#157446=CARTESIAN_POINT('Ctrl Pts',(-17.2910127431203,67.8540944890057,
12.));
#157447=CARTESIAN_POINT('Ctrl Pts',(-17.2911366591419,67.8424198971214,
0.));
#157448=CARTESIAN_POINT('Ctrl Pts',(-17.2911366591419,67.8424198971214,
12.));
#157449=CARTESIAN_POINT('Ctrl Pts',(-17.2912149114145,67.8346476309106,
0.));
#157450=CARTESIAN_POINT('Ctrl Pts',(-17.2912149114145,67.8346476309106,
12.));
#157451=CARTESIAN_POINT('Ctrl Pts',(-17.2912529479484,67.8307641965655,
0.));
#157452=CARTESIAN_POINT('Ctrl Pts',(-17.2912529479484,67.8307641965655,
12.));
#157453=CARTESIAN_POINT('',(-17.2912529479484,67.8307641965655,12.));
#157454=CARTESIAN_POINT('Ctrl Pts',(-17.2912529479484,67.8307641965655,
12.));
#157455=CARTESIAN_POINT('Ctrl Pts',(-17.2912149114145,67.8346476309106,
12.));
#157456=CARTESIAN_POINT('Ctrl Pts',(-17.2911366591419,67.8424198971214,
12.));
#157457=CARTESIAN_POINT('Ctrl Pts',(-17.2910127431203,67.8540944890057,
12.));
#157458=CARTESIAN_POINT('Ctrl Pts',(-17.2908344459816,67.8696929979178,
12.));
#157459=CARTESIAN_POINT('Ctrl Pts',(-17.2905897724029,67.8892451049871,
12.));
#157460=CARTESIAN_POINT('Ctrl Pts',(-17.2903232740717,67.908851149676,12.));
#157461=CARTESIAN_POINT('Ctrl Pts',(-17.2900349103956,67.9285110571662,
12.));
#157462=CARTESIAN_POINT('Ctrl Pts',(-17.2897246158895,67.9482246901517,
12.));
#157463=CARTESIAN_POINT('Ctrl Pts',(-17.2893923013852,67.9679918502441,
12.));
#157464=CARTESIAN_POINT('Ctrl Pts',(-17.2890378644843,67.9878123049133,
12.));
#157465=CARTESIAN_POINT('Ctrl Pts',(-17.28866119774,68.007685808115,12.));
#157466=CARTESIAN_POINT('Ctrl Pts',(-17.2882621974737,68.027612122741,12.));
#157467=CARTESIAN_POINT('Ctrl Pts',(-17.2878407730981,68.0475910442494,
12.));
#157468=CARTESIAN_POINT('Ctrl Pts',(-17.2873968440855,68.0676223930469,
12.));
#157469=CARTESIAN_POINT('Ctrl Pts',(-17.2869303355438,68.0877060033229,
12.));
#157470=CARTESIAN_POINT('Ctrl Pts',(-17.2864411745455,68.1078417137865,
12.));
#157471=CARTESIAN_POINT('Ctrl Pts',(-17.2859292855694,68.1280293561473,
12.));
#157472=CARTESIAN_POINT('Ctrl Pts',(-17.2853945882059,68.1482687493176,
12.));
#157473=CARTESIAN_POINT('Ctrl Pts',(-17.2848369995283,68.1685597054193,
12.));
#157474=CARTESIAN_POINT('Ctrl Pts',(-17.2842564355796,68.1889020335418,
12.));
#157475=CARTESIAN_POINT('Ctrl Pts',(-17.2836528130825,68.2092955440591,
12.));
#157476=CARTESIAN_POINT('Ctrl Pts',(-17.2830260513879,68.2297400535339,
12.));
#157477=CARTESIAN_POINT('Ctrl Pts',(-17.2823760723886,68.250235384512,12.));
#157478=CARTESIAN_POINT('Ctrl Pts',(-17.2817027995838,68.2707813631761,
12.));
#157479=CARTESIAN_POINT('Ctrl Pts',(-17.2810061574352,68.2913778177258,
12.));
#157480=CARTESIAN_POINT('Ctrl Pts',(-17.2802860705807,68.3120245763884,
12.));
#157481=CARTESIAN_POINT('Ctrl Pts',(-17.2795424631789,68.3327214657533,
12.));
#157482=CARTESIAN_POINT('Ctrl Pts',(-17.2787752592475,68.353468311648,12.));
#157483=CARTESIAN_POINT('Ctrl Pts',(-17.2779843829605,68.374264939895,12.));
#157484=CARTESIAN_POINT('Ctrl Pts',(-17.2771697589387,68.3951111770498,
12.));
#157485=CARTESIAN_POINT('Ctrl Pts',(-17.2763313126026,68.4160068512781,
12.));
#157486=CARTESIAN_POINT('Ctrl Pts',(-17.2754689703001,68.4369517926803,
12.));
#157487=CARTESIAN_POINT('Ctrl Pts',(-17.2745826591125,68.4579458328208,
12.));
#157488=CARTESIAN_POINT('Ctrl Pts',(-17.2736723067367,68.4789888044357,
12.));
#157489=CARTESIAN_POINT('Ctrl Pts',(-17.2727378413485,68.5000805410897,
12.));
#157490=CARTESIAN_POINT('Ctrl Pts',(-17.2717791914538,68.5212208767835,
12.));
#157491=CARTESIAN_POINT('Ctrl Pts',(-17.2707962858912,68.5424096459746,
12.));
#157492=CARTESIAN_POINT('Ctrl Pts',(-17.2697890538956,68.5636466837502,
12.));
#157493=CARTESIAN_POINT('Ctrl Pts',(-17.2687574251429,68.5849318259449,
12.));
#157494=CARTESIAN_POINT('Ctrl Pts',(-17.2677013298061,68.6062649092781,
12.));
#157495=CARTESIAN_POINT('Ctrl Pts',(-17.2666206986091,68.6276457714757,
12.));
#157496=CARTESIAN_POINT('Ctrl Pts',(-17.2655154627935,68.6490742512085,
12.));
#157497=CARTESIAN_POINT('Ctrl Pts',(-17.2643855540896,68.6705501880263,
12.));
#157498=CARTESIAN_POINT('Ctrl Pts',(-17.263230904689,68.6920734222932,12.));
#157499=CARTESIAN_POINT('Ctrl Pts',(-17.2620514472176,68.7136437951075,
12.));
#157500=CARTESIAN_POINT('Ctrl Pts',(-17.2608471147178,68.7352611482519,
12.));
#157501=CARTESIAN_POINT('Ctrl Pts',(-17.2596178406545,68.7569253242312,
12.));
#157502=CARTESIAN_POINT('Ctrl Pts',(-17.2583635589197,68.7786361662876,
12.));
#157503=CARTESIAN_POINT('Ctrl Pts',(-17.2570842038385,68.8003935184193,
12.));
#157504=CARTESIAN_POINT('Ctrl Pts',(-17.2557797101816,68.8221972253954,
12.));
#157505=CARTESIAN_POINT('Ctrl Pts',(-17.2544500131627,68.8440471327563,
12.));
#157506=CARTESIAN_POINT('Ctrl Pts',(-17.2530950484259,68.8659430867977,
12.));
#157507=CARTESIAN_POINT('Ctrl Pts',(-17.2517147520376,68.8878849345557,
12.));
#157508=CARTESIAN_POINT('Ctrl Pts',(-17.2503090604792,68.9098725237868,
12.));
#157509=CARTESIAN_POINT('Ctrl Pts',(-17.248877910643,68.9319057029407,12.));
#157510=CARTESIAN_POINT('Ctrl Pts',(-17.2474212398275,68.9539843211618,
12.));
#157511=CARTESIAN_POINT('Ctrl Pts',(-17.2459389857327,68.9761082282922,
12.));
#157512=CARTESIAN_POINT('Ctrl Pts',(-17.2444310864585,68.9982772748694,
12.));
#157513=CARTESIAN_POINT('Ctrl Pts',(-17.2428974805043,69.0204913121226,
12.));
#157514=CARTESIAN_POINT('Ctrl Pts',(-17.2413381067722,69.0427501919636,
12.));
#157515=CARTESIAN_POINT('Ctrl Pts',(-17.2397529045587,69.0650537669859,
12.));
#157516=CARTESIAN_POINT('Ctrl Pts',(-17.238141813549,69.0874018904598,12.));
#157517=CARTESIAN_POINT('Ctrl Pts',(-17.2365047738125,69.1097944163243,
12.));
#157518=CARTESIAN_POINT('Ctrl Pts',(-17.2348417258017,69.1322311991759,
12.));
#157519=CARTESIAN_POINT('Ctrl Pts',(-17.2331526103511,69.1547120942542,
12.));
#157520=CARTESIAN_POINT('Ctrl Pts',(-17.2314373686705,69.1772369574462,
12.));
#157521=CARTESIAN_POINT('Ctrl Pts',(-17.229695942341,69.1998056452837,12.));
#157522=CARTESIAN_POINT('Ctrl Pts',(-17.2279282733119,69.2224180149377,
12.));
#157523=CARTESIAN_POINT('Ctrl Pts',(-17.2261343039015,69.2450739242092,
12.));
#157524=CARTESIAN_POINT('Ctrl Pts',(-17.2243139767963,69.26777323152,12.));
#157525=CARTESIAN_POINT('Ctrl Pts',(-17.2224672350432,69.2905157959142,
12.));
#157526=CARTESIAN_POINT('Ctrl Pts',(-17.2205940220455,69.3133014770541,
12.));
#157527=CARTESIAN_POINT('Ctrl Pts',(-17.2186942815604,69.3361301352149,
12.));
#157528=CARTESIAN_POINT('Ctrl Pts',(-17.2167679576991,69.359001631272,12.));
#157529=CARTESIAN_POINT('Ctrl Pts',(-17.2148149949261,69.3819158266955,
12.));
#157530=CARTESIAN_POINT('Ctrl Pts',(-17.2128353380511,69.4048725835516,
12.));
#157531=CARTESIAN_POINT('Ctrl Pts',(-17.2108289322258,69.4278717644989,
12.));
#157532=CARTESIAN_POINT('Ctrl Pts',(-17.208795722942,69.4509132327836,12.));
#157533=CARTESIAN_POINT('Ctrl Pts',(-17.2067356560326,69.4739968522271,
12.));
#157534=CARTESIAN_POINT('Ctrl Pts',(-17.2046486776697,69.497122487222,12.));
#157535=CARTESIAN_POINT('Ctrl Pts',(-17.2025347343568,69.5202900027329,
12.));
#157536=CARTESIAN_POINT('Ctrl Pts',(-17.2003937729266,69.5434992642932,
12.));
#157537=CARTESIAN_POINT('Ctrl Pts',(-17.198225740538,69.5667501379984,12.));
#157538=CARTESIAN_POINT('Ctrl Pts',(-17.1960305846787,69.5900424904954,
12.));
#157539=CARTESIAN_POINT('Ctrl Pts',(-17.193808253162,69.6133761889787,12.));
#157540=CARTESIAN_POINT('Ctrl Pts',(-17.1915586941198,69.6367511011927,
12.));
#157541=CARTESIAN_POINT('Ctrl Pts',(-17.1892818560004,69.6601670954277,
12.));
#157542=CARTESIAN_POINT('Ctrl Pts',(-17.1869776875663,69.6836240405152,
12.));
#157543=CARTESIAN_POINT('Ctrl Pts',(-17.1846461378966,69.7071218058149,
12.));
#157544=CARTESIAN_POINT('Ctrl Pts',(-17.1822871563835,69.7306602612125,
12.));
#157545=CARTESIAN_POINT('Ctrl Pts',(-17.1799006927256,69.7542392771216,
12.));
#157546=CARTESIAN_POINT('Ctrl Pts',(-17.1774866969256,69.7778587244788,
12.));
#157547=CARTESIAN_POINT('Ctrl Pts',(-17.1750451192887,69.8015184747404,
12.));
#157548=CARTESIAN_POINT('Ctrl Pts',(-17.1725759104254,69.8252183998713,
12.));
#157549=CARTESIAN_POINT('Ctrl Pts',(-17.1700790212476,69.8489583723417,
12.));
#157550=CARTESIAN_POINT('Ctrl Pts',(-17.1675544029622,69.8727382651292,
12.));
#157551=CARTESIAN_POINT('Ctrl Pts',(-17.1650020070686,69.8965579517147,
12.));
#157552=CARTESIAN_POINT('Ctrl Pts',(-17.1624217853577,69.9204173060779,
12.));
#157553=CARTESIAN_POINT('Ctrl Pts',(-17.1598136899144,69.9443162026865,
12.));
#157554=CARTESIAN_POINT('Ctrl Pts',(-17.157177673114,69.9682545164942,12.));
#157555=CARTESIAN_POINT('Ctrl Pts',(-17.1545136876162,69.9922321229428,
12.));
#157556=CARTESIAN_POINT('Ctrl Pts',(-17.1518216863624,70.0162488979587,
12.));
#157557=CARTESIAN_POINT('Ctrl Pts',(-17.1491016225748,70.0403047179481,
12.));
#157558=CARTESIAN_POINT('Ctrl Pts',(-17.1463534497592,70.0643994597865,
12.));
#157559=CARTESIAN_POINT('Ctrl Pts',(-17.1435771217015,70.0885330008169,
12.));
#157560=CARTESIAN_POINT('Ctrl Pts',(-17.1407725924615,70.1127052188515,
12.));
#157561=CARTESIAN_POINT('Ctrl Pts',(-17.1379398163708,70.1369159921686,
12.));
#157562=CARTESIAN_POINT('Ctrl Pts',(-17.1350787480313,70.1611651995085,
12.));
#157563=CARTESIAN_POINT('Ctrl Pts',(-17.1321893423183,70.1854527200636,
12.));
#157564=CARTESIAN_POINT('Ctrl Pts',(-17.1292715543779,70.2097784334749,
12.));
#157565=CARTESIAN_POINT('Ctrl Pts',(-17.1263253396202,70.2341422198363,
12.));
#157566=CARTESIAN_POINT('Ctrl Pts',(-17.1233506537176,70.2585439596899,
12.));
#157567=CARTESIAN_POINT('Ctrl Pts',(-17.1203474526031,70.2829835340239,
12.));
#157568=CARTESIAN_POINT('Ctrl Pts',(-17.1173156924734,70.3074608242613,
12.));
#157569=CARTESIAN_POINT('Ctrl Pts',(-17.1142553297869,70.3319757122577,
12.));
#157570=CARTESIAN_POINT('Ctrl Pts',(-17.111166321257,70.356528080303,12.));
#157571=CARTESIAN_POINT('Ctrl Pts',(-17.10804862385,70.3811178111206,12.));
#157572=CARTESIAN_POINT('Ctrl Pts',(-17.1049021947833,70.4057447878621,
12.));
#157573=CARTESIAN_POINT('Ctrl Pts',(-17.1017269915289,70.4304088940998,
12.));
#157574=CARTESIAN_POINT('Ctrl Pts',(-17.098522971812,70.4551100138221,12.));
#157575=CARTESIAN_POINT('Ctrl Pts',(-17.0952900936044,70.4798480314364,
12.));
#157576=CARTESIAN_POINT('Ctrl Pts',(-17.0920283151217,70.5046228317669,
12.));
#157577=CARTESIAN_POINT('Ctrl Pts',(-17.0887375948221,70.5294343000516,
12.));
#157578=CARTESIAN_POINT('Ctrl Pts',(-17.085417891409,70.5542823219346,12.));
#157579=CARTESIAN_POINT('Ctrl Pts',(-17.0820691638314,70.5791667834599,
12.));
#157580=CARTESIAN_POINT('Ctrl Pts',(-17.0786913712767,70.6040875710762,
12.));
#157581=CARTESIAN_POINT('Ctrl Pts',(-17.0752844731679,70.6290445716341,
12.));
#157582=CARTESIAN_POINT('Ctrl Pts',(-17.0718484291623,70.6540376723839,
12.));
#157583=CARTESIAN_POINT('Ctrl Pts',(-17.0683831991532,70.6790667609678,
12.));
#157584=CARTESIAN_POINT('Ctrl Pts',(-17.0648887432714,70.7041317254128,
12.));
#157585=CARTESIAN_POINT('Ctrl Pts',(-17.0613650218789,70.7292324541348,
12.));
#157586=CARTESIAN_POINT('Ctrl Pts',(-17.0578119955651,70.754368835938,12.));
#157587=CARTESIAN_POINT('Ctrl Pts',(-17.0542296251462,70.7795407600127,
12.));
#157588=CARTESIAN_POINT('Ctrl Pts',(-17.0506178716662,70.8047481159298,
12.));
#157589=CARTESIAN_POINT('Ctrl Pts',(-17.0469766964001,70.8299907936334,
12.));
#157590=CARTESIAN_POINT('Ctrl Pts',(-17.0433060608475,70.8552686834423,
12.));
#157591=CARTESIAN_POINT('Ctrl Pts',(-17.0396059267277,70.8805816760501,
12.));
#157592=CARTESIAN_POINT('Ctrl Pts',(-17.0358762559786,70.9059296625214,
12.));
#157593=CARTESIAN_POINT('Ctrl Pts',(-17.0321170107564,70.9313125342876,
12.));
#157594=CARTESIAN_POINT('Ctrl Pts',(-17.0283281534392,70.956730183136,12.));
#157595=CARTESIAN_POINT('Ctrl Pts',(-17.0245096466229,70.9821825012136,
12.));
#157596=CARTESIAN_POINT('Ctrl Pts',(-17.0206614531166,71.0076693810301,
12.));
#157597=CARTESIAN_POINT('Ctrl Pts',(-17.0167835359419,71.0331907154574,
12.));
#157598=CARTESIAN_POINT('Ctrl Pts',(-17.0128758583335,71.0587463977268,
12.));
#157599=CARTESIAN_POINT('Ctrl Pts',(-17.0089383837437,71.0843363214221,
12.));
#157600=CARTESIAN_POINT('Ctrl Pts',(-17.0049710758394,71.1099603804786,
12.));
#157601=CARTESIAN_POINT('Ctrl Pts',(-17.0009738984936,71.1356184691806,
12.));
#157602=CARTESIAN_POINT('Ctrl Pts',(-16.9969468157824,71.1613104821568,
12.));
#157603=CARTESIAN_POINT('Ctrl Pts',(-16.9928897919828,71.187036314374,12.));
#157604=CARTESIAN_POINT('Ctrl Pts',(-16.9888027915742,71.212795861124,12.));
#157605=CARTESIAN_POINT('Ctrl Pts',(-16.9846857792384,71.2385890180221,
12.));
#157606=CARTESIAN_POINT('Ctrl Pts',(-16.9805387198571,71.2644156810198,
12.));
#157607=CARTESIAN_POINT('Ctrl Pts',(-16.9763615785137,71.290275746412,12.));
#157608=CARTESIAN_POINT('Ctrl Pts',(-16.9721543204951,71.3161691108427,
12.));
#157609=CARTESIAN_POINT('Ctrl Pts',(-16.9679169112994,71.3420956713082,
12.));
#157610=CARTESIAN_POINT('Ctrl Pts',(-16.9636493166397,71.3680553251562,
12.));
#157611=CARTESIAN_POINT('Ctrl Pts',(-16.9593515024276,71.3940479700677,
12.));
#157612=CARTESIAN_POINT('Ctrl Pts',(-16.9550234347621,71.4200735040384,
12.));
#157613=CARTESIAN_POINT('Ctrl Pts',(-16.9506650799189,71.4461318253563,
12.));
#157614=CARTESIAN_POINT('Ctrl Pts',(-16.9462764043443,71.4722228325794,
12.));
#157615=CARTESIAN_POINT('Ctrl Pts',(-16.9418573746489,71.4983464245055,
12.));
#157616=CARTESIAN_POINT('Ctrl Pts',(-16.9374079576201,71.5245025002139,
12.));
#157617=CARTESIAN_POINT('Ctrl Pts',(-16.9329281202377,71.5506909591129,
12.));
#157618=CARTESIAN_POINT('Ctrl Pts',(-16.9284178296933,71.5769117009842,
12.));
#157619=CARTESIAN_POINT('Ctrl Pts',(-16.9238770534071,71.6031646260174,
12.));
#157620=CARTESIAN_POINT('Ctrl Pts',(-16.9193057590607,71.6294496348653,
12.));
#157621=CARTESIAN_POINT('Ctrl Pts',(-16.9147039145717,71.6557666285917,
12.));
#157622=CARTESIAN_POINT('Ctrl Pts',(-16.9100714880368,71.6821155085612,
12.));
#157623=CARTESIAN_POINT('Ctrl Pts',(-16.9054084476847,71.7084961763357,
12.));
#157624=CARTESIAN_POINT('Ctrl Pts',(-16.9007147618344,71.7349085335796,
12.));
#157625=CARTESIAN_POINT('Ctrl Pts',(-16.895990398841,71.7613524819235,12.));
#157626=CARTESIAN_POINT('Ctrl Pts',(-16.8912353270942,71.7878279229546,
12.));
#157627=CARTESIAN_POINT('Ctrl Pts',(-16.8864495151344,71.8143347584962,
12.));
#157628=CARTESIAN_POINT('Ctrl Pts',(-16.881632931747,71.8408728908258,12.));
#157629=CARTESIAN_POINT('Ctrl Pts',(-16.87678554607,71.867442222915,12.));
#157630=CARTESIAN_POINT('Ctrl Pts',(-16.871907327697,71.8940426586534,12.));
#157631=CARTESIAN_POINT('Ctrl Pts',(-16.866998246792,71.9206741030887,12.));
#157632=CARTESIAN_POINT('Ctrl Pts',(-16.8620582738437,71.9473364618922,
12.));
#157633=CARTESIAN_POINT('Ctrl Pts',(-16.8570873794269,71.9740296408347,
12.));
#157634=CARTESIAN_POINT('Ctrl Pts',(-16.8520855339446,72.0007535452081,
12.));
#157635=CARTESIAN_POINT('Ctrl Pts',(-16.8470527074275,72.0275080793727,
12.));
#157636=CARTESIAN_POINT('Ctrl Pts',(-16.8419888691976,72.0542931459825,
12.));
#157637=CARTESIAN_POINT('Ctrl Pts',(-16.8368939881446,72.0811086466121,
12.));
#157638=CARTESIAN_POINT('Ctrl Pts',(-16.8317680333404,72.1079544831513,
12.));
#157639=CARTESIAN_POINT('Ctrl Pts',(-16.8266109745795,72.13483055902,12.));
#157640=CARTESIAN_POINT('Ctrl Pts',(-16.8214227828943,72.1617367803235,
12.));
#157641=CARTESIAN_POINT('Ctrl Pts',(-16.8162034312269,72.1886730573452,
12.));
#157642=CARTESIAN_POINT('Ctrl Pts',(-16.8109528945896,72.2156393048975,
12.));
#157643=CARTESIAN_POINT('Ctrl Pts',(-16.8064254147776,72.2387802230856,
12.));
#157644=CARTESIAN_POINT('Ctrl Pts',(-16.8029374213794,72.256538003526,12.));
#157645=CARTESIAN_POINT('Ctrl Pts',(-16.8005027425863,72.2688994295264,
12.));
#157646=CARTESIAN_POINT('Ctrl Pts',(-16.7991305317749,72.2758557891329,
12.));
#157647=CARTESIAN_POINT('Ctrl Pts',(-16.7988252568748,72.2774028393914,
12.));
#157648=CARTESIAN_POINT('',(-17.2912529479484,67.8307641965655,0.));
#157649=CARTESIAN_POINT('',(-17.2912529479484,67.8307641965655,0.));
#157650=CARTESIAN_POINT('Ctrl Pts',(-16.7988252568748,72.2774028393914,
0.));
#157651=CARTESIAN_POINT('Ctrl Pts',(-16.7991305317749,72.2758557891329,
0.));
#157652=CARTESIAN_POINT('Ctrl Pts',(-16.8005027425863,72.2688994295264,
0.));
#157653=CARTESIAN_POINT('Ctrl Pts',(-16.8029374213794,72.256538003526,0.));
#157654=CARTESIAN_POINT('Ctrl Pts',(-16.8064254147776,72.2387802230856,
0.));
#157655=CARTESIAN_POINT('Ctrl Pts',(-16.8109528945896,72.2156393048975,
0.));
#157656=CARTESIAN_POINT('Ctrl Pts',(-16.8162034312269,72.1886730573452,
0.));
#157657=CARTESIAN_POINT('Ctrl Pts',(-16.8214227828943,72.1617367803235,
0.));
#157658=CARTESIAN_POINT('Ctrl Pts',(-16.8266109745795,72.13483055902,0.));
#157659=CARTESIAN_POINT('Ctrl Pts',(-16.8317680333404,72.1079544831513,
0.));
#157660=CARTESIAN_POINT('Ctrl Pts',(-16.8368939881446,72.0811086466121,
0.));
#157661=CARTESIAN_POINT('Ctrl Pts',(-16.8419888691976,72.0542931459825,
0.));
#157662=CARTESIAN_POINT('Ctrl Pts',(-16.8470527074275,72.0275080793727,
0.));
#157663=CARTESIAN_POINT('Ctrl Pts',(-16.8520855339446,72.0007535452081,
0.));
#157664=CARTESIAN_POINT('Ctrl Pts',(-16.8570873794269,71.9740296408347,
0.));
#157665=CARTESIAN_POINT('Ctrl Pts',(-16.8620582738437,71.9473364618922,
0.));
#157666=CARTESIAN_POINT('Ctrl Pts',(-16.866998246792,71.9206741030887,0.));
#157667=CARTESIAN_POINT('Ctrl Pts',(-16.871907327697,71.8940426586534,0.));
#157668=CARTESIAN_POINT('Ctrl Pts',(-16.87678554607,71.867442222915,0.));
#157669=CARTESIAN_POINT('Ctrl Pts',(-16.881632931747,71.8408728908258,0.));
#157670=CARTESIAN_POINT('Ctrl Pts',(-16.8864495151344,71.8143347584962,
0.));
#157671=CARTESIAN_POINT('Ctrl Pts',(-16.8912353270942,71.7878279229546,
0.));
#157672=CARTESIAN_POINT('Ctrl Pts',(-16.895990398841,71.7613524819235,0.));
#157673=CARTESIAN_POINT('Ctrl Pts',(-16.9007147618344,71.7349085335796,
0.));
#157674=CARTESIAN_POINT('Ctrl Pts',(-16.9054084476847,71.7084961763357,
0.));
#157675=CARTESIAN_POINT('Ctrl Pts',(-16.9100714880368,71.6821155085612,
0.));
#157676=CARTESIAN_POINT('Ctrl Pts',(-16.9147039145717,71.6557666285917,
0.));
#157677=CARTESIAN_POINT('Ctrl Pts',(-16.9193057590607,71.6294496348653,
0.));
#157678=CARTESIAN_POINT('Ctrl Pts',(-16.9238770534071,71.6031646260174,
0.));
#157679=CARTESIAN_POINT('Ctrl Pts',(-16.9284178296933,71.5769117009842,
0.));
#157680=CARTESIAN_POINT('Ctrl Pts',(-16.9329281202377,71.5506909591129,
0.));
#157681=CARTESIAN_POINT('Ctrl Pts',(-16.9374079576201,71.5245025002139,
0.));
#157682=CARTESIAN_POINT('Ctrl Pts',(-16.9418573746489,71.4983464245055,
0.));
#157683=CARTESIAN_POINT('Ctrl Pts',(-16.9462764043443,71.4722228325794,
0.));
#157684=CARTESIAN_POINT('Ctrl Pts',(-16.9506650799189,71.4461318253563,
0.));
#157685=CARTESIAN_POINT('Ctrl Pts',(-16.9550234347621,71.4200735040384,
0.));
#157686=CARTESIAN_POINT('Ctrl Pts',(-16.9593515024276,71.3940479700677,
0.));
#157687=CARTESIAN_POINT('Ctrl Pts',(-16.9636493166397,71.3680553251562,
0.));
#157688=CARTESIAN_POINT('Ctrl Pts',(-16.9679169112994,71.3420956713082,
0.));
#157689=CARTESIAN_POINT('Ctrl Pts',(-16.9721543204951,71.3161691108427,
0.));
#157690=CARTESIAN_POINT('Ctrl Pts',(-16.9763615785137,71.290275746412,0.));
#157691=CARTESIAN_POINT('Ctrl Pts',(-16.9805387198571,71.2644156810198,
0.));
#157692=CARTESIAN_POINT('Ctrl Pts',(-16.9846857792384,71.2385890180221,
0.));
#157693=CARTESIAN_POINT('Ctrl Pts',(-16.9888027915742,71.212795861124,0.));
#157694=CARTESIAN_POINT('Ctrl Pts',(-16.9928897919828,71.187036314374,0.));
#157695=CARTESIAN_POINT('Ctrl Pts',(-16.9969468157824,71.1613104821568,
0.));
#157696=CARTESIAN_POINT('Ctrl Pts',(-17.0009738984936,71.1356184691806,
0.));
#157697=CARTESIAN_POINT('Ctrl Pts',(-17.0049710758394,71.1099603804786,
0.));
#157698=CARTESIAN_POINT('Ctrl Pts',(-17.0089383837437,71.0843363214221,
0.));
#157699=CARTESIAN_POINT('Ctrl Pts',(-17.0128758583335,71.0587463977268,
0.));
#157700=CARTESIAN_POINT('Ctrl Pts',(-17.0167835359419,71.0331907154574,
0.));
#157701=CARTESIAN_POINT('Ctrl Pts',(-17.0206614531166,71.0076693810301,
0.));
#157702=CARTESIAN_POINT('Ctrl Pts',(-17.0245096466229,70.9821825012136,
0.));
#157703=CARTESIAN_POINT('Ctrl Pts',(-17.0283281534392,70.956730183136,0.));
#157704=CARTESIAN_POINT('Ctrl Pts',(-17.0321170107564,70.9313125342876,
0.));
#157705=CARTESIAN_POINT('Ctrl Pts',(-17.0358762559786,70.9059296625214,
0.));
#157706=CARTESIAN_POINT('Ctrl Pts',(-17.0396059267277,70.8805816760501,
0.));
#157707=CARTESIAN_POINT('Ctrl Pts',(-17.0433060608475,70.8552686834423,
0.));
#157708=CARTESIAN_POINT('Ctrl Pts',(-17.0469766964001,70.8299907936334,
0.));
#157709=CARTESIAN_POINT('Ctrl Pts',(-17.0506178716662,70.8047481159298,
0.));
#157710=CARTESIAN_POINT('Ctrl Pts',(-17.0542296251462,70.7795407600127,
0.));
#157711=CARTESIAN_POINT('Ctrl Pts',(-17.0578119955651,70.754368835938,0.));
#157712=CARTESIAN_POINT('Ctrl Pts',(-17.0613650218789,70.7292324541348,
0.));
#157713=CARTESIAN_POINT('Ctrl Pts',(-17.0648887432714,70.7041317254128,
0.));
#157714=CARTESIAN_POINT('Ctrl Pts',(-17.0683831991532,70.6790667609678,
0.));
#157715=CARTESIAN_POINT('Ctrl Pts',(-17.0718484291623,70.6540376723839,
0.));
#157716=CARTESIAN_POINT('Ctrl Pts',(-17.0752844731679,70.6290445716341,
0.));
#157717=CARTESIAN_POINT('Ctrl Pts',(-17.0786913712767,70.6040875710762,
0.));
#157718=CARTESIAN_POINT('Ctrl Pts',(-17.0820691638314,70.5791667834599,
0.));
#157719=CARTESIAN_POINT('Ctrl Pts',(-17.085417891409,70.5542823219346,0.));
#157720=CARTESIAN_POINT('Ctrl Pts',(-17.0887375948221,70.5294343000516,
0.));
#157721=CARTESIAN_POINT('Ctrl Pts',(-17.0920283151217,70.5046228317669,
0.));
#157722=CARTESIAN_POINT('Ctrl Pts',(-17.0952900936044,70.4798480314364,
0.));
#157723=CARTESIAN_POINT('Ctrl Pts',(-17.098522971812,70.4551100138221,0.));
#157724=CARTESIAN_POINT('Ctrl Pts',(-17.1017269915289,70.4304088940998,
0.));
#157725=CARTESIAN_POINT('Ctrl Pts',(-17.1049021947833,70.4057447878621,
0.));
#157726=CARTESIAN_POINT('Ctrl Pts',(-17.10804862385,70.3811178111206,0.));
#157727=CARTESIAN_POINT('Ctrl Pts',(-17.111166321257,70.356528080303,0.));
#157728=CARTESIAN_POINT('Ctrl Pts',(-17.1142553297869,70.3319757122577,
0.));
#157729=CARTESIAN_POINT('Ctrl Pts',(-17.1173156924734,70.3074608242613,
0.));
#157730=CARTESIAN_POINT('Ctrl Pts',(-17.1203474526031,70.2829835340239,
0.));
#157731=CARTESIAN_POINT('Ctrl Pts',(-17.1233506537176,70.2585439596899,
0.));
#157732=CARTESIAN_POINT('Ctrl Pts',(-17.1263253396202,70.2341422198363,
0.));
#157733=CARTESIAN_POINT('Ctrl Pts',(-17.1292715543779,70.2097784334749,
0.));
#157734=CARTESIAN_POINT('Ctrl Pts',(-17.1321893423183,70.1854527200636,
0.));
#157735=CARTESIAN_POINT('Ctrl Pts',(-17.1350787480313,70.1611651995085,
0.));
#157736=CARTESIAN_POINT('Ctrl Pts',(-17.1379398163708,70.1369159921686,
0.));
#157737=CARTESIAN_POINT('Ctrl Pts',(-17.1407725924615,70.1127052188515,
0.));
#157738=CARTESIAN_POINT('Ctrl Pts',(-17.1435771217015,70.0885330008169,
0.));
#157739=CARTESIAN_POINT('Ctrl Pts',(-17.1463534497592,70.0643994597865,
0.));
#157740=CARTESIAN_POINT('Ctrl Pts',(-17.1491016225748,70.0403047179481,
0.));
#157741=CARTESIAN_POINT('Ctrl Pts',(-17.1518216863624,70.0162488979587,
0.));
#157742=CARTESIAN_POINT('Ctrl Pts',(-17.1545136876162,69.9922321229428,
0.));
#157743=CARTESIAN_POINT('Ctrl Pts',(-17.157177673114,69.9682545164942,0.));
#157744=CARTESIAN_POINT('Ctrl Pts',(-17.1598136899144,69.9443162026865,
0.));
#157745=CARTESIAN_POINT('Ctrl Pts',(-17.1624217853577,69.9204173060779,
0.));
#157746=CARTESIAN_POINT('Ctrl Pts',(-17.1650020070686,69.8965579517147,
0.));
#157747=CARTESIAN_POINT('Ctrl Pts',(-17.1675544029622,69.8727382651292,
0.));
#157748=CARTESIAN_POINT('Ctrl Pts',(-17.1700790212476,69.8489583723417,
0.));
#157749=CARTESIAN_POINT('Ctrl Pts',(-17.1725759104254,69.8252183998713,
0.));
#157750=CARTESIAN_POINT('Ctrl Pts',(-17.1750451192887,69.8015184747404,
0.));
#157751=CARTESIAN_POINT('Ctrl Pts',(-17.1774866969256,69.7778587244788,
0.));
#157752=CARTESIAN_POINT('Ctrl Pts',(-17.1799006927256,69.7542392771216,
0.));
#157753=CARTESIAN_POINT('Ctrl Pts',(-17.1822871563835,69.7306602612125,
0.));
#157754=CARTESIAN_POINT('Ctrl Pts',(-17.1846461378966,69.7071218058149,
0.));
#157755=CARTESIAN_POINT('Ctrl Pts',(-17.1869776875663,69.6836240405152,
0.));
#157756=CARTESIAN_POINT('Ctrl Pts',(-17.1892818560004,69.6601670954277,
0.));
#157757=CARTESIAN_POINT('Ctrl Pts',(-17.1915586941198,69.6367511011927,
0.));
#157758=CARTESIAN_POINT('Ctrl Pts',(-17.193808253162,69.6133761889787,0.));
#157759=CARTESIAN_POINT('Ctrl Pts',(-17.1960305846787,69.5900424904954,
0.));
#157760=CARTESIAN_POINT('Ctrl Pts',(-17.198225740538,69.5667501379984,0.));
#157761=CARTESIAN_POINT('Ctrl Pts',(-17.2003937729266,69.5434992642932,
0.));
#157762=CARTESIAN_POINT('Ctrl Pts',(-17.2025347343568,69.5202900027329,
0.));
#157763=CARTESIAN_POINT('Ctrl Pts',(-17.2046486776697,69.497122487222,0.));
#157764=CARTESIAN_POINT('Ctrl Pts',(-17.2067356560326,69.4739968522271,
0.));
#157765=CARTESIAN_POINT('Ctrl Pts',(-17.208795722942,69.4509132327836,0.));
#157766=CARTESIAN_POINT('Ctrl Pts',(-17.2108289322258,69.4278717644989,
0.));
#157767=CARTESIAN_POINT('Ctrl Pts',(-17.2128353380511,69.4048725835516,
0.));
#157768=CARTESIAN_POINT('Ctrl Pts',(-17.2148149949261,69.3819158266955,
0.));
#157769=CARTESIAN_POINT('Ctrl Pts',(-17.2167679576991,69.359001631272,0.));
#157770=CARTESIAN_POINT('Ctrl Pts',(-17.2186942815604,69.3361301352149,
0.));
#157771=CARTESIAN_POINT('Ctrl Pts',(-17.2205940220455,69.3133014770541,
0.));
#157772=CARTESIAN_POINT('Ctrl Pts',(-17.2224672350432,69.2905157959142,
0.));
#157773=CARTESIAN_POINT('Ctrl Pts',(-17.2243139767963,69.26777323152,0.));
#157774=CARTESIAN_POINT('Ctrl Pts',(-17.2261343039015,69.2450739242092,
0.));
#157775=CARTESIAN_POINT('Ctrl Pts',(-17.2279282733119,69.2224180149377,
0.));
#157776=CARTESIAN_POINT('Ctrl Pts',(-17.229695942341,69.1998056452837,0.));
#157777=CARTESIAN_POINT('Ctrl Pts',(-17.2314373686705,69.1772369574462,
0.));
#157778=CARTESIAN_POINT('Ctrl Pts',(-17.2331526103511,69.1547120942542,
0.));
#157779=CARTESIAN_POINT('Ctrl Pts',(-17.2348417258017,69.1322311991759,
0.));
#157780=CARTESIAN_POINT('Ctrl Pts',(-17.2365047738125,69.1097944163243,
0.));
#157781=CARTESIAN_POINT('Ctrl Pts',(-17.238141813549,69.0874018904598,0.));
#157782=CARTESIAN_POINT('Ctrl Pts',(-17.2397529045587,69.0650537669859,
0.));
#157783=CARTESIAN_POINT('Ctrl Pts',(-17.2413381067722,69.0427501919636,
0.));
#157784=CARTESIAN_POINT('Ctrl Pts',(-17.2428974805043,69.0204913121226,
0.));
#157785=CARTESIAN_POINT('Ctrl Pts',(-17.2444310864585,68.9982772748694,
0.));
#157786=CARTESIAN_POINT('Ctrl Pts',(-17.2459389857327,68.9761082282922,
0.));
#157787=CARTESIAN_POINT('Ctrl Pts',(-17.2474212398275,68.9539843211618,
0.));
#157788=CARTESIAN_POINT('Ctrl Pts',(-17.248877910643,68.9319057029407,0.));
#157789=CARTESIAN_POINT('Ctrl Pts',(-17.2503090604792,68.9098725237868,
0.));
#157790=CARTESIAN_POINT('Ctrl Pts',(-17.2517147520376,68.8878849345557,
0.));
#157791=CARTESIAN_POINT('Ctrl Pts',(-17.2530950484259,68.8659430867977,
0.));
#157792=CARTESIAN_POINT('Ctrl Pts',(-17.2544500131627,68.8440471327563,
0.));
#157793=CARTESIAN_POINT('Ctrl Pts',(-17.2557797101816,68.8221972253954,
0.));
#157794=CARTESIAN_POINT('Ctrl Pts',(-17.2570842038385,68.8003935184193,
0.));
#157795=CARTESIAN_POINT('Ctrl Pts',(-17.2583635589197,68.7786361662876,
0.));
#157796=CARTESIAN_POINT('Ctrl Pts',(-17.2596178406545,68.7569253242312,
0.));
#157797=CARTESIAN_POINT('Ctrl Pts',(-17.2608471147178,68.7352611482519,
0.));
#157798=CARTESIAN_POINT('Ctrl Pts',(-17.2620514472176,68.7136437951075,
0.));
#157799=CARTESIAN_POINT('Ctrl Pts',(-17.263230904689,68.6920734222932,0.));
#157800=CARTESIAN_POINT('Ctrl Pts',(-17.2643855540896,68.6705501880263,
0.));
#157801=CARTESIAN_POINT('Ctrl Pts',(-17.2655154627935,68.6490742512085,
0.));
#157802=CARTESIAN_POINT('Ctrl Pts',(-17.2666206986091,68.6276457714757,
0.));
#157803=CARTESIAN_POINT('Ctrl Pts',(-17.2677013298061,68.6062649092781,
0.));
#157804=CARTESIAN_POINT('Ctrl Pts',(-17.2687574251429,68.5849318259449,
0.));
#157805=CARTESIAN_POINT('Ctrl Pts',(-17.2697890538956,68.5636466837502,
0.));
#157806=CARTESIAN_POINT('Ctrl Pts',(-17.2707962858912,68.5424096459746,
0.));
#157807=CARTESIAN_POINT('Ctrl Pts',(-17.2717791914538,68.5212208767835,
0.));
#157808=CARTESIAN_POINT('Ctrl Pts',(-17.2727378413485,68.5000805410897,
0.));
#157809=CARTESIAN_POINT('Ctrl Pts',(-17.2736723067367,68.4789888044357,
0.));
#157810=CARTESIAN_POINT('Ctrl Pts',(-17.2745826591125,68.4579458328208,
0.));
#157811=CARTESIAN_POINT('Ctrl Pts',(-17.2754689703001,68.4369517926803,
0.));
#157812=CARTESIAN_POINT('Ctrl Pts',(-17.2763313126026,68.4160068512781,
0.));
#157813=CARTESIAN_POINT('Ctrl Pts',(-17.2771697589387,68.3951111770498,
0.));
#157814=CARTESIAN_POINT('Ctrl Pts',(-17.2779843829605,68.374264939895,0.));
#157815=CARTESIAN_POINT('Ctrl Pts',(-17.2787752592475,68.353468311648,0.));
#157816=CARTESIAN_POINT('Ctrl Pts',(-17.2795424631789,68.3327214657533,
0.));
#157817=CARTESIAN_POINT('Ctrl Pts',(-17.2802860705807,68.3120245763884,
0.));
#157818=CARTESIAN_POINT('Ctrl Pts',(-17.2810061574352,68.2913778177258,
0.));
#157819=CARTESIAN_POINT('Ctrl Pts',(-17.2817027995838,68.2707813631761,
0.));
#157820=CARTESIAN_POINT('Ctrl Pts',(-17.2823760723886,68.250235384512,0.));
#157821=CARTESIAN_POINT('Ctrl Pts',(-17.2830260513879,68.2297400535339,
0.));
#157822=CARTESIAN_POINT('Ctrl Pts',(-17.2836528130825,68.2092955440591,
0.));
#157823=CARTESIAN_POINT('Ctrl Pts',(-17.2842564355796,68.1889020335418,
0.));
#157824=CARTESIAN_POINT('Ctrl Pts',(-17.2848369995283,68.1685597054193,
0.));
#157825=CARTESIAN_POINT('Ctrl Pts',(-17.2853945882059,68.1482687493176,
0.));
#157826=CARTESIAN_POINT('Ctrl Pts',(-17.2859292855694,68.1280293561473,
0.));
#157827=CARTESIAN_POINT('Ctrl Pts',(-17.2864411745455,68.1078417137865,
0.));
#157828=CARTESIAN_POINT('Ctrl Pts',(-17.2869303355438,68.0877060033229,
0.));
#157829=CARTESIAN_POINT('Ctrl Pts',(-17.2873968440855,68.0676223930469,
0.));
#157830=CARTESIAN_POINT('Ctrl Pts',(-17.2878407730981,68.0475910442494,
0.));
#157831=CARTESIAN_POINT('Ctrl Pts',(-17.2882621974737,68.027612122741,0.));
#157832=CARTESIAN_POINT('Ctrl Pts',(-17.28866119774,68.007685808115,0.));
#157833=CARTESIAN_POINT('Ctrl Pts',(-17.2890378644843,67.9878123049133,
0.));
#157834=CARTESIAN_POINT('Ctrl Pts',(-17.2893923013852,67.9679918502441,
0.));
#157835=CARTESIAN_POINT('Ctrl Pts',(-17.2897246158895,67.9482246901517,
0.));
#157836=CARTESIAN_POINT('Ctrl Pts',(-17.2900349103956,67.9285110571662,
0.));
#157837=CARTESIAN_POINT('Ctrl Pts',(-17.2903232740717,67.908851149676,0.));
#157838=CARTESIAN_POINT('Ctrl Pts',(-17.2905897724029,67.8892451049871,
0.));
#157839=CARTESIAN_POINT('Ctrl Pts',(-17.2908344459816,67.8696929979178,
0.));
#157840=CARTESIAN_POINT('Ctrl Pts',(-17.2910127431203,67.8540944890057,
0.));
#157841=CARTESIAN_POINT('Ctrl Pts',(-17.2911366591419,67.8424198971214,
0.));
#157842=CARTESIAN_POINT('Ctrl Pts',(-17.2912149114145,67.8346476309106,
0.));
#157843=CARTESIAN_POINT('Ctrl Pts',(-17.2912529479484,67.8307641965655,
0.));
#157844=CARTESIAN_POINT('Ctrl Pts',(-10.343287191141,73.778495580227,0.));
#157845=CARTESIAN_POINT('Ctrl Pts',(-10.343287191141,73.778495580227,12.));
#157846=CARTESIAN_POINT('Ctrl Pts',(-10.3449014384453,73.7731377048058,
0.));
#157847=CARTESIAN_POINT('Ctrl Pts',(-10.3449014384453,73.7731377048058,
12.));
#157848=CARTESIAN_POINT('Ctrl Pts',(-10.3481265449342,73.7624245587789,
0.));
#157849=CARTESIAN_POINT('Ctrl Pts',(-10.3481265449342,73.7624245587789,
12.));
#157850=CARTESIAN_POINT('Ctrl Pts',(-10.3529540403092,73.7463626541854,
0.));
#157851=CARTESIAN_POINT('Ctrl Pts',(-10.3529540403092,73.7463626541854,
12.));
#157852=CARTESIAN_POINT('Ctrl Pts',(-10.359370371262,73.7249624109173,0.));
#157853=CARTESIAN_POINT('Ctrl Pts',(-10.359370371262,73.7249624109173,12.));
#157854=CARTESIAN_POINT('Ctrl Pts',(-10.3673568984582,73.6982381645206,
0.));
#157855=CARTESIAN_POINT('Ctrl Pts',(-10.3673568984582,73.6982381645206,
12.));
#157856=CARTESIAN_POINT('Ctrl Pts',(-10.3753095356342,73.6715399947839,
0.));
#157857=CARTESIAN_POINT('Ctrl Pts',(-10.3753095356342,73.6715399947839,
12.));
#157858=CARTESIAN_POINT('Ctrl Pts',(-10.3832282820371,73.6448679350696,
0.));
#157859=CARTESIAN_POINT('Ctrl Pts',(-10.3832282820371,73.6448679350696,
12.));
#157860=CARTESIAN_POINT('Ctrl Pts',(-10.3911131417463,73.6182220363156,
0.));
#157861=CARTESIAN_POINT('Ctrl Pts',(-10.3911131417463,73.6182220363156,
12.));
#157862=CARTESIAN_POINT('Ctrl Pts',(-10.3989641265285,73.5916023719713,
0.));
#157863=CARTESIAN_POINT('Ctrl Pts',(-10.3989641265285,73.5916023719713,
12.));
#157864=CARTESIAN_POINT('Ctrl Pts',(-10.406781255551,73.5650090359839,0.));
#157865=CARTESIAN_POINT('Ctrl Pts',(-10.406781255551,73.5650090359839,12.));
#157866=CARTESIAN_POINT('Ctrl Pts',(-10.414564552681,73.5384421354543,0.));
#157867=CARTESIAN_POINT('Ctrl Pts',(-10.414564552681,73.5384421354543,12.));
#157868=CARTESIAN_POINT('Ctrl Pts',(-10.4223140444605,73.5119017847575,
0.));
#157869=CARTESIAN_POINT('Ctrl Pts',(-10.4223140444605,73.5119017847575,
12.));
#157870=CARTESIAN_POINT('Ctrl Pts',(-10.430029757865,73.485388099225,0.));
#157871=CARTESIAN_POINT('Ctrl Pts',(-10.430029757865,73.485388099225,12.));
#157872=CARTESIAN_POINT('Ctrl Pts',(-10.4377117180222,73.4589011886197,
0.));
#157873=CARTESIAN_POINT('Ctrl Pts',(-10.4377117180222,73.4589011886197,
12.));
#157874=CARTESIAN_POINT('Ctrl Pts',(-10.4453599463547,73.4324411518554,
0.));
#157875=CARTESIAN_POINT('Ctrl Pts',(-10.4453599463547,73.4324411518554,
12.));
#157876=CARTESIAN_POINT('Ctrl Pts',(-10.452974461845,73.4060080806686,0.));
#157877=CARTESIAN_POINT('Ctrl Pts',(-10.452974461845,73.4060080806686,12.));
#157878=CARTESIAN_POINT('Ctrl Pts',(-10.4605552819397,73.37960206225,0.));
#157879=CARTESIAN_POINT('Ctrl Pts',(-10.4605552819397,73.37960206225,12.));
#157880=CARTESIAN_POINT('Ctrl Pts',(-10.4681024236289,73.3532231823659,
0.));
#157881=CARTESIAN_POINT('Ctrl Pts',(-10.4681024236289,73.3532231823659,
12.));
#157882=CARTESIAN_POINT('Ctrl Pts',(-10.4756159043806,73.3268715280575,
0.));
#157883=CARTESIAN_POINT('Ctrl Pts',(-10.4756159043806,73.3268715280575,
12.));
#157884=CARTESIAN_POINT('Ctrl Pts',(-10.4830957433305,73.3005471910583,
0.));
#157885=CARTESIAN_POINT('Ctrl Pts',(-10.4830957433305,73.3005471910583,
12.));
#157886=CARTESIAN_POINT('Ctrl Pts',(-10.4905419611523,73.2742502674304,
0.));
#157887=CARTESIAN_POINT('Ctrl Pts',(-10.4905419611523,73.2742502674304,
12.));
#157888=CARTESIAN_POINT('Ctrl Pts',(-10.4979545795192,73.2479808560189,
0.));
#157889=CARTESIAN_POINT('Ctrl Pts',(-10.4979545795192,73.2479808560189,
12.));
#157890=CARTESIAN_POINT('Ctrl Pts',(-10.5053336206908,73.2217390572562,
0.));
#157891=CARTESIAN_POINT('Ctrl Pts',(-10.5053336206908,73.2217390572562,
12.));
#157892=CARTESIAN_POINT('Ctrl Pts',(-10.5126791070805,73.1955249719048,
0.));
#157893=CARTESIAN_POINT('Ctrl Pts',(-10.5126791070805,73.1955249719048,
12.));
#157894=CARTESIAN_POINT('Ctrl Pts',(-10.5199910607654,73.1693386996138,
0.));
#157895=CARTESIAN_POINT('Ctrl Pts',(-10.5199910607654,73.1693386996138,
12.));
#157896=CARTESIAN_POINT('Ctrl Pts',(-10.5272695032653,73.1431803382711,
0.));
#157897=CARTESIAN_POINT('Ctrl Pts',(-10.5272695032653,73.1431803382711,
12.));
#157898=CARTESIAN_POINT('Ctrl Pts',(-10.53451445581,73.1170499848039,0.));
#157899=CARTESIAN_POINT('Ctrl Pts',(-10.53451445581,73.1170499848039,12.));
#157900=CARTESIAN_POINT('Ctrl Pts',(-10.5417259395003,73.0909477356474,
0.));
#157901=CARTESIAN_POINT('Ctrl Pts',(-10.5417259395003,73.0909477356474,
12.));
#157902=CARTESIAN_POINT('Ctrl Pts',(-10.5489039755138,73.0648736873434,
0.));
#157903=CARTESIAN_POINT('Ctrl Pts',(-10.5489039755138,73.0648736873434,
12.));
#157904=CARTESIAN_POINT('Ctrl Pts',(-10.5560485852974,73.0388279370834,
0.));
#157905=CARTESIAN_POINT('Ctrl Pts',(-10.5560485852974,73.0388279370834,
12.));
#157906=CARTESIAN_POINT('Ctrl Pts',(-10.5631597907651,73.0128105832621,
0.));
#157907=CARTESIAN_POINT('Ctrl Pts',(-10.5631597907651,73.0128105832621,
12.));
#157908=CARTESIAN_POINT('Ctrl Pts',(-10.570237614205,72.9868217252283,0.));
#157909=CARTESIAN_POINT('Ctrl Pts',(-10.570237614205,72.9868217252283,12.));
#157910=CARTESIAN_POINT('Ctrl Pts',(-10.5772820781958,72.9608614630534,
0.));
#157911=CARTESIAN_POINT('Ctrl Pts',(-10.5772820781958,72.9608614630534,
12.));
#157912=CARTESIAN_POINT('Ctrl Pts',(-10.5842932055209,72.9349298972822,
0.));
#157913=CARTESIAN_POINT('Ctrl Pts',(-10.5842932055209,72.9349298972822,
12.));
#157914=CARTESIAN_POINT('Ctrl Pts',(-10.5912710190928,72.9090271287083,
0.));
#157915=CARTESIAN_POINT('Ctrl Pts',(-10.5912710190928,72.9090271287083,
12.));
#157916=CARTESIAN_POINT('Ctrl Pts',(-10.5982155418626,72.8831532580845,
0.));
#157917=CARTESIAN_POINT('Ctrl Pts',(-10.5982155418626,72.8831532580845,
12.));
#157918=CARTESIAN_POINT('Ctrl Pts',(-10.6051267968203,72.8573083861337,
0.));
#157919=CARTESIAN_POINT('Ctrl Pts',(-10.6051267968203,72.8573083861337,
12.));
#157920=CARTESIAN_POINT('Ctrl Pts',(-10.6120048070367,72.8314926136881,
0.));
#157921=CARTESIAN_POINT('Ctrl Pts',(-10.6120048070367,72.8314926136881,
12.));
#157922=CARTESIAN_POINT('Ctrl Pts',(-10.6188495956973,72.8057060417887,
0.));
#157923=CARTESIAN_POINT('Ctrl Pts',(-10.6188495956973,72.8057060417887,
12.));
#157924=CARTESIAN_POINT('Ctrl Pts',(-10.6256611861394,72.7799487717911,
0.));
#157925=CARTESIAN_POINT('Ctrl Pts',(-10.6256611861394,72.7799487717911,
12.));
#157926=CARTESIAN_POINT('Ctrl Pts',(-10.6324396018998,72.7542209054812,
0.));
#157927=CARTESIAN_POINT('Ctrl Pts',(-10.6324396018998,72.7542209054812,
12.));
#157928=CARTESIAN_POINT('Ctrl Pts',(-10.6391848667352,72.7285225451293,
0.));
#157929=CARTESIAN_POINT('Ctrl Pts',(-10.6391848667352,72.7285225451293,
12.));
#157930=CARTESIAN_POINT('Ctrl Pts',(-10.6458970045946,72.7028537934317,
0.));
#157931=CARTESIAN_POINT('Ctrl Pts',(-10.6458970045946,72.7028537934317,
12.));
#157932=CARTESIAN_POINT('Ctrl Pts',(-10.6525760396054,72.6772147534752,
0.));
#157933=CARTESIAN_POINT('Ctrl Pts',(-10.6525760396054,72.6772147534752,
12.));
#157934=CARTESIAN_POINT('Ctrl Pts',(-10.659221996058,72.651605528691,0.));
#157935=CARTESIAN_POINT('Ctrl Pts',(-10.659221996058,72.651605528691,12.));
#157936=CARTESIAN_POINT('Ctrl Pts',(-10.6658348983944,72.6260262228065,
0.));
#157937=CARTESIAN_POINT('Ctrl Pts',(-10.6658348983944,72.6260262228065,
12.));
#157938=CARTESIAN_POINT('Ctrl Pts',(-10.6724147711995,72.6004769398019,
0.));
#157939=CARTESIAN_POINT('Ctrl Pts',(-10.6724147711995,72.6004769398019,
12.));
#157940=CARTESIAN_POINT('Ctrl Pts',(-10.6789616392042,72.5749577839415,
0.));
#157941=CARTESIAN_POINT('Ctrl Pts',(-10.6789616392042,72.5749577839415,
12.));
#157942=CARTESIAN_POINT('Ctrl Pts',(-10.6854755272904,72.5494688597961,
0.));
#157943=CARTESIAN_POINT('Ctrl Pts',(-10.6854755272904,72.5494688597961,
12.));
#157944=CARTESIAN_POINT('Ctrl Pts',(-10.691956460499,72.5240102722664,0.));
#157945=CARTESIAN_POINT('Ctrl Pts',(-10.691956460499,72.5240102722664,12.));
#157946=CARTESIAN_POINT('Ctrl Pts',(-10.6984044640398,72.4985821266023,
0.));
#157947=CARTESIAN_POINT('Ctrl Pts',(-10.6984044640398,72.4985821266023,
12.));
#157948=CARTESIAN_POINT('Ctrl Pts',(-10.7048195633061,72.4731845284227,
0.));
#157949=CARTESIAN_POINT('Ctrl Pts',(-10.7048195633061,72.4731845284227,
12.));
#157950=CARTESIAN_POINT('Ctrl Pts',(-10.7112017838706,72.4478175837156,
0.));
#157951=CARTESIAN_POINT('Ctrl Pts',(-10.7112017838706,72.4478175837156,
12.));
#157952=CARTESIAN_POINT('Ctrl Pts',(-10.7175511514788,72.4224813988347,
0.));
#157953=CARTESIAN_POINT('Ctrl Pts',(-10.7175511514788,72.4224813988347,
12.));
#157954=CARTESIAN_POINT('Ctrl Pts',(-10.7238676920469,72.3971760804933,
0.));
#157955=CARTESIAN_POINT('Ctrl Pts',(-10.7238676920469,72.3971760804933,
12.));
#157956=CARTESIAN_POINT('Ctrl Pts',(-10.7301514316607,72.3719017357571,
0.));
#157957=CARTESIAN_POINT('Ctrl Pts',(-10.7301514316607,72.3719017357571,
12.));
#157958=CARTESIAN_POINT('Ctrl Pts',(-10.73640239658,72.3466584720318,0.));
#157959=CARTESIAN_POINT('Ctrl Pts',(-10.73640239658,72.3466584720318,12.));
#157960=CARTESIAN_POINT('Ctrl Pts',(-10.7426206132375,72.3214463970641,
0.));
#157961=CARTESIAN_POINT('Ctrl Pts',(-10.7426206132375,72.3214463970641,
12.));
#157962=CARTESIAN_POINT('Ctrl Pts',(-10.7488061082368,72.2962656189556,
0.));
#157963=CARTESIAN_POINT('Ctrl Pts',(-10.7488061082368,72.2962656189556,
12.));
#157964=CARTESIAN_POINT('Ctrl Pts',(-10.7549589083535,72.2711162461681,
0.));
#157965=CARTESIAN_POINT('Ctrl Pts',(-10.7549589083535,72.2711162461681,
12.));
#157966=CARTESIAN_POINT('Ctrl Pts',(-10.7610790405385,72.2459983875296,
0.));
#157967=CARTESIAN_POINT('Ctrl Pts',(-10.7610790405385,72.2459983875296,
12.));
#157968=CARTESIAN_POINT('Ctrl Pts',(-10.7671665319255,72.2209121522366,
0.));
#157969=CARTESIAN_POINT('Ctrl Pts',(-10.7671665319255,72.2209121522366,
12.));
#157970=CARTESIAN_POINT('Ctrl Pts',(-10.7732214098344,72.1958576498558,
0.));
#157971=CARTESIAN_POINT('Ctrl Pts',(-10.7732214098344,72.1958576498558,
12.));
#157972=CARTESIAN_POINT('Ctrl Pts',(-10.7792437017662,72.1708349903305,
0.));
#157973=CARTESIAN_POINT('Ctrl Pts',(-10.7792437017662,72.1708349903305,
12.));
#157974=CARTESIAN_POINT('Ctrl Pts',(-10.7852334354016,72.1458442839834,
0.));
#157975=CARTESIAN_POINT('Ctrl Pts',(-10.7852334354016,72.1458442839834,
12.));
#157976=CARTESIAN_POINT('Ctrl Pts',(-10.7911906386027,72.1208856415171,
0.));
#157977=CARTESIAN_POINT('Ctrl Pts',(-10.7911906386027,72.1208856415171,
12.));
#157978=CARTESIAN_POINT('Ctrl Pts',(-10.7971153394166,72.0959591740114,
0.));
#157979=CARTESIAN_POINT('Ctrl Pts',(-10.7971153394166,72.0959591740114,
12.));
#157980=CARTESIAN_POINT('Ctrl Pts',(-10.8030075660808,72.0710649929202,
0.));
#157981=CARTESIAN_POINT('Ctrl Pts',(-10.8030075660808,72.0710649929202,
12.));
#157982=CARTESIAN_POINT('Ctrl Pts',(-10.8088673470184,72.0462032100815,
0.));
#157983=CARTESIAN_POINT('Ctrl Pts',(-10.8088673470184,72.0462032100815,
12.));
#157984=CARTESIAN_POINT('Ctrl Pts',(-10.8146947108375,72.0213739377223,
0.));
#157985=CARTESIAN_POINT('Ctrl Pts',(-10.8146947108375,72.0213739377223,
12.));
#157986=CARTESIAN_POINT('Ctrl Pts',(-10.8204896863328,71.9965772884619,
0.));
#157987=CARTESIAN_POINT('Ctrl Pts',(-10.8204896863328,71.9965772884619,
12.));
#157988=CARTESIAN_POINT('Ctrl Pts',(-10.8262523024898,71.9718133753127,
0.));
#157989=CARTESIAN_POINT('Ctrl Pts',(-10.8262523024898,71.9718133753127,
12.));
#157990=CARTESIAN_POINT('Ctrl Pts',(-10.8319825884918,71.9470823116785,
0.));
#157991=CARTESIAN_POINT('Ctrl Pts',(-10.8319825884918,71.9470823116785,
12.));
#157992=CARTESIAN_POINT('Ctrl Pts',(-10.8376805737159,71.9223842113625,
0.));
#157993=CARTESIAN_POINT('Ctrl Pts',(-10.8376805737159,71.9223842113625,
12.));
#157994=CARTESIAN_POINT('Ctrl Pts',(-10.8433462877311,71.8977191885725,
0.));
#157995=CARTESIAN_POINT('Ctrl Pts',(-10.8433462877311,71.8977191885725,
12.));
#157996=CARTESIAN_POINT('Ctrl Pts',(-10.8489797602997,71.8730873579224,
0.));
#157997=CARTESIAN_POINT('Ctrl Pts',(-10.8489797602997,71.8730873579224,
12.));
#157998=CARTESIAN_POINT('Ctrl Pts',(-10.8545810213799,71.8484888344339,
0.));
#157999=CARTESIAN_POINT('Ctrl Pts',(-10.8545810213799,71.8484888344339,
12.));
#158000=CARTESIAN_POINT('Ctrl Pts',(-10.8601501011332,71.8239237335331,
0.));
#158001=CARTESIAN_POINT('Ctrl Pts',(-10.8601501011332,71.8239237335331,
12.));
#158002=CARTESIAN_POINT('Ctrl Pts',(-10.865687029922,71.7993921710564,0.));
#158003=CARTESIAN_POINT('Ctrl Pts',(-10.865687029922,71.7993921710564,12.));
#158004=CARTESIAN_POINT('Ctrl Pts',(-10.8711918383073,71.7748942632593,
0.));
#158005=CARTESIAN_POINT('Ctrl Pts',(-10.8711918383073,71.7748942632593,
12.));
#158006=CARTESIAN_POINT('Ctrl Pts',(-10.8766645570497,71.7504301268181,
0.));
#158007=CARTESIAN_POINT('Ctrl Pts',(-10.8766645570497,71.7504301268181,
12.));
#158008=CARTESIAN_POINT('Ctrl Pts',(-10.8821052171121,71.7259998788328,
0.));
#158009=CARTESIAN_POINT('Ctrl Pts',(-10.8821052171121,71.7259998788328,
12.));
#158010=CARTESIAN_POINT('Ctrl Pts',(-10.8875138496671,71.7016036368236,
0.));
#158011=CARTESIAN_POINT('Ctrl Pts',(-10.8875138496671,71.7016036368236,
12.));
#158012=CARTESIAN_POINT('Ctrl Pts',(-10.8928904860964,71.6772415187364,
0.));
#158013=CARTESIAN_POINT('Ctrl Pts',(-10.8928904860964,71.6772415187364,
12.));
#158014=CARTESIAN_POINT('Ctrl Pts',(-10.8982351579871,71.6529136429504,
0.));
#158015=CARTESIAN_POINT('Ctrl Pts',(-10.8982351579871,71.6529136429504,
12.));
#158016=CARTESIAN_POINT('Ctrl Pts',(-10.9035478971328,71.6286201282812,
0.));
#158017=CARTESIAN_POINT('Ctrl Pts',(-10.9035478971328,71.6286201282812,
12.));
#158018=CARTESIAN_POINT('Ctrl Pts',(-10.9088287355365,71.6043610939835,
0.));
#158019=CARTESIAN_POINT('Ctrl Pts',(-10.9088287355365,71.6043610939835,
12.));
#158020=CARTESIAN_POINT('Ctrl Pts',(-10.914077705417,71.5801366597488,0.));
#158021=CARTESIAN_POINT('Ctrl Pts',(-10.914077705417,71.5801366597488,12.));
#158022=CARTESIAN_POINT('Ctrl Pts',(-10.91929483921,71.5559469457091,0.));
#158023=CARTESIAN_POINT('Ctrl Pts',(-10.91929483921,71.5559469457091,12.));
#158024=CARTESIAN_POINT('Ctrl Pts',(-10.9244801695642,71.5317920724459,
0.));
#158025=CARTESIAN_POINT('Ctrl Pts',(-10.9244801695642,71.5317920724459,
12.));
#158026=CARTESIAN_POINT('Ctrl Pts',(-10.9296337293424,71.5076721609937,
0.));
#158027=CARTESIAN_POINT('Ctrl Pts',(-10.9296337293424,71.5076721609937,
12.));
#158028=CARTESIAN_POINT('Ctrl Pts',(-10.9347555516235,71.4835873328423,
0.));
#158029=CARTESIAN_POINT('Ctrl Pts',(-10.9347555516235,71.4835873328423,
12.));
#158030=CARTESIAN_POINT('Ctrl Pts',(-10.9398456697095,71.4595377099351,
0.));
#158031=CARTESIAN_POINT('Ctrl Pts',(-10.9398456697095,71.4595377099351,
12.));
#158032=CARTESIAN_POINT('Ctrl Pts',(-10.944904117127,71.435523414672,0.));
#158033=CARTESIAN_POINT('Ctrl Pts',(-10.944904117127,71.435523414672,12.));
#158034=CARTESIAN_POINT('Ctrl Pts',(-10.9499309276236,71.4115445699194,
0.));
#158035=CARTESIAN_POINT('Ctrl Pts',(-10.9499309276236,71.4115445699194,
12.));
#158036=CARTESIAN_POINT('Ctrl Pts',(-10.954926135169,71.3876012990138,0.));
#158037=CARTESIAN_POINT('Ctrl Pts',(-10.954926135169,71.3876012990138,12.));
#158038=CARTESIAN_POINT('Ctrl Pts',(-10.9598897739564,71.3636937257649,
0.));
#158039=CARTESIAN_POINT('Ctrl Pts',(-10.9598897739564,71.3636937257649,
12.));
#158040=CARTESIAN_POINT('Ctrl Pts',(-10.9648218784098,71.339821974454,0.));
#158041=CARTESIAN_POINT('Ctrl Pts',(-10.9648218784098,71.339821974454,12.));
#158042=CARTESIAN_POINT('Ctrl Pts',(-10.969722483186,71.3159861698358,0.));
#158043=CARTESIAN_POINT('Ctrl Pts',(-10.969722483186,71.3159861698358,12.));
#158044=CARTESIAN_POINT('Ctrl Pts',(-10.9745916231709,71.2921864371491,
0.));
#158045=CARTESIAN_POINT('Ctrl Pts',(-10.9745916231709,71.2921864371491,
12.));
#158046=CARTESIAN_POINT('Ctrl Pts',(-10.9794293334805,71.2684229021207,
0.));
#158047=CARTESIAN_POINT('Ctrl Pts',(-10.9794293334805,71.2684229021207,
12.));
#158048=CARTESIAN_POINT('Ctrl Pts',(-10.9842356494627,71.2446956909687,
0.));
#158049=CARTESIAN_POINT('Ctrl Pts',(-10.9842356494627,71.2446956909687,
12.));
#158050=CARTESIAN_POINT('Ctrl Pts',(-10.9890106067039,71.2210049304014,
0.));
#158051=CARTESIAN_POINT('Ctrl Pts',(-10.9890106067039,71.2210049304014,
12.));
#158052=CARTESIAN_POINT('Ctrl Pts',(-10.993754241032,71.1973507476191,0.));
#158053=CARTESIAN_POINT('Ctrl Pts',(-10.993754241032,71.1973507476191,12.));
#158054=CARTESIAN_POINT('Ctrl Pts',(-10.9984665885127,71.1737332703248,
0.));
#158055=CARTESIAN_POINT('Ctrl Pts',(-10.9984665885127,71.1737332703248,
12.));
#158056=CARTESIAN_POINT('Ctrl Pts',(-11.0031476854502,71.1501526267286,
0.));
#158057=CARTESIAN_POINT('Ctrl Pts',(-11.0031476854502,71.1501526267286,
12.));
#158058=CARTESIAN_POINT('Ctrl Pts',(-11.0077975683895,71.1266089455517,
0.));
#158059=CARTESIAN_POINT('Ctrl Pts',(-11.0077975683895,71.1266089455517,
12.));
#158060=CARTESIAN_POINT('Ctrl Pts',(-11.0124162741224,71.1031023560249,
0.));
#158061=CARTESIAN_POINT('Ctrl Pts',(-11.0124162741224,71.1031023560249,
12.));
#158062=CARTESIAN_POINT('Ctrl Pts',(-11.0170038396915,71.0796329878907,
0.));
#158063=CARTESIAN_POINT('Ctrl Pts',(-11.0170038396915,71.0796329878907,
12.));
#158064=CARTESIAN_POINT('Ctrl Pts',(-11.0215603023856,71.0562009714136,
0.));
#158065=CARTESIAN_POINT('Ctrl Pts',(-11.0215603023856,71.0562009714136,
12.));
#158066=CARTESIAN_POINT('Ctrl Pts',(-11.0260856997415,71.0328064373856,
0.));
#158067=CARTESIAN_POINT('Ctrl Pts',(-11.0260856997415,71.0328064373856,
12.));
#158068=CARTESIAN_POINT('Ctrl Pts',(-11.0305800695456,71.0094495171292,
0.));
#158069=CARTESIAN_POINT('Ctrl Pts',(-11.0305800695456,71.0094495171292,
12.));
#158070=CARTESIAN_POINT('Ctrl Pts',(-11.0350434498405,70.986130342497,0.));
#158071=CARTESIAN_POINT('Ctrl Pts',(-11.0350434498405,70.986130342497,12.));
#158072=CARTESIAN_POINT('Ctrl Pts',(-11.0394758789285,70.9628490458748,
0.));
#158073=CARTESIAN_POINT('Ctrl Pts',(-11.0394758789285,70.9628490458748,
12.));
#158074=CARTESIAN_POINT('Ctrl Pts',(-11.0438773953681,70.9396057601924,
0.));
#158075=CARTESIAN_POINT('Ctrl Pts',(-11.0438773953681,70.9396057601924,
12.));
#158076=CARTESIAN_POINT('Ctrl Pts',(-11.048248037975,70.916400618927,0.));
#158077=CARTESIAN_POINT('Ctrl Pts',(-11.048248037975,70.916400618927,12.));
#158078=CARTESIAN_POINT('Ctrl Pts',(-11.0525878458243,70.8932337561087,
0.));
#158079=CARTESIAN_POINT('Ctrl Pts',(-11.0525878458243,70.8932337561087,
12.));
#158080=CARTESIAN_POINT('Ctrl Pts',(-11.0568968582569,70.8701053063186,
0.));
#158081=CARTESIAN_POINT('Ctrl Pts',(-11.0568968582569,70.8701053063186,
12.));
#158082=CARTESIAN_POINT('Ctrl Pts',(-11.0611751148835,70.8470154046919,
0.));
#158083=CARTESIAN_POINT('Ctrl Pts',(-11.0611751148835,70.8470154046919,
12.));
#158084=CARTESIAN_POINT('Ctrl Pts',(-11.0654226555802,70.8239641869299,
0.));
#158085=CARTESIAN_POINT('Ctrl Pts',(-11.0654226555802,70.8239641869299,
12.));
#158086=CARTESIAN_POINT('Ctrl Pts',(-11.0696395204909,70.8009517893057,
0.));
#158087=CARTESIAN_POINT('Ctrl Pts',(-11.0696395204909,70.8009517893057,
12.));
#158088=CARTESIAN_POINT('Ctrl Pts',(-11.073825750029,70.7779783486677,0.));
#158089=CARTESIAN_POINT('Ctrl Pts',(-11.073825750029,70.7779783486677,12.));
#158090=CARTESIAN_POINT('Ctrl Pts',(-11.0779813848846,70.7550440024384,
0.));
#158091=CARTESIAN_POINT('Ctrl Pts',(-11.0779813848846,70.7550440024384,
12.));
#158092=CARTESIAN_POINT('Ctrl Pts',(-11.0821064660269,70.732148888618,0.));
#158093=CARTESIAN_POINT('Ctrl Pts',(-11.0821064660269,70.732148888618,12.));
#158094=CARTESIAN_POINT('Ctrl Pts',(-11.0862010347016,70.7092931457954,
0.));
#158095=CARTESIAN_POINT('Ctrl Pts',(-11.0862010347016,70.7092931457954,
12.));
#158096=CARTESIAN_POINT('Ctrl Pts',(-11.0902651324323,70.6864769131546,
0.));
#158097=CARTESIAN_POINT('Ctrl Pts',(-11.0902651324323,70.6864769131546,
12.));
#158098=CARTESIAN_POINT('Ctrl Pts',(-11.0942988010233,70.6637003304785,
0.));
#158099=CARTESIAN_POINT('Ctrl Pts',(-11.0942988010233,70.6637003304785,
12.));
#158100=CARTESIAN_POINT('Ctrl Pts',(-11.0983020825667,70.6409635381482,
0.));
#158101=CARTESIAN_POINT('Ctrl Pts',(-11.0983020825667,70.6409635381482,
12.));
#158102=CARTESIAN_POINT('Ctrl Pts',(-11.1022750194446,70.6182666771481,
0.));
#158103=CARTESIAN_POINT('Ctrl Pts',(-11.1022750194446,70.6182666771481,
12.));
#158104=CARTESIAN_POINT('Ctrl Pts',(-11.1062176543262,70.5956098890773,
0.));
#158105=CARTESIAN_POINT('Ctrl Pts',(-11.1062176543262,70.5956098890773,
12.));
#158106=CARTESIAN_POINT('Ctrl Pts',(-11.1101300301701,70.5729933161546,
0.));
#158107=CARTESIAN_POINT('Ctrl Pts',(-11.1101300301701,70.5729933161546,
12.));
#158108=CARTESIAN_POINT('Ctrl Pts',(-11.1140121902271,70.5504171012233,
0.));
#158109=CARTESIAN_POINT('Ctrl Pts',(-11.1140121902271,70.5504171012233,
12.));
#158110=CARTESIAN_POINT('Ctrl Pts',(-11.1178641780476,70.5278813877494,
0.));
#158111=CARTESIAN_POINT('Ctrl Pts',(-11.1178641780476,70.5278813877494,
12.));
#158112=CARTESIAN_POINT('Ctrl Pts',(-11.1216860374826,70.505386319828,0.));
#158113=CARTESIAN_POINT('Ctrl Pts',(-11.1216860374826,70.505386319828,12.));
#158114=CARTESIAN_POINT('Ctrl Pts',(-11.1254778126821,70.4829320421957,
0.));
#158115=CARTESIAN_POINT('Ctrl Pts',(-11.1254778126821,70.4829320421957,
12.));
#158116=CARTESIAN_POINT('Ctrl Pts',(-11.1292395480974,70.4605187002354,
0.));
#158117=CARTESIAN_POINT('Ctrl Pts',(-11.1292395480974,70.4605187002354,
12.));
#158118=CARTESIAN_POINT('Ctrl Pts',(-11.1329712884846,70.4381464399819,
0.));
#158119=CARTESIAN_POINT('Ctrl Pts',(-11.1329712884846,70.4381464399819,
12.));
#158120=CARTESIAN_POINT('Ctrl Pts',(-11.1366730789126,70.4158154081205,
0.));
#158121=CARTESIAN_POINT('Ctrl Pts',(-11.1366730789126,70.4158154081205,
12.));
#158122=CARTESIAN_POINT('Ctrl Pts',(-11.1403449647625,70.393525751996,0.));
#158123=CARTESIAN_POINT('Ctrl Pts',(-11.1403449647625,70.393525751996,12.));
#158124=CARTESIAN_POINT('Ctrl Pts',(-11.143986991727,70.3712776196223,0.));
#158125=CARTESIAN_POINT('Ctrl Pts',(-11.143986991727,70.3712776196223,12.));
#158126=CARTESIAN_POINT('Ctrl Pts',(-11.1475992058124,70.349071159688,0.));
#158127=CARTESIAN_POINT('Ctrl Pts',(-11.1475992058124,70.349071159688,12.));
#158128=CARTESIAN_POINT('Ctrl Pts',(-11.1511816533421,70.326906521559,0.));
#158129=CARTESIAN_POINT('Ctrl Pts',(-11.1511816533421,70.326906521559,12.));
#158130=CARTESIAN_POINT('Ctrl Pts',(-11.1547343809646,70.3047838552756,
0.));
#158131=CARTESIAN_POINT('Ctrl Pts',(-11.1547343809646,70.3047838552756,
12.));
#158132=CARTESIAN_POINT('Ctrl Pts',(-11.1582574356521,70.2827033115662,
0.));
#158133=CARTESIAN_POINT('Ctrl Pts',(-11.1582574356521,70.2827033115662,
12.));
#158134=CARTESIAN_POINT('Ctrl Pts',(-11.1617508647016,70.2606650418589,
0.));
#158135=CARTESIAN_POINT('Ctrl Pts',(-11.1617508647016,70.2606650418589,
12.));
#158136=CARTESIAN_POINT('Ctrl Pts',(-11.1652147157383,70.2386691982902,
0.));
#158137=CARTESIAN_POINT('Ctrl Pts',(-11.1652147157383,70.2386691982902,
12.));
#158138=CARTESIAN_POINT('Ctrl Pts',(-11.168649036721,70.2167159337094,0.));
#158139=CARTESIAN_POINT('Ctrl Pts',(-11.168649036721,70.2167159337094,12.));
#158140=CARTESIAN_POINT('Ctrl Pts',(-11.1720538759499,70.1948054016816,
0.));
#158141=CARTESIAN_POINT('Ctrl Pts',(-11.1720538759499,70.1948054016816,
12.));
#158142=CARTESIAN_POINT('Ctrl Pts',(-11.1754292820631,70.1729377564954,
0.));
#158143=CARTESIAN_POINT('Ctrl Pts',(-11.1754292820631,70.1729377564954,
12.));
#158144=CARTESIAN_POINT('Ctrl Pts',(-11.1787753040363,70.1511131531672,
0.));
#158145=CARTESIAN_POINT('Ctrl Pts',(-11.1787753040363,70.1511131531672,
12.));
#158146=CARTESIAN_POINT('Ctrl Pts',(-11.1820919911846,70.1293317474432,
0.));
#158147=CARTESIAN_POINT('Ctrl Pts',(-11.1820919911846,70.1293317474432,
12.));
#158148=CARTESIAN_POINT('Ctrl Pts',(-11.185379393167,70.1075936957973,0.));
#158149=CARTESIAN_POINT('Ctrl Pts',(-11.185379393167,70.1075936957973,12.));
#158150=CARTESIAN_POINT('Ctrl Pts',(-11.1886375599916,70.0858991554295,
0.));
#158151=CARTESIAN_POINT('Ctrl Pts',(-11.1886375599916,70.0858991554295,
12.));
#158152=CARTESIAN_POINT('Ctrl Pts',(-11.1918665420168,70.0642482842942,
0.));
#158153=CARTESIAN_POINT('Ctrl Pts',(-11.1918665420168,70.0642482842942,
12.));
#158154=CARTESIAN_POINT('Ctrl Pts',(-11.1950663899578,70.0426412411194,
0.));
#158155=CARTESIAN_POINT('Ctrl Pts',(-11.1950663899578,70.0426412411194,
12.));
#158156=CARTESIAN_POINT('Ctrl Pts',(-11.1982371548918,70.0210781854236,
0.));
#158157=CARTESIAN_POINT('Ctrl Pts',(-11.1982371548918,70.0210781854236,
12.));
#158158=CARTESIAN_POINT('Ctrl Pts',(-11.2013788882711,69.9995592775322,
0.));
#158159=CARTESIAN_POINT('Ctrl Pts',(-11.2013788882711,69.9995592775322,
12.));
#158160=CARTESIAN_POINT('Ctrl Pts',(-11.2044916419239,69.9780846785771,
0.));
#158161=CARTESIAN_POINT('Ctrl Pts',(-11.2044916419239,69.9780846785771,
12.));
#158162=CARTESIAN_POINT('Ctrl Pts',(-11.2075754680445,69.9566545504813,
0.));
#158163=CARTESIAN_POINT('Ctrl Pts',(-11.2075754680445,69.9566545504813,
12.));
#158164=CARTESIAN_POINT('Ctrl Pts',(-11.2106304191881,69.9352690559399,
0.));
#158165=CARTESIAN_POINT('Ctrl Pts',(-11.2106304191881,69.9352690559399,
12.));
#158166=CARTESIAN_POINT('Ctrl Pts',(-11.2136565482679,69.9139283584036,
0.));
#158167=CARTESIAN_POINT('Ctrl Pts',(-11.2136565482679,69.9139283584036,
12.));
#158168=CARTESIAN_POINT('Ctrl Pts',(-11.2166539085527,69.8926326220414,
0.));
#158169=CARTESIAN_POINT('Ctrl Pts',(-11.2166539085527,69.8926326220414,
12.));
#158170=CARTESIAN_POINT('Ctrl Pts',(-11.2196225536794,69.8713820117918,
0.));
#158171=CARTESIAN_POINT('Ctrl Pts',(-11.2196225536794,69.8713820117918,
12.));
#158172=CARTESIAN_POINT('Ctrl Pts',(-11.2225625376739,69.8501766934445,
0.));
#158173=CARTESIAN_POINT('Ctrl Pts',(-11.2225625376739,69.8501766934445,
12.));
#158174=CARTESIAN_POINT('Ctrl Pts',(-11.225473914972,69.8290168337076,0.));
#158175=CARTESIAN_POINT('Ctrl Pts',(-11.225473914972,69.8290168337076,12.));
#158176=CARTESIAN_POINT('Ctrl Pts',(-11.2283567404434,69.8079026002753,
0.));
#158177=CARTESIAN_POINT('Ctrl Pts',(-11.2283567404434,69.8079026002753,
12.));
#158178=CARTESIAN_POINT('Ctrl Pts',(-11.2312110694183,69.7868341618927,
0.));
#158179=CARTESIAN_POINT('Ctrl Pts',(-11.2312110694183,69.7868341618927,
12.));
#158180=CARTESIAN_POINT('Ctrl Pts',(-11.2340369576452,69.7658116882298,
0.));
#158181=CARTESIAN_POINT('Ctrl Pts',(-11.2340369576452,69.7658116882298,
12.));
#158182=CARTESIAN_POINT('Ctrl Pts',(-11.236834461247,69.7448353497394,0.));
#158183=CARTESIAN_POINT('Ctrl Pts',(-11.236834461247,69.7448353497394,12.));
#158184=CARTESIAN_POINT('Ctrl Pts',(-11.2396036366861,69.7239053175362,
0.));
#158185=CARTESIAN_POINT('Ctrl Pts',(-11.2396036366861,69.7239053175362,
12.));
#158186=CARTESIAN_POINT('Ctrl Pts',(-11.242344540717,69.7030217632187,0.));
#158187=CARTESIAN_POINT('Ctrl Pts',(-11.242344540717,69.7030217632187,12.));
#158188=CARTESIAN_POINT('Ctrl Pts',(-11.2450572303847,69.6821848588492,
0.));
#158189=CARTESIAN_POINT('Ctrl Pts',(-11.2450572303847,69.6821848588492,
12.));
#158190=CARTESIAN_POINT('Ctrl Pts',(-11.2477417631391,69.6613947773563,
0.));
#158191=CARTESIAN_POINT('Ctrl Pts',(-11.2477417631391,69.6613947773563,
12.));
#158192=CARTESIAN_POINT('Ctrl Pts',(-11.2503981969413,69.6406516928902,
0.));
#158193=CARTESIAN_POINT('Ctrl Pts',(-11.2503981969413,69.6406516928902,
12.));
#158194=CARTESIAN_POINT('Ctrl Pts',(-11.2530265903555,69.6199557811231,
0.));
#158195=CARTESIAN_POINT('Ctrl Pts',(-11.2530265903555,69.6199557811231,
12.));
#158196=CARTESIAN_POINT('Ctrl Pts',(-11.255627002701,69.5993072197355,0.));
#158197=CARTESIAN_POINT('Ctrl Pts',(-11.255627002701,69.5993072197355,12.));
#158198=CARTESIAN_POINT('Ctrl Pts',(-11.2581994939534,69.5787061880815,
0.));
#158199=CARTESIAN_POINT('Ctrl Pts',(-11.2581994939534,69.5787061880815,
12.));
#158200=CARTESIAN_POINT('Ctrl Pts',(-11.2607441244698,69.5581528662846,
0.));
#158201=CARTESIAN_POINT('Ctrl Pts',(-11.2607441244698,69.5581528662846,
12.));
#158202=CARTESIAN_POINT('Ctrl Pts',(-11.2632609547629,69.5376474344768,
0.));
#158203=CARTESIAN_POINT('Ctrl Pts',(-11.2632609547629,69.5376474344768,
12.));
#158204=CARTESIAN_POINT('Ctrl Pts',(-11.2657500452721,69.5171900720188,
0.));
#158205=CARTESIAN_POINT('Ctrl Pts',(-11.2657500452721,69.5171900720188,
12.));
#158206=CARTESIAN_POINT('Ctrl Pts',(-11.2682114561015,69.4967809565978,
0.));
#158207=CARTESIAN_POINT('Ctrl Pts',(-11.2682114561015,69.4967809565978,
12.));
#158208=CARTESIAN_POINT('Ctrl Pts',(-11.2706452475287,69.4764202659443,
0.));
#158209=CARTESIAN_POINT('Ctrl Pts',(-11.2706452475287,69.4764202659443,
12.));
#158210=CARTESIAN_POINT('Ctrl Pts',(-11.2730514806143,69.4561081798815,
0.));
#158211=CARTESIAN_POINT('Ctrl Pts',(-11.2730514806143,69.4561081798815,
12.));
#158212=CARTESIAN_POINT('Ctrl Pts',(-11.2754302177019,69.4358448819957,
0.));
#158213=CARTESIAN_POINT('Ctrl Pts',(-11.2754302177019,69.4358448819957,
12.));
#158214=CARTESIAN_POINT('Ctrl Pts',(-11.2777815231462,69.4156305620554,
0.));
#158215=CARTESIAN_POINT('Ctrl Pts',(-11.2777815231462,69.4156305620554,
12.));
#158216=CARTESIAN_POINT('Ctrl Pts',(-11.2801054633807,69.395465416223,0.));
#158217=CARTESIAN_POINT('Ctrl Pts',(-11.2801054633807,69.395465416223,12.));
#158218=CARTESIAN_POINT('Ctrl Pts',(-11.2824021054038,69.375349642,0.));
#158219=CARTESIAN_POINT('Ctrl Pts',(-11.2824021054038,69.375349642,12.));
#158220=CARTESIAN_POINT('Ctrl Pts',(-11.2846715154521,69.3552834337771,
0.));
#158221=CARTESIAN_POINT('Ctrl Pts',(-11.2846715154521,69.3552834337771,
12.));
#158222=CARTESIAN_POINT('Ctrl Pts',(-11.2869137578463,69.3352669789611,
0.));
#158223=CARTESIAN_POINT('Ctrl Pts',(-11.2869137578463,69.3352669789611,
12.));
#158224=CARTESIAN_POINT('Ctrl Pts',(-11.2891288931528,69.315300451784,0.));
#158225=CARTESIAN_POINT('Ctrl Pts',(-11.2891288931528,69.315300451784,12.));
#158226=CARTESIAN_POINT('Ctrl Pts',(-11.2913169799642,69.2953840192792,
0.));
#158227=CARTESIAN_POINT('Ctrl Pts',(-11.2913169799642,69.2953840192792,
12.));
#158228=CARTESIAN_POINT('Ctrl Pts',(-11.2934780784361,69.2755178531534,
0.));
#158229=CARTESIAN_POINT('Ctrl Pts',(-11.2934780784361,69.2755178531534,
12.));
#158230=CARTESIAN_POINT('Ctrl Pts',(-11.2956122531375,69.255702139335,0.));
#158231=CARTESIAN_POINT('Ctrl Pts',(-11.2956122531375,69.255702139335,12.));
#158232=CARTESIAN_POINT('Ctrl Pts',(-11.2977195764836,69.2359370894828,
0.));
#158233=CARTESIAN_POINT('Ctrl Pts',(-11.2977195764836,69.2359370894828,
12.));
#158234=CARTESIAN_POINT('Ctrl Pts',(-11.2998001310934,69.216222948839,0.));
#158235=CARTESIAN_POINT('Ctrl Pts',(-11.2998001310934,69.216222948839,12.));
#158236=CARTESIAN_POINT('Ctrl Pts',(-11.3018540025605,69.1965599718761,
0.));
#158237=CARTESIAN_POINT('Ctrl Pts',(-11.3018540025605,69.1965599718761,
12.));
#158238=CARTESIAN_POINT('Ctrl Pts',(-11.3038812726275,69.1769483991639,
0.));
#158239=CARTESIAN_POINT('Ctrl Pts',(-11.3038812726275,69.1769483991639,
12.));
#158240=CARTESIAN_POINT('Ctrl Pts',(-11.3058820128323,69.1573884361076,
0.));
#158241=CARTESIAN_POINT('Ctrl Pts',(-11.3058820128323,69.1573884361076,
12.));
#158242=CARTESIAN_POINT('Ctrl Pts',(-11.3078562764442,69.137880225198,0.));
#158243=CARTESIAN_POINT('Ctrl Pts',(-11.3078562764442,69.137880225198,12.));
#158244=CARTESIAN_POINT('Ctrl Pts',(-11.3098040973799,69.1184238445065,
0.));
#158245=CARTESIAN_POINT('Ctrl Pts',(-11.3098040973799,69.1184238445065,
12.));
#158246=CARTESIAN_POINT('Ctrl Pts',(-11.3113412156742,69.1029002322497,
0.));
#158247=CARTESIAN_POINT('Ctrl Pts',(-11.3113412156742,69.1029002322497,
12.));
#158248=CARTESIAN_POINT('Ctrl Pts',(-11.3124821678849,69.0912808657051,
0.));
#158249=CARTESIAN_POINT('Ctrl Pts',(-11.3124821678849,69.0912808657051,
12.));
#158250=CARTESIAN_POINT('Ctrl Pts',(-11.3132375200184,69.0835449954486,
0.));
#158251=CARTESIAN_POINT('Ctrl Pts',(-11.3132375200184,69.0835449954486,
12.));
#158252=CARTESIAN_POINT('Ctrl Pts',(-11.3136138754165,69.079679653846,0.));
#158253=CARTESIAN_POINT('Ctrl Pts',(-11.3136138754165,69.079679653846,12.));
#158254=CARTESIAN_POINT('',(-11.3136138754165,69.079679653846,12.));
#158255=CARTESIAN_POINT('Ctrl Pts',(-11.3136138754165,69.079679653846,12.));
#158256=CARTESIAN_POINT('Ctrl Pts',(-11.3132375200184,69.0835449954486,
12.));
#158257=CARTESIAN_POINT('Ctrl Pts',(-11.3124821678849,69.0912808657051,
12.));
#158258=CARTESIAN_POINT('Ctrl Pts',(-11.3113412156742,69.1029002322497,
12.));
#158259=CARTESIAN_POINT('Ctrl Pts',(-11.3098040973799,69.1184238445065,
12.));
#158260=CARTESIAN_POINT('Ctrl Pts',(-11.3078562764442,69.137880225198,12.));
#158261=CARTESIAN_POINT('Ctrl Pts',(-11.3058820128323,69.1573884361076,
12.));
#158262=CARTESIAN_POINT('Ctrl Pts',(-11.3038812726275,69.1769483991639,
12.));
#158263=CARTESIAN_POINT('Ctrl Pts',(-11.3018540025605,69.1965599718761,
12.));
#158264=CARTESIAN_POINT('Ctrl Pts',(-11.2998001310934,69.216222948839,12.));
#158265=CARTESIAN_POINT('Ctrl Pts',(-11.2977195764836,69.2359370894828,
12.));
#158266=CARTESIAN_POINT('Ctrl Pts',(-11.2956122531375,69.255702139335,12.));
#158267=CARTESIAN_POINT('Ctrl Pts',(-11.2934780784361,69.2755178531534,
12.));
#158268=CARTESIAN_POINT('Ctrl Pts',(-11.2913169799642,69.2953840192792,
12.));
#158269=CARTESIAN_POINT('Ctrl Pts',(-11.2891288931528,69.315300451784,12.));
#158270=CARTESIAN_POINT('Ctrl Pts',(-11.2869137578463,69.3352669789611,
12.));
#158271=CARTESIAN_POINT('Ctrl Pts',(-11.2846715154521,69.3552834337771,
12.));
#158272=CARTESIAN_POINT('Ctrl Pts',(-11.2824021054038,69.375349642,12.));
#158273=CARTESIAN_POINT('Ctrl Pts',(-11.2801054633807,69.395465416223,12.));
#158274=CARTESIAN_POINT('Ctrl Pts',(-11.2777815231462,69.4156305620554,
12.));
#158275=CARTESIAN_POINT('Ctrl Pts',(-11.2754302177019,69.4358448819957,
12.));
#158276=CARTESIAN_POINT('Ctrl Pts',(-11.2730514806143,69.4561081798815,
12.));
#158277=CARTESIAN_POINT('Ctrl Pts',(-11.2706452475287,69.4764202659443,
12.));
#158278=CARTESIAN_POINT('Ctrl Pts',(-11.2682114561015,69.4967809565978,
12.));
#158279=CARTESIAN_POINT('Ctrl Pts',(-11.2657500452721,69.5171900720188,
12.));
#158280=CARTESIAN_POINT('Ctrl Pts',(-11.2632609547629,69.5376474344768,
12.));
#158281=CARTESIAN_POINT('Ctrl Pts',(-11.2607441244698,69.5581528662846,
12.));
#158282=CARTESIAN_POINT('Ctrl Pts',(-11.2581994939534,69.5787061880815,
12.));
#158283=CARTESIAN_POINT('Ctrl Pts',(-11.255627002701,69.5993072197355,12.));
#158284=CARTESIAN_POINT('Ctrl Pts',(-11.2530265903555,69.6199557811231,
12.));
#158285=CARTESIAN_POINT('Ctrl Pts',(-11.2503981969413,69.6406516928902,
12.));
#158286=CARTESIAN_POINT('Ctrl Pts',(-11.2477417631391,69.6613947773563,
12.));
#158287=CARTESIAN_POINT('Ctrl Pts',(-11.2450572303847,69.6821848588492,
12.));
#158288=CARTESIAN_POINT('Ctrl Pts',(-11.242344540717,69.7030217632187,12.));
#158289=CARTESIAN_POINT('Ctrl Pts',(-11.2396036366861,69.7239053175362,
12.));
#158290=CARTESIAN_POINT('Ctrl Pts',(-11.236834461247,69.7448353497394,12.));
#158291=CARTESIAN_POINT('Ctrl Pts',(-11.2340369576452,69.7658116882298,
12.));
#158292=CARTESIAN_POINT('Ctrl Pts',(-11.2312110694183,69.7868341618927,
12.));
#158293=CARTESIAN_POINT('Ctrl Pts',(-11.2283567404434,69.8079026002753,
12.));
#158294=CARTESIAN_POINT('Ctrl Pts',(-11.225473914972,69.8290168337076,12.));
#158295=CARTESIAN_POINT('Ctrl Pts',(-11.2225625376739,69.8501766934445,
12.));
#158296=CARTESIAN_POINT('Ctrl Pts',(-11.2196225536794,69.8713820117918,
12.));
#158297=CARTESIAN_POINT('Ctrl Pts',(-11.2166539085527,69.8926326220414,
12.));
#158298=CARTESIAN_POINT('Ctrl Pts',(-11.2136565482679,69.9139283584036,
12.));
#158299=CARTESIAN_POINT('Ctrl Pts',(-11.2106304191881,69.9352690559399,
12.));
#158300=CARTESIAN_POINT('Ctrl Pts',(-11.2075754680445,69.9566545504813,
12.));
#158301=CARTESIAN_POINT('Ctrl Pts',(-11.2044916419239,69.9780846785771,
12.));
#158302=CARTESIAN_POINT('Ctrl Pts',(-11.2013788882711,69.9995592775322,
12.));
#158303=CARTESIAN_POINT('Ctrl Pts',(-11.1982371548918,70.0210781854236,
12.));
#158304=CARTESIAN_POINT('Ctrl Pts',(-11.1950663899578,70.0426412411194,
12.));
#158305=CARTESIAN_POINT('Ctrl Pts',(-11.1918665420168,70.0642482842942,
12.));
#158306=CARTESIAN_POINT('Ctrl Pts',(-11.1886375599916,70.0858991554295,
12.));
#158307=CARTESIAN_POINT('Ctrl Pts',(-11.185379393167,70.1075936957973,12.));
#158308=CARTESIAN_POINT('Ctrl Pts',(-11.1820919911846,70.1293317474432,
12.));
#158309=CARTESIAN_POINT('Ctrl Pts',(-11.1787753040363,70.1511131531672,
12.));
#158310=CARTESIAN_POINT('Ctrl Pts',(-11.1754292820631,70.1729377564954,
12.));
#158311=CARTESIAN_POINT('Ctrl Pts',(-11.1720538759499,70.1948054016816,
12.));
#158312=CARTESIAN_POINT('Ctrl Pts',(-11.168649036721,70.2167159337094,12.));
#158313=CARTESIAN_POINT('Ctrl Pts',(-11.1652147157383,70.2386691982902,
12.));
#158314=CARTESIAN_POINT('Ctrl Pts',(-11.1617508647016,70.2606650418589,
12.));
#158315=CARTESIAN_POINT('Ctrl Pts',(-11.1582574356521,70.2827033115662,
12.));
#158316=CARTESIAN_POINT('Ctrl Pts',(-11.1547343809646,70.3047838552756,
12.));
#158317=CARTESIAN_POINT('Ctrl Pts',(-11.1511816533421,70.326906521559,12.));
#158318=CARTESIAN_POINT('Ctrl Pts',(-11.1475992058124,70.349071159688,12.));
#158319=CARTESIAN_POINT('Ctrl Pts',(-11.143986991727,70.3712776196223,12.));
#158320=CARTESIAN_POINT('Ctrl Pts',(-11.1403449647625,70.393525751996,12.));
#158321=CARTESIAN_POINT('Ctrl Pts',(-11.1366730789126,70.4158154081205,
12.));
#158322=CARTESIAN_POINT('Ctrl Pts',(-11.1329712884846,70.4381464399819,
12.));
#158323=CARTESIAN_POINT('Ctrl Pts',(-11.1292395480974,70.4605187002354,
12.));
#158324=CARTESIAN_POINT('Ctrl Pts',(-11.1254778126821,70.4829320421957,
12.));
#158325=CARTESIAN_POINT('Ctrl Pts',(-11.1216860374826,70.505386319828,12.));
#158326=CARTESIAN_POINT('Ctrl Pts',(-11.1178641780476,70.5278813877494,
12.));
#158327=CARTESIAN_POINT('Ctrl Pts',(-11.1140121902271,70.5504171012233,
12.));
#158328=CARTESIAN_POINT('Ctrl Pts',(-11.1101300301701,70.5729933161546,
12.));
#158329=CARTESIAN_POINT('Ctrl Pts',(-11.1062176543262,70.5956098890773,
12.));
#158330=CARTESIAN_POINT('Ctrl Pts',(-11.1022750194446,70.6182666771481,
12.));
#158331=CARTESIAN_POINT('Ctrl Pts',(-11.0983020825667,70.6409635381482,
12.));
#158332=CARTESIAN_POINT('Ctrl Pts',(-11.0942988010233,70.6637003304785,
12.));
#158333=CARTESIAN_POINT('Ctrl Pts',(-11.0902651324323,70.6864769131546,
12.));
#158334=CARTESIAN_POINT('Ctrl Pts',(-11.0862010347016,70.7092931457954,
12.));
#158335=CARTESIAN_POINT('Ctrl Pts',(-11.0821064660269,70.732148888618,12.));
#158336=CARTESIAN_POINT('Ctrl Pts',(-11.0779813848846,70.7550440024384,
12.));
#158337=CARTESIAN_POINT('Ctrl Pts',(-11.073825750029,70.7779783486677,12.));
#158338=CARTESIAN_POINT('Ctrl Pts',(-11.0696395204909,70.8009517893057,
12.));
#158339=CARTESIAN_POINT('Ctrl Pts',(-11.0654226555802,70.8239641869299,
12.));
#158340=CARTESIAN_POINT('Ctrl Pts',(-11.0611751148835,70.8470154046919,
12.));
#158341=CARTESIAN_POINT('Ctrl Pts',(-11.0568968582569,70.8701053063186,
12.));
#158342=CARTESIAN_POINT('Ctrl Pts',(-11.0525878458243,70.8932337561087,
12.));
#158343=CARTESIAN_POINT('Ctrl Pts',(-11.048248037975,70.916400618927,12.));
#158344=CARTESIAN_POINT('Ctrl Pts',(-11.0438773953681,70.9396057601924,
12.));
#158345=CARTESIAN_POINT('Ctrl Pts',(-11.0394758789285,70.9628490458748,
12.));
#158346=CARTESIAN_POINT('Ctrl Pts',(-11.0350434498405,70.986130342497,12.));
#158347=CARTESIAN_POINT('Ctrl Pts',(-11.0305800695456,71.0094495171292,
12.));
#158348=CARTESIAN_POINT('Ctrl Pts',(-11.0260856997415,71.0328064373856,
12.));
#158349=CARTESIAN_POINT('Ctrl Pts',(-11.0215603023856,71.0562009714136,
12.));
#158350=CARTESIAN_POINT('Ctrl Pts',(-11.0170038396915,71.0796329878907,
12.));
#158351=CARTESIAN_POINT('Ctrl Pts',(-11.0124162741224,71.1031023560249,
12.));
#158352=CARTESIAN_POINT('Ctrl Pts',(-11.0077975683895,71.1266089455517,
12.));
#158353=CARTESIAN_POINT('Ctrl Pts',(-11.0031476854502,71.1501526267286,
12.));
#158354=CARTESIAN_POINT('Ctrl Pts',(-10.9984665885127,71.1737332703248,
12.));
#158355=CARTESIAN_POINT('Ctrl Pts',(-10.993754241032,71.1973507476191,12.));
#158356=CARTESIAN_POINT('Ctrl Pts',(-10.9890106067039,71.2210049304014,
12.));
#158357=CARTESIAN_POINT('Ctrl Pts',(-10.9842356494627,71.2446956909687,
12.));
#158358=CARTESIAN_POINT('Ctrl Pts',(-10.9794293334805,71.2684229021207,
12.));
#158359=CARTESIAN_POINT('Ctrl Pts',(-10.9745916231709,71.2921864371491,
12.));
#158360=CARTESIAN_POINT('Ctrl Pts',(-10.969722483186,71.3159861698358,12.));
#158361=CARTESIAN_POINT('Ctrl Pts',(-10.9648218784098,71.339821974454,12.));
#158362=CARTESIAN_POINT('Ctrl Pts',(-10.9598897739564,71.3636937257649,
12.));
#158363=CARTESIAN_POINT('Ctrl Pts',(-10.954926135169,71.3876012990138,12.));
#158364=CARTESIAN_POINT('Ctrl Pts',(-10.9499309276236,71.4115445699194,
12.));
#158365=CARTESIAN_POINT('Ctrl Pts',(-10.944904117127,71.435523414672,12.));
#158366=CARTESIAN_POINT('Ctrl Pts',(-10.9398456697095,71.4595377099351,
12.));
#158367=CARTESIAN_POINT('Ctrl Pts',(-10.9347555516235,71.4835873328423,
12.));
#158368=CARTESIAN_POINT('Ctrl Pts',(-10.9296337293424,71.5076721609937,
12.));
#158369=CARTESIAN_POINT('Ctrl Pts',(-10.9244801695642,71.5317920724459,
12.));
#158370=CARTESIAN_POINT('Ctrl Pts',(-10.91929483921,71.5559469457091,12.));
#158371=CARTESIAN_POINT('Ctrl Pts',(-10.914077705417,71.5801366597488,12.));
#158372=CARTESIAN_POINT('Ctrl Pts',(-10.9088287355365,71.6043610939835,
12.));
#158373=CARTESIAN_POINT('Ctrl Pts',(-10.9035478971328,71.6286201282812,
12.));
#158374=CARTESIAN_POINT('Ctrl Pts',(-10.8982351579871,71.6529136429504,
12.));
#158375=CARTESIAN_POINT('Ctrl Pts',(-10.8928904860964,71.6772415187364,
12.));
#158376=CARTESIAN_POINT('Ctrl Pts',(-10.8875138496671,71.7016036368236,
12.));
#158377=CARTESIAN_POINT('Ctrl Pts',(-10.8821052171121,71.7259998788328,
12.));
#158378=CARTESIAN_POINT('Ctrl Pts',(-10.8766645570497,71.7504301268181,
12.));
#158379=CARTESIAN_POINT('Ctrl Pts',(-10.8711918383073,71.7748942632593,
12.));
#158380=CARTESIAN_POINT('Ctrl Pts',(-10.865687029922,71.7993921710564,12.));
#158381=CARTESIAN_POINT('Ctrl Pts',(-10.8601501011332,71.8239237335331,
12.));
#158382=CARTESIAN_POINT('Ctrl Pts',(-10.8545810213799,71.8484888344339,
12.));
#158383=CARTESIAN_POINT('Ctrl Pts',(-10.8489797602997,71.8730873579224,
12.));
#158384=CARTESIAN_POINT('Ctrl Pts',(-10.8433462877311,71.8977191885725,
12.));
#158385=CARTESIAN_POINT('Ctrl Pts',(-10.8376805737159,71.9223842113625,
12.));
#158386=CARTESIAN_POINT('Ctrl Pts',(-10.8319825884918,71.9470823116785,
12.));
#158387=CARTESIAN_POINT('Ctrl Pts',(-10.8262523024898,71.9718133753127,
12.));
#158388=CARTESIAN_POINT('Ctrl Pts',(-10.8204896863328,71.9965772884619,
12.));
#158389=CARTESIAN_POINT('Ctrl Pts',(-10.8146947108375,72.0213739377223,
12.));
#158390=CARTESIAN_POINT('Ctrl Pts',(-10.8088673470184,72.0462032100815,
12.));
#158391=CARTESIAN_POINT('Ctrl Pts',(-10.8030075660808,72.0710649929202,
12.));
#158392=CARTESIAN_POINT('Ctrl Pts',(-10.7971153394166,72.0959591740114,
12.));
#158393=CARTESIAN_POINT('Ctrl Pts',(-10.7911906386027,72.1208856415171,
12.));
#158394=CARTESIAN_POINT('Ctrl Pts',(-10.7852334354016,72.1458442839834,
12.));
#158395=CARTESIAN_POINT('Ctrl Pts',(-10.7792437017662,72.1708349903305,
12.));
#158396=CARTESIAN_POINT('Ctrl Pts',(-10.7732214098344,72.1958576498558,
12.));
#158397=CARTESIAN_POINT('Ctrl Pts',(-10.7671665319255,72.2209121522366,
12.));
#158398=CARTESIAN_POINT('Ctrl Pts',(-10.7610790405385,72.2459983875296,
12.));
#158399=CARTESIAN_POINT('Ctrl Pts',(-10.7549589083535,72.2711162461681,
12.));
#158400=CARTESIAN_POINT('Ctrl Pts',(-10.7488061082368,72.2962656189556,
12.));
#158401=CARTESIAN_POINT('Ctrl Pts',(-10.7426206132375,72.3214463970641,
12.));
#158402=CARTESIAN_POINT('Ctrl Pts',(-10.73640239658,72.3466584720318,12.));
#158403=CARTESIAN_POINT('Ctrl Pts',(-10.7301514316607,72.3719017357571,
12.));
#158404=CARTESIAN_POINT('Ctrl Pts',(-10.7238676920469,72.3971760804933,
12.));
#158405=CARTESIAN_POINT('Ctrl Pts',(-10.7175511514788,72.4224813988347,
12.));
#158406=CARTESIAN_POINT('Ctrl Pts',(-10.7112017838706,72.4478175837156,
12.));
#158407=CARTESIAN_POINT('Ctrl Pts',(-10.7048195633061,72.4731845284227,
12.));
#158408=CARTESIAN_POINT('Ctrl Pts',(-10.6984044640398,72.4985821266023,
12.));
#158409=CARTESIAN_POINT('Ctrl Pts',(-10.691956460499,72.5240102722664,12.));
#158410=CARTESIAN_POINT('Ctrl Pts',(-10.6854755272904,72.5494688597961,
12.));
#158411=CARTESIAN_POINT('Ctrl Pts',(-10.6789616392042,72.5749577839415,
12.));
#158412=CARTESIAN_POINT('Ctrl Pts',(-10.6724147711995,72.6004769398019,
12.));
#158413=CARTESIAN_POINT('Ctrl Pts',(-10.6658348983944,72.6260262228065,
12.));
#158414=CARTESIAN_POINT('Ctrl Pts',(-10.659221996058,72.651605528691,12.));
#158415=CARTESIAN_POINT('Ctrl Pts',(-10.6525760396054,72.6772147534752,
12.));
#158416=CARTESIAN_POINT('Ctrl Pts',(-10.6458970045946,72.7028537934317,
12.));
#158417=CARTESIAN_POINT('Ctrl Pts',(-10.6391848667352,72.7285225451293,
12.));
#158418=CARTESIAN_POINT('Ctrl Pts',(-10.6324396018998,72.7542209054812,
12.));
#158419=CARTESIAN_POINT('Ctrl Pts',(-10.6256611861394,72.7799487717911,
12.));
#158420=CARTESIAN_POINT('Ctrl Pts',(-10.6188495956973,72.8057060417887,
12.));
#158421=CARTESIAN_POINT('Ctrl Pts',(-10.6120048070367,72.8314926136881,
12.));
#158422=CARTESIAN_POINT('Ctrl Pts',(-10.6051267968203,72.8573083861337,
12.));
#158423=CARTESIAN_POINT('Ctrl Pts',(-10.5982155418626,72.8831532580845,
12.));
#158424=CARTESIAN_POINT('Ctrl Pts',(-10.5912710190928,72.9090271287083,
12.));
#158425=CARTESIAN_POINT('Ctrl Pts',(-10.5842932055209,72.9349298972822,
12.));
#158426=CARTESIAN_POINT('Ctrl Pts',(-10.5772820781958,72.9608614630534,
12.));
#158427=CARTESIAN_POINT('Ctrl Pts',(-10.570237614205,72.9868217252283,12.));
#158428=CARTESIAN_POINT('Ctrl Pts',(-10.5631597907651,73.0128105832621,
12.));
#158429=CARTESIAN_POINT('Ctrl Pts',(-10.5560485852974,73.0388279370834,
12.));
#158430=CARTESIAN_POINT('Ctrl Pts',(-10.5489039755138,73.0648736873434,
12.));
#158431=CARTESIAN_POINT('Ctrl Pts',(-10.5417259395003,73.0909477356474,
12.));
#158432=CARTESIAN_POINT('Ctrl Pts',(-10.53451445581,73.1170499848039,12.));
#158433=CARTESIAN_POINT('Ctrl Pts',(-10.5272695032653,73.1431803382711,
12.));
#158434=CARTESIAN_POINT('Ctrl Pts',(-10.5199910607654,73.1693386996138,
12.));
#158435=CARTESIAN_POINT('Ctrl Pts',(-10.5126791070805,73.1955249719048,
12.));
#158436=CARTESIAN_POINT('Ctrl Pts',(-10.5053336206908,73.2217390572562,
12.));
#158437=CARTESIAN_POINT('Ctrl Pts',(-10.4979545795192,73.2479808560189,
12.));
#158438=CARTESIAN_POINT('Ctrl Pts',(-10.4905419611523,73.2742502674304,
12.));
#158439=CARTESIAN_POINT('Ctrl Pts',(-10.4830957433305,73.3005471910583,
12.));
#158440=CARTESIAN_POINT('Ctrl Pts',(-10.4756159043806,73.3268715280575,
12.));
#158441=CARTESIAN_POINT('Ctrl Pts',(-10.4681024236289,73.3532231823659,
12.));
#158442=CARTESIAN_POINT('Ctrl Pts',(-10.4605552819397,73.37960206225,12.));
#158443=CARTESIAN_POINT('Ctrl Pts',(-10.452974461845,73.4060080806686,12.));
#158444=CARTESIAN_POINT('Ctrl Pts',(-10.4464473465479,73.4286663448107,
12.));
#158445=CARTESIAN_POINT('Ctrl Pts',(-10.4414249334739,73.44605255288,12.));
#158446=CARTESIAN_POINT('Ctrl Pts',(-10.4379221501041,73.4581547436838,
12.));
#158447=CARTESIAN_POINT('Ctrl Pts',(-10.4359488742809,73.4649650361894,
12.));
#158448=CARTESIAN_POINT('Ctrl Pts',(-10.4355099267296,73.4664795929939,
12.));
#158449=CARTESIAN_POINT('',(-11.3136138754165,69.079679653846,0.));
#158450=CARTESIAN_POINT('',(-11.3136138754165,69.079679653846,0.));
#158451=CARTESIAN_POINT('Ctrl Pts',(-10.4355099267296,73.4664795929939,
0.));
#158452=CARTESIAN_POINT('Ctrl Pts',(-10.4359488742809,73.4649650361894,
0.));
#158453=CARTESIAN_POINT('Ctrl Pts',(-10.4379221501041,73.4581547436838,
0.));
#158454=CARTESIAN_POINT('Ctrl Pts',(-10.4414249334739,73.44605255288,0.));
#158455=CARTESIAN_POINT('Ctrl Pts',(-10.4464473465479,73.4286663448107,
0.));
#158456=CARTESIAN_POINT('Ctrl Pts',(-10.452974461845,73.4060080806686,0.));
#158457=CARTESIAN_POINT('Ctrl Pts',(-10.4605552819397,73.37960206225,0.));
#158458=CARTESIAN_POINT('Ctrl Pts',(-10.4681024236289,73.3532231823659,
0.));
#158459=CARTESIAN_POINT('Ctrl Pts',(-10.4756159043806,73.3268715280575,
0.));
#158460=CARTESIAN_POINT('Ctrl Pts',(-10.4830957433305,73.3005471910583,
0.));
#158461=CARTESIAN_POINT('Ctrl Pts',(-10.4905419611523,73.2742502674304,
0.));
#158462=CARTESIAN_POINT('Ctrl Pts',(-10.4979545795192,73.2479808560189,
0.));
#158463=CARTESIAN_POINT('Ctrl Pts',(-10.5053336206908,73.2217390572562,
0.));
#158464=CARTESIAN_POINT('Ctrl Pts',(-10.5126791070805,73.1955249719048,
0.));
#158465=CARTESIAN_POINT('Ctrl Pts',(-10.5199910607654,73.1693386996138,
0.));
#158466=CARTESIAN_POINT('Ctrl Pts',(-10.5272695032653,73.1431803382711,
0.));
#158467=CARTESIAN_POINT('Ctrl Pts',(-10.53451445581,73.1170499848039,0.));
#158468=CARTESIAN_POINT('Ctrl Pts',(-10.5417259395003,73.0909477356474,
0.));
#158469=CARTESIAN_POINT('Ctrl Pts',(-10.5489039755138,73.0648736873434,
0.));
#158470=CARTESIAN_POINT('Ctrl Pts',(-10.5560485852974,73.0388279370834,
0.));
#158471=CARTESIAN_POINT('Ctrl Pts',(-10.5631597907651,73.0128105832621,
0.));
#158472=CARTESIAN_POINT('Ctrl Pts',(-10.570237614205,72.9868217252283,0.));
#158473=CARTESIAN_POINT('Ctrl Pts',(-10.5772820781958,72.9608614630534,
0.));
#158474=CARTESIAN_POINT('Ctrl Pts',(-10.5842932055209,72.9349298972822,
0.));
#158475=CARTESIAN_POINT('Ctrl Pts',(-10.5912710190928,72.9090271287083,
0.));
#158476=CARTESIAN_POINT('Ctrl Pts',(-10.5982155418626,72.8831532580845,
0.));
#158477=CARTESIAN_POINT('Ctrl Pts',(-10.6051267968203,72.8573083861337,
0.));
#158478=CARTESIAN_POINT('Ctrl Pts',(-10.6120048070367,72.8314926136881,
0.));
#158479=CARTESIAN_POINT('Ctrl Pts',(-10.6188495956973,72.8057060417887,
0.));
#158480=CARTESIAN_POINT('Ctrl Pts',(-10.6256611861394,72.7799487717911,
0.));
#158481=CARTESIAN_POINT('Ctrl Pts',(-10.6324396018998,72.7542209054812,
0.));
#158482=CARTESIAN_POINT('Ctrl Pts',(-10.6391848667352,72.7285225451293,
0.));
#158483=CARTESIAN_POINT('Ctrl Pts',(-10.6458970045946,72.7028537934317,
0.));
#158484=CARTESIAN_POINT('Ctrl Pts',(-10.6525760396054,72.6772147534752,
0.));
#158485=CARTESIAN_POINT('Ctrl Pts',(-10.659221996058,72.651605528691,0.));
#158486=CARTESIAN_POINT('Ctrl Pts',(-10.6658348983944,72.6260262228065,
0.));
#158487=CARTESIAN_POINT('Ctrl Pts',(-10.6724147711995,72.6004769398019,
0.));
#158488=CARTESIAN_POINT('Ctrl Pts',(-10.6789616392042,72.5749577839415,
0.));
#158489=CARTESIAN_POINT('Ctrl Pts',(-10.6854755272904,72.5494688597961,
0.));
#158490=CARTESIAN_POINT('Ctrl Pts',(-10.691956460499,72.5240102722664,0.));
#158491=CARTESIAN_POINT('Ctrl Pts',(-10.6984044640398,72.4985821266023,
0.));
#158492=CARTESIAN_POINT('Ctrl Pts',(-10.7048195633061,72.4731845284227,
0.));
#158493=CARTESIAN_POINT('Ctrl Pts',(-10.7112017838706,72.4478175837156,
0.));
#158494=CARTESIAN_POINT('Ctrl Pts',(-10.7175511514788,72.4224813988347,
0.));
#158495=CARTESIAN_POINT('Ctrl Pts',(-10.7238676920469,72.3971760804933,
0.));
#158496=CARTESIAN_POINT('Ctrl Pts',(-10.7301514316607,72.3719017357571,
0.));
#158497=CARTESIAN_POINT('Ctrl Pts',(-10.73640239658,72.3466584720318,0.));
#158498=CARTESIAN_POINT('Ctrl Pts',(-10.7426206132375,72.3214463970641,
0.));
#158499=CARTESIAN_POINT('Ctrl Pts',(-10.7488061082368,72.2962656189556,
0.));
#158500=CARTESIAN_POINT('Ctrl Pts',(-10.7549589083535,72.2711162461681,
0.));
#158501=CARTESIAN_POINT('Ctrl Pts',(-10.7610790405385,72.2459983875296,
0.));
#158502=CARTESIAN_POINT('Ctrl Pts',(-10.7671665319255,72.2209121522366,
0.));
#158503=CARTESIAN_POINT('Ctrl Pts',(-10.7732214098344,72.1958576498558,
0.));
#158504=CARTESIAN_POINT('Ctrl Pts',(-10.7792437017662,72.1708349903305,
0.));
#158505=CARTESIAN_POINT('Ctrl Pts',(-10.7852334354016,72.1458442839834,
0.));
#158506=CARTESIAN_POINT('Ctrl Pts',(-10.7911906386027,72.1208856415171,
0.));
#158507=CARTESIAN_POINT('Ctrl Pts',(-10.7971153394166,72.0959591740114,
0.));
#158508=CARTESIAN_POINT('Ctrl Pts',(-10.8030075660808,72.0710649929202,
0.));
#158509=CARTESIAN_POINT('Ctrl Pts',(-10.8088673470184,72.0462032100815,
0.));
#158510=CARTESIAN_POINT('Ctrl Pts',(-10.8146947108375,72.0213739377223,
0.));
#158511=CARTESIAN_POINT('Ctrl Pts',(-10.8204896863328,71.9965772884619,
0.));
#158512=CARTESIAN_POINT('Ctrl Pts',(-10.8262523024898,71.9718133753127,
0.));
#158513=CARTESIAN_POINT('Ctrl Pts',(-10.8319825884918,71.9470823116785,
0.));
#158514=CARTESIAN_POINT('Ctrl Pts',(-10.8376805737159,71.9223842113625,
0.));
#158515=CARTESIAN_POINT('Ctrl Pts',(-10.8433462877311,71.8977191885725,
0.));
#158516=CARTESIAN_POINT('Ctrl Pts',(-10.8489797602997,71.8730873579224,
0.));
#158517=CARTESIAN_POINT('Ctrl Pts',(-10.8545810213799,71.8484888344339,
0.));
#158518=CARTESIAN_POINT('Ctrl Pts',(-10.8601501011332,71.8239237335331,
0.));
#158519=CARTESIAN_POINT('Ctrl Pts',(-10.865687029922,71.7993921710564,0.));
#158520=CARTESIAN_POINT('Ctrl Pts',(-10.8711918383073,71.7748942632593,
0.));
#158521=CARTESIAN_POINT('Ctrl Pts',(-10.8766645570497,71.7504301268181,
0.));
#158522=CARTESIAN_POINT('Ctrl Pts',(-10.8821052171121,71.7259998788328,
0.));
#158523=CARTESIAN_POINT('Ctrl Pts',(-10.8875138496671,71.7016036368236,
0.));
#158524=CARTESIAN_POINT('Ctrl Pts',(-10.8928904860964,71.6772415187364,
0.));
#158525=CARTESIAN_POINT('Ctrl Pts',(-10.8982351579871,71.6529136429504,
0.));
#158526=CARTESIAN_POINT('Ctrl Pts',(-10.9035478971328,71.6286201282812,
0.));
#158527=CARTESIAN_POINT('Ctrl Pts',(-10.9088287355365,71.6043610939835,
0.));
#158528=CARTESIAN_POINT('Ctrl Pts',(-10.914077705417,71.5801366597488,0.));
#158529=CARTESIAN_POINT('Ctrl Pts',(-10.91929483921,71.5559469457091,0.));
#158530=CARTESIAN_POINT('Ctrl Pts',(-10.9244801695642,71.5317920724459,
0.));
#158531=CARTESIAN_POINT('Ctrl Pts',(-10.9296337293424,71.5076721609937,
0.));
#158532=CARTESIAN_POINT('Ctrl Pts',(-10.9347555516235,71.4835873328423,
0.));
#158533=CARTESIAN_POINT('Ctrl Pts',(-10.9398456697095,71.4595377099351,
0.));
#158534=CARTESIAN_POINT('Ctrl Pts',(-10.944904117127,71.435523414672,0.));
#158535=CARTESIAN_POINT('Ctrl Pts',(-10.9499309276236,71.4115445699194,
0.));
#158536=CARTESIAN_POINT('Ctrl Pts',(-10.954926135169,71.3876012990138,0.));
#158537=CARTESIAN_POINT('Ctrl Pts',(-10.9598897739564,71.3636937257649,
0.));
#158538=CARTESIAN_POINT('Ctrl Pts',(-10.9648218784098,71.339821974454,0.));
#158539=CARTESIAN_POINT('Ctrl Pts',(-10.969722483186,71.3159861698358,0.));
#158540=CARTESIAN_POINT('Ctrl Pts',(-10.9745916231709,71.2921864371491,
0.));
#158541=CARTESIAN_POINT('Ctrl Pts',(-10.9794293334805,71.2684229021207,
0.));
#158542=CARTESIAN_POINT('Ctrl Pts',(-10.9842356494627,71.2446956909687,
0.));
#158543=CARTESIAN_POINT('Ctrl Pts',(-10.9890106067039,71.2210049304014,
0.));
#158544=CARTESIAN_POINT('Ctrl Pts',(-10.993754241032,71.1973507476191,0.));
#158545=CARTESIAN_POINT('Ctrl Pts',(-10.9984665885127,71.1737332703248,
0.));
#158546=CARTESIAN_POINT('Ctrl Pts',(-11.0031476854502,71.1501526267286,
0.));
#158547=CARTESIAN_POINT('Ctrl Pts',(-11.0077975683895,71.1266089455517,
0.));
#158548=CARTESIAN_POINT('Ctrl Pts',(-11.0124162741224,71.1031023560249,
0.));
#158549=CARTESIAN_POINT('Ctrl Pts',(-11.0170038396915,71.0796329878907,
0.));
#158550=CARTESIAN_POINT('Ctrl Pts',(-11.0215603023856,71.0562009714136,
0.));
#158551=CARTESIAN_POINT('Ctrl Pts',(-11.0260856997415,71.0328064373856,
0.));
#158552=CARTESIAN_POINT('Ctrl Pts',(-11.0305800695456,71.0094495171292,
0.));
#158553=CARTESIAN_POINT('Ctrl Pts',(-11.0350434498405,70.986130342497,0.));
#158554=CARTESIAN_POINT('Ctrl Pts',(-11.0394758789285,70.9628490458748,
0.));
#158555=CARTESIAN_POINT('Ctrl Pts',(-11.0438773953681,70.9396057601924,
0.));
#158556=CARTESIAN_POINT('Ctrl Pts',(-11.048248037975,70.916400618927,0.));
#158557=CARTESIAN_POINT('Ctrl Pts',(-11.0525878458243,70.8932337561087,
0.));
#158558=CARTESIAN_POINT('Ctrl Pts',(-11.0568968582569,70.8701053063186,
0.));
#158559=CARTESIAN_POINT('Ctrl Pts',(-11.0611751148835,70.8470154046919,
0.));
#158560=CARTESIAN_POINT('Ctrl Pts',(-11.0654226555802,70.8239641869299,
0.));
#158561=CARTESIAN_POINT('Ctrl Pts',(-11.0696395204909,70.8009517893057,
0.));
#158562=CARTESIAN_POINT('Ctrl Pts',(-11.073825750029,70.7779783486677,0.));
#158563=CARTESIAN_POINT('Ctrl Pts',(-11.0779813848846,70.7550440024384,
0.));
#158564=CARTESIAN_POINT('Ctrl Pts',(-11.0821064660269,70.732148888618,0.));
#158565=CARTESIAN_POINT('Ctrl Pts',(-11.0862010347016,70.7092931457954,
0.));
#158566=CARTESIAN_POINT('Ctrl Pts',(-11.0902651324323,70.6864769131546,
0.));
#158567=CARTESIAN_POINT('Ctrl Pts',(-11.0942988010233,70.6637003304785,
0.));
#158568=CARTESIAN_POINT('Ctrl Pts',(-11.0983020825667,70.6409635381482,
0.));
#158569=CARTESIAN_POINT('Ctrl Pts',(-11.1022750194446,70.6182666771481,
0.));
#158570=CARTESIAN_POINT('Ctrl Pts',(-11.1062176543262,70.5956098890773,
0.));
#158571=CARTESIAN_POINT('Ctrl Pts',(-11.1101300301701,70.5729933161546,
0.));
#158572=CARTESIAN_POINT('Ctrl Pts',(-11.1140121902271,70.5504171012233,
0.));
#158573=CARTESIAN_POINT('Ctrl Pts',(-11.1178641780476,70.5278813877494,
0.));
#158574=CARTESIAN_POINT('Ctrl Pts',(-11.1216860374826,70.505386319828,0.));
#158575=CARTESIAN_POINT('Ctrl Pts',(-11.1254778126821,70.4829320421957,
0.));
#158576=CARTESIAN_POINT('Ctrl Pts',(-11.1292395480974,70.4605187002354,
0.));
#158577=CARTESIAN_POINT('Ctrl Pts',(-11.1329712884846,70.4381464399819,
0.));
#158578=CARTESIAN_POINT('Ctrl Pts',(-11.1366730789126,70.4158154081205,
0.));
#158579=CARTESIAN_POINT('Ctrl Pts',(-11.1403449647625,70.393525751996,0.));
#158580=CARTESIAN_POINT('Ctrl Pts',(-11.143986991727,70.3712776196223,0.));
#158581=CARTESIAN_POINT('Ctrl Pts',(-11.1475992058124,70.349071159688,0.));
#158582=CARTESIAN_POINT('Ctrl Pts',(-11.1511816533421,70.326906521559,0.));
#158583=CARTESIAN_POINT('Ctrl Pts',(-11.1547343809646,70.3047838552756,
0.));
#158584=CARTESIAN_POINT('Ctrl Pts',(-11.1582574356521,70.2827033115662,
0.));
#158585=CARTESIAN_POINT('Ctrl Pts',(-11.1617508647016,70.2606650418589,
0.));
#158586=CARTESIAN_POINT('Ctrl Pts',(-11.1652147157383,70.2386691982902,
0.));
#158587=CARTESIAN_POINT('Ctrl Pts',(-11.168649036721,70.2167159337094,0.));
#158588=CARTESIAN_POINT('Ctrl Pts',(-11.1720538759499,70.1948054016816,
0.));
#158589=CARTESIAN_POINT('Ctrl Pts',(-11.1754292820631,70.1729377564954,
0.));
#158590=CARTESIAN_POINT('Ctrl Pts',(-11.1787753040363,70.1511131531672,
0.));
#158591=CARTESIAN_POINT('Ctrl Pts',(-11.1820919911846,70.1293317474432,
0.));
#158592=CARTESIAN_POINT('Ctrl Pts',(-11.185379393167,70.1075936957973,0.));
#158593=CARTESIAN_POINT('Ctrl Pts',(-11.1886375599916,70.0858991554295,
0.));
#158594=CARTESIAN_POINT('Ctrl Pts',(-11.1918665420168,70.0642482842942,
0.));
#158595=CARTESIAN_POINT('Ctrl Pts',(-11.1950663899578,70.0426412411194,
0.));
#158596=CARTESIAN_POINT('Ctrl Pts',(-11.1982371548918,70.0210781854236,
0.));
#158597=CARTESIAN_POINT('Ctrl Pts',(-11.2013788882711,69.9995592775322,
0.));
#158598=CARTESIAN_POINT('Ctrl Pts',(-11.2044916419239,69.9780846785771,
0.));
#158599=CARTESIAN_POINT('Ctrl Pts',(-11.2075754680445,69.9566545504813,
0.));
#158600=CARTESIAN_POINT('Ctrl Pts',(-11.2106304191881,69.9352690559399,
0.));
#158601=CARTESIAN_POINT('Ctrl Pts',(-11.2136565482679,69.9139283584036,
0.));
#158602=CARTESIAN_POINT('Ctrl Pts',(-11.2166539085527,69.8926326220414,
0.));
#158603=CARTESIAN_POINT('Ctrl Pts',(-11.2196225536794,69.8713820117918,
0.));
#158604=CARTESIAN_POINT('Ctrl Pts',(-11.2225625376739,69.8501766934445,
0.));
#158605=CARTESIAN_POINT('Ctrl Pts',(-11.225473914972,69.8290168337076,0.));
#158606=CARTESIAN_POINT('Ctrl Pts',(-11.2283567404434,69.8079026002753,
0.));
#158607=CARTESIAN_POINT('Ctrl Pts',(-11.2312110694183,69.7868341618927,
0.));
#158608=CARTESIAN_POINT('Ctrl Pts',(-11.2340369576452,69.7658116882298,
0.));
#158609=CARTESIAN_POINT('Ctrl Pts',(-11.236834461247,69.7448353497394,0.));
#158610=CARTESIAN_POINT('Ctrl Pts',(-11.2396036366861,69.7239053175362,
0.));
#158611=CARTESIAN_POINT('Ctrl Pts',(-11.242344540717,69.7030217632187,0.));
#158612=CARTESIAN_POINT('Ctrl Pts',(-11.2450572303847,69.6821848588492,
0.));
#158613=CARTESIAN_POINT('Ctrl Pts',(-11.2477417631391,69.6613947773563,
0.));
#158614=CARTESIAN_POINT('Ctrl Pts',(-11.2503981969413,69.6406516928902,
0.));
#158615=CARTESIAN_POINT('Ctrl Pts',(-11.2530265903555,69.6199557811231,
0.));
#158616=CARTESIAN_POINT('Ctrl Pts',(-11.255627002701,69.5993072197355,0.));
#158617=CARTESIAN_POINT('Ctrl Pts',(-11.2581994939534,69.5787061880815,
0.));
#158618=CARTESIAN_POINT('Ctrl Pts',(-11.2607441244698,69.5581528662846,
0.));
#158619=CARTESIAN_POINT('Ctrl Pts',(-11.2632609547629,69.5376474344768,
0.));
#158620=CARTESIAN_POINT('Ctrl Pts',(-11.2657500452721,69.5171900720188,
0.));
#158621=CARTESIAN_POINT('Ctrl Pts',(-11.2682114561015,69.4967809565978,
0.));
#158622=CARTESIAN_POINT('Ctrl Pts',(-11.2706452475287,69.4764202659443,
0.));
#158623=CARTESIAN_POINT('Ctrl Pts',(-11.2730514806143,69.4561081798815,
0.));
#158624=CARTESIAN_POINT('Ctrl Pts',(-11.2754302177019,69.4358448819957,
0.));
#158625=CARTESIAN_POINT('Ctrl Pts',(-11.2777815231462,69.4156305620554,
0.));
#158626=CARTESIAN_POINT('Ctrl Pts',(-11.2801054633807,69.395465416223,0.));
#158627=CARTESIAN_POINT('Ctrl Pts',(-11.2824021054038,69.375349642,0.));
#158628=CARTESIAN_POINT('Ctrl Pts',(-11.2846715154521,69.3552834337771,
0.));
#158629=CARTESIAN_POINT('Ctrl Pts',(-11.2869137578463,69.3352669789611,
0.));
#158630=CARTESIAN_POINT('Ctrl Pts',(-11.2891288931528,69.315300451784,0.));
#158631=CARTESIAN_POINT('Ctrl Pts',(-11.2913169799642,69.2953840192792,
0.));
#158632=CARTESIAN_POINT('Ctrl Pts',(-11.2934780784361,69.2755178531534,
0.));
#158633=CARTESIAN_POINT('Ctrl Pts',(-11.2956122531375,69.255702139335,0.));
#158634=CARTESIAN_POINT('Ctrl Pts',(-11.2977195764836,69.2359370894828,
0.));
#158635=CARTESIAN_POINT('Ctrl Pts',(-11.2998001310934,69.216222948839,0.));
#158636=CARTESIAN_POINT('Ctrl Pts',(-11.3018540025605,69.1965599718761,
0.));
#158637=CARTESIAN_POINT('Ctrl Pts',(-11.3038812726275,69.1769483991639,
0.));
#158638=CARTESIAN_POINT('Ctrl Pts',(-11.3058820128323,69.1573884361076,
0.));
#158639=CARTESIAN_POINT('Ctrl Pts',(-11.3078562764442,69.137880225198,0.));
#158640=CARTESIAN_POINT('Ctrl Pts',(-11.3098040973799,69.1184238445065,
0.));
#158641=CARTESIAN_POINT('Ctrl Pts',(-11.3113412156742,69.1029002322497,
0.));
#158642=CARTESIAN_POINT('Ctrl Pts',(-11.3124821678849,69.0912808657051,
0.));
#158643=CARTESIAN_POINT('Ctrl Pts',(-11.3132375200184,69.0835449954486,
0.));
#158644=CARTESIAN_POINT('Ctrl Pts',(-11.3136138754165,69.079679653846,0.));
#158645=CARTESIAN_POINT('Ctrl Pts',(-3.87370827955544,74.3992230078037,
0.));
#158646=CARTESIAN_POINT('Ctrl Pts',(-3.87370827955544,74.3992230078037,
12.));
#158647=CARTESIAN_POINT('Ctrl Pts',(-3.87578335377325,74.3940262116388,
0.));
#158648=CARTESIAN_POINT('Ctrl Pts',(-3.87578335377325,74.3940262116388,
12.));
#158649=CARTESIAN_POINT('Ctrl Pts',(-3.87992989995747,74.3836349189184,
0.));
#158650=CARTESIAN_POINT('Ctrl Pts',(-3.87992989995747,74.3836349189184,
12.));
#158651=CARTESIAN_POINT('Ctrl Pts',(-3.88613891247984,74.3680548786661,
0.));
#158652=CARTESIAN_POINT('Ctrl Pts',(-3.88613891247984,74.3680548786661,
12.));
#158653=CARTESIAN_POINT('Ctrl Pts',(-3.89439598145329,74.3472952898745,
0.));
#158654=CARTESIAN_POINT('Ctrl Pts',(-3.89439598145329,74.3472952898745,
12.));
#158655=CARTESIAN_POINT('Ctrl Pts',(-3.90468128904634,74.3213688090134,
0.));
#158656=CARTESIAN_POINT('Ctrl Pts',(-3.90468128904634,74.3213688090134,
12.));
#158657=CARTESIAN_POINT('Ctrl Pts',(-3.9149305628503,74.2954653518728,0.));
#158658=CARTESIAN_POINT('Ctrl Pts',(-3.9149305628503,74.2954653518728,12.));
#158659=CARTESIAN_POINT('Ctrl Pts',(-3.92514379920743,74.2695849516226,
0.));
#158660=CARTESIAN_POINT('Ctrl Pts',(-3.92514379920743,74.2695849516226,
12.));
#158661=CARTESIAN_POINT('Ctrl Pts',(-3.93532099774204,74.2437276593623,
0.));
#158662=CARTESIAN_POINT('Ctrl Pts',(-3.93532099774204,74.2437276593623,
12.));
#158663=CARTESIAN_POINT('Ctrl Pts',(-3.94546216377451,74.2178935492876,
0.));
#158664=CARTESIAN_POINT('Ctrl Pts',(-3.94546216377451,74.2178935492876,
12.));
#158665=CARTESIAN_POINT('Ctrl Pts',(-3.95556730821111,74.1920827166585,
0.));
#158666=CARTESIAN_POINT('Ctrl Pts',(-3.95556730821111,74.1920827166585,
12.));
#158667=CARTESIAN_POINT('Ctrl Pts',(-3.96563644549385,74.1662952702485,
0.));
#158668=CARTESIAN_POINT('Ctrl Pts',(-3.96563644549385,74.1662952702485,
12.));
#158669=CARTESIAN_POINT('Ctrl Pts',(-3.97566959209529,74.1405313263109,
0.));
#158670=CARTESIAN_POINT('Ctrl Pts',(-3.97566959209529,74.1405313263109,
12.));
#158671=CARTESIAN_POINT('Ctrl Pts',(-3.98566676483642,74.1147910020891,
0.));
#158672=CARTESIAN_POINT('Ctrl Pts',(-3.98566676483642,74.1147910020891,
12.));
#158673=CARTESIAN_POINT('Ctrl Pts',(-3.99562797918287,74.0890744091186,
0.));
#158674=CARTESIAN_POINT('Ctrl Pts',(-3.99562797918287,74.0890744091186,
12.));
#158675=CARTESIAN_POINT('Ctrl Pts',(-4.0055532478548,74.0633816478037,0.));
#158676=CARTESIAN_POINT('Ctrl Pts',(-4.0055532478548,74.0633816478037,12.));
#158677=CARTESIAN_POINT('Ctrl Pts',(-4.01544258176711,74.0377128111863,
0.));
#158678=CARTESIAN_POINT('Ctrl Pts',(-4.01544258176711,74.0377128111863,
12.));
#158679=CARTESIAN_POINT('Ctrl Pts',(-4.02529599070095,74.012067987646,0.));
#158680=CARTESIAN_POINT('Ctrl Pts',(-4.02529599070095,74.012067987646,12.));
#158681=CARTESIAN_POINT('Ctrl Pts',(-4.0351134841066,73.9864472641033,0.));
#158682=CARTESIAN_POINT('Ctrl Pts',(-4.0351134841066,73.9864472641033,12.));
#158683=CARTESIAN_POINT('Ctrl Pts',(-4.04489507179957,73.9608507287909,
0.));
#158684=CARTESIAN_POINT('Ctrl Pts',(-4.04489507179957,73.9608507287909,
12.));
#158685=CARTESIAN_POINT('Ctrl Pts',(-4.05464076484752,73.9352784747608,
0.));
#158686=CARTESIAN_POINT('Ctrl Pts',(-4.05464076484752,73.9352784747608,
12.));
#158687=CARTESIAN_POINT('Ctrl Pts',(-4.06435057547325,73.9097305995115,
0.));
#158688=CARTESIAN_POINT('Ctrl Pts',(-4.06435057547325,73.9097305995115,
12.));
#158689=CARTESIAN_POINT('Ctrl Pts',(-4.07402451665245,73.8842072034008,
0.));
#158690=CARTESIAN_POINT('Ctrl Pts',(-4.07402451665245,73.8842072034008,
12.));
#158691=CARTESIAN_POINT('Ctrl Pts',(-4.08366260180674,73.8587083884191,
0.));
#158692=CARTESIAN_POINT('Ctrl Pts',(-4.08366260180674,73.8587083884191,
12.));
#158693=CARTESIAN_POINT('Ctrl Pts',(-4.09326484448233,73.8332342568989,
0.));
#158694=CARTESIAN_POINT('Ctrl Pts',(-4.09326484448233,73.8332342568989,
12.));
#158695=CARTESIAN_POINT('Ctrl Pts',(-4.10283125798729,73.8077849100342,
0.));
#158696=CARTESIAN_POINT('Ctrl Pts',(-4.10283125798729,73.8077849100342,
12.));
#158697=CARTESIAN_POINT('Ctrl Pts',(-4.11236185522787,73.7823604472159,
0.));
#158698=CARTESIAN_POINT('Ctrl Pts',(-4.11236185522787,73.7823604472159,
12.));
#158699=CARTESIAN_POINT('Ctrl Pts',(-4.12185664890557,73.7569609668528,
0.));
#158700=CARTESIAN_POINT('Ctrl Pts',(-4.12185664890557,73.7569609668528,
12.));
#158701=CARTESIAN_POINT('Ctrl Pts',(-4.13131565163578,73.7315865668522,
0.));
#158702=CARTESIAN_POINT('Ctrl Pts',(-4.13131565163578,73.7315865668522,
12.));
#158703=CARTESIAN_POINT('Ctrl Pts',(-4.14073887610153,73.7062373452342,
0.));
#158704=CARTESIAN_POINT('Ctrl Pts',(-4.14073887610153,73.7062373452342,
12.));
#158705=CARTESIAN_POINT('Ctrl Pts',(-4.15012633519723,73.6809134006897,
0.));
#158706=CARTESIAN_POINT('Ctrl Pts',(-4.15012633519723,73.6809134006897,
12.));
#158707=CARTESIAN_POINT('Ctrl Pts',(-4.15947804217784,73.6556148331489,
0.));
#158708=CARTESIAN_POINT('Ctrl Pts',(-4.15947804217784,73.6556148331489,
12.));
#158709=CARTESIAN_POINT('Ctrl Pts',(-4.1687940105878,73.6303417435251,0.));
#158710=CARTESIAN_POINT('Ctrl Pts',(-4.1687940105878,73.6303417435251,12.));
#158711=CARTESIAN_POINT('Ctrl Pts',(-4.17807425419813,73.6050942334768,
0.));
#158712=CARTESIAN_POINT('Ctrl Pts',(-4.17807425419813,73.6050942334768,
12.));
#158713=CARTESIAN_POINT('Ctrl Pts',(-4.18731878694236,73.5798724051519,
0.));
#158714=CARTESIAN_POINT('Ctrl Pts',(-4.18731878694236,73.5798724051519,
12.));
#158715=CARTESIAN_POINT('Ctrl Pts',(-4.19652762286127,73.5546763609572,
0.));
#158716=CARTESIAN_POINT('Ctrl Pts',(-4.19652762286127,73.5546763609572,
12.));
#158717=CARTESIAN_POINT('Ctrl Pts',(-4.2057007760373,73.5295062032628,0.));
#158718=CARTESIAN_POINT('Ctrl Pts',(-4.2057007760373,73.5295062032628,12.));
#158719=CARTESIAN_POINT('Ctrl Pts',(-4.21483826059441,73.5043620344116,
0.));
#158720=CARTESIAN_POINT('Ctrl Pts',(-4.21483826059441,73.5043620344116,
12.));
#158721=CARTESIAN_POINT('Ctrl Pts',(-4.22394009072756,73.4792439568633,
0.));
#158722=CARTESIAN_POINT('Ctrl Pts',(-4.22394009072756,73.4792439568633,
12.));
#158723=CARTESIAN_POINT('Ctrl Pts',(-4.23300628072758,73.4541520732948,
0.));
#158724=CARTESIAN_POINT('Ctrl Pts',(-4.23300628072758,73.4541520732948,
12.));
#158725=CARTESIAN_POINT('Ctrl Pts',(-4.24203684500939,73.4290864867101,
0.));
#158726=CARTESIAN_POINT('Ctrl Pts',(-4.24203684500939,73.4290864867101,
12.));
#158727=CARTESIAN_POINT('Ctrl Pts',(-4.25103179814887,73.4040473005592,
0.));
#158728=CARTESIAN_POINT('Ctrl Pts',(-4.25103179814887,73.4040473005592,
12.));
#158729=CARTESIAN_POINT('Ctrl Pts',(-4.25999115489899,73.3790346187938,
0.));
#158730=CARTESIAN_POINT('Ctrl Pts',(-4.25999115489899,73.3790346187938,
12.));
#158731=CARTESIAN_POINT('Ctrl Pts',(-4.268914930167,73.3540485458065,0.));
#158732=CARTESIAN_POINT('Ctrl Pts',(-4.268914930167,73.3540485458065,12.));
#158733=CARTESIAN_POINT('Ctrl Pts',(-4.2778031390039,73.3290891863949,0.));
#158734=CARTESIAN_POINT('Ctrl Pts',(-4.2778031390039,73.3290891863949,12.));
#158735=CARTESIAN_POINT('Ctrl Pts',(-4.28665579659301,73.3041566457135,
0.));
#158736=CARTESIAN_POINT('Ctrl Pts',(-4.28665579659301,73.3041566457135,
12.));
#158737=CARTESIAN_POINT('Ctrl Pts',(-4.29547291824287,73.2792510292254,
0.));
#158738=CARTESIAN_POINT('Ctrl Pts',(-4.29547291824287,73.2792510292254,
12.));
#158739=CARTESIAN_POINT('Ctrl Pts',(-4.3042545193823,73.2543724426577,0.));
#158740=CARTESIAN_POINT('Ctrl Pts',(-4.3042545193823,73.2543724426577,12.));
#158741=CARTESIAN_POINT('Ctrl Pts',(-4.31300061556098,73.2295209920334,
0.));
#158742=CARTESIAN_POINT('Ctrl Pts',(-4.31300061556098,73.2295209920334,
12.));
#158743=CARTESIAN_POINT('Ctrl Pts',(-4.32171122245214,73.204696783694,0.));
#158744=CARTESIAN_POINT('Ctrl Pts',(-4.32171122245214,73.204696783694,12.));
#158745=CARTESIAN_POINT('Ctrl Pts',(-4.33038635585877,73.1798999243235,
0.));
#158746=CARTESIAN_POINT('Ctrl Pts',(-4.33038635585877,73.1798999243235,
12.));
#158747=CARTESIAN_POINT('Ctrl Pts',(-4.33902603172141,73.1551305209685,
0.));
#158748=CARTESIAN_POINT('Ctrl Pts',(-4.33902603172141,73.1551305209685,
12.));
#158749=CARTESIAN_POINT('Ctrl Pts',(-4.34763026613158,73.130388681059,0.));
#158750=CARTESIAN_POINT('Ctrl Pts',(-4.34763026613158,73.130388681059,12.));
#158751=CARTESIAN_POINT('Ctrl Pts',(-4.3561990753272,73.1056745124087,0.));
#158752=CARTESIAN_POINT('Ctrl Pts',(-4.3561990753272,73.1056745124087,12.));
#158753=CARTESIAN_POINT('Ctrl Pts',(-4.36473247568641,73.0809881232103,
0.));
#158754=CARTESIAN_POINT('Ctrl Pts',(-4.36473247568641,73.0809881232103,
12.));
#158755=CARTESIAN_POINT('Ctrl Pts',(-4.37323048372607,73.0563296220299,
0.));
#158756=CARTESIAN_POINT('Ctrl Pts',(-4.37323048372607,73.0563296220299,
12.));
#158757=CARTESIAN_POINT('Ctrl Pts',(-4.38169311610151,73.0316991177993,
0.));
#158758=CARTESIAN_POINT('Ctrl Pts',(-4.38169311610151,73.0316991177993,
12.));
#158759=CARTESIAN_POINT('Ctrl Pts',(-4.39012038961139,73.007096719804,0.));
#158760=CARTESIAN_POINT('Ctrl Pts',(-4.39012038961139,73.007096719804,12.));
#158761=CARTESIAN_POINT('Ctrl Pts',(-4.39851232119722,72.9825225376846,
0.));
#158762=CARTESIAN_POINT('Ctrl Pts',(-4.39851232119722,72.9825225376846,
12.));
#158763=CARTESIAN_POINT('Ctrl Pts',(-4.40686892793957,72.95797668145,0.));
#158764=CARTESIAN_POINT('Ctrl Pts',(-4.40686892793957,72.95797668145,12.));
#158765=CARTESIAN_POINT('Ctrl Pts',(-4.41519022705921,72.9334592614829,
0.));
#158766=CARTESIAN_POINT('Ctrl Pts',(-4.41519022705921,72.9334592614829,
12.));
#158767=CARTESIAN_POINT('Ctrl Pts',(-4.42347623591942,72.9089703885462,
0.));
#158768=CARTESIAN_POINT('Ctrl Pts',(-4.42347623591942,72.9089703885462,
12.));
#158769=CARTESIAN_POINT('Ctrl Pts',(-4.43172697203349,72.8845101737855,
0.));
#158770=CARTESIAN_POINT('Ctrl Pts',(-4.43172697203349,72.8845101737855,
12.));
#158771=CARTESIAN_POINT('Ctrl Pts',(-4.43994245306818,72.8600787287318,
0.));
#158772=CARTESIAN_POINT('Ctrl Pts',(-4.43994245306818,72.8600787287318,
12.));
#158773=CARTESIAN_POINT('Ctrl Pts',(-4.44812269683738,72.8356761653069,
0.));
#158774=CARTESIAN_POINT('Ctrl Pts',(-4.44812269683738,72.8356761653069,
12.));
#158775=CARTESIAN_POINT('Ctrl Pts',(-4.45626772130146,72.8113025958262,
0.));
#158776=CARTESIAN_POINT('Ctrl Pts',(-4.45626772130146,72.8113025958262,
12.));
#158777=CARTESIAN_POINT('Ctrl Pts',(-4.46437754456793,72.7869581329994,
0.));
#158778=CARTESIAN_POINT('Ctrl Pts',(-4.46437754456793,72.7869581329994,
12.));
#158779=CARTESIAN_POINT('Ctrl Pts',(-4.4724521848961,72.7626428899281,0.));
#158780=CARTESIAN_POINT('Ctrl Pts',(-4.4724521848961,72.7626428899281,12.));
#158781=CARTESIAN_POINT('Ctrl Pts',(-4.48049166070205,72.738356980103,0.));
#158782=CARTESIAN_POINT('Ctrl Pts',(-4.48049166070205,72.738356980103,12.));
#158783=CARTESIAN_POINT('Ctrl Pts',(-4.48849599055337,72.714100517414,0.));
#158784=CARTESIAN_POINT('Ctrl Pts',(-4.48849599055337,72.714100517414,12.));
#158785=CARTESIAN_POINT('Ctrl Pts',(-4.49646519316813,72.6898736161542,
0.));
#158786=CARTESIAN_POINT('Ctrl Pts',(-4.49646519316813,72.6898736161542,
12.));
#158787=CARTESIAN_POINT('Ctrl Pts',(-4.50439928741604,72.6656763910241,
0.));
#158788=CARTESIAN_POINT('Ctrl Pts',(-4.50439928741604,72.6656763910241,
12.));
#158789=CARTESIAN_POINT('Ctrl Pts',(-4.51229829232264,72.6415089571321,
0.));
#158790=CARTESIAN_POINT('Ctrl Pts',(-4.51229829232264,72.6415089571321,
12.));
#158791=CARTESIAN_POINT('Ctrl Pts',(-4.52016222707638,72.6173714299942,
0.));
#158792=CARTESIAN_POINT('Ctrl Pts',(-4.52016222707638,72.6173714299942,
12.));
#158793=CARTESIAN_POINT('Ctrl Pts',(-4.52799111102392,72.5932639255409,
0.));
#158794=CARTESIAN_POINT('Ctrl Pts',(-4.52799111102392,72.5932639255409,
12.));
#158795=CARTESIAN_POINT('Ctrl Pts',(-4.535784963668,72.5691865601223,0.));
#158796=CARTESIAN_POINT('Ctrl Pts',(-4.535784963668,72.5691865601223,12.));
#158797=CARTESIAN_POINT('Ctrl Pts',(-4.54354380466822,72.5451394505104,
0.));
#158798=CARTESIAN_POINT('Ctrl Pts',(-4.54354380466822,72.5451394505104,
12.));
#158799=CARTESIAN_POINT('Ctrl Pts',(-4.55126765384404,72.5211227139001,
0.));
#158800=CARTESIAN_POINT('Ctrl Pts',(-4.55126765384404,72.5211227139001,
12.));
#158801=CARTESIAN_POINT('Ctrl Pts',(-4.55895653118221,72.4971364679068,
0.));
#158802=CARTESIAN_POINT('Ctrl Pts',(-4.55895653118221,72.4971364679068,
12.));
#158803=CARTESIAN_POINT('Ctrl Pts',(-4.56661045683376,72.4731808305728,
0.));
#158804=CARTESIAN_POINT('Ctrl Pts',(-4.56661045683376,72.4731808305728,
12.));
#158805=CARTESIAN_POINT('Ctrl Pts',(-4.57422945111102,72.4492559203745,
0.));
#158806=CARTESIAN_POINT('Ctrl Pts',(-4.57422945111102,72.4492559203745,
12.));
#158807=CARTESIAN_POINT('Ctrl Pts',(-4.58181353448852,72.4253618562252,
0.));
#158808=CARTESIAN_POINT('Ctrl Pts',(-4.58181353448852,72.4253618562252,
12.));
#158809=CARTESIAN_POINT('Ctrl Pts',(-4.58936272760544,72.401498757478,0.));
#158810=CARTESIAN_POINT('Ctrl Pts',(-4.58936272760544,72.401498757478,12.));
#158811=CARTESIAN_POINT('Ctrl Pts',(-4.5968770512733,72.3776667439227,0.));
#158812=CARTESIAN_POINT('Ctrl Pts',(-4.5968770512733,72.3776667439227,12.));
#158813=CARTESIAN_POINT('Ctrl Pts',(-4.60435652647453,72.3538659357913,
0.));
#158814=CARTESIAN_POINT('Ctrl Pts',(-4.60435652647453,72.3538659357913,
12.));
#158815=CARTESIAN_POINT('Ctrl Pts',(-4.61180117435862,72.3300964537658,
0.));
#158816=CARTESIAN_POINT('Ctrl Pts',(-4.61180117435862,72.3300964537658,
12.));
#158817=CARTESIAN_POINT('Ctrl Pts',(-4.61921101624292,72.3063584189807,
0.));
#158818=CARTESIAN_POINT('Ctrl Pts',(-4.61921101624292,72.3063584189807,
12.));
#158819=CARTESIAN_POINT('Ctrl Pts',(-4.62658607361466,72.2826519530259,
0.));
#158820=CARTESIAN_POINT('Ctrl Pts',(-4.62658607361466,72.2826519530259,
12.));
#158821=CARTESIAN_POINT('Ctrl Pts',(-4.63392636813844,72.2589771779456,
0.));
#158822=CARTESIAN_POINT('Ctrl Pts',(-4.63392636813844,72.2589771779456,
12.));
#158823=CARTESIAN_POINT('Ctrl Pts',(-4.64123192165628,72.2353342162417,
0.));
#158824=CARTESIAN_POINT('Ctrl Pts',(-4.64123192165628,72.2353342162417,
12.));
#158825=CARTESIAN_POINT('Ctrl Pts',(-4.64850275618323,72.2117231908822,
0.));
#158826=CARTESIAN_POINT('Ctrl Pts',(-4.64850275618323,72.2117231908822,
12.));
#158827=CARTESIAN_POINT('Ctrl Pts',(-4.65573889390822,72.1881442253053,
0.));
#158828=CARTESIAN_POINT('Ctrl Pts',(-4.65573889390822,72.1881442253053,
12.));
#158829=CARTESIAN_POINT('Ctrl Pts',(-4.6629403571957,72.1645974434216,0.));
#158830=CARTESIAN_POINT('Ctrl Pts',(-4.6629403571957,72.1645974434216,12.));
#158831=CARTESIAN_POINT('Ctrl Pts',(-4.67010716859285,72.1410829696128,
0.));
#158832=CARTESIAN_POINT('Ctrl Pts',(-4.67010716859285,72.1410829696128,
12.));
#158833=CARTESIAN_POINT('Ctrl Pts',(-4.67723935083095,72.1176009287351,
0.));
#158834=CARTESIAN_POINT('Ctrl Pts',(-4.67723935083095,72.1176009287351,
12.));
#158835=CARTESIAN_POINT('Ctrl Pts',(-4.68433692682069,72.0941514461287,
0.));
#158836=CARTESIAN_POINT('Ctrl Pts',(-4.68433692682069,72.0941514461287,
12.));
#158837=CARTESIAN_POINT('Ctrl Pts',(-4.69139991965284,72.0707346476213,
0.));
#158838=CARTESIAN_POINT('Ctrl Pts',(-4.69139991965284,72.0707346476213,
12.));
#158839=CARTESIAN_POINT('Ctrl Pts',(-4.69842835259992,72.0473506595318,
0.));
#158840=CARTESIAN_POINT('Ctrl Pts',(-4.69842835259992,72.0473506595318,
12.));
#158841=CARTESIAN_POINT('Ctrl Pts',(-4.70542224912301,72.0239996086686,
0.));
#158842=CARTESIAN_POINT('Ctrl Pts',(-4.70542224912301,72.0239996086686,
12.));
#158843=CARTESIAN_POINT('Ctrl Pts',(-4.71238163287397,72.0006816223325,
0.));
#158844=CARTESIAN_POINT('Ctrl Pts',(-4.71238163287397,72.0006816223325,
12.));
#158845=CARTESIAN_POINT('Ctrl Pts',(-4.7193065276907,71.9773968283259,0.));
#158846=CARTESIAN_POINT('Ctrl Pts',(-4.7193065276907,71.9773968283259,12.));
#158847=CARTESIAN_POINT('Ctrl Pts',(-4.72619695759774,71.9541453549579,
0.));
#158848=CARTESIAN_POINT('Ctrl Pts',(-4.72619695759774,71.9541453549579,
12.));
#158849=CARTESIAN_POINT('Ctrl Pts',(-4.73305294680785,71.9309273310471,
0.));
#158850=CARTESIAN_POINT('Ctrl Pts',(-4.73305294680785,71.9309273310471,
12.));
#158851=CARTESIAN_POINT('Ctrl Pts',(-4.73987451972864,71.9077428859212,
0.));
#158852=CARTESIAN_POINT('Ctrl Pts',(-4.73987451972864,71.9077428859212,
12.));
#158853=CARTESIAN_POINT('Ctrl Pts',(-4.74666170096547,71.8845921494189,
0.));
#158854=CARTESIAN_POINT('Ctrl Pts',(-4.74666170096547,71.8845921494189,
12.));
#158855=CARTESIAN_POINT('Ctrl Pts',(-4.7534145153167,71.8614752519008,0.));
#158856=CARTESIAN_POINT('Ctrl Pts',(-4.7534145153167,71.8614752519008,12.));
#158857=CARTESIAN_POINT('Ctrl Pts',(-4.7601329877742,71.8383923242531,0.));
#158858=CARTESIAN_POINT('Ctrl Pts',(-4.7601329877742,71.8383923242531,12.));
#158859=CARTESIAN_POINT('Ctrl Pts',(-4.76681714352502,71.8153434978923,
0.));
#158860=CARTESIAN_POINT('Ctrl Pts',(-4.76681714352502,71.8153434978923,
12.));
#158861=CARTESIAN_POINT('Ctrl Pts',(-4.77346700795792,71.7923289047643,
0.));
#158862=CARTESIAN_POINT('Ctrl Pts',(-4.77346700795792,71.7923289047643,
12.));
#158863=CARTESIAN_POINT('Ctrl Pts',(-4.7800826066665,71.769348677346,0.));
#158864=CARTESIAN_POINT('Ctrl Pts',(-4.7800826066665,71.769348677346,12.));
#158865=CARTESIAN_POINT('Ctrl Pts',(-4.78666396544458,71.7464029486563,
0.));
#158866=CARTESIAN_POINT('Ctrl Pts',(-4.78666396544458,71.7464029486563,
12.));
#158867=CARTESIAN_POINT('Ctrl Pts',(-4.79321111028676,71.723491852261,0.));
#158868=CARTESIAN_POINT('Ctrl Pts',(-4.79321111028676,71.723491852261,12.));
#158869=CARTESIAN_POINT('Ctrl Pts',(-4.79972406739011,71.7006155222764,
0.));
#158870=CARTESIAN_POINT('Ctrl Pts',(-4.79972406739011,71.7006155222764,
12.));
#158871=CARTESIAN_POINT('Ctrl Pts',(-4.80620286316075,71.6777740933687,
0.));
#158872=CARTESIAN_POINT('Ctrl Pts',(-4.80620286316075,71.6777740933687,
12.));
#158873=CARTESIAN_POINT('Ctrl Pts',(-4.81264752421713,71.6549677007582,
0.));
#158874=CARTESIAN_POINT('Ctrl Pts',(-4.81264752421713,71.6549677007582,
12.));
#158875=CARTESIAN_POINT('Ctrl Pts',(-4.81905807738542,71.6321964802297,
0.));
#158876=CARTESIAN_POINT('Ctrl Pts',(-4.81905807738542,71.6321964802297,
12.));
#158877=CARTESIAN_POINT('Ctrl Pts',(-4.82543454970021,71.6094605681353,
0.));
#158878=CARTESIAN_POINT('Ctrl Pts',(-4.82543454970021,71.6094605681353,
12.));
#158879=CARTESIAN_POINT('Ctrl Pts',(-4.8317769684064,71.5867601014008,0.));
#158880=CARTESIAN_POINT('Ctrl Pts',(-4.8317769684064,71.5867601014008,12.));
#158881=CARTESIAN_POINT('Ctrl Pts',(-4.83808536096589,71.5640952175239,
0.));
#158882=CARTESIAN_POINT('Ctrl Pts',(-4.83808536096589,71.5640952175239,
12.));
#158883=CARTESIAN_POINT('Ctrl Pts',(-4.84435975506056,71.5414660545778,
0.));
#158884=CARTESIAN_POINT('Ctrl Pts',(-4.84435975506056,71.5414660545778,
12.));
#158885=CARTESIAN_POINT('Ctrl Pts',(-4.85060017858786,71.5188727512231,
0.));
#158886=CARTESIAN_POINT('Ctrl Pts',(-4.85060017858786,71.5188727512231,
12.));
#158887=CARTESIAN_POINT('Ctrl Pts',(-4.85680665966184,71.4963154467128,
0.));
#158888=CARTESIAN_POINT('Ctrl Pts',(-4.85680665966184,71.4963154467128,
12.));
#158889=CARTESIAN_POINT('Ctrl Pts',(-4.86297922661499,71.4737942808971,
0.));
#158890=CARTESIAN_POINT('Ctrl Pts',(-4.86297922661499,71.4737942808971,
12.));
#158891=CARTESIAN_POINT('Ctrl Pts',(-4.86911790800533,71.4513093942216,
0.));
#158892=CARTESIAN_POINT('Ctrl Pts',(-4.86911790800533,71.4513093942216,
12.));
#158893=CARTESIAN_POINT('Ctrl Pts',(-4.87522273261881,71.4288609277324,
0.));
#158894=CARTESIAN_POINT('Ctrl Pts',(-4.87522273261881,71.4288609277324,
12.));
#158895=CARTESIAN_POINT('Ctrl Pts',(-4.88129372946524,71.4064490230857,
0.));
#158896=CARTESIAN_POINT('Ctrl Pts',(-4.88129372946524,71.4064490230857,
12.));
#158897=CARTESIAN_POINT('Ctrl Pts',(-4.88733092777964,71.3840738225547,
0.));
#158898=CARTESIAN_POINT('Ctrl Pts',(-4.88733092777964,71.3840738225547,
12.));
#158899=CARTESIAN_POINT('Ctrl Pts',(-4.89333435702424,71.3617354690342,
0.));
#158900=CARTESIAN_POINT('Ctrl Pts',(-4.89333435702424,71.3617354690342,
12.));
#158901=CARTESIAN_POINT('Ctrl Pts',(-4.89930404689599,71.3394341060396,
0.));
#158902=CARTESIAN_POINT('Ctrl Pts',(-4.89930404689599,71.3394341060396,
12.));
#158903=CARTESIAN_POINT('Ctrl Pts',(-4.90524002732806,71.3171698777124,
0.));
#158904=CARTESIAN_POINT('Ctrl Pts',(-4.90524002732806,71.3171698777124,
12.));
#158905=CARTESIAN_POINT('Ctrl Pts',(-4.91114232848623,71.2949429288319,
0.));
#158906=CARTESIAN_POINT('Ctrl Pts',(-4.91114232848623,71.2949429288319,
12.));
#158907=CARTESIAN_POINT('Ctrl Pts',(-4.91701098077041,71.27275340482,0.));
#158908=CARTESIAN_POINT('Ctrl Pts',(-4.91701098077041,71.27275340482,12.));
#158909=CARTESIAN_POINT('Ctrl Pts',(-4.9228460148171,71.2506014517457,0.));
#158910=CARTESIAN_POINT('Ctrl Pts',(-4.9228460148171,71.2506014517457,12.));
#158911=CARTESIAN_POINT('Ctrl Pts',(-4.92864746150711,71.2284872163248,
0.));
#158912=CARTESIAN_POINT('Ctrl Pts',(-4.92864746150711,71.2284872163248,
12.));
#158913=CARTESIAN_POINT('Ctrl Pts',(-4.93441535196594,71.206410845926,0.));
#158914=CARTESIAN_POINT('Ctrl Pts',(-4.93441535196594,71.206410845926,12.));
#158915=CARTESIAN_POINT('Ctrl Pts',(-4.94014971756097,71.184372488583,0.));
#158916=CARTESIAN_POINT('Ctrl Pts',(-4.94014971756097,71.184372488583,12.));
#158917=CARTESIAN_POINT('Ctrl Pts',(-4.94585058990337,71.1623722929998,
0.));
#158918=CARTESIAN_POINT('Ctrl Pts',(-4.94585058990337,71.1623722929998,
12.));
#158919=CARTESIAN_POINT('Ctrl Pts',(-4.95151800085111,71.1404104085561,
0.));
#158920=CARTESIAN_POINT('Ctrl Pts',(-4.95151800085111,71.1404104085561,
12.));
#158921=CARTESIAN_POINT('Ctrl Pts',(-4.95715198251704,71.1184869853071,
0.));
#158922=CARTESIAN_POINT('Ctrl Pts',(-4.95715198251704,71.1184869853071,
12.));
#158923=CARTESIAN_POINT('Ctrl Pts',(-4.96275256726787,71.0966021739922,
0.));
#158924=CARTESIAN_POINT('Ctrl Pts',(-4.96275256726787,71.0966021739922,
12.));
#158925=CARTESIAN_POINT('Ctrl Pts',(-4.96831978772201,71.0747561260443,
0.));
#158926=CARTESIAN_POINT('Ctrl Pts',(-4.96831978772201,71.0747561260443,
12.));
#158927=CARTESIAN_POINT('Ctrl Pts',(-4.97385367675157,71.0529489935959,
0.));
#158928=CARTESIAN_POINT('Ctrl Pts',(-4.97385367675157,71.0529489935959,
12.));
#158929=CARTESIAN_POINT('Ctrl Pts',(-4.97935426748577,71.031180929482,0.));
#158930=CARTESIAN_POINT('Ctrl Pts',(-4.97935426748577,71.031180929482,12.));
#158931=CARTESIAN_POINT('Ctrl Pts',(-4.98482159331851,71.0094520872375,
0.));
#158932=CARTESIAN_POINT('Ctrl Pts',(-4.98482159331851,71.0094520872375,
12.));
#158933=CARTESIAN_POINT('Ctrl Pts',(-4.99025568790653,70.9877626211112,
0.));
#158934=CARTESIAN_POINT('Ctrl Pts',(-4.99025568790653,70.9877626211112,
12.));
#158935=CARTESIAN_POINT('Ctrl Pts',(-4.99565658516906,70.9661126860773,
0.));
#158936=CARTESIAN_POINT('Ctrl Pts',(-4.99565658516906,70.9661126860773,
12.));
#158937=CARTESIAN_POINT('Ctrl Pts',(-5.00102431929039,70.9445024378439,
0.));
#158938=CARTESIAN_POINT('Ctrl Pts',(-5.00102431929039,70.9445024378439,
12.));
#158939=CARTESIAN_POINT('Ctrl Pts',(-5.00635892472518,70.9229320328588,
0.));
#158940=CARTESIAN_POINT('Ctrl Pts',(-5.00635892472518,70.9229320328588,
12.));
#158941=CARTESIAN_POINT('Ctrl Pts',(-5.01166043620573,70.9014016283123,
0.));
#158942=CARTESIAN_POINT('Ctrl Pts',(-5.01166043620573,70.9014016283123,
12.));
#158943=CARTESIAN_POINT('Ctrl Pts',(-5.01692888873793,70.8799113821449,
0.));
#158944=CARTESIAN_POINT('Ctrl Pts',(-5.01692888873793,70.8799113821449,
12.));
#158945=CARTESIAN_POINT('Ctrl Pts',(-5.0221643176006,70.8584614530517,0.));
#158946=CARTESIAN_POINT('Ctrl Pts',(-5.0221643176006,70.8584614530517,12.));
#158947=CARTESIAN_POINT('Ctrl Pts',(-5.02736675834691,70.8370520004844,
0.));
#158948=CARTESIAN_POINT('Ctrl Pts',(-5.02736675834691,70.8370520004844,
12.));
#158949=CARTESIAN_POINT('Ctrl Pts',(-5.03253624680941,70.8156831846494,
0.));
#158950=CARTESIAN_POINT('Ctrl Pts',(-5.03253624680941,70.8156831846494,
12.));
#158951=CARTESIAN_POINT('Ctrl Pts',(-5.03767281910483,70.7943551665071,
0.));
#158952=CARTESIAN_POINT('Ctrl Pts',(-5.03767281910483,70.7943551665071,
12.));
#158953=CARTESIAN_POINT('Ctrl Pts',(-5.04277651163356,70.7730681077997,
0.));
#158954=CARTESIAN_POINT('Ctrl Pts',(-5.04277651163356,70.7730681077997,
12.));
#158955=CARTESIAN_POINT('Ctrl Pts',(-5.04784736108351,70.7518221710715,
0.));
#158956=CARTESIAN_POINT('Ctrl Pts',(-5.04784736108351,70.7518221710715,
12.));
#158957=CARTESIAN_POINT('Ctrl Pts',(-5.05288540443478,70.7306175196856,
0.));
#158958=CARTESIAN_POINT('Ctrl Pts',(-5.05288540443478,70.7306175196856,
12.));
#158959=CARTESIAN_POINT('Ctrl Pts',(-5.05789067897041,70.7094543178416,
0.));
#158960=CARTESIAN_POINT('Ctrl Pts',(-5.05789067897041,70.7094543178416,
12.));
#158961=CARTESIAN_POINT('Ctrl Pts',(-5.06286322227797,70.6883327305755,
0.));
#158962=CARTESIAN_POINT('Ctrl Pts',(-5.06286322227797,70.6883327305755,
12.));
#158963=CARTESIAN_POINT('Ctrl Pts',(-5.06780307224053,70.6672529237431,
0.));
#158964=CARTESIAN_POINT('Ctrl Pts',(-5.06780307224053,70.6672529237431,
12.));
#158965=CARTESIAN_POINT('Ctrl Pts',(-5.0727102670335,70.6462150640009,0.));
#158966=CARTESIAN_POINT('Ctrl Pts',(-5.0727102670335,70.6462150640009,12.));
#158967=CARTESIAN_POINT('Ctrl Pts',(-5.0775848451231,70.6252193187892,0.));
#158968=CARTESIAN_POINT('Ctrl Pts',(-5.0775848451231,70.6252193187892,12.));
#158969=CARTESIAN_POINT('Ctrl Pts',(-5.08242684526704,70.6042658562951,
0.));
#158970=CARTESIAN_POINT('Ctrl Pts',(-5.08242684526704,70.6042658562951,
12.));
#158971=CARTESIAN_POINT('Ctrl Pts',(-5.08723630652291,70.5833548455043,
0.));
#158972=CARTESIAN_POINT('Ctrl Pts',(-5.08723630652291,70.5833548455043,
12.));
#158973=CARTESIAN_POINT('Ctrl Pts',(-5.09201326826146,70.5624864562841,
0.));
#158974=CARTESIAN_POINT('Ctrl Pts',(-5.09201326826146,70.5624864562841,
12.));
#158975=CARTESIAN_POINT('Ctrl Pts',(-5.09675777018182,70.5416608594526,
0.));
#158976=CARTESIAN_POINT('Ctrl Pts',(-5.09675777018182,70.5416608594526,
12.));
#158977=CARTESIAN_POINT('Ctrl Pts',(-5.10146985232928,70.5208782268482,
0.));
#158978=CARTESIAN_POINT('Ctrl Pts',(-5.10146985232928,70.5208782268482,
12.));
#158979=CARTESIAN_POINT('Ctrl Pts',(-5.10614955511643,70.5001387313963,
0.));
#158980=CARTESIAN_POINT('Ctrl Pts',(-5.10614955511643,70.5001387313963,
12.));
#158981=CARTESIAN_POINT('Ctrl Pts',(-5.11079691929193,70.4794425469799,
0.));
#158982=CARTESIAN_POINT('Ctrl Pts',(-5.11079691929193,70.4794425469799,
12.));
#158983=CARTESIAN_POINT('Ctrl Pts',(-5.1154119859092,70.4587898482946,0.));
#158984=CARTESIAN_POINT('Ctrl Pts',(-5.1154119859092,70.4587898482946,12.));
#158985=CARTESIAN_POINT('Ctrl Pts',(-5.11999479630215,70.438180810725,0.));
#158986=CARTESIAN_POINT('Ctrl Pts',(-5.11999479630215,70.438180810725,12.));
#158987=CARTESIAN_POINT('Ctrl Pts',(-5.12454539205347,70.4176156101633,
0.));
#158988=CARTESIAN_POINT('Ctrl Pts',(-5.12454539205347,70.4176156101633,
12.));
#158989=CARTESIAN_POINT('Ctrl Pts',(-5.12906381499486,70.3970944229885,
0.));
#158990=CARTESIAN_POINT('Ctrl Pts',(-5.12906381499486,70.3970944229885,
12.));
#158991=CARTESIAN_POINT('Ctrl Pts',(-5.13355010728591,70.3766174264786,
0.));
#158992=CARTESIAN_POINT('Ctrl Pts',(-5.13355010728591,70.3766174264786,
12.));
#158993=CARTESIAN_POINT('Ctrl Pts',(-5.13800431148911,70.3561847991725,
0.));
#158994=CARTESIAN_POINT('Ctrl Pts',(-5.13800431148911,70.3561847991725,
12.));
#158995=CARTESIAN_POINT('Ctrl Pts',(-5.14242647063467,70.3357967211782,
0.));
#158996=CARTESIAN_POINT('Ctrl Pts',(-5.14242647063467,70.3357967211782,
12.));
#158997=CARTESIAN_POINT('Ctrl Pts',(-5.14681662833054,70.31545337467,0.));
#158998=CARTESIAN_POINT('Ctrl Pts',(-5.14681662833054,70.31545337467,12.));
#158999=CARTESIAN_POINT('Ctrl Pts',(-5.15117482869224,70.2951549435469,
0.));
#159000=CARTESIAN_POINT('Ctrl Pts',(-5.15117482869224,70.2951549435469,
12.));
#159001=CARTESIAN_POINT('Ctrl Pts',(-5.15550111614838,70.2749016125073,
0.));
#159002=CARTESIAN_POINT('Ctrl Pts',(-5.15550111614838,70.2749016125073,
12.));
#159003=CARTESIAN_POINT('Ctrl Pts',(-5.159795535282,70.2546935662719,0.));
#159004=CARTESIAN_POINT('Ctrl Pts',(-5.159795535282,70.2546935662719,12.));
#159005=CARTESIAN_POINT('Ctrl Pts',(-5.16405813066994,70.2345309887864,
0.));
#159006=CARTESIAN_POINT('Ctrl Pts',(-5.16405813066994,70.2345309887864,
12.));
#159007=CARTESIAN_POINT('Ctrl Pts',(-5.1682889467014,70.2144140623004,0.));
#159008=CARTESIAN_POINT('Ctrl Pts',(-5.1682889467014,70.2144140623004,12.));
#159009=CARTESIAN_POINT('Ctrl Pts',(-5.1724880279342,70.1943429691214,0.));
#159010=CARTESIAN_POINT('Ctrl Pts',(-5.1724880279342,70.1943429691214,12.));
#159011=CARTESIAN_POINT('Ctrl Pts',(-5.176655419524,70.1743178937102,0.));
#159012=CARTESIAN_POINT('Ctrl Pts',(-5.176655419524,70.1743178937102,12.));
#159013=CARTESIAN_POINT('Ctrl Pts',(-5.18079116757659,70.1543390243882,
0.));
#159014=CARTESIAN_POINT('Ctrl Pts',(-5.18079116757659,70.1543390243882,
12.));
#159015=CARTESIAN_POINT('Ctrl Pts',(-5.18489531966234,70.1344065558106,
0.));
#159016=CARTESIAN_POINT('Ctrl Pts',(-5.18489531966234,70.1344065558106,
12.));
#159017=CARTESIAN_POINT('Ctrl Pts',(-5.18896792486523,70.1145206891833,
0.));
#159018=CARTESIAN_POINT('Ctrl Pts',(-5.18896792486523,70.1145206891833,
12.));
#159019=CARTESIAN_POINT('Ctrl Pts',(-5.19300903271544,70.0946816270957,
0.));
#159020=CARTESIAN_POINT('Ctrl Pts',(-5.19300903271544,70.0946816270957,
12.));
#159021=CARTESIAN_POINT('Ctrl Pts',(-5.19701869225514,70.0748895689716,
0.));
#159022=CARTESIAN_POINT('Ctrl Pts',(-5.19701869225514,70.0748895689716,
12.));
#159023=CARTESIAN_POINT('Ctrl Pts',(-5.20099695122677,70.0551447071106,
0.));
#159024=CARTESIAN_POINT('Ctrl Pts',(-5.20099695122677,70.0551447071106,
12.));
#159025=CARTESIAN_POINT('Ctrl Pts',(-5.20494385478083,70.0354472203604,
0.));
#159026=CARTESIAN_POINT('Ctrl Pts',(-5.20494385478083,70.0354472203604,
12.));
#159027=CARTESIAN_POINT('Ctrl Pts',(-5.20885944672914,70.0157972802255,
0.));
#159028=CARTESIAN_POINT('Ctrl Pts',(-5.20885944672914,70.0157972802255,
12.));
#159029=CARTESIAN_POINT('Ctrl Pts',(-5.21274377203321,69.996195063002,0.));
#159030=CARTESIAN_POINT('Ctrl Pts',(-5.21274377203321,69.996195063002,12.));
#159031=CARTESIAN_POINT('Ctrl Pts',(-5.21659687881139,69.9766407595385,
0.));
#159032=CARTESIAN_POINT('Ctrl Pts',(-5.21659687881139,69.9766407595385,
12.));
#159033=CARTESIAN_POINT('Ctrl Pts',(-5.22041882075627,69.9571345869996,
0.));
#159034=CARTESIAN_POINT('Ctrl Pts',(-5.22041882075627,69.9571345869996,
12.));
#159035=CARTESIAN_POINT('Ctrl Pts',(-5.22420965879808,69.9376767968951,
0.));
#159036=CARTESIAN_POINT('Ctrl Pts',(-5.22420965879808,69.9376767968951,
12.));
#159037=CARTESIAN_POINT('Ctrl Pts',(-5.22796945602603,69.9182676501892,
0.));
#159038=CARTESIAN_POINT('Ctrl Pts',(-5.22796945602603,69.9182676501892,
12.));
#159039=CARTESIAN_POINT('Ctrl Pts',(-5.23169827290452,69.8989073936606,
0.));
#159040=CARTESIAN_POINT('Ctrl Pts',(-5.23169827290452,69.8989073936606,
12.));
#159041=CARTESIAN_POINT('Ctrl Pts',(-5.23539616279715,69.8795962381676,
0.));
#159042=CARTESIAN_POINT('Ctrl Pts',(-5.23539616279715,69.8795962381676,
12.));
#159043=CARTESIAN_POINT('Ctrl Pts',(-5.23906316635141,69.8603343303016,
0.));
#159044=CARTESIAN_POINT('Ctrl Pts',(-5.23906316635141,69.8603343303016,
12.));
#159045=CARTESIAN_POINT('Ctrl Pts',(-5.24269931055075,69.8411217507931,
0.));
#159046=CARTESIAN_POINT('Ctrl Pts',(-5.24269931055075,69.8411217507931,
12.));
#159047=CARTESIAN_POINT('Ctrl Pts',(-5.2455835516022,69.8257911792542,0.));
#159048=CARTESIAN_POINT('Ctrl Pts',(-5.2455835516022,69.8257911792542,12.));
#159049=CARTESIAN_POINT('Ctrl Pts',(-5.24773285666673,69.8143154684447,
0.));
#159050=CARTESIAN_POINT('Ctrl Pts',(-5.24773285666673,69.8143154684447,
12.));
#159051=CARTESIAN_POINT('Ctrl Pts',(-5.24915955997537,69.8066748687863,
0.));
#159052=CARTESIAN_POINT('Ctrl Pts',(-5.24915955997537,69.8066748687863,
12.));
#159053=CARTESIAN_POINT('Ctrl Pts',(-5.24987136994591,69.8028570375098,
0.));
#159054=CARTESIAN_POINT('Ctrl Pts',(-5.24987136994591,69.8028570375098,
12.));
#159055=CARTESIAN_POINT('',(-5.24987136994591,69.8028570375098,12.));
#159056=CARTESIAN_POINT('Ctrl Pts',(-5.24987136994591,69.8028570375098,
12.));
#159057=CARTESIAN_POINT('Ctrl Pts',(-5.24915955997537,69.8066748687863,
12.));
#159058=CARTESIAN_POINT('Ctrl Pts',(-5.24773285666673,69.8143154684447,
12.));
#159059=CARTESIAN_POINT('Ctrl Pts',(-5.2455835516022,69.8257911792542,12.));
#159060=CARTESIAN_POINT('Ctrl Pts',(-5.24269931055075,69.8411217507931,
12.));
#159061=CARTESIAN_POINT('Ctrl Pts',(-5.23906316635141,69.8603343303016,
12.));
#159062=CARTESIAN_POINT('Ctrl Pts',(-5.23539616279715,69.8795962381676,
12.));
#159063=CARTESIAN_POINT('Ctrl Pts',(-5.23169827290452,69.8989073936606,
12.));
#159064=CARTESIAN_POINT('Ctrl Pts',(-5.22796945602603,69.9182676501892,
12.));
#159065=CARTESIAN_POINT('Ctrl Pts',(-5.22420965879808,69.9376767968951,
12.));
#159066=CARTESIAN_POINT('Ctrl Pts',(-5.22041882075627,69.9571345869996,
12.));
#159067=CARTESIAN_POINT('Ctrl Pts',(-5.21659687881139,69.9766407595385,
12.));
#159068=CARTESIAN_POINT('Ctrl Pts',(-5.21274377203321,69.996195063002,12.));
#159069=CARTESIAN_POINT('Ctrl Pts',(-5.20885944672914,70.0157972802255,
12.));
#159070=CARTESIAN_POINT('Ctrl Pts',(-5.20494385478083,70.0354472203604,
12.));
#159071=CARTESIAN_POINT('Ctrl Pts',(-5.20099695122677,70.0551447071106,
12.));
#159072=CARTESIAN_POINT('Ctrl Pts',(-5.19701869225514,70.0748895689716,
12.));
#159073=CARTESIAN_POINT('Ctrl Pts',(-5.19300903271544,70.0946816270957,
12.));
#159074=CARTESIAN_POINT('Ctrl Pts',(-5.18896792486523,70.1145206891833,
12.));
#159075=CARTESIAN_POINT('Ctrl Pts',(-5.18489531966234,70.1344065558106,
12.));
#159076=CARTESIAN_POINT('Ctrl Pts',(-5.18079116757659,70.1543390243882,
12.));
#159077=CARTESIAN_POINT('Ctrl Pts',(-5.176655419524,70.1743178937102,12.));
#159078=CARTESIAN_POINT('Ctrl Pts',(-5.1724880279342,70.1943429691214,12.));
#159079=CARTESIAN_POINT('Ctrl Pts',(-5.1682889467014,70.2144140623004,12.));
#159080=CARTESIAN_POINT('Ctrl Pts',(-5.16405813066994,70.2345309887864,
12.));
#159081=CARTESIAN_POINT('Ctrl Pts',(-5.159795535282,70.2546935662719,12.));
#159082=CARTESIAN_POINT('Ctrl Pts',(-5.15550111614838,70.2749016125073,
12.));
#159083=CARTESIAN_POINT('Ctrl Pts',(-5.15117482869224,70.2951549435469,
12.));
#159084=CARTESIAN_POINT('Ctrl Pts',(-5.14681662833054,70.31545337467,12.));
#159085=CARTESIAN_POINT('Ctrl Pts',(-5.14242647063467,70.3357967211782,
12.));
#159086=CARTESIAN_POINT('Ctrl Pts',(-5.13800431148911,70.3561847991725,
12.));
#159087=CARTESIAN_POINT('Ctrl Pts',(-5.13355010728591,70.3766174264786,
12.));
#159088=CARTESIAN_POINT('Ctrl Pts',(-5.12906381499486,70.3970944229885,
12.));
#159089=CARTESIAN_POINT('Ctrl Pts',(-5.12454539205347,70.4176156101633,
12.));
#159090=CARTESIAN_POINT('Ctrl Pts',(-5.11999479630215,70.438180810725,12.));
#159091=CARTESIAN_POINT('Ctrl Pts',(-5.1154119859092,70.4587898482946,12.));
#159092=CARTESIAN_POINT('Ctrl Pts',(-5.11079691929193,70.4794425469799,
12.));
#159093=CARTESIAN_POINT('Ctrl Pts',(-5.10614955511643,70.5001387313963,
12.));
#159094=CARTESIAN_POINT('Ctrl Pts',(-5.10146985232928,70.5208782268482,
12.));
#159095=CARTESIAN_POINT('Ctrl Pts',(-5.09675777018182,70.5416608594526,
12.));
#159096=CARTESIAN_POINT('Ctrl Pts',(-5.09201326826146,70.5624864562841,
12.));
#159097=CARTESIAN_POINT('Ctrl Pts',(-5.08723630652291,70.5833548455043,
12.));
#159098=CARTESIAN_POINT('Ctrl Pts',(-5.08242684526704,70.6042658562951,
12.));
#159099=CARTESIAN_POINT('Ctrl Pts',(-5.0775848451231,70.6252193187892,12.));
#159100=CARTESIAN_POINT('Ctrl Pts',(-5.0727102670335,70.6462150640009,12.));
#159101=CARTESIAN_POINT('Ctrl Pts',(-5.06780307224053,70.6672529237431,
12.));
#159102=CARTESIAN_POINT('Ctrl Pts',(-5.06286322227797,70.6883327305755,
12.));
#159103=CARTESIAN_POINT('Ctrl Pts',(-5.05789067897041,70.7094543178416,
12.));
#159104=CARTESIAN_POINT('Ctrl Pts',(-5.05288540443478,70.7306175196856,
12.));
#159105=CARTESIAN_POINT('Ctrl Pts',(-5.04784736108351,70.7518221710715,
12.));
#159106=CARTESIAN_POINT('Ctrl Pts',(-5.04277651163356,70.7730681077997,
12.));
#159107=CARTESIAN_POINT('Ctrl Pts',(-5.03767281910483,70.7943551665071,
12.));
#159108=CARTESIAN_POINT('Ctrl Pts',(-5.03253624680941,70.8156831846494,
12.));
#159109=CARTESIAN_POINT('Ctrl Pts',(-5.02736675834691,70.8370520004844,
12.));
#159110=CARTESIAN_POINT('Ctrl Pts',(-5.0221643176006,70.8584614530517,12.));
#159111=CARTESIAN_POINT('Ctrl Pts',(-5.01692888873793,70.8799113821449,
12.));
#159112=CARTESIAN_POINT('Ctrl Pts',(-5.01166043620573,70.9014016283123,
12.));
#159113=CARTESIAN_POINT('Ctrl Pts',(-5.00635892472518,70.9229320328588,
12.));
#159114=CARTESIAN_POINT('Ctrl Pts',(-5.00102431929039,70.9445024378439,
12.));
#159115=CARTESIAN_POINT('Ctrl Pts',(-4.99565658516906,70.9661126860773,
12.));
#159116=CARTESIAN_POINT('Ctrl Pts',(-4.99025568790653,70.9877626211112,
12.));
#159117=CARTESIAN_POINT('Ctrl Pts',(-4.98482159331851,71.0094520872375,
12.));
#159118=CARTESIAN_POINT('Ctrl Pts',(-4.97935426748577,71.031180929482,12.));
#159119=CARTESIAN_POINT('Ctrl Pts',(-4.97385367675157,71.0529489935959,
12.));
#159120=CARTESIAN_POINT('Ctrl Pts',(-4.96831978772201,71.0747561260443,
12.));
#159121=CARTESIAN_POINT('Ctrl Pts',(-4.96275256726787,71.0966021739922,
12.));
#159122=CARTESIAN_POINT('Ctrl Pts',(-4.95715198251704,71.1184869853071,
12.));
#159123=CARTESIAN_POINT('Ctrl Pts',(-4.95151800085111,71.1404104085561,
12.));
#159124=CARTESIAN_POINT('Ctrl Pts',(-4.94585058990337,71.1623722929998,
12.));
#159125=CARTESIAN_POINT('Ctrl Pts',(-4.94014971756097,71.184372488583,12.));
#159126=CARTESIAN_POINT('Ctrl Pts',(-4.93441535196594,71.206410845926,12.));
#159127=CARTESIAN_POINT('Ctrl Pts',(-4.92864746150711,71.2284872163248,
12.));
#159128=CARTESIAN_POINT('Ctrl Pts',(-4.9228460148171,71.2506014517457,12.));
#159129=CARTESIAN_POINT('Ctrl Pts',(-4.91701098077041,71.27275340482,12.));
#159130=CARTESIAN_POINT('Ctrl Pts',(-4.91114232848623,71.2949429288319,
12.));
#159131=CARTESIAN_POINT('Ctrl Pts',(-4.90524002732806,71.3171698777124,
12.));
#159132=CARTESIAN_POINT('Ctrl Pts',(-4.89930404689599,71.3394341060396,
12.));
#159133=CARTESIAN_POINT('Ctrl Pts',(-4.89333435702424,71.3617354690342,
12.));
#159134=CARTESIAN_POINT('Ctrl Pts',(-4.88733092777964,71.3840738225547,
12.));
#159135=CARTESIAN_POINT('Ctrl Pts',(-4.88129372946524,71.4064490230857,
12.));
#159136=CARTESIAN_POINT('Ctrl Pts',(-4.87522273261881,71.4288609277324,
12.));
#159137=CARTESIAN_POINT('Ctrl Pts',(-4.86911790800533,71.4513093942216,
12.));
#159138=CARTESIAN_POINT('Ctrl Pts',(-4.86297922661499,71.4737942808971,
12.));
#159139=CARTESIAN_POINT('Ctrl Pts',(-4.85680665966184,71.4963154467128,
12.));
#159140=CARTESIAN_POINT('Ctrl Pts',(-4.85060017858786,71.5188727512231,
12.));
#159141=CARTESIAN_POINT('Ctrl Pts',(-4.84435975506056,71.5414660545778,
12.));
#159142=CARTESIAN_POINT('Ctrl Pts',(-4.83808536096589,71.5640952175239,
12.));
#159143=CARTESIAN_POINT('Ctrl Pts',(-4.8317769684064,71.5867601014008,12.));
#159144=CARTESIAN_POINT('Ctrl Pts',(-4.82543454970021,71.6094605681353,
12.));
#159145=CARTESIAN_POINT('Ctrl Pts',(-4.81905807738542,71.6321964802297,
12.));
#159146=CARTESIAN_POINT('Ctrl Pts',(-4.81264752421713,71.6549677007582,
12.));
#159147=CARTESIAN_POINT('Ctrl Pts',(-4.80620286316075,71.6777740933687,
12.));
#159148=CARTESIAN_POINT('Ctrl Pts',(-4.79972406739011,71.7006155222764,
12.));
#159149=CARTESIAN_POINT('Ctrl Pts',(-4.79321111028676,71.723491852261,12.));
#159150=CARTESIAN_POINT('Ctrl Pts',(-4.78666396544458,71.7464029486563,
12.));
#159151=CARTESIAN_POINT('Ctrl Pts',(-4.7800826066665,71.769348677346,12.));
#159152=CARTESIAN_POINT('Ctrl Pts',(-4.77346700795792,71.7923289047643,
12.));
#159153=CARTESIAN_POINT('Ctrl Pts',(-4.76681714352502,71.8153434978923,
12.));
#159154=CARTESIAN_POINT('Ctrl Pts',(-4.7601329877742,71.8383923242531,12.));
#159155=CARTESIAN_POINT('Ctrl Pts',(-4.7534145153167,71.8614752519008,12.));
#159156=CARTESIAN_POINT('Ctrl Pts',(-4.74666170096547,71.8845921494189,
12.));
#159157=CARTESIAN_POINT('Ctrl Pts',(-4.73987451972864,71.9077428859212,
12.));
#159158=CARTESIAN_POINT('Ctrl Pts',(-4.73305294680785,71.9309273310471,
12.));
#159159=CARTESIAN_POINT('Ctrl Pts',(-4.72619695759774,71.9541453549579,
12.));
#159160=CARTESIAN_POINT('Ctrl Pts',(-4.7193065276907,71.9773968283259,12.));
#159161=CARTESIAN_POINT('Ctrl Pts',(-4.71238163287397,72.0006816223325,
12.));
#159162=CARTESIAN_POINT('Ctrl Pts',(-4.70542224912301,72.0239996086686,
12.));
#159163=CARTESIAN_POINT('Ctrl Pts',(-4.69842835259992,72.0473506595318,
12.));
#159164=CARTESIAN_POINT('Ctrl Pts',(-4.69139991965284,72.0707346476213,
12.));
#159165=CARTESIAN_POINT('Ctrl Pts',(-4.68433692682069,72.0941514461287,
12.));
#159166=CARTESIAN_POINT('Ctrl Pts',(-4.67723935083095,72.1176009287351,
12.));
#159167=CARTESIAN_POINT('Ctrl Pts',(-4.67010716859285,72.1410829696128,
12.));
#159168=CARTESIAN_POINT('Ctrl Pts',(-4.6629403571957,72.1645974434216,12.));
#159169=CARTESIAN_POINT('Ctrl Pts',(-4.65573889390822,72.1881442253053,
12.));
#159170=CARTESIAN_POINT('Ctrl Pts',(-4.64850275618323,72.2117231908822,
12.));
#159171=CARTESIAN_POINT('Ctrl Pts',(-4.64123192165628,72.2353342162417,
12.));
#159172=CARTESIAN_POINT('Ctrl Pts',(-4.63392636813844,72.2589771779456,
12.));
#159173=CARTESIAN_POINT('Ctrl Pts',(-4.62658607361466,72.2826519530259,
12.));
#159174=CARTESIAN_POINT('Ctrl Pts',(-4.61921101624292,72.3063584189807,
12.));
#159175=CARTESIAN_POINT('Ctrl Pts',(-4.61180117435862,72.3300964537658,
12.));
#159176=CARTESIAN_POINT('Ctrl Pts',(-4.60435652647453,72.3538659357913,
12.));
#159177=CARTESIAN_POINT('Ctrl Pts',(-4.5968770512733,72.3776667439227,12.));
#159178=CARTESIAN_POINT('Ctrl Pts',(-4.58936272760544,72.401498757478,12.));
#159179=CARTESIAN_POINT('Ctrl Pts',(-4.58181353448852,72.4253618562252,
12.));
#159180=CARTESIAN_POINT('Ctrl Pts',(-4.57422945111102,72.4492559203745,
12.));
#159181=CARTESIAN_POINT('Ctrl Pts',(-4.56661045683376,72.4731808305728,
12.));
#159182=CARTESIAN_POINT('Ctrl Pts',(-4.55895653118221,72.4971364679068,
12.));
#159183=CARTESIAN_POINT('Ctrl Pts',(-4.55126765384404,72.5211227139001,
12.));
#159184=CARTESIAN_POINT('Ctrl Pts',(-4.54354380466822,72.5451394505104,
12.));
#159185=CARTESIAN_POINT('Ctrl Pts',(-4.535784963668,72.5691865601223,12.));
#159186=CARTESIAN_POINT('Ctrl Pts',(-4.52799111102392,72.5932639255409,
12.));
#159187=CARTESIAN_POINT('Ctrl Pts',(-4.52016222707638,72.6173714299942,
12.));
#159188=CARTESIAN_POINT('Ctrl Pts',(-4.51229829232264,72.6415089571321,
12.));
#159189=CARTESIAN_POINT('Ctrl Pts',(-4.50439928741604,72.6656763910241,
12.));
#159190=CARTESIAN_POINT('Ctrl Pts',(-4.49646519316813,72.6898736161542,
12.));
#159191=CARTESIAN_POINT('Ctrl Pts',(-4.48849599055337,72.714100517414,12.));
#159192=CARTESIAN_POINT('Ctrl Pts',(-4.48049166070205,72.738356980103,12.));
#159193=CARTESIAN_POINT('Ctrl Pts',(-4.4724521848961,72.7626428899281,12.));
#159194=CARTESIAN_POINT('Ctrl Pts',(-4.46437754456793,72.7869581329994,
12.));
#159195=CARTESIAN_POINT('Ctrl Pts',(-4.45626772130146,72.8113025958262,
12.));
#159196=CARTESIAN_POINT('Ctrl Pts',(-4.44812269683738,72.8356761653069,
12.));
#159197=CARTESIAN_POINT('Ctrl Pts',(-4.43994245306818,72.8600787287318,
12.));
#159198=CARTESIAN_POINT('Ctrl Pts',(-4.43172697203349,72.8845101737855,
12.));
#159199=CARTESIAN_POINT('Ctrl Pts',(-4.42347623591942,72.9089703885462,
12.));
#159200=CARTESIAN_POINT('Ctrl Pts',(-4.41519022705921,72.9334592614829,
12.));
#159201=CARTESIAN_POINT('Ctrl Pts',(-4.40686892793957,72.95797668145,12.));
#159202=CARTESIAN_POINT('Ctrl Pts',(-4.39851232119722,72.9825225376846,
12.));
#159203=CARTESIAN_POINT('Ctrl Pts',(-4.39012038961139,73.007096719804,12.));
#159204=CARTESIAN_POINT('Ctrl Pts',(-4.38169311610151,73.0316991177993,
12.));
#159205=CARTESIAN_POINT('Ctrl Pts',(-4.37323048372607,73.0563296220299,
12.));
#159206=CARTESIAN_POINT('Ctrl Pts',(-4.36473247568641,73.0809881232103,
12.));
#159207=CARTESIAN_POINT('Ctrl Pts',(-4.3561990753272,73.1056745124087,12.));
#159208=CARTESIAN_POINT('Ctrl Pts',(-4.34763026613158,73.130388681059,12.));
#159209=CARTESIAN_POINT('Ctrl Pts',(-4.33902603172141,73.1551305209685,
12.));
#159210=CARTESIAN_POINT('Ctrl Pts',(-4.33038635585877,73.1798999243235,
12.));
#159211=CARTESIAN_POINT('Ctrl Pts',(-4.32171122245214,73.204696783694,12.));
#159212=CARTESIAN_POINT('Ctrl Pts',(-4.31300061556098,73.2295209920334,
12.));
#159213=CARTESIAN_POINT('Ctrl Pts',(-4.3042545193823,73.2543724426577,12.));
#159214=CARTESIAN_POINT('Ctrl Pts',(-4.29547291824287,73.2792510292254,
12.));
#159215=CARTESIAN_POINT('Ctrl Pts',(-4.28665579659301,73.3041566457135,
12.));
#159216=CARTESIAN_POINT('Ctrl Pts',(-4.2778031390039,73.3290891863949,12.));
#159217=CARTESIAN_POINT('Ctrl Pts',(-4.268914930167,73.3540485458065,12.));
#159218=CARTESIAN_POINT('Ctrl Pts',(-4.25999115489899,73.3790346187938,
12.));
#159219=CARTESIAN_POINT('Ctrl Pts',(-4.25103179814887,73.4040473005592,
12.));
#159220=CARTESIAN_POINT('Ctrl Pts',(-4.24203684500939,73.4290864867101,
12.));
#159221=CARTESIAN_POINT('Ctrl Pts',(-4.23300628072758,73.4541520732948,
12.));
#159222=CARTESIAN_POINT('Ctrl Pts',(-4.22394009072756,73.4792439568633,
12.));
#159223=CARTESIAN_POINT('Ctrl Pts',(-4.21483826059441,73.5043620344116,
12.));
#159224=CARTESIAN_POINT('Ctrl Pts',(-4.2057007760373,73.5295062032628,12.));
#159225=CARTESIAN_POINT('Ctrl Pts',(-4.19652762286127,73.5546763609572,
12.));
#159226=CARTESIAN_POINT('Ctrl Pts',(-4.18731878694236,73.5798724051519,
12.));
#159227=CARTESIAN_POINT('Ctrl Pts',(-4.17807425419813,73.6050942334768,
12.));
#159228=CARTESIAN_POINT('Ctrl Pts',(-4.1687940105878,73.6303417435251,12.));
#159229=CARTESIAN_POINT('Ctrl Pts',(-4.15947804217784,73.6556148331489,
12.));
#159230=CARTESIAN_POINT('Ctrl Pts',(-4.15012633519723,73.6809134006897,
12.));
#159231=CARTESIAN_POINT('Ctrl Pts',(-4.14073887610153,73.7062373452342,
12.));
#159232=CARTESIAN_POINT('Ctrl Pts',(-4.13131565163578,73.7315865668522,
12.));
#159233=CARTESIAN_POINT('Ctrl Pts',(-4.12185664890557,73.7569609668528,
12.));
#159234=CARTESIAN_POINT('Ctrl Pts',(-4.11236185522787,73.7823604472159,
12.));
#159235=CARTESIAN_POINT('Ctrl Pts',(-4.10283125798729,73.8077849100342,
12.));
#159236=CARTESIAN_POINT('Ctrl Pts',(-4.09326484448233,73.8332342568989,
12.));
#159237=CARTESIAN_POINT('Ctrl Pts',(-4.08366260180674,73.8587083884191,
12.));
#159238=CARTESIAN_POINT('Ctrl Pts',(-4.07402451665245,73.8842072034008,
12.));
#159239=CARTESIAN_POINT('Ctrl Pts',(-4.06435057547325,73.9097305995115,
12.));
#159240=CARTESIAN_POINT('Ctrl Pts',(-4.05464076484752,73.9352784747608,
12.));
#159241=CARTESIAN_POINT('Ctrl Pts',(-4.04489507179957,73.9608507287909,
12.));
#159242=CARTESIAN_POINT('Ctrl Pts',(-4.0351134841066,73.9864472641033,12.));
#159243=CARTESIAN_POINT('Ctrl Pts',(-4.02529599070095,74.012067987646,12.));
#159244=CARTESIAN_POINT('Ctrl Pts',(-4.01544258176711,74.0377128111863,
12.));
#159245=CARTESIAN_POINT('Ctrl Pts',(-4.00696550627365,74.0597159782109,
12.));
#159246=CARTESIAN_POINT('Ctrl Pts',(-4.00044689711984,74.0765982943677,
12.));
#159247=CARTESIAN_POINT('Ctrl Pts',(-3.99590266746992,74.0883491449954,
12.));
#159248=CARTESIAN_POINT('Ctrl Pts',(-3.99334334445529,74.0949615399619,
12.));
#159249=CARTESIAN_POINT('Ctrl Pts',(-3.99277406490873,74.0964320766207,
12.));
#159250=CARTESIAN_POINT('',(-5.24987136994591,69.8028570375098,0.));
#159251=CARTESIAN_POINT('',(-5.24987136994591,69.8028570375097,0.));
#159252=CARTESIAN_POINT('Ctrl Pts',(-3.99277406490868,74.0964320766208,
0.));
#159253=CARTESIAN_POINT('Ctrl Pts',(-3.99334334445525,74.094961539962,0.));
#159254=CARTESIAN_POINT('Ctrl Pts',(-3.99590266746989,74.0883491449955,
0.));
#159255=CARTESIAN_POINT('Ctrl Pts',(-4.00044689711982,74.0765982943677,
0.));
#159256=CARTESIAN_POINT('Ctrl Pts',(-4.00696550627364,74.059715978211,0.));
#159257=CARTESIAN_POINT('Ctrl Pts',(-4.01544258176711,74.0377128111863,
0.));
#159258=CARTESIAN_POINT('Ctrl Pts',(-4.02529599070095,74.012067987646,0.));
#159259=CARTESIAN_POINT('Ctrl Pts',(-4.0351134841066,73.9864472641033,0.));
#159260=CARTESIAN_POINT('Ctrl Pts',(-4.04489507179957,73.9608507287909,
0.));
#159261=CARTESIAN_POINT('Ctrl Pts',(-4.05464076484752,73.9352784747608,
0.));
#159262=CARTESIAN_POINT('Ctrl Pts',(-4.06435057547325,73.9097305995115,
0.));
#159263=CARTESIAN_POINT('Ctrl Pts',(-4.07402451665245,73.8842072034008,
0.));
#159264=CARTESIAN_POINT('Ctrl Pts',(-4.08366260180674,73.8587083884191,
0.));
#159265=CARTESIAN_POINT('Ctrl Pts',(-4.09326484448233,73.8332342568989,
0.));
#159266=CARTESIAN_POINT('Ctrl Pts',(-4.10283125798729,73.8077849100342,
0.));
#159267=CARTESIAN_POINT('Ctrl Pts',(-4.11236185522787,73.7823604472159,
0.));
#159268=CARTESIAN_POINT('Ctrl Pts',(-4.12185664890557,73.7569609668528,
0.));
#159269=CARTESIAN_POINT('Ctrl Pts',(-4.13131565163578,73.7315865668522,
0.));
#159270=CARTESIAN_POINT('Ctrl Pts',(-4.14073887610153,73.7062373452342,
0.));
#159271=CARTESIAN_POINT('Ctrl Pts',(-4.15012633519723,73.6809134006897,
0.));
#159272=CARTESIAN_POINT('Ctrl Pts',(-4.15947804217784,73.6556148331489,
0.));
#159273=CARTESIAN_POINT('Ctrl Pts',(-4.1687940105878,73.6303417435251,0.));
#159274=CARTESIAN_POINT('Ctrl Pts',(-4.17807425419813,73.6050942334768,
0.));
#159275=CARTESIAN_POINT('Ctrl Pts',(-4.18731878694236,73.5798724051519,
0.));
#159276=CARTESIAN_POINT('Ctrl Pts',(-4.19652762286127,73.5546763609572,
0.));
#159277=CARTESIAN_POINT('Ctrl Pts',(-4.2057007760373,73.5295062032628,0.));
#159278=CARTESIAN_POINT('Ctrl Pts',(-4.21483826059441,73.5043620344116,
0.));
#159279=CARTESIAN_POINT('Ctrl Pts',(-4.22394009072756,73.4792439568633,
0.));
#159280=CARTESIAN_POINT('Ctrl Pts',(-4.23300628072758,73.4541520732948,
0.));
#159281=CARTESIAN_POINT('Ctrl Pts',(-4.24203684500939,73.4290864867101,
0.));
#159282=CARTESIAN_POINT('Ctrl Pts',(-4.25103179814887,73.4040473005592,
0.));
#159283=CARTESIAN_POINT('Ctrl Pts',(-4.25999115489899,73.3790346187938,
0.));
#159284=CARTESIAN_POINT('Ctrl Pts',(-4.268914930167,73.3540485458065,0.));
#159285=CARTESIAN_POINT('Ctrl Pts',(-4.2778031390039,73.3290891863949,0.));
#159286=CARTESIAN_POINT('Ctrl Pts',(-4.28665579659301,73.3041566457135,
0.));
#159287=CARTESIAN_POINT('Ctrl Pts',(-4.29547291824287,73.2792510292254,
0.));
#159288=CARTESIAN_POINT('Ctrl Pts',(-4.3042545193823,73.2543724426577,0.));
#159289=CARTESIAN_POINT('Ctrl Pts',(-4.31300061556098,73.2295209920334,
0.));
#159290=CARTESIAN_POINT('Ctrl Pts',(-4.32171122245214,73.204696783694,0.));
#159291=CARTESIAN_POINT('Ctrl Pts',(-4.33038635585877,73.1798999243235,
0.));
#159292=CARTESIAN_POINT('Ctrl Pts',(-4.33902603172141,73.1551305209685,
0.));
#159293=CARTESIAN_POINT('Ctrl Pts',(-4.34763026613158,73.130388681059,0.));
#159294=CARTESIAN_POINT('Ctrl Pts',(-4.3561990753272,73.1056745124087,0.));
#159295=CARTESIAN_POINT('Ctrl Pts',(-4.36473247568641,73.0809881232103,
0.));
#159296=CARTESIAN_POINT('Ctrl Pts',(-4.37323048372607,73.0563296220299,
0.));
#159297=CARTESIAN_POINT('Ctrl Pts',(-4.38169311610151,73.0316991177993,
0.));
#159298=CARTESIAN_POINT('Ctrl Pts',(-4.39012038961139,73.007096719804,0.));
#159299=CARTESIAN_POINT('Ctrl Pts',(-4.39851232119722,72.9825225376846,
0.));
#159300=CARTESIAN_POINT('Ctrl Pts',(-4.40686892793957,72.95797668145,0.));
#159301=CARTESIAN_POINT('Ctrl Pts',(-4.41519022705921,72.9334592614829,
0.));
#159302=CARTESIAN_POINT('Ctrl Pts',(-4.42347623591942,72.9089703885462,
0.));
#159303=CARTESIAN_POINT('Ctrl Pts',(-4.43172697203349,72.8845101737855,
0.));
#159304=CARTESIAN_POINT('Ctrl Pts',(-4.43994245306818,72.8600787287318,
0.));
#159305=CARTESIAN_POINT('Ctrl Pts',(-4.44812269683738,72.8356761653069,
0.));
#159306=CARTESIAN_POINT('Ctrl Pts',(-4.45626772130146,72.8113025958262,
0.));
#159307=CARTESIAN_POINT('Ctrl Pts',(-4.46437754456793,72.7869581329994,
0.));
#159308=CARTESIAN_POINT('Ctrl Pts',(-4.4724521848961,72.7626428899281,0.));
#159309=CARTESIAN_POINT('Ctrl Pts',(-4.48049166070205,72.738356980103,0.));
#159310=CARTESIAN_POINT('Ctrl Pts',(-4.48849599055337,72.714100517414,0.));
#159311=CARTESIAN_POINT('Ctrl Pts',(-4.49646519316813,72.6898736161542,
0.));
#159312=CARTESIAN_POINT('Ctrl Pts',(-4.50439928741604,72.6656763910241,
0.));
#159313=CARTESIAN_POINT('Ctrl Pts',(-4.51229829232264,72.6415089571321,
0.));
#159314=CARTESIAN_POINT('Ctrl Pts',(-4.52016222707638,72.6173714299942,
0.));
#159315=CARTESIAN_POINT('Ctrl Pts',(-4.52799111102392,72.5932639255409,
0.));
#159316=CARTESIAN_POINT('Ctrl Pts',(-4.535784963668,72.5691865601223,0.));
#159317=CARTESIAN_POINT('Ctrl Pts',(-4.54354380466822,72.5451394505104,
0.));
#159318=CARTESIAN_POINT('Ctrl Pts',(-4.55126765384404,72.5211227139001,
0.));
#159319=CARTESIAN_POINT('Ctrl Pts',(-4.55895653118221,72.4971364679068,
0.));
#159320=CARTESIAN_POINT('Ctrl Pts',(-4.56661045683376,72.4731808305728,
0.));
#159321=CARTESIAN_POINT('Ctrl Pts',(-4.57422945111102,72.4492559203745,
0.));
#159322=CARTESIAN_POINT('Ctrl Pts',(-4.58181353448852,72.4253618562252,
0.));
#159323=CARTESIAN_POINT('Ctrl Pts',(-4.58936272760544,72.401498757478,0.));
#159324=CARTESIAN_POINT('Ctrl Pts',(-4.5968770512733,72.3776667439227,0.));
#159325=CARTESIAN_POINT('Ctrl Pts',(-4.60435652647453,72.3538659357913,
0.));
#159326=CARTESIAN_POINT('Ctrl Pts',(-4.61180117435862,72.3300964537658,
0.));
#159327=CARTESIAN_POINT('Ctrl Pts',(-4.61921101624292,72.3063584189807,
0.));
#159328=CARTESIAN_POINT('Ctrl Pts',(-4.62658607361466,72.2826519530259,
0.));
#159329=CARTESIAN_POINT('Ctrl Pts',(-4.63392636813844,72.2589771779456,
0.));
#159330=CARTESIAN_POINT('Ctrl Pts',(-4.64123192165628,72.2353342162417,
0.));
#159331=CARTESIAN_POINT('Ctrl Pts',(-4.64850275618323,72.2117231908822,
0.));
#159332=CARTESIAN_POINT('Ctrl Pts',(-4.65573889390822,72.1881442253053,
0.));
#159333=CARTESIAN_POINT('Ctrl Pts',(-4.6629403571957,72.1645974434216,0.));
#159334=CARTESIAN_POINT('Ctrl Pts',(-4.67010716859285,72.1410829696128,
0.));
#159335=CARTESIAN_POINT('Ctrl Pts',(-4.67723935083095,72.1176009287351,
0.));
#159336=CARTESIAN_POINT('Ctrl Pts',(-4.68433692682069,72.0941514461287,
0.));
#159337=CARTESIAN_POINT('Ctrl Pts',(-4.69139991965284,72.0707346476213,
0.));
#159338=CARTESIAN_POINT('Ctrl Pts',(-4.69842835259992,72.0473506595318,
0.));
#159339=CARTESIAN_POINT('Ctrl Pts',(-4.70542224912301,72.0239996086686,
0.));
#159340=CARTESIAN_POINT('Ctrl Pts',(-4.71238163287397,72.0006816223325,
0.));
#159341=CARTESIAN_POINT('Ctrl Pts',(-4.7193065276907,71.9773968283259,0.));
#159342=CARTESIAN_POINT('Ctrl Pts',(-4.72619695759774,71.9541453549579,
0.));
#159343=CARTESIAN_POINT('Ctrl Pts',(-4.73305294680785,71.9309273310471,
0.));
#159344=CARTESIAN_POINT('Ctrl Pts',(-4.73987451972864,71.9077428859212,
0.));
#159345=CARTESIAN_POINT('Ctrl Pts',(-4.74666170096547,71.8845921494189,
0.));
#159346=CARTESIAN_POINT('Ctrl Pts',(-4.7534145153167,71.8614752519008,0.));
#159347=CARTESIAN_POINT('Ctrl Pts',(-4.7601329877742,71.8383923242531,0.));
#159348=CARTESIAN_POINT('Ctrl Pts',(-4.76681714352502,71.8153434978923,
0.));
#159349=CARTESIAN_POINT('Ctrl Pts',(-4.77346700795792,71.7923289047643,
0.));
#159350=CARTESIAN_POINT('Ctrl Pts',(-4.7800826066665,71.769348677346,0.));
#159351=CARTESIAN_POINT('Ctrl Pts',(-4.78666396544458,71.7464029486563,
0.));
#159352=CARTESIAN_POINT('Ctrl Pts',(-4.79321111028676,71.723491852261,0.));
#159353=CARTESIAN_POINT('Ctrl Pts',(-4.79972406739011,71.7006155222764,
0.));
#159354=CARTESIAN_POINT('Ctrl Pts',(-4.80620286316075,71.6777740933687,
0.));
#159355=CARTESIAN_POINT('Ctrl Pts',(-4.81264752421713,71.6549677007582,
0.));
#159356=CARTESIAN_POINT('Ctrl Pts',(-4.81905807738542,71.6321964802297,
0.));
#159357=CARTESIAN_POINT('Ctrl Pts',(-4.82543454970021,71.6094605681353,
0.));
#159358=CARTESIAN_POINT('Ctrl Pts',(-4.8317769684064,71.5867601014008,0.));
#159359=CARTESIAN_POINT('Ctrl Pts',(-4.83808536096589,71.5640952175239,
0.));
#159360=CARTESIAN_POINT('Ctrl Pts',(-4.84435975506056,71.5414660545778,
0.));
#159361=CARTESIAN_POINT('Ctrl Pts',(-4.85060017858786,71.5188727512231,
0.));
#159362=CARTESIAN_POINT('Ctrl Pts',(-4.85680665966184,71.4963154467128,
0.));
#159363=CARTESIAN_POINT('Ctrl Pts',(-4.86297922661499,71.4737942808971,
0.));
#159364=CARTESIAN_POINT('Ctrl Pts',(-4.86911790800533,71.4513093942216,
0.));
#159365=CARTESIAN_POINT('Ctrl Pts',(-4.87522273261881,71.4288609277324,
0.));
#159366=CARTESIAN_POINT('Ctrl Pts',(-4.88129372946524,71.4064490230857,
0.));
#159367=CARTESIAN_POINT('Ctrl Pts',(-4.88733092777964,71.3840738225547,
0.));
#159368=CARTESIAN_POINT('Ctrl Pts',(-4.89333435702424,71.3617354690342,
0.));
#159369=CARTESIAN_POINT('Ctrl Pts',(-4.89930404689599,71.3394341060396,
0.));
#159370=CARTESIAN_POINT('Ctrl Pts',(-4.90524002732806,71.3171698777124,
0.));
#159371=CARTESIAN_POINT('Ctrl Pts',(-4.91114232848623,71.2949429288319,
0.));
#159372=CARTESIAN_POINT('Ctrl Pts',(-4.91701098077041,71.27275340482,0.));
#159373=CARTESIAN_POINT('Ctrl Pts',(-4.9228460148171,71.2506014517457,0.));
#159374=CARTESIAN_POINT('Ctrl Pts',(-4.92864746150711,71.2284872163248,
0.));
#159375=CARTESIAN_POINT('Ctrl Pts',(-4.93441535196594,71.206410845926,0.));
#159376=CARTESIAN_POINT('Ctrl Pts',(-4.94014971756097,71.184372488583,0.));
#159377=CARTESIAN_POINT('Ctrl Pts',(-4.94585058990337,71.1623722929998,
0.));
#159378=CARTESIAN_POINT('Ctrl Pts',(-4.95151800085111,71.1404104085561,
0.));
#159379=CARTESIAN_POINT('Ctrl Pts',(-4.95715198251704,71.1184869853071,
0.));
#159380=CARTESIAN_POINT('Ctrl Pts',(-4.96275256726787,71.0966021739922,
0.));
#159381=CARTESIAN_POINT('Ctrl Pts',(-4.96831978772201,71.0747561260443,
0.));
#159382=CARTESIAN_POINT('Ctrl Pts',(-4.97385367675157,71.0529489935959,
0.));
#159383=CARTESIAN_POINT('Ctrl Pts',(-4.97935426748577,71.031180929482,0.));
#159384=CARTESIAN_POINT('Ctrl Pts',(-4.98482159331851,71.0094520872375,
0.));
#159385=CARTESIAN_POINT('Ctrl Pts',(-4.99025568790653,70.9877626211112,
0.));
#159386=CARTESIAN_POINT('Ctrl Pts',(-4.99565658516906,70.9661126860773,
0.));
#159387=CARTESIAN_POINT('Ctrl Pts',(-5.00102431929039,70.9445024378439,
0.));
#159388=CARTESIAN_POINT('Ctrl Pts',(-5.00635892472518,70.9229320328588,
0.));
#159389=CARTESIAN_POINT('Ctrl Pts',(-5.01166043620573,70.9014016283123,
0.));
#159390=CARTESIAN_POINT('Ctrl Pts',(-5.01692888873793,70.8799113821449,
0.));
#159391=CARTESIAN_POINT('Ctrl Pts',(-5.0221643176006,70.8584614530517,0.));
#159392=CARTESIAN_POINT('Ctrl Pts',(-5.02736675834691,70.8370520004844,
0.));
#159393=CARTESIAN_POINT('Ctrl Pts',(-5.03253624680941,70.8156831846494,
0.));
#159394=CARTESIAN_POINT('Ctrl Pts',(-5.03767281910483,70.7943551665071,
0.));
#159395=CARTESIAN_POINT('Ctrl Pts',(-5.04277651163356,70.7730681077997,
0.));
#159396=CARTESIAN_POINT('Ctrl Pts',(-5.04784736108351,70.7518221710715,
0.));
#159397=CARTESIAN_POINT('Ctrl Pts',(-5.05288540443478,70.7306175196856,
0.));
#159398=CARTESIAN_POINT('Ctrl Pts',(-5.05789067897041,70.7094543178416,
0.));
#159399=CARTESIAN_POINT('Ctrl Pts',(-5.06286322227797,70.6883327305755,
0.));
#159400=CARTESIAN_POINT('Ctrl Pts',(-5.06780307224053,70.6672529237431,
0.));
#159401=CARTESIAN_POINT('Ctrl Pts',(-5.0727102670335,70.6462150640009,0.));
#159402=CARTESIAN_POINT('Ctrl Pts',(-5.0775848451231,70.6252193187892,0.));
#159403=CARTESIAN_POINT('Ctrl Pts',(-5.08242684526704,70.6042658562951,
0.));
#159404=CARTESIAN_POINT('Ctrl Pts',(-5.08723630652291,70.5833548455043,
0.));
#159405=CARTESIAN_POINT('Ctrl Pts',(-5.09201326826146,70.5624864562841,
0.));
#159406=CARTESIAN_POINT('Ctrl Pts',(-5.09675777018182,70.5416608594526,
0.));
#159407=CARTESIAN_POINT('Ctrl Pts',(-5.10146985232928,70.5208782268482,
0.));
#159408=CARTESIAN_POINT('Ctrl Pts',(-5.10614955511643,70.5001387313963,
0.));
#159409=CARTESIAN_POINT('Ctrl Pts',(-5.11079691929193,70.4794425469799,
0.));
#159410=CARTESIAN_POINT('Ctrl Pts',(-5.1154119859092,70.4587898482946,0.));
#159411=CARTESIAN_POINT('Ctrl Pts',(-5.11999479630215,70.438180810725,0.));
#159412=CARTESIAN_POINT('Ctrl Pts',(-5.12454539205347,70.4176156101633,
0.));
#159413=CARTESIAN_POINT('Ctrl Pts',(-5.12906381499486,70.3970944229885,
0.));
#159414=CARTESIAN_POINT('Ctrl Pts',(-5.13355010728591,70.3766174264786,
0.));
#159415=CARTESIAN_POINT('Ctrl Pts',(-5.13800431148911,70.3561847991725,
0.));
#159416=CARTESIAN_POINT('Ctrl Pts',(-5.14242647063467,70.3357967211782,
0.));
#159417=CARTESIAN_POINT('Ctrl Pts',(-5.14681662833054,70.31545337467,0.));
#159418=CARTESIAN_POINT('Ctrl Pts',(-5.15117482869224,70.2951549435469,
0.));
#159419=CARTESIAN_POINT('Ctrl Pts',(-5.15550111614838,70.2749016125073,
0.));
#159420=CARTESIAN_POINT('Ctrl Pts',(-5.159795535282,70.2546935662719,0.));
#159421=CARTESIAN_POINT('Ctrl Pts',(-5.16405813066994,70.2345309887864,
0.));
#159422=CARTESIAN_POINT('Ctrl Pts',(-5.1682889467014,70.2144140623004,0.));
#159423=CARTESIAN_POINT('Ctrl Pts',(-5.1724880279342,70.1943429691214,0.));
#159424=CARTESIAN_POINT('Ctrl Pts',(-5.176655419524,70.1743178937102,0.));
#159425=CARTESIAN_POINT('Ctrl Pts',(-5.18079116757659,70.1543390243882,
0.));
#159426=CARTESIAN_POINT('Ctrl Pts',(-5.18489531966234,70.1344065558106,
0.));
#159427=CARTESIAN_POINT('Ctrl Pts',(-5.18896792486523,70.1145206891833,
0.));
#159428=CARTESIAN_POINT('Ctrl Pts',(-5.19300903271544,70.0946816270957,
0.));
#159429=CARTESIAN_POINT('Ctrl Pts',(-5.19701869225514,70.0748895689716,
0.));
#159430=CARTESIAN_POINT('Ctrl Pts',(-5.20099695122677,70.0551447071106,
0.));
#159431=CARTESIAN_POINT('Ctrl Pts',(-5.20494385478083,70.0354472203604,
0.));
#159432=CARTESIAN_POINT('Ctrl Pts',(-5.20885944672914,70.0157972802255,
0.));
#159433=CARTESIAN_POINT('Ctrl Pts',(-5.21274377203321,69.996195063002,0.));
#159434=CARTESIAN_POINT('Ctrl Pts',(-5.21659687881139,69.9766407595385,
0.));
#159435=CARTESIAN_POINT('Ctrl Pts',(-5.22041882075627,69.9571345869996,
0.));
#159436=CARTESIAN_POINT('Ctrl Pts',(-5.22420965879808,69.9376767968951,
0.));
#159437=CARTESIAN_POINT('Ctrl Pts',(-5.22796945602603,69.9182676501892,
0.));
#159438=CARTESIAN_POINT('Ctrl Pts',(-5.23169827290452,69.8989073936606,
0.));
#159439=CARTESIAN_POINT('Ctrl Pts',(-5.23539616279715,69.8795962381676,
0.));
#159440=CARTESIAN_POINT('Ctrl Pts',(-5.23906316635141,69.8603343303016,
0.));
#159441=CARTESIAN_POINT('Ctrl Pts',(-5.24269931055075,69.8411217507931,
0.));
#159442=CARTESIAN_POINT('Ctrl Pts',(-5.2455835516022,69.8257911792542,0.));
#159443=CARTESIAN_POINT('Ctrl Pts',(-5.24773285666673,69.8143154684447,
0.));
#159444=CARTESIAN_POINT('Ctrl Pts',(-5.24915955997537,69.8066748687863,
0.));
#159445=CARTESIAN_POINT('Ctrl Pts',(-5.24987136994591,69.8028570375098,
0.));
#159446=CARTESIAN_POINT('Ctrl Pts',(2.62535189104657,74.4537274248118,0.));
#159447=CARTESIAN_POINT('Ctrl Pts',(2.62535189104657,74.4537274248118,12.));
#159448=CARTESIAN_POINT('Ctrl Pts',(2.62283178248298,74.4487312586601,0.));
#159449=CARTESIAN_POINT('Ctrl Pts',(2.62283178248298,74.4487312586601,12.));
#159450=CARTESIAN_POINT('Ctrl Pts',(2.61779535432371,74.4387409032582,0.));
#159451=CARTESIAN_POINT('Ctrl Pts',(2.61779535432371,74.4387409032582,12.));
#159452=CARTESIAN_POINT('Ctrl Pts',(2.61025207898832,74.4237613008609,0.));
#159453=CARTESIAN_POINT('Ctrl Pts',(2.61025207898832,74.4237613008609,12.));
#159454=CARTESIAN_POINT('Ctrl Pts',(2.60021711327492,74.4038003595514,0.));
#159455=CARTESIAN_POINT('Ctrl Pts',(2.60021711327492,74.4038003595514,12.));
#159456=CARTESIAN_POINT('Ctrl Pts',(2.5877113026862,74.3788689604,0.));
#159457=CARTESIAN_POINT('Ctrl Pts',(2.5877113026862,74.3788689604,12.));
#159458=CARTESIAN_POINT('Ctrl Pts',(2.57524339541658,74.3539573568054,0.));
#159459=CARTESIAN_POINT('Ctrl Pts',(2.57524339541658,74.3539573568054,12.));
#159460=CARTESIAN_POINT('Ctrl Pts',(2.56281339800083,74.3290655814922,0.));
#159461=CARTESIAN_POINT('Ctrl Pts',(2.56281339800083,74.3290655814922,12.));
#159462=CARTESIAN_POINT('Ctrl Pts',(2.55042131526685,74.3041936853329,0.));
#159463=CARTESIAN_POINT('Ctrl Pts',(2.55042131526685,74.3041936853329,12.));
#159464=CARTESIAN_POINT('Ctrl Pts',(2.53806714838104,74.2793417427044,0.));
#159465=CARTESIAN_POINT('Ctrl Pts',(2.53806714838104,74.2793417427044,12.));
#159466=CARTESIAN_POINT('Ctrl Pts',(2.52575089478113,74.2545098494549,0.));
#159467=CARTESIAN_POINT('Ctrl Pts',(2.52575089478113,74.2545098494549,12.));
#159468=CARTESIAN_POINT('Ctrl Pts',(2.51347254956027,74.2296981152027,0.));
#159469=CARTESIAN_POINT('Ctrl Pts',(2.51347254956027,74.2296981152027,12.));
#159470=CARTESIAN_POINT('Ctrl Pts',(2.50123210644075,74.2049066571942,0.));
#159471=CARTESIAN_POINT('Ctrl Pts',(2.50123210644075,74.2049066571942,12.));
#159472=CARTESIAN_POINT('Ctrl Pts',(2.48902955888402,74.180135593693,0.));
#159473=CARTESIAN_POINT('Ctrl Pts',(2.48902955888402,74.180135593693,12.));
#159474=CARTESIAN_POINT('Ctrl Pts',(2.47686490120424,74.1553850371577,0.));
#159475=CARTESIAN_POINT('Ctrl Pts',(2.47686490120424,74.1553850371577,12.));
#159476=CARTESIAN_POINT('Ctrl Pts',(2.46473812948049,74.1306550887196,0.));
#159477=CARTESIAN_POINT('Ctrl Pts',(2.46473812948049,74.1306550887196,12.));
#159478=CARTESIAN_POINT('Ctrl Pts',(2.45264924094853,74.1059458420175,0.));
#159479=CARTESIAN_POINT('Ctrl Pts',(2.45264924094853,74.1059458420175,12.));
#159480=CARTESIAN_POINT('Ctrl Pts',(2.44059823356722,74.0812573859474,0.));
#159481=CARTESIAN_POINT('Ctrl Pts',(2.44059823356722,74.0812573859474,12.));
#159482=CARTESIAN_POINT('Ctrl Pts',(2.42858510549787,74.0565898079227,0.));
#159483=CARTESIAN_POINT('Ctrl Pts',(2.42858510549787,74.0565898079227,12.));
#159484=CARTESIAN_POINT('Ctrl Pts',(2.41660985465229,74.0319431966956,0.));
#159485=CARTESIAN_POINT('Ctrl Pts',(2.41660985465229,74.0319431966956,12.));
#159486=CARTESIAN_POINT('Ctrl Pts',(2.40467247811497,74.0073176459287,0.));
#159487=CARTESIAN_POINT('Ctrl Pts',(2.40467247811497,74.0073176459287,12.));
#159488=CARTESIAN_POINT('Ctrl Pts',(2.39277297220717,73.9827132538149,0.));
#159489=CARTESIAN_POINT('Ctrl Pts',(2.39277297220717,73.9827132538149,12.));
#159490=CARTESIAN_POINT('Ctrl Pts',(2.38091133274933,73.9581301214609,0.));
#159491=CARTESIAN_POINT('Ctrl Pts',(2.38091133274933,73.9581301214609,12.));
#159492=CARTESIAN_POINT('Ctrl Pts',(2.36908755525995,73.9335683516388,0.));
#159493=CARTESIAN_POINT('Ctrl Pts',(2.36908755525995,73.9335683516388,12.));
#159494=CARTESIAN_POINT('Ctrl Pts',(2.35730163516325,73.9090280474723,0.));
#159495=CARTESIAN_POINT('Ctrl Pts',(2.35730163516325,73.9090280474723,12.));
#159496=CARTESIAN_POINT('Ctrl Pts',(2.34555356802141,73.8845093109302,0.));
#159497=CARTESIAN_POINT('Ctrl Pts',(2.34555356802141,73.8845093109302,12.));
#159498=CARTESIAN_POINT('Ctrl Pts',(2.33384334963981,73.8600122421502,0.));
#159499=CARTESIAN_POINT('Ctrl Pts',(2.33384334963981,73.8600122421502,12.));
#159500=CARTESIAN_POINT('Ctrl Pts',(2.32217097594216,73.8355369402733,0.));
#159501=CARTESIAN_POINT('Ctrl Pts',(2.32217097594216,73.8355369402733,12.));
#159502=CARTESIAN_POINT('Ctrl Pts',(2.31053644289426,73.8110835039341,0.));
#159503=CARTESIAN_POINT('Ctrl Pts',(2.31053644289426,73.8110835039341,12.));
#159504=CARTESIAN_POINT('Ctrl Pts',(2.29893974640436,73.7866520318849,0.));
#159505=CARTESIAN_POINT('Ctrl Pts',(2.29893974640436,73.7866520318849,12.));
#159506=CARTESIAN_POINT('Ctrl Pts',(2.28738088222859,73.7622426235648,0.));
#159507=CARTESIAN_POINT('Ctrl Pts',(2.28738088222859,73.7622426235648,12.));
#159508=CARTESIAN_POINT('Ctrl Pts',(2.27585984587193,73.7378553796792,0.));
#159509=CARTESIAN_POINT('Ctrl Pts',(2.27585984587193,73.7378553796792,12.));
#159510=CARTESIAN_POINT('Ctrl Pts',(2.26437663263664,73.7134904019378,0.));
#159511=CARTESIAN_POINT('Ctrl Pts',(2.26437663263664,73.7134904019378,12.));
#159512=CARTESIAN_POINT('Ctrl Pts',(2.25293123766425,73.6891477928124,0.));
#159513=CARTESIAN_POINT('Ctrl Pts',(2.25293123766425,73.6891477928124,12.));
#159514=CARTESIAN_POINT('Ctrl Pts',(2.241523655977,73.6648276552766,0.));
#159515=CARTESIAN_POINT('Ctrl Pts',(2.241523655977,73.6648276552766,12.));
#159516=CARTESIAN_POINT('Ctrl Pts',(2.2301538825129,73.6405300925714,0.));
#159517=CARTESIAN_POINT('Ctrl Pts',(2.2301538825129,73.6405300925714,12.));
#159518=CARTESIAN_POINT('Ctrl Pts',(2.21882191216522,73.6162552079044,0.));
#159519=CARTESIAN_POINT('Ctrl Pts',(2.21882191216522,73.6162552079044,12.));
#159520=CARTESIAN_POINT('Ctrl Pts',(2.20752773978354,73.5920031044604,0.));
#159521=CARTESIAN_POINT('Ctrl Pts',(2.20752773978354,73.5920031044604,12.));
#159522=CARTESIAN_POINT('Ctrl Pts',(2.19627136015683,73.5677738855461,0.));
#159523=CARTESIAN_POINT('Ctrl Pts',(2.19627136015683,73.5677738855461,12.));
#159524=CARTESIAN_POINT('Ctrl Pts',(2.18505276799757,73.5435676546934,0.));
#159525=CARTESIAN_POINT('Ctrl Pts',(2.18505276799757,73.5435676546934,12.));
#159526=CARTESIAN_POINT('Ctrl Pts',(2.17387195792306,73.5193845157705,0.));
#159527=CARTESIAN_POINT('Ctrl Pts',(2.17387195792306,73.5193845157705,12.));
#159528=CARTESIAN_POINT('Ctrl Pts',(2.16272892442916,73.4952245731044,0.));
#159529=CARTESIAN_POINT('Ctrl Pts',(2.16272892442916,73.4952245731044,12.));
#159530=CARTESIAN_POINT('Ctrl Pts',(2.151623661879,73.4710879315367,0.));
#159531=CARTESIAN_POINT('Ctrl Pts',(2.151623661879,73.4710879315367,12.));
#159532=CARTESIAN_POINT('Ctrl Pts',(2.14055616452049,73.4469746963622,0.));
#159533=CARTESIAN_POINT('Ctrl Pts',(2.14055616452049,73.4469746963622,12.));
#159534=CARTESIAN_POINT('Ctrl Pts',(2.12952642649361,73.4228849732915,0.));
#159535=CARTESIAN_POINT('Ctrl Pts',(2.12952642649361,73.4228849732915,12.));
#159536=CARTESIAN_POINT('Ctrl Pts',(2.11853444183764,73.3988188684022,0.));
#159537=CARTESIAN_POINT('Ctrl Pts',(2.11853444183764,73.3988188684022,12.));
#159538=CARTESIAN_POINT('Ctrl Pts',(2.10758020449401,73.3747764880903,0.));
#159539=CARTESIAN_POINT('Ctrl Pts',(2.10758020449401,73.3747764880903,12.));
#159540=CARTESIAN_POINT('Ctrl Pts',(2.09666370830734,73.3507579390254,0.));
#159541=CARTESIAN_POINT('Ctrl Pts',(2.09666370830734,73.3507579390254,12.));
#159542=CARTESIAN_POINT('Ctrl Pts',(2.08578494702762,73.3267633281822,0.));
#159543=CARTESIAN_POINT('Ctrl Pts',(2.08578494702762,73.3267633281822,12.));
#159544=CARTESIAN_POINT('Ctrl Pts',(2.07494391430955,73.3027927628636,0.));
#159545=CARTESIAN_POINT('Ctrl Pts',(2.07494391430955,73.3027927628636,12.));
#159546=CARTESIAN_POINT('Ctrl Pts',(2.06414060370838,73.2788463507248,0.));
#159547=CARTESIAN_POINT('Ctrl Pts',(2.06414060370838,73.2788463507248,12.));
#159548=CARTESIAN_POINT('Ctrl Pts',(2.05337500867396,73.2549241997946,0.));
#159549=CARTESIAN_POINT('Ctrl Pts',(2.05337500867396,73.2549241997946,12.));
#159550=CARTESIAN_POINT('Ctrl Pts',(2.04264712253916,73.2310264184965,0.));
#159551=CARTESIAN_POINT('Ctrl Pts',(2.04264712253916,73.2310264184965,12.));
#159552=CARTESIAN_POINT('Ctrl Pts',(2.03195693852441,73.2071531156492,0.));
#159553=CARTESIAN_POINT('Ctrl Pts',(2.03195693852441,73.2071531156492,12.));
#159554=CARTESIAN_POINT('Ctrl Pts',(2.02130444974352,73.1833044004612,0.));
#159555=CARTESIAN_POINT('Ctrl Pts',(2.02130444974352,73.1833044004612,12.));
#159556=CARTESIAN_POINT('Ctrl Pts',(2.01068964920465,73.159480382525,0.));
#159557=CARTESIAN_POINT('Ctrl Pts',(2.01068964920465,73.159480382525,12.));
#159558=CARTESIAN_POINT('Ctrl Pts',(2.00011252980988,73.1356811718094,0.));
#159559=CARTESIAN_POINT('Ctrl Pts',(2.00011252980988,73.1356811718094,12.));
#159560=CARTESIAN_POINT('Ctrl Pts',(1.98957308434931,73.1119068786482,0.));
#159561=CARTESIAN_POINT('Ctrl Pts',(1.98957308434931,73.1119068786482,12.));
#159562=CARTESIAN_POINT('Ctrl Pts',(1.97907130550173,73.0881576137415,0.));
#159563=CARTESIAN_POINT('Ctrl Pts',(1.97907130550173,73.0881576137415,12.));
#159564=CARTESIAN_POINT('Ctrl Pts',(1.96860718583945,73.0644334881679,0.));
#159565=CARTESIAN_POINT('Ctrl Pts',(1.96860718583945,73.0644334881679,12.));
#159566=CARTESIAN_POINT('Ctrl Pts',(1.95818071782774,73.0407346133912,0.));
#159567=CARTESIAN_POINT('Ctrl Pts',(1.95818071782774,73.0407346133912,12.));
#159568=CARTESIAN_POINT('Ctrl Pts',(1.94779189382301,73.0170611012659,0.));
#159569=CARTESIAN_POINT('Ctrl Pts',(1.94779189382301,73.0170611012659,12.));
#159570=CARTESIAN_POINT('Ctrl Pts',(1.93744070606558,72.9934130640414,0.));
#159571=CARTESIAN_POINT('Ctrl Pts',(1.93744070606558,72.9934130640414,12.));
#159572=CARTESIAN_POINT('Ctrl Pts',(1.92712714667649,72.9697906143638,0.));
#159573=CARTESIAN_POINT('Ctrl Pts',(1.92712714667649,72.9697906143638,12.));
#159574=CARTESIAN_POINT('Ctrl Pts',(1.91685120766428,72.9461938652816,0.));
#159575=CARTESIAN_POINT('Ctrl Pts',(1.91685120766428,72.9461938652816,12.));
#159576=CARTESIAN_POINT('Ctrl Pts',(1.90661288092583,72.9226229302483,0.));
#159577=CARTESIAN_POINT('Ctrl Pts',(1.90661288092583,72.9226229302483,12.));
#159578=CARTESIAN_POINT('Ctrl Pts',(1.89641215824585,72.8990779231226,0.));
#159579=CARTESIAN_POINT('Ctrl Pts',(1.89641215824585,72.8990779231226,12.));
#159580=CARTESIAN_POINT('Ctrl Pts',(1.88624903129196,72.8755589581674,0.));
#159581=CARTESIAN_POINT('Ctrl Pts',(1.88624903129196,72.8755589581674,12.));
#159582=CARTESIAN_POINT('Ctrl Pts',(1.87612349160953,72.8520661500465,0.));
#159583=CARTESIAN_POINT('Ctrl Pts',(1.87612349160953,72.8520661500465,12.));
#159584=CARTESIAN_POINT('Ctrl Pts',(1.86603553062777,72.8285996138346,0.));
#159585=CARTESIAN_POINT('Ctrl Pts',(1.86603553062777,72.8285996138346,12.));
#159586=CARTESIAN_POINT('Ctrl Pts',(1.85598513966116,72.8051594650214,0.));
#159587=CARTESIAN_POINT('Ctrl Pts',(1.85598513966116,72.8051594650214,12.));
#159588=CARTESIAN_POINT('Ctrl Pts',(1.84597230990859,72.7817458195155,0.));
#159589=CARTESIAN_POINT('Ctrl Pts',(1.84597230990859,72.7817458195155,12.));
#159590=CARTESIAN_POINT('Ctrl Pts',(1.83599703244927,72.7583587936454,0.));
#159591=CARTESIAN_POINT('Ctrl Pts',(1.83599703244927,72.7583587936454,12.));
#159592=CARTESIAN_POINT('Ctrl Pts',(1.82605929823566,72.73499850416,0.));
#159593=CARTESIAN_POINT('Ctrl Pts',(1.82605929823566,72.73499850416,12.));
#159594=CARTESIAN_POINT('Ctrl Pts',(1.81615909809873,72.7116650682347,0.));
#159595=CARTESIAN_POINT('Ctrl Pts',(1.81615909809873,72.7116650682347,12.));
#159596=CARTESIAN_POINT('Ctrl Pts',(1.80629642275052,72.6883586034768,0.));
#159597=CARTESIAN_POINT('Ctrl Pts',(1.80629642275052,72.6883586034768,12.));
#159598=CARTESIAN_POINT('Ctrl Pts',(1.7964712627836,72.6650792279271,0.));
#159599=CARTESIAN_POINT('Ctrl Pts',(1.7964712627836,72.6650792279271,12.));
#159600=CARTESIAN_POINT('Ctrl Pts',(1.78668360866814,72.6418270600623,0.));
#159601=CARTESIAN_POINT('Ctrl Pts',(1.78668360866814,72.6418270600623,12.));
#159602=CARTESIAN_POINT('Ctrl Pts',(1.77693345074431,72.618602218792,0.));
#159603=CARTESIAN_POINT('Ctrl Pts',(1.77693345074431,72.618602218792,12.));
#159604=CARTESIAN_POINT('Ctrl Pts',(1.76722077922581,72.5954048234655,0.));
#159605=CARTESIAN_POINT('Ctrl Pts',(1.76722077922581,72.5954048234655,12.));
#159606=CARTESIAN_POINT('Ctrl Pts',(1.75754558420351,72.5722349938789,0.));
#159607=CARTESIAN_POINT('Ctrl Pts',(1.75754558420351,72.5722349938789,12.));
#159608=CARTESIAN_POINT('Ctrl Pts',(1.74790785564477,72.5490928502773,0.));
#159609=CARTESIAN_POINT('Ctrl Pts',(1.74790785564477,72.5490928502773,12.));
#159610=CARTESIAN_POINT('Ctrl Pts',(1.73830758339124,72.5259785133586,0.));
#159611=CARTESIAN_POINT('Ctrl Pts',(1.73830758339124,72.5259785133586,12.));
#159612=CARTESIAN_POINT('Ctrl Pts',(1.72874475715099,72.5028921042704,0.));
#159613=CARTESIAN_POINT('Ctrl Pts',(1.72874475715099,72.5028921042704,12.));
#159614=CARTESIAN_POINT('Ctrl Pts',(1.71921936650033,72.4798337446162,0.));
#159615=CARTESIAN_POINT('Ctrl Pts',(1.71921936650033,72.4798337446162,12.));
#159616=CARTESIAN_POINT('Ctrl Pts',(1.70973140088838,72.4568035564618,0.));
#159617=CARTESIAN_POINT('Ctrl Pts',(1.70973140088838,72.4568035564618,12.));
#159618=CARTESIAN_POINT('Ctrl Pts',(1.70028084963648,72.4338016623388,0.));
#159619=CARTESIAN_POINT('Ctrl Pts',(1.70028084963648,72.4338016623388,12.));
#159620=CARTESIAN_POINT('Ctrl Pts',(1.69086770193642,72.4108281852473,0.));
#159621=CARTESIAN_POINT('Ctrl Pts',(1.69086770193642,72.4108281852473,12.));
#159622=CARTESIAN_POINT('Ctrl Pts',(1.68149194684289,72.3878832486549,0.));
#159623=CARTESIAN_POINT('Ctrl Pts',(1.68149194684289,72.3878832486549,12.));
#159624=CARTESIAN_POINT('Ctrl Pts',(1.67215357327373,72.3649669765013,0.));
#159625=CARTESIAN_POINT('Ctrl Pts',(1.67215357327373,72.3649669765013,12.));
#159626=CARTESIAN_POINT('Ctrl Pts',(1.66285257001503,72.3420794932052,0.));
#159627=CARTESIAN_POINT('Ctrl Pts',(1.66285257001503,72.3420794932052,12.));
#159628=CARTESIAN_POINT('Ctrl Pts',(1.65358892572066,72.3192209236691,0.));
#159629=CARTESIAN_POINT('Ctrl Pts',(1.65358892572066,72.3192209236691,12.));
#159630=CARTESIAN_POINT('Ctrl Pts',(1.64436262891079,72.2963913932811,0.));
#159631=CARTESIAN_POINT('Ctrl Pts',(1.64436262891079,72.2963913932811,12.));
#159632=CARTESIAN_POINT('Ctrl Pts',(1.63517366796459,72.2735910279149,0.));
#159633=CARTESIAN_POINT('Ctrl Pts',(1.63517366796459,72.2735910279149,12.));
#159634=CARTESIAN_POINT('Ctrl Pts',(1.62602203111925,72.2508199539325,0.));
#159635=CARTESIAN_POINT('Ctrl Pts',(1.62602203111925,72.2508199539325,12.));
#159636=CARTESIAN_POINT('Ctrl Pts',(1.61690770647536,72.2280782981941,0.));
#159637=CARTESIAN_POINT('Ctrl Pts',(1.61690770647536,72.2280782981941,12.));
#159638=CARTESIAN_POINT('Ctrl Pts',(1.60783068199663,72.2053661880611,0.));
#159639=CARTESIAN_POINT('Ctrl Pts',(1.60783068199663,72.2053661880611,12.));
#159640=CARTESIAN_POINT('Ctrl Pts',(1.59879094550851,72.1826837514,0.));
#159641=CARTESIAN_POINT('Ctrl Pts',(1.59879094550851,72.1826837514,12.));
#159642=CARTESIAN_POINT('Ctrl Pts',(1.58978848469129,72.1600311165813,0.));
#159643=CARTESIAN_POINT('Ctrl Pts',(1.58978848469129,72.1600311165813,12.));
#159644=CARTESIAN_POINT('Ctrl Pts',(1.58082328707809,72.1374084124829,0.));
#159645=CARTESIAN_POINT('Ctrl Pts',(1.58082328707809,72.1374084124829,12.));
#159646=CARTESIAN_POINT('Ctrl Pts',(1.57189534006044,72.1148157684987,0.));
#159647=CARTESIAN_POINT('Ctrl Pts',(1.57189534006044,72.1148157684987,12.));
#159648=CARTESIAN_POINT('Ctrl Pts',(1.56300463088812,72.092253314543,0.));
#159649=CARTESIAN_POINT('Ctrl Pts',(1.56300463088812,72.092253314543,12.));
#159650=CARTESIAN_POINT('Ctrl Pts',(1.55415114666775,72.0697211810548,0.));
#159651=CARTESIAN_POINT('Ctrl Pts',(1.55415114666775,72.0697211810548,12.));
#159652=CARTESIAN_POINT('Ctrl Pts',(1.54533487435627,72.0472194989968,0.));
#159653=CARTESIAN_POINT('Ctrl Pts',(1.54533487435627,72.0472194989968,12.));
#159654=CARTESIAN_POINT('Ctrl Pts',(1.53655580075814,72.0247483998582,0.));
#159655=CARTESIAN_POINT('Ctrl Pts',(1.53655580075814,72.0247483998582,12.));
#159656=CARTESIAN_POINT('Ctrl Pts',(1.52781391253104,72.0023080156647,0.));
#159657=CARTESIAN_POINT('Ctrl Pts',(1.52781391253104,72.0023080156647,12.));
#159658=CARTESIAN_POINT('Ctrl Pts',(1.51910919618568,71.9798984789828,0.));
#159659=CARTESIAN_POINT('Ctrl Pts',(1.51910919618568,71.9798984789828,12.));
#159660=CARTESIAN_POINT('Ctrl Pts',(1.51044163808456,71.9575199229241,0.));
#159661=CARTESIAN_POINT('Ctrl Pts',(1.51044163808456,71.9575199229241,12.));
#159662=CARTESIAN_POINT('Ctrl Pts',(1.50181122443536,71.935172481145,0.));
#159663=CARTESIAN_POINT('Ctrl Pts',(1.50181122443536,71.935172481145,12.));
#159664=CARTESIAN_POINT('Ctrl Pts',(1.49321794128801,71.9128562878491,0.));
#159665=CARTESIAN_POINT('Ctrl Pts',(1.49321794128801,71.9128562878491,12.));
#159666=CARTESIAN_POINT('Ctrl Pts',(1.48466177454022,71.8905714777972,0.));
#159667=CARTESIAN_POINT('Ctrl Pts',(1.48466177454022,71.8905714777972,12.));
#159668=CARTESIAN_POINT('Ctrl Pts',(1.47614270993731,71.8683181863123,0.));
#159669=CARTESIAN_POINT('Ctrl Pts',(1.47614270993731,71.8683181863123,12.));
#159670=CARTESIAN_POINT('Ctrl Pts',(1.4676607330709,71.8460965492836,0.));
#159671=CARTESIAN_POINT('Ctrl Pts',(1.4676607330709,71.8460965492836,12.));
#159672=CARTESIAN_POINT('Ctrl Pts',(1.4592158293723,71.8239067031664,0.));
#159673=CARTESIAN_POINT('Ctrl Pts',(1.4592158293723,71.8239067031664,12.));
#159674=CARTESIAN_POINT('Ctrl Pts',(1.45080798410958,71.8017487849865,0.));
#159675=CARTESIAN_POINT('Ctrl Pts',(1.45080798410958,71.8017487849865,12.));
#159676=CARTESIAN_POINT('Ctrl Pts',(1.44243718239306,71.7796229323496,0.));
#159677=CARTESIAN_POINT('Ctrl Pts',(1.44243718239306,71.7796229323496,12.));
#159678=CARTESIAN_POINT('Ctrl Pts',(1.4341034091749,71.7575292834456,0.));
#159679=CARTESIAN_POINT('Ctrl Pts',(1.4341034091749,71.7575292834456,12.));
#159680=CARTESIAN_POINT('Ctrl Pts',(1.42580664924775,71.7354679770537,0.));
#159681=CARTESIAN_POINT('Ctrl Pts',(1.42580664924775,71.7354679770537,12.));
#159682=CARTESIAN_POINT('Ctrl Pts',(1.41754688723792,71.7134391525417,0.));
#159683=CARTESIAN_POINT('Ctrl Pts',(1.41754688723792,71.7134391525417,12.));
#159684=CARTESIAN_POINT('Ctrl Pts',(1.40932410760276,71.6914429498702,0.));
#159685=CARTESIAN_POINT('Ctrl Pts',(1.40932410760276,71.6914429498702,12.));
#159686=CARTESIAN_POINT('Ctrl Pts',(1.401138294636,71.6694795096034,0.));
#159687=CARTESIAN_POINT('Ctrl Pts',(1.401138294636,71.6694795096034,12.));
#159688=CARTESIAN_POINT('Ctrl Pts',(1.39298943246732,71.6475489729149,0.));
#159689=CARTESIAN_POINT('Ctrl Pts',(1.39298943246732,71.6475489729149,12.));
#159690=CARTESIAN_POINT('Ctrl Pts',(1.38487750506077,71.6256514815918,0.));
#159691=CARTESIAN_POINT('Ctrl Pts',(1.38487750506077,71.6256514815918,12.));
#159692=CARTESIAN_POINT('Ctrl Pts',(1.37680249620764,71.6037871780347,0.));
#159693=CARTESIAN_POINT('Ctrl Pts',(1.37680249620764,71.6037871780347,12.));
#159694=CARTESIAN_POINT('Ctrl Pts',(1.3687643895245,71.5819562052613,0.));
#159695=CARTESIAN_POINT('Ctrl Pts',(1.3687643895245,71.5819562052613,12.));
#159696=CARTESIAN_POINT('Ctrl Pts',(1.36076316845807,71.5601587069175,0.));
#159697=CARTESIAN_POINT('Ctrl Pts',(1.36076316845807,71.5601587069175,12.));
#159698=CARTESIAN_POINT('Ctrl Pts',(1.35279881628454,71.538394827283,0.));
#159699=CARTESIAN_POINT('Ctrl Pts',(1.35279881628454,71.538394827283,12.));
#159700=CARTESIAN_POINT('Ctrl Pts',(1.34487131610786,71.5166647112766,0.));
#159701=CARTESIAN_POINT('Ctrl Pts',(1.34487131610786,71.5166647112766,12.));
#159702=CARTESIAN_POINT('Ctrl Pts',(1.33698065085229,71.4949685044559,0.));
#159703=CARTESIAN_POINT('Ctrl Pts',(1.33698065085229,71.4949685044559,12.));
#159704=CARTESIAN_POINT('Ctrl Pts',(1.32912680326132,71.4733063530227,0.));
#159705=CARTESIAN_POINT('Ctrl Pts',(1.32912680326132,71.4733063530227,12.));
#159706=CARTESIAN_POINT('Ctrl Pts',(1.32130975590232,71.4516784038346,0.));
#159707=CARTESIAN_POINT('Ctrl Pts',(1.32130975590232,71.4516784038346,12.));
#159708=CARTESIAN_POINT('Ctrl Pts',(1.31352949116539,71.4300848044095,0.));
#159709=CARTESIAN_POINT('Ctrl Pts',(1.31352949116539,71.4300848044095,12.));
#159710=CARTESIAN_POINT('Ctrl Pts',(1.3057859912614,71.4085257029308,0.));
#159711=CARTESIAN_POINT('Ctrl Pts',(1.3057859912614,71.4085257029308,12.));
#159712=CARTESIAN_POINT('Ctrl Pts',(1.29807923821415,71.3870012482474,0.));
#159713=CARTESIAN_POINT('Ctrl Pts',(1.29807923821415,71.3870012482474,12.));
#159714=CARTESIAN_POINT('Ctrl Pts',(1.29040921386062,71.3655115898801,0.));
#159715=CARTESIAN_POINT('Ctrl Pts',(1.29040921386062,71.3655115898801,12.));
#159716=CARTESIAN_POINT('Ctrl Pts',(1.28277589985475,71.344056878033,0.));
#159717=CARTESIAN_POINT('Ctrl Pts',(1.28277589985475,71.344056878033,12.));
#159718=CARTESIAN_POINT('Ctrl Pts',(1.27517927766612,71.3226372635993,0.));
#159719=CARTESIAN_POINT('Ctrl Pts',(1.27517927766612,71.3226372635993,12.));
#159720=CARTESIAN_POINT('Ctrl Pts',(1.26761932857724,71.301252898167,0.));
#159721=CARTESIAN_POINT('Ctrl Pts',(1.26761932857724,71.301252898167,12.));
#159722=CARTESIAN_POINT('Ctrl Pts',(1.26009603367565,71.2799039340191,0.));
#159723=CARTESIAN_POINT('Ctrl Pts',(1.26009603367565,71.2799039340191,12.));
#159724=CARTESIAN_POINT('Ctrl Pts',(1.25260937385562,71.2585905241422,0.));
#159725=CARTESIAN_POINT('Ctrl Pts',(1.25260937385562,71.2585905241422,12.));
#159726=CARTESIAN_POINT('Ctrl Pts',(1.24515932982109,71.2373128222359,0.));
#159727=CARTESIAN_POINT('Ctrl Pts',(1.24515932982109,71.2373128222359,12.));
#159728=CARTESIAN_POINT('Ctrl Pts',(1.23774588208428,71.2160709827189,0.));
#159729=CARTESIAN_POINT('Ctrl Pts',(1.23774588208428,71.2160709827189,12.));
#159730=CARTESIAN_POINT('Ctrl Pts',(1.23036901096247,71.1948651607319,0.));
#159731=CARTESIAN_POINT('Ctrl Pts',(1.23036901096247,71.1948651607319,12.));
#159732=CARTESIAN_POINT('Ctrl Pts',(1.22302869657029,71.1736955121361,0.));
#159733=CARTESIAN_POINT('Ctrl Pts',(1.22302869657029,71.1736955121361,12.));
#159734=CARTESIAN_POINT('Ctrl Pts',(1.21572491882274,71.1525621935266,0.));
#159735=CARTESIAN_POINT('Ctrl Pts',(1.21572491882274,71.1525621935266,12.));
#159736=CARTESIAN_POINT('Ctrl Pts',(1.20845765743655,71.1314653622442,0.));
#159737=CARTESIAN_POINT('Ctrl Pts',(1.20845765743655,71.1314653622442,12.));
#159738=CARTESIAN_POINT('Ctrl Pts',(1.20122689192837,71.1104051763839,0.));
#159739=CARTESIAN_POINT('Ctrl Pts',(1.20122689192837,71.1104051763839,12.));
#159740=CARTESIAN_POINT('Ctrl Pts',(1.19403260160998,71.089381794801,0.));
#159741=CARTESIAN_POINT('Ctrl Pts',(1.19403260160998,71.089381794801,12.));
#159742=CARTESIAN_POINT('Ctrl Pts',(1.18687476558127,71.0683953771147,0.));
#159743=CARTESIAN_POINT('Ctrl Pts',(1.18687476558127,71.0683953771147,12.));
#159744=CARTESIAN_POINT('Ctrl Pts',(1.179753362735,71.0474460837157,0.));
#159745=CARTESIAN_POINT('Ctrl Pts',(1.179753362735,71.0474460837157,12.));
#159746=CARTESIAN_POINT('Ctrl Pts',(1.17266837175777,71.0265340757697,0.));
#159747=CARTESIAN_POINT('Ctrl Pts',(1.17266837175777,71.0265340757697,12.));
#159748=CARTESIAN_POINT('Ctrl Pts',(1.16561977112883,71.0056595152204,0.));
#159749=CARTESIAN_POINT('Ctrl Pts',(1.16561977112883,71.0056595152204,12.));
#159750=CARTESIAN_POINT('Ctrl Pts',(1.15860753911491,70.9848225647876,0.));
#159751=CARTESIAN_POINT('Ctrl Pts',(1.15860753911491,70.9848225647876,12.));
#159752=CARTESIAN_POINT('Ctrl Pts',(1.15163165376531,70.9640233879671,0.));
#159753=CARTESIAN_POINT('Ctrl Pts',(1.15163165376531,70.9640233879671,12.));
#159754=CARTESIAN_POINT('Ctrl Pts',(1.14469209291495,70.943262149058,0.));
#159755=CARTESIAN_POINT('Ctrl Pts',(1.14469209291495,70.943262149058,12.));
#159756=CARTESIAN_POINT('Ctrl Pts',(1.13778883418217,70.9225390131835,0.));
#159757=CARTESIAN_POINT('Ctrl Pts',(1.13778883418217,70.9225390131835,12.));
#159758=CARTESIAN_POINT('Ctrl Pts',(1.13092185496564,70.9018541463083,0.));
#159759=CARTESIAN_POINT('Ctrl Pts',(1.13092185496564,70.9018541463083,12.));
#159760=CARTESIAN_POINT('Ctrl Pts',(1.12409113243512,70.8812077152564,0.));
#159761=CARTESIAN_POINT('Ctrl Pts',(1.12409113243512,70.8812077152564,12.));
#159762=CARTESIAN_POINT('Ctrl Pts',(1.11729664352991,70.860599887712,0.));
#159763=CARTESIAN_POINT('Ctrl Pts',(1.11729664352991,70.860599887712,12.));
#159764=CARTESIAN_POINT('Ctrl Pts',(1.11053836496639,70.8400308322013,0.));
#159765=CARTESIAN_POINT('Ctrl Pts',(1.11053836496639,70.8400308322013,12.));
#159766=CARTESIAN_POINT('Ctrl Pts',(1.10381627323946,70.8195007180739,0.));
#159767=CARTESIAN_POINT('Ctrl Pts',(1.10381627323946,70.8195007180739,12.));
#159768=CARTESIAN_POINT('Ctrl Pts',(1.09713034462271,70.7990097154855,0.));
#159769=CARTESIAN_POINT('Ctrl Pts',(1.09713034462271,70.7990097154855,12.));
#159770=CARTESIAN_POINT('Ctrl Pts',(1.09048055516435,70.7785579953611,0.));
#159771=CARTESIAN_POINT('Ctrl Pts',(1.09048055516435,70.7785579953611,12.));
#159772=CARTESIAN_POINT('Ctrl Pts',(1.08386688068349,70.7581457294475,0.));
#159773=CARTESIAN_POINT('Ctrl Pts',(1.08386688068349,70.7581457294475,12.));
#159774=CARTESIAN_POINT('Ctrl Pts',(1.07728929676413,70.7377730903971,0.));
#159775=CARTESIAN_POINT('Ctrl Pts',(1.07728929676413,70.7377730903971,12.));
#159776=CARTESIAN_POINT('Ctrl Pts',(1.07074777874597,70.7174402518378,0.));
#159777=CARTESIAN_POINT('Ctrl Pts',(1.07074777874597,70.7174402518378,12.));
#159778=CARTESIAN_POINT('Ctrl Pts',(1.06424230171281,70.6971473884443,0.));
#159779=CARTESIAN_POINT('Ctrl Pts',(1.06424230171281,70.6971473884443,12.));
#159780=CARTESIAN_POINT('Ctrl Pts',(1.05777284047728,70.6768946760063,0.));
#159781=CARTESIAN_POINT('Ctrl Pts',(1.05777284047728,70.6768946760063,12.));
#159782=CARTESIAN_POINT('Ctrl Pts',(1.0513393696007,70.6566822912965,0.));
#159783=CARTESIAN_POINT('Ctrl Pts',(1.0513393696007,70.6566822912965,12.));
#159784=CARTESIAN_POINT('Ctrl Pts',(1.04494186341157,70.6365104119238,0.));
#159785=CARTESIAN_POINT('Ctrl Pts',(1.04494186341157,70.6365104119238,12.));
#159786=CARTESIAN_POINT('Ctrl Pts',(1.03858029601906,70.6163792162079,0.));
#159787=CARTESIAN_POINT('Ctrl Pts',(1.03858029601906,70.6163792162079,12.));
#159788=CARTESIAN_POINT('Ctrl Pts',(1.03225464132873,70.5962888829958,0.));
#159789=CARTESIAN_POINT('Ctrl Pts',(1.03225464132873,70.5962888829958,12.));
#159790=CARTESIAN_POINT('Ctrl Pts',(1.0259648730405,70.5762395916412,0.));
#159791=CARTESIAN_POINT('Ctrl Pts',(1.0259648730405,70.5762395916412,12.));
#159792=CARTESIAN_POINT('Ctrl Pts',(1.019710964606,70.5562315224219,0.));
#159793=CARTESIAN_POINT('Ctrl Pts',(1.019710964606,70.5562315224219,12.));
#159794=CARTESIAN_POINT('Ctrl Pts',(1.01349288918541,70.5362648569072,0.));
#159795=CARTESIAN_POINT('Ctrl Pts',(1.01349288918541,70.5362648569072,12.));
#159796=CARTESIAN_POINT('Ctrl Pts',(1.00731061960968,70.5163397782699,0.));
#159797=CARTESIAN_POINT('Ctrl Pts',(1.00731061960968,70.5163397782699,12.));
#159798=CARTESIAN_POINT('Ctrl Pts',(1.00116412831439,70.4964564717917,0.));
#159799=CARTESIAN_POINT('Ctrl Pts',(1.00116412831439,70.4964564717917,12.));
#159800=CARTESIAN_POINT('Ctrl Pts',(0.995053387379687,70.476615124517,0.));
#159801=CARTESIAN_POINT('Ctrl Pts',(0.995053387379687,70.476615124517,12.));
#159802=CARTESIAN_POINT('Ctrl Pts',(0.988978368643597,70.4568159243131,
0.));
#159803=CARTESIAN_POINT('Ctrl Pts',(0.988978368643597,70.4568159243131,
12.));
#159804=CARTESIAN_POINT('Ctrl Pts',(0.982939043792167,70.4370590590839,
0.));
#159805=CARTESIAN_POINT('Ctrl Pts',(0.982939043792167,70.4370590590839,
12.));
#159806=CARTESIAN_POINT('Ctrl Pts',(0.976935384450135,70.41734471596,0.));
#159807=CARTESIAN_POINT('Ctrl Pts',(0.976935384450135,70.41734471596,12.));
#159808=CARTESIAN_POINT('Ctrl Pts',(0.97096736228131,70.3976730803664,0.));
#159809=CARTESIAN_POINT('Ctrl Pts',(0.97096736228131,70.3976730803664,12.));
#159810=CARTESIAN_POINT('Ctrl Pts',(0.965034948786566,70.3780443378003,
0.));
#159811=CARTESIAN_POINT('Ctrl Pts',(0.965034948786566,70.3780443378003,
12.));
#159812=CARTESIAN_POINT('Ctrl Pts',(0.959138115058893,70.3584586759561,
0.));
#159813=CARTESIAN_POINT('Ctrl Pts',(0.959138115058893,70.3584586759561,
12.));
#159814=CARTESIAN_POINT('Ctrl Pts',(0.953276831581241,70.338916286457,0.));
#159815=CARTESIAN_POINT('Ctrl Pts',(0.953276831581241,70.338916286457,12.));
#159816=CARTESIAN_POINT('Ctrl Pts',(0.94745106792957,70.3194173673635,0.));
#159817=CARTESIAN_POINT('Ctrl Pts',(0.94745106792957,70.3194173673635,12.));
#159818=CARTESIAN_POINT('Ctrl Pts',(0.941660792742961,70.2999621233938,
0.));
#159819=CARTESIAN_POINT('Ctrl Pts',(0.941660792742961,70.2999621233938,
12.));
#159820=CARTESIAN_POINT('Ctrl Pts',(0.935905974336497,70.2805507606832,
0.));
#159821=CARTESIAN_POINT('Ctrl Pts',(0.935905974336497,70.2805507606832,
12.));
#159822=CARTESIAN_POINT('Ctrl Pts',(0.930186581235583,70.2611834821711,
0.));
#159823=CARTESIAN_POINT('Ctrl Pts',(0.930186581235583,70.2611834821711,
12.));
#159824=CARTESIAN_POINT('Ctrl Pts',(0.924502582639459,70.241860483586,0.));
#159825=CARTESIAN_POINT('Ctrl Pts',(0.924502582639459,70.241860483586,12.));
#159826=CARTESIAN_POINT('Ctrl Pts',(0.918853949157051,70.2225819470306,
0.));
#159827=CARTESIAN_POINT('Ctrl Pts',(0.918853949157051,70.2225819470306,
12.));
#159828=CARTESIAN_POINT('Ctrl Pts',(0.913240652090848,70.2033480471749,
0.));
#159829=CARTESIAN_POINT('Ctrl Pts',(0.913240652090848,70.2033480471749,
12.));
#159830=CARTESIAN_POINT('Ctrl Pts',(0.907662662015657,70.184158963563,0.));
#159831=CARTESIAN_POINT('Ctrl Pts',(0.907662662015657,70.184158963563,12.));
#159832=CARTESIAN_POINT('Ctrl Pts',(0.902119947629781,70.1650148905109,
0.));
#159833=CARTESIAN_POINT('Ctrl Pts',(0.902119947629781,70.1650148905109,
12.));
#159834=CARTESIAN_POINT('Ctrl Pts',(0.896612474372092,70.1459160490366,
0.));
#159835=CARTESIAN_POINT('Ctrl Pts',(0.896612474372092,70.1459160490366,
12.));
#159836=CARTESIAN_POINT('Ctrl Pts',(0.891140203464733,70.1268626950031,
0.));
#159837=CARTESIAN_POINT('Ctrl Pts',(0.891140203464733,70.1268626950031,
12.));
#159838=CARTESIAN_POINT('Ctrl Pts',(0.885703094803093,70.1078550938801,
0.));
#159839=CARTESIAN_POINT('Ctrl Pts',(0.885703094803093,70.1078550938801,
12.));
#159840=CARTESIAN_POINT('Ctrl Pts',(0.880301109661046,70.0888934967772,
0.));
#159841=CARTESIAN_POINT('Ctrl Pts',(0.880301109661046,70.0888934967772,
12.));
#159842=CARTESIAN_POINT('Ctrl Pts',(0.874934213255579,70.0699781184013,
0.));
#159843=CARTESIAN_POINT('Ctrl Pts',(0.874934213255579,70.0699781184013,
12.));
#159844=CARTESIAN_POINT('Ctrl Pts',(0.869602377870148,70.0511091083285,
0.));
#159845=CARTESIAN_POINT('Ctrl Pts',(0.869602377870148,70.0511091083285,
12.));
#159846=CARTESIAN_POINT('Ctrl Pts',(0.864305583660099,70.0322865493339,
0.));
#159847=CARTESIAN_POINT('Ctrl Pts',(0.864305583660099,70.0322865493339,
12.));
#159848=CARTESIAN_POINT('Ctrl Pts',(0.860096170667407,70.0172656934192,
0.));
#159849=CARTESIAN_POINT('Ctrl Pts',(0.860096170667407,70.0172656934192,
12.));
#159850=CARTESIAN_POINT('Ctrl Pts',(0.85695487025838,70.0060209754332,0.));
#159851=CARTESIAN_POINT('Ctrl Pts',(0.85695487025838,70.0060209754332,12.));
#159852=CARTESIAN_POINT('Ctrl Pts',(0.8548676738483,69.9985337959499,0.));
#159853=CARTESIAN_POINT('Ctrl Pts',(0.8548676738483,69.9985337959499,12.));
#159854=CARTESIAN_POINT('Ctrl Pts',(0.853825826608999,69.9947925310006,
0.));
#159855=CARTESIAN_POINT('Ctrl Pts',(0.853825826608999,69.9947925310006,
12.));
#159856=CARTESIAN_POINT('',(0.853825826608999,69.9947925310006,12.));
#159857=CARTESIAN_POINT('Ctrl Pts',(0.853825826608999,69.9947925310006,
12.));
#159858=CARTESIAN_POINT('Ctrl Pts',(0.8548676738483,69.9985337959499,12.));
#159859=CARTESIAN_POINT('Ctrl Pts',(0.85695487025838,70.0060209754332,12.));
#159860=CARTESIAN_POINT('Ctrl Pts',(0.860096170667407,70.0172656934192,
12.));
#159861=CARTESIAN_POINT('Ctrl Pts',(0.864305583660099,70.0322865493339,
12.));
#159862=CARTESIAN_POINT('Ctrl Pts',(0.869602377870148,70.0511091083285,
12.));
#159863=CARTESIAN_POINT('Ctrl Pts',(0.874934213255579,70.0699781184013,
12.));
#159864=CARTESIAN_POINT('Ctrl Pts',(0.880301109661046,70.0888934967772,
12.));
#159865=CARTESIAN_POINT('Ctrl Pts',(0.885703094803093,70.1078550938801,
12.));
#159866=CARTESIAN_POINT('Ctrl Pts',(0.891140203464733,70.1268626950031,
12.));
#159867=CARTESIAN_POINT('Ctrl Pts',(0.896612474372092,70.1459160490366,
12.));
#159868=CARTESIAN_POINT('Ctrl Pts',(0.902119947629781,70.1650148905109,
12.));
#159869=CARTESIAN_POINT('Ctrl Pts',(0.907662662015657,70.184158963563,12.));
#159870=CARTESIAN_POINT('Ctrl Pts',(0.913240652090848,70.2033480471749,
12.));
#159871=CARTESIAN_POINT('Ctrl Pts',(0.918853949157051,70.2225819470306,
12.));
#159872=CARTESIAN_POINT('Ctrl Pts',(0.924502582639459,70.241860483586,12.));
#159873=CARTESIAN_POINT('Ctrl Pts',(0.930186581235583,70.2611834821711,
12.));
#159874=CARTESIAN_POINT('Ctrl Pts',(0.935905974336497,70.2805507606832,
12.));
#159875=CARTESIAN_POINT('Ctrl Pts',(0.941660792742961,70.2999621233938,
12.));
#159876=CARTESIAN_POINT('Ctrl Pts',(0.94745106792957,70.3194173673635,12.));
#159877=CARTESIAN_POINT('Ctrl Pts',(0.953276831581241,70.338916286457,12.));
#159878=CARTESIAN_POINT('Ctrl Pts',(0.959138115058893,70.3584586759561,
12.));
#159879=CARTESIAN_POINT('Ctrl Pts',(0.965034948786566,70.3780443378003,
12.));
#159880=CARTESIAN_POINT('Ctrl Pts',(0.97096736228131,70.3976730803664,12.));
#159881=CARTESIAN_POINT('Ctrl Pts',(0.976935384450135,70.41734471596,12.));
#159882=CARTESIAN_POINT('Ctrl Pts',(0.982939043792167,70.4370590590839,
12.));
#159883=CARTESIAN_POINT('Ctrl Pts',(0.988978368643597,70.4568159243131,
12.));
#159884=CARTESIAN_POINT('Ctrl Pts',(0.995053387379687,70.476615124517,12.));
#159885=CARTESIAN_POINT('Ctrl Pts',(1.00116412831439,70.4964564717917,12.));
#159886=CARTESIAN_POINT('Ctrl Pts',(1.00731061960968,70.5163397782699,12.));
#159887=CARTESIAN_POINT('Ctrl Pts',(1.01349288918541,70.5362648569072,12.));
#159888=CARTESIAN_POINT('Ctrl Pts',(1.019710964606,70.5562315224219,12.));
#159889=CARTESIAN_POINT('Ctrl Pts',(1.0259648730405,70.5762395916412,12.));
#159890=CARTESIAN_POINT('Ctrl Pts',(1.03225464132873,70.5962888829958,12.));
#159891=CARTESIAN_POINT('Ctrl Pts',(1.03858029601906,70.6163792162079,12.));
#159892=CARTESIAN_POINT('Ctrl Pts',(1.04494186341157,70.6365104119238,12.));
#159893=CARTESIAN_POINT('Ctrl Pts',(1.0513393696007,70.6566822912965,12.));
#159894=CARTESIAN_POINT('Ctrl Pts',(1.05777284047728,70.6768946760063,12.));
#159895=CARTESIAN_POINT('Ctrl Pts',(1.06424230171281,70.6971473884443,12.));
#159896=CARTESIAN_POINT('Ctrl Pts',(1.07074777874597,70.7174402518378,12.));
#159897=CARTESIAN_POINT('Ctrl Pts',(1.07728929676413,70.7377730903971,12.));
#159898=CARTESIAN_POINT('Ctrl Pts',(1.08386688068349,70.7581457294475,12.));
#159899=CARTESIAN_POINT('Ctrl Pts',(1.09048055516435,70.7785579953611,12.));
#159900=CARTESIAN_POINT('Ctrl Pts',(1.09713034462271,70.7990097154855,12.));
#159901=CARTESIAN_POINT('Ctrl Pts',(1.10381627323946,70.8195007180739,12.));
#159902=CARTESIAN_POINT('Ctrl Pts',(1.11053836496639,70.8400308322013,12.));
#159903=CARTESIAN_POINT('Ctrl Pts',(1.11729664352991,70.860599887712,12.));
#159904=CARTESIAN_POINT('Ctrl Pts',(1.12409113243512,70.8812077152564,12.));
#159905=CARTESIAN_POINT('Ctrl Pts',(1.13092185496564,70.9018541463083,12.));
#159906=CARTESIAN_POINT('Ctrl Pts',(1.13778883418217,70.9225390131835,12.));
#159907=CARTESIAN_POINT('Ctrl Pts',(1.14469209291495,70.943262149058,12.));
#159908=CARTESIAN_POINT('Ctrl Pts',(1.15163165376531,70.9640233879671,12.));
#159909=CARTESIAN_POINT('Ctrl Pts',(1.15860753911491,70.9848225647876,12.));
#159910=CARTESIAN_POINT('Ctrl Pts',(1.16561977112883,71.0056595152204,12.));
#159911=CARTESIAN_POINT('Ctrl Pts',(1.17266837175777,71.0265340757697,12.));
#159912=CARTESIAN_POINT('Ctrl Pts',(1.179753362735,71.0474460837157,12.));
#159913=CARTESIAN_POINT('Ctrl Pts',(1.18687476558127,71.0683953771147,12.));
#159914=CARTESIAN_POINT('Ctrl Pts',(1.19403260160998,71.089381794801,12.));
#159915=CARTESIAN_POINT('Ctrl Pts',(1.20122689192837,71.1104051763839,12.));
#159916=CARTESIAN_POINT('Ctrl Pts',(1.20845765743655,71.1314653622442,12.));
#159917=CARTESIAN_POINT('Ctrl Pts',(1.21572491882274,71.1525621935266,12.));
#159918=CARTESIAN_POINT('Ctrl Pts',(1.22302869657029,71.1736955121361,12.));
#159919=CARTESIAN_POINT('Ctrl Pts',(1.23036901096247,71.1948651607319,12.));
#159920=CARTESIAN_POINT('Ctrl Pts',(1.23774588208428,71.2160709827189,12.));
#159921=CARTESIAN_POINT('Ctrl Pts',(1.24515932982109,71.2373128222359,12.));
#159922=CARTESIAN_POINT('Ctrl Pts',(1.25260937385562,71.2585905241422,12.));
#159923=CARTESIAN_POINT('Ctrl Pts',(1.26009603367565,71.2799039340191,12.));
#159924=CARTESIAN_POINT('Ctrl Pts',(1.26761932857724,71.301252898167,12.));
#159925=CARTESIAN_POINT('Ctrl Pts',(1.27517927766612,71.3226372635993,12.));
#159926=CARTESIAN_POINT('Ctrl Pts',(1.28277589985475,71.344056878033,12.));
#159927=CARTESIAN_POINT('Ctrl Pts',(1.29040921386062,71.3655115898801,12.));
#159928=CARTESIAN_POINT('Ctrl Pts',(1.29807923821415,71.3870012482474,12.));
#159929=CARTESIAN_POINT('Ctrl Pts',(1.3057859912614,71.4085257029308,12.));
#159930=CARTESIAN_POINT('Ctrl Pts',(1.31352949116539,71.4300848044095,12.));
#159931=CARTESIAN_POINT('Ctrl Pts',(1.32130975590232,71.4516784038346,12.));
#159932=CARTESIAN_POINT('Ctrl Pts',(1.32912680326132,71.4733063530227,12.));
#159933=CARTESIAN_POINT('Ctrl Pts',(1.33698065085229,71.4949685044559,12.));
#159934=CARTESIAN_POINT('Ctrl Pts',(1.34487131610786,71.5166647112766,12.));
#159935=CARTESIAN_POINT('Ctrl Pts',(1.35279881628454,71.538394827283,12.));
#159936=CARTESIAN_POINT('Ctrl Pts',(1.36076316845807,71.5601587069175,12.));
#159937=CARTESIAN_POINT('Ctrl Pts',(1.3687643895245,71.5819562052613,12.));
#159938=CARTESIAN_POINT('Ctrl Pts',(1.37680249620764,71.6037871780347,12.));
#159939=CARTESIAN_POINT('Ctrl Pts',(1.38487750506077,71.6256514815918,12.));
#159940=CARTESIAN_POINT('Ctrl Pts',(1.39298943246732,71.6475489729149,12.));
#159941=CARTESIAN_POINT('Ctrl Pts',(1.401138294636,71.6694795096034,12.));
#159942=CARTESIAN_POINT('Ctrl Pts',(1.40932410760276,71.6914429498702,12.));
#159943=CARTESIAN_POINT('Ctrl Pts',(1.41754688723792,71.7134391525417,12.));
#159944=CARTESIAN_POINT('Ctrl Pts',(1.42580664924775,71.7354679770537,12.));
#159945=CARTESIAN_POINT('Ctrl Pts',(1.4341034091749,71.7575292834456,12.));
#159946=CARTESIAN_POINT('Ctrl Pts',(1.44243718239306,71.7796229323496,12.));
#159947=CARTESIAN_POINT('Ctrl Pts',(1.45080798410958,71.8017487849865,12.));
#159948=CARTESIAN_POINT('Ctrl Pts',(1.4592158293723,71.8239067031664,12.));
#159949=CARTESIAN_POINT('Ctrl Pts',(1.4676607330709,71.8460965492836,12.));
#159950=CARTESIAN_POINT('Ctrl Pts',(1.47614270993731,71.8683181863123,12.));
#159951=CARTESIAN_POINT('Ctrl Pts',(1.48466177454022,71.8905714777972,12.));
#159952=CARTESIAN_POINT('Ctrl Pts',(1.49321794128801,71.9128562878491,12.));
#159953=CARTESIAN_POINT('Ctrl Pts',(1.50181122443536,71.935172481145,12.));
#159954=CARTESIAN_POINT('Ctrl Pts',(1.51044163808456,71.9575199229241,12.));
#159955=CARTESIAN_POINT('Ctrl Pts',(1.51910919618568,71.9798984789828,12.));
#159956=CARTESIAN_POINT('Ctrl Pts',(1.52781391253104,72.0023080156647,12.));
#159957=CARTESIAN_POINT('Ctrl Pts',(1.53655580075814,72.0247483998582,12.));
#159958=CARTESIAN_POINT('Ctrl Pts',(1.54533487435627,72.0472194989968,12.));
#159959=CARTESIAN_POINT('Ctrl Pts',(1.55415114666775,72.0697211810548,12.));
#159960=CARTESIAN_POINT('Ctrl Pts',(1.56300463088812,72.092253314543,12.));
#159961=CARTESIAN_POINT('Ctrl Pts',(1.57189534006044,72.1148157684987,12.));
#159962=CARTESIAN_POINT('Ctrl Pts',(1.58082328707809,72.1374084124829,12.));
#159963=CARTESIAN_POINT('Ctrl Pts',(1.58978848469129,72.1600311165813,12.));
#159964=CARTESIAN_POINT('Ctrl Pts',(1.59879094550851,72.1826837514,12.));
#159965=CARTESIAN_POINT('Ctrl Pts',(1.60783068199663,72.2053661880611,12.));
#159966=CARTESIAN_POINT('Ctrl Pts',(1.61690770647536,72.2280782981941,12.));
#159967=CARTESIAN_POINT('Ctrl Pts',(1.62602203111925,72.2508199539325,12.));
#159968=CARTESIAN_POINT('Ctrl Pts',(1.63517366796459,72.2735910279149,12.));
#159969=CARTESIAN_POINT('Ctrl Pts',(1.64436262891079,72.2963913932811,12.));
#159970=CARTESIAN_POINT('Ctrl Pts',(1.65358892572066,72.3192209236691,12.));
#159971=CARTESIAN_POINT('Ctrl Pts',(1.66285257001503,72.3420794932052,12.));
#159972=CARTESIAN_POINT('Ctrl Pts',(1.67215357327373,72.3649669765013,12.));
#159973=CARTESIAN_POINT('Ctrl Pts',(1.68149194684289,72.3878832486549,12.));
#159974=CARTESIAN_POINT('Ctrl Pts',(1.69086770193642,72.4108281852473,12.));
#159975=CARTESIAN_POINT('Ctrl Pts',(1.70028084963648,72.4338016623388,12.));
#159976=CARTESIAN_POINT('Ctrl Pts',(1.70973140088838,72.4568035564618,12.));
#159977=CARTESIAN_POINT('Ctrl Pts',(1.71921936650033,72.4798337446162,12.));
#159978=CARTESIAN_POINT('Ctrl Pts',(1.72874475715099,72.5028921042704,12.));
#159979=CARTESIAN_POINT('Ctrl Pts',(1.73830758339124,72.5259785133586,12.));
#159980=CARTESIAN_POINT('Ctrl Pts',(1.74790785564477,72.5490928502773,12.));
#159981=CARTESIAN_POINT('Ctrl Pts',(1.75754558420351,72.5722349938789,12.));
#159982=CARTESIAN_POINT('Ctrl Pts',(1.76722077922581,72.5954048234655,12.));
#159983=CARTESIAN_POINT('Ctrl Pts',(1.77693345074431,72.618602218792,12.));
#159984=CARTESIAN_POINT('Ctrl Pts',(1.78668360866814,72.6418270600623,12.));
#159985=CARTESIAN_POINT('Ctrl Pts',(1.7964712627836,72.6650792279271,12.));
#159986=CARTESIAN_POINT('Ctrl Pts',(1.80629642275052,72.6883586034768,12.));
#159987=CARTESIAN_POINT('Ctrl Pts',(1.81615909809873,72.7116650682347,12.));
#159988=CARTESIAN_POINT('Ctrl Pts',(1.82605929823566,72.73499850416,12.));
#159989=CARTESIAN_POINT('Ctrl Pts',(1.83599703244927,72.7583587936454,12.));
#159990=CARTESIAN_POINT('Ctrl Pts',(1.84597230990859,72.7817458195155,12.));
#159991=CARTESIAN_POINT('Ctrl Pts',(1.85598513966116,72.8051594650214,12.));
#159992=CARTESIAN_POINT('Ctrl Pts',(1.86603553062777,72.8285996138346,12.));
#159993=CARTESIAN_POINT('Ctrl Pts',(1.87612349160953,72.8520661500465,12.));
#159994=CARTESIAN_POINT('Ctrl Pts',(1.88624903129196,72.8755589581674,12.));
#159995=CARTESIAN_POINT('Ctrl Pts',(1.89641215824585,72.8990779231226,12.));
#159996=CARTESIAN_POINT('Ctrl Pts',(1.90661288092583,72.9226229302483,12.));
#159997=CARTESIAN_POINT('Ctrl Pts',(1.91685120766428,72.9461938652816,12.));
#159998=CARTESIAN_POINT('Ctrl Pts',(1.92712714667649,72.9697906143638,12.));
#159999=CARTESIAN_POINT('Ctrl Pts',(1.93744070606558,72.9934130640414,12.));
#160000=CARTESIAN_POINT('Ctrl Pts',(1.94779189382301,73.0170611012659,12.));
#160001=CARTESIAN_POINT('Ctrl Pts',(1.95818071782774,73.0407346133912,12.));
#160002=CARTESIAN_POINT('Ctrl Pts',(1.96860718583945,73.0644334881679,12.));
#160003=CARTESIAN_POINT('Ctrl Pts',(1.97907130550173,73.0881576137415,12.));
#160004=CARTESIAN_POINT('Ctrl Pts',(1.98957308434931,73.1119068786482,12.));
#160005=CARTESIAN_POINT('Ctrl Pts',(2.00011252980988,73.1356811718094,12.));
#160006=CARTESIAN_POINT('Ctrl Pts',(2.01068964920465,73.159480382525,12.));
#160007=CARTESIAN_POINT('Ctrl Pts',(2.02130444974352,73.1833044004612,12.));
#160008=CARTESIAN_POINT('Ctrl Pts',(2.03195693852441,73.2071531156492,12.));
#160009=CARTESIAN_POINT('Ctrl Pts',(2.04264712253916,73.2310264184965,12.));
#160010=CARTESIAN_POINT('Ctrl Pts',(2.05337500867396,73.2549241997946,12.));
#160011=CARTESIAN_POINT('Ctrl Pts',(2.06414060370838,73.2788463507248,12.));
#160012=CARTESIAN_POINT('Ctrl Pts',(2.07494391430955,73.3027927628636,12.));
#160013=CARTESIAN_POINT('Ctrl Pts',(2.08578494702762,73.3267633281822,12.));
#160014=CARTESIAN_POINT('Ctrl Pts',(2.09666370830734,73.3507579390254,12.));
#160015=CARTESIAN_POINT('Ctrl Pts',(2.10758020449401,73.3747764880903,12.));
#160016=CARTESIAN_POINT('Ctrl Pts',(2.11853444183764,73.3988188684022,12.));
#160017=CARTESIAN_POINT('Ctrl Pts',(2.12952642649361,73.4228849732915,12.));
#160018=CARTESIAN_POINT('Ctrl Pts',(2.14055616452049,73.4469746963622,12.));
#160019=CARTESIAN_POINT('Ctrl Pts',(2.151623661879,73.4710879315367,12.));
#160020=CARTESIAN_POINT('Ctrl Pts',(2.16272892442916,73.4952245731044,12.));
#160021=CARTESIAN_POINT('Ctrl Pts',(2.17387195792306,73.5193845157705,12.));
#160022=CARTESIAN_POINT('Ctrl Pts',(2.18505276799757,73.5435676546934,12.));
#160023=CARTESIAN_POINT('Ctrl Pts',(2.19627136015683,73.5677738855461,12.));
#160024=CARTESIAN_POINT('Ctrl Pts',(2.20752773978354,73.5920031044604,12.));
#160025=CARTESIAN_POINT('Ctrl Pts',(2.21882191216522,73.6162552079044,12.));
#160026=CARTESIAN_POINT('Ctrl Pts',(2.2301538825129,73.6405300925714,12.));
#160027=CARTESIAN_POINT('Ctrl Pts',(2.241523655977,73.6648276552766,12.));
#160028=CARTESIAN_POINT('Ctrl Pts',(2.25293123766425,73.6891477928124,12.));
#160029=CARTESIAN_POINT('Ctrl Pts',(2.26437663263664,73.7134904019378,12.));
#160030=CARTESIAN_POINT('Ctrl Pts',(2.27585984587193,73.7378553796792,12.));
#160031=CARTESIAN_POINT('Ctrl Pts',(2.28738088222859,73.7622426235648,12.));
#160032=CARTESIAN_POINT('Ctrl Pts',(2.29893974640436,73.7866520318849,12.));
#160033=CARTESIAN_POINT('Ctrl Pts',(2.31053644289426,73.8110835039341,12.));
#160034=CARTESIAN_POINT('Ctrl Pts',(2.32217097594216,73.8355369402733,12.));
#160035=CARTESIAN_POINT('Ctrl Pts',(2.33384334963981,73.8600122421502,12.));
#160036=CARTESIAN_POINT('Ctrl Pts',(2.34555356802141,73.8845093109302,12.));
#160037=CARTESIAN_POINT('Ctrl Pts',(2.35730163516325,73.9090280474723,12.));
#160038=CARTESIAN_POINT('Ctrl Pts',(2.36908755525995,73.9335683516388,12.));
#160039=CARTESIAN_POINT('Ctrl Pts',(2.38091133274933,73.9581301214609,12.));
#160040=CARTESIAN_POINT('Ctrl Pts',(2.39277297220717,73.9827132538149,12.));
#160041=CARTESIAN_POINT('Ctrl Pts',(2.40467247811497,74.0073176459287,12.));
#160042=CARTESIAN_POINT('Ctrl Pts',(2.41660985465229,74.0319431966956,12.));
#160043=CARTESIAN_POINT('Ctrl Pts',(2.42858510549787,74.0565898079227,12.));
#160044=CARTESIAN_POINT('Ctrl Pts',(2.44059823356722,74.0812573859474,12.));
#160045=CARTESIAN_POINT('Ctrl Pts',(2.45264924094853,74.1059458420175,12.));
#160046=CARTESIAN_POINT('Ctrl Pts',(2.46301176097527,74.1271264545378,12.));
#160047=CARTESIAN_POINT('Ctrl Pts',(2.47097695565715,74.1433763941621,12.));
#160048=CARTESIAN_POINT('Ctrl Pts',(2.47652804725569,74.1546864735452,12.));
#160049=CARTESIAN_POINT('Ctrl Pts',(2.4796539394682,74.1610506466542,12.));
#160050=CARTESIAN_POINT('Ctrl Pts',(2.48034921844894,74.1624659714953,12.));
#160051=CARTESIAN_POINT('',(0.853825826608999,69.9947925310006,0.));
#160052=CARTESIAN_POINT('',(0.853825826608999,69.9947925310006,0.));
#160053=CARTESIAN_POINT('Ctrl Pts',(2.48034921844894,74.1624659714953,0.));
#160054=CARTESIAN_POINT('Ctrl Pts',(2.47965393946819,74.1610506466542,0.));
#160055=CARTESIAN_POINT('Ctrl Pts',(2.47652804725569,74.1546864735452,0.));
#160056=CARTESIAN_POINT('Ctrl Pts',(2.47097695565715,74.1433763941621,0.));
#160057=CARTESIAN_POINT('Ctrl Pts',(2.46301176097527,74.1271264545378,0.));
#160058=CARTESIAN_POINT('Ctrl Pts',(2.45264924094853,74.1059458420175,0.));
#160059=CARTESIAN_POINT('Ctrl Pts',(2.44059823356722,74.0812573859474,0.));
#160060=CARTESIAN_POINT('Ctrl Pts',(2.42858510549787,74.0565898079227,0.));
#160061=CARTESIAN_POINT('Ctrl Pts',(2.41660985465229,74.0319431966956,0.));
#160062=CARTESIAN_POINT('Ctrl Pts',(2.40467247811497,74.0073176459287,0.));
#160063=CARTESIAN_POINT('Ctrl Pts',(2.39277297220717,73.9827132538149,0.));
#160064=CARTESIAN_POINT('Ctrl Pts',(2.38091133274933,73.9581301214609,0.));
#160065=CARTESIAN_POINT('Ctrl Pts',(2.36908755525995,73.9335683516388,0.));
#160066=CARTESIAN_POINT('Ctrl Pts',(2.35730163516325,73.9090280474723,0.));
#160067=CARTESIAN_POINT('Ctrl Pts',(2.34555356802141,73.8845093109302,0.));
#160068=CARTESIAN_POINT('Ctrl Pts',(2.33384334963981,73.8600122421502,0.));
#160069=CARTESIAN_POINT('Ctrl Pts',(2.32217097594216,73.8355369402733,0.));
#160070=CARTESIAN_POINT('Ctrl Pts',(2.31053644289426,73.8110835039341,0.));
#160071=CARTESIAN_POINT('Ctrl Pts',(2.29893974640436,73.7866520318849,0.));
#160072=CARTESIAN_POINT('Ctrl Pts',(2.28738088222859,73.7622426235648,0.));
#160073=CARTESIAN_POINT('Ctrl Pts',(2.27585984587193,73.7378553796792,0.));
#160074=CARTESIAN_POINT('Ctrl Pts',(2.26437663263664,73.7134904019378,0.));
#160075=CARTESIAN_POINT('Ctrl Pts',(2.25293123766425,73.6891477928124,0.));
#160076=CARTESIAN_POINT('Ctrl Pts',(2.241523655977,73.6648276552766,0.));
#160077=CARTESIAN_POINT('Ctrl Pts',(2.2301538825129,73.6405300925714,0.));
#160078=CARTESIAN_POINT('Ctrl Pts',(2.21882191216522,73.6162552079044,0.));
#160079=CARTESIAN_POINT('Ctrl Pts',(2.20752773978354,73.5920031044604,0.));
#160080=CARTESIAN_POINT('Ctrl Pts',(2.19627136015683,73.5677738855461,0.));
#160081=CARTESIAN_POINT('Ctrl Pts',(2.18505276799757,73.5435676546934,0.));
#160082=CARTESIAN_POINT('Ctrl Pts',(2.17387195792306,73.5193845157705,0.));
#160083=CARTESIAN_POINT('Ctrl Pts',(2.16272892442916,73.4952245731044,0.));
#160084=CARTESIAN_POINT('Ctrl Pts',(2.151623661879,73.4710879315367,0.));
#160085=CARTESIAN_POINT('Ctrl Pts',(2.14055616452049,73.4469746963622,0.));
#160086=CARTESIAN_POINT('Ctrl Pts',(2.12952642649361,73.4228849732915,0.));
#160087=CARTESIAN_POINT('Ctrl Pts',(2.11853444183764,73.3988188684022,0.));
#160088=CARTESIAN_POINT('Ctrl Pts',(2.10758020449401,73.3747764880903,0.));
#160089=CARTESIAN_POINT('Ctrl Pts',(2.09666370830734,73.3507579390254,0.));
#160090=CARTESIAN_POINT('Ctrl Pts',(2.08578494702762,73.3267633281822,0.));
#160091=CARTESIAN_POINT('Ctrl Pts',(2.07494391430955,73.3027927628636,0.));
#160092=CARTESIAN_POINT('Ctrl Pts',(2.06414060370838,73.2788463507248,0.));
#160093=CARTESIAN_POINT('Ctrl Pts',(2.05337500867396,73.2549241997946,0.));
#160094=CARTESIAN_POINT('Ctrl Pts',(2.04264712253916,73.2310264184965,0.));
#160095=CARTESIAN_POINT('Ctrl Pts',(2.03195693852441,73.2071531156492,0.));
#160096=CARTESIAN_POINT('Ctrl Pts',(2.02130444974352,73.1833044004612,0.));
#160097=CARTESIAN_POINT('Ctrl Pts',(2.01068964920465,73.159480382525,0.));
#160098=CARTESIAN_POINT('Ctrl Pts',(2.00011252980988,73.1356811718094,0.));
#160099=CARTESIAN_POINT('Ctrl Pts',(1.98957308434931,73.1119068786482,0.));
#160100=CARTESIAN_POINT('Ctrl Pts',(1.97907130550173,73.0881576137415,0.));
#160101=CARTESIAN_POINT('Ctrl Pts',(1.96860718583945,73.0644334881679,0.));
#160102=CARTESIAN_POINT('Ctrl Pts',(1.95818071782774,73.0407346133912,0.));
#160103=CARTESIAN_POINT('Ctrl Pts',(1.94779189382301,73.0170611012659,0.));
#160104=CARTESIAN_POINT('Ctrl Pts',(1.93744070606558,72.9934130640414,0.));
#160105=CARTESIAN_POINT('Ctrl Pts',(1.92712714667649,72.9697906143638,0.));
#160106=CARTESIAN_POINT('Ctrl Pts',(1.91685120766428,72.9461938652816,0.));
#160107=CARTESIAN_POINT('Ctrl Pts',(1.90661288092583,72.9226229302483,0.));
#160108=CARTESIAN_POINT('Ctrl Pts',(1.89641215824585,72.8990779231226,0.));
#160109=CARTESIAN_POINT('Ctrl Pts',(1.88624903129196,72.8755589581674,0.));
#160110=CARTESIAN_POINT('Ctrl Pts',(1.87612349160953,72.8520661500465,0.));
#160111=CARTESIAN_POINT('Ctrl Pts',(1.86603553062777,72.8285996138346,0.));
#160112=CARTESIAN_POINT('Ctrl Pts',(1.85598513966116,72.8051594650214,0.));
#160113=CARTESIAN_POINT('Ctrl Pts',(1.84597230990859,72.7817458195155,0.));
#160114=CARTESIAN_POINT('Ctrl Pts',(1.83599703244927,72.7583587936454,0.));
#160115=CARTESIAN_POINT('Ctrl Pts',(1.82605929823566,72.73499850416,0.));
#160116=CARTESIAN_POINT('Ctrl Pts',(1.81615909809873,72.7116650682347,0.));
#160117=CARTESIAN_POINT('Ctrl Pts',(1.80629642275052,72.6883586034768,0.));
#160118=CARTESIAN_POINT('Ctrl Pts',(1.7964712627836,72.6650792279271,0.));
#160119=CARTESIAN_POINT('Ctrl Pts',(1.78668360866814,72.6418270600623,0.));
#160120=CARTESIAN_POINT('Ctrl Pts',(1.77693345074431,72.618602218792,0.));
#160121=CARTESIAN_POINT('Ctrl Pts',(1.76722077922581,72.5954048234655,0.));
#160122=CARTESIAN_POINT('Ctrl Pts',(1.75754558420351,72.5722349938789,0.));
#160123=CARTESIAN_POINT('Ctrl Pts',(1.74790785564477,72.5490928502773,0.));
#160124=CARTESIAN_POINT('Ctrl Pts',(1.73830758339124,72.5259785133586,0.));
#160125=CARTESIAN_POINT('Ctrl Pts',(1.72874475715099,72.5028921042704,0.));
#160126=CARTESIAN_POINT('Ctrl Pts',(1.71921936650033,72.4798337446162,0.));
#160127=CARTESIAN_POINT('Ctrl Pts',(1.70973140088838,72.4568035564618,0.));
#160128=CARTESIAN_POINT('Ctrl Pts',(1.70028084963648,72.4338016623388,0.));
#160129=CARTESIAN_POINT('Ctrl Pts',(1.69086770193642,72.4108281852473,0.));
#160130=CARTESIAN_POINT('Ctrl Pts',(1.68149194684289,72.3878832486549,0.));
#160131=CARTESIAN_POINT('Ctrl Pts',(1.67215357327373,72.3649669765013,0.));
#160132=CARTESIAN_POINT('Ctrl Pts',(1.66285257001503,72.3420794932052,0.));
#160133=CARTESIAN_POINT('Ctrl Pts',(1.65358892572066,72.3192209236691,0.));
#160134=CARTESIAN_POINT('Ctrl Pts',(1.64436262891079,72.2963913932811,0.));
#160135=CARTESIAN_POINT('Ctrl Pts',(1.63517366796459,72.2735910279149,0.));
#160136=CARTESIAN_POINT('Ctrl Pts',(1.62602203111925,72.2508199539325,0.));
#160137=CARTESIAN_POINT('Ctrl Pts',(1.61690770647536,72.2280782981941,0.));
#160138=CARTESIAN_POINT('Ctrl Pts',(1.60783068199663,72.2053661880611,0.));
#160139=CARTESIAN_POINT('Ctrl Pts',(1.59879094550851,72.1826837514,0.));
#160140=CARTESIAN_POINT('Ctrl Pts',(1.58978848469129,72.1600311165813,0.));
#160141=CARTESIAN_POINT('Ctrl Pts',(1.58082328707809,72.1374084124829,0.));
#160142=CARTESIAN_POINT('Ctrl Pts',(1.57189534006044,72.1148157684987,0.));
#160143=CARTESIAN_POINT('Ctrl Pts',(1.56300463088812,72.092253314543,0.));
#160144=CARTESIAN_POINT('Ctrl Pts',(1.55415114666775,72.0697211810548,0.));
#160145=CARTESIAN_POINT('Ctrl Pts',(1.54533487435627,72.0472194989968,0.));
#160146=CARTESIAN_POINT('Ctrl Pts',(1.53655580075814,72.0247483998582,0.));
#160147=CARTESIAN_POINT('Ctrl Pts',(1.52781391253104,72.0023080156647,0.));
#160148=CARTESIAN_POINT('Ctrl Pts',(1.51910919618568,71.9798984789828,0.));
#160149=CARTESIAN_POINT('Ctrl Pts',(1.51044163808456,71.9575199229241,0.));
#160150=CARTESIAN_POINT('Ctrl Pts',(1.50181122443536,71.935172481145,0.));
#160151=CARTESIAN_POINT('Ctrl Pts',(1.49321794128801,71.9128562878491,0.));
#160152=CARTESIAN_POINT('Ctrl Pts',(1.48466177454022,71.8905714777972,0.));
#160153=CARTESIAN_POINT('Ctrl Pts',(1.47614270993731,71.8683181863123,0.));
#160154=CARTESIAN_POINT('Ctrl Pts',(1.4676607330709,71.8460965492836,0.));
#160155=CARTESIAN_POINT('Ctrl Pts',(1.4592158293723,71.8239067031664,0.));
#160156=CARTESIAN_POINT('Ctrl Pts',(1.45080798410958,71.8017487849865,0.));
#160157=CARTESIAN_POINT('Ctrl Pts',(1.44243718239306,71.7796229323496,0.));
#160158=CARTESIAN_POINT('Ctrl Pts',(1.4341034091749,71.7575292834456,0.));
#160159=CARTESIAN_POINT('Ctrl Pts',(1.42580664924775,71.7354679770537,0.));
#160160=CARTESIAN_POINT('Ctrl Pts',(1.41754688723792,71.7134391525417,0.));
#160161=CARTESIAN_POINT('Ctrl Pts',(1.40932410760276,71.6914429498702,0.));
#160162=CARTESIAN_POINT('Ctrl Pts',(1.401138294636,71.6694795096034,0.));
#160163=CARTESIAN_POINT('Ctrl Pts',(1.39298943246732,71.6475489729149,0.));
#160164=CARTESIAN_POINT('Ctrl Pts',(1.38487750506077,71.6256514815918,0.));
#160165=CARTESIAN_POINT('Ctrl Pts',(1.37680249620764,71.6037871780347,0.));
#160166=CARTESIAN_POINT('Ctrl Pts',(1.3687643895245,71.5819562052613,0.));
#160167=CARTESIAN_POINT('Ctrl Pts',(1.36076316845807,71.5601587069175,0.));
#160168=CARTESIAN_POINT('Ctrl Pts',(1.35279881628454,71.538394827283,0.));
#160169=CARTESIAN_POINT('Ctrl Pts',(1.34487131610786,71.5166647112766,0.));
#160170=CARTESIAN_POINT('Ctrl Pts',(1.33698065085229,71.4949685044559,0.));
#160171=CARTESIAN_POINT('Ctrl Pts',(1.32912680326132,71.4733063530227,0.));
#160172=CARTESIAN_POINT('Ctrl Pts',(1.32130975590232,71.4516784038346,0.));
#160173=CARTESIAN_POINT('Ctrl Pts',(1.31352949116539,71.4300848044095,0.));
#160174=CARTESIAN_POINT('Ctrl Pts',(1.3057859912614,71.4085257029308,0.));
#160175=CARTESIAN_POINT('Ctrl Pts',(1.29807923821415,71.3870012482474,0.));
#160176=CARTESIAN_POINT('Ctrl Pts',(1.29040921386062,71.3655115898801,0.));
#160177=CARTESIAN_POINT('Ctrl Pts',(1.28277589985475,71.344056878033,0.));
#160178=CARTESIAN_POINT('Ctrl Pts',(1.27517927766612,71.3226372635993,0.));
#160179=CARTESIAN_POINT('Ctrl Pts',(1.26761932857724,71.301252898167,0.));
#160180=CARTESIAN_POINT('Ctrl Pts',(1.26009603367565,71.2799039340191,0.));
#160181=CARTESIAN_POINT('Ctrl Pts',(1.25260937385562,71.2585905241422,0.));
#160182=CARTESIAN_POINT('Ctrl Pts',(1.24515932982109,71.2373128222359,0.));
#160183=CARTESIAN_POINT('Ctrl Pts',(1.23774588208428,71.2160709827189,0.));
#160184=CARTESIAN_POINT('Ctrl Pts',(1.23036901096247,71.1948651607319,0.));
#160185=CARTESIAN_POINT('Ctrl Pts',(1.22302869657029,71.1736955121361,0.));
#160186=CARTESIAN_POINT('Ctrl Pts',(1.21572491882274,71.1525621935266,0.));
#160187=CARTESIAN_POINT('Ctrl Pts',(1.20845765743655,71.1314653622442,0.));
#160188=CARTESIAN_POINT('Ctrl Pts',(1.20122689192837,71.1104051763839,0.));
#160189=CARTESIAN_POINT('Ctrl Pts',(1.19403260160998,71.089381794801,0.));
#160190=CARTESIAN_POINT('Ctrl Pts',(1.18687476558127,71.0683953771147,0.));
#160191=CARTESIAN_POINT('Ctrl Pts',(1.179753362735,71.0474460837157,0.));
#160192=CARTESIAN_POINT('Ctrl Pts',(1.17266837175777,71.0265340757697,0.));
#160193=CARTESIAN_POINT('Ctrl Pts',(1.16561977112883,71.0056595152204,0.));
#160194=CARTESIAN_POINT('Ctrl Pts',(1.15860753911491,70.9848225647876,0.));
#160195=CARTESIAN_POINT('Ctrl Pts',(1.15163165376531,70.9640233879671,0.));
#160196=CARTESIAN_POINT('Ctrl Pts',(1.14469209291495,70.943262149058,0.));
#160197=CARTESIAN_POINT('Ctrl Pts',(1.13778883418217,70.9225390131835,0.));
#160198=CARTESIAN_POINT('Ctrl Pts',(1.13092185496564,70.9018541463083,0.));
#160199=CARTESIAN_POINT('Ctrl Pts',(1.12409113243512,70.8812077152564,0.));
#160200=CARTESIAN_POINT('Ctrl Pts',(1.11729664352991,70.860599887712,0.));
#160201=CARTESIAN_POINT('Ctrl Pts',(1.11053836496639,70.8400308322013,0.));
#160202=CARTESIAN_POINT('Ctrl Pts',(1.10381627323946,70.8195007180739,0.));
#160203=CARTESIAN_POINT('Ctrl Pts',(1.09713034462271,70.7990097154855,0.));
#160204=CARTESIAN_POINT('Ctrl Pts',(1.09048055516435,70.7785579953611,0.));
#160205=CARTESIAN_POINT('Ctrl Pts',(1.08386688068349,70.7581457294475,0.));
#160206=CARTESIAN_POINT('Ctrl Pts',(1.07728929676413,70.7377730903971,0.));
#160207=CARTESIAN_POINT('Ctrl Pts',(1.07074777874597,70.7174402518378,0.));
#160208=CARTESIAN_POINT('Ctrl Pts',(1.06424230171281,70.6971473884443,0.));
#160209=CARTESIAN_POINT('Ctrl Pts',(1.05777284047728,70.6768946760063,0.));
#160210=CARTESIAN_POINT('Ctrl Pts',(1.0513393696007,70.6566822912965,0.));
#160211=CARTESIAN_POINT('Ctrl Pts',(1.04494186341157,70.6365104119238,0.));
#160212=CARTESIAN_POINT('Ctrl Pts',(1.03858029601906,70.6163792162079,0.));
#160213=CARTESIAN_POINT('Ctrl Pts',(1.03225464132873,70.5962888829958,0.));
#160214=CARTESIAN_POINT('Ctrl Pts',(1.0259648730405,70.5762395916412,0.));
#160215=CARTESIAN_POINT('Ctrl Pts',(1.019710964606,70.5562315224219,0.));
#160216=CARTESIAN_POINT('Ctrl Pts',(1.01349288918541,70.5362648569072,0.));
#160217=CARTESIAN_POINT('Ctrl Pts',(1.00731061960968,70.5163397782699,0.));
#160218=CARTESIAN_POINT('Ctrl Pts',(1.00116412831439,70.4964564717917,0.));
#160219=CARTESIAN_POINT('Ctrl Pts',(0.995053387379687,70.476615124517,0.));
#160220=CARTESIAN_POINT('Ctrl Pts',(0.988978368643597,70.4568159243131,
0.));
#160221=CARTESIAN_POINT('Ctrl Pts',(0.982939043792167,70.4370590590839,
0.));
#160222=CARTESIAN_POINT('Ctrl Pts',(0.976935384450135,70.41734471596,0.));
#160223=CARTESIAN_POINT('Ctrl Pts',(0.97096736228131,70.3976730803664,0.));
#160224=CARTESIAN_POINT('Ctrl Pts',(0.965034948786566,70.3780443378003,
0.));
#160225=CARTESIAN_POINT('Ctrl Pts',(0.959138115058893,70.3584586759561,
0.));
#160226=CARTESIAN_POINT('Ctrl Pts',(0.953276831581241,70.338916286457,0.));
#160227=CARTESIAN_POINT('Ctrl Pts',(0.94745106792957,70.3194173673635,0.));
#160228=CARTESIAN_POINT('Ctrl Pts',(0.941660792742961,70.2999621233938,
0.));
#160229=CARTESIAN_POINT('Ctrl Pts',(0.935905974336497,70.2805507606832,
0.));
#160230=CARTESIAN_POINT('Ctrl Pts',(0.930186581235583,70.2611834821711,
0.));
#160231=CARTESIAN_POINT('Ctrl Pts',(0.924502582639459,70.241860483586,0.));
#160232=CARTESIAN_POINT('Ctrl Pts',(0.918853949157051,70.2225819470306,
0.));
#160233=CARTESIAN_POINT('Ctrl Pts',(0.913240652090848,70.2033480471749,
0.));
#160234=CARTESIAN_POINT('Ctrl Pts',(0.907662662015657,70.184158963563,0.));
#160235=CARTESIAN_POINT('Ctrl Pts',(0.902119947629781,70.1650148905109,
0.));
#160236=CARTESIAN_POINT('Ctrl Pts',(0.896612474372092,70.1459160490366,
0.));
#160237=CARTESIAN_POINT('Ctrl Pts',(0.891140203464733,70.1268626950031,
0.));
#160238=CARTESIAN_POINT('Ctrl Pts',(0.885703094803093,70.1078550938801,
0.));
#160239=CARTESIAN_POINT('Ctrl Pts',(0.880301109661046,70.0888934967772,
0.));
#160240=CARTESIAN_POINT('Ctrl Pts',(0.874934213255579,70.0699781184013,
0.));
#160241=CARTESIAN_POINT('Ctrl Pts',(0.869602377870148,70.0511091083285,
0.));
#160242=CARTESIAN_POINT('Ctrl Pts',(0.864305583660099,70.0322865493339,
0.));
#160243=CARTESIAN_POINT('Ctrl Pts',(0.860096170667407,70.0172656934192,
0.));
#160244=CARTESIAN_POINT('Ctrl Pts',(0.85695487025838,70.0060209754332,0.));
#160245=CARTESIAN_POINT('Ctrl Pts',(0.8548676738483,69.9985337959499,0.));
#160246=CARTESIAN_POINT('Ctrl Pts',(0.853825826608999,69.9947925310006,
0.));
#160247=CARTESIAN_POINT('Ctrl Pts',(9.10443154852689,73.9415940197274,0.));
#160248=CARTESIAN_POINT('Ctrl Pts',(9.10443154852689,73.9415940197274,12.));
#160249=CARTESIAN_POINT('Ctrl Pts',(9.10148558516538,73.9368365074299,0.));
#160250=CARTESIAN_POINT('Ctrl Pts',(9.10148558516538,73.9368365074299,12.));
#160251=CARTESIAN_POINT('Ctrl Pts',(9.09559760529043,73.9273231219835,0.));
#160252=CARTESIAN_POINT('Ctrl Pts',(9.09559760529043,73.9273231219835,12.));
#160253=CARTESIAN_POINT('Ctrl Pts',(9.08677747602206,73.9130579612604,0.));
#160254=CARTESIAN_POINT('Ctrl Pts',(9.08677747602206,73.9130579612604,12.));
#160255=CARTESIAN_POINT('Ctrl Pts',(9.07504098571708,73.8940475822492,0.));
#160256=CARTESIAN_POINT('Ctrl Pts',(9.07504098571708,73.8940475822492,12.));
#160257=CARTESIAN_POINT('Ctrl Pts',(9.06040984890247,73.8703010078091,0.));
#160258=CARTESIAN_POINT('Ctrl Pts',(9.06040984890247,73.8703010078091,12.));
#160259=CARTESIAN_POINT('Ctrl Pts',(9.04581819646985,73.8465708501057,0.));
#160260=CARTESIAN_POINT('Ctrl Pts',(9.04581819646985,73.8465708501057,12.));
#160261=CARTESIAN_POINT('Ctrl Pts',(9.03126603778126,73.8228571411697,0.));
#160262=CARTESIAN_POINT('Ctrl Pts',(9.03126603778126,73.8228571411697,12.));
#160263=CARTESIAN_POINT('Ctrl Pts',(9.01675338208005,73.7991599312592,0.));
#160264=CARTESIAN_POINT('Ctrl Pts',(9.01675338208005,73.7991599312592,12.));
#160265=CARTESIAN_POINT('Ctrl Pts',(9.00228023701056,73.7754792943665,0.));
#160266=CARTESIAN_POINT('Ctrl Pts',(9.00228023701056,73.7754792943665,12.));
#160267=CARTESIAN_POINT('Ctrl Pts',(8.98784660837398,73.7518153261981,0.));
#160268=CARTESIAN_POINT('Ctrl Pts',(8.98784660837398,73.7518153261981,12.));
#160269=CARTESIAN_POINT('Ctrl Pts',(8.97345250083601,73.728168136383,0.));
#160270=CARTESIAN_POINT('Ctrl Pts',(8.97345250083601,73.728168136383,12.));
#160271=CARTESIAN_POINT('Ctrl Pts',(8.95909791836153,73.7045378422686,0.));
#160272=CARTESIAN_POINT('Ctrl Pts',(8.95909791836153,73.7045378422686,12.));
#160273=CARTESIAN_POINT('Ctrl Pts',(8.9447828647442,73.6809245622383,0.));
#160274=CARTESIAN_POINT('Ctrl Pts',(8.9447828647442,73.6809245622383,12.));
#160275=CARTESIAN_POINT('Ctrl Pts',(8.93050734412125,73.6573284088184,0.));
#160276=CARTESIAN_POINT('Ctrl Pts',(8.93050734412125,73.6573284088184,12.));
#160277=CARTESIAN_POINT('Ctrl Pts',(8.91627136140085,73.633749483097,0.));
#160278=CARTESIAN_POINT('Ctrl Pts',(8.91627136140085,73.633749483097,12.));
#160279=CARTESIAN_POINT('Ctrl Pts',(8.90207492199043,73.6101878785976,0.));
#160280=CARTESIAN_POINT('Ctrl Pts',(8.90207492199043,73.6101878785976,12.));
#160281=CARTESIAN_POINT('Ctrl Pts',(8.88791803160443,73.5866436840556,0.));
#160282=CARTESIAN_POINT('Ctrl Pts',(8.88791803160443,73.5866436840556,12.));
#160283=CARTESIAN_POINT('Ctrl Pts',(8.87380069602971,73.5631169867122,0.));
#160284=CARTESIAN_POINT('Ctrl Pts',(8.87380069602971,73.5631169867122,12.));
#160285=CARTESIAN_POINT('Ctrl Pts',(8.85972292092131,73.5396078751639,0.));
#160286=CARTESIAN_POINT('Ctrl Pts',(8.85972292092131,73.5396078751639,12.));
#160287=CARTESIAN_POINT('Ctrl Pts',(8.84568471153806,73.5161164429709,0.));
#160288=CARTESIAN_POINT('Ctrl Pts',(8.84568471153806,73.5161164429709,12.));
#160289=CARTESIAN_POINT('Ctrl Pts',(8.83168607277326,73.492642788273,0.));
#160290=CARTESIAN_POINT('Ctrl Pts',(8.83168607277326,73.492642788273,12.));
#160291=CARTESIAN_POINT('Ctrl Pts',(8.81772700927531,73.4691870121567,0.));
#160292=CARTESIAN_POINT('Ctrl Pts',(8.81772700927531,73.4691870121567,12.));
#160293=CARTESIAN_POINT('Ctrl Pts',(8.80380752553692,73.4457492173933,0.));
#160294=CARTESIAN_POINT('Ctrl Pts',(8.80380752553692,73.4457492173933,12.));
#160295=CARTESIAN_POINT('Ctrl Pts',(8.78992762598757,73.422329507113,0.));
#160296=CARTESIAN_POINT('Ctrl Pts',(8.78992762598757,73.422329507113,12.));
#160297=CARTESIAN_POINT('Ctrl Pts',(8.77608731509348,73.3989279832835,0.));
#160298=CARTESIAN_POINT('Ctrl Pts',(8.77608731509348,73.3989279832835,12.));
#160299=CARTESIAN_POINT('Ctrl Pts',(8.76228659740358,73.3755447460269,0.));
#160300=CARTESIAN_POINT('Ctrl Pts',(8.76228659740358,73.3755447460269,12.));
#160301=CARTESIAN_POINT('Ctrl Pts',(8.74852547749778,73.3521798944622,0.));
#160302=CARTESIAN_POINT('Ctrl Pts',(8.74852547749778,73.3521798944622,12.));
#160303=CARTESIAN_POINT('Ctrl Pts',(8.7348039599538,73.3288335272002,0.));
#160304=CARTESIAN_POINT('Ctrl Pts',(8.7348039599538,73.3288335272002,12.));
#160305=CARTESIAN_POINT('Ctrl Pts',(8.72112204930232,73.3055057429742,0.));
#160306=CARTESIAN_POINT('Ctrl Pts',(8.72112204930232,73.3055057429742,12.));
#160307=CARTESIAN_POINT('Ctrl Pts',(8.7074797499823,73.2821966412148,0.));
#160308=CARTESIAN_POINT('Ctrl Pts',(8.7074797499823,73.2821966412148,12.));
#160309=CARTESIAN_POINT('Ctrl Pts',(8.69387706629286,73.2589063226358,0.));
#160310=CARTESIAN_POINT('Ctrl Pts',(8.69387706629286,73.2589063226358,12.));
#160311=CARTESIAN_POINT('Ctrl Pts',(8.68031400241872,73.2356348889693,0.));
#160312=CARTESIAN_POINT('Ctrl Pts',(8.68031400241872,73.2356348889693,12.));
#160313=CARTESIAN_POINT('Ctrl Pts',(8.66679056245092,73.2123824427208,0.));
#160314=CARTESIAN_POINT('Ctrl Pts',(8.66679056245092,73.2123824427208,12.));
#160315=CARTESIAN_POINT('Ctrl Pts',(8.65330675040537,73.1891490869056,0.));
#160316=CARTESIAN_POINT('Ctrl Pts',(8.65330675040537,73.1891490869056,12.));
#160317=CARTESIAN_POINT('Ctrl Pts',(8.63986257023739,73.1659349248133,0.));
#160318=CARTESIAN_POINT('Ctrl Pts',(8.63986257023739,73.1659349248133,12.));
#160319=CARTESIAN_POINT('Ctrl Pts',(8.62645802585484,73.1427400597037,0.));
#160320=CARTESIAN_POINT('Ctrl Pts',(8.62645802585484,73.1427400597037,12.));
#160321=CARTESIAN_POINT('Ctrl Pts',(8.61309312112002,73.1195645948178,0.));
#160322=CARTESIAN_POINT('Ctrl Pts',(8.61309312112002,73.1195645948178,12.));
#160323=CARTESIAN_POINT('Ctrl Pts',(8.59976785984552,73.0964086335235,0.));
#160324=CARTESIAN_POINT('Ctrl Pts',(8.59976785984552,73.0964086335235,12.));
#160325=CARTESIAN_POINT('Ctrl Pts',(8.58648224578732,73.0732722794195,0.));
#160326=CARTESIAN_POINT('Ctrl Pts',(8.58648224578732,73.0732722794195,12.));
#160327=CARTESIAN_POINT('Ctrl Pts',(8.57323628263593,73.0501556364479,0.));
#160328=CARTESIAN_POINT('Ctrl Pts',(8.57323628263593,73.0501556364479,12.));
#160329=CARTESIAN_POINT('Ctrl Pts',(8.56002997400084,73.0270588090183,0.));
#160330=CARTESIAN_POINT('Ctrl Pts',(8.56002997400084,73.0270588090183,12.));
#160331=CARTESIAN_POINT('Ctrl Pts',(8.54686332340418,73.0039819020648,0.));
#160332=CARTESIAN_POINT('Ctrl Pts',(8.54686332340418,73.0039819020648,12.));
#160333=CARTESIAN_POINT('Ctrl Pts',(8.53373633429281,72.9809250209828,0.));
#160334=CARTESIAN_POINT('Ctrl Pts',(8.53373633429281,72.9809250209828,12.));
#160335=CARTESIAN_POINT('Ctrl Pts',(8.52064901004228,72.9578882715912,0.));
#160336=CARTESIAN_POINT('Ctrl Pts',(8.52064901004228,72.9578882715912,12.));
#160337=CARTESIAN_POINT('Ctrl Pts',(8.50760135395984,72.9348717600838,0.));
#160338=CARTESIAN_POINT('Ctrl Pts',(8.50760135395984,72.9348717600838,12.));
#160339=CARTESIAN_POINT('Ctrl Pts',(8.49459336928296,72.9118755929795,0.));
#160340=CARTESIAN_POINT('Ctrl Pts',(8.49459336928296,72.9118755929795,12.));
#160341=CARTESIAN_POINT('Ctrl Pts',(8.48162505917658,72.8888998770785,0.));
#160342=CARTESIAN_POINT('Ctrl Pts',(8.48162505917658,72.8888998770785,12.));
#160343=CARTESIAN_POINT('Ctrl Pts',(8.46869642673795,72.8659447194933,0.));
#160344=CARTESIAN_POINT('Ctrl Pts',(8.46869642673795,72.8659447194933,12.));
#160345=CARTESIAN_POINT('Ctrl Pts',(8.45580747499793,72.8430102276713,0.));
#160346=CARTESIAN_POINT('Ctrl Pts',(8.45580747499793,72.8430102276713,12.));
#160347=CARTESIAN_POINT('Ctrl Pts',(8.44295820691912,72.8200965094199,0.));
#160348=CARTESIAN_POINT('Ctrl Pts',(8.44295820691912,72.8200965094199,12.));
#160349=CARTESIAN_POINT('Ctrl Pts',(8.43014862539158,72.7972036729276,0.));
#160350=CARTESIAN_POINT('Ctrl Pts',(8.43014862539158,72.7972036729276,12.));
#160351=CARTESIAN_POINT('Ctrl Pts',(8.4173787332233,72.7743318267865,0.));
#160352=CARTESIAN_POINT('Ctrl Pts',(8.4173787332233,72.7743318267865,12.));
#160353=CARTESIAN_POINT('Ctrl Pts',(8.40464853314469,72.751481079992,0.));
#160354=CARTESIAN_POINT('Ctrl Pts',(8.40464853314469,72.751481079992,12.));
#160355=CARTESIAN_POINT('Ctrl Pts',(8.39195802781391,72.7286515419373,0.));
#160356=CARTESIAN_POINT('Ctrl Pts',(8.39195802781391,72.7286515419373,12.));
#160357=CARTESIAN_POINT('Ctrl Pts',(8.37930721981731,72.705843322407,0.));
#160358=CARTESIAN_POINT('Ctrl Pts',(8.37930721981731,72.705843322407,12.));
#160359=CARTESIAN_POINT('Ctrl Pts',(8.36669611166843,72.6830565315703,0.));
#160360=CARTESIAN_POINT('Ctrl Pts',(8.36669611166843,72.6830565315703,12.));
#160361=CARTESIAN_POINT('Ctrl Pts',(8.35412470580102,72.6602912799696,0.));
#160362=CARTESIAN_POINT('Ctrl Pts',(8.35412470580102,72.6602912799696,12.));
#160363=CARTESIAN_POINT('Ctrl Pts',(8.34159300456987,72.6375476785215,0.));
#160364=CARTESIAN_POINT('Ctrl Pts',(8.34159300456987,72.6375476785215,12.));
#160365=CARTESIAN_POINT('Ctrl Pts',(8.32910101025671,72.6148258385296,0.));
#160366=CARTESIAN_POINT('Ctrl Pts',(8.32910101025671,72.6148258385296,12.));
#160367=CARTESIAN_POINT('Ctrl Pts',(8.31664872507017,72.5921258716901,0.));
#160368=CARTESIAN_POINT('Ctrl Pts',(8.31664872507017,72.5921258716901,12.));
#160369=CARTESIAN_POINT('Ctrl Pts',(8.30423615114453,72.5694478900982,0.));
#160370=CARTESIAN_POINT('Ctrl Pts',(8.30423615114453,72.5694478900982,12.));
#160371=CARTESIAN_POINT('Ctrl Pts',(8.29186329053279,72.5467920062521,0.));
#160372=CARTESIAN_POINT('Ctrl Pts',(8.29186329053279,72.5467920062521,12.));
#160373=CARTESIAN_POINT('Ctrl Pts',(8.27953014520376,72.5241583330562,0.));
#160374=CARTESIAN_POINT('Ctrl Pts',(8.27953014520376,72.5241583330562,12.));
#160375=CARTESIAN_POINT('Ctrl Pts',(8.2672367170492,72.5015469838254,0.));
#160376=CARTESIAN_POINT('Ctrl Pts',(8.2672367170492,72.5015469838254,12.));
#160377=CARTESIAN_POINT('Ctrl Pts',(8.25498300788494,72.4789580722875,0.));
#160378=CARTESIAN_POINT('Ctrl Pts',(8.25498300788494,72.4789580722875,12.));
#160379=CARTESIAN_POINT('Ctrl Pts',(8.2427690194504,72.4563917125842,0.));
#160380=CARTESIAN_POINT('Ctrl Pts',(8.2427690194504,72.4563917125842,12.));
#160381=CARTESIAN_POINT('Ctrl Pts',(8.23059475340357,72.4338480192695,0.));
#160382=CARTESIAN_POINT('Ctrl Pts',(8.23059475340357,72.4338480192695,12.));
#160383=CARTESIAN_POINT('Ctrl Pts',(8.21846021131561,72.4113271073079,0.));
#160384=CARTESIAN_POINT('Ctrl Pts',(8.21846021131561,72.4113271073079,12.));
#160385=CARTESIAN_POINT('Ctrl Pts',(8.20636539467776,72.3888290920832,0.));
#160386=CARTESIAN_POINT('Ctrl Pts',(8.20636539467776,72.3888290920832,12.));
#160387=CARTESIAN_POINT('Ctrl Pts',(8.19431030490315,72.3663540894026,0.));
#160388=CARTESIAN_POINT('Ctrl Pts',(8.19431030490315,72.3663540894026,12.));
#160389=CARTESIAN_POINT('Ctrl Pts',(8.18229494332624,72.3439022155007,0.));
#160390=CARTESIAN_POINT('Ctrl Pts',(8.18229494332624,72.3439022155007,12.));
#160391=CARTESIAN_POINT('Ctrl Pts',(8.17031931119891,72.3214735870409,0.));
#160392=CARTESIAN_POINT('Ctrl Pts',(8.17031931119891,72.3214735870409,12.));
#160393=CARTESIAN_POINT('Ctrl Pts',(8.15838340968336,72.2990683211162,0.));
#160394=CARTESIAN_POINT('Ctrl Pts',(8.15838340968336,72.2990683211162,12.));
#160395=CARTESIAN_POINT('Ctrl Pts',(8.14648723985798,72.2766865352555,0.));
#160396=CARTESIAN_POINT('Ctrl Pts',(8.14648723985798,72.2766865352555,12.));
#160397=CARTESIAN_POINT('Ctrl Pts',(8.13463080272029,72.2543283474278,0.));
#160398=CARTESIAN_POINT('Ctrl Pts',(8.13463080272029,72.2543283474278,12.));
#160399=CARTESIAN_POINT('Ctrl Pts',(8.12281409918661,72.2319938760449,0.));
#160400=CARTESIAN_POINT('Ctrl Pts',(8.12281409918661,72.2319938760449,12.));
#160401=CARTESIAN_POINT('Ctrl Pts',(8.11103713008928,72.209683239963,0.));
#160402=CARTESIAN_POINT('Ctrl Pts',(8.11103713008928,72.209683239963,12.));
#160403=CARTESIAN_POINT('Ctrl Pts',(8.0992998961689,72.1873965584813,0.));
#160404=CARTESIAN_POINT('Ctrl Pts',(8.0992998961689,72.1873965584813,12.));
#160405=CARTESIAN_POINT('Ctrl Pts',(8.08760239807837,72.1651339513477,0.));
#160406=CARTESIAN_POINT('Ctrl Pts',(8.08760239807837,72.1651339513477,12.));
#160407=CARTESIAN_POINT('Ctrl Pts',(8.07594463638719,72.1428955387663,0.));
#160408=CARTESIAN_POINT('Ctrl Pts',(8.07594463638719,72.1428955387663,12.));
#160409=CARTESIAN_POINT('Ctrl Pts',(8.06432661158096,72.1206814413988,0.));
#160410=CARTESIAN_POINT('Ctrl Pts',(8.06432661158096,72.1206814413988,12.));
#160411=CARTESIAN_POINT('Ctrl Pts',(8.05274832405949,72.0984917803693,0.));
#160412=CARTESIAN_POINT('Ctrl Pts',(8.05274832405949,72.0984917803693,12.));
#160413=CARTESIAN_POINT('Ctrl Pts',(8.04120977412872,72.0763266772615,0.));
#160414=CARTESIAN_POINT('Ctrl Pts',(8.04120977412872,72.0763266772615,12.));
#160415=CARTESIAN_POINT('Ctrl Pts',(8.02971096200308,72.0541862541243,0.));
#160416=CARTESIAN_POINT('Ctrl Pts',(8.02971096200308,72.0541862541243,12.));
#160417=CARTESIAN_POINT('Ctrl Pts',(8.01825188781057,72.032070633479,0.));
#160418=CARTESIAN_POINT('Ctrl Pts',(8.01825188781057,72.032070633479,12.));
#160419=CARTESIAN_POINT('Ctrl Pts',(8.00683255159248,72.0099799383213,0.));
#160420=CARTESIAN_POINT('Ctrl Pts',(8.00683255159248,72.0099799383213,12.));
#160421=CARTESIAN_POINT('Ctrl Pts',(7.99545295330191,71.9879142921254,0.));
#160422=CARTESIAN_POINT('Ctrl Pts',(7.99545295330191,71.9879142921254,12.));
#160423=CARTESIAN_POINT('Ctrl Pts',(7.98411309279613,71.965873818843,0.));
#160424=CARTESIAN_POINT('Ctrl Pts',(7.98411309279613,71.965873818843,12.));
#160425=CARTESIAN_POINT('Ctrl Pts',(7.97281296983718,71.9438586429081,0.));
#160426=CARTESIAN_POINT('Ctrl Pts',(7.97281296983718,71.9438586429081,12.));
#160427=CARTESIAN_POINT('Ctrl Pts',(7.96155258409764,71.9218688892431,0.));
#160428=CARTESIAN_POINT('Ctrl Pts',(7.96155258409764,71.9218688892431,12.));
#160429=CARTESIAN_POINT('Ctrl Pts',(7.95033193516051,71.8999046832643,0.));
#160430=CARTESIAN_POINT('Ctrl Pts',(7.95033193516051,71.8999046832643,12.));
#160431=CARTESIAN_POINT('Ctrl Pts',(7.93915102251795,71.8779661508832,0.));
#160432=CARTESIAN_POINT('Ctrl Pts',(7.93915102251795,71.8779661508832,12.));
#160433=CARTESIAN_POINT('Ctrl Pts',(7.92800984556396,71.8560534185071,0.));
#160434=CARTESIAN_POINT('Ctrl Pts',(7.92800984556396,71.8560534185071,12.));
#160435=CARTESIAN_POINT('Ctrl Pts',(7.91690840359367,71.8341666130426,0.));
#160436=CARTESIAN_POINT('Ctrl Pts',(7.91690840359367,71.8341666130426,12.));
#160437=CARTESIAN_POINT('Ctrl Pts',(7.90584669580956,71.8123058619042,0.));
#160438=CARTESIAN_POINT('Ctrl Pts',(7.90584669580956,71.8123058619042,12.));
#160439=CARTESIAN_POINT('Ctrl Pts',(7.89482472132137,71.7904712930175,0.));
#160440=CARTESIAN_POINT('Ctrl Pts',(7.89482472132137,71.7904712930175,12.));
#160441=CARTESIAN_POINT('Ctrl Pts',(7.88384247914524,71.7686630348238,0.));
#160442=CARTESIAN_POINT('Ctrl Pts',(7.88384247914524,71.7686630348238,12.));
#160443=CARTESIAN_POINT('Ctrl Pts',(7.87289996819654,71.7468812162788,0.));
#160444=CARTESIAN_POINT('Ctrl Pts',(7.87289996819654,71.7468812162788,12.));
#160445=CARTESIAN_POINT('Ctrl Pts',(7.86199718728826,71.7251259668563,0.));
#160446=CARTESIAN_POINT('Ctrl Pts',(7.86199718728826,71.7251259668563,12.));
#160447=CARTESIAN_POINT('Ctrl Pts',(7.85113413513736,71.7033974165568,0.));
#160448=CARTESIAN_POINT('Ctrl Pts',(7.85113413513736,71.7033974165568,12.));
#160449=CARTESIAN_POINT('Ctrl Pts',(7.8403108103649,71.6816956959117,0.));
#160450=CARTESIAN_POINT('Ctrl Pts',(7.8403108103649,71.6816956959117,12.));
#160451=CARTESIAN_POINT('Ctrl Pts',(7.82952721149508,71.6600209359872,0.));
#160452=CARTESIAN_POINT('Ctrl Pts',(7.82952721149508,71.6600209359872,12.));
#160453=CARTESIAN_POINT('Ctrl Pts',(7.81878333694861,71.6383732683844,0.));
#160454=CARTESIAN_POINT('Ctrl Pts',(7.81878333694861,71.6383732683844,12.));
#160455=CARTESIAN_POINT('Ctrl Pts',(7.80807918504022,71.6167528252423,0.));
#160456=CARTESIAN_POINT('Ctrl Pts',(7.80807918504022,71.6167528252423,12.));
#160457=CARTESIAN_POINT('Ctrl Pts',(7.79741475398514,71.5951597392471,0.));
#160458=CARTESIAN_POINT('Ctrl Pts',(7.79741475398514,71.5951597392471,12.));
#160459=CARTESIAN_POINT('Ctrl Pts',(7.78679004189935,71.5735941436364,0.));
#160460=CARTESIAN_POINT('Ctrl Pts',(7.78679004189935,71.5735941436364,12.));
#160461=CARTESIAN_POINT('Ctrl Pts',(7.7762050467987,71.5520561722039,0.));
#160462=CARTESIAN_POINT('Ctrl Pts',(7.7762050467987,71.5520561722039,12.));
#160463=CARTESIAN_POINT('Ctrl Pts',(7.76565976659226,71.5305459592994,0.));
#160464=CARTESIAN_POINT('Ctrl Pts',(7.76565976659226,71.5305459592994,12.));
#160465=CARTESIAN_POINT('Ctrl Pts',(7.75515419907967,71.5090636398318,0.));
#160466=CARTESIAN_POINT('Ctrl Pts',(7.75515419907967,71.5090636398318,12.));
#160467=CARTESIAN_POINT('Ctrl Pts',(7.74468834195746,71.4876093492781,0.));
#160468=CARTESIAN_POINT('Ctrl Pts',(7.74468834195746,71.4876093492781,12.));
#160469=CARTESIAN_POINT('Ctrl Pts',(7.7342621928194,71.4661832236888,0.));
#160470=CARTESIAN_POINT('Ctrl Pts',(7.7342621928194,71.4661832236888,12.));
#160471=CARTESIAN_POINT('Ctrl Pts',(7.72387574915544,71.4447853996916,0.));
#160472=CARTESIAN_POINT('Ctrl Pts',(7.72387574915544,71.4447853996916,12.));
#160473=CARTESIAN_POINT('Ctrl Pts',(7.7135290083452,71.4234160144925,0.));
#160474=CARTESIAN_POINT('Ctrl Pts',(7.7135290083452,71.4234160144925,12.));
#160475=CARTESIAN_POINT('Ctrl Pts',(7.70322196765539,71.4020752058796,0.));
#160476=CARTESIAN_POINT('Ctrl Pts',(7.70322196765539,71.4020752058796,12.));
#160477=CARTESIAN_POINT('Ctrl Pts',(7.69295462424612,71.3807631122331,0.));
#160478=CARTESIAN_POINT('Ctrl Pts',(7.69295462424612,71.3807631122331,12.));
#160479=CARTESIAN_POINT('Ctrl Pts',(7.68272697517086,71.3594798725281,0.));
#160480=CARTESIAN_POINT('Ctrl Pts',(7.68272697517086,71.3594798725281,12.));
#160481=CARTESIAN_POINT('Ctrl Pts',(7.67253901737553,71.3382256263414,0.));
#160482=CARTESIAN_POINT('Ctrl Pts',(7.67253901737553,71.3382256263414,12.));
#160483=CARTESIAN_POINT('Ctrl Pts',(7.66239074769163,71.3170005138502,0.));
#160484=CARTESIAN_POINT('Ctrl Pts',(7.66239074769163,71.3170005138502,12.));
#160485=CARTESIAN_POINT('Ctrl Pts',(7.65228216283404,71.2958046758372,0.));
#160486=CARTESIAN_POINT('Ctrl Pts',(7.65228216283404,71.2958046758372,12.));
#160487=CARTESIAN_POINT('Ctrl Pts',(7.64221325940725,71.2746382537007,0.));
#160488=CARTESIAN_POINT('Ctrl Pts',(7.64221325940725,71.2746382537007,12.));
#160489=CARTESIAN_POINT('Ctrl Pts',(7.63218403390538,71.2535013894602,0.));
#160490=CARTESIAN_POINT('Ctrl Pts',(7.63218403390538,71.2535013894602,12.));
#160491=CARTESIAN_POINT('Ctrl Pts',(7.62219448271109,71.2323942257609,0.));
#160492=CARTESIAN_POINT('Ctrl Pts',(7.62219448271109,71.2323942257609,12.));
#160493=CARTESIAN_POINT('Ctrl Pts',(7.61224460208838,71.211316905874,0.));
#160494=CARTESIAN_POINT('Ctrl Pts',(7.61224460208838,71.211316905874,12.));
#160495=CARTESIAN_POINT('Ctrl Pts',(7.60233438818097,71.1902695737013,0.));
#160496=CARTESIAN_POINT('Ctrl Pts',(7.60233438818097,71.1902695737013,12.));
#160497=CARTESIAN_POINT('Ctrl Pts',(7.59246383701814,71.1692523737844,0.));
#160498=CARTESIAN_POINT('Ctrl Pts',(7.59246383701814,71.1692523737844,12.));
#160499=CARTESIAN_POINT('Ctrl Pts',(7.58263294451452,71.1482654513119,0.));
#160500=CARTESIAN_POINT('Ctrl Pts',(7.58263294451452,71.1482654513119,12.));
#160501=CARTESIAN_POINT('Ctrl Pts',(7.57284170646886,71.1273089521234,0.));
#160502=CARTESIAN_POINT('Ctrl Pts',(7.57284170646886,71.1273089521234,12.));
#160503=CARTESIAN_POINT('Ctrl Pts',(7.56309011855657,71.106383022711,0.));
#160504=CARTESIAN_POINT('Ctrl Pts',(7.56309011855657,71.106383022711,12.));
#160505=CARTESIAN_POINT('Ctrl Pts',(7.55337817632917,71.0854878102243,0.));
#160506=CARTESIAN_POINT('Ctrl Pts',(7.55337817632917,71.0854878102243,12.));
#160507=CARTESIAN_POINT('Ctrl Pts',(7.5437058752198,71.0646234624811,0.));
#160508=CARTESIAN_POINT('Ctrl Pts',(7.5437058752198,71.0646234624811,12.));
#160509=CARTESIAN_POINT('Ctrl Pts',(7.53407321054263,71.043790127973,0.));
#160510=CARTESIAN_POINT('Ctrl Pts',(7.53407321054263,71.043790127973,12.));
#160511=CARTESIAN_POINT('Ctrl Pts',(7.52448017749125,71.0229879558699,0.));
#160512=CARTESIAN_POINT('Ctrl Pts',(7.52448017749125,71.0229879558699,12.));
#160513=CARTESIAN_POINT('Ctrl Pts',(7.51492677113091,71.002217096021,0.));
#160514=CARTESIAN_POINT('Ctrl Pts',(7.51492677113091,71.002217096021,12.));
#160515=CARTESIAN_POINT('Ctrl Pts',(7.50541298639928,70.9814776989612,0.));
#160516=CARTESIAN_POINT('Ctrl Pts',(7.50541298639928,70.9814776989612,12.));
#160517=CARTESIAN_POINT('Ctrl Pts',(7.4959388181113,70.9607699159218,0.));
#160518=CARTESIAN_POINT('Ctrl Pts',(7.4959388181113,70.9607699159218,12.));
#160519=CARTESIAN_POINT('Ctrl Pts',(7.48650426095824,70.940093898837,0.));
#160520=CARTESIAN_POINT('Ctrl Pts',(7.48650426095824,70.940093898837,12.));
#160521=CARTESIAN_POINT('Ctrl Pts',(7.47710930950563,70.9194498003493,0.));
#160522=CARTESIAN_POINT('Ctrl Pts',(7.47710930950563,70.9194498003493,12.));
#160523=CARTESIAN_POINT('Ctrl Pts',(7.46775395818527,70.8988377738104,0.));
#160524=CARTESIAN_POINT('Ctrl Pts',(7.46775395818527,70.8988377738104,12.));
#160525=CARTESIAN_POINT('Ctrl Pts',(7.45843820129782,70.87825797329,0.));
#160526=CARTESIAN_POINT('Ctrl Pts',(7.45843820129782,70.87825797329,12.));
#160527=CARTESIAN_POINT('Ctrl Pts',(7.44916203301648,70.8577105535848,0.));
#160528=CARTESIAN_POINT('Ctrl Pts',(7.44916203301648,70.8577105535848,12.));
#160529=CARTESIAN_POINT('Ctrl Pts',(7.43992544738606,70.8371956702241,0.));
#160530=CARTESIAN_POINT('Ctrl Pts',(7.43992544738606,70.8371956702241,12.));
#160531=CARTESIAN_POINT('Ctrl Pts',(7.43072843832015,70.8167134794737,0.));
#160532=CARTESIAN_POINT('Ctrl Pts',(7.43072843832015,70.8167134794737,12.));
#160533=CARTESIAN_POINT('Ctrl Pts',(7.42157099959326,70.796264138335,0.));
#160534=CARTESIAN_POINT('Ctrl Pts',(7.42157099959326,70.796264138335,12.));
#160535=CARTESIAN_POINT('Ctrl Pts',(7.41245312484498,70.7758478045576,0.));
#160536=CARTESIAN_POINT('Ctrl Pts',(7.41245312484498,70.7758478045576,12.));
#160537=CARTESIAN_POINT('Ctrl Pts',(7.40337480758237,70.7554646366514,0.));
#160538=CARTESIAN_POINT('Ctrl Pts',(7.40337480758237,70.7554646366514,12.));
#160539=CARTESIAN_POINT('Ctrl Pts',(7.39433604117891,70.735114793895,0.));
#160540=CARTESIAN_POINT('Ctrl Pts',(7.39433604117891,70.735114793895,12.));
#160541=CARTESIAN_POINT('Ctrl Pts',(7.38533681887028,70.7147984363423,0.));
#160542=CARTESIAN_POINT('Ctrl Pts',(7.38533681887028,70.7147984363423,12.));
#160543=CARTESIAN_POINT('Ctrl Pts',(7.37637713374761,70.6945157248269,0.));
#160544=CARTESIAN_POINT('Ctrl Pts',(7.37637713374761,70.6945157248269,12.));
#160545=CARTESIAN_POINT('Ctrl Pts',(7.36745697876295,70.6742668209685,0.));
#160546=CARTESIAN_POINT('Ctrl Pts',(7.36745697876295,70.6742668209685,12.));
#160547=CARTESIAN_POINT('Ctrl Pts',(7.35857634673052,70.6540518871772,0.));
#160548=CARTESIAN_POINT('Ctrl Pts',(7.35857634673052,70.6540518871772,12.));
#160549=CARTESIAN_POINT('Ctrl Pts',(7.34973523032581,70.6338710866562,0.));
#160550=CARTESIAN_POINT('Ctrl Pts',(7.34973523032581,70.6338710866562,12.));
#160551=CARTESIAN_POINT('Ctrl Pts',(7.34093362208018,70.6137245834002,0.));
#160552=CARTESIAN_POINT('Ctrl Pts',(7.34093362208018,70.6137245834002,12.));
#160553=CARTESIAN_POINT('Ctrl Pts',(7.33217151437608,70.5936125421958,0.));
#160554=CARTESIAN_POINT('Ctrl Pts',(7.33217151437608,70.5936125421958,12.));
#160555=CARTESIAN_POINT('Ctrl Pts',(7.32344889945237,70.573535128649,0.));
#160556=CARTESIAN_POINT('Ctrl Pts',(7.32344889945237,70.573535128649,12.));
#160557=CARTESIAN_POINT('Ctrl Pts',(7.31476576940404,70.5534925092053,0.));
#160558=CARTESIAN_POINT('Ctrl Pts',(7.31476576940404,70.5534925092053,12.));
#160559=CARTESIAN_POINT('Ctrl Pts',(7.30612211618047,70.5334848511675,0.));
#160560=CARTESIAN_POINT('Ctrl Pts',(7.30612211618047,70.5334848511675,12.));
#160561=CARTESIAN_POINT('Ctrl Pts',(7.29751793157801,70.5135123227147,0.));
#160562=CARTESIAN_POINT('Ctrl Pts',(7.29751793157801,70.5135123227147,12.));
#160563=CARTESIAN_POINT('Ctrl Pts',(7.28895320723836,70.4935750929029,0.));
#160564=CARTESIAN_POINT('Ctrl Pts',(7.28895320723836,70.4935750929029,12.));
#160565=CARTESIAN_POINT('Ctrl Pts',(7.2804279346545,70.4736733316463,0.));
#160566=CARTESIAN_POINT('Ctrl Pts',(7.2804279346545,70.4736733316463,12.));
#160567=CARTESIAN_POINT('Ctrl Pts',(7.27194210517058,70.4538072096986,0.));
#160568=CARTESIAN_POINT('Ctrl Pts',(7.27194210517058,70.4538072096986,12.));
#160569=CARTESIAN_POINT('Ctrl Pts',(7.26349570998051,70.433976898636,0.));
#160570=CARTESIAN_POINT('Ctrl Pts',(7.26349570998051,70.433976898636,12.));
#160571=CARTESIAN_POINT('Ctrl Pts',(7.25508874012076,70.4141825708207,0.));
#160572=CARTESIAN_POINT('Ctrl Pts',(7.25508874012076,70.4141825708207,12.));
#160573=CARTESIAN_POINT('Ctrl Pts',(7.24672118647116,70.3944243994532,0.));
#160574=CARTESIAN_POINT('Ctrl Pts',(7.24672118647116,70.3944243994532,12.));
#160575=CARTESIAN_POINT('Ctrl Pts',(7.23839303975626,70.3747025586569,0.));
#160576=CARTESIAN_POINT('Ctrl Pts',(7.23839303975626,70.3747025586569,12.));
#160577=CARTESIAN_POINT('Ctrl Pts',(7.23010429054231,70.3550172235486,0.));
#160578=CARTESIAN_POINT('Ctrl Pts',(7.23010429054231,70.3550172235486,12.));
#160579=CARTESIAN_POINT('Ctrl Pts',(7.22185492923178,70.3353685703097,0.));
#160580=CARTESIAN_POINT('Ctrl Pts',(7.22185492923178,70.3353685703097,12.));
#160581=CARTESIAN_POINT('Ctrl Pts',(7.21364494605425,70.3157567762561,0.));
#160582=CARTESIAN_POINT('Ctrl Pts',(7.21364494605425,70.3157567762561,12.));
#160583=CARTESIAN_POINT('Ctrl Pts',(7.20547433107458,70.2961820197051,0.));
#160584=CARTESIAN_POINT('Ctrl Pts',(7.20547433107458,70.2961820197051,12.));
#160585=CARTESIAN_POINT('Ctrl Pts',(7.19734307419861,70.276644479827,0.));
#160586=CARTESIAN_POINT('Ctrl Pts',(7.19734307419861,70.276644479827,12.));
#160587=CARTESIAN_POINT('Ctrl Pts',(7.18925116517563,70.2571443365198,0.));
#160588=CARTESIAN_POINT('Ctrl Pts',(7.18925116517563,70.2571443365198,12.));
#160589=CARTESIAN_POINT('Ctrl Pts',(7.18119859359801,70.2376817702239,0.));
#160590=CARTESIAN_POINT('Ctrl Pts',(7.18119859359801,70.2376817702239,12.));
#160591=CARTESIAN_POINT('Ctrl Pts',(7.17318534889747,70.2182569619028,0.));
#160592=CARTESIAN_POINT('Ctrl Pts',(7.17318534889747,70.2182569619028,12.));
#160593=CARTESIAN_POINT('Ctrl Pts',(7.16521142033893,70.1988700934622,0.));
#160594=CARTESIAN_POINT('Ctrl Pts',(7.16521142033893,70.1988700934622,12.));
#160595=CARTESIAN_POINT('Ctrl Pts',(7.15727679700946,70.1795213481196,0.));
#160596=CARTESIAN_POINT('Ctrl Pts',(7.15727679700946,70.1795213481196,12.));
#160597=CARTESIAN_POINT('Ctrl Pts',(7.14938146780801,70.1602109107188,0.));
#160598=CARTESIAN_POINT('Ctrl Pts',(7.14938146780801,70.1602109107188,12.));
#160599=CARTESIAN_POINT('Ctrl Pts',(7.14152542142339,70.1409389682389,0.));
#160600=CARTESIAN_POINT('Ctrl Pts',(7.14152542142339,70.1409389682389,12.));
#160601=CARTESIAN_POINT('Ctrl Pts',(7.13370864634399,70.1217057094456,0.));
#160602=CARTESIAN_POINT('Ctrl Pts',(7.13370864634399,70.1217057094456,12.));
#160603=CARTESIAN_POINT('Ctrl Pts',(7.12593113088871,70.1025113239463,0.));
#160604=CARTESIAN_POINT('Ctrl Pts',(7.12593113088871,70.1025113239463,12.));
#160605=CARTESIAN_POINT('Ctrl Pts',(7.11819286322824,70.0833560013971,0.));
#160606=CARTESIAN_POINT('Ctrl Pts',(7.11819286322824,70.0833560013971,12.));
#160607=CARTESIAN_POINT('Ctrl Pts',(7.11049383140482,70.06423993069,0.));
#160608=CARTESIAN_POINT('Ctrl Pts',(7.11049383140482,70.06423993069,12.));
#160609=CARTESIAN_POINT('Ctrl Pts',(7.10283402335091,70.0451632990137,0.));
#160610=CARTESIAN_POINT('Ctrl Pts',(7.10283402335091,70.0451632990137,12.));
#160611=CARTESIAN_POINT('Ctrl Pts',(7.09521342684301,70.0261262936435,0.));
#160612=CARTESIAN_POINT('Ctrl Pts',(7.09521342684301,70.0261262936435,12.));
#160613=CARTESIAN_POINT('Ctrl Pts',(7.08763202944274,70.0071291040791,0.));
#160614=CARTESIAN_POINT('Ctrl Pts',(7.08763202944274,70.0071291040791,12.));
#160615=CARTESIAN_POINT('Ctrl Pts',(7.08008981844643,69.988171923787,0.));
#160616=CARTESIAN_POINT('Ctrl Pts',(7.08008981844643,69.988171923787,12.));
#160617=CARTESIAN_POINT('Ctrl Pts',(7.07258678080793,69.9692549527256,0.));
#160618=CARTESIAN_POINT('Ctrl Pts',(7.07258678080793,69.9692549527256,12.));
#160619=CARTESIAN_POINT('Ctrl Pts',(7.06512290312803,69.9503783975676,0.));
#160620=CARTESIAN_POINT('Ctrl Pts',(7.06512290312803,69.9503783975676,12.));
#160621=CARTESIAN_POINT('Ctrl Pts',(7.05769817180825,69.9315424664252,0.));
#160622=CARTESIAN_POINT('Ctrl Pts',(7.05769817180825,69.9315424664252,12.));
#160623=CARTESIAN_POINT('Ctrl Pts',(7.05031257318108,69.9127473642087,0.));
#160624=CARTESIAN_POINT('Ctrl Pts',(7.05031257318108,69.9127473642087,12.));
#160625=CARTESIAN_POINT('Ctrl Pts',(7.04296609362187,69.8939932885864,0.));
#160626=CARTESIAN_POINT('Ctrl Pts',(7.04296609362187,69.8939932885864,12.));
#160627=CARTESIAN_POINT('Ctrl Pts',(7.03565871972266,69.8752804235296,0.));
#160628=CARTESIAN_POINT('Ctrl Pts',(7.03565871972266,69.8752804235296,12.));
#160629=CARTESIAN_POINT('Ctrl Pts',(7.02839043811863,69.8566089455448,0.));
#160630=CARTESIAN_POINT('Ctrl Pts',(7.02839043811863,69.8566089455448,12.));
#160631=CARTESIAN_POINT('Ctrl Pts',(7.02116123514488,69.8379790360574,0.));
#160632=CARTESIAN_POINT('Ctrl Pts',(7.02116123514488,69.8379790360574,12.));
#160633=CARTESIAN_POINT('Ctrl Pts',(7.01397109655456,69.8193908913722,0.));
#160634=CARTESIAN_POINT('Ctrl Pts',(7.01397109655456,69.8193908913722,12.));
#160635=CARTESIAN_POINT('Ctrl Pts',(7.00682000718105,69.8008447346782,0.));
#160636=CARTESIAN_POINT('Ctrl Pts',(7.00682000718105,69.8008447346782,12.));
#160637=CARTESIAN_POINT('Ctrl Pts',(6.99970795069399,69.7823408242446,0.));
#160638=CARTESIAN_POINT('Ctrl Pts',(6.99970795069399,69.7823408242446,12.));
#160639=CARTESIAN_POINT('Ctrl Pts',(6.9926349102786,69.7638794280263,0.));
#160640=CARTESIAN_POINT('Ctrl Pts',(6.9926349102786,69.7638794280263,12.));
#160641=CARTESIAN_POINT('Ctrl Pts',(6.98560086924173,69.7454607995524,0.));
#160642=CARTESIAN_POINT('Ctrl Pts',(6.98560086924173,69.7454607995524,12.));
#160643=CARTESIAN_POINT('Ctrl Pts',(6.97860581164569,69.7270851557443,0.));
#160644=CARTESIAN_POINT('Ctrl Pts',(6.97860581164569,69.7270851557443,12.));
#160645=CARTESIAN_POINT('Ctrl Pts',(6.97164972291582,69.7087526480249,0.));
#160646=CARTESIAN_POINT('Ctrl Pts',(6.97164972291582,69.7087526480249,12.));
#160647=CARTESIAN_POINT('Ctrl Pts',(6.9647325904973,69.6904633605834,0.));
#160648=CARTESIAN_POINT('Ctrl Pts',(6.9647325904973,69.6904633605834,12.));
#160649=CARTESIAN_POINT('Ctrl Pts',(6.95923004173796,69.6758665380764,0.));
#160650=CARTESIAN_POINT('Ctrl Pts',(6.95923004173796,69.6758665380764,12.));
#160651=CARTESIAN_POINT('Ctrl Pts',(6.95512065317731,69.6649383920075,0.));
#160652=CARTESIAN_POINT('Ctrl Pts',(6.95512065317731,69.6649383920075,12.));
#160653=CARTESIAN_POINT('Ctrl Pts',(6.95238884849076,69.6576616146559,0.));
#160654=CARTESIAN_POINT('Ctrl Pts',(6.95238884849076,69.6576616146559,12.));
#160655=CARTESIAN_POINT('Ctrl Pts',(6.95102489306928,69.6540253893193,0.));
#160656=CARTESIAN_POINT('Ctrl Pts',(6.95102489306928,69.6540253893193,12.));
#160657=CARTESIAN_POINT('',(6.95102489306928,69.6540253893193,12.));
#160658=CARTESIAN_POINT('Ctrl Pts',(6.95102489306928,69.6540253893193,12.));
#160659=CARTESIAN_POINT('Ctrl Pts',(6.95238884849076,69.6576616146559,12.));
#160660=CARTESIAN_POINT('Ctrl Pts',(6.95512065317731,69.6649383920075,12.));
#160661=CARTESIAN_POINT('Ctrl Pts',(6.95923004173796,69.6758665380764,12.));
#160662=CARTESIAN_POINT('Ctrl Pts',(6.9647325904973,69.6904633605834,12.));
#160663=CARTESIAN_POINT('Ctrl Pts',(6.97164972291582,69.7087526480249,12.));
#160664=CARTESIAN_POINT('Ctrl Pts',(6.97860581164569,69.7270851557443,12.));
#160665=CARTESIAN_POINT('Ctrl Pts',(6.98560086924173,69.7454607995524,12.));
#160666=CARTESIAN_POINT('Ctrl Pts',(6.9926349102786,69.7638794280263,12.));
#160667=CARTESIAN_POINT('Ctrl Pts',(6.99970795069399,69.7823408242446,12.));
#160668=CARTESIAN_POINT('Ctrl Pts',(7.00682000718105,69.8008447346782,12.));
#160669=CARTESIAN_POINT('Ctrl Pts',(7.01397109655456,69.8193908913722,12.));
#160670=CARTESIAN_POINT('Ctrl Pts',(7.02116123514488,69.8379790360574,12.));
#160671=CARTESIAN_POINT('Ctrl Pts',(7.02839043811863,69.8566089455448,12.));
#160672=CARTESIAN_POINT('Ctrl Pts',(7.03565871972266,69.8752804235296,12.));
#160673=CARTESIAN_POINT('Ctrl Pts',(7.04296609362187,69.8939932885864,12.));
#160674=CARTESIAN_POINT('Ctrl Pts',(7.05031257318108,69.9127473642087,12.));
#160675=CARTESIAN_POINT('Ctrl Pts',(7.05769817180825,69.9315424664252,12.));
#160676=CARTESIAN_POINT('Ctrl Pts',(7.06512290312803,69.9503783975676,12.));
#160677=CARTESIAN_POINT('Ctrl Pts',(7.07258678080793,69.9692549527256,12.));
#160678=CARTESIAN_POINT('Ctrl Pts',(7.08008981844643,69.988171923787,12.));
#160679=CARTESIAN_POINT('Ctrl Pts',(7.08763202944274,70.0071291040791,12.));
#160680=CARTESIAN_POINT('Ctrl Pts',(7.09521342684301,70.0261262936435,12.));
#160681=CARTESIAN_POINT('Ctrl Pts',(7.10283402335091,70.0451632990137,12.));
#160682=CARTESIAN_POINT('Ctrl Pts',(7.11049383140482,70.06423993069,12.));
#160683=CARTESIAN_POINT('Ctrl Pts',(7.11819286322824,70.0833560013971,12.));
#160684=CARTESIAN_POINT('Ctrl Pts',(7.12593113088871,70.1025113239463,12.));
#160685=CARTESIAN_POINT('Ctrl Pts',(7.13370864634399,70.1217057094456,12.));
#160686=CARTESIAN_POINT('Ctrl Pts',(7.14152542142339,70.1409389682389,12.));
#160687=CARTESIAN_POINT('Ctrl Pts',(7.14938146780801,70.1602109107188,12.));
#160688=CARTESIAN_POINT('Ctrl Pts',(7.15727679700946,70.1795213481196,12.));
#160689=CARTESIAN_POINT('Ctrl Pts',(7.16521142033893,70.1988700934622,12.));
#160690=CARTESIAN_POINT('Ctrl Pts',(7.17318534889747,70.2182569619028,12.));
#160691=CARTESIAN_POINT('Ctrl Pts',(7.18119859359801,70.2376817702239,12.));
#160692=CARTESIAN_POINT('Ctrl Pts',(7.18925116517563,70.2571443365198,12.));
#160693=CARTESIAN_POINT('Ctrl Pts',(7.19734307419861,70.276644479827,12.));
#160694=CARTESIAN_POINT('Ctrl Pts',(7.20547433107458,70.2961820197051,12.));
#160695=CARTESIAN_POINT('Ctrl Pts',(7.21364494605425,70.3157567762561,12.));
#160696=CARTESIAN_POINT('Ctrl Pts',(7.22185492923178,70.3353685703097,12.));
#160697=CARTESIAN_POINT('Ctrl Pts',(7.23010429054231,70.3550172235486,12.));
#160698=CARTESIAN_POINT('Ctrl Pts',(7.23839303975626,70.3747025586569,12.));
#160699=CARTESIAN_POINT('Ctrl Pts',(7.24672118647116,70.3944243994532,12.));
#160700=CARTESIAN_POINT('Ctrl Pts',(7.25508874012076,70.4141825708207,12.));
#160701=CARTESIAN_POINT('Ctrl Pts',(7.26349570998051,70.433976898636,12.));
#160702=CARTESIAN_POINT('Ctrl Pts',(7.27194210517058,70.4538072096986,12.));
#160703=CARTESIAN_POINT('Ctrl Pts',(7.2804279346545,70.4736733316463,12.));
#160704=CARTESIAN_POINT('Ctrl Pts',(7.28895320723836,70.4935750929029,12.));
#160705=CARTESIAN_POINT('Ctrl Pts',(7.29751793157801,70.5135123227147,12.));
#160706=CARTESIAN_POINT('Ctrl Pts',(7.30612211618047,70.5334848511675,12.));
#160707=CARTESIAN_POINT('Ctrl Pts',(7.31476576940404,70.5534925092053,12.));
#160708=CARTESIAN_POINT('Ctrl Pts',(7.32344889945237,70.573535128649,12.));
#160709=CARTESIAN_POINT('Ctrl Pts',(7.33217151437608,70.5936125421958,12.));
#160710=CARTESIAN_POINT('Ctrl Pts',(7.34093362208018,70.6137245834002,12.));
#160711=CARTESIAN_POINT('Ctrl Pts',(7.34973523032581,70.6338710866562,12.));
#160712=CARTESIAN_POINT('Ctrl Pts',(7.35857634673052,70.6540518871772,12.));
#160713=CARTESIAN_POINT('Ctrl Pts',(7.36745697876295,70.6742668209685,12.));
#160714=CARTESIAN_POINT('Ctrl Pts',(7.37637713374761,70.6945157248269,12.));
#160715=CARTESIAN_POINT('Ctrl Pts',(7.38533681887028,70.7147984363423,12.));
#160716=CARTESIAN_POINT('Ctrl Pts',(7.39433604117891,70.735114793895,12.));
#160717=CARTESIAN_POINT('Ctrl Pts',(7.40337480758237,70.7554646366514,12.));
#160718=CARTESIAN_POINT('Ctrl Pts',(7.41245312484498,70.7758478045576,12.));
#160719=CARTESIAN_POINT('Ctrl Pts',(7.42157099959326,70.796264138335,12.));
#160720=CARTESIAN_POINT('Ctrl Pts',(7.43072843832015,70.8167134794737,12.));
#160721=CARTESIAN_POINT('Ctrl Pts',(7.43992544738606,70.8371956702241,12.));
#160722=CARTESIAN_POINT('Ctrl Pts',(7.44916203301648,70.8577105535848,12.));
#160723=CARTESIAN_POINT('Ctrl Pts',(7.45843820129782,70.87825797329,12.));
#160724=CARTESIAN_POINT('Ctrl Pts',(7.46775395818527,70.8988377738104,12.));
#160725=CARTESIAN_POINT('Ctrl Pts',(7.47710930950563,70.9194498003493,12.));
#160726=CARTESIAN_POINT('Ctrl Pts',(7.48650426095824,70.940093898837,12.));
#160727=CARTESIAN_POINT('Ctrl Pts',(7.4959388181113,70.9607699159218,12.));
#160728=CARTESIAN_POINT('Ctrl Pts',(7.50541298639928,70.9814776989612,12.));
#160729=CARTESIAN_POINT('Ctrl Pts',(7.51492677113091,71.002217096021,12.));
#160730=CARTESIAN_POINT('Ctrl Pts',(7.52448017749125,71.0229879558699,12.));
#160731=CARTESIAN_POINT('Ctrl Pts',(7.53407321054263,71.043790127973,12.));
#160732=CARTESIAN_POINT('Ctrl Pts',(7.5437058752198,71.0646234624811,12.));
#160733=CARTESIAN_POINT('Ctrl Pts',(7.55337817632917,71.0854878102243,12.));
#160734=CARTESIAN_POINT('Ctrl Pts',(7.56309011855657,71.106383022711,12.));
#160735=CARTESIAN_POINT('Ctrl Pts',(7.57284170646886,71.1273089521234,12.));
#160736=CARTESIAN_POINT('Ctrl Pts',(7.58263294451452,71.1482654513119,12.));
#160737=CARTESIAN_POINT('Ctrl Pts',(7.59246383701814,71.1692523737844,12.));
#160738=CARTESIAN_POINT('Ctrl Pts',(7.60233438818097,71.1902695737013,12.));
#160739=CARTESIAN_POINT('Ctrl Pts',(7.61224460208838,71.211316905874,12.));
#160740=CARTESIAN_POINT('Ctrl Pts',(7.62219448271109,71.2323942257609,12.));
#160741=CARTESIAN_POINT('Ctrl Pts',(7.63218403390538,71.2535013894602,12.));
#160742=CARTESIAN_POINT('Ctrl Pts',(7.64221325940725,71.2746382537007,12.));
#160743=CARTESIAN_POINT('Ctrl Pts',(7.65228216283404,71.2958046758372,12.));
#160744=CARTESIAN_POINT('Ctrl Pts',(7.66239074769163,71.3170005138502,12.));
#160745=CARTESIAN_POINT('Ctrl Pts',(7.67253901737553,71.3382256263414,12.));
#160746=CARTESIAN_POINT('Ctrl Pts',(7.68272697517086,71.3594798725281,12.));
#160747=CARTESIAN_POINT('Ctrl Pts',(7.69295462424612,71.3807631122331,12.));
#160748=CARTESIAN_POINT('Ctrl Pts',(7.70322196765539,71.4020752058796,12.));
#160749=CARTESIAN_POINT('Ctrl Pts',(7.7135290083452,71.4234160144925,12.));
#160750=CARTESIAN_POINT('Ctrl Pts',(7.72387574915544,71.4447853996916,12.));
#160751=CARTESIAN_POINT('Ctrl Pts',(7.7342621928194,71.4661832236888,12.));
#160752=CARTESIAN_POINT('Ctrl Pts',(7.74468834195746,71.4876093492781,12.));
#160753=CARTESIAN_POINT('Ctrl Pts',(7.75515419907967,71.5090636398318,12.));
#160754=CARTESIAN_POINT('Ctrl Pts',(7.76565976659226,71.5305459592994,12.));
#160755=CARTESIAN_POINT('Ctrl Pts',(7.7762050467987,71.5520561722039,12.));
#160756=CARTESIAN_POINT('Ctrl Pts',(7.78679004189935,71.5735941436364,12.));
#160757=CARTESIAN_POINT('Ctrl Pts',(7.79741475398514,71.5951597392471,12.));
#160758=CARTESIAN_POINT('Ctrl Pts',(7.80807918504022,71.6167528252423,12.));
#160759=CARTESIAN_POINT('Ctrl Pts',(7.81878333694861,71.6383732683844,12.));
#160760=CARTESIAN_POINT('Ctrl Pts',(7.82952721149508,71.6600209359872,12.));
#160761=CARTESIAN_POINT('Ctrl Pts',(7.8403108103649,71.6816956959117,12.));
#160762=CARTESIAN_POINT('Ctrl Pts',(7.85113413513736,71.7033974165568,12.));
#160763=CARTESIAN_POINT('Ctrl Pts',(7.86199718728826,71.7251259668563,12.));
#160764=CARTESIAN_POINT('Ctrl Pts',(7.87289996819654,71.7468812162788,12.));
#160765=CARTESIAN_POINT('Ctrl Pts',(7.88384247914524,71.7686630348238,12.));
#160766=CARTESIAN_POINT('Ctrl Pts',(7.89482472132137,71.7904712930175,12.));
#160767=CARTESIAN_POINT('Ctrl Pts',(7.90584669580956,71.8123058619042,12.));
#160768=CARTESIAN_POINT('Ctrl Pts',(7.91690840359367,71.8341666130426,12.));
#160769=CARTESIAN_POINT('Ctrl Pts',(7.92800984556396,71.8560534185071,12.));
#160770=CARTESIAN_POINT('Ctrl Pts',(7.93915102251795,71.8779661508832,12.));
#160771=CARTESIAN_POINT('Ctrl Pts',(7.95033193516051,71.8999046832643,12.));
#160772=CARTESIAN_POINT('Ctrl Pts',(7.96155258409764,71.9218688892431,12.));
#160773=CARTESIAN_POINT('Ctrl Pts',(7.97281296983718,71.9438586429081,12.));
#160774=CARTESIAN_POINT('Ctrl Pts',(7.98411309279613,71.965873818843,12.));
#160775=CARTESIAN_POINT('Ctrl Pts',(7.99545295330191,71.9879142921254,12.));
#160776=CARTESIAN_POINT('Ctrl Pts',(8.00683255159248,72.0099799383213,12.));
#160777=CARTESIAN_POINT('Ctrl Pts',(8.01825188781057,72.032070633479,12.));
#160778=CARTESIAN_POINT('Ctrl Pts',(8.02971096200308,72.0541862541243,12.));
#160779=CARTESIAN_POINT('Ctrl Pts',(8.04120977412872,72.0763266772615,12.));
#160780=CARTESIAN_POINT('Ctrl Pts',(8.05274832405949,72.0984917803693,12.));
#160781=CARTESIAN_POINT('Ctrl Pts',(8.06432661158096,72.1206814413988,12.));
#160782=CARTESIAN_POINT('Ctrl Pts',(8.07594463638719,72.1428955387663,12.));
#160783=CARTESIAN_POINT('Ctrl Pts',(8.08760239807837,72.1651339513477,12.));
#160784=CARTESIAN_POINT('Ctrl Pts',(8.0992998961689,72.1873965584813,12.));
#160785=CARTESIAN_POINT('Ctrl Pts',(8.11103713008928,72.209683239963,12.));
#160786=CARTESIAN_POINT('Ctrl Pts',(8.12281409918661,72.2319938760449,12.));
#160787=CARTESIAN_POINT('Ctrl Pts',(8.13463080272029,72.2543283474278,12.));
#160788=CARTESIAN_POINT('Ctrl Pts',(8.14648723985798,72.2766865352555,12.));
#160789=CARTESIAN_POINT('Ctrl Pts',(8.15838340968336,72.2990683211162,12.));
#160790=CARTESIAN_POINT('Ctrl Pts',(8.17031931119891,72.3214735870409,12.));
#160791=CARTESIAN_POINT('Ctrl Pts',(8.18229494332624,72.3439022155007,12.));
#160792=CARTESIAN_POINT('Ctrl Pts',(8.19431030490315,72.3663540894026,12.));
#160793=CARTESIAN_POINT('Ctrl Pts',(8.20636539467776,72.3888290920832,12.));
#160794=CARTESIAN_POINT('Ctrl Pts',(8.21846021131561,72.4113271073079,12.));
#160795=CARTESIAN_POINT('Ctrl Pts',(8.23059475340357,72.4338480192695,12.));
#160796=CARTESIAN_POINT('Ctrl Pts',(8.2427690194504,72.4563917125842,12.));
#160797=CARTESIAN_POINT('Ctrl Pts',(8.25498300788494,72.4789580722875,12.));
#160798=CARTESIAN_POINT('Ctrl Pts',(8.2672367170492,72.5015469838254,12.));
#160799=CARTESIAN_POINT('Ctrl Pts',(8.27953014520376,72.5241583330562,12.));
#160800=CARTESIAN_POINT('Ctrl Pts',(8.29186329053279,72.5467920062521,12.));
#160801=CARTESIAN_POINT('Ctrl Pts',(8.30423615114453,72.5694478900982,12.));
#160802=CARTESIAN_POINT('Ctrl Pts',(8.31664872507017,72.5921258716901,12.));
#160803=CARTESIAN_POINT('Ctrl Pts',(8.32910101025671,72.6148258385296,12.));
#160804=CARTESIAN_POINT('Ctrl Pts',(8.34159300456987,72.6375476785215,12.));
#160805=CARTESIAN_POINT('Ctrl Pts',(8.35412470580102,72.6602912799696,12.));
#160806=CARTESIAN_POINT('Ctrl Pts',(8.36669611166843,72.6830565315703,12.));
#160807=CARTESIAN_POINT('Ctrl Pts',(8.37930721981731,72.705843322407,12.));
#160808=CARTESIAN_POINT('Ctrl Pts',(8.39195802781391,72.7286515419373,12.));
#160809=CARTESIAN_POINT('Ctrl Pts',(8.40464853314469,72.751481079992,12.));
#160810=CARTESIAN_POINT('Ctrl Pts',(8.4173787332233,72.7743318267865,12.));
#160811=CARTESIAN_POINT('Ctrl Pts',(8.43014862539158,72.7972036729276,12.));
#160812=CARTESIAN_POINT('Ctrl Pts',(8.44295820691912,72.8200965094199,12.));
#160813=CARTESIAN_POINT('Ctrl Pts',(8.45580747499793,72.8430102276713,12.));
#160814=CARTESIAN_POINT('Ctrl Pts',(8.46869642673795,72.8659447194933,12.));
#160815=CARTESIAN_POINT('Ctrl Pts',(8.48162505917658,72.8888998770785,12.));
#160816=CARTESIAN_POINT('Ctrl Pts',(8.49459336928296,72.9118755929795,12.));
#160817=CARTESIAN_POINT('Ctrl Pts',(8.50760135395984,72.9348717600838,12.));
#160818=CARTESIAN_POINT('Ctrl Pts',(8.52064901004228,72.9578882715912,12.));
#160819=CARTESIAN_POINT('Ctrl Pts',(8.53373633429281,72.9809250209828,12.));
#160820=CARTESIAN_POINT('Ctrl Pts',(8.54686332340418,73.0039819020648,12.));
#160821=CARTESIAN_POINT('Ctrl Pts',(8.56002997400084,73.0270588090183,12.));
#160822=CARTESIAN_POINT('Ctrl Pts',(8.57323628263593,73.0501556364479,12.));
#160823=CARTESIAN_POINT('Ctrl Pts',(8.58648224578732,73.0732722794195,12.));
#160824=CARTESIAN_POINT('Ctrl Pts',(8.59976785984552,73.0964086335235,12.));
#160825=CARTESIAN_POINT('Ctrl Pts',(8.61309312112002,73.1195645948178,12.));
#160826=CARTESIAN_POINT('Ctrl Pts',(8.62645802585484,73.1427400597037,12.));
#160827=CARTESIAN_POINT('Ctrl Pts',(8.63986257023739,73.1659349248133,12.));
#160828=CARTESIAN_POINT('Ctrl Pts',(8.65330675040537,73.1891490869056,12.));
#160829=CARTESIAN_POINT('Ctrl Pts',(8.66679056245092,73.2123824427208,12.));
#160830=CARTESIAN_POINT('Ctrl Pts',(8.68031400241872,73.2356348889693,12.));
#160831=CARTESIAN_POINT('Ctrl Pts',(8.69387706629286,73.2589063226358,12.));
#160832=CARTESIAN_POINT('Ctrl Pts',(8.7074797499823,73.2821966412148,12.));
#160833=CARTESIAN_POINT('Ctrl Pts',(8.72112204930232,73.3055057429742,12.));
#160834=CARTESIAN_POINT('Ctrl Pts',(8.7348039599538,73.3288335272002,12.));
#160835=CARTESIAN_POINT('Ctrl Pts',(8.74852547749778,73.3521798944622,12.));
#160836=CARTESIAN_POINT('Ctrl Pts',(8.76228659740358,73.3755447460269,12.));
#160837=CARTESIAN_POINT('Ctrl Pts',(8.77608731509348,73.3989279832835,12.));
#160838=CARTESIAN_POINT('Ctrl Pts',(8.78992762598757,73.422329507113,12.));
#160839=CARTESIAN_POINT('Ctrl Pts',(8.80380752553692,73.4457492173933,12.));
#160840=CARTESIAN_POINT('Ctrl Pts',(8.81772700927531,73.4691870121567,12.));
#160841=CARTESIAN_POINT('Ctrl Pts',(8.83168607277326,73.492642788273,12.));
#160842=CARTESIAN_POINT('Ctrl Pts',(8.84568471153806,73.5161164429709,12.));
#160843=CARTESIAN_POINT('Ctrl Pts',(8.85972292092131,73.5396078751639,12.));
#160844=CARTESIAN_POINT('Ctrl Pts',(8.87380069602971,73.5631169867122,12.));
#160845=CARTESIAN_POINT('Ctrl Pts',(8.88791803160443,73.5866436840556,12.));
#160846=CARTESIAN_POINT('Ctrl Pts',(8.90207492199043,73.6101878785976,12.));
#160847=CARTESIAN_POINT('Ctrl Pts',(8.91424402151598,73.6303847393629,12.));
#160848=CARTESIAN_POINT('Ctrl Pts',(8.9235951817849,73.6458786306023,12.));
#160849=CARTESIAN_POINT('Ctrl Pts',(8.93011088817314,73.6566618622074,12.));
#160850=CARTESIAN_POINT('Ctrl Pts',(8.93377955965632,73.6627293782587,12.));
#160851=CARTESIAN_POINT('Ctrl Pts',(8.93459554657838,73.6640787198055,12.));
#160852=CARTESIAN_POINT('',(6.95102489306928,69.6540253893193,0.));
#160853=CARTESIAN_POINT('',(6.95102489306928,69.6540253893193,0.));
#160854=CARTESIAN_POINT('Ctrl Pts',(8.93459554657838,73.6640787198055,0.));
#160855=CARTESIAN_POINT('Ctrl Pts',(8.93377955965632,73.6627293782587,0.));
#160856=CARTESIAN_POINT('Ctrl Pts',(8.93011088817314,73.6566618622074,0.));
#160857=CARTESIAN_POINT('Ctrl Pts',(8.9235951817849,73.6458786306023,0.));
#160858=CARTESIAN_POINT('Ctrl Pts',(8.91424402151598,73.6303847393629,0.));
#160859=CARTESIAN_POINT('Ctrl Pts',(8.90207492199043,73.6101878785976,0.));
#160860=CARTESIAN_POINT('Ctrl Pts',(8.88791803160443,73.5866436840556,0.));
#160861=CARTESIAN_POINT('Ctrl Pts',(8.87380069602971,73.5631169867122,0.));
#160862=CARTESIAN_POINT('Ctrl Pts',(8.85972292092131,73.5396078751639,0.));
#160863=CARTESIAN_POINT('Ctrl Pts',(8.84568471153806,73.5161164429709,0.));
#160864=CARTESIAN_POINT('Ctrl Pts',(8.83168607277326,73.492642788273,0.));
#160865=CARTESIAN_POINT('Ctrl Pts',(8.81772700927531,73.4691870121567,0.));
#160866=CARTESIAN_POINT('Ctrl Pts',(8.80380752553692,73.4457492173933,0.));
#160867=CARTESIAN_POINT('Ctrl Pts',(8.78992762598757,73.422329507113,0.));
#160868=CARTESIAN_POINT('Ctrl Pts',(8.77608731509348,73.3989279832835,0.));
#160869=CARTESIAN_POINT('Ctrl Pts',(8.76228659740358,73.3755447460269,0.));
#160870=CARTESIAN_POINT('Ctrl Pts',(8.74852547749778,73.3521798944622,0.));
#160871=CARTESIAN_POINT('Ctrl Pts',(8.7348039599538,73.3288335272002,0.));
#160872=CARTESIAN_POINT('Ctrl Pts',(8.72112204930232,73.3055057429742,0.));
#160873=CARTESIAN_POINT('Ctrl Pts',(8.7074797499823,73.2821966412148,0.));
#160874=CARTESIAN_POINT('Ctrl Pts',(8.69387706629286,73.2589063226358,0.));
#160875=CARTESIAN_POINT('Ctrl Pts',(8.68031400241872,73.2356348889693,0.));
#160876=CARTESIAN_POINT('Ctrl Pts',(8.66679056245092,73.2123824427208,0.));
#160877=CARTESIAN_POINT('Ctrl Pts',(8.65330675040537,73.1891490869056,0.));
#160878=CARTESIAN_POINT('Ctrl Pts',(8.63986257023739,73.1659349248133,0.));
#160879=CARTESIAN_POINT('Ctrl Pts',(8.62645802585484,73.1427400597037,0.));
#160880=CARTESIAN_POINT('Ctrl Pts',(8.61309312112002,73.1195645948178,0.));
#160881=CARTESIAN_POINT('Ctrl Pts',(8.59976785984552,73.0964086335235,0.));
#160882=CARTESIAN_POINT('Ctrl Pts',(8.58648224578732,73.0732722794195,0.));
#160883=CARTESIAN_POINT('Ctrl Pts',(8.57323628263593,73.0501556364479,0.));
#160884=CARTESIAN_POINT('Ctrl Pts',(8.56002997400084,73.0270588090183,0.));
#160885=CARTESIAN_POINT('Ctrl Pts',(8.54686332340418,73.0039819020648,0.));
#160886=CARTESIAN_POINT('Ctrl Pts',(8.53373633429281,72.9809250209828,0.));
#160887=CARTESIAN_POINT('Ctrl Pts',(8.52064901004228,72.9578882715912,0.));
#160888=CARTESIAN_POINT('Ctrl Pts',(8.50760135395984,72.9348717600838,0.));
#160889=CARTESIAN_POINT('Ctrl Pts',(8.49459336928296,72.9118755929795,0.));
#160890=CARTESIAN_POINT('Ctrl Pts',(8.48162505917658,72.8888998770785,0.));
#160891=CARTESIAN_POINT('Ctrl Pts',(8.46869642673795,72.8659447194933,0.));
#160892=CARTESIAN_POINT('Ctrl Pts',(8.45580747499793,72.8430102276713,0.));
#160893=CARTESIAN_POINT('Ctrl Pts',(8.44295820691912,72.8200965094199,0.));
#160894=CARTESIAN_POINT('Ctrl Pts',(8.43014862539158,72.7972036729276,0.));
#160895=CARTESIAN_POINT('Ctrl Pts',(8.4173787332233,72.7743318267865,0.));
#160896=CARTESIAN_POINT('Ctrl Pts',(8.40464853314469,72.751481079992,0.));
#160897=CARTESIAN_POINT('Ctrl Pts',(8.39195802781391,72.7286515419373,0.));
#160898=CARTESIAN_POINT('Ctrl Pts',(8.37930721981731,72.705843322407,0.));
#160899=CARTESIAN_POINT('Ctrl Pts',(8.36669611166843,72.6830565315703,0.));
#160900=CARTESIAN_POINT('Ctrl Pts',(8.35412470580102,72.6602912799696,0.));
#160901=CARTESIAN_POINT('Ctrl Pts',(8.34159300456987,72.6375476785215,0.));
#160902=CARTESIAN_POINT('Ctrl Pts',(8.32910101025671,72.6148258385296,0.));
#160903=CARTESIAN_POINT('Ctrl Pts',(8.31664872507017,72.5921258716901,0.));
#160904=CARTESIAN_POINT('Ctrl Pts',(8.30423615114453,72.5694478900982,0.));
#160905=CARTESIAN_POINT('Ctrl Pts',(8.29186329053279,72.5467920062521,0.));
#160906=CARTESIAN_POINT('Ctrl Pts',(8.27953014520376,72.5241583330562,0.));
#160907=CARTESIAN_POINT('Ctrl Pts',(8.2672367170492,72.5015469838254,0.));
#160908=CARTESIAN_POINT('Ctrl Pts',(8.25498300788494,72.4789580722875,0.));
#160909=CARTESIAN_POINT('Ctrl Pts',(8.2427690194504,72.4563917125842,0.));
#160910=CARTESIAN_POINT('Ctrl Pts',(8.23059475340357,72.4338480192695,0.));
#160911=CARTESIAN_POINT('Ctrl Pts',(8.21846021131561,72.4113271073079,0.));
#160912=CARTESIAN_POINT('Ctrl Pts',(8.20636539467776,72.3888290920832,0.));
#160913=CARTESIAN_POINT('Ctrl Pts',(8.19431030490315,72.3663540894026,0.));
#160914=CARTESIAN_POINT('Ctrl Pts',(8.18229494332624,72.3439022155007,0.));
#160915=CARTESIAN_POINT('Ctrl Pts',(8.17031931119891,72.3214735870409,0.));
#160916=CARTESIAN_POINT('Ctrl Pts',(8.15838340968336,72.2990683211162,0.));
#160917=CARTESIAN_POINT('Ctrl Pts',(8.14648723985798,72.2766865352555,0.));
#160918=CARTESIAN_POINT('Ctrl Pts',(8.13463080272029,72.2543283474278,0.));
#160919=CARTESIAN_POINT('Ctrl Pts',(8.12281409918661,72.2319938760449,0.));
#160920=CARTESIAN_POINT('Ctrl Pts',(8.11103713008928,72.209683239963,0.));
#160921=CARTESIAN_POINT('Ctrl Pts',(8.0992998961689,72.1873965584813,0.));
#160922=CARTESIAN_POINT('Ctrl Pts',(8.08760239807837,72.1651339513477,0.));
#160923=CARTESIAN_POINT('Ctrl Pts',(8.07594463638719,72.1428955387663,0.));
#160924=CARTESIAN_POINT('Ctrl Pts',(8.06432661158096,72.1206814413988,0.));
#160925=CARTESIAN_POINT('Ctrl Pts',(8.05274832405949,72.0984917803693,0.));
#160926=CARTESIAN_POINT('Ctrl Pts',(8.04120977412872,72.0763266772615,0.));
#160927=CARTESIAN_POINT('Ctrl Pts',(8.02971096200308,72.0541862541243,0.));
#160928=CARTESIAN_POINT('Ctrl Pts',(8.01825188781057,72.032070633479,0.));
#160929=CARTESIAN_POINT('Ctrl Pts',(8.00683255159248,72.0099799383213,0.));
#160930=CARTESIAN_POINT('Ctrl Pts',(7.99545295330191,71.9879142921254,0.));
#160931=CARTESIAN_POINT('Ctrl Pts',(7.98411309279613,71.965873818843,0.));
#160932=CARTESIAN_POINT('Ctrl Pts',(7.97281296983718,71.9438586429081,0.));
#160933=CARTESIAN_POINT('Ctrl Pts',(7.96155258409764,71.9218688892431,0.));
#160934=CARTESIAN_POINT('Ctrl Pts',(7.95033193516051,71.8999046832643,0.));
#160935=CARTESIAN_POINT('Ctrl Pts',(7.93915102251795,71.8779661508832,0.));
#160936=CARTESIAN_POINT('Ctrl Pts',(7.92800984556396,71.8560534185071,0.));
#160937=CARTESIAN_POINT('Ctrl Pts',(7.91690840359367,71.8341666130426,0.));
#160938=CARTESIAN_POINT('Ctrl Pts',(7.90584669580956,71.8123058619042,0.));
#160939=CARTESIAN_POINT('Ctrl Pts',(7.89482472132137,71.7904712930175,0.));
#160940=CARTESIAN_POINT('Ctrl Pts',(7.88384247914524,71.7686630348238,0.));
#160941=CARTESIAN_POINT('Ctrl Pts',(7.87289996819654,71.7468812162788,0.));
#160942=CARTESIAN_POINT('Ctrl Pts',(7.86199718728826,71.7251259668563,0.));
#160943=CARTESIAN_POINT('Ctrl Pts',(7.85113413513736,71.7033974165568,0.));
#160944=CARTESIAN_POINT('Ctrl Pts',(7.8403108103649,71.6816956959117,0.));
#160945=CARTESIAN_POINT('Ctrl Pts',(7.82952721149508,71.6600209359872,0.));
#160946=CARTESIAN_POINT('Ctrl Pts',(7.81878333694861,71.6383732683844,0.));
#160947=CARTESIAN_POINT('Ctrl Pts',(7.80807918504022,71.6167528252423,0.));
#160948=CARTESIAN_POINT('Ctrl Pts',(7.79741475398514,71.5951597392471,0.));
#160949=CARTESIAN_POINT('Ctrl Pts',(7.78679004189935,71.5735941436364,0.));
#160950=CARTESIAN_POINT('Ctrl Pts',(7.7762050467987,71.5520561722039,0.));
#160951=CARTESIAN_POINT('Ctrl Pts',(7.76565976659226,71.5305459592994,0.));
#160952=CARTESIAN_POINT('Ctrl Pts',(7.75515419907967,71.5090636398318,0.));
#160953=CARTESIAN_POINT('Ctrl Pts',(7.74468834195746,71.4876093492781,0.));
#160954=CARTESIAN_POINT('Ctrl Pts',(7.7342621928194,71.4661832236888,0.));
#160955=CARTESIAN_POINT('Ctrl Pts',(7.72387574915544,71.4447853996916,0.));
#160956=CARTESIAN_POINT('Ctrl Pts',(7.7135290083452,71.4234160144925,0.));
#160957=CARTESIAN_POINT('Ctrl Pts',(7.70322196765539,71.4020752058796,0.));
#160958=CARTESIAN_POINT('Ctrl Pts',(7.69295462424612,71.3807631122331,0.));
#160959=CARTESIAN_POINT('Ctrl Pts',(7.68272697517086,71.3594798725281,0.));
#160960=CARTESIAN_POINT('Ctrl Pts',(7.67253901737553,71.3382256263414,0.));
#160961=CARTESIAN_POINT('Ctrl Pts',(7.66239074769163,71.3170005138502,0.));
#160962=CARTESIAN_POINT('Ctrl Pts',(7.65228216283404,71.2958046758372,0.));
#160963=CARTESIAN_POINT('Ctrl Pts',(7.64221325940725,71.2746382537007,0.));
#160964=CARTESIAN_POINT('Ctrl Pts',(7.63218403390538,71.2535013894602,0.));
#160965=CARTESIAN_POINT('Ctrl Pts',(7.62219448271109,71.2323942257609,0.));
#160966=CARTESIAN_POINT('Ctrl Pts',(7.61224460208838,71.211316905874,0.));
#160967=CARTESIAN_POINT('Ctrl Pts',(7.60233438818097,71.1902695737013,0.));
#160968=CARTESIAN_POINT('Ctrl Pts',(7.59246383701814,71.1692523737844,0.));
#160969=CARTESIAN_POINT('Ctrl Pts',(7.58263294451452,71.1482654513119,0.));
#160970=CARTESIAN_POINT('Ctrl Pts',(7.57284170646886,71.1273089521234,0.));
#160971=CARTESIAN_POINT('Ctrl Pts',(7.56309011855657,71.106383022711,0.));
#160972=CARTESIAN_POINT('Ctrl Pts',(7.55337817632917,71.0854878102243,0.));
#160973=CARTESIAN_POINT('Ctrl Pts',(7.5437058752198,71.0646234624811,0.));
#160974=CARTESIAN_POINT('Ctrl Pts',(7.53407321054263,71.043790127973,0.));
#160975=CARTESIAN_POINT('Ctrl Pts',(7.52448017749125,71.0229879558699,0.));
#160976=CARTESIAN_POINT('Ctrl Pts',(7.51492677113091,71.002217096021,0.));
#160977=CARTESIAN_POINT('Ctrl Pts',(7.50541298639928,70.9814776989612,0.));
#160978=CARTESIAN_POINT('Ctrl Pts',(7.4959388181113,70.9607699159218,0.));
#160979=CARTESIAN_POINT('Ctrl Pts',(7.48650426095824,70.940093898837,0.));
#160980=CARTESIAN_POINT('Ctrl Pts',(7.47710930950563,70.9194498003493,0.));
#160981=CARTESIAN_POINT('Ctrl Pts',(7.46775395818527,70.8988377738104,0.));
#160982=CARTESIAN_POINT('Ctrl Pts',(7.45843820129782,70.87825797329,0.));
#160983=CARTESIAN_POINT('Ctrl Pts',(7.44916203301648,70.8577105535848,0.));
#160984=CARTESIAN_POINT('Ctrl Pts',(7.43992544738606,70.8371956702241,0.));
#160985=CARTESIAN_POINT('Ctrl Pts',(7.43072843832015,70.8167134794737,0.));
#160986=CARTESIAN_POINT('Ctrl Pts',(7.42157099959326,70.796264138335,0.));
#160987=CARTESIAN_POINT('Ctrl Pts',(7.41245312484498,70.7758478045576,0.));
#160988=CARTESIAN_POINT('Ctrl Pts',(7.40337480758237,70.7554646366514,0.));
#160989=CARTESIAN_POINT('Ctrl Pts',(7.39433604117891,70.735114793895,0.));
#160990=CARTESIAN_POINT('Ctrl Pts',(7.38533681887028,70.7147984363423,0.));
#160991=CARTESIAN_POINT('Ctrl Pts',(7.37637713374761,70.6945157248269,0.));
#160992=CARTESIAN_POINT('Ctrl Pts',(7.36745697876295,70.6742668209685,0.));
#160993=CARTESIAN_POINT('Ctrl Pts',(7.35857634673052,70.6540518871772,0.));
#160994=CARTESIAN_POINT('Ctrl Pts',(7.34973523032581,70.6338710866562,0.));
#160995=CARTESIAN_POINT('Ctrl Pts',(7.34093362208018,70.6137245834002,0.));
#160996=CARTESIAN_POINT('Ctrl Pts',(7.33217151437608,70.5936125421958,0.));
#160997=CARTESIAN_POINT('Ctrl Pts',(7.32344889945237,70.573535128649,0.));
#160998=CARTESIAN_POINT('Ctrl Pts',(7.31476576940404,70.5534925092053,0.));
#160999=CARTESIAN_POINT('Ctrl Pts',(7.30612211618047,70.5334848511675,0.));
#161000=CARTESIAN_POINT('Ctrl Pts',(7.29751793157801,70.5135123227147,0.));
#161001=CARTESIAN_POINT('Ctrl Pts',(7.28895320723836,70.4935750929029,0.));
#161002=CARTESIAN_POINT('Ctrl Pts',(7.2804279346545,70.4736733316463,0.));
#161003=CARTESIAN_POINT('Ctrl Pts',(7.27194210517058,70.4538072096986,0.));
#161004=CARTESIAN_POINT('Ctrl Pts',(7.26349570998051,70.433976898636,0.));
#161005=CARTESIAN_POINT('Ctrl Pts',(7.25508874012076,70.4141825708207,0.));
#161006=CARTESIAN_POINT('Ctrl Pts',(7.24672118647116,70.3944243994532,0.));
#161007=CARTESIAN_POINT('Ctrl Pts',(7.23839303975626,70.3747025586569,0.));
#161008=CARTESIAN_POINT('Ctrl Pts',(7.23010429054231,70.3550172235486,0.));
#161009=CARTESIAN_POINT('Ctrl Pts',(7.22185492923178,70.3353685703097,0.));
#161010=CARTESIAN_POINT('Ctrl Pts',(7.21364494605425,70.3157567762561,0.));
#161011=CARTESIAN_POINT('Ctrl Pts',(7.20547433107458,70.2961820197051,0.));
#161012=CARTESIAN_POINT('Ctrl Pts',(7.19734307419861,70.276644479827,0.));
#161013=CARTESIAN_POINT('Ctrl Pts',(7.18925116517563,70.2571443365198,0.));
#161014=CARTESIAN_POINT('Ctrl Pts',(7.18119859359801,70.2376817702239,0.));
#161015=CARTESIAN_POINT('Ctrl Pts',(7.17318534889747,70.2182569619028,0.));
#161016=CARTESIAN_POINT('Ctrl Pts',(7.16521142033893,70.1988700934622,0.));
#161017=CARTESIAN_POINT('Ctrl Pts',(7.15727679700946,70.1795213481196,0.));
#161018=CARTESIAN_POINT('Ctrl Pts',(7.14938146780801,70.1602109107188,0.));
#161019=CARTESIAN_POINT('Ctrl Pts',(7.14152542142339,70.1409389682389,0.));
#161020=CARTESIAN_POINT('Ctrl Pts',(7.13370864634399,70.1217057094456,0.));
#161021=CARTESIAN_POINT('Ctrl Pts',(7.12593113088871,70.1025113239463,0.));
#161022=CARTESIAN_POINT('Ctrl Pts',(7.11819286322824,70.0833560013971,0.));
#161023=CARTESIAN_POINT('Ctrl Pts',(7.11049383140482,70.06423993069,0.));
#161024=CARTESIAN_POINT('Ctrl Pts',(7.10283402335091,70.0451632990137,0.));
#161025=CARTESIAN_POINT('Ctrl Pts',(7.09521342684301,70.0261262936435,0.));
#161026=CARTESIAN_POINT('Ctrl Pts',(7.08763202944274,70.0071291040791,0.));
#161027=CARTESIAN_POINT('Ctrl Pts',(7.08008981844643,69.988171923787,0.));
#161028=CARTESIAN_POINT('Ctrl Pts',(7.07258678080793,69.9692549527256,0.));
#161029=CARTESIAN_POINT('Ctrl Pts',(7.06512290312803,69.9503783975676,0.));
#161030=CARTESIAN_POINT('Ctrl Pts',(7.05769817180825,69.9315424664252,0.));
#161031=CARTESIAN_POINT('Ctrl Pts',(7.05031257318108,69.9127473642087,0.));
#161032=CARTESIAN_POINT('Ctrl Pts',(7.04296609362187,69.8939932885864,0.));
#161033=CARTESIAN_POINT('Ctrl Pts',(7.03565871972266,69.8752804235296,0.));
#161034=CARTESIAN_POINT('Ctrl Pts',(7.02839043811863,69.8566089455448,0.));
#161035=CARTESIAN_POINT('Ctrl Pts',(7.02116123514488,69.8379790360574,0.));
#161036=CARTESIAN_POINT('Ctrl Pts',(7.01397109655456,69.8193908913722,0.));
#161037=CARTESIAN_POINT('Ctrl Pts',(7.00682000718105,69.8008447346782,0.));
#161038=CARTESIAN_POINT('Ctrl Pts',(6.99970795069399,69.7823408242446,0.));
#161039=CARTESIAN_POINT('Ctrl Pts',(6.9926349102786,69.7638794280263,0.));
#161040=CARTESIAN_POINT('Ctrl Pts',(6.98560086924173,69.7454607995524,0.));
#161041=CARTESIAN_POINT('Ctrl Pts',(6.97860581164569,69.7270851557443,0.));
#161042=CARTESIAN_POINT('Ctrl Pts',(6.97164972291582,69.7087526480249,0.));
#161043=CARTESIAN_POINT('Ctrl Pts',(6.9647325904973,69.6904633605834,0.));
#161044=CARTESIAN_POINT('Ctrl Pts',(6.95923004173796,69.6758665380764,0.));
#161045=CARTESIAN_POINT('Ctrl Pts',(6.95512065317731,69.6649383920075,0.));
#161046=CARTESIAN_POINT('Ctrl Pts',(6.95238884849076,69.6576616146559,0.));
#161047=CARTESIAN_POINT('Ctrl Pts',(6.95102489306928,69.6540253893193,0.));
#161048=CARTESIAN_POINT('Ctrl Pts',(15.5142209845168,72.8667204369977,0.));
#161049=CARTESIAN_POINT('Ctrl Pts',(15.5142209845168,72.8667204369977,12.));
#161050=CARTESIAN_POINT('Ctrl Pts',(15.5108715869174,72.8622377860957,0.));
#161051=CARTESIAN_POINT('Ctrl Pts',(15.5108715869174,72.8622377860957,12.));
#161052=CARTESIAN_POINT('Ctrl Pts',(15.5041768664089,72.8532737732124,0.));
#161053=CARTESIAN_POINT('Ctrl Pts',(15.5041768664089,72.8532737732124,12.));
#161054=CARTESIAN_POINT('Ctrl Pts',(15.494147009717,72.8398316206501,0.));
#161055=CARTESIAN_POINT('Ctrl Pts',(15.494147009717,72.8398316206501,12.));
#161056=CARTESIAN_POINT('Ctrl Pts',(15.4807983165984,72.8219164844002,0.));
#161057=CARTESIAN_POINT('Ctrl Pts',(15.4807983165984,72.8219164844002,12.));
#161058=CARTESIAN_POINT('Ctrl Pts',(15.4641532053435,72.7995354604414,0.));
#161059=CARTESIAN_POINT('Ctrl Pts',(15.4641532053435,72.7995354604414,12.));
#161060=CARTESIAN_POINT('Ctrl Pts',(15.4475488590336,72.7771673494582,0.));
#161061=CARTESIAN_POINT('Ctrl Pts',(15.4475488590336,72.7771673494582,12.));
#161062=CARTESIAN_POINT('Ctrl Pts',(15.4309852897866,72.7548121825431,0.));
#161063=CARTESIAN_POINT('Ctrl Pts',(15.4309852897866,72.7548121825431,12.));
#161064=CARTESIAN_POINT('Ctrl Pts',(15.4144625111911,72.7324700089576,0.));
#161065=CARTESIAN_POINT('Ctrl Pts',(15.4144625111911,72.7324700089576,12.));
#161066=CARTESIAN_POINT('Ctrl Pts',(15.397980537311,72.710140901746,0.));
#161067=CARTESIAN_POINT('Ctrl Pts',(15.397980537311,72.710140901746,12.));
#161068=CARTESIAN_POINT('Ctrl Pts',(15.3815393822669,72.6878249557452,0.));
#161069=CARTESIAN_POINT('Ctrl Pts',(15.3815393822669,72.6878249557452,12.));
#161070=CARTESIAN_POINT('Ctrl Pts',(15.3651390602616,72.6655222797603,0.));
#161071=CARTESIAN_POINT('Ctrl Pts',(15.3651390602616,72.6655222797603,12.));
#161072=CARTESIAN_POINT('Ctrl Pts',(15.3487795854723,72.6432329903466,0.));
#161073=CARTESIAN_POINT('Ctrl Pts',(15.3487795854723,72.6432329903466,12.));
#161074=CARTESIAN_POINT('Ctrl Pts',(15.3324609719961,72.6209572051064,0.));
#161075=CARTESIAN_POINT('Ctrl Pts',(15.3324609719961,72.6209572051064,12.));
#161076=CARTESIAN_POINT('Ctrl Pts',(15.3161832337617,72.5986950357771,0.));
#161077=CARTESIAN_POINT('Ctrl Pts',(15.3161832337617,72.5986950357771,12.));
#161078=CARTESIAN_POINT('Ctrl Pts',(15.2999463844691,72.5764465826345,0.));
#161079=CARTESIAN_POINT('Ctrl Pts',(15.2999463844691,72.5764465826345,12.));
#161080=CARTESIAN_POINT('Ctrl Pts',(15.2837504376562,72.5542119383748,0.));
#161081=CARTESIAN_POINT('Ctrl Pts',(15.2837504376562,72.5542119383748,12.));
#161082=CARTESIAN_POINT('Ctrl Pts',(15.2675954067495,72.5319911908978,0.));
#161083=CARTESIAN_POINT('Ctrl Pts',(15.2675954067495,72.5319911908978,12.));
#161084=CARTESIAN_POINT('Ctrl Pts',(15.2514813051174,72.5097844266083,0.));
#161085=CARTESIAN_POINT('Ctrl Pts',(15.2514813051174,72.5097844266083,12.));
#161086=CARTESIAN_POINT('Ctrl Pts',(15.2354081461152,72.4875917332729,0.));
#161087=CARTESIAN_POINT('Ctrl Pts',(15.2354081461152,72.4875917332729,12.));
#161088=CARTESIAN_POINT('Ctrl Pts',(15.2193759431359,72.4654132036373,0.));
#161089=CARTESIAN_POINT('Ctrl Pts',(15.2193759431359,72.4654132036373,12.));
#161090=CARTESIAN_POINT('Ctrl Pts',(15.2033847096077,72.4432489350415,0.));
#161091=CARTESIAN_POINT('Ctrl Pts',(15.2033847096077,72.4432489350415,12.));
#161092=CARTESIAN_POINT('Ctrl Pts',(15.1874344589716,72.4210990277819,0.));
#161093=CARTESIAN_POINT('Ctrl Pts',(15.1874344589716,72.4210990277819,12.));
#161094=CARTESIAN_POINT('Ctrl Pts',(15.1715252046602,72.3989635838476,0.));
#161095=CARTESIAN_POINT('Ctrl Pts',(15.1715252046602,72.3989635838476,12.));
#161096=CARTESIAN_POINT('Ctrl Pts',(15.1556569600747,72.37684270559,0.));
#161097=CARTESIAN_POINT('Ctrl Pts',(15.1556569600747,72.37684270559,12.));
#161098=CARTESIAN_POINT('Ctrl Pts',(15.1398297385513,72.3547364941996,0.));
#161099=CARTESIAN_POINT('Ctrl Pts',(15.1398297385513,72.3547364941996,12.));
#161100=CARTESIAN_POINT('Ctrl Pts',(15.1240435533478,72.332645049021,0.));
#161101=CARTESIAN_POINT('Ctrl Pts',(15.1240435533478,72.332645049021,12.));
#161102=CARTESIAN_POINT('Ctrl Pts',(15.1082984176655,72.3105684683971,0.));
#161103=CARTESIAN_POINT('Ctrl Pts',(15.1082984176655,72.3105684683971,12.));
#161104=CARTESIAN_POINT('Ctrl Pts',(15.0925943446593,72.2885068501641,0.));
#161105=CARTESIAN_POINT('Ctrl Pts',(15.0925943446593,72.2885068501641,12.));
#161106=CARTESIAN_POINT('Ctrl Pts',(15.0769313474476,72.266460292285,0.));
#161107=CARTESIAN_POINT('Ctrl Pts',(15.0769313474476,72.266460292285,12.));
#161108=CARTESIAN_POINT('Ctrl Pts',(15.0613094391186,72.244428893425,0.));
#161109=CARTESIAN_POINT('Ctrl Pts',(15.0613094391186,72.244428893425,12.));
#161110=CARTESIAN_POINT('Ctrl Pts',(15.0457286327328,72.2224127535401,0.));
#161111=CARTESIAN_POINT('Ctrl Pts',(15.0457286327328,72.2224127535401,12.));
#161112=CARTESIAN_POINT('Ctrl Pts',(15.0301889413255,72.2004119736104,0.));
#161113=CARTESIAN_POINT('Ctrl Pts',(15.0301889413255,72.2004119736104,12.));
#161114=CARTESIAN_POINT('Ctrl Pts',(15.0146903779061,72.1784266553948,0.));
#161115=CARTESIAN_POINT('Ctrl Pts',(15.0146903779061,72.1784266553948,12.));
#161116=CARTESIAN_POINT('Ctrl Pts',(14.9992329554537,72.1564569011668,0.));
#161117=CARTESIAN_POINT('Ctrl Pts',(14.9992329554537,72.1564569011668,12.));
#161118=CARTESIAN_POINT('Ctrl Pts',(14.9838166869107,72.1345028134779,0.));
#161119=CARTESIAN_POINT('Ctrl Pts',(14.9838166869107,72.1345028134779,12.));
#161120=CARTESIAN_POINT('Ctrl Pts',(14.9684415851699,72.1125644948547,0.));
#161121=CARTESIAN_POINT('Ctrl Pts',(14.9684415851699,72.1125644948547,12.));
#161122=CARTESIAN_POINT('Ctrl Pts',(14.953107663077,72.0906420478085,0.));
#161123=CARTESIAN_POINT('Ctrl Pts',(14.953107663077,72.0906420478085,12.));
#161124=CARTESIAN_POINT('Ctrl Pts',(14.937814933439,72.0687355749815,0.));
#161125=CARTESIAN_POINT('Ctrl Pts',(14.937814933439,72.0687355749815,12.));
#161126=CARTESIAN_POINT('Ctrl Pts',(14.9225634090269,72.046845179251,0.));
#161127=CARTESIAN_POINT('Ctrl Pts',(14.9225634090269,72.046845179251,12.));
#161128=CARTESIAN_POINT('Ctrl Pts',(14.9073531025763,72.0249709638419,0.));
#161129=CARTESIAN_POINT('Ctrl Pts',(14.9073531025763,72.0249709638419,12.));
#161130=CARTESIAN_POINT('Ctrl Pts',(14.892184026783,72.0031130324519,0.));
#161131=CARTESIAN_POINT('Ctrl Pts',(14.892184026783,72.0031130324519,12.));
#161132=CARTESIAN_POINT('Ctrl Pts',(14.8770561943011,71.9812714893087,0.));
#161133=CARTESIAN_POINT('Ctrl Pts',(14.8770561943011,71.9812714893087,12.));
#161134=CARTESIAN_POINT('Ctrl Pts',(14.8619696177503,71.9594464391063,0.));
#161135=CARTESIAN_POINT('Ctrl Pts',(14.8619696177503,71.9594464391063,12.));
#161136=CARTESIAN_POINT('Ctrl Pts',(14.846924309716,71.9376379869668,0.));
#161137=CARTESIAN_POINT('Ctrl Pts',(14.846924309716,71.9376379869668,12.));
#161138=CARTESIAN_POINT('Ctrl Pts',(14.8319202827482,71.9158462383915,0.));
#161139=CARTESIAN_POINT('Ctrl Pts',(14.8319202827482,71.9158462383915,12.));
#161140=CARTESIAN_POINT('Ctrl Pts',(14.816957549356,71.8940712992119,0.));
#161141=CARTESIAN_POINT('Ctrl Pts',(14.816957549356,71.8940712992119,12.));
#161142=CARTESIAN_POINT('Ctrl Pts',(14.8020361220003,71.872313275546,0.));
#161143=CARTESIAN_POINT('Ctrl Pts',(14.8020361220003,71.872313275546,12.));
#161144=CARTESIAN_POINT('Ctrl Pts',(14.7871560131021,71.8505722738286,0.));
#161145=CARTESIAN_POINT('Ctrl Pts',(14.7871560131021,71.8505722738286,12.));
#161146=CARTESIAN_POINT('Ctrl Pts',(14.7723172350454,71.8288484008343,0.));
#161147=CARTESIAN_POINT('Ctrl Pts',(14.7723172350454,71.8288484008343,12.));
#161148=CARTESIAN_POINT('Ctrl Pts',(14.7575198001776,71.8071417637019,0.));
#161149=CARTESIAN_POINT('Ctrl Pts',(14.7575198001776,71.8071417637019,12.));
#161150=CARTESIAN_POINT('Ctrl Pts',(14.7427637208071,71.7854524699563,0.));
#161151=CARTESIAN_POINT('Ctrl Pts',(14.7427637208071,71.7854524699563,12.));
#161152=CARTESIAN_POINT('Ctrl Pts',(14.7280490091954,71.7637806275316,0.));
#161153=CARTESIAN_POINT('Ctrl Pts',(14.7280490091954,71.7637806275316,12.));
#161154=CARTESIAN_POINT('Ctrl Pts',(14.7133756775622,71.7421263447707,0.));
#161155=CARTESIAN_POINT('Ctrl Pts',(14.7133756775622,71.7421263447707,12.));
#161156=CARTESIAN_POINT('Ctrl Pts',(14.6987437380898,71.7204897304186,0.));
#161157=CARTESIAN_POINT('Ctrl Pts',(14.6987437380898,71.7204897304186,12.));
#161158=CARTESIAN_POINT('Ctrl Pts',(14.6841532029231,71.698870893617,0.));
#161159=CARTESIAN_POINT('Ctrl Pts',(14.6841532029231,71.698870893617,12.));
#161160=CARTESIAN_POINT('Ctrl Pts',(14.6696040841679,71.6772699438966,0.));
#161161=CARTESIAN_POINT('Ctrl Pts',(14.6696040841679,71.6772699438966,12.));
#161162=CARTESIAN_POINT('Ctrl Pts',(14.6550963938832,71.6556869911669,0.));
#161163=CARTESIAN_POINT('Ctrl Pts',(14.6550963938832,71.6556869911669,12.));
#161164=CARTESIAN_POINT('Ctrl Pts',(14.6406301440817,71.6341221457175,0.));
#161165=CARTESIAN_POINT('Ctrl Pts',(14.6406301440817,71.6341221457175,12.));
#161166=CARTESIAN_POINT('Ctrl Pts',(14.6262053467372,71.6125755182295,0.));
#161167=CARTESIAN_POINT('Ctrl Pts',(14.6262053467372,71.6125755182295,12.));
#161168=CARTESIAN_POINT('Ctrl Pts',(14.611822013785,71.5910472197815,0.));
#161169=CARTESIAN_POINT('Ctrl Pts',(14.611822013785,71.5910472197815,12.));
#161170=CARTESIAN_POINT('Ctrl Pts',(14.597480157121,71.569537361856,0.));
#161171=CARTESIAN_POINT('Ctrl Pts',(14.597480157121,71.569537361856,12.));
#161172=CARTESIAN_POINT('Ctrl Pts',(14.5831797885951,71.5480460563445,0.));
#161173=CARTESIAN_POINT('Ctrl Pts',(14.5831797885951,71.5480460563445,12.));
#161174=CARTESIAN_POINT('Ctrl Pts',(14.568920920009,71.5265734155501,0.));
#161175=CARTESIAN_POINT('Ctrl Pts',(14.568920920009,71.5265734155501,12.));
#161176=CARTESIAN_POINT('Ctrl Pts',(14.5547035631234,71.5051195521914,0.));
#161177=CARTESIAN_POINT('Ctrl Pts',(14.5547035631234,71.5051195521914,12.));
#161178=CARTESIAN_POINT('Ctrl Pts',(14.540527729659,71.4836845794052,0.));
#161179=CARTESIAN_POINT('Ctrl Pts',(14.540527729659,71.4836845794052,12.));
#161180=CARTESIAN_POINT('Ctrl Pts',(14.5263934312969,71.4622686107475,0.));
#161181=CARTESIAN_POINT('Ctrl Pts',(14.5263934312969,71.4622686107475,12.));
#161182=CARTESIAN_POINT('Ctrl Pts',(14.5123006796728,71.4408717601917,0.));
#161183=CARTESIAN_POINT('Ctrl Pts',(14.5123006796728,71.4408717601917,12.));
#161184=CARTESIAN_POINT('Ctrl Pts',(14.4982494863716,71.4194941421279,0.));
#161185=CARTESIAN_POINT('Ctrl Pts',(14.4982494863716,71.4194941421279,12.));
#161186=CARTESIAN_POINT('Ctrl Pts',(14.4842398629353,71.398135871371,0.));
#161187=CARTESIAN_POINT('Ctrl Pts',(14.4842398629353,71.398135871371,12.));
#161188=CARTESIAN_POINT('Ctrl Pts',(14.470271820865,71.3767970631642,0.));
#161189=CARTESIAN_POINT('Ctrl Pts',(14.470271820865,71.3767970631642,12.));
#161190=CARTESIAN_POINT('Ctrl Pts',(14.4563453716204,71.3554778331835,0.));
#161191=CARTESIAN_POINT('Ctrl Pts',(14.4563453716204,71.3554778331835,12.));
#161192=CARTESIAN_POINT('Ctrl Pts',(14.4424605266166,71.3341782975393,0.));
#161193=CARTESIAN_POINT('Ctrl Pts',(14.4424605266166,71.3341782975393,12.));
#161194=CARTESIAN_POINT('Ctrl Pts',(14.4286172972168,71.3128985727777,0.));
#161195=CARTESIAN_POINT('Ctrl Pts',(14.4286172972168,71.3128985727777,12.));
#161196=CARTESIAN_POINT('Ctrl Pts',(14.4148156947384,71.2916387758864,0.));
#161197=CARTESIAN_POINT('Ctrl Pts',(14.4148156947384,71.2916387758864,12.));
#161198=CARTESIAN_POINT('Ctrl Pts',(14.401055730457,71.2703990242986,0.));
#161199=CARTESIAN_POINT('Ctrl Pts',(14.401055730457,71.2703990242986,12.));
#161200=CARTESIAN_POINT('Ctrl Pts',(14.3873374156056,71.2491794358956,0.));
#161201=CARTESIAN_POINT('Ctrl Pts',(14.3873374156056,71.2491794358956,12.));
#161202=CARTESIAN_POINT('Ctrl Pts',(14.3736607613723,71.2279801290088,0.));
#161203=CARTESIAN_POINT('Ctrl Pts',(14.3736607613723,71.2279801290088,12.));
#161204=CARTESIAN_POINT('Ctrl Pts',(14.3600257788927,71.2068012224187,0.));
#161205=CARTESIAN_POINT('Ctrl Pts',(14.3600257788927,71.2068012224187,12.));
#161206=CARTESIAN_POINT('Ctrl Pts',(14.3464324792537,71.185642835361,0.));
#161207=CARTESIAN_POINT('Ctrl Pts',(14.3464324792537,71.185642835361,12.));
#161208=CARTESIAN_POINT('Ctrl Pts',(14.3328808734993,71.1645050875323,0.));
#161209=CARTESIAN_POINT('Ctrl Pts',(14.3328808734993,71.1645050875323,12.));
#161210=CARTESIAN_POINT('Ctrl Pts',(14.3193709726295,71.1433880990932,0.));
#161211=CARTESIAN_POINT('Ctrl Pts',(14.3193709726295,71.1433880990932,12.));
#161212=CARTESIAN_POINT('Ctrl Pts',(14.3059027875993,71.1222919906719,0.));
#161213=CARTESIAN_POINT('Ctrl Pts',(14.3059027875993,71.1222919906719,12.));
#161214=CARTESIAN_POINT('Ctrl Pts',(14.2924763293101,71.1012168833626,0.));
#161215=CARTESIAN_POINT('Ctrl Pts',(14.2924763293101,71.1012168833626,12.));
#161216=CARTESIAN_POINT('Ctrl Pts',(14.2790916086129,71.0801628987314,0.));
#161217=CARTESIAN_POINT('Ctrl Pts',(14.2790916086129,71.0801628987314,12.));
#161218=CARTESIAN_POINT('Ctrl Pts',(14.2657486363136,71.059130158822,0.));
#161219=CARTESIAN_POINT('Ctrl Pts',(14.2657486363136,71.059130158822,12.));
#161220=CARTESIAN_POINT('Ctrl Pts',(14.2524474231732,71.0381187861585,0.));
#161221=CARTESIAN_POINT('Ctrl Pts',(14.2524474231732,71.0381187861585,12.));
#161222=CARTESIAN_POINT('Ctrl Pts',(14.2391879799063,71.0171289037493,0.));
#161223=CARTESIAN_POINT('Ctrl Pts',(14.2391879799063,71.0171289037493,12.));
#161224=CARTESIAN_POINT('Ctrl Pts',(14.2259703171739,70.996160635087,0.));
#161225=CARTESIAN_POINT('Ctrl Pts',(14.2259703171739,70.996160635087,12.));
#161226=CARTESIAN_POINT('Ctrl Pts',(14.2127944455841,70.9752141041527,0.));
#161227=CARTESIAN_POINT('Ctrl Pts',(14.2127944455841,70.9752141041527,12.));
#161228=CARTESIAN_POINT('Ctrl Pts',(14.1996603756984,70.9542894354221,0.));
#161229=CARTESIAN_POINT('Ctrl Pts',(14.1996603756984,70.9542894354221,12.));
#161230=CARTESIAN_POINT('Ctrl Pts',(14.1865681180321,70.9333867538705,0.));
#161231=CARTESIAN_POINT('Ctrl Pts',(14.1865681180321,70.9333867538705,12.));
#161232=CARTESIAN_POINT('Ctrl Pts',(14.1735176830533,70.9125061849744,0.));
#161233=CARTESIAN_POINT('Ctrl Pts',(14.1735176830533,70.9125061849744,12.));
#161234=CARTESIAN_POINT('Ctrl Pts',(14.1605090811754,70.8916478547131,0.));
#161235=CARTESIAN_POINT('Ctrl Pts',(14.1605090811754,70.8916478547131,12.));
#161236=CARTESIAN_POINT('Ctrl Pts',(14.1475423227567,70.8708118895718,0.));
#161237=CARTESIAN_POINT('Ctrl Pts',(14.1475423227567,70.8708118895718,12.));
#161238=CARTESIAN_POINT('Ctrl Pts',(14.1346174181079,70.8499984165493,0.));
#161239=CARTESIAN_POINT('Ctrl Pts',(14.1346174181079,70.8499984165493,12.));
#161240=CARTESIAN_POINT('Ctrl Pts',(14.1217343774914,70.8292075631624,0.));
#161241=CARTESIAN_POINT('Ctrl Pts',(14.1217343774914,70.8292075631624,12.));
#161242=CARTESIAN_POINT('Ctrl Pts',(14.1088932111214,70.8084394574491,0.));
#161243=CARTESIAN_POINT('Ctrl Pts',(14.1088932111214,70.8084394574491,12.));
#161244=CARTESIAN_POINT('Ctrl Pts',(14.0960939291568,70.787694227969,0.));
#161245=CARTESIAN_POINT('Ctrl Pts',(14.0960939291568,70.787694227969,12.));
#161246=CARTESIAN_POINT('Ctrl Pts',(14.0833365416995,70.7669720038067,0.));
#161247=CARTESIAN_POINT('Ctrl Pts',(14.0833365416995,70.7669720038067,12.));
#161248=CARTESIAN_POINT('Ctrl Pts',(14.0706210588015,70.7462729145799,0.));
#161249=CARTESIAN_POINT('Ctrl Pts',(14.0706210588015,70.7462729145799,12.));
#161250=CARTESIAN_POINT('Ctrl Pts',(14.0579474904657,70.7255970904433,0.));
#161251=CARTESIAN_POINT('Ctrl Pts',(14.0579474904657,70.7255970904433,12.));
#161252=CARTESIAN_POINT('Ctrl Pts',(14.0453158466451,70.7049446620931,0.));
#161253=CARTESIAN_POINT('Ctrl Pts',(14.0453158466451,70.7049446620931,12.));
#161254=CARTESIAN_POINT('Ctrl Pts',(14.0327261372363,70.6843157607672,0.));
#161255=CARTESIAN_POINT('Ctrl Pts',(14.0327261372363,70.6843157607672,12.));
#161256=CARTESIAN_POINT('Ctrl Pts',(14.020178372077,70.6637105182487,0.));
#161257=CARTESIAN_POINT('Ctrl Pts',(14.020178372077,70.6637105182487,12.));
#161258=CARTESIAN_POINT('Ctrl Pts',(14.0076725609537,70.6431290668744,0.));
#161259=CARTESIAN_POINT('Ctrl Pts',(14.0076725609537,70.6431290668744,12.));
#161260=CARTESIAN_POINT('Ctrl Pts',(13.9952087136018,70.6225715395392,0.));
#161261=CARTESIAN_POINT('Ctrl Pts',(13.9952087136018,70.6225715395392,12.));
#161262=CARTESIAN_POINT('Ctrl Pts',(13.9827868397057,70.6020380697004,0.));
#161263=CARTESIAN_POINT('Ctrl Pts',(13.9827868397057,70.6020380697004,12.));
#161264=CARTESIAN_POINT('Ctrl Pts',(13.9704069488918,70.5815287913791,0.));
#161265=CARTESIAN_POINT('Ctrl Pts',(13.9704069488918,70.5815287913791,12.));
#161266=CARTESIAN_POINT('Ctrl Pts',(13.9580690507262,70.5610438391622,0.));
#161267=CARTESIAN_POINT('Ctrl Pts',(13.9580690507262,70.5610438391622,12.));
#161268=CARTESIAN_POINT('Ctrl Pts',(13.9457731547217,70.5405833482123,0.));
#161269=CARTESIAN_POINT('Ctrl Pts',(13.9457731547217,70.5405833482123,12.));
#161270=CARTESIAN_POINT('Ctrl Pts',(13.9335192703389,70.5201474542717,0.));
#161271=CARTESIAN_POINT('Ctrl Pts',(13.9335192703389,70.5201474542717,12.));
#161272=CARTESIAN_POINT('Ctrl Pts',(13.9213074069852,70.4997362936671,0.));
#161273=CARTESIAN_POINT('Ctrl Pts',(13.9213074069852,70.4997362936671,12.));
#161274=CARTESIAN_POINT('Ctrl Pts',(13.9091375740084,70.4793500033106,0.));
#161275=CARTESIAN_POINT('Ctrl Pts',(13.9091375740084,70.4793500033106,12.));
#161276=CARTESIAN_POINT('Ctrl Pts',(13.8970097806947,70.4589887207043,0.));
#161277=CARTESIAN_POINT('Ctrl Pts',(13.8970097806947,70.4589887207043,12.));
#161278=CARTESIAN_POINT('Ctrl Pts',(13.8849240362757,70.4386525839492,0.));
#161279=CARTESIAN_POINT('Ctrl Pts',(13.8849240362757,70.4386525839492,12.));
#161280=CARTESIAN_POINT('Ctrl Pts',(13.8728803499284,70.4183417317486,0.));
#161281=CARTESIAN_POINT('Ctrl Pts',(13.8728803499284,70.4183417317486,12.));
#161282=CARTESIAN_POINT('Ctrl Pts',(13.8608787307754,70.3980563034142,0.));
#161283=CARTESIAN_POINT('Ctrl Pts',(13.8608787307754,70.3980563034142,12.));
#161284=CARTESIAN_POINT('Ctrl Pts',(13.8489191878774,70.377796438866,0.));
#161285=CARTESIAN_POINT('Ctrl Pts',(13.8489191878774,70.377796438866,12.));
#161286=CARTESIAN_POINT('Ctrl Pts',(13.8370017302319,70.3575622786373,0.));
#161287=CARTESIAN_POINT('Ctrl Pts',(13.8370017302319,70.3575622786373,12.));
#161288=CARTESIAN_POINT('Ctrl Pts',(13.8251263667799,70.3373539638841,0.));
#161289=CARTESIAN_POINT('Ctrl Pts',(13.8251263667799,70.3373539638841,12.));
#161290=CARTESIAN_POINT('Ctrl Pts',(13.8132931064067,70.3171716363912,0.));
#161291=CARTESIAN_POINT('Ctrl Pts',(13.8132931064067,70.3171716363912,12.));
#161292=CARTESIAN_POINT('Ctrl Pts',(13.8015019579411,70.2970154385763,0.));
#161293=CARTESIAN_POINT('Ctrl Pts',(13.8015019579411,70.2970154385763,12.));
#161294=CARTESIAN_POINT('Ctrl Pts',(13.7897529301483,70.2768855134909,0.));
#161295=CARTESIAN_POINT('Ctrl Pts',(13.7897529301483,70.2768855134909,12.));
#161296=CARTESIAN_POINT('Ctrl Pts',(13.7780460317284,70.2567820048253,0.));
#161297=CARTESIAN_POINT('Ctrl Pts',(13.7780460317284,70.2567820048253,12.));
#161298=CARTESIAN_POINT('Ctrl Pts',(13.7663812713235,70.2367050569174,0.));
#161299=CARTESIAN_POINT('Ctrl Pts',(13.7663812713235,70.2367050569174,12.));
#161300=CARTESIAN_POINT('Ctrl Pts',(13.7547586575178,70.216654814759,0.));
#161301=CARTESIAN_POINT('Ctrl Pts',(13.7547586575178,70.216654814759,12.));
#161302=CARTESIAN_POINT('Ctrl Pts',(13.7431781988368,70.1966314240012,0.));
#161303=CARTESIAN_POINT('Ctrl Pts',(13.7431781988368,70.1966314240012,12.));
#161304=CARTESIAN_POINT('Ctrl Pts',(13.73163990374,70.1766350309554,0.));
#161305=CARTESIAN_POINT('Ctrl Pts',(13.73163990374,70.1766350309554,12.));
#161306=CARTESIAN_POINT('Ctrl Pts',(13.7201437806207,70.1566657825989,0.));
#161307=CARTESIAN_POINT('Ctrl Pts',(13.7201437806207,70.1566657825989,12.));
#161308=CARTESIAN_POINT('Ctrl Pts',(13.7086898378127,70.1367238265853,0.));
#161309=CARTESIAN_POINT('Ctrl Pts',(13.7086898378127,70.1367238265853,12.));
#161310=CARTESIAN_POINT('Ctrl Pts',(13.6972780835898,70.1168093112493,0.));
#161311=CARTESIAN_POINT('Ctrl Pts',(13.6972780835898,70.1168093112493,12.));
#161312=CARTESIAN_POINT('Ctrl Pts',(13.685908526165,70.0969223856123,0.));
#161313=CARTESIAN_POINT('Ctrl Pts',(13.685908526165,70.0969223856123,12.));
#161314=CARTESIAN_POINT('Ctrl Pts',(13.6745811736825,70.0770631993831,0.));
#161315=CARTESIAN_POINT('Ctrl Pts',(13.6745811736825,70.0770631993831,12.));
#161316=CARTESIAN_POINT('Ctrl Pts',(13.6632960342192,70.057231902965,0.));
#161317=CARTESIAN_POINT('Ctrl Pts',(13.6632960342192,70.057231902965,12.));
#161318=CARTESIAN_POINT('Ctrl Pts',(13.6520531157904,70.037428647466,0.));
#161319=CARTESIAN_POINT('Ctrl Pts',(13.6520531157904,70.037428647466,12.));
#161320=CARTESIAN_POINT('Ctrl Pts',(13.6408524263496,70.0176535847047,0.));
#161321=CARTESIAN_POINT('Ctrl Pts',(13.6408524263496,70.0176535847047,12.));
#161322=CARTESIAN_POINT('Ctrl Pts',(13.6296939737866,69.9979068672163,0.));
#161323=CARTESIAN_POINT('Ctrl Pts',(13.6296939737866,69.9979068672163,12.));
#161324=CARTESIAN_POINT('Ctrl Pts',(13.61857776592,69.9781886482543,0.));
#161325=CARTESIAN_POINT('Ctrl Pts',(13.61857776592,69.9781886482543,12.));
#161326=CARTESIAN_POINT('Ctrl Pts',(13.6075038105,69.9584990817989,0.));
#161327=CARTESIAN_POINT('Ctrl Pts',(13.6075038105,69.9584990817989,12.));
#161328=CARTESIAN_POINT('Ctrl Pts',(13.5964721152136,69.9388383225655,0.));
#161329=CARTESIAN_POINT('Ctrl Pts',(13.5964721152136,69.9388383225655,12.));
#161330=CARTESIAN_POINT('Ctrl Pts',(13.5854826876834,69.9192065260107,0.));
#161331=CARTESIAN_POINT('Ctrl Pts',(13.5854826876834,69.9192065260107,12.));
#161332=CARTESIAN_POINT('Ctrl Pts',(13.5745355354657,69.899603848336,0.));
#161333=CARTESIAN_POINT('Ctrl Pts',(13.5745355354657,69.899603848336,12.));
#161334=CARTESIAN_POINT('Ctrl Pts',(13.5636306660422,69.880030446488,0.));
#161335=CARTESIAN_POINT('Ctrl Pts',(13.5636306660422,69.880030446488,12.));
#161336=CARTESIAN_POINT('Ctrl Pts',(13.5527680868256,69.8604864781705,0.));
#161337=CARTESIAN_POINT('Ctrl Pts',(13.5527680868256,69.8604864781705,12.));
#161338=CARTESIAN_POINT('Ctrl Pts',(13.5419478051626,69.840972101856,0.));
#161339=CARTESIAN_POINT('Ctrl Pts',(13.5419478051626,69.840972101856,12.));
#161340=CARTESIAN_POINT('Ctrl Pts',(13.5311698283339,69.8214874767944,0.));
#161341=CARTESIAN_POINT('Ctrl Pts',(13.5311698283339,69.8214874767944,12.));
#161342=CARTESIAN_POINT('Ctrl Pts',(13.5204341635507,69.8020327630204,0.));
#161343=CARTESIAN_POINT('Ctrl Pts',(13.5204341635507,69.8020327630204,12.));
#161344=CARTESIAN_POINT('Ctrl Pts',(13.5097408179478,69.7826081213575,0.));
#161345=CARTESIAN_POINT('Ctrl Pts',(13.5097408179478,69.7826081213575,12.));
#161346=CARTESIAN_POINT('Ctrl Pts',(13.4990897985904,69.7632137134247,0.));
#161347=CARTESIAN_POINT('Ctrl Pts',(13.4990897985904,69.7632137134247,12.));
#161348=CARTESIAN_POINT('Ctrl Pts',(13.4884811124748,69.7438497016404,0.));
#161349=CARTESIAN_POINT('Ctrl Pts',(13.4884811124748,69.7438497016404,12.));
#161350=CARTESIAN_POINT('Ctrl Pts',(13.4779147665285,69.7245162492251,0.));
#161351=CARTESIAN_POINT('Ctrl Pts',(13.4779147665285,69.7245162492251,12.));
#161352=CARTESIAN_POINT('Ctrl Pts',(13.4673907676045,69.7052135202003,0.));
#161353=CARTESIAN_POINT('Ctrl Pts',(13.4673907676045,69.7052135202003,12.));
#161354=CARTESIAN_POINT('Ctrl Pts',(13.4569091224762,69.6859416793898,0.));
#161355=CARTESIAN_POINT('Ctrl Pts',(13.4569091224762,69.6859416793898,12.));
#161356=CARTESIAN_POINT('Ctrl Pts',(13.4464698378456,69.6667008924454,0.));
#161357=CARTESIAN_POINT('Ctrl Pts',(13.4464698378456,69.6667008924454,12.));
#161358=CARTESIAN_POINT('Ctrl Pts',(13.4360729203444,69.6474913258684,0.));
#161359=CARTESIAN_POINT('Ctrl Pts',(13.4360729203444,69.6474913258684,12.));
#161360=CARTESIAN_POINT('Ctrl Pts',(13.425718376534,69.6283131470267,0.));
#161361=CARTESIAN_POINT('Ctrl Pts',(13.425718376534,69.6283131470267,12.));
#161362=CARTESIAN_POINT('Ctrl Pts',(13.4154062128998,69.6091665241743,0.));
#161363=CARTESIAN_POINT('Ctrl Pts',(13.4154062128998,69.6091665241743,12.));
#161364=CARTESIAN_POINT('Ctrl Pts',(13.4051364358494,69.5900516264524,0.));
#161365=CARTESIAN_POINT('Ctrl Pts',(13.4051364358494,69.5900516264524,12.));
#161366=CARTESIAN_POINT('Ctrl Pts',(13.3949090517173,69.5709686238701,0.));
#161367=CARTESIAN_POINT('Ctrl Pts',(13.3949090517173,69.5709686238701,12.));
#161368=CARTESIAN_POINT('Ctrl Pts',(13.3847240667626,69.5519176872857,0.));
#161369=CARTESIAN_POINT('Ctrl Pts',(13.3847240667626,69.5519176872857,12.));
#161370=CARTESIAN_POINT('Ctrl Pts',(13.3745814871667,69.5328989883899,0.));
#161371=CARTESIAN_POINT('Ctrl Pts',(13.3745814871667,69.5328989883899,12.));
#161372=CARTESIAN_POINT('Ctrl Pts',(13.3644813190225,69.5139126996703,0.));
#161373=CARTESIAN_POINT('Ctrl Pts',(13.3644813190225,69.5139126996703,12.));
#161374=CARTESIAN_POINT('Ctrl Pts',(13.3544235683399,69.4949589944633,0.));
#161375=CARTESIAN_POINT('Ctrl Pts',(13.3544235683399,69.4949589944633,12.));
#161376=CARTESIAN_POINT('Ctrl Pts',(13.3444082410546,69.4760380470382,0.));
#161377=CARTESIAN_POINT('Ctrl Pts',(13.3444082410546,69.4760380470382,12.));
#161378=CARTESIAN_POINT('Ctrl Pts',(13.3344353430313,69.4571500326673,0.));
#161379=CARTESIAN_POINT('Ctrl Pts',(13.3344353430313,69.4571500326673,12.));
#161380=CARTESIAN_POINT('Ctrl Pts',(13.3245048800641,69.4382951276983,0.));
#161381=CARTESIAN_POINT('Ctrl Pts',(13.3245048800641,69.4382951276983,12.));
#161382=CARTESIAN_POINT('Ctrl Pts',(13.3146168578738,69.4194735096238,0.));
#161383=CARTESIAN_POINT('Ctrl Pts',(13.3146168578738,69.4194735096238,12.));
#161384=CARTESIAN_POINT('Ctrl Pts',(13.3047712821046,69.4006853569485,0.));
#161385=CARTESIAN_POINT('Ctrl Pts',(13.3047712821046,69.4006853569485,12.));
#161386=CARTESIAN_POINT('Ctrl Pts',(13.2949681583164,69.3819308490408,0.));
#161387=CARTESIAN_POINT('Ctrl Pts',(13.2949681583164,69.3819308490408,12.));
#161388=CARTESIAN_POINT('Ctrl Pts',(13.2852074919767,69.3632101660072,0.));
#161389=CARTESIAN_POINT('Ctrl Pts',(13.2852074919767,69.3632101660072,12.));
#161390=CARTESIAN_POINT('Ctrl Pts',(13.2754892884437,69.3445234885088,0.));
#161391=CARTESIAN_POINT('Ctrl Pts',(13.2754892884437,69.3445234885088,12.));
#161392=CARTESIAN_POINT('Ctrl Pts',(13.2658135529616,69.3258709977416,0.));
#161393=CARTESIAN_POINT('Ctrl Pts',(13.2658135529616,69.3258709977416,12.));
#161394=CARTESIAN_POINT('Ctrl Pts',(13.2561802906901,69.3072528758546,0.));
#161395=CARTESIAN_POINT('Ctrl Pts',(13.2561802906901,69.3072528758546,12.));
#161396=CARTESIAN_POINT('Ctrl Pts',(13.2465895067264,69.2886693063193,0.));
#161397=CARTESIAN_POINT('Ctrl Pts',(13.2465895067264,69.2886693063193,12.));
#161398=CARTESIAN_POINT('Ctrl Pts',(13.2370412061218,69.2701204742436,0.));
#161399=CARTESIAN_POINT('Ctrl Pts',(13.2370412061218,69.2701204742436,12.));
#161400=CARTESIAN_POINT('Ctrl Pts',(13.2275353939044,69.2516065668809,0.));
#161401=CARTESIAN_POINT('Ctrl Pts',(13.2275353939044,69.2516065668809,12.));
#161402=CARTESIAN_POINT('Ctrl Pts',(13.2180720750586,69.2331277732819,0.));
#161403=CARTESIAN_POINT('Ctrl Pts',(13.2180720750586,69.2331277732819,12.));
#161404=CARTESIAN_POINT('Ctrl Pts',(13.2086512544729,69.2146842833506,0.));
#161405=CARTESIAN_POINT('Ctrl Pts',(13.2086512544729,69.2146842833506,12.));
#161406=CARTESIAN_POINT('Ctrl Pts',(13.1992729368928,69.1962762870524,0.));
#161407=CARTESIAN_POINT('Ctrl Pts',(13.1992729368928,69.1962762870524,12.));
#161408=CARTESIAN_POINT('Ctrl Pts',(13.1899371268689,69.1779039736026,0.));
#161409=CARTESIAN_POINT('Ctrl Pts',(13.1899371268689,69.1779039736026,12.));
#161410=CARTESIAN_POINT('Ctrl Pts',(13.1806438286944,69.1595675305294,0.));
#161411=CARTESIAN_POINT('Ctrl Pts',(13.1806438286944,69.1595675305294,12.));
#161412=CARTESIAN_POINT('Ctrl Pts',(13.1713930465142,69.141267145461,0.));
#161413=CARTESIAN_POINT('Ctrl Pts',(13.1713930465142,69.141267145461,12.));
#161414=CARTESIAN_POINT('Ctrl Pts',(13.1621847844533,69.1230030082598,0.));
#161415=CARTESIAN_POINT('Ctrl Pts',(13.1621847844533,69.1230030082598,12.));
#161416=CARTESIAN_POINT('Ctrl Pts',(13.1530190467181,69.1047753127633,0.));
#161417=CARTESIAN_POINT('Ctrl Pts',(13.1530190467181,69.1047753127633,12.));
#161418=CARTESIAN_POINT('Ctrl Pts',(13.1438958377397,69.0865842593063,0.));
#161419=CARTESIAN_POINT('Ctrl Pts',(13.1438958377397,69.0865842593063,12.));
#161420=CARTESIAN_POINT('Ctrl Pts',(13.1348151621824,69.0684300549426,0.));
#161421=CARTESIAN_POINT('Ctrl Pts',(13.1348151621824,69.0684300549426,12.));
#161422=CARTESIAN_POINT('Ctrl Pts',(13.1257770246379,69.0503129081778,0.));
#161423=CARTESIAN_POINT('Ctrl Pts',(13.1257770246379,69.0503129081778,12.));
#161424=CARTESIAN_POINT('Ctrl Pts',(13.1167814293495,69.0322330243336,0.));
#161425=CARTESIAN_POINT('Ctrl Pts',(13.1167814293495,69.0322330243336,12.));
#161426=CARTESIAN_POINT('Ctrl Pts',(13.1078283799726,69.0141906015137,0.));
#161427=CARTESIAN_POINT('Ctrl Pts',(13.1078283799726,69.0141906015137,12.));
#161428=CARTESIAN_POINT('Ctrl Pts',(13.0989178791843,68.9961858241577,0.));
#161429=CARTESIAN_POINT('Ctrl Pts',(13.0989178791843,68.9961858241577,12.));
#161430=CARTESIAN_POINT('Ctrl Pts',(13.0900499290542,68.9782188692654,0.));
#161431=CARTESIAN_POINT('Ctrl Pts',(13.0900499290542,68.9782188692654,12.));
#161432=CARTESIAN_POINT('Ctrl Pts',(13.0812245317816,68.9602899187628,0.));
#161433=CARTESIAN_POINT('Ctrl Pts',(13.0812245317816,68.9602899187628,12.));
#161434=CARTESIAN_POINT('Ctrl Pts',(13.072441690283,68.9423991694493,0.));
#161435=CARTESIAN_POINT('Ctrl Pts',(13.072441690283,68.9423991694493,12.));
#161436=CARTESIAN_POINT('Ctrl Pts',(13.0637014089018,68.9245468449865,0.));
#161437=CARTESIAN_POINT('Ctrl Pts',(13.0637014089018,68.9245468449865,12.));
#161438=CARTESIAN_POINT('Ctrl Pts',(13.0550036938793,68.9067332040842,0.));
#161439=CARTESIAN_POINT('Ctrl Pts',(13.0550036938793,68.9067332040842,12.));
#161440=CARTESIAN_POINT('Ctrl Pts',(13.0463485518185,68.8889585151431,0.));
#161441=CARTESIAN_POINT('Ctrl Pts',(13.0463485518185,68.8889585151431,12.));
#161442=CARTESIAN_POINT('Ctrl Pts',(13.0377359881864,68.8712230321823,0.));
#161443=CARTESIAN_POINT('Ctrl Pts',(13.0377359881864,68.8712230321823,12.));
#161444=CARTESIAN_POINT('Ctrl Pts',(13.0291660060118,68.8535269726871,0.));
#161445=CARTESIAN_POINT('Ctrl Pts',(13.0291660060118,68.8535269726871,12.));
#161446=CARTESIAN_POINT('Ctrl Pts',(13.0206386039729,68.835870488774,0.));
#161447=CARTESIAN_POINT('Ctrl Pts',(13.0206386039729,68.835870488774,12.));
#161448=CARTESIAN_POINT('Ctrl Pts',(13.0121537769003,68.8182536654067,0.));
#161449=CARTESIAN_POINT('Ctrl Pts',(13.0121537769003,68.8182536654067,12.));
#161450=CARTESIAN_POINT('Ctrl Pts',(13.0053999700929,68.8041919669403,0.));
#161451=CARTESIAN_POINT('Ctrl Pts',(13.0053999700929,68.8041919669403,12.));
#161452=CARTESIAN_POINT('Ctrl Pts',(13.0003537683089,68.7936635625788,0.));
#161453=CARTESIAN_POINT('Ctrl Pts',(13.0003537683089,68.7936635625788,12.));
#161454=CARTESIAN_POINT('Ctrl Pts',(12.996998146029,68.7866525680284,0.));
#161455=CARTESIAN_POINT('Ctrl Pts',(12.996998146029,68.7866525680284,12.));
#161456=CARTESIAN_POINT('Ctrl Pts',(12.9953224629497,68.7831490561748,0.));
#161457=CARTESIAN_POINT('Ctrl Pts',(12.9953224629497,68.7831490561748,12.));
#161458=CARTESIAN_POINT('',(12.9953224629497,68.7831490561748,12.));
#161459=CARTESIAN_POINT('Ctrl Pts',(12.9953224629497,68.7831490561748,12.));
#161460=CARTESIAN_POINT('Ctrl Pts',(12.996998146029,68.7866525680284,12.));
#161461=CARTESIAN_POINT('Ctrl Pts',(13.0003537683089,68.7936635625788,12.));
#161462=CARTESIAN_POINT('Ctrl Pts',(13.0053999700929,68.8041919669403,12.));
#161463=CARTESIAN_POINT('Ctrl Pts',(13.0121537769003,68.8182536654067,12.));
#161464=CARTESIAN_POINT('Ctrl Pts',(13.0206386039729,68.835870488774,12.));
#161465=CARTESIAN_POINT('Ctrl Pts',(13.0291660060118,68.8535269726871,12.));
#161466=CARTESIAN_POINT('Ctrl Pts',(13.0377359881864,68.8712230321823,12.));
#161467=CARTESIAN_POINT('Ctrl Pts',(13.0463485518185,68.8889585151431,12.));
#161468=CARTESIAN_POINT('Ctrl Pts',(13.0550036938793,68.9067332040842,12.));
#161469=CARTESIAN_POINT('Ctrl Pts',(13.0637014089018,68.9245468449865,12.));
#161470=CARTESIAN_POINT('Ctrl Pts',(13.072441690283,68.9423991694493,12.));
#161471=CARTESIAN_POINT('Ctrl Pts',(13.0812245317816,68.9602899187628,12.));
#161472=CARTESIAN_POINT('Ctrl Pts',(13.0900499290542,68.9782188692654,12.));
#161473=CARTESIAN_POINT('Ctrl Pts',(13.0989178791843,68.9961858241577,12.));
#161474=CARTESIAN_POINT('Ctrl Pts',(13.1078283799726,69.0141906015137,12.));
#161475=CARTESIAN_POINT('Ctrl Pts',(13.1167814293495,69.0322330243336,12.));
#161476=CARTESIAN_POINT('Ctrl Pts',(13.1257770246379,69.0503129081778,12.));
#161477=CARTESIAN_POINT('Ctrl Pts',(13.1348151621824,69.0684300549426,12.));
#161478=CARTESIAN_POINT('Ctrl Pts',(13.1438958377397,69.0865842593063,12.));
#161479=CARTESIAN_POINT('Ctrl Pts',(13.1530190467181,69.1047753127633,12.));
#161480=CARTESIAN_POINT('Ctrl Pts',(13.1621847844533,69.1230030082598,12.));
#161481=CARTESIAN_POINT('Ctrl Pts',(13.1713930465142,69.141267145461,12.));
#161482=CARTESIAN_POINT('Ctrl Pts',(13.1806438286944,69.1595675305294,12.));
#161483=CARTESIAN_POINT('Ctrl Pts',(13.1899371268689,69.1779039736026,12.));
#161484=CARTESIAN_POINT('Ctrl Pts',(13.1992729368928,69.1962762870524,12.));
#161485=CARTESIAN_POINT('Ctrl Pts',(13.2086512544729,69.2146842833506,12.));
#161486=CARTESIAN_POINT('Ctrl Pts',(13.2180720750586,69.2331277732819,12.));
#161487=CARTESIAN_POINT('Ctrl Pts',(13.2275353939044,69.2516065668809,12.));
#161488=CARTESIAN_POINT('Ctrl Pts',(13.2370412061218,69.2701204742436,12.));
#161489=CARTESIAN_POINT('Ctrl Pts',(13.2465895067264,69.2886693063193,12.));
#161490=CARTESIAN_POINT('Ctrl Pts',(13.2561802906901,69.3072528758546,12.));
#161491=CARTESIAN_POINT('Ctrl Pts',(13.2658135529616,69.3258709977416,12.));
#161492=CARTESIAN_POINT('Ctrl Pts',(13.2754892884437,69.3445234885088,12.));
#161493=CARTESIAN_POINT('Ctrl Pts',(13.2852074919767,69.3632101660072,12.));
#161494=CARTESIAN_POINT('Ctrl Pts',(13.2949681583164,69.3819308490408,12.));
#161495=CARTESIAN_POINT('Ctrl Pts',(13.3047712821046,69.4006853569485,12.));
#161496=CARTESIAN_POINT('Ctrl Pts',(13.3146168578738,69.4194735096238,12.));
#161497=CARTESIAN_POINT('Ctrl Pts',(13.3245048800641,69.4382951276983,12.));
#161498=CARTESIAN_POINT('Ctrl Pts',(13.3344353430313,69.4571500326673,12.));
#161499=CARTESIAN_POINT('Ctrl Pts',(13.3444082410546,69.4760380470382,12.));
#161500=CARTESIAN_POINT('Ctrl Pts',(13.3544235683399,69.4949589944633,12.));
#161501=CARTESIAN_POINT('Ctrl Pts',(13.3644813190225,69.5139126996703,12.));
#161502=CARTESIAN_POINT('Ctrl Pts',(13.3745814871667,69.5328989883899,12.));
#161503=CARTESIAN_POINT('Ctrl Pts',(13.3847240667626,69.5519176872857,12.));
#161504=CARTESIAN_POINT('Ctrl Pts',(13.3949090517173,69.5709686238701,12.));
#161505=CARTESIAN_POINT('Ctrl Pts',(13.4051364358494,69.5900516264524,12.));
#161506=CARTESIAN_POINT('Ctrl Pts',(13.4154062128998,69.6091665241743,12.));
#161507=CARTESIAN_POINT('Ctrl Pts',(13.425718376534,69.6283131470267,12.));
#161508=CARTESIAN_POINT('Ctrl Pts',(13.4360729203444,69.6474913258684,12.));
#161509=CARTESIAN_POINT('Ctrl Pts',(13.4464698378456,69.6667008924454,12.));
#161510=CARTESIAN_POINT('Ctrl Pts',(13.4569091224762,69.6859416793898,12.));
#161511=CARTESIAN_POINT('Ctrl Pts',(13.4673907676045,69.7052135202003,12.));
#161512=CARTESIAN_POINT('Ctrl Pts',(13.4779147665285,69.7245162492251,12.));
#161513=CARTESIAN_POINT('Ctrl Pts',(13.4884811124748,69.7438497016404,12.));
#161514=CARTESIAN_POINT('Ctrl Pts',(13.4990897985904,69.7632137134247,12.));
#161515=CARTESIAN_POINT('Ctrl Pts',(13.5097408179478,69.7826081213575,12.));
#161516=CARTESIAN_POINT('Ctrl Pts',(13.5204341635507,69.8020327630204,12.));
#161517=CARTESIAN_POINT('Ctrl Pts',(13.5311698283339,69.8214874767944,12.));
#161518=CARTESIAN_POINT('Ctrl Pts',(13.5419478051626,69.840972101856,12.));
#161519=CARTESIAN_POINT('Ctrl Pts',(13.5527680868256,69.8604864781705,12.));
#161520=CARTESIAN_POINT('Ctrl Pts',(13.5636306660422,69.880030446488,12.));
#161521=CARTESIAN_POINT('Ctrl Pts',(13.5745355354657,69.899603848336,12.));
#161522=CARTESIAN_POINT('Ctrl Pts',(13.5854826876834,69.9192065260107,12.));
#161523=CARTESIAN_POINT('Ctrl Pts',(13.5964721152136,69.9388383225655,12.));
#161524=CARTESIAN_POINT('Ctrl Pts',(13.6075038105,69.9584990817989,12.));
#161525=CARTESIAN_POINT('Ctrl Pts',(13.61857776592,69.9781886482543,12.));
#161526=CARTESIAN_POINT('Ctrl Pts',(13.6296939737866,69.9979068672163,12.));
#161527=CARTESIAN_POINT('Ctrl Pts',(13.6408524263496,70.0176535847047,12.));
#161528=CARTESIAN_POINT('Ctrl Pts',(13.6520531157904,70.037428647466,12.));
#161529=CARTESIAN_POINT('Ctrl Pts',(13.6632960342192,70.057231902965,12.));
#161530=CARTESIAN_POINT('Ctrl Pts',(13.6745811736825,70.0770631993831,12.));
#161531=CARTESIAN_POINT('Ctrl Pts',(13.685908526165,70.0969223856123,12.));
#161532=CARTESIAN_POINT('Ctrl Pts',(13.6972780835898,70.1168093112493,12.));
#161533=CARTESIAN_POINT('Ctrl Pts',(13.7086898378127,70.1367238265853,12.));
#161534=CARTESIAN_POINT('Ctrl Pts',(13.7201437806207,70.1566657825989,12.));
#161535=CARTESIAN_POINT('Ctrl Pts',(13.73163990374,70.1766350309554,12.));
#161536=CARTESIAN_POINT('Ctrl Pts',(13.7431781988368,70.1966314240012,12.));
#161537=CARTESIAN_POINT('Ctrl Pts',(13.7547586575178,70.216654814759,12.));
#161538=CARTESIAN_POINT('Ctrl Pts',(13.7663812713235,70.2367050569174,12.));
#161539=CARTESIAN_POINT('Ctrl Pts',(13.7780460317284,70.2567820048253,12.));
#161540=CARTESIAN_POINT('Ctrl Pts',(13.7897529301483,70.2768855134909,12.));
#161541=CARTESIAN_POINT('Ctrl Pts',(13.8015019579411,70.2970154385763,12.));
#161542=CARTESIAN_POINT('Ctrl Pts',(13.8132931064067,70.3171716363912,12.));
#161543=CARTESIAN_POINT('Ctrl Pts',(13.8251263667799,70.3373539638841,12.));
#161544=CARTESIAN_POINT('Ctrl Pts',(13.8370017302319,70.3575622786373,12.));
#161545=CARTESIAN_POINT('Ctrl Pts',(13.8489191878774,70.377796438866,12.));
#161546=CARTESIAN_POINT('Ctrl Pts',(13.8608787307754,70.3980563034142,12.));
#161547=CARTESIAN_POINT('Ctrl Pts',(13.8728803499284,70.4183417317486,12.));
#161548=CARTESIAN_POINT('Ctrl Pts',(13.8849240362757,70.4386525839492,12.));
#161549=CARTESIAN_POINT('Ctrl Pts',(13.8970097806947,70.4589887207043,12.));
#161550=CARTESIAN_POINT('Ctrl Pts',(13.9091375740084,70.4793500033106,12.));
#161551=CARTESIAN_POINT('Ctrl Pts',(13.9213074069852,70.4997362936671,12.));
#161552=CARTESIAN_POINT('Ctrl Pts',(13.9335192703389,70.5201474542717,12.));
#161553=CARTESIAN_POINT('Ctrl Pts',(13.9457731547217,70.5405833482123,12.));
#161554=CARTESIAN_POINT('Ctrl Pts',(13.9580690507262,70.5610438391622,12.));
#161555=CARTESIAN_POINT('Ctrl Pts',(13.9704069488918,70.5815287913791,12.));
#161556=CARTESIAN_POINT('Ctrl Pts',(13.9827868397057,70.6020380697004,12.));
#161557=CARTESIAN_POINT('Ctrl Pts',(13.9952087136018,70.6225715395392,12.));
#161558=CARTESIAN_POINT('Ctrl Pts',(14.0076725609537,70.6431290668744,12.));
#161559=CARTESIAN_POINT('Ctrl Pts',(14.020178372077,70.6637105182487,12.));
#161560=CARTESIAN_POINT('Ctrl Pts',(14.0327261372363,70.6843157607672,12.));
#161561=CARTESIAN_POINT('Ctrl Pts',(14.0453158466451,70.7049446620931,12.));
#161562=CARTESIAN_POINT('Ctrl Pts',(14.0579474904657,70.7255970904433,12.));
#161563=CARTESIAN_POINT('Ctrl Pts',(14.0706210588015,70.7462729145799,12.));
#161564=CARTESIAN_POINT('Ctrl Pts',(14.0833365416995,70.7669720038067,12.));
#161565=CARTESIAN_POINT('Ctrl Pts',(14.0960939291568,70.787694227969,12.));
#161566=CARTESIAN_POINT('Ctrl Pts',(14.1088932111214,70.8084394574491,12.));
#161567=CARTESIAN_POINT('Ctrl Pts',(14.1217343774914,70.8292075631624,12.));
#161568=CARTESIAN_POINT('Ctrl Pts',(14.1346174181079,70.8499984165493,12.));
#161569=CARTESIAN_POINT('Ctrl Pts',(14.1475423227567,70.8708118895718,12.));
#161570=CARTESIAN_POINT('Ctrl Pts',(14.1605090811754,70.8916478547131,12.));
#161571=CARTESIAN_POINT('Ctrl Pts',(14.1735176830533,70.9125061849744,12.));
#161572=CARTESIAN_POINT('Ctrl Pts',(14.1865681180321,70.9333867538705,12.));
#161573=CARTESIAN_POINT('Ctrl Pts',(14.1996603756984,70.9542894354221,12.));
#161574=CARTESIAN_POINT('Ctrl Pts',(14.2127944455841,70.9752141041527,12.));
#161575=CARTESIAN_POINT('Ctrl Pts',(14.2259703171739,70.996160635087,12.));
#161576=CARTESIAN_POINT('Ctrl Pts',(14.2391879799063,71.0171289037493,12.));
#161577=CARTESIAN_POINT('Ctrl Pts',(14.2524474231732,71.0381187861585,12.));
#161578=CARTESIAN_POINT('Ctrl Pts',(14.2657486363136,71.059130158822,12.));
#161579=CARTESIAN_POINT('Ctrl Pts',(14.2790916086129,71.0801628987314,12.));
#161580=CARTESIAN_POINT('Ctrl Pts',(14.2924763293101,71.1012168833626,12.));
#161581=CARTESIAN_POINT('Ctrl Pts',(14.3059027875993,71.1222919906719,12.));
#161582=CARTESIAN_POINT('Ctrl Pts',(14.3193709726295,71.1433880990932,12.));
#161583=CARTESIAN_POINT('Ctrl Pts',(14.3328808734993,71.1645050875323,12.));
#161584=CARTESIAN_POINT('Ctrl Pts',(14.3464324792537,71.185642835361,12.));
#161585=CARTESIAN_POINT('Ctrl Pts',(14.3600257788927,71.2068012224187,12.));
#161586=CARTESIAN_POINT('Ctrl Pts',(14.3736607613723,71.2279801290088,12.));
#161587=CARTESIAN_POINT('Ctrl Pts',(14.3873374156056,71.2491794358956,12.));
#161588=CARTESIAN_POINT('Ctrl Pts',(14.401055730457,71.2703990242986,12.));
#161589=CARTESIAN_POINT('Ctrl Pts',(14.4148156947384,71.2916387758864,12.));
#161590=CARTESIAN_POINT('Ctrl Pts',(14.4286172972168,71.3128985727777,12.));
#161591=CARTESIAN_POINT('Ctrl Pts',(14.4424605266166,71.3341782975393,12.));
#161592=CARTESIAN_POINT('Ctrl Pts',(14.4563453716204,71.3554778331835,12.));
#161593=CARTESIAN_POINT('Ctrl Pts',(14.470271820865,71.3767970631642,12.));
#161594=CARTESIAN_POINT('Ctrl Pts',(14.4842398629353,71.398135871371,12.));
#161595=CARTESIAN_POINT('Ctrl Pts',(14.4982494863716,71.4194941421279,12.));
#161596=CARTESIAN_POINT('Ctrl Pts',(14.5123006796728,71.4408717601917,12.));
#161597=CARTESIAN_POINT('Ctrl Pts',(14.5263934312969,71.4622686107475,12.));
#161598=CARTESIAN_POINT('Ctrl Pts',(14.540527729659,71.4836845794052,12.));
#161599=CARTESIAN_POINT('Ctrl Pts',(14.5547035631234,71.5051195521914,12.));
#161600=CARTESIAN_POINT('Ctrl Pts',(14.568920920009,71.5265734155501,12.));
#161601=CARTESIAN_POINT('Ctrl Pts',(14.5831797885951,71.5480460563445,12.));
#161602=CARTESIAN_POINT('Ctrl Pts',(14.597480157121,71.569537361856,12.));
#161603=CARTESIAN_POINT('Ctrl Pts',(14.611822013785,71.5910472197815,12.));
#161604=CARTESIAN_POINT('Ctrl Pts',(14.6262053467372,71.6125755182295,12.));
#161605=CARTESIAN_POINT('Ctrl Pts',(14.6406301440817,71.6341221457175,12.));
#161606=CARTESIAN_POINT('Ctrl Pts',(14.6550963938832,71.6556869911669,12.));
#161607=CARTESIAN_POINT('Ctrl Pts',(14.6696040841679,71.6772699438966,12.));
#161608=CARTESIAN_POINT('Ctrl Pts',(14.6841532029231,71.698870893617,12.));
#161609=CARTESIAN_POINT('Ctrl Pts',(14.6987437380898,71.7204897304186,12.));
#161610=CARTESIAN_POINT('Ctrl Pts',(14.7133756775622,71.7421263447707,12.));
#161611=CARTESIAN_POINT('Ctrl Pts',(14.7280490091954,71.7637806275316,12.));
#161612=CARTESIAN_POINT('Ctrl Pts',(14.7427637208071,71.7854524699563,12.));
#161613=CARTESIAN_POINT('Ctrl Pts',(14.7575198001776,71.8071417637019,12.));
#161614=CARTESIAN_POINT('Ctrl Pts',(14.7723172350454,71.8288484008343,12.));
#161615=CARTESIAN_POINT('Ctrl Pts',(14.7871560131021,71.8505722738286,12.));
#161616=CARTESIAN_POINT('Ctrl Pts',(14.8020361220003,71.872313275546,12.));
#161617=CARTESIAN_POINT('Ctrl Pts',(14.816957549356,71.8940712992119,12.));
#161618=CARTESIAN_POINT('Ctrl Pts',(14.8319202827482,71.9158462383915,12.));
#161619=CARTESIAN_POINT('Ctrl Pts',(14.846924309716,71.9376379869668,12.));
#161620=CARTESIAN_POINT('Ctrl Pts',(14.8619696177503,71.9594464391063,12.));
#161621=CARTESIAN_POINT('Ctrl Pts',(14.8770561943011,71.9812714893087,12.));
#161622=CARTESIAN_POINT('Ctrl Pts',(14.892184026783,72.0031130324519,12.));
#161623=CARTESIAN_POINT('Ctrl Pts',(14.9073531025763,72.0249709638419,12.));
#161624=CARTESIAN_POINT('Ctrl Pts',(14.9225634090269,72.046845179251,12.));
#161625=CARTESIAN_POINT('Ctrl Pts',(14.937814933439,72.0687355749815,12.));
#161626=CARTESIAN_POINT('Ctrl Pts',(14.953107663077,72.0906420478085,12.));
#161627=CARTESIAN_POINT('Ctrl Pts',(14.9684415851699,72.1125644948547,12.));
#161628=CARTESIAN_POINT('Ctrl Pts',(14.9838166869107,72.1345028134779,12.));
#161629=CARTESIAN_POINT('Ctrl Pts',(14.9992329554537,72.1564569011668,12.));
#161630=CARTESIAN_POINT('Ctrl Pts',(15.0146903779061,72.1784266553948,12.));
#161631=CARTESIAN_POINT('Ctrl Pts',(15.0301889413255,72.2004119736104,12.));
#161632=CARTESIAN_POINT('Ctrl Pts',(15.0457286327328,72.2224127535401,12.));
#161633=CARTESIAN_POINT('Ctrl Pts',(15.0613094391186,72.244428893425,12.));
#161634=CARTESIAN_POINT('Ctrl Pts',(15.0769313474476,72.266460292285,12.));
#161635=CARTESIAN_POINT('Ctrl Pts',(15.0925943446593,72.2885068501641,12.));
#161636=CARTESIAN_POINT('Ctrl Pts',(15.1082984176655,72.3105684683971,12.));
#161637=CARTESIAN_POINT('Ctrl Pts',(15.1240435533478,72.332645049021,12.));
#161638=CARTESIAN_POINT('Ctrl Pts',(15.1398297385513,72.3547364941996,12.));
#161639=CARTESIAN_POINT('Ctrl Pts',(15.1556569600747,72.37684270559,12.));
#161640=CARTESIAN_POINT('Ctrl Pts',(15.1715252046602,72.3989635838476,12.));
#161641=CARTESIAN_POINT('Ctrl Pts',(15.1874344589716,72.4210990277819,12.));
#161642=CARTESIAN_POINT('Ctrl Pts',(15.2033847096077,72.4432489350415,12.));
#161643=CARTESIAN_POINT('Ctrl Pts',(15.2193759431359,72.4654132036373,12.));
#161644=CARTESIAN_POINT('Ctrl Pts',(15.2354081461152,72.4875917332729,12.));
#161645=CARTESIAN_POINT('Ctrl Pts',(15.2514813051174,72.5097844266083,12.));
#161646=CARTESIAN_POINT('Ctrl Pts',(15.2675954067495,72.5319911908978,12.));
#161647=CARTESIAN_POINT('Ctrl Pts',(15.2837504376562,72.5542119383748,12.));
#161648=CARTESIAN_POINT('Ctrl Pts',(15.2976335024853,72.5732713370797,12.));
#161649=CARTESIAN_POINT('Ctrl Pts',(15.3082994603653,72.5878912620665,12.));
#161650=CARTESIAN_POINT('Ctrl Pts',(15.3157301930835,72.5980655789901,12.));
#161651=CARTESIAN_POINT('Ctrl Pts',(15.3199137230322,72.6037902605231,12.));
#161652=CARTESIAN_POINT('Ctrl Pts',(15.3208442077425,72.6050633494718,12.));
#161653=CARTESIAN_POINT('',(12.9953224629497,68.7831490561748,0.));
#161654=CARTESIAN_POINT('',(12.9953224629497,68.7831490561748,0.));
#161655=CARTESIAN_POINT('Ctrl Pts',(15.3208442077425,72.6050633494718,0.));
#161656=CARTESIAN_POINT('Ctrl Pts',(15.3199137230322,72.6037902605231,0.));
#161657=CARTESIAN_POINT('Ctrl Pts',(15.3157301930835,72.5980655789901,0.));
#161658=CARTESIAN_POINT('Ctrl Pts',(15.3082994603653,72.5878912620665,0.));
#161659=CARTESIAN_POINT('Ctrl Pts',(15.2976335024853,72.5732713370797,0.));
#161660=CARTESIAN_POINT('Ctrl Pts',(15.2837504376562,72.5542119383748,0.));
#161661=CARTESIAN_POINT('Ctrl Pts',(15.2675954067495,72.5319911908978,0.));
#161662=CARTESIAN_POINT('Ctrl Pts',(15.2514813051174,72.5097844266083,0.));
#161663=CARTESIAN_POINT('Ctrl Pts',(15.2354081461152,72.4875917332729,0.));
#161664=CARTESIAN_POINT('Ctrl Pts',(15.2193759431359,72.4654132036373,0.));
#161665=CARTESIAN_POINT('Ctrl Pts',(15.2033847096077,72.4432489350415,0.));
#161666=CARTESIAN_POINT('Ctrl Pts',(15.1874344589716,72.4210990277819,0.));
#161667=CARTESIAN_POINT('Ctrl Pts',(15.1715252046602,72.3989635838476,0.));
#161668=CARTESIAN_POINT('Ctrl Pts',(15.1556569600747,72.37684270559,0.));
#161669=CARTESIAN_POINT('Ctrl Pts',(15.1398297385513,72.3547364941996,0.));
#161670=CARTESIAN_POINT('Ctrl Pts',(15.1240435533478,72.332645049021,0.));
#161671=CARTESIAN_POINT('Ctrl Pts',(15.1082984176655,72.3105684683971,0.));
#161672=CARTESIAN_POINT('Ctrl Pts',(15.0925943446593,72.2885068501641,0.));
#161673=CARTESIAN_POINT('Ctrl Pts',(15.0769313474476,72.266460292285,0.));
#161674=CARTESIAN_POINT('Ctrl Pts',(15.0613094391186,72.244428893425,0.));
#161675=CARTESIAN_POINT('Ctrl Pts',(15.0457286327328,72.2224127535401,0.));
#161676=CARTESIAN_POINT('Ctrl Pts',(15.0301889413255,72.2004119736104,0.));
#161677=CARTESIAN_POINT('Ctrl Pts',(15.0146903779061,72.1784266553948,0.));
#161678=CARTESIAN_POINT('Ctrl Pts',(14.9992329554537,72.1564569011668,0.));
#161679=CARTESIAN_POINT('Ctrl Pts',(14.9838166869107,72.1345028134779,0.));
#161680=CARTESIAN_POINT('Ctrl Pts',(14.9684415851699,72.1125644948547,0.));
#161681=CARTESIAN_POINT('Ctrl Pts',(14.953107663077,72.0906420478085,0.));
#161682=CARTESIAN_POINT('Ctrl Pts',(14.937814933439,72.0687355749815,0.));
#161683=CARTESIAN_POINT('Ctrl Pts',(14.9225634090269,72.046845179251,0.));
#161684=CARTESIAN_POINT('Ctrl Pts',(14.9073531025763,72.0249709638419,0.));
#161685=CARTESIAN_POINT('Ctrl Pts',(14.892184026783,72.0031130324519,0.));
#161686=CARTESIAN_POINT('Ctrl Pts',(14.8770561943011,71.9812714893087,0.));
#161687=CARTESIAN_POINT('Ctrl Pts',(14.8619696177503,71.9594464391063,0.));
#161688=CARTESIAN_POINT('Ctrl Pts',(14.846924309716,71.9376379869668,0.));
#161689=CARTESIAN_POINT('Ctrl Pts',(14.8319202827482,71.9158462383915,0.));
#161690=CARTESIAN_POINT('Ctrl Pts',(14.816957549356,71.8940712992119,0.));
#161691=CARTESIAN_POINT('Ctrl Pts',(14.8020361220003,71.872313275546,0.));
#161692=CARTESIAN_POINT('Ctrl Pts',(14.7871560131021,71.8505722738286,0.));
#161693=CARTESIAN_POINT('Ctrl Pts',(14.7723172350454,71.8288484008343,0.));
#161694=CARTESIAN_POINT('Ctrl Pts',(14.7575198001776,71.8071417637019,0.));
#161695=CARTESIAN_POINT('Ctrl Pts',(14.7427637208071,71.7854524699563,0.));
#161696=CARTESIAN_POINT('Ctrl Pts',(14.7280490091954,71.7637806275316,0.));
#161697=CARTESIAN_POINT('Ctrl Pts',(14.7133756775622,71.7421263447707,0.));
#161698=CARTESIAN_POINT('Ctrl Pts',(14.6987437380898,71.7204897304186,0.));
#161699=CARTESIAN_POINT('Ctrl Pts',(14.6841532029231,71.698870893617,0.));
#161700=CARTESIAN_POINT('Ctrl Pts',(14.6696040841679,71.6772699438966,0.));
#161701=CARTESIAN_POINT('Ctrl Pts',(14.6550963938832,71.6556869911669,0.));
#161702=CARTESIAN_POINT('Ctrl Pts',(14.6406301440817,71.6341221457175,0.));
#161703=CARTESIAN_POINT('Ctrl Pts',(14.6262053467372,71.6125755182295,0.));
#161704=CARTESIAN_POINT('Ctrl Pts',(14.611822013785,71.5910472197815,0.));
#161705=CARTESIAN_POINT('Ctrl Pts',(14.597480157121,71.569537361856,0.));
#161706=CARTESIAN_POINT('Ctrl Pts',(14.5831797885951,71.5480460563445,0.));
#161707=CARTESIAN_POINT('Ctrl Pts',(14.568920920009,71.5265734155501,0.));
#161708=CARTESIAN_POINT('Ctrl Pts',(14.5547035631234,71.5051195521914,0.));
#161709=CARTESIAN_POINT('Ctrl Pts',(14.540527729659,71.4836845794052,0.));
#161710=CARTESIAN_POINT('Ctrl Pts',(14.5263934312969,71.4622686107475,0.));
#161711=CARTESIAN_POINT('Ctrl Pts',(14.5123006796728,71.4408717601917,0.));
#161712=CARTESIAN_POINT('Ctrl Pts',(14.4982494863716,71.4194941421279,0.));
#161713=CARTESIAN_POINT('Ctrl Pts',(14.4842398629353,71.398135871371,0.));
#161714=CARTESIAN_POINT('Ctrl Pts',(14.470271820865,71.3767970631642,0.));
#161715=CARTESIAN_POINT('Ctrl Pts',(14.4563453716204,71.3554778331835,0.));
#161716=CARTESIAN_POINT('Ctrl Pts',(14.4424605266166,71.3341782975393,0.));
#161717=CARTESIAN_POINT('Ctrl Pts',(14.4286172972168,71.3128985727777,0.));
#161718=CARTESIAN_POINT('Ctrl Pts',(14.4148156947384,71.2916387758864,0.));
#161719=CARTESIAN_POINT('Ctrl Pts',(14.401055730457,71.2703990242986,0.));
#161720=CARTESIAN_POINT('Ctrl Pts',(14.3873374156056,71.2491794358956,0.));
#161721=CARTESIAN_POINT('Ctrl Pts',(14.3736607613723,71.2279801290088,0.));
#161722=CARTESIAN_POINT('Ctrl Pts',(14.3600257788927,71.2068012224187,0.));
#161723=CARTESIAN_POINT('Ctrl Pts',(14.3464324792537,71.185642835361,0.));
#161724=CARTESIAN_POINT('Ctrl Pts',(14.3328808734993,71.1645050875323,0.));
#161725=CARTESIAN_POINT('Ctrl Pts',(14.3193709726295,71.1433880990932,0.));
#161726=CARTESIAN_POINT('Ctrl Pts',(14.3059027875993,71.1222919906719,0.));
#161727=CARTESIAN_POINT('Ctrl Pts',(14.2924763293101,71.1012168833626,0.));
#161728=CARTESIAN_POINT('Ctrl Pts',(14.2790916086129,71.0801628987314,0.));
#161729=CARTESIAN_POINT('Ctrl Pts',(14.2657486363136,71.059130158822,0.));
#161730=CARTESIAN_POINT('Ctrl Pts',(14.2524474231732,71.0381187861585,0.));
#161731=CARTESIAN_POINT('Ctrl Pts',(14.2391879799063,71.0171289037493,0.));
#161732=CARTESIAN_POINT('Ctrl Pts',(14.2259703171739,70.996160635087,0.));
#161733=CARTESIAN_POINT('Ctrl Pts',(14.2127944455841,70.9752141041527,0.));
#161734=CARTESIAN_POINT('Ctrl Pts',(14.1996603756984,70.9542894354221,0.));
#161735=CARTESIAN_POINT('Ctrl Pts',(14.1865681180321,70.9333867538705,0.));
#161736=CARTESIAN_POINT('Ctrl Pts',(14.1735176830533,70.9125061849744,0.));
#161737=CARTESIAN_POINT('Ctrl Pts',(14.1605090811754,70.8916478547131,0.));
#161738=CARTESIAN_POINT('Ctrl Pts',(14.1475423227567,70.8708118895718,0.));
#161739=CARTESIAN_POINT('Ctrl Pts',(14.1346174181079,70.8499984165493,0.));
#161740=CARTESIAN_POINT('Ctrl Pts',(14.1217343774914,70.8292075631624,0.));
#161741=CARTESIAN_POINT('Ctrl Pts',(14.1088932111214,70.8084394574491,0.));
#161742=CARTESIAN_POINT('Ctrl Pts',(14.0960939291568,70.787694227969,0.));
#161743=CARTESIAN_POINT('Ctrl Pts',(14.0833365416995,70.7669720038067,0.));
#161744=CARTESIAN_POINT('Ctrl Pts',(14.0706210588015,70.7462729145799,0.));
#161745=CARTESIAN_POINT('Ctrl Pts',(14.0579474904657,70.7255970904433,0.));
#161746=CARTESIAN_POINT('Ctrl Pts',(14.0453158466451,70.7049446620931,0.));
#161747=CARTESIAN_POINT('Ctrl Pts',(14.0327261372363,70.6843157607672,0.));
#161748=CARTESIAN_POINT('Ctrl Pts',(14.020178372077,70.6637105182487,0.));
#161749=CARTESIAN_POINT('Ctrl Pts',(14.0076725609537,70.6431290668744,0.));
#161750=CARTESIAN_POINT('Ctrl Pts',(13.9952087136018,70.6225715395392,0.));
#161751=CARTESIAN_POINT('Ctrl Pts',(13.9827868397057,70.6020380697004,0.));
#161752=CARTESIAN_POINT('Ctrl Pts',(13.9704069488918,70.5815287913791,0.));
#161753=CARTESIAN_POINT('Ctrl Pts',(13.9580690507262,70.5610438391622,0.));
#161754=CARTESIAN_POINT('Ctrl Pts',(13.9457731547217,70.5405833482123,0.));
#161755=CARTESIAN_POINT('Ctrl Pts',(13.9335192703389,70.5201474542717,0.));
#161756=CARTESIAN_POINT('Ctrl Pts',(13.9213074069852,70.4997362936671,0.));
#161757=CARTESIAN_POINT('Ctrl Pts',(13.9091375740084,70.4793500033106,0.));
#161758=CARTESIAN_POINT('Ctrl Pts',(13.8970097806947,70.4589887207043,0.));
#161759=CARTESIAN_POINT('Ctrl Pts',(13.8849240362757,70.4386525839492,0.));
#161760=CARTESIAN_POINT('Ctrl Pts',(13.8728803499284,70.4183417317486,0.));
#161761=CARTESIAN_POINT('Ctrl Pts',(13.8608787307754,70.3980563034142,0.));
#161762=CARTESIAN_POINT('Ctrl Pts',(13.8489191878774,70.377796438866,0.));
#161763=CARTESIAN_POINT('Ctrl Pts',(13.8370017302319,70.3575622786373,0.));
#161764=CARTESIAN_POINT('Ctrl Pts',(13.8251263667799,70.3373539638841,0.));
#161765=CARTESIAN_POINT('Ctrl Pts',(13.8132931064067,70.3171716363912,0.));
#161766=CARTESIAN_POINT('Ctrl Pts',(13.8015019579411,70.2970154385763,0.));
#161767=CARTESIAN_POINT('Ctrl Pts',(13.7897529301483,70.2768855134909,0.));
#161768=CARTESIAN_POINT('Ctrl Pts',(13.7780460317284,70.2567820048253,0.));
#161769=CARTESIAN_POINT('Ctrl Pts',(13.7663812713235,70.2367050569174,0.));
#161770=CARTESIAN_POINT('Ctrl Pts',(13.7547586575178,70.216654814759,0.));
#161771=CARTESIAN_POINT('Ctrl Pts',(13.7431781988368,70.1966314240012,0.));
#161772=CARTESIAN_POINT('Ctrl Pts',(13.73163990374,70.1766350309554,0.));
#161773=CARTESIAN_POINT('Ctrl Pts',(13.7201437806207,70.1566657825989,0.));
#161774=CARTESIAN_POINT('Ctrl Pts',(13.7086898378127,70.1367238265853,0.));
#161775=CARTESIAN_POINT('Ctrl Pts',(13.6972780835898,70.1168093112493,0.));
#161776=CARTESIAN_POINT('Ctrl Pts',(13.685908526165,70.0969223856123,0.));
#161777=CARTESIAN_POINT('Ctrl Pts',(13.6745811736825,70.0770631993831,0.));
#161778=CARTESIAN_POINT('Ctrl Pts',(13.6632960342192,70.057231902965,0.));
#161779=CARTESIAN_POINT('Ctrl Pts',(13.6520531157904,70.037428647466,0.));
#161780=CARTESIAN_POINT('Ctrl Pts',(13.6408524263496,70.0176535847047,0.));
#161781=CARTESIAN_POINT('Ctrl Pts',(13.6296939737866,69.9979068672163,0.));
#161782=CARTESIAN_POINT('Ctrl Pts',(13.61857776592,69.9781886482543,0.));
#161783=CARTESIAN_POINT('Ctrl Pts',(13.6075038105,69.9584990817989,0.));
#161784=CARTESIAN_POINT('Ctrl Pts',(13.5964721152136,69.9388383225655,0.));
#161785=CARTESIAN_POINT('Ctrl Pts',(13.5854826876834,69.9192065260107,0.));
#161786=CARTESIAN_POINT('Ctrl Pts',(13.5745355354657,69.899603848336,0.));
#161787=CARTESIAN_POINT('Ctrl Pts',(13.5636306660422,69.880030446488,0.));
#161788=CARTESIAN_POINT('Ctrl Pts',(13.5527680868256,69.8604864781705,0.));
#161789=CARTESIAN_POINT('Ctrl Pts',(13.5419478051626,69.840972101856,0.));
#161790=CARTESIAN_POINT('Ctrl Pts',(13.5311698283339,69.8214874767944,0.));
#161791=CARTESIAN_POINT('Ctrl Pts',(13.5204341635507,69.8020327630204,0.));
#161792=CARTESIAN_POINT('Ctrl Pts',(13.5097408179478,69.7826081213575,0.));
#161793=CARTESIAN_POINT('Ctrl Pts',(13.4990897985904,69.7632137134247,0.));
#161794=CARTESIAN_POINT('Ctrl Pts',(13.4884811124748,69.7438497016404,0.));
#161795=CARTESIAN_POINT('Ctrl Pts',(13.4779147665285,69.7245162492251,0.));
#161796=CARTESIAN_POINT('Ctrl Pts',(13.4673907676045,69.7052135202003,0.));
#161797=CARTESIAN_POINT('Ctrl Pts',(13.4569091224762,69.6859416793898,0.));
#161798=CARTESIAN_POINT('Ctrl Pts',(13.4464698378456,69.6667008924454,0.));
#161799=CARTESIAN_POINT('Ctrl Pts',(13.4360729203444,69.6474913258684,0.));
#161800=CARTESIAN_POINT('Ctrl Pts',(13.425718376534,69.6283131470267,0.));
#161801=CARTESIAN_POINT('Ctrl Pts',(13.4154062128998,69.6091665241743,0.));
#161802=CARTESIAN_POINT('Ctrl Pts',(13.4051364358494,69.5900516264524,0.));
#161803=CARTESIAN_POINT('Ctrl Pts',(13.3949090517173,69.5709686238701,0.));
#161804=CARTESIAN_POINT('Ctrl Pts',(13.3847240667626,69.5519176872857,0.));
#161805=CARTESIAN_POINT('Ctrl Pts',(13.3745814871667,69.5328989883899,0.));
#161806=CARTESIAN_POINT('Ctrl Pts',(13.3644813190225,69.5139126996703,0.));
#161807=CARTESIAN_POINT('Ctrl Pts',(13.3544235683399,69.4949589944633,0.));
#161808=CARTESIAN_POINT('Ctrl Pts',(13.3444082410546,69.4760380470382,0.));
#161809=CARTESIAN_POINT('Ctrl Pts',(13.3344353430313,69.4571500326673,0.));
#161810=CARTESIAN_POINT('Ctrl Pts',(13.3245048800641,69.4382951276983,0.));
#161811=CARTESIAN_POINT('Ctrl Pts',(13.3146168578738,69.4194735096238,0.));
#161812=CARTESIAN_POINT('Ctrl Pts',(13.3047712821046,69.4006853569485,0.));
#161813=CARTESIAN_POINT('Ctrl Pts',(13.2949681583164,69.3819308490408,0.));
#161814=CARTESIAN_POINT('Ctrl Pts',(13.2852074919767,69.3632101660072,0.));
#161815=CARTESIAN_POINT('Ctrl Pts',(13.2754892884437,69.3445234885088,0.));
#161816=CARTESIAN_POINT('Ctrl Pts',(13.2658135529616,69.3258709977416,0.));
#161817=CARTESIAN_POINT('Ctrl Pts',(13.2561802906901,69.3072528758546,0.));
#161818=CARTESIAN_POINT('Ctrl Pts',(13.2465895067264,69.2886693063193,0.));
#161819=CARTESIAN_POINT('Ctrl Pts',(13.2370412061218,69.2701204742436,0.));
#161820=CARTESIAN_POINT('Ctrl Pts',(13.2275353939044,69.2516065668809,0.));
#161821=CARTESIAN_POINT('Ctrl Pts',(13.2180720750586,69.2331277732819,0.));
#161822=CARTESIAN_POINT('Ctrl Pts',(13.2086512544729,69.2146842833506,0.));
#161823=CARTESIAN_POINT('Ctrl Pts',(13.1992729368928,69.1962762870524,0.));
#161824=CARTESIAN_POINT('Ctrl Pts',(13.1899371268689,69.1779039736026,0.));
#161825=CARTESIAN_POINT('Ctrl Pts',(13.1806438286944,69.1595675305294,0.));
#161826=CARTESIAN_POINT('Ctrl Pts',(13.1713930465142,69.141267145461,0.));
#161827=CARTESIAN_POINT('Ctrl Pts',(13.1621847844533,69.1230030082598,0.));
#161828=CARTESIAN_POINT('Ctrl Pts',(13.1530190467181,69.1047753127633,0.));
#161829=CARTESIAN_POINT('Ctrl Pts',(13.1438958377397,69.0865842593063,0.));
#161830=CARTESIAN_POINT('Ctrl Pts',(13.1348151621824,69.0684300549426,0.));
#161831=CARTESIAN_POINT('Ctrl Pts',(13.1257770246379,69.0503129081778,0.));
#161832=CARTESIAN_POINT('Ctrl Pts',(13.1167814293495,69.0322330243336,0.));
#161833=CARTESIAN_POINT('Ctrl Pts',(13.1078283799726,69.0141906015137,0.));
#161834=CARTESIAN_POINT('Ctrl Pts',(13.0989178791843,68.9961858241577,0.));
#161835=CARTESIAN_POINT('Ctrl Pts',(13.0900499290542,68.9782188692654,0.));
#161836=CARTESIAN_POINT('Ctrl Pts',(13.0812245317816,68.9602899187628,0.));
#161837=CARTESIAN_POINT('Ctrl Pts',(13.072441690283,68.9423991694493,0.));
#161838=CARTESIAN_POINT('Ctrl Pts',(13.0637014089018,68.9245468449865,0.));
#161839=CARTESIAN_POINT('Ctrl Pts',(13.0550036938793,68.9067332040842,0.));
#161840=CARTESIAN_POINT('Ctrl Pts',(13.0463485518185,68.8889585151431,0.));
#161841=CARTESIAN_POINT('Ctrl Pts',(13.0377359881864,68.8712230321823,0.));
#161842=CARTESIAN_POINT('Ctrl Pts',(13.0291660060118,68.8535269726871,0.));
#161843=CARTESIAN_POINT('Ctrl Pts',(13.0206386039729,68.835870488774,0.));
#161844=CARTESIAN_POINT('Ctrl Pts',(13.0121537769003,68.8182536654067,0.));
#161845=CARTESIAN_POINT('Ctrl Pts',(13.0053999700929,68.8041919669403,0.));
#161846=CARTESIAN_POINT('Ctrl Pts',(13.0003537683089,68.7936635625788,0.));
#161847=CARTESIAN_POINT('Ctrl Pts',(12.996998146029,68.7866525680284,0.));
#161848=CARTESIAN_POINT('Ctrl Pts',(12.9953224629497,68.7831490561748,0.));
#161849=CARTESIAN_POINT('Ctrl Pts',(21.8059378310719,71.2372871136137,0.));
#161850=CARTESIAN_POINT('Ctrl Pts',(21.8059378310719,71.2372871136137,12.));
#161851=CARTESIAN_POINT('Ctrl Pts',(21.8022104901727,71.2331134397872,0.));
#161852=CARTESIAN_POINT('Ctrl Pts',(21.8022104901727,71.2331134397872,12.));
#161853=CARTESIAN_POINT('Ctrl Pts',(21.794759979896,71.2247670210176,0.));
#161854=CARTESIAN_POINT('Ctrl Pts',(21.794759979896,71.2247670210176,12.));
#161855=CARTESIAN_POINT('Ctrl Pts',(21.7835967290463,71.2122501795138,0.));
#161856=CARTESIAN_POINT('Ctrl Pts',(21.7835967290463,71.2122501795138,12.));
#161857=CARTESIAN_POINT('Ctrl Pts',(21.7687374247287,71.1955666310295,0.));
#161858=CARTESIAN_POINT('Ctrl Pts',(21.7687374247287,71.1955666310295,12.));
#161859=CARTESIAN_POINT('Ctrl Pts',(21.750205018381,71.1747214906585,0.));
#161860=CARTESIAN_POINT('Ctrl Pts',(21.750205018381,71.1747214906585,12.));
#161861=CARTESIAN_POINT('Ctrl Pts',(21.7317143472951,71.1538856612261,0.));
#161862=CARTESIAN_POINT('Ctrl Pts',(21.7317143472951,71.1538856612261,12.));
#161863=CARTESIAN_POINT('Ctrl Pts',(21.7132654262531,71.1330591726507,0.));
#161864=CARTESIAN_POINT('Ctrl Pts',(21.7132654262531,71.1330591726507,12.));
#161865=CARTESIAN_POINT('Ctrl Pts',(21.694858273085,71.1122420728217,0.));
#161866=CARTESIAN_POINT('Ctrl Pts',(21.694858273085,71.1122420728217,12.));
#161867=CARTESIAN_POINT('Ctrl Pts',(21.6764929081677,71.0914344332798,0.));
#161868=CARTESIAN_POINT('Ctrl Pts',(21.6764929081677,71.0914344332798,12.));
#161869=CARTESIAN_POINT('Ctrl Pts',(21.6581693538335,71.0706363472704,0.));
#161870=CARTESIAN_POINT('Ctrl Pts',(21.6581693538335,71.0706363472704,12.));
#161871=CARTESIAN_POINT('Ctrl Pts',(21.639887633714,71.0498479219467,0.));
#161872=CARTESIAN_POINT('Ctrl Pts',(21.639887633714,71.0498479219467,12.));
#161873=CARTESIAN_POINT('Ctrl Pts',(21.6216477720912,71.0290692721848,0.));
#161874=CARTESIAN_POINT('Ctrl Pts',(21.6216477720912,71.0290692721848,12.));
#161875=CARTESIAN_POINT('Ctrl Pts',(21.6034497932581,71.0083005139107,0.));
#161876=CARTESIAN_POINT('Ctrl Pts',(21.6034497932581,71.0083005139107,12.));
#161877=CARTESIAN_POINT('Ctrl Pts',(21.585293720829,70.987541757223,0.));
#161878=CARTESIAN_POINT('Ctrl Pts',(21.585293720829,70.987541757223,12.));
#161879=CARTESIAN_POINT('Ctrl Pts',(21.5671795771913,70.9667931008215,0.));
#161880=CARTESIAN_POINT('Ctrl Pts',(21.5671795771913,70.9667931008215,12.));
#161881=CARTESIAN_POINT('Ctrl Pts',(21.5491073839106,70.94605463587,0.));
#161882=CARTESIAN_POINT('Ctrl Pts',(21.5491073839106,70.94605463587,12.));
#161883=CARTESIAN_POINT('Ctrl Pts',(21.531077162023,70.9253264487637,0.));
#161884=CARTESIAN_POINT('Ctrl Pts',(21.531077162023,70.9253264487637,12.));
#161885=CARTESIAN_POINT('Ctrl Pts',(21.513088932377,70.9046086244131,0.));
#161886=CARTESIAN_POINT('Ctrl Pts',(21.513088932377,70.9046086244131,12.));
#161887=CARTESIAN_POINT('Ctrl Pts',(21.4951427159261,70.8839012490871,0.));
#161888=CARTESIAN_POINT('Ctrl Pts',(21.4951427159261,70.8839012490871,12.));
#161889=CARTESIAN_POINT('Ctrl Pts',(21.477238534096,70.8632044140112,0.));
#161890=CARTESIAN_POINT('Ctrl Pts',(21.477238534096,70.8632044140112,12.));
#161891=CARTESIAN_POINT('Ctrl Pts',(21.4593764087473,70.8425182149846,0.));
#161892=CARTESIAN_POINT('Ctrl Pts',(21.4593764087473,70.8425182149846,12.));
#161893=CARTESIAN_POINT('Ctrl Pts',(21.4415563620114,70.8218427507506,0.));
#161894=CARTESIAN_POINT('Ctrl Pts',(21.4415563620114,70.8218427507506,12.));
#161895=CARTESIAN_POINT('Ctrl Pts',(21.4237784161587,70.8011781217394,0.));
#161896=CARTESIAN_POINT('Ctrl Pts',(21.4237784161587,70.8011781217394,12.));
#161897=CARTESIAN_POINT('Ctrl Pts',(21.4060425934598,70.780524428745,0.));
#161898=CARTESIAN_POINT('Ctrl Pts',(21.4060425934598,70.780524428745,12.));
#161899=CARTESIAN_POINT('Ctrl Pts',(21.3883489160196,70.7598817714105,0.));
#161900=CARTESIAN_POINT('Ctrl Pts',(21.3883489160196,70.7598817714105,12.));
#161901=CARTESIAN_POINT('Ctrl Pts',(21.3706974057039,70.7392502475469,0.));
#161902=CARTESIAN_POINT('Ctrl Pts',(21.3706974057039,70.7392502475469,12.));
#161903=CARTESIAN_POINT('Ctrl Pts',(21.3530880842349,70.7186299539724,0.));
#161904=CARTESIAN_POINT('Ctrl Pts',(21.3530880842349,70.7186299539724,12.));
#161905=CARTESIAN_POINT('Ctrl Pts',(21.3355209732443,70.6980209870045,0.));
#161906=CARTESIAN_POINT('Ctrl Pts',(21.3355209732443,70.6980209870045,12.));
#161907=CARTESIAN_POINT('Ctrl Pts',(21.3179960943388,70.6774234430897,0.));
#161908=CARTESIAN_POINT('Ctrl Pts',(21.3179960943388,70.6774234430897,12.));
#161909=CARTESIAN_POINT('Ctrl Pts',(21.300513469156,70.6568374193774,0.));
#161910=CARTESIAN_POINT('Ctrl Pts',(21.300513469156,70.6568374193774,12.));
#161911=CARTESIAN_POINT('Ctrl Pts',(21.2830731194183,70.6362630143047,0.));
#161912=CARTESIAN_POINT('Ctrl Pts',(21.2830731194183,70.6362630143047,12.));
#161913=CARTESIAN_POINT('Ctrl Pts',(21.2656750669126,70.6157003273316,0.));
#161914=CARTESIAN_POINT('Ctrl Pts',(21.2656750669126,70.6157003273316,12.));
#161915=CARTESIAN_POINT('Ctrl Pts',(21.2483193334675,70.5951494586957,0.));
#161916=CARTESIAN_POINT('Ctrl Pts',(21.2483193334675,70.5951494586957,12.));
#161917=CARTESIAN_POINT('Ctrl Pts',(21.2310059409265,70.5746105091502,0.));
#161918=CARTESIAN_POINT('Ctrl Pts',(21.2310059409265,70.5746105091502,12.));
#161919=CARTESIAN_POINT('Ctrl Pts',(21.2137349111208,70.5540835797283,0.));
#161920=CARTESIAN_POINT('Ctrl Pts',(21.2137349111208,70.5540835797283,12.));
#161921=CARTESIAN_POINT('Ctrl Pts',(21.1965062658298,70.5335687714429,0.));
#161922=CARTESIAN_POINT('Ctrl Pts',(21.1965062658298,70.5335687714429,12.));
#161923=CARTESIAN_POINT('Ctrl Pts',(21.1793200267846,70.5130661852955,0.));
#161924=CARTESIAN_POINT('Ctrl Pts',(21.1793200267846,70.5130661852955,12.));
#161925=CARTESIAN_POINT('Ctrl Pts',(21.1621762156897,70.4925759224216,0.));
#161926=CARTESIAN_POINT('Ctrl Pts',(21.1621762156897,70.4925759224216,12.));
#161927=CARTESIAN_POINT('Ctrl Pts',(21.1450748542336,70.4720980841939,0.));
#161928=CARTESIAN_POINT('Ctrl Pts',(21.1450748542336,70.4720980841939,12.));
#161929=CARTESIAN_POINT('Ctrl Pts',(21.1280159641002,70.4516327723346,0.));
#161930=CARTESIAN_POINT('Ctrl Pts',(21.1280159641002,70.4516327723346,12.));
#161931=CARTESIAN_POINT('Ctrl Pts',(21.1109995669747,70.4311800890402,0.));
#161932=CARTESIAN_POINT('Ctrl Pts',(21.1109995669747,70.4311800890402,12.));
#161933=CARTESIAN_POINT('Ctrl Pts',(21.0940256845472,70.4107401370389,0.));
#161934=CARTESIAN_POINT('Ctrl Pts',(21.0940256845472,70.4107401370389,12.));
#161935=CARTESIAN_POINT('Ctrl Pts',(21.0770943385141,70.3903130195265,0.));
#161936=CARTESIAN_POINT('Ctrl Pts',(21.0770943385141,70.3903130195265,12.));
#161937=CARTESIAN_POINT('Ctrl Pts',(21.0602055505748,70.3698988401281,0.));
#161938=CARTESIAN_POINT('Ctrl Pts',(21.0602055505748,70.3698988401281,12.));
#161939=CARTESIAN_POINT('Ctrl Pts',(21.0433593424266,70.3494977028498,0.));
#161940=CARTESIAN_POINT('Ctrl Pts',(21.0433593424266,70.3494977028498,12.));
#161941=CARTESIAN_POINT('Ctrl Pts',(21.0265557357548,70.3291097120302,0.));
#161942=CARTESIAN_POINT('Ctrl Pts',(21.0265557357548,70.3291097120302,12.));
#161943=CARTESIAN_POINT('Ctrl Pts',(21.0097947522218,70.3087349722973,0.));
#161944=CARTESIAN_POINT('Ctrl Pts',(21.0097947522218,70.3087349722973,12.));
#161945=CARTESIAN_POINT('Ctrl Pts',(20.9930764134776,70.2883735885984,0.));
#161946=CARTESIAN_POINT('Ctrl Pts',(20.9930764134776,70.2883735885984,12.));
#161947=CARTESIAN_POINT('Ctrl Pts',(20.9764007411652,70.2680256662224,0.));
#161948=CARTESIAN_POINT('Ctrl Pts',(20.9764007411652,70.2680256662224,12.));
#161949=CARTESIAN_POINT('Ctrl Pts',(20.9597677569228,70.2476913108244,0.));
#161950=CARTESIAN_POINT('Ctrl Pts',(20.9597677569228,70.2476913108244,12.));
#161951=CARTESIAN_POINT('Ctrl Pts',(20.9431774823831,70.2273706284472,0.));
#161952=CARTESIAN_POINT('Ctrl Pts',(20.9431774823831,70.2273706284472,12.));
#161953=CARTESIAN_POINT('Ctrl Pts',(20.9266299391684,70.2070637255458,0.));
#161954=CARTESIAN_POINT('Ctrl Pts',(20.9266299391684,70.2070637255458,12.));
#161955=CARTESIAN_POINT('Ctrl Pts',(20.9101251488943,70.1867707089854,0.));
#161956=CARTESIAN_POINT('Ctrl Pts',(20.9101251488943,70.1867707089854,12.));
#161957=CARTESIAN_POINT('Ctrl Pts',(20.8936631331748,70.1664916860358,0.));
#161958=CARTESIAN_POINT('Ctrl Pts',(20.8936631331748,70.1664916860358,12.));
#161959=CARTESIAN_POINT('Ctrl Pts',(20.8772439136206,70.1462267643647,0.));
#161960=CARTESIAN_POINT('Ctrl Pts',(20.8772439136206,70.1462267643647,12.));
#161961=CARTESIAN_POINT('Ctrl Pts',(20.8608675118378,70.1259760520309,0.));
#161962=CARTESIAN_POINT('Ctrl Pts',(20.8608675118378,70.1259760520309,12.));
#161963=CARTESIAN_POINT('Ctrl Pts',(20.8445339494187,70.1057396574747,0.));
#161964=CARTESIAN_POINT('Ctrl Pts',(20.8445339494187,70.1057396574747,12.));
#161965=CARTESIAN_POINT('Ctrl Pts',(20.8282432479428,70.0855176895191,0.));
#161966=CARTESIAN_POINT('Ctrl Pts',(20.8282432479428,70.0855176895191,12.));
#161967=CARTESIAN_POINT('Ctrl Pts',(20.8119954289848,70.0653102573803,0.));
#161968=CARTESIAN_POINT('Ctrl Pts',(20.8119954289848,70.0653102573803,12.));
#161969=CARTESIAN_POINT('Ctrl Pts',(20.7957905141156,70.0451174706741,0.));
#161970=CARTESIAN_POINT('Ctrl Pts',(20.7957905141156,70.0451174706741,12.));
#161971=CARTESIAN_POINT('Ctrl Pts',(20.7796285249022,70.024939439422,0.));
#161972=CARTESIAN_POINT('Ctrl Pts',(20.7796285249022,70.024939439422,12.));
#161973=CARTESIAN_POINT('Ctrl Pts',(20.7635094829015,70.0047762740568,0.));
#161974=CARTESIAN_POINT('Ctrl Pts',(20.7635094829015,70.0047762740568,12.));
#161975=CARTESIAN_POINT('Ctrl Pts',(20.7474334096581,69.9846280854257,0.));
#161976=CARTESIAN_POINT('Ctrl Pts',(20.7474334096581,69.9846280854257,12.));
#161977=CARTESIAN_POINT('Ctrl Pts',(20.7314003267119,69.9644949847934,0.));
#161978=CARTESIAN_POINT('Ctrl Pts',(20.7314003267119,69.9644949847934,12.));
#161979=CARTESIAN_POINT('Ctrl Pts',(20.7154102555997,69.9443770838448,0.));
#161980=CARTESIAN_POINT('Ctrl Pts',(20.7154102555997,69.9443770838448,12.));
#161981=CARTESIAN_POINT('Ctrl Pts',(20.6994632178551,69.9242744946854,0.));
#161982=CARTESIAN_POINT('Ctrl Pts',(20.6994632178551,69.9242744946854,12.));
#161983=CARTESIAN_POINT('Ctrl Pts',(20.683559235003,69.904187329841,0.));
#161984=CARTESIAN_POINT('Ctrl Pts',(20.683559235003,69.904187329841,12.));
#161985=CARTESIAN_POINT('Ctrl Pts',(20.667698328554,69.8841157022568,0.));
#161986=CARTESIAN_POINT('Ctrl Pts',(20.667698328554,69.8841157022568,12.));
#161987=CARTESIAN_POINT('Ctrl Pts',(20.6518805200129,69.8640597253045,0.));
#161988=CARTESIAN_POINT('Ctrl Pts',(20.6518805200129,69.8640597253045,12.));
#161989=CARTESIAN_POINT('Ctrl Pts',(20.636105830881,69.8440195127866,0.));
#161990=CARTESIAN_POINT('Ctrl Pts',(20.636105830881,69.8440195127866,12.));
#161991=CARTESIAN_POINT('Ctrl Pts',(20.6203742826566,69.8239951789402,0.));
#161992=CARTESIAN_POINT('Ctrl Pts',(20.6203742826566,69.8239951789402,12.));
#161993=CARTESIAN_POINT('Ctrl Pts',(20.6046858968307,69.8039868384389,0.));
#161994=CARTESIAN_POINT('Ctrl Pts',(20.6046858968307,69.8039868384389,12.));
#161995=CARTESIAN_POINT('Ctrl Pts',(20.5890406948811,69.7839946063949,0.));
#161996=CARTESIAN_POINT('Ctrl Pts',(20.5890406948811,69.7839946063949,12.));
#161997=CARTESIAN_POINT('Ctrl Pts',(20.5734386982782,69.7640185983644,0.));
#161998=CARTESIAN_POINT('Ctrl Pts',(20.5734386982782,69.7640185983644,12.));
#161999=CARTESIAN_POINT('Ctrl Pts',(20.5578799284897,69.744058930351,0.));
#162000=CARTESIAN_POINT('Ctrl Pts',(20.5578799284897,69.744058930351,12.));
#162001=CARTESIAN_POINT('Ctrl Pts',(20.5423644069799,69.7241157188083,0.));
#162002=CARTESIAN_POINT('Ctrl Pts',(20.5423644069799,69.7241157188083,12.));
#162003=CARTESIAN_POINT('Ctrl Pts',(20.5268921552077,69.7041890806425,0.));
#162004=CARTESIAN_POINT('Ctrl Pts',(20.5268921552077,69.7041890806425,12.));
#162005=CARTESIAN_POINT('Ctrl Pts',(20.5114631946184,69.6842791332115,0.));
#162006=CARTESIAN_POINT('Ctrl Pts',(20.5114631946184,69.6842791332115,12.));
#162007=CARTESIAN_POINT('Ctrl Pts',(20.4960775466492,69.6643859943308,0.));
#162008=CARTESIAN_POINT('Ctrl Pts',(20.4960775466492,69.6643859943308,12.));
#162009=CARTESIAN_POINT('Ctrl Pts',(20.4807352327339,69.6445097822792,0.));
#162010=CARTESIAN_POINT('Ctrl Pts',(20.4807352327339,69.6445097822792,12.));
#162011=CARTESIAN_POINT('Ctrl Pts',(20.4654362743037,69.6246506158013,0.));
#162012=CARTESIAN_POINT('Ctrl Pts',(20.4654362743037,69.6246506158013,12.));
#162013=CARTESIAN_POINT('Ctrl Pts',(20.4501806927851,69.6048086141113,0.));
#162014=CARTESIAN_POINT('Ctrl Pts',(20.4501806927851,69.6048086141113,12.));
#162015=CARTESIAN_POINT('Ctrl Pts',(20.4349685095923,69.5849838968928,0.));
#162016=CARTESIAN_POINT('Ctrl Pts',(20.4349685095923,69.5849838968928,12.));
#162017=CARTESIAN_POINT('Ctrl Pts',(20.41979974613,69.5651765843033,0.));
#162018=CARTESIAN_POINT('Ctrl Pts',(20.41979974613,69.5651765843033,12.));
#162019=CARTESIAN_POINT('Ctrl Pts',(20.4046744237999,69.5453867969804,0.));
#162020=CARTESIAN_POINT('Ctrl Pts',(20.4046744237999,69.5453867969804,12.));
#162021=CARTESIAN_POINT('Ctrl Pts',(20.3895925640005,69.5256146560441,0.));
#162022=CARTESIAN_POINT('Ctrl Pts',(20.3895925640005,69.5256146560441,12.));
#162023=CARTESIAN_POINT('Ctrl Pts',(20.3745541881268,69.5058602831008,0.));
#162024=CARTESIAN_POINT('Ctrl Pts',(20.3745541881268,69.5058602831008,12.));
#162025=CARTESIAN_POINT('Ctrl Pts',(20.3595593175622,69.4861238002441,0.));
#162026=CARTESIAN_POINT('Ctrl Pts',(20.3595593175622,69.4861238002441,12.));
#162027=CARTESIAN_POINT('Ctrl Pts',(20.3446079736802,69.4664053300587,0.));
#162028=CARTESIAN_POINT('Ctrl Pts',(20.3446079736802,69.4664053300587,12.));
#162029=CARTESIAN_POINT('Ctrl Pts',(20.3297001778507,69.4467049956262,0.));
#162030=CARTESIAN_POINT('Ctrl Pts',(20.3297001778507,69.4467049956262,12.));
#162031=CARTESIAN_POINT('Ctrl Pts',(20.3148359514415,69.4270229205297,0.));
#162032=CARTESIAN_POINT('Ctrl Pts',(20.3148359514415,69.4270229205297,12.));
#162033=CARTESIAN_POINT('Ctrl Pts',(20.3000153158166,69.407359228856,0.));
#162034=CARTESIAN_POINT('Ctrl Pts',(20.3000153158166,69.407359228856,12.));
#162035=CARTESIAN_POINT('Ctrl Pts',(20.2852382923299,69.3877140451975,0.));
#162036=CARTESIAN_POINT('Ctrl Pts',(20.2852382923299,69.3877140451975,12.));
#162037=CARTESIAN_POINT('Ctrl Pts',(20.2705049023241,69.368087494655,0.));
#162038=CARTESIAN_POINT('Ctrl Pts',(20.2705049023241,69.368087494655,12.));
#162039=CARTESIAN_POINT('Ctrl Pts',(20.2558151671391,69.3484797028458,0.));
#162040=CARTESIAN_POINT('Ctrl Pts',(20.2558151671391,69.3484797028458,12.));
#162041=CARTESIAN_POINT('Ctrl Pts',(20.2411691081123,69.3288907959067,0.));
#162042=CARTESIAN_POINT('Ctrl Pts',(20.2411691081123,69.3288907959067,12.));
#162043=CARTESIAN_POINT('Ctrl Pts',(20.2265667465784,69.3093209004984,0.));
#162044=CARTESIAN_POINT('Ctrl Pts',(20.2265667465784,69.3093209004984,12.));
#162045=CARTESIAN_POINT('Ctrl Pts',(20.212008103862,69.2897701438059,0.));
#162046=CARTESIAN_POINT('Ctrl Pts',(20.212008103862,69.2897701438059,12.));
#162047=CARTESIAN_POINT('Ctrl Pts',(20.1974932012773,69.2702386535422,0.));
#162048=CARTESIAN_POINT('Ctrl Pts',(20.1974932012773,69.2702386535422,12.));
#162049=CARTESIAN_POINT('Ctrl Pts',(20.1830220601348,69.2507265579554,0.));
#162050=CARTESIAN_POINT('Ctrl Pts',(20.1830220601348,69.2507265579554,12.));
#162051=CARTESIAN_POINT('Ctrl Pts',(20.1685947017433,69.2312339858335,0.));
#162052=CARTESIAN_POINT('Ctrl Pts',(20.1685947017433,69.2312339858335,12.));
#162053=CARTESIAN_POINT('Ctrl Pts',(20.1542111474087,69.2117610665076,0.));
#162054=CARTESIAN_POINT('Ctrl Pts',(20.1542111474087,69.2117610665076,12.));
#162055=CARTESIAN_POINT('Ctrl Pts',(20.1398714184279,69.1923079298538,0.));
#162056=CARTESIAN_POINT('Ctrl Pts',(20.1398714184279,69.1923079298538,12.));
#162057=CARTESIAN_POINT('Ctrl Pts',(20.1255755360872,69.1728747062963,0.));
#162058=CARTESIAN_POINT('Ctrl Pts',(20.1255755360872,69.1728747062963,12.));
#162059=CARTESIAN_POINT('Ctrl Pts',(20.1113235216694,69.1534615268153,0.));
#162060=CARTESIAN_POINT('Ctrl Pts',(20.1113235216694,69.1534615268153,12.));
#162061=CARTESIAN_POINT('Ctrl Pts',(20.0971153964557,69.1340685229514,0.));
#162062=CARTESIAN_POINT('Ctrl Pts',(20.0971153964557,69.1340685229514,12.));
#162063=CARTESIAN_POINT('Ctrl Pts',(20.0829511817251,69.1146958268104,0.));
#162064=CARTESIAN_POINT('Ctrl Pts',(20.0829511817251,69.1146958268104,12.));
#162065=CARTESIAN_POINT('Ctrl Pts',(20.068830898748,69.095343571064,0.));
#162066=CARTESIAN_POINT('Ctrl Pts',(20.068830898748,69.095343571064,12.));
#162067=CARTESIAN_POINT('Ctrl Pts',(20.0547545687842,69.0760118889535,0.));
#162068=CARTESIAN_POINT('Ctrl Pts',(20.0547545687842,69.0760118889535,12.));
#162069=CARTESIAN_POINT('Ctrl Pts',(20.0407222130905,69.0567009142978,0.));
#162070=CARTESIAN_POINT('Ctrl Pts',(20.0407222130905,69.0567009142978,12.));
#162071=CARTESIAN_POINT('Ctrl Pts',(20.0267338529223,69.0374107814984,0.));
#162072=CARTESIAN_POINT('Ctrl Pts',(20.0267338529223,69.0374107814984,12.));
#162073=CARTESIAN_POINT('Ctrl Pts',(20.0127895095326,69.0181416255431,0.));
#162074=CARTESIAN_POINT('Ctrl Pts',(20.0127895095326,69.0181416255431,12.));
#162075=CARTESIAN_POINT('Ctrl Pts',(19.9988892041666,68.9988935820084,0.));
#162076=CARTESIAN_POINT('Ctrl Pts',(19.9988892041666,68.9988935820084,12.));
#162077=CARTESIAN_POINT('Ctrl Pts',(19.9850329580591,68.9796667870638,0.));
#162078=CARTESIAN_POINT('Ctrl Pts',(19.9850329580591,68.9796667870638,12.));
#162079=CARTESIAN_POINT('Ctrl Pts',(19.9712207924428,68.9604613774802,0.));
#162080=CARTESIAN_POINT('Ctrl Pts',(19.9712207924428,68.9604613774802,12.));
#162081=CARTESIAN_POINT('Ctrl Pts',(19.9574527285488,68.9412774906333,0.));
#162082=CARTESIAN_POINT('Ctrl Pts',(19.9574527285488,68.9412774906333,12.));
#162083=CARTESIAN_POINT('Ctrl Pts',(19.9437287876066,68.9221152645095,0.));
#162084=CARTESIAN_POINT('Ctrl Pts',(19.9437287876066,68.9221152645095,12.));
#162085=CARTESIAN_POINT('Ctrl Pts',(19.9300489908374,68.9029748377067,0.));
#162086=CARTESIAN_POINT('Ctrl Pts',(19.9300489908374,68.9029748377067,12.));
#162087=CARTESIAN_POINT('Ctrl Pts',(19.9164133594525,68.8838563494393,0.));
#162088=CARTESIAN_POINT('Ctrl Pts',(19.9164133594525,68.8838563494393,12.));
#162089=CARTESIAN_POINT('Ctrl Pts',(19.9028219146618,68.8647599395469,0.));
#162090=CARTESIAN_POINT('Ctrl Pts',(19.9028219146618,68.8647599395469,12.));
#162091=CARTESIAN_POINT('Ctrl Pts',(19.8892746776739,68.8456857485002,0.));
#162092=CARTESIAN_POINT('Ctrl Pts',(19.8892746776739,68.8456857485002,12.));
#162093=CARTESIAN_POINT('Ctrl Pts',(19.8757716696965,68.8266339174056,0.));
#162094=CARTESIAN_POINT('Ctrl Pts',(19.8757716696965,68.8266339174056,12.));
#162095=CARTESIAN_POINT('Ctrl Pts',(19.8623129119293,68.8076045880065,0.));
#162096=CARTESIAN_POINT('Ctrl Pts',(19.8623129119293,68.8076045880065,12.));
#162097=CARTESIAN_POINT('Ctrl Pts',(19.8488984255627,68.7885979026879,0.));
#162098=CARTESIAN_POINT('Ctrl Pts',(19.8488984255627,68.7885979026879,12.));
#162099=CARTESIAN_POINT('Ctrl Pts',(19.8355282317858,68.7696140044851,0.));
#162100=CARTESIAN_POINT('Ctrl Pts',(19.8355282317858,68.7696140044851,12.));
#162101=CARTESIAN_POINT('Ctrl Pts',(19.822202351787,68.7506530370904,0.));
#162102=CARTESIAN_POINT('Ctrl Pts',(19.822202351787,68.7506530370904,12.));
#162103=CARTESIAN_POINT('Ctrl Pts',(19.8089208067537,68.7317151448573,0.));
#162104=CARTESIAN_POINT('Ctrl Pts',(19.8089208067537,68.7317151448573,12.));
#162105=CARTESIAN_POINT('Ctrl Pts',(19.7956836178651,68.7128004728034,0.));
#162106=CARTESIAN_POINT('Ctrl Pts',(19.7956836178651,68.7128004728034,12.));
#162107=CARTESIAN_POINT('Ctrl Pts',(19.7824908062924,68.693909166615,0.));
#162108=CARTESIAN_POINT('Ctrl Pts',(19.7824908062924,68.693909166615,12.));
#162109=CARTESIAN_POINT('Ctrl Pts',(19.7693423932066,68.6750413726575,0.));
#162110=CARTESIAN_POINT('Ctrl Pts',(19.7693423932066,68.6750413726575,12.));
#162111=CARTESIAN_POINT('Ctrl Pts',(19.7562383997783,68.65619723798,0.));
#162112=CARTESIAN_POINT('Ctrl Pts',(19.7562383997783,68.65619723798,12.));
#162113=CARTESIAN_POINT('Ctrl Pts',(19.7431788471772,68.6373769103211,0.));
#162114=CARTESIAN_POINT('Ctrl Pts',(19.7431788471772,68.6373769103211,12.));
#162115=CARTESIAN_POINT('Ctrl Pts',(19.7301637565645,68.6185805381102,0.));
#162116=CARTESIAN_POINT('Ctrl Pts',(19.7301637565645,68.6185805381102,12.));
#162117=CARTESIAN_POINT('Ctrl Pts',(19.717193149095,68.5998082704741,0.));
#162118=CARTESIAN_POINT('Ctrl Pts',(19.717193149095,68.5998082704741,12.));
#162119=CARTESIAN_POINT('Ctrl Pts',(19.7042670459233,68.5810602572474,0.));
#162120=CARTESIAN_POINT('Ctrl Pts',(19.7042670459233,68.5810602572474,12.));
#162121=CARTESIAN_POINT('Ctrl Pts',(19.6913854682046,68.5623366489776,0.));
#162122=CARTESIAN_POINT('Ctrl Pts',(19.6913854682046,68.5623366489776,12.));
#162123=CARTESIAN_POINT('Ctrl Pts',(19.6785484370929,68.543637596932,0.));
#162124=CARTESIAN_POINT('Ctrl Pts',(19.6785484370929,68.543637596932,12.));
#162125=CARTESIAN_POINT('Ctrl Pts',(19.665755973734,68.5249632530994,0.));
#162126=CARTESIAN_POINT('Ctrl Pts',(19.665755973734,68.5249632530994,12.));
#162127=CARTESIAN_POINT('Ctrl Pts',(19.6530080992689,68.5063137701986,0.));
#162128=CARTESIAN_POINT('Ctrl Pts',(19.6530080992689,68.5063137701986,12.));
#162129=CARTESIAN_POINT('Ctrl Pts',(19.6403048348396,68.4876893016863,0.));
#162130=CARTESIAN_POINT('Ctrl Pts',(19.6403048348396,68.4876893016863,12.));
#162131=CARTESIAN_POINT('Ctrl Pts',(19.6276462015888,68.4690900017631,0.));
#162132=CARTESIAN_POINT('Ctrl Pts',(19.6276462015888,68.4690900017631,12.));
#162133=CARTESIAN_POINT('Ctrl Pts',(19.6150322206577,68.4505160253777,0.));
#162134=CARTESIAN_POINT('Ctrl Pts',(19.6150322206577,68.4505160253777,12.));
#162135=CARTESIAN_POINT('Ctrl Pts',(19.6024629131785,68.4319675282273,0.));
#162136=CARTESIAN_POINT('Ctrl Pts',(19.6024629131785,68.4319675282273,12.));
#162137=CARTESIAN_POINT('Ctrl Pts',(19.5899383002803,68.4134446667695,0.));
#162138=CARTESIAN_POINT('Ctrl Pts',(19.5899383002803,68.4134446667695,12.));
#162139=CARTESIAN_POINT('Ctrl Pts',(19.5774584030938,68.3949475982334,0.));
#162140=CARTESIAN_POINT('Ctrl Pts',(19.5774584030938,68.3949475982334,12.));
#162141=CARTESIAN_POINT('Ctrl Pts',(19.5650232427516,68.3764764806287,0.));
#162142=CARTESIAN_POINT('Ctrl Pts',(19.5650232427516,68.3764764806287,12.));
#162143=CARTESIAN_POINT('Ctrl Pts',(19.5526328403851,68.3580314727522,0.));
#162144=CARTESIAN_POINT('Ctrl Pts',(19.5526328403851,68.3580314727522,12.));
#162145=CARTESIAN_POINT('Ctrl Pts',(19.540287217119,68.3396127341937,0.));
#162146=CARTESIAN_POINT('Ctrl Pts',(19.540287217119,68.3396127341937,12.));
#162147=CARTESIAN_POINT('Ctrl Pts',(19.5279863940772,68.3212204253416,0.));
#162148=CARTESIAN_POINT('Ctrl Pts',(19.5279863940772,68.3212204253416,12.));
#162149=CARTESIAN_POINT('Ctrl Pts',(19.5157303923855,68.3028547073862,0.));
#162150=CARTESIAN_POINT('Ctrl Pts',(19.5157303923855,68.3028547073862,12.));
#162151=CARTESIAN_POINT('Ctrl Pts',(19.5035192331706,68.2845157423234,0.));
#162152=CARTESIAN_POINT('Ctrl Pts',(19.5035192331706,68.2845157423234,12.));
#162153=CARTESIAN_POINT('Ctrl Pts',(19.4913529375545,68.2662036929531,0.));
#162154=CARTESIAN_POINT('Ctrl Pts',(19.4913529375545,68.2662036929531,12.));
#162155=CARTESIAN_POINT('Ctrl Pts',(19.4792315266505,68.2479187228815,0.));
#162156=CARTESIAN_POINT('Ctrl Pts',(19.4792315266505,68.2479187228815,12.));
#162157=CARTESIAN_POINT('Ctrl Pts',(19.4671550215724,68.2296609965461,0.));
#162158=CARTESIAN_POINT('Ctrl Pts',(19.4671550215724,68.2296609965461,12.));
#162159=CARTESIAN_POINT('Ctrl Pts',(19.4551234434383,68.2114306792366,0.));
#162160=CARTESIAN_POINT('Ctrl Pts',(19.4551234434383,68.2114306792366,12.));
#162161=CARTESIAN_POINT('Ctrl Pts',(19.4431368133718,68.1932279371121,0.));
#162162=CARTESIAN_POINT('Ctrl Pts',(19.4431368133718,68.1932279371121,12.));
#162163=CARTESIAN_POINT('Ctrl Pts',(19.4311951524977,68.1750529372211,0.));
#162164=CARTESIAN_POINT('Ctrl Pts',(19.4311951524977,68.1750529372211,12.));
#162165=CARTESIAN_POINT('Ctrl Pts',(19.419298481941,68.1569058475026,0.));
#162166=CARTESIAN_POINT('Ctrl Pts',(19.419298481941,68.1569058475026,12.));
#162167=CARTESIAN_POINT('Ctrl Pts',(19.4074468228293,68.1387868367668,0.));
#162168=CARTESIAN_POINT('Ctrl Pts',(19.4074468228293,68.1387868367668,12.));
#162169=CARTESIAN_POINT('Ctrl Pts',(19.3956401962893,68.1206960746763,0.));
#162170=CARTESIAN_POINT('Ctrl Pts',(19.3956401962893,68.1206960746763,12.));
#162171=CARTESIAN_POINT('Ctrl Pts',(19.3838786234425,68.1026337317298,0.));
#162172=CARTESIAN_POINT('Ctrl Pts',(19.3838786234425,68.1026337317298,12.));
#162173=CARTESIAN_POINT('Ctrl Pts',(19.372162125392,68.0845999792274,0.));
#162174=CARTESIAN_POINT('Ctrl Pts',(19.372162125392,68.0845999792274,12.));
#162175=CARTESIAN_POINT('Ctrl Pts',(19.3604907232322,68.0665949893222,0.));
#162176=CARTESIAN_POINT('Ctrl Pts',(19.3604907232322,68.0665949893222,12.));
#162177=CARTESIAN_POINT('Ctrl Pts',(19.3488644380646,68.0486189351027,0.));
#162178=CARTESIAN_POINT('Ctrl Pts',(19.3488644380646,68.0486189351027,12.));
#162179=CARTESIAN_POINT('Ctrl Pts',(19.3372832910076,68.0306719906636,0.));
#162180=CARTESIAN_POINT('Ctrl Pts',(19.3372832910076,68.0306719906636,12.));
#162181=CARTESIAN_POINT('Ctrl Pts',(19.3257473032031,68.0127543311761,0.));
#162182=CARTESIAN_POINT('Ctrl Pts',(19.3257473032031,68.0127543311761,12.));
#162183=CARTESIAN_POINT('Ctrl Pts',(19.3142564958195,67.9948661329592,0.));
#162184=CARTESIAN_POINT('Ctrl Pts',(19.3142564958195,67.9948661329592,12.));
#162185=CARTESIAN_POINT('Ctrl Pts',(19.3028108900373,67.977007573346,0.));
#162186=CARTESIAN_POINT('Ctrl Pts',(19.3028108900373,67.977007573346,12.));
#162187=CARTESIAN_POINT('Ctrl Pts',(19.2914105070282,67.959178830538,0.));
#162188=CARTESIAN_POINT('Ctrl Pts',(19.2914105070282,67.959178830538,12.));
#162189=CARTESIAN_POINT('Ctrl Pts',(19.2800553679362,67.9413800834798,0.));
#162190=CARTESIAN_POINT('Ctrl Pts',(19.2800553679362,67.9413800834798,12.));
#162191=CARTESIAN_POINT('Ctrl Pts',(19.2687454938448,67.9236115116781,0.));
#162192=CARTESIAN_POINT('Ctrl Pts',(19.2687454938448,67.9236115116781,12.));
#162193=CARTESIAN_POINT('Ctrl Pts',(19.2574809057705,67.9058732951822,0.));
#162194=CARTESIAN_POINT('Ctrl Pts',(19.2574809057705,67.9058732951822,12.));
#162195=CARTESIAN_POINT('Ctrl Pts',(19.2462616247287,67.8881656149983,0.));
#162196=CARTESIAN_POINT('Ctrl Pts',(19.2462616247287,67.8881656149983,12.));
#162197=CARTESIAN_POINT('Ctrl Pts',(19.2350876717877,67.8704886534555,0.));
#162198=CARTESIAN_POINT('Ctrl Pts',(19.2350876717877,67.8704886534555,12.));
#162199=CARTESIAN_POINT('Ctrl Pts',(19.2239590681129,67.852842594517,0.));
#162200=CARTESIAN_POINT('Ctrl Pts',(19.2239590681129,67.852842594517,12.));
#162201=CARTESIAN_POINT('Ctrl Pts',(19.2128758350336,67.8352276242856,0.));
#162202=CARTESIAN_POINT('Ctrl Pts',(19.2128758350336,67.8352276242856,12.));
#162203=CARTESIAN_POINT('Ctrl Pts',(19.2018379939918,67.817643930658,0.));
#162204=CARTESIAN_POINT('Ctrl Pts',(19.2018379939918,67.817643930658,12.));
#162205=CARTESIAN_POINT('Ctrl Pts',(19.1908455664089,67.8000917023896,0.));
#162206=CARTESIAN_POINT('Ctrl Pts',(19.1908455664089,67.8000917023896,12.));
#162207=CARTESIAN_POINT('Ctrl Pts',(19.1798985735687,67.7825711283092,0.));
#162208=CARTESIAN_POINT('Ctrl Pts',(19.1798985735687,67.7825711283092,12.));
#162209=CARTESIAN_POINT('Ctrl Pts',(19.1689970364958,67.7650823965156,0.));
#162210=CARTESIAN_POINT('Ctrl Pts',(19.1689970364958,67.7650823965156,12.));
#162211=CARTESIAN_POINT('Ctrl Pts',(19.1581409758111,67.7476256934493,0.));
#162212=CARTESIAN_POINT('Ctrl Pts',(19.1581409758111,67.7476256934493,12.));
#162213=CARTESIAN_POINT('Ctrl Pts',(19.1473304119968,67.730201205663,0.));
#162214=CARTESIAN_POINT('Ctrl Pts',(19.1473304119968,67.730201205663,12.));
#162215=CARTESIAN_POINT('Ctrl Pts',(19.1365653657097,67.7128091219372,0.));
#162216=CARTESIAN_POINT('Ctrl Pts',(19.1365653657097,67.7128091219372,12.));
#162217=CARTESIAN_POINT('Ctrl Pts',(19.1258458580343,67.6954496350053,0.));
#162218=CARTESIAN_POINT('Ctrl Pts',(19.1258458580343,67.6954496350053,12.));
#162219=CARTESIAN_POINT('Ctrl Pts',(19.115171910845,67.6781229440535,0.));
#162220=CARTESIAN_POINT('Ctrl Pts',(19.115171910845,67.6781229440535,12.));
#162221=CARTESIAN_POINT('Ctrl Pts',(19.1045435468344,67.6608292549412,0.));
#162222=CARTESIAN_POINT('Ctrl Pts',(19.1045435468344,67.6608292549412,12.));
#162223=CARTESIAN_POINT('Ctrl Pts',(19.0939607887491,67.6435687749803,0.));
#162224=CARTESIAN_POINT('Ctrl Pts',(19.0939607887491,67.6435687749803,12.));
#162225=CARTESIAN_POINT('Ctrl Pts',(19.0834236587115,67.6263417083414,0.));
#162226=CARTESIAN_POINT('Ctrl Pts',(19.0834236587115,67.6263417083414,12.));
#162227=CARTESIAN_POINT('Ctrl Pts',(19.0729321776286,67.6091482520558,0.));
#162228=CARTESIAN_POINT('Ctrl Pts',(19.0729321776286,67.6091482520558,12.));
#162229=CARTESIAN_POINT('Ctrl Pts',(19.0624863642425,67.5919885896278,0.));
#162230=CARTESIAN_POINT('Ctrl Pts',(19.0624863642425,67.5919885896278,12.));
#162231=CARTESIAN_POINT('Ctrl Pts',(19.0520862360413,67.5748628972035,0.));
#162232=CARTESIAN_POINT('Ctrl Pts',(19.0520862360413,67.5748628972035,12.));
#162233=CARTESIAN_POINT('Ctrl Pts',(19.0417318110721,67.5577713558248,0.));
#162234=CARTESIAN_POINT('Ctrl Pts',(19.0417318110721,67.5577713558248,12.));
#162235=CARTESIAN_POINT('Ctrl Pts',(19.0314231093923,67.5407141612881,0.));
#162236=CARTESIAN_POINT('Ctrl Pts',(19.0314231093923,67.5407141612881,12.));
#162237=CARTESIAN_POINT('Ctrl Pts',(19.0211601548222,67.5236915360253,0.));
#162238=CARTESIAN_POINT('Ctrl Pts',(19.0211601548222,67.5236915360253,12.));
#162239=CARTESIAN_POINT('Ctrl Pts',(19.0109429761274,67.5067037372177,0.));
#162240=CARTESIAN_POINT('Ctrl Pts',(19.0109429761274,67.5067037372177,12.));
#162241=CARTESIAN_POINT('Ctrl Pts',(19.0007716032784,67.4897510316692,0.));
#162242=CARTESIAN_POINT('Ctrl Pts',(19.0007716032784,67.4897510316692,12.));
#162243=CARTESIAN_POINT('Ctrl Pts',(18.9906460638607,67.4728336719559,0.));
#162244=CARTESIAN_POINT('Ctrl Pts',(18.9906460638607,67.4728336719559,12.));
#162245=CARTESIAN_POINT('Ctrl Pts',(18.9805663798466,67.4559518744714,0.));
#162246=CARTESIAN_POINT('Ctrl Pts',(18.9805663798466,67.4559518744714,12.));
#162247=CARTESIAN_POINT('Ctrl Pts',(18.9705325631772,67.4391057908687,0.));
#162248=CARTESIAN_POINT('Ctrl Pts',(18.9705325631772,67.4391057908687,12.));
#162249=CARTESIAN_POINT('Ctrl Pts',(18.9605446161078,67.4222955062385,0.));
#162250=CARTESIAN_POINT('Ctrl Pts',(18.9605446161078,67.4222955062385,12.));
#162251=CARTESIAN_POINT('Ctrl Pts',(18.9525909518002,67.4088759498287,0.));
#162252=CARTESIAN_POINT('Ctrl Pts',(18.9525909518002,67.4088759498287,12.));
#162253=CARTESIAN_POINT('Ctrl Pts',(18.9466463414354,67.398827414689,0.));
#162254=CARTESIAN_POINT('Ctrl Pts',(18.9466463414354,67.398827414689,12.));
#162255=CARTESIAN_POINT('Ctrl Pts',(18.942692439874,67.3921355608417,0.));
#162256=CARTESIAN_POINT('Ctrl Pts',(18.942692439874,67.3921355608417,12.));
#162257=CARTESIAN_POINT('Ctrl Pts',(18.9407177820969,67.3887914263119,0.));
#162258=CARTESIAN_POINT('Ctrl Pts',(18.9407177820969,67.3887914263119,12.));
#162259=CARTESIAN_POINT('',(18.9407177820969,67.3887914263119,12.));
#162260=CARTESIAN_POINT('Ctrl Pts',(18.9407177820969,67.3887914263119,12.));
#162261=CARTESIAN_POINT('Ctrl Pts',(18.942692439874,67.3921355608417,12.));
#162262=CARTESIAN_POINT('Ctrl Pts',(18.9466463414354,67.398827414689,12.));
#162263=CARTESIAN_POINT('Ctrl Pts',(18.9525909518002,67.4088759498287,12.));
#162264=CARTESIAN_POINT('Ctrl Pts',(18.9605446161078,67.4222955062385,12.));
#162265=CARTESIAN_POINT('Ctrl Pts',(18.9705325631772,67.4391057908687,12.));
#162266=CARTESIAN_POINT('Ctrl Pts',(18.9805663798466,67.4559518744714,12.));
#162267=CARTESIAN_POINT('Ctrl Pts',(18.9906460638607,67.4728336719559,12.));
#162268=CARTESIAN_POINT('Ctrl Pts',(19.0007716032784,67.4897510316692,12.));
#162269=CARTESIAN_POINT('Ctrl Pts',(19.0109429761274,67.5067037372177,12.));
#162270=CARTESIAN_POINT('Ctrl Pts',(19.0211601548222,67.5236915360253,12.));
#162271=CARTESIAN_POINT('Ctrl Pts',(19.0314231093923,67.5407141612881,12.));
#162272=CARTESIAN_POINT('Ctrl Pts',(19.0417318110721,67.5577713558248,12.));
#162273=CARTESIAN_POINT('Ctrl Pts',(19.0520862360413,67.5748628972035,12.));
#162274=CARTESIAN_POINT('Ctrl Pts',(19.0624863642425,67.5919885896278,12.));
#162275=CARTESIAN_POINT('Ctrl Pts',(19.0729321776286,67.6091482520558,12.));
#162276=CARTESIAN_POINT('Ctrl Pts',(19.0834236587115,67.6263417083414,12.));
#162277=CARTESIAN_POINT('Ctrl Pts',(19.0939607887491,67.6435687749803,12.));
#162278=CARTESIAN_POINT('Ctrl Pts',(19.1045435468344,67.6608292549412,12.));
#162279=CARTESIAN_POINT('Ctrl Pts',(19.115171910845,67.6781229440535,12.));
#162280=CARTESIAN_POINT('Ctrl Pts',(19.1258458580343,67.6954496350053,12.));
#162281=CARTESIAN_POINT('Ctrl Pts',(19.1365653657097,67.7128091219372,12.));
#162282=CARTESIAN_POINT('Ctrl Pts',(19.1473304119968,67.730201205663,12.));
#162283=CARTESIAN_POINT('Ctrl Pts',(19.1581409758111,67.7476256934493,12.));
#162284=CARTESIAN_POINT('Ctrl Pts',(19.1689970364958,67.7650823965156,12.));
#162285=CARTESIAN_POINT('Ctrl Pts',(19.1798985735687,67.7825711283092,12.));
#162286=CARTESIAN_POINT('Ctrl Pts',(19.1908455664089,67.8000917023896,12.));
#162287=CARTESIAN_POINT('Ctrl Pts',(19.2018379939918,67.817643930658,12.));
#162288=CARTESIAN_POINT('Ctrl Pts',(19.2128758350336,67.8352276242856,12.));
#162289=CARTESIAN_POINT('Ctrl Pts',(19.2239590681129,67.852842594517,12.));
#162290=CARTESIAN_POINT('Ctrl Pts',(19.2350876717877,67.8704886534555,12.));
#162291=CARTESIAN_POINT('Ctrl Pts',(19.2462616247287,67.8881656149983,12.));
#162292=CARTESIAN_POINT('Ctrl Pts',(19.2574809057705,67.9058732951822,12.));
#162293=CARTESIAN_POINT('Ctrl Pts',(19.2687454938448,67.9236115116781,12.));
#162294=CARTESIAN_POINT('Ctrl Pts',(19.2800553679362,67.9413800834798,12.));
#162295=CARTESIAN_POINT('Ctrl Pts',(19.2914105070282,67.959178830538,12.));
#162296=CARTESIAN_POINT('Ctrl Pts',(19.3028108900373,67.977007573346,12.));
#162297=CARTESIAN_POINT('Ctrl Pts',(19.3142564958195,67.9948661329592,12.));
#162298=CARTESIAN_POINT('Ctrl Pts',(19.3257473032031,68.0127543311761,12.));
#162299=CARTESIAN_POINT('Ctrl Pts',(19.3372832910076,68.0306719906636,12.));
#162300=CARTESIAN_POINT('Ctrl Pts',(19.3488644380646,68.0486189351027,12.));
#162301=CARTESIAN_POINT('Ctrl Pts',(19.3604907232322,68.0665949893222,12.));
#162302=CARTESIAN_POINT('Ctrl Pts',(19.372162125392,68.0845999792274,12.));
#162303=CARTESIAN_POINT('Ctrl Pts',(19.3838786234425,68.1026337317298,12.));
#162304=CARTESIAN_POINT('Ctrl Pts',(19.3956401962893,68.1206960746763,12.));
#162305=CARTESIAN_POINT('Ctrl Pts',(19.4074468228293,68.1387868367668,12.));
#162306=CARTESIAN_POINT('Ctrl Pts',(19.419298481941,68.1569058475026,12.));
#162307=CARTESIAN_POINT('Ctrl Pts',(19.4311951524977,68.1750529372211,12.));
#162308=CARTESIAN_POINT('Ctrl Pts',(19.4431368133718,68.1932279371121,12.));
#162309=CARTESIAN_POINT('Ctrl Pts',(19.4551234434383,68.2114306792366,12.));
#162310=CARTESIAN_POINT('Ctrl Pts',(19.4671550215724,68.2296609965461,12.));
#162311=CARTESIAN_POINT('Ctrl Pts',(19.4792315266505,68.2479187228815,12.));
#162312=CARTESIAN_POINT('Ctrl Pts',(19.4913529375545,68.2662036929531,12.));
#162313=CARTESIAN_POINT('Ctrl Pts',(19.5035192331706,68.2845157423234,12.));
#162314=CARTESIAN_POINT('Ctrl Pts',(19.5157303923855,68.3028547073862,12.));
#162315=CARTESIAN_POINT('Ctrl Pts',(19.5279863940772,68.3212204253416,12.));
#162316=CARTESIAN_POINT('Ctrl Pts',(19.540287217119,68.3396127341937,12.));
#162317=CARTESIAN_POINT('Ctrl Pts',(19.5526328403851,68.3580314727522,12.));
#162318=CARTESIAN_POINT('Ctrl Pts',(19.5650232427516,68.3764764806287,12.));
#162319=CARTESIAN_POINT('Ctrl Pts',(19.5774584030938,68.3949475982334,12.));
#162320=CARTESIAN_POINT('Ctrl Pts',(19.5899383002803,68.4134446667695,12.));
#162321=CARTESIAN_POINT('Ctrl Pts',(19.6024629131785,68.4319675282273,12.));
#162322=CARTESIAN_POINT('Ctrl Pts',(19.6150322206577,68.4505160253777,12.));
#162323=CARTESIAN_POINT('Ctrl Pts',(19.6276462015888,68.4690900017631,12.));
#162324=CARTESIAN_POINT('Ctrl Pts',(19.6403048348396,68.4876893016863,12.));
#162325=CARTESIAN_POINT('Ctrl Pts',(19.6530080992689,68.5063137701986,12.));
#162326=CARTESIAN_POINT('Ctrl Pts',(19.665755973734,68.5249632530994,12.));
#162327=CARTESIAN_POINT('Ctrl Pts',(19.6785484370929,68.543637596932,12.));
#162328=CARTESIAN_POINT('Ctrl Pts',(19.6913854682046,68.5623366489776,12.));
#162329=CARTESIAN_POINT('Ctrl Pts',(19.7042670459233,68.5810602572474,12.));
#162330=CARTESIAN_POINT('Ctrl Pts',(19.717193149095,68.5998082704741,12.));
#162331=CARTESIAN_POINT('Ctrl Pts',(19.7301637565645,68.6185805381102,12.));
#162332=CARTESIAN_POINT('Ctrl Pts',(19.7431788471772,68.6373769103211,12.));
#162333=CARTESIAN_POINT('Ctrl Pts',(19.7562383997783,68.65619723798,12.));
#162334=CARTESIAN_POINT('Ctrl Pts',(19.7693423932066,68.6750413726575,12.));
#162335=CARTESIAN_POINT('Ctrl Pts',(19.7824908062924,68.693909166615,12.));
#162336=CARTESIAN_POINT('Ctrl Pts',(19.7956836178651,68.7128004728034,12.));
#162337=CARTESIAN_POINT('Ctrl Pts',(19.8089208067537,68.7317151448573,12.));
#162338=CARTESIAN_POINT('Ctrl Pts',(19.822202351787,68.7506530370904,12.));
#162339=CARTESIAN_POINT('Ctrl Pts',(19.8355282317858,68.7696140044851,12.));
#162340=CARTESIAN_POINT('Ctrl Pts',(19.8488984255627,68.7885979026879,12.));
#162341=CARTESIAN_POINT('Ctrl Pts',(19.8623129119293,68.8076045880065,12.));
#162342=CARTESIAN_POINT('Ctrl Pts',(19.8757716696965,68.8266339174056,12.));
#162343=CARTESIAN_POINT('Ctrl Pts',(19.8892746776739,68.8456857485002,12.));
#162344=CARTESIAN_POINT('Ctrl Pts',(19.9028219146618,68.8647599395469,12.));
#162345=CARTESIAN_POINT('Ctrl Pts',(19.9164133594525,68.8838563494393,12.));
#162346=CARTESIAN_POINT('Ctrl Pts',(19.9300489908374,68.9029748377067,12.));
#162347=CARTESIAN_POINT('Ctrl Pts',(19.9437287876066,68.9221152645095,12.));
#162348=CARTESIAN_POINT('Ctrl Pts',(19.9574527285488,68.9412774906333,12.));
#162349=CARTESIAN_POINT('Ctrl Pts',(19.9712207924428,68.9604613774802,12.));
#162350=CARTESIAN_POINT('Ctrl Pts',(19.9850329580591,68.9796667870638,12.));
#162351=CARTESIAN_POINT('Ctrl Pts',(19.9988892041666,68.9988935820084,12.));
#162352=CARTESIAN_POINT('Ctrl Pts',(20.0127895095326,69.0181416255431,12.));
#162353=CARTESIAN_POINT('Ctrl Pts',(20.0267338529223,69.0374107814984,12.));
#162354=CARTESIAN_POINT('Ctrl Pts',(20.0407222130905,69.0567009142978,12.));
#162355=CARTESIAN_POINT('Ctrl Pts',(20.0547545687842,69.0760118889535,12.));
#162356=CARTESIAN_POINT('Ctrl Pts',(20.068830898748,69.095343571064,12.));
#162357=CARTESIAN_POINT('Ctrl Pts',(20.0829511817251,69.1146958268104,12.));
#162358=CARTESIAN_POINT('Ctrl Pts',(20.0971153964557,69.1340685229514,12.));
#162359=CARTESIAN_POINT('Ctrl Pts',(20.1113235216694,69.1534615268153,12.));
#162360=CARTESIAN_POINT('Ctrl Pts',(20.1255755360872,69.1728747062963,12.));
#162361=CARTESIAN_POINT('Ctrl Pts',(20.1398714184279,69.1923079298538,12.));
#162362=CARTESIAN_POINT('Ctrl Pts',(20.1542111474087,69.2117610665076,12.));
#162363=CARTESIAN_POINT('Ctrl Pts',(20.1685947017433,69.2312339858335,12.));
#162364=CARTESIAN_POINT('Ctrl Pts',(20.1830220601348,69.2507265579554,12.));
#162365=CARTESIAN_POINT('Ctrl Pts',(20.1974932012773,69.2702386535422,12.));
#162366=CARTESIAN_POINT('Ctrl Pts',(20.212008103862,69.2897701438059,12.));
#162367=CARTESIAN_POINT('Ctrl Pts',(20.2265667465784,69.3093209004984,12.));
#162368=CARTESIAN_POINT('Ctrl Pts',(20.2411691081123,69.3288907959067,12.));
#162369=CARTESIAN_POINT('Ctrl Pts',(20.2558151671391,69.3484797028458,12.));
#162370=CARTESIAN_POINT('Ctrl Pts',(20.2705049023241,69.368087494655,12.));
#162371=CARTESIAN_POINT('Ctrl Pts',(20.2852382923299,69.3877140451975,12.));
#162372=CARTESIAN_POINT('Ctrl Pts',(20.3000153158166,69.407359228856,12.));
#162373=CARTESIAN_POINT('Ctrl Pts',(20.3148359514415,69.4270229205297,12.));
#162374=CARTESIAN_POINT('Ctrl Pts',(20.3297001778507,69.4467049956262,12.));
#162375=CARTESIAN_POINT('Ctrl Pts',(20.3446079736802,69.4664053300587,12.));
#162376=CARTESIAN_POINT('Ctrl Pts',(20.3595593175622,69.4861238002441,12.));
#162377=CARTESIAN_POINT('Ctrl Pts',(20.3745541881268,69.5058602831008,12.));
#162378=CARTESIAN_POINT('Ctrl Pts',(20.3895925640005,69.5256146560441,12.));
#162379=CARTESIAN_POINT('Ctrl Pts',(20.4046744237999,69.5453867969804,12.));
#162380=CARTESIAN_POINT('Ctrl Pts',(20.41979974613,69.5651765843033,12.));
#162381=CARTESIAN_POINT('Ctrl Pts',(20.4349685095923,69.5849838968928,12.));
#162382=CARTESIAN_POINT('Ctrl Pts',(20.4501806927851,69.6048086141113,12.));
#162383=CARTESIAN_POINT('Ctrl Pts',(20.4654362743037,69.6246506158013,12.));
#162384=CARTESIAN_POINT('Ctrl Pts',(20.4807352327339,69.6445097822792,12.));
#162385=CARTESIAN_POINT('Ctrl Pts',(20.4960775466492,69.6643859943308,12.));
#162386=CARTESIAN_POINT('Ctrl Pts',(20.5114631946184,69.6842791332115,12.));
#162387=CARTESIAN_POINT('Ctrl Pts',(20.5268921552077,69.7041890806425,12.));
#162388=CARTESIAN_POINT('Ctrl Pts',(20.5423644069799,69.7241157188083,12.));
#162389=CARTESIAN_POINT('Ctrl Pts',(20.5578799284897,69.744058930351,12.));
#162390=CARTESIAN_POINT('Ctrl Pts',(20.5734386982782,69.7640185983644,12.));
#162391=CARTESIAN_POINT('Ctrl Pts',(20.5890406948811,69.7839946063949,12.));
#162392=CARTESIAN_POINT('Ctrl Pts',(20.6046858968307,69.8039868384389,12.));
#162393=CARTESIAN_POINT('Ctrl Pts',(20.6203742826566,69.8239951789402,12.));
#162394=CARTESIAN_POINT('Ctrl Pts',(20.636105830881,69.8440195127866,12.));
#162395=CARTESIAN_POINT('Ctrl Pts',(20.6518805200129,69.8640597253045,12.));
#162396=CARTESIAN_POINT('Ctrl Pts',(20.667698328554,69.8841157022568,12.));
#162397=CARTESIAN_POINT('Ctrl Pts',(20.683559235003,69.904187329841,12.));
#162398=CARTESIAN_POINT('Ctrl Pts',(20.6994632178551,69.9242744946854,12.));
#162399=CARTESIAN_POINT('Ctrl Pts',(20.7154102555997,69.9443770838448,12.));
#162400=CARTESIAN_POINT('Ctrl Pts',(20.7314003267119,69.9644949847934,12.));
#162401=CARTESIAN_POINT('Ctrl Pts',(20.7474334096581,69.9846280854257,12.));
#162402=CARTESIAN_POINT('Ctrl Pts',(20.7635094829015,70.0047762740568,12.));
#162403=CARTESIAN_POINT('Ctrl Pts',(20.7796285249022,70.024939439422,12.));
#162404=CARTESIAN_POINT('Ctrl Pts',(20.7957905141156,70.0451174706741,12.));
#162405=CARTESIAN_POINT('Ctrl Pts',(20.8119954289848,70.0653102573803,12.));
#162406=CARTESIAN_POINT('Ctrl Pts',(20.8282432479428,70.0855176895191,12.));
#162407=CARTESIAN_POINT('Ctrl Pts',(20.8445339494187,70.1057396574747,12.));
#162408=CARTESIAN_POINT('Ctrl Pts',(20.8608675118378,70.1259760520309,12.));
#162409=CARTESIAN_POINT('Ctrl Pts',(20.8772439136206,70.1462267643647,12.));
#162410=CARTESIAN_POINT('Ctrl Pts',(20.8936631331748,70.1664916860358,12.));
#162411=CARTESIAN_POINT('Ctrl Pts',(20.9101251488943,70.1867707089854,12.));
#162412=CARTESIAN_POINT('Ctrl Pts',(20.9266299391684,70.2070637255458,12.));
#162413=CARTESIAN_POINT('Ctrl Pts',(20.9431774823831,70.2273706284472,12.));
#162414=CARTESIAN_POINT('Ctrl Pts',(20.9597677569228,70.2476913108244,12.));
#162415=CARTESIAN_POINT('Ctrl Pts',(20.9764007411652,70.2680256662224,12.));
#162416=CARTESIAN_POINT('Ctrl Pts',(20.9930764134776,70.2883735885984,12.));
#162417=CARTESIAN_POINT('Ctrl Pts',(21.0097947522218,70.3087349722973,12.));
#162418=CARTESIAN_POINT('Ctrl Pts',(21.0265557357548,70.3291097120302,12.));
#162419=CARTESIAN_POINT('Ctrl Pts',(21.0433593424266,70.3494977028498,12.));
#162420=CARTESIAN_POINT('Ctrl Pts',(21.0602055505748,70.3698988401281,12.));
#162421=CARTESIAN_POINT('Ctrl Pts',(21.0770943385141,70.3903130195265,12.));
#162422=CARTESIAN_POINT('Ctrl Pts',(21.0940256845472,70.4107401370389,12.));
#162423=CARTESIAN_POINT('Ctrl Pts',(21.1109995669747,70.4311800890402,12.));
#162424=CARTESIAN_POINT('Ctrl Pts',(21.1280159641002,70.4516327723346,12.));
#162425=CARTESIAN_POINT('Ctrl Pts',(21.1450748542336,70.4720980841939,12.));
#162426=CARTESIAN_POINT('Ctrl Pts',(21.1621762156897,70.4925759224216,12.));
#162427=CARTESIAN_POINT('Ctrl Pts',(21.1793200267846,70.5130661852955,12.));
#162428=CARTESIAN_POINT('Ctrl Pts',(21.1965062658298,70.5335687714429,12.));
#162429=CARTESIAN_POINT('Ctrl Pts',(21.2137349111208,70.5540835797283,12.));
#162430=CARTESIAN_POINT('Ctrl Pts',(21.2310059409265,70.5746105091502,12.));
#162431=CARTESIAN_POINT('Ctrl Pts',(21.2483193334675,70.5951494586957,12.));
#162432=CARTESIAN_POINT('Ctrl Pts',(21.2656750669126,70.6157003273316,12.));
#162433=CARTESIAN_POINT('Ctrl Pts',(21.2830731194183,70.6362630143047,12.));
#162434=CARTESIAN_POINT('Ctrl Pts',(21.300513469156,70.6568374193774,12.));
#162435=CARTESIAN_POINT('Ctrl Pts',(21.3179960943388,70.6774234430897,12.));
#162436=CARTESIAN_POINT('Ctrl Pts',(21.3355209732443,70.6980209870045,12.));
#162437=CARTESIAN_POINT('Ctrl Pts',(21.3530880842349,70.7186299539724,12.));
#162438=CARTESIAN_POINT('Ctrl Pts',(21.3706974057039,70.7392502475469,12.));
#162439=CARTESIAN_POINT('Ctrl Pts',(21.3883489160196,70.7598817714105,12.));
#162440=CARTESIAN_POINT('Ctrl Pts',(21.4060425934598,70.780524428745,12.));
#162441=CARTESIAN_POINT('Ctrl Pts',(21.4237784161587,70.8011781217394,12.));
#162442=CARTESIAN_POINT('Ctrl Pts',(21.4415563620114,70.8218427507506,12.));
#162443=CARTESIAN_POINT('Ctrl Pts',(21.4593764087473,70.8425182149846,12.));
#162444=CARTESIAN_POINT('Ctrl Pts',(21.477238534096,70.8632044140112,12.));
#162445=CARTESIAN_POINT('Ctrl Pts',(21.4951427159261,70.8839012490871,12.));
#162446=CARTESIAN_POINT('Ctrl Pts',(21.513088932377,70.9046086244131,12.));
#162447=CARTESIAN_POINT('Ctrl Pts',(21.531077162023,70.9253264487637,12.));
#162448=CARTESIAN_POINT('Ctrl Pts',(21.5491073839106,70.94605463587,12.));
#162449=CARTESIAN_POINT('Ctrl Pts',(21.564598755537,70.9638315189818,12.));
#162450=CARTESIAN_POINT('Ctrl Pts',(21.5764983366483,70.977466211259,12.));
#162451=CARTESIAN_POINT('Ctrl Pts',(21.5847875433334,70.9869541808057,12.));
#162452=CARTESIAN_POINT('Ctrl Pts',(21.5894540925586,70.9922924595372,12.));
#162453=CARTESIAN_POINT('Ctrl Pts',(21.5904919935065,70.993479606912,12.));
#162454=CARTESIAN_POINT('',(18.9407177820969,67.3887914263119,0.));
#162455=CARTESIAN_POINT('',(18.9407177820969,67.3887914263118,0.));
#162456=CARTESIAN_POINT('Ctrl Pts',(21.5904919935065,70.993479606912,0.));
#162457=CARTESIAN_POINT('Ctrl Pts',(21.5894540925586,70.9922924595372,0.));
#162458=CARTESIAN_POINT('Ctrl Pts',(21.5847875433334,70.9869541808057,0.));
#162459=CARTESIAN_POINT('Ctrl Pts',(21.5764983366483,70.977466211259,0.));
#162460=CARTESIAN_POINT('Ctrl Pts',(21.564598755537,70.9638315189818,0.));
#162461=CARTESIAN_POINT('Ctrl Pts',(21.5491073839106,70.94605463587,0.));
#162462=CARTESIAN_POINT('Ctrl Pts',(21.531077162023,70.9253264487637,0.));
#162463=CARTESIAN_POINT('Ctrl Pts',(21.513088932377,70.9046086244131,0.));
#162464=CARTESIAN_POINT('Ctrl Pts',(21.4951427159261,70.8839012490871,0.));
#162465=CARTESIAN_POINT('Ctrl Pts',(21.477238534096,70.8632044140112,0.));
#162466=CARTESIAN_POINT('Ctrl Pts',(21.4593764087473,70.8425182149846,0.));
#162467=CARTESIAN_POINT('Ctrl Pts',(21.4415563620114,70.8218427507506,0.));
#162468=CARTESIAN_POINT('Ctrl Pts',(21.4237784161587,70.8011781217394,0.));
#162469=CARTESIAN_POINT('Ctrl Pts',(21.4060425934598,70.780524428745,0.));
#162470=CARTESIAN_POINT('Ctrl Pts',(21.3883489160196,70.7598817714105,0.));
#162471=CARTESIAN_POINT('Ctrl Pts',(21.3706974057039,70.7392502475469,0.));
#162472=CARTESIAN_POINT('Ctrl Pts',(21.3530880842349,70.7186299539724,0.));
#162473=CARTESIAN_POINT('Ctrl Pts',(21.3355209732443,70.6980209870045,0.));
#162474=CARTESIAN_POINT('Ctrl Pts',(21.3179960943388,70.6774234430897,0.));
#162475=CARTESIAN_POINT('Ctrl Pts',(21.300513469156,70.6568374193774,0.));
#162476=CARTESIAN_POINT('Ctrl Pts',(21.2830731194183,70.6362630143047,0.));
#162477=CARTESIAN_POINT('Ctrl Pts',(21.2656750669126,70.6157003273316,0.));
#162478=CARTESIAN_POINT('Ctrl Pts',(21.2483193334675,70.5951494586957,0.));
#162479=CARTESIAN_POINT('Ctrl Pts',(21.2310059409265,70.5746105091502,0.));
#162480=CARTESIAN_POINT('Ctrl Pts',(21.2137349111208,70.5540835797283,0.));
#162481=CARTESIAN_POINT('Ctrl Pts',(21.1965062658298,70.5335687714429,0.));
#162482=CARTESIAN_POINT('Ctrl Pts',(21.1793200267846,70.5130661852955,0.));
#162483=CARTESIAN_POINT('Ctrl Pts',(21.1621762156897,70.4925759224216,0.));
#162484=CARTESIAN_POINT('Ctrl Pts',(21.1450748542336,70.4720980841939,0.));
#162485=CARTESIAN_POINT('Ctrl Pts',(21.1280159641002,70.4516327723346,0.));
#162486=CARTESIAN_POINT('Ctrl Pts',(21.1109995669747,70.4311800890402,0.));
#162487=CARTESIAN_POINT('Ctrl Pts',(21.0940256845472,70.4107401370389,0.));
#162488=CARTESIAN_POINT('Ctrl Pts',(21.0770943385141,70.3903130195265,0.));
#162489=CARTESIAN_POINT('Ctrl Pts',(21.0602055505748,70.3698988401281,0.));
#162490=CARTESIAN_POINT('Ctrl Pts',(21.0433593424266,70.3494977028498,0.));
#162491=CARTESIAN_POINT('Ctrl Pts',(21.0265557357548,70.3291097120302,0.));
#162492=CARTESIAN_POINT('Ctrl Pts',(21.0097947522218,70.3087349722973,0.));
#162493=CARTESIAN_POINT('Ctrl Pts',(20.9930764134776,70.2883735885984,0.));
#162494=CARTESIAN_POINT('Ctrl Pts',(20.9764007411652,70.2680256662224,0.));
#162495=CARTESIAN_POINT('Ctrl Pts',(20.9597677569228,70.2476913108244,0.));
#162496=CARTESIAN_POINT('Ctrl Pts',(20.9431774823831,70.2273706284472,0.));
#162497=CARTESIAN_POINT('Ctrl Pts',(20.9266299391684,70.2070637255458,0.));
#162498=CARTESIAN_POINT('Ctrl Pts',(20.9101251488943,70.1867707089854,0.));
#162499=CARTESIAN_POINT('Ctrl Pts',(20.8936631331748,70.1664916860358,0.));
#162500=CARTESIAN_POINT('Ctrl Pts',(20.8772439136206,70.1462267643647,0.));
#162501=CARTESIAN_POINT('Ctrl Pts',(20.8608675118378,70.1259760520309,0.));
#162502=CARTESIAN_POINT('Ctrl Pts',(20.8445339494187,70.1057396574747,0.));
#162503=CARTESIAN_POINT('Ctrl Pts',(20.8282432479428,70.0855176895191,0.));
#162504=CARTESIAN_POINT('Ctrl Pts',(20.8119954289848,70.0653102573803,0.));
#162505=CARTESIAN_POINT('Ctrl Pts',(20.7957905141156,70.0451174706741,0.));
#162506=CARTESIAN_POINT('Ctrl Pts',(20.7796285249022,70.024939439422,0.));
#162507=CARTESIAN_POINT('Ctrl Pts',(20.7635094829015,70.0047762740568,0.));
#162508=CARTESIAN_POINT('Ctrl Pts',(20.7474334096581,69.9846280854257,0.));
#162509=CARTESIAN_POINT('Ctrl Pts',(20.7314003267119,69.9644949847934,0.));
#162510=CARTESIAN_POINT('Ctrl Pts',(20.7154102555997,69.9443770838448,0.));
#162511=CARTESIAN_POINT('Ctrl Pts',(20.6994632178551,69.9242744946854,0.));
#162512=CARTESIAN_POINT('Ctrl Pts',(20.683559235003,69.904187329841,0.));
#162513=CARTESIAN_POINT('Ctrl Pts',(20.667698328554,69.8841157022568,0.));
#162514=CARTESIAN_POINT('Ctrl Pts',(20.6518805200129,69.8640597253045,0.));
#162515=CARTESIAN_POINT('Ctrl Pts',(20.636105830881,69.8440195127866,0.));
#162516=CARTESIAN_POINT('Ctrl Pts',(20.6203742826566,69.8239951789402,0.));
#162517=CARTESIAN_POINT('Ctrl Pts',(20.6046858968307,69.8039868384389,0.));
#162518=CARTESIAN_POINT('Ctrl Pts',(20.5890406948811,69.7839946063949,0.));
#162519=CARTESIAN_POINT('Ctrl Pts',(20.5734386982782,69.7640185983644,0.));
#162520=CARTESIAN_POINT('Ctrl Pts',(20.5578799284897,69.744058930351,0.));
#162521=CARTESIAN_POINT('Ctrl Pts',(20.5423644069799,69.7241157188083,0.));
#162522=CARTESIAN_POINT('Ctrl Pts',(20.5268921552077,69.7041890806425,0.));
#162523=CARTESIAN_POINT('Ctrl Pts',(20.5114631946184,69.6842791332115,0.));
#162524=CARTESIAN_POINT('Ctrl Pts',(20.4960775466492,69.6643859943308,0.));
#162525=CARTESIAN_POINT('Ctrl Pts',(20.4807352327339,69.6445097822792,0.));
#162526=CARTESIAN_POINT('Ctrl Pts',(20.4654362743037,69.6246506158013,0.));
#162527=CARTESIAN_POINT('Ctrl Pts',(20.4501806927851,69.6048086141113,0.));
#162528=CARTESIAN_POINT('Ctrl Pts',(20.4349685095923,69.5849838968928,0.));
#162529=CARTESIAN_POINT('Ctrl Pts',(20.41979974613,69.5651765843033,0.));
#162530=CARTESIAN_POINT('Ctrl Pts',(20.4046744237999,69.5453867969804,0.));
#162531=CARTESIAN_POINT('Ctrl Pts',(20.3895925640005,69.5256146560441,0.));
#162532=CARTESIAN_POINT('Ctrl Pts',(20.3745541881268,69.5058602831008,0.));
#162533=CARTESIAN_POINT('Ctrl Pts',(20.3595593175622,69.4861238002441,0.));
#162534=CARTESIAN_POINT('Ctrl Pts',(20.3446079736802,69.4664053300587,0.));
#162535=CARTESIAN_POINT('Ctrl Pts',(20.3297001778507,69.4467049956262,0.));
#162536=CARTESIAN_POINT('Ctrl Pts',(20.3148359514415,69.4270229205297,0.));
#162537=CARTESIAN_POINT('Ctrl Pts',(20.3000153158166,69.407359228856,0.));
#162538=CARTESIAN_POINT('Ctrl Pts',(20.2852382923299,69.3877140451975,0.));
#162539=CARTESIAN_POINT('Ctrl Pts',(20.2705049023241,69.368087494655,0.));
#162540=CARTESIAN_POINT('Ctrl Pts',(20.2558151671391,69.3484797028458,0.));
#162541=CARTESIAN_POINT('Ctrl Pts',(20.2411691081123,69.3288907959067,0.));
#162542=CARTESIAN_POINT('Ctrl Pts',(20.2265667465784,69.3093209004984,0.));
#162543=CARTESIAN_POINT('Ctrl Pts',(20.212008103862,69.2897701438059,0.));
#162544=CARTESIAN_POINT('Ctrl Pts',(20.1974932012773,69.2702386535422,0.));
#162545=CARTESIAN_POINT('Ctrl Pts',(20.1830220601348,69.2507265579554,0.));
#162546=CARTESIAN_POINT('Ctrl Pts',(20.1685947017433,69.2312339858335,0.));
#162547=CARTESIAN_POINT('Ctrl Pts',(20.1542111474087,69.2117610665076,0.));
#162548=CARTESIAN_POINT('Ctrl Pts',(20.1398714184279,69.1923079298538,0.));
#162549=CARTESIAN_POINT('Ctrl Pts',(20.1255755360872,69.1728747062963,0.));
#162550=CARTESIAN_POINT('Ctrl Pts',(20.1113235216694,69.1534615268153,0.));
#162551=CARTESIAN_POINT('Ctrl Pts',(20.0971153964557,69.1340685229514,0.));
#162552=CARTESIAN_POINT('Ctrl Pts',(20.0829511817251,69.1146958268104,0.));
#162553=CARTESIAN_POINT('Ctrl Pts',(20.068830898748,69.095343571064,0.));
#162554=CARTESIAN_POINT('Ctrl Pts',(20.0547545687842,69.0760118889535,0.));
#162555=CARTESIAN_POINT('Ctrl Pts',(20.0407222130905,69.0567009142978,0.));
#162556=CARTESIAN_POINT('Ctrl Pts',(20.0267338529223,69.0374107814984,0.));
#162557=CARTESIAN_POINT('Ctrl Pts',(20.0127895095326,69.0181416255431,0.));
#162558=CARTESIAN_POINT('Ctrl Pts',(19.9988892041666,68.9988935820084,0.));
#162559=CARTESIAN_POINT('Ctrl Pts',(19.9850329580591,68.9796667870638,0.));
#162560=CARTESIAN_POINT('Ctrl Pts',(19.9712207924428,68.9604613774802,0.));
#162561=CARTESIAN_POINT('Ctrl Pts',(19.9574527285488,68.9412774906333,0.));
#162562=CARTESIAN_POINT('Ctrl Pts',(19.9437287876066,68.9221152645095,0.));
#162563=CARTESIAN_POINT('Ctrl Pts',(19.9300489908374,68.9029748377067,0.));
#162564=CARTESIAN_POINT('Ctrl Pts',(19.9164133594525,68.8838563494393,0.));
#162565=CARTESIAN_POINT('Ctrl Pts',(19.9028219146618,68.8647599395469,0.));
#162566=CARTESIAN_POINT('Ctrl Pts',(19.8892746776739,68.8456857485002,0.));
#162567=CARTESIAN_POINT('Ctrl Pts',(19.8757716696965,68.8266339174056,0.));
#162568=CARTESIAN_POINT('Ctrl Pts',(19.8623129119293,68.8076045880065,0.));
#162569=CARTESIAN_POINT('Ctrl Pts',(19.8488984255627,68.7885979026879,0.));
#162570=CARTESIAN_POINT('Ctrl Pts',(19.8355282317858,68.7696140044851,0.));
#162571=CARTESIAN_POINT('Ctrl Pts',(19.822202351787,68.7506530370904,0.));
#162572=CARTESIAN_POINT('Ctrl Pts',(19.8089208067537,68.7317151448573,0.));
#162573=CARTESIAN_POINT('Ctrl Pts',(19.7956836178651,68.7128004728034,0.));
#162574=CARTESIAN_POINT('Ctrl Pts',(19.7824908062924,68.693909166615,0.));
#162575=CARTESIAN_POINT('Ctrl Pts',(19.7693423932066,68.6750413726575,0.));
#162576=CARTESIAN_POINT('Ctrl Pts',(19.7562383997783,68.65619723798,0.));
#162577=CARTESIAN_POINT('Ctrl Pts',(19.7431788471772,68.6373769103211,0.));
#162578=CARTESIAN_POINT('Ctrl Pts',(19.7301637565645,68.6185805381102,0.));
#162579=CARTESIAN_POINT('Ctrl Pts',(19.717193149095,68.5998082704741,0.));
#162580=CARTESIAN_POINT('Ctrl Pts',(19.7042670459233,68.5810602572474,0.));
#162581=CARTESIAN_POINT('Ctrl Pts',(19.6913854682046,68.5623366489776,0.));
#162582=CARTESIAN_POINT('Ctrl Pts',(19.6785484370929,68.543637596932,0.));
#162583=CARTESIAN_POINT('Ctrl Pts',(19.665755973734,68.5249632530994,0.));
#162584=CARTESIAN_POINT('Ctrl Pts',(19.6530080992689,68.5063137701986,0.));
#162585=CARTESIAN_POINT('Ctrl Pts',(19.6403048348396,68.4876893016863,0.));
#162586=CARTESIAN_POINT('Ctrl Pts',(19.6276462015888,68.4690900017631,0.));
#162587=CARTESIAN_POINT('Ctrl Pts',(19.6150322206577,68.4505160253777,0.));
#162588=CARTESIAN_POINT('Ctrl Pts',(19.6024629131785,68.4319675282273,0.));
#162589=CARTESIAN_POINT('Ctrl Pts',(19.5899383002803,68.4134446667695,0.));
#162590=CARTESIAN_POINT('Ctrl Pts',(19.5774584030938,68.3949475982334,0.));
#162591=CARTESIAN_POINT('Ctrl Pts',(19.5650232427516,68.3764764806287,0.));
#162592=CARTESIAN_POINT('Ctrl Pts',(19.5526328403851,68.3580314727522,0.));
#162593=CARTESIAN_POINT('Ctrl Pts',(19.540287217119,68.3396127341937,0.));
#162594=CARTESIAN_POINT('Ctrl Pts',(19.5279863940772,68.3212204253416,0.));
#162595=CARTESIAN_POINT('Ctrl Pts',(19.5157303923855,68.3028547073862,0.));
#162596=CARTESIAN_POINT('Ctrl Pts',(19.5035192331706,68.2845157423234,0.));
#162597=CARTESIAN_POINT('Ctrl Pts',(19.4913529375545,68.2662036929531,0.));
#162598=CARTESIAN_POINT('Ctrl Pts',(19.4792315266505,68.2479187228815,0.));
#162599=CARTESIAN_POINT('Ctrl Pts',(19.4671550215724,68.2296609965461,0.));
#162600=CARTESIAN_POINT('Ctrl Pts',(19.4551234434383,68.2114306792366,0.));
#162601=CARTESIAN_POINT('Ctrl Pts',(19.4431368133718,68.1932279371121,0.));
#162602=CARTESIAN_POINT('Ctrl Pts',(19.4311951524977,68.1750529372211,0.));
#162603=CARTESIAN_POINT('Ctrl Pts',(19.419298481941,68.1569058475026,0.));
#162604=CARTESIAN_POINT('Ctrl Pts',(19.4074468228293,68.1387868367668,0.));
#162605=CARTESIAN_POINT('Ctrl Pts',(19.3956401962893,68.1206960746763,0.));
#162606=CARTESIAN_POINT('Ctrl Pts',(19.3838786234425,68.1026337317298,0.));
#162607=CARTESIAN_POINT('Ctrl Pts',(19.372162125392,68.0845999792274,0.));
#162608=CARTESIAN_POINT('Ctrl Pts',(19.3604907232322,68.0665949893222,0.));
#162609=CARTESIAN_POINT('Ctrl Pts',(19.3488644380646,68.0486189351027,0.));
#162610=CARTESIAN_POINT('Ctrl Pts',(19.3372832910076,68.0306719906636,0.));
#162611=CARTESIAN_POINT('Ctrl Pts',(19.3257473032031,68.0127543311761,0.));
#162612=CARTESIAN_POINT('Ctrl Pts',(19.3142564958195,67.9948661329592,0.));
#162613=CARTESIAN_POINT('Ctrl Pts',(19.3028108900373,67.977007573346,0.));
#162614=CARTESIAN_POINT('Ctrl Pts',(19.2914105070282,67.959178830538,0.));
#162615=CARTESIAN_POINT('Ctrl Pts',(19.2800553679362,67.9413800834798,0.));
#162616=CARTESIAN_POINT('Ctrl Pts',(19.2687454938448,67.9236115116781,0.));
#162617=CARTESIAN_POINT('Ctrl Pts',(19.2574809057705,67.9058732951822,0.));
#162618=CARTESIAN_POINT('Ctrl Pts',(19.2462616247287,67.8881656149983,0.));
#162619=CARTESIAN_POINT('Ctrl Pts',(19.2350876717877,67.8704886534555,0.));
#162620=CARTESIAN_POINT('Ctrl Pts',(19.2239590681129,67.852842594517,0.));
#162621=CARTESIAN_POINT('Ctrl Pts',(19.2128758350336,67.8352276242856,0.));
#162622=CARTESIAN_POINT('Ctrl Pts',(19.2018379939918,67.817643930658,0.));
#162623=CARTESIAN_POINT('Ctrl Pts',(19.1908455664089,67.8000917023896,0.));
#162624=CARTESIAN_POINT('Ctrl Pts',(19.1798985735687,67.7825711283092,0.));
#162625=CARTESIAN_POINT('Ctrl Pts',(19.1689970364958,67.7650823965156,0.));
#162626=CARTESIAN_POINT('Ctrl Pts',(19.1581409758111,67.7476256934493,0.));
#162627=CARTESIAN_POINT('Ctrl Pts',(19.1473304119968,67.730201205663,0.));
#162628=CARTESIAN_POINT('Ctrl Pts',(19.1365653657097,67.7128091219372,0.));
#162629=CARTESIAN_POINT('Ctrl Pts',(19.1258458580343,67.6954496350053,0.));
#162630=CARTESIAN_POINT('Ctrl Pts',(19.115171910845,67.6781229440535,0.));
#162631=CARTESIAN_POINT('Ctrl Pts',(19.1045435468344,67.6608292549412,0.));
#162632=CARTESIAN_POINT('Ctrl Pts',(19.0939607887491,67.6435687749803,0.));
#162633=CARTESIAN_POINT('Ctrl Pts',(19.0834236587115,67.6263417083414,0.));
#162634=CARTESIAN_POINT('Ctrl Pts',(19.0729321776286,67.6091482520558,0.));
#162635=CARTESIAN_POINT('Ctrl Pts',(19.0624863642425,67.5919885896278,0.));
#162636=CARTESIAN_POINT('Ctrl Pts',(19.0520862360413,67.5748628972035,0.));
#162637=CARTESIAN_POINT('Ctrl Pts',(19.0417318110721,67.5577713558248,0.));
#162638=CARTESIAN_POINT('Ctrl Pts',(19.0314231093923,67.5407141612881,0.));
#162639=CARTESIAN_POINT('Ctrl Pts',(19.0211601548222,67.5236915360253,0.));
#162640=CARTESIAN_POINT('Ctrl Pts',(19.0109429761274,67.5067037372177,0.));
#162641=CARTESIAN_POINT('Ctrl Pts',(19.0007716032784,67.4897510316692,0.));
#162642=CARTESIAN_POINT('Ctrl Pts',(18.9906460638607,67.4728336719559,0.));
#162643=CARTESIAN_POINT('Ctrl Pts',(18.9805663798466,67.4559518744714,0.));
#162644=CARTESIAN_POINT('Ctrl Pts',(18.9705325631772,67.4391057908687,0.));
#162645=CARTESIAN_POINT('Ctrl Pts',(18.9605446161078,67.4222955062385,0.));
#162646=CARTESIAN_POINT('Ctrl Pts',(18.9525909518002,67.4088759498287,0.));
#162647=CARTESIAN_POINT('Ctrl Pts',(18.9466463414354,67.398827414689,0.));
#162648=CARTESIAN_POINT('Ctrl Pts',(18.942692439874,67.3921355608417,0.));
#162649=CARTESIAN_POINT('Ctrl Pts',(18.9407177820969,67.3887914263119,0.));
#162650=CARTESIAN_POINT('Ctrl Pts',(27.9316983239472,69.065695021045,0.));
#162651=CARTESIAN_POINT('Ctrl Pts',(27.9316983239472,69.065695021045,12.));
#162652=CARTESIAN_POINT('Ctrl Pts',(27.9276214070631,69.0618620884721,0.));
#162653=CARTESIAN_POINT('Ctrl Pts',(27.9276214070631,69.0618620884721,12.));
#162654=CARTESIAN_POINT('Ctrl Pts',(27.9194718099003,69.0541967851028,0.));
#162655=CARTESIAN_POINT('Ctrl Pts',(27.9194718099003,69.0541967851028,12.));
#162656=CARTESIAN_POINT('Ctrl Pts',(27.9072601239722,69.0427005153791,0.));
#162657=CARTESIAN_POINT('Ctrl Pts',(27.9072601239722,69.0427005153791,12.));
#162658=CARTESIAN_POINT('Ctrl Pts',(27.8910032967339,69.0273755265383,0.));
#162659=CARTESIAN_POINT('Ctrl Pts',(27.8910032967339,69.0273755265383,12.));
#162660=CARTESIAN_POINT('Ctrl Pts',(27.8707246380956,69.0082249138598,0.));
#162661=CARTESIAN_POINT('Ctrl Pts',(27.8707246380956,69.0082249138598,12.));
#162662=CARTESIAN_POINT('Ctrl Pts',(27.8504883674058,68.9890799392213,0.));
#162663=CARTESIAN_POINT('Ctrl Pts',(27.8504883674058,68.9890799392213,12.));
#162664=CARTESIAN_POINT('Ctrl Pts',(27.8302945019976,68.9699406311389,0.));
#162665=CARTESIAN_POINT('Ctrl Pts',(27.8302945019976,68.9699406311389,12.));
#162666=CARTESIAN_POINT('Ctrl Pts',(27.8101430638071,68.9508070357658,0.));
#162667=CARTESIAN_POINT('Ctrl Pts',(27.8101430638071,68.9508070357658,12.));
#162668=CARTESIAN_POINT('Ctrl Pts',(27.7900340793689,68.9316792225946,0.));
#162669=CARTESIAN_POINT('Ctrl Pts',(27.7900340793689,68.9316792225946,12.));
#162670=CARTESIAN_POINT('Ctrl Pts',(27.7699675790571,68.9125572825694,0.));
#162671=CARTESIAN_POINT('Ctrl Pts',(27.7699675790571,68.9125572825694,12.));
#162672=CARTESIAN_POINT('Ctrl Pts',(27.7499435957525,68.8934413203759,0.));
#162673=CARTESIAN_POINT('Ctrl Pts',(27.7499435957525,68.8934413203759,12.));
#162674=CARTESIAN_POINT('Ctrl Pts',(27.7299621636566,68.8743314483369,0.));
#162675=CARTESIAN_POINT('Ctrl Pts',(27.7299621636566,68.8743314483369,12.));
#162676=CARTESIAN_POINT('Ctrl Pts',(27.7100233170737,68.85522777982,0.));
#162677=CARTESIAN_POINT('Ctrl Pts',(27.7100233170737,68.85522777982,12.));
#162678=CARTESIAN_POINT('Ctrl Pts',(27.6901270891241,68.8361304224467,0.));
#162679=CARTESIAN_POINT('Ctrl Pts',(27.6901270891241,68.8361304224467,12.));
#162680=CARTESIAN_POINT('Ctrl Pts',(27.6702735107121,68.81703947259,0.));
#162681=CARTESIAN_POINT('Ctrl Pts',(27.6702735107121,68.81703947259,12.));
#162682=CARTESIAN_POINT('Ctrl Pts',(27.6504626112666,68.7979550191872,0.));
#162683=CARTESIAN_POINT('Ctrl Pts',(27.6504626112666,68.7979550191872,12.));
#162684=CARTESIAN_POINT('Ctrl Pts',(27.6306944192737,68.7788771464713,0.));
#162685=CARTESIAN_POINT('Ctrl Pts',(27.6306944192737,68.7788771464713,12.));
#162686=CARTESIAN_POINT('Ctrl Pts',(27.6109689629029,68.7598059372129,0.));
#162687=CARTESIAN_POINT('Ctrl Pts',(27.6109689629029,68.7598059372129,12.));
#162688=CARTESIAN_POINT('Ctrl Pts',(27.5912862705468,68.740741475526,0.));
#162689=CARTESIAN_POINT('Ctrl Pts',(27.5912862705468,68.740741475526,12.));
#162690=CARTESIAN_POINT('Ctrl Pts',(27.5716463715004,68.7216838504218,0.));
#162691=CARTESIAN_POINT('Ctrl Pts',(27.5716463715004,68.7216838504218,12.));
#162692=CARTESIAN_POINT('Ctrl Pts',(27.5520492958906,68.7026331554296,0.));
#162693=CARTESIAN_POINT('Ctrl Pts',(27.5520492958906,68.7026331554296,12.));
#162694=CARTESIAN_POINT('Ctrl Pts',(27.5324950743706,68.6835894869882,0.));
#162695=CARTESIAN_POINT('Ctrl Pts',(27.5324950743706,68.6835894869882,12.));
#162696=CARTESIAN_POINT('Ctrl Pts',(27.5129837378791,68.6645529432045,0.));
#162697=CARTESIAN_POINT('Ctrl Pts',(27.5129837378791,68.6645529432045,12.));
#162698=CARTESIAN_POINT('Ctrl Pts',(27.4935153173868,68.645523622548,0.));
#162699=CARTESIAN_POINT('Ctrl Pts',(27.4935153173868,68.645523622548,12.));
#162700=CARTESIAN_POINT('Ctrl Pts',(27.4740898435988,68.6265016223561,0.));
#162701=CARTESIAN_POINT('Ctrl Pts',(27.4740898435988,68.6265016223561,12.));
#162702=CARTESIAN_POINT('Ctrl Pts',(27.4547073468226,68.6074870381619,0.));
#162703=CARTESIAN_POINT('Ctrl Pts',(27.4547073468226,68.6074870381619,12.));
#162704=CARTESIAN_POINT('Ctrl Pts',(27.435367857136,68.5884799645218,0.));
#162705=CARTESIAN_POINT('Ctrl Pts',(27.435367857136,68.5884799645218,12.));
#162706=CARTESIAN_POINT('Ctrl Pts',(27.4160714044831,68.5694804955014,0.));
#162707=CARTESIAN_POINT('Ctrl Pts',(27.4160714044831,68.5694804955014,12.));
#162708=CARTESIAN_POINT('Ctrl Pts',(27.3968180187941,68.5504887252975,0.));
#162709=CARTESIAN_POINT('Ctrl Pts',(27.3968180187941,68.5504887252975,12.));
#162710=CARTESIAN_POINT('Ctrl Pts',(27.3776077300914,68.5315047488035,0.));
#162711=CARTESIAN_POINT('Ctrl Pts',(27.3776077300914,68.5315047488035,12.));
#162712=CARTESIAN_POINT('Ctrl Pts',(27.3584405685941,68.5125286621888,0.));
#162713=CARTESIAN_POINT('Ctrl Pts',(27.3584405685941,68.5125286621888,12.));
#162714=CARTESIAN_POINT('Ctrl Pts',(27.3393165646748,68.4935605626362,0.));
#162715=CARTESIAN_POINT('Ctrl Pts',(27.3393165646748,68.4935605626362,12.));
#162716=CARTESIAN_POINT('Ctrl Pts',(27.3202357488153,68.4746005480993,0.));
#162717=CARTESIAN_POINT('Ctrl Pts',(27.3202357488153,68.4746005480993,12.));
#162718=CARTESIAN_POINT('Ctrl Pts',(27.301198151557,68.455648717044,0.));
#162719=CARTESIAN_POINT('Ctrl Pts',(27.301198151557,68.455648717044,12.));
#162720=CARTESIAN_POINT('Ctrl Pts',(27.2822038034539,68.4367051682166,0.));
#162721=CARTESIAN_POINT('Ctrl Pts',(27.2822038034539,68.4367051682166,12.));
#162722=CARTESIAN_POINT('Ctrl Pts',(27.2632527350062,68.4177700003471,0.));
#162723=CARTESIAN_POINT('Ctrl Pts',(27.2632527350062,68.4177700003471,12.));
#162724=CARTESIAN_POINT('Ctrl Pts',(27.2443449766654,68.398843312159,0.));
#162725=CARTESIAN_POINT('Ctrl Pts',(27.2443449766654,68.398843312159,12.));
#162726=CARTESIAN_POINT('Ctrl Pts',(27.2254805588677,68.379925202511,0.));
#162727=CARTESIAN_POINT('Ctrl Pts',(27.2254805588677,68.379925202511,12.));
#162728=CARTESIAN_POINT('Ctrl Pts',(27.2066595120544,68.3610157704999,0.));
#162729=CARTESIAN_POINT('Ctrl Pts',(27.2066595120544,68.3610157704999,12.));
#162730=CARTESIAN_POINT('Ctrl Pts',(27.1878818666925,68.3421151155708,0.));
#162731=CARTESIAN_POINT('Ctrl Pts',(27.1878818666925,68.3421151155708,12.));
#162732=CARTESIAN_POINT('Ctrl Pts',(27.1691476532917,68.3232233376415,0.));
#162733=CARTESIAN_POINT('Ctrl Pts',(27.1691476532917,68.3232233376415,12.));
#162734=CARTESIAN_POINT('Ctrl Pts',(27.150456902413,68.3043405371589,0.));
#162735=CARTESIAN_POINT('Ctrl Pts',(27.150456902413,68.3043405371589,12.));
#162736=CARTESIAN_POINT('Ctrl Pts',(27.1318096446643,68.285466815035,0.));
#162737=CARTESIAN_POINT('Ctrl Pts',(27.1318096446643,68.285466815035,12.));
#162738=CARTESIAN_POINT('Ctrl Pts',(27.1132059106938,68.2666022726094,0.));
#162739=CARTESIAN_POINT('Ctrl Pts',(27.1132059106938,68.2666022726094,12.));
#162740=CARTESIAN_POINT('Ctrl Pts',(27.0946457311813,68.2477470116014,0.));
#162741=CARTESIAN_POINT('Ctrl Pts',(27.0946457311813,68.2477470116014,12.));
#162742=CARTESIAN_POINT('Ctrl Pts',(27.076129136823,68.2289011340624,0.));
#162743=CARTESIAN_POINT('Ctrl Pts',(27.076129136823,68.2289011340624,12.));
#162744=CARTESIAN_POINT('Ctrl Pts',(27.0576561583179,68.2100647423345,0.));
#162745=CARTESIAN_POINT('Ctrl Pts',(27.0576561583179,68.2100647423345,12.));
#162746=CARTESIAN_POINT('Ctrl Pts',(27.0392268263804,68.1912379390787,0.));
#162747=CARTESIAN_POINT('Ctrl Pts',(27.0392268263804,68.1912379390787,12.));
#162748=CARTESIAN_POINT('Ctrl Pts',(27.0208411717477,68.1724208272967,0.));
#162749=CARTESIAN_POINT('Ctrl Pts',(27.0208411717477,68.1724208272967,12.));
#162750=CARTESIAN_POINT('Ctrl Pts',(27.0024992251839,68.1536135103558,0.));
#162751=CARTESIAN_POINT('Ctrl Pts',(27.0024992251839,68.1536135103558,12.));
#162752=CARTESIAN_POINT('Ctrl Pts',(26.9842010174818,68.13481609201,0.));
#162753=CARTESIAN_POINT('Ctrl Pts',(26.9842010174818,68.13481609201,12.));
#162754=CARTESIAN_POINT('Ctrl Pts',(26.9659465794596,68.1160286764244,0.));
#162755=CARTESIAN_POINT('Ctrl Pts',(26.9659465794596,68.1160286764244,12.));
#162756=CARTESIAN_POINT('Ctrl Pts',(26.9477359419646,68.0972513681739,0.));
#162757=CARTESIAN_POINT('Ctrl Pts',(26.9477359419646,68.0972513681739,12.));
#162758=CARTESIAN_POINT('Ctrl Pts',(26.9295691358775,68.0784842722362,0.));
#162759=CARTESIAN_POINT('Ctrl Pts',(26.9295691358775,68.0784842722362,12.));
#162760=CARTESIAN_POINT('Ctrl Pts',(26.9114461921108,68.0597274939857,0.));
#162761=CARTESIAN_POINT('Ctrl Pts',(26.9114461921108,68.0597274939857,12.));
#162762=CARTESIAN_POINT('Ctrl Pts',(26.8933671416064,68.0409811391872,0.));
#162763=CARTESIAN_POINT('Ctrl Pts',(26.8933671416064,68.0409811391872,12.));
#162764=CARTESIAN_POINT('Ctrl Pts',(26.8753320153255,68.0222453139862,0.));
#162765=CARTESIAN_POINT('Ctrl Pts',(26.8753320153255,68.0222453139862,12.));
#162766=CARTESIAN_POINT('Ctrl Pts',(26.85734084425,68.0035201249108,0.));
#162767=CARTESIAN_POINT('Ctrl Pts',(26.85734084425,68.0035201249108,12.));
#162768=CARTESIAN_POINT('Ctrl Pts',(26.8393936593914,67.9848056788814,0.));
#162769=CARTESIAN_POINT('Ctrl Pts',(26.8393936593914,67.9848056788814,12.));
#162770=CARTESIAN_POINT('Ctrl Pts',(26.8214904917921,67.9661020832165,0.));
#162771=CARTESIAN_POINT('Ctrl Pts',(26.8214904917921,67.9661020832165,12.));
#162772=CARTESIAN_POINT('Ctrl Pts',(26.8036313725262,67.9474094456395,0.));
#162773=CARTESIAN_POINT('Ctrl Pts',(26.8036313725262,67.9474094456395,12.));
#162774=CARTESIAN_POINT('Ctrl Pts',(26.7858163326932,67.9287278742839,0.));
#162775=CARTESIAN_POINT('Ctrl Pts',(26.7858163326932,67.9287278742839,12.));
#162776=CARTESIAN_POINT('Ctrl Pts',(26.7680454034168,67.9100574776974,0.));
#162777=CARTESIAN_POINT('Ctrl Pts',(26.7680454034168,67.9100574776974,12.));
#162778=CARTESIAN_POINT('Ctrl Pts',(26.7503186158523,67.8913983648441,0.));
#162779=CARTESIAN_POINT('Ctrl Pts',(26.7503186158523,67.8913983648441,12.));
#162780=CARTESIAN_POINT('Ctrl Pts',(26.7326360011886,67.8727506451068,0.));
#162781=CARTESIAN_POINT('Ctrl Pts',(26.7326360011886,67.8727506451068,12.));
#162782=CARTESIAN_POINT('Ctrl Pts',(26.7149975906478,67.8541144282875,0.));
#162783=CARTESIAN_POINT('Ctrl Pts',(26.7149975906478,67.8541144282875,12.));
#162784=CARTESIAN_POINT('Ctrl Pts',(26.6974034154802,67.8354898246079,0.));
#162785=CARTESIAN_POINT('Ctrl Pts',(26.6974034154802,67.8354898246079,12.));
#162786=CARTESIAN_POINT('Ctrl Pts',(26.6798535069586,67.8168769447086,0.));
#162787=CARTESIAN_POINT('Ctrl Pts',(26.6798535069586,67.8168769447086,12.));
#162788=CARTESIAN_POINT('Ctrl Pts',(26.6623478963867,67.7982758996557,0.));
#162789=CARTESIAN_POINT('Ctrl Pts',(26.6623478963867,67.7982758996557,12.));
#162790=CARTESIAN_POINT('Ctrl Pts',(26.6448866151027,67.7796868009447,0.));
#162791=CARTESIAN_POINT('Ctrl Pts',(26.6448866151027,67.7796868009447,12.));
#162792=CARTESIAN_POINT('Ctrl Pts',(26.6274696944793,67.7611097605042,0.));
#162793=CARTESIAN_POINT('Ctrl Pts',(26.6274696944793,67.7611097605042,12.));
#162794=CARTESIAN_POINT('Ctrl Pts',(26.6100971659204,67.7425448906983,0.));
#162795=CARTESIAN_POINT('Ctrl Pts',(26.6100971659204,67.7425448906983,12.));
#162796=CARTESIAN_POINT('Ctrl Pts',(26.5927690608546,67.7239923043295,0.));
#162797=CARTESIAN_POINT('Ctrl Pts',(26.5927690608546,67.7239923043295,12.));
#162798=CARTESIAN_POINT('Ctrl Pts',(26.5754854107422,67.7054521146427,0.));
#162799=CARTESIAN_POINT('Ctrl Pts',(26.5754854107422,67.7054521146427,12.));
#162800=CARTESIAN_POINT('Ctrl Pts',(26.5582462470794,67.6869244353292,0.));
#162801=CARTESIAN_POINT('Ctrl Pts',(26.5582462470794,67.6869244353292,12.));
#162802=CARTESIAN_POINT('Ctrl Pts',(26.5410516013984,67.6684093805288,0.));
#162803=CARTESIAN_POINT('Ctrl Pts',(26.5410516013984,67.6684093805288,12.));
#162804=CARTESIAN_POINT('Ctrl Pts',(26.5239015052655,67.6499070648323,0.));
#162805=CARTESIAN_POINT('Ctrl Pts',(26.5239015052655,67.6499070648323,12.));
#162806=CARTESIAN_POINT('Ctrl Pts',(26.506795990273,67.6314176032823,0.));
#162807=CARTESIAN_POINT('Ctrl Pts',(26.506795990273,67.6314176032823,12.));
#162808=CARTESIAN_POINT('Ctrl Pts',(26.4897350880446,67.6129411113774,0.));
#162809=CARTESIAN_POINT('Ctrl Pts',(26.4897350880446,67.6129411113774,12.));
#162810=CARTESIAN_POINT('Ctrl Pts',(26.4727188302415,67.5944777050782,0.));
#162811=CARTESIAN_POINT('Ctrl Pts',(26.4727188302415,67.5944777050782,12.));
#162812=CARTESIAN_POINT('Ctrl Pts',(26.4557472485622,67.5760275008096,0.));
#162813=CARTESIAN_POINT('Ctrl Pts',(26.4557472485622,67.5760275008096,12.));
#162814=CARTESIAN_POINT('Ctrl Pts',(26.4388203747422,67.5575906154648,0.));
#162815=CARTESIAN_POINT('Ctrl Pts',(26.4388203747422,67.5575906154648,12.));
#162816=CARTESIAN_POINT('Ctrl Pts',(26.4219382405452,67.5391671664055,0.));
#162817=CARTESIAN_POINT('Ctrl Pts',(26.4219382405452,67.5391671664055,12.));
#162818=CARTESIAN_POINT('Ctrl Pts',(26.4051008777668,67.5207572714666,0.));
#162819=CARTESIAN_POINT('Ctrl Pts',(26.4051008777668,67.5207572714666,12.));
#162820=CARTESIAN_POINT('Ctrl Pts',(26.3883083182417,67.5023610489611,0.));
#162821=CARTESIAN_POINT('Ctrl Pts',(26.3883083182417,67.5023610489611,12.));
#162822=CARTESIAN_POINT('Ctrl Pts',(26.3715605938432,67.4839786176833,0.));
#162823=CARTESIAN_POINT('Ctrl Pts',(26.3715605938432,67.4839786176833,12.));
#162824=CARTESIAN_POINT('Ctrl Pts',(26.3548577364835,67.4656100969121,0.));
#162825=CARTESIAN_POINT('Ctrl Pts',(26.3548577364835,67.4656100969121,12.));
#162826=CARTESIAN_POINT('Ctrl Pts',(26.3381997781059,67.4472556064127,0.));
#162827=CARTESIAN_POINT('Ctrl Pts',(26.3381997781059,67.4472556064127,12.));
#162828=CARTESIAN_POINT('Ctrl Pts',(26.3215867506864,67.4289152664406,0.));
#162829=CARTESIAN_POINT('Ctrl Pts',(26.3215867506864,67.4289152664406,12.));
#162830=CARTESIAN_POINT('Ctrl Pts',(26.305018686241,67.4105891977465,0.));
#162831=CARTESIAN_POINT('Ctrl Pts',(26.305018686241,67.4105891977465,12.));
#162832=CARTESIAN_POINT('Ctrl Pts',(26.288495616827,67.392277521581,0.));
#162833=CARTESIAN_POINT('Ctrl Pts',(26.288495616827,67.392277521581,12.));
#162834=CARTESIAN_POINT('Ctrl Pts',(26.2720175745422,67.3739803596967,0.));
#162835=CARTESIAN_POINT('Ctrl Pts',(26.2720175745422,67.3739803596967,12.));
#162836=CARTESIAN_POINT('Ctrl Pts',(26.255584591518,67.3556978343506,0.));
#162837=CARTESIAN_POINT('Ctrl Pts',(26.255584591518,67.3556978343506,12.));
#162838=CARTESIAN_POINT('Ctrl Pts',(26.2391966999192,67.3374300683076,0.));
#162839=CARTESIAN_POINT('Ctrl Pts',(26.2391966999192,67.3374300683076,12.));
#162840=CARTESIAN_POINT('Ctrl Pts',(26.2228539319527,67.3191771848468,0.));
#162841=CARTESIAN_POINT('Ctrl Pts',(26.2228539319527,67.3191771848468,12.));
#162842=CARTESIAN_POINT('Ctrl Pts',(26.2065563198684,67.3009393077654,0.));
#162843=CARTESIAN_POINT('Ctrl Pts',(26.2065563198684,67.3009393077654,12.));
#162844=CARTESIAN_POINT('Ctrl Pts',(26.1903038959589,67.2827165613828,0.));
#162845=CARTESIAN_POINT('Ctrl Pts',(26.1903038959589,67.2827165613828,12.));
#162846=CARTESIAN_POINT('Ctrl Pts',(26.1740966925527,67.2645090705414,0.));
#162847=CARTESIAN_POINT('Ctrl Pts',(26.1740966925527,67.2645090705414,12.));
#162848=CARTESIAN_POINT('Ctrl Pts',(26.1579347420135,67.2463169606105,0.));
#162849=CARTESIAN_POINT('Ctrl Pts',(26.1579347420135,67.2463169606105,12.));
#162850=CARTESIAN_POINT('Ctrl Pts',(26.1418180767486,67.228140357493,0.));
#162851=CARTESIAN_POINT('Ctrl Pts',(26.1418180767486,67.228140357493,12.));
#162852=CARTESIAN_POINT('Ctrl Pts',(26.1257467292102,67.2099793876295,0.));
#162853=CARTESIAN_POINT('Ctrl Pts',(26.1257467292102,67.2099793876295,12.));
#162854=CARTESIAN_POINT('Ctrl Pts',(26.109720731895,67.191834178002,0.));
#162855=CARTESIAN_POINT('Ctrl Pts',(26.109720731895,67.191834178002,12.));
#162856=CARTESIAN_POINT('Ctrl Pts',(26.0937401173385,67.1737048561364,0.));
#162857=CARTESIAN_POINT('Ctrl Pts',(26.0937401173385,67.1737048561364,12.));
#162858=CARTESIAN_POINT('Ctrl Pts',(26.0778049181129,67.1555915501052,0.));
#162859=CARTESIAN_POINT('Ctrl Pts',(26.0778049181129,67.1555915501052,12.));
#162860=CARTESIAN_POINT('Ctrl Pts',(26.061915166836,67.1374943885353,0.));
#162861=CARTESIAN_POINT('Ctrl Pts',(26.061915166836,67.1374943885353,12.));
#162862=CARTESIAN_POINT('Ctrl Pts',(26.0460708961724,67.1194135006122,0.));
#162863=CARTESIAN_POINT('Ctrl Pts',(26.0460708961724,67.1194135006122,12.));
#162864=CARTESIAN_POINT('Ctrl Pts',(26.030272138834,67.101349016084,0.));
#162865=CARTESIAN_POINT('Ctrl Pts',(26.030272138834,67.101349016084,12.));
#162866=CARTESIAN_POINT('Ctrl Pts',(26.0145189275732,67.083301065264,0.));
#162867=CARTESIAN_POINT('Ctrl Pts',(26.0145189275732,67.083301065264,12.));
#162868=CARTESIAN_POINT('Ctrl Pts',(25.9988112951818,67.0652697790335,0.));
#162869=CARTESIAN_POINT('Ctrl Pts',(25.9988112951818,67.0652697790335,12.));
#162870=CARTESIAN_POINT('Ctrl Pts',(25.9831492744988,67.0472552888495,0.));
#162871=CARTESIAN_POINT('Ctrl Pts',(25.9831492744988,67.0472552888495,12.));
#162872=CARTESIAN_POINT('Ctrl Pts',(25.9675328984123,67.0292577267495,0.));
#162873=CARTESIAN_POINT('Ctrl Pts',(25.9675328984123,67.0292577267495,12.));
#162874=CARTESIAN_POINT('Ctrl Pts',(25.9519621998598,67.0112772253553,0.));
#162875=CARTESIAN_POINT('Ctrl Pts',(25.9519621998598,67.0112772253553,12.));
#162876=CARTESIAN_POINT('Ctrl Pts',(25.9364372118216,66.993313917876,0.));
#162877=CARTESIAN_POINT('Ctrl Pts',(25.9364372118216,66.993313917876,12.));
#162878=CARTESIAN_POINT('Ctrl Pts',(25.9209579673198,66.9753679381122,0.));
#162879=CARTESIAN_POINT('Ctrl Pts',(25.9209579673198,66.9753679381122,12.));
#162880=CARTESIAN_POINT('Ctrl Pts',(25.9055244994266,66.9574394204635,0.));
#162881=CARTESIAN_POINT('Ctrl Pts',(25.9055244994266,66.9574394204635,12.));
#162882=CARTESIAN_POINT('Ctrl Pts',(25.8901368412655,66.9395284999327,0.));
#162883=CARTESIAN_POINT('Ctrl Pts',(25.8901368412655,66.9395284999327,12.));
#162884=CARTESIAN_POINT('Ctrl Pts',(25.8747950260114,66.9216353121308,0.));
#162885=CARTESIAN_POINT('Ctrl Pts',(25.8747950260114,66.9216353121308,12.));
#162886=CARTESIAN_POINT('Ctrl Pts',(25.8594990868844,66.9037599932787,0.));
#162887=CARTESIAN_POINT('Ctrl Pts',(25.8594990868844,66.9037599932787,12.));
#162888=CARTESIAN_POINT('Ctrl Pts',(25.8442490571486,66.8859026802123,0.));
#162889=CARTESIAN_POINT('Ctrl Pts',(25.8442490571486,66.8859026802123,12.));
#162890=CARTESIAN_POINT('Ctrl Pts',(25.8290449701206,66.8680635103907,0.));
#162891=CARTESIAN_POINT('Ctrl Pts',(25.8290449701206,66.8680635103907,12.));
#162892=CARTESIAN_POINT('Ctrl Pts',(25.8138868591715,66.8502426219015,0.));
#162893=CARTESIAN_POINT('Ctrl Pts',(25.8138868591715,66.8502426219015,12.));
#162894=CARTESIAN_POINT('Ctrl Pts',(25.7987747577264,66.8324401534657,0.));
#162895=CARTESIAN_POINT('Ctrl Pts',(25.7987747577264,66.8324401534657,12.));
#162896=CARTESIAN_POINT('Ctrl Pts',(25.783708699258,66.8146562444397,0.));
#162897=CARTESIAN_POINT('Ctrl Pts',(25.783708699258,66.8146562444397,12.));
#162898=CARTESIAN_POINT('Ctrl Pts',(25.7686887172859,66.7968910348199,0.));
#162899=CARTESIAN_POINT('Ctrl Pts',(25.7686887172859,66.7968910348199,12.));
#162900=CARTESIAN_POINT('Ctrl Pts',(25.7537148453848,66.7791446652505,0.));
#162901=CARTESIAN_POINT('Ctrl Pts',(25.7537148453848,66.7791446652505,12.));
#162902=CARTESIAN_POINT('Ctrl Pts',(25.7387871171861,66.7614172770302,0.));
#162903=CARTESIAN_POINT('Ctrl Pts',(25.7387871171861,66.7614172770302,12.));
#162904=CARTESIAN_POINT('Ctrl Pts',(25.7239055663778,66.7437090121168,0.));
#162905=CARTESIAN_POINT('Ctrl Pts',(25.7239055663778,66.7437090121168,12.));
#162906=CARTESIAN_POINT('Ctrl Pts',(25.7090702266976,66.72602001313,0.));
#162907=CARTESIAN_POINT('Ctrl Pts',(25.7090702266976,66.72602001313,12.));
#162908=CARTESIAN_POINT('Ctrl Pts',(25.6942811319337,66.7083504233566,0.));
#162909=CARTESIAN_POINT('Ctrl Pts',(25.6942811319337,66.7083504233566,12.));
#162910=CARTESIAN_POINT('Ctrl Pts',(25.6795383159329,66.6907003867599,0.));
#162911=CARTESIAN_POINT('Ctrl Pts',(25.6795383159329,66.6907003867599,12.));
#162912=CARTESIAN_POINT('Ctrl Pts',(25.6648418126016,66.6730700479844,0.));
#162913=CARTESIAN_POINT('Ctrl Pts',(25.6648418126016,66.6730700479844,12.));
#162914=CARTESIAN_POINT('Ctrl Pts',(25.650191655905,66.6554595523611,0.));
#162915=CARTESIAN_POINT('Ctrl Pts',(25.650191655905,66.6554595523611,12.));
#162916=CARTESIAN_POINT('Ctrl Pts',(25.6355878798605,66.6378690459105,0.));
#162917=CARTESIAN_POINT('Ctrl Pts',(25.6355878798605,66.6378690459105,12.));
#162918=CARTESIAN_POINT('Ctrl Pts',(25.6210305185394,66.6202986753482,0.));
#162919=CARTESIAN_POINT('Ctrl Pts',(25.6210305185394,66.6202986753482,12.));
#162920=CARTESIAN_POINT('Ctrl Pts',(25.606519606075,66.6027485880947,0.));
#162921=CARTESIAN_POINT('Ctrl Pts',(25.606519606075,66.6027485880947,12.));
#162922=CARTESIAN_POINT('Ctrl Pts',(25.5920551766629,66.5852189322811,0.));
#162923=CARTESIAN_POINT('Ctrl Pts',(25.5920551766629,66.5852189322811,12.));
#162924=CARTESIAN_POINT('Ctrl Pts',(25.5776372645605,66.5677098567551,0.));
#162925=CARTESIAN_POINT('Ctrl Pts',(25.5776372645605,66.5677098567551,12.));
#162926=CARTESIAN_POINT('Ctrl Pts',(25.5632659040797,66.5502215110843,0.));
#162927=CARTESIAN_POINT('Ctrl Pts',(25.5632659040797,66.5502215110843,12.));
#162928=CARTESIAN_POINT('Ctrl Pts',(25.5489411295916,66.5327540455639,0.));
#162929=CARTESIAN_POINT('Ctrl Pts',(25.5489411295916,66.5327540455639,12.));
#162930=CARTESIAN_POINT('Ctrl Pts',(25.5346629755322,66.5153076112237,0.));
#162931=CARTESIAN_POINT('Ctrl Pts',(25.5346629755322,66.5153076112237,12.));
#162932=CARTESIAN_POINT('Ctrl Pts',(25.5204314764033,66.4978823598352,0.));
#162933=CARTESIAN_POINT('Ctrl Pts',(25.5204314764033,66.4978823598352,12.));
#162934=CARTESIAN_POINT('Ctrl Pts',(25.5062466667703,66.4804784439146,0.));
#162935=CARTESIAN_POINT('Ctrl Pts',(25.5062466667703,66.4804784439146,12.));
#162936=CARTESIAN_POINT('Ctrl Pts',(25.4921085812548,66.463096016725,0.));
#162937=CARTESIAN_POINT('Ctrl Pts',(25.4921085812548,66.463096016725,12.));
#162938=CARTESIAN_POINT('Ctrl Pts',(25.4780172545418,66.445735232287,0.));
#162939=CARTESIAN_POINT('Ctrl Pts',(25.4780172545418,66.445735232287,12.));
#162940=CARTESIAN_POINT('Ctrl Pts',(25.463972721385,66.4283962453899,0.));
#162941=CARTESIAN_POINT('Ctrl Pts',(25.463972721385,66.4283962453899,12.));
#162942=CARTESIAN_POINT('Ctrl Pts',(25.4499750166079,66.4110792116,0.));
#162943=CARTESIAN_POINT('Ctrl Pts',(25.4499750166079,66.4110792116,12.));
#162944=CARTESIAN_POINT('Ctrl Pts',(25.4360241751017,66.3937842872684,0.));
#162945=CARTESIAN_POINT('Ctrl Pts',(25.4360241751017,66.3937842872684,12.));
#162946=CARTESIAN_POINT('Ctrl Pts',(25.4221202318198,66.3765116295364,0.));
#162947=CARTESIAN_POINT('Ctrl Pts',(25.4221202318198,66.3765116295364,12.));
#162948=CARTESIAN_POINT('Ctrl Pts',(25.4082632217846,66.3592613963407,0.));
#162949=CARTESIAN_POINT('Ctrl Pts',(25.4082632217846,66.3592613963407,12.));
#162950=CARTESIAN_POINT('Ctrl Pts',(25.39445318009,66.3420337464176,0.));
#162951=CARTESIAN_POINT('Ctrl Pts',(25.39445318009,66.3420337464176,12.));
#162952=CARTESIAN_POINT('Ctrl Pts',(25.3806901419012,66.3248288393046,0.));
#162953=CARTESIAN_POINT('Ctrl Pts',(25.3806901419012,66.3248288393046,12.));
#162954=CARTESIAN_POINT('Ctrl Pts',(25.366974142449,66.3076468353417,0.));
#162955=CARTESIAN_POINT('Ctrl Pts',(25.366974142449,66.3076468353417,12.));
#162956=CARTESIAN_POINT('Ctrl Pts',(25.3533052170253,66.2904878956721,0.));
#162957=CARTESIAN_POINT('Ctrl Pts',(25.3533052170253,66.2904878956721,12.));
#162958=CARTESIAN_POINT('Ctrl Pts',(25.3396834009954,66.2733521822675,0.));
#162959=CARTESIAN_POINT('Ctrl Pts',(25.3396834009954,66.2733521822675,12.));
#162960=CARTESIAN_POINT('Ctrl Pts',(25.3261087298029,66.2562398579479,0.));
#162961=CARTESIAN_POINT('Ctrl Pts',(25.3261087298029,66.2562398579479,12.));
#162962=CARTESIAN_POINT('Ctrl Pts',(25.3125812389727,66.2391510863992,0.));
#162963=CARTESIAN_POINT('Ctrl Pts',(25.3125812389727,66.2391510863992,12.));
#162964=CARTESIAN_POINT('Ctrl Pts',(25.2991009641086,66.2220860321931,0.));
#162965=CARTESIAN_POINT('Ctrl Pts',(25.2991009641086,66.2220860321931,12.));
#162966=CARTESIAN_POINT('Ctrl Pts',(25.285667940892,66.2050448607883,0.));
#162967=CARTESIAN_POINT('Ctrl Pts',(25.285667940892,66.2050448607883,12.));
#162968=CARTESIAN_POINT('Ctrl Pts',(25.2722822050828,66.1880277385114,0.));
#162969=CARTESIAN_POINT('Ctrl Pts',(25.2722822050828,66.1880277385114,12.));
#162970=CARTESIAN_POINT('Ctrl Pts',(25.2589437925144,66.1710348325378,0.));
#162971=CARTESIAN_POINT('Ctrl Pts',(25.2589437925144,66.1710348325378,12.));
#162972=CARTESIAN_POINT('Ctrl Pts',(25.245652739088,66.1540663108767,0.));
#162973=CARTESIAN_POINT('Ctrl Pts',(25.245652739088,66.1540663108767,12.));
#162974=CARTESIAN_POINT('Ctrl Pts',(25.232409080756,66.1371223423372,0.));
#162975=CARTESIAN_POINT('Ctrl Pts',(25.232409080756,66.1371223423372,12.));
#162976=CARTESIAN_POINT('Ctrl Pts',(25.2192128535367,66.1202030965785,0.));
#162977=CARTESIAN_POINT('Ctrl Pts',(25.2192128535367,66.1202030965785,12.));
#162978=CARTESIAN_POINT('Ctrl Pts',(25.2060640935371,66.1033087441916,0.));
#162979=CARTESIAN_POINT('Ctrl Pts',(25.2060640935371,66.1033087441916,12.));
#162980=CARTESIAN_POINT('Ctrl Pts',(25.1929628369685,66.086439456768,0.));
#162981=CARTESIAN_POINT('Ctrl Pts',(25.1929628369685,66.086439456768,12.));
#162982=CARTESIAN_POINT('Ctrl Pts',(25.1799091201594,66.0695954069699,0.));
#162983=CARTESIAN_POINT('Ctrl Pts',(25.1799091201594,66.0695954069699,12.));
#162984=CARTESIAN_POINT('Ctrl Pts',(25.1669029795651,66.0527767686,0.));
#162985=CARTESIAN_POINT('Ctrl Pts',(25.1669029795651,66.0527767686,12.));
#162986=CARTESIAN_POINT('Ctrl Pts',(25.1539444517409,66.0359837164709,0.));
#162987=CARTESIAN_POINT('Ctrl Pts',(25.1539444517409,66.0359837164709,12.));
#162988=CARTESIAN_POINT('Ctrl Pts',(25.1410335733094,66.0192164262607,0.));
#162989=CARTESIAN_POINT('Ctrl Pts',(25.1410335733094,66.0192164262607,12.));
#162990=CARTESIAN_POINT('Ctrl Pts',(25.1281703809299,66.0024750743902,0.));
#162991=CARTESIAN_POINT('Ctrl Pts',(25.1281703809299,66.0024750743902,12.));
#162992=CARTESIAN_POINT('Ctrl Pts',(25.1153549112511,65.9857598378455,0.));
#162993=CARTESIAN_POINT('Ctrl Pts',(25.1153549112511,65.9857598378455,12.));
#162994=CARTESIAN_POINT('Ctrl Pts',(25.1025872009015,65.9690708941591,0.));
#162995=CARTESIAN_POINT('Ctrl Pts',(25.1025872009015,65.9690708941591,12.));
#162996=CARTESIAN_POINT('Ctrl Pts',(25.0898672865925,65.9524084218167,0.));
#162997=CARTESIAN_POINT('Ctrl Pts',(25.0898672865925,65.9524084218167,12.));
#162998=CARTESIAN_POINT('Ctrl Pts',(25.0771952052032,65.9357726006174,0.));
#162999=CARTESIAN_POINT('Ctrl Pts',(25.0771952052032,65.9357726006174,12.));
#163000=CARTESIAN_POINT('Ctrl Pts',(25.0645709938519,65.9191636119796,0.));
#163001=CARTESIAN_POINT('Ctrl Pts',(25.0645709938519,65.9191636119796,12.));
#163002=CARTESIAN_POINT('Ctrl Pts',(25.0519946900066,65.9025816394391,0.));
#163003=CARTESIAN_POINT('Ctrl Pts',(25.0519946900066,65.9025816394391,12.));
#163004=CARTESIAN_POINT('Ctrl Pts',(25.039466331404,65.8860268683088,0.));
#163005=CARTESIAN_POINT('Ctrl Pts',(25.039466331404,65.8860268683088,12.));
#163006=CARTESIAN_POINT('Ctrl Pts',(25.0269859558351,65.8694994847587,0.));
#163007=CARTESIAN_POINT('Ctrl Pts',(25.0269859558351,65.8694994847587,12.));
#163008=CARTESIAN_POINT('Ctrl Pts',(25.0145536009603,65.8529996750441,0.));
#163009=CARTESIAN_POINT('Ctrl Pts',(25.0145536009603,65.8529996750441,12.));
#163010=CARTESIAN_POINT('Ctrl Pts',(25.0021693041181,65.8365276247157,0.));
#163011=CARTESIAN_POINT('Ctrl Pts',(25.0021693041181,65.8365276247157,12.));
#163012=CARTESIAN_POINT('Ctrl Pts',(24.9898331021002,65.8200835177071,0.));
#163013=CARTESIAN_POINT('Ctrl Pts',(24.9898331021002,65.8200835177071,12.));
#163014=CARTESIAN_POINT('Ctrl Pts',(24.97754503157,65.8036675380761,0.));
#163015=CARTESIAN_POINT('Ctrl Pts',(24.97754503157,65.8036675380761,12.));
#163016=CARTESIAN_POINT('Ctrl Pts',(24.965305129559,65.7872798720847,0.));
#163017=CARTESIAN_POINT('Ctrl Pts',(24.965305129559,65.7872798720847,12.));
#163018=CARTESIAN_POINT('Ctrl Pts',(24.9531134338693,65.7709207098949,0.));
#163019=CARTESIAN_POINT('Ctrl Pts',(24.9531134338693,65.7709207098949,12.));
#163020=CARTESIAN_POINT('Ctrl Pts',(24.9409699836523,65.7545902480286,0.));
#163021=CARTESIAN_POINT('Ctrl Pts',(24.9409699836523,65.7545902480286,12.));
#163022=CARTESIAN_POINT('Ctrl Pts',(24.9288748194562,65.7382886895839,0.));
#163023=CARTESIAN_POINT('Ctrl Pts',(24.9288748194562,65.7382886895839,12.));
#163024=CARTESIAN_POINT('Ctrl Pts',(24.9168279820093,65.7220162391016,0.));
#163025=CARTESIAN_POINT('Ctrl Pts',(24.9168279820093,65.7220162391016,12.));
#163026=CARTESIAN_POINT('Ctrl Pts',(24.9048295111444,65.7057730980471,0.));
#163027=CARTESIAN_POINT('Ctrl Pts',(24.9048295111444,65.7057730980471,12.));
#163028=CARTESIAN_POINT('Ctrl Pts',(24.8928794448615,65.6895594608798,0.));
#163029=CARTESIAN_POINT('Ctrl Pts',(24.8928794448615,65.6895594608798,12.));
#163030=CARTESIAN_POINT('Ctrl Pts',(24.8809778178248,65.6733755087724,0.));
#163031=CARTESIAN_POINT('Ctrl Pts',(24.8809778178248,65.6733755087724,12.));
#163032=CARTESIAN_POINT('Ctrl Pts',(24.869124662808,65.6572214156761,0.));
#163033=CARTESIAN_POINT('Ctrl Pts',(24.869124662808,65.6572214156761,12.));
#163034=CARTESIAN_POINT('Ctrl Pts',(24.8573200135683,65.6410973603713,0.));
#163035=CARTESIAN_POINT('Ctrl Pts',(24.8573200135683,65.6410973603713,12.));
#163036=CARTESIAN_POINT('Ctrl Pts',(24.8455639071517,65.6250035361612,0.));
#163037=CARTESIAN_POINT('Ctrl Pts',(24.8455639071517,65.6250035361612,12.));
#163038=CARTESIAN_POINT('Ctrl Pts',(24.8338563866739,65.6089401625552,0.));
#163039=CARTESIAN_POINT('Ctrl Pts',(24.8338563866739,65.6089401625552,12.));
#163040=CARTESIAN_POINT('Ctrl Pts',(24.8221975032059,65.5929074932487,0.));
#163041=CARTESIAN_POINT('Ctrl Pts',(24.8221975032059,65.5929074932487,12.));
#163042=CARTESIAN_POINT('Ctrl Pts',(24.8105873098578,65.5769057914184,0.));
#163043=CARTESIAN_POINT('Ctrl Pts',(24.8105873098578,65.5769057914184,12.));
#163044=CARTESIAN_POINT('Ctrl Pts',(24.7990258561234,65.560935306275,0.));
#163045=CARTESIAN_POINT('Ctrl Pts',(24.7990258561234,65.560935306275,12.));
#163046=CARTESIAN_POINT('Ctrl Pts',(24.7875131827515,65.5449962514735,0.));
#163047=CARTESIAN_POINT('Ctrl Pts',(24.7875131827515,65.5449962514735,12.));
#163048=CARTESIAN_POINT('Ctrl Pts',(24.776049314855,65.5290887770494,0.));
#163049=CARTESIAN_POINT('Ctrl Pts',(24.776049314855,65.5290887770494,12.));
#163050=CARTESIAN_POINT('Ctrl Pts',(24.7646342620969,65.5132129675727,0.));
#163051=CARTESIAN_POINT('Ctrl Pts',(24.7646342620969,65.5132129675727,12.));
#163052=CARTESIAN_POINT('Ctrl Pts',(24.755541272477,65.5005376841469,0.));
#163053=CARTESIAN_POINT('Ctrl Pts',(24.755541272477,65.5005376841469,12.));
#163054=CARTESIAN_POINT('Ctrl Pts',(24.7487434956058,65.4910454936487,0.));
#163055=CARTESIAN_POINT('Ctrl Pts',(24.7487434956058,65.4910454936487,12.));
#163056=CARTESIAN_POINT('Ctrl Pts',(24.7442214063411,65.484723709553,0.));
#163057=CARTESIAN_POINT('Ctrl Pts',(24.7442214063411,65.484723709553,12.));
#163058=CARTESIAN_POINT('Ctrl Pts',(24.7419628022042,65.4815644032299,0.));
#163059=CARTESIAN_POINT('Ctrl Pts',(24.7419628022042,65.4815644032299,12.));
#163060=CARTESIAN_POINT('',(24.7419628022042,65.4815644032299,12.));
#163061=CARTESIAN_POINT('Ctrl Pts',(24.7419628022042,65.4815644032299,12.));
#163062=CARTESIAN_POINT('Ctrl Pts',(24.7442214063411,65.484723709553,12.));
#163063=CARTESIAN_POINT('Ctrl Pts',(24.7487434956058,65.4910454936487,12.));
#163064=CARTESIAN_POINT('Ctrl Pts',(24.755541272477,65.5005376841469,12.));
#163065=CARTESIAN_POINT('Ctrl Pts',(24.7646342620969,65.5132129675727,12.));
#163066=CARTESIAN_POINT('Ctrl Pts',(24.776049314855,65.5290887770494,12.));
#163067=CARTESIAN_POINT('Ctrl Pts',(24.7875131827515,65.5449962514735,12.));
#163068=CARTESIAN_POINT('Ctrl Pts',(24.7990258561234,65.560935306275,12.));
#163069=CARTESIAN_POINT('Ctrl Pts',(24.8105873098578,65.5769057914184,12.));
#163070=CARTESIAN_POINT('Ctrl Pts',(24.8221975032059,65.5929074932487,12.));
#163071=CARTESIAN_POINT('Ctrl Pts',(24.8338563866739,65.6089401625552,12.));
#163072=CARTESIAN_POINT('Ctrl Pts',(24.8455639071517,65.6250035361612,12.));
#163073=CARTESIAN_POINT('Ctrl Pts',(24.8573200135683,65.6410973603713,12.));
#163074=CARTESIAN_POINT('Ctrl Pts',(24.869124662808,65.6572214156761,12.));
#163075=CARTESIAN_POINT('Ctrl Pts',(24.8809778178248,65.6733755087724,12.));
#163076=CARTESIAN_POINT('Ctrl Pts',(24.8928794448615,65.6895594608798,12.));
#163077=CARTESIAN_POINT('Ctrl Pts',(24.9048295111444,65.7057730980471,12.));
#163078=CARTESIAN_POINT('Ctrl Pts',(24.9168279820093,65.7220162391016,12.));
#163079=CARTESIAN_POINT('Ctrl Pts',(24.9288748194562,65.7382886895839,12.));
#163080=CARTESIAN_POINT('Ctrl Pts',(24.9409699836523,65.7545902480286,12.));
#163081=CARTESIAN_POINT('Ctrl Pts',(24.9531134338693,65.7709207098949,12.));
#163082=CARTESIAN_POINT('Ctrl Pts',(24.965305129559,65.7872798720847,12.));
#163083=CARTESIAN_POINT('Ctrl Pts',(24.97754503157,65.8036675380761,12.));
#163084=CARTESIAN_POINT('Ctrl Pts',(24.9898331021002,65.8200835177071,12.));
#163085=CARTESIAN_POINT('Ctrl Pts',(25.0021693041181,65.8365276247157,12.));
#163086=CARTESIAN_POINT('Ctrl Pts',(25.0145536009603,65.8529996750441,12.));
#163087=CARTESIAN_POINT('Ctrl Pts',(25.0269859558351,65.8694994847587,12.));
#163088=CARTESIAN_POINT('Ctrl Pts',(25.039466331404,65.8860268683088,12.));
#163089=CARTESIAN_POINT('Ctrl Pts',(25.0519946900066,65.9025816394391,12.));
#163090=CARTESIAN_POINT('Ctrl Pts',(25.0645709938519,65.9191636119796,12.));
#163091=CARTESIAN_POINT('Ctrl Pts',(25.0771952052032,65.9357726006174,12.));
#163092=CARTESIAN_POINT('Ctrl Pts',(25.0898672865925,65.9524084218167,12.));
#163093=CARTESIAN_POINT('Ctrl Pts',(25.1025872009015,65.9690708941591,12.));
#163094=CARTESIAN_POINT('Ctrl Pts',(25.1153549112511,65.9857598378455,12.));
#163095=CARTESIAN_POINT('Ctrl Pts',(25.1281703809299,66.0024750743902,12.));
#163096=CARTESIAN_POINT('Ctrl Pts',(25.1410335733094,66.0192164262607,12.));
#163097=CARTESIAN_POINT('Ctrl Pts',(25.1539444517409,66.0359837164709,12.));
#163098=CARTESIAN_POINT('Ctrl Pts',(25.1669029795651,66.0527767686,12.));
#163099=CARTESIAN_POINT('Ctrl Pts',(25.1799091201594,66.0695954069699,12.));
#163100=CARTESIAN_POINT('Ctrl Pts',(25.1929628369685,66.086439456768,12.));
#163101=CARTESIAN_POINT('Ctrl Pts',(25.2060640935371,66.1033087441916,12.));
#163102=CARTESIAN_POINT('Ctrl Pts',(25.2192128535367,66.1202030965785,12.));
#163103=CARTESIAN_POINT('Ctrl Pts',(25.232409080756,66.1371223423372,12.));
#163104=CARTESIAN_POINT('Ctrl Pts',(25.245652739088,66.1540663108767,12.));
#163105=CARTESIAN_POINT('Ctrl Pts',(25.2589437925144,66.1710348325378,12.));
#163106=CARTESIAN_POINT('Ctrl Pts',(25.2722822050828,66.1880277385114,12.));
#163107=CARTESIAN_POINT('Ctrl Pts',(25.285667940892,66.2050448607883,12.));
#163108=CARTESIAN_POINT('Ctrl Pts',(25.2991009641086,66.2220860321931,12.));
#163109=CARTESIAN_POINT('Ctrl Pts',(25.3125812389727,66.2391510863992,12.));
#163110=CARTESIAN_POINT('Ctrl Pts',(25.3261087298029,66.2562398579479,12.));
#163111=CARTESIAN_POINT('Ctrl Pts',(25.3396834009954,66.2733521822675,12.));
#163112=CARTESIAN_POINT('Ctrl Pts',(25.3533052170253,66.2904878956721,12.));
#163113=CARTESIAN_POINT('Ctrl Pts',(25.366974142449,66.3076468353417,12.));
#163114=CARTESIAN_POINT('Ctrl Pts',(25.3806901419012,66.3248288393046,12.));
#163115=CARTESIAN_POINT('Ctrl Pts',(25.39445318009,66.3420337464176,12.));
#163116=CARTESIAN_POINT('Ctrl Pts',(25.4082632217846,66.3592613963407,12.));
#163117=CARTESIAN_POINT('Ctrl Pts',(25.4221202318198,66.3765116295364,12.));
#163118=CARTESIAN_POINT('Ctrl Pts',(25.4360241751017,66.3937842872684,12.));
#163119=CARTESIAN_POINT('Ctrl Pts',(25.4499750166079,66.4110792116,12.));
#163120=CARTESIAN_POINT('Ctrl Pts',(25.463972721385,66.4283962453899,12.));
#163121=CARTESIAN_POINT('Ctrl Pts',(25.4780172545418,66.445735232287,12.));
#163122=CARTESIAN_POINT('Ctrl Pts',(25.4921085812548,66.463096016725,12.));
#163123=CARTESIAN_POINT('Ctrl Pts',(25.5062466667703,66.4804784439146,12.));
#163124=CARTESIAN_POINT('Ctrl Pts',(25.5204314764033,66.4978823598352,12.));
#163125=CARTESIAN_POINT('Ctrl Pts',(25.5346629755322,66.5153076112237,12.));
#163126=CARTESIAN_POINT('Ctrl Pts',(25.5489411295916,66.5327540455639,12.));
#163127=CARTESIAN_POINT('Ctrl Pts',(25.5632659040797,66.5502215110843,12.));
#163128=CARTESIAN_POINT('Ctrl Pts',(25.5776372645605,66.5677098567551,12.));
#163129=CARTESIAN_POINT('Ctrl Pts',(25.5920551766629,66.5852189322811,12.));
#163130=CARTESIAN_POINT('Ctrl Pts',(25.606519606075,66.6027485880947,12.));
#163131=CARTESIAN_POINT('Ctrl Pts',(25.6210305185394,66.6202986753482,12.));
#163132=CARTESIAN_POINT('Ctrl Pts',(25.6355878798605,66.6378690459105,12.));
#163133=CARTESIAN_POINT('Ctrl Pts',(25.650191655905,66.6554595523611,12.));
#163134=CARTESIAN_POINT('Ctrl Pts',(25.6648418126016,66.6730700479844,12.));
#163135=CARTESIAN_POINT('Ctrl Pts',(25.6795383159329,66.6907003867599,12.));
#163136=CARTESIAN_POINT('Ctrl Pts',(25.6942811319337,66.7083504233566,12.));
#163137=CARTESIAN_POINT('Ctrl Pts',(25.7090702266976,66.72602001313,12.));
#163138=CARTESIAN_POINT('Ctrl Pts',(25.7239055663778,66.7437090121168,12.));
#163139=CARTESIAN_POINT('Ctrl Pts',(25.7387871171861,66.7614172770302,12.));
#163140=CARTESIAN_POINT('Ctrl Pts',(25.7537148453848,66.7791446652505,12.));
#163141=CARTESIAN_POINT('Ctrl Pts',(25.7686887172859,66.7968910348199,12.));
#163142=CARTESIAN_POINT('Ctrl Pts',(25.783708699258,66.8146562444397,12.));
#163143=CARTESIAN_POINT('Ctrl Pts',(25.7987747577264,66.8324401534657,12.));
#163144=CARTESIAN_POINT('Ctrl Pts',(25.8138868591715,66.8502426219015,12.));
#163145=CARTESIAN_POINT('Ctrl Pts',(25.8290449701206,66.8680635103907,12.));
#163146=CARTESIAN_POINT('Ctrl Pts',(25.8442490571486,66.8859026802123,12.));
#163147=CARTESIAN_POINT('Ctrl Pts',(25.8594990868844,66.9037599932787,12.));
#163148=CARTESIAN_POINT('Ctrl Pts',(25.8747950260114,66.9216353121308,12.));
#163149=CARTESIAN_POINT('Ctrl Pts',(25.8901368412655,66.9395284999327,12.));
#163150=CARTESIAN_POINT('Ctrl Pts',(25.9055244994266,66.9574394204635,12.));
#163151=CARTESIAN_POINT('Ctrl Pts',(25.9209579673198,66.9753679381122,12.));
#163152=CARTESIAN_POINT('Ctrl Pts',(25.9364372118216,66.993313917876,12.));
#163153=CARTESIAN_POINT('Ctrl Pts',(25.9519621998598,67.0112772253553,12.));
#163154=CARTESIAN_POINT('Ctrl Pts',(25.9675328984123,67.0292577267495,12.));
#163155=CARTESIAN_POINT('Ctrl Pts',(25.9831492744988,67.0472552888495,12.));
#163156=CARTESIAN_POINT('Ctrl Pts',(25.9988112951818,67.0652697790335,12.));
#163157=CARTESIAN_POINT('Ctrl Pts',(26.0145189275732,67.083301065264,12.));
#163158=CARTESIAN_POINT('Ctrl Pts',(26.030272138834,67.101349016084,12.));
#163159=CARTESIAN_POINT('Ctrl Pts',(26.0460708961724,67.1194135006122,12.));
#163160=CARTESIAN_POINT('Ctrl Pts',(26.061915166836,67.1374943885353,12.));
#163161=CARTESIAN_POINT('Ctrl Pts',(26.0778049181129,67.1555915501052,12.));
#163162=CARTESIAN_POINT('Ctrl Pts',(26.0937401173385,67.1737048561364,12.));
#163163=CARTESIAN_POINT('Ctrl Pts',(26.109720731895,67.191834178002,12.));
#163164=CARTESIAN_POINT('Ctrl Pts',(26.1257467292102,67.2099793876295,12.));
#163165=CARTESIAN_POINT('Ctrl Pts',(26.1418180767486,67.228140357493,12.));
#163166=CARTESIAN_POINT('Ctrl Pts',(26.1579347420135,67.2463169606105,12.));
#163167=CARTESIAN_POINT('Ctrl Pts',(26.1740966925527,67.2645090705414,12.));
#163168=CARTESIAN_POINT('Ctrl Pts',(26.1903038959589,67.2827165613828,12.));
#163169=CARTESIAN_POINT('Ctrl Pts',(26.2065563198684,67.3009393077654,12.));
#163170=CARTESIAN_POINT('Ctrl Pts',(26.2228539319527,67.3191771848468,12.));
#163171=CARTESIAN_POINT('Ctrl Pts',(26.2391966999192,67.3374300683076,12.));
#163172=CARTESIAN_POINT('Ctrl Pts',(26.255584591518,67.3556978343506,12.));
#163173=CARTESIAN_POINT('Ctrl Pts',(26.2720175745422,67.3739803596967,12.));
#163174=CARTESIAN_POINT('Ctrl Pts',(26.288495616827,67.392277521581,12.));
#163175=CARTESIAN_POINT('Ctrl Pts',(26.305018686241,67.4105891977465,12.));
#163176=CARTESIAN_POINT('Ctrl Pts',(26.3215867506864,67.4289152664406,12.));
#163177=CARTESIAN_POINT('Ctrl Pts',(26.3381997781059,67.4472556064127,12.));
#163178=CARTESIAN_POINT('Ctrl Pts',(26.3548577364835,67.4656100969121,12.));
#163179=CARTESIAN_POINT('Ctrl Pts',(26.3715605938432,67.4839786176833,12.));
#163180=CARTESIAN_POINT('Ctrl Pts',(26.3883083182417,67.5023610489611,12.));
#163181=CARTESIAN_POINT('Ctrl Pts',(26.4051008777668,67.5207572714666,12.));
#163182=CARTESIAN_POINT('Ctrl Pts',(26.4219382405452,67.5391671664055,12.));
#163183=CARTESIAN_POINT('Ctrl Pts',(26.4388203747422,67.5575906154648,12.));
#163184=CARTESIAN_POINT('Ctrl Pts',(26.4557472485622,67.5760275008096,12.));
#163185=CARTESIAN_POINT('Ctrl Pts',(26.4727188302415,67.5944777050782,12.));
#163186=CARTESIAN_POINT('Ctrl Pts',(26.4897350880446,67.6129411113774,12.));
#163187=CARTESIAN_POINT('Ctrl Pts',(26.506795990273,67.6314176032823,12.));
#163188=CARTESIAN_POINT('Ctrl Pts',(26.5239015052655,67.6499070648323,12.));
#163189=CARTESIAN_POINT('Ctrl Pts',(26.5410516013984,67.6684093805288,12.));
#163190=CARTESIAN_POINT('Ctrl Pts',(26.5582462470794,67.6869244353292,12.));
#163191=CARTESIAN_POINT('Ctrl Pts',(26.5754854107422,67.7054521146427,12.));
#163192=CARTESIAN_POINT('Ctrl Pts',(26.5927690608546,67.7239923043295,12.));
#163193=CARTESIAN_POINT('Ctrl Pts',(26.6100971659204,67.7425448906983,12.));
#163194=CARTESIAN_POINT('Ctrl Pts',(26.6274696944793,67.7611097605042,12.));
#163195=CARTESIAN_POINT('Ctrl Pts',(26.6448866151027,67.7796868009447,12.));
#163196=CARTESIAN_POINT('Ctrl Pts',(26.6623478963867,67.7982758996557,12.));
#163197=CARTESIAN_POINT('Ctrl Pts',(26.6798535069586,67.8168769447086,12.));
#163198=CARTESIAN_POINT('Ctrl Pts',(26.6974034154802,67.8354898246079,12.));
#163199=CARTESIAN_POINT('Ctrl Pts',(26.7149975906478,67.8541144282875,12.));
#163200=CARTESIAN_POINT('Ctrl Pts',(26.7326360011886,67.8727506451068,12.));
#163201=CARTESIAN_POINT('Ctrl Pts',(26.7503186158523,67.8913983648441,12.));
#163202=CARTESIAN_POINT('Ctrl Pts',(26.7680454034168,67.9100574776974,12.));
#163203=CARTESIAN_POINT('Ctrl Pts',(26.7858163326932,67.9287278742839,12.));
#163204=CARTESIAN_POINT('Ctrl Pts',(26.8036313725262,67.9474094456395,12.));
#163205=CARTESIAN_POINT('Ctrl Pts',(26.8214904917921,67.9661020832165,12.));
#163206=CARTESIAN_POINT('Ctrl Pts',(26.8393936593914,67.9848056788814,12.));
#163207=CARTESIAN_POINT('Ctrl Pts',(26.85734084425,68.0035201249108,12.));
#163208=CARTESIAN_POINT('Ctrl Pts',(26.8753320153255,68.0222453139862,12.));
#163209=CARTESIAN_POINT('Ctrl Pts',(26.8933671416064,68.0409811391872,12.));
#163210=CARTESIAN_POINT('Ctrl Pts',(26.9114461921108,68.0597274939857,12.));
#163211=CARTESIAN_POINT('Ctrl Pts',(26.9295691358775,68.0784842722362,12.));
#163212=CARTESIAN_POINT('Ctrl Pts',(26.9477359419646,68.0972513681739,12.));
#163213=CARTESIAN_POINT('Ctrl Pts',(26.9659465794596,68.1160286764244,12.));
#163214=CARTESIAN_POINT('Ctrl Pts',(26.9842010174818,68.13481609201,12.));
#163215=CARTESIAN_POINT('Ctrl Pts',(27.0024992251839,68.1536135103558,12.));
#163216=CARTESIAN_POINT('Ctrl Pts',(27.0208411717477,68.1724208272967,12.));
#163217=CARTESIAN_POINT('Ctrl Pts',(27.0392268263804,68.1912379390787,12.));
#163218=CARTESIAN_POINT('Ctrl Pts',(27.0576561583179,68.2100647423345,12.));
#163219=CARTESIAN_POINT('Ctrl Pts',(27.076129136823,68.2289011340624,12.));
#163220=CARTESIAN_POINT('Ctrl Pts',(27.0946457311813,68.2477470116014,12.));
#163221=CARTESIAN_POINT('Ctrl Pts',(27.1132059106938,68.2666022726094,12.));
#163222=CARTESIAN_POINT('Ctrl Pts',(27.1318096446643,68.285466815035,12.));
#163223=CARTESIAN_POINT('Ctrl Pts',(27.150456902413,68.3043405371589,12.));
#163224=CARTESIAN_POINT('Ctrl Pts',(27.1691476532917,68.3232233376415,12.));
#163225=CARTESIAN_POINT('Ctrl Pts',(27.1878818666925,68.3421151155708,12.));
#163226=CARTESIAN_POINT('Ctrl Pts',(27.2066595120544,68.3610157704999,12.));
#163227=CARTESIAN_POINT('Ctrl Pts',(27.2254805588677,68.379925202511,12.));
#163228=CARTESIAN_POINT('Ctrl Pts',(27.2443449766654,68.398843312159,12.));
#163229=CARTESIAN_POINT('Ctrl Pts',(27.2632527350062,68.4177700003471,12.));
#163230=CARTESIAN_POINT('Ctrl Pts',(27.2822038034539,68.4367051682166,12.));
#163231=CARTESIAN_POINT('Ctrl Pts',(27.301198151557,68.455648717044,12.));
#163232=CARTESIAN_POINT('Ctrl Pts',(27.3202357488153,68.4746005480993,12.));
#163233=CARTESIAN_POINT('Ctrl Pts',(27.3393165646748,68.4935605626362,12.));
#163234=CARTESIAN_POINT('Ctrl Pts',(27.3584405685941,68.5125286621888,12.));
#163235=CARTESIAN_POINT('Ctrl Pts',(27.3776077300914,68.5315047488035,12.));
#163236=CARTESIAN_POINT('Ctrl Pts',(27.3968180187941,68.5504887252975,12.));
#163237=CARTESIAN_POINT('Ctrl Pts',(27.4160714044831,68.5694804955014,12.));
#163238=CARTESIAN_POINT('Ctrl Pts',(27.435367857136,68.5884799645218,12.));
#163239=CARTESIAN_POINT('Ctrl Pts',(27.4547073468226,68.6074870381619,12.));
#163240=CARTESIAN_POINT('Ctrl Pts',(27.4740898435988,68.6265016223561,12.));
#163241=CARTESIAN_POINT('Ctrl Pts',(27.4935153173868,68.645523622548,12.));
#163242=CARTESIAN_POINT('Ctrl Pts',(27.5129837378791,68.6645529432045,12.));
#163243=CARTESIAN_POINT('Ctrl Pts',(27.5324950743706,68.6835894869882,12.));
#163244=CARTESIAN_POINT('Ctrl Pts',(27.5520492958906,68.7026331554296,12.));
#163245=CARTESIAN_POINT('Ctrl Pts',(27.5716463715004,68.7216838504218,12.));
#163246=CARTESIAN_POINT('Ctrl Pts',(27.5912862705468,68.740741475526,12.));
#163247=CARTESIAN_POINT('Ctrl Pts',(27.6109689629029,68.7598059372129,12.));
#163248=CARTESIAN_POINT('Ctrl Pts',(27.6306944192737,68.7788771464713,12.));
#163249=CARTESIAN_POINT('Ctrl Pts',(27.6504626112666,68.7979550191872,12.));
#163250=CARTESIAN_POINT('Ctrl Pts',(27.6674443909983,68.8143140938915,12.));
#163251=CARTESIAN_POINT('Ctrl Pts',(27.6804870323433,68.8268597852179,12.));
#163252=CARTESIAN_POINT('Ctrl Pts',(27.6895716271274,68.8355891982106,12.));
#163253=CARTESIAN_POINT('Ctrl Pts',(27.6946856803717,68.8405004466159,12.));
#163254=CARTESIAN_POINT('Ctrl Pts',(27.6958230985043,68.8415926175084,12.));
#163255=CARTESIAN_POINT('',(24.7419628022042,65.4815644032299,0.));
#163256=CARTESIAN_POINT('',(24.7419628022042,65.4815644032299,0.));
#163257=CARTESIAN_POINT('Ctrl Pts',(27.6958230985043,68.8415926175085,0.));
#163258=CARTESIAN_POINT('Ctrl Pts',(27.6946856803717,68.8405004466159,0.));
#163259=CARTESIAN_POINT('Ctrl Pts',(27.6895716271274,68.8355891982106,0.));
#163260=CARTESIAN_POINT('Ctrl Pts',(27.6804870323433,68.8268597852179,0.));
#163261=CARTESIAN_POINT('Ctrl Pts',(27.6674443909983,68.8143140938915,0.));
#163262=CARTESIAN_POINT('Ctrl Pts',(27.6504626112666,68.7979550191872,0.));
#163263=CARTESIAN_POINT('Ctrl Pts',(27.6306944192737,68.7788771464713,0.));
#163264=CARTESIAN_POINT('Ctrl Pts',(27.6109689629029,68.7598059372129,0.));
#163265=CARTESIAN_POINT('Ctrl Pts',(27.5912862705468,68.740741475526,0.));
#163266=CARTESIAN_POINT('Ctrl Pts',(27.5716463715004,68.7216838504218,0.));
#163267=CARTESIAN_POINT('Ctrl Pts',(27.5520492958906,68.7026331554296,0.));
#163268=CARTESIAN_POINT('Ctrl Pts',(27.5324950743706,68.6835894869882,0.));
#163269=CARTESIAN_POINT('Ctrl Pts',(27.5129837378791,68.6645529432045,0.));
#163270=CARTESIAN_POINT('Ctrl Pts',(27.4935153173868,68.645523622548,0.));
#163271=CARTESIAN_POINT('Ctrl Pts',(27.4740898435988,68.6265016223561,0.));
#163272=CARTESIAN_POINT('Ctrl Pts',(27.4547073468226,68.6074870381619,0.));
#163273=CARTESIAN_POINT('Ctrl Pts',(27.435367857136,68.5884799645218,0.));
#163274=CARTESIAN_POINT('Ctrl Pts',(27.4160714044831,68.5694804955014,0.));
#163275=CARTESIAN_POINT('Ctrl Pts',(27.3968180187941,68.5504887252975,0.));
#163276=CARTESIAN_POINT('Ctrl Pts',(27.3776077300914,68.5315047488035,0.));
#163277=CARTESIAN_POINT('Ctrl Pts',(27.3584405685941,68.5125286621888,0.));
#163278=CARTESIAN_POINT('Ctrl Pts',(27.3393165646748,68.4935605626362,0.));
#163279=CARTESIAN_POINT('Ctrl Pts',(27.3202357488153,68.4746005480993,0.));
#163280=CARTESIAN_POINT('Ctrl Pts',(27.301198151557,68.455648717044,0.));
#163281=CARTESIAN_POINT('Ctrl Pts',(27.2822038034539,68.4367051682166,0.));
#163282=CARTESIAN_POINT('Ctrl Pts',(27.2632527350062,68.4177700003471,0.));
#163283=CARTESIAN_POINT('Ctrl Pts',(27.2443449766654,68.398843312159,0.));
#163284=CARTESIAN_POINT('Ctrl Pts',(27.2254805588677,68.379925202511,0.));
#163285=CARTESIAN_POINT('Ctrl Pts',(27.2066595120544,68.3610157704999,0.));
#163286=CARTESIAN_POINT('Ctrl Pts',(27.1878818666925,68.3421151155708,0.));
#163287=CARTESIAN_POINT('Ctrl Pts',(27.1691476532917,68.3232233376415,0.));
#163288=CARTESIAN_POINT('Ctrl Pts',(27.150456902413,68.3043405371589,0.));
#163289=CARTESIAN_POINT('Ctrl Pts',(27.1318096446643,68.285466815035,0.));
#163290=CARTESIAN_POINT('Ctrl Pts',(27.1132059106938,68.2666022726094,0.));
#163291=CARTESIAN_POINT('Ctrl Pts',(27.0946457311813,68.2477470116014,0.));
#163292=CARTESIAN_POINT('Ctrl Pts',(27.076129136823,68.2289011340624,0.));
#163293=CARTESIAN_POINT('Ctrl Pts',(27.0576561583179,68.2100647423345,0.));
#163294=CARTESIAN_POINT('Ctrl Pts',(27.0392268263804,68.1912379390787,0.));
#163295=CARTESIAN_POINT('Ctrl Pts',(27.0208411717477,68.1724208272967,0.));
#163296=CARTESIAN_POINT('Ctrl Pts',(27.0024992251839,68.1536135103558,0.));
#163297=CARTESIAN_POINT('Ctrl Pts',(26.9842010174818,68.13481609201,0.));
#163298=CARTESIAN_POINT('Ctrl Pts',(26.9659465794596,68.1160286764244,0.));
#163299=CARTESIAN_POINT('Ctrl Pts',(26.9477359419646,68.0972513681739,0.));
#163300=CARTESIAN_POINT('Ctrl Pts',(26.9295691358775,68.0784842722362,0.));
#163301=CARTESIAN_POINT('Ctrl Pts',(26.9114461921108,68.0597274939857,0.));
#163302=CARTESIAN_POINT('Ctrl Pts',(26.8933671416064,68.0409811391872,0.));
#163303=CARTESIAN_POINT('Ctrl Pts',(26.8753320153255,68.0222453139862,0.));
#163304=CARTESIAN_POINT('Ctrl Pts',(26.85734084425,68.0035201249108,0.));
#163305=CARTESIAN_POINT('Ctrl Pts',(26.8393936593914,67.9848056788814,0.));
#163306=CARTESIAN_POINT('Ctrl Pts',(26.8214904917921,67.9661020832165,0.));
#163307=CARTESIAN_POINT('Ctrl Pts',(26.8036313725262,67.9474094456395,0.));
#163308=CARTESIAN_POINT('Ctrl Pts',(26.7858163326932,67.9287278742839,0.));
#163309=CARTESIAN_POINT('Ctrl Pts',(26.7680454034168,67.9100574776974,0.));
#163310=CARTESIAN_POINT('Ctrl Pts',(26.7503186158523,67.8913983648441,0.));
#163311=CARTESIAN_POINT('Ctrl Pts',(26.7326360011886,67.8727506451068,0.));
#163312=CARTESIAN_POINT('Ctrl Pts',(26.7149975906478,67.8541144282875,0.));
#163313=CARTESIAN_POINT('Ctrl Pts',(26.6974034154802,67.8354898246079,0.));
#163314=CARTESIAN_POINT('Ctrl Pts',(26.6798535069586,67.8168769447086,0.));
#163315=CARTESIAN_POINT('Ctrl Pts',(26.6623478963867,67.7982758996557,0.));
#163316=CARTESIAN_POINT('Ctrl Pts',(26.6448866151027,67.7796868009447,0.));
#163317=CARTESIAN_POINT('Ctrl Pts',(26.6274696944793,67.7611097605042,0.));
#163318=CARTESIAN_POINT('Ctrl Pts',(26.6100971659204,67.7425448906983,0.));
#163319=CARTESIAN_POINT('Ctrl Pts',(26.5927690608546,67.7239923043295,0.));
#163320=CARTESIAN_POINT('Ctrl Pts',(26.5754854107422,67.7054521146427,0.));
#163321=CARTESIAN_POINT('Ctrl Pts',(26.5582462470794,67.6869244353292,0.));
#163322=CARTESIAN_POINT('Ctrl Pts',(26.5410516013984,67.6684093805288,0.));
#163323=CARTESIAN_POINT('Ctrl Pts',(26.5239015052655,67.6499070648323,0.));
#163324=CARTESIAN_POINT('Ctrl Pts',(26.506795990273,67.6314176032823,0.));
#163325=CARTESIAN_POINT('Ctrl Pts',(26.4897350880446,67.6129411113774,0.));
#163326=CARTESIAN_POINT('Ctrl Pts',(26.4727188302415,67.5944777050782,0.));
#163327=CARTESIAN_POINT('Ctrl Pts',(26.4557472485622,67.5760275008096,0.));
#163328=CARTESIAN_POINT('Ctrl Pts',(26.4388203747422,67.5575906154648,0.));
#163329=CARTESIAN_POINT('Ctrl Pts',(26.4219382405452,67.5391671664055,0.));
#163330=CARTESIAN_POINT('Ctrl Pts',(26.4051008777668,67.5207572714666,0.));
#163331=CARTESIAN_POINT('Ctrl Pts',(26.3883083182417,67.5023610489611,0.));
#163332=CARTESIAN_POINT('Ctrl Pts',(26.3715605938432,67.4839786176833,0.));
#163333=CARTESIAN_POINT('Ctrl Pts',(26.3548577364835,67.4656100969121,0.));
#163334=CARTESIAN_POINT('Ctrl Pts',(26.3381997781059,67.4472556064127,0.));
#163335=CARTESIAN_POINT('Ctrl Pts',(26.3215867506864,67.4289152664406,0.));
#163336=CARTESIAN_POINT('Ctrl Pts',(26.305018686241,67.4105891977465,0.));
#163337=CARTESIAN_POINT('Ctrl Pts',(26.288495616827,67.392277521581,0.));
#163338=CARTESIAN_POINT('Ctrl Pts',(26.2720175745422,67.3739803596967,0.));
#163339=CARTESIAN_POINT('Ctrl Pts',(26.255584591518,67.3556978343506,0.));
#163340=CARTESIAN_POINT('Ctrl Pts',(26.2391966999192,67.3374300683076,0.));
#163341=CARTESIAN_POINT('Ctrl Pts',(26.2228539319527,67.3191771848468,0.));
#163342=CARTESIAN_POINT('Ctrl Pts',(26.2065563198684,67.3009393077654,0.));
#163343=CARTESIAN_POINT('Ctrl Pts',(26.1903038959589,67.2827165613828,0.));
#163344=CARTESIAN_POINT('Ctrl Pts',(26.1740966925527,67.2645090705414,0.));
#163345=CARTESIAN_POINT('Ctrl Pts',(26.1579347420135,67.2463169606105,0.));
#163346=CARTESIAN_POINT('Ctrl Pts',(26.1418180767486,67.228140357493,0.));
#163347=CARTESIAN_POINT('Ctrl Pts',(26.1257467292102,67.2099793876295,0.));
#163348=CARTESIAN_POINT('Ctrl Pts',(26.109720731895,67.191834178002,0.));
#163349=CARTESIAN_POINT('Ctrl Pts',(26.0937401173385,67.1737048561364,0.));
#163350=CARTESIAN_POINT('Ctrl Pts',(26.0778049181129,67.1555915501052,0.));
#163351=CARTESIAN_POINT('Ctrl Pts',(26.061915166836,67.1374943885353,0.));
#163352=CARTESIAN_POINT('Ctrl Pts',(26.0460708961724,67.1194135006122,0.));
#163353=CARTESIAN_POINT('Ctrl Pts',(26.030272138834,67.101349016084,0.));
#163354=CARTESIAN_POINT('Ctrl Pts',(26.0145189275732,67.083301065264,0.));
#163355=CARTESIAN_POINT('Ctrl Pts',(25.9988112951818,67.0652697790335,0.));
#163356=CARTESIAN_POINT('Ctrl Pts',(25.9831492744988,67.0472552888495,0.));
#163357=CARTESIAN_POINT('Ctrl Pts',(25.9675328984123,67.0292577267495,0.));
#163358=CARTESIAN_POINT('Ctrl Pts',(25.9519621998598,67.0112772253553,0.));
#163359=CARTESIAN_POINT('Ctrl Pts',(25.9364372118216,66.993313917876,0.));
#163360=CARTESIAN_POINT('Ctrl Pts',(25.9209579673198,66.9753679381122,0.));
#163361=CARTESIAN_POINT('Ctrl Pts',(25.9055244994266,66.9574394204635,0.));
#163362=CARTESIAN_POINT('Ctrl Pts',(25.8901368412655,66.9395284999327,0.));
#163363=CARTESIAN_POINT('Ctrl Pts',(25.8747950260114,66.9216353121308,0.));
#163364=CARTESIAN_POINT('Ctrl Pts',(25.8594990868844,66.9037599932787,0.));
#163365=CARTESIAN_POINT('Ctrl Pts',(25.8442490571486,66.8859026802123,0.));
#163366=CARTESIAN_POINT('Ctrl Pts',(25.8290449701206,66.8680635103907,0.));
#163367=CARTESIAN_POINT('Ctrl Pts',(25.8138868591715,66.8502426219015,0.));
#163368=CARTESIAN_POINT('Ctrl Pts',(25.7987747577264,66.8324401534657,0.));
#163369=CARTESIAN_POINT('Ctrl Pts',(25.783708699258,66.8146562444397,0.));
#163370=CARTESIAN_POINT('Ctrl Pts',(25.7686887172859,66.7968910348199,0.));
#163371=CARTESIAN_POINT('Ctrl Pts',(25.7537148453848,66.7791446652505,0.));
#163372=CARTESIAN_POINT('Ctrl Pts',(25.7387871171861,66.7614172770302,0.));
#163373=CARTESIAN_POINT('Ctrl Pts',(25.7239055663778,66.7437090121168,0.));
#163374=CARTESIAN_POINT('Ctrl Pts',(25.7090702266976,66.72602001313,0.));
#163375=CARTESIAN_POINT('Ctrl Pts',(25.6942811319337,66.7083504233566,0.));
#163376=CARTESIAN_POINT('Ctrl Pts',(25.6795383159329,66.6907003867599,0.));
#163377=CARTESIAN_POINT('Ctrl Pts',(25.6648418126016,66.6730700479844,0.));
#163378=CARTESIAN_POINT('Ctrl Pts',(25.650191655905,66.6554595523611,0.));
#163379=CARTESIAN_POINT('Ctrl Pts',(25.6355878798605,66.6378690459105,0.));
#163380=CARTESIAN_POINT('Ctrl Pts',(25.6210305185394,66.6202986753482,0.));
#163381=CARTESIAN_POINT('Ctrl Pts',(25.606519606075,66.6027485880947,0.));
#163382=CARTESIAN_POINT('Ctrl Pts',(25.5920551766629,66.5852189322811,0.));
#163383=CARTESIAN_POINT('Ctrl Pts',(25.5776372645605,66.5677098567551,0.));
#163384=CARTESIAN_POINT('Ctrl Pts',(25.5632659040797,66.5502215110843,0.));
#163385=CARTESIAN_POINT('Ctrl Pts',(25.5489411295916,66.5327540455639,0.));
#163386=CARTESIAN_POINT('Ctrl Pts',(25.5346629755322,66.5153076112237,0.));
#163387=CARTESIAN_POINT('Ctrl Pts',(25.5204314764033,66.4978823598352,0.));
#163388=CARTESIAN_POINT('Ctrl Pts',(25.5062466667703,66.4804784439146,0.));
#163389=CARTESIAN_POINT('Ctrl Pts',(25.4921085812548,66.463096016725,0.));
#163390=CARTESIAN_POINT('Ctrl Pts',(25.4780172545418,66.445735232287,0.));
#163391=CARTESIAN_POINT('Ctrl Pts',(25.463972721385,66.4283962453899,0.));
#163392=CARTESIAN_POINT('Ctrl Pts',(25.4499750166079,66.4110792116,0.));
#163393=CARTESIAN_POINT('Ctrl Pts',(25.4360241751017,66.3937842872684,0.));
#163394=CARTESIAN_POINT('Ctrl Pts',(25.4221202318198,66.3765116295364,0.));
#163395=CARTESIAN_POINT('Ctrl Pts',(25.4082632217846,66.3592613963407,0.));
#163396=CARTESIAN_POINT('Ctrl Pts',(25.39445318009,66.3420337464176,0.));
#163397=CARTESIAN_POINT('Ctrl Pts',(25.3806901419012,66.3248288393046,0.));
#163398=CARTESIAN_POINT('Ctrl Pts',(25.366974142449,66.3076468353417,0.));
#163399=CARTESIAN_POINT('Ctrl Pts',(25.3533052170253,66.2904878956721,0.));
#163400=CARTESIAN_POINT('Ctrl Pts',(25.3396834009954,66.2733521822675,0.));
#163401=CARTESIAN_POINT('Ctrl Pts',(25.3261087298029,66.2562398579479,0.));
#163402=CARTESIAN_POINT('Ctrl Pts',(25.3125812389727,66.2391510863992,0.));
#163403=CARTESIAN_POINT('Ctrl Pts',(25.2991009641086,66.2220860321931,0.));
#163404=CARTESIAN_POINT('Ctrl Pts',(25.285667940892,66.2050448607883,0.));
#163405=CARTESIAN_POINT('Ctrl Pts',(25.2722822050828,66.1880277385114,0.));
#163406=CARTESIAN_POINT('Ctrl Pts',(25.2589437925144,66.1710348325378,0.));
#163407=CARTESIAN_POINT('Ctrl Pts',(25.245652739088,66.1540663108767,0.));
#163408=CARTESIAN_POINT('Ctrl Pts',(25.232409080756,66.1371223423372,0.));
#163409=CARTESIAN_POINT('Ctrl Pts',(25.2192128535367,66.1202030965785,0.));
#163410=CARTESIAN_POINT('Ctrl Pts',(25.2060640935371,66.1033087441916,0.));
#163411=CARTESIAN_POINT('Ctrl Pts',(25.1929628369685,66.086439456768,0.));
#163412=CARTESIAN_POINT('Ctrl Pts',(25.1799091201594,66.0695954069699,0.));
#163413=CARTESIAN_POINT('Ctrl Pts',(25.1669029795651,66.0527767686,0.));
#163414=CARTESIAN_POINT('Ctrl Pts',(25.1539444517409,66.0359837164709,0.));
#163415=CARTESIAN_POINT('Ctrl Pts',(25.1410335733094,66.0192164262607,0.));
#163416=CARTESIAN_POINT('Ctrl Pts',(25.1281703809299,66.0024750743902,0.));
#163417=CARTESIAN_POINT('Ctrl Pts',(25.1153549112511,65.9857598378455,0.));
#163418=CARTESIAN_POINT('Ctrl Pts',(25.1025872009015,65.9690708941591,0.));
#163419=CARTESIAN_POINT('Ctrl Pts',(25.0898672865925,65.9524084218167,0.));
#163420=CARTESIAN_POINT('Ctrl Pts',(25.0771952052032,65.9357726006174,0.));
#163421=CARTESIAN_POINT('Ctrl Pts',(25.0645709938519,65.9191636119796,0.));
#163422=CARTESIAN_POINT('Ctrl Pts',(25.0519946900066,65.9025816394391,0.));
#163423=CARTESIAN_POINT('Ctrl Pts',(25.039466331404,65.8860268683088,0.));
#163424=CARTESIAN_POINT('Ctrl Pts',(25.0269859558351,65.8694994847587,0.));
#163425=CARTESIAN_POINT('Ctrl Pts',(25.0145536009603,65.8529996750441,0.));
#163426=CARTESIAN_POINT('Ctrl Pts',(25.0021693041181,65.8365276247157,0.));
#163427=CARTESIAN_POINT('Ctrl Pts',(24.9898331021002,65.8200835177071,0.));
#163428=CARTESIAN_POINT('Ctrl Pts',(24.97754503157,65.8036675380761,0.));
#163429=CARTESIAN_POINT('Ctrl Pts',(24.965305129559,65.7872798720847,0.));
#163430=CARTESIAN_POINT('Ctrl Pts',(24.9531134338693,65.7709207098949,0.));
#163431=CARTESIAN_POINT('Ctrl Pts',(24.9409699836523,65.7545902480286,0.));
#163432=CARTESIAN_POINT('Ctrl Pts',(24.9288748194562,65.7382886895839,0.));
#163433=CARTESIAN_POINT('Ctrl Pts',(24.9168279820093,65.7220162391016,0.));
#163434=CARTESIAN_POINT('Ctrl Pts',(24.9048295111444,65.7057730980471,0.));
#163435=CARTESIAN_POINT('Ctrl Pts',(24.8928794448615,65.6895594608798,0.));
#163436=CARTESIAN_POINT('Ctrl Pts',(24.8809778178248,65.6733755087724,0.));
#163437=CARTESIAN_POINT('Ctrl Pts',(24.869124662808,65.6572214156761,0.));
#163438=CARTESIAN_POINT('Ctrl Pts',(24.8573200135683,65.6410973603713,0.));
#163439=CARTESIAN_POINT('Ctrl Pts',(24.8455639071517,65.6250035361612,0.));
#163440=CARTESIAN_POINT('Ctrl Pts',(24.8338563866739,65.6089401625552,0.));
#163441=CARTESIAN_POINT('Ctrl Pts',(24.8221975032059,65.5929074932487,0.));
#163442=CARTESIAN_POINT('Ctrl Pts',(24.8105873098578,65.5769057914184,0.));
#163443=CARTESIAN_POINT('Ctrl Pts',(24.7990258561234,65.560935306275,0.));
#163444=CARTESIAN_POINT('Ctrl Pts',(24.7875131827515,65.5449962514735,0.));
#163445=CARTESIAN_POINT('Ctrl Pts',(24.776049314855,65.5290887770494,0.));
#163446=CARTESIAN_POINT('Ctrl Pts',(24.7646342620969,65.5132129675727,0.));
#163447=CARTESIAN_POINT('Ctrl Pts',(24.755541272477,65.5005376841469,0.));
#163448=CARTESIAN_POINT('Ctrl Pts',(24.7487434956058,65.4910454936487,0.));
#163449=CARTESIAN_POINT('Ctrl Pts',(24.7442214063411,65.484723709553,0.));
#163450=CARTESIAN_POINT('Ctrl Pts',(24.7419628022042,65.4815644032299,0.));
#163451=CARTESIAN_POINT('Ctrl Pts',(33.8448817269567,66.3684712863594,0.));
#163452=CARTESIAN_POINT('Ctrl Pts',(33.8448817269567,66.3684712863594,12.));
#163453=CARTESIAN_POINT('Ctrl Pts',(33.8404862618869,66.3650082659713,0.));
#163454=CARTESIAN_POINT('Ctrl Pts',(33.8404862618869,66.3650082659713,12.));
#163455=CARTESIAN_POINT('Ctrl Pts',(33.8316996011932,66.3580824155893,0.));
#163456=CARTESIAN_POINT('Ctrl Pts',(33.8316996011932,66.3580824155893,12.));
#163457=CARTESIAN_POINT('Ctrl Pts',(33.8185324184903,66.3476942112,0.));
#163458=CARTESIAN_POINT('Ctrl Pts',(33.8185324184903,66.3476942112,12.));
#163459=CARTESIAN_POINT('Ctrl Pts',(33.8010017926027,66.3338444144211,0.));
#163460=CARTESIAN_POINT('Ctrl Pts',(33.8010017926027,66.3338444144211,12.));
#163461=CARTESIAN_POINT('Ctrl Pts',(33.7791312145108,66.3165340771611,0.));
#163462=CARTESIAN_POINT('Ctrl Pts',(33.7791312145108,66.3165340771611,12.));
#163463=CARTESIAN_POINT('Ctrl Pts',(33.7573033544559,66.2992256621336,0.));
#163464=CARTESIAN_POINT('Ctrl Pts',(33.7573033544559,66.2992256621336,12.));
#163465=CARTESIAN_POINT('Ctrl Pts',(33.7355182321907,66.2819191962353,0.));
#163466=CARTESIAN_POINT('Ctrl Pts',(33.7355182321907,66.2819191962353,12.));
#163467=CARTESIAN_POINT('Ctrl Pts',(33.7137758735902,66.2646147235322,0.));
#163468=CARTESIAN_POINT('Ctrl Pts',(33.7137758735902,66.2646147235322,12.));
#163469=CARTESIAN_POINT('Ctrl Pts',(33.6920763111448,66.2473123109395,0.));
#163470=CARTESIAN_POINT('Ctrl Pts',(33.6920763111448,66.2473123109395,12.));
#163471=CARTESIAN_POINT('Ctrl Pts',(33.6704195830392,66.2300120464082,0.));
#163472=CARTESIAN_POINT('Ctrl Pts',(33.6704195830392,66.2300120464082,12.));
#163473=CARTESIAN_POINT('Ctrl Pts',(33.6488057311532,66.2127140313598,0.));
#163474=CARTESIAN_POINT('Ctrl Pts',(33.6488057311532,66.2127140313598,12.));
#163475=CARTESIAN_POINT('Ctrl Pts',(33.6272347993476,66.1954183747089,0.));
#163476=CARTESIAN_POINT('Ctrl Pts',(33.6272347993476,66.1954183747089,12.));
#163477=CARTESIAN_POINT('Ctrl Pts',(33.6057068316769,66.1781251864017,0.));
#163478=CARTESIAN_POINT('Ctrl Pts',(33.6057068316769,66.1781251864017,12.));
#163479=CARTESIAN_POINT('Ctrl Pts',(33.584221870515,66.1608345707637,0.));
#163480=CARTESIAN_POINT('Ctrl Pts',(33.584221870515,66.1608345707637,12.));
#163481=CARTESIAN_POINT('Ctrl Pts',(33.5627799550483,66.1435466211076,0.));
#163482=CARTESIAN_POINT('Ctrl Pts',(33.5627799550483,66.1435466211076,12.));
#163483=CARTESIAN_POINT('Ctrl Pts',(33.541381122345,66.1262614234674,0.));
#163484=CARTESIAN_POINT('Ctrl Pts',(33.541381122345,66.1262614234674,12.));
#163485=CARTESIAN_POINT('Ctrl Pts',(33.5200254081243,66.1089790592729,0.));
#163486=CARTESIAN_POINT('Ctrl Pts',(33.5200254081243,66.1089790592729,12.));
#163487=CARTESIAN_POINT('Ctrl Pts',(33.4987128476622,66.0916996085245,0.));
#163488=CARTESIAN_POINT('Ctrl Pts',(33.4987128476622,66.0916996085245,12.));
#163489=CARTESIAN_POINT('Ctrl Pts',(33.4774434765745,66.0744231525415,0.));
#163490=CARTESIAN_POINT('Ctrl Pts',(33.4774434765745,66.0744231525415,12.));
#163491=CARTESIAN_POINT('Ctrl Pts',(33.4562173318025,66.0571497774434,0.));
#163492=CARTESIAN_POINT('Ctrl Pts',(33.4562173318025,66.0571497774434,12.));
#163493=CARTESIAN_POINT('Ctrl Pts',(33.43503445151,66.0398795737777,0.));
#163494=CARTESIAN_POINT('Ctrl Pts',(33.43503445151,66.0398795737777,12.));
#163495=CARTESIAN_POINT('Ctrl Pts',(33.4138948746388,66.0226126349446,0.));
#163496=CARTESIAN_POINT('Ctrl Pts',(33.4138948746388,66.0226126349446,12.));
#163497=CARTESIAN_POINT('Ctrl Pts',(33.3927986405605,66.0053490559812,0.));
#163498=CARTESIAN_POINT('Ctrl Pts',(33.3927986405605,66.0053490559812,12.));
#163499=CARTESIAN_POINT('Ctrl Pts',(33.37174578871,65.9880889322831,0.));
#163500=CARTESIAN_POINT('Ctrl Pts',(33.37174578871,65.9880889322831,12.));
#163501=CARTESIAN_POINT('Ctrl Pts',(33.3507363581592,65.970832358141,0.));
#163502=CARTESIAN_POINT('Ctrl Pts',(33.3507363581592,65.970832358141,12.));
#163503=CARTESIAN_POINT('Ctrl Pts',(33.3297703874265,65.9535794260831,0.));
#163504=CARTESIAN_POINT('Ctrl Pts',(33.3297703874265,65.9535794260831,12.));
#163505=CARTESIAN_POINT('Ctrl Pts',(33.3088479147164,65.9363302276846,0.));
#163506=CARTESIAN_POINT('Ctrl Pts',(33.3088479147164,65.9363302276846,12.));
#163507=CARTESIAN_POINT('Ctrl Pts',(33.2879689780572,65.9190848540433,0.));
#163508=CARTESIAN_POINT('Ctrl Pts',(33.2879689780572,65.9190848540433,12.));
#163509=CARTESIAN_POINT('Ctrl Pts',(33.2671336154753,65.9018433963889,0.));
#163510=CARTESIAN_POINT('Ctrl Pts',(33.2671336154753,65.9018433963889,12.));
#163511=CARTESIAN_POINT('Ctrl Pts',(33.2463418651492,65.8846059466372,0.));
#163512=CARTESIAN_POINT('Ctrl Pts',(33.2463418651492,65.8846059466372,12.));
#163513=CARTESIAN_POINT('Ctrl Pts',(33.2255937655649,65.8673725979578,0.));
#163514=CARTESIAN_POINT('Ctrl Pts',(33.2255937655649,65.8673725979578,12.));
#163515=CARTESIAN_POINT('Ctrl Pts',(33.2048893554491,65.8501434445164,0.));
#163516=CARTESIAN_POINT('Ctrl Pts',(33.2048893554491,65.8501434445164,12.));
#163517=CARTESIAN_POINT('Ctrl Pts',(33.1842286737051,65.8329185812375,0.));
#163518=CARTESIAN_POINT('Ctrl Pts',(33.1842286737051,65.8329185812375,12.));
#163519=CARTESIAN_POINT('Ctrl Pts',(33.16361175934,65.8156981035503,0.));
#163520=CARTESIAN_POINT('Ctrl Pts',(33.16361175934,65.8156981035503,12.));
#163521=CARTESIAN_POINT('Ctrl Pts',(33.1430386513976,65.7984821071623,0.));
#163522=CARTESIAN_POINT('Ctrl Pts',(33.1430386513976,65.7984821071623,12.));
#163523=CARTESIAN_POINT('Ctrl Pts',(33.1225093888672,65.7812706877697,0.));
#163524=CARTESIAN_POINT('Ctrl Pts',(33.1225093888672,65.7812706877697,12.));
#163525=CARTESIAN_POINT('Ctrl Pts',(33.1020240106884,65.7640639410661,0.));
#163526=CARTESIAN_POINT('Ctrl Pts',(33.1020240106884,65.7640639410661,12.));
#163527=CARTESIAN_POINT('Ctrl Pts',(33.081582555798,65.7468619628816,0.));
#163528=CARTESIAN_POINT('Ctrl Pts',(33.081582555798,65.7468619628816,12.));
#163529=CARTESIAN_POINT('Ctrl Pts',(33.0611850631582,65.7296648492825,0.));
#163530=CARTESIAN_POINT('Ctrl Pts',(33.0611850631582,65.7296648492825,12.));
#163531=CARTESIAN_POINT('Ctrl Pts',(33.0408315717873,65.7124726966802,0.));
#163532=CARTESIAN_POINT('Ctrl Pts',(33.0408315717873,65.7124726966802,12.));
#163533=CARTESIAN_POINT('Ctrl Pts',(33.0205221207873,65.6952856019533,0.));
#163534=CARTESIAN_POINT('Ctrl Pts',(33.0205221207873,65.6952856019533,12.));
#163535=CARTESIAN_POINT('Ctrl Pts',(33.0002567493573,65.6781036625027,0.));
#163536=CARTESIAN_POINT('Ctrl Pts',(33.0002567493573,65.6781036625027,12.));
#163537=CARTESIAN_POINT('Ctrl Pts',(32.980035496784,65.6609269761889,0.));
#163538=CARTESIAN_POINT('Ctrl Pts',(32.980035496784,65.6609269761889,12.));
#163539=CARTESIAN_POINT('Ctrl Pts',(32.9598584024312,65.6437556412947,0.));
#163540=CARTESIAN_POINT('Ctrl Pts',(32.9598584024312,65.6437556412947,12.));
#163541=CARTESIAN_POINT('Ctrl Pts',(32.9397255057274,65.6265897564783,0.));
#163542=CARTESIAN_POINT('Ctrl Pts',(32.9397255057274,65.6265897564783,12.));
#163543=CARTESIAN_POINT('Ctrl Pts',(32.9196368461463,65.6094294207276,0.));
#163544=CARTESIAN_POINT('Ctrl Pts',(32.9196368461463,65.6094294207276,12.));
#163545=CARTESIAN_POINT('Ctrl Pts',(32.8995924631898,65.5922747333194,0.));
#163546=CARTESIAN_POINT('Ctrl Pts',(32.8995924631898,65.5922747333194,12.));
#163547=CARTESIAN_POINT('Ctrl Pts',(32.879592396403,65.5751257938473,0.));
#163548=CARTESIAN_POINT('Ctrl Pts',(32.879592396403,65.5751257938473,12.));
#163549=CARTESIAN_POINT('Ctrl Pts',(32.8596366853832,65.5579827022421,0.));
#163550=CARTESIAN_POINT('Ctrl Pts',(32.8596366853832,65.5579827022421,12.));
#163551=CARTESIAN_POINT('Ctrl Pts',(32.8397253697865,65.5408455587965,0.));
#163552=CARTESIAN_POINT('Ctrl Pts',(32.8397253697865,65.5408455587965,12.));
#163553=CARTESIAN_POINT('Ctrl Pts',(32.8198584893315,65.5237144641858,0.));
#163554=CARTESIAN_POINT('Ctrl Pts',(32.8198584893315,65.5237144641858,12.));
#163555=CARTESIAN_POINT('Ctrl Pts',(32.8000360837975,65.5065895194928,0.));
#163556=CARTESIAN_POINT('Ctrl Pts',(32.8000360837975,65.5065895194928,12.));
#163557=CARTESIAN_POINT('Ctrl Pts',(32.7802581930287,65.4894708262061,0.));
#163558=CARTESIAN_POINT('Ctrl Pts',(32.7802581930287,65.4894708262061,12.));
#163559=CARTESIAN_POINT('Ctrl Pts',(32.7605248569378,65.4723584862122,0.));
#163560=CARTESIAN_POINT('Ctrl Pts',(32.7605248569378,65.4723584862122,12.));
#163561=CARTESIAN_POINT('Ctrl Pts',(32.7408361155037,65.4552526017905,0.));
#163562=CARTESIAN_POINT('Ctrl Pts',(32.7408361155037,65.4552526017905,12.));
#163563=CARTESIAN_POINT('Ctrl Pts',(32.7211920087684,65.4381532756065,0.));
#163564=CARTESIAN_POINT('Ctrl Pts',(32.7211920087684,65.4381532756065,12.));
#163565=CARTESIAN_POINT('Ctrl Pts',(32.7015925768265,65.4210606107035,0.));
#163566=CARTESIAN_POINT('Ctrl Pts',(32.7015925768265,65.4210606107035,12.));
#163567=CARTESIAN_POINT('Ctrl Pts',(32.6820378598267,65.4039747105038,0.));
#163568=CARTESIAN_POINT('Ctrl Pts',(32.6820378598267,65.4039747105038,12.));
#163569=CARTESIAN_POINT('Ctrl Pts',(32.662527897981,65.3868956788182,0.));
#163570=CARTESIAN_POINT('Ctrl Pts',(32.662527897981,65.3868956788182,12.));
#163571=CARTESIAN_POINT('Ctrl Pts',(32.6430627315674,65.3698236198513,0.));
#163572=CARTESIAN_POINT('Ctrl Pts',(32.6430627315674,65.3698236198513,12.));
#163573=CARTESIAN_POINT('Ctrl Pts',(32.6236424009301,65.3527586382081,0.));
#163574=CARTESIAN_POINT('Ctrl Pts',(32.6236424009301,65.3527586382081,12.));
#163575=CARTESIAN_POINT('Ctrl Pts',(32.6042669464751,65.3357008389004,0.));
#163576=CARTESIAN_POINT('Ctrl Pts',(32.6042669464751,65.3357008389004,12.));
#163577=CARTESIAN_POINT('Ctrl Pts',(32.5849364086678,65.31865032735,0.));
#163578=CARTESIAN_POINT('Ctrl Pts',(32.5849364086678,65.31865032735,12.));
#163579=CARTESIAN_POINT('Ctrl Pts',(32.5656508280421,65.3016072093912,0.));
#163580=CARTESIAN_POINT('Ctrl Pts',(32.5656508280421,65.3016072093912,12.));
#163581=CARTESIAN_POINT('Ctrl Pts',(32.5464102452014,65.2845715912721,0.));
#163582=CARTESIAN_POINT('Ctrl Pts',(32.5464102452014,65.2845715912721,12.));
#163583=CARTESIAN_POINT('Ctrl Pts',(32.5272147008191,65.2675435796558,0.));
#163584=CARTESIAN_POINT('Ctrl Pts',(32.5272147008191,65.2675435796558,12.));
#163585=CARTESIAN_POINT('Ctrl Pts',(32.5080642356328,65.2505232816209,0.));
#163586=CARTESIAN_POINT('Ctrl Pts',(32.5080642356328,65.2505232816209,12.));
#163587=CARTESIAN_POINT('Ctrl Pts',(32.4889588904392,65.2335108046614,0.));
#163588=CARTESIAN_POINT('Ctrl Pts',(32.4889588904392,65.2335108046614,12.));
#163589=CARTESIAN_POINT('Ctrl Pts',(32.4698987061032,65.2165062566924,0.));
#163590=CARTESIAN_POINT('Ctrl Pts',(32.4698987061032,65.2165062566924,12.));
#163591=CARTESIAN_POINT('Ctrl Pts',(32.450883723561,65.1995097460538,0.));
#163592=CARTESIAN_POINT('Ctrl Pts',(32.450883723561,65.1995097460538,12.));
#163593=CARTESIAN_POINT('Ctrl Pts',(32.4319139838212,65.182521381514,0.));
#163594=CARTESIAN_POINT('Ctrl Pts',(32.4319139838212,65.182521381514,12.));
#163595=CARTESIAN_POINT('Ctrl Pts',(32.4129895279615,65.1655412722726,0.));
#163596=CARTESIAN_POINT('Ctrl Pts',(32.4129895279615,65.1655412722726,12.));
#163597=CARTESIAN_POINT('Ctrl Pts',(32.3941103971221,65.1485695279635,0.));
#163598=CARTESIAN_POINT('Ctrl Pts',(32.3941103971221,65.1485695279635,12.));
#163599=CARTESIAN_POINT('Ctrl Pts',(32.3752766325136,65.1316062586588,0.));
#163600=CARTESIAN_POINT('Ctrl Pts',(32.3752766325136,65.1316062586588,12.));
#163601=CARTESIAN_POINT('Ctrl Pts',(32.3564882754212,65.1146515748722,0.));
#163602=CARTESIAN_POINT('Ctrl Pts',(32.3564882754212,65.1146515748722,12.));
#163603=CARTESIAN_POINT('Ctrl Pts',(32.3377453672051,65.0977055875608,0.));
#163604=CARTESIAN_POINT('Ctrl Pts',(32.3377453672051,65.0977055875608,12.));
#163605=CARTESIAN_POINT('Ctrl Pts',(32.3190479492987,65.0807684081282,0.));
#163606=CARTESIAN_POINT('Ctrl Pts',(32.3190479492987,65.0807684081282,12.));
#163607=CARTESIAN_POINT('Ctrl Pts',(32.3003960632006,65.0638401484257,0.));
#163608=CARTESIAN_POINT('Ctrl Pts',(32.3003960632006,65.0638401484257,12.));
#163609=CARTESIAN_POINT('Ctrl Pts',(32.2817897504807,65.0469209207563,0.));
#163610=CARTESIAN_POINT('Ctrl Pts',(32.2817897504807,65.0469209207563,12.));
#163611=CARTESIAN_POINT('Ctrl Pts',(32.2632290527862,65.03001083788,0.));
#163612=CARTESIAN_POINT('Ctrl Pts',(32.2632290527862,65.03001083788,12.));
#163613=CARTESIAN_POINT('Ctrl Pts',(32.2447140118422,65.0131100130158,0.));
#163614=CARTESIAN_POINT('Ctrl Pts',(32.2447140118422,65.0131100130158,12.));
#163615=CARTESIAN_POINT('Ctrl Pts',(32.2262446694512,64.9962185598462,0.));
#163616=CARTESIAN_POINT('Ctrl Pts',(32.2262446694512,64.9962185598462,12.));
#163617=CARTESIAN_POINT('Ctrl Pts',(32.207821067485,64.9793365925178,0.));
#163618=CARTESIAN_POINT('Ctrl Pts',(32.207821067485,64.9793365925178,12.));
#163619=CARTESIAN_POINT('Ctrl Pts',(32.189443247888,64.9624642256461,0.));
#163620=CARTESIAN_POINT('Ctrl Pts',(32.189443247888,64.9624642256461,12.));
#163621=CARTESIAN_POINT('Ctrl Pts',(32.1711112526854,64.9456015743193,0.));
#163622=CARTESIAN_POINT('Ctrl Pts',(32.1711112526854,64.9456015743193,12.));
#163623=CARTESIAN_POINT('Ctrl Pts',(32.152825123983,64.9287487541015,0.));
#163624=CARTESIAN_POINT('Ctrl Pts',(32.152825123983,64.9287487541015,12.));
#163625=CARTESIAN_POINT('Ctrl Pts',(32.1345849039674,64.9119058810367,0.));
#163626=CARTESIAN_POINT('Ctrl Pts',(32.1345849039674,64.9119058810367,12.));
#163627=CARTESIAN_POINT('Ctrl Pts',(32.1163906348983,64.8950730716501,0.));
#163628=CARTESIAN_POINT('Ctrl Pts',(32.1163906348983,64.8950730716501,12.));
#163629=CARTESIAN_POINT('Ctrl Pts',(32.0982423591112,64.8782504429527,0.));
#163630=CARTESIAN_POINT('Ctrl Pts',(32.0982423591112,64.8782504429527,12.));
#163631=CARTESIAN_POINT('Ctrl Pts',(32.0801401190244,64.8614381124455,0.));
#163632=CARTESIAN_POINT('Ctrl Pts',(32.0801401190244,64.8614381124455,12.));
#163633=CARTESIAN_POINT('Ctrl Pts',(32.0620839571409,64.8446361981234,0.));
#163634=CARTESIAN_POINT('Ctrl Pts',(32.0620839571409,64.8446361981234,12.));
#163635=CARTESIAN_POINT('Ctrl Pts',(32.0440739160476,64.8278448184785,0.));
#163636=CARTESIAN_POINT('Ctrl Pts',(32.0440739160476,64.8278448184785,12.));
#163637=CARTESIAN_POINT('Ctrl Pts',(32.0261100384092,64.811064092502,0.));
#163638=CARTESIAN_POINT('Ctrl Pts',(32.0261100384092,64.811064092502,12.));
#163639=CARTESIAN_POINT('Ctrl Pts',(32.0081923669677,64.7942941396883,0.));
#163640=CARTESIAN_POINT('Ctrl Pts',(32.0081923669677,64.7942941396883,12.));
#163641=CARTESIAN_POINT('Ctrl Pts',(31.9903209445521,64.7775350800404,0.));
#163642=CARTESIAN_POINT('Ctrl Pts',(31.9903209445521,64.7775350800404,12.));
#163643=CARTESIAN_POINT('Ctrl Pts',(31.972495814079,64.7607870340738,0.));
#163644=CARTESIAN_POINT('Ctrl Pts',(31.972495814079,64.7607870340738,12.));
#163645=CARTESIAN_POINT('Ctrl Pts',(31.9547170185533,64.7440501228201,0.));
#163646=CARTESIAN_POINT('Ctrl Pts',(31.9547170185533,64.7440501228201,12.));
#163647=CARTESIAN_POINT('Ctrl Pts',(31.9369846010613,64.727324467829,0.));
#163648=CARTESIAN_POINT('Ctrl Pts',(31.9369846010613,64.727324467829,12.));
#163649=CARTESIAN_POINT('Ctrl Pts',(31.9192986047702,64.7106101911723,0.));
#163650=CARTESIAN_POINT('Ctrl Pts',(31.9192986047702,64.7106101911723,12.));
#163651=CARTESIAN_POINT('Ctrl Pts',(31.9016590729371,64.6939074154491,0.));
#163652=CARTESIAN_POINT('Ctrl Pts',(31.9016590729371,64.6939074154491,12.));
#163653=CARTESIAN_POINT('Ctrl Pts',(31.8840660489106,64.6772162637905,0.));
#163654=CARTESIAN_POINT('Ctrl Pts',(31.8840660489106,64.6772162637905,12.));
#163655=CARTESIAN_POINT('Ctrl Pts',(31.8665195761312,64.6605368598631,0.));
#163656=CARTESIAN_POINT('Ctrl Pts',(31.8665195761312,64.6605368598631,12.));
#163657=CARTESIAN_POINT('Ctrl Pts',(31.849019698125,64.6438693278718,0.));
#163658=CARTESIAN_POINT('Ctrl Pts',(31.849019698125,64.6438693278718,12.));
#163659=CARTESIAN_POINT('Ctrl Pts',(31.8315664585027,64.627213792563,0.));
#163660=CARTESIAN_POINT('Ctrl Pts',(31.8315664585027,64.627213792563,12.));
#163661=CARTESIAN_POINT('Ctrl Pts',(31.8141599009684,64.6105703792311,0.));
#163662=CARTESIAN_POINT('Ctrl Pts',(31.8141599009684,64.6105703792311,12.));
#163663=CARTESIAN_POINT('Ctrl Pts',(31.7968000693218,64.5939392137233,0.));
#163664=CARTESIAN_POINT('Ctrl Pts',(31.7968000693218,64.5939392137233,12.));
#163665=CARTESIAN_POINT('Ctrl Pts',(31.7794870074583,64.5773204224429,0.));
#163666=CARTESIAN_POINT('Ctrl Pts',(31.7794870074583,64.5773204224429,12.));
#163667=CARTESIAN_POINT('Ctrl Pts',(31.7622207593637,64.5607141323527,0.));
#163668=CARTESIAN_POINT('Ctrl Pts',(31.7622207593637,64.5607141323527,12.));
#163669=CARTESIAN_POINT('Ctrl Pts',(31.7450013691117,64.544120470978,0.));
#163670=CARTESIAN_POINT('Ctrl Pts',(31.7450013691117,64.544120470978,12.));
#163671=CARTESIAN_POINT('Ctrl Pts',(31.7278288808736,64.5275395664134,0.));
#163672=CARTESIAN_POINT('Ctrl Pts',(31.7278288808736,64.5275395664134,12.));
#163673=CARTESIAN_POINT('Ctrl Pts',(31.7107033389204,64.5109715473277,0.));
#163674=CARTESIAN_POINT('Ctrl Pts',(31.7107033389204,64.5109715473277,12.));
#163675=CARTESIAN_POINT('Ctrl Pts',(31.6936247876228,64.4944165429672,0.));
#163676=CARTESIAN_POINT('Ctrl Pts',(31.6936247876228,64.4944165429672,12.));
#163677=CARTESIAN_POINT('Ctrl Pts',(31.6765932714456,64.4778746831598,0.));
#163678=CARTESIAN_POINT('Ctrl Pts',(31.6765932714456,64.4778746831598,12.));
#163679=CARTESIAN_POINT('Ctrl Pts',(31.6596088349468,64.4613460983186,0.));
#163680=CARTESIAN_POINT('Ctrl Pts',(31.6596088349468,64.4613460983186,12.));
#163681=CARTESIAN_POINT('Ctrl Pts',(31.6426715227865,64.4448309194499,0.));
#163682=CARTESIAN_POINT('Ctrl Pts',(31.6426715227865,64.4448309194499,12.));
#163683=CARTESIAN_POINT('Ctrl Pts',(31.6257813797281,64.4283292781553,0.));
#163684=CARTESIAN_POINT('Ctrl Pts',(31.6257813797281,64.4283292781553,12.));
#163685=CARTESIAN_POINT('Ctrl Pts',(31.6089384506399,64.4118413066386,0.));
#163686=CARTESIAN_POINT('Ctrl Pts',(31.6089384506399,64.4118413066386,12.));
#163687=CARTESIAN_POINT('Ctrl Pts',(31.5921427804879,64.3953671377071,0.));
#163688=CARTESIAN_POINT('Ctrl Pts',(31.5921427804879,64.3953671377071,12.));
#163689=CARTESIAN_POINT('Ctrl Pts',(31.5753944143355,64.3789069047768,0.));
#163690=CARTESIAN_POINT('Ctrl Pts',(31.5753944143355,64.3789069047768,12.));
#163691=CARTESIAN_POINT('Ctrl Pts',(31.5586933973531,64.3624607418798,0.));
#163692=CARTESIAN_POINT('Ctrl Pts',(31.5586933973531,64.3624607418798,12.));
#163693=CARTESIAN_POINT('Ctrl Pts',(31.5420397748198,64.34602878367,0.));
#163694=CARTESIAN_POINT('Ctrl Pts',(31.5420397748198,64.34602878367,12.));
#163695=CARTESIAN_POINT('Ctrl Pts',(31.5254335921239,64.3296111654273,0.));
#163696=CARTESIAN_POINT('Ctrl Pts',(31.5254335921239,64.3296111654273,12.));
#163697=CARTESIAN_POINT('Ctrl Pts',(31.5088748947565,64.3132080230603,0.));
#163698=CARTESIAN_POINT('Ctrl Pts',(31.5088748947565,64.3132080230603,12.));
#163699=CARTESIAN_POINT('Ctrl Pts',(31.4923637283109,64.2968194931113,0.));
#163700=CARTESIAN_POINT('Ctrl Pts',(31.4923637283109,64.2968194931113,12.));
#163701=CARTESIAN_POINT('Ctrl Pts',(31.4759001384922,64.2804457127633,0.));
#163702=CARTESIAN_POINT('Ctrl Pts',(31.4759001384922,64.2804457127633,12.));
#163703=CARTESIAN_POINT('Ctrl Pts',(31.4594841711188,64.264086819846,0.));
#163704=CARTESIAN_POINT('Ctrl Pts',(31.4594841711188,64.264086819846,12.));
#163705=CARTESIAN_POINT('Ctrl Pts',(31.4431158721229,64.2477429528408,0.));
#163706=CARTESIAN_POINT('Ctrl Pts',(31.4431158721229,64.2477429528408,12.));
#163707=CARTESIAN_POINT('Ctrl Pts',(31.426795287544,64.2314142508843,0.));
#163708=CARTESIAN_POINT('Ctrl Pts',(31.426795287544,64.2314142508843,12.));
#163709=CARTESIAN_POINT('Ctrl Pts',(31.4105224635298,64.2151008537733,0.));
#163710=CARTESIAN_POINT('Ctrl Pts',(31.4105224635298,64.2151008537733,12.));
#163711=CARTESIAN_POINT('Ctrl Pts',(31.3942974463458,64.1988029019733,0.));
#163712=CARTESIAN_POINT('Ctrl Pts',(31.3942974463458,64.1988029019733,12.));
#163713=CARTESIAN_POINT('Ctrl Pts',(31.3781202823758,64.1825205366231,0.));
#163714=CARTESIAN_POINT('Ctrl Pts',(31.3781202823758,64.1825205366231,12.));
#163715=CARTESIAN_POINT('Ctrl Pts',(31.3619910181222,64.1662538995407,0.));
#163716=CARTESIAN_POINT('Ctrl Pts',(31.3619910181222,64.1662538995407,12.));
#163717=CARTESIAN_POINT('Ctrl Pts',(31.3459097001995,64.150003133226,0.));
#163718=CARTESIAN_POINT('Ctrl Pts',(31.3459097001995,64.150003133226,12.));
#163719=CARTESIAN_POINT('Ctrl Pts',(31.3298763753366,64.1337683808667,0.));
#163720=CARTESIAN_POINT('Ctrl Pts',(31.3298763753366,64.1337683808667,12.));
#163721=CARTESIAN_POINT('Ctrl Pts',(31.3138910903852,64.1175497863475,0.));
#163722=CARTESIAN_POINT('Ctrl Pts',(31.3138910903852,64.1175497863475,12.));
#163723=CARTESIAN_POINT('Ctrl Pts',(31.2979538923213,64.1013474942554,0.));
#163724=CARTESIAN_POINT('Ctrl Pts',(31.2979538923213,64.1013474942554,12.));
#163725=CARTESIAN_POINT('Ctrl Pts',(31.2820648282451,64.0851616498861,0.));
#163726=CARTESIAN_POINT('Ctrl Pts',(31.2820648282451,64.0851616498861,12.));
#163727=CARTESIAN_POINT('Ctrl Pts',(31.2662239453734,64.0689923992475,0.));
#163728=CARTESIAN_POINT('Ctrl Pts',(31.2662239453734,64.0689923992475,12.));
#163729=CARTESIAN_POINT('Ctrl Pts',(31.2504312910457,64.0528398890671,0.));
#163730=CARTESIAN_POINT('Ctrl Pts',(31.2504312910457,64.0528398890671,12.));
#163731=CARTESIAN_POINT('Ctrl Pts',(31.23468691273,64.036704266799,0.));
#163732=CARTESIAN_POINT('Ctrl Pts',(31.23468691273,64.036704266799,12.));
#163733=CARTESIAN_POINT('Ctrl Pts',(31.2189908580245,64.0205856806298,0.));
#163734=CARTESIAN_POINT('Ctrl Pts',(31.2189908580245,64.0205856806298,12.));
#163735=CARTESIAN_POINT('Ctrl Pts',(31.2033431746558,64.004484279483,0.));
#163736=CARTESIAN_POINT('Ctrl Pts',(31.2033431746558,64.004484279483,12.));
#163737=CARTESIAN_POINT('Ctrl Pts',(31.1877439104717,63.9884002130209,0.));
#163738=CARTESIAN_POINT('Ctrl Pts',(31.1877439104717,63.9884002130209,12.));
#163739=CARTESIAN_POINT('Ctrl Pts',(31.1721931134488,63.972333631655,0.));
#163740=CARTESIAN_POINT('Ctrl Pts',(31.1721931134488,63.972333631655,12.));
#163741=CARTESIAN_POINT('Ctrl Pts',(31.1566908316992,63.9562846865566,0.));
#163742=CARTESIAN_POINT('Ctrl Pts',(31.1566908316992,63.9562846865566,12.));
#163743=CARTESIAN_POINT('Ctrl Pts',(31.1412371134727,63.9402535296651,0.));
#163744=CARTESIAN_POINT('Ctrl Pts',(31.1412371134727,63.9402535296651,12.));
#163745=CARTESIAN_POINT('Ctrl Pts',(31.1258320071545,63.9242403136954,0.));
#163746=CARTESIAN_POINT('Ctrl Pts',(31.1258320071545,63.9242403136954,12.));
#163747=CARTESIAN_POINT('Ctrl Pts',(31.1104755612606,63.9082451921447,0.));
#163748=CARTESIAN_POINT('Ctrl Pts',(31.1104755612606,63.9082451921447,12.));
#163749=CARTESIAN_POINT('Ctrl Pts',(31.0951678244454,63.8922683192963,0.));
#163750=CARTESIAN_POINT('Ctrl Pts',(31.0951678244454,63.8922683192963,12.));
#163751=CARTESIAN_POINT('Ctrl Pts',(31.079908845504,63.8763098502235,0.));
#163752=CARTESIAN_POINT('Ctrl Pts',(31.079908845504,63.8763098502235,12.));
#163753=CARTESIAN_POINT('Ctrl Pts',(31.0646986733723,63.8603699407922,0.));
#163754=CARTESIAN_POINT('Ctrl Pts',(31.0646986733723,63.8603699407922,12.));
#163755=CARTESIAN_POINT('Ctrl Pts',(31.0495373571217,63.8444487476615,0.));
#163756=CARTESIAN_POINT('Ctrl Pts',(31.0495373571217,63.8444487476615,12.));
#163757=CARTESIAN_POINT('Ctrl Pts',(31.0344249459544,63.8285464282857,0.));
#163758=CARTESIAN_POINT('Ctrl Pts',(31.0344249459544,63.8285464282857,12.));
#163759=CARTESIAN_POINT('Ctrl Pts',(31.0193614892177,63.8126631409376,0.));
#163760=CARTESIAN_POINT('Ctrl Pts',(31.0193614892177,63.8126631409376,12.));
#163761=CARTESIAN_POINT('Ctrl Pts',(31.0043470364112,63.7967990447288,0.));
#163762=CARTESIAN_POINT('Ctrl Pts',(31.0043470364112,63.7967990447288,12.));
#163763=CARTESIAN_POINT('Ctrl Pts',(30.9893816371907,63.7809542996258,0.));
#163764=CARTESIAN_POINT('Ctrl Pts',(30.9893816371907,63.7809542996258,12.));
#163765=CARTESIAN_POINT('Ctrl Pts',(30.9744653413679,63.7651290664713,0.));
#163766=CARTESIAN_POINT('Ctrl Pts',(30.9744653413679,63.7651290664713,12.));
#163767=CARTESIAN_POINT('Ctrl Pts',(30.9595981989091,63.7493235069844,0.));
#163768=CARTESIAN_POINT('Ctrl Pts',(30.9595981989091,63.7493235069844,12.));
#163769=CARTESIAN_POINT('Ctrl Pts',(30.9447802599345,63.733537783742,0.));
#163770=CARTESIAN_POINT('Ctrl Pts',(30.9447802599345,63.733537783742,12.));
#163771=CARTESIAN_POINT('Ctrl Pts',(30.9300115747113,63.7177720601604,0.));
#163772=CARTESIAN_POINT('Ctrl Pts',(30.9300115747113,63.7177720601604,12.));
#163773=CARTESIAN_POINT('Ctrl Pts',(30.9152921936471,63.7020265004805,0.));
#163774=CARTESIAN_POINT('Ctrl Pts',(30.9152921936471,63.7020265004805,12.));
#163775=CARTESIAN_POINT('Ctrl Pts',(30.9006221672703,63.6863012697354,0.));
#163776=CARTESIAN_POINT('Ctrl Pts',(30.9006221672703,63.6863012697354,12.));
#163777=CARTESIAN_POINT('Ctrl Pts',(30.8860015462488,63.6705965337996,0.));
#163778=CARTESIAN_POINT('Ctrl Pts',(30.8860015462488,63.6705965337996,12.));
#163779=CARTESIAN_POINT('Ctrl Pts',(30.8714303814202,63.6549124594681,0.));
#163780=CARTESIAN_POINT('Ctrl Pts',(30.8714303814202,63.6549124594681,12.));
#163781=CARTESIAN_POINT('Ctrl Pts',(30.8569087238131,63.6392492145233,0.));
#163782=CARTESIAN_POINT('Ctrl Pts',(30.8569087238131,63.6392492145233,12.));
#163783=CARTESIAN_POINT('Ctrl Pts',(30.8424366246665,63.6236069678041,0.));
#163784=CARTESIAN_POINT('Ctrl Pts',(30.8424366246665,63.6236069678041,12.));
#163785=CARTESIAN_POINT('Ctrl Pts',(30.8280141354447,63.6079858892747,0.));
#163786=CARTESIAN_POINT('Ctrl Pts',(30.8280141354447,63.6079858892747,12.));
#163787=CARTESIAN_POINT('Ctrl Pts',(30.8136413077999,63.5923861498964,0.));
#163788=CARTESIAN_POINT('Ctrl Pts',(30.8136413077999,63.5923861498964,12.));
#163789=CARTESIAN_POINT('Ctrl Pts',(30.7993181935265,63.5768079214868,0.));
#163790=CARTESIAN_POINT('Ctrl Pts',(30.7993181935265,63.5768079214868,12.));
#163791=CARTESIAN_POINT('Ctrl Pts',(30.7850448445207,63.5612513766005,0.));
#163792=CARTESIAN_POINT('Ctrl Pts',(30.7850448445207,63.5612513766005,12.));
#163793=CARTESIAN_POINT('Ctrl Pts',(30.7708213127169,63.5457166883558,0.));
#163794=CARTESIAN_POINT('Ctrl Pts',(30.7708213127169,63.5457166883558,12.));
#163795=CARTESIAN_POINT('Ctrl Pts',(30.7566476500772,63.5302040304173,0.));
#163796=CARTESIAN_POINT('Ctrl Pts',(30.7566476500772,63.5302040304173,12.));
#163797=CARTESIAN_POINT('Ctrl Pts',(30.7425239087294,63.514713577392,0.));
#163798=CARTESIAN_POINT('Ctrl Pts',(30.7425239087294,63.514713577392,12.));
#163799=CARTESIAN_POINT('Ctrl Pts',(30.7284501410827,63.4992455051805,0.));
#163800=CARTESIAN_POINT('Ctrl Pts',(30.7284501410827,63.4992455051805,12.));
#163801=CARTESIAN_POINT('Ctrl Pts',(30.7144263999259,63.4837999912758,0.));
#163802=CARTESIAN_POINT('Ctrl Pts',(30.7144263999259,63.4837999912758,12.));
#163803=CARTESIAN_POINT('Ctrl Pts',(30.7004527385806,63.4683772152497,0.));
#163804=CARTESIAN_POINT('Ctrl Pts',(30.7004527385806,63.4683772152497,12.));
#163805=CARTESIAN_POINT('Ctrl Pts',(30.686529210791,63.4529773584211,0.));
#163806=CARTESIAN_POINT('Ctrl Pts',(30.686529210791,63.4529773584211,12.));
#163807=CARTESIAN_POINT('Ctrl Pts',(30.6726558704301,63.4376006029575,0.));
#163808=CARTESIAN_POINT('Ctrl Pts',(30.6726558704301,63.4376006029575,12.));
#163809=CARTESIAN_POINT('Ctrl Pts',(30.6588327712482,63.4222471311236,0.));
#163810=CARTESIAN_POINT('Ctrl Pts',(30.6588327712482,63.4222471311236,12.));
#163811=CARTESIAN_POINT('Ctrl Pts',(30.6450599666135,63.4069171245094,0.));
#163812=CARTESIAN_POINT('Ctrl Pts',(30.6450599666135,63.4069171245094,12.));
#163813=CARTESIAN_POINT('Ctrl Pts',(30.6313375092084,63.3916107631421,0.));
#163814=CARTESIAN_POINT('Ctrl Pts',(30.6313375092084,63.3916107631421,12.));
#163815=CARTESIAN_POINT('Ctrl Pts',(30.6176654515988,63.3763282271838,0.));
#163816=CARTESIAN_POINT('Ctrl Pts',(30.6176654515988,63.3763282271838,12.));
#163817=CARTESIAN_POINT('Ctrl Pts',(30.6040438469089,63.3610696989599,0.));
#163818=CARTESIAN_POINT('Ctrl Pts',(30.6040438469089,63.3610696989599,12.));
#163819=CARTESIAN_POINT('Ctrl Pts',(30.5904727493707,63.3458353646144,0.));
#163820=CARTESIAN_POINT('Ctrl Pts',(30.5904727493707,63.3458353646144,12.));
#163821=CARTESIAN_POINT('Ctrl Pts',(30.5769522151147,63.330625416509,0.));
#163822=CARTESIAN_POINT('Ctrl Pts',(30.5769522151147,63.330625416509,12.));
#163823=CARTESIAN_POINT('Ctrl Pts',(30.5634823022358,63.315440053435,0.));
#163824=CARTESIAN_POINT('Ctrl Pts',(30.5634823022358,63.315440053435,12.));
#163825=CARTESIAN_POINT('Ctrl Pts',(30.5500630691342,63.300279475605,0.));
#163826=CARTESIAN_POINT('Ctrl Pts',(30.5500630691342,63.300279475605,12.));
#163827=CARTESIAN_POINT('Ctrl Pts',(30.5366945730503,63.2851438802462,0.));
#163828=CARTESIAN_POINT('Ctrl Pts',(30.5366945730503,63.2851438802462,12.));
#163829=CARTESIAN_POINT('Ctrl Pts',(30.5233768687875,63.2700334577661,0.));
#163830=CARTESIAN_POINT('Ctrl Pts',(30.5233768687875,63.2700334577661,12.));
#163831=CARTESIAN_POINT('Ctrl Pts',(30.5101100066683,63.2549483856268,0.));
#163832=CARTESIAN_POINT('Ctrl Pts',(30.5101100066683,63.2549483856268,12.));
#163833=CARTESIAN_POINT('Ctrl Pts',(30.4968940345027,63.2398888342612,0.));
#163834=CARTESIAN_POINT('Ctrl Pts',(30.4968940345027,63.2398888342612,12.));
#163835=CARTESIAN_POINT('Ctrl Pts',(30.4837290015011,63.2248549788272,0.));
#163836=CARTESIAN_POINT('Ctrl Pts',(30.4837290015011,63.2248549788272,12.));
#163837=CARTESIAN_POINT('Ctrl Pts',(30.470614961416,63.2098470086636,0.));
#163838=CARTESIAN_POINT('Ctrl Pts',(30.470614961416,63.2098470086636,12.));
#163839=CARTESIAN_POINT('Ctrl Pts',(30.4575519763305,63.1948651386868,0.));
#163840=CARTESIAN_POINT('Ctrl Pts',(30.4575519763305,63.1948651386868,12.));
#163841=CARTESIAN_POINT('Ctrl Pts',(30.4445401192324,63.1799096171757,0.));
#163842=CARTESIAN_POINT('Ctrl Pts',(30.4445401192324,63.1799096171757,12.));
#163843=CARTESIAN_POINT('Ctrl Pts',(30.431579465967,63.1649807016766,0.));
#163844=CARTESIAN_POINT('Ctrl Pts',(30.431579465967,63.1649807016766,12.));
#163845=CARTESIAN_POINT('Ctrl Pts',(30.4186700875598,63.1500786361382,0.));
#163846=CARTESIAN_POINT('Ctrl Pts',(30.4186700875598,63.1500786361382,12.));
#163847=CARTESIAN_POINT('Ctrl Pts',(30.4058120432259,63.1352036298512,0.));
#163848=CARTESIAN_POINT('Ctrl Pts',(30.4058120432259,63.1352036298512,12.));
#163849=CARTESIAN_POINT('Ctrl Pts',(30.3930053710592,63.1203558300911,0.));
#163850=CARTESIAN_POINT('Ctrl Pts',(30.3930053710592,63.1203558300911,12.));
#163851=CARTESIAN_POINT('Ctrl Pts',(30.3802500880565,63.1055353202641,0.));
#163852=CARTESIAN_POINT('Ctrl Pts',(30.3802500880565,63.1055353202641,12.));
#163853=CARTESIAN_POINT('Ctrl Pts',(30.3700869762658,63.0937007763826,0.));
#163854=CARTESIAN_POINT('Ctrl Pts',(30.3700869762658,63.0937007763826,12.));
#163855=CARTESIAN_POINT('Ctrl Pts',(30.3624877680747,63.0848371718274,0.));
#163856=CARTESIAN_POINT('Ctrl Pts',(30.3624877680747,63.0848371718274,12.));
#163857=CARTESIAN_POINT('Ctrl Pts',(30.3574319069365,63.0789335700774,0.));
#163858=CARTESIAN_POINT('Ctrl Pts',(30.3574319069365,63.0789335700774,12.));
#163859=CARTESIAN_POINT('Ctrl Pts',(30.3549065457811,63.0759831361898,0.));
#163860=CARTESIAN_POINT('Ctrl Pts',(30.3549065457811,63.0759831361898,12.));
#163861=CARTESIAN_POINT('',(30.3549065457811,63.0759831361898,12.));
#163862=CARTESIAN_POINT('Ctrl Pts',(30.3549065457811,63.0759831361898,12.));
#163863=CARTESIAN_POINT('Ctrl Pts',(30.3574319069365,63.0789335700774,12.));
#163864=CARTESIAN_POINT('Ctrl Pts',(30.3624877680747,63.0848371718274,12.));
#163865=CARTESIAN_POINT('Ctrl Pts',(30.3700869762658,63.0937007763826,12.));
#163866=CARTESIAN_POINT('Ctrl Pts',(30.3802500880565,63.1055353202641,12.));
#163867=CARTESIAN_POINT('Ctrl Pts',(30.3930053710592,63.1203558300911,12.));
#163868=CARTESIAN_POINT('Ctrl Pts',(30.4058120432259,63.1352036298512,12.));
#163869=CARTESIAN_POINT('Ctrl Pts',(30.4186700875598,63.1500786361382,12.));
#163870=CARTESIAN_POINT('Ctrl Pts',(30.431579465967,63.1649807016766,12.));
#163871=CARTESIAN_POINT('Ctrl Pts',(30.4445401192324,63.1799096171757,12.));
#163872=CARTESIAN_POINT('Ctrl Pts',(30.4575519763305,63.1948651386868,12.));
#163873=CARTESIAN_POINT('Ctrl Pts',(30.470614961416,63.2098470086636,12.));
#163874=CARTESIAN_POINT('Ctrl Pts',(30.4837290015011,63.2248549788272,12.));
#163875=CARTESIAN_POINT('Ctrl Pts',(30.4968940345027,63.2398888342612,12.));
#163876=CARTESIAN_POINT('Ctrl Pts',(30.5101100066683,63.2549483856268,12.));
#163877=CARTESIAN_POINT('Ctrl Pts',(30.5233768687875,63.2700334577661,12.));
#163878=CARTESIAN_POINT('Ctrl Pts',(30.5366945730503,63.2851438802462,12.));
#163879=CARTESIAN_POINT('Ctrl Pts',(30.5500630691342,63.300279475605,12.));
#163880=CARTESIAN_POINT('Ctrl Pts',(30.5634823022358,63.315440053435,12.));
#163881=CARTESIAN_POINT('Ctrl Pts',(30.5769522151147,63.330625416509,12.));
#163882=CARTESIAN_POINT('Ctrl Pts',(30.5904727493707,63.3458353646144,12.));
#163883=CARTESIAN_POINT('Ctrl Pts',(30.6040438469089,63.3610696989599,12.));
#163884=CARTESIAN_POINT('Ctrl Pts',(30.6176654515988,63.3763282271838,12.));
#163885=CARTESIAN_POINT('Ctrl Pts',(30.6313375092084,63.3916107631421,12.));
#163886=CARTESIAN_POINT('Ctrl Pts',(30.6450599666135,63.4069171245094,12.));
#163887=CARTESIAN_POINT('Ctrl Pts',(30.6588327712482,63.4222471311236,12.));
#163888=CARTESIAN_POINT('Ctrl Pts',(30.6726558704301,63.4376006029575,12.));
#163889=CARTESIAN_POINT('Ctrl Pts',(30.686529210791,63.4529773584211,12.));
#163890=CARTESIAN_POINT('Ctrl Pts',(30.7004527385806,63.4683772152497,12.));
#163891=CARTESIAN_POINT('Ctrl Pts',(30.7144263999259,63.4837999912758,12.));
#163892=CARTESIAN_POINT('Ctrl Pts',(30.7284501410827,63.4992455051805,12.));
#163893=CARTESIAN_POINT('Ctrl Pts',(30.7425239087294,63.514713577392,12.));
#163894=CARTESIAN_POINT('Ctrl Pts',(30.7566476500772,63.5302040304173,12.));
#163895=CARTESIAN_POINT('Ctrl Pts',(30.7708213127169,63.5457166883558,12.));
#163896=CARTESIAN_POINT('Ctrl Pts',(30.7850448445207,63.5612513766005,12.));
#163897=CARTESIAN_POINT('Ctrl Pts',(30.7993181935265,63.5768079214868,12.));
#163898=CARTESIAN_POINT('Ctrl Pts',(30.8136413077999,63.5923861498964,12.));
#163899=CARTESIAN_POINT('Ctrl Pts',(30.8280141354447,63.6079858892747,12.));
#163900=CARTESIAN_POINT('Ctrl Pts',(30.8424366246665,63.6236069678041,12.));
#163901=CARTESIAN_POINT('Ctrl Pts',(30.8569087238131,63.6392492145233,12.));
#163902=CARTESIAN_POINT('Ctrl Pts',(30.8714303814202,63.6549124594681,12.));
#163903=CARTESIAN_POINT('Ctrl Pts',(30.8860015462488,63.6705965337996,12.));
#163904=CARTESIAN_POINT('Ctrl Pts',(30.9006221672703,63.6863012697354,12.));
#163905=CARTESIAN_POINT('Ctrl Pts',(30.9152921936471,63.7020265004805,12.));
#163906=CARTESIAN_POINT('Ctrl Pts',(30.9300115747113,63.7177720601604,12.));
#163907=CARTESIAN_POINT('Ctrl Pts',(30.9447802599345,63.733537783742,12.));
#163908=CARTESIAN_POINT('Ctrl Pts',(30.9595981989091,63.7493235069844,12.));
#163909=CARTESIAN_POINT('Ctrl Pts',(30.9744653413679,63.7651290664713,12.));
#163910=CARTESIAN_POINT('Ctrl Pts',(30.9893816371907,63.7809542996258,12.));
#163911=CARTESIAN_POINT('Ctrl Pts',(31.0043470364112,63.7967990447288,12.));
#163912=CARTESIAN_POINT('Ctrl Pts',(31.0193614892177,63.8126631409376,12.));
#163913=CARTESIAN_POINT('Ctrl Pts',(31.0344249459544,63.8285464282857,12.));
#163914=CARTESIAN_POINT('Ctrl Pts',(31.0495373571217,63.8444487476615,12.));
#163915=CARTESIAN_POINT('Ctrl Pts',(31.0646986733723,63.8603699407922,12.));
#163916=CARTESIAN_POINT('Ctrl Pts',(31.079908845504,63.8763098502235,12.));
#163917=CARTESIAN_POINT('Ctrl Pts',(31.0951678244454,63.8922683192963,12.));
#163918=CARTESIAN_POINT('Ctrl Pts',(31.1104755612606,63.9082451921447,12.));
#163919=CARTESIAN_POINT('Ctrl Pts',(31.1258320071545,63.9242403136954,12.));
#163920=CARTESIAN_POINT('Ctrl Pts',(31.1412371134727,63.9402535296651,12.));
#163921=CARTESIAN_POINT('Ctrl Pts',(31.1566908316992,63.9562846865566,12.));
#163922=CARTESIAN_POINT('Ctrl Pts',(31.1721931134488,63.972333631655,12.));
#163923=CARTESIAN_POINT('Ctrl Pts',(31.1877439104717,63.9884002130209,12.));
#163924=CARTESIAN_POINT('Ctrl Pts',(31.2033431746558,64.004484279483,12.));
#163925=CARTESIAN_POINT('Ctrl Pts',(31.2189908580245,64.0205856806298,12.));
#163926=CARTESIAN_POINT('Ctrl Pts',(31.23468691273,64.036704266799,12.));
#163927=CARTESIAN_POINT('Ctrl Pts',(31.2504312910457,64.0528398890671,12.));
#163928=CARTESIAN_POINT('Ctrl Pts',(31.2662239453734,64.0689923992475,12.));
#163929=CARTESIAN_POINT('Ctrl Pts',(31.2820648282451,64.0851616498861,12.));
#163930=CARTESIAN_POINT('Ctrl Pts',(31.2979538923213,64.1013474942554,12.));
#163931=CARTESIAN_POINT('Ctrl Pts',(31.3138910903852,64.1175497863475,12.));
#163932=CARTESIAN_POINT('Ctrl Pts',(31.3298763753366,64.1337683808667,12.));
#163933=CARTESIAN_POINT('Ctrl Pts',(31.3459097001995,64.150003133226,12.));
#163934=CARTESIAN_POINT('Ctrl Pts',(31.3619910181222,64.1662538995407,12.));
#163935=CARTESIAN_POINT('Ctrl Pts',(31.3781202823758,64.1825205366231,12.));
#163936=CARTESIAN_POINT('Ctrl Pts',(31.3942974463458,64.1988029019733,12.));
#163937=CARTESIAN_POINT('Ctrl Pts',(31.4105224635298,64.2151008537733,12.));
#163938=CARTESIAN_POINT('Ctrl Pts',(31.426795287544,64.2314142508843,12.));
#163939=CARTESIAN_POINT('Ctrl Pts',(31.4431158721229,64.2477429528408,12.));
#163940=CARTESIAN_POINT('Ctrl Pts',(31.4594841711188,64.264086819846,12.));
#163941=CARTESIAN_POINT('Ctrl Pts',(31.4759001384922,64.2804457127633,12.));
#163942=CARTESIAN_POINT('Ctrl Pts',(31.4923637283109,64.2968194931113,12.));
#163943=CARTESIAN_POINT('Ctrl Pts',(31.5088748947565,64.3132080230603,12.));
#163944=CARTESIAN_POINT('Ctrl Pts',(31.5254335921239,64.3296111654273,12.));
#163945=CARTESIAN_POINT('Ctrl Pts',(31.5420397748198,64.34602878367,12.));
#163946=CARTESIAN_POINT('Ctrl Pts',(31.5586933973531,64.3624607418798,12.));
#163947=CARTESIAN_POINT('Ctrl Pts',(31.5753944143355,64.3789069047768,12.));
#163948=CARTESIAN_POINT('Ctrl Pts',(31.5921427804879,64.3953671377071,12.));
#163949=CARTESIAN_POINT('Ctrl Pts',(31.6089384506399,64.4118413066386,12.));
#163950=CARTESIAN_POINT('Ctrl Pts',(31.6257813797281,64.4283292781553,12.));
#163951=CARTESIAN_POINT('Ctrl Pts',(31.6426715227865,64.4448309194499,12.));
#163952=CARTESIAN_POINT('Ctrl Pts',(31.6596088349468,64.4613460983186,12.));
#163953=CARTESIAN_POINT('Ctrl Pts',(31.6765932714456,64.4778746831598,12.));
#163954=CARTESIAN_POINT('Ctrl Pts',(31.6936247876228,64.4944165429672,12.));
#163955=CARTESIAN_POINT('Ctrl Pts',(31.7107033389204,64.5109715473277,12.));
#163956=CARTESIAN_POINT('Ctrl Pts',(31.7278288808736,64.5275395664134,12.));
#163957=CARTESIAN_POINT('Ctrl Pts',(31.7450013691117,64.544120470978,12.));
#163958=CARTESIAN_POINT('Ctrl Pts',(31.7622207593637,64.5607141323527,12.));
#163959=CARTESIAN_POINT('Ctrl Pts',(31.7794870074583,64.5773204224429,12.));
#163960=CARTESIAN_POINT('Ctrl Pts',(31.7968000693218,64.5939392137233,12.));
#163961=CARTESIAN_POINT('Ctrl Pts',(31.8141599009684,64.6105703792311,12.));
#163962=CARTESIAN_POINT('Ctrl Pts',(31.8315664585027,64.627213792563,12.));
#163963=CARTESIAN_POINT('Ctrl Pts',(31.849019698125,64.6438693278718,12.));
#163964=CARTESIAN_POINT('Ctrl Pts',(31.8665195761312,64.6605368598631,12.));
#163965=CARTESIAN_POINT('Ctrl Pts',(31.8840660489106,64.6772162637905,12.));
#163966=CARTESIAN_POINT('Ctrl Pts',(31.9016590729371,64.6939074154491,12.));
#163967=CARTESIAN_POINT('Ctrl Pts',(31.9192986047702,64.7106101911723,12.));
#163968=CARTESIAN_POINT('Ctrl Pts',(31.9369846010613,64.727324467829,12.));
#163969=CARTESIAN_POINT('Ctrl Pts',(31.9547170185533,64.7440501228201,12.));
#163970=CARTESIAN_POINT('Ctrl Pts',(31.972495814079,64.7607870340738,12.));
#163971=CARTESIAN_POINT('Ctrl Pts',(31.9903209445521,64.7775350800404,12.));
#163972=CARTESIAN_POINT('Ctrl Pts',(32.0081923669677,64.7942941396883,12.));
#163973=CARTESIAN_POINT('Ctrl Pts',(32.0261100384092,64.811064092502,12.));
#163974=CARTESIAN_POINT('Ctrl Pts',(32.0440739160476,64.8278448184785,12.));
#163975=CARTESIAN_POINT('Ctrl Pts',(32.0620839571409,64.8446361981234,12.));
#163976=CARTESIAN_POINT('Ctrl Pts',(32.0801401190244,64.8614381124455,12.));
#163977=CARTESIAN_POINT('Ctrl Pts',(32.0982423591112,64.8782504429527,12.));
#163978=CARTESIAN_POINT('Ctrl Pts',(32.1163906348983,64.8950730716501,12.));
#163979=CARTESIAN_POINT('Ctrl Pts',(32.1345849039674,64.9119058810367,12.));
#163980=CARTESIAN_POINT('Ctrl Pts',(32.152825123983,64.9287487541015,12.));
#163981=CARTESIAN_POINT('Ctrl Pts',(32.1711112526854,64.9456015743193,12.));
#163982=CARTESIAN_POINT('Ctrl Pts',(32.189443247888,64.9624642256461,12.));
#163983=CARTESIAN_POINT('Ctrl Pts',(32.207821067485,64.9793365925178,12.));
#163984=CARTESIAN_POINT('Ctrl Pts',(32.2262446694512,64.9962185598462,12.));
#163985=CARTESIAN_POINT('Ctrl Pts',(32.2447140118422,65.0131100130158,12.));
#163986=CARTESIAN_POINT('Ctrl Pts',(32.2632290527862,65.03001083788,12.));
#163987=CARTESIAN_POINT('Ctrl Pts',(32.2817897504807,65.0469209207563,12.));
#163988=CARTESIAN_POINT('Ctrl Pts',(32.3003960632006,65.0638401484257,12.));
#163989=CARTESIAN_POINT('Ctrl Pts',(32.3190479492987,65.0807684081282,12.));
#163990=CARTESIAN_POINT('Ctrl Pts',(32.3377453672051,65.0977055875608,12.));
#163991=CARTESIAN_POINT('Ctrl Pts',(32.3564882754212,65.1146515748722,12.));
#163992=CARTESIAN_POINT('Ctrl Pts',(32.3752766325136,65.1316062586588,12.));
#163993=CARTESIAN_POINT('Ctrl Pts',(32.3941103971221,65.1485695279635,12.));
#163994=CARTESIAN_POINT('Ctrl Pts',(32.4129895279615,65.1655412722726,12.));
#163995=CARTESIAN_POINT('Ctrl Pts',(32.4319139838212,65.182521381514,12.));
#163996=CARTESIAN_POINT('Ctrl Pts',(32.450883723561,65.1995097460538,12.));
#163997=CARTESIAN_POINT('Ctrl Pts',(32.4698987061032,65.2165062566924,12.));
#163998=CARTESIAN_POINT('Ctrl Pts',(32.4889588904392,65.2335108046614,12.));
#163999=CARTESIAN_POINT('Ctrl Pts',(32.5080642356328,65.2505232816209,12.));
#164000=CARTESIAN_POINT('Ctrl Pts',(32.5272147008191,65.2675435796558,12.));
#164001=CARTESIAN_POINT('Ctrl Pts',(32.5464102452014,65.2845715912721,12.));
#164002=CARTESIAN_POINT('Ctrl Pts',(32.5656508280421,65.3016072093912,12.));
#164003=CARTESIAN_POINT('Ctrl Pts',(32.5849364086678,65.31865032735,12.));
#164004=CARTESIAN_POINT('Ctrl Pts',(32.6042669464751,65.3357008389004,12.));
#164005=CARTESIAN_POINT('Ctrl Pts',(32.6236424009301,65.3527586382081,12.));
#164006=CARTESIAN_POINT('Ctrl Pts',(32.6430627315674,65.3698236198513,12.));
#164007=CARTESIAN_POINT('Ctrl Pts',(32.662527897981,65.3868956788182,12.));
#164008=CARTESIAN_POINT('Ctrl Pts',(32.6820378598267,65.4039747105038,12.));
#164009=CARTESIAN_POINT('Ctrl Pts',(32.7015925768265,65.4210606107035,12.));
#164010=CARTESIAN_POINT('Ctrl Pts',(32.7211920087684,65.4381532756065,12.));
#164011=CARTESIAN_POINT('Ctrl Pts',(32.7408361155037,65.4552526017905,12.));
#164012=CARTESIAN_POINT('Ctrl Pts',(32.7605248569378,65.4723584862122,12.));
#164013=CARTESIAN_POINT('Ctrl Pts',(32.7802581930287,65.4894708262061,12.));
#164014=CARTESIAN_POINT('Ctrl Pts',(32.8000360837975,65.5065895194928,12.));
#164015=CARTESIAN_POINT('Ctrl Pts',(32.8198584893315,65.5237144641858,12.));
#164016=CARTESIAN_POINT('Ctrl Pts',(32.8397253697865,65.5408455587965,12.));
#164017=CARTESIAN_POINT('Ctrl Pts',(32.8596366853832,65.5579827022421,12.));
#164018=CARTESIAN_POINT('Ctrl Pts',(32.879592396403,65.5751257938473,12.));
#164019=CARTESIAN_POINT('Ctrl Pts',(32.8995924631898,65.5922747333194,12.));
#164020=CARTESIAN_POINT('Ctrl Pts',(32.9196368461463,65.6094294207276,12.));
#164021=CARTESIAN_POINT('Ctrl Pts',(32.9397255057274,65.6265897564783,12.));
#164022=CARTESIAN_POINT('Ctrl Pts',(32.9598584024312,65.6437556412947,12.));
#164023=CARTESIAN_POINT('Ctrl Pts',(32.980035496784,65.6609269761889,12.));
#164024=CARTESIAN_POINT('Ctrl Pts',(33.0002567493573,65.6781036625027,12.));
#164025=CARTESIAN_POINT('Ctrl Pts',(33.0205221207873,65.6952856019533,12.));
#164026=CARTESIAN_POINT('Ctrl Pts',(33.0408315717873,65.7124726966802,12.));
#164027=CARTESIAN_POINT('Ctrl Pts',(33.0611850631582,65.7296648492825,12.));
#164028=CARTESIAN_POINT('Ctrl Pts',(33.081582555798,65.7468619628816,12.));
#164029=CARTESIAN_POINT('Ctrl Pts',(33.1020240106884,65.7640639410661,12.));
#164030=CARTESIAN_POINT('Ctrl Pts',(33.1225093888672,65.7812706877697,12.));
#164031=CARTESIAN_POINT('Ctrl Pts',(33.1430386513976,65.7984821071623,12.));
#164032=CARTESIAN_POINT('Ctrl Pts',(33.16361175934,65.8156981035503,12.));
#164033=CARTESIAN_POINT('Ctrl Pts',(33.1842286737051,65.8329185812375,12.));
#164034=CARTESIAN_POINT('Ctrl Pts',(33.2048893554491,65.8501434445164,12.));
#164035=CARTESIAN_POINT('Ctrl Pts',(33.2255937655649,65.8673725979578,12.));
#164036=CARTESIAN_POINT('Ctrl Pts',(33.2463418651492,65.8846059466372,12.));
#164037=CARTESIAN_POINT('Ctrl Pts',(33.2671336154753,65.9018433963889,12.));
#164038=CARTESIAN_POINT('Ctrl Pts',(33.2879689780572,65.9190848540433,12.));
#164039=CARTESIAN_POINT('Ctrl Pts',(33.3088479147164,65.9363302276846,12.));
#164040=CARTESIAN_POINT('Ctrl Pts',(33.3297703874265,65.9535794260831,12.));
#164041=CARTESIAN_POINT('Ctrl Pts',(33.3507363581592,65.970832358141,12.));
#164042=CARTESIAN_POINT('Ctrl Pts',(33.37174578871,65.9880889322831,12.));
#164043=CARTESIAN_POINT('Ctrl Pts',(33.3927986405605,66.0053490559812,12.));
#164044=CARTESIAN_POINT('Ctrl Pts',(33.4138948746388,66.0226126349446,12.));
#164045=CARTESIAN_POINT('Ctrl Pts',(33.43503445151,66.0398795737777,12.));
#164046=CARTESIAN_POINT('Ctrl Pts',(33.4562173318025,66.0571497774434,12.));
#164047=CARTESIAN_POINT('Ctrl Pts',(33.4774434765745,66.0744231525415,12.));
#164048=CARTESIAN_POINT('Ctrl Pts',(33.4987128476622,66.0916996085245,12.));
#164049=CARTESIAN_POINT('Ctrl Pts',(33.5200254081243,66.1089790592729,12.));
#164050=CARTESIAN_POINT('Ctrl Pts',(33.541381122345,66.1262614234674,12.));
#164051=CARTESIAN_POINT('Ctrl Pts',(33.5597240685845,66.1410781873278,12.));
#164052=CARTESIAN_POINT('Ctrl Pts',(33.5738105077873,66.1524393974172,12.));
#164053=CARTESIAN_POINT('Ctrl Pts',(33.5836213514186,66.160343817752,12.));
#164054=CARTESIAN_POINT('Ctrl Pts',(33.5891439876489,66.1647906582654,12.));
#164055=CARTESIAN_POINT('Ctrl Pts',(33.5903722665274,66.1657795405958,12.));
#164056=CARTESIAN_POINT('',(30.3549065457811,63.0759831361898,0.));
#164057=CARTESIAN_POINT('',(30.3549065457811,63.0759831361898,0.));
#164058=CARTESIAN_POINT('Ctrl Pts',(33.5903722665274,66.1657795405958,0.));
#164059=CARTESIAN_POINT('Ctrl Pts',(33.5891439876489,66.1647906582654,0.));
#164060=CARTESIAN_POINT('Ctrl Pts',(33.5836213514186,66.160343817752,0.));
#164061=CARTESIAN_POINT('Ctrl Pts',(33.5738105077873,66.1524393974172,0.));
#164062=CARTESIAN_POINT('Ctrl Pts',(33.5597240685845,66.1410781873278,0.));
#164063=CARTESIAN_POINT('Ctrl Pts',(33.541381122345,66.1262614234674,0.));
#164064=CARTESIAN_POINT('Ctrl Pts',(33.5200254081243,66.1089790592729,0.));
#164065=CARTESIAN_POINT('Ctrl Pts',(33.4987128476622,66.0916996085245,0.));
#164066=CARTESIAN_POINT('Ctrl Pts',(33.4774434765745,66.0744231525415,0.));
#164067=CARTESIAN_POINT('Ctrl Pts',(33.4562173318025,66.0571497774434,0.));
#164068=CARTESIAN_POINT('Ctrl Pts',(33.43503445151,66.0398795737777,0.));
#164069=CARTESIAN_POINT('Ctrl Pts',(33.4138948746388,66.0226126349446,0.));
#164070=CARTESIAN_POINT('Ctrl Pts',(33.3927986405605,66.0053490559812,0.));
#164071=CARTESIAN_POINT('Ctrl Pts',(33.37174578871,65.9880889322831,0.));
#164072=CARTESIAN_POINT('Ctrl Pts',(33.3507363581592,65.970832358141,0.));
#164073=CARTESIAN_POINT('Ctrl Pts',(33.3297703874265,65.9535794260831,0.));
#164074=CARTESIAN_POINT('Ctrl Pts',(33.3088479147164,65.9363302276846,0.));
#164075=CARTESIAN_POINT('Ctrl Pts',(33.2879689780572,65.9190848540433,0.));
#164076=CARTESIAN_POINT('Ctrl Pts',(33.2671336154753,65.9018433963889,0.));
#164077=CARTESIAN_POINT('Ctrl Pts',(33.2463418651492,65.8846059466372,0.));
#164078=CARTESIAN_POINT('Ctrl Pts',(33.2255937655649,65.8673725979578,0.));
#164079=CARTESIAN_POINT('Ctrl Pts',(33.2048893554491,65.8501434445164,0.));
#164080=CARTESIAN_POINT('Ctrl Pts',(33.1842286737051,65.8329185812375,0.));
#164081=CARTESIAN_POINT('Ctrl Pts',(33.16361175934,65.8156981035503,0.));
#164082=CARTESIAN_POINT('Ctrl Pts',(33.1430386513976,65.7984821071623,0.));
#164083=CARTESIAN_POINT('Ctrl Pts',(33.1225093888672,65.7812706877697,0.));
#164084=CARTESIAN_POINT('Ctrl Pts',(33.1020240106884,65.7640639410661,0.));
#164085=CARTESIAN_POINT('Ctrl Pts',(33.081582555798,65.7468619628816,0.));
#164086=CARTESIAN_POINT('Ctrl Pts',(33.0611850631582,65.7296648492825,0.));
#164087=CARTESIAN_POINT('Ctrl Pts',(33.0408315717873,65.7124726966802,0.));
#164088=CARTESIAN_POINT('Ctrl Pts',(33.0205221207873,65.6952856019533,0.));
#164089=CARTESIAN_POINT('Ctrl Pts',(33.0002567493573,65.6781036625027,0.));
#164090=CARTESIAN_POINT('Ctrl Pts',(32.980035496784,65.6609269761889,0.));
#164091=CARTESIAN_POINT('Ctrl Pts',(32.9598584024312,65.6437556412947,0.));
#164092=CARTESIAN_POINT('Ctrl Pts',(32.9397255057274,65.6265897564783,0.));
#164093=CARTESIAN_POINT('Ctrl Pts',(32.9196368461463,65.6094294207276,0.));
#164094=CARTESIAN_POINT('Ctrl Pts',(32.8995924631898,65.5922747333194,0.));
#164095=CARTESIAN_POINT('Ctrl Pts',(32.879592396403,65.5751257938473,0.));
#164096=CARTESIAN_POINT('Ctrl Pts',(32.8596366853832,65.5579827022421,0.));
#164097=CARTESIAN_POINT('Ctrl Pts',(32.8397253697865,65.5408455587965,0.));
#164098=CARTESIAN_POINT('Ctrl Pts',(32.8198584893315,65.5237144641858,0.));
#164099=CARTESIAN_POINT('Ctrl Pts',(32.8000360837975,65.5065895194928,0.));
#164100=CARTESIAN_POINT('Ctrl Pts',(32.7802581930287,65.4894708262061,0.));
#164101=CARTESIAN_POINT('Ctrl Pts',(32.7605248569378,65.4723584862122,0.));
#164102=CARTESIAN_POINT('Ctrl Pts',(32.7408361155037,65.4552526017905,0.));
#164103=CARTESIAN_POINT('Ctrl Pts',(32.7211920087684,65.4381532756065,0.));
#164104=CARTESIAN_POINT('Ctrl Pts',(32.7015925768265,65.4210606107035,0.));
#164105=CARTESIAN_POINT('Ctrl Pts',(32.6820378598267,65.4039747105038,0.));
#164106=CARTESIAN_POINT('Ctrl Pts',(32.662527897981,65.3868956788182,0.));
#164107=CARTESIAN_POINT('Ctrl Pts',(32.6430627315674,65.3698236198513,0.));
#164108=CARTESIAN_POINT('Ctrl Pts',(32.6236424009301,65.3527586382081,0.));
#164109=CARTESIAN_POINT('Ctrl Pts',(32.6042669464751,65.3357008389004,0.));
#164110=CARTESIAN_POINT('Ctrl Pts',(32.5849364086678,65.31865032735,0.));
#164111=CARTESIAN_POINT('Ctrl Pts',(32.5656508280421,65.3016072093912,0.));
#164112=CARTESIAN_POINT('Ctrl Pts',(32.5464102452014,65.2845715912721,0.));
#164113=CARTESIAN_POINT('Ctrl Pts',(32.5272147008191,65.2675435796558,0.));
#164114=CARTESIAN_POINT('Ctrl Pts',(32.5080642356328,65.2505232816209,0.));
#164115=CARTESIAN_POINT('Ctrl Pts',(32.4889588904392,65.2335108046614,0.));
#164116=CARTESIAN_POINT('Ctrl Pts',(32.4698987061032,65.2165062566924,0.));
#164117=CARTESIAN_POINT('Ctrl Pts',(32.450883723561,65.1995097460538,0.));
#164118=CARTESIAN_POINT('Ctrl Pts',(32.4319139838212,65.182521381514,0.));
#164119=CARTESIAN_POINT('Ctrl Pts',(32.4129895279615,65.1655412722726,0.));
#164120=CARTESIAN_POINT('Ctrl Pts',(32.3941103971221,65.1485695279635,0.));
#164121=CARTESIAN_POINT('Ctrl Pts',(32.3752766325136,65.1316062586588,0.));
#164122=CARTESIAN_POINT('Ctrl Pts',(32.3564882754212,65.1146515748722,0.));
#164123=CARTESIAN_POINT('Ctrl Pts',(32.3377453672051,65.0977055875608,0.));
#164124=CARTESIAN_POINT('Ctrl Pts',(32.3190479492987,65.0807684081282,0.));
#164125=CARTESIAN_POINT('Ctrl Pts',(32.3003960632006,65.0638401484257,0.));
#164126=CARTESIAN_POINT('Ctrl Pts',(32.2817897504807,65.0469209207563,0.));
#164127=CARTESIAN_POINT('Ctrl Pts',(32.2632290527862,65.03001083788,0.));
#164128=CARTESIAN_POINT('Ctrl Pts',(32.2447140118422,65.0131100130158,0.));
#164129=CARTESIAN_POINT('Ctrl Pts',(32.2262446694512,64.9962185598462,0.));
#164130=CARTESIAN_POINT('Ctrl Pts',(32.207821067485,64.9793365925178,0.));
#164131=CARTESIAN_POINT('Ctrl Pts',(32.189443247888,64.9624642256461,0.));
#164132=CARTESIAN_POINT('Ctrl Pts',(32.1711112526854,64.9456015743193,0.));
#164133=CARTESIAN_POINT('Ctrl Pts',(32.152825123983,64.9287487541015,0.));
#164134=CARTESIAN_POINT('Ctrl Pts',(32.1345849039674,64.9119058810367,0.));
#164135=CARTESIAN_POINT('Ctrl Pts',(32.1163906348983,64.8950730716501,0.));
#164136=CARTESIAN_POINT('Ctrl Pts',(32.0982423591112,64.8782504429527,0.));
#164137=CARTESIAN_POINT('Ctrl Pts',(32.0801401190244,64.8614381124455,0.));
#164138=CARTESIAN_POINT('Ctrl Pts',(32.0620839571409,64.8446361981234,0.));
#164139=CARTESIAN_POINT('Ctrl Pts',(32.0440739160476,64.8278448184785,0.));
#164140=CARTESIAN_POINT('Ctrl Pts',(32.0261100384092,64.811064092502,0.));
#164141=CARTESIAN_POINT('Ctrl Pts',(32.0081923669677,64.7942941396883,0.));
#164142=CARTESIAN_POINT('Ctrl Pts',(31.9903209445521,64.7775350800404,0.));
#164143=CARTESIAN_POINT('Ctrl Pts',(31.972495814079,64.7607870340738,0.));
#164144=CARTESIAN_POINT('Ctrl Pts',(31.9547170185533,64.7440501228201,0.));
#164145=CARTESIAN_POINT('Ctrl Pts',(31.9369846010613,64.727324467829,0.));
#164146=CARTESIAN_POINT('Ctrl Pts',(31.9192986047702,64.7106101911723,0.));
#164147=CARTESIAN_POINT('Ctrl Pts',(31.9016590729371,64.6939074154491,0.));
#164148=CARTESIAN_POINT('Ctrl Pts',(31.8840660489106,64.6772162637905,0.));
#164149=CARTESIAN_POINT('Ctrl Pts',(31.8665195761312,64.6605368598631,0.));
#164150=CARTESIAN_POINT('Ctrl Pts',(31.849019698125,64.6438693278718,0.));
#164151=CARTESIAN_POINT('Ctrl Pts',(31.8315664585027,64.627213792563,0.));
#164152=CARTESIAN_POINT('Ctrl Pts',(31.8141599009684,64.6105703792311,0.));
#164153=CARTESIAN_POINT('Ctrl Pts',(31.7968000693218,64.5939392137233,0.));
#164154=CARTESIAN_POINT('Ctrl Pts',(31.7794870074583,64.5773204224429,0.));
#164155=CARTESIAN_POINT('Ctrl Pts',(31.7622207593637,64.5607141323527,0.));
#164156=CARTESIAN_POINT('Ctrl Pts',(31.7450013691117,64.544120470978,0.));
#164157=CARTESIAN_POINT('Ctrl Pts',(31.7278288808736,64.5275395664134,0.));
#164158=CARTESIAN_POINT('Ctrl Pts',(31.7107033389204,64.5109715473277,0.));
#164159=CARTESIAN_POINT('Ctrl Pts',(31.6936247876228,64.4944165429672,0.));
#164160=CARTESIAN_POINT('Ctrl Pts',(31.6765932714456,64.4778746831598,0.));
#164161=CARTESIAN_POINT('Ctrl Pts',(31.6596088349468,64.4613460983186,0.));
#164162=CARTESIAN_POINT('Ctrl Pts',(31.6426715227865,64.4448309194499,0.));
#164163=CARTESIAN_POINT('Ctrl Pts',(31.6257813797281,64.4283292781553,0.));
#164164=CARTESIAN_POINT('Ctrl Pts',(31.6089384506399,64.4118413066386,0.));
#164165=CARTESIAN_POINT('Ctrl Pts',(31.5921427804879,64.3953671377071,0.));
#164166=CARTESIAN_POINT('Ctrl Pts',(31.5753944143355,64.3789069047768,0.));
#164167=CARTESIAN_POINT('Ctrl Pts',(31.5586933973531,64.3624607418798,0.));
#164168=CARTESIAN_POINT('Ctrl Pts',(31.5420397748198,64.34602878367,0.));
#164169=CARTESIAN_POINT('Ctrl Pts',(31.5254335921239,64.3296111654273,0.));
#164170=CARTESIAN_POINT('Ctrl Pts',(31.5088748947565,64.3132080230603,0.));
#164171=CARTESIAN_POINT('Ctrl Pts',(31.4923637283109,64.2968194931113,0.));
#164172=CARTESIAN_POINT('Ctrl Pts',(31.4759001384922,64.2804457127633,0.));
#164173=CARTESIAN_POINT('Ctrl Pts',(31.4594841711188,64.264086819846,0.));
#164174=CARTESIAN_POINT('Ctrl Pts',(31.4431158721229,64.2477429528408,0.));
#164175=CARTESIAN_POINT('Ctrl Pts',(31.426795287544,64.2314142508843,0.));
#164176=CARTESIAN_POINT('Ctrl Pts',(31.4105224635298,64.2151008537733,0.));
#164177=CARTESIAN_POINT('Ctrl Pts',(31.3942974463458,64.1988029019733,0.));
#164178=CARTESIAN_POINT('Ctrl Pts',(31.3781202823758,64.1825205366231,0.));
#164179=CARTESIAN_POINT('Ctrl Pts',(31.3619910181222,64.1662538995407,0.));
#164180=CARTESIAN_POINT('Ctrl Pts',(31.3459097001995,64.150003133226,0.));
#164181=CARTESIAN_POINT('Ctrl Pts',(31.3298763753366,64.1337683808667,0.));
#164182=CARTESIAN_POINT('Ctrl Pts',(31.3138910903852,64.1175497863475,0.));
#164183=CARTESIAN_POINT('Ctrl Pts',(31.2979538923213,64.1013474942554,0.));
#164184=CARTESIAN_POINT('Ctrl Pts',(31.2820648282451,64.0851616498861,0.));
#164185=CARTESIAN_POINT('Ctrl Pts',(31.2662239453734,64.0689923992475,0.));
#164186=CARTESIAN_POINT('Ctrl Pts',(31.2504312910457,64.0528398890671,0.));
#164187=CARTESIAN_POINT('Ctrl Pts',(31.23468691273,64.036704266799,0.));
#164188=CARTESIAN_POINT('Ctrl Pts',(31.2189908580245,64.0205856806298,0.));
#164189=CARTESIAN_POINT('Ctrl Pts',(31.2033431746558,64.004484279483,0.));
#164190=CARTESIAN_POINT('Ctrl Pts',(31.1877439104717,63.9884002130209,0.));
#164191=CARTESIAN_POINT('Ctrl Pts',(31.1721931134488,63.972333631655,0.));
#164192=CARTESIAN_POINT('Ctrl Pts',(31.1566908316992,63.9562846865566,0.));
#164193=CARTESIAN_POINT('Ctrl Pts',(31.1412371134727,63.9402535296651,0.));
#164194=CARTESIAN_POINT('Ctrl Pts',(31.1258320071545,63.9242403136954,0.));
#164195=CARTESIAN_POINT('Ctrl Pts',(31.1104755612606,63.9082451921447,0.));
#164196=CARTESIAN_POINT('Ctrl Pts',(31.0951678244454,63.8922683192963,0.));
#164197=CARTESIAN_POINT('Ctrl Pts',(31.079908845504,63.8763098502235,0.));
#164198=CARTESIAN_POINT('Ctrl Pts',(31.0646986733723,63.8603699407922,0.));
#164199=CARTESIAN_POINT('Ctrl Pts',(31.0495373571217,63.8444487476615,0.));
#164200=CARTESIAN_POINT('Ctrl Pts',(31.0344249459544,63.8285464282857,0.));
#164201=CARTESIAN_POINT('Ctrl Pts',(31.0193614892177,63.8126631409376,0.));
#164202=CARTESIAN_POINT('Ctrl Pts',(31.0043470364112,63.7967990447288,0.));
#164203=CARTESIAN_POINT('Ctrl Pts',(30.9893816371907,63.7809542996258,0.));
#164204=CARTESIAN_POINT('Ctrl Pts',(30.9744653413679,63.7651290664713,0.));
#164205=CARTESIAN_POINT('Ctrl Pts',(30.9595981989091,63.7493235069844,0.));
#164206=CARTESIAN_POINT('Ctrl Pts',(30.9447802599345,63.733537783742,0.));
#164207=CARTESIAN_POINT('Ctrl Pts',(30.9300115747113,63.7177720601604,0.));
#164208=CARTESIAN_POINT('Ctrl Pts',(30.9152921936471,63.7020265004805,0.));
#164209=CARTESIAN_POINT('Ctrl Pts',(30.9006221672703,63.6863012697354,0.));
#164210=CARTESIAN_POINT('Ctrl Pts',(30.8860015462488,63.6705965337996,0.));
#164211=CARTESIAN_POINT('Ctrl Pts',(30.8714303814202,63.6549124594681,0.));
#164212=CARTESIAN_POINT('Ctrl Pts',(30.8569087238131,63.6392492145233,0.));
#164213=CARTESIAN_POINT('Ctrl Pts',(30.8424366246665,63.6236069678041,0.));
#164214=CARTESIAN_POINT('Ctrl Pts',(30.8280141354447,63.6079858892747,0.));
#164215=CARTESIAN_POINT('Ctrl Pts',(30.8136413077999,63.5923861498964,0.));
#164216=CARTESIAN_POINT('Ctrl Pts',(30.7993181935265,63.5768079214868,0.));
#164217=CARTESIAN_POINT('Ctrl Pts',(30.7850448445207,63.5612513766005,0.));
#164218=CARTESIAN_POINT('Ctrl Pts',(30.7708213127169,63.5457166883558,0.));
#164219=CARTESIAN_POINT('Ctrl Pts',(30.7566476500772,63.5302040304173,0.));
#164220=CARTESIAN_POINT('Ctrl Pts',(30.7425239087294,63.514713577392,0.));
#164221=CARTESIAN_POINT('Ctrl Pts',(30.7284501410827,63.4992455051805,0.));
#164222=CARTESIAN_POINT('Ctrl Pts',(30.7144263999259,63.4837999912758,0.));
#164223=CARTESIAN_POINT('Ctrl Pts',(30.7004527385806,63.4683772152497,0.));
#164224=CARTESIAN_POINT('Ctrl Pts',(30.686529210791,63.4529773584211,0.));
#164225=CARTESIAN_POINT('Ctrl Pts',(30.6726558704301,63.4376006029575,0.));
#164226=CARTESIAN_POINT('Ctrl Pts',(30.6588327712482,63.4222471311236,0.));
#164227=CARTESIAN_POINT('Ctrl Pts',(30.6450599666135,63.4069171245094,0.));
#164228=CARTESIAN_POINT('Ctrl Pts',(30.6313375092084,63.3916107631421,0.));
#164229=CARTESIAN_POINT('Ctrl Pts',(30.6176654515988,63.3763282271838,0.));
#164230=CARTESIAN_POINT('Ctrl Pts',(30.6040438469089,63.3610696989599,0.));
#164231=CARTESIAN_POINT('Ctrl Pts',(30.5904727493707,63.3458353646144,0.));
#164232=CARTESIAN_POINT('Ctrl Pts',(30.5769522151147,63.330625416509,0.));
#164233=CARTESIAN_POINT('Ctrl Pts',(30.5634823022358,63.315440053435,0.));
#164234=CARTESIAN_POINT('Ctrl Pts',(30.5500630691342,63.300279475605,0.));
#164235=CARTESIAN_POINT('Ctrl Pts',(30.5366945730503,63.2851438802462,0.));
#164236=CARTESIAN_POINT('Ctrl Pts',(30.5233768687875,63.2700334577661,0.));
#164237=CARTESIAN_POINT('Ctrl Pts',(30.5101100066683,63.2549483856268,0.));
#164238=CARTESIAN_POINT('Ctrl Pts',(30.4968940345027,63.2398888342612,0.));
#164239=CARTESIAN_POINT('Ctrl Pts',(30.4837290015011,63.2248549788272,0.));
#164240=CARTESIAN_POINT('Ctrl Pts',(30.470614961416,63.2098470086636,0.));
#164241=CARTESIAN_POINT('Ctrl Pts',(30.4575519763305,63.1948651386868,0.));
#164242=CARTESIAN_POINT('Ctrl Pts',(30.4445401192324,63.1799096171757,0.));
#164243=CARTESIAN_POINT('Ctrl Pts',(30.431579465967,63.1649807016766,0.));
#164244=CARTESIAN_POINT('Ctrl Pts',(30.4186700875598,63.1500786361382,0.));
#164245=CARTESIAN_POINT('Ctrl Pts',(30.4058120432259,63.1352036298512,0.));
#164246=CARTESIAN_POINT('Ctrl Pts',(30.3930053710592,63.1203558300911,0.));
#164247=CARTESIAN_POINT('Ctrl Pts',(30.3802500880565,63.1055353202641,0.));
#164248=CARTESIAN_POINT('Ctrl Pts',(30.3700869762658,63.0937007763826,0.));
#164249=CARTESIAN_POINT('Ctrl Pts',(30.3624877680747,63.0848371718274,0.));
#164250=CARTESIAN_POINT('Ctrl Pts',(30.3574319069365,63.0789335700774,0.));
#164251=CARTESIAN_POINT('Ctrl Pts',(30.3549065457811,63.0759831361898,0.));
#164252=CARTESIAN_POINT('Ctrl Pts',(39.5004851439258,63.1661434108059,0.));
#164253=CARTESIAN_POINT('Ctrl Pts',(39.5004851439258,63.1661434108059,12.));
#164254=CARTESIAN_POINT('Ctrl Pts',(39.4958045828135,63.1630766582788,0.));
#164255=CARTESIAN_POINT('Ctrl Pts',(39.4958045828135,63.1630766582788,12.));
#164256=CARTESIAN_POINT('Ctrl Pts',(39.4864477303823,63.1569429707875,0.));
#164257=CARTESIAN_POINT('Ctrl Pts',(39.4864477303823,63.1569429707875,12.));
#164258=CARTESIAN_POINT('Ctrl Pts',(39.4724252611155,63.1477418922406,0.));
#164259=CARTESIAN_POINT('Ctrl Pts',(39.4724252611155,63.1477418922406,12.));
#164260=CARTESIAN_POINT('Ctrl Pts',(39.4537542552268,63.1354726928398,0.));
#164261=CARTESIAN_POINT('Ctrl Pts',(39.4537542552268,63.1354726928398,12.));
#164262=CARTESIAN_POINT('Ctrl Pts',(39.4304582059864,63.1201343731172,0.));
#164263=CARTESIAN_POINT('Ctrl Pts',(39.4304582059864,63.1201343731172,12.));
#164264=CARTESIAN_POINT('Ctrl Pts',(39.4072048797615,63.10479424519,0.));
#164265=CARTESIAN_POINT('Ctrl Pts',(39.4072048797615,63.10479424519,12.));
#164266=CARTESIAN_POINT('Ctrl Pts',(39.3839942985739,63.0894523341314,0.));
#164267=CARTESIAN_POINT('Ctrl Pts',(39.3839942985739,63.0894523341314,12.));
#164268=CARTESIAN_POINT('Ctrl Pts',(39.3608264920409,63.0741086815841,0.));
#164269=CARTESIAN_POINT('Ctrl Pts',(39.3608264920409,63.0741086815841,12.));
#164270=CARTESIAN_POINT('Ctrl Pts',(39.3377014983609,63.0587633513774,0.));
#164271=CARTESIAN_POINT('Ctrl Pts',(39.3377014983609,63.0587633513774,12.));
#164272=CARTESIAN_POINT('Ctrl Pts',(39.3146193632392,63.0434164277992,0.));
#164273=CARTESIAN_POINT('Ctrl Pts',(39.3146193632392,63.0434164277992,12.));
#164274=CARTESIAN_POINT('Ctrl Pts',(39.2915801372354,63.0280680082353,0.));
#164275=CARTESIAN_POINT('Ctrl Pts',(39.2915801372354,63.0280680082353,12.));
#164276=CARTESIAN_POINT('Ctrl Pts',(39.2685838735361,63.0127181973628,0.));
#164277=CARTESIAN_POINT('Ctrl Pts',(39.2685838735361,63.0127181973628,12.));
#164278=CARTESIAN_POINT('Ctrl Pts',(39.2456306256104,62.9973671008704,0.));
#164279=CARTESIAN_POINT('Ctrl Pts',(39.2456306256104,62.9973671008704,12.));
#164280=CARTESIAN_POINT('Ctrl Pts',(39.2227204447638,62.9820148189929,0.));
#164281=CARTESIAN_POINT('Ctrl Pts',(39.2227204447638,62.9820148189929,12.));
#164282=CARTESIAN_POINT('Ctrl Pts',(39.199853378166,62.9666614412731,0.));
#164283=CARTESIAN_POINT('Ctrl Pts',(39.199853378166,62.9666614412731,12.));
#164284=CARTESIAN_POINT('Ctrl Pts',(39.1770294702428,62.9513070501867,0.));
#164285=CARTESIAN_POINT('Ctrl Pts',(39.1770294702428,62.9513070501867,12.));
#164286=CARTESIAN_POINT('Ctrl Pts',(39.1542487636743,62.9359517237404,0.));
#164287=CARTESIAN_POINT('Ctrl Pts',(39.1542487636743,62.9359517237404,12.));
#164288=CARTESIAN_POINT('Ctrl Pts',(39.131511300575,62.9205955385558,0.));
#164289=CARTESIAN_POINT('Ctrl Pts',(39.131511300575,62.9205955385558,12.));
#164290=CARTESIAN_POINT('Ctrl Pts',(39.1088171235125,62.9052385725388,0.));
#164291=CARTESIAN_POINT('Ctrl Pts',(39.1088171235125,62.9052385725388,12.));
#164292=CARTESIAN_POINT('Ctrl Pts',(39.0861662767932,62.8898809082612,0.));
#164293=CARTESIAN_POINT('Ctrl Pts',(39.0861662767932,62.8898809082612,12.));
#164294=CARTESIAN_POINT('Ctrl Pts',(39.0635588063276,62.8745226325998,0.));
#164295=CARTESIAN_POINT('Ctrl Pts',(39.0635588063276,62.8745226325998,12.));
#164296=CARTESIAN_POINT('Ctrl Pts',(39.0409947590496,62.8591638352056,0.));
#164297=CARTESIAN_POINT('Ctrl Pts',(39.0409947590496,62.8591638352056,12.));
#164298=CARTESIAN_POINT('Ctrl Pts',(39.0184741824641,62.8438046073224,0.));
#164299=CARTESIAN_POINT('Ctrl Pts',(39.0184741824641,62.8438046073224,12.));
#164300=CARTESIAN_POINT('Ctrl Pts',(38.9959971241701,62.8284450405459,0.));
#164301=CARTESIAN_POINT('Ctrl Pts',(38.9959971241701,62.8284450405459,12.));
#164302=CARTESIAN_POINT('Ctrl Pts',(38.9735636313088,62.8130852254027,0.));
#164303=CARTESIAN_POINT('Ctrl Pts',(38.9735636313088,62.8130852254027,12.));
#164304=CARTESIAN_POINT('Ctrl Pts',(38.9511737503165,62.7977252507118,0.));
#164305=CARTESIAN_POINT('Ctrl Pts',(38.9511737503165,62.7977252507118,12.));
#164306=CARTESIAN_POINT('Ctrl Pts',(38.9288275272335,62.78236520437,0.));
#164307=CARTESIAN_POINT('Ctrl Pts',(38.9288275272335,62.78236520437,12.));
#164308=CARTESIAN_POINT('Ctrl Pts',(38.9065250078832,62.7670051738143,0.));
#164309=CARTESIAN_POINT('Ctrl Pts',(38.9065250078832,62.7670051738143,12.));
#164310=CARTESIAN_POINT('Ctrl Pts',(38.8842662380984,62.7516452466128,0.));
#164311=CARTESIAN_POINT('Ctrl Pts',(38.8842662380984,62.7516452466128,12.));
#164312=CARTESIAN_POINT('Ctrl Pts',(38.8620512639232,62.7362855110042,0.));
#164313=CARTESIAN_POINT('Ctrl Pts',(38.8620512639232,62.7362855110042,12.));
#164314=CARTESIAN_POINT('Ctrl Pts',(38.8398801318176,62.7209260564493,0.));
#164315=CARTESIAN_POINT('Ctrl Pts',(38.8398801318176,62.7209260564493,12.));
#164316=CARTESIAN_POINT('Ctrl Pts',(38.8177528885681,62.7055669733802,0.));
#164317=CARTESIAN_POINT('Ctrl Pts',(38.8177528885681,62.7055669733802,12.));
#164318=CARTESIAN_POINT('Ctrl Pts',(38.795669581203,62.6902083529695,0.));
#164319=CARTESIAN_POINT('Ctrl Pts',(38.795669581203,62.6902083529695,12.));
#164320=CARTESIAN_POINT('Ctrl Pts',(38.7736302568982,62.6748502868835,0.));
#164321=CARTESIAN_POINT('Ctrl Pts',(38.7736302568982,62.6748502868835,12.));
#164322=CARTESIAN_POINT('Ctrl Pts',(38.7516349628903,62.6594928670628,0.));
#164323=CARTESIAN_POINT('Ctrl Pts',(38.7516349628903,62.6594928670628,12.));
#164324=CARTESIAN_POINT('Ctrl Pts',(38.7296837463608,62.6441361854411,0.));
#164325=CARTESIAN_POINT('Ctrl Pts',(38.7296837463608,62.6441361854411,12.));
#164326=CARTESIAN_POINT('Ctrl Pts',(38.7077766544416,62.6287803339542,0.));
#164327=CARTESIAN_POINT('Ctrl Pts',(38.7077766544416,62.6287803339542,12.));
#164328=CARTESIAN_POINT('Ctrl Pts',(38.685913734273,62.6134254046739,0.));
#164329=CARTESIAN_POINT('Ctrl Pts',(38.685913734273,62.6134254046739,12.));
#164330=CARTESIAN_POINT('Ctrl Pts',(38.6640950330421,62.5980714899052,0.));
#164331=CARTESIAN_POINT('Ctrl Pts',(38.6640950330421,62.5980714899052,12.));
#164332=CARTESIAN_POINT('Ctrl Pts',(38.6423205980213,62.5827186822921,0.));
#164333=CARTESIAN_POINT('Ctrl Pts',(38.6423205980213,62.5827186822921,12.));
#164334=CARTESIAN_POINT('Ctrl Pts',(38.6205904766072,62.5673670749362,0.));
#164335=CARTESIAN_POINT('Ctrl Pts',(38.6205904766072,62.5673670749362,12.));
#164336=CARTESIAN_POINT('Ctrl Pts',(38.5989047163393,62.5520167614516,0.));
#164337=CARTESIAN_POINT('Ctrl Pts',(38.5989047163393,62.5520167614516,12.));
#164338=CARTESIAN_POINT('Ctrl Pts',(38.5772633648832,62.5366678359023,0.));
#164339=CARTESIAN_POINT('Ctrl Pts',(38.5772633648832,62.5366678359023,12.));
#164340=CARTESIAN_POINT('Ctrl Pts',(38.5556664700195,62.5213203927663,0.));
#164341=CARTESIAN_POINT('Ctrl Pts',(38.5556664700195,62.5213203927663,12.));
#164342=CARTESIAN_POINT('Ctrl Pts',(38.5341140796248,62.5059745268901,0.));
#164343=CARTESIAN_POINT('Ctrl Pts',(38.5341140796248,62.5059745268901,12.));
#164344=CARTESIAN_POINT('Ctrl Pts',(38.5126062416502,62.4906303334443,0.));
#164345=CARTESIAN_POINT('Ctrl Pts',(38.5126062416502,62.4906303334443,12.));
#164346=CARTESIAN_POINT('Ctrl Pts',(38.4911430040997,62.4752879078854,0.));
#164347=CARTESIAN_POINT('Ctrl Pts',(38.4911430040997,62.4752879078854,12.));
#164348=CARTESIAN_POINT('Ctrl Pts',(38.4697244150482,62.4599473459811,0.));
#164349=CARTESIAN_POINT('Ctrl Pts',(38.4697244150482,62.4599473459811,12.));
#164350=CARTESIAN_POINT('Ctrl Pts',(38.4483505226518,62.4446087438312,0.));
#164351=CARTESIAN_POINT('Ctrl Pts',(38.4483505226518,62.4446087438312,12.));
#164352=CARTESIAN_POINT('Ctrl Pts',(38.4270213751568,62.4292721978901,0.));
#164353=CARTESIAN_POINT('Ctrl Pts',(38.4270213751568,62.4292721978901,12.));
#164354=CARTESIAN_POINT('Ctrl Pts',(38.405737020905,62.4139378049886,0.));
#164355=CARTESIAN_POINT('Ctrl Pts',(38.405737020905,62.4139378049886,12.));
#164356=CARTESIAN_POINT('Ctrl Pts',(38.3844975083343,62.3986056623577,0.));
#164357=CARTESIAN_POINT('Ctrl Pts',(38.3844975083343,62.3986056623577,12.));
#164358=CARTESIAN_POINT('Ctrl Pts',(38.3633028859828,62.3832758676271,0.));
#164359=CARTESIAN_POINT('Ctrl Pts',(38.3633028859828,62.3832758676271,12.));
#164360=CARTESIAN_POINT('Ctrl Pts',(38.342153202491,62.3679485188172,0.));
#164361=CARTESIAN_POINT('Ctrl Pts',(38.342153202491,62.3679485188172,12.));
#164362=CARTESIAN_POINT('Ctrl Pts',(38.3210485066001,62.3526237143336,0.));
#164363=CARTESIAN_POINT('Ctrl Pts',(38.3210485066001,62.3526237143336,12.));
#164364=CARTESIAN_POINT('Ctrl Pts',(38.2999888471476,62.3373015529613,0.));
#164365=CARTESIAN_POINT('Ctrl Pts',(38.2999888471476,62.3373015529613,12.));
#164366=CARTESIAN_POINT('Ctrl Pts',(38.2789742730563,62.3219821338569,0.));
#164367=CARTESIAN_POINT('Ctrl Pts',(38.2789742730563,62.3219821338569,12.));
#164368=CARTESIAN_POINT('Ctrl Pts',(38.258004833336,62.3066655565503,0.));
#164369=CARTESIAN_POINT('Ctrl Pts',(38.258004833336,62.3066655565503,12.));
#164370=CARTESIAN_POINT('Ctrl Pts',(38.2370805770935,62.2913519209521,0.));
#164371=CARTESIAN_POINT('Ctrl Pts',(38.2370805770935,62.2913519209521,12.));
#164372=CARTESIAN_POINT('Ctrl Pts',(38.2162015535352,62.2760413273602,0.));
#164373=CARTESIAN_POINT('Ctrl Pts',(38.2162015535352,62.2760413273602,12.));
#164374=CARTESIAN_POINT('Ctrl Pts',(38.1953678119691,62.2607338764654,0.));
#164375=CARTESIAN_POINT('Ctrl Pts',(38.1953678119691,62.2607338764654,12.));
#164376=CARTESIAN_POINT('Ctrl Pts',(38.1745794017995,62.245429669358,0.));
#164377=CARTESIAN_POINT('Ctrl Pts',(38.1745794017995,62.245429669358,12.));
#164378=CARTESIAN_POINT('Ctrl Pts',(38.1538363725263,62.2301288075321,0.));
#164379=CARTESIAN_POINT('Ctrl Pts',(38.1538363725263,62.2301288075321,12.));
#164380=CARTESIAN_POINT('Ctrl Pts',(38.1331387737529,62.2148313928863,0.));
#164381=CARTESIAN_POINT('Ctrl Pts',(38.1331387737529,62.2148313928863,12.));
#164382=CARTESIAN_POINT('Ctrl Pts',(38.1124866551885,62.1995375277257,0.));
#164383=CARTESIAN_POINT('Ctrl Pts',(38.1124866551885,62.1995375277257,12.));
#164384=CARTESIAN_POINT('Ctrl Pts',(38.0918800666479,62.1842473147626,0.));
#164385=CARTESIAN_POINT('Ctrl Pts',(38.0918800666479,62.1842473147626,12.));
#164386=CARTESIAN_POINT('Ctrl Pts',(38.0713190580463,62.1689608571176,0.));
#164387=CARTESIAN_POINT('Ctrl Pts',(38.0713190580463,62.1689608571176,12.));
#164388=CARTESIAN_POINT('Ctrl Pts',(38.0508036793939,62.1536782583199,0.));
#164389=CARTESIAN_POINT('Ctrl Pts',(38.0508036793939,62.1536782583199,12.));
#164390=CARTESIAN_POINT('Ctrl Pts',(38.0303339808053,62.1383996223125,0.));
#164391=CARTESIAN_POINT('Ctrl Pts',(38.0303339808053,62.1383996223125,12.));
#164392=CARTESIAN_POINT('Ctrl Pts',(38.0099100125037,62.123125053455,0.));
#164393=CARTESIAN_POINT('Ctrl Pts',(38.0099100125037,62.123125053455,12.));
#164394=CARTESIAN_POINT('Ctrl Pts',(37.9895318248212,62.107854656528,0.));
#164395=CARTESIAN_POINT('Ctrl Pts',(37.9895318248212,62.107854656528,12.));
#164396=CARTESIAN_POINT('Ctrl Pts',(37.9691994681966,62.0925885367352,0.));
#164397=CARTESIAN_POINT('Ctrl Pts',(37.9691994681966,62.0925885367352,12.));
#164398=CARTESIAN_POINT('Ctrl Pts',(37.9489129931688,62.0773267997079,0.));
#164399=CARTESIAN_POINT('Ctrl Pts',(37.9489129931688,62.0773267997079,12.));
#164400=CARTESIAN_POINT('Ctrl Pts',(37.9286724503851,62.0620695515075,0.));
#164401=CARTESIAN_POINT('Ctrl Pts',(37.9286724503851,62.0620695515075,12.));
#164402=CARTESIAN_POINT('Ctrl Pts',(37.9084778906053,62.0468168986288,0.));
#164403=CARTESIAN_POINT('Ctrl Pts',(37.9084778906053,62.0468168986288,12.));
#164404=CARTESIAN_POINT('Ctrl Pts',(37.8883293647029,62.031568948002,0.));
#164405=CARTESIAN_POINT('Ctrl Pts',(37.8883293647029,62.031568948002,12.));
#164406=CARTESIAN_POINT('Ctrl Pts',(37.868226923663,62.0163258069957,0.));
#164407=CARTESIAN_POINT('Ctrl Pts',(37.868226923663,62.0163258069957,12.));
#164408=CARTESIAN_POINT('Ctrl Pts',(37.8481706185749,62.0010875834187,0.));
#164409=CARTESIAN_POINT('Ctrl Pts',(37.8481706185749,62.0010875834187,12.));
#164410=CARTESIAN_POINT('Ctrl Pts',(37.828160500638,61.9858543855236,0.));
#164411=CARTESIAN_POINT('Ctrl Pts',(37.828160500638,61.9858543855236,12.));
#164412=CARTESIAN_POINT('Ctrl Pts',(37.8081966211688,61.9706263220114,0.));
#164413=CARTESIAN_POINT('Ctrl Pts',(37.8081966211688,61.9706263220114,12.));
#164414=CARTESIAN_POINT('Ctrl Pts',(37.7882790316014,61.9554035020338,0.));
#164415=CARTESIAN_POINT('Ctrl Pts',(37.7882790316014,61.9554035020338,12.));
#164416=CARTESIAN_POINT('Ctrl Pts',(37.7684077834872,61.9401860351973,0.));
#164417=CARTESIAN_POINT('Ctrl Pts',(37.7684077834872,61.9401860351973,12.));
#164418=CARTESIAN_POINT('Ctrl Pts',(37.7485829284871,61.9249740315649,0.));
#164419=CARTESIAN_POINT('Ctrl Pts',(37.7485829284871,61.9249740315649,12.));
#164420=CARTESIAN_POINT('Ctrl Pts',(37.7288045183756,61.9097676016601,0.));
#164421=CARTESIAN_POINT('Ctrl Pts',(37.7288045183756,61.9097676016601,12.));
#164422=CARTESIAN_POINT('Ctrl Pts',(37.7090726050482,61.8945668564704,0.));
#164423=CARTESIAN_POINT('Ctrl Pts',(37.7090726050482,61.8945668564704,12.));
#164424=CARTESIAN_POINT('Ctrl Pts',(37.6893872405228,61.8793719074507,0.));
#164425=CARTESIAN_POINT('Ctrl Pts',(37.6893872405228,61.8793719074507,12.));
#164426=CARTESIAN_POINT('Ctrl Pts',(37.6697484769392,61.8641828665262,0.));
#164427=CARTESIAN_POINT('Ctrl Pts',(37.6697484769392,61.8641828665262,12.));
#164428=CARTESIAN_POINT('Ctrl Pts',(37.6501563665523,61.8489998460957,0.));
#164429=CARTESIAN_POINT('Ctrl Pts',(37.6501563665523,61.8489998460957,12.));
#164430=CARTESIAN_POINT('Ctrl Pts',(37.6306109617346,61.8338229590353,0.));
#164431=CARTESIAN_POINT('Ctrl Pts',(37.6306109617346,61.8338229590353,12.));
#164432=CARTESIAN_POINT('Ctrl Pts',(37.6111123149839,61.8186523187015,0.));
#164433=CARTESIAN_POINT('Ctrl Pts',(37.6111123149839,61.8186523187015,12.));
#164434=CARTESIAN_POINT('Ctrl Pts',(37.5916604789253,61.8034880389363,0.));
#164435=CARTESIAN_POINT('Ctrl Pts',(37.5916604789253,61.8034880389363,12.));
#164436=CARTESIAN_POINT('Ctrl Pts',(37.5722555063111,61.7883302340687,0.));
#164437=CARTESIAN_POINT('Ctrl Pts',(37.5722555063111,61.7883302340687,12.));
#164438=CARTESIAN_POINT('Ctrl Pts',(37.5528974500141,61.7731790189191,0.));
#164439=CARTESIAN_POINT('Ctrl Pts',(37.5528974500141,61.7731790189191,12.));
#164440=CARTESIAN_POINT('Ctrl Pts',(37.5335863630287,61.7580345088016,0.));
#164441=CARTESIAN_POINT('Ctrl Pts',(37.5335863630287,61.7580345088016,12.));
#164442=CARTESIAN_POINT('Ctrl Pts',(37.5143222984795,61.7428968195299,0.));
#164443=CARTESIAN_POINT('Ctrl Pts',(37.5143222984795,61.7428968195299,12.));
#164444=CARTESIAN_POINT('Ctrl Pts',(37.4951053096237,61.7277660674205,0.));
#164445=CARTESIAN_POINT('Ctrl Pts',(37.4951053096237,61.7277660674205,12.));
#164446=CARTESIAN_POINT('Ctrl Pts',(37.4759354498509,61.7126423692963,0.));
#164447=CARTESIAN_POINT('Ctrl Pts',(37.4759354498509,61.7126423692963,12.));
#164448=CARTESIAN_POINT('Ctrl Pts',(37.4568127726773,61.6975258424894,0.));
#164449=CARTESIAN_POINT('Ctrl Pts',(37.4568127726773,61.6975258424894,12.));
#164450=CARTESIAN_POINT('Ctrl Pts',(37.4377373317451,61.6824166048444,0.));
#164451=CARTESIAN_POINT('Ctrl Pts',(37.4377373317451,61.6824166048444,12.));
#164452=CARTESIAN_POINT('Ctrl Pts',(37.418709180832,61.6673147747242,0.));
#164453=CARTESIAN_POINT('Ctrl Pts',(37.418709180832,61.6673147747242,12.));
#164454=CARTESIAN_POINT('Ctrl Pts',(37.3997283738533,61.6522204710131,0.));
#164455=CARTESIAN_POINT('Ctrl Pts',(37.3997283738533,61.6522204710131,12.));
#164456=CARTESIAN_POINT('Ctrl Pts',(37.3807949648624,61.637133813121,0.));
#164457=CARTESIAN_POINT('Ctrl Pts',(37.3807949648624,61.637133813121,12.));
#164458=CARTESIAN_POINT('Ctrl Pts',(37.3619090080449,61.6220549209866,0.));
#164459=CARTESIAN_POINT('Ctrl Pts',(37.3619090080449,61.6220549209866,12.));
#164460=CARTESIAN_POINT('Ctrl Pts',(37.343070557718,61.6069839150807,0.));
#164461=CARTESIAN_POINT('Ctrl Pts',(37.343070557718,61.6069839150807,12.));
#164462=CARTESIAN_POINT('Ctrl Pts',(37.3242796683395,61.591920916412,0.));
#164463=CARTESIAN_POINT('Ctrl Pts',(37.3242796683395,61.591920916412,12.));
#164464=CARTESIAN_POINT('Ctrl Pts',(37.3055363945107,61.5768660465311,0.));
#164465=CARTESIAN_POINT('Ctrl Pts',(37.3055363945107,61.5768660465311,12.));
#164466=CARTESIAN_POINT('Ctrl Pts',(37.286840790977,61.5618194275348,0.));
#164467=CARTESIAN_POINT('Ctrl Pts',(37.286840790977,61.5618194275348,12.));
#164468=CARTESIAN_POINT('Ctrl Pts',(37.2681929126221,61.5467811820691,0.));
#164469=CARTESIAN_POINT('Ctrl Pts',(37.2681929126221,61.5467811820691,12.));
#164470=CARTESIAN_POINT('Ctrl Pts',(37.2495928144666,61.5317514333328,0.));
#164471=CARTESIAN_POINT('Ctrl Pts',(37.2495928144666,61.5317514333328,12.));
#164472=CARTESIAN_POINT('Ctrl Pts',(37.2310405516781,61.5167303050832,0.));
#164473=CARTESIAN_POINT('Ctrl Pts',(37.2310405516781,61.5167303050832,12.));
#164474=CARTESIAN_POINT('Ctrl Pts',(37.2125361795731,61.501717921641,0.));
#164475=CARTESIAN_POINT('Ctrl Pts',(37.2125361795731,61.501717921641,12.));
#164476=CARTESIAN_POINT('Ctrl Pts',(37.1940797536181,61.4867144078937,0.));
#164477=CARTESIAN_POINT('Ctrl Pts',(37.1940797536181,61.4867144078937,12.));
#164478=CARTESIAN_POINT('Ctrl Pts',(37.175671329424,61.4717198892994,0.));
#164479=CARTESIAN_POINT('Ctrl Pts',(37.175671329424,61.4717198892994,12.));
#164480=CARTESIAN_POINT('Ctrl Pts',(37.1573109627454,61.456734491892,0.));
#164481=CARTESIAN_POINT('Ctrl Pts',(37.1573109627454,61.456734491892,12.));
#164482=CARTESIAN_POINT('Ctrl Pts',(37.1389987094904,61.4417583422863,0.));
#164483=CARTESIAN_POINT('Ctrl Pts',(37.1389987094904,61.4417583422863,12.));
#164484=CARTESIAN_POINT('Ctrl Pts',(37.1207346257221,61.4267915676822,0.));
#164485=CARTESIAN_POINT('Ctrl Pts',(37.1207346257221,61.4267915676822,12.));
#164486=CARTESIAN_POINT('Ctrl Pts',(37.1025187676602,61.4118342958697,0.));
#164487=CARTESIAN_POINT('Ctrl Pts',(37.1025187676602,61.4118342958697,12.));
#164488=CARTESIAN_POINT('Ctrl Pts',(37.0843511916744,61.3968866552318,0.));
#164489=CARTESIAN_POINT('Ctrl Pts',(37.0843511916744,61.3968866552318,12.));
#164490=CARTESIAN_POINT('Ctrl Pts',(37.0662319542849,61.381948774749,0.));
#164491=CARTESIAN_POINT('Ctrl Pts',(37.0662319542849,61.381948774749,12.));
#164492=CARTESIAN_POINT('Ctrl Pts',(37.0481611121717,61.3670207840069,0.));
#164493=CARTESIAN_POINT('Ctrl Pts',(37.0481611121717,61.3670207840069,12.));
#164494=CARTESIAN_POINT('Ctrl Pts',(37.0301387221774,61.3521028132003,0.));
#164495=CARTESIAN_POINT('Ctrl Pts',(37.0301387221774,61.3521028132003,12.));
#164496=CARTESIAN_POINT('Ctrl Pts',(37.0121648413081,61.3371949931387,0.));
#164497=CARTESIAN_POINT('Ctrl Pts',(37.0121648413081,61.3371949931387,12.));
#164498=CARTESIAN_POINT('Ctrl Pts',(36.994239526727,61.3222974552487,0.));
#164499=CARTESIAN_POINT('Ctrl Pts',(36.994239526727,61.3222974552487,12.));
#164500=CARTESIAN_POINT('Ctrl Pts',(36.9763628357544,61.3074103315792,0.));
#164501=CARTESIAN_POINT('Ctrl Pts',(36.9763628357544,61.3074103315792,12.));
#164502=CARTESIAN_POINT('Ctrl Pts',(36.9585348258776,61.2925337548077,0.));
#164503=CARTESIAN_POINT('Ctrl Pts',(36.9585348258776,61.2925337548077,12.));
#164504=CARTESIAN_POINT('Ctrl Pts',(36.9407555547534,61.2776678582461,0.));
#164505=CARTESIAN_POINT('Ctrl Pts',(36.9407555547534,61.2776678582461,12.));
#164506=CARTESIAN_POINT('Ctrl Pts',(36.9230250802087,61.2628127758457,0.));
#164507=CARTESIAN_POINT('Ctrl Pts',(36.9230250802087,61.2628127758457,12.));
#164508=CARTESIAN_POINT('Ctrl Pts',(36.9053434602343,61.247968642201,0.));
#164509=CARTESIAN_POINT('Ctrl Pts',(36.9053434602343,61.247968642201,12.));
#164510=CARTESIAN_POINT('Ctrl Pts',(36.8877107529865,61.2331355925547,0.));
#164511=CARTESIAN_POINT('Ctrl Pts',(36.8877107529865,61.2331355925547,12.));
#164512=CARTESIAN_POINT('Ctrl Pts',(36.8701270167969,61.2183137628056,0.));
#164513=CARTESIAN_POINT('Ctrl Pts',(36.8701270167969,61.2183137628056,12.));
#164514=CARTESIAN_POINT('Ctrl Pts',(36.852592310174,61.2035032895127,0.));
#164515=CARTESIAN_POINT('Ctrl Pts',(36.852592310174,61.2035032895127,12.));
#164516=CARTESIAN_POINT('Ctrl Pts',(36.8351066918036,61.1887043099014,0.));
#164517=CARTESIAN_POINT('Ctrl Pts',(36.8351066918036,61.1887043099014,12.));
#164518=CARTESIAN_POINT('Ctrl Pts',(36.8176702205423,61.1739169618667,0.));
#164519=CARTESIAN_POINT('Ctrl Pts',(36.8176702205423,61.1739169618667,12.));
#164520=CARTESIAN_POINT('Ctrl Pts',(36.8002829554209,61.1591413839787,0.));
#164521=CARTESIAN_POINT('Ctrl Pts',(36.8002829554209,61.1591413839787,12.));
#164522=CARTESIAN_POINT('Ctrl Pts',(36.7829449556532,61.1443777154911,0.));
#164523=CARTESIAN_POINT('Ctrl Pts',(36.7829449556532,61.1443777154911,12.));
#164524=CARTESIAN_POINT('Ctrl Pts',(36.765656280638,61.1296260963466,0.));
#164525=CARTESIAN_POINT('Ctrl Pts',(36.765656280638,61.1296260963466,12.));
#164526=CARTESIAN_POINT('Ctrl Pts',(36.7484169899596,61.1148866671829,0.));
#164527=CARTESIAN_POINT('Ctrl Pts',(36.7484169899596,61.1148866671829,12.));
#164528=CARTESIAN_POINT('Ctrl Pts',(36.7312271433807,61.100159569337,0.));
#164529=CARTESIAN_POINT('Ctrl Pts',(36.7312271433807,61.100159569337,12.));
#164530=CARTESIAN_POINT('Ctrl Pts',(36.7140868008486,61.0854449448524,0.));
#164531=CARTESIAN_POINT('Ctrl Pts',(36.7140868008486,61.0854449448524,12.));
#164532=CARTESIAN_POINT('Ctrl Pts',(36.6969960225022,61.0707429364847,0.));
#164533=CARTESIAN_POINT('Ctrl Pts',(36.6969960225022,61.0707429364847,12.));
#164534=CARTESIAN_POINT('Ctrl Pts',(36.679954868674,61.0560536877083,0.));
#164535=CARTESIAN_POINT('Ctrl Pts',(36.679954868674,61.0560536877083,12.));
#164536=CARTESIAN_POINT('Ctrl Pts',(36.6629633998886,61.0413773427203,0.));
#164537=CARTESIAN_POINT('Ctrl Pts',(36.6629633998886,61.0413773427203,12.));
#164538=CARTESIAN_POINT('Ctrl Pts',(36.6460216768553,61.0267140464432,0.));
#164539=CARTESIAN_POINT('Ctrl Pts',(36.6460216768553,61.0267140464432,12.));
#164540=CARTESIAN_POINT('Ctrl Pts',(36.6291297604776,61.0120639445349,0.));
#164541=CARTESIAN_POINT('Ctrl Pts',(36.6291297604776,61.0120639445349,12.));
#164542=CARTESIAN_POINT('Ctrl Pts',(36.61228771186,60.9974271833981,0.));
#164543=CARTESIAN_POINT('Ctrl Pts',(36.61228771186,60.9974271833981,12.));
#164544=CARTESIAN_POINT('Ctrl Pts',(36.5954955923109,60.9828039101887,0.));
#164545=CARTESIAN_POINT('Ctrl Pts',(36.5954955923109,60.9828039101887,12.));
#164546=CARTESIAN_POINT('Ctrl Pts',(36.5787534633415,60.9681942728237,0.));
#164547=CARTESIAN_POINT('Ctrl Pts',(36.5787534633415,60.9681942728237,12.));
#164548=CARTESIAN_POINT('Ctrl Pts',(36.5620613866614,60.9535984199873,0.));
#164549=CARTESIAN_POINT('Ctrl Pts',(36.5620613866614,60.9535984199873,12.));
#164550=CARTESIAN_POINT('Ctrl Pts',(36.5454194241865,60.9390165011355,0.));
#164551=CARTESIAN_POINT('Ctrl Pts',(36.5454194241865,60.9390165011355,12.));
#164552=CARTESIAN_POINT('Ctrl Pts',(36.5288276380416,60.9244486664988,0.));
#164553=CARTESIAN_POINT('Ctrl Pts',(36.5288276380416,60.9244486664988,12.));
#164554=CARTESIAN_POINT('Ctrl Pts',(36.5122860905612,60.9098950670847,0.));
#164555=CARTESIAN_POINT('Ctrl Pts',(36.5122860905612,60.9098950670847,12.));
#164556=CARTESIAN_POINT('Ctrl Pts',(36.4957948442835,60.8953558546795,0.));
#164557=CARTESIAN_POINT('Ctrl Pts',(36.4957948442835,60.8953558546795,12.));
#164558=CARTESIAN_POINT('Ctrl Pts',(36.4793539619466,60.8808311818499,0.));
#164559=CARTESIAN_POINT('Ctrl Pts',(36.4793539619466,60.8808311818499,12.));
#164560=CARTESIAN_POINT('Ctrl Pts',(36.4629635065045,60.8663212019657,0.));
#164561=CARTESIAN_POINT('Ctrl Pts',(36.4629635065045,60.8663212019657,12.));
#164562=CARTESIAN_POINT('Ctrl Pts',(36.4466235411358,60.8518260692188,0.));
#164563=CARTESIAN_POINT('Ctrl Pts',(36.4466235411358,60.8518260692188,12.));
#164564=CARTESIAN_POINT('Ctrl Pts',(36.4303341292494,60.8373459386392,0.));
#164565=CARTESIAN_POINT('Ctrl Pts',(36.4303341292494,60.8373459386392,12.));
#164566=CARTESIAN_POINT('Ctrl Pts',(36.4140953344858,60.8228809661161,0.));
#164567=CARTESIAN_POINT('Ctrl Pts',(36.4140953344858,60.8228809661161,12.));
#164568=CARTESIAN_POINT('Ctrl Pts',(36.397907220716,60.8084313083984,0.));
#164569=CARTESIAN_POINT('Ctrl Pts',(36.397907220716,60.8084313083984,12.));
#164570=CARTESIAN_POINT('Ctrl Pts',(36.3817698520388,60.7939971230761,0.));
#164571=CARTESIAN_POINT('Ctrl Pts',(36.3817698520388,60.7939971230761,12.));
#164572=CARTESIAN_POINT('Ctrl Pts',(36.365683292773,60.7795785685625,0.));
#164573=CARTESIAN_POINT('Ctrl Pts',(36.365683292773,60.7795785685625,12.));
#164574=CARTESIAN_POINT('Ctrl Pts',(36.3496476074488,60.7651758040804,0.));
#164575=CARTESIAN_POINT('Ctrl Pts',(36.3496476074488,60.7651758040804,12.));
#164576=CARTESIAN_POINT('Ctrl Pts',(36.3336628607858,60.7507889896308,0.));
#164577=CARTESIAN_POINT('Ctrl Pts',(36.3336628607858,60.7507889896308,12.));
#164578=CARTESIAN_POINT('Ctrl Pts',(36.3177291177163,60.7364182860412,0.));
#164579=CARTESIAN_POINT('Ctrl Pts',(36.3177291177163,60.7364182860412,12.));
#164580=CARTESIAN_POINT('Ctrl Pts',(36.3018464434213,60.722063855041,0.));
#164581=CARTESIAN_POINT('Ctrl Pts',(36.3018464434213,60.722063855041,12.));
#164582=CARTESIAN_POINT('Ctrl Pts',(36.2860149033587,60.7077258593268,0.));
#164583=CARTESIAN_POINT('Ctrl Pts',(36.2860149033587,60.7077258593268,12.));
#164584=CARTESIAN_POINT('Ctrl Pts',(36.2702345632875,60.6934044626291,0.));
#164585=CARTESIAN_POINT('Ctrl Pts',(36.2702345632875,60.6934044626291,12.));
#164586=CARTESIAN_POINT('Ctrl Pts',(36.2545054892897,60.67909982978,0.));
#164587=CARTESIAN_POINT('Ctrl Pts',(36.2545054892897,60.67909982978,12.));
#164588=CARTESIAN_POINT('Ctrl Pts',(36.2388277477212,60.6648121265885,0.));
#164589=CARTESIAN_POINT('Ctrl Pts',(36.2388277477212,60.6648121265885,12.));
#164590=CARTESIAN_POINT('Ctrl Pts',(36.2232014051541,60.6505415197042,0.));
#164591=CARTESIAN_POINT('Ctrl Pts',(36.2232014051541,60.6505415197042,12.));
#164592=CARTESIAN_POINT('Ctrl Pts',(36.2076265283264,60.6362881765019,0.));
#164593=CARTESIAN_POINT('Ctrl Pts',(36.2076265283264,60.6362881765019,12.));
#164594=CARTESIAN_POINT('Ctrl Pts',(36.1921031840629,60.6220522649149,0.));
#164595=CARTESIAN_POINT('Ctrl Pts',(36.1921031840629,60.6220522649149,12.));
#164596=CARTESIAN_POINT('Ctrl Pts',(36.1766314392641,60.6078339534181,0.));
#164597=CARTESIAN_POINT('Ctrl Pts',(36.1766314392641,60.6078339534181,12.));
#164598=CARTESIAN_POINT('Ctrl Pts',(36.1612113610773,60.5936334114108,0.));
#164599=CARTESIAN_POINT('Ctrl Pts',(36.1612113610773,60.5936334114108,12.));
#164600=CARTESIAN_POINT('Ctrl Pts',(36.145843017043,60.5794508095565,0.));
#164601=CARTESIAN_POINT('Ctrl Pts',(36.145843017043,60.5794508095565,12.));
#164602=CARTESIAN_POINT('Ctrl Pts',(36.1305264752187,60.565286320072,0.));
#164603=CARTESIAN_POINT('Ctrl Pts',(36.1305264752187,60.565286320072,12.));
#164604=CARTESIAN_POINT('Ctrl Pts',(36.1152618043738,60.5511401171984,0.));
#164605=CARTESIAN_POINT('Ctrl Pts',(36.1152618043738,60.5511401171984,12.));
#164606=CARTESIAN_POINT('Ctrl Pts',(36.100049073851,60.5370123768804,0.));
#164607=CARTESIAN_POINT('Ctrl Pts',(36.100049073851,60.5370123768804,12.));
#164608=CARTESIAN_POINT('Ctrl Pts',(36.0848883531952,60.5229032758974,0.));
#164609=CARTESIAN_POINT('Ctrl Pts',(36.0848883531952,60.5229032758974,12.));
#164610=CARTESIAN_POINT('Ctrl Pts',(36.0697797118375,60.5088129911354,0.));
#164611=CARTESIAN_POINT('Ctrl Pts',(36.0697797118375,60.5088129911354,12.));
#164612=CARTESIAN_POINT('Ctrl Pts',(36.0547232187697,60.4947416988422,0.));
#164613=CARTESIAN_POINT('Ctrl Pts',(36.0547232187697,60.4947416988422,12.));
#164614=CARTESIAN_POINT('Ctrl Pts',(36.0397189421644,60.4806895737686,0.));
#164615=CARTESIAN_POINT('Ctrl Pts',(36.0397189421644,60.4806895737686,12.));
#164616=CARTESIAN_POINT('Ctrl Pts',(36.0247669500891,60.4666567908093,0.));
#164617=CARTESIAN_POINT('Ctrl Pts',(36.0247669500891,60.4666567908093,12.));
#164618=CARTESIAN_POINT('Ctrl Pts',(36.009867311357,60.4526435269662,0.));
#164619=CARTESIAN_POINT('Ctrl Pts',(36.009867311357,60.4526435269662,12.));
#164620=CARTESIAN_POINT('Ctrl Pts',(35.995020096217,60.4386499629481,0.));
#164621=CARTESIAN_POINT('Ctrl Pts',(35.995020096217,60.4386499629481,12.));
#164622=CARTESIAN_POINT('Ctrl Pts',(35.9802253773514,60.4246762854926,0.));
#164623=CARTESIAN_POINT('Ctrl Pts',(35.9802253773514,60.4246762854926,12.));
#164624=CARTESIAN_POINT('Ctrl Pts',(35.9654832299601,60.4107226875714,0.));
#164625=CARTESIAN_POINT('Ctrl Pts',(35.9654832299601,60.4107226875714,12.));
#164626=CARTESIAN_POINT('Ctrl Pts',(35.9507937296706,60.3967893635452,0.));
#164627=CARTESIAN_POINT('Ctrl Pts',(35.9507937296706,60.3967893635452,12.));
#164628=CARTESIAN_POINT('Ctrl Pts',(35.9361569506949,60.3828765049019,0.));
#164629=CARTESIAN_POINT('Ctrl Pts',(35.9361569506949,60.3828765049019,12.));
#164630=CARTESIAN_POINT('Ctrl Pts',(35.9215729642231,60.3689842965481,0.));
#164631=CARTESIAN_POINT('Ctrl Pts',(35.9215729642231,60.3689842965481,12.));
#164632=CARTESIAN_POINT('Ctrl Pts',(35.907041835853,60.3551129108845,0.));
#164633=CARTESIAN_POINT('Ctrl Pts',(35.907041835853,60.3551129108845,12.));
#164634=CARTESIAN_POINT('Ctrl Pts',(35.8925636280668,60.3412625135287,0.));
#164635=CARTESIAN_POINT('Ctrl Pts',(35.8925636280668,60.3412625135287,12.));
#164636=CARTESIAN_POINT('Ctrl Pts',(35.8781384051536,60.327433274683,0.));
#164637=CARTESIAN_POINT('Ctrl Pts',(35.8781384051536,60.327433274683,12.));
#164638=CARTESIAN_POINT('Ctrl Pts',(35.8637662371635,60.313625378281,0.));
#164639=CARTESIAN_POINT('Ctrl Pts',(35.8637662371635,60.313625378281,12.));
#164640=CARTESIAN_POINT('Ctrl Pts',(35.8494472046745,60.2998390330102,0.));
#164641=CARTESIAN_POINT('Ctrl Pts',(35.8494472046745,60.2998390330102,12.));
#164642=CARTESIAN_POINT('Ctrl Pts',(35.8351814020356,60.2860744798436,0.));
#164643=CARTESIAN_POINT('Ctrl Pts',(35.8351814020356,60.2860744798436,12.));
#164644=CARTESIAN_POINT('Ctrl Pts',(35.82096892725,60.2723319687369,0.));
#164645=CARTESIAN_POINT('Ctrl Pts',(35.82096892725,60.2723319687369,12.));
#164646=CARTESIAN_POINT('Ctrl Pts',(35.8068098723347,60.2586117365205,0.));
#164647=CARTESIAN_POINT('Ctrl Pts',(35.8068098723347,60.2586117365205,12.));
#164648=CARTESIAN_POINT('Ctrl Pts',(35.7927043145201,60.2449139865275,0.));
#164649=CARTESIAN_POINT('Ctrl Pts',(35.7927043145201,60.2449139865275,12.));
#164650=CARTESIAN_POINT('Ctrl Pts',(35.7786523045911,60.2312388621529,0.));
#164651=CARTESIAN_POINT('Ctrl Pts',(35.7786523045911,60.2312388621529,12.));
#164652=CARTESIAN_POINT('Ctrl Pts',(35.7646538667493,60.2175864450043,0.));
#164653=CARTESIAN_POINT('Ctrl Pts',(35.7646538667493,60.2175864450043,12.));
#164654=CARTESIAN_POINT('Ctrl Pts',(35.7534979802053,60.206682708692,0.));
#164655=CARTESIAN_POINT('Ctrl Pts',(35.7534979802053,60.206682708692,12.));
#164656=CARTESIAN_POINT('Ctrl Pts',(35.7451551752572,60.1985151474623,0.));
#164657=CARTESIAN_POINT('Ctrl Pts',(35.7451551752572,60.1985151474623,12.));
#164658=CARTESIAN_POINT('Ctrl Pts',(35.7396040204017,60.193074658032,0.));
#164659=CARTESIAN_POINT('Ctrl Pts',(35.7396040204017,60.193074658032,12.));
#164660=CARTESIAN_POINT('Ctrl Pts',(35.7368311217509,60.1903555511633,0.));
#164661=CARTESIAN_POINT('Ctrl Pts',(35.7368311217509,60.1903555511633,12.));
#164662=CARTESIAN_POINT('',(35.7368311217509,60.1903555511633,12.));
#164663=CARTESIAN_POINT('Ctrl Pts',(35.7368311217509,60.1903555511633,12.));
#164664=CARTESIAN_POINT('Ctrl Pts',(35.7396040204017,60.193074658032,12.));
#164665=CARTESIAN_POINT('Ctrl Pts',(35.7451551752572,60.1985151474623,12.));
#164666=CARTESIAN_POINT('Ctrl Pts',(35.7534979802053,60.206682708692,12.));
#164667=CARTESIAN_POINT('Ctrl Pts',(35.7646538667493,60.2175864450043,12.));
#164668=CARTESIAN_POINT('Ctrl Pts',(35.7786523045911,60.2312388621529,12.));
#164669=CARTESIAN_POINT('Ctrl Pts',(35.7927043145201,60.2449139865275,12.));
#164670=CARTESIAN_POINT('Ctrl Pts',(35.8068098723347,60.2586117365205,12.));
#164671=CARTESIAN_POINT('Ctrl Pts',(35.82096892725,60.2723319687369,12.));
#164672=CARTESIAN_POINT('Ctrl Pts',(35.8351814020356,60.2860744798436,12.));
#164673=CARTESIAN_POINT('Ctrl Pts',(35.8494472046745,60.2998390330102,12.));
#164674=CARTESIAN_POINT('Ctrl Pts',(35.8637662371635,60.313625378281,12.));
#164675=CARTESIAN_POINT('Ctrl Pts',(35.8781384051536,60.327433274683,12.));
#164676=CARTESIAN_POINT('Ctrl Pts',(35.8925636280668,60.3412625135287,12.));
#164677=CARTESIAN_POINT('Ctrl Pts',(35.907041835853,60.3551129108845,12.));
#164678=CARTESIAN_POINT('Ctrl Pts',(35.9215729642231,60.3689842965481,12.));
#164679=CARTESIAN_POINT('Ctrl Pts',(35.9361569506949,60.3828765049019,12.));
#164680=CARTESIAN_POINT('Ctrl Pts',(35.9507937296706,60.3967893635452,12.));
#164681=CARTESIAN_POINT('Ctrl Pts',(35.9654832299601,60.4107226875714,12.));
#164682=CARTESIAN_POINT('Ctrl Pts',(35.9802253773514,60.4246762854926,12.));
#164683=CARTESIAN_POINT('Ctrl Pts',(35.995020096217,60.4386499629481,12.));
#164684=CARTESIAN_POINT('Ctrl Pts',(36.009867311357,60.4526435269662,12.));
#164685=CARTESIAN_POINT('Ctrl Pts',(36.0247669500891,60.4666567908093,12.));
#164686=CARTESIAN_POINT('Ctrl Pts',(36.0397189421644,60.4806895737686,12.));
#164687=CARTESIAN_POINT('Ctrl Pts',(36.0547232187697,60.4947416988422,12.));
#164688=CARTESIAN_POINT('Ctrl Pts',(36.0697797118375,60.5088129911354,12.));
#164689=CARTESIAN_POINT('Ctrl Pts',(36.0848883531952,60.5229032758974,12.));
#164690=CARTESIAN_POINT('Ctrl Pts',(36.100049073851,60.5370123768804,12.));
#164691=CARTESIAN_POINT('Ctrl Pts',(36.1152618043738,60.5511401171984,12.));
#164692=CARTESIAN_POINT('Ctrl Pts',(36.1305264752187,60.565286320072,12.));
#164693=CARTESIAN_POINT('Ctrl Pts',(36.145843017043,60.5794508095565,12.));
#164694=CARTESIAN_POINT('Ctrl Pts',(36.1612113610773,60.5936334114108,12.));
#164695=CARTESIAN_POINT('Ctrl Pts',(36.1766314392641,60.6078339534181,12.));
#164696=CARTESIAN_POINT('Ctrl Pts',(36.1921031840629,60.6220522649149,12.));
#164697=CARTESIAN_POINT('Ctrl Pts',(36.2076265283264,60.6362881765019,12.));
#164698=CARTESIAN_POINT('Ctrl Pts',(36.2232014051541,60.6505415197042,12.));
#164699=CARTESIAN_POINT('Ctrl Pts',(36.2388277477212,60.6648121265885,12.));
#164700=CARTESIAN_POINT('Ctrl Pts',(36.2545054892897,60.67909982978,12.));
#164701=CARTESIAN_POINT('Ctrl Pts',(36.2702345632875,60.6934044626291,12.));
#164702=CARTESIAN_POINT('Ctrl Pts',(36.2860149033587,60.7077258593268,12.));
#164703=CARTESIAN_POINT('Ctrl Pts',(36.3018464434213,60.722063855041,12.));
#164704=CARTESIAN_POINT('Ctrl Pts',(36.3177291177163,60.7364182860412,12.));
#164705=CARTESIAN_POINT('Ctrl Pts',(36.3336628607858,60.7507889896308,12.));
#164706=CARTESIAN_POINT('Ctrl Pts',(36.3496476074488,60.7651758040804,12.));
#164707=CARTESIAN_POINT('Ctrl Pts',(36.365683292773,60.7795785685625,12.));
#164708=CARTESIAN_POINT('Ctrl Pts',(36.3817698520388,60.7939971230761,12.));
#164709=CARTESIAN_POINT('Ctrl Pts',(36.397907220716,60.8084313083984,12.));
#164710=CARTESIAN_POINT('Ctrl Pts',(36.4140953344858,60.8228809661161,12.));
#164711=CARTESIAN_POINT('Ctrl Pts',(36.4303341292494,60.8373459386392,12.));
#164712=CARTESIAN_POINT('Ctrl Pts',(36.4466235411358,60.8518260692188,12.));
#164713=CARTESIAN_POINT('Ctrl Pts',(36.4629635065045,60.8663212019657,12.));
#164714=CARTESIAN_POINT('Ctrl Pts',(36.4793539619466,60.8808311818499,12.));
#164715=CARTESIAN_POINT('Ctrl Pts',(36.4957948442835,60.8953558546795,12.));
#164716=CARTESIAN_POINT('Ctrl Pts',(36.5122860905612,60.9098950670847,12.));
#164717=CARTESIAN_POINT('Ctrl Pts',(36.5288276380416,60.9244486664988,12.));
#164718=CARTESIAN_POINT('Ctrl Pts',(36.5454194241865,60.9390165011355,12.));
#164719=CARTESIAN_POINT('Ctrl Pts',(36.5620613866614,60.9535984199873,12.));
#164720=CARTESIAN_POINT('Ctrl Pts',(36.5787534633415,60.9681942728237,12.));
#164721=CARTESIAN_POINT('Ctrl Pts',(36.5954955923109,60.9828039101887,12.));
#164722=CARTESIAN_POINT('Ctrl Pts',(36.61228771186,60.9974271833981,12.));
#164723=CARTESIAN_POINT('Ctrl Pts',(36.6291297604776,61.0120639445349,12.));
#164724=CARTESIAN_POINT('Ctrl Pts',(36.6460216768553,61.0267140464432,12.));
#164725=CARTESIAN_POINT('Ctrl Pts',(36.6629633998886,61.0413773427203,12.));
#164726=CARTESIAN_POINT('Ctrl Pts',(36.679954868674,61.0560536877083,12.));
#164727=CARTESIAN_POINT('Ctrl Pts',(36.6969960225022,61.0707429364847,12.));
#164728=CARTESIAN_POINT('Ctrl Pts',(36.7140868008486,61.0854449448524,12.));
#164729=CARTESIAN_POINT('Ctrl Pts',(36.7312271433807,61.100159569337,12.));
#164730=CARTESIAN_POINT('Ctrl Pts',(36.7484169899596,61.1148866671829,12.));
#164731=CARTESIAN_POINT('Ctrl Pts',(36.765656280638,61.1296260963466,12.));
#164732=CARTESIAN_POINT('Ctrl Pts',(36.7829449556532,61.1443777154911,12.));
#164733=CARTESIAN_POINT('Ctrl Pts',(36.8002829554209,61.1591413839787,12.));
#164734=CARTESIAN_POINT('Ctrl Pts',(36.8176702205423,61.1739169618667,12.));
#164735=CARTESIAN_POINT('Ctrl Pts',(36.8351066918036,61.1887043099014,12.));
#164736=CARTESIAN_POINT('Ctrl Pts',(36.852592310174,61.2035032895127,12.));
#164737=CARTESIAN_POINT('Ctrl Pts',(36.8701270167969,61.2183137628056,12.));
#164738=CARTESIAN_POINT('Ctrl Pts',(36.8877107529865,61.2331355925547,12.));
#164739=CARTESIAN_POINT('Ctrl Pts',(36.9053434602343,61.247968642201,12.));
#164740=CARTESIAN_POINT('Ctrl Pts',(36.9230250802087,61.2628127758457,12.));
#164741=CARTESIAN_POINT('Ctrl Pts',(36.9407555547534,61.2776678582461,12.));
#164742=CARTESIAN_POINT('Ctrl Pts',(36.9585348258776,61.2925337548077,12.));
#164743=CARTESIAN_POINT('Ctrl Pts',(36.9763628357544,61.3074103315792,12.));
#164744=CARTESIAN_POINT('Ctrl Pts',(36.994239526727,61.3222974552487,12.));
#164745=CARTESIAN_POINT('Ctrl Pts',(37.0121648413081,61.3371949931387,12.));
#164746=CARTESIAN_POINT('Ctrl Pts',(37.0301387221774,61.3521028132003,12.));
#164747=CARTESIAN_POINT('Ctrl Pts',(37.0481611121717,61.3670207840069,12.));
#164748=CARTESIAN_POINT('Ctrl Pts',(37.0662319542849,61.381948774749,12.));
#164749=CARTESIAN_POINT('Ctrl Pts',(37.0843511916744,61.3968866552318,12.));
#164750=CARTESIAN_POINT('Ctrl Pts',(37.1025187676602,61.4118342958697,12.));
#164751=CARTESIAN_POINT('Ctrl Pts',(37.1207346257221,61.4267915676822,12.));
#164752=CARTESIAN_POINT('Ctrl Pts',(37.1389987094904,61.4417583422863,12.));
#164753=CARTESIAN_POINT('Ctrl Pts',(37.1573109627454,61.456734491892,12.));
#164754=CARTESIAN_POINT('Ctrl Pts',(37.175671329424,61.4717198892994,12.));
#164755=CARTESIAN_POINT('Ctrl Pts',(37.1940797536181,61.4867144078937,12.));
#164756=CARTESIAN_POINT('Ctrl Pts',(37.2125361795731,61.501717921641,12.));
#164757=CARTESIAN_POINT('Ctrl Pts',(37.2310405516781,61.5167303050832,12.));
#164758=CARTESIAN_POINT('Ctrl Pts',(37.2495928144666,61.5317514333328,12.));
#164759=CARTESIAN_POINT('Ctrl Pts',(37.2681929126221,61.5467811820691,12.));
#164760=CARTESIAN_POINT('Ctrl Pts',(37.286840790977,61.5618194275348,12.));
#164761=CARTESIAN_POINT('Ctrl Pts',(37.3055363945107,61.5768660465311,12.));
#164762=CARTESIAN_POINT('Ctrl Pts',(37.3242796683395,61.591920916412,12.));
#164763=CARTESIAN_POINT('Ctrl Pts',(37.343070557718,61.6069839150807,12.));
#164764=CARTESIAN_POINT('Ctrl Pts',(37.3619090080449,61.6220549209866,12.));
#164765=CARTESIAN_POINT('Ctrl Pts',(37.3807949648624,61.637133813121,12.));
#164766=CARTESIAN_POINT('Ctrl Pts',(37.3997283738533,61.6522204710131,12.));
#164767=CARTESIAN_POINT('Ctrl Pts',(37.418709180832,61.6673147747242,12.));
#164768=CARTESIAN_POINT('Ctrl Pts',(37.4377373317451,61.6824166048444,12.));
#164769=CARTESIAN_POINT('Ctrl Pts',(37.4568127726773,61.6975258424894,12.));
#164770=CARTESIAN_POINT('Ctrl Pts',(37.4759354498509,61.7126423692963,12.));
#164771=CARTESIAN_POINT('Ctrl Pts',(37.4951053096237,61.7277660674205,12.));
#164772=CARTESIAN_POINT('Ctrl Pts',(37.5143222984795,61.7428968195299,12.));
#164773=CARTESIAN_POINT('Ctrl Pts',(37.5335863630287,61.7580345088016,12.));
#164774=CARTESIAN_POINT('Ctrl Pts',(37.5528974500141,61.7731790189191,12.));
#164775=CARTESIAN_POINT('Ctrl Pts',(37.5722555063111,61.7883302340687,12.));
#164776=CARTESIAN_POINT('Ctrl Pts',(37.5916604789253,61.8034880389363,12.));
#164777=CARTESIAN_POINT('Ctrl Pts',(37.6111123149839,61.8186523187015,12.));
#164778=CARTESIAN_POINT('Ctrl Pts',(37.6306109617346,61.8338229590353,12.));
#164779=CARTESIAN_POINT('Ctrl Pts',(37.6501563665523,61.8489998460957,12.));
#164780=CARTESIAN_POINT('Ctrl Pts',(37.6697484769392,61.8641828665262,12.));
#164781=CARTESIAN_POINT('Ctrl Pts',(37.6893872405228,61.8793719074507,12.));
#164782=CARTESIAN_POINT('Ctrl Pts',(37.7090726050482,61.8945668564704,12.));
#164783=CARTESIAN_POINT('Ctrl Pts',(37.7288045183756,61.9097676016601,12.));
#164784=CARTESIAN_POINT('Ctrl Pts',(37.7485829284871,61.9249740315649,12.));
#164785=CARTESIAN_POINT('Ctrl Pts',(37.7684077834872,61.9401860351973,12.));
#164786=CARTESIAN_POINT('Ctrl Pts',(37.7882790316014,61.9554035020338,12.));
#164787=CARTESIAN_POINT('Ctrl Pts',(37.8081966211688,61.9706263220114,12.));
#164788=CARTESIAN_POINT('Ctrl Pts',(37.828160500638,61.9858543855236,12.));
#164789=CARTESIAN_POINT('Ctrl Pts',(37.8481706185749,62.0010875834187,12.));
#164790=CARTESIAN_POINT('Ctrl Pts',(37.868226923663,62.0163258069957,12.));
#164791=CARTESIAN_POINT('Ctrl Pts',(37.8883293647029,62.031568948002,12.));
#164792=CARTESIAN_POINT('Ctrl Pts',(37.9084778906053,62.0468168986288,12.));
#164793=CARTESIAN_POINT('Ctrl Pts',(37.9286724503851,62.0620695515075,12.));
#164794=CARTESIAN_POINT('Ctrl Pts',(37.9489129931688,62.0773267997079,12.));
#164795=CARTESIAN_POINT('Ctrl Pts',(37.9691994681966,62.0925885367352,12.));
#164796=CARTESIAN_POINT('Ctrl Pts',(37.9895318248212,62.107854656528,12.));
#164797=CARTESIAN_POINT('Ctrl Pts',(38.0099100125037,62.123125053455,12.));
#164798=CARTESIAN_POINT('Ctrl Pts',(38.0303339808053,62.1383996223125,12.));
#164799=CARTESIAN_POINT('Ctrl Pts',(38.0508036793939,62.1536782583199,12.));
#164800=CARTESIAN_POINT('Ctrl Pts',(38.0713190580463,62.1689608571176,12.));
#164801=CARTESIAN_POINT('Ctrl Pts',(38.0918800666479,62.1842473147626,12.));
#164802=CARTESIAN_POINT('Ctrl Pts',(38.1124866551885,62.1995375277257,12.));
#164803=CARTESIAN_POINT('Ctrl Pts',(38.1331387737529,62.2148313928863,12.));
#164804=CARTESIAN_POINT('Ctrl Pts',(38.1538363725263,62.2301288075321,12.));
#164805=CARTESIAN_POINT('Ctrl Pts',(38.1745794017995,62.245429669358,12.));
#164806=CARTESIAN_POINT('Ctrl Pts',(38.1953678119691,62.2607338764654,12.));
#164807=CARTESIAN_POINT('Ctrl Pts',(38.2162015535352,62.2760413273602,12.));
#164808=CARTESIAN_POINT('Ctrl Pts',(38.2370805770935,62.2913519209521,12.));
#164809=CARTESIAN_POINT('Ctrl Pts',(38.258004833336,62.3066655565503,12.));
#164810=CARTESIAN_POINT('Ctrl Pts',(38.2789742730563,62.3219821338569,12.));
#164811=CARTESIAN_POINT('Ctrl Pts',(38.2999888471476,62.3373015529613,12.));
#164812=CARTESIAN_POINT('Ctrl Pts',(38.3210485066001,62.3526237143336,12.));
#164813=CARTESIAN_POINT('Ctrl Pts',(38.342153202491,62.3679485188172,12.));
#164814=CARTESIAN_POINT('Ctrl Pts',(38.3633028859828,62.3832758676271,12.));
#164815=CARTESIAN_POINT('Ctrl Pts',(38.3844975083343,62.3986056623577,12.));
#164816=CARTESIAN_POINT('Ctrl Pts',(38.405737020905,62.4139378049886,12.));
#164817=CARTESIAN_POINT('Ctrl Pts',(38.4270213751568,62.4292721978901,12.));
#164818=CARTESIAN_POINT('Ctrl Pts',(38.4483505226518,62.4446087438312,12.));
#164819=CARTESIAN_POINT('Ctrl Pts',(38.4697244150482,62.4599473459811,12.));
#164820=CARTESIAN_POINT('Ctrl Pts',(38.4911430040997,62.4752879078854,12.));
#164821=CARTESIAN_POINT('Ctrl Pts',(38.5126062416502,62.4906303334443,12.));
#164822=CARTESIAN_POINT('Ctrl Pts',(38.5341140796248,62.5059745268901,12.));
#164823=CARTESIAN_POINT('Ctrl Pts',(38.5556664700195,62.5213203927663,12.));
#164824=CARTESIAN_POINT('Ctrl Pts',(38.5772633648832,62.5366678359023,12.));
#164825=CARTESIAN_POINT('Ctrl Pts',(38.5989047163393,62.5520167614516,12.));
#164826=CARTESIAN_POINT('Ctrl Pts',(38.6205904766072,62.5673670749362,12.));
#164827=CARTESIAN_POINT('Ctrl Pts',(38.6423205980213,62.5827186822921,12.));
#164828=CARTESIAN_POINT('Ctrl Pts',(38.6640950330421,62.5980714899052,12.));
#164829=CARTESIAN_POINT('Ctrl Pts',(38.685913734273,62.6134254046739,12.));
#164830=CARTESIAN_POINT('Ctrl Pts',(38.7077766544416,62.6287803339542,12.));
#164831=CARTESIAN_POINT('Ctrl Pts',(38.7296837463608,62.6441361854411,12.));
#164832=CARTESIAN_POINT('Ctrl Pts',(38.7516349628903,62.6594928670628,12.));
#164833=CARTESIAN_POINT('Ctrl Pts',(38.7736302568982,62.6748502868835,12.));
#164834=CARTESIAN_POINT('Ctrl Pts',(38.795669581203,62.6902083529695,12.));
#164835=CARTESIAN_POINT('Ctrl Pts',(38.8177528885681,62.7055669733802,12.));
#164836=CARTESIAN_POINT('Ctrl Pts',(38.8398801318176,62.7209260564493,12.));
#164837=CARTESIAN_POINT('Ctrl Pts',(38.8620512639232,62.7362855110042,12.));
#164838=CARTESIAN_POINT('Ctrl Pts',(38.8842662380984,62.7516452466128,12.));
#164839=CARTESIAN_POINT('Ctrl Pts',(38.9065250078832,62.7670051738143,12.));
#164840=CARTESIAN_POINT('Ctrl Pts',(38.9288275272335,62.78236520437,12.));
#164841=CARTESIAN_POINT('Ctrl Pts',(38.9511737503165,62.7977252507118,12.));
#164842=CARTESIAN_POINT('Ctrl Pts',(38.9735636313088,62.8130852254027,12.));
#164843=CARTESIAN_POINT('Ctrl Pts',(38.9959971241701,62.8284450405459,12.));
#164844=CARTESIAN_POINT('Ctrl Pts',(39.0184741824641,62.8438046073224,12.));
#164845=CARTESIAN_POINT('Ctrl Pts',(39.0409947590496,62.8591638352056,12.));
#164846=CARTESIAN_POINT('Ctrl Pts',(39.0635588063276,62.8745226325998,12.));
#164847=CARTESIAN_POINT('Ctrl Pts',(39.0861662767932,62.8898809082612,12.));
#164848=CARTESIAN_POINT('Ctrl Pts',(39.1088171235125,62.9052385725388,12.));
#164849=CARTESIAN_POINT('Ctrl Pts',(39.131511300575,62.9205955385558,12.));
#164850=CARTESIAN_POINT('Ctrl Pts',(39.1542487636743,62.9359517237404,12.));
#164851=CARTESIAN_POINT('Ctrl Pts',(39.1770294702428,62.9513070501867,12.));
#164852=CARTESIAN_POINT('Ctrl Pts',(39.1965939820933,62.9644687386836,12.));
#164853=CARTESIAN_POINT('Ctrl Pts',(39.2116170128461,62.9745590018673,12.));
#164854=CARTESIAN_POINT('Ctrl Pts',(39.2220794388807,62.9815782721326,12.));
#164855=CARTESIAN_POINT('Ctrl Pts',(39.2279686275008,62.9855268616129,12.));
#164856=CARTESIAN_POINT('Ctrl Pts',(39.2292784191814,62.9864049293895,12.));
#164857=CARTESIAN_POINT('',(35.7368311217509,60.1903555511633,0.));
#164858=CARTESIAN_POINT('',(35.7368311217509,60.1903555511633,0.));
#164859=CARTESIAN_POINT('Ctrl Pts',(39.2292784191814,62.9864049293895,0.));
#164860=CARTESIAN_POINT('Ctrl Pts',(39.2279686275008,62.9855268616129,0.));
#164861=CARTESIAN_POINT('Ctrl Pts',(39.2220794388807,62.9815782721326,0.));
#164862=CARTESIAN_POINT('Ctrl Pts',(39.2116170128461,62.9745590018673,0.));
#164863=CARTESIAN_POINT('Ctrl Pts',(39.1965939820933,62.9644687386836,0.));
#164864=CARTESIAN_POINT('Ctrl Pts',(39.1770294702428,62.9513070501867,0.));
#164865=CARTESIAN_POINT('Ctrl Pts',(39.1542487636743,62.9359517237404,0.));
#164866=CARTESIAN_POINT('Ctrl Pts',(39.131511300575,62.9205955385558,0.));
#164867=CARTESIAN_POINT('Ctrl Pts',(39.1088171235125,62.9052385725388,0.));
#164868=CARTESIAN_POINT('Ctrl Pts',(39.0861662767932,62.8898809082612,0.));
#164869=CARTESIAN_POINT('Ctrl Pts',(39.0635588063276,62.8745226325998,0.));
#164870=CARTESIAN_POINT('Ctrl Pts',(39.0409947590496,62.8591638352056,0.));
#164871=CARTESIAN_POINT('Ctrl Pts',(39.0184741824641,62.8438046073224,0.));
#164872=CARTESIAN_POINT('Ctrl Pts',(38.9959971241701,62.8284450405459,0.));
#164873=CARTESIAN_POINT('Ctrl Pts',(38.9735636313088,62.8130852254027,0.));
#164874=CARTESIAN_POINT('Ctrl Pts',(38.9511737503165,62.7977252507118,0.));
#164875=CARTESIAN_POINT('Ctrl Pts',(38.9288275272335,62.78236520437,0.));
#164876=CARTESIAN_POINT('Ctrl Pts',(38.9065250078832,62.7670051738143,0.));
#164877=CARTESIAN_POINT('Ctrl Pts',(38.8842662380984,62.7516452466128,0.));
#164878=CARTESIAN_POINT('Ctrl Pts',(38.8620512639232,62.7362855110042,0.));
#164879=CARTESIAN_POINT('Ctrl Pts',(38.8398801318176,62.7209260564493,0.));
#164880=CARTESIAN_POINT('Ctrl Pts',(38.8177528885681,62.7055669733802,0.));
#164881=CARTESIAN_POINT('Ctrl Pts',(38.795669581203,62.6902083529695,0.));
#164882=CARTESIAN_POINT('Ctrl Pts',(38.7736302568982,62.6748502868835,0.));
#164883=CARTESIAN_POINT('Ctrl Pts',(38.7516349628903,62.6594928670628,0.));
#164884=CARTESIAN_POINT('Ctrl Pts',(38.7296837463608,62.6441361854411,0.));
#164885=CARTESIAN_POINT('Ctrl Pts',(38.7077766544416,62.6287803339542,0.));
#164886=CARTESIAN_POINT('Ctrl Pts',(38.685913734273,62.6134254046739,0.));
#164887=CARTESIAN_POINT('Ctrl Pts',(38.6640950330421,62.5980714899052,0.));
#164888=CARTESIAN_POINT('Ctrl Pts',(38.6423205980213,62.5827186822921,0.));
#164889=CARTESIAN_POINT('Ctrl Pts',(38.6205904766072,62.5673670749362,0.));
#164890=CARTESIAN_POINT('Ctrl Pts',(38.5989047163393,62.5520167614516,0.));
#164891=CARTESIAN_POINT('Ctrl Pts',(38.5772633648832,62.5366678359023,0.));
#164892=CARTESIAN_POINT('Ctrl Pts',(38.5556664700195,62.5213203927663,0.));
#164893=CARTESIAN_POINT('Ctrl Pts',(38.5341140796248,62.5059745268901,0.));
#164894=CARTESIAN_POINT('Ctrl Pts',(38.5126062416502,62.4906303334443,0.));
#164895=CARTESIAN_POINT('Ctrl Pts',(38.4911430040997,62.4752879078854,0.));
#164896=CARTESIAN_POINT('Ctrl Pts',(38.4697244150482,62.4599473459811,0.));
#164897=CARTESIAN_POINT('Ctrl Pts',(38.4483505226518,62.4446087438312,0.));
#164898=CARTESIAN_POINT('Ctrl Pts',(38.4270213751568,62.4292721978901,0.));
#164899=CARTESIAN_POINT('Ctrl Pts',(38.405737020905,62.4139378049886,0.));
#164900=CARTESIAN_POINT('Ctrl Pts',(38.3844975083343,62.3986056623577,0.));
#164901=CARTESIAN_POINT('Ctrl Pts',(38.3633028859828,62.3832758676271,0.));
#164902=CARTESIAN_POINT('Ctrl Pts',(38.342153202491,62.3679485188172,0.));
#164903=CARTESIAN_POINT('Ctrl Pts',(38.3210485066001,62.3526237143336,0.));
#164904=CARTESIAN_POINT('Ctrl Pts',(38.2999888471476,62.3373015529613,0.));
#164905=CARTESIAN_POINT('Ctrl Pts',(38.2789742730563,62.3219821338569,0.));
#164906=CARTESIAN_POINT('Ctrl Pts',(38.258004833336,62.3066655565503,0.));
#164907=CARTESIAN_POINT('Ctrl Pts',(38.2370805770935,62.2913519209521,0.));
#164908=CARTESIAN_POINT('Ctrl Pts',(38.2162015535352,62.2760413273602,0.));
#164909=CARTESIAN_POINT('Ctrl Pts',(38.1953678119691,62.2607338764654,0.));
#164910=CARTESIAN_POINT('Ctrl Pts',(38.1745794017995,62.245429669358,0.));
#164911=CARTESIAN_POINT('Ctrl Pts',(38.1538363725263,62.2301288075321,0.));
#164912=CARTESIAN_POINT('Ctrl Pts',(38.1331387737529,62.2148313928863,0.));
#164913=CARTESIAN_POINT('Ctrl Pts',(38.1124866551885,62.1995375277257,0.));
#164914=CARTESIAN_POINT('Ctrl Pts',(38.0918800666479,62.1842473147626,0.));
#164915=CARTESIAN_POINT('Ctrl Pts',(38.0713190580463,62.1689608571176,0.));
#164916=CARTESIAN_POINT('Ctrl Pts',(38.0508036793939,62.1536782583199,0.));
#164917=CARTESIAN_POINT('Ctrl Pts',(38.0303339808053,62.1383996223125,0.));
#164918=CARTESIAN_POINT('Ctrl Pts',(38.0099100125037,62.123125053455,0.));
#164919=CARTESIAN_POINT('Ctrl Pts',(37.9895318248212,62.107854656528,0.));
#164920=CARTESIAN_POINT('Ctrl Pts',(37.9691994681966,62.0925885367352,0.));
#164921=CARTESIAN_POINT('Ctrl Pts',(37.9489129931688,62.0773267997079,0.));
#164922=CARTESIAN_POINT('Ctrl Pts',(37.9286724503851,62.0620695515075,0.));
#164923=CARTESIAN_POINT('Ctrl Pts',(37.9084778906053,62.0468168986288,0.));
#164924=CARTESIAN_POINT('Ctrl Pts',(37.8883293647029,62.031568948002,0.));
#164925=CARTESIAN_POINT('Ctrl Pts',(37.868226923663,62.0163258069957,0.));
#164926=CARTESIAN_POINT('Ctrl Pts',(37.8481706185749,62.0010875834187,0.));
#164927=CARTESIAN_POINT('Ctrl Pts',(37.828160500638,61.9858543855236,0.));
#164928=CARTESIAN_POINT('Ctrl Pts',(37.8081966211688,61.9706263220114,0.));
#164929=CARTESIAN_POINT('Ctrl Pts',(37.7882790316014,61.9554035020338,0.));
#164930=CARTESIAN_POINT('Ctrl Pts',(37.7684077834872,61.9401860351973,0.));
#164931=CARTESIAN_POINT('Ctrl Pts',(37.7485829284871,61.9249740315649,0.));
#164932=CARTESIAN_POINT('Ctrl Pts',(37.7288045183756,61.9097676016601,0.));
#164933=CARTESIAN_POINT('Ctrl Pts',(37.7090726050482,61.8945668564704,0.));
#164934=CARTESIAN_POINT('Ctrl Pts',(37.6893872405228,61.8793719074507,0.));
#164935=CARTESIAN_POINT('Ctrl Pts',(37.6697484769392,61.8641828665262,0.));
#164936=CARTESIAN_POINT('Ctrl Pts',(37.6501563665523,61.8489998460957,0.));
#164937=CARTESIAN_POINT('Ctrl Pts',(37.6306109617346,61.8338229590353,0.));
#164938=CARTESIAN_POINT('Ctrl Pts',(37.6111123149839,61.8186523187015,0.));
#164939=CARTESIAN_POINT('Ctrl Pts',(37.5916604789253,61.8034880389363,0.));
#164940=CARTESIAN_POINT('Ctrl Pts',(37.5722555063111,61.7883302340687,0.));
#164941=CARTESIAN_POINT('Ctrl Pts',(37.5528974500141,61.7731790189191,0.));
#164942=CARTESIAN_POINT('Ctrl Pts',(37.5335863630287,61.7580345088016,0.));
#164943=CARTESIAN_POINT('Ctrl Pts',(37.5143222984795,61.7428968195299,0.));
#164944=CARTESIAN_POINT('Ctrl Pts',(37.4951053096237,61.7277660674205,0.));
#164945=CARTESIAN_POINT('Ctrl Pts',(37.4759354498509,61.7126423692963,0.));
#164946=CARTESIAN_POINT('Ctrl Pts',(37.4568127726773,61.6975258424894,0.));
#164947=CARTESIAN_POINT('Ctrl Pts',(37.4377373317451,61.6824166048444,0.));
#164948=CARTESIAN_POINT('Ctrl Pts',(37.418709180832,61.6673147747242,0.));
#164949=CARTESIAN_POINT('Ctrl Pts',(37.3997283738533,61.6522204710131,0.));
#164950=CARTESIAN_POINT('Ctrl Pts',(37.3807949648624,61.637133813121,0.));
#164951=CARTESIAN_POINT('Ctrl Pts',(37.3619090080449,61.6220549209866,0.));
#164952=CARTESIAN_POINT('Ctrl Pts',(37.343070557718,61.6069839150807,0.));
#164953=CARTESIAN_POINT('Ctrl Pts',(37.3242796683395,61.591920916412,0.));
#164954=CARTESIAN_POINT('Ctrl Pts',(37.3055363945107,61.5768660465311,0.));
#164955=CARTESIAN_POINT('Ctrl Pts',(37.286840790977,61.5618194275348,0.));
#164956=CARTESIAN_POINT('Ctrl Pts',(37.2681929126221,61.5467811820691,0.));
#164957=CARTESIAN_POINT('Ctrl Pts',(37.2495928144666,61.5317514333328,0.));
#164958=CARTESIAN_POINT('Ctrl Pts',(37.2310405516781,61.5167303050832,0.));
#164959=CARTESIAN_POINT('Ctrl Pts',(37.2125361795731,61.501717921641,0.));
#164960=CARTESIAN_POINT('Ctrl Pts',(37.1940797536181,61.4867144078937,0.));
#164961=CARTESIAN_POINT('Ctrl Pts',(37.175671329424,61.4717198892994,0.));
#164962=CARTESIAN_POINT('Ctrl Pts',(37.1573109627454,61.456734491892,0.));
#164963=CARTESIAN_POINT('Ctrl Pts',(37.1389987094904,61.4417583422863,0.));
#164964=CARTESIAN_POINT('Ctrl Pts',(37.1207346257221,61.4267915676822,0.));
#164965=CARTESIAN_POINT('Ctrl Pts',(37.1025187676602,61.4118342958697,0.));
#164966=CARTESIAN_POINT('Ctrl Pts',(37.0843511916744,61.3968866552318,0.));
#164967=CARTESIAN_POINT('Ctrl Pts',(37.0662319542849,61.381948774749,0.));
#164968=CARTESIAN_POINT('Ctrl Pts',(37.0481611121717,61.3670207840069,0.));
#164969=CARTESIAN_POINT('Ctrl Pts',(37.0301387221774,61.3521028132003,0.));
#164970=CARTESIAN_POINT('Ctrl Pts',(37.0121648413081,61.3371949931387,0.));
#164971=CARTESIAN_POINT('Ctrl Pts',(36.994239526727,61.3222974552487,0.));
#164972=CARTESIAN_POINT('Ctrl Pts',(36.9763628357544,61.3074103315792,0.));
#164973=CARTESIAN_POINT('Ctrl Pts',(36.9585348258776,61.2925337548077,0.));
#164974=CARTESIAN_POINT('Ctrl Pts',(36.9407555547534,61.2776678582461,0.));
#164975=CARTESIAN_POINT('Ctrl Pts',(36.9230250802087,61.2628127758457,0.));
#164976=CARTESIAN_POINT('Ctrl Pts',(36.9053434602343,61.247968642201,0.));
#164977=CARTESIAN_POINT('Ctrl Pts',(36.8877107529865,61.2331355925547,0.));
#164978=CARTESIAN_POINT('Ctrl Pts',(36.8701270167969,61.2183137628056,0.));
#164979=CARTESIAN_POINT('Ctrl Pts',(36.852592310174,61.2035032895127,0.));
#164980=CARTESIAN_POINT('Ctrl Pts',(36.8351066918036,61.1887043099014,0.));
#164981=CARTESIAN_POINT('Ctrl Pts',(36.8176702205423,61.1739169618667,0.));
#164982=CARTESIAN_POINT('Ctrl Pts',(36.8002829554209,61.1591413839787,0.));
#164983=CARTESIAN_POINT('Ctrl Pts',(36.7829449556532,61.1443777154911,0.));
#164984=CARTESIAN_POINT('Ctrl Pts',(36.765656280638,61.1296260963466,0.));
#164985=CARTESIAN_POINT('Ctrl Pts',(36.7484169899596,61.1148866671829,0.));
#164986=CARTESIAN_POINT('Ctrl Pts',(36.7312271433807,61.100159569337,0.));
#164987=CARTESIAN_POINT('Ctrl Pts',(36.7140868008486,61.0854449448524,0.));
#164988=CARTESIAN_POINT('Ctrl Pts',(36.6969960225022,61.0707429364847,0.));
#164989=CARTESIAN_POINT('Ctrl Pts',(36.679954868674,61.0560536877083,0.));
#164990=CARTESIAN_POINT('Ctrl Pts',(36.6629633998886,61.0413773427203,0.));
#164991=CARTESIAN_POINT('Ctrl Pts',(36.6460216768553,61.0267140464432,0.));
#164992=CARTESIAN_POINT('Ctrl Pts',(36.6291297604776,61.0120639445349,0.));
#164993=CARTESIAN_POINT('Ctrl Pts',(36.61228771186,60.9974271833981,0.));
#164994=CARTESIAN_POINT('Ctrl Pts',(36.5954955923109,60.9828039101887,0.));
#164995=CARTESIAN_POINT('Ctrl Pts',(36.5787534633415,60.9681942728237,0.));
#164996=CARTESIAN_POINT('Ctrl Pts',(36.5620613866614,60.9535984199873,0.));
#164997=CARTESIAN_POINT('Ctrl Pts',(36.5454194241865,60.9390165011355,0.));
#164998=CARTESIAN_POINT('Ctrl Pts',(36.5288276380416,60.9244486664988,0.));
#164999=CARTESIAN_POINT('Ctrl Pts',(36.5122860905612,60.9098950670847,0.));
#165000=CARTESIAN_POINT('Ctrl Pts',(36.4957948442835,60.8953558546795,0.));
#165001=CARTESIAN_POINT('Ctrl Pts',(36.4793539619466,60.8808311818499,0.));
#165002=CARTESIAN_POINT('Ctrl Pts',(36.4629635065045,60.8663212019657,0.));
#165003=CARTESIAN_POINT('Ctrl Pts',(36.4466235411358,60.8518260692188,0.));
#165004=CARTESIAN_POINT('Ctrl Pts',(36.4303341292494,60.8373459386392,0.));
#165005=CARTESIAN_POINT('Ctrl Pts',(36.4140953344858,60.8228809661161,0.));
#165006=CARTESIAN_POINT('Ctrl Pts',(36.397907220716,60.8084313083984,0.));
#165007=CARTESIAN_POINT('Ctrl Pts',(36.3817698520388,60.7939971230761,0.));
#165008=CARTESIAN_POINT('Ctrl Pts',(36.365683292773,60.7795785685625,0.));
#165009=CARTESIAN_POINT('Ctrl Pts',(36.3496476074488,60.7651758040804,0.));
#165010=CARTESIAN_POINT('Ctrl Pts',(36.3336628607858,60.7507889896308,0.));
#165011=CARTESIAN_POINT('Ctrl Pts',(36.3177291177163,60.7364182860412,0.));
#165012=CARTESIAN_POINT('Ctrl Pts',(36.3018464434213,60.722063855041,0.));
#165013=CARTESIAN_POINT('Ctrl Pts',(36.2860149033587,60.7077258593268,0.));
#165014=CARTESIAN_POINT('Ctrl Pts',(36.2702345632875,60.6934044626291,0.));
#165015=CARTESIAN_POINT('Ctrl Pts',(36.2545054892897,60.67909982978,0.));
#165016=CARTESIAN_POINT('Ctrl Pts',(36.2388277477212,60.6648121265885,0.));
#165017=CARTESIAN_POINT('Ctrl Pts',(36.2232014051541,60.6505415197042,0.));
#165018=CARTESIAN_POINT('Ctrl Pts',(36.2076265283264,60.6362881765019,0.));
#165019=CARTESIAN_POINT('Ctrl Pts',(36.1921031840629,60.6220522649149,0.));
#165020=CARTESIAN_POINT('Ctrl Pts',(36.1766314392641,60.6078339534181,0.));
#165021=CARTESIAN_POINT('Ctrl Pts',(36.1612113610773,60.5936334114108,0.));
#165022=CARTESIAN_POINT('Ctrl Pts',(36.145843017043,60.5794508095565,0.));
#165023=CARTESIAN_POINT('Ctrl Pts',(36.1305264752187,60.565286320072,0.));
#165024=CARTESIAN_POINT('Ctrl Pts',(36.1152618043738,60.5511401171984,0.));
#165025=CARTESIAN_POINT('Ctrl Pts',(36.100049073851,60.5370123768804,0.));
#165026=CARTESIAN_POINT('Ctrl Pts',(36.0848883531952,60.5229032758974,0.));
#165027=CARTESIAN_POINT('Ctrl Pts',(36.0697797118375,60.5088129911354,0.));
#165028=CARTESIAN_POINT('Ctrl Pts',(36.0547232187697,60.4947416988422,0.));
#165029=CARTESIAN_POINT('Ctrl Pts',(36.0397189421644,60.4806895737686,0.));
#165030=CARTESIAN_POINT('Ctrl Pts',(36.0247669500891,60.4666567908093,0.));
#165031=CARTESIAN_POINT('Ctrl Pts',(36.009867311357,60.4526435269662,0.));
#165032=CARTESIAN_POINT('Ctrl Pts',(35.995020096217,60.4386499629481,0.));
#165033=CARTESIAN_POINT('Ctrl Pts',(35.9802253773514,60.4246762854926,0.));
#165034=CARTESIAN_POINT('Ctrl Pts',(35.9654832299601,60.4107226875714,0.));
#165035=CARTESIAN_POINT('Ctrl Pts',(35.9507937296706,60.3967893635452,0.));
#165036=CARTESIAN_POINT('Ctrl Pts',(35.9361569506949,60.3828765049019,0.));
#165037=CARTESIAN_POINT('Ctrl Pts',(35.9215729642231,60.3689842965481,0.));
#165038=CARTESIAN_POINT('Ctrl Pts',(35.907041835853,60.3551129108845,0.));
#165039=CARTESIAN_POINT('Ctrl Pts',(35.8925636280668,60.3412625135287,0.));
#165040=CARTESIAN_POINT('Ctrl Pts',(35.8781384051536,60.327433274683,0.));
#165041=CARTESIAN_POINT('Ctrl Pts',(35.8637662371635,60.313625378281,0.));
#165042=CARTESIAN_POINT('Ctrl Pts',(35.8494472046745,60.2998390330102,0.));
#165043=CARTESIAN_POINT('Ctrl Pts',(35.8351814020356,60.2860744798436,0.));
#165044=CARTESIAN_POINT('Ctrl Pts',(35.82096892725,60.2723319687369,0.));
#165045=CARTESIAN_POINT('Ctrl Pts',(35.8068098723347,60.2586117365205,0.));
#165046=CARTESIAN_POINT('Ctrl Pts',(35.7927043145201,60.2449139865275,0.));
#165047=CARTESIAN_POINT('Ctrl Pts',(35.7786523045911,60.2312388621529,0.));
#165048=CARTESIAN_POINT('Ctrl Pts',(35.7646538667493,60.2175864450043,0.));
#165049=CARTESIAN_POINT('Ctrl Pts',(35.7534979802053,60.206682708692,0.));
#165050=CARTESIAN_POINT('Ctrl Pts',(35.7451551752572,60.1985151474623,0.));
#165051=CARTESIAN_POINT('Ctrl Pts',(35.7396040204017,60.193074658032,0.));
#165052=CARTESIAN_POINT('Ctrl Pts',(35.7368311217509,60.1903555511633,0.));
#165053=CARTESIAN_POINT('Ctrl Pts',(44.8554660179045,59.483083043136,0.));
#165054=CARTESIAN_POINT('Ctrl Pts',(44.8554660179045,59.483083043136,12.));
#165055=CARTESIAN_POINT('Ctrl Pts',(44.850535982646,59.4804358983083,0.));
#165056=CARTESIAN_POINT('Ctrl Pts',(44.850535982646,59.4804358983083,12.));
#165057=CARTESIAN_POINT('Ctrl Pts',(44.8406801497742,59.4751410547732,0.));
#165058=CARTESIAN_POINT('Ctrl Pts',(44.8406801497742,59.4751410547732,12.));
#165059=CARTESIAN_POINT('Ctrl Pts',(44.8259091134015,59.4671971278321,0.));
#165060=CARTESIAN_POINT('Ctrl Pts',(44.8259091134015,59.4671971278321,12.));
#165061=CARTESIAN_POINT('Ctrl Pts',(44.8062398251406,59.4566019018254,0.));
#165062=CARTESIAN_POINT('Ctrl Pts',(44.8062398251406,59.4566019018254,12.));
#165063=CARTESIAN_POINT('Ctrl Pts',(44.7816956017528,59.4433523335147,0.));
#165064=CARTESIAN_POINT('Ctrl Pts',(44.7816956017528,59.4433523335147,12.));
#165065=CARTESIAN_POINT('Ctrl Pts',(44.7571937812113,59.4300972403241,0.));
#165066=CARTESIAN_POINT('Ctrl Pts',(44.7571937812113,59.4300972403241,12.));
#165067=CARTESIAN_POINT('Ctrl Pts',(44.7327343876391,59.4168366453118,0.));
#165068=CARTESIAN_POINT('Ctrl Pts',(44.7327343876391,59.4168366453118,12.));
#165069=CARTESIAN_POINT('Ctrl Pts',(44.7083174541702,59.4035705873811,0.));
#165070=CARTESIAN_POINT('Ctrl Pts',(44.7083174541702,59.4035705873811,12.));
#165071=CARTESIAN_POINT('Ctrl Pts',(44.683943024421,59.3902991267889,0.));
#165072=CARTESIAN_POINT('Ctrl Pts',(44.683943024421,59.3902991267889,12.));
#165073=CARTESIAN_POINT('Ctrl Pts',(44.6596111512687,59.377022343519,0.));
#165074=CARTESIAN_POINT('Ctrl Pts',(44.6596111512687,59.377022343519,12.));
#165075=CARTESIAN_POINT('Ctrl Pts',(44.6353218935685,59.3637403301801,0.));
#165076=CARTESIAN_POINT('Ctrl Pts',(44.6353218935685,59.3637403301801,12.));
#165077=CARTESIAN_POINT('Ctrl Pts',(44.6110753134277,59.3504531864154,0.));
#165078=CARTESIAN_POINT('Ctrl Pts',(44.6110753134277,59.3504531864154,12.));
#165079=CARTESIAN_POINT('Ctrl Pts',(44.5868714733234,59.3371610128511,0.));
#165080=CARTESIAN_POINT('Ctrl Pts',(44.5868714733234,59.3371610128511,12.));
#165081=CARTESIAN_POINT('Ctrl Pts',(44.5627104331017,59.3238639048694,0.));
#165082=CARTESIAN_POINT('Ctrl Pts',(44.5627104331017,59.3238639048694,12.));
#165083=CARTESIAN_POINT('Ctrl Pts',(44.5385922475573,59.3105619475609,0.));
#165084=CARTESIAN_POINT('Ctrl Pts',(44.5385922475573,59.3105619475609,12.));
#165085=CARTESIAN_POINT('Ctrl Pts',(44.5145169681349,59.2972552192156,0.));
#165086=CARTESIAN_POINT('Ctrl Pts',(44.5145169681349,59.2972552192156,12.));
#165087=CARTESIAN_POINT('Ctrl Pts',(44.490484644151,59.2839437938237,0.));
#165088=CARTESIAN_POINT('Ctrl Pts',(44.490484644151,59.2839437938237,12.));
#165089=CARTESIAN_POINT('Ctrl Pts',(44.4664953242378,59.2706277440445,0.));
#165090=CARTESIAN_POINT('Ctrl Pts',(44.4664953242378,59.2706277440445,12.));
#165091=CARTESIAN_POINT('Ctrl Pts',(44.4425490575911,59.2573071437774,0.));
#165092=CARTESIAN_POINT('Ctrl Pts',(44.4425490575911,59.2573071437774,12.));
#165093=CARTESIAN_POINT('Ctrl Pts',(44.418645895545,59.2439820714187,0.));
#165094=CARTESIAN_POINT('Ctrl Pts',(44.418645895545,59.2439820714187,12.));
#165095=CARTESIAN_POINT('Ctrl Pts',(44.3947858914074,59.2306526095131,0.));
#165096=CARTESIAN_POINT('Ctrl Pts',(44.3947858914074,59.2306526095131,12.));
#165097=CARTESIAN_POINT('Ctrl Pts',(44.3709690997469,59.2173188432798,0.));
#165098=CARTESIAN_POINT('Ctrl Pts',(44.3709690997469,59.2173188432798,12.));
#165099=CARTESIAN_POINT('Ctrl Pts',(44.3471955758402,59.2039808594752,0.));
#165100=CARTESIAN_POINT('Ctrl Pts',(44.3471955758402,59.2039808594752,12.));
#165101=CARTESIAN_POINT('Ctrl Pts',(44.3234653750884,59.1906387451979,0.));
#165102=CARTESIAN_POINT('Ctrl Pts',(44.3234653750884,59.1906387451979,12.));
#165103=CARTESIAN_POINT('Ctrl Pts',(44.2997785523431,59.1772925865213,0.));
#165104=CARTESIAN_POINT('Ctrl Pts',(44.2997785523431,59.1772925865213,12.));
#165105=CARTESIAN_POINT('Ctrl Pts',(44.2761351616048,59.1639424678793,0.));
#165106=CARTESIAN_POINT('Ctrl Pts',(44.2761351616048,59.1639424678793,12.));
#165107=CARTESIAN_POINT('Ctrl Pts',(44.2525352563996,59.1505884728215,0.));
#165108=CARTESIAN_POINT('Ctrl Pts',(44.2525352563996,59.1505884728215,12.));
#165109=CARTESIAN_POINT('Ctrl Pts',(44.228978889997,59.1372306844586,0.));
#165110=CARTESIAN_POINT('Ctrl Pts',(44.228978889997,59.1372306844586,12.));
#165111=CARTESIAN_POINT('Ctrl Pts',(44.2054661156875,59.1238691860306,0.));
#165112=CARTESIAN_POINT('Ctrl Pts',(44.2054661156875,59.1238691860306,12.));
#165113=CARTESIAN_POINT('Ctrl Pts',(44.1819969870307,59.1105040614276,0.));
#165114=CARTESIAN_POINT('Ctrl Pts',(44.1819969870307,59.1105040614276,12.));
#165115=CARTESIAN_POINT('Ctrl Pts',(44.1585715581064,59.0971353957206,0.));
#165116=CARTESIAN_POINT('Ctrl Pts',(44.1585715581064,59.0971353957206,12.));
#165117=CARTESIAN_POINT('Ctrl Pts',(44.1351898834051,59.08376327492,0.));
#165118=CARTESIAN_POINT('Ctrl Pts',(44.1351898834051,59.08376327492,12.));
#165119=CARTESIAN_POINT('Ctrl Pts',(44.1118520177221,59.0703877857526,0.));
#165120=CARTESIAN_POINT('Ctrl Pts',(44.1118520177221,59.0703877857526,12.));
#165121=CARTESIAN_POINT('Ctrl Pts',(44.0885580160432,59.0570090154242,0.));
#165122=CARTESIAN_POINT('Ctrl Pts',(44.0885580160432,59.0570090154242,12.));
#165123=CARTESIAN_POINT('Ctrl Pts',(44.0653079334385,59.0436270514087,0.));
#165124=CARTESIAN_POINT('Ctrl Pts',(44.0653079334385,59.0436270514087,12.));
#165125=CARTESIAN_POINT('Ctrl Pts',(44.0421018249223,59.0302419811777,0.));
#165126=CARTESIAN_POINT('Ctrl Pts',(44.0421018249223,59.0302419811777,12.));
#165127=CARTESIAN_POINT('Ctrl Pts',(44.0189397454599,59.0168538922095,0.));
#165128=CARTESIAN_POINT('Ctrl Pts',(44.0189397454599,59.0168538922095,12.));
#165129=CARTESIAN_POINT('Ctrl Pts',(43.9958217500369,59.0034628721168,0.));
#165130=CARTESIAN_POINT('Ctrl Pts',(43.9958217500369,59.0034628721168,12.));
#165131=CARTESIAN_POINT('Ctrl Pts',(43.9727478937056,58.9900690087408,0.));
#165132=CARTESIAN_POINT('Ctrl Pts',(43.9727478937056,58.9900690087408,12.));
#165133=CARTESIAN_POINT('Ctrl Pts',(43.9497182316331,58.9766723902529,0.));
#165134=CARTESIAN_POINT('Ctrl Pts',(43.9497182316331,58.9766723902529,12.));
#165135=CARTESIAN_POINT('Ctrl Pts',(43.9267328191501,58.9632731052696,0.));
#165136=CARTESIAN_POINT('Ctrl Pts',(43.9267328191501,58.9632731052696,12.));
#165137=CARTESIAN_POINT('Ctrl Pts',(43.9037917117739,58.9498712429054,0.));
#165138=CARTESIAN_POINT('Ctrl Pts',(43.9037917117739,58.9498712429054,12.));
#165139=CARTESIAN_POINT('Ctrl Pts',(43.8808949651872,58.936466892712,0.));
#165140=CARTESIAN_POINT('Ctrl Pts',(43.8808949651872,58.936466892712,12.));
#165141=CARTESIAN_POINT('Ctrl Pts',(43.858042635223,58.9230601446436,0.));
#165142=CARTESIAN_POINT('Ctrl Pts',(43.858042635223,58.9230601446436,12.));
#165143=CARTESIAN_POINT('Ctrl Pts',(43.835234777842,58.9096510890129,0.));
#165144=CARTESIAN_POINT('Ctrl Pts',(43.835234777842,58.9096510890129,12.));
#165145=CARTESIAN_POINT('Ctrl Pts',(43.8124714491076,58.8962398164493,0.));
#165146=CARTESIAN_POINT('Ctrl Pts',(43.8124714491076,58.8962398164493,12.));
#165147=CARTESIAN_POINT('Ctrl Pts',(43.7897527051609,58.8828264178621,0.));
#165148=CARTESIAN_POINT('Ctrl Pts',(43.7897527051609,58.8828264178621,12.));
#165149=CARTESIAN_POINT('Ctrl Pts',(43.7670786022402,58.8694109844648,0.));
#165150=CARTESIAN_POINT('Ctrl Pts',(43.7670786022402,58.8694109844648,12.));
#165151=CARTESIAN_POINT('Ctrl Pts',(43.7444491966942,58.8559936077941,0.));
#165152=CARTESIAN_POINT('Ctrl Pts',(43.7444491966942,58.8559936077941,12.));
#165153=CARTESIAN_POINT('Ctrl Pts',(43.7218645449922,58.8425743797326,0.));
#165154=CARTESIAN_POINT('Ctrl Pts',(43.7218645449922,58.8425743797326,12.));
#165155=CARTESIAN_POINT('Ctrl Pts',(43.6993247037314,58.8291533925293,0.));
#165156=CARTESIAN_POINT('Ctrl Pts',(43.6993247037314,58.8291533925293,12.));
#165157=CARTESIAN_POINT('Ctrl Pts',(43.6768297296395,58.8157307388238,0.));
#165158=CARTESIAN_POINT('Ctrl Pts',(43.6768297296395,58.8157307388238,12.));
#165159=CARTESIAN_POINT('Ctrl Pts',(43.6543796795789,58.8023065116436,0.));
#165160=CARTESIAN_POINT('Ctrl Pts',(43.6543796795789,58.8023065116436,12.));
#165161=CARTESIAN_POINT('Ctrl Pts',(43.6319746105482,58.788880804397,0.));
#165162=CARTESIAN_POINT('Ctrl Pts',(43.6319746105482,58.788880804397,12.));
#165163=CARTESIAN_POINT('Ctrl Pts',(43.6096145796796,58.775453710867,0.));
#165164=CARTESIAN_POINT('Ctrl Pts',(43.6096145796796,58.775453710867,12.));
#165165=CARTESIAN_POINT('Ctrl Pts',(43.5872996442345,58.7620253252062,0.));
#165166=CARTESIAN_POINT('Ctrl Pts',(43.5872996442345,58.7620253252062,12.));
#165167=CARTESIAN_POINT('Ctrl Pts',(43.5650298615916,58.74859574193,0.));
#165168=CARTESIAN_POINT('Ctrl Pts',(43.5650298615916,58.74859574193,12.));
#165169=CARTESIAN_POINT('Ctrl Pts',(43.5428052892488,58.7351650559181,0.));
#165170=CARTESIAN_POINT('Ctrl Pts',(43.5428052892488,58.7351650559181,12.));
#165171=CARTESIAN_POINT('Ctrl Pts',(43.5206259848337,58.7217333624209,0.));
#165172=CARTESIAN_POINT('Ctrl Pts',(43.5206259848337,58.7217333624209,12.));
#165173=CARTESIAN_POINT('Ctrl Pts',(43.4984920061073,58.7083007570661,0.));
#165174=CARTESIAN_POINT('Ctrl Pts',(43.4984920061073,58.7083007570661,12.));
#165175=CARTESIAN_POINT('Ctrl Pts',(43.4764034109654,58.6948673358638,0.));
#165176=CARTESIAN_POINT('Ctrl Pts',(43.4764034109654,58.6948673358638,12.));
#165177=CARTESIAN_POINT('Ctrl Pts',(43.4543602574351,58.6814331952138,0.));
#165178=CARTESIAN_POINT('Ctrl Pts',(43.4543602574351,58.6814331952138,12.));
#165179=CARTESIAN_POINT('Ctrl Pts',(43.4323626036736,58.6679984319097,0.));
#165180=CARTESIAN_POINT('Ctrl Pts',(43.4323626036736,58.6679984319097,12.));
#165181=CARTESIAN_POINT('Ctrl Pts',(43.4104105079768,58.6545631431393,0.));
#165182=CARTESIAN_POINT('Ctrl Pts',(43.4104105079768,58.6545631431393,12.));
#165183=CARTESIAN_POINT('Ctrl Pts',(43.388504028781,58.6411274264857,0.));
#165184=CARTESIAN_POINT('Ctrl Pts',(43.388504028781,58.6411274264857,12.));
#165185=CARTESIAN_POINT('Ctrl Pts',(43.3666432246635,58.627691379929,0.));
#165186=CARTESIAN_POINT('Ctrl Pts',(43.3666432246635,58.627691379929,12.));
#165187=CARTESIAN_POINT('Ctrl Pts',(43.3448281543371,58.6142551018467,0.));
#165188=CARTESIAN_POINT('Ctrl Pts',(43.3448281543371,58.6142551018467,12.));
#165189=CARTESIAN_POINT('Ctrl Pts',(43.3230588766449,58.6008186910156,0.));
#165190=CARTESIAN_POINT('Ctrl Pts',(43.3230588766449,58.6008186910156,12.));
#165191=CARTESIAN_POINT('Ctrl Pts',(43.3013354505701,58.5873822466152,0.));
#165192=CARTESIAN_POINT('Ctrl Pts',(43.3013354505701,58.5873822466152,12.));
#165193=CARTESIAN_POINT('Ctrl Pts',(43.27965793524,58.573945868231,0.));
#165194=CARTESIAN_POINT('Ctrl Pts',(43.27965793524,58.573945868231,12.));
#165195=CARTESIAN_POINT('Ctrl Pts',(43.2580263899278,58.5605096558578,0.));
#165196=CARTESIAN_POINT('Ctrl Pts',(43.2580263899278,58.5605096558578,12.));
#165197=CARTESIAN_POINT('Ctrl Pts',(43.2364408740493,58.5470737099032,0.));
#165198=CARTESIAN_POINT('Ctrl Pts',(43.2364408740493,58.5470737099032,12.));
#165199=CARTESIAN_POINT('Ctrl Pts',(43.2149014471574,58.5336381311917,0.));
#165200=CARTESIAN_POINT('Ctrl Pts',(43.2149014471574,58.5336381311917,12.));
#165201=CARTESIAN_POINT('Ctrl Pts',(43.1934081689505,58.5202030209669,0.));
#165202=CARTESIAN_POINT('Ctrl Pts',(43.1934081689505,58.5202030209669,12.));
#165203=CARTESIAN_POINT('Ctrl Pts',(43.1719610992771,58.5067684808944,0.));
#165204=CARTESIAN_POINT('Ctrl Pts',(43.1719610992771,58.5067684808944,12.));
#165205=CARTESIAN_POINT('Ctrl Pts',(43.1505602981365,58.4933346130636,0.));
#165206=CARTESIAN_POINT('Ctrl Pts',(43.1505602981365,58.4933346130636,12.));
#165207=CARTESIAN_POINT('Ctrl Pts',(43.1292058256776,58.4799015199907,0.));
#165208=CARTESIAN_POINT('Ctrl Pts',(43.1292058256776,58.4799015199907,12.));
#165209=CARTESIAN_POINT('Ctrl Pts',(43.1078977421916,58.4664693046217,0.));
#165210=CARTESIAN_POINT('Ctrl Pts',(43.1078977421916,58.4664693046217,12.));
#165211=CARTESIAN_POINT('Ctrl Pts',(43.0866361081177,58.4530380703349,0.));
#165212=CARTESIAN_POINT('Ctrl Pts',(43.0866361081177,58.4530380703349,12.));
#165213=CARTESIAN_POINT('Ctrl Pts',(43.0654209840511,58.4396079209451,0.));
#165214=CARTESIAN_POINT('Ctrl Pts',(43.0654209840511,58.4396079209451,12.));
#165215=CARTESIAN_POINT('Ctrl Pts',(43.0442524307434,58.4261789607058,0.));
#165216=CARTESIAN_POINT('Ctrl Pts',(43.0442524307434,58.4261789607058,12.));
#165217=CARTESIAN_POINT('Ctrl Pts',(43.0231305091027,58.4127512943136,0.));
#165218=CARTESIAN_POINT('Ctrl Pts',(43.0231305091027,58.4127512943136,12.));
#165219=CARTESIAN_POINT('Ctrl Pts',(43.0020552801859,58.3993250269101,0.));
#165220=CARTESIAN_POINT('Ctrl Pts',(43.0020552801859,58.3993250269101,12.));
#165221=CARTESIAN_POINT('Ctrl Pts',(42.9810268052032,58.3859002640857,0.));
#165222=CARTESIAN_POINT('Ctrl Pts',(42.9810268052032,58.3859002640857,12.));
#165223=CARTESIAN_POINT('Ctrl Pts',(42.960045145526,58.3724771118826,0.));
#165224=CARTESIAN_POINT('Ctrl Pts',(42.960045145526,58.3724771118826,12.));
#165225=CARTESIAN_POINT('Ctrl Pts',(42.9391103626879,58.3590556767978,0.));
#165226=CARTESIAN_POINT('Ctrl Pts',(42.9391103626879,58.3590556767978,12.));
#165227=CARTESIAN_POINT('Ctrl Pts',(42.9182225183854,58.3456360657865,0.));
#165228=CARTESIAN_POINT('Ctrl Pts',(42.9182225183854,58.3456360657865,12.));
#165229=CARTESIAN_POINT('Ctrl Pts',(42.8973816744709,58.3322183862654,0.));
#165230=CARTESIAN_POINT('Ctrl Pts',(42.8973816744709,58.3322183862654,12.));
#165231=CARTESIAN_POINT('Ctrl Pts',(42.8765878929551,58.3188027461164,0.));
#165232=CARTESIAN_POINT('Ctrl Pts',(42.8765878929551,58.3188027461164,12.));
#165233=CARTESIAN_POINT('Ctrl Pts',(42.8558412360158,58.3053892536894,0.));
#165234=CARTESIAN_POINT('Ctrl Pts',(42.8558412360158,58.3053892536894,12.));
#165235=CARTESIAN_POINT('Ctrl Pts',(42.8351417659999,58.2919780178064,0.));
#165236=CARTESIAN_POINT('Ctrl Pts',(42.8351417659999,58.2919780178064,12.));
#165237=CARTESIAN_POINT('Ctrl Pts',(42.8144895454233,58.2785691477638,0.));
#165238=CARTESIAN_POINT('Ctrl Pts',(42.8144895454233,58.2785691477638,12.));
#165239=CARTESIAN_POINT('Ctrl Pts',(42.7938846369651,58.2651627533368,0.));
#165240=CARTESIAN_POINT('Ctrl Pts',(42.7938846369651,58.2651627533368,12.));
#165241=CARTESIAN_POINT('Ctrl Pts',(42.7733271034679,58.2517589447821,0.));
#165242=CARTESIAN_POINT('Ctrl Pts',(42.7733271034679,58.2517589447821,12.));
#165243=CARTESIAN_POINT('Ctrl Pts',(42.7528170079484,58.2383578328424,0.));
#165244=CARTESIAN_POINT('Ctrl Pts',(42.7528170079484,58.2383578328424,12.));
#165245=CARTESIAN_POINT('Ctrl Pts',(42.7323544135985,58.22495952875,0.));
#165246=CARTESIAN_POINT('Ctrl Pts',(42.7323544135985,58.22495952875,12.));
#165247=CARTESIAN_POINT('Ctrl Pts',(42.7119393837866,58.21156414423,0.));
#165248=CARTESIAN_POINT('Ctrl Pts',(42.7119393837866,58.21156414423,12.));
#165249=CARTESIAN_POINT('Ctrl Pts',(42.6915719820513,58.1981717915037,0.));
#165250=CARTESIAN_POINT('Ctrl Pts',(42.6915719820513,58.1981717915037,12.));
#165251=CARTESIAN_POINT('Ctrl Pts',(42.6712522721016,58.1847825832923,0.));
#165252=CARTESIAN_POINT('Ctrl Pts',(42.6712522721016,58.1847825832923,12.));
#165253=CARTESIAN_POINT('Ctrl Pts',(42.6509803178265,58.171396632821,0.));
#165254=CARTESIAN_POINT('Ctrl Pts',(42.6509803178265,58.171396632821,12.));
#165255=CARTESIAN_POINT('Ctrl Pts',(42.6307561832976,58.1580140538228,0.));
#165256=CARTESIAN_POINT('Ctrl Pts',(42.6307561832976,58.1580140538228,12.));
#165257=CARTESIAN_POINT('Ctrl Pts',(42.6105799327699,58.1446349605421,0.));
#165258=CARTESIAN_POINT('Ctrl Pts',(42.6105799327699,58.1446349605421,12.));
#165259=CARTESIAN_POINT('Ctrl Pts',(42.5904516306762,58.1312594677386,0.));
#165260=CARTESIAN_POINT('Ctrl Pts',(42.5904516306762,58.1312594677386,12.));
#165261=CARTESIAN_POINT('Ctrl Pts',(42.5703713416265,58.1178876906907,0.));
#165262=CARTESIAN_POINT('Ctrl Pts',(42.5703713416265,58.1178876906907,12.));
#165263=CARTESIAN_POINT('Ctrl Pts',(42.5503391304183,58.1045197452003,0.));
#165264=CARTESIAN_POINT('Ctrl Pts',(42.5503391304183,58.1045197452003,12.));
#165265=CARTESIAN_POINT('Ctrl Pts',(42.5303550620387,58.0911557475965,0.));
#165266=CARTESIAN_POINT('Ctrl Pts',(42.5303550620387,58.0911557475965,12.));
#165267=CARTESIAN_POINT('Ctrl Pts',(42.5104192016664,58.0777958147403,0.));
#165268=CARTESIAN_POINT('Ctrl Pts',(42.5104192016664,58.0777958147403,12.));
#165269=CARTESIAN_POINT('Ctrl Pts',(42.4905316146653,58.0644400640275,0.));
#165270=CARTESIAN_POINT('Ctrl Pts',(42.4905316146653,58.0644400640275,12.));
#165271=CARTESIAN_POINT('Ctrl Pts',(42.4706923665845,58.0510886133926,0.));
#165272=CARTESIAN_POINT('Ctrl Pts',(42.4706923665845,58.0510886133926,12.));
#165273=CARTESIAN_POINT('Ctrl Pts',(42.4509015231674,58.037741581314,0.));
#165274=CARTESIAN_POINT('Ctrl Pts',(42.4509015231674,58.037741581314,12.));
#165275=CARTESIAN_POINT('Ctrl Pts',(42.4311591503555,58.0243990868181,0.));
#165276=CARTESIAN_POINT('Ctrl Pts',(42.4311591503555,58.0243990868181,12.));
#165277=CARTESIAN_POINT('Ctrl Pts',(42.411465314289,58.0110612494828,0.));
#165278=CARTESIAN_POINT('Ctrl Pts',(42.411465314289,58.0110612494828,12.));
#165279=CARTESIAN_POINT('Ctrl Pts',(42.3918200813014,57.9977281894422,0.));
#165280=CARTESIAN_POINT('Ctrl Pts',(42.3918200813014,57.9977281894422,12.));
#165281=CARTESIAN_POINT('Ctrl Pts',(42.3722235179197,57.9844000273911,0.));
#165282=CARTESIAN_POINT('Ctrl Pts',(42.3722235179197,57.9844000273911,12.));
#165283=CARTESIAN_POINT('Ctrl Pts',(42.3526756908746,57.9710768845899,0.));
#165284=CARTESIAN_POINT('Ctrl Pts',(42.3526756908746,57.9710768845899,12.));
#165285=CARTESIAN_POINT('Ctrl Pts',(42.333176667102,57.9577588828683,0.));
#165286=CARTESIAN_POINT('Ctrl Pts',(42.333176667102,57.9577588828683,12.));
#165287=CARTESIAN_POINT('Ctrl Pts',(42.3137265137452,57.9444461446299,0.));
#165288=CARTESIAN_POINT('Ctrl Pts',(42.3137265137452,57.9444461446299,12.));
#165289=CARTESIAN_POINT('Ctrl Pts',(42.2943252981489,57.9311387928563,0.));
#165290=CARTESIAN_POINT('Ctrl Pts',(42.2943252981489,57.9311387928563,12.));
#165291=CARTESIAN_POINT('Ctrl Pts',(42.2749730878594,57.9178369511114,0.));
#165292=CARTESIAN_POINT('Ctrl Pts',(42.2749730878594,57.9178369511114,12.));
#165293=CARTESIAN_POINT('Ctrl Pts',(42.2556699506353,57.9045407435474,0.));
#165294=CARTESIAN_POINT('Ctrl Pts',(42.2556699506353,57.9045407435474,12.));
#165295=CARTESIAN_POINT('Ctrl Pts',(42.2364159544501,57.8912502949096,0.));
#165296=CARTESIAN_POINT('Ctrl Pts',(42.2364159544501,57.8912502949096,12.));
#165297=CARTESIAN_POINT('Ctrl Pts',(42.2172111674938,57.8779657305413,0.));
#165298=CARTESIAN_POINT('Ctrl Pts',(42.2172111674938,57.8779657305413,12.));
#165299=CARTESIAN_POINT('Ctrl Pts',(42.1980556581665,57.864687176387,0.));
#165300=CARTESIAN_POINT('Ctrl Pts',(42.1980556581665,57.864687176387,12.));
#165301=CARTESIAN_POINT('Ctrl Pts',(42.1789494950794,57.8514147589972,0.));
#165302=CARTESIAN_POINT('Ctrl Pts',(42.1789494950794,57.8514147589972,12.));
#165303=CARTESIAN_POINT('Ctrl Pts',(42.1598927470646,57.8381486055342,0.));
#165304=CARTESIAN_POINT('Ctrl Pts',(42.1598927470646,57.8381486055342,12.));
#165305=CARTESIAN_POINT('Ctrl Pts',(42.1408854831783,57.8248888437775,0.));
#165306=CARTESIAN_POINT('Ctrl Pts',(42.1408854831783,57.8248888437775,12.));
#165307=CARTESIAN_POINT('Ctrl Pts',(42.121927772702,57.8116356021288,0.));
#165308=CARTESIAN_POINT('Ctrl Pts',(42.121927772702,57.8116356021288,12.));
#165309=CARTESIAN_POINT('Ctrl Pts',(42.1030196851366,57.798389009616,0.));
#165310=CARTESIAN_POINT('Ctrl Pts',(42.1030196851366,57.798389009616,12.));
#165311=CARTESIAN_POINT('Ctrl Pts',(42.0841612902042,57.7851491958987,0.));
#165312=CARTESIAN_POINT('Ctrl Pts',(42.0841612902042,57.7851491958987,12.));
#165313=CARTESIAN_POINT('Ctrl Pts',(42.0653526578588,57.7719162912744,0.));
#165314=CARTESIAN_POINT('Ctrl Pts',(42.0653526578588,57.7719162912744,12.));
#165315=CARTESIAN_POINT('Ctrl Pts',(42.0465938582882,57.7586904266834,0.));
#165316=CARTESIAN_POINT('Ctrl Pts',(42.0465938582882,57.7586904266834,12.));
#165317=CARTESIAN_POINT('Ctrl Pts',(42.0278849619148,57.745471733714,0.));
#165318=CARTESIAN_POINT('Ctrl Pts',(42.0278849619148,57.745471733714,12.));
#165319=CARTESIAN_POINT('Ctrl Pts',(42.0092260393897,57.7322603446066,0.));
#165320=CARTESIAN_POINT('Ctrl Pts',(42.0092260393897,57.7322603446066,12.));
#165321=CARTESIAN_POINT('Ctrl Pts',(41.990617161596,57.7190563922593,0.));
#165322=CARTESIAN_POINT('Ctrl Pts',(41.990617161596,57.7190563922593,12.));
#165323=CARTESIAN_POINT('Ctrl Pts',(41.9720583996592,57.7058600102351,0.));
#165324=CARTESIAN_POINT('Ctrl Pts',(41.9720583996592,57.7058600102351,12.));
#165325=CARTESIAN_POINT('Ctrl Pts',(41.9535498249488,57.6926713327672,0.));
#165326=CARTESIAN_POINT('Ctrl Pts',(41.9535498249488,57.6926713327672,12.));
#165327=CARTESIAN_POINT('Ctrl Pts',(41.9350915090796,57.6794904947649,0.));
#165328=CARTESIAN_POINT('Ctrl Pts',(41.9350915090796,57.6794904947649,12.));
#165329=CARTESIAN_POINT('Ctrl Pts',(41.9166835239054,57.6663176318189,0.));
#165330=CARTESIAN_POINT('Ctrl Pts',(41.9166835239054,57.6663176318189,12.));
#165331=CARTESIAN_POINT('Ctrl Pts',(41.8983259415253,57.6531528802072,0.));
#165332=CARTESIAN_POINT('Ctrl Pts',(41.8983259415253,57.6531528802072,12.));
#165333=CARTESIAN_POINT('Ctrl Pts',(41.8800188342912,57.6399963769009,0.));
#165334=CARTESIAN_POINT('Ctrl Pts',(41.8800188342912,57.6399963769009,12.));
#165335=CARTESIAN_POINT('Ctrl Pts',(41.8617622748107,57.6268482595701,0.));
#165336=CARTESIAN_POINT('Ctrl Pts',(41.8617622748107,57.6268482595701,12.));
#165337=CARTESIAN_POINT('Ctrl Pts',(41.8435563359456,57.613708666588,0.));
#165338=CARTESIAN_POINT('Ctrl Pts',(41.8435563359456,57.613708666588,12.));
#165339=CARTESIAN_POINT('Ctrl Pts',(41.8254010908051,57.6005777370347,0.));
#165340=CARTESIAN_POINT('Ctrl Pts',(41.8254010908051,57.6005777370347,12.));
#165341=CARTESIAN_POINT('Ctrl Pts',(41.8072966127559,57.5874556107054,0.));
#165342=CARTESIAN_POINT('Ctrl Pts',(41.8072966127559,57.5874556107054,12.));
#165343=CARTESIAN_POINT('Ctrl Pts',(41.7892429754298,57.5743424281204,0.));
#165344=CARTESIAN_POINT('Ctrl Pts',(41.7892429754298,57.5743424281204,12.));
#165345=CARTESIAN_POINT('Ctrl Pts',(41.7712402527273,57.561238330532,0.));
#165346=CARTESIAN_POINT('Ctrl Pts',(41.7712402527273,57.561238330532,12.));
#165347=CARTESIAN_POINT('Ctrl Pts',(41.7532885188174,57.5481434599334,0.));
#165348=CARTESIAN_POINT('Ctrl Pts',(41.7532885188174,57.5481434599334,12.));
#165349=CARTESIAN_POINT('Ctrl Pts',(41.7353878481335,57.5350579590648,0.));
#165350=CARTESIAN_POINT('Ctrl Pts',(41.7353878481335,57.5350579590648,12.));
#165351=CARTESIAN_POINT('Ctrl Pts',(41.7175383153819,57.5219819714169,0.));
#165352=CARTESIAN_POINT('Ctrl Pts',(41.7175383153819,57.5219819714169,12.));
#165353=CARTESIAN_POINT('Ctrl Pts',(41.6997399955445,57.5089156412341,0.));
#165354=CARTESIAN_POINT('Ctrl Pts',(41.6997399955445,57.5089156412341,12.));
#165355=CARTESIAN_POINT('Ctrl Pts',(41.6819929638797,57.4958591135165,0.));
#165356=CARTESIAN_POINT('Ctrl Pts',(41.6819929638797,57.4958591135165,12.));
#165357=CARTESIAN_POINT('Ctrl Pts',(41.6642972959168,57.4828125340222,0.));
#165358=CARTESIAN_POINT('Ctrl Pts',(41.6642972959168,57.4828125340222,12.));
#165359=CARTESIAN_POINT('Ctrl Pts',(41.6466530674522,57.4697760492693,0.));
#165360=CARTESIAN_POINT('Ctrl Pts',(41.6466530674522,57.4697760492693,12.));
#165361=CARTESIAN_POINT('Ctrl Pts',(41.6290603545674,57.4567498065573,0.));
#165362=CARTESIAN_POINT('Ctrl Pts',(41.6290603545674,57.4567498065573,12.));
#165363=CARTESIAN_POINT('Ctrl Pts',(41.6115192336393,57.4437339539848,0.));
#165364=CARTESIAN_POINT('Ctrl Pts',(41.6115192336393,57.4437339539848,12.));
#165365=CARTESIAN_POINT('Ctrl Pts',(41.5940297813473,57.4307286404657,0.));
#165366=CARTESIAN_POINT('Ctrl Pts',(41.5940297813473,57.4307286404657,12.));
#165367=CARTESIAN_POINT('Ctrl Pts',(41.5765920746764,57.417734015749,0.));
#165368=CARTESIAN_POINT('Ctrl Pts',(41.5765920746764,57.417734015749,12.));
#165369=CARTESIAN_POINT('Ctrl Pts',(41.5592061909159,57.4047502304207,0.));
#165370=CARTESIAN_POINT('Ctrl Pts',(41.5592061909159,57.4047502304207,12.));
#165371=CARTESIAN_POINT('Ctrl Pts',(41.5418722076558,57.3917774358844,0.));
#165372=CARTESIAN_POINT('Ctrl Pts',(41.5418722076558,57.3917774358844,12.));
#165373=CARTESIAN_POINT('Ctrl Pts',(41.5245902027767,57.378815784345,0.));
#165374=CARTESIAN_POINT('Ctrl Pts',(41.5245902027767,57.378815784345,12.));
#165375=CARTESIAN_POINT('Ctrl Pts',(41.5073602544404,57.3658654287948,0.));
#165376=CARTESIAN_POINT('Ctrl Pts',(41.5073602544404,57.3658654287948,12.));
#165377=CARTESIAN_POINT('Ctrl Pts',(41.4901824410654,57.3529265229858,0.));
#165378=CARTESIAN_POINT('Ctrl Pts',(41.4901824410654,57.3529265229858,12.));
#165379=CARTESIAN_POINT('Ctrl Pts',(41.4730568413535,57.339999221474,0.));
#165380=CARTESIAN_POINT('Ctrl Pts',(41.4730568413535,57.339999221474,12.));
#165381=CARTESIAN_POINT('Ctrl Pts',(41.4559835343338,57.3270836796925,0.));
#165382=CARTESIAN_POINT('Ctrl Pts',(41.4559835343338,57.3270836796925,12.));
#165383=CARTESIAN_POINT('Ctrl Pts',(41.4389625993948,57.3141800540137,0.));
#165384=CARTESIAN_POINT('Ctrl Pts',(41.4389625993948,57.3141800540137,12.));
#165385=CARTESIAN_POINT('Ctrl Pts',(41.4219941163154,57.3012885018139,0.));
#165386=CARTESIAN_POINT('Ctrl Pts',(41.4219941163154,57.3012885018139,12.));
#165387=CARTESIAN_POINT('Ctrl Pts',(41.4050781652923,57.2884091815385,0.));
#165388=CARTESIAN_POINT('Ctrl Pts',(41.4050781652923,57.2884091815385,12.));
#165389=CARTESIAN_POINT('Ctrl Pts',(41.3882148268798,57.2755422525822,0.));
#165390=CARTESIAN_POINT('Ctrl Pts',(41.3882148268798,57.2755422525822,12.));
#165391=CARTESIAN_POINT('Ctrl Pts',(41.3714041819215,57.2626878751584,0.));
#165392=CARTESIAN_POINT('Ctrl Pts',(41.3714041819215,57.2626878751584,12.));
#165393=CARTESIAN_POINT('Ctrl Pts',(41.3546463114889,57.2498462101883,0.));
#165394=CARTESIAN_POINT('Ctrl Pts',(41.3546463114889,57.2498462101883,12.));
#165395=CARTESIAN_POINT('Ctrl Pts',(41.3379412967889,57.237017419142,0.));
#165396=CARTESIAN_POINT('Ctrl Pts',(41.3379412967889,57.237017419142,12.));
#165397=CARTESIAN_POINT('Ctrl Pts',(41.321289219151,57.2242016640226,0.));
#165398=CARTESIAN_POINT('Ctrl Pts',(41.321289219151,57.2242016640226,12.));
#165399=CARTESIAN_POINT('Ctrl Pts',(41.304690160231,57.2113991077325,0.));
#165400=CARTESIAN_POINT('Ctrl Pts',(41.304690160231,57.2113991077325,12.));
#165401=CARTESIAN_POINT('Ctrl Pts',(41.2881442021869,57.1986099143992,0.));
#165402=CARTESIAN_POINT('Ctrl Pts',(41.2881442021869,57.1986099143992,12.));
#165403=CARTESIAN_POINT('Ctrl Pts',(41.2716514278268,57.1858342496526,0.));
#165404=CARTESIAN_POINT('Ctrl Pts',(41.2716514278268,57.1858342496526,12.));
#165405=CARTESIAN_POINT('Ctrl Pts',(41.2552119208445,57.1730722810771,0.));
#165406=CARTESIAN_POINT('Ctrl Pts',(41.2552119208445,57.1730722810771,12.));
#165407=CARTESIAN_POINT('Ctrl Pts',(41.2388257656534,57.1603241779043,0.));
#165408=CARTESIAN_POINT('Ctrl Pts',(41.2388257656534,57.1603241779043,12.));
#165409=CARTESIAN_POINT('Ctrl Pts',(41.2224930469412,57.1475901101795,0.));
#165410=CARTESIAN_POINT('Ctrl Pts',(41.2224930469412,57.1475901101795,12.));
#165411=CARTESIAN_POINT('Ctrl Pts',(41.2062138492913,57.1348702480644,0.));
#165412=CARTESIAN_POINT('Ctrl Pts',(41.2062138492913,57.1348702480644,12.));
#165413=CARTESIAN_POINT('Ctrl Pts',(41.1899882567941,57.1221647611232,0.));
#165414=CARTESIAN_POINT('Ctrl Pts',(41.1899882567941,57.1221647611232,12.));
#165415=CARTESIAN_POINT('Ctrl Pts',(41.1738163525931,57.1094738174998,0.));
#165416=CARTESIAN_POINT('Ctrl Pts',(41.1738163525931,57.1094738174998,12.));
#165417=CARTESIAN_POINT('Ctrl Pts',(41.1576982197402,57.0967975854912,0.));
#165418=CARTESIAN_POINT('Ctrl Pts',(41.1576982197402,57.0967975854912,12.));
#165419=CARTESIAN_POINT('Ctrl Pts',(41.1416339422132,57.0841362354281,0.));
#165420=CARTESIAN_POINT('Ctrl Pts',(41.1416339422132,57.0841362354281,12.));
#165421=CARTESIAN_POINT('Ctrl Pts',(41.1256236057436,57.0714899412091,0.));
#165422=CARTESIAN_POINT('Ctrl Pts',(41.1256236057436,57.0714899412091,12.));
#165423=CARTESIAN_POINT('Ctrl Pts',(41.1096672990125,57.0588588825266,0.));
#165424=CARTESIAN_POINT('Ctrl Pts',(41.1096672990125,57.0588588825266,12.));
#165425=CARTESIAN_POINT('Ctrl Pts',(41.0937651137519,57.0462432450637,0.));
#165426=CARTESIAN_POINT('Ctrl Pts',(41.0937651137519,57.0462432450637,12.));
#165427=CARTESIAN_POINT('Ctrl Pts',(41.0779171422415,57.0336432158504,0.));
#165428=CARTESIAN_POINT('Ctrl Pts',(41.0779171422415,57.0336432158504,12.));
#165429=CARTESIAN_POINT('Ctrl Pts',(41.0621234751,57.0210589791777,0.));
#165430=CARTESIAN_POINT('Ctrl Pts',(41.0621234751,57.0210589791777,12.));
#165431=CARTESIAN_POINT('Ctrl Pts',(41.0463841993622,57.008490713044,0.));
#165432=CARTESIAN_POINT('Ctrl Pts',(41.0463841993622,57.008490713044,12.));
#165433=CARTESIAN_POINT('Ctrl Pts',(41.0306993954021,56.9959385834768,0.));
#165434=CARTESIAN_POINT('Ctrl Pts',(41.0306993954021,56.9959385834768,12.));
#165435=CARTESIAN_POINT('Ctrl Pts',(41.0150691398988,56.9834027500178,0.));
#165436=CARTESIAN_POINT('Ctrl Pts',(41.0150691398988,56.9834027500178,12.));
#165437=CARTESIAN_POINT('Ctrl Pts',(40.9994935117307,56.9708833766184,0.));
#165438=CARTESIAN_POINT('Ctrl Pts',(40.9994935117307,56.9708833766184,12.));
#165439=CARTESIAN_POINT('Ctrl Pts',(40.9839725967121,56.9583806404069,0.));
#165440=CARTESIAN_POINT('Ctrl Pts',(40.9839725967121,56.9583806404069,12.));
#165441=CARTESIAN_POINT('Ctrl Pts',(40.968506493303,56.9458947422541,0.));
#165442=CARTESIAN_POINT('Ctrl Pts',(40.968506493303,56.9458947422541,12.));
#165443=CARTESIAN_POINT('Ctrl Pts',(40.9530953164952,56.9334259139928,0.));
#165444=CARTESIAN_POINT('Ctrl Pts',(40.9530953164952,56.9334259139928,12.));
#165445=CARTESIAN_POINT('Ctrl Pts',(40.9377391857043,56.9209743960861,0.));
#165446=CARTESIAN_POINT('Ctrl Pts',(40.9377391857043,56.9209743960861,12.));
#165447=CARTESIAN_POINT('Ctrl Pts',(40.9224382132382,56.9085404164432,0.));
#165448=CARTESIAN_POINT('Ctrl Pts',(40.9224382132382,56.9085404164432,12.));
#165449=CARTESIAN_POINT('Ctrl Pts',(40.907192493755,56.8961241708926,0.));
#165450=CARTESIAN_POINT('Ctrl Pts',(40.907192493755,56.8961241708926,12.));
#165451=CARTESIAN_POINT('Ctrl Pts',(40.8920020903443,56.8837257978574,0.));
#165452=CARTESIAN_POINT('Ctrl Pts',(40.8920020903443,56.8837257978574,12.));
#165453=CARTESIAN_POINT('Ctrl Pts',(40.8768670342278,56.8713453765253,0.));
#165454=CARTESIAN_POINT('Ctrl Pts',(40.8768670342278,56.8713453765253,12.));
#165455=CARTESIAN_POINT('Ctrl Pts',(40.8648032759631,56.8614554317993,0.));
#165456=CARTESIAN_POINT('Ctrl Pts',(40.8648032759631,56.8614554317993,12.));
#165457=CARTESIAN_POINT('Ctrl Pts',(40.8557803680411,56.8540460739677,0.));
#165458=CARTESIAN_POINT('Ctrl Pts',(40.8557803680411,56.8540460739677,12.));
#165459=CARTESIAN_POINT('Ctrl Pts',(40.8497761671086,56.8491101022668,0.));
#165460=CARTESIAN_POINT('Ctrl Pts',(40.8497761671086,56.8491101022668,12.));
#165461=CARTESIAN_POINT('Ctrl Pts',(40.8467768343956,56.8466430164621,0.));
#165462=CARTESIAN_POINT('Ctrl Pts',(40.8467768343956,56.8466430164621,12.));
#165463=CARTESIAN_POINT('',(40.8467768343956,56.8466430164621,12.));
#165464=CARTESIAN_POINT('Ctrl Pts',(40.8467768343956,56.8466430164621,12.));
#165465=CARTESIAN_POINT('Ctrl Pts',(40.8497761671086,56.8491101022668,12.));
#165466=CARTESIAN_POINT('Ctrl Pts',(40.8557803680411,56.8540460739677,12.));
#165467=CARTESIAN_POINT('Ctrl Pts',(40.8648032759631,56.8614554317993,12.));
#165468=CARTESIAN_POINT('Ctrl Pts',(40.8768670342278,56.8713453765253,12.));
#165469=CARTESIAN_POINT('Ctrl Pts',(40.8920020903443,56.8837257978574,12.));
#165470=CARTESIAN_POINT('Ctrl Pts',(40.907192493755,56.8961241708926,12.));
#165471=CARTESIAN_POINT('Ctrl Pts',(40.9224382132382,56.9085404164432,12.));
#165472=CARTESIAN_POINT('Ctrl Pts',(40.9377391857043,56.9209743960861,12.));
#165473=CARTESIAN_POINT('Ctrl Pts',(40.9530953164952,56.9334259139928,12.));
#165474=CARTESIAN_POINT('Ctrl Pts',(40.968506493303,56.9458947422541,12.));
#165475=CARTESIAN_POINT('Ctrl Pts',(40.9839725967121,56.9583806404069,12.));
#165476=CARTESIAN_POINT('Ctrl Pts',(40.9994935117307,56.9708833766184,12.));
#165477=CARTESIAN_POINT('Ctrl Pts',(41.0150691398988,56.9834027500178,12.));
#165478=CARTESIAN_POINT('Ctrl Pts',(41.0306993954021,56.9959385834768,12.));
#165479=CARTESIAN_POINT('Ctrl Pts',(41.0463841993622,57.008490713044,12.));
#165480=CARTESIAN_POINT('Ctrl Pts',(41.0621234751,57.0210589791777,12.));
#165481=CARTESIAN_POINT('Ctrl Pts',(41.0779171422415,57.0336432158504,12.));
#165482=CARTESIAN_POINT('Ctrl Pts',(41.0937651137519,57.0462432450637,12.));
#165483=CARTESIAN_POINT('Ctrl Pts',(41.1096672990125,57.0588588825266,12.));
#165484=CARTESIAN_POINT('Ctrl Pts',(41.1256236057436,57.0714899412091,12.));
#165485=CARTESIAN_POINT('Ctrl Pts',(41.1416339422132,57.0841362354281,12.));
#165486=CARTESIAN_POINT('Ctrl Pts',(41.1576982197402,57.0967975854912,12.));
#165487=CARTESIAN_POINT('Ctrl Pts',(41.1738163525931,57.1094738174998,12.));
#165488=CARTESIAN_POINT('Ctrl Pts',(41.1899882567941,57.1221647611232,12.));
#165489=CARTESIAN_POINT('Ctrl Pts',(41.2062138492913,57.1348702480644,12.));
#165490=CARTESIAN_POINT('Ctrl Pts',(41.2224930469412,57.1475901101795,12.));
#165491=CARTESIAN_POINT('Ctrl Pts',(41.2388257656534,57.1603241779043,12.));
#165492=CARTESIAN_POINT('Ctrl Pts',(41.2552119208445,57.1730722810771,12.));
#165493=CARTESIAN_POINT('Ctrl Pts',(41.2716514278268,57.1858342496526,12.));
#165494=CARTESIAN_POINT('Ctrl Pts',(41.2881442021869,57.1986099143992,12.));
#165495=CARTESIAN_POINT('Ctrl Pts',(41.304690160231,57.2113991077325,12.));
#165496=CARTESIAN_POINT('Ctrl Pts',(41.321289219151,57.2242016640226,12.));
#165497=CARTESIAN_POINT('Ctrl Pts',(41.3379412967889,57.237017419142,12.));
#165498=CARTESIAN_POINT('Ctrl Pts',(41.3546463114889,57.2498462101883,12.));
#165499=CARTESIAN_POINT('Ctrl Pts',(41.3714041819215,57.2626878751584,12.));
#165500=CARTESIAN_POINT('Ctrl Pts',(41.3882148268798,57.2755422525822,12.));
#165501=CARTESIAN_POINT('Ctrl Pts',(41.4050781652923,57.2884091815385,12.));
#165502=CARTESIAN_POINT('Ctrl Pts',(41.4219941163154,57.3012885018139,12.));
#165503=CARTESIAN_POINT('Ctrl Pts',(41.4389625993948,57.3141800540137,12.));
#165504=CARTESIAN_POINT('Ctrl Pts',(41.4559835343338,57.3270836796925,12.));
#165505=CARTESIAN_POINT('Ctrl Pts',(41.4730568413535,57.339999221474,12.));
#165506=CARTESIAN_POINT('Ctrl Pts',(41.4901824410654,57.3529265229858,12.));
#165507=CARTESIAN_POINT('Ctrl Pts',(41.5073602544404,57.3658654287948,12.));
#165508=CARTESIAN_POINT('Ctrl Pts',(41.5245902027767,57.378815784345,12.));
#165509=CARTESIAN_POINT('Ctrl Pts',(41.5418722076558,57.3917774358844,12.));
#165510=CARTESIAN_POINT('Ctrl Pts',(41.5592061909159,57.4047502304207,12.));
#165511=CARTESIAN_POINT('Ctrl Pts',(41.5765920746764,57.417734015749,12.));
#165512=CARTESIAN_POINT('Ctrl Pts',(41.5940297813473,57.4307286404657,12.));
#165513=CARTESIAN_POINT('Ctrl Pts',(41.6115192336393,57.4437339539848,12.));
#165514=CARTESIAN_POINT('Ctrl Pts',(41.6290603545674,57.4567498065573,12.));
#165515=CARTESIAN_POINT('Ctrl Pts',(41.6466530674522,57.4697760492693,12.));
#165516=CARTESIAN_POINT('Ctrl Pts',(41.6642972959168,57.4828125340222,12.));
#165517=CARTESIAN_POINT('Ctrl Pts',(41.6819929638797,57.4958591135165,12.));
#165518=CARTESIAN_POINT('Ctrl Pts',(41.6997399955445,57.5089156412341,12.));
#165519=CARTESIAN_POINT('Ctrl Pts',(41.7175383153819,57.5219819714169,12.));
#165520=CARTESIAN_POINT('Ctrl Pts',(41.7353878481335,57.5350579590648,12.));
#165521=CARTESIAN_POINT('Ctrl Pts',(41.7532885188174,57.5481434599334,12.));
#165522=CARTESIAN_POINT('Ctrl Pts',(41.7712402527273,57.561238330532,12.));
#165523=CARTESIAN_POINT('Ctrl Pts',(41.7892429754298,57.5743424281204,12.));
#165524=CARTESIAN_POINT('Ctrl Pts',(41.8072966127559,57.5874556107054,12.));
#165525=CARTESIAN_POINT('Ctrl Pts',(41.8254010908051,57.6005777370347,12.));
#165526=CARTESIAN_POINT('Ctrl Pts',(41.8435563359456,57.613708666588,12.));
#165527=CARTESIAN_POINT('Ctrl Pts',(41.8617622748107,57.6268482595701,12.));
#165528=CARTESIAN_POINT('Ctrl Pts',(41.8800188342912,57.6399963769009,12.));
#165529=CARTESIAN_POINT('Ctrl Pts',(41.8983259415253,57.6531528802072,12.));
#165530=CARTESIAN_POINT('Ctrl Pts',(41.9166835239054,57.6663176318189,12.));
#165531=CARTESIAN_POINT('Ctrl Pts',(41.9350915090796,57.6794904947649,12.));
#165532=CARTESIAN_POINT('Ctrl Pts',(41.9535498249488,57.6926713327672,12.));
#165533=CARTESIAN_POINT('Ctrl Pts',(41.9720583996592,57.7058600102351,12.));
#165534=CARTESIAN_POINT('Ctrl Pts',(41.990617161596,57.7190563922593,12.));
#165535=CARTESIAN_POINT('Ctrl Pts',(42.0092260393897,57.7322603446066,12.));
#165536=CARTESIAN_POINT('Ctrl Pts',(42.0278849619148,57.745471733714,12.));
#165537=CARTESIAN_POINT('Ctrl Pts',(42.0465938582882,57.7586904266834,12.));
#165538=CARTESIAN_POINT('Ctrl Pts',(42.0653526578588,57.7719162912744,12.));
#165539=CARTESIAN_POINT('Ctrl Pts',(42.0841612902042,57.7851491958987,12.));
#165540=CARTESIAN_POINT('Ctrl Pts',(42.1030196851366,57.798389009616,12.));
#165541=CARTESIAN_POINT('Ctrl Pts',(42.121927772702,57.8116356021288,12.));
#165542=CARTESIAN_POINT('Ctrl Pts',(42.1408854831783,57.8248888437775,12.));
#165543=CARTESIAN_POINT('Ctrl Pts',(42.1598927470646,57.8381486055342,12.));
#165544=CARTESIAN_POINT('Ctrl Pts',(42.1789494950794,57.8514147589972,12.));
#165545=CARTESIAN_POINT('Ctrl Pts',(42.1980556581665,57.864687176387,12.));
#165546=CARTESIAN_POINT('Ctrl Pts',(42.2172111674938,57.8779657305413,12.));
#165547=CARTESIAN_POINT('Ctrl Pts',(42.2364159544501,57.8912502949096,12.));
#165548=CARTESIAN_POINT('Ctrl Pts',(42.2556699506353,57.9045407435474,12.));
#165549=CARTESIAN_POINT('Ctrl Pts',(42.2749730878594,57.9178369511114,12.));
#165550=CARTESIAN_POINT('Ctrl Pts',(42.2943252981489,57.9311387928563,12.));
#165551=CARTESIAN_POINT('Ctrl Pts',(42.3137265137452,57.9444461446299,12.));
#165552=CARTESIAN_POINT('Ctrl Pts',(42.333176667102,57.9577588828683,12.));
#165553=CARTESIAN_POINT('Ctrl Pts',(42.3526756908746,57.9710768845899,12.));
#165554=CARTESIAN_POINT('Ctrl Pts',(42.3722235179197,57.9844000273911,12.));
#165555=CARTESIAN_POINT('Ctrl Pts',(42.3918200813014,57.9977281894422,12.));
#165556=CARTESIAN_POINT('Ctrl Pts',(42.411465314289,58.0110612494828,12.));
#165557=CARTESIAN_POINT('Ctrl Pts',(42.4311591503555,58.0243990868181,12.));
#165558=CARTESIAN_POINT('Ctrl Pts',(42.4509015231674,58.037741581314,12.));
#165559=CARTESIAN_POINT('Ctrl Pts',(42.4706923665845,58.0510886133926,12.));
#165560=CARTESIAN_POINT('Ctrl Pts',(42.4905316146653,58.0644400640275,12.));
#165561=CARTESIAN_POINT('Ctrl Pts',(42.5104192016664,58.0777958147403,12.));
#165562=CARTESIAN_POINT('Ctrl Pts',(42.5303550620387,58.0911557475965,12.));
#165563=CARTESIAN_POINT('Ctrl Pts',(42.5503391304183,58.1045197452003,12.));
#165564=CARTESIAN_POINT('Ctrl Pts',(42.5703713416265,58.1178876906907,12.));
#165565=CARTESIAN_POINT('Ctrl Pts',(42.5904516306762,58.1312594677386,12.));
#165566=CARTESIAN_POINT('Ctrl Pts',(42.6105799327699,58.1446349605421,12.));
#165567=CARTESIAN_POINT('Ctrl Pts',(42.6307561832976,58.1580140538228,12.));
#165568=CARTESIAN_POINT('Ctrl Pts',(42.6509803178265,58.171396632821,12.));
#165569=CARTESIAN_POINT('Ctrl Pts',(42.6712522721016,58.1847825832923,12.));
#165570=CARTESIAN_POINT('Ctrl Pts',(42.6915719820513,58.1981717915037,12.));
#165571=CARTESIAN_POINT('Ctrl Pts',(42.7119393837866,58.21156414423,12.));
#165572=CARTESIAN_POINT('Ctrl Pts',(42.7323544135985,58.22495952875,12.));
#165573=CARTESIAN_POINT('Ctrl Pts',(42.7528170079484,58.2383578328424,12.));
#165574=CARTESIAN_POINT('Ctrl Pts',(42.7733271034679,58.2517589447821,12.));
#165575=CARTESIAN_POINT('Ctrl Pts',(42.7938846369651,58.2651627533368,12.));
#165576=CARTESIAN_POINT('Ctrl Pts',(42.8144895454233,58.2785691477638,12.));
#165577=CARTESIAN_POINT('Ctrl Pts',(42.8351417659999,58.2919780178064,12.));
#165578=CARTESIAN_POINT('Ctrl Pts',(42.8558412360158,58.3053892536894,12.));
#165579=CARTESIAN_POINT('Ctrl Pts',(42.8765878929551,58.3188027461164,12.));
#165580=CARTESIAN_POINT('Ctrl Pts',(42.8973816744709,58.3322183862654,12.));
#165581=CARTESIAN_POINT('Ctrl Pts',(42.9182225183854,58.3456360657865,12.));
#165582=CARTESIAN_POINT('Ctrl Pts',(42.9391103626879,58.3590556767978,12.));
#165583=CARTESIAN_POINT('Ctrl Pts',(42.960045145526,58.3724771118826,12.));
#165584=CARTESIAN_POINT('Ctrl Pts',(42.9810268052032,58.3859002640857,12.));
#165585=CARTESIAN_POINT('Ctrl Pts',(43.0020552801859,58.3993250269101,12.));
#165586=CARTESIAN_POINT('Ctrl Pts',(43.0231305091027,58.4127512943136,12.));
#165587=CARTESIAN_POINT('Ctrl Pts',(43.0442524307434,58.4261789607058,12.));
#165588=CARTESIAN_POINT('Ctrl Pts',(43.0654209840511,58.4396079209451,12.));
#165589=CARTESIAN_POINT('Ctrl Pts',(43.0866361081177,58.4530380703349,12.));
#165590=CARTESIAN_POINT('Ctrl Pts',(43.1078977421916,58.4664693046217,12.));
#165591=CARTESIAN_POINT('Ctrl Pts',(43.1292058256776,58.4799015199907,12.));
#165592=CARTESIAN_POINT('Ctrl Pts',(43.1505602981365,58.4933346130636,12.));
#165593=CARTESIAN_POINT('Ctrl Pts',(43.1719610992771,58.5067684808944,12.));
#165594=CARTESIAN_POINT('Ctrl Pts',(43.1934081689505,58.5202030209669,12.));
#165595=CARTESIAN_POINT('Ctrl Pts',(43.2149014471574,58.5336381311917,12.));
#165596=CARTESIAN_POINT('Ctrl Pts',(43.2364408740493,58.5470737099032,12.));
#165597=CARTESIAN_POINT('Ctrl Pts',(43.2580263899278,58.5605096558578,12.));
#165598=CARTESIAN_POINT('Ctrl Pts',(43.27965793524,58.573945868231,12.));
#165599=CARTESIAN_POINT('Ctrl Pts',(43.3013354505701,58.5873822466152,12.));
#165600=CARTESIAN_POINT('Ctrl Pts',(43.3230588766449,58.6008186910156,12.));
#165601=CARTESIAN_POINT('Ctrl Pts',(43.3448281543371,58.6142551018467,12.));
#165602=CARTESIAN_POINT('Ctrl Pts',(43.3666432246635,58.627691379929,12.));
#165603=CARTESIAN_POINT('Ctrl Pts',(43.388504028781,58.6411274264857,12.));
#165604=CARTESIAN_POINT('Ctrl Pts',(43.4104105079768,58.6545631431393,12.));
#165605=CARTESIAN_POINT('Ctrl Pts',(43.4323626036736,58.6679984319097,12.));
#165606=CARTESIAN_POINT('Ctrl Pts',(43.4543602574351,58.6814331952138,12.));
#165607=CARTESIAN_POINT('Ctrl Pts',(43.4764034109654,58.6948673358638,12.));
#165608=CARTESIAN_POINT('Ctrl Pts',(43.4984920061073,58.7083007570661,12.));
#165609=CARTESIAN_POINT('Ctrl Pts',(43.5206259848337,58.7217333624209,12.));
#165610=CARTESIAN_POINT('Ctrl Pts',(43.5428052892488,58.7351650559181,12.));
#165611=CARTESIAN_POINT('Ctrl Pts',(43.5650298615916,58.74859574193,12.));
#165612=CARTESIAN_POINT('Ctrl Pts',(43.5872996442345,58.7620253252062,12.));
#165613=CARTESIAN_POINT('Ctrl Pts',(43.6096145796796,58.775453710867,12.));
#165614=CARTESIAN_POINT('Ctrl Pts',(43.6319746105482,58.788880804397,12.));
#165615=CARTESIAN_POINT('Ctrl Pts',(43.6543796795789,58.8023065116436,12.));
#165616=CARTESIAN_POINT('Ctrl Pts',(43.6768297296395,58.8157307388238,12.));
#165617=CARTESIAN_POINT('Ctrl Pts',(43.6993247037314,58.8291533925293,12.));
#165618=CARTESIAN_POINT('Ctrl Pts',(43.7218645449922,58.8425743797326,12.));
#165619=CARTESIAN_POINT('Ctrl Pts',(43.7444491966942,58.8559936077941,12.));
#165620=CARTESIAN_POINT('Ctrl Pts',(43.7670786022402,58.8694109844648,12.));
#165621=CARTESIAN_POINT('Ctrl Pts',(43.7897527051609,58.8828264178621,12.));
#165622=CARTESIAN_POINT('Ctrl Pts',(43.8124714491076,58.8962398164493,12.));
#165623=CARTESIAN_POINT('Ctrl Pts',(43.835234777842,58.9096510890129,12.));
#165624=CARTESIAN_POINT('Ctrl Pts',(43.858042635223,58.9230601446436,12.));
#165625=CARTESIAN_POINT('Ctrl Pts',(43.8808949651872,58.936466892712,12.));
#165626=CARTESIAN_POINT('Ctrl Pts',(43.9037917117739,58.9498712429054,12.));
#165627=CARTESIAN_POINT('Ctrl Pts',(43.9267328191501,58.9632731052696,12.));
#165628=CARTESIAN_POINT('Ctrl Pts',(43.9497182316331,58.9766723902529,12.));
#165629=CARTESIAN_POINT('Ctrl Pts',(43.9727478937056,58.9900690087408,12.));
#165630=CARTESIAN_POINT('Ctrl Pts',(43.9958217500369,59.0034628721168,12.));
#165631=CARTESIAN_POINT('Ctrl Pts',(44.0189397454599,59.0168538922095,12.));
#165632=CARTESIAN_POINT('Ctrl Pts',(44.0421018249223,59.0302419811777,12.));
#165633=CARTESIAN_POINT('Ctrl Pts',(44.0653079334385,59.0436270514087,12.));
#165634=CARTESIAN_POINT('Ctrl Pts',(44.0885580160432,59.0570090154242,12.));
#165635=CARTESIAN_POINT('Ctrl Pts',(44.1118520177221,59.0703877857526,12.));
#165636=CARTESIAN_POINT('Ctrl Pts',(44.1351898834051,59.08376327492,12.));
#165637=CARTESIAN_POINT('Ctrl Pts',(44.1585715581064,59.0971353957206,12.));
#165638=CARTESIAN_POINT('Ctrl Pts',(44.1819969870307,59.1105040614276,12.));
#165639=CARTESIAN_POINT('Ctrl Pts',(44.2054661156875,59.1238691860306,12.));
#165640=CARTESIAN_POINT('Ctrl Pts',(44.228978889997,59.1372306844586,12.));
#165641=CARTESIAN_POINT('Ctrl Pts',(44.2525352563996,59.1505884728215,12.));
#165642=CARTESIAN_POINT('Ctrl Pts',(44.2761351616048,59.1639424678793,12.));
#165643=CARTESIAN_POINT('Ctrl Pts',(44.2997785523431,59.1772925865213,12.));
#165644=CARTESIAN_POINT('Ctrl Pts',(44.3234653750884,59.1906387451979,12.));
#165645=CARTESIAN_POINT('Ctrl Pts',(44.3471955758402,59.2039808594752,12.));
#165646=CARTESIAN_POINT('Ctrl Pts',(44.3709690997469,59.2173188432798,12.));
#165647=CARTESIAN_POINT('Ctrl Pts',(44.3947858914074,59.2306526095131,12.));
#165648=CARTESIAN_POINT('Ctrl Pts',(44.418645895545,59.2439820714187,12.));
#165649=CARTESIAN_POINT('Ctrl Pts',(44.4425490575911,59.2573071437774,12.));
#165650=CARTESIAN_POINT('Ctrl Pts',(44.4664953242378,59.2706277440445,12.));
#165651=CARTESIAN_POINT('Ctrl Pts',(44.490484644151,59.2839437938237,12.));
#165652=CARTESIAN_POINT('Ctrl Pts',(44.5145169681349,59.2972552192156,12.));
#165653=CARTESIAN_POINT('Ctrl Pts',(44.535154147848,59.3086616639524,12.));
#165654=CARTESIAN_POINT('Ctrl Pts',(44.5509994358156,59.3174041872348,12.));
#165655=CARTESIAN_POINT('Ctrl Pts',(44.5620338188741,59.3234848865457,12.));
#165656=CARTESIAN_POINT('Ctrl Pts',(44.5682447396025,59.3269051738425,12.));
#165657=CARTESIAN_POINT('Ctrl Pts',(44.5696260757798,59.3276657444395,12.));
#165658=CARTESIAN_POINT('',(40.8467768343956,56.8466430164621,0.));
#165659=CARTESIAN_POINT('',(40.8467768343956,56.8466430164621,0.));
#165660=CARTESIAN_POINT('Ctrl Pts',(44.5696260757798,59.3276657444395,0.));
#165661=CARTESIAN_POINT('Ctrl Pts',(44.5682447396025,59.3269051738425,0.));
#165662=CARTESIAN_POINT('Ctrl Pts',(44.5620338188741,59.3234848865457,0.));
#165663=CARTESIAN_POINT('Ctrl Pts',(44.5509994358156,59.3174041872348,0.));
#165664=CARTESIAN_POINT('Ctrl Pts',(44.535154147848,59.3086616639524,0.));
#165665=CARTESIAN_POINT('Ctrl Pts',(44.5145169681349,59.2972552192156,0.));
#165666=CARTESIAN_POINT('Ctrl Pts',(44.490484644151,59.2839437938237,0.));
#165667=CARTESIAN_POINT('Ctrl Pts',(44.4664953242378,59.2706277440445,0.));
#165668=CARTESIAN_POINT('Ctrl Pts',(44.4425490575911,59.2573071437774,0.));
#165669=CARTESIAN_POINT('Ctrl Pts',(44.418645895545,59.2439820714187,0.));
#165670=CARTESIAN_POINT('Ctrl Pts',(44.3947858914074,59.2306526095131,0.));
#165671=CARTESIAN_POINT('Ctrl Pts',(44.3709690997469,59.2173188432798,0.));
#165672=CARTESIAN_POINT('Ctrl Pts',(44.3471955758402,59.2039808594752,0.));
#165673=CARTESIAN_POINT('Ctrl Pts',(44.3234653750884,59.1906387451979,0.));
#165674=CARTESIAN_POINT('Ctrl Pts',(44.2997785523431,59.1772925865213,0.));
#165675=CARTESIAN_POINT('Ctrl Pts',(44.2761351616048,59.1639424678793,0.));
#165676=CARTESIAN_POINT('Ctrl Pts',(44.2525352563996,59.1505884728215,0.));
#165677=CARTESIAN_POINT('Ctrl Pts',(44.228978889997,59.1372306844586,0.));
#165678=CARTESIAN_POINT('Ctrl Pts',(44.2054661156875,59.1238691860306,0.));
#165679=CARTESIAN_POINT('Ctrl Pts',(44.1819969870307,59.1105040614276,0.));
#165680=CARTESIAN_POINT('Ctrl Pts',(44.1585715581064,59.0971353957206,0.));
#165681=CARTESIAN_POINT('Ctrl Pts',(44.1351898834051,59.08376327492,0.));
#165682=CARTESIAN_POINT('Ctrl Pts',(44.1118520177221,59.0703877857526,0.));
#165683=CARTESIAN_POINT('Ctrl Pts',(44.0885580160432,59.0570090154242,0.));
#165684=CARTESIAN_POINT('Ctrl Pts',(44.0653079334385,59.0436270514087,0.));
#165685=CARTESIAN_POINT('Ctrl Pts',(44.0421018249223,59.0302419811777,0.));
#165686=CARTESIAN_POINT('Ctrl Pts',(44.0189397454599,59.0168538922095,0.));
#165687=CARTESIAN_POINT('Ctrl Pts',(43.9958217500369,59.0034628721168,0.));
#165688=CARTESIAN_POINT('Ctrl Pts',(43.9727478937056,58.9900690087408,0.));
#165689=CARTESIAN_POINT('Ctrl Pts',(43.9497182316331,58.9766723902529,0.));
#165690=CARTESIAN_POINT('Ctrl Pts',(43.9267328191501,58.9632731052696,0.));
#165691=CARTESIAN_POINT('Ctrl Pts',(43.9037917117739,58.9498712429054,0.));
#165692=CARTESIAN_POINT('Ctrl Pts',(43.8808949651872,58.936466892712,0.));
#165693=CARTESIAN_POINT('Ctrl Pts',(43.858042635223,58.9230601446436,0.));
#165694=CARTESIAN_POINT('Ctrl Pts',(43.835234777842,58.9096510890129,0.));
#165695=CARTESIAN_POINT('Ctrl Pts',(43.8124714491076,58.8962398164493,0.));
#165696=CARTESIAN_POINT('Ctrl Pts',(43.7897527051609,58.8828264178621,0.));
#165697=CARTESIAN_POINT('Ctrl Pts',(43.7670786022402,58.8694109844648,0.));
#165698=CARTESIAN_POINT('Ctrl Pts',(43.7444491966942,58.8559936077941,0.));
#165699=CARTESIAN_POINT('Ctrl Pts',(43.7218645449922,58.8425743797326,0.));
#165700=CARTESIAN_POINT('Ctrl Pts',(43.6993247037314,58.8291533925293,0.));
#165701=CARTESIAN_POINT('Ctrl Pts',(43.6768297296395,58.8157307388238,0.));
#165702=CARTESIAN_POINT('Ctrl Pts',(43.6543796795789,58.8023065116436,0.));
#165703=CARTESIAN_POINT('Ctrl Pts',(43.6319746105482,58.788880804397,0.));
#165704=CARTESIAN_POINT('Ctrl Pts',(43.6096145796796,58.775453710867,0.));
#165705=CARTESIAN_POINT('Ctrl Pts',(43.5872996442345,58.7620253252062,0.));
#165706=CARTESIAN_POINT('Ctrl Pts',(43.5650298615916,58.74859574193,0.));
#165707=CARTESIAN_POINT('Ctrl Pts',(43.5428052892488,58.7351650559181,0.));
#165708=CARTESIAN_POINT('Ctrl Pts',(43.5206259848337,58.7217333624209,0.));
#165709=CARTESIAN_POINT('Ctrl Pts',(43.4984920061073,58.7083007570661,0.));
#165710=CARTESIAN_POINT('Ctrl Pts',(43.4764034109654,58.6948673358638,0.));
#165711=CARTESIAN_POINT('Ctrl Pts',(43.4543602574351,58.6814331952138,0.));
#165712=CARTESIAN_POINT('Ctrl Pts',(43.4323626036736,58.6679984319097,0.));
#165713=CARTESIAN_POINT('Ctrl Pts',(43.4104105079768,58.6545631431393,0.));
#165714=CARTESIAN_POINT('Ctrl Pts',(43.388504028781,58.6411274264857,0.));
#165715=CARTESIAN_POINT('Ctrl Pts',(43.3666432246635,58.627691379929,0.));
#165716=CARTESIAN_POINT('Ctrl Pts',(43.3448281543371,58.6142551018467,0.));
#165717=CARTESIAN_POINT('Ctrl Pts',(43.3230588766449,58.6008186910156,0.));
#165718=CARTESIAN_POINT('Ctrl Pts',(43.3013354505701,58.5873822466152,0.));
#165719=CARTESIAN_POINT('Ctrl Pts',(43.27965793524,58.573945868231,0.));
#165720=CARTESIAN_POINT('Ctrl Pts',(43.2580263899278,58.5605096558578,0.));
#165721=CARTESIAN_POINT('Ctrl Pts',(43.2364408740493,58.5470737099032,0.));
#165722=CARTESIAN_POINT('Ctrl Pts',(43.2149014471574,58.5336381311917,0.));
#165723=CARTESIAN_POINT('Ctrl Pts',(43.1934081689505,58.5202030209669,0.));
#165724=CARTESIAN_POINT('Ctrl Pts',(43.1719610992771,58.5067684808944,0.));
#165725=CARTESIAN_POINT('Ctrl Pts',(43.1505602981365,58.4933346130636,0.));
#165726=CARTESIAN_POINT('Ctrl Pts',(43.1292058256776,58.4799015199907,0.));
#165727=CARTESIAN_POINT('Ctrl Pts',(43.1078977421916,58.4664693046217,0.));
#165728=CARTESIAN_POINT('Ctrl Pts',(43.0866361081177,58.4530380703349,0.));
#165729=CARTESIAN_POINT('Ctrl Pts',(43.0654209840511,58.4396079209451,0.));
#165730=CARTESIAN_POINT('Ctrl Pts',(43.0442524307434,58.4261789607058,0.));
#165731=CARTESIAN_POINT('Ctrl Pts',(43.0231305091027,58.4127512943136,0.));
#165732=CARTESIAN_POINT('Ctrl Pts',(43.0020552801859,58.3993250269101,0.));
#165733=CARTESIAN_POINT('Ctrl Pts',(42.9810268052032,58.3859002640857,0.));
#165734=CARTESIAN_POINT('Ctrl Pts',(42.960045145526,58.3724771118826,0.));
#165735=CARTESIAN_POINT('Ctrl Pts',(42.9391103626879,58.3590556767978,0.));
#165736=CARTESIAN_POINT('Ctrl Pts',(42.9182225183854,58.3456360657865,0.));
#165737=CARTESIAN_POINT('Ctrl Pts',(42.8973816744709,58.3322183862654,0.));
#165738=CARTESIAN_POINT('Ctrl Pts',(42.8765878929551,58.3188027461164,0.));
#165739=CARTESIAN_POINT('Ctrl Pts',(42.8558412360158,58.3053892536894,0.));
#165740=CARTESIAN_POINT('Ctrl Pts',(42.8351417659999,58.2919780178064,0.));
#165741=CARTESIAN_POINT('Ctrl Pts',(42.8144895454233,58.2785691477638,0.));
#165742=CARTESIAN_POINT('Ctrl Pts',(42.7938846369651,58.2651627533368,0.));
#165743=CARTESIAN_POINT('Ctrl Pts',(42.7733271034679,58.2517589447821,0.));
#165744=CARTESIAN_POINT('Ctrl Pts',(42.7528170079484,58.2383578328424,0.));
#165745=CARTESIAN_POINT('Ctrl Pts',(42.7323544135985,58.22495952875,0.));
#165746=CARTESIAN_POINT('Ctrl Pts',(42.7119393837866,58.21156414423,0.));
#165747=CARTESIAN_POINT('Ctrl Pts',(42.6915719820513,58.1981717915037,0.));
#165748=CARTESIAN_POINT('Ctrl Pts',(42.6712522721016,58.1847825832923,0.));
#165749=CARTESIAN_POINT('Ctrl Pts',(42.6509803178265,58.171396632821,0.));
#165750=CARTESIAN_POINT('Ctrl Pts',(42.6307561832976,58.1580140538228,0.));
#165751=CARTESIAN_POINT('Ctrl Pts',(42.6105799327699,58.1446349605421,0.));
#165752=CARTESIAN_POINT('Ctrl Pts',(42.5904516306762,58.1312594677386,0.));
#165753=CARTESIAN_POINT('Ctrl Pts',(42.5703713416265,58.1178876906907,0.));
#165754=CARTESIAN_POINT('Ctrl Pts',(42.5503391304183,58.1045197452003,0.));
#165755=CARTESIAN_POINT('Ctrl Pts',(42.5303550620387,58.0911557475965,0.));
#165756=CARTESIAN_POINT('Ctrl Pts',(42.5104192016664,58.0777958147403,0.));
#165757=CARTESIAN_POINT('Ctrl Pts',(42.4905316146653,58.0644400640275,0.));
#165758=CARTESIAN_POINT('Ctrl Pts',(42.4706923665845,58.0510886133926,0.));
#165759=CARTESIAN_POINT('Ctrl Pts',(42.4509015231674,58.037741581314,0.));
#165760=CARTESIAN_POINT('Ctrl Pts',(42.4311591503555,58.0243990868181,0.));
#165761=CARTESIAN_POINT('Ctrl Pts',(42.411465314289,58.0110612494828,0.));
#165762=CARTESIAN_POINT('Ctrl Pts',(42.3918200813014,57.9977281894422,0.));
#165763=CARTESIAN_POINT('Ctrl Pts',(42.3722235179197,57.9844000273911,0.));
#165764=CARTESIAN_POINT('Ctrl Pts',(42.3526756908746,57.9710768845899,0.));
#165765=CARTESIAN_POINT('Ctrl Pts',(42.333176667102,57.9577588828683,0.));
#165766=CARTESIAN_POINT('Ctrl Pts',(42.3137265137452,57.9444461446299,0.));
#165767=CARTESIAN_POINT('Ctrl Pts',(42.2943252981489,57.9311387928563,0.));
#165768=CARTESIAN_POINT('Ctrl Pts',(42.2749730878594,57.9178369511114,0.));
#165769=CARTESIAN_POINT('Ctrl Pts',(42.2556699506353,57.9045407435474,0.));
#165770=CARTESIAN_POINT('Ctrl Pts',(42.2364159544501,57.8912502949096,0.));
#165771=CARTESIAN_POINT('Ctrl Pts',(42.2172111674938,57.8779657305413,0.));
#165772=CARTESIAN_POINT('Ctrl Pts',(42.1980556581665,57.864687176387,0.));
#165773=CARTESIAN_POINT('Ctrl Pts',(42.1789494950794,57.8514147589972,0.));
#165774=CARTESIAN_POINT('Ctrl Pts',(42.1598927470646,57.8381486055342,0.));
#165775=CARTESIAN_POINT('Ctrl Pts',(42.1408854831783,57.8248888437775,0.));
#165776=CARTESIAN_POINT('Ctrl Pts',(42.121927772702,57.8116356021288,0.));
#165777=CARTESIAN_POINT('Ctrl Pts',(42.1030196851366,57.798389009616,0.));
#165778=CARTESIAN_POINT('Ctrl Pts',(42.0841612902042,57.7851491958987,0.));
#165779=CARTESIAN_POINT('Ctrl Pts',(42.0653526578588,57.7719162912744,0.));
#165780=CARTESIAN_POINT('Ctrl Pts',(42.0465938582882,57.7586904266834,0.));
#165781=CARTESIAN_POINT('Ctrl Pts',(42.0278849619148,57.745471733714,0.));
#165782=CARTESIAN_POINT('Ctrl Pts',(42.0092260393897,57.7322603446066,0.));
#165783=CARTESIAN_POINT('Ctrl Pts',(41.990617161596,57.7190563922593,0.));
#165784=CARTESIAN_POINT('Ctrl Pts',(41.9720583996592,57.7058600102351,0.));
#165785=CARTESIAN_POINT('Ctrl Pts',(41.9535498249488,57.6926713327672,0.));
#165786=CARTESIAN_POINT('Ctrl Pts',(41.9350915090796,57.6794904947649,0.));
#165787=CARTESIAN_POINT('Ctrl Pts',(41.9166835239054,57.6663176318189,0.));
#165788=CARTESIAN_POINT('Ctrl Pts',(41.8983259415253,57.6531528802072,0.));
#165789=CARTESIAN_POINT('Ctrl Pts',(41.8800188342912,57.6399963769009,0.));
#165790=CARTESIAN_POINT('Ctrl Pts',(41.8617622748107,57.6268482595701,0.));
#165791=CARTESIAN_POINT('Ctrl Pts',(41.8435563359456,57.613708666588,0.));
#165792=CARTESIAN_POINT('Ctrl Pts',(41.8254010908051,57.6005777370347,0.));
#165793=CARTESIAN_POINT('Ctrl Pts',(41.8072966127559,57.5874556107054,0.));
#165794=CARTESIAN_POINT('Ctrl Pts',(41.7892429754298,57.5743424281204,0.));
#165795=CARTESIAN_POINT('Ctrl Pts',(41.7712402527273,57.561238330532,0.));
#165796=CARTESIAN_POINT('Ctrl Pts',(41.7532885188174,57.5481434599334,0.));
#165797=CARTESIAN_POINT('Ctrl Pts',(41.7353878481335,57.5350579590648,0.));
#165798=CARTESIAN_POINT('Ctrl Pts',(41.7175383153819,57.5219819714169,0.));
#165799=CARTESIAN_POINT('Ctrl Pts',(41.6997399955445,57.5089156412341,0.));
#165800=CARTESIAN_POINT('Ctrl Pts',(41.6819929638797,57.4958591135165,0.));
#165801=CARTESIAN_POINT('Ctrl Pts',(41.6642972959168,57.4828125340222,0.));
#165802=CARTESIAN_POINT('Ctrl Pts',(41.6466530674522,57.4697760492693,0.));
#165803=CARTESIAN_POINT('Ctrl Pts',(41.6290603545674,57.4567498065573,0.));
#165804=CARTESIAN_POINT('Ctrl Pts',(41.6115192336393,57.4437339539848,0.));
#165805=CARTESIAN_POINT('Ctrl Pts',(41.5940297813473,57.4307286404657,0.));
#165806=CARTESIAN_POINT('Ctrl Pts',(41.5765920746764,57.417734015749,0.));
#165807=CARTESIAN_POINT('Ctrl Pts',(41.5592061909159,57.4047502304207,0.));
#165808=CARTESIAN_POINT('Ctrl Pts',(41.5418722076558,57.3917774358844,0.));
#165809=CARTESIAN_POINT('Ctrl Pts',(41.5245902027767,57.378815784345,0.));
#165810=CARTESIAN_POINT('Ctrl Pts',(41.5073602544404,57.3658654287948,0.));
#165811=CARTESIAN_POINT('Ctrl Pts',(41.4901824410654,57.3529265229858,0.));
#165812=CARTESIAN_POINT('Ctrl Pts',(41.4730568413535,57.339999221474,0.));
#165813=CARTESIAN_POINT('Ctrl Pts',(41.4559835343338,57.3270836796925,0.));
#165814=CARTESIAN_POINT('Ctrl Pts',(41.4389625993948,57.3141800540137,0.));
#165815=CARTESIAN_POINT('Ctrl Pts',(41.4219941163154,57.3012885018139,0.));
#165816=CARTESIAN_POINT('Ctrl Pts',(41.4050781652923,57.2884091815385,0.));
#165817=CARTESIAN_POINT('Ctrl Pts',(41.3882148268798,57.2755422525822,0.));
#165818=CARTESIAN_POINT('Ctrl Pts',(41.3714041819215,57.2626878751584,0.));
#165819=CARTESIAN_POINT('Ctrl Pts',(41.3546463114889,57.2498462101883,0.));
#165820=CARTESIAN_POINT('Ctrl Pts',(41.3379412967889,57.237017419142,0.));
#165821=CARTESIAN_POINT('Ctrl Pts',(41.321289219151,57.2242016640226,0.));
#165822=CARTESIAN_POINT('Ctrl Pts',(41.304690160231,57.2113991077325,0.));
#165823=CARTESIAN_POINT('Ctrl Pts',(41.2881442021869,57.1986099143992,0.));
#165824=CARTESIAN_POINT('Ctrl Pts',(41.2716514278268,57.1858342496526,0.));
#165825=CARTESIAN_POINT('Ctrl Pts',(41.2552119208445,57.1730722810771,0.));
#165826=CARTESIAN_POINT('Ctrl Pts',(41.2388257656534,57.1603241779043,0.));
#165827=CARTESIAN_POINT('Ctrl Pts',(41.2224930469412,57.1475901101795,0.));
#165828=CARTESIAN_POINT('Ctrl Pts',(41.2062138492913,57.1348702480644,0.));
#165829=CARTESIAN_POINT('Ctrl Pts',(41.1899882567941,57.1221647611232,0.));
#165830=CARTESIAN_POINT('Ctrl Pts',(41.1738163525931,57.1094738174998,0.));
#165831=CARTESIAN_POINT('Ctrl Pts',(41.1576982197402,57.0967975854912,0.));
#165832=CARTESIAN_POINT('Ctrl Pts',(41.1416339422132,57.0841362354281,0.));
#165833=CARTESIAN_POINT('Ctrl Pts',(41.1256236057436,57.0714899412091,0.));
#165834=CARTESIAN_POINT('Ctrl Pts',(41.1096672990125,57.0588588825266,0.));
#165835=CARTESIAN_POINT('Ctrl Pts',(41.0937651137519,57.0462432450637,0.));
#165836=CARTESIAN_POINT('Ctrl Pts',(41.0779171422415,57.0336432158504,0.));
#165837=CARTESIAN_POINT('Ctrl Pts',(41.0621234751,57.0210589791777,0.));
#165838=CARTESIAN_POINT('Ctrl Pts',(41.0463841993622,57.008490713044,0.));
#165839=CARTESIAN_POINT('Ctrl Pts',(41.0306993954021,56.9959385834768,0.));
#165840=CARTESIAN_POINT('Ctrl Pts',(41.0150691398988,56.9834027500178,0.));
#165841=CARTESIAN_POINT('Ctrl Pts',(40.9994935117307,56.9708833766184,0.));
#165842=CARTESIAN_POINT('Ctrl Pts',(40.9839725967121,56.9583806404069,0.));
#165843=CARTESIAN_POINT('Ctrl Pts',(40.968506493303,56.9458947422541,0.));
#165844=CARTESIAN_POINT('Ctrl Pts',(40.9530953164952,56.9334259139928,0.));
#165845=CARTESIAN_POINT('Ctrl Pts',(40.9377391857043,56.9209743960861,0.));
#165846=CARTESIAN_POINT('Ctrl Pts',(40.9224382132382,56.9085404164432,0.));
#165847=CARTESIAN_POINT('Ctrl Pts',(40.907192493755,56.8961241708926,0.));
#165848=CARTESIAN_POINT('Ctrl Pts',(40.8920020903443,56.8837257978574,0.));
#165849=CARTESIAN_POINT('Ctrl Pts',(40.8768670342278,56.8713453765253,0.));
#165850=CARTESIAN_POINT('Ctrl Pts',(40.8648032759631,56.8614554317993,0.));
#165851=CARTESIAN_POINT('Ctrl Pts',(40.8557803680411,56.8540460739677,0.));
#165852=CARTESIAN_POINT('Ctrl Pts',(40.8497761671086,56.8491101022668,0.));
#165853=CARTESIAN_POINT('Ctrl Pts',(40.8467768343956,56.8466430164621,0.));
#165854=CARTESIAN_POINT('Ctrl Pts',(49.8690697110161,55.3473204966403,0.));
#165855=CARTESIAN_POINT('Ctrl Pts',(49.8690697110161,55.3473204966403,12.));
#165856=CARTESIAN_POINT('Ctrl Pts',(49.8639277221566,55.3451131058826,0.));
#165857=CARTESIAN_POINT('Ctrl Pts',(49.8639277221566,55.3451131058826,12.));
#165858=CARTESIAN_POINT('Ctrl Pts',(49.8536479176833,55.34069740326,0.));
#165859=CARTESIAN_POINT('Ctrl Pts',(49.8536479176833,55.34069740326,12.));
#165860=CARTESIAN_POINT('Ctrl Pts',(49.8382407307107,55.3340710860055,0.));
#165861=CARTESIAN_POINT('Ctrl Pts',(49.8382407307107,55.3340710860055,12.));
#165862=CARTESIAN_POINT('Ctrl Pts',(49.8177228552376,55.3252304694602,0.));
#165863=CARTESIAN_POINT('Ctrl Pts',(49.8177228552376,55.3252304694602,12.));
#165864=CARTESIAN_POINT('Ctrl Pts',(49.7921172540628,55.3141704897766,0.));
#165865=CARTESIAN_POINT('Ctrl Pts',(49.7921172540628,55.3141704897766,12.));
#165866=CARTESIAN_POINT('Ctrl Pts',(49.7665534128535,55.3031013105853,0.));
#165867=CARTESIAN_POINT('Ctrl Pts',(49.7665534128535,55.3031013105853,12.));
#165868=CARTESIAN_POINT('Ctrl Pts',(49.7410313576508,55.2920229527546,0.));
#165869=CARTESIAN_POINT('Ctrl Pts',(49.7410313576508,55.2920229527546,12.));
#165870=CARTESIAN_POINT('Ctrl Pts',(49.7155511248531,55.2809354521515,0.));
#165871=CARTESIAN_POINT('Ctrl Pts',(49.7155511248531,55.2809354521515,12.));
#165872=CARTESIAN_POINT('Ctrl Pts',(49.6901127631627,55.2698388650025,0.));
#165873=CARTESIAN_POINT('Ctrl Pts',(49.6901127631627,55.2698388650025,12.));
#165874=CARTESIAN_POINT('Ctrl Pts',(49.6647163322266,55.2587332663783,0.));
#165875=CARTESIAN_POINT('Ctrl Pts',(49.6647163322266,55.2587332663783,12.));
#165876=CARTESIAN_POINT('Ctrl Pts',(49.6393618987473,55.2476187434057,0.));
#165877=CARTESIAN_POINT('Ctrl Pts',(49.6393618987473,55.2476187434057,12.));
#165878=CARTESIAN_POINT('Ctrl Pts',(49.6140495332803,55.2364953899358,0.));
#165879=CARTESIAN_POINT('Ctrl Pts',(49.6140495332803,55.2364953899358,12.));
#165880=CARTESIAN_POINT('Ctrl Pts',(49.5887793068352,55.2253633007666,0.));
#165881=CARTESIAN_POINT('Ctrl Pts',(49.5887793068352,55.2253633007666,12.));
#165882=CARTESIAN_POINT('Ctrl Pts',(49.5635512873435,55.2142225657013,0.));
#165883=CARTESIAN_POINT('Ctrl Pts',(49.5635512873435,55.2142225657013,12.));
#165884=CARTESIAN_POINT('Ctrl Pts',(49.5383655368073,55.2030732647312,0.));
#165885=CARTESIAN_POINT('Ctrl Pts',(49.5383655368073,55.2030732647312,12.));
#165886=CARTESIAN_POINT('Ctrl Pts',(49.5132221132992,55.1919154713647,0.));
#165887=CARTESIAN_POINT('Ctrl Pts',(49.5132221132992,55.1919154713647,12.));
#165888=CARTESIAN_POINT('Ctrl Pts',(49.4881210723966,55.1807492550119,0.));
#165889=CARTESIAN_POINT('Ctrl Pts',(49.4881210723966,55.1807492550119,12.));
#165890=CARTESIAN_POINT('Ctrl Pts',(49.4630624688793,55.1695746838174,0.));
#165891=CARTESIAN_POINT('Ctrl Pts',(49.4630624688793,55.1695746838174,12.));
#165892=CARTESIAN_POINT('Ctrl Pts',(49.4380463581965,55.1583918271116,0.));
#165893=CARTESIAN_POINT('Ctrl Pts',(49.4380463581965,55.1583918271116,12.));
#165894=CARTESIAN_POINT('Ctrl Pts',(49.4130727983201,55.1472007585183,0.));
#165895=CARTESIAN_POINT('Ctrl Pts',(49.4130727983201,55.1472007585183,12.));
#165896=CARTESIAN_POINT('Ctrl Pts',(49.3881418495489,55.1360015556221,0.));
#165897=CARTESIAN_POINT('Ctrl Pts',(49.3881418495489,55.1360015556221,12.));
#165898=CARTESIAN_POINT('Ctrl Pts',(49.3632535736715,55.1247942985619,0.));
#165899=CARTESIAN_POINT('Ctrl Pts',(49.3632535736715,55.1247942985619,12.));
#165900=CARTESIAN_POINT('Ctrl Pts',(49.3384080333155,55.1135790689464,0.));
#165901=CARTESIAN_POINT('Ctrl Pts',(49.3384080333155,55.1135790689464,12.));
#165902=CARTESIAN_POINT('Ctrl Pts',(49.3136052912621,55.102355948714,0.));
#165903=CARTESIAN_POINT('Ctrl Pts',(49.3136052912621,55.102355948714,12.));
#165904=CARTESIAN_POINT('Ctrl Pts',(49.2888454096563,55.0911250188302,0.));
#165905=CARTESIAN_POINT('Ctrl Pts',(49.2888454096563,55.0911250188302,12.));
#165906=CARTESIAN_POINT('Ctrl Pts',(49.264128449652,55.079886358701,0.));
#165907=CARTESIAN_POINT('Ctrl Pts',(49.264128449652,55.079886358701,12.));
#165908=CARTESIAN_POINT('Ctrl Pts',(49.2394544718531,55.0686400468931,0.));
#165909=CARTESIAN_POINT('Ctrl Pts',(49.2394544718531,55.0686400468931,12.));
#165910=CARTESIAN_POINT('Ctrl Pts',(49.2148235365703,55.0573861615579,0.));
#165911=CARTESIAN_POINT('Ctrl Pts',(49.2148235365703,55.0573861615579,12.));
#165912=CARTESIAN_POINT('Ctrl Pts',(49.1902357041461,55.0461247809744,0.));
#165913=CARTESIAN_POINT('Ctrl Pts',(49.1902357041461,55.0461247809744,12.));
#165914=CARTESIAN_POINT('Ctrl Pts',(49.1656910352476,55.0348559840453,0.));
#165915=CARTESIAN_POINT('Ctrl Pts',(49.1656910352476,55.0348559840453,12.));
#165916=CARTESIAN_POINT('Ctrl Pts',(49.1411895911635,55.0235798508045,0.));
#165917=CARTESIAN_POINT('Ctrl Pts',(49.1411895911635,55.0235798508045,12.));
#165918=CARTESIAN_POINT('Ctrl Pts',(49.116731433673,55.012296462186,0.));
#165919=CARTESIAN_POINT('Ctrl Pts',(49.116731433673,55.012296462186,12.));
#165920=CARTESIAN_POINT('Ctrl Pts',(49.0923166249219,55.0010058998107,0.));
#165921=CARTESIAN_POINT('Ctrl Pts',(49.0923166249219,55.0010058998107,12.));
#165922=CARTESIAN_POINT('Ctrl Pts',(49.067945227287,54.9897082457606,0.));
#165923=CARTESIAN_POINT('Ctrl Pts',(49.067945227287,54.9897082457606,12.));
#165924=CARTESIAN_POINT('Ctrl Pts',(49.0436173032528,54.9784035823766,0.));
#165925=CARTESIAN_POINT('Ctrl Pts',(49.0436173032528,54.9784035823766,12.));
#165926=CARTESIAN_POINT('Ctrl Pts',(49.0193329152479,54.9670919920029,0.));
#165927=CARTESIAN_POINT('Ctrl Pts',(49.0193329152479,54.9670919920029,12.));
#165928=CARTESIAN_POINT('Ctrl Pts',(48.9950921256526,54.9557735569943,0.));
#165929=CARTESIAN_POINT('Ctrl Pts',(48.9950921256526,54.9557735569943,12.));
#165930=CARTESIAN_POINT('Ctrl Pts',(48.9708949968795,54.9444483598378,0.));
#165931=CARTESIAN_POINT('Ctrl Pts',(48.9708949968795,54.9444483598378,12.));
#165932=CARTESIAN_POINT('Ctrl Pts',(48.9467415914269,54.9331164832424,0.));
#165933=CARTESIAN_POINT('Ctrl Pts',(48.9467415914269,54.9331164832424,12.));
#165934=CARTESIAN_POINT('Ctrl Pts',(48.9226319719368,54.9217780102355,0.));
#165935=CARTESIAN_POINT('Ctrl Pts',(48.9226319719368,54.9217780102355,12.));
#165936=CARTESIAN_POINT('Ctrl Pts',(48.8985662012528,54.9104330242742,0.));
#165937=CARTESIAN_POINT('Ctrl Pts',(48.8985662012528,54.9104330242742,12.));
#165938=CARTESIAN_POINT('Ctrl Pts',(48.8745443424477,54.8990816092953,0.));
#165939=CARTESIAN_POINT('Ctrl Pts',(48.8745443424477,54.8990816092953,12.));
#165940=CARTESIAN_POINT('Ctrl Pts',(48.8505664587974,54.8877238496566,0.));
#165941=CARTESIAN_POINT('Ctrl Pts',(48.8505664587974,54.8877238496566,12.));
#165942=CARTESIAN_POINT('Ctrl Pts',(48.8266326137622,54.8763598301037,0.));
#165943=CARTESIAN_POINT('Ctrl Pts',(48.8266326137622,54.8763598301037,12.));
#165944=CARTESIAN_POINT('Ctrl Pts',(48.8027428709614,54.8649896357285,0.));
#165945=CARTESIAN_POINT('Ctrl Pts',(48.8027428709614,54.8649896357285,12.));
#165946=CARTESIAN_POINT('Ctrl Pts',(48.7788972941438,54.8536133519292,0.));
#165947=CARTESIAN_POINT('Ctrl Pts',(48.7788972941438,54.8536133519292,12.));
#165948=CARTESIAN_POINT('Ctrl Pts',(48.7550959471601,54.8422310643763,0.));
#165949=CARTESIAN_POINT('Ctrl Pts',(48.7550959471601,54.8422310643763,12.));
#165950=CARTESIAN_POINT('Ctrl Pts',(48.7313388939845,54.8308428590344,0.));
#165951=CARTESIAN_POINT('Ctrl Pts',(48.7313388939845,54.8308428590344,12.));
#165952=CARTESIAN_POINT('Ctrl Pts',(48.7076261987292,54.819448822181,0.));
#165953=CARTESIAN_POINT('Ctrl Pts',(48.7076261987292,54.819448822181,12.));
#165954=CARTESIAN_POINT('Ctrl Pts',(48.6839579256566,54.8080490404275,0.));
#165955=CARTESIAN_POINT('Ctrl Pts',(48.6839579256566,54.8080490404275,12.));
#165956=CARTESIAN_POINT('Ctrl Pts',(48.6603341391886,54.796643600739,0.));
#165957=CARTESIAN_POINT('Ctrl Pts',(48.6603341391886,54.796643600739,12.));
#165958=CARTESIAN_POINT('Ctrl Pts',(48.6367549039112,54.7852325904583,0.));
#165959=CARTESIAN_POINT('Ctrl Pts',(48.6367549039112,54.7852325904583,12.));
#165960=CARTESIAN_POINT('Ctrl Pts',(48.6132202845783,54.7738160973031,0.));
#165961=CARTESIAN_POINT('Ctrl Pts',(48.6132202845783,54.7738160973031,12.));
#165962=CARTESIAN_POINT('Ctrl Pts',(48.5897303461125,54.7623942093586,0.));
#165963=CARTESIAN_POINT('Ctrl Pts',(48.5897303461125,54.7623942093586,12.));
#165964=CARTESIAN_POINT('Ctrl Pts',(48.5662851536026,54.7509670150714,0.));
#165965=CARTESIAN_POINT('Ctrl Pts',(48.5662851536026,54.7509670150714,12.));
#165966=CARTESIAN_POINT('Ctrl Pts',(48.5428847722977,54.7395346032453,0.));
#165967=CARTESIAN_POINT('Ctrl Pts',(48.5428847722977,54.7395346032453,12.));
#165968=CARTESIAN_POINT('Ctrl Pts',(48.519529267596,54.7280970630351,0.));
#165969=CARTESIAN_POINT('Ctrl Pts',(48.519529267596,54.7280970630351,12.));
#165970=CARTESIAN_POINT('Ctrl Pts',(48.4962187050457,54.716654483948,0.));
#165971=CARTESIAN_POINT('Ctrl Pts',(48.4962187050457,54.716654483948,12.));
#165972=CARTESIAN_POINT('Ctrl Pts',(48.472953150357,54.7052069558497,0.));
#165973=CARTESIAN_POINT('Ctrl Pts',(48.472953150357,54.7052069558497,12.));
#165974=CARTESIAN_POINT('Ctrl Pts',(48.4497326694052,54.6937545689695,0.));
#165975=CARTESIAN_POINT('Ctrl Pts',(48.4497326694052,54.6937545689695,12.));
#165976=CARTESIAN_POINT('Ctrl Pts',(48.426557328234,54.6822974139064,0.));
#165977=CARTESIAN_POINT('Ctrl Pts',(48.426557328234,54.6822974139064,12.));
#165978=CARTESIAN_POINT('Ctrl Pts',(48.4034271930514,54.6708355816358,0.));
#165979=CARTESIAN_POINT('Ctrl Pts',(48.4034271930514,54.6708355816358,12.));
#165980=CARTESIAN_POINT('Ctrl Pts',(48.3803423302294,54.6593691635145,0.));
#165981=CARTESIAN_POINT('Ctrl Pts',(48.3803423302294,54.6593691635145,12.));
#165982=CARTESIAN_POINT('Ctrl Pts',(48.3573028063124,54.6478982512794,0.));
#165983=CARTESIAN_POINT('Ctrl Pts',(48.3573028063124,54.6478982512794,12.));
#165984=CARTESIAN_POINT('Ctrl Pts',(48.3343086880194,54.6364229370494,0.));
#165985=CARTESIAN_POINT('Ctrl Pts',(48.3343086880194,54.6364229370494,12.));
#165986=CARTESIAN_POINT('Ctrl Pts',(48.3113600422443,54.6249433133261,0.));
#165987=CARTESIAN_POINT('Ctrl Pts',(48.3113600422443,54.6249433133261,12.));
#165988=CARTESIAN_POINT('Ctrl Pts',(48.2884569360506,54.6134594729959,0.));
#165989=CARTESIAN_POINT('Ctrl Pts',(48.2884569360506,54.6134594729959,12.));
#165990=CARTESIAN_POINT('Ctrl Pts',(48.2655994366665,54.6019715093309,0.));
#165991=CARTESIAN_POINT('Ctrl Pts',(48.2655994366665,54.6019715093309,12.));
#165992=CARTESIAN_POINT('Ctrl Pts',(48.2427876114947,54.5904795159926,0.));
#165993=CARTESIAN_POINT('Ctrl Pts',(48.2427876114947,54.5904795159926,12.));
#165994=CARTESIAN_POINT('Ctrl Pts',(48.2200215281173,54.5789835870342,0.));
#165995=CARTESIAN_POINT('Ctrl Pts',(48.2200215281173,54.5789835870342,12.));
#165996=CARTESIAN_POINT('Ctrl Pts',(48.1973012542966,54.5674838169041,0.));
#165997=CARTESIAN_POINT('Ctrl Pts',(48.1973012542966,54.5674838169041,12.));
#165998=CARTESIAN_POINT('Ctrl Pts',(48.1746268579736,54.5559803004492,0.));
#165999=CARTESIAN_POINT('Ctrl Pts',(48.1746268579736,54.5559803004492,12.));
#166000=CARTESIAN_POINT('Ctrl Pts',(48.1519984072622,54.5444731329201,0.));
#166001=CARTESIAN_POINT('Ctrl Pts',(48.1519984072622,54.5444731329201,12.));
#166002=CARTESIAN_POINT('Ctrl Pts',(48.1294159704573,54.5329624099721,0.));
#166003=CARTESIAN_POINT('Ctrl Pts',(48.1294159704573,54.5329624099721,12.));
#166004=CARTESIAN_POINT('Ctrl Pts',(48.1068796160405,54.5214482276678,0.));
#166005=CARTESIAN_POINT('Ctrl Pts',(48.1068796160405,54.5214482276678,12.));
#166006=CARTESIAN_POINT('Ctrl Pts',(48.0843894126806,54.5099306824786,0.));
#166007=CARTESIAN_POINT('Ctrl Pts',(48.0843894126806,54.5099306824786,12.));
#166008=CARTESIAN_POINT('Ctrl Pts',(48.0619454292324,54.4984098712886,0.));
#166009=CARTESIAN_POINT('Ctrl Pts',(48.0619454292324,54.4984098712886,12.));
#166010=CARTESIAN_POINT('Ctrl Pts',(48.0395477347298,54.4868858913971,0.));
#166011=CARTESIAN_POINT('Ctrl Pts',(48.0395477347298,54.4868858913971,12.));
#166012=CARTESIAN_POINT('Ctrl Pts',(48.0171963983924,54.4753588405215,0.));
#166013=CARTESIAN_POINT('Ctrl Pts',(48.0171963983924,54.4753588405215,12.));
#166014=CARTESIAN_POINT('Ctrl Pts',(47.9948914896326,54.4638288168003,0.));
#166015=CARTESIAN_POINT('Ctrl Pts',(47.9948914896326,54.4638288168003,12.));
#166016=CARTESIAN_POINT('Ctrl Pts',(47.9726330780572,54.4522959187955,0.));
#166017=CARTESIAN_POINT('Ctrl Pts',(47.9726330780572,54.4522959187955,12.));
#166018=CARTESIAN_POINT('Ctrl Pts',(47.9504212334675,54.4407602454967,0.));
#166019=CARTESIAN_POINT('Ctrl Pts',(47.9504212334675,54.4407602454967,12.));
#166020=CARTESIAN_POINT('Ctrl Pts',(47.9282560258516,54.429221896324,0.));
#166021=CARTESIAN_POINT('Ctrl Pts',(47.9282560258516,54.429221896324,12.));
#166022=CARTESIAN_POINT('Ctrl Pts',(47.9061375253897,54.4176809711311,0.));
#166023=CARTESIAN_POINT('Ctrl Pts',(47.9061375253897,54.4176809711311,12.));
#166024=CARTESIAN_POINT('Ctrl Pts',(47.8840658024618,54.4061375702079,0.));
#166025=CARTESIAN_POINT('Ctrl Pts',(47.8840658024618,54.4061375702079,12.));
#166026=CARTESIAN_POINT('Ctrl Pts',(47.8620409276493,54.3945917942832,0.));
#166027=CARTESIAN_POINT('Ctrl Pts',(47.8620409276493,54.3945917942832,12.));
#166028=CARTESIAN_POINT('Ctrl Pts',(47.8400629717355,54.3830437445279,0.));
#166029=CARTESIAN_POINT('Ctrl Pts',(47.8400629717355,54.3830437445279,12.));
#166030=CARTESIAN_POINT('Ctrl Pts',(47.8181320056995,54.3714935225591,0.));
#166031=CARTESIAN_POINT('Ctrl Pts',(47.8181320056995,54.3714935225591,12.));
#166032=CARTESIAN_POINT('Ctrl Pts',(47.7962481007185,54.3599412304437,0.));
#166033=CARTESIAN_POINT('Ctrl Pts',(47.7962481007185,54.3599412304437,12.));
#166034=CARTESIAN_POINT('Ctrl Pts',(47.7744113281771,54.3483869707002,0.));
#166035=CARTESIAN_POINT('Ctrl Pts',(47.7744113281771,54.3483869707002,12.));
#166036=CARTESIAN_POINT('Ctrl Pts',(47.7526217596694,54.3368308463023,0.));
#166037=CARTESIAN_POINT('Ctrl Pts',(47.7526217596694,54.3368308463023,12.));
#166038=CARTESIAN_POINT('Ctrl Pts',(47.7308794669993,54.3252729606823,0.));
#166039=CARTESIAN_POINT('Ctrl Pts',(47.7308794669993,54.3252729606823,12.));
#166040=CARTESIAN_POINT('Ctrl Pts',(47.7091845221747,54.3137134177345,0.));
#166041=CARTESIAN_POINT('Ctrl Pts',(47.7091845221747,54.3137134177345,12.));
#166042=CARTESIAN_POINT('Ctrl Pts',(47.6875369974087,54.302152321819,0.));
#166043=CARTESIAN_POINT('Ctrl Pts',(47.6875369974087,54.302152321819,12.));
#166044=CARTESIAN_POINT('Ctrl Pts',(47.6659369651301,54.290589777765,0.));
#166045=CARTESIAN_POINT('Ctrl Pts',(47.6659369651301,54.290589777765,12.));
#166046=CARTESIAN_POINT('Ctrl Pts',(47.6443844979847,54.2790258908738,0.));
#166047=CARTESIAN_POINT('Ctrl Pts',(47.6443844979847,54.2790258908738,12.));
#166048=CARTESIAN_POINT('Ctrl Pts',(47.6228796688375,54.2674607669226,0.));
#166049=CARTESIAN_POINT('Ctrl Pts',(47.6228796688375,54.2674607669226,12.));
#166050=CARTESIAN_POINT('Ctrl Pts',(47.6014225507659,54.2558945121678,0.));
#166051=CARTESIAN_POINT('Ctrl Pts',(47.6014225507659,54.2558945121678,12.));
#166052=CARTESIAN_POINT('Ctrl Pts',(47.5800132170608,54.244327233349,0.));
#166053=CARTESIAN_POINT('Ctrl Pts',(47.5800132170608,54.244327233349,12.));
#166054=CARTESIAN_POINT('Ctrl Pts',(47.5586517412363,54.2327590376924,0.));
#166055=CARTESIAN_POINT('Ctrl Pts',(47.5586517412363,54.2327590376924,12.));
#166056=CARTESIAN_POINT('Ctrl Pts',(47.5373381970326,54.2211900329138,0.));
#166057=CARTESIAN_POINT('Ctrl Pts',(47.5373381970326,54.2211900329138,12.));
#166058=CARTESIAN_POINT('Ctrl Pts',(47.5160726584174,54.209620327223,0.));
#166059=CARTESIAN_POINT('Ctrl Pts',(47.5160726584174,54.209620327223,12.));
#166060=CARTESIAN_POINT('Ctrl Pts',(47.4948551995801,54.198050029327,0.));
#166061=CARTESIAN_POINT('Ctrl Pts',(47.4948551995801,54.198050029327,12.));
#166062=CARTESIAN_POINT('Ctrl Pts',(47.4736858949322,54.1864792484345,0.));
#166063=CARTESIAN_POINT('Ctrl Pts',(47.4736858949322,54.1864792484345,12.));
#166064=CARTESIAN_POINT('Ctrl Pts',(47.4525648191173,54.1749080942593,0.));
#166065=CARTESIAN_POINT('Ctrl Pts',(47.4525648191173,54.1749080942593,12.));
#166066=CARTESIAN_POINT('Ctrl Pts',(47.4314920470141,54.1633366770239,0.));
#166067=CARTESIAN_POINT('Ctrl Pts',(47.4314920470141,54.1633366770239,12.));
#166068=CARTESIAN_POINT('Ctrl Pts',(47.4104676537381,54.1517651074637,0.));
#166069=CARTESIAN_POINT('Ctrl Pts',(47.4104676537381,54.1517651074637,12.));
#166070=CARTESIAN_POINT('Ctrl Pts',(47.3894917146365,54.1401934968311,0.));
#166071=CARTESIAN_POINT('Ctrl Pts',(47.3894917146365,54.1401934968311,12.));
#166072=CARTESIAN_POINT('Ctrl Pts',(47.3685643052874,54.1286219568989,0.));
#166073=CARTESIAN_POINT('Ctrl Pts',(47.3685643052874,54.1286219568989,12.));
#166074=CARTESIAN_POINT('Ctrl Pts',(47.3476855015102,54.1170505999645,0.));
#166075=CARTESIAN_POINT('Ctrl Pts',(47.3476855015102,54.1170505999645,12.));
#166076=CARTESIAN_POINT('Ctrl Pts',(47.3268553793694,54.1054795388543,0.));
#166077=CARTESIAN_POINT('Ctrl Pts',(47.3268553793694,54.1054795388543,12.));
#166078=CARTESIAN_POINT('Ctrl Pts',(47.3060740151752,54.0939088869269,0.));
#166079=CARTESIAN_POINT('Ctrl Pts',(47.3060740151752,54.0939088869269,12.));
#166080=CARTESIAN_POINT('Ctrl Pts',(47.2853414854793,54.0823387580776,0.));
#166081=CARTESIAN_POINT('Ctrl Pts',(47.2853414854793,54.0823387580776,12.));
#166082=CARTESIAN_POINT('Ctrl Pts',(47.2646578670746,54.0707692667438,0.));
#166083=CARTESIAN_POINT('Ctrl Pts',(47.2646578670746,54.0707692667438,12.));
#166084=CARTESIAN_POINT('Ctrl Pts',(47.2440232370065,54.0592005279086,0.));
#166085=CARTESIAN_POINT('Ctrl Pts',(47.2440232370065,54.0592005279086,12.));
#166086=CARTESIAN_POINT('Ctrl Pts',(47.2234376725743,54.047632657104,0.));
#166087=CARTESIAN_POINT('Ctrl Pts',(47.2234376725743,54.047632657104,12.));
#166088=CARTESIAN_POINT('Ctrl Pts',(47.202901251334,54.0360657704163,0.));
#166089=CARTESIAN_POINT('Ctrl Pts',(47.202901251334,54.0360657704163,12.));
#166090=CARTESIAN_POINT('Ctrl Pts',(47.1824140510926,54.0244999844893,0.));
#166091=CARTESIAN_POINT('Ctrl Pts',(47.1824140510926,54.0244999844893,12.));
#166092=CARTESIAN_POINT('Ctrl Pts',(47.1619761499087,54.0129354165297,0.));
#166093=CARTESIAN_POINT('Ctrl Pts',(47.1619761499087,54.0129354165297,12.));
#166094=CARTESIAN_POINT('Ctrl Pts',(47.1415876261035,54.0013721843118,0.));
#166095=CARTESIAN_POINT('Ctrl Pts',(47.1415876261035,54.0013721843118,12.));
#166096=CARTESIAN_POINT('Ctrl Pts',(47.1212485582643,53.989810406182,0.));
#166097=CARTESIAN_POINT('Ctrl Pts',(47.1212485582643,53.989810406182,12.));
#166098=CARTESIAN_POINT('Ctrl Pts',(47.1009590252458,53.9782502010634,0.));
#166099=CARTESIAN_POINT('Ctrl Pts',(47.1009590252458,53.9782502010634,12.));
#166100=CARTESIAN_POINT('Ctrl Pts',(47.0807191061648,53.9666916884596,0.));
#166101=CARTESIAN_POINT('Ctrl Pts',(47.0807191061648,53.9666916884596,12.));
#166102=CARTESIAN_POINT('Ctrl Pts',(47.0605288804008,53.95513498846,0.));
#166103=CARTESIAN_POINT('Ctrl Pts',(47.0605288804008,53.95513498846,12.));
#166104=CARTESIAN_POINT('Ctrl Pts',(47.0403884276071,53.9435802217436,0.));
#166105=CARTESIAN_POINT('Ctrl Pts',(47.0403884276071,53.9435802217436,12.));
#166106=CARTESIAN_POINT('Ctrl Pts',(47.0202978277138,53.9320275095853,0.));
#166107=CARTESIAN_POINT('Ctrl Pts',(47.0202978277138,53.9320275095853,12.));
#166108=CARTESIAN_POINT('Ctrl Pts',(47.0002571609297,53.9204769738596,0.));
#166109=CARTESIAN_POINT('Ctrl Pts',(47.0002571609297,53.9204769738596,12.));
#166110=CARTESIAN_POINT('Ctrl Pts',(46.9802665077366,53.9089287370463,0.));
#166111=CARTESIAN_POINT('Ctrl Pts',(46.9802665077366,53.9089287370463,12.));
#166112=CARTESIAN_POINT('Ctrl Pts',(46.960325948892,53.8973829222348,0.));
#166113=CARTESIAN_POINT('Ctrl Pts',(46.960325948892,53.8973829222348,12.));
#166114=CARTESIAN_POINT('Ctrl Pts',(46.94043556544,53.8858396531298,0.));
#166115=CARTESIAN_POINT('Ctrl Pts',(46.94043556544,53.8858396531298,12.));
#166116=CARTESIAN_POINT('Ctrl Pts',(46.9205954387133,53.8742990540563,0.));
#166117=CARTESIAN_POINT('Ctrl Pts',(46.9205954387133,53.8742990540563,12.));
#166118=CARTESIAN_POINT('Ctrl Pts',(46.9008056503351,53.8627612499638,0.));
#166119=CARTESIAN_POINT('Ctrl Pts',(46.9008056503351,53.8627612499638,12.));
#166120=CARTESIAN_POINT('Ctrl Pts',(46.881066282213,53.8512263664321,0.));
#166121=CARTESIAN_POINT('Ctrl Pts',(46.881066282213,53.8512263664321,12.));
#166122=CARTESIAN_POINT('Ctrl Pts',(46.8613774165435,53.8396945296757,0.));
#166123=CARTESIAN_POINT('Ctrl Pts',(46.8613774165435,53.8396945296757,12.));
#166124=CARTESIAN_POINT('Ctrl Pts',(46.841739135822,53.8281658665503,0.));
#166125=CARTESIAN_POINT('Ctrl Pts',(46.841739135822,53.8281658665503,12.));
#166126=CARTESIAN_POINT('Ctrl Pts',(46.8221515228457,53.816640504558,0.));
#166127=CARTESIAN_POINT('Ctrl Pts',(46.8221515228457,53.816640504558,12.));
#166128=CARTESIAN_POINT('Ctrl Pts',(46.802614660715,53.8051185718532,0.));
#166129=CARTESIAN_POINT('Ctrl Pts',(46.802614660715,53.8051185718532,12.));
#166130=CARTESIAN_POINT('Ctrl Pts',(46.7831286328278,53.793600197248,0.));
#166131=CARTESIAN_POINT('Ctrl Pts',(46.7831286328278,53.793600197248,12.));
#166132=CARTESIAN_POINT('Ctrl Pts',(46.763693522886,53.7820855102182,0.));
#166133=CARTESIAN_POINT('Ctrl Pts',(46.763693522886,53.7820855102182,12.));
#166134=CARTESIAN_POINT('Ctrl Pts',(46.7443094149045,53.7705746409076,0.));
#166135=CARTESIAN_POINT('Ctrl Pts',(46.7443094149045,53.7705746409076,12.));
#166136=CARTESIAN_POINT('Ctrl Pts',(46.7249763932129,53.7590677201342,0.));
#166137=CARTESIAN_POINT('Ctrl Pts',(46.7249763932129,53.7590677201342,12.));
#166138=CARTESIAN_POINT('Ctrl Pts',(46.7056945424559,53.7475648793946,0.));
#166139=CARTESIAN_POINT('Ctrl Pts',(46.7056945424559,53.7475648793946,12.));
#166140=CARTESIAN_POINT('Ctrl Pts',(46.6864639475862,53.7360662508675,0.));
#166141=CARTESIAN_POINT('Ctrl Pts',(46.6864639475862,53.7360662508675,12.));
#166142=CARTESIAN_POINT('Ctrl Pts',(46.6672846938752,53.7245719674221,0.));
#166143=CARTESIAN_POINT('Ctrl Pts',(46.6672846938752,53.7245719674221,12.));
#166144=CARTESIAN_POINT('Ctrl Pts',(46.6481568669217,53.7130821626262,0.));
#166145=CARTESIAN_POINT('Ctrl Pts',(46.6481568669217,53.7130821626262,12.));
#166146=CARTESIAN_POINT('Ctrl Pts',(46.6290805526559,53.7015969707541,0.));
#166147=CARTESIAN_POINT('Ctrl Pts',(46.6290805526559,53.7015969707541,12.));
#166148=CARTESIAN_POINT('Ctrl Pts',(46.6100558373401,53.690116526794,0.));
#166149=CARTESIAN_POINT('Ctrl Pts',(46.6100558373401,53.690116526794,12.));
#166150=CARTESIAN_POINT('Ctrl Pts',(46.5910828075652,53.678640966456,0.));
#166151=CARTESIAN_POINT('Ctrl Pts',(46.5910828075652,53.678640966456,12.));
#166152=CARTESIAN_POINT('Ctrl Pts',(46.5721615502589,53.6671704261735,0.));
#166153=CARTESIAN_POINT('Ctrl Pts',(46.5721615502589,53.6671704261735,12.));
#166154=CARTESIAN_POINT('Ctrl Pts',(46.5532921526899,53.6557050431069,0.));
#166155=CARTESIAN_POINT('Ctrl Pts',(46.5532921526899,53.6557050431069,12.));
#166156=CARTESIAN_POINT('Ctrl Pts',(46.5344747024677,53.6442449551455,0.));
#166157=CARTESIAN_POINT('Ctrl Pts',(46.5344747024677,53.6442449551455,12.));
#166158=CARTESIAN_POINT('Ctrl Pts',(46.5157092875377,53.6327903009098,0.));
#166159=CARTESIAN_POINT('Ctrl Pts',(46.5157092875377,53.6327903009098,12.));
#166160=CARTESIAN_POINT('Ctrl Pts',(46.4969959961779,53.6213412197542,0.));
#166161=CARTESIAN_POINT('Ctrl Pts',(46.4969959961779,53.6213412197542,12.));
#166162=CARTESIAN_POINT('Ctrl Pts',(46.4783349170182,53.6098978517869,0.));
#166163=CARTESIAN_POINT('Ctrl Pts',(46.4783349170182,53.6098978517869,12.));
#166164=CARTESIAN_POINT('Ctrl Pts',(46.4597261390526,53.5984603378862,0.));
#166165=CARTESIAN_POINT('Ctrl Pts',(46.4597261390526,53.5984603378862,12.));
#166166=CARTESIAN_POINT('Ctrl Pts',(46.4411697516474,53.5870288197161,0.));
#166167=CARTESIAN_POINT('Ctrl Pts',(46.4411697516474,53.5870288197161,12.));
#166168=CARTESIAN_POINT('Ctrl Pts',(46.422665844546,53.5756034397464,0.));
#166169=CARTESIAN_POINT('Ctrl Pts',(46.422665844546,53.5756034397464,12.));
#166170=CARTESIAN_POINT('Ctrl Pts',(46.4042145078682,53.5641843412537,0.));
#166171=CARTESIAN_POINT('Ctrl Pts',(46.4042145078682,53.5641843412537,12.));
#166172=CARTESIAN_POINT('Ctrl Pts',(46.3858158321044,53.552771668303,0.));
#166173=CARTESIAN_POINT('Ctrl Pts',(46.3858158321044,53.552771668303,12.));
#166174=CARTESIAN_POINT('Ctrl Pts',(46.3674699081043,53.5413655657323,0.));
#166175=CARTESIAN_POINT('Ctrl Pts',(46.3674699081043,53.5413655657323,12.));
#166176=CARTESIAN_POINT('Ctrl Pts',(46.3491768270664,53.5299661791396,0.));
#166177=CARTESIAN_POINT('Ctrl Pts',(46.3491768270664,53.5299661791396,12.));
#166178=CARTESIAN_POINT('Ctrl Pts',(46.3309366805112,53.518573654857,0.));
#166179=CARTESIAN_POINT('Ctrl Pts',(46.3309366805112,53.518573654857,12.));
#166180=CARTESIAN_POINT('Ctrl Pts',(46.3127495603117,53.5071881399932,0.));
#166181=CARTESIAN_POINT('Ctrl Pts',(46.3127495603117,53.5071881399932,12.));
#166182=CARTESIAN_POINT('Ctrl Pts',(46.2946155587428,53.4958097825019,0.));
#166183=CARTESIAN_POINT('Ctrl Pts',(46.2946155587428,53.4958097825019,12.));
#166184=CARTESIAN_POINT('Ctrl Pts',(46.2765347685198,53.4844387312414,0.));
#166185=CARTESIAN_POINT('Ctrl Pts',(46.2765347685198,53.4844387312414,12.));
#166186=CARTESIAN_POINT('Ctrl Pts',(46.2585072828343,53.4730751360359,0.));
#166187=CARTESIAN_POINT('Ctrl Pts',(46.2585072828343,53.4730751360359,12.));
#166188=CARTESIAN_POINT('Ctrl Pts',(46.2405331953872,53.4617191477382,0.));
#166189=CARTESIAN_POINT('Ctrl Pts',(46.2405331953872,53.4617191477382,12.));
#166190=CARTESIAN_POINT('Ctrl Pts',(46.2226126003185,53.4503709181158,0.));
#166191=CARTESIAN_POINT('Ctrl Pts',(46.2226126003185,53.4503709181158,12.));
#166192=CARTESIAN_POINT('Ctrl Pts',(46.2047455921276,53.4390305997263,0.));
#166193=CARTESIAN_POINT('Ctrl Pts',(46.2047455921276,53.4390305997263,12.));
#166194=CARTESIAN_POINT('Ctrl Pts',(46.1869322656027,53.4276983458129,0.));
#166195=CARTESIAN_POINT('Ctrl Pts',(46.1869322656027,53.4276983458129,12.));
#166196=CARTESIAN_POINT('Ctrl Pts',(46.1691727157149,53.4163743101535,0.));
#166197=CARTESIAN_POINT('Ctrl Pts',(46.1691727157149,53.4163743101535,12.));
#166198=CARTESIAN_POINT('Ctrl Pts',(46.1514670376035,53.4050586470463,0.));
#166199=CARTESIAN_POINT('Ctrl Pts',(46.1514670376035,53.4050586470463,12.));
#166200=CARTESIAN_POINT('Ctrl Pts',(46.1338153268116,53.3937515116572,0.));
#166201=CARTESIAN_POINT('Ctrl Pts',(46.1338153268116,53.3937515116572,12.));
#166202=CARTESIAN_POINT('Ctrl Pts',(46.1162176794891,53.3824530603284,0.));
#166203=CARTESIAN_POINT('Ctrl Pts',(46.1162176794891,53.3824530603284,12.));
#166204=CARTESIAN_POINT('Ctrl Pts',(46.0986741925646,53.3711634508426,0.));
#166205=CARTESIAN_POINT('Ctrl Pts',(46.0986741925646,53.3711634508426,12.));
#166206=CARTESIAN_POINT('Ctrl Pts',(46.0811849640195,53.3598828428519,0.));
#166207=CARTESIAN_POINT('Ctrl Pts',(46.0811849640195,53.3598828428519,12.));
#166208=CARTESIAN_POINT('Ctrl Pts',(46.0637500926954,53.3486113975868,0.));
#166209=CARTESIAN_POINT('Ctrl Pts',(46.0637500926954,53.3486113975868,12.));
#166210=CARTESIAN_POINT('Ctrl Pts',(46.046369677778,53.3373492770647,0.));
#166211=CARTESIAN_POINT('Ctrl Pts',(46.046369677778,53.3373492770647,12.));
#166212=CARTESIAN_POINT('Ctrl Pts',(46.0290438183598,53.3260966434277,0.));
#166213=CARTESIAN_POINT('Ctrl Pts',(46.0290438183598,53.3260966434277,12.));
#166214=CARTESIAN_POINT('Ctrl Pts',(46.0117726129893,53.3148536582658,0.));
#166215=CARTESIAN_POINT('Ctrl Pts',(46.0117726129893,53.3148536582658,12.));
#166216=CARTESIAN_POINT('Ctrl Pts',(45.9945561591486,53.3036204818367,0.));
#166217=CARTESIAN_POINT('Ctrl Pts',(45.9945561591486,53.3036204818367,12.));
#166218=CARTESIAN_POINT('Ctrl Pts',(45.9773945542415,53.2923972745585,0.));
#166219=CARTESIAN_POINT('Ctrl Pts',(45.9773945542415,53.2923972745585,12.));
#166220=CARTESIAN_POINT('Ctrl Pts',(45.9602878967714,53.2811841987945,0.));
#166221=CARTESIAN_POINT('Ctrl Pts',(45.9602878967714,53.2811841987945,12.));
#166222=CARTESIAN_POINT('Ctrl Pts',(45.9432362873001,53.2699814203097,0.));
#166223=CARTESIAN_POINT('Ctrl Pts',(45.9432362873001,53.2699814203097,12.));
#166224=CARTESIAN_POINT('Ctrl Pts',(45.9262398298323,53.2587891103835,0.));
#166225=CARTESIAN_POINT('Ctrl Pts',(45.9262398298323,53.2587891103835,12.));
#166226=CARTESIAN_POINT('Ctrl Pts',(45.9092986319343,53.2476074459977,0.));
#166227=CARTESIAN_POINT('Ctrl Pts',(45.9092986319343,53.2476074459977,12.));
#166228=CARTESIAN_POINT('Ctrl Pts',(45.8924128018354,53.2364366054276,0.));
#166229=CARTESIAN_POINT('Ctrl Pts',(45.8924128018354,53.2364366054276,12.));
#166230=CARTESIAN_POINT('Ctrl Pts',(45.8755824458715,53.2252767643652,0.));
#166231=CARTESIAN_POINT('Ctrl Pts',(45.8755824458715,53.2252767643652,12.));
#166232=CARTESIAN_POINT('Ctrl Pts',(45.8588076662598,53.2141280925458,0.));
#166233=CARTESIAN_POINT('Ctrl Pts',(45.8588076662598,53.2141280925458,12.));
#166234=CARTESIAN_POINT('Ctrl Pts',(45.8420885575386,53.2029907483602,0.));
#166235=CARTESIAN_POINT('Ctrl Pts',(45.8420885575386,53.2029907483602,12.));
#166236=CARTESIAN_POINT('Ctrl Pts',(45.8254252100003,53.1918648840598,0.));
#166237=CARTESIAN_POINT('Ctrl Pts',(45.8254252100003,53.1918648840598,12.));
#166238=CARTESIAN_POINT('Ctrl Pts',(45.8088177165124,53.1807506560977,0.));
#166239=CARTESIAN_POINT('Ctrl Pts',(45.8088177165124,53.1807506560977,12.));
#166240=CARTESIAN_POINT('Ctrl Pts',(45.7922661780005,53.1696482334487,0.));
#166241=CARTESIAN_POINT('Ctrl Pts',(45.7922661780005,53.1696482334487,12.));
#166242=CARTESIAN_POINT('Ctrl Pts',(45.7757707100568,53.158557807638,0.));
#166243=CARTESIAN_POINT('Ctrl Pts',(45.7757707100568,53.158557807638,12.));
#166244=CARTESIAN_POINT('Ctrl Pts',(45.7593314474412,53.147479599594,0.));
#166245=CARTESIAN_POINT('Ctrl Pts',(45.7593314474412,53.147479599594,12.));
#166246=CARTESIAN_POINT('Ctrl Pts',(45.7429485300727,53.136413838457,0.));
#166247=CARTESIAN_POINT('Ctrl Pts',(45.7429485300727,53.136413838457,12.));
#166248=CARTESIAN_POINT('Ctrl Pts',(45.7266220896951,53.1253607414806,0.));
#166249=CARTESIAN_POINT('Ctrl Pts',(45.7266220896951,53.1253607414806,12.));
#166250=CARTESIAN_POINT('Ctrl Pts',(45.7103522376744,53.1143204954981,0.));
#166251=CARTESIAN_POINT('Ctrl Pts',(45.7103522376744,53.1143204954981,12.));
#166252=CARTESIAN_POINT('Ctrl Pts',(45.6941390489239,53.1032932329074,0.));
#166253=CARTESIAN_POINT('Ctrl Pts',(45.6941390489239,53.1032932329074,12.));
#166254=CARTESIAN_POINT('Ctrl Pts',(45.6779825614486,53.0922790298736,0.));
#166255=CARTESIAN_POINT('Ctrl Pts',(45.6779825614486,53.0922790298736,12.));
#166256=CARTESIAN_POINT('Ctrl Pts',(45.6651027439479,53.083478145185,0.));
#166257=CARTESIAN_POINT('Ctrl Pts',(45.6651027439479,53.083478145185,12.));
#166258=CARTESIAN_POINT('Ctrl Pts',(45.6554684028296,53.0768833804386,0.));
#166259=CARTESIAN_POINT('Ctrl Pts',(45.6554684028296,53.0768833804386,12.));
#166260=CARTESIAN_POINT('Ctrl Pts',(45.6490568514146,53.0724894921921,0.));
#166261=CARTESIAN_POINT('Ctrl Pts',(45.6490568514146,53.0724894921921,12.));
#166262=CARTESIAN_POINT('Ctrl Pts',(45.6458539113724,53.0702932034641,0.));
#166263=CARTESIAN_POINT('Ctrl Pts',(45.6458539113724,53.0702932034641,12.));
#166264=CARTESIAN_POINT('',(45.6458539113724,53.0702932034641,12.));
#166265=CARTESIAN_POINT('Ctrl Pts',(45.6458539113724,53.0702932034641,12.));
#166266=CARTESIAN_POINT('Ctrl Pts',(45.6490568514146,53.0724894921921,12.));
#166267=CARTESIAN_POINT('Ctrl Pts',(45.6554684028296,53.0768833804386,12.));
#166268=CARTESIAN_POINT('Ctrl Pts',(45.6651027439479,53.083478145185,12.));
#166269=CARTESIAN_POINT('Ctrl Pts',(45.6779825614486,53.0922790298736,12.));
#166270=CARTESIAN_POINT('Ctrl Pts',(45.6941390489239,53.1032932329074,12.));
#166271=CARTESIAN_POINT('Ctrl Pts',(45.7103522376744,53.1143204954981,12.));
#166272=CARTESIAN_POINT('Ctrl Pts',(45.7266220896951,53.1253607414806,12.));
#166273=CARTESIAN_POINT('Ctrl Pts',(45.7429485300727,53.136413838457,12.));
#166274=CARTESIAN_POINT('Ctrl Pts',(45.7593314474412,53.147479599594,12.));
#166275=CARTESIAN_POINT('Ctrl Pts',(45.7757707100568,53.158557807638,12.));
#166276=CARTESIAN_POINT('Ctrl Pts',(45.7922661780005,53.1696482334487,12.));
#166277=CARTESIAN_POINT('Ctrl Pts',(45.8088177165124,53.1807506560977,12.));
#166278=CARTESIAN_POINT('Ctrl Pts',(45.8254252100003,53.1918648840598,12.));
#166279=CARTESIAN_POINT('Ctrl Pts',(45.8420885575386,53.2029907483602,12.));
#166280=CARTESIAN_POINT('Ctrl Pts',(45.8588076662598,53.2141280925458,12.));
#166281=CARTESIAN_POINT('Ctrl Pts',(45.8755824458715,53.2252767643652,12.));
#166282=CARTESIAN_POINT('Ctrl Pts',(45.8924128018354,53.2364366054276,12.));
#166283=CARTESIAN_POINT('Ctrl Pts',(45.9092986319343,53.2476074459977,12.));
#166284=CARTESIAN_POINT('Ctrl Pts',(45.9262398298323,53.2587891103835,12.));
#166285=CARTESIAN_POINT('Ctrl Pts',(45.9432362873001,53.2699814203097,12.));
#166286=CARTESIAN_POINT('Ctrl Pts',(45.9602878967714,53.2811841987945,12.));
#166287=CARTESIAN_POINT('Ctrl Pts',(45.9773945542415,53.2923972745585,12.));
#166288=CARTESIAN_POINT('Ctrl Pts',(45.9945561591486,53.3036204818367,12.));
#166289=CARTESIAN_POINT('Ctrl Pts',(46.0117726129893,53.3148536582658,12.));
#166290=CARTESIAN_POINT('Ctrl Pts',(46.0290438183598,53.3260966434277,12.));
#166291=CARTESIAN_POINT('Ctrl Pts',(46.046369677778,53.3373492770647,12.));
#166292=CARTESIAN_POINT('Ctrl Pts',(46.0637500926954,53.3486113975868,12.));
#166293=CARTESIAN_POINT('Ctrl Pts',(46.0811849640195,53.3598828428519,12.));
#166294=CARTESIAN_POINT('Ctrl Pts',(46.0986741925646,53.3711634508426,12.));
#166295=CARTESIAN_POINT('Ctrl Pts',(46.1162176794891,53.3824530603284,12.));
#166296=CARTESIAN_POINT('Ctrl Pts',(46.1338153268116,53.3937515116572,12.));
#166297=CARTESIAN_POINT('Ctrl Pts',(46.1514670376035,53.4050586470463,12.));
#166298=CARTESIAN_POINT('Ctrl Pts',(46.1691727157149,53.4163743101535,12.));
#166299=CARTESIAN_POINT('Ctrl Pts',(46.1869322656027,53.4276983458129,12.));
#166300=CARTESIAN_POINT('Ctrl Pts',(46.2047455921276,53.4390305997263,12.));
#166301=CARTESIAN_POINT('Ctrl Pts',(46.2226126003185,53.4503709181158,12.));
#166302=CARTESIAN_POINT('Ctrl Pts',(46.2405331953872,53.4617191477382,12.));
#166303=CARTESIAN_POINT('Ctrl Pts',(46.2585072828343,53.4730751360359,12.));
#166304=CARTESIAN_POINT('Ctrl Pts',(46.2765347685198,53.4844387312414,12.));
#166305=CARTESIAN_POINT('Ctrl Pts',(46.2946155587428,53.4958097825019,12.));
#166306=CARTESIAN_POINT('Ctrl Pts',(46.3127495603117,53.5071881399932,12.));
#166307=CARTESIAN_POINT('Ctrl Pts',(46.3309366805112,53.518573654857,12.));
#166308=CARTESIAN_POINT('Ctrl Pts',(46.3491768270664,53.5299661791396,12.));
#166309=CARTESIAN_POINT('Ctrl Pts',(46.3674699081043,53.5413655657323,12.));
#166310=CARTESIAN_POINT('Ctrl Pts',(46.3858158321044,53.552771668303,12.));
#166311=CARTESIAN_POINT('Ctrl Pts',(46.4042145078682,53.5641843412537,12.));
#166312=CARTESIAN_POINT('Ctrl Pts',(46.422665844546,53.5756034397464,12.));
#166313=CARTESIAN_POINT('Ctrl Pts',(46.4411697516474,53.5870288197161,12.));
#166314=CARTESIAN_POINT('Ctrl Pts',(46.4597261390526,53.5984603378862,12.));
#166315=CARTESIAN_POINT('Ctrl Pts',(46.4783349170182,53.6098978517869,12.));
#166316=CARTESIAN_POINT('Ctrl Pts',(46.4969959961779,53.6213412197542,12.));
#166317=CARTESIAN_POINT('Ctrl Pts',(46.5157092875377,53.6327903009098,12.));
#166318=CARTESIAN_POINT('Ctrl Pts',(46.5344747024677,53.6442449551455,12.));
#166319=CARTESIAN_POINT('Ctrl Pts',(46.5532921526899,53.6557050431069,12.));
#166320=CARTESIAN_POINT('Ctrl Pts',(46.5721615502589,53.6671704261735,12.));
#166321=CARTESIAN_POINT('Ctrl Pts',(46.5910828075652,53.678640966456,12.));
#166322=CARTESIAN_POINT('Ctrl Pts',(46.6100558373401,53.690116526794,12.));
#166323=CARTESIAN_POINT('Ctrl Pts',(46.6290805526559,53.7015969707541,12.));
#166324=CARTESIAN_POINT('Ctrl Pts',(46.6481568669217,53.7130821626262,12.));
#166325=CARTESIAN_POINT('Ctrl Pts',(46.6672846938752,53.7245719674221,12.));
#166326=CARTESIAN_POINT('Ctrl Pts',(46.6864639475862,53.7360662508675,12.));
#166327=CARTESIAN_POINT('Ctrl Pts',(46.7056945424559,53.7475648793946,12.));
#166328=CARTESIAN_POINT('Ctrl Pts',(46.7249763932129,53.7590677201342,12.));
#166329=CARTESIAN_POINT('Ctrl Pts',(46.7443094149045,53.7705746409076,12.));
#166330=CARTESIAN_POINT('Ctrl Pts',(46.763693522886,53.7820855102182,12.));
#166331=CARTESIAN_POINT('Ctrl Pts',(46.7831286328278,53.793600197248,12.));
#166332=CARTESIAN_POINT('Ctrl Pts',(46.802614660715,53.8051185718532,12.));
#166333=CARTESIAN_POINT('Ctrl Pts',(46.8221515228457,53.816640504558,12.));
#166334=CARTESIAN_POINT('Ctrl Pts',(46.841739135822,53.8281658665503,12.));
#166335=CARTESIAN_POINT('Ctrl Pts',(46.8613774165435,53.8396945296757,12.));
#166336=CARTESIAN_POINT('Ctrl Pts',(46.881066282213,53.8512263664321,12.));
#166337=CARTESIAN_POINT('Ctrl Pts',(46.9008056503351,53.8627612499638,12.));
#166338=CARTESIAN_POINT('Ctrl Pts',(46.9205954387133,53.8742990540563,12.));
#166339=CARTESIAN_POINT('Ctrl Pts',(46.94043556544,53.8858396531298,12.));
#166340=CARTESIAN_POINT('Ctrl Pts',(46.960325948892,53.8973829222348,12.));
#166341=CARTESIAN_POINT('Ctrl Pts',(46.9802665077366,53.9089287370463,12.));
#166342=CARTESIAN_POINT('Ctrl Pts',(47.0002571609297,53.9204769738596,12.));
#166343=CARTESIAN_POINT('Ctrl Pts',(47.0202978277138,53.9320275095853,12.));
#166344=CARTESIAN_POINT('Ctrl Pts',(47.0403884276071,53.9435802217436,12.));
#166345=CARTESIAN_POINT('Ctrl Pts',(47.0605288804008,53.95513498846,12.));
#166346=CARTESIAN_POINT('Ctrl Pts',(47.0807191061648,53.9666916884596,12.));
#166347=CARTESIAN_POINT('Ctrl Pts',(47.1009590252458,53.9782502010634,12.));
#166348=CARTESIAN_POINT('Ctrl Pts',(47.1212485582643,53.989810406182,12.));
#166349=CARTESIAN_POINT('Ctrl Pts',(47.1415876261035,54.0013721843118,12.));
#166350=CARTESIAN_POINT('Ctrl Pts',(47.1619761499087,54.0129354165297,12.));
#166351=CARTESIAN_POINT('Ctrl Pts',(47.1824140510926,54.0244999844893,12.));
#166352=CARTESIAN_POINT('Ctrl Pts',(47.202901251334,54.0360657704163,12.));
#166353=CARTESIAN_POINT('Ctrl Pts',(47.2234376725743,54.047632657104,12.));
#166354=CARTESIAN_POINT('Ctrl Pts',(47.2440232370065,54.0592005279086,12.));
#166355=CARTESIAN_POINT('Ctrl Pts',(47.2646578670746,54.0707692667438,12.));
#166356=CARTESIAN_POINT('Ctrl Pts',(47.2853414854793,54.0823387580776,12.));
#166357=CARTESIAN_POINT('Ctrl Pts',(47.3060740151752,54.0939088869269,12.));
#166358=CARTESIAN_POINT('Ctrl Pts',(47.3268553793694,54.1054795388543,12.));
#166359=CARTESIAN_POINT('Ctrl Pts',(47.3476855015102,54.1170505999645,12.));
#166360=CARTESIAN_POINT('Ctrl Pts',(47.3685643052874,54.1286219568989,12.));
#166361=CARTESIAN_POINT('Ctrl Pts',(47.3894917146365,54.1401934968311,12.));
#166362=CARTESIAN_POINT('Ctrl Pts',(47.4104676537381,54.1517651074637,12.));
#166363=CARTESIAN_POINT('Ctrl Pts',(47.4314920470141,54.1633366770239,12.));
#166364=CARTESIAN_POINT('Ctrl Pts',(47.4525648191173,54.1749080942593,12.));
#166365=CARTESIAN_POINT('Ctrl Pts',(47.4736858949322,54.1864792484345,12.));
#166366=CARTESIAN_POINT('Ctrl Pts',(47.4948551995801,54.198050029327,12.));
#166367=CARTESIAN_POINT('Ctrl Pts',(47.5160726584174,54.209620327223,12.));
#166368=CARTESIAN_POINT('Ctrl Pts',(47.5373381970326,54.2211900329138,12.));
#166369=CARTESIAN_POINT('Ctrl Pts',(47.5586517412363,54.2327590376924,12.));
#166370=CARTESIAN_POINT('Ctrl Pts',(47.5800132170608,54.244327233349,12.));
#166371=CARTESIAN_POINT('Ctrl Pts',(47.6014225507659,54.2558945121678,12.));
#166372=CARTESIAN_POINT('Ctrl Pts',(47.6228796688375,54.2674607669226,12.));
#166373=CARTESIAN_POINT('Ctrl Pts',(47.6443844979847,54.2790258908738,12.));
#166374=CARTESIAN_POINT('Ctrl Pts',(47.6659369651301,54.290589777765,12.));
#166375=CARTESIAN_POINT('Ctrl Pts',(47.6875369974087,54.302152321819,12.));
#166376=CARTESIAN_POINT('Ctrl Pts',(47.7091845221747,54.3137134177345,12.));
#166377=CARTESIAN_POINT('Ctrl Pts',(47.7308794669993,54.3252729606823,12.));
#166378=CARTESIAN_POINT('Ctrl Pts',(47.7526217596694,54.3368308463023,12.));
#166379=CARTESIAN_POINT('Ctrl Pts',(47.7744113281771,54.3483869707002,12.));
#166380=CARTESIAN_POINT('Ctrl Pts',(47.7962481007185,54.3599412304437,12.));
#166381=CARTESIAN_POINT('Ctrl Pts',(47.8181320056995,54.3714935225591,12.));
#166382=CARTESIAN_POINT('Ctrl Pts',(47.8400629717355,54.3830437445279,12.));
#166383=CARTESIAN_POINT('Ctrl Pts',(47.8620409276493,54.3945917942832,12.));
#166384=CARTESIAN_POINT('Ctrl Pts',(47.8840658024618,54.4061375702079,12.));
#166385=CARTESIAN_POINT('Ctrl Pts',(47.9061375253897,54.4176809711311,12.));
#166386=CARTESIAN_POINT('Ctrl Pts',(47.9282560258516,54.429221896324,12.));
#166387=CARTESIAN_POINT('Ctrl Pts',(47.9504212334675,54.4407602454967,12.));
#166388=CARTESIAN_POINT('Ctrl Pts',(47.9726330780572,54.4522959187955,12.));
#166389=CARTESIAN_POINT('Ctrl Pts',(47.9948914896326,54.4638288168003,12.));
#166390=CARTESIAN_POINT('Ctrl Pts',(48.0171963983924,54.4753588405215,12.));
#166391=CARTESIAN_POINT('Ctrl Pts',(48.0395477347298,54.4868858913971,12.));
#166392=CARTESIAN_POINT('Ctrl Pts',(48.0619454292324,54.4984098712886,12.));
#166393=CARTESIAN_POINT('Ctrl Pts',(48.0843894126806,54.5099306824786,12.));
#166394=CARTESIAN_POINT('Ctrl Pts',(48.1068796160405,54.5214482276678,12.));
#166395=CARTESIAN_POINT('Ctrl Pts',(48.1294159704573,54.5329624099721,12.));
#166396=CARTESIAN_POINT('Ctrl Pts',(48.1519984072622,54.5444731329201,12.));
#166397=CARTESIAN_POINT('Ctrl Pts',(48.1746268579736,54.5559803004492,12.));
#166398=CARTESIAN_POINT('Ctrl Pts',(48.1973012542966,54.5674838169041,12.));
#166399=CARTESIAN_POINT('Ctrl Pts',(48.2200215281173,54.5789835870342,12.));
#166400=CARTESIAN_POINT('Ctrl Pts',(48.2427876114947,54.5904795159926,12.));
#166401=CARTESIAN_POINT('Ctrl Pts',(48.2655994366665,54.6019715093309,12.));
#166402=CARTESIAN_POINT('Ctrl Pts',(48.2884569360506,54.6134594729959,12.));
#166403=CARTESIAN_POINT('Ctrl Pts',(48.3113600422443,54.6249433133261,12.));
#166404=CARTESIAN_POINT('Ctrl Pts',(48.3343086880194,54.6364229370494,12.));
#166405=CARTESIAN_POINT('Ctrl Pts',(48.3573028063124,54.6478982512794,12.));
#166406=CARTESIAN_POINT('Ctrl Pts',(48.3803423302294,54.6593691635145,12.));
#166407=CARTESIAN_POINT('Ctrl Pts',(48.4034271930514,54.6708355816358,12.));
#166408=CARTESIAN_POINT('Ctrl Pts',(48.426557328234,54.6822974139064,12.));
#166409=CARTESIAN_POINT('Ctrl Pts',(48.4497326694052,54.6937545689695,12.));
#166410=CARTESIAN_POINT('Ctrl Pts',(48.472953150357,54.7052069558497,12.));
#166411=CARTESIAN_POINT('Ctrl Pts',(48.4962187050457,54.716654483948,12.));
#166412=CARTESIAN_POINT('Ctrl Pts',(48.519529267596,54.7280970630351,12.));
#166413=CARTESIAN_POINT('Ctrl Pts',(48.5428847722977,54.7395346032453,12.));
#166414=CARTESIAN_POINT('Ctrl Pts',(48.5662851536026,54.7509670150714,12.));
#166415=CARTESIAN_POINT('Ctrl Pts',(48.5897303461125,54.7623942093586,12.));
#166416=CARTESIAN_POINT('Ctrl Pts',(48.6132202845783,54.7738160973031,12.));
#166417=CARTESIAN_POINT('Ctrl Pts',(48.6367549039112,54.7852325904583,12.));
#166418=CARTESIAN_POINT('Ctrl Pts',(48.6603341391886,54.796643600739,12.));
#166419=CARTESIAN_POINT('Ctrl Pts',(48.6839579256566,54.8080490404275,12.));
#166420=CARTESIAN_POINT('Ctrl Pts',(48.7076261987292,54.819448822181,12.));
#166421=CARTESIAN_POINT('Ctrl Pts',(48.7313388939845,54.8308428590344,12.));
#166422=CARTESIAN_POINT('Ctrl Pts',(48.7550959471601,54.8422310643763,12.));
#166423=CARTESIAN_POINT('Ctrl Pts',(48.7788972941438,54.8536133519292,12.));
#166424=CARTESIAN_POINT('Ctrl Pts',(48.8027428709614,54.8649896357285,12.));
#166425=CARTESIAN_POINT('Ctrl Pts',(48.8266326137622,54.8763598301037,12.));
#166426=CARTESIAN_POINT('Ctrl Pts',(48.8505664587974,54.8877238496566,12.));
#166427=CARTESIAN_POINT('Ctrl Pts',(48.8745443424477,54.8990816092953,12.));
#166428=CARTESIAN_POINT('Ctrl Pts',(48.8985662012528,54.9104330242742,12.));
#166429=CARTESIAN_POINT('Ctrl Pts',(48.9226319719368,54.9217780102355,12.));
#166430=CARTESIAN_POINT('Ctrl Pts',(48.9467415914269,54.9331164832424,12.));
#166431=CARTESIAN_POINT('Ctrl Pts',(48.9708949968795,54.9444483598378,12.));
#166432=CARTESIAN_POINT('Ctrl Pts',(48.9950921256526,54.9557735569943,12.));
#166433=CARTESIAN_POINT('Ctrl Pts',(49.0193329152479,54.9670919920029,12.));
#166434=CARTESIAN_POINT('Ctrl Pts',(49.0436173032528,54.9784035823766,12.));
#166435=CARTESIAN_POINT('Ctrl Pts',(49.067945227287,54.9897082457606,12.));
#166436=CARTESIAN_POINT('Ctrl Pts',(49.0923166249219,55.0010058998107,12.));
#166437=CARTESIAN_POINT('Ctrl Pts',(49.116731433673,55.012296462186,12.));
#166438=CARTESIAN_POINT('Ctrl Pts',(49.1411895911635,55.0235798508045,12.));
#166439=CARTESIAN_POINT('Ctrl Pts',(49.1656910352476,55.0348559840453,12.));
#166440=CARTESIAN_POINT('Ctrl Pts',(49.1902357041461,55.0461247809744,12.));
#166441=CARTESIAN_POINT('Ctrl Pts',(49.2148235365703,55.0573861615579,12.));
#166442=CARTESIAN_POINT('Ctrl Pts',(49.2394544718531,55.0686400468931,12.));
#166443=CARTESIAN_POINT('Ctrl Pts',(49.264128449652,55.079886358701,12.));
#166444=CARTESIAN_POINT('Ctrl Pts',(49.2888454096563,55.0911250188302,12.));
#166445=CARTESIAN_POINT('Ctrl Pts',(49.3136052912621,55.102355948714,12.));
#166446=CARTESIAN_POINT('Ctrl Pts',(49.3384080333155,55.1135790689464,12.));
#166447=CARTESIAN_POINT('Ctrl Pts',(49.3632535736715,55.1247942985619,12.));
#166448=CARTESIAN_POINT('Ctrl Pts',(49.3881418495489,55.1360015556221,12.));
#166449=CARTESIAN_POINT('Ctrl Pts',(49.4130727983201,55.1472007585183,12.));
#166450=CARTESIAN_POINT('Ctrl Pts',(49.4380463581965,55.1583918271116,12.));
#166451=CARTESIAN_POINT('Ctrl Pts',(49.4630624688793,55.1695746838174,12.));
#166452=CARTESIAN_POINT('Ctrl Pts',(49.4881210723966,55.1807492550119,12.));
#166453=CARTESIAN_POINT('Ctrl Pts',(49.5132221132992,55.1919154713647,12.));
#166454=CARTESIAN_POINT('Ctrl Pts',(49.5347748994759,55.2014798624093,12.));
#166455=CARTESIAN_POINT('Ctrl Pts',(49.551321852449,55.2088081099093,12.));
#166456=CARTESIAN_POINT('Ctrl Pts',(49.5628442142133,55.2139039604722,12.));
#166457=CARTESIAN_POINT('Ctrl Pts',(49.5693295981928,55.2167699151339,12.));
#166458=CARTESIAN_POINT('Ctrl Pts',(49.5707719660639,55.2174072001495,12.));
#166459=CARTESIAN_POINT('',(45.6458539113724,53.0702932034641,0.));
#166460=CARTESIAN_POINT('',(45.6458539113724,53.0702932034641,0.));
#166461=CARTESIAN_POINT('Ctrl Pts',(49.5707719660639,55.2174072001495,0.));
#166462=CARTESIAN_POINT('Ctrl Pts',(49.5693295981928,55.2167699151339,0.));
#166463=CARTESIAN_POINT('Ctrl Pts',(49.5628442142133,55.2139039604722,0.));
#166464=CARTESIAN_POINT('Ctrl Pts',(49.551321852449,55.2088081099093,0.));
#166465=CARTESIAN_POINT('Ctrl Pts',(49.5347748994759,55.2014798624093,0.));
#166466=CARTESIAN_POINT('Ctrl Pts',(49.5132221132992,55.1919154713647,0.));
#166467=CARTESIAN_POINT('Ctrl Pts',(49.4881210723966,55.1807492550119,0.));
#166468=CARTESIAN_POINT('Ctrl Pts',(49.4630624688793,55.1695746838174,0.));
#166469=CARTESIAN_POINT('Ctrl Pts',(49.4380463581965,55.1583918271116,0.));
#166470=CARTESIAN_POINT('Ctrl Pts',(49.4130727983201,55.1472007585183,0.));
#166471=CARTESIAN_POINT('Ctrl Pts',(49.3881418495489,55.1360015556221,0.));
#166472=CARTESIAN_POINT('Ctrl Pts',(49.3632535736715,55.1247942985619,0.));
#166473=CARTESIAN_POINT('Ctrl Pts',(49.3384080333155,55.1135790689464,0.));
#166474=CARTESIAN_POINT('Ctrl Pts',(49.3136052912621,55.102355948714,0.));
#166475=CARTESIAN_POINT('Ctrl Pts',(49.2888454096563,55.0911250188302,0.));
#166476=CARTESIAN_POINT('Ctrl Pts',(49.264128449652,55.079886358701,0.));
#166477=CARTESIAN_POINT('Ctrl Pts',(49.2394544718531,55.0686400468931,0.));
#166478=CARTESIAN_POINT('Ctrl Pts',(49.2148235365703,55.0573861615579,0.));
#166479=CARTESIAN_POINT('Ctrl Pts',(49.1902357041461,55.0461247809744,0.));
#166480=CARTESIAN_POINT('Ctrl Pts',(49.1656910352476,55.0348559840453,0.));
#166481=CARTESIAN_POINT('Ctrl Pts',(49.1411895911635,55.0235798508045,0.));
#166482=CARTESIAN_POINT('Ctrl Pts',(49.116731433673,55.012296462186,0.));
#166483=CARTESIAN_POINT('Ctrl Pts',(49.0923166249219,55.0010058998107,0.));
#166484=CARTESIAN_POINT('Ctrl Pts',(49.067945227287,54.9897082457606,0.));
#166485=CARTESIAN_POINT('Ctrl Pts',(49.0436173032528,54.9784035823766,0.));
#166486=CARTESIAN_POINT('Ctrl Pts',(49.0193329152479,54.9670919920029,0.));
#166487=CARTESIAN_POINT('Ctrl Pts',(48.9950921256526,54.9557735569943,0.));
#166488=CARTESIAN_POINT('Ctrl Pts',(48.9708949968795,54.9444483598378,0.));
#166489=CARTESIAN_POINT('Ctrl Pts',(48.9467415914269,54.9331164832424,0.));
#166490=CARTESIAN_POINT('Ctrl Pts',(48.9226319719368,54.9217780102355,0.));
#166491=CARTESIAN_POINT('Ctrl Pts',(48.8985662012528,54.9104330242742,0.));
#166492=CARTESIAN_POINT('Ctrl Pts',(48.8745443424477,54.8990816092953,0.));
#166493=CARTESIAN_POINT('Ctrl Pts',(48.8505664587974,54.8877238496566,0.));
#166494=CARTESIAN_POINT('Ctrl Pts',(48.8266326137622,54.8763598301037,0.));
#166495=CARTESIAN_POINT('Ctrl Pts',(48.8027428709614,54.8649896357285,0.));
#166496=CARTESIAN_POINT('Ctrl Pts',(48.7788972941438,54.8536133519292,0.));
#166497=CARTESIAN_POINT('Ctrl Pts',(48.7550959471601,54.8422310643763,0.));
#166498=CARTESIAN_POINT('Ctrl Pts',(48.7313388939845,54.8308428590344,0.));
#166499=CARTESIAN_POINT('Ctrl Pts',(48.7076261987292,54.819448822181,0.));
#166500=CARTESIAN_POINT('Ctrl Pts',(48.6839579256566,54.8080490404275,0.));
#166501=CARTESIAN_POINT('Ctrl Pts',(48.6603341391886,54.796643600739,0.));
#166502=CARTESIAN_POINT('Ctrl Pts',(48.6367549039112,54.7852325904583,0.));
#166503=CARTESIAN_POINT('Ctrl Pts',(48.6132202845783,54.7738160973031,0.));
#166504=CARTESIAN_POINT('Ctrl Pts',(48.5897303461125,54.7623942093586,0.));
#166505=CARTESIAN_POINT('Ctrl Pts',(48.5662851536026,54.7509670150714,0.));
#166506=CARTESIAN_POINT('Ctrl Pts',(48.5428847722977,54.7395346032453,0.));
#166507=CARTESIAN_POINT('Ctrl Pts',(48.519529267596,54.7280970630351,0.));
#166508=CARTESIAN_POINT('Ctrl Pts',(48.4962187050457,54.716654483948,0.));
#166509=CARTESIAN_POINT('Ctrl Pts',(48.472953150357,54.7052069558497,0.));
#166510=CARTESIAN_POINT('Ctrl Pts',(48.4497326694052,54.6937545689695,0.));
#166511=CARTESIAN_POINT('Ctrl Pts',(48.426557328234,54.6822974139064,0.));
#166512=CARTESIAN_POINT('Ctrl Pts',(48.4034271930514,54.6708355816358,0.));
#166513=CARTESIAN_POINT('Ctrl Pts',(48.3803423302294,54.6593691635145,0.));
#166514=CARTESIAN_POINT('Ctrl Pts',(48.3573028063124,54.6478982512794,0.));
#166515=CARTESIAN_POINT('Ctrl Pts',(48.3343086880194,54.6364229370494,0.));
#166516=CARTESIAN_POINT('Ctrl Pts',(48.3113600422443,54.6249433133261,0.));
#166517=CARTESIAN_POINT('Ctrl Pts',(48.2884569360506,54.6134594729959,0.));
#166518=CARTESIAN_POINT('Ctrl Pts',(48.2655994366665,54.6019715093309,0.));
#166519=CARTESIAN_POINT('Ctrl Pts',(48.2427876114947,54.5904795159926,0.));
#166520=CARTESIAN_POINT('Ctrl Pts',(48.2200215281173,54.5789835870342,0.));
#166521=CARTESIAN_POINT('Ctrl Pts',(48.1973012542966,54.5674838169041,0.));
#166522=CARTESIAN_POINT('Ctrl Pts',(48.1746268579736,54.5559803004492,0.));
#166523=CARTESIAN_POINT('Ctrl Pts',(48.1519984072622,54.5444731329201,0.));
#166524=CARTESIAN_POINT('Ctrl Pts',(48.1294159704573,54.5329624099721,0.));
#166525=CARTESIAN_POINT('Ctrl Pts',(48.1068796160405,54.5214482276678,0.));
#166526=CARTESIAN_POINT('Ctrl Pts',(48.0843894126806,54.5099306824786,0.));
#166527=CARTESIAN_POINT('Ctrl Pts',(48.0619454292324,54.4984098712886,0.));
#166528=CARTESIAN_POINT('Ctrl Pts',(48.0395477347298,54.4868858913971,0.));
#166529=CARTESIAN_POINT('Ctrl Pts',(48.0171963983924,54.4753588405215,0.));
#166530=CARTESIAN_POINT('Ctrl Pts',(47.9948914896326,54.4638288168003,0.));
#166531=CARTESIAN_POINT('Ctrl Pts',(47.9726330780572,54.4522959187955,0.));
#166532=CARTESIAN_POINT('Ctrl Pts',(47.9504212334675,54.4407602454967,0.));
#166533=CARTESIAN_POINT('Ctrl Pts',(47.9282560258516,54.429221896324,0.));
#166534=CARTESIAN_POINT('Ctrl Pts',(47.9061375253897,54.4176809711311,0.));
#166535=CARTESIAN_POINT('Ctrl Pts',(47.8840658024618,54.4061375702079,0.));
#166536=CARTESIAN_POINT('Ctrl Pts',(47.8620409276493,54.3945917942832,0.));
#166537=CARTESIAN_POINT('Ctrl Pts',(47.8400629717355,54.3830437445279,0.));
#166538=CARTESIAN_POINT('Ctrl Pts',(47.8181320056995,54.3714935225591,0.));
#166539=CARTESIAN_POINT('Ctrl Pts',(47.7962481007185,54.3599412304437,0.));
#166540=CARTESIAN_POINT('Ctrl Pts',(47.7744113281771,54.3483869707002,0.));
#166541=CARTESIAN_POINT('Ctrl Pts',(47.7526217596694,54.3368308463023,0.));
#166542=CARTESIAN_POINT('Ctrl Pts',(47.7308794669993,54.3252729606823,0.));
#166543=CARTESIAN_POINT('Ctrl Pts',(47.7091845221747,54.3137134177345,0.));
#166544=CARTESIAN_POINT('Ctrl Pts',(47.6875369974087,54.302152321819,0.));
#166545=CARTESIAN_POINT('Ctrl Pts',(47.6659369651301,54.290589777765,0.));
#166546=CARTESIAN_POINT('Ctrl Pts',(47.6443844979847,54.2790258908738,0.));
#166547=CARTESIAN_POINT('Ctrl Pts',(47.6228796688375,54.2674607669226,0.));
#166548=CARTESIAN_POINT('Ctrl Pts',(47.6014225507659,54.2558945121678,0.));
#166549=CARTESIAN_POINT('Ctrl Pts',(47.5800132170608,54.244327233349,0.));
#166550=CARTESIAN_POINT('Ctrl Pts',(47.5586517412363,54.2327590376924,0.));
#166551=CARTESIAN_POINT('Ctrl Pts',(47.5373381970326,54.2211900329138,0.));
#166552=CARTESIAN_POINT('Ctrl Pts',(47.5160726584174,54.209620327223,0.));
#166553=CARTESIAN_POINT('Ctrl Pts',(47.4948551995801,54.198050029327,0.));
#166554=CARTESIAN_POINT('Ctrl Pts',(47.4736858949322,54.1864792484345,0.));
#166555=CARTESIAN_POINT('Ctrl Pts',(47.4525648191173,54.1749080942593,0.));
#166556=CARTESIAN_POINT('Ctrl Pts',(47.4314920470141,54.1633366770239,0.));
#166557=CARTESIAN_POINT('Ctrl Pts',(47.4104676537381,54.1517651074637,0.));
#166558=CARTESIAN_POINT('Ctrl Pts',(47.3894917146365,54.1401934968311,0.));
#166559=CARTESIAN_POINT('Ctrl Pts',(47.3685643052874,54.1286219568989,0.));
#166560=CARTESIAN_POINT('Ctrl Pts',(47.3476855015102,54.1170505999645,0.));
#166561=CARTESIAN_POINT('Ctrl Pts',(47.3268553793694,54.1054795388543,0.));
#166562=CARTESIAN_POINT('Ctrl Pts',(47.3060740151752,54.0939088869269,0.));
#166563=CARTESIAN_POINT('Ctrl Pts',(47.2853414854793,54.0823387580776,0.));
#166564=CARTESIAN_POINT('Ctrl Pts',(47.2646578670746,54.0707692667438,0.));
#166565=CARTESIAN_POINT('Ctrl Pts',(47.2440232370065,54.0592005279086,0.));
#166566=CARTESIAN_POINT('Ctrl Pts',(47.2234376725743,54.047632657104,0.));
#166567=CARTESIAN_POINT('Ctrl Pts',(47.202901251334,54.0360657704163,0.));
#166568=CARTESIAN_POINT('Ctrl Pts',(47.1824140510926,54.0244999844893,0.));
#166569=CARTESIAN_POINT('Ctrl Pts',(47.1619761499087,54.0129354165297,0.));
#166570=CARTESIAN_POINT('Ctrl Pts',(47.1415876261035,54.0013721843118,0.));
#166571=CARTESIAN_POINT('Ctrl Pts',(47.1212485582643,53.989810406182,0.));
#166572=CARTESIAN_POINT('Ctrl Pts',(47.1009590252458,53.9782502010634,0.));
#166573=CARTESIAN_POINT('Ctrl Pts',(47.0807191061648,53.9666916884596,0.));
#166574=CARTESIAN_POINT('Ctrl Pts',(47.0605288804008,53.95513498846,0.));
#166575=CARTESIAN_POINT('Ctrl Pts',(47.0403884276071,53.9435802217436,0.));
#166576=CARTESIAN_POINT('Ctrl Pts',(47.0202978277138,53.9320275095853,0.));
#166577=CARTESIAN_POINT('Ctrl Pts',(47.0002571609297,53.9204769738596,0.));
#166578=CARTESIAN_POINT('Ctrl Pts',(46.9802665077366,53.9089287370463,0.));
#166579=CARTESIAN_POINT('Ctrl Pts',(46.960325948892,53.8973829222348,0.));
#166580=CARTESIAN_POINT('Ctrl Pts',(46.94043556544,53.8858396531298,0.));
#166581=CARTESIAN_POINT('Ctrl Pts',(46.9205954387133,53.8742990540563,0.));
#166582=CARTESIAN_POINT('Ctrl Pts',(46.9008056503351,53.8627612499638,0.));
#166583=CARTESIAN_POINT('Ctrl Pts',(46.881066282213,53.8512263664321,0.));
#166584=CARTESIAN_POINT('Ctrl Pts',(46.8613774165435,53.8396945296757,0.));
#166585=CARTESIAN_POINT('Ctrl Pts',(46.841739135822,53.8281658665503,0.));
#166586=CARTESIAN_POINT('Ctrl Pts',(46.8221515228457,53.816640504558,0.));
#166587=CARTESIAN_POINT('Ctrl Pts',(46.802614660715,53.8051185718532,0.));
#166588=CARTESIAN_POINT('Ctrl Pts',(46.7831286328278,53.793600197248,0.));
#166589=CARTESIAN_POINT('Ctrl Pts',(46.763693522886,53.7820855102182,0.));
#166590=CARTESIAN_POINT('Ctrl Pts',(46.7443094149045,53.7705746409076,0.));
#166591=CARTESIAN_POINT('Ctrl Pts',(46.7249763932129,53.7590677201342,0.));
#166592=CARTESIAN_POINT('Ctrl Pts',(46.7056945424559,53.7475648793946,0.));
#166593=CARTESIAN_POINT('Ctrl Pts',(46.6864639475862,53.7360662508675,0.));
#166594=CARTESIAN_POINT('Ctrl Pts',(46.6672846938752,53.7245719674221,0.));
#166595=CARTESIAN_POINT('Ctrl Pts',(46.6481568669217,53.7130821626262,0.));
#166596=CARTESIAN_POINT('Ctrl Pts',(46.6290805526559,53.7015969707541,0.));
#166597=CARTESIAN_POINT('Ctrl Pts',(46.6100558373401,53.690116526794,0.));
#166598=CARTESIAN_POINT('Ctrl Pts',(46.5910828075652,53.678640966456,0.));
#166599=CARTESIAN_POINT('Ctrl Pts',(46.5721615502589,53.6671704261735,0.));
#166600=CARTESIAN_POINT('Ctrl Pts',(46.5532921526899,53.6557050431069,0.));
#166601=CARTESIAN_POINT('Ctrl Pts',(46.5344747024677,53.6442449551455,0.));
#166602=CARTESIAN_POINT('Ctrl Pts',(46.5157092875377,53.6327903009098,0.));
#166603=CARTESIAN_POINT('Ctrl Pts',(46.4969959961779,53.6213412197542,0.));
#166604=CARTESIAN_POINT('Ctrl Pts',(46.4783349170182,53.6098978517869,0.));
#166605=CARTESIAN_POINT('Ctrl Pts',(46.4597261390526,53.5984603378862,0.));
#166606=CARTESIAN_POINT('Ctrl Pts',(46.4411697516474,53.5870288197161,0.));
#166607=CARTESIAN_POINT('Ctrl Pts',(46.422665844546,53.5756034397464,0.));
#166608=CARTESIAN_POINT('Ctrl Pts',(46.4042145078682,53.5641843412537,0.));
#166609=CARTESIAN_POINT('Ctrl Pts',(46.3858158321044,53.552771668303,0.));
#166610=CARTESIAN_POINT('Ctrl Pts',(46.3674699081043,53.5413655657323,0.));
#166611=CARTESIAN_POINT('Ctrl Pts',(46.3491768270664,53.5299661791396,0.));
#166612=CARTESIAN_POINT('Ctrl Pts',(46.3309366805112,53.518573654857,0.));
#166613=CARTESIAN_POINT('Ctrl Pts',(46.3127495603117,53.5071881399932,0.));
#166614=CARTESIAN_POINT('Ctrl Pts',(46.2946155587428,53.4958097825019,0.));
#166615=CARTESIAN_POINT('Ctrl Pts',(46.2765347685198,53.4844387312414,0.));
#166616=CARTESIAN_POINT('Ctrl Pts',(46.2585072828343,53.4730751360359,0.));
#166617=CARTESIAN_POINT('Ctrl Pts',(46.2405331953872,53.4617191477382,0.));
#166618=CARTESIAN_POINT('Ctrl Pts',(46.2226126003185,53.4503709181158,0.));
#166619=CARTESIAN_POINT('Ctrl Pts',(46.2047455921276,53.4390305997263,0.));
#166620=CARTESIAN_POINT('Ctrl Pts',(46.1869322656027,53.4276983458129,0.));
#166621=CARTESIAN_POINT('Ctrl Pts',(46.1691727157149,53.4163743101535,0.));
#166622=CARTESIAN_POINT('Ctrl Pts',(46.1514670376035,53.4050586470463,0.));
#166623=CARTESIAN_POINT('Ctrl Pts',(46.1338153268116,53.3937515116572,0.));
#166624=CARTESIAN_POINT('Ctrl Pts',(46.1162176794891,53.3824530603284,0.));
#166625=CARTESIAN_POINT('Ctrl Pts',(46.0986741925646,53.3711634508426,0.));
#166626=CARTESIAN_POINT('Ctrl Pts',(46.0811849640195,53.3598828428519,0.));
#166627=CARTESIAN_POINT('Ctrl Pts',(46.0637500926954,53.3486113975868,0.));
#166628=CARTESIAN_POINT('Ctrl Pts',(46.046369677778,53.3373492770647,0.));
#166629=CARTESIAN_POINT('Ctrl Pts',(46.0290438183598,53.3260966434277,0.));
#166630=CARTESIAN_POINT('Ctrl Pts',(46.0117726129893,53.3148536582658,0.));
#166631=CARTESIAN_POINT('Ctrl Pts',(45.9945561591486,53.3036204818367,0.));
#166632=CARTESIAN_POINT('Ctrl Pts',(45.9773945542415,53.2923972745585,0.));
#166633=CARTESIAN_POINT('Ctrl Pts',(45.9602878967714,53.2811841987945,0.));
#166634=CARTESIAN_POINT('Ctrl Pts',(45.9432362873001,53.2699814203097,0.));
#166635=CARTESIAN_POINT('Ctrl Pts',(45.9262398298323,53.2587891103835,0.));
#166636=CARTESIAN_POINT('Ctrl Pts',(45.9092986319343,53.2476074459977,0.));
#166637=CARTESIAN_POINT('Ctrl Pts',(45.8924128018354,53.2364366054276,0.));
#166638=CARTESIAN_POINT('Ctrl Pts',(45.8755824458715,53.2252767643652,0.));
#166639=CARTESIAN_POINT('Ctrl Pts',(45.8588076662598,53.2141280925458,0.));
#166640=CARTESIAN_POINT('Ctrl Pts',(45.8420885575386,53.2029907483602,0.));
#166641=CARTESIAN_POINT('Ctrl Pts',(45.8254252100003,53.1918648840598,0.));
#166642=CARTESIAN_POINT('Ctrl Pts',(45.8088177165124,53.1807506560977,0.));
#166643=CARTESIAN_POINT('Ctrl Pts',(45.7922661780005,53.1696482334487,0.));
#166644=CARTESIAN_POINT('Ctrl Pts',(45.7757707100568,53.158557807638,0.));
#166645=CARTESIAN_POINT('Ctrl Pts',(45.7593314474412,53.147479599594,0.));
#166646=CARTESIAN_POINT('Ctrl Pts',(45.7429485300727,53.136413838457,0.));
#166647=CARTESIAN_POINT('Ctrl Pts',(45.7266220896951,53.1253607414806,0.));
#166648=CARTESIAN_POINT('Ctrl Pts',(45.7103522376744,53.1143204954981,0.));
#166649=CARTESIAN_POINT('Ctrl Pts',(45.6941390489239,53.1032932329074,0.));
#166650=CARTESIAN_POINT('Ctrl Pts',(45.6779825614486,53.0922790298736,0.));
#166651=CARTESIAN_POINT('Ctrl Pts',(45.6651027439479,53.083478145185,0.));
#166652=CARTESIAN_POINT('Ctrl Pts',(45.6554684028296,53.0768833804386,0.));
#166653=CARTESIAN_POINT('Ctrl Pts',(45.6490568514146,53.0724894921921,0.));
#166654=CARTESIAN_POINT('Ctrl Pts',(45.6458539113724,53.0702932034641,0.));
#166655=CARTESIAN_POINT('Ctrl Pts',(54.5031396718592,50.7903314215393,0.));
#166656=CARTESIAN_POINT('Ctrl Pts',(54.5031396718592,50.7903314215393,12.));
#166657=CARTESIAN_POINT('Ctrl Pts',(54.4978248630387,50.7885805844281,0.));
#166658=CARTESIAN_POINT('Ctrl Pts',(54.4978248630387,50.7885805844281,12.));
#166659=CARTESIAN_POINT('Ctrl Pts',(54.4871993224832,50.7850776288814,0.));
#166660=CARTESIAN_POINT('Ctrl Pts',(54.4871993224832,50.7850776288814,12.));
#166661=CARTESIAN_POINT('Ctrl Pts',(54.4712732429066,50.7798193515888,0.));
#166662=CARTESIAN_POINT('Ctrl Pts',(54.4712732429066,50.7798193515888,12.));
#166663=CARTESIAN_POINT('Ctrl Pts',(54.4500629336429,50.7728006269349,0.));
#166664=CARTESIAN_POINT('Ctrl Pts',(54.4500629336429,50.7728006269349,12.));
#166665=CARTESIAN_POINT('Ctrl Pts',(54.423590828767,50.764014409002,0.));
#166666=CARTESIAN_POINT('Ctrl Pts',(54.423590828767,50.764014409002,12.));
#166667=CARTESIAN_POINT('Ctrl Pts',(54.3971595231574,50.7552153869475,0.));
#166668=CARTESIAN_POINT('Ctrl Pts',(54.3971595231574,50.7552153869475,12.));
#166669=CARTESIAN_POINT('Ctrl Pts',(54.3707690445749,50.7464035792906,0.));
#166670=CARTESIAN_POINT('Ctrl Pts',(54.3707690445749,50.7464035792906,12.));
#166671=CARTESIAN_POINT('Ctrl Pts',(54.3444194324054,50.7375790185896,0.));
#166672=CARTESIAN_POINT('Ctrl Pts',(54.3444194324054,50.7375790185896,12.));
#166673=CARTESIAN_POINT('Ctrl Pts',(54.3181107400663,50.7287417566123,0.));
#166674=CARTESIAN_POINT('Ctrl Pts',(54.3181107400663,50.7287417566123,12.));
#166675=CARTESIAN_POINT('Ctrl Pts',(54.2918430335206,50.7198918629451,0.));
#166676=CARTESIAN_POINT('Ctrl Pts',(54.2918430335206,50.7198918629451,12.));
#166677=CARTESIAN_POINT('Ctrl Pts',(54.2656163868104,50.7110294185698,0.));
#166678=CARTESIAN_POINT('Ctrl Pts',(54.2656163868104,50.7110294185698,12.));
#166679=CARTESIAN_POINT('Ctrl Pts',(54.2394308784026,50.7021545108311,0.));
#166680=CARTESIAN_POINT('Ctrl Pts',(54.2394308784026,50.7021545108311,12.));
#166681=CARTESIAN_POINT('Ctrl Pts',(54.2132865872985,50.6932672279772,0.));
#166682=CARTESIAN_POINT('Ctrl Pts',(54.2132865872985,50.6932672279772,12.));
#166683=CARTESIAN_POINT('Ctrl Pts',(54.1871835889981,50.6843676535492,0.));
#166684=CARTESIAN_POINT('Ctrl Pts',(54.1871835889981,50.6843676535492,12.));
#166685=CARTESIAN_POINT('Ctrl Pts',(54.1611219522394,50.67545586183,0.));
#166686=CARTESIAN_POINT('Ctrl Pts',(54.1611219522394,50.67545586183,12.));
#166687=CARTESIAN_POINT('Ctrl Pts',(54.1351017412804,50.6665319209869,0.));
#166688=CARTESIAN_POINT('Ctrl Pts',(54.1351017412804,50.6665319209869,12.));
#166689=CARTESIAN_POINT('Ctrl Pts',(54.1091230175367,50.6575958953221,0.));
#166690=CARTESIAN_POINT('Ctrl Pts',(54.1091230175367,50.6575958953221,12.));
#166691=CARTESIAN_POINT('Ctrl Pts',(54.0831858415189,50.6486478479465,0.));
#166692=CARTESIAN_POINT('Ctrl Pts',(54.0831858415189,50.6486478479465,12.));
#166693=CARTESIAN_POINT('Ctrl Pts',(54.0572902745076,50.6396878430939,0.));
#166694=CARTESIAN_POINT('Ctrl Pts',(54.0572902745076,50.6396878430939,12.));
#166695=CARTESIAN_POINT('Ctrl Pts',(54.0314363806708,50.6307159490553,0.));
#166696=CARTESIAN_POINT('Ctrl Pts',(54.0314363806708,50.6307159490553,12.));
#166697=CARTESIAN_POINT('Ctrl Pts',(54.0056242268399,50.6217322378648,0.));
#166698=CARTESIAN_POINT('Ctrl Pts',(54.0056242268399,50.6217322378648,12.));
#166699=CARTESIAN_POINT('Ctrl Pts',(53.979853881553,50.6127367839711,0.));
#166700=CARTESIAN_POINT('Ctrl Pts',(53.979853881553,50.6127367839711,12.));
#166701=CARTESIAN_POINT('Ctrl Pts',(53.9541254143119,50.603729663214,0.));
#166702=CARTESIAN_POINT('Ctrl Pts',(53.9541254143119,50.603729663214,12.));
#166703=CARTESIAN_POINT('Ctrl Pts',(53.9284388948004,50.5947109517483,0.));
#166704=CARTESIAN_POINT('Ctrl Pts',(53.9284388948004,50.5947109517483,12.));
#166705=CARTESIAN_POINT('Ctrl Pts',(53.9027943919836,50.5856807248151,0.));
#166706=CARTESIAN_POINT('Ctrl Pts',(53.9027943919836,50.5856807248151,12.));
#166707=CARTESIAN_POINT('Ctrl Pts',(53.8771919737032,50.5766390561884,0.));
#166708=CARTESIAN_POINT('Ctrl Pts',(53.8771919737032,50.5766390561884,12.));
#166709=CARTESIAN_POINT('Ctrl Pts',(53.8516317071804,50.5675860188538,0.));
#166710=CARTESIAN_POINT('Ctrl Pts',(53.8516317071804,50.5675860188538,12.));
#166711=CARTESIAN_POINT('Ctrl Pts',(53.8261136593075,50.5585216854091,0.));
#166712=CARTESIAN_POINT('Ctrl Pts',(53.8261136593075,50.5585216854091,12.));
#166713=CARTESIAN_POINT('Ctrl Pts',(53.8006378970197,50.5494461285761,0.));
#166714=CARTESIAN_POINT('Ctrl Pts',(53.8006378970197,50.5494461285761,12.));
#166715=CARTESIAN_POINT('Ctrl Pts',(53.7752044876304,50.5403594216698,0.));
#166716=CARTESIAN_POINT('Ctrl Pts',(53.7752044876304,50.5403594216698,12.));
#166717=CARTESIAN_POINT('Ctrl Pts',(53.7498134991703,50.5312616390779,0.));
#166718=CARTESIAN_POINT('Ctrl Pts',(53.7498134991703,50.5312616390779,12.));
#166719=CARTESIAN_POINT('Ctrl Pts',(53.7244650002374,50.522152856042,0.));
#166720=CARTESIAN_POINT('Ctrl Pts',(53.7244650002374,50.522152856042,12.));
#166721=CARTESIAN_POINT('Ctrl Pts',(53.6991590598548,50.513033148456,0.));
#166722=CARTESIAN_POINT('Ctrl Pts',(53.6991590598548,50.513033148456,12.));
#166723=CARTESIAN_POINT('Ctrl Pts',(53.6738957473158,50.503902592653,0.));
#166724=CARTESIAN_POINT('Ctrl Pts',(53.6738957473158,50.503902592653,12.));
#166725=CARTESIAN_POINT('Ctrl Pts',(53.6486751320436,50.4947612652149,0.));
#166726=CARTESIAN_POINT('Ctrl Pts',(53.6486751320436,50.4947612652149,12.));
#166727=CARTESIAN_POINT('Ctrl Pts',(53.623497283406,50.4856092427314,0.));
#166728=CARTESIAN_POINT('Ctrl Pts',(53.623497283406,50.4856092427314,12.));
#166729=CARTESIAN_POINT('Ctrl Pts',(53.5983622707238,50.4764466018071,0.));
#166730=CARTESIAN_POINT('Ctrl Pts',(53.5983622707238,50.4764466018071,12.));
#166731=CARTESIAN_POINT('Ctrl Pts',(53.5732701633609,50.4672734191756,0.));
#166732=CARTESIAN_POINT('Ctrl Pts',(53.5732701633609,50.4672734191756,12.));
#166733=CARTESIAN_POINT('Ctrl Pts',(53.5482210307868,50.4580897717838,0.));
#166734=CARTESIAN_POINT('Ctrl Pts',(53.5482210307868,50.4580897717838,12.));
#166735=CARTESIAN_POINT('Ctrl Pts',(53.5232149426413,50.4488957368839,0.));
#166736=CARTESIAN_POINT('Ctrl Pts',(53.5232149426413,50.4488957368839,12.));
#166737=CARTESIAN_POINT('Ctrl Pts',(53.4982519688024,50.4396913921382,0.));
#166738=CARTESIAN_POINT('Ctrl Pts',(53.4982519688024,50.4396913921382,12.));
#166739=CARTESIAN_POINT('Ctrl Pts',(53.4733321794188,50.4304768156667,0.));
#166740=CARTESIAN_POINT('Ctrl Pts',(53.4733321794188,50.4304768156667,12.));
#166741=CARTESIAN_POINT('Ctrl Pts',(53.4484556448776,50.4212520859914,0.));
#166742=CARTESIAN_POINT('Ctrl Pts',(53.4484556448776,50.4212520859914,12.));
#166743=CARTESIAN_POINT('Ctrl Pts',(53.4236224357838,50.4120172820047,0.));
#166744=CARTESIAN_POINT('Ctrl Pts',(53.4236224357838,50.4120172820047,12.));
#166745=CARTESIAN_POINT('Ctrl Pts',(53.398832622931,50.4027724829297,0.));
#166746=CARTESIAN_POINT('Ctrl Pts',(53.398832622931,50.4027724829297,12.));
#166747=CARTESIAN_POINT('Ctrl Pts',(53.3740862772681,50.3935177682837,0.));
#166748=CARTESIAN_POINT('Ctrl Pts',(53.3740862772681,50.3935177682837,12.));
#166749=CARTESIAN_POINT('Ctrl Pts',(53.3493834698697,50.384253217846,0.));
#166750=CARTESIAN_POINT('Ctrl Pts',(53.3493834698697,50.384253217846,12.));
#166751=CARTESIAN_POINT('Ctrl Pts',(53.3247242719587,50.3749789116786,0.));
#166752=CARTESIAN_POINT('Ctrl Pts',(53.3247242719587,50.3749789116786,12.));
#166753=CARTESIAN_POINT('Ctrl Pts',(53.300108754923,50.365694930143,0.));
#166754=CARTESIAN_POINT('Ctrl Pts',(53.300108754923,50.365694930143,12.));
#166755=CARTESIAN_POINT('Ctrl Pts',(53.2755369903293,50.3564013539199,0.));
#166756=CARTESIAN_POINT('Ctrl Pts',(53.2755369903293,50.3564013539199,12.));
#166757=CARTESIAN_POINT('Ctrl Pts',(53.2510090499336,50.3470982640289,0.));
#166758=CARTESIAN_POINT('Ctrl Pts',(53.2510090499336,50.3470982640289,12.));
#166759=CARTESIAN_POINT('Ctrl Pts',(53.2265250056887,50.3377857418515,0.));
#166760=CARTESIAN_POINT('Ctrl Pts',(53.2265250056887,50.3377857418515,12.));
#166761=CARTESIAN_POINT('Ctrl Pts',(53.2020849297471,50.3284638691278,0.));
#166762=CARTESIAN_POINT('Ctrl Pts',(53.2020849297471,50.3284638691278,12.));
#166763=CARTESIAN_POINT('Ctrl Pts',(53.1776888944616,50.3191327279493,0.));
#166764=CARTESIAN_POINT('Ctrl Pts',(53.1776888944616,50.3191327279493,12.));
#166765=CARTESIAN_POINT('Ctrl Pts',(53.1533369723818,50.3097924007534,0.));
#166766=CARTESIAN_POINT('Ctrl Pts',(53.1533369723818,50.3097924007534,12.));
#166767=CARTESIAN_POINT('Ctrl Pts',(53.1290292362485,50.300442970319,0.));
#166768=CARTESIAN_POINT('Ctrl Pts',(53.1290292362485,50.300442970319,12.));
#166769=CARTESIAN_POINT('Ctrl Pts',(53.1047657589812,50.2910845197619,0.));
#166770=CARTESIAN_POINT('Ctrl Pts',(53.1047657589812,50.2910845197619,12.));
#166771=CARTESIAN_POINT('Ctrl Pts',(53.0805466136798,50.2817171325358,0.));
#166772=CARTESIAN_POINT('Ctrl Pts',(53.0805466136798,50.2817171325358,12.));
#166773=CARTESIAN_POINT('Ctrl Pts',(53.0563718736366,50.2723408924373,0.));
#166774=CARTESIAN_POINT('Ctrl Pts',(53.0563718736366,50.2723408924373,12.));
#166775=CARTESIAN_POINT('Ctrl Pts',(53.0322416123406,50.2629558836111,0.));
#166776=CARTESIAN_POINT('Ctrl Pts',(53.0322416123406,50.2629558836111,12.));
#166777=CARTESIAN_POINT('Ctrl Pts',(53.0081559034801,50.2535621905552,0.));
#166778=CARTESIAN_POINT('Ctrl Pts',(53.0081559034801,50.2535621905552,12.));
#166779=CARTESIAN_POINT('Ctrl Pts',(52.9841148209402,50.2441598981286,0.));
#166780=CARTESIAN_POINT('Ctrl Pts',(52.9841148209402,50.2441598981286,12.));
#166781=CARTESIAN_POINT('Ctrl Pts',(52.9601184388028,50.2347490915555,0.));
#166782=CARTESIAN_POINT('Ctrl Pts',(52.9601184388028,50.2347490915555,12.));
#166783=CARTESIAN_POINT('Ctrl Pts',(52.9361668313542,50.2253298564241,0.));
#166784=CARTESIAN_POINT('Ctrl Pts',(52.9361668313542,50.2253298564241,12.));
#166785=CARTESIAN_POINT('Ctrl Pts',(52.9122600730884,50.2159022786879,0.));
#166786=CARTESIAN_POINT('Ctrl Pts',(52.9122600730884,50.2159022786879,12.));
#166787=CARTESIAN_POINT('Ctrl Pts',(52.8883982387068,50.2064664446663,0.));
#166788=CARTESIAN_POINT('Ctrl Pts',(52.8883982387068,50.2064664446663,12.));
#166789=CARTESIAN_POINT('Ctrl Pts',(52.8645814031133,50.1970224410471,0.));
#166790=CARTESIAN_POINT('Ctrl Pts',(52.8645814031133,50.1970224410471,12.));
#166791=CARTESIAN_POINT('Ctrl Pts',(52.8408096414093,50.1875703548884,0.));
#166792=CARTESIAN_POINT('Ctrl Pts',(52.8408096414093,50.1875703548884,12.));
#166793=CARTESIAN_POINT('Ctrl Pts',(52.8170830289044,50.1781102736205,0.));
#166794=CARTESIAN_POINT('Ctrl Pts',(52.8170830289044,50.1781102736205,12.));
#166795=CARTESIAN_POINT('Ctrl Pts',(52.7934016411205,50.1686422850488,0.));
#166796=CARTESIAN_POINT('Ctrl Pts',(52.7934016411205,50.1686422850488,12.));
#166797=CARTESIAN_POINT('Ctrl Pts',(52.769765553794,50.1591664773561,0.));
#166798=CARTESIAN_POINT('Ctrl Pts',(52.769765553794,50.1591664773561,12.));
#166799=CARTESIAN_POINT('Ctrl Pts',(52.7461748428738,50.1496829391073,0.));
#166800=CARTESIAN_POINT('Ctrl Pts',(52.7461748428738,50.1496829391073,12.));
#166801=CARTESIAN_POINT('Ctrl Pts',(52.7226295845161,50.1401917592537,0.));
#166802=CARTESIAN_POINT('Ctrl Pts',(52.7226295845161,50.1401917592537,12.));
#166803=CARTESIAN_POINT('Ctrl Pts',(52.699129855093,50.1306930271345,0.));
#166804=CARTESIAN_POINT('Ctrl Pts',(52.699129855093,50.1306930271345,12.));
#166805=CARTESIAN_POINT('Ctrl Pts',(52.6756757311978,50.1211868324781,0.));
#166806=CARTESIAN_POINT('Ctrl Pts',(52.6756757311978,50.1211868324781,12.));
#166807=CARTESIAN_POINT('Ctrl Pts',(52.652267289646,50.111673265404,0.));
#166808=CARTESIAN_POINT('Ctrl Pts',(52.652267289646,50.111673265404,12.));
#166809=CARTESIAN_POINT('Ctrl Pts',(52.6289046074746,50.1021524164264,0.));
#166810=CARTESIAN_POINT('Ctrl Pts',(52.6289046074746,50.1021524164264,12.));
#166811=CARTESIAN_POINT('Ctrl Pts',(52.6055877619348,50.0926243764578,0.));
#166812=CARTESIAN_POINT('Ctrl Pts',(52.6055877619348,50.0926243764578,12.));
#166813=CARTESIAN_POINT('Ctrl Pts',(52.5823168304994,50.0830892368107,0.));
#166814=CARTESIAN_POINT('Ctrl Pts',(52.5823168304994,50.0830892368107,12.));
#166815=CARTESIAN_POINT('Ctrl Pts',(52.5590918908702,50.0735470892007,0.));
#166816=CARTESIAN_POINT('Ctrl Pts',(52.5590918908702,50.0735470892007,12.));
#166817=CARTESIAN_POINT('Ctrl Pts',(52.5359130209792,50.0639980257479,0.));
#166818=CARTESIAN_POINT('Ctrl Pts',(52.5359130209792,50.0639980257479,12.));
#166819=CARTESIAN_POINT('Ctrl Pts',(52.5127802989896,50.0544421389818,0.));
#166820=CARTESIAN_POINT('Ctrl Pts',(52.5127802989896,50.0544421389818,12.));
#166821=CARTESIAN_POINT('Ctrl Pts',(52.4896938032884,50.0448795218441,0.));
#166822=CARTESIAN_POINT('Ctrl Pts',(52.4896938032884,50.0448795218441,12.));
#166823=CARTESIAN_POINT('Ctrl Pts',(52.4666536124913,50.0353102676921,0.));
#166824=CARTESIAN_POINT('Ctrl Pts',(52.4666536124913,50.0353102676921,12.));
#166825=CARTESIAN_POINT('Ctrl Pts',(52.4436598054515,50.0257344703,0.));
#166826=CARTESIAN_POINT('Ctrl Pts',(52.4436598054515,50.0257344703,12.));
#166827=CARTESIAN_POINT('Ctrl Pts',(52.4207124612608,50.0161522238616,0.));
#166828=CARTESIAN_POINT('Ctrl Pts',(52.4207124612608,50.0161522238616,12.));
#166829=CARTESIAN_POINT('Ctrl Pts',(52.3978116592509,50.0065636229938,0.));
#166830=CARTESIAN_POINT('Ctrl Pts',(52.3978116592509,50.0065636229938,12.));
#166831=CARTESIAN_POINT('Ctrl Pts',(52.3749574789871,49.9969687627408,0.));
#166832=CARTESIAN_POINT('Ctrl Pts',(52.3749574789871,49.9969687627408,12.));
#166833=CARTESIAN_POINT('Ctrl Pts',(52.3521500002718,49.9873677385775,0.));
#166834=CARTESIAN_POINT('Ctrl Pts',(52.3521500002718,49.9873677385775,12.));
#166835=CARTESIAN_POINT('Ctrl Pts',(52.3293893031528,49.9777606464106,0.));
#166836=CARTESIAN_POINT('Ctrl Pts',(52.3293893031528,49.9777606464106,12.));
#166837=CARTESIAN_POINT('Ctrl Pts',(52.3066754679265,49.9681475825824,0.));
#166838=CARTESIAN_POINT('Ctrl Pts',(52.3066754679265,49.9681475825824,12.));
#166839=CARTESIAN_POINT('Ctrl Pts',(52.2840085751384,49.9585286438733,0.));
#166840=CARTESIAN_POINT('Ctrl Pts',(52.2840085751384,49.9585286438733,12.));
#166841=CARTESIAN_POINT('Ctrl Pts',(52.2613887055773,49.9489039275064,0.));
#166842=CARTESIAN_POINT('Ctrl Pts',(52.2613887055773,49.9489039275064,12.));
#166843=CARTESIAN_POINT('Ctrl Pts',(52.2388159402771,49.9392735311509,0.));
#166844=CARTESIAN_POINT('Ctrl Pts',(52.2388159402771,49.9392735311509,12.));
#166845=CARTESIAN_POINT('Ctrl Pts',(52.2162903605275,49.9296375529245,0.));
#166846=CARTESIAN_POINT('Ctrl Pts',(52.2162903605275,49.9296375529245,12.));
#166847=CARTESIAN_POINT('Ctrl Pts',(52.1938120478754,49.9199960913962,0.));
#166848=CARTESIAN_POINT('Ctrl Pts',(52.1938120478754,49.9199960913962,12.));
#166849=CARTESIAN_POINT('Ctrl Pts',(52.1713810841276,49.9103492455902,0.));
#166850=CARTESIAN_POINT('Ctrl Pts',(52.1713810841276,49.9103492455902,12.));
#166851=CARTESIAN_POINT('Ctrl Pts',(52.1489975513445,49.9006971149895,0.));
#166852=CARTESIAN_POINT('Ctrl Pts',(52.1489975513445,49.9006971149895,12.));
#166853=CARTESIAN_POINT('Ctrl Pts',(52.1266615318407,49.8910397995397,0.));
#166854=CARTESIAN_POINT('Ctrl Pts',(52.1266615318407,49.8910397995397,12.));
#166855=CARTESIAN_POINT('Ctrl Pts',(52.1043731081962,49.8813773996517,0.));
#166856=CARTESIAN_POINT('Ctrl Pts',(52.1043731081962,49.8813773996517,12.));
#166857=CARTESIAN_POINT('Ctrl Pts',(52.0821323632587,49.8717100162048,0.));
#166858=CARTESIAN_POINT('Ctrl Pts',(52.0821323632587,49.8717100162048,12.));
#166859=CARTESIAN_POINT('Ctrl Pts',(52.0599393801452,49.86203775055,0.));
#166860=CARTESIAN_POINT('Ctrl Pts',(52.0599393801452,49.86203775055,12.));
#166861=CARTESIAN_POINT('Ctrl Pts',(52.0377942422376,49.8523607045149,0.));
#166862=CARTESIAN_POINT('Ctrl Pts',(52.0377942422376,49.8523607045149,12.));
#166863=CARTESIAN_POINT('Ctrl Pts',(52.0156970331823,49.8426789804071,0.));
#166864=CARTESIAN_POINT('Ctrl Pts',(52.0156970331823,49.8426789804071,12.));
#166865=CARTESIAN_POINT('Ctrl Pts',(51.9936478369008,49.8329926810172,0.));
#166866=CARTESIAN_POINT('Ctrl Pts',(51.9936478369008,49.8329926810172,12.));
#166867=CARTESIAN_POINT('Ctrl Pts',(51.9716467375937,49.8233019096222,0.));
#166868=CARTESIAN_POINT('Ctrl Pts',(51.9716467375937,49.8233019096222,12.));
#166869=CARTESIAN_POINT('Ctrl Pts',(51.9496938197418,49.8136067699896,0.));
#166870=CARTESIAN_POINT('Ctrl Pts',(51.9496938197418,49.8136067699896,12.));
#166871=CARTESIAN_POINT('Ctrl Pts',(51.9277891681018,49.8039073663812,0.));
#166872=CARTESIAN_POINT('Ctrl Pts',(51.9277891681018,49.8039073663812,12.));
#166873=CARTESIAN_POINT('Ctrl Pts',(51.9059328677059,49.7942038035576,0.));
#166874=CARTESIAN_POINT('Ctrl Pts',(51.9059328677059,49.7942038035576,12.));
#166875=CARTESIAN_POINT('Ctrl Pts',(51.8841250038724,49.7844961867808,0.));
#166876=CARTESIAN_POINT('Ctrl Pts',(51.8841250038724,49.7844961867808,12.));
#166877=CARTESIAN_POINT('Ctrl Pts',(51.8623656622097,49.7747846218182,0.));
#166878=CARTESIAN_POINT('Ctrl Pts',(51.8623656622097,49.7747846218182,12.));
#166879=CARTESIAN_POINT('Ctrl Pts',(51.8406549286175,49.7650692149462,0.));
#166880=CARTESIAN_POINT('Ctrl Pts',(51.8406549286175,49.7650692149462,12.));
#166881=CARTESIAN_POINT('Ctrl Pts',(51.8189928892828,49.755350072955,0.));
#166882=CARTESIAN_POINT('Ctrl Pts',(51.8189928892828,49.755350072955,12.));
#166883=CARTESIAN_POINT('Ctrl Pts',(51.7973796306803,49.7456273031534,0.));
#166884=CARTESIAN_POINT('Ctrl Pts',(51.7973796306803,49.7456273031534,12.));
#166885=CARTESIAN_POINT('Ctrl Pts',(51.7758152395836,49.7359010133721,0.));
#166886=CARTESIAN_POINT('Ctrl Pts',(51.7758152395836,49.7359010133721,12.));
#166887=CARTESIAN_POINT('Ctrl Pts',(51.754299803067,49.7261713119663,0.));
#166888=CARTESIAN_POINT('Ctrl Pts',(51.754299803067,49.7261713119663,12.));
#166889=CARTESIAN_POINT('Ctrl Pts',(51.7328334085091,49.7164383078212,0.));
#166890=CARTESIAN_POINT('Ctrl Pts',(51.7328334085091,49.7164383078212,12.));
#166891=CARTESIAN_POINT('Ctrl Pts',(51.7114161435869,49.7067021103553,0.));
#166892=CARTESIAN_POINT('Ctrl Pts',(51.7114161435869,49.7067021103553,12.));
#166893=CARTESIAN_POINT('Ctrl Pts',(51.6900480962773,49.6969628295262,0.));
#166894=CARTESIAN_POINT('Ctrl Pts',(51.6900480962773,49.6969628295262,12.));
#166895=CARTESIAN_POINT('Ctrl Pts',(51.6687293548682,49.6872205758336,0.));
#166896=CARTESIAN_POINT('Ctrl Pts',(51.6687293548682,49.6872205758336,12.));
#166897=CARTESIAN_POINT('Ctrl Pts',(51.6474600079622,49.6774754603245,0.));
#166898=CARTESIAN_POINT('Ctrl Pts',(51.6474600079622,49.6774754603245,12.));
#166899=CARTESIAN_POINT('Ctrl Pts',(51.626240144479,49.6677275945967,0.));
#166900=CARTESIAN_POINT('Ctrl Pts',(51.626240144479,49.6677275945967,12.));
#166901=CARTESIAN_POINT('Ctrl Pts',(51.6050698536496,49.6579770908037,0.));
#166902=CARTESIAN_POINT('Ctrl Pts',(51.6050698536496,49.6579770908037,12.));
#166903=CARTESIAN_POINT('Ctrl Pts',(51.5839492250181,49.6482240616593,0.));
#166904=CARTESIAN_POINT('Ctrl Pts',(51.5839492250181,49.6482240616593,12.));
#166905=CARTESIAN_POINT('Ctrl Pts',(51.5628783484525,49.6384686204413,0.));
#166906=CARTESIAN_POINT('Ctrl Pts',(51.5628783484525,49.6384686204413,12.));
#166907=CARTESIAN_POINT('Ctrl Pts',(51.5418573141484,49.6287108809966,0.));
#166908=CARTESIAN_POINT('Ctrl Pts',(51.5418573141484,49.6287108809966,12.));
#166909=CARTESIAN_POINT('Ctrl Pts',(51.5208862126315,49.6189509577452,0.));
#166910=CARTESIAN_POINT('Ctrl Pts',(51.5208862126315,49.6189509577452,12.));
#166911=CARTESIAN_POINT('Ctrl Pts',(51.4999651347523,49.6091889656866,0.));
#166912=CARTESIAN_POINT('Ctrl Pts',(51.4999651347523,49.6091889656866,12.));
#166913=CARTESIAN_POINT('Ctrl Pts',(51.4790941716888,49.5994250204031,0.));
#166914=CARTESIAN_POINT('Ctrl Pts',(51.4790941716888,49.5994250204031,12.));
#166915=CARTESIAN_POINT('Ctrl Pts',(51.4582734149583,49.5896592380654,0.));
#166916=CARTESIAN_POINT('Ctrl Pts',(51.4582734149583,49.5896592380654,12.));
#166917=CARTESIAN_POINT('Ctrl Pts',(51.4375029564197,49.5798917354366,0.));
#166918=CARTESIAN_POINT('Ctrl Pts',(51.4375029564197,49.5798917354366,12.));
#166919=CARTESIAN_POINT('Ctrl Pts',(51.4167828882756,49.5701226298769,0.));
#166920=CARTESIAN_POINT('Ctrl Pts',(51.4167828882756,49.5701226298769,12.));
#166921=CARTESIAN_POINT('Ctrl Pts',(51.396113303067,49.5603520393496,0.));
#166922=CARTESIAN_POINT('Ctrl Pts',(51.396113303067,49.5603520393496,12.));
#166923=CARTESIAN_POINT('Ctrl Pts',(51.3754942936778,49.550580082425,0.));
#166924=CARTESIAN_POINT('Ctrl Pts',(51.3754942936778,49.550580082425,12.));
#166925=CARTESIAN_POINT('Ctrl Pts',(51.3549259533458,49.5408068782859,0.));
#166926=CARTESIAN_POINT('Ctrl Pts',(51.3549259533458,49.5408068782859,12.));
#166927=CARTESIAN_POINT('Ctrl Pts',(51.3344083756657,49.5310325467332,0.));
#166928=CARTESIAN_POINT('Ctrl Pts',(51.3344083756657,49.5310325467332,12.));
#166929=CARTESIAN_POINT('Ctrl Pts',(51.313941654591,49.5212572081908,0.));
#166930=CARTESIAN_POINT('Ctrl Pts',(51.313941654591,49.5212572081908,12.));
#166931=CARTESIAN_POINT('Ctrl Pts',(51.2935258844289,49.5114809837122,0.));
#166932=CARTESIAN_POINT('Ctrl Pts',(51.2935258844289,49.5114809837122,12.));
#166933=CARTESIAN_POINT('Ctrl Pts',(51.2731611598475,49.5017039949852,0.));
#166934=CARTESIAN_POINT('Ctrl Pts',(51.2731611598475,49.5017039949852,12.));
#166935=CARTESIAN_POINT('Ctrl Pts',(51.2528475758846,49.4919263643362,0.));
#166936=CARTESIAN_POINT('Ctrl Pts',(51.2528475758846,49.4919263643362,12.));
#166937=CARTESIAN_POINT('Ctrl Pts',(51.2325852279506,49.4821482147356,0.));
#166938=CARTESIAN_POINT('Ctrl Pts',(51.2325852279506,49.4821482147356,12.));
#166939=CARTESIAN_POINT('Ctrl Pts',(51.2123742118287,49.4723696698021,0.));
#166940=CARTESIAN_POINT('Ctrl Pts',(51.2123742118287,49.4723696698021,12.));
#166941=CARTESIAN_POINT('Ctrl Pts',(51.1922146236686,49.4625908538074,0.));
#166942=CARTESIAN_POINT('Ctrl Pts',(51.1922146236686,49.4625908538074,12.));
#166943=CARTESIAN_POINT('Ctrl Pts',(51.1721065599973,49.4528118916832,0.));
#166944=CARTESIAN_POINT('Ctrl Pts',(51.1721065599973,49.4528118916832,12.));
#166945=CARTESIAN_POINT('Ctrl Pts',(51.1520501177291,49.4430329090287,0.));
#166946=CARTESIAN_POINT('Ctrl Pts',(51.1520501177291,49.4430329090287,12.));
#166947=CARTESIAN_POINT('Ctrl Pts',(51.1320453941702,49.4332540321178,0.));
#166948=CARTESIAN_POINT('Ctrl Pts',(51.1320453941702,49.4332540321178,12.));
#166949=CARTESIAN_POINT('Ctrl Pts',(51.1120924870195,49.423475387907,0.));
#166950=CARTESIAN_POINT('Ctrl Pts',(51.1120924870195,49.423475387907,12.));
#166951=CARTESIAN_POINT('Ctrl Pts',(51.0921914943662,49.4136971040428,0.));
#166952=CARTESIAN_POINT('Ctrl Pts',(51.0921914943662,49.4136971040428,12.));
#166953=CARTESIAN_POINT('Ctrl Pts',(51.0723425146985,49.4039193088634,0.));
#166954=CARTESIAN_POINT('Ctrl Pts',(51.0723425146985,49.4039193088634,12.));
#166955=CARTESIAN_POINT('Ctrl Pts',(51.052545646907,49.3941421314013,0.));
#166956=CARTESIAN_POINT('Ctrl Pts',(51.052545646907,49.3941421314013,12.));
#166957=CARTESIAN_POINT('Ctrl Pts',(51.0328009902858,49.3843657013852,0.));
#166958=CARTESIAN_POINT('Ctrl Pts',(51.0328009902858,49.3843657013852,12.));
#166959=CARTESIAN_POINT('Ctrl Pts',(51.0131086445272,49.3745901492432,0.));
#166960=CARTESIAN_POINT('Ctrl Pts',(51.0131086445272,49.3745901492432,12.));
#166961=CARTESIAN_POINT('Ctrl Pts',(50.9934687097188,49.3648156061058,0.));
#166962=CARTESIAN_POINT('Ctrl Pts',(50.9934687097188,49.3648156061058,12.));
#166963=CARTESIAN_POINT('Ctrl Pts',(50.9738812863646,49.355042203823,0.));
#166964=CARTESIAN_POINT('Ctrl Pts',(50.9738812863646,49.355042203823,12.));
#166965=CARTESIAN_POINT('Ctrl Pts',(50.9543464753981,49.345270074981,0.));
#166966=CARTESIAN_POINT('Ctrl Pts',(50.9543464753981,49.345270074981,12.));
#166967=CARTESIAN_POINT('Ctrl Pts',(50.9348643781924,49.3354993529159,0.));
#166968=CARTESIAN_POINT('Ctrl Pts',(50.9348643781924,49.3354993529159,12.));
#166969=CARTESIAN_POINT('Ctrl Pts',(50.9154350965666,49.3257301717335,0.));
#166970=CARTESIAN_POINT('Ctrl Pts',(50.9154350965666,49.3257301717335,12.));
#166971=CARTESIAN_POINT('Ctrl Pts',(50.8960587327848,49.3159626663109,0.));
#166972=CARTESIAN_POINT('Ctrl Pts',(50.8960587327848,49.3159626663109,12.));
#166973=CARTESIAN_POINT('Ctrl Pts',(50.8767353895492,49.3061969722781,0.));
#166974=CARTESIAN_POINT('Ctrl Pts',(50.8767353895492,49.3061969722781,12.));
#166975=CARTESIAN_POINT('Ctrl Pts',(50.8574651699873,49.2964332260039,0.));
#166976=CARTESIAN_POINT('Ctrl Pts',(50.8574651699873,49.2964332260039,12.));
#166977=CARTESIAN_POINT('Ctrl Pts',(50.8382481776403,49.2866715645838,0.));
#166978=CARTESIAN_POINT('Ctrl Pts',(50.8382481776403,49.2866715645838,12.));
#166979=CARTESIAN_POINT('Ctrl Pts',(50.819084516434,49.2769121258164,0.));
#166980=CARTESIAN_POINT('Ctrl Pts',(50.819084516434,49.2769121258164,12.));
#166981=CARTESIAN_POINT('Ctrl Pts',(50.7999742907131,49.2671550482435,0.));
#166982=CARTESIAN_POINT('Ctrl Pts',(50.7999742907131,49.2671550482435,12.));
#166983=CARTESIAN_POINT('Ctrl Pts',(50.7809176052966,49.2574004712134,0.));
#166984=CARTESIAN_POINT('Ctrl Pts',(50.7809176052966,49.2574004712134,12.));
#166985=CARTESIAN_POINT('Ctrl Pts',(50.7619145655207,49.2476485349373,0.));
#166986=CARTESIAN_POINT('Ctrl Pts',(50.7619145655207,49.2476485349373,12.));
#166987=CARTESIAN_POINT('Ctrl Pts',(50.7429652772805,49.2378993805471,0.));
#166988=CARTESIAN_POINT('Ctrl Pts',(50.7429652772805,49.2378993805471,12.));
#166989=CARTESIAN_POINT('Ctrl Pts',(50.7240698470679,49.228153150155,0.));
#166990=CARTESIAN_POINT('Ctrl Pts',(50.7240698470679,49.228153150155,12.));
#166991=CARTESIAN_POINT('Ctrl Pts',(50.7052283818922,49.2184099867461,0.));
#166992=CARTESIAN_POINT('Ctrl Pts',(50.7052283818922,49.2184099867461,12.));
#166993=CARTESIAN_POINT('Ctrl Pts',(50.6864409891895,49.2086700340614,0.));
#166994=CARTESIAN_POINT('Ctrl Pts',(50.6864409891895,49.2086700340614,12.));
#166995=CARTESIAN_POINT('Ctrl Pts',(50.6677077767432,49.1989334364996,0.));
#166996=CARTESIAN_POINT('Ctrl Pts',(50.6677077767432,49.1989334364996,12.));
#166997=CARTESIAN_POINT('Ctrl Pts',(50.6490288525656,49.189200338976,0.));
#166998=CARTESIAN_POINT('Ctrl Pts',(50.6490288525656,49.189200338976,12.));
#166999=CARTESIAN_POINT('Ctrl Pts',(50.6304043248821,49.1794708869099,0.));
#167000=CARTESIAN_POINT('Ctrl Pts',(50.6304043248821,49.1794708869099,12.));
#167001=CARTESIAN_POINT('Ctrl Pts',(50.6118343023958,49.1697452265494,0.));
#167002=CARTESIAN_POINT('Ctrl Pts',(50.6118343023958,49.1697452265494,12.));
#167003=CARTESIAN_POINT('Ctrl Pts',(50.5933188945168,49.1600235052621,0.));
#167004=CARTESIAN_POINT('Ctrl Pts',(50.5933188945168,49.1600235052621,12.));
#167005=CARTESIAN_POINT('Ctrl Pts',(50.5748582115565,49.1503058717821,0.));
#167006=CARTESIAN_POINT('Ctrl Pts',(50.5748582115565,49.1503058717821,12.));
#167007=CARTESIAN_POINT('Ctrl Pts',(50.556452365038,49.1405924766144,0.));
#167008=CARTESIAN_POINT('Ctrl Pts',(50.556452365038,49.1405924766144,12.));
#167009=CARTESIAN_POINT('Ctrl Pts',(50.5381014674791,49.1308834717615,0.));
#167010=CARTESIAN_POINT('Ctrl Pts',(50.5381014674791,49.1308834717615,12.));
#167011=CARTESIAN_POINT('Ctrl Pts',(50.5198056318089,49.1211790099795,0.));
#167012=CARTESIAN_POINT('Ctrl Pts',(50.5198056318089,49.1211790099795,12.));
#167013=CARTESIAN_POINT('Ctrl Pts',(50.501564970874,49.1114792441571,0.));
#167014=CARTESIAN_POINT('Ctrl Pts',(50.501564970874,49.1114792441571,12.));
#167015=CARTESIAN_POINT('Ctrl Pts',(50.4833795969318,49.1017843266803,0.));
#167016=CARTESIAN_POINT('Ctrl Pts',(50.4833795969318,49.1017843266803,12.));
#167017=CARTESIAN_POINT('Ctrl Pts',(50.4652496210607,49.0920944087008,0.));
#167018=CARTESIAN_POINT('Ctrl Pts',(50.4652496210607,49.0920944087008,12.));
#167019=CARTESIAN_POINT('Ctrl Pts',(50.4471751542751,49.0824096415371,0.));
#167020=CARTESIAN_POINT('Ctrl Pts',(50.4471751542751,49.0824096415371,12.));
#167021=CARTESIAN_POINT('Ctrl Pts',(50.4291563088547,49.0727301783494,0.));
#167022=CARTESIAN_POINT('Ctrl Pts',(50.4291563088547,49.0727301783494,12.));
#167023=CARTESIAN_POINT('Ctrl Pts',(50.4111931994257,49.0630561755075,0.));
#167024=CARTESIAN_POINT('Ctrl Pts',(50.4111931994257,49.0630561755075,12.));
#167025=CARTESIAN_POINT('Ctrl Pts',(50.3932859445252,49.0533877945744,0.));
#167026=CARTESIAN_POINT('Ctrl Pts',(50.3932859445252,49.0533877945744,12.));
#167027=CARTESIAN_POINT('Ctrl Pts',(50.3754346667353,49.0437252024832,0.));
#167028=CARTESIAN_POINT('Ctrl Pts',(50.3754346667353,49.0437252024832,12.));
#167029=CARTESIAN_POINT('Ctrl Pts',(50.3576394894108,49.0340685673982,0.));
#167030=CARTESIAN_POINT('Ctrl Pts',(50.3576394894108,49.0340685673982,12.));
#167031=CARTESIAN_POINT('Ctrl Pts',(50.3399005337958,49.024418055075,0.));
#167032=CARTESIAN_POINT('Ctrl Pts',(50.3399005337958,49.024418055075,12.));
#167033=CARTESIAN_POINT('Ctrl Pts',(50.3222179165119,49.0147738256942,0.));
#167034=CARTESIAN_POINT('Ctrl Pts',(50.3222179165119,49.0147738256942,12.));
#167035=CARTESIAN_POINT('Ctrl Pts',(50.3045917455424,49.0051360288044,0.));
#167036=CARTESIAN_POINT('Ctrl Pts',(50.3045917455424,49.0051360288044,12.));
#167037=CARTESIAN_POINT('Ctrl Pts',(50.2870221241054,48.9955048082081,0.));
#167038=CARTESIAN_POINT('Ctrl Pts',(50.2870221241054,48.9955048082081,12.));
#167039=CARTESIAN_POINT('Ctrl Pts',(50.2695091583511,48.9858803116689,0.));
#167040=CARTESIAN_POINT('Ctrl Pts',(50.2695091583511,48.9858803116689,12.));
#167041=CARTESIAN_POINT('Ctrl Pts',(50.252052963548,48.9762626987227,0.));
#167042=CARTESIAN_POINT('Ctrl Pts',(50.252052963548,48.9762626987227,12.));
#167043=CARTESIAN_POINT('Ctrl Pts',(50.234653671541,48.9666521500911,0.));
#167044=CARTESIAN_POINT('Ctrl Pts',(50.234653671541,48.9666521500911,12.));
#167045=CARTESIAN_POINT('Ctrl Pts',(50.2173114358325,48.9570488741167,0.));
#167046=CARTESIAN_POINT('Ctrl Pts',(50.2173114358325,48.9570488741167,12.));
#167047=CARTESIAN_POINT('Ctrl Pts',(50.2000264157797,48.9474530868733,0.));
#167048=CARTESIAN_POINT('Ctrl Pts',(50.2000264157797,48.9474530868733,12.));
#167049=CARTESIAN_POINT('Ctrl Pts',(50.1827987615602,48.9378649933055,0.));
#167050=CARTESIAN_POINT('Ctrl Pts',(50.1827987615602,48.9378649933055,12.));
#167051=CARTESIAN_POINT('Ctrl Pts',(50.1656286003997,48.9282847698294,0.));
#167052=CARTESIAN_POINT('Ctrl Pts',(50.1656286003997,48.9282847698294,12.));
#167053=CARTESIAN_POINT('Ctrl Pts',(50.1485160184657,48.9187125418099,0.));
#167054=CARTESIAN_POINT('Ctrl Pts',(50.1485160184657,48.9187125418099,12.));
#167055=CARTESIAN_POINT('Ctrl Pts',(50.1314610602569,48.90914838181,0.));
#167056=CARTESIAN_POINT('Ctrl Pts',(50.1314610602569,48.90914838181,12.));
#167057=CARTESIAN_POINT('Ctrl Pts',(50.1178632067084,48.9015035372055,0.));
#167058=CARTESIAN_POINT('Ctrl Pts',(50.1178632067084,48.9015035372055,12.));
#167059=CARTESIAN_POINT('Ctrl Pts',(50.1076907555471,48.895773555686,0.));
#167060=CARTESIAN_POINT('Ctrl Pts',(50.1076907555471,48.895773555686,12.));
#167061=CARTESIAN_POINT('Ctrl Pts',(50.1009206494272,48.8919551910366,0.));
#167062=CARTESIAN_POINT('Ctrl Pts',(50.1009206494272,48.8919551910366,12.));
#167063=CARTESIAN_POINT('Ctrl Pts',(50.0975384783635,48.8900464144686,0.));
#167064=CARTESIAN_POINT('Ctrl Pts',(50.0975384783635,48.8900464144686,12.));
#167065=CARTESIAN_POINT('',(50.0975384783635,48.8900464144686,12.));
#167066=CARTESIAN_POINT('Ctrl Pts',(50.0975384783635,48.8900464144686,12.));
#167067=CARTESIAN_POINT('Ctrl Pts',(50.1009206494272,48.8919551910366,12.));
#167068=CARTESIAN_POINT('Ctrl Pts',(50.1076907555471,48.895773555686,12.));
#167069=CARTESIAN_POINT('Ctrl Pts',(50.1178632067084,48.9015035372055,12.));
#167070=CARTESIAN_POINT('Ctrl Pts',(50.1314610602569,48.90914838181,12.));
#167071=CARTESIAN_POINT('Ctrl Pts',(50.1485160184657,48.9187125418099,12.));
#167072=CARTESIAN_POINT('Ctrl Pts',(50.1656286003997,48.9282847698294,12.));
#167073=CARTESIAN_POINT('Ctrl Pts',(50.1827987615602,48.9378649933055,12.));
#167074=CARTESIAN_POINT('Ctrl Pts',(50.2000264157797,48.9474530868733,12.));
#167075=CARTESIAN_POINT('Ctrl Pts',(50.2173114358325,48.9570488741167,12.));
#167076=CARTESIAN_POINT('Ctrl Pts',(50.234653671541,48.9666521500911,12.));
#167077=CARTESIAN_POINT('Ctrl Pts',(50.252052963548,48.9762626987227,12.));
#167078=CARTESIAN_POINT('Ctrl Pts',(50.2695091583511,48.9858803116689,12.));
#167079=CARTESIAN_POINT('Ctrl Pts',(50.2870221241054,48.9955048082081,12.));
#167080=CARTESIAN_POINT('Ctrl Pts',(50.3045917455424,49.0051360288044,12.));
#167081=CARTESIAN_POINT('Ctrl Pts',(50.3222179165119,49.0147738256942,12.));
#167082=CARTESIAN_POINT('Ctrl Pts',(50.3399005337958,49.024418055075,12.));
#167083=CARTESIAN_POINT('Ctrl Pts',(50.3576394894108,49.0340685673982,12.));
#167084=CARTESIAN_POINT('Ctrl Pts',(50.3754346667353,49.0437252024832,12.));
#167085=CARTESIAN_POINT('Ctrl Pts',(50.3932859445252,49.0533877945744,12.));
#167086=CARTESIAN_POINT('Ctrl Pts',(50.4111931994257,49.0630561755075,12.));
#167087=CARTESIAN_POINT('Ctrl Pts',(50.4291563088547,49.0727301783494,12.));
#167088=CARTESIAN_POINT('Ctrl Pts',(50.4471751542751,49.0824096415371,12.));
#167089=CARTESIAN_POINT('Ctrl Pts',(50.4652496210607,49.0920944087008,12.));
#167090=CARTESIAN_POINT('Ctrl Pts',(50.4833795969318,49.1017843266803,12.));
#167091=CARTESIAN_POINT('Ctrl Pts',(50.501564970874,49.1114792441571,12.));
#167092=CARTESIAN_POINT('Ctrl Pts',(50.5198056318089,49.1211790099795,12.));
#167093=CARTESIAN_POINT('Ctrl Pts',(50.5381014674791,49.1308834717615,12.));
#167094=CARTESIAN_POINT('Ctrl Pts',(50.556452365038,49.1405924766144,12.));
#167095=CARTESIAN_POINT('Ctrl Pts',(50.5748582115565,49.1503058717821,12.));
#167096=CARTESIAN_POINT('Ctrl Pts',(50.5933188945168,49.1600235052621,12.));
#167097=CARTESIAN_POINT('Ctrl Pts',(50.6118343023958,49.1697452265494,12.));
#167098=CARTESIAN_POINT('Ctrl Pts',(50.6304043248821,49.1794708869099,12.));
#167099=CARTESIAN_POINT('Ctrl Pts',(50.6490288525656,49.189200338976,12.));
#167100=CARTESIAN_POINT('Ctrl Pts',(50.6677077767432,49.1989334364996,12.));
#167101=CARTESIAN_POINT('Ctrl Pts',(50.6864409891895,49.2086700340614,12.));
#167102=CARTESIAN_POINT('Ctrl Pts',(50.7052283818922,49.2184099867461,12.));
#167103=CARTESIAN_POINT('Ctrl Pts',(50.7240698470679,49.228153150155,12.));
#167104=CARTESIAN_POINT('Ctrl Pts',(50.7429652772805,49.2378993805471,12.));
#167105=CARTESIAN_POINT('Ctrl Pts',(50.7619145655207,49.2476485349373,12.));
#167106=CARTESIAN_POINT('Ctrl Pts',(50.7809176052966,49.2574004712134,12.));
#167107=CARTESIAN_POINT('Ctrl Pts',(50.7999742907131,49.2671550482435,12.));
#167108=CARTESIAN_POINT('Ctrl Pts',(50.819084516434,49.2769121258164,12.));
#167109=CARTESIAN_POINT('Ctrl Pts',(50.8382481776403,49.2866715645838,12.));
#167110=CARTESIAN_POINT('Ctrl Pts',(50.8574651699873,49.2964332260039,12.));
#167111=CARTESIAN_POINT('Ctrl Pts',(50.8767353895492,49.3061969722781,12.));
#167112=CARTESIAN_POINT('Ctrl Pts',(50.8960587327848,49.3159626663109,12.));
#167113=CARTESIAN_POINT('Ctrl Pts',(50.9154350965666,49.3257301717335,12.));
#167114=CARTESIAN_POINT('Ctrl Pts',(50.9348643781924,49.3354993529159,12.));
#167115=CARTESIAN_POINT('Ctrl Pts',(50.9543464753981,49.345270074981,12.));
#167116=CARTESIAN_POINT('Ctrl Pts',(50.9738812863646,49.355042203823,12.));
#167117=CARTESIAN_POINT('Ctrl Pts',(50.9934687097188,49.3648156061058,12.));
#167118=CARTESIAN_POINT('Ctrl Pts',(51.0131086445272,49.3745901492432,12.));
#167119=CARTESIAN_POINT('Ctrl Pts',(51.0328009902858,49.3843657013852,12.));
#167120=CARTESIAN_POINT('Ctrl Pts',(51.052545646907,49.3941421314013,12.));
#167121=CARTESIAN_POINT('Ctrl Pts',(51.0723425146985,49.4039193088634,12.));
#167122=CARTESIAN_POINT('Ctrl Pts',(51.0921914943662,49.4136971040428,12.));
#167123=CARTESIAN_POINT('Ctrl Pts',(51.1120924870195,49.423475387907,12.));
#167124=CARTESIAN_POINT('Ctrl Pts',(51.1320453941702,49.4332540321178,12.));
#167125=CARTESIAN_POINT('Ctrl Pts',(51.1520501177291,49.4430329090287,12.));
#167126=CARTESIAN_POINT('Ctrl Pts',(51.1721065599973,49.4528118916832,12.));
#167127=CARTESIAN_POINT('Ctrl Pts',(51.1922146236686,49.4625908538074,12.));
#167128=CARTESIAN_POINT('Ctrl Pts',(51.2123742118287,49.4723696698021,12.));
#167129=CARTESIAN_POINT('Ctrl Pts',(51.2325852279506,49.4821482147356,12.));
#167130=CARTESIAN_POINT('Ctrl Pts',(51.2528475758846,49.4919263643362,12.));
#167131=CARTESIAN_POINT('Ctrl Pts',(51.2731611598475,49.5017039949852,12.));
#167132=CARTESIAN_POINT('Ctrl Pts',(51.2935258844289,49.5114809837122,12.));
#167133=CARTESIAN_POINT('Ctrl Pts',(51.313941654591,49.5212572081908,12.));
#167134=CARTESIAN_POINT('Ctrl Pts',(51.3344083756657,49.5310325467332,12.));
#167135=CARTESIAN_POINT('Ctrl Pts',(51.3549259533458,49.5408068782859,12.));
#167136=CARTESIAN_POINT('Ctrl Pts',(51.3754942936778,49.550580082425,12.));
#167137=CARTESIAN_POINT('Ctrl Pts',(51.396113303067,49.5603520393496,12.));
#167138=CARTESIAN_POINT('Ctrl Pts',(51.4167828882756,49.5701226298769,12.));
#167139=CARTESIAN_POINT('Ctrl Pts',(51.4375029564197,49.5798917354366,12.));
#167140=CARTESIAN_POINT('Ctrl Pts',(51.4582734149583,49.5896592380654,12.));
#167141=CARTESIAN_POINT('Ctrl Pts',(51.4790941716888,49.5994250204031,12.));
#167142=CARTESIAN_POINT('Ctrl Pts',(51.4999651347523,49.6091889656866,12.));
#167143=CARTESIAN_POINT('Ctrl Pts',(51.5208862126315,49.6189509577452,12.));
#167144=CARTESIAN_POINT('Ctrl Pts',(51.5418573141484,49.6287108809966,12.));
#167145=CARTESIAN_POINT('Ctrl Pts',(51.5628783484525,49.6384686204413,12.));
#167146=CARTESIAN_POINT('Ctrl Pts',(51.5839492250181,49.6482240616593,12.));
#167147=CARTESIAN_POINT('Ctrl Pts',(51.6050698536496,49.6579770908037,12.));
#167148=CARTESIAN_POINT('Ctrl Pts',(51.626240144479,49.6677275945967,12.));
#167149=CARTESIAN_POINT('Ctrl Pts',(51.6474600079622,49.6774754603245,12.));
#167150=CARTESIAN_POINT('Ctrl Pts',(51.6687293548682,49.6872205758336,12.));
#167151=CARTESIAN_POINT('Ctrl Pts',(51.6900480962773,49.6969628295262,12.));
#167152=CARTESIAN_POINT('Ctrl Pts',(51.7114161435869,49.7067021103553,12.));
#167153=CARTESIAN_POINT('Ctrl Pts',(51.7328334085091,49.7164383078212,12.));
#167154=CARTESIAN_POINT('Ctrl Pts',(51.754299803067,49.7261713119663,12.));
#167155=CARTESIAN_POINT('Ctrl Pts',(51.7758152395836,49.7359010133721,12.));
#167156=CARTESIAN_POINT('Ctrl Pts',(51.7973796306803,49.7456273031534,12.));
#167157=CARTESIAN_POINT('Ctrl Pts',(51.8189928892828,49.755350072955,12.));
#167158=CARTESIAN_POINT('Ctrl Pts',(51.8406549286175,49.7650692149462,12.));
#167159=CARTESIAN_POINT('Ctrl Pts',(51.8623656622097,49.7747846218182,12.));
#167160=CARTESIAN_POINT('Ctrl Pts',(51.8841250038724,49.7844961867808,12.));
#167161=CARTESIAN_POINT('Ctrl Pts',(51.9059328677059,49.7942038035576,12.));
#167162=CARTESIAN_POINT('Ctrl Pts',(51.9277891681018,49.8039073663812,12.));
#167163=CARTESIAN_POINT('Ctrl Pts',(51.9496938197418,49.8136067699896,12.));
#167164=CARTESIAN_POINT('Ctrl Pts',(51.9716467375937,49.8233019096222,12.));
#167165=CARTESIAN_POINT('Ctrl Pts',(51.9936478369008,49.8329926810172,12.));
#167166=CARTESIAN_POINT('Ctrl Pts',(52.0156970331823,49.8426789804071,12.));
#167167=CARTESIAN_POINT('Ctrl Pts',(52.0377942422376,49.8523607045149,12.));
#167168=CARTESIAN_POINT('Ctrl Pts',(52.0599393801452,49.86203775055,12.));
#167169=CARTESIAN_POINT('Ctrl Pts',(52.0821323632587,49.8717100162048,12.));
#167170=CARTESIAN_POINT('Ctrl Pts',(52.1043731081962,49.8813773996517,12.));
#167171=CARTESIAN_POINT('Ctrl Pts',(52.1266615318407,49.8910397995397,12.));
#167172=CARTESIAN_POINT('Ctrl Pts',(52.1489975513445,49.9006971149895,12.));
#167173=CARTESIAN_POINT('Ctrl Pts',(52.1713810841276,49.9103492455902,12.));
#167174=CARTESIAN_POINT('Ctrl Pts',(52.1938120478754,49.9199960913962,12.));
#167175=CARTESIAN_POINT('Ctrl Pts',(52.2162903605275,49.9296375529245,12.));
#167176=CARTESIAN_POINT('Ctrl Pts',(52.2388159402771,49.9392735311509,12.));
#167177=CARTESIAN_POINT('Ctrl Pts',(52.2613887055773,49.9489039275064,12.));
#167178=CARTESIAN_POINT('Ctrl Pts',(52.2840085751384,49.9585286438733,12.));
#167179=CARTESIAN_POINT('Ctrl Pts',(52.3066754679265,49.9681475825824,12.));
#167180=CARTESIAN_POINT('Ctrl Pts',(52.3293893031528,49.9777606464106,12.));
#167181=CARTESIAN_POINT('Ctrl Pts',(52.3521500002718,49.9873677385775,12.));
#167182=CARTESIAN_POINT('Ctrl Pts',(52.3749574789871,49.9969687627408,12.));
#167183=CARTESIAN_POINT('Ctrl Pts',(52.3978116592509,50.0065636229938,12.));
#167184=CARTESIAN_POINT('Ctrl Pts',(52.4207124612608,50.0161522238616,12.));
#167185=CARTESIAN_POINT('Ctrl Pts',(52.4436598054515,50.0257344703,12.));
#167186=CARTESIAN_POINT('Ctrl Pts',(52.4666536124913,50.0353102676921,12.));
#167187=CARTESIAN_POINT('Ctrl Pts',(52.4896938032884,50.0448795218441,12.));
#167188=CARTESIAN_POINT('Ctrl Pts',(52.5127802989896,50.0544421389818,12.));
#167189=CARTESIAN_POINT('Ctrl Pts',(52.5359130209792,50.0639980257479,12.));
#167190=CARTESIAN_POINT('Ctrl Pts',(52.5590918908702,50.0735470892007,12.));
#167191=CARTESIAN_POINT('Ctrl Pts',(52.5823168304994,50.0830892368107,12.));
#167192=CARTESIAN_POINT('Ctrl Pts',(52.6055877619348,50.0926243764578,12.));
#167193=CARTESIAN_POINT('Ctrl Pts',(52.6289046074746,50.1021524164264,12.));
#167194=CARTESIAN_POINT('Ctrl Pts',(52.652267289646,50.111673265404,12.));
#167195=CARTESIAN_POINT('Ctrl Pts',(52.6756757311978,50.1211868324781,12.));
#167196=CARTESIAN_POINT('Ctrl Pts',(52.699129855093,50.1306930271345,12.));
#167197=CARTESIAN_POINT('Ctrl Pts',(52.7226295845161,50.1401917592537,12.));
#167198=CARTESIAN_POINT('Ctrl Pts',(52.7461748428738,50.1496829391073,12.));
#167199=CARTESIAN_POINT('Ctrl Pts',(52.769765553794,50.1591664773561,12.));
#167200=CARTESIAN_POINT('Ctrl Pts',(52.7934016411205,50.1686422850488,12.));
#167201=CARTESIAN_POINT('Ctrl Pts',(52.8170830289044,50.1781102736205,12.));
#167202=CARTESIAN_POINT('Ctrl Pts',(52.8408096414093,50.1875703548884,12.));
#167203=CARTESIAN_POINT('Ctrl Pts',(52.8645814031133,50.1970224410471,12.));
#167204=CARTESIAN_POINT('Ctrl Pts',(52.8883982387068,50.2064664446663,12.));
#167205=CARTESIAN_POINT('Ctrl Pts',(52.9122600730884,50.2159022786879,12.));
#167206=CARTESIAN_POINT('Ctrl Pts',(52.9361668313542,50.2253298564241,12.));
#167207=CARTESIAN_POINT('Ctrl Pts',(52.9601184388028,50.2347490915555,12.));
#167208=CARTESIAN_POINT('Ctrl Pts',(52.9841148209402,50.2441598981286,12.));
#167209=CARTESIAN_POINT('Ctrl Pts',(53.0081559034801,50.2535621905552,12.));
#167210=CARTESIAN_POINT('Ctrl Pts',(53.0322416123406,50.2629558836111,12.));
#167211=CARTESIAN_POINT('Ctrl Pts',(53.0563718736366,50.2723408924373,12.));
#167212=CARTESIAN_POINT('Ctrl Pts',(53.0805466136798,50.2817171325358,12.));
#167213=CARTESIAN_POINT('Ctrl Pts',(53.1047657589812,50.2910845197619,12.));
#167214=CARTESIAN_POINT('Ctrl Pts',(53.1290292362485,50.300442970319,12.));
#167215=CARTESIAN_POINT('Ctrl Pts',(53.1533369723818,50.3097924007534,12.));
#167216=CARTESIAN_POINT('Ctrl Pts',(53.1776888944616,50.3191327279493,12.));
#167217=CARTESIAN_POINT('Ctrl Pts',(53.2020849297471,50.3284638691278,12.));
#167218=CARTESIAN_POINT('Ctrl Pts',(53.2265250056887,50.3377857418515,12.));
#167219=CARTESIAN_POINT('Ctrl Pts',(53.2510090499336,50.3470982640289,12.));
#167220=CARTESIAN_POINT('Ctrl Pts',(53.2755369903293,50.3564013539199,12.));
#167221=CARTESIAN_POINT('Ctrl Pts',(53.300108754923,50.365694930143,12.));
#167222=CARTESIAN_POINT('Ctrl Pts',(53.3247242719587,50.3749789116786,12.));
#167223=CARTESIAN_POINT('Ctrl Pts',(53.3493834698697,50.384253217846,12.));
#167224=CARTESIAN_POINT('Ctrl Pts',(53.3740862772681,50.3935177682837,12.));
#167225=CARTESIAN_POINT('Ctrl Pts',(53.398832622931,50.4027724829297,12.));
#167226=CARTESIAN_POINT('Ctrl Pts',(53.4236224357838,50.4120172820047,12.));
#167227=CARTESIAN_POINT('Ctrl Pts',(53.4484556448776,50.4212520859914,12.));
#167228=CARTESIAN_POINT('Ctrl Pts',(53.4733321794188,50.4304768156667,12.));
#167229=CARTESIAN_POINT('Ctrl Pts',(53.4982519688024,50.4396913921382,12.));
#167230=CARTESIAN_POINT('Ctrl Pts',(53.5232149426413,50.4488957368839,12.));
#167231=CARTESIAN_POINT('Ctrl Pts',(53.5482210307868,50.4580897717838,12.));
#167232=CARTESIAN_POINT('Ctrl Pts',(53.5732701633609,50.4672734191756,12.));
#167233=CARTESIAN_POINT('Ctrl Pts',(53.5983622707238,50.4764466018071,12.));
#167234=CARTESIAN_POINT('Ctrl Pts',(53.623497283406,50.4856092427314,12.));
#167235=CARTESIAN_POINT('Ctrl Pts',(53.6486751320436,50.4947612652149,12.));
#167236=CARTESIAN_POINT('Ctrl Pts',(53.6738957473158,50.503902592653,12.));
#167237=CARTESIAN_POINT('Ctrl Pts',(53.6991590598548,50.513033148456,12.));
#167238=CARTESIAN_POINT('Ctrl Pts',(53.7244650002374,50.522152856042,12.));
#167239=CARTESIAN_POINT('Ctrl Pts',(53.7498134991703,50.5312616390779,12.));
#167240=CARTESIAN_POINT('Ctrl Pts',(53.7752044876304,50.5403594216698,12.));
#167241=CARTESIAN_POINT('Ctrl Pts',(53.8006378970197,50.5494461285761,12.));
#167242=CARTESIAN_POINT('Ctrl Pts',(53.8261136593075,50.5585216854091,12.));
#167243=CARTESIAN_POINT('Ctrl Pts',(53.8516317071804,50.5675860188538,12.));
#167244=CARTESIAN_POINT('Ctrl Pts',(53.8771919737032,50.5766390561884,12.));
#167245=CARTESIAN_POINT('Ctrl Pts',(53.9027943919836,50.5856807248151,12.));
#167246=CARTESIAN_POINT('Ctrl Pts',(53.9284388948004,50.5947109517483,12.));
#167247=CARTESIAN_POINT('Ctrl Pts',(53.9541254143119,50.603729663214,12.));
#167248=CARTESIAN_POINT('Ctrl Pts',(53.979853881553,50.6127367839711,12.));
#167249=CARTESIAN_POINT('Ctrl Pts',(54.0056242268399,50.6217322378648,12.));
#167250=CARTESIAN_POINT('Ctrl Pts',(54.0314363806708,50.6307159490553,12.));
#167251=CARTESIAN_POINT('Ctrl Pts',(54.0572902745076,50.6396878430939,12.));
#167252=CARTESIAN_POINT('Ctrl Pts',(54.0831858415189,50.6486478479465,12.));
#167253=CARTESIAN_POINT('Ctrl Pts',(54.1091230175367,50.6575958953221,12.));
#167254=CARTESIAN_POINT('Ctrl Pts',(54.1351017412804,50.6665319209869,12.));
#167255=CARTESIAN_POINT('Ctrl Pts',(54.1574061042043,50.6741814675486,12.));
#167256=CARTESIAN_POINT('Ctrl Pts',(54.1745287898797,50.6800396668778,12.));
#167257=CARTESIAN_POINT('Ctrl Pts',(54.1864514382196,50.6841118861931,12.));
#167258=CARTESIAN_POINT('Ctrl Pts',(54.1931619277624,50.6864016965744,12.));
#167259=CARTESIAN_POINT('Ctrl Pts',(54.1946543500373,50.6869108458851,12.));
#167260=CARTESIAN_POINT('',(50.0975384783635,48.8900464144686,0.));
#167261=CARTESIAN_POINT('',(50.0975384783634,48.8900464144686,0.));
#167262=CARTESIAN_POINT('Ctrl Pts',(54.1946543500373,50.6869108458851,0.));
#167263=CARTESIAN_POINT('Ctrl Pts',(54.1931619277624,50.6864016965744,0.));
#167264=CARTESIAN_POINT('Ctrl Pts',(54.1864514382196,50.6841118861931,0.));
#167265=CARTESIAN_POINT('Ctrl Pts',(54.1745287898797,50.6800396668778,0.));
#167266=CARTESIAN_POINT('Ctrl Pts',(54.1574061042043,50.6741814675486,0.));
#167267=CARTESIAN_POINT('Ctrl Pts',(54.1351017412804,50.6665319209869,0.));
#167268=CARTESIAN_POINT('Ctrl Pts',(54.1091230175367,50.6575958953221,0.));
#167269=CARTESIAN_POINT('Ctrl Pts',(54.0831858415189,50.6486478479465,0.));
#167270=CARTESIAN_POINT('Ctrl Pts',(54.0572902745076,50.6396878430939,0.));
#167271=CARTESIAN_POINT('Ctrl Pts',(54.0314363806708,50.6307159490553,0.));
#167272=CARTESIAN_POINT('Ctrl Pts',(54.0056242268399,50.6217322378648,0.));
#167273=CARTESIAN_POINT('Ctrl Pts',(53.979853881553,50.6127367839711,0.));
#167274=CARTESIAN_POINT('Ctrl Pts',(53.9541254143119,50.603729663214,0.));
#167275=CARTESIAN_POINT('Ctrl Pts',(53.9284388948004,50.5947109517483,0.));
#167276=CARTESIAN_POINT('Ctrl Pts',(53.9027943919836,50.5856807248151,0.));
#167277=CARTESIAN_POINT('Ctrl Pts',(53.8771919737032,50.5766390561884,0.));
#167278=CARTESIAN_POINT('Ctrl Pts',(53.8516317071804,50.5675860188538,0.));
#167279=CARTESIAN_POINT('Ctrl Pts',(53.8261136593075,50.5585216854091,0.));
#167280=CARTESIAN_POINT('Ctrl Pts',(53.8006378970197,50.5494461285761,0.));
#167281=CARTESIAN_POINT('Ctrl Pts',(53.7752044876304,50.5403594216698,0.));
#167282=CARTESIAN_POINT('Ctrl Pts',(53.7498134991703,50.5312616390779,0.));
#167283=CARTESIAN_POINT('Ctrl Pts',(53.7244650002374,50.522152856042,0.));
#167284=CARTESIAN_POINT('Ctrl Pts',(53.6991590598548,50.513033148456,0.));
#167285=CARTESIAN_POINT('Ctrl Pts',(53.6738957473158,50.503902592653,0.));
#167286=CARTESIAN_POINT('Ctrl Pts',(53.6486751320436,50.4947612652149,0.));
#167287=CARTESIAN_POINT('Ctrl Pts',(53.623497283406,50.4856092427314,0.));
#167288=CARTESIAN_POINT('Ctrl Pts',(53.5983622707238,50.4764466018071,0.));
#167289=CARTESIAN_POINT('Ctrl Pts',(53.5732701633609,50.4672734191756,0.));
#167290=CARTESIAN_POINT('Ctrl Pts',(53.5482210307868,50.4580897717838,0.));
#167291=CARTESIAN_POINT('Ctrl Pts',(53.5232149426413,50.4488957368839,0.));
#167292=CARTESIAN_POINT('Ctrl Pts',(53.4982519688024,50.4396913921382,0.));
#167293=CARTESIAN_POINT('Ctrl Pts',(53.4733321794188,50.4304768156667,0.));
#167294=CARTESIAN_POINT('Ctrl Pts',(53.4484556448776,50.4212520859914,0.));
#167295=CARTESIAN_POINT('Ctrl Pts',(53.4236224357838,50.4120172820047,0.));
#167296=CARTESIAN_POINT('Ctrl Pts',(53.398832622931,50.4027724829297,0.));
#167297=CARTESIAN_POINT('Ctrl Pts',(53.3740862772681,50.3935177682837,0.));
#167298=CARTESIAN_POINT('Ctrl Pts',(53.3493834698697,50.384253217846,0.));
#167299=CARTESIAN_POINT('Ctrl Pts',(53.3247242719587,50.3749789116786,0.));
#167300=CARTESIAN_POINT('Ctrl Pts',(53.300108754923,50.365694930143,0.));
#167301=CARTESIAN_POINT('Ctrl Pts',(53.2755369903293,50.3564013539199,0.));
#167302=CARTESIAN_POINT('Ctrl Pts',(53.2510090499336,50.3470982640289,0.));
#167303=CARTESIAN_POINT('Ctrl Pts',(53.2265250056887,50.3377857418515,0.));
#167304=CARTESIAN_POINT('Ctrl Pts',(53.2020849297471,50.3284638691278,0.));
#167305=CARTESIAN_POINT('Ctrl Pts',(53.1776888944616,50.3191327279493,0.));
#167306=CARTESIAN_POINT('Ctrl Pts',(53.1533369723818,50.3097924007534,0.));
#167307=CARTESIAN_POINT('Ctrl Pts',(53.1290292362485,50.300442970319,0.));
#167308=CARTESIAN_POINT('Ctrl Pts',(53.1047657589812,50.2910845197619,0.));
#167309=CARTESIAN_POINT('Ctrl Pts',(53.0805466136798,50.2817171325358,0.));
#167310=CARTESIAN_POINT('Ctrl Pts',(53.0563718736366,50.2723408924373,0.));
#167311=CARTESIAN_POINT('Ctrl Pts',(53.0322416123406,50.2629558836111,0.));
#167312=CARTESIAN_POINT('Ctrl Pts',(53.0081559034801,50.2535621905552,0.));
#167313=CARTESIAN_POINT('Ctrl Pts',(52.9841148209402,50.2441598981286,0.));
#167314=CARTESIAN_POINT('Ctrl Pts',(52.9601184388028,50.2347490915555,0.));
#167315=CARTESIAN_POINT('Ctrl Pts',(52.9361668313542,50.2253298564241,0.));
#167316=CARTESIAN_POINT('Ctrl Pts',(52.9122600730884,50.2159022786879,0.));
#167317=CARTESIAN_POINT('Ctrl Pts',(52.8883982387068,50.2064664446663,0.));
#167318=CARTESIAN_POINT('Ctrl Pts',(52.8645814031133,50.1970224410471,0.));
#167319=CARTESIAN_POINT('Ctrl Pts',(52.8408096414093,50.1875703548884,0.));
#167320=CARTESIAN_POINT('Ctrl Pts',(52.8170830289044,50.1781102736205,0.));
#167321=CARTESIAN_POINT('Ctrl Pts',(52.7934016411205,50.1686422850488,0.));
#167322=CARTESIAN_POINT('Ctrl Pts',(52.769765553794,50.1591664773561,0.));
#167323=CARTESIAN_POINT('Ctrl Pts',(52.7461748428738,50.1496829391073,0.));
#167324=CARTESIAN_POINT('Ctrl Pts',(52.7226295845161,50.1401917592537,0.));
#167325=CARTESIAN_POINT('Ctrl Pts',(52.699129855093,50.1306930271345,0.));
#167326=CARTESIAN_POINT('Ctrl Pts',(52.6756757311978,50.1211868324781,0.));
#167327=CARTESIAN_POINT('Ctrl Pts',(52.652267289646,50.111673265404,0.));
#167328=CARTESIAN_POINT('Ctrl Pts',(52.6289046074746,50.1021524164264,0.));
#167329=CARTESIAN_POINT('Ctrl Pts',(52.6055877619348,50.0926243764578,0.));
#167330=CARTESIAN_POINT('Ctrl Pts',(52.5823168304994,50.0830892368107,0.));
#167331=CARTESIAN_POINT('Ctrl Pts',(52.5590918908702,50.0735470892007,0.));
#167332=CARTESIAN_POINT('Ctrl Pts',(52.5359130209792,50.0639980257479,0.));
#167333=CARTESIAN_POINT('Ctrl Pts',(52.5127802989896,50.0544421389818,0.));
#167334=CARTESIAN_POINT('Ctrl Pts',(52.4896938032884,50.0448795218441,0.));
#167335=CARTESIAN_POINT('Ctrl Pts',(52.4666536124913,50.0353102676921,0.));
#167336=CARTESIAN_POINT('Ctrl Pts',(52.4436598054515,50.0257344703,0.));
#167337=CARTESIAN_POINT('Ctrl Pts',(52.4207124612608,50.0161522238616,0.));
#167338=CARTESIAN_POINT('Ctrl Pts',(52.3978116592509,50.0065636229938,0.));
#167339=CARTESIAN_POINT('Ctrl Pts',(52.3749574789871,49.9969687627408,0.));
#167340=CARTESIAN_POINT('Ctrl Pts',(52.3521500002718,49.9873677385775,0.));
#167341=CARTESIAN_POINT('Ctrl Pts',(52.3293893031528,49.9777606464106,0.));
#167342=CARTESIAN_POINT('Ctrl Pts',(52.3066754679265,49.9681475825824,0.));
#167343=CARTESIAN_POINT('Ctrl Pts',(52.2840085751384,49.9585286438733,0.));
#167344=CARTESIAN_POINT('Ctrl Pts',(52.2613887055773,49.9489039275064,0.));
#167345=CARTESIAN_POINT('Ctrl Pts',(52.2388159402771,49.9392735311509,0.));
#167346=CARTESIAN_POINT('Ctrl Pts',(52.2162903605275,49.9296375529245,0.));
#167347=CARTESIAN_POINT('Ctrl Pts',(52.1938120478754,49.9199960913962,0.));
#167348=CARTESIAN_POINT('Ctrl Pts',(52.1713810841276,49.9103492455902,0.));
#167349=CARTESIAN_POINT('Ctrl Pts',(52.1489975513445,49.9006971149895,0.));
#167350=CARTESIAN_POINT('Ctrl Pts',(52.1266615318407,49.8910397995397,0.));
#167351=CARTESIAN_POINT('Ctrl Pts',(52.1043731081962,49.8813773996517,0.));
#167352=CARTESIAN_POINT('Ctrl Pts',(52.0821323632587,49.8717100162048,0.));
#167353=CARTESIAN_POINT('Ctrl Pts',(52.0599393801452,49.86203775055,0.));
#167354=CARTESIAN_POINT('Ctrl Pts',(52.0377942422376,49.8523607045149,0.));
#167355=CARTESIAN_POINT('Ctrl Pts',(52.0156970331823,49.8426789804071,0.));
#167356=CARTESIAN_POINT('Ctrl Pts',(51.9936478369008,49.8329926810172,0.));
#167357=CARTESIAN_POINT('Ctrl Pts',(51.9716467375937,49.8233019096222,0.));
#167358=CARTESIAN_POINT('Ctrl Pts',(51.9496938197418,49.8136067699896,0.));
#167359=CARTESIAN_POINT('Ctrl Pts',(51.9277891681018,49.8039073663812,0.));
#167360=CARTESIAN_POINT('Ctrl Pts',(51.9059328677059,49.7942038035576,0.));
#167361=CARTESIAN_POINT('Ctrl Pts',(51.8841250038724,49.7844961867808,0.));
#167362=CARTESIAN_POINT('Ctrl Pts',(51.8623656622097,49.7747846218182,0.));
#167363=CARTESIAN_POINT('Ctrl Pts',(51.8406549286175,49.7650692149462,0.));
#167364=CARTESIAN_POINT('Ctrl Pts',(51.8189928892828,49.755350072955,0.));
#167365=CARTESIAN_POINT('Ctrl Pts',(51.7973796306803,49.7456273031534,0.));
#167366=CARTESIAN_POINT('Ctrl Pts',(51.7758152395836,49.7359010133721,0.));
#167367=CARTESIAN_POINT('Ctrl Pts',(51.754299803067,49.7261713119663,0.));
#167368=CARTESIAN_POINT('Ctrl Pts',(51.7328334085091,49.7164383078212,0.));
#167369=CARTESIAN_POINT('Ctrl Pts',(51.7114161435869,49.7067021103553,0.));
#167370=CARTESIAN_POINT('Ctrl Pts',(51.6900480962773,49.6969628295262,0.));
#167371=CARTESIAN_POINT('Ctrl Pts',(51.6687293548682,49.6872205758336,0.));
#167372=CARTESIAN_POINT('Ctrl Pts',(51.6474600079622,49.6774754603245,0.));
#167373=CARTESIAN_POINT('Ctrl Pts',(51.626240144479,49.6677275945967,0.));
#167374=CARTESIAN_POINT('Ctrl Pts',(51.6050698536496,49.6579770908037,0.));
#167375=CARTESIAN_POINT('Ctrl Pts',(51.5839492250181,49.6482240616593,0.));
#167376=CARTESIAN_POINT('Ctrl Pts',(51.5628783484525,49.6384686204413,0.));
#167377=CARTESIAN_POINT('Ctrl Pts',(51.5418573141484,49.6287108809966,0.));
#167378=CARTESIAN_POINT('Ctrl Pts',(51.5208862126315,49.6189509577452,0.));
#167379=CARTESIAN_POINT('Ctrl Pts',(51.4999651347523,49.6091889656866,0.));
#167380=CARTESIAN_POINT('Ctrl Pts',(51.4790941716888,49.5994250204031,0.));
#167381=CARTESIAN_POINT('Ctrl Pts',(51.4582734149583,49.5896592380654,0.));
#167382=CARTESIAN_POINT('Ctrl Pts',(51.4375029564197,49.5798917354366,0.));
#167383=CARTESIAN_POINT('Ctrl Pts',(51.4167828882756,49.5701226298769,0.));
#167384=CARTESIAN_POINT('Ctrl Pts',(51.396113303067,49.5603520393496,0.));
#167385=CARTESIAN_POINT('Ctrl Pts',(51.3754942936778,49.550580082425,0.));
#167386=CARTESIAN_POINT('Ctrl Pts',(51.3549259533458,49.5408068782859,0.));
#167387=CARTESIAN_POINT('Ctrl Pts',(51.3344083756657,49.5310325467332,0.));
#167388=CARTESIAN_POINT('Ctrl Pts',(51.313941654591,49.5212572081908,0.));
#167389=CARTESIAN_POINT('Ctrl Pts',(51.2935258844289,49.5114809837122,0.));
#167390=CARTESIAN_POINT('Ctrl Pts',(51.2731611598475,49.5017039949852,0.));
#167391=CARTESIAN_POINT('Ctrl Pts',(51.2528475758846,49.4919263643362,0.));
#167392=CARTESIAN_POINT('Ctrl Pts',(51.2325852279506,49.4821482147356,0.));
#167393=CARTESIAN_POINT('Ctrl Pts',(51.2123742118287,49.4723696698021,0.));
#167394=CARTESIAN_POINT('Ctrl Pts',(51.1922146236686,49.4625908538074,0.));
#167395=CARTESIAN_POINT('Ctrl Pts',(51.1721065599973,49.4528118916832,0.));
#167396=CARTESIAN_POINT('Ctrl Pts',(51.1520501177291,49.4430329090287,0.));
#167397=CARTESIAN_POINT('Ctrl Pts',(51.1320453941702,49.4332540321178,0.));
#167398=CARTESIAN_POINT('Ctrl Pts',(51.1120924870195,49.423475387907,0.));
#167399=CARTESIAN_POINT('Ctrl Pts',(51.0921914943662,49.4136971040428,0.));
#167400=CARTESIAN_POINT('Ctrl Pts',(51.0723425146985,49.4039193088634,0.));
#167401=CARTESIAN_POINT('Ctrl Pts',(51.052545646907,49.3941421314013,0.));
#167402=CARTESIAN_POINT('Ctrl Pts',(51.0328009902858,49.3843657013852,0.));
#167403=CARTESIAN_POINT('Ctrl Pts',(51.0131086445272,49.3745901492432,0.));
#167404=CARTESIAN_POINT('Ctrl Pts',(50.9934687097188,49.3648156061058,0.));
#167405=CARTESIAN_POINT('Ctrl Pts',(50.9738812863646,49.355042203823,0.));
#167406=CARTESIAN_POINT('Ctrl Pts',(50.9543464753981,49.345270074981,0.));
#167407=CARTESIAN_POINT('Ctrl Pts',(50.9348643781924,49.3354993529159,0.));
#167408=CARTESIAN_POINT('Ctrl Pts',(50.9154350965666,49.3257301717335,0.));
#167409=CARTESIAN_POINT('Ctrl Pts',(50.8960587327848,49.3159626663109,0.));
#167410=CARTESIAN_POINT('Ctrl Pts',(50.8767353895492,49.3061969722781,0.));
#167411=CARTESIAN_POINT('Ctrl Pts',(50.8574651699873,49.2964332260039,0.));
#167412=CARTESIAN_POINT('Ctrl Pts',(50.8382481776403,49.2866715645838,0.));
#167413=CARTESIAN_POINT('Ctrl Pts',(50.819084516434,49.2769121258164,0.));
#167414=CARTESIAN_POINT('Ctrl Pts',(50.7999742907131,49.2671550482435,0.));
#167415=CARTESIAN_POINT('Ctrl Pts',(50.7809176052966,49.2574004712134,0.));
#167416=CARTESIAN_POINT('Ctrl Pts',(50.7619145655207,49.2476485349373,0.));
#167417=CARTESIAN_POINT('Ctrl Pts',(50.7429652772805,49.2378993805471,0.));
#167418=CARTESIAN_POINT('Ctrl Pts',(50.7240698470679,49.228153150155,0.));
#167419=CARTESIAN_POINT('Ctrl Pts',(50.7052283818922,49.2184099867461,0.));
#167420=CARTESIAN_POINT('Ctrl Pts',(50.6864409891895,49.2086700340614,0.));
#167421=CARTESIAN_POINT('Ctrl Pts',(50.6677077767432,49.1989334364996,0.));
#167422=CARTESIAN_POINT('Ctrl Pts',(50.6490288525656,49.189200338976,0.));
#167423=CARTESIAN_POINT('Ctrl Pts',(50.6304043248821,49.1794708869099,0.));
#167424=CARTESIAN_POINT('Ctrl Pts',(50.6118343023958,49.1697452265494,0.));
#167425=CARTESIAN_POINT('Ctrl Pts',(50.5933188945168,49.1600235052621,0.));
#167426=CARTESIAN_POINT('Ctrl Pts',(50.5748582115565,49.1503058717821,0.));
#167427=CARTESIAN_POINT('Ctrl Pts',(50.556452365038,49.1405924766144,0.));
#167428=CARTESIAN_POINT('Ctrl Pts',(50.5381014674791,49.1308834717615,0.));
#167429=CARTESIAN_POINT('Ctrl Pts',(50.5198056318089,49.1211790099795,0.));
#167430=CARTESIAN_POINT('Ctrl Pts',(50.501564970874,49.1114792441571,0.));
#167431=CARTESIAN_POINT('Ctrl Pts',(50.4833795969318,49.1017843266803,0.));
#167432=CARTESIAN_POINT('Ctrl Pts',(50.4652496210607,49.0920944087008,0.));
#167433=CARTESIAN_POINT('Ctrl Pts',(50.4471751542751,49.0824096415371,0.));
#167434=CARTESIAN_POINT('Ctrl Pts',(50.4291563088547,49.0727301783494,0.));
#167435=CARTESIAN_POINT('Ctrl Pts',(50.4111931994257,49.0630561755075,0.));
#167436=CARTESIAN_POINT('Ctrl Pts',(50.3932859445252,49.0533877945744,0.));
#167437=CARTESIAN_POINT('Ctrl Pts',(50.3754346667353,49.0437252024832,0.));
#167438=CARTESIAN_POINT('Ctrl Pts',(50.3576394894108,49.0340685673982,0.));
#167439=CARTESIAN_POINT('Ctrl Pts',(50.3399005337958,49.024418055075,0.));
#167440=CARTESIAN_POINT('Ctrl Pts',(50.3222179165119,49.0147738256942,0.));
#167441=CARTESIAN_POINT('Ctrl Pts',(50.3045917455424,49.0051360288044,0.));
#167442=CARTESIAN_POINT('Ctrl Pts',(50.2870221241054,48.9955048082081,0.));
#167443=CARTESIAN_POINT('Ctrl Pts',(50.2695091583511,48.9858803116689,0.));
#167444=CARTESIAN_POINT('Ctrl Pts',(50.252052963548,48.9762626987227,0.));
#167445=CARTESIAN_POINT('Ctrl Pts',(50.234653671541,48.9666521500911,0.));
#167446=CARTESIAN_POINT('Ctrl Pts',(50.2173114358325,48.9570488741167,0.));
#167447=CARTESIAN_POINT('Ctrl Pts',(50.2000264157797,48.9474530868733,0.));
#167448=CARTESIAN_POINT('Ctrl Pts',(50.1827987615602,48.9378649933055,0.));
#167449=CARTESIAN_POINT('Ctrl Pts',(50.1656286003997,48.9282847698294,0.));
#167450=CARTESIAN_POINT('Ctrl Pts',(50.1485160184657,48.9187125418099,0.));
#167451=CARTESIAN_POINT('Ctrl Pts',(50.1314610602569,48.90914838181,0.));
#167452=CARTESIAN_POINT('Ctrl Pts',(50.1178632067084,48.9015035372055,0.));
#167453=CARTESIAN_POINT('Ctrl Pts',(50.1076907555471,48.895773555686,0.));
#167454=CARTESIAN_POINT('Ctrl Pts',(50.1009206494272,48.8919551910366,0.));
#167455=CARTESIAN_POINT('Ctrl Pts',(50.0975384783635,48.8900464144686,0.));
#167456=CARTESIAN_POINT('Ctrl Pts',(58.722407829904,45.8467972562798,0.));
#167457=CARTESIAN_POINT('Ctrl Pts',(58.722407829904,45.8467972562798,12.));
#167458=CARTESIAN_POINT('Ctrl Pts',(58.7169606500268,45.8455162977427,0.));
#167459=CARTESIAN_POINT('Ctrl Pts',(58.7169606500268,45.8455162977427,12.));
#167460=CARTESIAN_POINT('Ctrl Pts',(58.7060702401686,45.8429527488786,0.));
#167461=CARTESIAN_POINT('Ctrl Pts',(58.7060702401686,45.8429527488786,12.));
#167462=CARTESIAN_POINT('Ctrl Pts',(58.6897464750699,45.8391025302132,0.));
#167463=CARTESIAN_POINT('Ctrl Pts',(58.6897464750699,45.8391025302132,12.));
#167464=CARTESIAN_POINT('Ctrl Pts',(58.6680051552762,45.8339591141834,0.));
#167465=CARTESIAN_POINT('Ctrl Pts',(58.6680051552762,45.8339591141834,12.));
#167466=CARTESIAN_POINT('Ctrl Pts',(58.6408680154016,45.827513526425,0.));
#167467=CARTESIAN_POINT('Ctrl Pts',(58.6408680154016,45.827513526425,12.));
#167468=CARTESIAN_POINT('Ctrl Pts',(58.6137704035871,45.8210516273781,0.));
#167469=CARTESIAN_POINT('Ctrl Pts',(58.6137704035871,45.8210516273781,12.));
#167470=CARTESIAN_POINT('Ctrl Pts',(58.5867123491018,45.814573433072,0.));
#167471=CARTESIAN_POINT('Ctrl Pts',(58.5867123491018,45.814573433072,12.));
#167472=CARTESIAN_POINT('Ctrl Pts',(58.5596938940195,45.8080789725084,0.));
#167473=CARTESIAN_POINT('Ctrl Pts',(58.5596938940195,45.8080789725084,12.));
#167474=CARTESIAN_POINT('Ctrl Pts',(58.5327150960661,45.8015682926025,0.));
#167475=CARTESIAN_POINT('Ctrl Pts',(58.5327150960661,45.8015682926025,12.));
#167476=CARTESIAN_POINT('Ctrl Pts',(58.5057760270184,45.7950414569268,0.));
#167477=CARTESIAN_POINT('Ctrl Pts',(58.5057760270184,45.7950414569268,12.));
#167478=CARTESIAN_POINT('Ctrl Pts',(58.4788767676949,45.7884985397018,0.));
#167479=CARTESIAN_POINT('Ctrl Pts',(58.4788767676949,45.7884985397018,12.));
#167480=CARTESIAN_POINT('Ctrl Pts',(58.4520174038764,45.7819396211009,0.));
#167481=CARTESIAN_POINT('Ctrl Pts',(58.4520174038764,45.7819396211009,12.));
#167482=CARTESIAN_POINT('Ctrl Pts',(58.425198021955,45.7753647821513,0.));
#167483=CARTESIAN_POINT('Ctrl Pts',(58.425198021955,45.7753647821513,12.));
#167484=CARTESIAN_POINT('Ctrl Pts',(58.3984187044245,45.7687740994957,0.));
#167485=CARTESIAN_POINT('Ctrl Pts',(58.3984187044245,45.7687740994957,12.));
#167486=CARTESIAN_POINT('Ctrl Pts',(58.3716795262353,45.7621676411434,0.));
#167487=CARTESIAN_POINT('Ctrl Pts',(58.3716795262353,45.7621676411434,12.));
#167488=CARTESIAN_POINT('Ctrl Pts',(58.3449805573423,45.755545469402,0.));
#167489=CARTESIAN_POINT('Ctrl Pts',(58.3449805573423,45.755545469402,12.));
#167490=CARTESIAN_POINT('Ctrl Pts',(58.3183218645316,45.7489076429763,0.));
#167491=CARTESIAN_POINT('Ctrl Pts',(58.3183218645316,45.7489076429763,12.));
#167492=CARTESIAN_POINT('Ctrl Pts',(58.291703513584,45.742254219463,0.));
#167493=CARTESIAN_POINT('Ctrl Pts',(58.291703513584,45.742254219463,12.));
#167494=CARTESIAN_POINT('Ctrl Pts',(58.2651255711453,45.7355852575107,0.));
#167495=CARTESIAN_POINT('Ctrl Pts',(58.2651255711453,45.7355852575107,12.));
#167496=CARTESIAN_POINT('Ctrl Pts',(58.2385881070913,45.7289008195579,0.));
#167497=CARTESIAN_POINT('Ctrl Pts',(58.2385881070913,45.7289008195579,12.));
#167498=CARTESIAN_POINT('Ctrl Pts',(58.2120911942772,45.7222009715397,0.));
#167499=CARTESIAN_POINT('Ctrl Pts',(58.2120911942772,45.7222009715397,12.));
#167500=CARTESIAN_POINT('Ctrl Pts',(58.185634907469,45.7154857816483,0.));
#167501=CARTESIAN_POINT('Ctrl Pts',(58.185634907469,45.7154857816483,12.));
#167502=CARTESIAN_POINT('Ctrl Pts',(58.1592193225137,45.7087553193771,0.));
#167503=CARTESIAN_POINT('Ctrl Pts',(58.1592193225137,45.7087553193771,12.));
#167504=CARTESIAN_POINT('Ctrl Pts',(58.1328445154676,45.702009654518,0.));
#167505=CARTESIAN_POINT('Ctrl Pts',(58.1328445154676,45.702009654518,12.));
#167506=CARTESIAN_POINT('Ctrl Pts',(58.1065105615907,45.695248856015,0.));
#167507=CARTESIAN_POINT('Ctrl Pts',(58.1065105615907,45.695248856015,12.));
#167508=CARTESIAN_POINT('Ctrl Pts',(58.0802175348966,45.6884729914485,0.));
#167509=CARTESIAN_POINT('Ctrl Pts',(58.0802175348966,45.6884729914485,12.));
#167510=CARTESIAN_POINT('Ctrl Pts',(58.0539655087117,45.6816821276678,0.));
#167511=CARTESIAN_POINT('Ctrl Pts',(58.0539655087117,45.6816821276678,12.));
#167512=CARTESIAN_POINT('Ctrl Pts',(58.0277545560012,45.6748763311643,0.));
#167513=CARTESIAN_POINT('Ctrl Pts',(58.0277545560012,45.6748763311643,12.));
#167514=CARTESIAN_POINT('Ctrl Pts',(58.0015847497837,45.6680556685493,0.));
#167515=CARTESIAN_POINT('Ctrl Pts',(58.0015847497837,45.6680556685493,12.));
#167516=CARTESIAN_POINT('Ctrl Pts',(57.9754561635061,45.661220206992,0.));
#167517=CARTESIAN_POINT('Ctrl Pts',(57.9754561635061,45.661220206992,12.));
#167518=CARTESIAN_POINT('Ctrl Pts',(57.9493688714237,45.6543700146679,0.));
#167519=CARTESIAN_POINT('Ctrl Pts',(57.9493688714237,45.6543700146679,12.));
#167520=CARTESIAN_POINT('Ctrl Pts',(57.9233229484311,45.6475051605535,0.));
#167521=CARTESIAN_POINT('Ctrl Pts',(57.9233229484311,45.6475051605535,12.));
#167522=CARTESIAN_POINT('Ctrl Pts',(57.8973184699034,45.6406257142382,0.));
#167523=CARTESIAN_POINT('Ctrl Pts',(57.8973184699034,45.6406257142382,12.));
#167524=CARTESIAN_POINT('Ctrl Pts',(57.8713555115232,45.6337317457252,0.));
#167525=CARTESIAN_POINT('Ctrl Pts',(57.8713555115232,45.6337317457252,12.));
#167526=CARTESIAN_POINT('Ctrl Pts',(57.8454341491238,45.6268233252544,0.));
#167527=CARTESIAN_POINT('Ctrl Pts',(57.8454341491238,45.6268233252544,12.));
#167528=CARTESIAN_POINT('Ctrl Pts',(57.8195544584845,45.6199005230784,0.));
#167529=CARTESIAN_POINT('Ctrl Pts',(57.8195544584845,45.6199005230784,12.));
#167530=CARTESIAN_POINT('Ctrl Pts',(57.7937165153387,45.6129634094683,0.));
#167531=CARTESIAN_POINT('Ctrl Pts',(57.7937165153387,45.6129634094683,12.));
#167532=CARTESIAN_POINT('Ctrl Pts',(57.7679203954742,45.6060120548205,0.));
#167533=CARTESIAN_POINT('Ctrl Pts',(57.7679203954742,45.6060120548205,12.));
#167534=CARTESIAN_POINT('Ctrl Pts',(57.7421661748026,45.5990465297344,0.));
#167535=CARTESIAN_POINT('Ctrl Pts',(57.7421661748026,45.5990465297344,12.));
#167536=CARTESIAN_POINT('Ctrl Pts',(57.7164539294314,45.5920669050986,0.));
#167537=CARTESIAN_POINT('Ctrl Pts',(57.7164539294314,45.5920669050986,12.));
#167538=CARTESIAN_POINT('Ctrl Pts',(57.6907837357417,45.5850732521896,0.));
#167539=CARTESIAN_POINT('Ctrl Pts',(57.6907837357417,45.5850732521896,12.));
#167540=CARTESIAN_POINT('Ctrl Pts',(57.6651556704237,45.5780656427163,0.));
#167541=CARTESIAN_POINT('Ctrl Pts',(57.6651556704237,45.5780656427163,12.));
#167542=CARTESIAN_POINT('Ctrl Pts',(57.6395698104404,45.5710441487674,0.));
#167543=CARTESIAN_POINT('Ctrl Pts',(57.6395698104404,45.5710441487674,12.));
#167544=CARTESIAN_POINT('Ctrl Pts',(57.614026233004,45.5640088427813,0.));
#167545=CARTESIAN_POINT('Ctrl Pts',(57.614026233004,45.5640088427813,12.));
#167546=CARTESIAN_POINT('Ctrl Pts',(57.5885250155433,45.5569597975096,0.));
#167547=CARTESIAN_POINT('Ctrl Pts',(57.5885250155433,45.5569597975096,12.));
#167548=CARTESIAN_POINT('Ctrl Pts',(57.563066235668,45.5498970859835,0.));
#167549=CARTESIAN_POINT('Ctrl Pts',(57.563066235668,45.5498970859835,12.));
#167550=CARTESIAN_POINT('Ctrl Pts',(57.537649971135,45.542820781484,0.));
#167551=CARTESIAN_POINT('Ctrl Pts',(57.537649971135,45.542820781484,12.));
#167552=CARTESIAN_POINT('Ctrl Pts',(57.5122762998745,45.5357309575611,0.));
#167553=CARTESIAN_POINT('Ctrl Pts',(57.5122762998745,45.5357309575611,12.));
#167554=CARTESIAN_POINT('Ctrl Pts',(57.4869453000063,45.5286276880485,0.));
#167555=CARTESIAN_POINT('Ctrl Pts',(57.4869453000063,45.5286276880485,12.));
#167556=CARTESIAN_POINT('Ctrl Pts',(57.4616570498568,45.5215110470825,0.));
#167557=CARTESIAN_POINT('Ctrl Pts',(57.4616570498568,45.5215110470825,12.));
#167558=CARTESIAN_POINT('Ctrl Pts',(57.4364116279702,45.5143811091205,0.));
#167559=CARTESIAN_POINT('Ctrl Pts',(57.4364116279702,45.5143811091205,12.));
#167560=CARTESIAN_POINT('Ctrl Pts',(57.4112091131183,45.5072379489631,0.));
#167561=CARTESIAN_POINT('Ctrl Pts',(57.4112091131183,45.5072379489631,12.));
#167562=CARTESIAN_POINT('Ctrl Pts',(57.3860495843033,45.500081641751,0.));
#167563=CARTESIAN_POINT('Ctrl Pts',(57.3860495843033,45.500081641751,12.));
#167564=CARTESIAN_POINT('Ctrl Pts',(57.3609331207574,45.4929122629572,0.));
#167565=CARTESIAN_POINT('Ctrl Pts',(57.3609331207574,45.4929122629572,12.));
#167566=CARTESIAN_POINT('Ctrl Pts',(57.3358598019389,45.4857298883824,0.));
#167567=CARTESIAN_POINT('Ctrl Pts',(57.3358598019389,45.4857298883824,12.));
#167568=CARTESIAN_POINT('Ctrl Pts',(57.3108297075265,45.4785345941507,0.));
#167569=CARTESIAN_POINT('Ctrl Pts',(57.3108297075265,45.4785345941507,12.));
#167570=CARTESIAN_POINT('Ctrl Pts',(57.2858429174062,45.4713264567063,0.));
#167571=CARTESIAN_POINT('Ctrl Pts',(57.2858429174062,45.4713264567063,12.));
#167572=CARTESIAN_POINT('Ctrl Pts',(57.2608995116733,45.4641055528141,0.));
#167573=CARTESIAN_POINT('Ctrl Pts',(57.2608995116733,45.4641055528141,12.));
#167574=CARTESIAN_POINT('Ctrl Pts',(57.2359995706447,45.4568719595642,0.));
#167575=CARTESIAN_POINT('Ctrl Pts',(57.2359995706447,45.4568719595642,12.));
#167576=CARTESIAN_POINT('Ctrl Pts',(57.2111431748631,45.4496257543759,0.));
#167577=CARTESIAN_POINT('Ctrl Pts',(57.2111431748631,45.4496257543759,12.));
#167578=CARTESIAN_POINT('Ctrl Pts',(57.186330405101,45.4423670150034,0.));
#167579=CARTESIAN_POINT('Ctrl Pts',(57.186330405101,45.4423670150034,12.));
#167580=CARTESIAN_POINT('Ctrl Pts',(57.1615613423584,45.4350958195434,0.));
#167581=CARTESIAN_POINT('Ctrl Pts',(57.1615613423584,45.4350958195434,12.));
#167582=CARTESIAN_POINT('Ctrl Pts',(57.136836067863,45.4278122464389,0.));
#167583=CARTESIAN_POINT('Ctrl Pts',(57.136836067863,45.4278122464389,12.));
#167584=CARTESIAN_POINT('Ctrl Pts',(57.112154663078,45.4205163744782,0.));
#167585=CARTESIAN_POINT('Ctrl Pts',(57.112154663078,45.4205163744782,12.));
#167586=CARTESIAN_POINT('Ctrl Pts',(57.0875172097051,45.4132082827948,0.));
#167587=CARTESIAN_POINT('Ctrl Pts',(57.0875172097051,45.4132082827948,12.));
#167588=CARTESIAN_POINT('Ctrl Pts',(57.0629237896848,45.4058880508693,0.));
#167589=CARTESIAN_POINT('Ctrl Pts',(57.0629237896848,45.4058880508693,12.));
#167590=CARTESIAN_POINT('Ctrl Pts',(57.0383744851913,45.3985557585311,0.));
#167591=CARTESIAN_POINT('Ctrl Pts',(57.0383744851913,45.3985557585311,12.));
#167592=CARTESIAN_POINT('Ctrl Pts',(57.0138693786278,45.3912114859616,0.));
#167593=CARTESIAN_POINT('Ctrl Pts',(57.0138693786278,45.3912114859616,12.));
#167594=CARTESIAN_POINT('Ctrl Pts',(56.9894085526373,45.3838553136948,0.));
#167595=CARTESIAN_POINT('Ctrl Pts',(56.9894085526373,45.3838553136948,12.));
#167596=CARTESIAN_POINT('Ctrl Pts',(56.9649920901073,45.3764873226196,0.));
#167597=CARTESIAN_POINT('Ctrl Pts',(56.9649920901073,45.3764873226196,12.));
#167598=CARTESIAN_POINT('Ctrl Pts',(56.9406200741714,45.3691075939827,0.));
#167599=CARTESIAN_POINT('Ctrl Pts',(56.9406200741714,45.3691075939827,12.));
#167600=CARTESIAN_POINT('Ctrl Pts',(56.9162925882085,45.3617162093923,0.));
#167601=CARTESIAN_POINT('Ctrl Pts',(56.9162925882085,45.3617162093923,12.));
#167602=CARTESIAN_POINT('Ctrl Pts',(56.8920097158377,45.3543132508239,0.));
#167603=CARTESIAN_POINT('Ctrl Pts',(56.8920097158377,45.3543132508239,12.));
#167604=CARTESIAN_POINT('Ctrl Pts',(56.8677715409268,45.3468988006203,0.));
#167605=CARTESIAN_POINT('Ctrl Pts',(56.8677715409268,45.3468988006203,12.));
#167606=CARTESIAN_POINT('Ctrl Pts',(56.8435781475981,45.3394729414931,0.));
#167607=CARTESIAN_POINT('Ctrl Pts',(56.8435781475981,45.3394729414931,12.));
#167608=CARTESIAN_POINT('Ctrl Pts',(56.8194296202291,45.332035756524,0.));
#167609=CARTESIAN_POINT('Ctrl Pts',(56.8194296202291,45.332035756524,12.));
#167610=CARTESIAN_POINT('Ctrl Pts',(56.7953260434524,45.3245873291684,0.));
#167611=CARTESIAN_POINT('Ctrl Pts',(56.7953260434524,45.3245873291684,12.));
#167612=CARTESIAN_POINT('Ctrl Pts',(56.7712675021491,45.31712774326,0.));
#167613=CARTESIAN_POINT('Ctrl Pts',(56.7712675021491,45.31712774326,12.));
#167614=CARTESIAN_POINT('Ctrl Pts',(56.7472540814553,45.3096570830118,0.));
#167615=CARTESIAN_POINT('Ctrl Pts',(56.7472540814553,45.3096570830118,12.));
#167616=CARTESIAN_POINT('Ctrl Pts',(56.7232858667709,45.3021754330179,0.));
#167617=CARTESIAN_POINT('Ctrl Pts',(56.7232858667709,45.3021754330179,12.));
#167618=CARTESIAN_POINT('Ctrl Pts',(56.69936294376,45.2946828782559,0.));
#167619=CARTESIAN_POINT('Ctrl Pts',(56.69936294376,45.2946828782559,12.));
#167620=CARTESIAN_POINT('Ctrl Pts',(56.6754853983528,45.2871795040906,0.));
#167621=CARTESIAN_POINT('Ctrl Pts',(56.6754853983528,45.2871795040906,12.));
#167622=CARTESIAN_POINT('Ctrl Pts',(56.6516533167384,45.2796653962785,0.));
#167623=CARTESIAN_POINT('Ctrl Pts',(56.6516533167384,45.2796653962785,12.));
#167624=CARTESIAN_POINT('Ctrl Pts',(56.6278667853702,45.2721406409695,0.));
#167625=CARTESIAN_POINT('Ctrl Pts',(56.6278667853702,45.2721406409695,12.));
#167626=CARTESIAN_POINT('Ctrl Pts',(56.6041258909741,45.2646053247087,0.));
#167627=CARTESIAN_POINT('Ctrl Pts',(56.6041258909741,45.2646053247087,12.));
#167628=CARTESIAN_POINT('Ctrl Pts',(56.5804307205505,45.257059534438,0.));
#167629=CARTESIAN_POINT('Ctrl Pts',(56.5804307205505,45.257059534438,12.));
#167630=CARTESIAN_POINT('Ctrl Pts',(56.5567813613756,45.2495033575,0.));
#167631=CARTESIAN_POINT('Ctrl Pts',(56.5567813613756,45.2495033575,12.));
#167632=CARTESIAN_POINT('Ctrl Pts',(56.5331779009958,45.2419368816429,0.));
#167633=CARTESIAN_POINT('Ctrl Pts',(56.5331779009958,45.2419368816429,12.));
#167634=CARTESIAN_POINT('Ctrl Pts',(56.5096204272306,45.2343601950228,0.));
#167635=CARTESIAN_POINT('Ctrl Pts',(56.5096204272306,45.2343601950228,12.));
#167636=CARTESIAN_POINT('Ctrl Pts',(56.4861090281823,45.2267733862049,0.));
#167637=CARTESIAN_POINT('Ctrl Pts',(56.4861090281823,45.2267733862049,12.));
#167638=CARTESIAN_POINT('Ctrl Pts',(56.4626437922386,45.2191765441667,0.));
#167639=CARTESIAN_POINT('Ctrl Pts',(56.4626437922386,45.2191765441667,12.));
#167640=CARTESIAN_POINT('Ctrl Pts',(56.4392248080732,45.2115697583001,0.));
#167641=CARTESIAN_POINT('Ctrl Pts',(56.4392248080732,45.2115697583001,12.));
#167642=CARTESIAN_POINT('Ctrl Pts',(56.4158521646411,45.2039531184172,0.));
#167643=CARTESIAN_POINT('Ctrl Pts',(56.4158521646411,45.2039531184172,12.));
#167644=CARTESIAN_POINT('Ctrl Pts',(56.3925259511806,45.1963267147529,0.));
#167645=CARTESIAN_POINT('Ctrl Pts',(56.3925259511806,45.1963267147529,12.));
#167646=CARTESIAN_POINT('Ctrl Pts',(56.3692462572231,45.1886906379667,0.));
#167647=CARTESIAN_POINT('Ctrl Pts',(56.3692462572231,45.1886906379667,12.));
#167648=CARTESIAN_POINT('Ctrl Pts',(56.3460131725964,45.1810449791453,0.));
#167649=CARTESIAN_POINT('Ctrl Pts',(56.3460131725964,45.1810449791453,12.));
#167650=CARTESIAN_POINT('Ctrl Pts',(56.3228267874264,45.1733898298061,0.));
#167651=CARTESIAN_POINT('Ctrl Pts',(56.3228267874264,45.1733898298061,12.));
#167652=CARTESIAN_POINT('Ctrl Pts',(56.2996871921316,45.1657252819013,0.));
#167653=CARTESIAN_POINT('Ctrl Pts',(56.2996871921316,45.1657252819013,12.));
#167654=CARTESIAN_POINT('Ctrl Pts',(56.2765944774245,45.1580514278223,0.));
#167655=CARTESIAN_POINT('Ctrl Pts',(56.2765944774245,45.1580514278223,12.));
#167656=CARTESIAN_POINT('Ctrl Pts',(56.2535487343221,45.1503683604005,0.));
#167657=CARTESIAN_POINT('Ctrl Pts',(56.2535487343221,45.1503683604005,12.));
#167658=CARTESIAN_POINT('Ctrl Pts',(56.2305500541489,45.1426761729105,0.));
#167659=CARTESIAN_POINT('Ctrl Pts',(56.2305500541489,45.1426761729105,12.));
#167660=CARTESIAN_POINT('Ctrl Pts',(56.2075985285393,45.1349749590738,0.));
#167661=CARTESIAN_POINT('Ctrl Pts',(56.2075985285393,45.1349749590738,12.));
#167662=CARTESIAN_POINT('Ctrl Pts',(56.1846942494325,45.127264813063,0.));
#167663=CARTESIAN_POINT('Ctrl Pts',(56.1846942494325,45.127264813063,12.));
#167664=CARTESIAN_POINT('Ctrl Pts',(56.1618373090732,45.1195458295063,0.));
#167665=CARTESIAN_POINT('Ctrl Pts',(56.1618373090732,45.1195458295063,12.));
#167666=CARTESIAN_POINT('Ctrl Pts',(56.1390278000226,45.1118181034888,0.));
#167667=CARTESIAN_POINT('Ctrl Pts',(56.1390278000226,45.1118181034888,12.));
#167668=CARTESIAN_POINT('Ctrl Pts',(56.116265815162,45.1040817305561,0.));
#167669=CARTESIAN_POINT('Ctrl Pts',(56.116265815162,45.1040817305561,12.));
#167670=CARTESIAN_POINT('Ctrl Pts',(56.0935514476945,45.0963368067177,0.));
#167671=CARTESIAN_POINT('Ctrl Pts',(56.0935514476945,45.0963368067177,12.));
#167672=CARTESIAN_POINT('Ctrl Pts',(56.0708847911416,45.0885834284517,0.));
#167673=CARTESIAN_POINT('Ctrl Pts',(56.0708847911416,45.0885834284517,12.));
#167674=CARTESIAN_POINT('Ctrl Pts',(56.048265939342,45.0808216927089,0.));
#167675=CARTESIAN_POINT('Ctrl Pts',(56.048265939342,45.0808216927089,12.));
#167676=CARTESIAN_POINT('Ctrl Pts',(56.0256949864639,45.0730516969149,0.));
#167677=CARTESIAN_POINT('Ctrl Pts',(56.0256949864639,45.0730516969149,12.));
#167678=CARTESIAN_POINT('Ctrl Pts',(56.003172027008,45.0652735389733,0.));
#167679=CARTESIAN_POINT('Ctrl Pts',(56.003172027008,45.0652735389733,12.));
#167680=CARTESIAN_POINT('Ctrl Pts',(55.9806971558097,45.0574873172695,0.));
#167681=CARTESIAN_POINT('Ctrl Pts',(55.9806971558097,45.0574873172695,12.));
#167682=CARTESIAN_POINT('Ctrl Pts',(55.9582704680356,45.0496931306755,0.));
#167683=CARTESIAN_POINT('Ctrl Pts',(55.9582704680356,45.0496931306755,12.));
#167684=CARTESIAN_POINT('Ctrl Pts',(55.9358920591837,45.0418910785551,0.));
#167685=CARTESIAN_POINT('Ctrl Pts',(55.9358920591837,45.0418910785551,12.));
#167686=CARTESIAN_POINT('Ctrl Pts',(55.9135620250954,45.0340812607657,0.));
#167687=CARTESIAN_POINT('Ctrl Pts',(55.9135620250954,45.0340812607657,12.));
#167688=CARTESIAN_POINT('Ctrl Pts',(55.8912804619577,45.0262637776615,0.));
#167689=CARTESIAN_POINT('Ctrl Pts',(55.8912804619577,45.0262637776615,12.));
#167690=CARTESIAN_POINT('Ctrl Pts',(55.8690474663065,45.0184387300973,0.));
#167691=CARTESIAN_POINT('Ctrl Pts',(55.8690474663065,45.0184387300973,12.));
#167692=CARTESIAN_POINT('Ctrl Pts',(55.8468631350218,45.0106062194342,0.));
#167693=CARTESIAN_POINT('Ctrl Pts',(55.8468631350218,45.0106062194342,12.));
#167694=CARTESIAN_POINT('Ctrl Pts',(55.8247275653289,45.0027663475433,0.));
#167695=CARTESIAN_POINT('Ctrl Pts',(55.8247275653289,45.0027663475433,12.));
#167696=CARTESIAN_POINT('Ctrl Pts',(55.8026408548105,44.9949192168093,0.));
#167697=CARTESIAN_POINT('Ctrl Pts',(55.8026408548105,44.9949192168093,12.));
#167698=CARTESIAN_POINT('Ctrl Pts',(55.7806031014106,44.9870649301342,0.));
#167699=CARTESIAN_POINT('Ctrl Pts',(55.7806031014106,44.9870649301342,12.));
#167700=CARTESIAN_POINT('Ctrl Pts',(55.7586144034367,44.9792035909413,0.));
#167701=CARTESIAN_POINT('Ctrl Pts',(55.7586144034367,44.9792035909413,12.));
#167702=CARTESIAN_POINT('Ctrl Pts',(55.7366748595551,44.9713353031804,0.));
#167703=CARTESIAN_POINT('Ctrl Pts',(55.7366748595551,44.9713353031804,12.));
#167704=CARTESIAN_POINT('Ctrl Pts',(55.714784568793,44.9634601713321,0.));
#167705=CARTESIAN_POINT('Ctrl Pts',(55.714784568793,44.9634601713321,12.));
#167706=CARTESIAN_POINT('Ctrl Pts',(55.6929436305489,44.9555783004106,0.));
#167707=CARTESIAN_POINT('Ctrl Pts',(55.6929436305489,44.9555783004106,12.));
#167708=CARTESIAN_POINT('Ctrl Pts',(55.6711521445979,44.9476897959685,0.));
#167709=CARTESIAN_POINT('Ctrl Pts',(55.6711521445979,44.9476897959685,12.));
#167710=CARTESIAN_POINT('Ctrl Pts',(55.6494102110935,44.9397947641007,0.));
#167711=CARTESIAN_POINT('Ctrl Pts',(55.6494102110935,44.9397947641007,12.));
#167712=CARTESIAN_POINT('Ctrl Pts',(55.6277179305633,44.9318933114507,0.));
#167713=CARTESIAN_POINT('Ctrl Pts',(55.6277179305633,44.9318933114507,12.));
#167714=CARTESIAN_POINT('Ctrl Pts',(55.6060754039121,44.9239855452144,0.));
#167715=CARTESIAN_POINT('Ctrl Pts',(55.6060754039121,44.9239855452144,12.));
#167716=CARTESIAN_POINT('Ctrl Pts',(55.5844827324338,44.9160715731443,0.));
#167717=CARTESIAN_POINT('Ctrl Pts',(55.5844827324338,44.9160715731443,12.));
#167718=CARTESIAN_POINT('Ctrl Pts',(55.5629400178142,44.908151503553,0.));
#167719=CARTESIAN_POINT('Ctrl Pts',(55.5629400178142,44.908151503553,12.));
#167720=CARTESIAN_POINT('Ctrl Pts',(55.541447362134,44.9002254453183,0.));
#167721=CARTESIAN_POINT('Ctrl Pts',(55.541447362134,44.9002254453183,12.));
#167722=CARTESIAN_POINT('Ctrl Pts',(55.5200048678629,44.8922935078889,0.));
#167723=CARTESIAN_POINT('Ctrl Pts',(55.5200048678629,44.8922935078889,12.));
#167724=CARTESIAN_POINT('Ctrl Pts',(55.4986126378656,44.8843558012886,0.));
#167725=CARTESIAN_POINT('Ctrl Pts',(55.4986126378656,44.8843558012886,12.));
#167726=CARTESIAN_POINT('Ctrl Pts',(55.4772707754126,44.8764124361207,0.));
#167727=CARTESIAN_POINT('Ctrl Pts',(55.4772707754126,44.8764124361207,12.));
#167728=CARTESIAN_POINT('Ctrl Pts',(55.4559793841836,44.8684635235725,0.));
#167729=CARTESIAN_POINT('Ctrl Pts',(55.4559793841836,44.8684635235725,12.));
#167730=CARTESIAN_POINT('Ctrl Pts',(55.4347385682704,44.8605091754214,0.));
#167731=CARTESIAN_POINT('Ctrl Pts',(55.4347385682704,44.8605091754214,12.));
#167732=CARTESIAN_POINT('Ctrl Pts',(55.4135484321718,44.8525495040408,0.));
#167733=CARTESIAN_POINT('Ctrl Pts',(55.4135484321718,44.8525495040408,12.));
#167734=CARTESIAN_POINT('Ctrl Pts',(55.3924090808014,44.8445846224044,0.));
#167735=CARTESIAN_POINT('Ctrl Pts',(55.3924090808014,44.8445846224044,12.));
#167736=CARTESIAN_POINT('Ctrl Pts',(55.3713206194967,44.8366146440901,0.));
#167737=CARTESIAN_POINT('Ctrl Pts',(55.3713206194967,44.8366146440901,12.));
#167738=CARTESIAN_POINT('Ctrl Pts',(55.3502831540228,44.8286396832848,0.));
#167739=CARTESIAN_POINT('Ctrl Pts',(55.3502831540228,44.8286396832848,12.));
#167740=CARTESIAN_POINT('Ctrl Pts',(55.3292967905725,44.8206598547888,0.));
#167741=CARTESIAN_POINT('Ctrl Pts',(55.3292967905725,44.8206598547888,12.));
#167742=CARTESIAN_POINT('Ctrl Pts',(55.3083616357605,44.8126752740208,0.));
#167743=CARTESIAN_POINT('Ctrl Pts',(55.3083616357605,44.8126752740208,12.));
#167744=CARTESIAN_POINT('Ctrl Pts',(55.287477796635,44.8046860570244,0.));
#167745=CARTESIAN_POINT('Ctrl Pts',(55.287477796635,44.8046860570244,12.));
#167746=CARTESIAN_POINT('Ctrl Pts',(55.2666453806883,44.796692320474,0.));
#167747=CARTESIAN_POINT('Ctrl Pts',(55.2666453806883,44.796692320474,12.));
#167748=CARTESIAN_POINT('Ctrl Pts',(55.2458644958617,44.7886941816823,0.));
#167749=CARTESIAN_POINT('Ctrl Pts',(55.2458644958617,44.7886941816823,12.));
#167750=CARTESIAN_POINT('Ctrl Pts',(55.2251352505474,44.7806917586077,0.));
#167751=CARTESIAN_POINT('Ctrl Pts',(55.2251352505474,44.7806917586077,12.));
#167752=CARTESIAN_POINT('Ctrl Pts',(55.2044577535865,44.7726851698618,0.));
#167753=CARTESIAN_POINT('Ctrl Pts',(55.2044577535865,44.7726851698618,12.));
#167754=CARTESIAN_POINT('Ctrl Pts',(55.1838321142777,44.7646745347108,0.));
#167755=CARTESIAN_POINT('Ctrl Pts',(55.1838321142777,44.7646745347108,12.));
#167756=CARTESIAN_POINT('Ctrl Pts',(55.1632584423813,44.7566599730771,0.));
#167757=CARTESIAN_POINT('Ctrl Pts',(55.1632584423813,44.7566599730771,12.));
#167758=CARTESIAN_POINT('Ctrl Pts',(55.1427368481201,44.748641605542,0.));
#167759=CARTESIAN_POINT('Ctrl Pts',(55.1427368481201,44.748641605542,12.));
#167760=CARTESIAN_POINT('Ctrl Pts',(55.1222674421747,44.7406195533483,0.));
#167761=CARTESIAN_POINT('Ctrl Pts',(55.1222674421747,44.7406195533483,12.));
#167762=CARTESIAN_POINT('Ctrl Pts',(55.1018503356806,44.7325939384042,0.));
#167763=CARTESIAN_POINT('Ctrl Pts',(55.1018503356806,44.7325939384042,12.));
#167764=CARTESIAN_POINT('Ctrl Pts',(55.0814856402507,44.7245648832988,0.));
#167765=CARTESIAN_POINT('Ctrl Pts',(55.0814856402507,44.7245648832988,12.));
#167766=CARTESIAN_POINT('Ctrl Pts',(55.0611734679902,44.7165325113165,0.));
#167767=CARTESIAN_POINT('Ctrl Pts',(55.0611734679902,44.7165325113165,12.));
#167768=CARTESIAN_POINT('Ctrl Pts',(55.0409139315074,44.7084969464509,0.));
#167769=CARTESIAN_POINT('Ctrl Pts',(55.0409139315074,44.7084969464509,12.));
#167770=CARTESIAN_POINT('Ctrl Pts',(55.020707143922,44.7004583134235,0.));
#167771=CARTESIAN_POINT('Ctrl Pts',(55.020707143922,44.7004583134235,12.));
#167772=CARTESIAN_POINT('Ctrl Pts',(55.0005532188644,44.6924167376851,0.));
#167773=CARTESIAN_POINT('Ctrl Pts',(55.0005532188644,44.6924167376851,12.));
#167774=CARTESIAN_POINT('Ctrl Pts',(54.9804522704668,44.6843723453985,0.));
#167775=CARTESIAN_POINT('Ctrl Pts',(54.9804522704668,44.6843723453985,12.));
#167776=CARTESIAN_POINT('Ctrl Pts',(54.9604044133497,44.6763252634255,0.));
#167777=CARTESIAN_POINT('Ctrl Pts',(54.9604044133497,44.6763252634255,12.));
#167778=CARTESIAN_POINT('Ctrl Pts',(54.9404097626088,44.6682756193156,0.));
#167779=CARTESIAN_POINT('Ctrl Pts',(54.9404097626088,44.6682756193156,12.));
#167780=CARTESIAN_POINT('Ctrl Pts',(54.9204684337845,44.6602235412854,0.));
#167781=CARTESIAN_POINT('Ctrl Pts',(54.9204684337845,44.6602235412854,12.));
#167782=CARTESIAN_POINT('Ctrl Pts',(54.9005805428991,44.6521691582551,0.));
#167783=CARTESIAN_POINT('Ctrl Pts',(54.9005805428991,44.6521691582551,12.));
#167784=CARTESIAN_POINT('Ctrl Pts',(54.8807462065177,44.6441125999074,0.));
#167785=CARTESIAN_POINT('Ctrl Pts',(54.8807462065177,44.6441125999074,12.));
#167786=CARTESIAN_POINT('Ctrl Pts',(54.860965541796,44.6360539967392,0.));
#167787=CARTESIAN_POINT('Ctrl Pts',(54.860965541796,44.6360539967392,12.));
#167788=CARTESIAN_POINT('Ctrl Pts',(54.8412386665264,44.6279934801159,0.));
#167789=CARTESIAN_POINT('Ctrl Pts',(54.8412386665264,44.6279934801159,12.));
#167790=CARTESIAN_POINT('Ctrl Pts',(54.8215656991817,44.6199311823276,0.));
#167791=CARTESIAN_POINT('Ctrl Pts',(54.8215656991817,44.6199311823276,12.));
#167792=CARTESIAN_POINT('Ctrl Pts',(54.8019467588257,44.6118672364889,0.));
#167793=CARTESIAN_POINT('Ctrl Pts',(54.8019467588257,44.6118672364889,12.));
#167794=CARTESIAN_POINT('Ctrl Pts',(54.7823819650137,44.60380177643,0.));
#167795=CARTESIAN_POINT('Ctrl Pts',(54.7823819650137,44.60380177643,12.));
#167796=CARTESIAN_POINT('Ctrl Pts',(54.7628714377041,44.5957349366062,0.));
#167797=CARTESIAN_POINT('Ctrl Pts',(54.7628714377041,44.5957349366062,12.));
#167798=CARTESIAN_POINT('Ctrl Pts',(54.7434152971285,44.5876668519676,0.));
#167799=CARTESIAN_POINT('Ctrl Pts',(54.7434152971285,44.5876668519676,12.));
#167800=CARTESIAN_POINT('Ctrl Pts',(54.7240136637744,44.5795976579476,0.));
#167801=CARTESIAN_POINT('Ctrl Pts',(54.7240136637744,44.5795976579476,12.));
#167802=CARTESIAN_POINT('Ctrl Pts',(54.7046666586776,44.5715274907637,0.));
#167803=CARTESIAN_POINT('Ctrl Pts',(54.7046666586776,44.5715274907637,12.));
#167804=CARTESIAN_POINT('Ctrl Pts',(54.685374403676,44.563456487687,0.));
#167805=CARTESIAN_POINT('Ctrl Pts',(54.685374403676,44.563456487687,12.));
#167806=CARTESIAN_POINT('Ctrl Pts',(54.6661370216242,44.5553847872712,0.));
#167807=CARTESIAN_POINT('Ctrl Pts',(54.6661370216242,44.5553847872712,12.));
#167808=CARTESIAN_POINT('Ctrl Pts',(54.6469546367381,44.5473125297289,0.));
#167809=CARTESIAN_POINT('Ctrl Pts',(54.6469546367381,44.5473125297289,12.));
#167810=CARTESIAN_POINT('Ctrl Pts',(54.6278273743554,44.5392398566775,0.));
#167811=CARTESIAN_POINT('Ctrl Pts',(54.6278273743554,44.5392398566775,12.));
#167812=CARTESIAN_POINT('Ctrl Pts',(54.6087553602889,44.5311669104495,0.));
#167813=CARTESIAN_POINT('Ctrl Pts',(54.6087553602889,44.5311669104495,12.));
#167814=CARTESIAN_POINT('Ctrl Pts',(54.5897387202812,44.5230938335165,0.));
#167815=CARTESIAN_POINT('Ctrl Pts',(54.5897387202812,44.5230938335165,12.));
#167816=CARTESIAN_POINT('Ctrl Pts',(54.5707775794436,44.5150207679007,0.));
#167817=CARTESIAN_POINT('Ctrl Pts',(54.5707775794436,44.5150207679007,12.));
#167818=CARTESIAN_POINT('Ctrl Pts',(54.5518720616056,44.5069478544977,0.));
#167819=CARTESIAN_POINT('Ctrl Pts',(54.5518720616056,44.5069478544977,12.));
#167820=CARTESIAN_POINT('Ctrl Pts',(54.5330222905475,44.4988752343744,0.));
#167821=CARTESIAN_POINT('Ctrl Pts',(54.5330222905475,44.4988752343744,12.));
#167822=CARTESIAN_POINT('Ctrl Pts',(54.5142283914704,44.4908030503225,0.));
#167823=CARTESIAN_POINT('Ctrl Pts',(54.5142283914704,44.4908030503225,12.));
#167824=CARTESIAN_POINT('Ctrl Pts',(54.495490492193,44.4827314481264,0.));
#167825=CARTESIAN_POINT('Ctrl Pts',(54.495490492193,44.4827314481264,12.));
#167826=CARTESIAN_POINT('Ctrl Pts',(54.4768087248824,44.4746605784031,0.));
#167827=CARTESIAN_POINT('Ctrl Pts',(54.4768087248824,44.4746605784031,12.));
#167828=CARTESIAN_POINT('Ctrl Pts',(54.4581832262033,44.4665905967668,0.));
#167829=CARTESIAN_POINT('Ctrl Pts',(54.4581832262033,44.4665905967668,12.));
#167830=CARTESIAN_POINT('Ctrl Pts',(54.4396141336978,44.4585216599908,0.));
#167831=CARTESIAN_POINT('Ctrl Pts',(54.4396141336978,44.4585216599908,12.));
#167832=CARTESIAN_POINT('Ctrl Pts',(54.421101582595,44.4504539226328,0.));
#167833=CARTESIAN_POINT('Ctrl Pts',(54.421101582595,44.4504539226328,12.));
#167834=CARTESIAN_POINT('Ctrl Pts',(54.4026457030335,44.4423875340996,0.));
#167835=CARTESIAN_POINT('Ctrl Pts',(54.4026457030335,44.4423875340996,12.));
#167836=CARTESIAN_POINT('Ctrl Pts',(54.3842466156196,44.4343226339593,0.));
#167837=CARTESIAN_POINT('Ctrl Pts',(54.3842466156196,44.4343226339593,12.));
#167838=CARTESIAN_POINT('Ctrl Pts',(54.3659044357119,44.4262593564712,0.));
#167839=CARTESIAN_POINT('Ctrl Pts',(54.3659044357119,44.4262593564712,12.));
#167840=CARTESIAN_POINT('Ctrl Pts',(54.3476192819352,44.4181978395851,0.));
#167841=CARTESIAN_POINT('Ctrl Pts',(54.3476192819352,44.4181978395851,12.));
#167842=CARTESIAN_POINT('Ctrl Pts',(54.3293912830237,44.4101382321834,0.));
#167843=CARTESIAN_POINT('Ctrl Pts',(54.3293912830237,44.4101382321834,12.));
#167844=CARTESIAN_POINT('Ctrl Pts',(54.3112205860716,44.402080702809,0.));
#167845=CARTESIAN_POINT('Ctrl Pts',(54.3112205860716,44.402080702809,12.));
#167846=CARTESIAN_POINT('Ctrl Pts',(54.2931073621553,44.3940254456331,0.));
#167847=CARTESIAN_POINT('Ctrl Pts',(54.2931073621553,44.3940254456331,12.));
#167848=CARTESIAN_POINT('Ctrl Pts',(54.2750517888579,44.3859726620183,0.));
#167849=CARTESIAN_POINT('Ctrl Pts',(54.2750517888579,44.3859726620183,12.));
#167850=CARTESIAN_POINT('Ctrl Pts',(54.2570540336475,44.3779225430406,0.));
#167851=CARTESIAN_POINT('Ctrl Pts',(54.2570540336475,44.3779225430406,12.));
#167852=CARTESIAN_POINT('Ctrl Pts',(54.2391142386412,44.3698752533562,0.));
#167853=CARTESIAN_POINT('Ctrl Pts',(54.2391142386412,44.3698752533562,12.));
#167854=CARTESIAN_POINT('Ctrl Pts',(54.2212325006052,44.361830910343,0.));
#167855=CARTESIAN_POINT('Ctrl Pts',(54.2212325006052,44.361830910343,12.));
#167856=CARTESIAN_POINT('Ctrl Pts',(54.2034088701928,44.3537895824096,0.));
#167857=CARTESIAN_POINT('Ctrl Pts',(54.2034088701928,44.3537895824096,12.));
#167858=CARTESIAN_POINT('Ctrl Pts',(54.1891964684727,44.3473589597726,0.));
#167859=CARTESIAN_POINT('Ctrl Pts',(54.1891964684727,44.3473589597726,12.));
#167860=CARTESIAN_POINT('Ctrl Pts',(54.1785633257639,44.3425373700993,0.));
#167861=CARTESIAN_POINT('Ctrl Pts',(54.1785633257639,44.3425373700993,12.));
#167862=CARTESIAN_POINT('Ctrl Pts',(54.1714861895346,44.3393235891075,0.));
#167863=CARTESIAN_POINT('Ctrl Pts',(54.1714861895346,44.3393235891075,12.));
#167864=CARTESIAN_POINT('Ctrl Pts',(54.1679505278134,44.3377168516418,0.));
#167865=CARTESIAN_POINT('Ctrl Pts',(54.1679505278134,44.3377168516418,12.));
#167866=CARTESIAN_POINT('',(54.1679505278134,44.3377168516418,12.));
#167867=CARTESIAN_POINT('Ctrl Pts',(54.1679505278134,44.3377168516418,12.));
#167868=CARTESIAN_POINT('Ctrl Pts',(54.1714861895346,44.3393235891075,12.));
#167869=CARTESIAN_POINT('Ctrl Pts',(54.1785633257639,44.3425373700993,12.));
#167870=CARTESIAN_POINT('Ctrl Pts',(54.1891964684727,44.3473589597726,12.));
#167871=CARTESIAN_POINT('Ctrl Pts',(54.2034088701928,44.3537895824096,12.));
#167872=CARTESIAN_POINT('Ctrl Pts',(54.2212325006052,44.361830910343,12.));
#167873=CARTESIAN_POINT('Ctrl Pts',(54.2391142386412,44.3698752533562,12.));
#167874=CARTESIAN_POINT('Ctrl Pts',(54.2570540336475,44.3779225430406,12.));
#167875=CARTESIAN_POINT('Ctrl Pts',(54.2750517888579,44.3859726620183,12.));
#167876=CARTESIAN_POINT('Ctrl Pts',(54.2931073621553,44.3940254456331,12.));
#167877=CARTESIAN_POINT('Ctrl Pts',(54.3112205860716,44.402080702809,12.));
#167878=CARTESIAN_POINT('Ctrl Pts',(54.3293912830237,44.4101382321834,12.));
#167879=CARTESIAN_POINT('Ctrl Pts',(54.3476192819352,44.4181978395851,12.));
#167880=CARTESIAN_POINT('Ctrl Pts',(54.3659044357119,44.4262593564712,12.));
#167881=CARTESIAN_POINT('Ctrl Pts',(54.3842466156196,44.4343226339593,12.));
#167882=CARTESIAN_POINT('Ctrl Pts',(54.4026457030335,44.4423875340996,12.));
#167883=CARTESIAN_POINT('Ctrl Pts',(54.421101582595,44.4504539226328,12.));
#167884=CARTESIAN_POINT('Ctrl Pts',(54.4396141336978,44.4585216599908,12.));
#167885=CARTESIAN_POINT('Ctrl Pts',(54.4581832262033,44.4665905967668,12.));
#167886=CARTESIAN_POINT('Ctrl Pts',(54.4768087248824,44.4746605784031,12.));
#167887=CARTESIAN_POINT('Ctrl Pts',(54.495490492193,44.4827314481264,12.));
#167888=CARTESIAN_POINT('Ctrl Pts',(54.5142283914704,44.4908030503225,12.));
#167889=CARTESIAN_POINT('Ctrl Pts',(54.5330222905475,44.4988752343744,12.));
#167890=CARTESIAN_POINT('Ctrl Pts',(54.5518720616056,44.5069478544977,12.));
#167891=CARTESIAN_POINT('Ctrl Pts',(54.5707775794436,44.5150207679007,12.));
#167892=CARTESIAN_POINT('Ctrl Pts',(54.5897387202812,44.5230938335165,12.));
#167893=CARTESIAN_POINT('Ctrl Pts',(54.6087553602889,44.5311669104495,12.));
#167894=CARTESIAN_POINT('Ctrl Pts',(54.6278273743554,44.5392398566775,12.));
#167895=CARTESIAN_POINT('Ctrl Pts',(54.6469546367381,44.5473125297289,12.));
#167896=CARTESIAN_POINT('Ctrl Pts',(54.6661370216242,44.5553847872712,12.));
#167897=CARTESIAN_POINT('Ctrl Pts',(54.685374403676,44.563456487687,12.));
#167898=CARTESIAN_POINT('Ctrl Pts',(54.7046666586776,44.5715274907637,12.));
#167899=CARTESIAN_POINT('Ctrl Pts',(54.7240136637744,44.5795976579476,12.));
#167900=CARTESIAN_POINT('Ctrl Pts',(54.7434152971285,44.5876668519676,12.));
#167901=CARTESIAN_POINT('Ctrl Pts',(54.7628714377041,44.5957349366062,12.));
#167902=CARTESIAN_POINT('Ctrl Pts',(54.7823819650137,44.60380177643,12.));
#167903=CARTESIAN_POINT('Ctrl Pts',(54.8019467588257,44.6118672364889,12.));
#167904=CARTESIAN_POINT('Ctrl Pts',(54.8215656991817,44.6199311823276,12.));
#167905=CARTESIAN_POINT('Ctrl Pts',(54.8412386665264,44.6279934801159,12.));
#167906=CARTESIAN_POINT('Ctrl Pts',(54.860965541796,44.6360539967392,12.));
#167907=CARTESIAN_POINT('Ctrl Pts',(54.8807462065177,44.6441125999074,12.));
#167908=CARTESIAN_POINT('Ctrl Pts',(54.9005805428991,44.6521691582551,12.));
#167909=CARTESIAN_POINT('Ctrl Pts',(54.9204684337845,44.6602235412854,12.));
#167910=CARTESIAN_POINT('Ctrl Pts',(54.9404097626088,44.6682756193156,12.));
#167911=CARTESIAN_POINT('Ctrl Pts',(54.9604044133497,44.6763252634255,12.));
#167912=CARTESIAN_POINT('Ctrl Pts',(54.9804522704668,44.6843723453985,12.));
#167913=CARTESIAN_POINT('Ctrl Pts',(55.0005532188644,44.6924167376851,12.));
#167914=CARTESIAN_POINT('Ctrl Pts',(55.020707143922,44.7004583134235,12.));
#167915=CARTESIAN_POINT('Ctrl Pts',(55.0409139315074,44.7084969464509,12.));
#167916=CARTESIAN_POINT('Ctrl Pts',(55.0611734679902,44.7165325113165,12.));
#167917=CARTESIAN_POINT('Ctrl Pts',(55.0814856402507,44.7245648832988,12.));
#167918=CARTESIAN_POINT('Ctrl Pts',(55.1018503356806,44.7325939384042,12.));
#167919=CARTESIAN_POINT('Ctrl Pts',(55.1222674421747,44.7406195533483,12.));
#167920=CARTESIAN_POINT('Ctrl Pts',(55.1427368481201,44.748641605542,12.));
#167921=CARTESIAN_POINT('Ctrl Pts',(55.1632584423813,44.7566599730771,12.));
#167922=CARTESIAN_POINT('Ctrl Pts',(55.1838321142777,44.7646745347108,12.));
#167923=CARTESIAN_POINT('Ctrl Pts',(55.2044577535865,44.7726851698618,12.));
#167924=CARTESIAN_POINT('Ctrl Pts',(55.2251352505474,44.7806917586077,12.));
#167925=CARTESIAN_POINT('Ctrl Pts',(55.2458644958617,44.7886941816823,12.));
#167926=CARTESIAN_POINT('Ctrl Pts',(55.2666453806883,44.796692320474,12.));
#167927=CARTESIAN_POINT('Ctrl Pts',(55.287477796635,44.8046860570244,12.));
#167928=CARTESIAN_POINT('Ctrl Pts',(55.3083616357605,44.8126752740208,12.));
#167929=CARTESIAN_POINT('Ctrl Pts',(55.3292967905725,44.8206598547888,12.));
#167930=CARTESIAN_POINT('Ctrl Pts',(55.3502831540228,44.8286396832848,12.));
#167931=CARTESIAN_POINT('Ctrl Pts',(55.3713206194967,44.8366146440901,12.));
#167932=CARTESIAN_POINT('Ctrl Pts',(55.3924090808014,44.8445846224044,12.));
#167933=CARTESIAN_POINT('Ctrl Pts',(55.4135484321718,44.8525495040408,12.));
#167934=CARTESIAN_POINT('Ctrl Pts',(55.4347385682704,44.8605091754214,12.));
#167935=CARTESIAN_POINT('Ctrl Pts',(55.4559793841836,44.8684635235725,12.));
#167936=CARTESIAN_POINT('Ctrl Pts',(55.4772707754126,44.8764124361207,12.));
#167937=CARTESIAN_POINT('Ctrl Pts',(55.4986126378656,44.8843558012886,12.));
#167938=CARTESIAN_POINT('Ctrl Pts',(55.5200048678629,44.8922935078889,12.));
#167939=CARTESIAN_POINT('Ctrl Pts',(55.541447362134,44.9002254453183,12.));
#167940=CARTESIAN_POINT('Ctrl Pts',(55.5629400178142,44.908151503553,12.));
#167941=CARTESIAN_POINT('Ctrl Pts',(55.5844827324338,44.9160715731443,12.));
#167942=CARTESIAN_POINT('Ctrl Pts',(55.6060754039121,44.9239855452144,12.));
#167943=CARTESIAN_POINT('Ctrl Pts',(55.6277179305633,44.9318933114507,12.));
#167944=CARTESIAN_POINT('Ctrl Pts',(55.6494102110935,44.9397947641007,12.));
#167945=CARTESIAN_POINT('Ctrl Pts',(55.6711521445979,44.9476897959685,12.));
#167946=CARTESIAN_POINT('Ctrl Pts',(55.6929436305489,44.9555783004106,12.));
#167947=CARTESIAN_POINT('Ctrl Pts',(55.714784568793,44.9634601713321,12.));
#167948=CARTESIAN_POINT('Ctrl Pts',(55.7366748595551,44.9713353031804,12.));
#167949=CARTESIAN_POINT('Ctrl Pts',(55.7586144034367,44.9792035909413,12.));
#167950=CARTESIAN_POINT('Ctrl Pts',(55.7806031014106,44.9870649301342,12.));
#167951=CARTESIAN_POINT('Ctrl Pts',(55.8026408548105,44.9949192168093,12.));
#167952=CARTESIAN_POINT('Ctrl Pts',(55.8247275653289,45.0027663475433,12.));
#167953=CARTESIAN_POINT('Ctrl Pts',(55.8468631350218,45.0106062194342,12.));
#167954=CARTESIAN_POINT('Ctrl Pts',(55.8690474663065,45.0184387300973,12.));
#167955=CARTESIAN_POINT('Ctrl Pts',(55.8912804619577,45.0262637776615,12.));
#167956=CARTESIAN_POINT('Ctrl Pts',(55.9135620250954,45.0340812607657,12.));
#167957=CARTESIAN_POINT('Ctrl Pts',(55.9358920591837,45.0418910785551,12.));
#167958=CARTESIAN_POINT('Ctrl Pts',(55.9582704680356,45.0496931306755,12.));
#167959=CARTESIAN_POINT('Ctrl Pts',(55.9806971558097,45.0574873172695,12.));
#167960=CARTESIAN_POINT('Ctrl Pts',(56.003172027008,45.0652735389733,12.));
#167961=CARTESIAN_POINT('Ctrl Pts',(56.0256949864639,45.0730516969149,12.));
#167962=CARTESIAN_POINT('Ctrl Pts',(56.048265939342,45.0808216927089,12.));
#167963=CARTESIAN_POINT('Ctrl Pts',(56.0708847911416,45.0885834284517,12.));
#167964=CARTESIAN_POINT('Ctrl Pts',(56.0935514476945,45.0963368067177,12.));
#167965=CARTESIAN_POINT('Ctrl Pts',(56.116265815162,45.1040817305561,12.));
#167966=CARTESIAN_POINT('Ctrl Pts',(56.1390278000226,45.1118181034888,12.));
#167967=CARTESIAN_POINT('Ctrl Pts',(56.1618373090732,45.1195458295063,12.));
#167968=CARTESIAN_POINT('Ctrl Pts',(56.1846942494325,45.127264813063,12.));
#167969=CARTESIAN_POINT('Ctrl Pts',(56.2075985285393,45.1349749590738,12.));
#167970=CARTESIAN_POINT('Ctrl Pts',(56.2305500541489,45.1426761729105,12.));
#167971=CARTESIAN_POINT('Ctrl Pts',(56.2535487343221,45.1503683604005,12.));
#167972=CARTESIAN_POINT('Ctrl Pts',(56.2765944774245,45.1580514278223,12.));
#167973=CARTESIAN_POINT('Ctrl Pts',(56.2996871921316,45.1657252819013,12.));
#167974=CARTESIAN_POINT('Ctrl Pts',(56.3228267874264,45.1733898298061,12.));
#167975=CARTESIAN_POINT('Ctrl Pts',(56.3460131725964,45.1810449791453,12.));
#167976=CARTESIAN_POINT('Ctrl Pts',(56.3692462572231,45.1886906379667,12.));
#167977=CARTESIAN_POINT('Ctrl Pts',(56.3925259511806,45.1963267147529,12.));
#167978=CARTESIAN_POINT('Ctrl Pts',(56.4158521646411,45.2039531184172,12.));
#167979=CARTESIAN_POINT('Ctrl Pts',(56.4392248080732,45.2115697583001,12.));
#167980=CARTESIAN_POINT('Ctrl Pts',(56.4626437922386,45.2191765441667,12.));
#167981=CARTESIAN_POINT('Ctrl Pts',(56.4861090281823,45.2267733862049,12.));
#167982=CARTESIAN_POINT('Ctrl Pts',(56.5096204272306,45.2343601950228,12.));
#167983=CARTESIAN_POINT('Ctrl Pts',(56.5331779009958,45.2419368816429,12.));
#167984=CARTESIAN_POINT('Ctrl Pts',(56.5567813613756,45.2495033575,12.));
#167985=CARTESIAN_POINT('Ctrl Pts',(56.5804307205505,45.257059534438,12.));
#167986=CARTESIAN_POINT('Ctrl Pts',(56.6041258909741,45.2646053247087,12.));
#167987=CARTESIAN_POINT('Ctrl Pts',(56.6278667853702,45.2721406409695,12.));
#167988=CARTESIAN_POINT('Ctrl Pts',(56.6516533167384,45.2796653962785,12.));
#167989=CARTESIAN_POINT('Ctrl Pts',(56.6754853983528,45.2871795040906,12.));
#167990=CARTESIAN_POINT('Ctrl Pts',(56.69936294376,45.2946828782559,12.));
#167991=CARTESIAN_POINT('Ctrl Pts',(56.7232858667709,45.3021754330179,12.));
#167992=CARTESIAN_POINT('Ctrl Pts',(56.7472540814553,45.3096570830118,12.));
#167993=CARTESIAN_POINT('Ctrl Pts',(56.7712675021491,45.31712774326,12.));
#167994=CARTESIAN_POINT('Ctrl Pts',(56.7953260434524,45.3245873291684,12.));
#167995=CARTESIAN_POINT('Ctrl Pts',(56.8194296202291,45.332035756524,12.));
#167996=CARTESIAN_POINT('Ctrl Pts',(56.8435781475981,45.3394729414931,12.));
#167997=CARTESIAN_POINT('Ctrl Pts',(56.8677715409268,45.3468988006203,12.));
#167998=CARTESIAN_POINT('Ctrl Pts',(56.8920097158377,45.3543132508239,12.));
#167999=CARTESIAN_POINT('Ctrl Pts',(56.9162925882085,45.3617162093923,12.));
#168000=CARTESIAN_POINT('Ctrl Pts',(56.9406200741714,45.3691075939827,12.));
#168001=CARTESIAN_POINT('Ctrl Pts',(56.9649920901073,45.3764873226196,12.));
#168002=CARTESIAN_POINT('Ctrl Pts',(56.9894085526373,45.3838553136948,12.));
#168003=CARTESIAN_POINT('Ctrl Pts',(57.0138693786278,45.3912114859616,12.));
#168004=CARTESIAN_POINT('Ctrl Pts',(57.0383744851913,45.3985557585311,12.));
#168005=CARTESIAN_POINT('Ctrl Pts',(57.0629237896848,45.4058880508693,12.));
#168006=CARTESIAN_POINT('Ctrl Pts',(57.0875172097051,45.4132082827948,12.));
#168007=CARTESIAN_POINT('Ctrl Pts',(57.112154663078,45.4205163744782,12.));
#168008=CARTESIAN_POINT('Ctrl Pts',(57.136836067863,45.4278122464389,12.));
#168009=CARTESIAN_POINT('Ctrl Pts',(57.1615613423584,45.4350958195434,12.));
#168010=CARTESIAN_POINT('Ctrl Pts',(57.186330405101,45.4423670150034,12.));
#168011=CARTESIAN_POINT('Ctrl Pts',(57.2111431748631,45.4496257543759,12.));
#168012=CARTESIAN_POINT('Ctrl Pts',(57.2359995706447,45.4568719595642,12.));
#168013=CARTESIAN_POINT('Ctrl Pts',(57.2608995116733,45.4641055528141,12.));
#168014=CARTESIAN_POINT('Ctrl Pts',(57.2858429174062,45.4713264567063,12.));
#168015=CARTESIAN_POINT('Ctrl Pts',(57.3108297075265,45.4785345941507,12.));
#168016=CARTESIAN_POINT('Ctrl Pts',(57.3358598019389,45.4857298883824,12.));
#168017=CARTESIAN_POINT('Ctrl Pts',(57.3609331207574,45.4929122629572,12.));
#168018=CARTESIAN_POINT('Ctrl Pts',(57.3860495843033,45.500081641751,12.));
#168019=CARTESIAN_POINT('Ctrl Pts',(57.4112091131183,45.5072379489631,12.));
#168020=CARTESIAN_POINT('Ctrl Pts',(57.4364116279702,45.5143811091205,12.));
#168021=CARTESIAN_POINT('Ctrl Pts',(57.4616570498568,45.5215110470825,12.));
#168022=CARTESIAN_POINT('Ctrl Pts',(57.4869453000063,45.5286276880485,12.));
#168023=CARTESIAN_POINT('Ctrl Pts',(57.5122762998745,45.5357309575611,12.));
#168024=CARTESIAN_POINT('Ctrl Pts',(57.537649971135,45.542820781484,12.));
#168025=CARTESIAN_POINT('Ctrl Pts',(57.563066235668,45.5498970859835,12.));
#168026=CARTESIAN_POINT('Ctrl Pts',(57.5885250155433,45.5569597975096,12.));
#168027=CARTESIAN_POINT('Ctrl Pts',(57.614026233004,45.5640088427813,12.));
#168028=CARTESIAN_POINT('Ctrl Pts',(57.6395698104404,45.5710441487674,12.));
#168029=CARTESIAN_POINT('Ctrl Pts',(57.6651556704237,45.5780656427163,12.));
#168030=CARTESIAN_POINT('Ctrl Pts',(57.6907837357417,45.5850732521896,12.));
#168031=CARTESIAN_POINT('Ctrl Pts',(57.7164539294314,45.5920669050986,12.));
#168032=CARTESIAN_POINT('Ctrl Pts',(57.7421661748026,45.5990465297344,12.));
#168033=CARTESIAN_POINT('Ctrl Pts',(57.7679203954742,45.6060120548205,12.));
#168034=CARTESIAN_POINT('Ctrl Pts',(57.7937165153387,45.6129634094683,12.));
#168035=CARTESIAN_POINT('Ctrl Pts',(57.8195544584845,45.6199005230784,12.));
#168036=CARTESIAN_POINT('Ctrl Pts',(57.8454341491238,45.6268233252544,12.));
#168037=CARTESIAN_POINT('Ctrl Pts',(57.8713555115232,45.6337317457252,12.));
#168038=CARTESIAN_POINT('Ctrl Pts',(57.8973184699034,45.6406257142382,12.));
#168039=CARTESIAN_POINT('Ctrl Pts',(57.9233229484311,45.6475051605535,12.));
#168040=CARTESIAN_POINT('Ctrl Pts',(57.9493688714237,45.6543700146679,12.));
#168041=CARTESIAN_POINT('Ctrl Pts',(57.9754561635061,45.661220206992,12.));
#168042=CARTESIAN_POINT('Ctrl Pts',(58.0015847497837,45.6680556685493,12.));
#168043=CARTESIAN_POINT('Ctrl Pts',(58.0277545560012,45.6748763311643,12.));
#168044=CARTESIAN_POINT('Ctrl Pts',(58.0539655087117,45.6816821276678,12.));
#168045=CARTESIAN_POINT('Ctrl Pts',(58.0802175348966,45.6884729914485,12.));
#168046=CARTESIAN_POINT('Ctrl Pts',(58.1065105615907,45.695248856015,12.));
#168047=CARTESIAN_POINT('Ctrl Pts',(58.1328445154676,45.702009654518,12.));
#168048=CARTESIAN_POINT('Ctrl Pts',(58.1592193225137,45.7087553193771,12.));
#168049=CARTESIAN_POINT('Ctrl Pts',(58.185634907469,45.7154857816483,12.));
#168050=CARTESIAN_POINT('Ctrl Pts',(58.2120911942772,45.7222009715397,12.));
#168051=CARTESIAN_POINT('Ctrl Pts',(58.2385881070913,45.7289008195579,12.));
#168052=CARTESIAN_POINT('Ctrl Pts',(58.2651255711453,45.7355852575107,12.));
#168053=CARTESIAN_POINT('Ctrl Pts',(58.291703513584,45.742254219463,12.));
#168054=CARTESIAN_POINT('Ctrl Pts',(58.3183218645316,45.7489076429763,12.));
#168055=CARTESIAN_POINT('Ctrl Pts',(58.3449805573423,45.755545469402,12.));
#168056=CARTESIAN_POINT('Ctrl Pts',(58.3678667473437,45.7612219538124,12.));
#168057=CARTESIAN_POINT('Ctrl Pts',(58.3854348517442,45.7655655205367,12.));
#168058=CARTESIAN_POINT('Ctrl Pts',(58.3976670481067,45.7685831165564,12.));
#168059=CARTESIAN_POINT('Ctrl Pts',(58.4045515723353,45.7702793558176,12.));
#168060=CARTESIAN_POINT('Ctrl Pts',(58.4060826907792,45.7706564944895,12.));
#168061=CARTESIAN_POINT('',(54.1679505278134,44.3377168516418,0.));
#168062=CARTESIAN_POINT('',(54.1679505278134,44.3377168516418,0.));
#168063=CARTESIAN_POINT('Ctrl Pts',(58.4060826907792,45.7706564944895,0.));
#168064=CARTESIAN_POINT('Ctrl Pts',(58.4045515723353,45.7702793558176,0.));
#168065=CARTESIAN_POINT('Ctrl Pts',(58.3976670481067,45.7685831165564,0.));
#168066=CARTESIAN_POINT('Ctrl Pts',(58.3854348517442,45.7655655205367,0.));
#168067=CARTESIAN_POINT('Ctrl Pts',(58.3678667473437,45.7612219538124,0.));
#168068=CARTESIAN_POINT('Ctrl Pts',(58.3449805573423,45.755545469402,0.));
#168069=CARTESIAN_POINT('Ctrl Pts',(58.3183218645316,45.7489076429763,0.));
#168070=CARTESIAN_POINT('Ctrl Pts',(58.291703513584,45.742254219463,0.));
#168071=CARTESIAN_POINT('Ctrl Pts',(58.2651255711453,45.7355852575107,0.));
#168072=CARTESIAN_POINT('Ctrl Pts',(58.2385881070913,45.7289008195579,0.));
#168073=CARTESIAN_POINT('Ctrl Pts',(58.2120911942772,45.7222009715397,0.));
#168074=CARTESIAN_POINT('Ctrl Pts',(58.185634907469,45.7154857816483,0.));
#168075=CARTESIAN_POINT('Ctrl Pts',(58.1592193225137,45.7087553193771,0.));
#168076=CARTESIAN_POINT('Ctrl Pts',(58.1328445154676,45.702009654518,0.));
#168077=CARTESIAN_POINT('Ctrl Pts',(58.1065105615907,45.695248856015,0.));
#168078=CARTESIAN_POINT('Ctrl Pts',(58.0802175348966,45.6884729914485,0.));
#168079=CARTESIAN_POINT('Ctrl Pts',(58.0539655087117,45.6816821276678,0.));
#168080=CARTESIAN_POINT('Ctrl Pts',(58.0277545560012,45.6748763311643,0.));
#168081=CARTESIAN_POINT('Ctrl Pts',(58.0015847497837,45.6680556685493,0.));
#168082=CARTESIAN_POINT('Ctrl Pts',(57.9754561635061,45.661220206992,0.));
#168083=CARTESIAN_POINT('Ctrl Pts',(57.9493688714237,45.6543700146679,0.));
#168084=CARTESIAN_POINT('Ctrl Pts',(57.9233229484311,45.6475051605535,0.));
#168085=CARTESIAN_POINT('Ctrl Pts',(57.8973184699034,45.6406257142382,0.));
#168086=CARTESIAN_POINT('Ctrl Pts',(57.8713555115232,45.6337317457252,0.));
#168087=CARTESIAN_POINT('Ctrl Pts',(57.8454341491238,45.6268233252544,0.));
#168088=CARTESIAN_POINT('Ctrl Pts',(57.8195544584845,45.6199005230784,0.));
#168089=CARTESIAN_POINT('Ctrl Pts',(57.7937165153387,45.6129634094683,0.));
#168090=CARTESIAN_POINT('Ctrl Pts',(57.7679203954742,45.6060120548205,0.));
#168091=CARTESIAN_POINT('Ctrl Pts',(57.7421661748026,45.5990465297344,0.));
#168092=CARTESIAN_POINT('Ctrl Pts',(57.7164539294314,45.5920669050986,0.));
#168093=CARTESIAN_POINT('Ctrl Pts',(57.6907837357417,45.5850732521896,0.));
#168094=CARTESIAN_POINT('Ctrl Pts',(57.6651556704237,45.5780656427163,0.));
#168095=CARTESIAN_POINT('Ctrl Pts',(57.6395698104404,45.5710441487674,0.));
#168096=CARTESIAN_POINT('Ctrl Pts',(57.614026233004,45.5640088427813,0.));
#168097=CARTESIAN_POINT('Ctrl Pts',(57.5885250155433,45.5569597975096,0.));
#168098=CARTESIAN_POINT('Ctrl Pts',(57.563066235668,45.5498970859835,0.));
#168099=CARTESIAN_POINT('Ctrl Pts',(57.537649971135,45.542820781484,0.));
#168100=CARTESIAN_POINT('Ctrl Pts',(57.5122762998745,45.5357309575611,0.));
#168101=CARTESIAN_POINT('Ctrl Pts',(57.4869453000063,45.5286276880485,0.));
#168102=CARTESIAN_POINT('Ctrl Pts',(57.4616570498568,45.5215110470825,0.));
#168103=CARTESIAN_POINT('Ctrl Pts',(57.4364116279702,45.5143811091205,0.));
#168104=CARTESIAN_POINT('Ctrl Pts',(57.4112091131183,45.5072379489631,0.));
#168105=CARTESIAN_POINT('Ctrl Pts',(57.3860495843033,45.500081641751,0.));
#168106=CARTESIAN_POINT('Ctrl Pts',(57.3609331207574,45.4929122629572,0.));
#168107=CARTESIAN_POINT('Ctrl Pts',(57.3358598019389,45.4857298883824,0.));
#168108=CARTESIAN_POINT('Ctrl Pts',(57.3108297075265,45.4785345941507,0.));
#168109=CARTESIAN_POINT('Ctrl Pts',(57.2858429174062,45.4713264567063,0.));
#168110=CARTESIAN_POINT('Ctrl Pts',(57.2608995116733,45.4641055528141,0.));
#168111=CARTESIAN_POINT('Ctrl Pts',(57.2359995706447,45.4568719595642,0.));
#168112=CARTESIAN_POINT('Ctrl Pts',(57.2111431748631,45.4496257543759,0.));
#168113=CARTESIAN_POINT('Ctrl Pts',(57.186330405101,45.4423670150034,0.));
#168114=CARTESIAN_POINT('Ctrl Pts',(57.1615613423584,45.4350958195434,0.));
#168115=CARTESIAN_POINT('Ctrl Pts',(57.136836067863,45.4278122464389,0.));
#168116=CARTESIAN_POINT('Ctrl Pts',(57.112154663078,45.4205163744782,0.));
#168117=CARTESIAN_POINT('Ctrl Pts',(57.0875172097051,45.4132082827948,0.));
#168118=CARTESIAN_POINT('Ctrl Pts',(57.0629237896848,45.4058880508693,0.));
#168119=CARTESIAN_POINT('Ctrl Pts',(57.0383744851913,45.3985557585311,0.));
#168120=CARTESIAN_POINT('Ctrl Pts',(57.0138693786278,45.3912114859616,0.));
#168121=CARTESIAN_POINT('Ctrl Pts',(56.9894085526373,45.3838553136948,0.));
#168122=CARTESIAN_POINT('Ctrl Pts',(56.9649920901073,45.3764873226196,0.));
#168123=CARTESIAN_POINT('Ctrl Pts',(56.9406200741714,45.3691075939827,0.));
#168124=CARTESIAN_POINT('Ctrl Pts',(56.9162925882085,45.3617162093923,0.));
#168125=CARTESIAN_POINT('Ctrl Pts',(56.8920097158377,45.3543132508239,0.));
#168126=CARTESIAN_POINT('Ctrl Pts',(56.8677715409268,45.3468988006203,0.));
#168127=CARTESIAN_POINT('Ctrl Pts',(56.8435781475981,45.3394729414931,0.));
#168128=CARTESIAN_POINT('Ctrl Pts',(56.8194296202291,45.332035756524,0.));
#168129=CARTESIAN_POINT('Ctrl Pts',(56.7953260434524,45.3245873291684,0.));
#168130=CARTESIAN_POINT('Ctrl Pts',(56.7712675021491,45.31712774326,0.));
#168131=CARTESIAN_POINT('Ctrl Pts',(56.7472540814553,45.3096570830118,0.));
#168132=CARTESIAN_POINT('Ctrl Pts',(56.7232858667709,45.3021754330179,0.));
#168133=CARTESIAN_POINT('Ctrl Pts',(56.69936294376,45.2946828782559,0.));
#168134=CARTESIAN_POINT('Ctrl Pts',(56.6754853983528,45.2871795040906,0.));
#168135=CARTESIAN_POINT('Ctrl Pts',(56.6516533167384,45.2796653962785,0.));
#168136=CARTESIAN_POINT('Ctrl Pts',(56.6278667853702,45.2721406409695,0.));
#168137=CARTESIAN_POINT('Ctrl Pts',(56.6041258909741,45.2646053247087,0.));
#168138=CARTESIAN_POINT('Ctrl Pts',(56.5804307205505,45.257059534438,0.));
#168139=CARTESIAN_POINT('Ctrl Pts',(56.5567813613756,45.2495033575,0.));
#168140=CARTESIAN_POINT('Ctrl Pts',(56.5331779009958,45.2419368816429,0.));
#168141=CARTESIAN_POINT('Ctrl Pts',(56.5096204272306,45.2343601950228,0.));
#168142=CARTESIAN_POINT('Ctrl Pts',(56.4861090281823,45.2267733862049,0.));
#168143=CARTESIAN_POINT('Ctrl Pts',(56.4626437922386,45.2191765441667,0.));
#168144=CARTESIAN_POINT('Ctrl Pts',(56.4392248080732,45.2115697583001,0.));
#168145=CARTESIAN_POINT('Ctrl Pts',(56.4158521646411,45.2039531184172,0.));
#168146=CARTESIAN_POINT('Ctrl Pts',(56.3925259511806,45.1963267147529,0.));
#168147=CARTESIAN_POINT('Ctrl Pts',(56.3692462572231,45.1886906379667,0.));
#168148=CARTESIAN_POINT('Ctrl Pts',(56.3460131725964,45.1810449791453,0.));
#168149=CARTESIAN_POINT('Ctrl Pts',(56.3228267874264,45.1733898298061,0.));
#168150=CARTESIAN_POINT('Ctrl Pts',(56.2996871921316,45.1657252819013,0.));
#168151=CARTESIAN_POINT('Ctrl Pts',(56.2765944774245,45.1580514278223,0.));
#168152=CARTESIAN_POINT('Ctrl Pts',(56.2535487343221,45.1503683604005,0.));
#168153=CARTESIAN_POINT('Ctrl Pts',(56.2305500541489,45.1426761729105,0.));
#168154=CARTESIAN_POINT('Ctrl Pts',(56.2075985285393,45.1349749590738,0.));
#168155=CARTESIAN_POINT('Ctrl Pts',(56.1846942494325,45.127264813063,0.));
#168156=CARTESIAN_POINT('Ctrl Pts',(56.1618373090732,45.1195458295063,0.));
#168157=CARTESIAN_POINT('Ctrl Pts',(56.1390278000226,45.1118181034888,0.));
#168158=CARTESIAN_POINT('Ctrl Pts',(56.116265815162,45.1040817305561,0.));
#168159=CARTESIAN_POINT('Ctrl Pts',(56.0935514476945,45.0963368067177,0.));
#168160=CARTESIAN_POINT('Ctrl Pts',(56.0708847911416,45.0885834284517,0.));
#168161=CARTESIAN_POINT('Ctrl Pts',(56.048265939342,45.0808216927089,0.));
#168162=CARTESIAN_POINT('Ctrl Pts',(56.0256949864639,45.0730516969149,0.));
#168163=CARTESIAN_POINT('Ctrl Pts',(56.003172027008,45.0652735389733,0.));
#168164=CARTESIAN_POINT('Ctrl Pts',(55.9806971558097,45.0574873172695,0.));
#168165=CARTESIAN_POINT('Ctrl Pts',(55.9582704680356,45.0496931306755,0.));
#168166=CARTESIAN_POINT('Ctrl Pts',(55.9358920591837,45.0418910785551,0.));
#168167=CARTESIAN_POINT('Ctrl Pts',(55.9135620250954,45.0340812607657,0.));
#168168=CARTESIAN_POINT('Ctrl Pts',(55.8912804619577,45.0262637776615,0.));
#168169=CARTESIAN_POINT('Ctrl Pts',(55.8690474663065,45.0184387300973,0.));
#168170=CARTESIAN_POINT('Ctrl Pts',(55.8468631350218,45.0106062194342,0.));
#168171=CARTESIAN_POINT('Ctrl Pts',(55.8247275653289,45.0027663475433,0.));
#168172=CARTESIAN_POINT('Ctrl Pts',(55.8026408548105,44.9949192168093,0.));
#168173=CARTESIAN_POINT('Ctrl Pts',(55.7806031014106,44.9870649301342,0.));
#168174=CARTESIAN_POINT('Ctrl Pts',(55.7586144034367,44.9792035909413,0.));
#168175=CARTESIAN_POINT('Ctrl Pts',(55.7366748595551,44.9713353031804,0.));
#168176=CARTESIAN_POINT('Ctrl Pts',(55.714784568793,44.9634601713321,0.));
#168177=CARTESIAN_POINT('Ctrl Pts',(55.6929436305489,44.9555783004106,0.));
#168178=CARTESIAN_POINT('Ctrl Pts',(55.6711521445979,44.9476897959685,0.));
#168179=CARTESIAN_POINT('Ctrl Pts',(55.6494102110935,44.9397947641007,0.));
#168180=CARTESIAN_POINT('Ctrl Pts',(55.6277179305633,44.9318933114507,0.));
#168181=CARTESIAN_POINT('Ctrl Pts',(55.6060754039121,44.9239855452144,0.));
#168182=CARTESIAN_POINT('Ctrl Pts',(55.5844827324338,44.9160715731443,0.));
#168183=CARTESIAN_POINT('Ctrl Pts',(55.5629400178142,44.908151503553,0.));
#168184=CARTESIAN_POINT('Ctrl Pts',(55.541447362134,44.9002254453183,0.));
#168185=CARTESIAN_POINT('Ctrl Pts',(55.5200048678629,44.8922935078889,0.));
#168186=CARTESIAN_POINT('Ctrl Pts',(55.4986126378656,44.8843558012886,0.));
#168187=CARTESIAN_POINT('Ctrl Pts',(55.4772707754126,44.8764124361207,0.));
#168188=CARTESIAN_POINT('Ctrl Pts',(55.4559793841836,44.8684635235725,0.));
#168189=CARTESIAN_POINT('Ctrl Pts',(55.4347385682704,44.8605091754214,0.));
#168190=CARTESIAN_POINT('Ctrl Pts',(55.4135484321718,44.8525495040408,0.));
#168191=CARTESIAN_POINT('Ctrl Pts',(55.3924090808014,44.8445846224044,0.));
#168192=CARTESIAN_POINT('Ctrl Pts',(55.3713206194967,44.8366146440901,0.));
#168193=CARTESIAN_POINT('Ctrl Pts',(55.3502831540228,44.8286396832848,0.));
#168194=CARTESIAN_POINT('Ctrl Pts',(55.3292967905725,44.8206598547888,0.));
#168195=CARTESIAN_POINT('Ctrl Pts',(55.3083616357605,44.8126752740208,0.));
#168196=CARTESIAN_POINT('Ctrl Pts',(55.287477796635,44.8046860570244,0.));
#168197=CARTESIAN_POINT('Ctrl Pts',(55.2666453806883,44.796692320474,0.));
#168198=CARTESIAN_POINT('Ctrl Pts',(55.2458644958617,44.7886941816823,0.));
#168199=CARTESIAN_POINT('Ctrl Pts',(55.2251352505474,44.7806917586077,0.));
#168200=CARTESIAN_POINT('Ctrl Pts',(55.2044577535865,44.7726851698618,0.));
#168201=CARTESIAN_POINT('Ctrl Pts',(55.1838321142777,44.7646745347108,0.));
#168202=CARTESIAN_POINT('Ctrl Pts',(55.1632584423813,44.7566599730771,0.));
#168203=CARTESIAN_POINT('Ctrl Pts',(55.1427368481201,44.748641605542,0.));
#168204=CARTESIAN_POINT('Ctrl Pts',(55.1222674421747,44.7406195533483,0.));
#168205=CARTESIAN_POINT('Ctrl Pts',(55.1018503356806,44.7325939384042,0.));
#168206=CARTESIAN_POINT('Ctrl Pts',(55.0814856402507,44.7245648832988,0.));
#168207=CARTESIAN_POINT('Ctrl Pts',(55.0611734679902,44.7165325113165,0.));
#168208=CARTESIAN_POINT('Ctrl Pts',(55.0409139315074,44.7084969464509,0.));
#168209=CARTESIAN_POINT('Ctrl Pts',(55.020707143922,44.7004583134235,0.));
#168210=CARTESIAN_POINT('Ctrl Pts',(55.0005532188644,44.6924167376851,0.));
#168211=CARTESIAN_POINT('Ctrl Pts',(54.9804522704668,44.6843723453985,0.));
#168212=CARTESIAN_POINT('Ctrl Pts',(54.9604044133497,44.6763252634255,0.));
#168213=CARTESIAN_POINT('Ctrl Pts',(54.9404097626088,44.6682756193156,0.));
#168214=CARTESIAN_POINT('Ctrl Pts',(54.9204684337845,44.6602235412854,0.));
#168215=CARTESIAN_POINT('Ctrl Pts',(54.9005805428991,44.6521691582551,0.));
#168216=CARTESIAN_POINT('Ctrl Pts',(54.8807462065177,44.6441125999074,0.));
#168217=CARTESIAN_POINT('Ctrl Pts',(54.860965541796,44.6360539967392,0.));
#168218=CARTESIAN_POINT('Ctrl Pts',(54.8412386665264,44.6279934801159,0.));
#168219=CARTESIAN_POINT('Ctrl Pts',(54.8215656991817,44.6199311823276,0.));
#168220=CARTESIAN_POINT('Ctrl Pts',(54.8019467588257,44.6118672364889,0.));
#168221=CARTESIAN_POINT('Ctrl Pts',(54.7823819650137,44.60380177643,0.));
#168222=CARTESIAN_POINT('Ctrl Pts',(54.7628714377041,44.5957349366062,0.));
#168223=CARTESIAN_POINT('Ctrl Pts',(54.7434152971285,44.5876668519676,0.));
#168224=CARTESIAN_POINT('Ctrl Pts',(54.7240136637744,44.5795976579476,0.));
#168225=CARTESIAN_POINT('Ctrl Pts',(54.7046666586776,44.5715274907637,0.));
#168226=CARTESIAN_POINT('Ctrl Pts',(54.685374403676,44.563456487687,0.));
#168227=CARTESIAN_POINT('Ctrl Pts',(54.6661370216242,44.5553847872712,0.));
#168228=CARTESIAN_POINT('Ctrl Pts',(54.6469546367381,44.5473125297289,0.));
#168229=CARTESIAN_POINT('Ctrl Pts',(54.6278273743554,44.5392398566775,0.));
#168230=CARTESIAN_POINT('Ctrl Pts',(54.6087553602889,44.5311669104495,0.));
#168231=CARTESIAN_POINT('Ctrl Pts',(54.5897387202812,44.5230938335165,0.));
#168232=CARTESIAN_POINT('Ctrl Pts',(54.5707775794436,44.5150207679007,0.));
#168233=CARTESIAN_POINT('Ctrl Pts',(54.5518720616056,44.5069478544977,0.));
#168234=CARTESIAN_POINT('Ctrl Pts',(54.5330222905475,44.4988752343744,0.));
#168235=CARTESIAN_POINT('Ctrl Pts',(54.5142283914704,44.4908030503225,0.));
#168236=CARTESIAN_POINT('Ctrl Pts',(54.495490492193,44.4827314481264,0.));
#168237=CARTESIAN_POINT('Ctrl Pts',(54.4768087248824,44.4746605784031,0.));
#168238=CARTESIAN_POINT('Ctrl Pts',(54.4581832262033,44.4665905967668,0.));
#168239=CARTESIAN_POINT('Ctrl Pts',(54.4396141336978,44.4585216599908,0.));
#168240=CARTESIAN_POINT('Ctrl Pts',(54.421101582595,44.4504539226328,0.));
#168241=CARTESIAN_POINT('Ctrl Pts',(54.4026457030335,44.4423875340996,0.));
#168242=CARTESIAN_POINT('Ctrl Pts',(54.3842466156196,44.4343226339593,0.));
#168243=CARTESIAN_POINT('Ctrl Pts',(54.3659044357119,44.4262593564712,0.));
#168244=CARTESIAN_POINT('Ctrl Pts',(54.3476192819352,44.4181978395851,0.));
#168245=CARTESIAN_POINT('Ctrl Pts',(54.3293912830237,44.4101382321834,0.));
#168246=CARTESIAN_POINT('Ctrl Pts',(54.3112205860716,44.402080702809,0.));
#168247=CARTESIAN_POINT('Ctrl Pts',(54.2931073621553,44.3940254456331,0.));
#168248=CARTESIAN_POINT('Ctrl Pts',(54.2750517888579,44.3859726620183,0.));
#168249=CARTESIAN_POINT('Ctrl Pts',(54.2570540336475,44.3779225430406,0.));
#168250=CARTESIAN_POINT('Ctrl Pts',(54.2391142386412,44.3698752533562,0.));
#168251=CARTESIAN_POINT('Ctrl Pts',(54.2212325006052,44.361830910343,0.));
#168252=CARTESIAN_POINT('Ctrl Pts',(54.2034088701928,44.3537895824096,0.));
#168253=CARTESIAN_POINT('Ctrl Pts',(54.1891964684727,44.3473589597726,0.));
#168254=CARTESIAN_POINT('Ctrl Pts',(54.1785633257639,44.3425373700993,0.));
#168255=CARTESIAN_POINT('Ctrl Pts',(54.1714861895346,44.3393235891075,0.));
#168256=CARTESIAN_POINT('Ctrl Pts',(54.1679505278134,44.3377168516418,0.));
#168257=CARTESIAN_POINT('Ctrl Pts',(62.494763006804,40.554341280847,0.));
#168258=CARTESIAN_POINT('Ctrl Pts',(62.494763006804,40.554341280847,12.));
#168259=CARTESIAN_POINT('Ctrl Pts',(62.489224912198,40.5535399497519,0.));
#168260=CARTESIAN_POINT('Ctrl Pts',(62.489224912198,40.5535399497519,12.));
#168261=CARTESIAN_POINT('Ctrl Pts',(62.4781525156318,40.5519353177252,0.));
#168262=CARTESIAN_POINT('Ctrl Pts',(62.4781525156318,40.5519353177252,12.));
#168263=CARTESIAN_POINT('Ctrl Pts',(62.4615552987202,40.5495224601758,0.));
#168264=CARTESIAN_POINT('Ctrl Pts',(62.4615552987202,40.5495224601758,12.));
#168265=CARTESIAN_POINT('Ctrl Pts',(62.4394484329678,40.5462934972718,0.));
#168266=CARTESIAN_POINT('Ctrl Pts',(62.4394484329678,40.5462934972718,12.));
#168267=CARTESIAN_POINT('Ctrl Pts',(62.4118527881148,40.5422375945026,0.));
#168268=CARTESIAN_POINT('Ctrl Pts',(62.4118527881148,40.5422375945026,12.));
#168269=CARTESIAN_POINT('Ctrl Pts',(62.3842950992833,40.5381619974169,0.));
#168270=CARTESIAN_POINT('Ctrl Pts',(62.3842950992833,40.5381619974169,12.));
#168271=CARTESIAN_POINT('Ctrl Pts',(62.3567753970279,40.5340667194319,0.));
#168272=CARTESIAN_POINT('Ctrl Pts',(62.3567753970279,40.5340667194319,12.));
#168273=CARTESIAN_POINT('Ctrl Pts',(62.3292937257901,40.5299517857721,0.));
#168274=CARTESIAN_POINT('Ctrl Pts',(62.3292937257901,40.5299517857721,12.));
#168275=CARTESIAN_POINT('Ctrl Pts',(62.301850147165,40.5258172381428,0.));
#168276=CARTESIAN_POINT('Ctrl Pts',(62.301850147165,40.5258172381428,12.));
#168277=CARTESIAN_POINT('Ctrl Pts',(62.2744447381971,40.5216631336193,0.));
#168278=CARTESIAN_POINT('Ctrl Pts',(62.2744447381971,40.5216631336193,12.));
#168279=CARTESIAN_POINT('Ctrl Pts',(62.247077585866,40.5174895390954,0.));
#168280=CARTESIAN_POINT('Ctrl Pts',(62.247077585866,40.5174895390954,12.));
#168281=CARTESIAN_POINT('Ctrl Pts',(62.2197487826136,40.5132965269633,0.));
#168282=CARTESIAN_POINT('Ctrl Pts',(62.2197487826136,40.5132965269633,12.));
#168283=CARTESIAN_POINT('Ctrl Pts',(62.1924584215653,40.5090841704122,0.));
#168284=CARTESIAN_POINT('Ctrl Pts',(62.1924584215653,40.5090841704122,12.));
#168285=CARTESIAN_POINT('Ctrl Pts',(62.1652065915808,40.5048525386035,0.));
#168286=CARTESIAN_POINT('Ctrl Pts',(62.1652065915808,40.5048525386035,12.));
#168287=CARTESIAN_POINT('Ctrl Pts',(62.1379933732528,40.5006016927554,0.));
#168288=CARTESIAN_POINT('Ctrl Pts',(62.1379933732528,40.5006016927554,12.));
#168289=CARTESIAN_POINT('Ctrl Pts',(62.1108188417003,40.4963316888412,0.));
#168290=CARTESIAN_POINT('Ctrl Pts',(62.1108188417003,40.4963316888412,12.));
#168291=CARTESIAN_POINT('Ctrl Pts',(62.0836830685719,40.4920425795217,0.));
#168292=CARTESIAN_POINT('Ctrl Pts',(62.0836830685719,40.4920425795217,12.));
#168293=CARTESIAN_POINT('Ctrl Pts',(62.0565861244179,40.4877344164411,0.));
#168294=CARTESIAN_POINT('Ctrl Pts',(62.0565861244179,40.4877344164411,12.));
#168295=CARTESIAN_POINT('Ctrl Pts',(62.029528080742,40.4834072522164,0.));
#168296=CARTESIAN_POINT('Ctrl Pts',(62.029528080742,40.4834072522164,12.));
#168297=CARTESIAN_POINT('Ctrl Pts',(62.0025090125959,40.4790611429583,0.));
#168298=CARTESIAN_POINT('Ctrl Pts',(62.0025090125959,40.4790611429583,12.));
#168299=CARTESIAN_POINT('Ctrl Pts',(61.9755289983044,40.4746961480015,0.));
#168300=CARTESIAN_POINT('Ctrl Pts',(61.9755289983044,40.4746961480015,12.));
#168301=CARTESIAN_POINT('Ctrl Pts',(61.9485881182921,40.4703123287621,0.));
#168302=CARTESIAN_POINT('Ctrl Pts',(61.9485881182921,40.4703123287621,12.));
#168303=CARTESIAN_POINT('Ctrl Pts',(61.9216864541744,40.4659097478587,0.));
#168304=CARTESIAN_POINT('Ctrl Pts',(61.9216864541744,40.4659097478587,12.));
#168305=CARTESIAN_POINT('Ctrl Pts',(61.8948240878008,40.4614884681889,0.));
#168306=CARTESIAN_POINT('Ctrl Pts',(61.8948240878008,40.4614884681889,12.));
#168307=CARTESIAN_POINT('Ctrl Pts',(61.8680011001537,40.4570485518749,0.));
#168308=CARTESIAN_POINT('Ctrl Pts',(61.8680011001537,40.4570485518749,12.));
#168309=CARTESIAN_POINT('Ctrl Pts',(61.8412175708552,40.4525900597894,0.));
#168310=CARTESIAN_POINT('Ctrl Pts',(61.8412175708552,40.4525900597894,12.));
#168311=CARTESIAN_POINT('Ctrl Pts',(61.814473578779,40.4481130521364,0.));
#168312=CARTESIAN_POINT('Ctrl Pts',(61.814473578779,40.4481130521364,12.));
#168313=CARTESIAN_POINT('Ctrl Pts',(61.7877692024076,40.4436175887949,0.));
#168314=CARTESIAN_POINT('Ctrl Pts',(61.7877692024076,40.4436175887949,12.));
#168315=CARTESIAN_POINT('Ctrl Pts',(61.7611045202874,40.4391037297589,0.));
#168316=CARTESIAN_POINT('Ctrl Pts',(61.7611045202874,40.4391037297589,12.));
#168317=CARTESIAN_POINT('Ctrl Pts',(61.7344796114399,40.4345715355405,0.));
#168318=CARTESIAN_POINT('Ctrl Pts',(61.7344796114399,40.4345715355405,12.));
#168319=CARTESIAN_POINT('Ctrl Pts',(61.7078945557799,40.430021067584,0.));
#168320=CARTESIAN_POINT('Ctrl Pts',(61.7078945557799,40.430021067584,12.));
#168321=CARTESIAN_POINT('Ctrl Pts',(61.6813494339286,40.425452388076,0.));
#168322=CARTESIAN_POINT('Ctrl Pts',(61.6813494339286,40.425452388076,12.));
#168323=CARTESIAN_POINT('Ctrl Pts',(61.6548443270394,40.4208655597717,0.));
#168324=CARTESIAN_POINT('Ctrl Pts',(61.6548443270394,40.4208655597717,12.));
#168325=CARTESIAN_POINT('Ctrl Pts',(61.628379316608,40.4162606458119,0.));
#168326=CARTESIAN_POINT('Ctrl Pts',(61.628379316608,40.4162606458119,12.));
#168327=CARTESIAN_POINT('Ctrl Pts',(61.601954484301,40.4116377095596,0.));
#168328=CARTESIAN_POINT('Ctrl Pts',(61.601954484301,40.4116377095596,12.));
#168329=CARTESIAN_POINT('Ctrl Pts',(61.5755699117324,40.4069968143956,0.));
#168330=CARTESIAN_POINT('Ctrl Pts',(61.5755699117324,40.4069968143956,12.));
#168331=CARTESIAN_POINT('Ctrl Pts',(61.5492256804717,40.4023380237232,0.));
#168332=CARTESIAN_POINT('Ctrl Pts',(61.5492256804717,40.4023380237232,12.));
#168333=CARTESIAN_POINT('Ctrl Pts',(61.522921872154,40.3976614010652,0.));
#168334=CARTESIAN_POINT('Ctrl Pts',(61.522921872154,40.3976614010652,12.));
#168335=CARTESIAN_POINT('Ctrl Pts',(61.4966585685549,40.3929670101366,0.));
#168336=CARTESIAN_POINT('Ctrl Pts',(61.4966585685549,40.3929670101366,12.));
#168337=CARTESIAN_POINT('Ctrl Pts',(61.4704358516709,40.3882549149228,0.));
#168338=CARTESIAN_POINT('Ctrl Pts',(61.4704358516709,40.3882549149228,12.));
#168339=CARTESIAN_POINT('Ctrl Pts',(61.4442538038044,40.383525179772,0.));
#168340=CARTESIAN_POINT('Ctrl Pts',(61.4442538038044,40.383525179772,12.));
#168341=CARTESIAN_POINT('Ctrl Pts',(61.4181125076037,40.3787778694364,0.));
#168342=CARTESIAN_POINT('Ctrl Pts',(61.4181125076037,40.3787778694364,12.));
#168343=CARTESIAN_POINT('Ctrl Pts',(61.3920120460219,40.3740130490225,0.));
#168344=CARTESIAN_POINT('Ctrl Pts',(61.3920120460219,40.3740130490225,12.));
#168345=CARTESIAN_POINT('Ctrl Pts',(61.3659525022908,40.3692307839636,0.));
#168346=CARTESIAN_POINT('Ctrl Pts',(61.3659525022908,40.3692307839636,12.));
#168347=CARTESIAN_POINT('Ctrl Pts',(61.3399339598853,40.3644311399861,0.));
#168348=CARTESIAN_POINT('Ctrl Pts',(61.3399339598853,40.3644311399861,12.));
#168349=CARTESIAN_POINT('Ctrl Pts',(61.3139565024847,40.3596141830791,0.));
#168350=CARTESIAN_POINT('Ctrl Pts',(61.3139565024847,40.3596141830791,12.));
#168351=CARTESIAN_POINT('Ctrl Pts',(61.2880202139371,40.3547799794679,0.));
#168352=CARTESIAN_POINT('Ctrl Pts',(61.2880202139371,40.3547799794679,12.));
#168353=CARTESIAN_POINT('Ctrl Pts',(61.2621251782863,40.3499285956304,0.));
#168354=CARTESIAN_POINT('Ctrl Pts',(61.2621251782863,40.3499285956304,12.));
#168355=CARTESIAN_POINT('Ctrl Pts',(61.23627147979,40.3450600983109,0.));
#168356=CARTESIAN_POINT('Ctrl Pts',(61.23627147979,40.3450600983109,12.));
#168357=CARTESIAN_POINT('Ctrl Pts',(61.2104592029377,40.340174554537,0.));
#168358=CARTESIAN_POINT('Ctrl Pts',(61.2104592029377,40.340174554537,12.));
#168359=CARTESIAN_POINT('Ctrl Pts',(61.1846884324644,40.335272031637,0.));
#168360=CARTESIAN_POINT('Ctrl Pts',(61.1846884324644,40.335272031637,12.));
#168361=CARTESIAN_POINT('Ctrl Pts',(61.1589592533613,40.3303525972615,0.));
#168362=CARTESIAN_POINT('Ctrl Pts',(61.1589592533613,40.3303525972615,12.));
#168363=CARTESIAN_POINT('Ctrl Pts',(61.1332717508789,40.32541631938,0.));
#168364=CARTESIAN_POINT('Ctrl Pts',(61.1332717508789,40.32541631938,12.));
#168365=CARTESIAN_POINT('Ctrl Pts',(61.1076260105258,40.3204632662725,0.));
#168366=CARTESIAN_POINT('Ctrl Pts',(61.1076260105258,40.3204632662725,12.));
#168367=CARTESIAN_POINT('Ctrl Pts',(61.0820221180645,40.3154935065262,0.));
#168368=CARTESIAN_POINT('Ctrl Pts',(61.0820221180645,40.3154935065262,12.));
#168369=CARTESIAN_POINT('Ctrl Pts',(61.056460159505,40.310507109031,0.));
#168370=CARTESIAN_POINT('Ctrl Pts',(61.056460159505,40.310507109031,12.));
#168371=CARTESIAN_POINT('Ctrl Pts',(61.0309402210921,40.3055041429775,0.));
#168372=CARTESIAN_POINT('Ctrl Pts',(61.0309402210921,40.3055041429775,12.));
#168373=CARTESIAN_POINT('Ctrl Pts',(61.0054623893066,40.300484677858,0.));
#168374=CARTESIAN_POINT('Ctrl Pts',(61.0054623893066,40.300484677858,12.));
#168375=CARTESIAN_POINT('Ctrl Pts',(60.9800267508786,40.295448783469,0.));
#168376=CARTESIAN_POINT('Ctrl Pts',(60.9800267508786,40.295448783469,12.));
#168377=CARTESIAN_POINT('Ctrl Pts',(60.9546333927921,40.2903965299155,0.));
#168378=CARTESIAN_POINT('Ctrl Pts',(60.9546333927921,40.2903965299155,12.));
#168379=CARTESIAN_POINT('Ctrl Pts',(60.9292824022887,40.2853279876161,0.));
#168380=CARTESIAN_POINT('Ctrl Pts',(60.9292824022887,40.2853279876161,12.));
#168381=CARTESIAN_POINT('Ctrl Pts',(60.9039738668669,40.2802432273104,0.));
#168382=CARTESIAN_POINT('Ctrl Pts',(60.9039738668669,40.2802432273104,12.));
#168383=CARTESIAN_POINT('Ctrl Pts',(60.8787078742818,40.2751423200639,0.));
#168384=CARTESIAN_POINT('Ctrl Pts',(60.8787078742818,40.2751423200639,12.));
#168385=CARTESIAN_POINT('Ctrl Pts',(60.8534845125538,40.2700253372648,0.));
#168386=CARTESIAN_POINT('Ctrl Pts',(60.8534845125538,40.2700253372648,12.));
#168387=CARTESIAN_POINT('Ctrl Pts',(60.8283038699706,40.2648923506248,0.));
#168388=CARTESIAN_POINT('Ctrl Pts',(60.8283038699706,40.2648923506248,12.));
#168389=CARTESIAN_POINT('Ctrl Pts',(60.8031660350879,40.2597434321803,0.));
#168390=CARTESIAN_POINT('Ctrl Pts',(60.8031660350879,40.2597434321803,12.));
#168391=CARTESIAN_POINT('Ctrl Pts',(60.7780710967248,40.2545786542953,0.));
#168392=CARTESIAN_POINT('Ctrl Pts',(60.7780710967248,40.2545786542953,12.));
#168393=CARTESIAN_POINT('Ctrl Pts',(60.7530191439593,40.2493980896638,0.));
#168394=CARTESIAN_POINT('Ctrl Pts',(60.7530191439593,40.2493980896638,12.));
#168395=CARTESIAN_POINT('Ctrl Pts',(60.728010266139,40.2442018113108,0.));
#168396=CARTESIAN_POINT('Ctrl Pts',(60.728010266139,40.2442018113108,12.));
#168397=CARTESIAN_POINT('Ctrl Pts',(60.7030445528857,40.2389898925932,0.));
#168398=CARTESIAN_POINT('Ctrl Pts',(60.7030445528857,40.2389898925932,12.));
#168399=CARTESIAN_POINT('Ctrl Pts',(60.678122094098,40.2337624072029,0.));
#168400=CARTESIAN_POINT('Ctrl Pts',(60.678122094098,40.2337624072029,12.));
#168401=CARTESIAN_POINT('Ctrl Pts',(60.6532429799499,40.2285194291706,0.));
#168402=CARTESIAN_POINT('Ctrl Pts',(60.6532429799499,40.2285194291706,12.));
#168403=CARTESIAN_POINT('Ctrl Pts',(60.6284073008871,40.2232610328721,0.));
#168404=CARTESIAN_POINT('Ctrl Pts',(60.6284073008871,40.2232610328721,12.));
#168405=CARTESIAN_POINT('Ctrl Pts',(60.6036151476349,40.2179872930273,0.));
#168406=CARTESIAN_POINT('Ctrl Pts',(60.6036151476349,40.2179872930273,12.));
#168407=CARTESIAN_POINT('Ctrl Pts',(60.5788666112042,40.2126982847011,0.));
#168408=CARTESIAN_POINT('Ctrl Pts',(60.5788666112042,40.2126982847011,12.));
#168409=CARTESIAN_POINT('Ctrl Pts',(60.5541617828925,40.2073940833053,0.));
#168410=CARTESIAN_POINT('Ctrl Pts',(60.5541617828925,40.2073940833053,12.));
#168411=CARTESIAN_POINT('Ctrl Pts',(60.5295007542841,40.2020747646014,0.));
#168412=CARTESIAN_POINT('Ctrl Pts',(60.5295007542841,40.2020747646014,12.));
#168413=CARTESIAN_POINT('Ctrl Pts',(60.5048836172435,40.1967404047062,0.));
#168414=CARTESIAN_POINT('Ctrl Pts',(60.5048836172435,40.1967404047062,12.));
#168415=CARTESIAN_POINT('Ctrl Pts',(60.4803104639225,40.1913910800921,0.));
#168416=CARTESIAN_POINT('Ctrl Pts',(60.4803104639225,40.1913910800921,12.));
#168417=CARTESIAN_POINT('Ctrl Pts',(60.455781386769,40.1860268675884,0.));
#168418=CARTESIAN_POINT('Ctrl Pts',(60.455781386769,40.1860268675884,12.));
#168419=CARTESIAN_POINT('Ctrl Pts',(60.4312964785273,40.180647844383,0.));
#168420=CARTESIAN_POINT('Ctrl Pts',(60.4312964785273,40.180647844383,12.));
#168421=CARTESIAN_POINT('Ctrl Pts',(60.4068558322407,40.1752540880268,0.));
#168422=CARTESIAN_POINT('Ctrl Pts',(60.4068558322407,40.1752540880268,12.));
#168423=CARTESIAN_POINT('Ctrl Pts',(60.3824595412445,40.1698456764377,0.));
#168424=CARTESIAN_POINT('Ctrl Pts',(60.3824595412445,40.1698456764377,12.));
#168425=CARTESIAN_POINT('Ctrl Pts',(60.3581076991716,40.1644226879033,0.));
#168426=CARTESIAN_POINT('Ctrl Pts',(60.3581076991716,40.1644226879033,12.));
#168427=CARTESIAN_POINT('Ctrl Pts',(60.3338003999607,40.1589852010804,0.));
#168428=CARTESIAN_POINT('Ctrl Pts',(60.3338003999607,40.1589852010804,12.));
#168429=CARTESIAN_POINT('Ctrl Pts',(60.3095377378586,40.1535332949976,0.));
#168430=CARTESIAN_POINT('Ctrl Pts',(60.3095377378586,40.1535332949976,12.));
#168431=CARTESIAN_POINT('Ctrl Pts',(60.285319807422,40.1480670490586,0.));
#168432=CARTESIAN_POINT('Ctrl Pts',(60.285319807422,40.1480670490586,12.));
#168433=CARTESIAN_POINT('Ctrl Pts',(60.2611467035116,40.1425865430472,0.));
#168434=CARTESIAN_POINT('Ctrl Pts',(60.2611467035116,40.1425865430472,12.));
#168435=CARTESIAN_POINT('Ctrl Pts',(60.2370185212964,40.1370918571304,0.));
#168436=CARTESIAN_POINT('Ctrl Pts',(60.2370185212964,40.1370918571304,12.));
#168437=CARTESIAN_POINT('Ctrl Pts',(60.2129353562622,40.1315830718577,0.));
#168438=CARTESIAN_POINT('Ctrl Pts',(60.2129353562622,40.1315830718577,12.));
#168439=CARTESIAN_POINT('Ctrl Pts',(60.1888973042152,40.1260602681644,0.));
#168440=CARTESIAN_POINT('Ctrl Pts',(60.1888973042152,40.1260602681644,12.));
#168441=CARTESIAN_POINT('Ctrl Pts',(60.1649044612828,40.1205235273739,0.));
#168442=CARTESIAN_POINT('Ctrl Pts',(60.1649044612828,40.1205235273739,12.));
#168443=CARTESIAN_POINT('Ctrl Pts',(60.1409569239092,40.1149729312036,0.));
#168444=CARTESIAN_POINT('Ctrl Pts',(60.1409569239092,40.1149729312036,12.));
#168445=CARTESIAN_POINT('Ctrl Pts',(60.1170547888574,40.1094085617674,0.));
#168446=CARTESIAN_POINT('Ctrl Pts',(60.1170547888574,40.1094085617674,12.));
#168447=CARTESIAN_POINT('Ctrl Pts',(60.0931981532198,40.1038305015766,0.));
#168448=CARTESIAN_POINT('Ctrl Pts',(60.0931981532198,40.1038305015766,12.));
#168449=CARTESIAN_POINT('Ctrl Pts',(60.069387114421,40.0982388335423,0.));
#168450=CARTESIAN_POINT('Ctrl Pts',(60.069387114421,40.0982388335423,12.));
#168451=CARTESIAN_POINT('Ctrl Pts',(60.0456217702202,40.0926336409785,0.));
#168452=CARTESIAN_POINT('Ctrl Pts',(60.0456217702202,40.0926336409785,12.));
#168453=CARTESIAN_POINT('Ctrl Pts',(60.021902218706,40.0870150076074,0.));
#168454=CARTESIAN_POINT('Ctrl Pts',(60.021902218706,40.0870150076074,12.));
#168455=CARTESIAN_POINT('Ctrl Pts',(59.9982285582983,40.0813830175623,0.));
#168456=CARTESIAN_POINT('Ctrl Pts',(59.9982285582983,40.0813830175623,12.));
#168457=CARTESIAN_POINT('Ctrl Pts',(59.9746008877584,40.0757377553888,0.));
#168458=CARTESIAN_POINT('Ctrl Pts',(59.9746008877584,40.0757377553888,12.));
#168459=CARTESIAN_POINT('Ctrl Pts',(59.9510193061927,40.0700793060473,0.));
#168460=CARTESIAN_POINT('Ctrl Pts',(59.9510193061927,40.0700793060473,12.));
#168461=CARTESIAN_POINT('Ctrl Pts',(59.9274839130553,40.0644077549159,0.));
#168462=CARTESIAN_POINT('Ctrl Pts',(59.9274839130553,40.0644077549159,12.));
#168463=CARTESIAN_POINT('Ctrl Pts',(59.9039948081432,40.0587231877961,0.));
#168464=CARTESIAN_POINT('Ctrl Pts',(59.9039948081432,40.0587231877961,12.));
#168465=CARTESIAN_POINT('Ctrl Pts',(59.8805520915975,40.0530256909162,0.));
#168466=CARTESIAN_POINT('Ctrl Pts',(59.8805520915975,40.0530256909162,12.));
#168467=CARTESIAN_POINT('Ctrl Pts',(59.8571558639145,40.0473153509323,0.));
#168468=CARTESIAN_POINT('Ctrl Pts',(59.8571558639145,40.0473153509323,12.));
#168469=CARTESIAN_POINT('Ctrl Pts',(59.8338062259491,40.0415922549313,0.));
#168470=CARTESIAN_POINT('Ctrl Pts',(59.8338062259491,40.0415922549313,12.));
#168471=CARTESIAN_POINT('Ctrl Pts',(59.8105032789179,40.035856490434,0.));
#168472=CARTESIAN_POINT('Ctrl Pts',(59.8105032789179,40.035856490434,12.));
#168473=CARTESIAN_POINT('Ctrl Pts',(59.7872471243948,40.0301081454006,0.));
#168474=CARTESIAN_POINT('Ctrl Pts',(59.7872471243948,40.0301081454006,12.));
#168475=CARTESIAN_POINT('Ctrl Pts',(59.7640378643115,40.0243473082343,0.));
#168476=CARTESIAN_POINT('Ctrl Pts',(59.7640378643115,40.0243473082343,12.));
#168477=CARTESIAN_POINT('Ctrl Pts',(59.7408756009688,40.0185740677827,0.));
#168478=CARTESIAN_POINT('Ctrl Pts',(59.7408756009688,40.0185740677827,12.));
#168479=CARTESIAN_POINT('Ctrl Pts',(59.7177604370409,40.0127885133407,0.));
#168480=CARTESIAN_POINT('Ctrl Pts',(59.7177604370409,40.0127885133407,12.));
#168481=CARTESIAN_POINT('Ctrl Pts',(59.6946924755771,40.0069907346536,0.));
#168482=CARTESIAN_POINT('Ctrl Pts',(59.6946924755771,40.0069907346536,12.));
#168483=CARTESIAN_POINT('Ctrl Pts',(59.671671819999,40.0011808219231,0.));
#168484=CARTESIAN_POINT('Ctrl Pts',(59.671671819999,40.0011808219231,12.));
#168485=CARTESIAN_POINT('Ctrl Pts',(59.6486985741015,39.9953588658114,0.));
#168486=CARTESIAN_POINT('Ctrl Pts',(59.6486985741015,39.9953588658114,12.));
#168487=CARTESIAN_POINT('Ctrl Pts',(59.6257728420644,39.9895249574432,0.));
#168488=CARTESIAN_POINT('Ctrl Pts',(59.6257728420644,39.9895249574432,12.));
#168489=CARTESIAN_POINT('Ctrl Pts',(59.6028947284551,39.9836791884071,0.));
#168490=CARTESIAN_POINT('Ctrl Pts',(59.6028947284551,39.9836791884071,12.));
#168491=CARTESIAN_POINT('Ctrl Pts',(59.5800643382322,39.9778216507609,0.));
#168492=CARTESIAN_POINT('Ctrl Pts',(59.5800643382322,39.9778216507609,12.));
#168493=CARTESIAN_POINT('Ctrl Pts',(59.5572817767412,39.971952437036,0.));
#168494=CARTESIAN_POINT('Ctrl Pts',(59.5572817767412,39.971952437036,12.));
#168495=CARTESIAN_POINT('Ctrl Pts',(59.5345471497162,39.9660716402423,0.));
#168496=CARTESIAN_POINT('Ctrl Pts',(59.5345471497162,39.9660716402423,12.));
#168497=CARTESIAN_POINT('Ctrl Pts',(59.511860563292,39.96017935387,0.));
#168498=CARTESIAN_POINT('Ctrl Pts',(59.511860563292,39.96017935387,12.));
#168499=CARTESIAN_POINT('Ctrl Pts',(59.4892221240081,39.954275671893,0.));
#168500=CARTESIAN_POINT('Ctrl Pts',(59.4892221240081,39.954275671893,12.));
#168501=CARTESIAN_POINT('Ctrl Pts',(59.4666319388123,39.9483606887731,0.));
#168502=CARTESIAN_POINT('Ctrl Pts',(59.4666319388123,39.9483606887731,12.));
#168503=CARTESIAN_POINT('Ctrl Pts',(59.444090115055,39.9424344994652,0.));
#168504=CARTESIAN_POINT('Ctrl Pts',(59.444090115055,39.9424344994652,12.));
#168505=CARTESIAN_POINT('Ctrl Pts',(59.4215967604925,39.9364971994215,0.));
#168506=CARTESIAN_POINT('Ctrl Pts',(59.4215967604925,39.9364971994215,12.));
#168507=CARTESIAN_POINT('Ctrl Pts',(59.3991519832981,39.9305488845934,0.));
#168508=CARTESIAN_POINT('Ctrl Pts',(59.3991519832981,39.9305488845934,12.));
#168509=CARTESIAN_POINT('Ctrl Pts',(59.3767558920663,39.9245896514359,0.));
#168510=CARTESIAN_POINT('Ctrl Pts',(59.3767558920663,39.9245896514359,12.));
#168511=CARTESIAN_POINT('Ctrl Pts',(59.3544085958165,39.9186195969113,0.));
#168512=CARTESIAN_POINT('Ctrl Pts',(59.3544085958165,39.9186195969113,12.));
#168513=CARTESIAN_POINT('Ctrl Pts',(59.3321102039883,39.9126388184956,0.));
#168514=CARTESIAN_POINT('Ctrl Pts',(59.3321102039883,39.9126388184956,12.));
#168515=CARTESIAN_POINT('Ctrl Pts',(59.3098608264452,39.9066474141826,0.));
#168516=CARTESIAN_POINT('Ctrl Pts',(59.3098608264452,39.9066474141826,12.));
#168517=CARTESIAN_POINT('Ctrl Pts',(59.2876605734871,39.9006454824861,0.));
#168518=CARTESIAN_POINT('Ctrl Pts',(59.2876605734871,39.9006454824861,12.));
#168519=CARTESIAN_POINT('Ctrl Pts',(59.2655095558527,39.8946331224442,0.));
#168520=CARTESIAN_POINT('Ctrl Pts',(59.2655095558527,39.8946331224442,12.));
#168521=CARTESIAN_POINT('Ctrl Pts',(59.2434078847236,39.8886104336234,0.));
#168522=CARTESIAN_POINT('Ctrl Pts',(59.2434078847236,39.8886104336234,12.));
#168523=CARTESIAN_POINT('Ctrl Pts',(59.2213556717189,39.8825775161252,0.));
#168524=CARTESIAN_POINT('Ctrl Pts',(59.2213556717189,39.8825775161252,12.));
#168525=CARTESIAN_POINT('Ctrl Pts',(59.1993530289008,39.8765344705895,0.));
#168526=CARTESIAN_POINT('Ctrl Pts',(59.1993530289008,39.8765344705895,12.));
#168527=CARTESIAN_POINT('Ctrl Pts',(59.1774000687865,39.8704813981978,0.));
#168528=CARTESIAN_POINT('Ctrl Pts',(59.1774000687865,39.8704813981978,12.));
#168529=CARTESIAN_POINT('Ctrl Pts',(59.155496904352,39.8644184006785,0.));
#168530=CARTESIAN_POINT('Ctrl Pts',(59.155496904352,39.8644184006785,12.));
#168531=CARTESIAN_POINT('Ctrl Pts',(59.133643649035,39.8583455803111,0.));
#168532=CARTESIAN_POINT('Ctrl Pts',(59.133643649035,39.8583455803111,12.));
#168533=CARTESIAN_POINT('Ctrl Pts',(59.1118404167304,39.8522630399337,0.));
#168534=CARTESIAN_POINT('Ctrl Pts',(59.1118404167304,39.8522630399337,12.));
#168535=CARTESIAN_POINT('Ctrl Pts',(59.0900873217992,39.8461708829465,0.));
#168536=CARTESIAN_POINT('Ctrl Pts',(59.0900873217992,39.8461708829465,12.));
#168537=CARTESIAN_POINT('Ctrl Pts',(59.068384479077,39.8400692133143,0.));
#168538=CARTESIAN_POINT('Ctrl Pts',(59.068384479077,39.8400692133143,12.));
#168539=CARTESIAN_POINT('Ctrl Pts',(59.0467320038782,39.8339581355715,0.));
#168540=CARTESIAN_POINT('Ctrl Pts',(59.0467320038782,39.8339581355715,12.));
#168541=CARTESIAN_POINT('Ctrl Pts',(59.0251300119972,39.8278377548261,0.));
#168542=CARTESIAN_POINT('Ctrl Pts',(59.0251300119972,39.8278377548261,12.));
#168543=CARTESIAN_POINT('Ctrl Pts',(59.0035786197024,39.8217081767658,0.));
#168544=CARTESIAN_POINT('Ctrl Pts',(59.0035786197024,39.8217081767658,12.));
#168545=CARTESIAN_POINT('Ctrl Pts',(58.9820779437485,39.8155695076625,0.));
#168546=CARTESIAN_POINT('Ctrl Pts',(58.9820779437485,39.8155695076625,12.));
#168547=CARTESIAN_POINT('Ctrl Pts',(58.9606281013876,39.8094218543781,0.));
#168548=CARTESIAN_POINT('Ctrl Pts',(58.9606281013876,39.8094218543781,12.));
#168549=CARTESIAN_POINT('Ctrl Pts',(58.9392292103747,39.8032653243712,0.));
#168550=CARTESIAN_POINT('Ctrl Pts',(58.9392292103747,39.8032653243712,12.));
#168551=CARTESIAN_POINT('Ctrl Pts',(58.9178813889703,39.7971000257044,0.));
#168552=CARTESIAN_POINT('Ctrl Pts',(58.9178813889703,39.7971000257044,12.));
#168553=CARTESIAN_POINT('Ctrl Pts',(58.896584755939,39.7909260670517,0.));
#168554=CARTESIAN_POINT('Ctrl Pts',(58.896584755939,39.7909260670517,12.));
#168555=CARTESIAN_POINT('Ctrl Pts',(58.8753394305583,39.7847435576995,0.));
#168556=CARTESIAN_POINT('Ctrl Pts',(58.8753394305583,39.7847435576995,12.));
#168557=CARTESIAN_POINT('Ctrl Pts',(58.8541455326229,39.7785526075477,0.));
#168558=CARTESIAN_POINT('Ctrl Pts',(58.8541455326229,39.7785526075477,12.));
#168559=CARTESIAN_POINT('Ctrl Pts',(58.8330031824453,39.772353327112,0.));
#168560=CARTESIAN_POINT('Ctrl Pts',(58.8330031824453,39.772353327112,12.));
#168561=CARTESIAN_POINT('Ctrl Pts',(58.8119125008521,39.7661458275276,0.));
#168562=CARTESIAN_POINT('Ctrl Pts',(58.8119125008521,39.7661458275276,12.));
#168563=CARTESIAN_POINT('Ctrl Pts',(58.7908736091808,39.7599302205527,0.));
#168564=CARTESIAN_POINT('Ctrl Pts',(58.7908736091808,39.7599302205527,12.));
#168565=CARTESIAN_POINT('Ctrl Pts',(58.769886629304,39.753706618582,0.));
#168566=CARTESIAN_POINT('Ctrl Pts',(58.769886629304,39.753706618582,12.));
#168567=CARTESIAN_POINT('Ctrl Pts',(58.7489516836453,39.7474751346603,0.));
#168568=CARTESIAN_POINT('Ctrl Pts',(58.7489516836453,39.7474751346603,12.));
#168569=CARTESIAN_POINT('Ctrl Pts',(58.7280688951911,39.7412358824949,0.));
#168570=CARTESIAN_POINT('Ctrl Pts',(58.7280688951911,39.7412358824949,12.));
#168571=CARTESIAN_POINT('Ctrl Pts',(58.7072383875009,39.7349889764737,0.));
#168572=CARTESIAN_POINT('Ctrl Pts',(58.7072383875009,39.7349889764737,12.));
#168573=CARTESIAN_POINT('Ctrl Pts',(58.6864602847064,39.7287345316664,0.));
#168574=CARTESIAN_POINT('Ctrl Pts',(58.6864602847064,39.7287345316664,12.));
#168575=CARTESIAN_POINT('Ctrl Pts',(58.6657347115014,39.7224726638087,0.));
#168576=CARTESIAN_POINT('Ctrl Pts',(58.6657347115014,39.7224726638087,12.));
#168577=CARTESIAN_POINT('Ctrl Pts',(58.6450617931269,39.7162034892896,0.));
#168578=CARTESIAN_POINT('Ctrl Pts',(58.6450617931269,39.7162034892896,12.));
#168579=CARTESIAN_POINT('Ctrl Pts',(58.6244416553574,39.7099271251421,0.));
#168580=CARTESIAN_POINT('Ctrl Pts',(58.6244416553574,39.7099271251421,12.));
#168581=CARTESIAN_POINT('Ctrl Pts',(58.6038744244683,39.7036436890248,0.));
#168582=CARTESIAN_POINT('Ctrl Pts',(58.6038744244683,39.7036436890248,12.));
#168583=CARTESIAN_POINT('Ctrl Pts',(58.5833602272767,39.6973532992555,0.));
#168584=CARTESIAN_POINT('Ctrl Pts',(58.5833602272767,39.6973532992555,12.));
#168585=CARTESIAN_POINT('Ctrl Pts',(58.5628991912067,39.6910560748639,0.));
#168586=CARTESIAN_POINT('Ctrl Pts',(58.5628991912067,39.6910560748639,12.));
#168587=CARTESIAN_POINT('Ctrl Pts',(58.5424914443415,39.6847521356395,0.));
#168588=CARTESIAN_POINT('Ctrl Pts',(58.5424914443415,39.6847521356395,12.));
#168589=CARTESIAN_POINT('Ctrl Pts',(58.5221371154748,39.6784416021817,0.));
#168590=CARTESIAN_POINT('Ctrl Pts',(58.5221371154748,39.6784416021817,12.));
#168591=CARTESIAN_POINT('Ctrl Pts',(58.5018363341582,39.6721245959516,0.));
#168592=CARTESIAN_POINT('Ctrl Pts',(58.5018363341582,39.6721245959516,12.));
#168593=CARTESIAN_POINT('Ctrl Pts',(58.4815892306044,39.66580123918,0.));
#168594=CARTESIAN_POINT('Ctrl Pts',(58.4815892306044,39.66580123918,12.));
#168595=CARTESIAN_POINT('Ctrl Pts',(58.4613959355776,39.6594716547681,0.));
#168596=CARTESIAN_POINT('Ctrl Pts',(58.4613959355776,39.6594716547681,12.));
#168597=CARTESIAN_POINT('Ctrl Pts',(58.4412565802984,39.6531359662043,0.));
#168598=CARTESIAN_POINT('Ctrl Pts',(58.4412565802984,39.6531359662043,12.));
#168599=CARTESIAN_POINT('Ctrl Pts',(58.4211712963023,39.6467942974465,0.));
#168600=CARTESIAN_POINT('Ctrl Pts',(58.4211712963023,39.6467942974465,12.));
#168601=CARTESIAN_POINT('Ctrl Pts',(58.4011402154225,39.6404467729113,0.));
#168602=CARTESIAN_POINT('Ctrl Pts',(58.4011402154225,39.6404467729113,12.));
#168603=CARTESIAN_POINT('Ctrl Pts',(58.3811634701061,39.6340935177492,0.));
#168604=CARTESIAN_POINT('Ctrl Pts',(58.3811634701061,39.6340935177492,12.));
#168605=CARTESIAN_POINT('Ctrl Pts',(58.3612411936914,39.6277346580898,0.));
#168606=CARTESIAN_POINT('Ctrl Pts',(58.3612411936914,39.6277346580898,12.));
#168607=CARTESIAN_POINT('Ctrl Pts',(58.3413735206412,39.6213703212523,0.));
#168608=CARTESIAN_POINT('Ctrl Pts',(58.3413735206412,39.6213703212523,12.));
#168609=CARTESIAN_POINT('Ctrl Pts',(58.3215605869192,39.6150006360894,0.));
#168610=CARTESIAN_POINT('Ctrl Pts',(58.3215605869192,39.6150006360894,12.));
#168611=CARTESIAN_POINT('Ctrl Pts',(58.3018025297288,39.6086257327559,0.));
#168612=CARTESIAN_POINT('Ctrl Pts',(58.3018025297288,39.6086257327559,12.));
#168613=CARTESIAN_POINT('Ctrl Pts',(58.2820994868092,39.6022457420772,0.));
#168614=CARTESIAN_POINT('Ctrl Pts',(58.2820994868092,39.6022457420772,12.));
#168615=CARTESIAN_POINT('Ctrl Pts',(58.2624515958416,39.5958607950237,0.));
#168616=CARTESIAN_POINT('Ctrl Pts',(58.2624515958416,39.5958607950237,12.));
#168617=CARTESIAN_POINT('Ctrl Pts',(58.2428589938394,39.589471022173,0.));
#168618=CARTESIAN_POINT('Ctrl Pts',(58.2428589938394,39.589471022173,12.));
#168619=CARTESIAN_POINT('Ctrl Pts',(58.2233218164407,39.5830765530919,0.));
#168620=CARTESIAN_POINT('Ctrl Pts',(58.2233218164407,39.5830765530919,12.));
#168621=CARTESIAN_POINT('Ctrl Pts',(58.2038401992496,39.5766775175226,0.));
#168622=CARTESIAN_POINT('Ctrl Pts',(58.2038401992496,39.5766775175226,12.));
#168623=CARTESIAN_POINT('Ctrl Pts',(58.1844142794359,39.5702740468013,0.));
#168624=CARTESIAN_POINT('Ctrl Pts',(58.1844142794359,39.5702740468013,12.));
#168625=CARTESIAN_POINT('Ctrl Pts',(58.1650441970379,39.5638662750174,0.));
#168626=CARTESIAN_POINT('Ctrl Pts',(58.1650441970379,39.5638662750174,12.));
#168627=CARTESIAN_POINT('Ctrl Pts',(58.1457300968467,39.5574543406959,0.));
#168628=CARTESIAN_POINT('Ctrl Pts',(58.1457300968467,39.5574543406959,12.));
#168629=CARTESIAN_POINT('Ctrl Pts',(58.1264721285698,39.5510383869476,0.));
#168630=CARTESIAN_POINT('Ctrl Pts',(58.1264721285698,39.5510383869476,12.));
#168631=CARTESIAN_POINT('Ctrl Pts',(58.1072704428895,39.5446185579615,0.));
#168632=CARTESIAN_POINT('Ctrl Pts',(58.1072704428895,39.5446185579615,12.));
#168633=CARTESIAN_POINT('Ctrl Pts',(58.088125187991,39.5381949959214,0.));
#168634=CARTESIAN_POINT('Ctrl Pts',(58.088125187991,39.5381949959214,12.));
#168635=CARTESIAN_POINT('Ctrl Pts',(58.0690365065393,39.5317678383231,0.));
#168636=CARTESIAN_POINT('Ctrl Pts',(58.0690365065393,39.5317678383231,12.));
#168637=CARTESIAN_POINT('Ctrl Pts',(58.050004530846,39.5253372136921,0.));
#168638=CARTESIAN_POINT('Ctrl Pts',(58.050004530846,39.5253372136921,12.));
#168639=CARTESIAN_POINT('Ctrl Pts',(58.0310293875321,39.5189032457227,0.));
#168640=CARTESIAN_POINT('Ctrl Pts',(58.0310293875321,39.5189032457227,12.));
#168641=CARTESIAN_POINT('Ctrl Pts',(58.012111206794,39.5124660615009,0.));
#168642=CARTESIAN_POINT('Ctrl Pts',(58.012111206794,39.5124660615009,12.));
#168643=CARTESIAN_POINT('Ctrl Pts',(57.9932501298522,39.5060257981225,0.));
#168644=CARTESIAN_POINT('Ctrl Pts',(57.9932501298522,39.5060257981225,12.));
#168645=CARTESIAN_POINT('Ctrl Pts',(57.9744463179305,39.4995826106691,0.));
#168646=CARTESIAN_POINT('Ctrl Pts',(57.9744463179305,39.4995826106691,12.));
#168647=CARTESIAN_POINT('Ctrl Pts',(57.9556999583777,39.4931366776627,0.));
#168648=CARTESIAN_POINT('Ctrl Pts',(57.9556999583777,39.4931366776627,12.));
#168649=CARTESIAN_POINT('Ctrl Pts',(57.9370112456506,39.4866881842223,0.));
#168650=CARTESIAN_POINT('Ctrl Pts',(57.9370112456506,39.4866881842223,12.));
#168651=CARTESIAN_POINT('Ctrl Pts',(57.9183803632337,39.4802373061008,0.));
#168652=CARTESIAN_POINT('Ctrl Pts',(57.9183803632337,39.4802373061008,12.));
#168653=CARTESIAN_POINT('Ctrl Pts',(57.8998074670541,39.4737841949417,0.));
#168654=CARTESIAN_POINT('Ctrl Pts',(57.8998074670541,39.4737841949417,12.));
#168655=CARTESIAN_POINT('Ctrl Pts',(57.8812926637397,39.4673289592425,0.));
#168656=CARTESIAN_POINT('Ctrl Pts',(57.8812926637397,39.4673289592425,12.));
#168657=CARTESIAN_POINT('Ctrl Pts',(57.8628360097134,39.4608716627367,0.));
#168658=CARTESIAN_POINT('Ctrl Pts',(57.8628360097134,39.4608716627367,12.));
#168659=CARTESIAN_POINT('Ctrl Pts',(57.8481172247805,39.4557042029884,0.));
#168660=CARTESIAN_POINT('Ctrl Pts',(57.8481172247805,39.4557042029884,12.));
#168661=CARTESIAN_POINT('Ctrl Pts',(57.8371043151607,39.45182770037,0.));
#168662=CARTESIAN_POINT('Ctrl Pts',(57.8371043151607,39.45182770037,12.));
#168663=CARTESIAN_POINT('Ctrl Pts',(57.829774010102,39.4492429618498,0.));
#168664=CARTESIAN_POINT('Ctrl Pts',(57.829774010102,39.4492429618498,12.));
#168665=CARTESIAN_POINT('Ctrl Pts',(57.8261117662439,39.4479504917286,0.));
#168666=CARTESIAN_POINT('Ctrl Pts',(57.8261117662439,39.4479504917286,12.));
#168667=CARTESIAN_POINT('',(57.8261117662439,39.4479504917286,12.));
#168668=CARTESIAN_POINT('Ctrl Pts',(57.8261117662439,39.4479504917286,12.));
#168669=CARTESIAN_POINT('Ctrl Pts',(57.829774010102,39.4492429618498,12.));
#168670=CARTESIAN_POINT('Ctrl Pts',(57.8371043151607,39.45182770037,12.));
#168671=CARTESIAN_POINT('Ctrl Pts',(57.8481172247805,39.4557042029884,12.));
#168672=CARTESIAN_POINT('Ctrl Pts',(57.8628360097134,39.4608716627367,12.));
#168673=CARTESIAN_POINT('Ctrl Pts',(57.8812926637397,39.4673289592425,12.));
#168674=CARTESIAN_POINT('Ctrl Pts',(57.8998074670541,39.4737841949417,12.));
#168675=CARTESIAN_POINT('Ctrl Pts',(57.9183803632337,39.4802373061008,12.));
#168676=CARTESIAN_POINT('Ctrl Pts',(57.9370112456506,39.4866881842223,12.));
#168677=CARTESIAN_POINT('Ctrl Pts',(57.9556999583777,39.4931366776627,12.));
#168678=CARTESIAN_POINT('Ctrl Pts',(57.9744463179305,39.4995826106691,12.));
#168679=CARTESIAN_POINT('Ctrl Pts',(57.9932501298522,39.5060257981225,12.));
#168680=CARTESIAN_POINT('Ctrl Pts',(58.012111206794,39.5124660615009,12.));
#168681=CARTESIAN_POINT('Ctrl Pts',(58.0310293875321,39.5189032457227,12.));
#168682=CARTESIAN_POINT('Ctrl Pts',(58.050004530846,39.5253372136921,12.));
#168683=CARTESIAN_POINT('Ctrl Pts',(58.0690365065393,39.5317678383231,12.));
#168684=CARTESIAN_POINT('Ctrl Pts',(58.088125187991,39.5381949959214,12.));
#168685=CARTESIAN_POINT('Ctrl Pts',(58.1072704428895,39.5446185579615,12.));
#168686=CARTESIAN_POINT('Ctrl Pts',(58.1264721285698,39.5510383869476,12.));
#168687=CARTESIAN_POINT('Ctrl Pts',(58.1457300968467,39.5574543406959,12.));
#168688=CARTESIAN_POINT('Ctrl Pts',(58.1650441970379,39.5638662750174,12.));
#168689=CARTESIAN_POINT('Ctrl Pts',(58.1844142794359,39.5702740468013,12.));
#168690=CARTESIAN_POINT('Ctrl Pts',(58.2038401992496,39.5766775175226,12.));
#168691=CARTESIAN_POINT('Ctrl Pts',(58.2233218164407,39.5830765530919,12.));
#168692=CARTESIAN_POINT('Ctrl Pts',(58.2428589938394,39.589471022173,12.));
#168693=CARTESIAN_POINT('Ctrl Pts',(58.2624515958416,39.5958607950237,12.));
#168694=CARTESIAN_POINT('Ctrl Pts',(58.2820994868092,39.6022457420772,12.));
#168695=CARTESIAN_POINT('Ctrl Pts',(58.3018025297288,39.6086257327559,12.));
#168696=CARTESIAN_POINT('Ctrl Pts',(58.3215605869192,39.6150006360894,12.));
#168697=CARTESIAN_POINT('Ctrl Pts',(58.3413735206412,39.6213703212523,12.));
#168698=CARTESIAN_POINT('Ctrl Pts',(58.3612411936914,39.6277346580898,12.));
#168699=CARTESIAN_POINT('Ctrl Pts',(58.3811634701061,39.6340935177492,12.));
#168700=CARTESIAN_POINT('Ctrl Pts',(58.4011402154225,39.6404467729113,12.));
#168701=CARTESIAN_POINT('Ctrl Pts',(58.4211712963023,39.6467942974465,12.));
#168702=CARTESIAN_POINT('Ctrl Pts',(58.4412565802984,39.6531359662043,12.));
#168703=CARTESIAN_POINT('Ctrl Pts',(58.4613959355776,39.6594716547681,12.));
#168704=CARTESIAN_POINT('Ctrl Pts',(58.4815892306044,39.66580123918,12.));
#168705=CARTESIAN_POINT('Ctrl Pts',(58.5018363341582,39.6721245959516,12.));
#168706=CARTESIAN_POINT('Ctrl Pts',(58.5221371154748,39.6784416021817,12.));
#168707=CARTESIAN_POINT('Ctrl Pts',(58.5424914443415,39.6847521356395,12.));
#168708=CARTESIAN_POINT('Ctrl Pts',(58.5628991912067,39.6910560748639,12.));
#168709=CARTESIAN_POINT('Ctrl Pts',(58.5833602272767,39.6973532992555,12.));
#168710=CARTESIAN_POINT('Ctrl Pts',(58.6038744244683,39.7036436890248,12.));
#168711=CARTESIAN_POINT('Ctrl Pts',(58.6244416553574,39.7099271251421,12.));
#168712=CARTESIAN_POINT('Ctrl Pts',(58.6450617931269,39.7162034892896,12.));
#168713=CARTESIAN_POINT('Ctrl Pts',(58.6657347115014,39.7224726638087,12.));
#168714=CARTESIAN_POINT('Ctrl Pts',(58.6864602847064,39.7287345316664,12.));
#168715=CARTESIAN_POINT('Ctrl Pts',(58.7072383875009,39.7349889764737,12.));
#168716=CARTESIAN_POINT('Ctrl Pts',(58.7280688951911,39.7412358824949,12.));
#168717=CARTESIAN_POINT('Ctrl Pts',(58.7489516836453,39.7474751346603,12.));
#168718=CARTESIAN_POINT('Ctrl Pts',(58.769886629304,39.753706618582,12.));
#168719=CARTESIAN_POINT('Ctrl Pts',(58.7908736091808,39.7599302205527,12.));
#168720=CARTESIAN_POINT('Ctrl Pts',(58.8119125008521,39.7661458275276,12.));
#168721=CARTESIAN_POINT('Ctrl Pts',(58.8330031824453,39.772353327112,12.));
#168722=CARTESIAN_POINT('Ctrl Pts',(58.8541455326229,39.7785526075477,12.));
#168723=CARTESIAN_POINT('Ctrl Pts',(58.8753394305583,39.7847435576995,12.));
#168724=CARTESIAN_POINT('Ctrl Pts',(58.896584755939,39.7909260670517,12.));
#168725=CARTESIAN_POINT('Ctrl Pts',(58.9178813889703,39.7971000257044,12.));
#168726=CARTESIAN_POINT('Ctrl Pts',(58.9392292103747,39.8032653243712,12.));
#168727=CARTESIAN_POINT('Ctrl Pts',(58.9606281013876,39.8094218543781,12.));
#168728=CARTESIAN_POINT('Ctrl Pts',(58.9820779437485,39.8155695076625,12.));
#168729=CARTESIAN_POINT('Ctrl Pts',(59.0035786197024,39.8217081767658,12.));
#168730=CARTESIAN_POINT('Ctrl Pts',(59.0251300119972,39.8278377548261,12.));
#168731=CARTESIAN_POINT('Ctrl Pts',(59.0467320038782,39.8339581355715,12.));
#168732=CARTESIAN_POINT('Ctrl Pts',(59.068384479077,39.8400692133143,12.));
#168733=CARTESIAN_POINT('Ctrl Pts',(59.0900873217992,39.8461708829465,12.));
#168734=CARTESIAN_POINT('Ctrl Pts',(59.1118404167304,39.8522630399337,12.));
#168735=CARTESIAN_POINT('Ctrl Pts',(59.133643649035,39.8583455803111,12.));
#168736=CARTESIAN_POINT('Ctrl Pts',(59.155496904352,39.8644184006785,12.));
#168737=CARTESIAN_POINT('Ctrl Pts',(59.1774000687865,39.8704813981978,12.));
#168738=CARTESIAN_POINT('Ctrl Pts',(59.1993530289008,39.8765344705895,12.));
#168739=CARTESIAN_POINT('Ctrl Pts',(59.2213556717189,39.8825775161252,12.));
#168740=CARTESIAN_POINT('Ctrl Pts',(59.2434078847236,39.8886104336234,12.));
#168741=CARTESIAN_POINT('Ctrl Pts',(59.2655095558527,39.8946331224442,12.));
#168742=CARTESIAN_POINT('Ctrl Pts',(59.2876605734871,39.9006454824861,12.));
#168743=CARTESIAN_POINT('Ctrl Pts',(59.3098608264452,39.9066474141826,12.));
#168744=CARTESIAN_POINT('Ctrl Pts',(59.3321102039883,39.9126388184956,12.));
#168745=CARTESIAN_POINT('Ctrl Pts',(59.3544085958165,39.9186195969113,12.));
#168746=CARTESIAN_POINT('Ctrl Pts',(59.3767558920663,39.9245896514359,12.));
#168747=CARTESIAN_POINT('Ctrl Pts',(59.3991519832981,39.9305488845934,12.));
#168748=CARTESIAN_POINT('Ctrl Pts',(59.4215967604925,39.9364971994215,12.));
#168749=CARTESIAN_POINT('Ctrl Pts',(59.444090115055,39.9424344994652,12.));
#168750=CARTESIAN_POINT('Ctrl Pts',(59.4666319388123,39.9483606887731,12.));
#168751=CARTESIAN_POINT('Ctrl Pts',(59.4892221240081,39.954275671893,12.));
#168752=CARTESIAN_POINT('Ctrl Pts',(59.511860563292,39.96017935387,12.));
#168753=CARTESIAN_POINT('Ctrl Pts',(59.5345471497162,39.9660716402423,12.));
#168754=CARTESIAN_POINT('Ctrl Pts',(59.5572817767412,39.971952437036,12.));
#168755=CARTESIAN_POINT('Ctrl Pts',(59.5800643382322,39.9778216507609,12.));
#168756=CARTESIAN_POINT('Ctrl Pts',(59.6028947284551,39.9836791884071,12.));
#168757=CARTESIAN_POINT('Ctrl Pts',(59.6257728420644,39.9895249574432,12.));
#168758=CARTESIAN_POINT('Ctrl Pts',(59.6486985741015,39.9953588658114,12.));
#168759=CARTESIAN_POINT('Ctrl Pts',(59.671671819999,40.0011808219231,12.));
#168760=CARTESIAN_POINT('Ctrl Pts',(59.6946924755771,40.0069907346536,12.));
#168761=CARTESIAN_POINT('Ctrl Pts',(59.7177604370409,40.0127885133407,12.));
#168762=CARTESIAN_POINT('Ctrl Pts',(59.7408756009688,40.0185740677827,12.));
#168763=CARTESIAN_POINT('Ctrl Pts',(59.7640378643115,40.0243473082343,12.));
#168764=CARTESIAN_POINT('Ctrl Pts',(59.7872471243948,40.0301081454006,12.));
#168765=CARTESIAN_POINT('Ctrl Pts',(59.8105032789179,40.035856490434,12.));
#168766=CARTESIAN_POINT('Ctrl Pts',(59.8338062259491,40.0415922549313,12.));
#168767=CARTESIAN_POINT('Ctrl Pts',(59.8571558639145,40.0473153509323,12.));
#168768=CARTESIAN_POINT('Ctrl Pts',(59.8805520915975,40.0530256909162,12.));
#168769=CARTESIAN_POINT('Ctrl Pts',(59.9039948081432,40.0587231877961,12.));
#168770=CARTESIAN_POINT('Ctrl Pts',(59.9274839130553,40.0644077549159,12.));
#168771=CARTESIAN_POINT('Ctrl Pts',(59.9510193061927,40.0700793060473,12.));
#168772=CARTESIAN_POINT('Ctrl Pts',(59.9746008877584,40.0757377553888,12.));
#168773=CARTESIAN_POINT('Ctrl Pts',(59.9982285582983,40.0813830175623,12.));
#168774=CARTESIAN_POINT('Ctrl Pts',(60.021902218706,40.0870150076074,12.));
#168775=CARTESIAN_POINT('Ctrl Pts',(60.0456217702202,40.0926336409785,12.));
#168776=CARTESIAN_POINT('Ctrl Pts',(60.069387114421,40.0982388335423,12.));
#168777=CARTESIAN_POINT('Ctrl Pts',(60.0931981532198,40.1038305015766,12.));
#168778=CARTESIAN_POINT('Ctrl Pts',(60.1170547888574,40.1094085617674,12.));
#168779=CARTESIAN_POINT('Ctrl Pts',(60.1409569239092,40.1149729312036,12.));
#168780=CARTESIAN_POINT('Ctrl Pts',(60.1649044612828,40.1205235273739,12.));
#168781=CARTESIAN_POINT('Ctrl Pts',(60.1888973042152,40.1260602681644,12.));
#168782=CARTESIAN_POINT('Ctrl Pts',(60.2129353562622,40.1315830718577,12.));
#168783=CARTESIAN_POINT('Ctrl Pts',(60.2370185212964,40.1370918571304,12.));
#168784=CARTESIAN_POINT('Ctrl Pts',(60.2611467035116,40.1425865430472,12.));
#168785=CARTESIAN_POINT('Ctrl Pts',(60.285319807422,40.1480670490586,12.));
#168786=CARTESIAN_POINT('Ctrl Pts',(60.3095377378586,40.1535332949976,12.));
#168787=CARTESIAN_POINT('Ctrl Pts',(60.3338003999607,40.1589852010804,12.));
#168788=CARTESIAN_POINT('Ctrl Pts',(60.3581076991716,40.1644226879033,12.));
#168789=CARTESIAN_POINT('Ctrl Pts',(60.3824595412445,40.1698456764377,12.));
#168790=CARTESIAN_POINT('Ctrl Pts',(60.4068558322407,40.1752540880268,12.));
#168791=CARTESIAN_POINT('Ctrl Pts',(60.4312964785273,40.180647844383,12.));
#168792=CARTESIAN_POINT('Ctrl Pts',(60.455781386769,40.1860268675884,12.));
#168793=CARTESIAN_POINT('Ctrl Pts',(60.4803104639225,40.1913910800921,12.));
#168794=CARTESIAN_POINT('Ctrl Pts',(60.5048836172435,40.1967404047062,12.));
#168795=CARTESIAN_POINT('Ctrl Pts',(60.5295007542841,40.2020747646014,12.));
#168796=CARTESIAN_POINT('Ctrl Pts',(60.5541617828925,40.2073940833053,12.));
#168797=CARTESIAN_POINT('Ctrl Pts',(60.5788666112042,40.2126982847011,12.));
#168798=CARTESIAN_POINT('Ctrl Pts',(60.6036151476349,40.2179872930273,12.));
#168799=CARTESIAN_POINT('Ctrl Pts',(60.6284073008871,40.2232610328721,12.));
#168800=CARTESIAN_POINT('Ctrl Pts',(60.6532429799499,40.2285194291706,12.));
#168801=CARTESIAN_POINT('Ctrl Pts',(60.678122094098,40.2337624072029,12.));
#168802=CARTESIAN_POINT('Ctrl Pts',(60.7030445528857,40.2389898925932,12.));
#168803=CARTESIAN_POINT('Ctrl Pts',(60.728010266139,40.2442018113108,12.));
#168804=CARTESIAN_POINT('Ctrl Pts',(60.7530191439593,40.2493980896638,12.));
#168805=CARTESIAN_POINT('Ctrl Pts',(60.7780710967248,40.2545786542953,12.));
#168806=CARTESIAN_POINT('Ctrl Pts',(60.8031660350879,40.2597434321803,12.));
#168807=CARTESIAN_POINT('Ctrl Pts',(60.8283038699706,40.2648923506248,12.));
#168808=CARTESIAN_POINT('Ctrl Pts',(60.8534845125538,40.2700253372648,12.));
#168809=CARTESIAN_POINT('Ctrl Pts',(60.8787078742818,40.2751423200639,12.));
#168810=CARTESIAN_POINT('Ctrl Pts',(60.9039738668669,40.2802432273104,12.));
#168811=CARTESIAN_POINT('Ctrl Pts',(60.9292824022887,40.2853279876161,12.));
#168812=CARTESIAN_POINT('Ctrl Pts',(60.9546333927921,40.2903965299155,12.));
#168813=CARTESIAN_POINT('Ctrl Pts',(60.9800267508786,40.295448783469,12.));
#168814=CARTESIAN_POINT('Ctrl Pts',(61.0054623893066,40.300484677858,12.));
#168815=CARTESIAN_POINT('Ctrl Pts',(61.0309402210921,40.3055041429775,12.));
#168816=CARTESIAN_POINT('Ctrl Pts',(61.056460159505,40.310507109031,12.));
#168817=CARTESIAN_POINT('Ctrl Pts',(61.0820221180645,40.3154935065262,12.));
#168818=CARTESIAN_POINT('Ctrl Pts',(61.1076260105258,40.3204632662725,12.));
#168819=CARTESIAN_POINT('Ctrl Pts',(61.1332717508789,40.32541631938,12.));
#168820=CARTESIAN_POINT('Ctrl Pts',(61.1589592533613,40.3303525972615,12.));
#168821=CARTESIAN_POINT('Ctrl Pts',(61.1846884324644,40.335272031637,12.));
#168822=CARTESIAN_POINT('Ctrl Pts',(61.2104592029377,40.340174554537,12.));
#168823=CARTESIAN_POINT('Ctrl Pts',(61.23627147979,40.3450600983109,12.));
#168824=CARTESIAN_POINT('Ctrl Pts',(61.2621251782863,40.3499285956304,12.));
#168825=CARTESIAN_POINT('Ctrl Pts',(61.2880202139371,40.3547799794679,12.));
#168826=CARTESIAN_POINT('Ctrl Pts',(61.3139565024847,40.3596141830791,12.));
#168827=CARTESIAN_POINT('Ctrl Pts',(61.3399339598853,40.3644311399861,12.));
#168828=CARTESIAN_POINT('Ctrl Pts',(61.3659525022908,40.3692307839636,12.));
#168829=CARTESIAN_POINT('Ctrl Pts',(61.3920120460219,40.3740130490225,12.));
#168830=CARTESIAN_POINT('Ctrl Pts',(61.4181125076037,40.3787778694364,12.));
#168831=CARTESIAN_POINT('Ctrl Pts',(61.4442538038044,40.383525179772,12.));
#168832=CARTESIAN_POINT('Ctrl Pts',(61.4704358516709,40.3882549149228,12.));
#168833=CARTESIAN_POINT('Ctrl Pts',(61.4966585685549,40.3929670101366,12.));
#168834=CARTESIAN_POINT('Ctrl Pts',(61.522921872154,40.3976614010652,12.));
#168835=CARTESIAN_POINT('Ctrl Pts',(61.5492256804717,40.4023380237232,12.));
#168836=CARTESIAN_POINT('Ctrl Pts',(61.5755699117324,40.4069968143956,12.));
#168837=CARTESIAN_POINT('Ctrl Pts',(61.601954484301,40.4116377095596,12.));
#168838=CARTESIAN_POINT('Ctrl Pts',(61.628379316608,40.4162606458119,12.));
#168839=CARTESIAN_POINT('Ctrl Pts',(61.6548443270394,40.4208655597717,12.));
#168840=CARTESIAN_POINT('Ctrl Pts',(61.6813494339286,40.425452388076,12.));
#168841=CARTESIAN_POINT('Ctrl Pts',(61.7078945557799,40.430021067584,12.));
#168842=CARTESIAN_POINT('Ctrl Pts',(61.7344796114399,40.4345715355405,12.));
#168843=CARTESIAN_POINT('Ctrl Pts',(61.7611045202874,40.4391037297589,12.));
#168844=CARTESIAN_POINT('Ctrl Pts',(61.7877692024076,40.4436175887949,12.));
#168845=CARTESIAN_POINT('Ctrl Pts',(61.814473578779,40.4481130521364,12.));
#168846=CARTESIAN_POINT('Ctrl Pts',(61.8412175708552,40.4525900597894,12.));
#168847=CARTESIAN_POINT('Ctrl Pts',(61.8680011001537,40.4570485518749,12.));
#168848=CARTESIAN_POINT('Ctrl Pts',(61.8948240878008,40.4614884681889,12.));
#168849=CARTESIAN_POINT('Ctrl Pts',(61.9216864541744,40.4659097478587,12.));
#168850=CARTESIAN_POINT('Ctrl Pts',(61.9485881182921,40.4703123287621,12.));
#168851=CARTESIAN_POINT('Ctrl Pts',(61.9755289983044,40.4746961480015,12.));
#168852=CARTESIAN_POINT('Ctrl Pts',(62.0025090125959,40.4790611429583,12.));
#168853=CARTESIAN_POINT('Ctrl Pts',(62.029528080742,40.4834072522164,12.));
#168854=CARTESIAN_POINT('Ctrl Pts',(62.0565861244179,40.4877344164411,12.));
#168855=CARTESIAN_POINT('Ctrl Pts',(62.0836830685719,40.4920425795217,12.));
#168856=CARTESIAN_POINT('Ctrl Pts',(62.1108188417003,40.4963316888412,12.));
#168857=CARTESIAN_POINT('Ctrl Pts',(62.1341126810541,40.4999919096264,12.));
#168858=CARTESIAN_POINT('Ctrl Pts',(62.1519925002974,40.5027877865802,12.));
#168859=CARTESIAN_POINT('Ctrl Pts',(62.1644411502821,40.5047277935767,12.));
#168860=CARTESIAN_POINT('Ctrl Pts',(62.1714473138102,40.5058175523127,12.));
#168861=CARTESIAN_POINT('Ctrl Pts',(62.1730054756871,40.5060598100929,12.));
#168862=CARTESIAN_POINT('',(57.8261117662439,39.4479504917286,0.));
#168863=CARTESIAN_POINT('',(57.8261117662439,39.4479504917286,0.));
#168864=CARTESIAN_POINT('Ctrl Pts',(62.1730054756871,40.5060598100929,0.));
#168865=CARTESIAN_POINT('Ctrl Pts',(62.1714473138102,40.5058175523127,0.));
#168866=CARTESIAN_POINT('Ctrl Pts',(62.1644411502821,40.5047277935767,0.));
#168867=CARTESIAN_POINT('Ctrl Pts',(62.1519925002974,40.5027877865802,0.));
#168868=CARTESIAN_POINT('Ctrl Pts',(62.1341126810541,40.4999919096264,0.));
#168869=CARTESIAN_POINT('Ctrl Pts',(62.1108188417003,40.4963316888412,0.));
#168870=CARTESIAN_POINT('Ctrl Pts',(62.0836830685719,40.4920425795217,0.));
#168871=CARTESIAN_POINT('Ctrl Pts',(62.0565861244179,40.4877344164411,0.));
#168872=CARTESIAN_POINT('Ctrl Pts',(62.029528080742,40.4834072522164,0.));
#168873=CARTESIAN_POINT('Ctrl Pts',(62.0025090125959,40.4790611429583,0.));
#168874=CARTESIAN_POINT('Ctrl Pts',(61.9755289983044,40.4746961480015,0.));
#168875=CARTESIAN_POINT('Ctrl Pts',(61.9485881182921,40.4703123287621,0.));
#168876=CARTESIAN_POINT('Ctrl Pts',(61.9216864541744,40.4659097478587,0.));
#168877=CARTESIAN_POINT('Ctrl Pts',(61.8948240878008,40.4614884681889,0.));
#168878=CARTESIAN_POINT('Ctrl Pts',(61.8680011001537,40.4570485518749,0.));
#168879=CARTESIAN_POINT('Ctrl Pts',(61.8412175708552,40.4525900597894,0.));
#168880=CARTESIAN_POINT('Ctrl Pts',(61.814473578779,40.4481130521364,0.));
#168881=CARTESIAN_POINT('Ctrl Pts',(61.7877692024076,40.4436175887949,0.));
#168882=CARTESIAN_POINT('Ctrl Pts',(61.7611045202874,40.4391037297589,0.));
#168883=CARTESIAN_POINT('Ctrl Pts',(61.7344796114399,40.4345715355405,0.));
#168884=CARTESIAN_POINT('Ctrl Pts',(61.7078945557799,40.430021067584,0.));
#168885=CARTESIAN_POINT('Ctrl Pts',(61.6813494339286,40.425452388076,0.));
#168886=CARTESIAN_POINT('Ctrl Pts',(61.6548443270394,40.4208655597717,0.));
#168887=CARTESIAN_POINT('Ctrl Pts',(61.628379316608,40.4162606458119,0.));
#168888=CARTESIAN_POINT('Ctrl Pts',(61.601954484301,40.4116377095596,0.));
#168889=CARTESIAN_POINT('Ctrl Pts',(61.5755699117324,40.4069968143956,0.));
#168890=CARTESIAN_POINT('Ctrl Pts',(61.5492256804717,40.4023380237232,0.));
#168891=CARTESIAN_POINT('Ctrl Pts',(61.522921872154,40.3976614010652,0.));
#168892=CARTESIAN_POINT('Ctrl Pts',(61.4966585685549,40.3929670101366,0.));
#168893=CARTESIAN_POINT('Ctrl Pts',(61.4704358516709,40.3882549149228,0.));
#168894=CARTESIAN_POINT('Ctrl Pts',(61.4442538038044,40.383525179772,0.));
#168895=CARTESIAN_POINT('Ctrl Pts',(61.4181125076037,40.3787778694364,0.));
#168896=CARTESIAN_POINT('Ctrl Pts',(61.3920120460219,40.3740130490225,0.));
#168897=CARTESIAN_POINT('Ctrl Pts',(61.3659525022908,40.3692307839636,0.));
#168898=CARTESIAN_POINT('Ctrl Pts',(61.3399339598853,40.3644311399861,0.));
#168899=CARTESIAN_POINT('Ctrl Pts',(61.3139565024847,40.3596141830791,0.));
#168900=CARTESIAN_POINT('Ctrl Pts',(61.2880202139371,40.3547799794679,0.));
#168901=CARTESIAN_POINT('Ctrl Pts',(61.2621251782863,40.3499285956304,0.));
#168902=CARTESIAN_POINT('Ctrl Pts',(61.23627147979,40.3450600983109,0.));
#168903=CARTESIAN_POINT('Ctrl Pts',(61.2104592029377,40.340174554537,0.));
#168904=CARTESIAN_POINT('Ctrl Pts',(61.1846884324644,40.335272031637,0.));
#168905=CARTESIAN_POINT('Ctrl Pts',(61.1589592533613,40.3303525972615,0.));
#168906=CARTESIAN_POINT('Ctrl Pts',(61.1332717508789,40.32541631938,0.));
#168907=CARTESIAN_POINT('Ctrl Pts',(61.1076260105258,40.3204632662725,0.));
#168908=CARTESIAN_POINT('Ctrl Pts',(61.0820221180645,40.3154935065262,0.));
#168909=CARTESIAN_POINT('Ctrl Pts',(61.056460159505,40.310507109031,0.));
#168910=CARTESIAN_POINT('Ctrl Pts',(61.0309402210921,40.3055041429775,0.));
#168911=CARTESIAN_POINT('Ctrl Pts',(61.0054623893066,40.300484677858,0.));
#168912=CARTESIAN_POINT('Ctrl Pts',(60.9800267508786,40.295448783469,0.));
#168913=CARTESIAN_POINT('Ctrl Pts',(60.9546333927921,40.2903965299155,0.));
#168914=CARTESIAN_POINT('Ctrl Pts',(60.9292824022887,40.2853279876161,0.));
#168915=CARTESIAN_POINT('Ctrl Pts',(60.9039738668669,40.2802432273104,0.));
#168916=CARTESIAN_POINT('Ctrl Pts',(60.8787078742818,40.2751423200639,0.));
#168917=CARTESIAN_POINT('Ctrl Pts',(60.8534845125538,40.2700253372648,0.));
#168918=CARTESIAN_POINT('Ctrl Pts',(60.8283038699706,40.2648923506248,0.));
#168919=CARTESIAN_POINT('Ctrl Pts',(60.8031660350879,40.2597434321803,0.));
#168920=CARTESIAN_POINT('Ctrl Pts',(60.7780710967248,40.2545786542953,0.));
#168921=CARTESIAN_POINT('Ctrl Pts',(60.7530191439593,40.2493980896638,0.));
#168922=CARTESIAN_POINT('Ctrl Pts',(60.728010266139,40.2442018113108,0.));
#168923=CARTESIAN_POINT('Ctrl Pts',(60.7030445528857,40.2389898925932,0.));
#168924=CARTESIAN_POINT('Ctrl Pts',(60.678122094098,40.2337624072029,0.));
#168925=CARTESIAN_POINT('Ctrl Pts',(60.6532429799499,40.2285194291706,0.));
#168926=CARTESIAN_POINT('Ctrl Pts',(60.6284073008871,40.2232610328721,0.));
#168927=CARTESIAN_POINT('Ctrl Pts',(60.6036151476349,40.2179872930273,0.));
#168928=CARTESIAN_POINT('Ctrl Pts',(60.5788666112042,40.2126982847011,0.));
#168929=CARTESIAN_POINT('Ctrl Pts',(60.5541617828925,40.2073940833053,0.));
#168930=CARTESIAN_POINT('Ctrl Pts',(60.5295007542841,40.2020747646014,0.));
#168931=CARTESIAN_POINT('Ctrl Pts',(60.5048836172435,40.1967404047062,0.));
#168932=CARTESIAN_POINT('Ctrl Pts',(60.4803104639225,40.1913910800921,0.));
#168933=CARTESIAN_POINT('Ctrl Pts',(60.455781386769,40.1860268675884,0.));
#168934=CARTESIAN_POINT('Ctrl Pts',(60.4312964785273,40.180647844383,0.));
#168935=CARTESIAN_POINT('Ctrl Pts',(60.4068558322407,40.1752540880268,0.));
#168936=CARTESIAN_POINT('Ctrl Pts',(60.3824595412445,40.1698456764377,0.));
#168937=CARTESIAN_POINT('Ctrl Pts',(60.3581076991716,40.1644226879033,0.));
#168938=CARTESIAN_POINT('Ctrl Pts',(60.3338003999607,40.1589852010804,0.));
#168939=CARTESIAN_POINT('Ctrl Pts',(60.3095377378586,40.1535332949976,0.));
#168940=CARTESIAN_POINT('Ctrl Pts',(60.285319807422,40.1480670490586,0.));
#168941=CARTESIAN_POINT('Ctrl Pts',(60.2611467035116,40.1425865430472,0.));
#168942=CARTESIAN_POINT('Ctrl Pts',(60.2370185212964,40.1370918571304,0.));
#168943=CARTESIAN_POINT('Ctrl Pts',(60.2129353562622,40.1315830718577,0.));
#168944=CARTESIAN_POINT('Ctrl Pts',(60.1888973042152,40.1260602681644,0.));
#168945=CARTESIAN_POINT('Ctrl Pts',(60.1649044612828,40.1205235273739,0.));
#168946=CARTESIAN_POINT('Ctrl Pts',(60.1409569239092,40.1149729312036,0.));
#168947=CARTESIAN_POINT('Ctrl Pts',(60.1170547888574,40.1094085617674,0.));
#168948=CARTESIAN_POINT('Ctrl Pts',(60.0931981532198,40.1038305015766,0.));
#168949=CARTESIAN_POINT('Ctrl Pts',(60.069387114421,40.0982388335423,0.));
#168950=CARTESIAN_POINT('Ctrl Pts',(60.0456217702202,40.0926336409785,0.));
#168951=CARTESIAN_POINT('Ctrl Pts',(60.021902218706,40.0870150076074,0.));
#168952=CARTESIAN_POINT('Ctrl Pts',(59.9982285582983,40.0813830175623,0.));
#168953=CARTESIAN_POINT('Ctrl Pts',(59.9746008877584,40.0757377553888,0.));
#168954=CARTESIAN_POINT('Ctrl Pts',(59.9510193061927,40.0700793060473,0.));
#168955=CARTESIAN_POINT('Ctrl Pts',(59.9274839130553,40.0644077549159,0.));
#168956=CARTESIAN_POINT('Ctrl Pts',(59.9039948081432,40.0587231877961,0.));
#168957=CARTESIAN_POINT('Ctrl Pts',(59.8805520915975,40.0530256909162,0.));
#168958=CARTESIAN_POINT('Ctrl Pts',(59.8571558639145,40.0473153509323,0.));
#168959=CARTESIAN_POINT('Ctrl Pts',(59.8338062259491,40.0415922549313,0.));
#168960=CARTESIAN_POINT('Ctrl Pts',(59.8105032789179,40.035856490434,0.));
#168961=CARTESIAN_POINT('Ctrl Pts',(59.7872471243948,40.0301081454006,0.));
#168962=CARTESIAN_POINT('Ctrl Pts',(59.7640378643115,40.0243473082343,0.));
#168963=CARTESIAN_POINT('Ctrl Pts',(59.7408756009688,40.0185740677827,0.));
#168964=CARTESIAN_POINT('Ctrl Pts',(59.7177604370409,40.0127885133407,0.));
#168965=CARTESIAN_POINT('Ctrl Pts',(59.6946924755771,40.0069907346536,0.));
#168966=CARTESIAN_POINT('Ctrl Pts',(59.671671819999,40.0011808219231,0.));
#168967=CARTESIAN_POINT('Ctrl Pts',(59.6486985741015,39.9953588658114,0.));
#168968=CARTESIAN_POINT('Ctrl Pts',(59.6257728420644,39.9895249574432,0.));
#168969=CARTESIAN_POINT('Ctrl Pts',(59.6028947284551,39.9836791884071,0.));
#168970=CARTESIAN_POINT('Ctrl Pts',(59.5800643382322,39.9778216507609,0.));
#168971=CARTESIAN_POINT('Ctrl Pts',(59.5572817767412,39.971952437036,0.));
#168972=CARTESIAN_POINT('Ctrl Pts',(59.5345471497162,39.9660716402423,0.));
#168973=CARTESIAN_POINT('Ctrl Pts',(59.511860563292,39.96017935387,0.));
#168974=CARTESIAN_POINT('Ctrl Pts',(59.4892221240081,39.954275671893,0.));
#168975=CARTESIAN_POINT('Ctrl Pts',(59.4666319388123,39.9483606887731,0.));
#168976=CARTESIAN_POINT('Ctrl Pts',(59.444090115055,39.9424344994652,0.));
#168977=CARTESIAN_POINT('Ctrl Pts',(59.4215967604925,39.9364971994215,0.));
#168978=CARTESIAN_POINT('Ctrl Pts',(59.3991519832981,39.9305488845934,0.));
#168979=CARTESIAN_POINT('Ctrl Pts',(59.3767558920663,39.9245896514359,0.));
#168980=CARTESIAN_POINT('Ctrl Pts',(59.3544085958165,39.9186195969113,0.));
#168981=CARTESIAN_POINT('Ctrl Pts',(59.3321102039883,39.9126388184956,0.));
#168982=CARTESIAN_POINT('Ctrl Pts',(59.3098608264452,39.9066474141826,0.));
#168983=CARTESIAN_POINT('Ctrl Pts',(59.2876605734871,39.9006454824861,0.));
#168984=CARTESIAN_POINT('Ctrl Pts',(59.2655095558527,39.8946331224442,0.));
#168985=CARTESIAN_POINT('Ctrl Pts',(59.2434078847236,39.8886104336234,0.));
#168986=CARTESIAN_POINT('Ctrl Pts',(59.2213556717189,39.8825775161252,0.));
#168987=CARTESIAN_POINT('Ctrl Pts',(59.1993530289008,39.8765344705895,0.));
#168988=CARTESIAN_POINT('Ctrl Pts',(59.1774000687865,39.8704813981978,0.));
#168989=CARTESIAN_POINT('Ctrl Pts',(59.155496904352,39.8644184006785,0.));
#168990=CARTESIAN_POINT('Ctrl Pts',(59.133643649035,39.8583455803111,0.));
#168991=CARTESIAN_POINT('Ctrl Pts',(59.1118404167304,39.8522630399337,0.));
#168992=CARTESIAN_POINT('Ctrl Pts',(59.0900873217992,39.8461708829465,0.));
#168993=CARTESIAN_POINT('Ctrl Pts',(59.068384479077,39.8400692133143,0.));
#168994=CARTESIAN_POINT('Ctrl Pts',(59.0467320038782,39.8339581355715,0.));
#168995=CARTESIAN_POINT('Ctrl Pts',(59.0251300119972,39.8278377548261,0.));
#168996=CARTESIAN_POINT('Ctrl Pts',(59.0035786197024,39.8217081767658,0.));
#168997=CARTESIAN_POINT('Ctrl Pts',(58.9820779437485,39.8155695076625,0.));
#168998=CARTESIAN_POINT('Ctrl Pts',(58.9606281013876,39.8094218543781,0.));
#168999=CARTESIAN_POINT('Ctrl Pts',(58.9392292103747,39.8032653243712,0.));
#169000=CARTESIAN_POINT('Ctrl Pts',(58.9178813889703,39.7971000257044,0.));
#169001=CARTESIAN_POINT('Ctrl Pts',(58.896584755939,39.7909260670517,0.));
#169002=CARTESIAN_POINT('Ctrl Pts',(58.8753394305583,39.7847435576995,0.));
#169003=CARTESIAN_POINT('Ctrl Pts',(58.8541455326229,39.7785526075477,0.));
#169004=CARTESIAN_POINT('Ctrl Pts',(58.8330031824453,39.772353327112,0.));
#169005=CARTESIAN_POINT('Ctrl Pts',(58.8119125008521,39.7661458275276,0.));
#169006=CARTESIAN_POINT('Ctrl Pts',(58.7908736091808,39.7599302205527,0.));
#169007=CARTESIAN_POINT('Ctrl Pts',(58.769886629304,39.753706618582,0.));
#169008=CARTESIAN_POINT('Ctrl Pts',(58.7489516836453,39.7474751346603,0.));
#169009=CARTESIAN_POINT('Ctrl Pts',(58.7280688951911,39.7412358824949,0.));
#169010=CARTESIAN_POINT('Ctrl Pts',(58.7072383875009,39.7349889764737,0.));
#169011=CARTESIAN_POINT('Ctrl Pts',(58.6864602847064,39.7287345316664,0.));
#169012=CARTESIAN_POINT('Ctrl Pts',(58.6657347115014,39.7224726638087,0.));
#169013=CARTESIAN_POINT('Ctrl Pts',(58.6450617931269,39.7162034892896,0.));
#169014=CARTESIAN_POINT('Ctrl Pts',(58.6244416553574,39.7099271251421,0.));
#169015=CARTESIAN_POINT('Ctrl Pts',(58.6038744244683,39.7036436890248,0.));
#169016=CARTESIAN_POINT('Ctrl Pts',(58.5833602272767,39.6973532992555,0.));
#169017=CARTESIAN_POINT('Ctrl Pts',(58.5628991912067,39.6910560748639,0.));
#169018=CARTESIAN_POINT('Ctrl Pts',(58.5424914443415,39.6847521356395,0.));
#169019=CARTESIAN_POINT('Ctrl Pts',(58.5221371154748,39.6784416021817,0.));
#169020=CARTESIAN_POINT('Ctrl Pts',(58.5018363341582,39.6721245959516,0.));
#169021=CARTESIAN_POINT('Ctrl Pts',(58.4815892306044,39.66580123918,0.));
#169022=CARTESIAN_POINT('Ctrl Pts',(58.4613959355776,39.6594716547681,0.));
#169023=CARTESIAN_POINT('Ctrl Pts',(58.4412565802984,39.6531359662043,0.));
#169024=CARTESIAN_POINT('Ctrl Pts',(58.4211712963023,39.6467942974465,0.));
#169025=CARTESIAN_POINT('Ctrl Pts',(58.4011402154225,39.6404467729113,0.));
#169026=CARTESIAN_POINT('Ctrl Pts',(58.3811634701061,39.6340935177492,0.));
#169027=CARTESIAN_POINT('Ctrl Pts',(58.3612411936914,39.6277346580898,0.));
#169028=CARTESIAN_POINT('Ctrl Pts',(58.3413735206412,39.6213703212523,0.));
#169029=CARTESIAN_POINT('Ctrl Pts',(58.3215605869192,39.6150006360894,0.));
#169030=CARTESIAN_POINT('Ctrl Pts',(58.3018025297288,39.6086257327559,0.));
#169031=CARTESIAN_POINT('Ctrl Pts',(58.2820994868092,39.6022457420772,0.));
#169032=CARTESIAN_POINT('Ctrl Pts',(58.2624515958416,39.5958607950237,0.));
#169033=CARTESIAN_POINT('Ctrl Pts',(58.2428589938394,39.589471022173,0.));
#169034=CARTESIAN_POINT('Ctrl Pts',(58.2233218164407,39.5830765530919,0.));
#169035=CARTESIAN_POINT('Ctrl Pts',(58.2038401992496,39.5766775175226,0.));
#169036=CARTESIAN_POINT('Ctrl Pts',(58.1844142794359,39.5702740468013,0.));
#169037=CARTESIAN_POINT('Ctrl Pts',(58.1650441970379,39.5638662750174,0.));
#169038=CARTESIAN_POINT('Ctrl Pts',(58.1457300968467,39.5574543406959,0.));
#169039=CARTESIAN_POINT('Ctrl Pts',(58.1264721285698,39.5510383869476,0.));
#169040=CARTESIAN_POINT('Ctrl Pts',(58.1072704428895,39.5446185579615,0.));
#169041=CARTESIAN_POINT('Ctrl Pts',(58.088125187991,39.5381949959214,0.));
#169042=CARTESIAN_POINT('Ctrl Pts',(58.0690365065393,39.5317678383231,0.));
#169043=CARTESIAN_POINT('Ctrl Pts',(58.050004530846,39.5253372136921,0.));
#169044=CARTESIAN_POINT('Ctrl Pts',(58.0310293875321,39.5189032457227,0.));
#169045=CARTESIAN_POINT('Ctrl Pts',(58.012111206794,39.5124660615009,0.));
#169046=CARTESIAN_POINT('Ctrl Pts',(57.9932501298522,39.5060257981225,0.));
#169047=CARTESIAN_POINT('Ctrl Pts',(57.9744463179305,39.4995826106691,0.));
#169048=CARTESIAN_POINT('Ctrl Pts',(57.9556999583777,39.4931366776627,0.));
#169049=CARTESIAN_POINT('Ctrl Pts',(57.9370112456506,39.4866881842223,0.));
#169050=CARTESIAN_POINT('Ctrl Pts',(57.9183803632337,39.4802373061008,0.));
#169051=CARTESIAN_POINT('Ctrl Pts',(57.8998074670541,39.4737841949417,0.));
#169052=CARTESIAN_POINT('Ctrl Pts',(57.8812926637397,39.4673289592425,0.));
#169053=CARTESIAN_POINT('Ctrl Pts',(57.8628360097134,39.4608716627367,0.));
#169054=CARTESIAN_POINT('Ctrl Pts',(57.8481172247805,39.4557042029884,0.));
#169055=CARTESIAN_POINT('Ctrl Pts',(57.8371043151607,39.45182770037,0.));
#169056=CARTESIAN_POINT('Ctrl Pts',(57.829774010102,39.4492429618498,0.));
#169057=CARTESIAN_POINT('Ctrl Pts',(57.8261117662439,39.4479504917286,0.));
#169058=CARTESIAN_POINT('Ctrl Pts',(65.7914953018525,34.9532422808861,0.));
#169059=CARTESIAN_POINT('Ctrl Pts',(65.7914953018525,34.9532422808861,12.));
#169060=CARTESIAN_POINT('Ctrl Pts',(65.7859084407617,34.9529266758466,0.));
#169061=CARTESIAN_POINT('Ctrl Pts',(65.7859084407617,34.9529266758466,12.));
#169062=CARTESIAN_POINT('Ctrl Pts',(65.7747383251112,34.9522931728759,0.));
#169063=CARTESIAN_POINT('Ctrl Pts',(65.7747383251112,34.9522931728759,12.));
#169064=CARTESIAN_POINT('Ctrl Pts',(65.7579939712289,34.9513360397454,0.));
#169065=CARTESIAN_POINT('Ctrl Pts',(65.7579939712289,34.9513360397454,12.));
#169066=CARTESIAN_POINT('Ctrl Pts',(65.7356898061147,34.9500461043246,0.));
#169067=CARTESIAN_POINT('Ctrl Pts',(65.7356898061147,34.9500461043246,12.));
#169068=CARTESIAN_POINT('Ctrl Pts',(65.7078456758034,34.9484107544137,0.));
#169069=CARTESIAN_POINT('Ctrl Pts',(65.7078456758034,34.9484107544137,12.));
#169070=CARTESIAN_POINT('Ctrl Pts',(65.6800376406066,34.9467524770439,0.));
#169071=CARTESIAN_POINT('Ctrl Pts',(65.6800376406066,34.9467524770439,12.));
#169072=CARTESIAN_POINT('Ctrl Pts',(65.6522657321322,34.9450712829183,0.));
#169073=CARTESIAN_POINT('Ctrl Pts',(65.6522657321322,34.9450712829183,12.));
#169074=CARTESIAN_POINT('Ctrl Pts',(65.624529996851,34.943367193292,0.));
#169075=CARTESIAN_POINT('Ctrl Pts',(65.624529996851,34.943367193292,12.));
#169076=CARTESIAN_POINT('Ctrl Pts',(65.5968304997584,34.9416402443435,0.));
#169077=CARTESIAN_POINT('Ctrl Pts',(65.5968304997584,34.9416402443435,12.));
#169078=CARTESIAN_POINT('Ctrl Pts',(65.5691673225803,34.9398904862157,0.));
#169079=CARTESIAN_POINT('Ctrl Pts',(65.5691673225803,34.9398904862157,12.));
#169080=CARTESIAN_POINT('Ctrl Pts',(65.5415405577955,34.9381179779673,0.));
#169081=CARTESIAN_POINT('Ctrl Pts',(65.5415405577955,34.9381179779673,12.));
#169082=CARTESIAN_POINT('Ctrl Pts',(65.5139503038036,34.9363227836582,0.));
#169083=CARTESIAN_POINT('Ctrl Pts',(65.5139503038036,34.9363227836582,12.));
#169084=CARTESIAN_POINT('Ctrl Pts',(65.4863966597544,34.9345049680826,0.));
#169085=CARTESIAN_POINT('Ctrl Pts',(65.4863966597544,34.9345049680826,12.));
#169086=CARTESIAN_POINT('Ctrl Pts',(65.4588797201972,34.932664592394,0.));
#169087=CARTESIAN_POINT('Ctrl Pts',(65.4588797201972,34.932664592394,12.));
#169088=CARTESIAN_POINT('Ctrl Pts',(65.4313995707536,34.9308017105536,0.));
#169089=CARTESIAN_POINT('Ctrl Pts',(65.4313995707536,34.9308017105536,12.));
#169090=CARTESIAN_POINT('Ctrl Pts',(65.4039562911352,34.9289163717747,0.));
#169091=CARTESIAN_POINT('Ctrl Pts',(65.4039562911352,34.9289163717747,12.));
#169092=CARTESIAN_POINT('Ctrl Pts',(65.3765499573077,34.9270086222731,0.));
#169093=CARTESIAN_POINT('Ctrl Pts',(65.3765499573077,34.9270086222731,12.));
#169094=CARTESIAN_POINT('Ctrl Pts',(65.3491806440537,34.9250785073477,0.));
#169095=CARTESIAN_POINT('Ctrl Pts',(65.3491806440537,34.9250785073477,12.));
#169096=CARTESIAN_POINT('Ctrl Pts',(65.321848427191,34.9231260731831,0.));
#169097=CARTESIAN_POINT('Ctrl Pts',(65.321848427191,34.9231260731831,12.));
#169098=CARTESIAN_POINT('Ctrl Pts',(65.2945533863761,34.9211513691355,0.));
#169099=CARTESIAN_POINT('Ctrl Pts',(65.2945533863761,34.9211513691355,12.));
#169100=CARTESIAN_POINT('Ctrl Pts',(65.2672956048069,34.9191544474872,0.));
#169101=CARTESIAN_POINT('Ctrl Pts',(65.2672956048069,34.9191544474872,12.));
#169102=CARTESIAN_POINT('Ctrl Pts',(65.2400751679549,34.9171353624113,0.));
#169103=CARTESIAN_POINT('Ctrl Pts',(65.2400751679549,34.9171353624113,12.));
#169104=CARTESIAN_POINT('Ctrl Pts',(65.2128921625823,34.9150941691747,0.));
#169105=CARTESIAN_POINT('Ctrl Pts',(65.2128921625823,34.9150941691747,12.));
#169106=CARTESIAN_POINT('Ctrl Pts',(65.1857466757092,34.9130309233022,0.));
#169107=CARTESIAN_POINT('Ctrl Pts',(65.1857466757092,34.9130309233022,12.));
#169108=CARTESIAN_POINT('Ctrl Pts',(65.1586387934241,34.9109456796213,0.));
#169109=CARTESIAN_POINT('Ctrl Pts',(65.1586387934241,34.9109456796213,12.));
#169110=CARTESIAN_POINT('Ctrl Pts',(65.1315686003516,34.9088384918336,0.));
#169111=CARTESIAN_POINT('Ctrl Pts',(65.1315686003516,34.9088384918336,12.));
#169112=CARTESIAN_POINT('Ctrl Pts',(65.1045361803121,34.9067094130399,0.));
#169113=CARTESIAN_POINT('Ctrl Pts',(65.1045361803121,34.9067094130399,12.));
#169114=CARTESIAN_POINT('Ctrl Pts',(65.0775416167085,34.9045584960509,0.));
#169115=CARTESIAN_POINT('Ctrl Pts',(65.0775416167085,34.9045584960509,12.));
#169116=CARTESIAN_POINT('Ctrl Pts',(65.0505849930171,34.9023857937865,0.));
#169117=CARTESIAN_POINT('Ctrl Pts',(65.0505849930171,34.9023857937865,12.));
#169118=CARTESIAN_POINT('Ctrl Pts',(65.0236663932328,34.9001913596416,0.));
#169119=CARTESIAN_POINT('Ctrl Pts',(65.0236663932328,34.9001913596416,12.));
#169120=CARTESIAN_POINT('Ctrl Pts',(64.9967859023212,34.8979752478616,0.));
#169121=CARTESIAN_POINT('Ctrl Pts',(64.9967859023212,34.8979752478616,12.));
#169122=CARTESIAN_POINT('Ctrl Pts',(64.9699436060169,34.8957375133697,0.));
#169123=CARTESIAN_POINT('Ctrl Pts',(64.9699436060169,34.8957375133697,12.));
#169124=CARTESIAN_POINT('Ctrl Pts',(64.9431395906337,34.8934782116095,0.));
#169125=CARTESIAN_POINT('Ctrl Pts',(64.9431395906337,34.8934782116095,12.));
#169126=CARTESIAN_POINT('Ctrl Pts',(64.9163739428605,34.8911973983785,0.));
#169127=CARTESIAN_POINT('Ctrl Pts',(64.9163739428605,34.8911973983785,12.));
#169128=CARTESIAN_POINT('Ctrl Pts',(64.8896467495757,34.888895129681,0.));
#169129=CARTESIAN_POINT('Ctrl Pts',(64.8896467495757,34.888895129681,12.));
#169130=CARTESIAN_POINT('Ctrl Pts',(64.8629580976063,34.8865714615436,0.));
#169131=CARTESIAN_POINT('Ctrl Pts',(64.8629580976063,34.8865714615436,12.));
#169132=CARTESIAN_POINT('Ctrl Pts',(64.8363080737377,34.8842264500188,0.));
#169133=CARTESIAN_POINT('Ctrl Pts',(64.8363080737377,34.8842264500188,12.));
#169134=CARTESIAN_POINT('Ctrl Pts',(64.8096967648307,34.881860151273,0.));
#169135=CARTESIAN_POINT('Ctrl Pts',(64.8096967648307,34.881860151273,12.));
#169136=CARTESIAN_POINT('Ctrl Pts',(64.7831242579028,34.8794726216513,0.));
#169137=CARTESIAN_POINT('Ctrl Pts',(64.7831242579028,34.8794726216513,12.));
#169138=CARTESIAN_POINT('Ctrl Pts',(64.7565906402151,34.8770639177493,0.));
#169139=CARTESIAN_POINT('Ctrl Pts',(64.7565906402151,34.8770639177493,12.));
#169140=CARTESIAN_POINT('Ctrl Pts',(64.7300959993653,34.8746340964972,0.));
#169141=CARTESIAN_POINT('Ctrl Pts',(64.7300959993653,34.8746340964972,12.));
#169142=CARTESIAN_POINT('Ctrl Pts',(64.7036404233306,34.8721832151975,0.));
#169143=CARTESIAN_POINT('Ctrl Pts',(64.7036404233306,34.8721832151975,12.));
#169144=CARTESIAN_POINT('Ctrl Pts',(64.6772240004228,34.869711331479,0.));
#169145=CARTESIAN_POINT('Ctrl Pts',(64.6772240004228,34.869711331479,12.));
#169146=CARTESIAN_POINT('Ctrl Pts',(64.6508468192599,34.867218503272,0.));
#169147=CARTESIAN_POINT('Ctrl Pts',(64.6508468192599,34.867218503272,12.));
#169148=CARTESIAN_POINT('Ctrl Pts',(64.6245089687277,34.8647047887774,0.));
#169149=CARTESIAN_POINT('Ctrl Pts',(64.6245089687277,34.8647047887774,12.));
#169150=CARTESIAN_POINT('Ctrl Pts',(64.5982105379383,34.8621702464401,0.));
#169151=CARTESIAN_POINT('Ctrl Pts',(64.5982105379383,34.8621702464401,12.));
#169152=CARTESIAN_POINT('Ctrl Pts',(64.5719516161927,34.8596149349257,0.));
#169153=CARTESIAN_POINT('Ctrl Pts',(64.5719516161927,34.8596149349257,12.));
#169154=CARTESIAN_POINT('Ctrl Pts',(64.5457322930088,34.857038913134,0.));
#169155=CARTESIAN_POINT('Ctrl Pts',(64.5457322930088,34.857038913134,12.));
#169156=CARTESIAN_POINT('Ctrl Pts',(64.5195526581407,34.8544422402118,0.));
#169157=CARTESIAN_POINT('Ctrl Pts',(64.5195526581407,34.8544422402118,12.));
#169158=CARTESIAN_POINT('Ctrl Pts',(64.4934128015985,34.851824975568,0.));
#169159=CARTESIAN_POINT('Ctrl Pts',(64.4934128015985,34.851824975568,12.));
#169160=CARTESIAN_POINT('Ctrl Pts',(64.4673128136625,34.8491871788896,0.));
#169161=CARTESIAN_POINT('Ctrl Pts',(64.4673128136625,34.8491871788896,12.));
#169162=CARTESIAN_POINT('Ctrl Pts',(64.4412527848969,34.8465289101622,0.));
#169163=CARTESIAN_POINT('Ctrl Pts',(64.4412527848969,34.8465289101622,12.));
#169164=CARTESIAN_POINT('Ctrl Pts',(64.4152328061515,34.8438502296664,0.));
#169165=CARTESIAN_POINT('Ctrl Pts',(64.4152328061515,34.8438502296664,12.));
#169166=CARTESIAN_POINT('Ctrl Pts',(64.3892529685607,34.8411511979702,0.));
#169167=CARTESIAN_POINT('Ctrl Pts',(64.3892529685607,34.8411511979702,12.));
#169168=CARTESIAN_POINT('Ctrl Pts',(64.3633133635382,34.8384318759248,0.));
#169169=CARTESIAN_POINT('Ctrl Pts',(64.3633133635382,34.8384318759248,12.));
#169170=CARTESIAN_POINT('Ctrl Pts',(64.3374140827711,34.8356923246618,0.));
#169171=CARTESIAN_POINT('Ctrl Pts',(64.3374140827711,34.8356923246618,12.));
#169172=CARTESIAN_POINT('Ctrl Pts',(64.3115552182062,34.8329326055919,0.));
#169173=CARTESIAN_POINT('Ctrl Pts',(64.3115552182062,34.8329326055919,12.));
#169174=CARTESIAN_POINT('Ctrl Pts',(64.285736862052,34.8301527804054,0.));
#169175=CARTESIAN_POINT('Ctrl Pts',(64.285736862052,34.8301527804054,12.));
#169176=CARTESIAN_POINT('Ctrl Pts',(64.2599591067916,34.8273529110744,0.));
#169177=CARTESIAN_POINT('Ctrl Pts',(64.2599591067916,34.8273529110744,12.));
#169178=CARTESIAN_POINT('Ctrl Pts',(64.234222045188,34.8245330598559,0.));
#169179=CARTESIAN_POINT('Ctrl Pts',(64.234222045188,34.8245330598559,12.));
#169180=CARTESIAN_POINT('Ctrl Pts',(64.2085257702884,34.8216932892969,0.));
#169181=CARTESIAN_POINT('Ctrl Pts',(64.2085257702884,34.8216932892969,12.));
#169182=CARTESIAN_POINT('Ctrl Pts',(64.1828703754236,34.8188336622419,0.));
#169183=CARTESIAN_POINT('Ctrl Pts',(64.1828703754236,34.8188336622419,12.));
#169184=CARTESIAN_POINT('Ctrl Pts',(64.1572559542086,34.8159542418374,0.));
#169185=CARTESIAN_POINT('Ctrl Pts',(64.1572559542086,34.8159542418374,12.));
#169186=CARTESIAN_POINT('Ctrl Pts',(64.1316826005506,34.8130550915287,0.));
#169187=CARTESIAN_POINT('Ctrl Pts',(64.1316826005506,34.8130550915287,12.));
#169188=CARTESIAN_POINT('Ctrl Pts',(64.1061504086515,34.8101362750597,0.));
#169189=CARTESIAN_POINT('Ctrl Pts',(64.1061504086515,34.8101362750597,12.));
#169190=CARTESIAN_POINT('Ctrl Pts',(64.0806594730085,34.8071978564748,0.));
#169191=CARTESIAN_POINT('Ctrl Pts',(64.0806594730085,34.8071978564748,12.));
#169192=CARTESIAN_POINT('Ctrl Pts',(64.0552098884095,34.8042399001211,0.));
#169193=CARTESIAN_POINT('Ctrl Pts',(64.0552098884095,34.8042399001211,12.));
#169194=CARTESIAN_POINT('Ctrl Pts',(64.0298017499294,34.8012624706527,0.));
#169195=CARTESIAN_POINT('Ctrl Pts',(64.0298017499294,34.8012624706527,12.));
#169196=CARTESIAN_POINT('Ctrl Pts',(64.0044351529402,34.7982656330293,0.));
#169197=CARTESIAN_POINT('Ctrl Pts',(64.0044351529402,34.7982656330293,12.));
#169198=CARTESIAN_POINT('Ctrl Pts',(63.9791101931162,34.7952494525178,0.));
#169199=CARTESIAN_POINT('Ctrl Pts',(63.9791101931162,34.7952494525178,12.));
#169200=CARTESIAN_POINT('Ctrl Pts',(63.9538269664366,34.7922139946943,0.));
#169201=CARTESIAN_POINT('Ctrl Pts',(63.9538269664366,34.7922139946943,12.));
#169202=CARTESIAN_POINT('Ctrl Pts',(63.9285855691845,34.7891593254488,0.));
#169203=CARTESIAN_POINT('Ctrl Pts',(63.9285855691845,34.7891593254488,12.));
#169204=CARTESIAN_POINT('Ctrl Pts',(63.9033860979435,34.7860855109911,0.));
#169205=CARTESIAN_POINT('Ctrl Pts',(63.9033860979435,34.7860855109911,12.));
#169206=CARTESIAN_POINT('Ctrl Pts',(63.8782286496062,34.7829926178496,0.));
#169207=CARTESIAN_POINT('Ctrl Pts',(63.8782286496062,34.7829926178496,12.));
#169208=CARTESIAN_POINT('Ctrl Pts',(63.8531133213793,34.7798807128715,0.));
#169209=CARTESIAN_POINT('Ctrl Pts',(63.8531133213793,34.7798807128715,12.));
#169210=CARTESIAN_POINT('Ctrl Pts',(63.8280402107856,34.7767498632243,0.));
#169211=CARTESIAN_POINT('Ctrl Pts',(63.8280402107856,34.7767498632243,12.));
#169212=CARTESIAN_POINT('Ctrl Pts',(63.8030094156639,34.7736001363993,0.));
#169213=CARTESIAN_POINT('Ctrl Pts',(63.8030094156639,34.7736001363993,12.));
#169214=CARTESIAN_POINT('Ctrl Pts',(63.778021034163,34.7704316002171,0.));
#169215=CARTESIAN_POINT('Ctrl Pts',(63.778021034163,34.7704316002171,12.));
#169216=CARTESIAN_POINT('Ctrl Pts',(63.7530751647494,34.7672443228275,0.));
#169217=CARTESIAN_POINT('Ctrl Pts',(63.7530751647494,34.7672443228275,12.));
#169218=CARTESIAN_POINT('Ctrl Pts',(63.7281719062149,34.7640383727101,0.));
#169219=CARTESIAN_POINT('Ctrl Pts',(63.7281719062149,34.7640383727101,12.));
#169220=CARTESIAN_POINT('Ctrl Pts',(63.7033113576785,34.7608138186759,0.));
#169221=CARTESIAN_POINT('Ctrl Pts',(63.7033113576785,34.7608138186759,12.));
#169222=CARTESIAN_POINT('Ctrl Pts',(63.6784936185885,34.7575707298713,0.));
#169223=CARTESIAN_POINT('Ctrl Pts',(63.6784936185885,34.7575707298713,12.));
#169224=CARTESIAN_POINT('Ctrl Pts',(63.6537187887159,34.7543091757833,0.));
#169225=CARTESIAN_POINT('Ctrl Pts',(63.6537187887159,34.7543091757833,12.));
#169226=CARTESIAN_POINT('Ctrl Pts',(63.6289869681604,34.7510292262406,0.));
#169227=CARTESIAN_POINT('Ctrl Pts',(63.6289869681604,34.7510292262406,12.));
#169228=CARTESIAN_POINT('Ctrl Pts',(63.6042982573588,34.7477309514136,0.));
#169229=CARTESIAN_POINT('Ctrl Pts',(63.6042982573588,34.7477309514136,12.));
#169230=CARTESIAN_POINT('Ctrl Pts',(63.5796527570871,34.744414421816,0.));
#169231=CARTESIAN_POINT('Ctrl Pts',(63.5796527570871,34.744414421816,12.));
#169232=CARTESIAN_POINT('Ctrl Pts',(63.5550505684626,34.7410797083081,0.));
#169233=CARTESIAN_POINT('Ctrl Pts',(63.5550505684626,34.7410797083081,12.));
#169234=CARTESIAN_POINT('Ctrl Pts',(63.5304917929386,34.7377268821026,0.));
#169235=CARTESIAN_POINT('Ctrl Pts',(63.5304917929386,34.7377268821026,12.));
#169236=CARTESIAN_POINT('Ctrl Pts',(63.505976532309,34.7343560147667,0.));
#169237=CARTESIAN_POINT('Ctrl Pts',(63.505976532309,34.7343560147667,12.));
#169238=CARTESIAN_POINT('Ctrl Pts',(63.4815048887165,34.7309671782214,0.));
#169239=CARTESIAN_POINT('Ctrl Pts',(63.4815048887165,34.7309671782214,12.));
#169240=CARTESIAN_POINT('Ctrl Pts',(63.4570769646569,34.7275604447439,0.));
#169241=CARTESIAN_POINT('Ctrl Pts',(63.4570769646569,34.7275604447439,12.));
#169242=CARTESIAN_POINT('Ctrl Pts',(63.4326928629795,34.7241358869701,0.));
#169243=CARTESIAN_POINT('Ctrl Pts',(63.4326928629795,34.7241358869701,12.));
#169244=CARTESIAN_POINT('Ctrl Pts',(63.4083526868836,34.7206935779007,0.));
#169245=CARTESIAN_POINT('Ctrl Pts',(63.4083526868836,34.7206935779007,12.));
#169246=CARTESIAN_POINT('Ctrl Pts',(63.3840565399208,34.7172335909038,0.));
#169247=CARTESIAN_POINT('Ctrl Pts',(63.3840565399208,34.7172335909038,12.));
#169248=CARTESIAN_POINT('Ctrl Pts',(63.3598045260053,34.7137559997146,0.));
#169249=CARTESIAN_POINT('Ctrl Pts',(63.3598045260053,34.7137559997146,12.));
#169250=CARTESIAN_POINT('Ctrl Pts',(63.3355967494171,34.7102608784374,0.));
#169251=CARTESIAN_POINT('Ctrl Pts',(63.3355967494171,34.7102608784374,12.));
#169252=CARTESIAN_POINT('Ctrl Pts',(63.3114333148048,34.7067483015491,0.));
#169253=CARTESIAN_POINT('Ctrl Pts',(63.3114333148048,34.7067483015491,12.));
#169254=CARTESIAN_POINT('Ctrl Pts',(63.2873143271806,34.7032183439041,0.));
#169255=CARTESIAN_POINT('Ctrl Pts',(63.2873143271806,34.7032183439041,12.));
#169256=CARTESIAN_POINT('Ctrl Pts',(63.2632398919225,34.6996710807378,0.));
#169257=CARTESIAN_POINT('Ctrl Pts',(63.2632398919225,34.6996710807378,12.));
#169258=CARTESIAN_POINT('Ctrl Pts',(63.2392101147847,34.6961065876666,0.));
#169259=CARTESIAN_POINT('Ctrl Pts',(63.2392101147847,34.6961065876666,12.));
#169260=CARTESIAN_POINT('Ctrl Pts',(63.2152251019012,34.6925249406897,0.));
#169261=CARTESIAN_POINT('Ctrl Pts',(63.2152251019012,34.6925249406897,12.));
#169262=CARTESIAN_POINT('Ctrl Pts',(63.1912849597887,34.6889262161924,0.));
#169263=CARTESIAN_POINT('Ctrl Pts',(63.1912849597887,34.6889262161924,12.));
#169264=CARTESIAN_POINT('Ctrl Pts',(63.1673897953429,34.6853104909518,0.));
#169265=CARTESIAN_POINT('Ctrl Pts',(63.1673897953429,34.6853104909518,12.));
#169266=CARTESIAN_POINT('Ctrl Pts',(63.1435397158388,34.6816778421402,0.));
#169267=CARTESIAN_POINT('Ctrl Pts',(63.1435397158388,34.6816778421402,12.));
#169268=CARTESIAN_POINT('Ctrl Pts',(63.119734828943,34.6780283473252,0.));
#169269=CARTESIAN_POINT('Ctrl Pts',(63.119734828943,34.6780283473252,12.));
#169270=CARTESIAN_POINT('Ctrl Pts',(63.0959752427168,34.674362084472,0.));
#169271=CARTESIAN_POINT('Ctrl Pts',(63.0959752427168,34.674362084472,12.));
#169272=CARTESIAN_POINT('Ctrl Pts',(63.0722610656194,34.670679131947,0.));
#169273=CARTESIAN_POINT('Ctrl Pts',(63.0722610656194,34.670679131947,12.));
#169274=CARTESIAN_POINT('Ctrl Pts',(63.0485924065045,34.6669795685229,0.));
#169275=CARTESIAN_POINT('Ctrl Pts',(63.0485924065045,34.6669795685229,12.));
#169276=CARTESIAN_POINT('Ctrl Pts',(63.0249693746208,34.6632634733824,0.));
#169277=CARTESIAN_POINT('Ctrl Pts',(63.0249693746208,34.6632634733824,12.));
#169278=CARTESIAN_POINT('Ctrl Pts',(63.0013920796235,34.6595309261191,0.));
#169279=CARTESIAN_POINT('Ctrl Pts',(63.0013920796235,34.6595309261191,12.));
#169280=CARTESIAN_POINT('Ctrl Pts',(62.9778606315783,34.6557820067393,0.));
#169281=CARTESIAN_POINT('Ctrl Pts',(62.9778606315783,34.6557820067393,12.));
#169282=CARTESIAN_POINT('Ctrl Pts',(62.9543751409645,34.6520167956655,0.));
#169283=CARTESIAN_POINT('Ctrl Pts',(62.9543751409645,34.6520167956655,12.));
#169284=CARTESIAN_POINT('Ctrl Pts',(62.9309357186717,34.6482353737424,0.));
#169285=CARTESIAN_POINT('Ctrl Pts',(62.9309357186717,34.6482353737424,12.));
#169286=CARTESIAN_POINT('Ctrl Pts',(62.9075424760015,34.6444378222411,0.));
#169287=CARTESIAN_POINT('Ctrl Pts',(62.9075424760015,34.6444378222411,12.));
#169288=CARTESIAN_POINT('Ctrl Pts',(62.8841955246794,34.6406242228592,0.));
#169289=CARTESIAN_POINT('Ctrl Pts',(62.8841955246794,34.6406242228592,12.));
#169290=CARTESIAN_POINT('Ctrl Pts',(62.8608949768571,34.6367946577235,0.));
#169291=CARTESIAN_POINT('Ctrl Pts',(62.8608949768571,34.6367946577235,12.));
#169292=CARTESIAN_POINT('Ctrl Pts',(62.8376409451175,34.6329492093935,0.));
#169293=CARTESIAN_POINT('Ctrl Pts',(62.8376409451175,34.6329492093935,12.));
#169294=CARTESIAN_POINT('Ctrl Pts',(62.8144335424697,34.6290879608673,0.));
#169295=CARTESIAN_POINT('Ctrl Pts',(62.8144335424697,34.6290879608673,12.));
#169296=CARTESIAN_POINT('Ctrl Pts',(62.7912728823518,34.6252109955853,0.));
#169297=CARTESIAN_POINT('Ctrl Pts',(62.7912728823518,34.6252109955853,12.));
#169298=CARTESIAN_POINT('Ctrl Pts',(62.7681590786429,34.6213183974317,0.));
#169299=CARTESIAN_POINT('Ctrl Pts',(62.7681590786429,34.6213183974317,12.));
#169300=CARTESIAN_POINT('Ctrl Pts',(62.7450922456676,34.6174102507375,0.));
#169301=CARTESIAN_POINT('Ctrl Pts',(62.7450922456676,34.6174102507375,12.));
#169302=CARTESIAN_POINT('Ctrl Pts',(62.7220724981994,34.6134866402837,0.));
#169303=CARTESIAN_POINT('Ctrl Pts',(62.7220724981994,34.6134866402837,12.));
#169304=CARTESIAN_POINT('Ctrl Pts',(62.6990999514563,34.6095476513077,0.));
#169305=CARTESIAN_POINT('Ctrl Pts',(62.6990999514563,34.6095476513077,12.));
#169306=CARTESIAN_POINT('Ctrl Pts',(62.6761747211037,34.6055933695069,0.));
#169307=CARTESIAN_POINT('Ctrl Pts',(62.6761747211037,34.6055933695069,12.));
#169308=CARTESIAN_POINT('Ctrl Pts',(62.6532969232657,34.6016238810399,0.));
#169309=CARTESIAN_POINT('Ctrl Pts',(62.6532969232657,34.6016238810399,12.));
#169310=CARTESIAN_POINT('Ctrl Pts',(62.6304666745306,34.5976392725296,0.));
#169311=CARTESIAN_POINT('Ctrl Pts',(62.6304666745306,34.5976392725296,12.));
#169312=CARTESIAN_POINT('Ctrl Pts',(62.6076840919536,34.5936396310679,0.));
#169313=CARTESIAN_POINT('Ctrl Pts',(62.6076840919536,34.5936396310679,12.));
#169314=CARTESIAN_POINT('Ctrl Pts',(62.5849492930533,34.5896250442216,0.));
#169315=CARTESIAN_POINT('Ctrl Pts',(62.5849492930533,34.5896250442216,12.));
#169316=CARTESIAN_POINT('Ctrl Pts',(62.562262395816,34.5855956000363,0.));
#169317=CARTESIAN_POINT('Ctrl Pts',(62.562262395816,34.5855956000363,12.));
#169318=CARTESIAN_POINT('Ctrl Pts',(62.5396235187079,34.5815513870377,0.));
#169319=CARTESIAN_POINT('Ctrl Pts',(62.5396235187079,34.5815513870377,12.));
#169320=CARTESIAN_POINT('Ctrl Pts',(62.5170327806781,34.5774924942355,0.));
#169321=CARTESIAN_POINT('Ctrl Pts',(62.5170327806781,34.5774924942355,12.));
#169322=CARTESIAN_POINT('Ctrl Pts',(62.4944903011628,34.5734190111272,0.));
#169323=CARTESIAN_POINT('Ctrl Pts',(62.4944903011628,34.5734190111272,12.));
#169324=CARTESIAN_POINT('Ctrl Pts',(62.4719962000808,34.5693310277051,0.));
#169325=CARTESIAN_POINT('Ctrl Pts',(62.4719962000808,34.5693310277051,12.));
#169326=CARTESIAN_POINT('Ctrl Pts',(62.4495505978393,34.5652286344593,0.));
#169327=CARTESIAN_POINT('Ctrl Pts',(62.4495505978393,34.5652286344593,12.));
#169328=CARTESIAN_POINT('Ctrl Pts',(62.4271536153459,34.5611119223799,0.));
#169329=CARTESIAN_POINT('Ctrl Pts',(62.4271536153459,34.5611119223799,12.));
#169330=CARTESIAN_POINT('Ctrl Pts',(62.4048053740127,34.5569809829613,0.));
#169331=CARTESIAN_POINT('Ctrl Pts',(62.4048053740127,34.5569809829613,12.));
#169332=CARTESIAN_POINT('Ctrl Pts',(62.3825059957601,34.5528359082075,0.));
#169333=CARTESIAN_POINT('Ctrl Pts',(62.3825059957601,34.5528359082075,12.));
#169334=CARTESIAN_POINT('Ctrl Pts',(62.3602556030127,34.5486767906384,0.));
#169335=CARTESIAN_POINT('Ctrl Pts',(62.3602556030127,34.5486767906384,12.));
#169336=CARTESIAN_POINT('Ctrl Pts',(62.338054318708,34.5445037232936,0.));
#169337=CARTESIAN_POINT('Ctrl Pts',(62.338054318708,34.5445037232936,12.));
#169338=CARTESIAN_POINT('Ctrl Pts',(62.3159022663058,34.5403167997337,0.));
#169339=CARTESIAN_POINT('Ctrl Pts',(62.3159022663058,34.5403167997337,12.));
#169340=CARTESIAN_POINT('Ctrl Pts',(62.2937995697925,34.5361161140449,0.));
#169341=CARTESIAN_POINT('Ctrl Pts',(62.2937995697925,34.5361161140449,12.));
#169342=CARTESIAN_POINT('Ctrl Pts',(62.2717463536827,34.5319017608433,0.));
#169343=CARTESIAN_POINT('Ctrl Pts',(62.2717463536827,34.5319017608433,12.));
#169344=CARTESIAN_POINT('Ctrl Pts',(62.2497427430135,34.5276738352808,0.));
#169345=CARTESIAN_POINT('Ctrl Pts',(62.2497427430135,34.5276738352808,12.));
#169346=CARTESIAN_POINT('Ctrl Pts',(62.2277888633576,34.5234324330491,0.));
#169347=CARTESIAN_POINT('Ctrl Pts',(62.2277888633576,34.5234324330491,12.));
#169348=CARTESIAN_POINT('Ctrl Pts',(62.2058848408347,34.5191776503842,0.));
#169349=CARTESIAN_POINT('Ctrl Pts',(62.2058848408347,34.5191776503842,12.));
#169350=CARTESIAN_POINT('Ctrl Pts',(62.1840308021171,34.514909584073,0.));
#169351=CARTESIAN_POINT('Ctrl Pts',(62.1840308021171,34.514909584073,12.));
#169352=CARTESIAN_POINT('Ctrl Pts',(62.1622268744336,34.5106283314594,0.));
#169353=CARTESIAN_POINT('Ctrl Pts',(62.1622268744336,34.5106283314594,12.));
#169354=CARTESIAN_POINT('Ctrl Pts',(62.1404731855686,34.5063339904533,0.));
#169355=CARTESIAN_POINT('Ctrl Pts',(62.1404731855686,34.5063339904533,12.));
#169356=CARTESIAN_POINT('Ctrl Pts',(62.1187698638705,34.5020266595292,0.));
#169357=CARTESIAN_POINT('Ctrl Pts',(62.1187698638705,34.5020266595292,12.));
#169358=CARTESIAN_POINT('Ctrl Pts',(62.0971170382565,34.4977064377281,0.));
#169359=CARTESIAN_POINT('Ctrl Pts',(62.0971170382565,34.4977064377281,12.));
#169360=CARTESIAN_POINT('Ctrl Pts',(62.0755148382136,34.4933734246593,0.));
#169361=CARTESIAN_POINT('Ctrl Pts',(62.0755148382136,34.4933734246593,12.));
#169362=CARTESIAN_POINT('Ctrl Pts',(62.0539633937944,34.4890277205042,0.));
#169363=CARTESIAN_POINT('Ctrl Pts',(62.0539633937944,34.4890277205042,12.));
#169364=CARTESIAN_POINT('Ctrl Pts',(62.0324628356152,34.4846694260205,0.));
#169365=CARTESIAN_POINT('Ctrl Pts',(62.0324628356152,34.4846694260205,12.));
#169366=CARTESIAN_POINT('Ctrl Pts',(62.0110132948807,34.4802986425535,0.));
#169367=CARTESIAN_POINT('Ctrl Pts',(62.0110132948807,34.4802986425535,12.));
#169368=CARTESIAN_POINT('Ctrl Pts',(61.9896149034009,34.4759154720477,0.));
#169369=CARTESIAN_POINT('Ctrl Pts',(61.9896149034009,34.4759154720477,12.));
#169370=CARTESIAN_POINT('Ctrl Pts',(61.9682677936048,34.4715200170589,0.));
#169371=CARTESIAN_POINT('Ctrl Pts',(61.9682677936048,34.4715200170589,12.));
#169372=CARTESIAN_POINT('Ctrl Pts',(61.9469720985512,34.4671123807706,0.));
#169373=CARTESIAN_POINT('Ctrl Pts',(61.9469720985512,34.4671123807706,12.));
#169374=CARTESIAN_POINT('Ctrl Pts',(61.9257279519283,34.462692666996,0.));
#169375=CARTESIAN_POINT('Ctrl Pts',(61.9257279519283,34.462692666996,12.));
#169376=CARTESIAN_POINT('Ctrl Pts',(61.9045354880424,34.4582609801625,0.));
#169377=CARTESIAN_POINT('Ctrl Pts',(61.9045354880424,34.4582609801625,12.));
#169378=CARTESIAN_POINT('Ctrl Pts',(61.883394841802,34.4538174253009,0.));
#169379=CARTESIAN_POINT('Ctrl Pts',(61.883394841802,34.4538174253009,12.));
#169380=CARTESIAN_POINT('Ctrl Pts',(61.862306148703,34.4493621080367,0.));
#169381=CARTESIAN_POINT('Ctrl Pts',(61.862306148703,34.4493621080367,12.));
#169382=CARTESIAN_POINT('Ctrl Pts',(61.8412695447951,34.4448951345753,0.));
#169383=CARTESIAN_POINT('Ctrl Pts',(61.8412695447951,34.4448951345753,12.));
#169384=CARTESIAN_POINT('Ctrl Pts',(61.8202851667247,34.4404166117313,0.));
#169385=CARTESIAN_POINT('Ctrl Pts',(61.8202851667247,34.4404166117313,12.));
#169386=CARTESIAN_POINT('Ctrl Pts',(61.7993531518052,34.4359266469757,0.));
#169387=CARTESIAN_POINT('Ctrl Pts',(61.7993531518052,34.4359266469757,12.));
#169388=CARTESIAN_POINT('Ctrl Pts',(61.7784736380727,34.4314253484792,0.));
#169389=CARTESIAN_POINT('Ctrl Pts',(61.7784736380727,34.4314253484792,12.));
#169390=CARTESIAN_POINT('Ctrl Pts',(61.7576467643419,34.4269128251569,0.));
#169391=CARTESIAN_POINT('Ctrl Pts',(61.7576467643419,34.4269128251569,12.));
#169392=CARTESIAN_POINT('Ctrl Pts',(61.7368726702573,34.4223891867166,0.));
#169393=CARTESIAN_POINT('Ctrl Pts',(61.7368726702573,34.4223891867166,12.));
#169394=CARTESIAN_POINT('Ctrl Pts',(61.7161514961892,34.4178545435753,0.));
#169395=CARTESIAN_POINT('Ctrl Pts',(61.7161514961892,34.4178545435753,12.));
#169396=CARTESIAN_POINT('Ctrl Pts',(61.6954833831157,34.4133090067696,0.));
#169397=CARTESIAN_POINT('Ctrl Pts',(61.6954833831157,34.4133090067696,12.));
#169398=CARTESIAN_POINT('Ctrl Pts',(61.674868472521,34.4087526878815,0.));
#169399=CARTESIAN_POINT('Ctrl Pts',(61.674868472521,34.4087526878815,12.));
#169400=CARTESIAN_POINT('Ctrl Pts',(61.6543069062436,34.4041856989328,0.));
#169401=CARTESIAN_POINT('Ctrl Pts',(61.6543069062436,34.4041856989328,12.));
#169402=CARTESIAN_POINT('Ctrl Pts',(61.6337988264586,34.399608152377,0.));
#169403=CARTESIAN_POINT('Ctrl Pts',(61.6337988264586,34.399608152377,12.));
#169404=CARTESIAN_POINT('Ctrl Pts',(61.6133443760168,34.3950201613446,0.));
#169405=CARTESIAN_POINT('Ctrl Pts',(61.6133443760168,34.3950201613446,12.));
#169406=CARTESIAN_POINT('Ctrl Pts',(61.5929436987419,34.3904218398642,0.));
#169407=CARTESIAN_POINT('Ctrl Pts',(61.5929436987419,34.3904218398642,12.));
#169408=CARTESIAN_POINT('Ctrl Pts',(61.5725969396817,34.3858133030511,0.));
#169409=CARTESIAN_POINT('Ctrl Pts',(61.5725969396817,34.3858133030511,12.));
#169410=CARTESIAN_POINT('Ctrl Pts',(61.5523042455127,34.3811946674179,0.));
#169411=CARTESIAN_POINT('Ctrl Pts',(61.5523042455127,34.3811946674179,12.));
#169412=CARTESIAN_POINT('Ctrl Pts',(61.5320657642601,34.3765660506659,0.));
#169413=CARTESIAN_POINT('Ctrl Pts',(61.5320657642601,34.3765660506659,12.));
#169414=CARTESIAN_POINT('Ctrl Pts',(61.511881644541,34.3719275711179,0.));
#169415=CARTESIAN_POINT('Ctrl Pts',(61.511881644541,34.3719275711179,12.));
#169416=CARTESIAN_POINT('Ctrl Pts',(61.4917520349276,34.3672793472464,0.));
#169417=CARTESIAN_POINT('Ctrl Pts',(61.4917520349276,34.3672793472464,12.));
#169418=CARTESIAN_POINT('Ctrl Pts',(61.4716770832924,34.3626214971903,0.));
#169419=CARTESIAN_POINT('Ctrl Pts',(61.4716770832924,34.3626214971903,12.));
#169420=CARTESIAN_POINT('Ctrl Pts',(61.4516569360499,34.357954138202,0.));
#169421=CARTESIAN_POINT('Ctrl Pts',(61.4516569360499,34.357954138202,12.));
#169422=CARTESIAN_POINT('Ctrl Pts',(61.4316917395959,34.3532773877112,0.));
#169423=CARTESIAN_POINT('Ctrl Pts',(61.4316917395959,34.3532773877112,12.));
#169424=CARTESIAN_POINT('Ctrl Pts',(61.4117816420251,34.3485913645991,0.));
#169425=CARTESIAN_POINT('Ctrl Pts',(61.4117816420251,34.3485913645991,12.));
#169426=CARTESIAN_POINT('Ctrl Pts',(61.3919267945293,34.34389619024,0.));
#169427=CARTESIAN_POINT('Ctrl Pts',(61.3919267945293,34.34389619024,12.));
#169428=CARTESIAN_POINT('Ctrl Pts',(61.3721273534222,34.339191990012,0.));
#169429=CARTESIAN_POINT('Ctrl Pts',(61.3721273534222,34.339191990012,12.));
#169430=CARTESIAN_POINT('Ctrl Pts',(61.3523834803144,34.3344788934337,0.));
#169431=CARTESIAN_POINT('Ctrl Pts',(61.3523834803144,34.3344788934337,12.));
#169432=CARTESIAN_POINT('Ctrl Pts',(61.3326953378817,34.3297570310126,0.));
#169433=CARTESIAN_POINT('Ctrl Pts',(61.3326953378817,34.3297570310126,12.));
#169434=CARTESIAN_POINT('Ctrl Pts',(61.3130630861375,34.3250265314761,0.));
#169435=CARTESIAN_POINT('Ctrl Pts',(61.3130630861375,34.3250265314761,12.));
#169436=CARTESIAN_POINT('Ctrl Pts',(61.2934868791875,34.3202875193629,0.));
#169437=CARTESIAN_POINT('Ctrl Pts',(61.2934868791875,34.3202875193629,12.));
#169438=CARTESIAN_POINT('Ctrl Pts',(61.2739668600415,34.3155401111777,0.));
#169439=CARTESIAN_POINT('Ctrl Pts',(61.2739668600415,34.3155401111777,12.));
#169440=CARTESIAN_POINT('Ctrl Pts',(61.2545031656196,34.3107844191081,0.));
#169441=CARTESIAN_POINT('Ctrl Pts',(61.2545031656196,34.3107844191081,12.));
#169442=CARTESIAN_POINT('Ctrl Pts',(61.2350959366987,34.3060205584093,0.));
#169443=CARTESIAN_POINT('Ctrl Pts',(61.2350959366987,34.3060205584093,12.));
#169444=CARTESIAN_POINT('Ctrl Pts',(61.2157453259107,34.3012486533474,0.));
#169445=CARTESIAN_POINT('Ctrl Pts',(61.2157453259107,34.3012486533474,12.));
#169446=CARTESIAN_POINT('Ctrl Pts',(61.1964515073823,34.296468844362,0.));
#169447=CARTESIAN_POINT('Ctrl Pts',(61.1964515073823,34.296468844362,12.));
#169448=CARTESIAN_POINT('Ctrl Pts',(61.1772146833083,34.2916812929675,0.));
#169449=CARTESIAN_POINT('Ctrl Pts',(61.1772146833083,34.2916812929675,12.));
#169450=CARTESIAN_POINT('Ctrl Pts',(61.15803506354,34.2868861666301,0.));
#169451=CARTESIAN_POINT('Ctrl Pts',(61.15803506354,34.2868861666301,12.));
#169452=CARTESIAN_POINT('Ctrl Pts',(61.1389128461815,34.2820836244425,0.));
#169453=CARTESIAN_POINT('Ctrl Pts',(61.1389128461815,34.2820836244425,12.));
#169454=CARTESIAN_POINT('Ctrl Pts',(61.119848199783,34.2772738038812,0.));
#169455=CARTESIAN_POINT('Ctrl Pts',(61.119848199783,34.2772738038812,12.));
#169456=CARTESIAN_POINT('Ctrl Pts',(61.100841240023,34.2724568037374,0.));
#169457=CARTESIAN_POINT('Ctrl Pts',(61.100841240023,34.2724568037374,12.));
#169458=CARTESIAN_POINT('Ctrl Pts',(61.0818920286644,34.2676326825846,0.));
#169459=CARTESIAN_POINT('Ctrl Pts',(61.0818920286644,34.2676326825846,12.));
#169460=CARTESIAN_POINT('Ctrl Pts',(61.0667788793594,34.2637677132139,0.));
#169461=CARTESIAN_POINT('Ctrl Pts',(61.0667788793594,34.2637677132139,12.));
#169462=CARTESIAN_POINT('Ctrl Pts',(61.0554700177206,34.2608658001761,0.));
#169463=CARTESIAN_POINT('Ctrl Pts',(61.0554700177206,34.2608658001761,12.));
#169464=CARTESIAN_POINT('Ctrl Pts',(61.0479423318803,34.2589297755482,0.));
#169465=CARTESIAN_POINT('Ctrl Pts',(61.0479423318803,34.2589297755482,12.));
#169466=CARTESIAN_POINT('Ctrl Pts',(61.0441813777723,34.2579614092497,0.));
#169467=CARTESIAN_POINT('Ctrl Pts',(61.0441813777723,34.2579614092497,12.));
#169468=CARTESIAN_POINT('',(61.0441813777723,34.2579614092497,12.));
#169469=CARTESIAN_POINT('Ctrl Pts',(61.0441813777723,34.2579614092497,12.));
#169470=CARTESIAN_POINT('Ctrl Pts',(61.0479423318803,34.2589297755482,12.));
#169471=CARTESIAN_POINT('Ctrl Pts',(61.0554700177206,34.2608658001761,12.));
#169472=CARTESIAN_POINT('Ctrl Pts',(61.0667788793594,34.2637677132139,12.));
#169473=CARTESIAN_POINT('Ctrl Pts',(61.0818920286644,34.2676326825846,12.));
#169474=CARTESIAN_POINT('Ctrl Pts',(61.100841240023,34.2724568037374,12.));
#169475=CARTESIAN_POINT('Ctrl Pts',(61.119848199783,34.2772738038812,12.));
#169476=CARTESIAN_POINT('Ctrl Pts',(61.1389128461815,34.2820836244425,12.));
#169477=CARTESIAN_POINT('Ctrl Pts',(61.15803506354,34.2868861666301,12.));
#169478=CARTESIAN_POINT('Ctrl Pts',(61.1772146833083,34.2916812929675,12.));
#169479=CARTESIAN_POINT('Ctrl Pts',(61.1964515073823,34.296468844362,12.));
#169480=CARTESIAN_POINT('Ctrl Pts',(61.2157453259107,34.3012486533474,12.));
#169481=CARTESIAN_POINT('Ctrl Pts',(61.2350959366987,34.3060205584093,12.));
#169482=CARTESIAN_POINT('Ctrl Pts',(61.2545031656196,34.3107844191081,12.));
#169483=CARTESIAN_POINT('Ctrl Pts',(61.2739668600415,34.3155401111777,12.));
#169484=CARTESIAN_POINT('Ctrl Pts',(61.2934868791875,34.3202875193629,12.));
#169485=CARTESIAN_POINT('Ctrl Pts',(61.3130630861375,34.3250265314761,12.));
#169486=CARTESIAN_POINT('Ctrl Pts',(61.3326953378817,34.3297570310126,12.));
#169487=CARTESIAN_POINT('Ctrl Pts',(61.3523834803144,34.3344788934337,12.));
#169488=CARTESIAN_POINT('Ctrl Pts',(61.3721273534222,34.339191990012,12.));
#169489=CARTESIAN_POINT('Ctrl Pts',(61.3919267945293,34.34389619024,12.));
#169490=CARTESIAN_POINT('Ctrl Pts',(61.4117816420251,34.3485913645991,12.));
#169491=CARTESIAN_POINT('Ctrl Pts',(61.4316917395959,34.3532773877112,12.));
#169492=CARTESIAN_POINT('Ctrl Pts',(61.4516569360499,34.357954138202,12.));
#169493=CARTESIAN_POINT('Ctrl Pts',(61.4716770832924,34.3626214971903,12.));
#169494=CARTESIAN_POINT('Ctrl Pts',(61.4917520349276,34.3672793472464,12.));
#169495=CARTESIAN_POINT('Ctrl Pts',(61.511881644541,34.3719275711179,12.));
#169496=CARTESIAN_POINT('Ctrl Pts',(61.5320657642601,34.3765660506659,12.));
#169497=CARTESIAN_POINT('Ctrl Pts',(61.5523042455127,34.3811946674179,12.));
#169498=CARTESIAN_POINT('Ctrl Pts',(61.5725969396817,34.3858133030511,12.));
#169499=CARTESIAN_POINT('Ctrl Pts',(61.5929436987419,34.3904218398642,12.));
#169500=CARTESIAN_POINT('Ctrl Pts',(61.6133443760168,34.3950201613446,12.));
#169501=CARTESIAN_POINT('Ctrl Pts',(61.6337988264586,34.399608152377,12.));
#169502=CARTESIAN_POINT('Ctrl Pts',(61.6543069062436,34.4041856989328,12.));
#169503=CARTESIAN_POINT('Ctrl Pts',(61.674868472521,34.4087526878815,12.));
#169504=CARTESIAN_POINT('Ctrl Pts',(61.6954833831157,34.4133090067696,12.));
#169505=CARTESIAN_POINT('Ctrl Pts',(61.7161514961892,34.4178545435753,12.));
#169506=CARTESIAN_POINT('Ctrl Pts',(61.7368726702573,34.4223891867166,12.));
#169507=CARTESIAN_POINT('Ctrl Pts',(61.7576467643419,34.4269128251569,12.));
#169508=CARTESIAN_POINT('Ctrl Pts',(61.7784736380727,34.4314253484792,12.));
#169509=CARTESIAN_POINT('Ctrl Pts',(61.7993531518052,34.4359266469757,12.));
#169510=CARTESIAN_POINT('Ctrl Pts',(61.8202851667247,34.4404166117313,12.));
#169511=CARTESIAN_POINT('Ctrl Pts',(61.8412695447951,34.4448951345753,12.));
#169512=CARTESIAN_POINT('Ctrl Pts',(61.862306148703,34.4493621080367,12.));
#169513=CARTESIAN_POINT('Ctrl Pts',(61.883394841802,34.4538174253009,12.));
#169514=CARTESIAN_POINT('Ctrl Pts',(61.9045354880424,34.4582609801625,12.));
#169515=CARTESIAN_POINT('Ctrl Pts',(61.9257279519283,34.462692666996,12.));
#169516=CARTESIAN_POINT('Ctrl Pts',(61.9469720985512,34.4671123807706,12.));
#169517=CARTESIAN_POINT('Ctrl Pts',(61.9682677936048,34.4715200170589,12.));
#169518=CARTESIAN_POINT('Ctrl Pts',(61.9896149034009,34.4759154720477,12.));
#169519=CARTESIAN_POINT('Ctrl Pts',(62.0110132948807,34.4802986425535,12.));
#169520=CARTESIAN_POINT('Ctrl Pts',(62.0324628356152,34.4846694260205,12.));
#169521=CARTESIAN_POINT('Ctrl Pts',(62.0539633937944,34.4890277205042,12.));
#169522=CARTESIAN_POINT('Ctrl Pts',(62.0755148382136,34.4933734246593,12.));
#169523=CARTESIAN_POINT('Ctrl Pts',(62.0971170382565,34.4977064377281,12.));
#169524=CARTESIAN_POINT('Ctrl Pts',(62.1187698638705,34.5020266595292,12.));
#169525=CARTESIAN_POINT('Ctrl Pts',(62.1404731855686,34.5063339904533,12.));
#169526=CARTESIAN_POINT('Ctrl Pts',(62.1622268744336,34.5106283314594,12.));
#169527=CARTESIAN_POINT('Ctrl Pts',(62.1840308021171,34.514909584073,12.));
#169528=CARTESIAN_POINT('Ctrl Pts',(62.2058848408347,34.5191776503842,12.));
#169529=CARTESIAN_POINT('Ctrl Pts',(62.2277888633576,34.5234324330491,12.));
#169530=CARTESIAN_POINT('Ctrl Pts',(62.2497427430135,34.5276738352808,12.));
#169531=CARTESIAN_POINT('Ctrl Pts',(62.2717463536827,34.5319017608433,12.));
#169532=CARTESIAN_POINT('Ctrl Pts',(62.2937995697925,34.5361161140449,12.));
#169533=CARTESIAN_POINT('Ctrl Pts',(62.3159022663058,34.5403167997337,12.));
#169534=CARTESIAN_POINT('Ctrl Pts',(62.338054318708,34.5445037232936,12.));
#169535=CARTESIAN_POINT('Ctrl Pts',(62.3602556030127,34.5486767906384,12.));
#169536=CARTESIAN_POINT('Ctrl Pts',(62.3825059957601,34.5528359082075,12.));
#169537=CARTESIAN_POINT('Ctrl Pts',(62.4048053740127,34.5569809829613,12.));
#169538=CARTESIAN_POINT('Ctrl Pts',(62.4271536153459,34.5611119223799,12.));
#169539=CARTESIAN_POINT('Ctrl Pts',(62.4495505978393,34.5652286344593,12.));
#169540=CARTESIAN_POINT('Ctrl Pts',(62.4719962000808,34.5693310277051,12.));
#169541=CARTESIAN_POINT('Ctrl Pts',(62.4944903011628,34.5734190111272,12.));
#169542=CARTESIAN_POINT('Ctrl Pts',(62.5170327806781,34.5774924942355,12.));
#169543=CARTESIAN_POINT('Ctrl Pts',(62.5396235187079,34.5815513870377,12.));
#169544=CARTESIAN_POINT('Ctrl Pts',(62.562262395816,34.5855956000363,12.));
#169545=CARTESIAN_POINT('Ctrl Pts',(62.5849492930533,34.5896250442216,12.));
#169546=CARTESIAN_POINT('Ctrl Pts',(62.6076840919536,34.5936396310679,12.));
#169547=CARTESIAN_POINT('Ctrl Pts',(62.6304666745306,34.5976392725296,12.));
#169548=CARTESIAN_POINT('Ctrl Pts',(62.6532969232657,34.6016238810399,12.));
#169549=CARTESIAN_POINT('Ctrl Pts',(62.6761747211037,34.6055933695069,12.));
#169550=CARTESIAN_POINT('Ctrl Pts',(62.6990999514563,34.6095476513077,12.));
#169551=CARTESIAN_POINT('Ctrl Pts',(62.7220724981994,34.6134866402837,12.));
#169552=CARTESIAN_POINT('Ctrl Pts',(62.7450922456676,34.6174102507375,12.));
#169553=CARTESIAN_POINT('Ctrl Pts',(62.7681590786429,34.6213183974317,12.));
#169554=CARTESIAN_POINT('Ctrl Pts',(62.7912728823518,34.6252109955853,12.));
#169555=CARTESIAN_POINT('Ctrl Pts',(62.8144335424697,34.6290879608673,12.));
#169556=CARTESIAN_POINT('Ctrl Pts',(62.8376409451175,34.6329492093935,12.));
#169557=CARTESIAN_POINT('Ctrl Pts',(62.8608949768571,34.6367946577235,12.));
#169558=CARTESIAN_POINT('Ctrl Pts',(62.8841955246794,34.6406242228592,12.));
#169559=CARTESIAN_POINT('Ctrl Pts',(62.9075424760015,34.6444378222411,12.));
#169560=CARTESIAN_POINT('Ctrl Pts',(62.9309357186717,34.6482353737424,12.));
#169561=CARTESIAN_POINT('Ctrl Pts',(62.9543751409645,34.6520167956655,12.));
#169562=CARTESIAN_POINT('Ctrl Pts',(62.9778606315783,34.6557820067393,12.));
#169563=CARTESIAN_POINT('Ctrl Pts',(63.0013920796235,34.6595309261191,12.));
#169564=CARTESIAN_POINT('Ctrl Pts',(63.0249693746208,34.6632634733824,12.));
#169565=CARTESIAN_POINT('Ctrl Pts',(63.0485924065045,34.6669795685229,12.));
#169566=CARTESIAN_POINT('Ctrl Pts',(63.0722610656194,34.670679131947,12.));
#169567=CARTESIAN_POINT('Ctrl Pts',(63.0959752427168,34.674362084472,12.));
#169568=CARTESIAN_POINT('Ctrl Pts',(63.119734828943,34.6780283473252,12.));
#169569=CARTESIAN_POINT('Ctrl Pts',(63.1435397158388,34.6816778421402,12.));
#169570=CARTESIAN_POINT('Ctrl Pts',(63.1673897953429,34.6853104909518,12.));
#169571=CARTESIAN_POINT('Ctrl Pts',(63.1912849597887,34.6889262161924,12.));
#169572=CARTESIAN_POINT('Ctrl Pts',(63.2152251019012,34.6925249406897,12.));
#169573=CARTESIAN_POINT('Ctrl Pts',(63.2392101147847,34.6961065876666,12.));
#169574=CARTESIAN_POINT('Ctrl Pts',(63.2632398919225,34.6996710807378,12.));
#169575=CARTESIAN_POINT('Ctrl Pts',(63.2873143271806,34.7032183439041,12.));
#169576=CARTESIAN_POINT('Ctrl Pts',(63.3114333148048,34.7067483015491,12.));
#169577=CARTESIAN_POINT('Ctrl Pts',(63.3355967494171,34.7102608784374,12.));
#169578=CARTESIAN_POINT('Ctrl Pts',(63.3598045260053,34.7137559997146,12.));
#169579=CARTESIAN_POINT('Ctrl Pts',(63.3840565399208,34.7172335909038,12.));
#169580=CARTESIAN_POINT('Ctrl Pts',(63.4083526868836,34.7206935779007,12.));
#169581=CARTESIAN_POINT('Ctrl Pts',(63.4326928629795,34.7241358869701,12.));
#169582=CARTESIAN_POINT('Ctrl Pts',(63.4570769646569,34.7275604447439,12.));
#169583=CARTESIAN_POINT('Ctrl Pts',(63.4815048887165,34.7309671782214,12.));
#169584=CARTESIAN_POINT('Ctrl Pts',(63.505976532309,34.7343560147667,12.));
#169585=CARTESIAN_POINT('Ctrl Pts',(63.5304917929386,34.7377268821026,12.));
#169586=CARTESIAN_POINT('Ctrl Pts',(63.5550505684626,34.7410797083081,12.));
#169587=CARTESIAN_POINT('Ctrl Pts',(63.5796527570871,34.744414421816,12.));
#169588=CARTESIAN_POINT('Ctrl Pts',(63.6042982573588,34.7477309514136,12.));
#169589=CARTESIAN_POINT('Ctrl Pts',(63.6289869681604,34.7510292262406,12.));
#169590=CARTESIAN_POINT('Ctrl Pts',(63.6537187887159,34.7543091757833,12.));
#169591=CARTESIAN_POINT('Ctrl Pts',(63.6784936185885,34.7575707298713,12.));
#169592=CARTESIAN_POINT('Ctrl Pts',(63.7033113576785,34.7608138186759,12.));
#169593=CARTESIAN_POINT('Ctrl Pts',(63.7281719062149,34.7640383727101,12.));
#169594=CARTESIAN_POINT('Ctrl Pts',(63.7530751647494,34.7672443228275,12.));
#169595=CARTESIAN_POINT('Ctrl Pts',(63.778021034163,34.7704316002171,12.));
#169596=CARTESIAN_POINT('Ctrl Pts',(63.8030094156639,34.7736001363993,12.));
#169597=CARTESIAN_POINT('Ctrl Pts',(63.8280402107856,34.7767498632243,12.));
#169598=CARTESIAN_POINT('Ctrl Pts',(63.8531133213793,34.7798807128715,12.));
#169599=CARTESIAN_POINT('Ctrl Pts',(63.8782286496062,34.7829926178496,12.));
#169600=CARTESIAN_POINT('Ctrl Pts',(63.9033860979435,34.7860855109911,12.));
#169601=CARTESIAN_POINT('Ctrl Pts',(63.9285855691845,34.7891593254488,12.));
#169602=CARTESIAN_POINT('Ctrl Pts',(63.9538269664366,34.7922139946943,12.));
#169603=CARTESIAN_POINT('Ctrl Pts',(63.9791101931162,34.7952494525178,12.));
#169604=CARTESIAN_POINT('Ctrl Pts',(64.0044351529402,34.7982656330293,12.));
#169605=CARTESIAN_POINT('Ctrl Pts',(64.0298017499294,34.8012624706527,12.));
#169606=CARTESIAN_POINT('Ctrl Pts',(64.0552098884095,34.8042399001211,12.));
#169607=CARTESIAN_POINT('Ctrl Pts',(64.0806594730085,34.8071978564748,12.));
#169608=CARTESIAN_POINT('Ctrl Pts',(64.1061504086515,34.8101362750597,12.));
#169609=CARTESIAN_POINT('Ctrl Pts',(64.1316826005506,34.8130550915287,12.));
#169610=CARTESIAN_POINT('Ctrl Pts',(64.1572559542086,34.8159542418374,12.));
#169611=CARTESIAN_POINT('Ctrl Pts',(64.1828703754236,34.8188336622419,12.));
#169612=CARTESIAN_POINT('Ctrl Pts',(64.2085257702884,34.8216932892969,12.));
#169613=CARTESIAN_POINT('Ctrl Pts',(64.234222045188,34.8245330598559,12.));
#169614=CARTESIAN_POINT('Ctrl Pts',(64.2599591067916,34.8273529110744,12.));
#169615=CARTESIAN_POINT('Ctrl Pts',(64.285736862052,34.8301527804054,12.));
#169616=CARTESIAN_POINT('Ctrl Pts',(64.3115552182062,34.8329326055919,12.));
#169617=CARTESIAN_POINT('Ctrl Pts',(64.3374140827711,34.8356923246618,12.));
#169618=CARTESIAN_POINT('Ctrl Pts',(64.3633133635382,34.8384318759248,12.));
#169619=CARTESIAN_POINT('Ctrl Pts',(64.3892529685607,34.8411511979702,12.));
#169620=CARTESIAN_POINT('Ctrl Pts',(64.4152328061515,34.8438502296664,12.));
#169621=CARTESIAN_POINT('Ctrl Pts',(64.4412527848969,34.8465289101622,12.));
#169622=CARTESIAN_POINT('Ctrl Pts',(64.4673128136625,34.8491871788896,12.));
#169623=CARTESIAN_POINT('Ctrl Pts',(64.4934128015985,34.851824975568,12.));
#169624=CARTESIAN_POINT('Ctrl Pts',(64.5195526581407,34.8544422402118,12.));
#169625=CARTESIAN_POINT('Ctrl Pts',(64.5457322930088,34.857038913134,12.));
#169626=CARTESIAN_POINT('Ctrl Pts',(64.5719516161927,34.8596149349257,12.));
#169627=CARTESIAN_POINT('Ctrl Pts',(64.5982105379383,34.8621702464401,12.));
#169628=CARTESIAN_POINT('Ctrl Pts',(64.6245089687277,34.8647047887774,12.));
#169629=CARTESIAN_POINT('Ctrl Pts',(64.6508468192599,34.867218503272,12.));
#169630=CARTESIAN_POINT('Ctrl Pts',(64.6772240004228,34.869711331479,12.));
#169631=CARTESIAN_POINT('Ctrl Pts',(64.7036404233306,34.8721832151975,12.));
#169632=CARTESIAN_POINT('Ctrl Pts',(64.7300959993653,34.8746340964972,12.));
#169633=CARTESIAN_POINT('Ctrl Pts',(64.7565906402151,34.8770639177493,12.));
#169634=CARTESIAN_POINT('Ctrl Pts',(64.7831242579028,34.8794726216513,12.));
#169635=CARTESIAN_POINT('Ctrl Pts',(64.8096967648307,34.881860151273,12.));
#169636=CARTESIAN_POINT('Ctrl Pts',(64.8363080737377,34.8842264500188,12.));
#169637=CARTESIAN_POINT('Ctrl Pts',(64.8629580976063,34.8865714615436,12.));
#169638=CARTESIAN_POINT('Ctrl Pts',(64.8896467495757,34.888895129681,12.));
#169639=CARTESIAN_POINT('Ctrl Pts',(64.9163739428605,34.8911973983785,12.));
#169640=CARTESIAN_POINT('Ctrl Pts',(64.9431395906337,34.8934782116095,12.));
#169641=CARTESIAN_POINT('Ctrl Pts',(64.9699436060169,34.8957375133697,12.));
#169642=CARTESIAN_POINT('Ctrl Pts',(64.9967859023212,34.8979752478616,12.));
#169643=CARTESIAN_POINT('Ctrl Pts',(65.0236663932328,34.9001913596416,12.));
#169644=CARTESIAN_POINT('Ctrl Pts',(65.0505849930171,34.9023857937865,12.));
#169645=CARTESIAN_POINT('Ctrl Pts',(65.0775416167085,34.9045584960509,12.));
#169646=CARTESIAN_POINT('Ctrl Pts',(65.1045361803121,34.9067094130399,12.));
#169647=CARTESIAN_POINT('Ctrl Pts',(65.1315686003516,34.9088384918336,12.));
#169648=CARTESIAN_POINT('Ctrl Pts',(65.1586387934241,34.9109456796213,12.));
#169649=CARTESIAN_POINT('Ctrl Pts',(65.1857466757092,34.9130309233022,12.));
#169650=CARTESIAN_POINT('Ctrl Pts',(65.2128921625823,34.9150941691747,12.));
#169651=CARTESIAN_POINT('Ctrl Pts',(65.2400751679549,34.9171353624113,12.));
#169652=CARTESIAN_POINT('Ctrl Pts',(65.2672956048069,34.9191544474872,12.));
#169653=CARTESIAN_POINT('Ctrl Pts',(65.2945533863761,34.9211513691355,12.));
#169654=CARTESIAN_POINT('Ctrl Pts',(65.321848427191,34.9231260731831,12.));
#169655=CARTESIAN_POINT('Ctrl Pts',(65.3491806440537,34.9250785073477,12.));
#169656=CARTESIAN_POINT('Ctrl Pts',(65.3765499573077,34.9270086222731,12.));
#169657=CARTESIAN_POINT('Ctrl Pts',(65.4039562911352,34.9289163717747,12.));
#169658=CARTESIAN_POINT('Ctrl Pts',(65.4274804996589,34.9305324724445,12.));
#169659=CARTESIAN_POINT('Ctrl Pts',(65.4455359575246,34.931759381316,12.));
#169660=CARTESIAN_POINT('Ctrl Pts',(65.4581063193885,34.9326070346645,12.));
#169661=CARTESIAN_POINT('Ctrl Pts',(65.4651808010812,34.9330820191535,12.));
#169662=CARTESIAN_POINT('Ctrl Pts',(65.4667541478387,34.933187552314,12.));
#169663=CARTESIAN_POINT('',(61.0441813777723,34.2579614092497,0.));
#169664=CARTESIAN_POINT('',(61.0441813777723,34.2579614092497,0.));
#169665=CARTESIAN_POINT('Ctrl Pts',(65.4667541478388,34.933187552314,0.));
#169666=CARTESIAN_POINT('Ctrl Pts',(65.4651808010814,34.9330820191535,0.));
#169667=CARTESIAN_POINT('Ctrl Pts',(65.4581063193886,34.9326070346645,0.));
#169668=CARTESIAN_POINT('Ctrl Pts',(65.4455359575246,34.931759381316,0.));
#169669=CARTESIAN_POINT('Ctrl Pts',(65.427480499659,34.9305324724445,0.));
#169670=CARTESIAN_POINT('Ctrl Pts',(65.4039562911352,34.9289163717747,0.));
#169671=CARTESIAN_POINT('Ctrl Pts',(65.3765499573077,34.9270086222731,0.));
#169672=CARTESIAN_POINT('Ctrl Pts',(65.3491806440537,34.9250785073477,0.));
#169673=CARTESIAN_POINT('Ctrl Pts',(65.321848427191,34.9231260731831,0.));
#169674=CARTESIAN_POINT('Ctrl Pts',(65.2945533863761,34.9211513691355,0.));
#169675=CARTESIAN_POINT('Ctrl Pts',(65.2672956048069,34.9191544474872,0.));
#169676=CARTESIAN_POINT('Ctrl Pts',(65.2400751679549,34.9171353624113,0.));
#169677=CARTESIAN_POINT('Ctrl Pts',(65.2128921625823,34.9150941691747,0.));
#169678=CARTESIAN_POINT('Ctrl Pts',(65.1857466757092,34.9130309233022,0.));
#169679=CARTESIAN_POINT('Ctrl Pts',(65.1586387934241,34.9109456796213,0.));
#169680=CARTESIAN_POINT('Ctrl Pts',(65.1315686003516,34.9088384918336,0.));
#169681=CARTESIAN_POINT('Ctrl Pts',(65.1045361803121,34.9067094130399,0.));
#169682=CARTESIAN_POINT('Ctrl Pts',(65.0775416167085,34.9045584960509,0.));
#169683=CARTESIAN_POINT('Ctrl Pts',(65.0505849930171,34.9023857937865,0.));
#169684=CARTESIAN_POINT('Ctrl Pts',(65.0236663932328,34.9001913596416,0.));
#169685=CARTESIAN_POINT('Ctrl Pts',(64.9967859023212,34.8979752478616,0.));
#169686=CARTESIAN_POINT('Ctrl Pts',(64.9699436060169,34.8957375133697,0.));
#169687=CARTESIAN_POINT('Ctrl Pts',(64.9431395906337,34.8934782116095,0.));
#169688=CARTESIAN_POINT('Ctrl Pts',(64.9163739428605,34.8911973983785,0.));
#169689=CARTESIAN_POINT('Ctrl Pts',(64.8896467495757,34.888895129681,0.));
#169690=CARTESIAN_POINT('Ctrl Pts',(64.8629580976063,34.8865714615436,0.));
#169691=CARTESIAN_POINT('Ctrl Pts',(64.8363080737377,34.8842264500188,0.));
#169692=CARTESIAN_POINT('Ctrl Pts',(64.8096967648307,34.881860151273,0.));
#169693=CARTESIAN_POINT('Ctrl Pts',(64.7831242579028,34.8794726216513,0.));
#169694=CARTESIAN_POINT('Ctrl Pts',(64.7565906402151,34.8770639177493,0.));
#169695=CARTESIAN_POINT('Ctrl Pts',(64.7300959993653,34.8746340964972,0.));
#169696=CARTESIAN_POINT('Ctrl Pts',(64.7036404233306,34.8721832151975,0.));
#169697=CARTESIAN_POINT('Ctrl Pts',(64.6772240004228,34.869711331479,0.));
#169698=CARTESIAN_POINT('Ctrl Pts',(64.6508468192599,34.867218503272,0.));
#169699=CARTESIAN_POINT('Ctrl Pts',(64.6245089687277,34.8647047887774,0.));
#169700=CARTESIAN_POINT('Ctrl Pts',(64.5982105379383,34.8621702464401,0.));
#169701=CARTESIAN_POINT('Ctrl Pts',(64.5719516161927,34.8596149349257,0.));
#169702=CARTESIAN_POINT('Ctrl Pts',(64.5457322930088,34.857038913134,0.));
#169703=CARTESIAN_POINT('Ctrl Pts',(64.5195526581407,34.8544422402118,0.));
#169704=CARTESIAN_POINT('Ctrl Pts',(64.4934128015985,34.851824975568,0.));
#169705=CARTESIAN_POINT('Ctrl Pts',(64.4673128136625,34.8491871788896,0.));
#169706=CARTESIAN_POINT('Ctrl Pts',(64.4412527848969,34.8465289101622,0.));
#169707=CARTESIAN_POINT('Ctrl Pts',(64.4152328061515,34.8438502296664,0.));
#169708=CARTESIAN_POINT('Ctrl Pts',(64.3892529685607,34.8411511979702,0.));
#169709=CARTESIAN_POINT('Ctrl Pts',(64.3633133635382,34.8384318759248,0.));
#169710=CARTESIAN_POINT('Ctrl Pts',(64.3374140827711,34.8356923246618,0.));
#169711=CARTESIAN_POINT('Ctrl Pts',(64.3115552182062,34.8329326055919,0.));
#169712=CARTESIAN_POINT('Ctrl Pts',(64.285736862052,34.8301527804054,0.));
#169713=CARTESIAN_POINT('Ctrl Pts',(64.2599591067916,34.8273529110744,0.));
#169714=CARTESIAN_POINT('Ctrl Pts',(64.234222045188,34.8245330598559,0.));
#169715=CARTESIAN_POINT('Ctrl Pts',(64.2085257702884,34.8216932892969,0.));
#169716=CARTESIAN_POINT('Ctrl Pts',(64.1828703754236,34.8188336622419,0.));
#169717=CARTESIAN_POINT('Ctrl Pts',(64.1572559542086,34.8159542418374,0.));
#169718=CARTESIAN_POINT('Ctrl Pts',(64.1316826005506,34.8130550915287,0.));
#169719=CARTESIAN_POINT('Ctrl Pts',(64.1061504086515,34.8101362750597,0.));
#169720=CARTESIAN_POINT('Ctrl Pts',(64.0806594730085,34.8071978564748,0.));
#169721=CARTESIAN_POINT('Ctrl Pts',(64.0552098884095,34.8042399001211,0.));
#169722=CARTESIAN_POINT('Ctrl Pts',(64.0298017499294,34.8012624706527,0.));
#169723=CARTESIAN_POINT('Ctrl Pts',(64.0044351529402,34.7982656330293,0.));
#169724=CARTESIAN_POINT('Ctrl Pts',(63.9791101931162,34.7952494525178,0.));
#169725=CARTESIAN_POINT('Ctrl Pts',(63.9538269664366,34.7922139946943,0.));
#169726=CARTESIAN_POINT('Ctrl Pts',(63.9285855691845,34.7891593254488,0.));
#169727=CARTESIAN_POINT('Ctrl Pts',(63.9033860979435,34.7860855109911,0.));
#169728=CARTESIAN_POINT('Ctrl Pts',(63.8782286496062,34.7829926178496,0.));
#169729=CARTESIAN_POINT('Ctrl Pts',(63.8531133213793,34.7798807128715,0.));
#169730=CARTESIAN_POINT('Ctrl Pts',(63.8280402107856,34.7767498632243,0.));
#169731=CARTESIAN_POINT('Ctrl Pts',(63.8030094156639,34.7736001363993,0.));
#169732=CARTESIAN_POINT('Ctrl Pts',(63.778021034163,34.7704316002171,0.));
#169733=CARTESIAN_POINT('Ctrl Pts',(63.7530751647494,34.7672443228275,0.));
#169734=CARTESIAN_POINT('Ctrl Pts',(63.7281719062149,34.7640383727101,0.));
#169735=CARTESIAN_POINT('Ctrl Pts',(63.7033113576785,34.7608138186759,0.));
#169736=CARTESIAN_POINT('Ctrl Pts',(63.6784936185885,34.7575707298713,0.));
#169737=CARTESIAN_POINT('Ctrl Pts',(63.6537187887159,34.7543091757833,0.));
#169738=CARTESIAN_POINT('Ctrl Pts',(63.6289869681604,34.7510292262406,0.));
#169739=CARTESIAN_POINT('Ctrl Pts',(63.6042982573588,34.7477309514136,0.));
#169740=CARTESIAN_POINT('Ctrl Pts',(63.5796527570871,34.744414421816,0.));
#169741=CARTESIAN_POINT('Ctrl Pts',(63.5550505684626,34.7410797083081,0.));
#169742=CARTESIAN_POINT('Ctrl Pts',(63.5304917929386,34.7377268821026,0.));
#169743=CARTESIAN_POINT('Ctrl Pts',(63.505976532309,34.7343560147667,0.));
#169744=CARTESIAN_POINT('Ctrl Pts',(63.4815048887165,34.7309671782214,0.));
#169745=CARTESIAN_POINT('Ctrl Pts',(63.4570769646569,34.7275604447439,0.));
#169746=CARTESIAN_POINT('Ctrl Pts',(63.4326928629795,34.7241358869701,0.));
#169747=CARTESIAN_POINT('Ctrl Pts',(63.4083526868836,34.7206935779007,0.));
#169748=CARTESIAN_POINT('Ctrl Pts',(63.3840565399208,34.7172335909038,0.));
#169749=CARTESIAN_POINT('Ctrl Pts',(63.3598045260053,34.7137559997146,0.));
#169750=CARTESIAN_POINT('Ctrl Pts',(63.3355967494171,34.7102608784374,0.));
#169751=CARTESIAN_POINT('Ctrl Pts',(63.3114333148048,34.7067483015491,0.));
#169752=CARTESIAN_POINT('Ctrl Pts',(63.2873143271806,34.7032183439041,0.));
#169753=CARTESIAN_POINT('Ctrl Pts',(63.2632398919225,34.6996710807378,0.));
#169754=CARTESIAN_POINT('Ctrl Pts',(63.2392101147847,34.6961065876666,0.));
#169755=CARTESIAN_POINT('Ctrl Pts',(63.2152251019012,34.6925249406897,0.));
#169756=CARTESIAN_POINT('Ctrl Pts',(63.1912849597887,34.6889262161924,0.));
#169757=CARTESIAN_POINT('Ctrl Pts',(63.1673897953429,34.6853104909518,0.));
#169758=CARTESIAN_POINT('Ctrl Pts',(63.1435397158388,34.6816778421402,0.));
#169759=CARTESIAN_POINT('Ctrl Pts',(63.119734828943,34.6780283473252,0.));
#169760=CARTESIAN_POINT('Ctrl Pts',(63.0959752427168,34.674362084472,0.));
#169761=CARTESIAN_POINT('Ctrl Pts',(63.0722610656194,34.670679131947,0.));
#169762=CARTESIAN_POINT('Ctrl Pts',(63.0485924065045,34.6669795685229,0.));
#169763=CARTESIAN_POINT('Ctrl Pts',(63.0249693746208,34.6632634733824,0.));
#169764=CARTESIAN_POINT('Ctrl Pts',(63.0013920796235,34.6595309261191,0.));
#169765=CARTESIAN_POINT('Ctrl Pts',(62.9778606315783,34.6557820067393,0.));
#169766=CARTESIAN_POINT('Ctrl Pts',(62.9543751409645,34.6520167956655,0.));
#169767=CARTESIAN_POINT('Ctrl Pts',(62.9309357186717,34.6482353737424,0.));
#169768=CARTESIAN_POINT('Ctrl Pts',(62.9075424760015,34.6444378222411,0.));
#169769=CARTESIAN_POINT('Ctrl Pts',(62.8841955246794,34.6406242228592,0.));
#169770=CARTESIAN_POINT('Ctrl Pts',(62.8608949768571,34.6367946577235,0.));
#169771=CARTESIAN_POINT('Ctrl Pts',(62.8376409451175,34.6329492093935,0.));
#169772=CARTESIAN_POINT('Ctrl Pts',(62.8144335424697,34.6290879608673,0.));
#169773=CARTESIAN_POINT('Ctrl Pts',(62.7912728823518,34.6252109955853,0.));
#169774=CARTESIAN_POINT('Ctrl Pts',(62.7681590786429,34.6213183974317,0.));
#169775=CARTESIAN_POINT('Ctrl Pts',(62.7450922456676,34.6174102507375,0.));
#169776=CARTESIAN_POINT('Ctrl Pts',(62.7220724981994,34.6134866402837,0.));
#169777=CARTESIAN_POINT('Ctrl Pts',(62.6990999514563,34.6095476513077,0.));
#169778=CARTESIAN_POINT('Ctrl Pts',(62.6761747211037,34.6055933695069,0.));
#169779=CARTESIAN_POINT('Ctrl Pts',(62.6532969232657,34.6016238810399,0.));
#169780=CARTESIAN_POINT('Ctrl Pts',(62.6304666745306,34.5976392725296,0.));
#169781=CARTESIAN_POINT('Ctrl Pts',(62.6076840919536,34.5936396310679,0.));
#169782=CARTESIAN_POINT('Ctrl Pts',(62.5849492930533,34.5896250442216,0.));
#169783=CARTESIAN_POINT('Ctrl Pts',(62.562262395816,34.5855956000363,0.));
#169784=CARTESIAN_POINT('Ctrl Pts',(62.5396235187079,34.5815513870377,0.));
#169785=CARTESIAN_POINT('Ctrl Pts',(62.5170327806781,34.5774924942355,0.));
#169786=CARTESIAN_POINT('Ctrl Pts',(62.4944903011628,34.5734190111272,0.));
#169787=CARTESIAN_POINT('Ctrl Pts',(62.4719962000808,34.5693310277051,0.));
#169788=CARTESIAN_POINT('Ctrl Pts',(62.4495505978393,34.5652286344593,0.));
#169789=CARTESIAN_POINT('Ctrl Pts',(62.4271536153459,34.5611119223799,0.));
#169790=CARTESIAN_POINT('Ctrl Pts',(62.4048053740127,34.5569809829613,0.));
#169791=CARTESIAN_POINT('Ctrl Pts',(62.3825059957601,34.5528359082075,0.));
#169792=CARTESIAN_POINT('Ctrl Pts',(62.3602556030127,34.5486767906384,0.));
#169793=CARTESIAN_POINT('Ctrl Pts',(62.338054318708,34.5445037232936,0.));
#169794=CARTESIAN_POINT('Ctrl Pts',(62.3159022663058,34.5403167997337,0.));
#169795=CARTESIAN_POINT('Ctrl Pts',(62.2937995697925,34.5361161140449,0.));
#169796=CARTESIAN_POINT('Ctrl Pts',(62.2717463536827,34.5319017608433,0.));
#169797=CARTESIAN_POINT('Ctrl Pts',(62.2497427430135,34.5276738352808,0.));
#169798=CARTESIAN_POINT('Ctrl Pts',(62.2277888633576,34.5234324330491,0.));
#169799=CARTESIAN_POINT('Ctrl Pts',(62.2058848408347,34.5191776503842,0.));
#169800=CARTESIAN_POINT('Ctrl Pts',(62.1840308021171,34.514909584073,0.));
#169801=CARTESIAN_POINT('Ctrl Pts',(62.1622268744336,34.5106283314594,0.));
#169802=CARTESIAN_POINT('Ctrl Pts',(62.1404731855686,34.5063339904533,0.));
#169803=CARTESIAN_POINT('Ctrl Pts',(62.1187698638705,34.5020266595292,0.));
#169804=CARTESIAN_POINT('Ctrl Pts',(62.0971170382565,34.4977064377281,0.));
#169805=CARTESIAN_POINT('Ctrl Pts',(62.0755148382136,34.4933734246593,0.));
#169806=CARTESIAN_POINT('Ctrl Pts',(62.0539633937944,34.4890277205042,0.));
#169807=CARTESIAN_POINT('Ctrl Pts',(62.0324628356152,34.4846694260205,0.));
#169808=CARTESIAN_POINT('Ctrl Pts',(62.0110132948807,34.4802986425535,0.));
#169809=CARTESIAN_POINT('Ctrl Pts',(61.9896149034009,34.4759154720477,0.));
#169810=CARTESIAN_POINT('Ctrl Pts',(61.9682677936048,34.4715200170589,0.));
#169811=CARTESIAN_POINT('Ctrl Pts',(61.9469720985512,34.4671123807706,0.));
#169812=CARTESIAN_POINT('Ctrl Pts',(61.9257279519283,34.462692666996,0.));
#169813=CARTESIAN_POINT('Ctrl Pts',(61.9045354880424,34.4582609801625,0.));
#169814=CARTESIAN_POINT('Ctrl Pts',(61.883394841802,34.4538174253009,0.));
#169815=CARTESIAN_POINT('Ctrl Pts',(61.862306148703,34.4493621080367,0.));
#169816=CARTESIAN_POINT('Ctrl Pts',(61.8412695447951,34.4448951345753,0.));
#169817=CARTESIAN_POINT('Ctrl Pts',(61.8202851667247,34.4404166117313,0.));
#169818=CARTESIAN_POINT('Ctrl Pts',(61.7993531518052,34.4359266469757,0.));
#169819=CARTESIAN_POINT('Ctrl Pts',(61.7784736380727,34.4314253484792,0.));
#169820=CARTESIAN_POINT('Ctrl Pts',(61.7576467643419,34.4269128251569,0.));
#169821=CARTESIAN_POINT('Ctrl Pts',(61.7368726702573,34.4223891867166,0.));
#169822=CARTESIAN_POINT('Ctrl Pts',(61.7161514961892,34.4178545435753,0.));
#169823=CARTESIAN_POINT('Ctrl Pts',(61.6954833831157,34.4133090067696,0.));
#169824=CARTESIAN_POINT('Ctrl Pts',(61.674868472521,34.4087526878815,0.));
#169825=CARTESIAN_POINT('Ctrl Pts',(61.6543069062436,34.4041856989328,0.));
#169826=CARTESIAN_POINT('Ctrl Pts',(61.6337988264586,34.399608152377,0.));
#169827=CARTESIAN_POINT('Ctrl Pts',(61.6133443760168,34.3950201613446,0.));
#169828=CARTESIAN_POINT('Ctrl Pts',(61.5929436987419,34.3904218398642,0.));
#169829=CARTESIAN_POINT('Ctrl Pts',(61.5725969396817,34.3858133030511,0.));
#169830=CARTESIAN_POINT('Ctrl Pts',(61.5523042455127,34.3811946674179,0.));
#169831=CARTESIAN_POINT('Ctrl Pts',(61.5320657642601,34.3765660506659,0.));
#169832=CARTESIAN_POINT('Ctrl Pts',(61.511881644541,34.3719275711179,0.));
#169833=CARTESIAN_POINT('Ctrl Pts',(61.4917520349276,34.3672793472464,0.));
#169834=CARTESIAN_POINT('Ctrl Pts',(61.4716770832924,34.3626214971903,0.));
#169835=CARTESIAN_POINT('Ctrl Pts',(61.4516569360499,34.357954138202,0.));
#169836=CARTESIAN_POINT('Ctrl Pts',(61.4316917395959,34.3532773877112,0.));
#169837=CARTESIAN_POINT('Ctrl Pts',(61.4117816420251,34.3485913645991,0.));
#169838=CARTESIAN_POINT('Ctrl Pts',(61.3919267945293,34.34389619024,0.));
#169839=CARTESIAN_POINT('Ctrl Pts',(61.3721273534222,34.339191990012,0.));
#169840=CARTESIAN_POINT('Ctrl Pts',(61.3523834803144,34.3344788934337,0.));
#169841=CARTESIAN_POINT('Ctrl Pts',(61.3326953378817,34.3297570310126,0.));
#169842=CARTESIAN_POINT('Ctrl Pts',(61.3130630861375,34.3250265314761,0.));
#169843=CARTESIAN_POINT('Ctrl Pts',(61.2934868791875,34.3202875193629,0.));
#169844=CARTESIAN_POINT('Ctrl Pts',(61.2739668600415,34.3155401111777,0.));
#169845=CARTESIAN_POINT('Ctrl Pts',(61.2545031656196,34.3107844191081,0.));
#169846=CARTESIAN_POINT('Ctrl Pts',(61.2350959366987,34.3060205584093,0.));
#169847=CARTESIAN_POINT('Ctrl Pts',(61.2157453259107,34.3012486533474,0.));
#169848=CARTESIAN_POINT('Ctrl Pts',(61.1964515073823,34.296468844362,0.));
#169849=CARTESIAN_POINT('Ctrl Pts',(61.1772146833083,34.2916812929675,0.));
#169850=CARTESIAN_POINT('Ctrl Pts',(61.15803506354,34.2868861666301,0.));
#169851=CARTESIAN_POINT('Ctrl Pts',(61.1389128461815,34.2820836244425,0.));
#169852=CARTESIAN_POINT('Ctrl Pts',(61.119848199783,34.2772738038812,0.));
#169853=CARTESIAN_POINT('Ctrl Pts',(61.100841240023,34.2724568037374,0.));
#169854=CARTESIAN_POINT('Ctrl Pts',(61.0818920286644,34.2676326825846,0.));
#169855=CARTESIAN_POINT('Ctrl Pts',(61.0667788793594,34.2637677132139,0.));
#169856=CARTESIAN_POINT('Ctrl Pts',(61.0554700177206,34.2608658001761,0.));
#169857=CARTESIAN_POINT('Ctrl Pts',(61.0479423318803,34.2589297755482,0.));
#169858=CARTESIAN_POINT('Ctrl Pts',(61.0441813777723,34.2579614092497,0.));
#169859=CARTESIAN_POINT('Ctrl Pts',(68.5875145916629,29.0861280018229,0.));
#169860=CARTESIAN_POINT('Ctrl Pts',(68.5875145916629,29.0861280018229,12.));
#169861=CARTESIAN_POINT('Ctrl Pts',(68.5819214834737,29.0863005247839,0.));
#169862=CARTESIAN_POINT('Ctrl Pts',(68.5819214834737,29.0863005247839,12.));
#169863=CARTESIAN_POINT('Ctrl Pts',(68.5707386600636,29.0866429722093,0.));
#169864=CARTESIAN_POINT('Ctrl Pts',(68.5707386600636,29.0866429722093,12.));
#169865=CARTESIAN_POINT('Ctrl Pts',(68.5539746038542,29.0871488478589,0.));
#169866=CARTESIAN_POINT('Ctrl Pts',(68.5539746038542,29.0871488478589,12.));
#169867=CARTESIAN_POINT('Ctrl Pts',(68.5316428875424,29.0878077571086,0.));
#169868=CARTESIAN_POINT('Ctrl Pts',(68.5316428875424,29.0878077571086,12.));
#169869=CARTESIAN_POINT('Ctrl Pts',(68.5037621824171,29.0886054060563,0.));
#169870=CARTESIAN_POINT('Ctrl Pts',(68.5037621824171,29.0886054060563,12.));
#169871=CARTESIAN_POINT('Ctrl Pts',(68.4759154367939,29.0893770688944,0.));
#169872=CARTESIAN_POINT('Ctrl Pts',(68.4759154367939,29.0893770688944,12.));
#169873=CARTESIAN_POINT('Ctrl Pts',(68.4481026830931,29.0901227535307,0.));
#169874=CARTESIAN_POINT('Ctrl Pts',(68.4481026830931,29.0901227535307,12.));
#169875=CARTESIAN_POINT('Ctrl Pts',(68.4203239694612,29.090842477089,0.));
#169876=CARTESIAN_POINT('Ctrl Pts',(68.4203239694612,29.090842477089,12.));
#169877=CARTESIAN_POINT('Ctrl Pts',(68.3925793637995,29.0915362699455,0.));
#169878=CARTESIAN_POINT('Ctrl Pts',(68.3925793637995,29.0915362699455,12.));
#169879=CARTESIAN_POINT('Ctrl Pts',(68.364868951893,29.0922041749294,0.));
#169880=CARTESIAN_POINT('Ctrl Pts',(68.364868951893,29.0922041749294,12.));
#169881=CARTESIAN_POINT('Ctrl Pts',(68.3371928310161,29.0928462428145,0.));
#169882=CARTESIAN_POINT('Ctrl Pts',(68.3371928310161,29.0928462428145,12.));
#169883=CARTESIAN_POINT('Ctrl Pts',(68.3095511047769,29.0934625288409,0.));
#169884=CARTESIAN_POINT('Ctrl Pts',(68.3095511047769,29.0934625288409,12.));
#169885=CARTESIAN_POINT('Ctrl Pts',(68.2819438775953,29.0940530889149,0.));
#169886=CARTESIAN_POINT('Ctrl Pts',(68.2819438775953,29.0940530889149,12.));
#169887=CARTESIAN_POINT('Ctrl Pts',(68.2543712489906,29.0946179757167,0.));
#169888=CARTESIAN_POINT('Ctrl Pts',(68.2543712489906,29.0946179757167,12.));
#169889=CARTESIAN_POINT('Ctrl Pts',(68.2268333089617,29.0951572355397,0.));
#169890=CARTESIAN_POINT('Ctrl Pts',(68.2268333089617,29.0951572355397,12.));
#169891=CARTESIAN_POINT('Ctrl Pts',(68.1993301412061,29.0956709104627,0.));
#169892=CARTESIAN_POINT('Ctrl Pts',(68.1993301412061,29.0956709104627,12.));
#169893=CARTESIAN_POINT('Ctrl Pts',(68.1718618254281,29.0961590399046,0.));
#169894=CARTESIAN_POINT('Ctrl Pts',(68.1718618254281,29.0961590399046,12.));
#169895=CARTESIAN_POINT('Ctrl Pts',(68.1444284400742,29.0966216624743,0.));
#169896=CARTESIAN_POINT('Ctrl Pts',(68.1444284400742,29.0966216624743,12.));
#169897=CARTESIAN_POINT('Ctrl Pts',(68.1170300646987,29.0970588175728,0.));
#169898=CARTESIAN_POINT('Ctrl Pts',(68.1170300646987,29.0970588175728,12.));
#169899=CARTESIAN_POINT('Ctrl Pts',(68.0896667829567,29.0974705474259,0.));
#169900=CARTESIAN_POINT('Ctrl Pts',(68.0896667829567,29.0974705474259,12.));
#169901=CARTESIAN_POINT('Ctrl Pts',(68.0623386822863,29.0978568968657,0.));
#169902=CARTESIAN_POINT('Ctrl Pts',(68.0623386822863,29.0978568968657,12.));
#169903=CARTESIAN_POINT('Ctrl Pts',(68.0350458525551,29.0982179124097,0.));
#169904=CARTESIAN_POINT('Ctrl Pts',(68.0350458525551,29.0982179124097,12.));
#169905=CARTESIAN_POINT('Ctrl Pts',(68.0077883850121,29.0985536415531,0.));
#169906=CARTESIAN_POINT('Ctrl Pts',(68.0077883850121,29.0985536415531,12.));
#169907=CARTESIAN_POINT('Ctrl Pts',(67.9805663711855,29.0988641320247,0.));
#169908=CARTESIAN_POINT('Ctrl Pts',(67.9805663711855,29.0988641320247,12.));
#169909=CARTESIAN_POINT('Ctrl Pts',(67.9533799016148,29.0991494309404,0.));
#169910=CARTESIAN_POINT('Ctrl Pts',(67.9533799016148,29.0991494309404,12.));
#169911=CARTESIAN_POINT('Ctrl Pts',(67.9262290652829,29.099409584422,0.));
#169912=CARTESIAN_POINT('Ctrl Pts',(67.9262290652829,29.099409584422,12.));
#169913=CARTESIAN_POINT('Ctrl Pts',(67.8991139503193,29.0996446380626,0.));
#169914=CARTESIAN_POINT('Ctrl Pts',(67.8991139503193,29.0996446380626,12.));
#169915=CARTESIAN_POINT('Ctrl Pts',(67.8720346444124,29.0998546372032,0.));
#169916=CARTESIAN_POINT('Ctrl Pts',(67.8720346444124,29.0998546372032,12.));
#169917=CARTESIAN_POINT('Ctrl Pts',(67.8449912353329,29.1000396272867,0.));
#169918=CARTESIAN_POINT('Ctrl Pts',(67.8449912353329,29.1000396272867,12.));
#169919=CARTESIAN_POINT('Ctrl Pts',(67.8179838114099,29.1001996541842,0.));
#169920=CARTESIAN_POINT('Ctrl Pts',(67.8179838114099,29.1001996541842,12.));
#169921=CARTESIAN_POINT('Ctrl Pts',(67.7910124620135,29.1003347645294,0.));
#169922=CARTESIAN_POINT('Ctrl Pts',(67.7910124620135,29.1003347645294,12.));
#169923=CARTESIAN_POINT('Ctrl Pts',(67.7640772773387,29.1004450055643,0.));
#169924=CARTESIAN_POINT('Ctrl Pts',(67.7640772773387,29.1004450055643,12.));
#169925=CARTESIAN_POINT('Ctrl Pts',(67.7371783482035,29.1005304249987,0.));
#169926=CARTESIAN_POINT('Ctrl Pts',(67.7371783482035,29.1005304249987,12.));
#169927=CARTESIAN_POINT('Ctrl Pts',(67.7103157658296,29.1005910708624,0.));
#169928=CARTESIAN_POINT('Ctrl Pts',(67.7103157658296,29.1005910708624,12.));
#169929=CARTESIAN_POINT('Ctrl Pts',(67.6834896216461,29.1006269913747,0.));
#169930=CARTESIAN_POINT('Ctrl Pts',(67.6834896216461,29.1006269913747,12.));
#169931=CARTESIAN_POINT('Ctrl Pts',(67.6567000070326,29.1006382347814,0.));
#169932=CARTESIAN_POINT('Ctrl Pts',(67.6567000070326,29.1006382347814,12.));
#169933=CARTESIAN_POINT('Ctrl Pts',(67.6299470133295,29.100624849358,0.));
#169934=CARTESIAN_POINT('Ctrl Pts',(67.6299470133295,29.100624849358,12.));
#169935=CARTESIAN_POINT('Ctrl Pts',(67.6032307319623,29.1005868834866,0.));
#169936=CARTESIAN_POINT('Ctrl Pts',(67.6032307319623,29.1005868834866,12.));
#169937=CARTESIAN_POINT('Ctrl Pts',(67.5765512545281,29.1005243857139,0.));
#169938=CARTESIAN_POINT('Ctrl Pts',(67.5765512545281,29.1005243857139,12.));
#169939=CARTESIAN_POINT('Ctrl Pts',(67.5499086728888,29.1004374048148,0.));
#169940=CARTESIAN_POINT('Ctrl Pts',(67.5499086728888,29.1004374048148,12.));
#169941=CARTESIAN_POINT('Ctrl Pts',(67.5233030792704,29.1003259898682,0.));
#169942=CARTESIAN_POINT('Ctrl Pts',(67.5233030792704,29.1003259898682,12.));
#169943=CARTESIAN_POINT('Ctrl Pts',(67.4967345663096,29.1001901902909,0.));
#169944=CARTESIAN_POINT('Ctrl Pts',(67.4967345663096,29.1001901902909,12.));
#169945=CARTESIAN_POINT('Ctrl Pts',(67.4702032270048,29.1000300557955,0.));
#169946=CARTESIAN_POINT('Ctrl Pts',(67.4702032270048,29.1000300557955,12.));
#169947=CARTESIAN_POINT('Ctrl Pts',(67.4437091546859,29.0998456363683,0.));
#169948=CARTESIAN_POINT('Ctrl Pts',(67.4437091546859,29.0998456363683,12.));
#169949=CARTESIAN_POINT('Ctrl Pts',(67.4172524429727,29.0996369822418,0.));
#169950=CARTESIAN_POINT('Ctrl Pts',(67.4172524429727,29.0996369822418,12.));
#169951=CARTESIAN_POINT('Ctrl Pts',(67.3908331857323,29.0994041438719,0.));
#169952=CARTESIAN_POINT('Ctrl Pts',(67.3908331857323,29.0994041438719,12.));
#169953=CARTESIAN_POINT('Ctrl Pts',(67.3644514770387,29.0991471719176,0.));
#169954=CARTESIAN_POINT('Ctrl Pts',(67.3644514770387,29.0991471719176,12.));
#169955=CARTESIAN_POINT('Ctrl Pts',(67.3381074112027,29.0988661172531,0.));
#169956=CARTESIAN_POINT('Ctrl Pts',(67.3381074112027,29.0988661172531,12.));
#169957=CARTESIAN_POINT('Ctrl Pts',(67.311801082792,29.0985610309771,0.));
#169958=CARTESIAN_POINT('Ctrl Pts',(67.311801082792,29.0985610309771,12.));
#169959=CARTESIAN_POINT('Ctrl Pts',(67.2855325866517,29.0982319644277,0.));
#169960=CARTESIAN_POINT('Ctrl Pts',(67.2855325866517,29.0982319644277,12.));
#169961=CARTESIAN_POINT('Ctrl Pts',(67.2593020179209,29.0978789691962,0.));
#169962=CARTESIAN_POINT('Ctrl Pts',(67.2593020179209,29.0978789691962,12.));
#169963=CARTESIAN_POINT('Ctrl Pts',(67.2331094720471,29.097502097147,0.));
#169964=CARTESIAN_POINT('Ctrl Pts',(67.2331094720471,29.097502097147,12.));
#169965=CARTESIAN_POINT('Ctrl Pts',(67.2069550447883,29.0971014004131,0.));
#169966=CARTESIAN_POINT('Ctrl Pts',(67.2069550447883,29.0971014004131,12.));
#169967=CARTESIAN_POINT('Ctrl Pts',(67.1808388322109,29.096676931389,0.));
#169968=CARTESIAN_POINT('Ctrl Pts',(67.1808388322109,29.096676931389,12.));
#169969=CARTESIAN_POINT('Ctrl Pts',(67.1547609306843,29.0962287427273,0.));
#169970=CARTESIAN_POINT('Ctrl Pts',(67.1547609306843,29.0962287427273,12.));
#169971=CARTESIAN_POINT('Ctrl Pts',(67.1287214368746,29.0957568873358,0.));
#169972=CARTESIAN_POINT('Ctrl Pts',(67.1287214368746,29.0957568873358,12.));
#169973=CARTESIAN_POINT('Ctrl Pts',(67.1027204477311,29.0952614183779,0.));
#169974=CARTESIAN_POINT('Ctrl Pts',(67.1027204477311,29.0952614183779,12.));
#169975=CARTESIAN_POINT('Ctrl Pts',(67.0767580604879,29.0947423892727,0.));
#169976=CARTESIAN_POINT('Ctrl Pts',(67.0767580604879,29.0947423892727,12.));
#169977=CARTESIAN_POINT('Ctrl Pts',(67.0508343726776,29.0941998536959,0.));
#169978=CARTESIAN_POINT('Ctrl Pts',(67.0508343726776,29.0941998536959,12.));
#169979=CARTESIAN_POINT('Ctrl Pts',(67.0249494821363,29.0936338655828,0.));
#169980=CARTESIAN_POINT('Ctrl Pts',(67.0249494821363,29.0936338655828,12.));
#169981=CARTESIAN_POINT('Ctrl Pts',(66.9991034870083,29.0930444791328,0.));
#169982=CARTESIAN_POINT('Ctrl Pts',(66.9991034870083,29.0930444791328,12.));
#169983=CARTESIAN_POINT('Ctrl Pts',(66.9732964857466,29.092431748817,0.));
#169984=CARTESIAN_POINT('Ctrl Pts',(66.9732964857466,29.092431748817,12.));
#169985=CARTESIAN_POINT('Ctrl Pts',(66.9475285771135,29.0917957293826,0.));
#169986=CARTESIAN_POINT('Ctrl Pts',(66.9475285771135,29.0917957293826,12.));
#169987=CARTESIAN_POINT('Ctrl Pts',(66.9217998601885,29.0911364758487,0.));
#169988=CARTESIAN_POINT('Ctrl Pts',(66.9217998601885,29.0911364758487,12.));
#169989=CARTESIAN_POINT('Ctrl Pts',(66.8961104343707,29.0904540435065,0.));
#169990=CARTESIAN_POINT('Ctrl Pts',(66.8961104343707,29.0904540435065,12.));
#169991=CARTESIAN_POINT('Ctrl Pts',(66.8704603993794,29.0897484879207,0.));
#169992=CARTESIAN_POINT('Ctrl Pts',(66.8704603993794,29.0897484879207,12.));
#169993=CARTESIAN_POINT('Ctrl Pts',(66.8448498552503,29.0890198649323,0.));
#169994=CARTESIAN_POINT('Ctrl Pts',(66.8448498552503,29.0890198649323,12.));
#169995=CARTESIAN_POINT('Ctrl Pts',(66.8192789023312,29.088268230663,0.));
#169996=CARTESIAN_POINT('Ctrl Pts',(66.8192789023312,29.088268230663,12.));
#169997=CARTESIAN_POINT('Ctrl Pts',(66.793747641293,29.0874936415132,0.));
#169998=CARTESIAN_POINT('Ctrl Pts',(66.793747641293,29.0874936415132,12.));
#169999=CARTESIAN_POINT('Ctrl Pts',(66.7682561731341,29.0866961541626,0.));
#170000=CARTESIAN_POINT('Ctrl Pts',(66.7682561731341,29.0866961541626,12.));
#170001=CARTESIAN_POINT('Ctrl Pts',(66.7428045991841,29.0858758255729,0.));
#170002=CARTESIAN_POINT('Ctrl Pts',(66.7428045991841,29.0858758255729,12.));
#170003=CARTESIAN_POINT('Ctrl Pts',(66.7173930211022,29.0850327129916,0.));
#170004=CARTESIAN_POINT('Ctrl Pts',(66.7173930211022,29.0850327129916,12.));
#170005=CARTESIAN_POINT('Ctrl Pts',(66.6920215408751,29.0841668739588,0.));
#170006=CARTESIAN_POINT('Ctrl Pts',(66.6920215408751,29.0841668739588,12.));
#170007=CARTESIAN_POINT('Ctrl Pts',(66.6666902608249,29.083278366305,0.));
#170008=CARTESIAN_POINT('Ctrl Pts',(66.6666902608249,29.083278366305,12.));
#170009=CARTESIAN_POINT('Ctrl Pts',(66.6413992836147,29.0823672481507,0.));
#170010=CARTESIAN_POINT('Ctrl Pts',(66.6413992836147,29.0823672481507,12.));
#170011=CARTESIAN_POINT('Ctrl Pts',(66.6161487122502,29.0814335779084,0.));
#170012=CARTESIAN_POINT('Ctrl Pts',(66.6161487122502,29.0814335779084,12.));
#170013=CARTESIAN_POINT('Ctrl Pts',(66.59093865008,29.0804774142854,0.));
#170014=CARTESIAN_POINT('Ctrl Pts',(66.59093865008,29.0804774142854,12.));
#170015=CARTESIAN_POINT('Ctrl Pts',(66.5657692007906,29.0794988162897,0.));
#170016=CARTESIAN_POINT('Ctrl Pts',(66.5657692007906,29.0794988162897,12.));
#170017=CARTESIAN_POINT('Ctrl Pts',(66.5406404684132,29.0784978432301,0.));
#170018=CARTESIAN_POINT('Ctrl Pts',(66.5406404684132,29.0784978432301,12.));
#170019=CARTESIAN_POINT('Ctrl Pts',(66.5155525573323,29.0774745547152,0.));
#170020=CARTESIAN_POINT('Ctrl Pts',(66.5155525573323,29.0774745547152,12.));
#170021=CARTESIAN_POINT('Ctrl Pts',(66.4905055722868,29.0764290106554,0.));
#170022=CARTESIAN_POINT('Ctrl Pts',(66.4905055722868,29.0764290106554,12.));
#170023=CARTESIAN_POINT('Ctrl Pts',(66.4654996183731,29.0753612712666,0.));
#170024=CARTESIAN_POINT('Ctrl Pts',(66.4654996183731,29.0753612712666,12.));
#170025=CARTESIAN_POINT('Ctrl Pts',(66.4405348010388,29.0742713970755,0.));
#170026=CARTESIAN_POINT('Ctrl Pts',(66.4405348010388,29.0742713970755,12.));
#170027=CARTESIAN_POINT('Ctrl Pts',(66.4156112260887,29.0731594489211,0.));
#170028=CARTESIAN_POINT('Ctrl Pts',(66.4156112260887,29.0731594489211,12.));
#170029=CARTESIAN_POINT('Ctrl Pts',(66.3907289996932,29.072025487953,0.));
#170030=CARTESIAN_POINT('Ctrl Pts',(66.3907289996932,29.072025487953,12.));
#170031=CARTESIAN_POINT('Ctrl Pts',(66.3658882283903,29.0708695756334,0.));
#170032=CARTESIAN_POINT('Ctrl Pts',(66.3658882283903,29.0708695756334,12.));
#170033=CARTESIAN_POINT('Ctrl Pts',(66.3410890190884,29.0696917737399,0.));
#170034=CARTESIAN_POINT('Ctrl Pts',(66.3410890190884,29.0696917737399,12.));
#170035=CARTESIAN_POINT('Ctrl Pts',(66.3163314790615,29.0684921443721,0.));
#170036=CARTESIAN_POINT('Ctrl Pts',(66.3163314790615,29.0684921443721,12.));
#170037=CARTESIAN_POINT('Ctrl Pts',(66.2916157159536,29.067270749953,0.));
#170038=CARTESIAN_POINT('Ctrl Pts',(66.2916157159536,29.067270749953,12.));
#170039=CARTESIAN_POINT('Ctrl Pts',(66.2669418377871,29.0660276532274,0.));
#170040=CARTESIAN_POINT('Ctrl Pts',(66.2669418377871,29.0660276532274,12.));
#170041=CARTESIAN_POINT('Ctrl Pts',(66.2423099529669,29.0647629172645,0.));
#170042=CARTESIAN_POINT('Ctrl Pts',(66.2423099529669,29.0647629172645,12.));
#170043=CARTESIAN_POINT('Ctrl Pts',(66.2177201702818,29.0634766054598,0.));
#170044=CARTESIAN_POINT('Ctrl Pts',(66.2177201702818,29.0634766054598,12.));
#170045=CARTESIAN_POINT('Ctrl Pts',(66.1931725989008,29.062168781542,0.));
#170046=CARTESIAN_POINT('Ctrl Pts',(66.1931725989008,29.062168781542,12.));
#170047=CARTESIAN_POINT('Ctrl Pts',(66.1686673483757,29.0608395095747,0.));
#170048=CARTESIAN_POINT('Ctrl Pts',(66.1686673483757,29.0608395095747,12.));
#170049=CARTESIAN_POINT('Ctrl Pts',(66.144204528652,29.0594888539558,0.));
#170050=CARTESIAN_POINT('Ctrl Pts',(66.144204528652,29.0594888539558,12.));
#170051=CARTESIAN_POINT('Ctrl Pts',(66.1197842500714,29.0581168794191,0.));
#170052=CARTESIAN_POINT('Ctrl Pts',(66.1197842500714,29.0581168794191,12.));
#170053=CARTESIAN_POINT('Ctrl Pts',(66.0954066233752,29.0567236510372,0.));
#170054=CARTESIAN_POINT('Ctrl Pts',(66.0954066233752,29.0567236510372,12.));
#170055=CARTESIAN_POINT('Ctrl Pts',(66.0710717597003,29.0553092342275,0.));
#170056=CARTESIAN_POINT('Ctrl Pts',(66.0710717597003,29.0553092342275,12.));
#170057=CARTESIAN_POINT('Ctrl Pts',(66.0467797705806,29.0538736947547,0.));
#170058=CARTESIAN_POINT('Ctrl Pts',(66.0467797705806,29.0538736947547,12.));
#170059=CARTESIAN_POINT('Ctrl Pts',(66.0225307679584,29.0524170987303,0.));
#170060=CARTESIAN_POINT('Ctrl Pts',(66.0225307679584,29.0524170987303,12.));
#170061=CARTESIAN_POINT('Ctrl Pts',(65.9983248641877,29.0509395126141,0.));
#170062=CARTESIAN_POINT('Ctrl Pts',(65.9983248641877,29.0509395126141,12.));
#170063=CARTESIAN_POINT('Ctrl Pts',(65.9741621720372,29.0494410032173,0.));
#170064=CARTESIAN_POINT('Ctrl Pts',(65.9741621720372,29.0494410032173,12.));
#170065=CARTESIAN_POINT('Ctrl Pts',(65.9500428046873,29.0479216377082,0.));
#170066=CARTESIAN_POINT('Ctrl Pts',(65.9500428046873,29.0479216377082,12.));
#170067=CARTESIAN_POINT('Ctrl Pts',(65.9259668757309,29.0463814836159,0.));
#170068=CARTESIAN_POINT('Ctrl Pts',(65.9259668757309,29.0463814836159,12.));
#170069=CARTESIAN_POINT('Ctrl Pts',(65.9019344991854,29.0448206088288,0.));
#170070=CARTESIAN_POINT('Ctrl Pts',(65.9019344991854,29.0448206088288,12.));
#170071=CARTESIAN_POINT('Ctrl Pts',(65.8779457894959,29.0432390815977,0.));
#170072=CARTESIAN_POINT('Ctrl Pts',(65.8779457894959,29.0432390815977,12.));
#170073=CARTESIAN_POINT('Ctrl Pts',(65.854000861539,29.0416369705375,0.));
#170074=CARTESIAN_POINT('Ctrl Pts',(65.854000861539,29.0416369705375,12.));
#170075=CARTESIAN_POINT('Ctrl Pts',(65.8300998306198,29.0400143446341,0.));
#170076=CARTESIAN_POINT('Ctrl Pts',(65.8300998306198,29.0400143446341,12.));
#170077=CARTESIAN_POINT('Ctrl Pts',(65.8062428124723,29.0383712732473,0.));
#170078=CARTESIAN_POINT('Ctrl Pts',(65.8062428124723,29.0383712732473,12.));
#170079=CARTESIAN_POINT('Ctrl Pts',(65.7824299232715,29.0367078261107,0.));
#170080=CARTESIAN_POINT('Ctrl Pts',(65.7824299232715,29.0367078261107,12.));
#170081=CARTESIAN_POINT('Ctrl Pts',(65.7586612796375,29.0350240733333,0.));
#170082=CARTESIAN_POINT('Ctrl Pts',(65.7586612796375,29.0350240733333,12.));
#170083=CARTESIAN_POINT('Ctrl Pts',(65.7349369986382,29.0333200854026,0.));
#170084=CARTESIAN_POINT('Ctrl Pts',(65.7349369986382,29.0333200854026,12.));
#170085=CARTESIAN_POINT('Ctrl Pts',(65.7112571977874,29.0315959331911,0.));
#170086=CARTESIAN_POINT('Ctrl Pts',(65.7112571977874,29.0315959331911,12.));
#170087=CARTESIAN_POINT('Ctrl Pts',(65.6876219950465,29.0298516879599,0.));
#170088=CARTESIAN_POINT('Ctrl Pts',(65.6876219950465,29.0298516879599,12.));
#170089=CARTESIAN_POINT('Ctrl Pts',(65.664031508836,29.0280874213584,0.));
#170090=CARTESIAN_POINT('Ctrl Pts',(65.664031508836,29.0280874213584,12.));
#170091=CARTESIAN_POINT('Ctrl Pts',(65.6404858580391,29.0263032054261,0.));
#170092=CARTESIAN_POINT('Ctrl Pts',(65.6404858580391,29.0263032054261,12.));
#170093=CARTESIAN_POINT('Ctrl Pts',(65.6169851620054,29.0244991125962,0.));
#170094=CARTESIAN_POINT('Ctrl Pts',(65.6169851620054,29.0244991125962,12.));
#170095=CARTESIAN_POINT('Ctrl Pts',(65.593529540548,29.0226752157013,0.));
#170096=CARTESIAN_POINT('Ctrl Pts',(65.593529540548,29.0226752157013,12.));
#170097=CARTESIAN_POINT('Ctrl Pts',(65.5701191139455,29.0208315879778,0.));
#170098=CARTESIAN_POINT('Ctrl Pts',(65.5701191139455,29.0208315879778,12.));
#170099=CARTESIAN_POINT('Ctrl Pts',(65.5467540029546,29.0189683030654,0.));
#170100=CARTESIAN_POINT('Ctrl Pts',(65.5467540029546,29.0189683030654,12.));
#170101=CARTESIAN_POINT('Ctrl Pts',(65.523434328815,29.01708543501,0.));
#170102=CARTESIAN_POINT('Ctrl Pts',(65.523434328815,29.01708543501,12.));
#170103=CARTESIAN_POINT('Ctrl Pts',(65.5001602132524,29.015183058267,0.));
#170104=CARTESIAN_POINT('Ctrl Pts',(65.5001602132524,29.015183058267,12.));
#170105=CARTESIAN_POINT('Ctrl Pts',(65.4769317784754,29.0132612477075,0.));
#170106=CARTESIAN_POINT('Ctrl Pts',(65.4769317784754,29.0132612477075,12.));
#170107=CARTESIAN_POINT('Ctrl Pts',(65.4537491471782,29.0113200786219,0.));
#170108=CARTESIAN_POINT('Ctrl Pts',(65.4537491471782,29.0113200786219,12.));
#170109=CARTESIAN_POINT('Ctrl Pts',(65.4306124425524,29.0093596267198,0.));
#170110=CARTESIAN_POINT('Ctrl Pts',(65.4306124425524,29.0093596267198,12.));
#170111=CARTESIAN_POINT('Ctrl Pts',(65.4075217882921,29.0073799681336,0.));
#170112=CARTESIAN_POINT('Ctrl Pts',(65.4075217882921,29.0073799681336,12.));
#170113=CARTESIAN_POINT('Ctrl Pts',(65.3844773085976,29.0053811794214,0.));
#170114=CARTESIAN_POINT('Ctrl Pts',(65.3844773085976,29.0053811794214,12.));
#170115=CARTESIAN_POINT('Ctrl Pts',(65.3614791281725,29.0033633375745,0.));
#170116=CARTESIAN_POINT('Ctrl Pts',(65.3614791281725,29.0033633375745,12.));
#170117=CARTESIAN_POINT('Ctrl Pts',(65.3385273722278,29.0013265200201,0.));
#170118=CARTESIAN_POINT('Ctrl Pts',(65.3385273722278,29.0013265200201,12.));
#170119=CARTESIAN_POINT('Ctrl Pts',(65.3156221664942,28.9992708046223,0.));
#170120=CARTESIAN_POINT('Ctrl Pts',(65.3156221664942,28.9992708046223,12.));
#170121=CARTESIAN_POINT('Ctrl Pts',(65.2927636372261,28.9971962696848,0.));
#170122=CARTESIAN_POINT('Ctrl Pts',(65.2927636372261,28.9971962696848,12.));
#170123=CARTESIAN_POINT('Ctrl Pts',(65.2699519112052,28.9951029939551,0.));
#170124=CARTESIAN_POINT('Ctrl Pts',(65.2699519112052,28.9951029939551,12.));
#170125=CARTESIAN_POINT('Ctrl Pts',(65.2471871157375,28.9929910566314,0.));
#170126=CARTESIAN_POINT('Ctrl Pts',(65.2471871157375,28.9929910566314,12.));
#170127=CARTESIAN_POINT('Ctrl Pts',(65.2244693786586,28.9908605373652,0.));
#170128=CARTESIAN_POINT('Ctrl Pts',(65.2244693786586,28.9908605373652,12.));
#170129=CARTESIAN_POINT('Ctrl Pts',(65.2017988283465,28.9887115162626,0.));
#170130=CARTESIAN_POINT('Ctrl Pts',(65.2017988283465,28.9887115162626,12.));
#170131=CARTESIAN_POINT('Ctrl Pts',(65.1791755937254,28.9865440738882,0.));
#170132=CARTESIAN_POINT('Ctrl Pts',(65.1791755937254,28.9865440738882,12.));
#170133=CARTESIAN_POINT('Ctrl Pts',(65.1565998042705,28.9843582912697,0.));
#170134=CARTESIAN_POINT('Ctrl Pts',(65.1565998042705,28.9843582912697,12.));
#170135=CARTESIAN_POINT('Ctrl Pts',(65.1340715900042,28.9821542499049,0.));
#170136=CARTESIAN_POINT('Ctrl Pts',(65.1340715900042,28.9821542499049,12.));
#170137=CARTESIAN_POINT('Ctrl Pts',(65.111591081505,28.9799320317648,0.));
#170138=CARTESIAN_POINT('Ctrl Pts',(65.111591081505,28.9799320317648,12.));
#170139=CARTESIAN_POINT('Ctrl Pts',(65.0891584099174,28.9776917192936,0.));
#170140=CARTESIAN_POINT('Ctrl Pts',(65.0891584099174,28.9776917192936,12.));
#170141=CARTESIAN_POINT('Ctrl Pts',(65.0667737069562,28.9754333954134,0.));
#170142=CARTESIAN_POINT('Ctrl Pts',(65.0667737069562,28.9754333954134,12.));
#170143=CARTESIAN_POINT('Ctrl Pts',(65.0444371049082,28.9731571435281,0.));
#170144=CARTESIAN_POINT('Ctrl Pts',(65.0444371049082,28.9731571435281,12.));
#170145=CARTESIAN_POINT('Ctrl Pts',(65.0221487366279,28.9708630475298,0.));
#170146=CARTESIAN_POINT('Ctrl Pts',(65.0221487366279,28.9708630475298,12.));
#170147=CARTESIAN_POINT('Ctrl Pts',(64.9999087355504,28.9685511918017,0.));
#170148=CARTESIAN_POINT('Ctrl Pts',(64.9999087355504,28.9685511918017,12.));
#170149=CARTESIAN_POINT('Ctrl Pts',(64.9777172357028,28.9662216612216,0.));
#170150=CARTESIAN_POINT('Ctrl Pts',(64.9777172357028,28.9662216612216,12.));
#170151=CARTESIAN_POINT('Ctrl Pts',(64.955574371711,28.9638745411677,0.));
#170152=CARTESIAN_POINT('Ctrl Pts',(64.955574371711,28.9638745411677,12.));
#170153=CARTESIAN_POINT('Ctrl Pts',(64.9334802788037,28.961509917525,0.));
#170154=CARTESIAN_POINT('Ctrl Pts',(64.9334802788037,28.961509917525,12.));
#170155=CARTESIAN_POINT('Ctrl Pts',(64.9114350928124,28.9591278766934,0.));
#170156=CARTESIAN_POINT('Ctrl Pts',(64.9114350928124,28.9591278766934,12.));
#170157=CARTESIAN_POINT('Ctrl Pts',(64.8894389501799,28.9567285055866,0.));
#170158=CARTESIAN_POINT('Ctrl Pts',(64.8894389501799,28.9567285055866,12.));
#170159=CARTESIAN_POINT('Ctrl Pts',(64.8674919879646,28.9543118916327,0.));
#170160=CARTESIAN_POINT('Ctrl Pts',(64.8674919879646,28.9543118916327,12.));
#170161=CARTESIAN_POINT('Ctrl Pts',(64.8455943438423,28.9518781227765,0.));
#170162=CARTESIAN_POINT('Ctrl Pts',(64.8455943438423,28.9518781227765,12.));
#170163=CARTESIAN_POINT('Ctrl Pts',(64.8237461561024,28.9494272874833,0.));
#170164=CARTESIAN_POINT('Ctrl Pts',(64.8237461561024,28.9494272874833,12.));
#170165=CARTESIAN_POINT('Ctrl Pts',(64.8019475636454,28.9469594747436,0.));
#170166=CARTESIAN_POINT('Ctrl Pts',(64.8019475636454,28.9469594747436,12.));
#170167=CARTESIAN_POINT('Ctrl Pts',(64.7801987060097,28.9444747740815,0.));
#170168=CARTESIAN_POINT('Ctrl Pts',(64.7801987060097,28.9444747740815,12.));
#170169=CARTESIAN_POINT('Ctrl Pts',(64.7584997233889,28.9419732755659,0.));
#170170=CARTESIAN_POINT('Ctrl Pts',(64.7584997233889,28.9419732755659,12.));
#170171=CARTESIAN_POINT('Ctrl Pts',(64.7368507566461,28.9394550698201,0.));
#170172=CARTESIAN_POINT('Ctrl Pts',(64.7368507566461,28.9394550698201,12.));
#170173=CARTESIAN_POINT('Ctrl Pts',(64.715251947327,28.9369202480383,0.));
#170174=CARTESIAN_POINT('Ctrl Pts',(64.715251947327,28.9369202480383,12.));
#170175=CARTESIAN_POINT('Ctrl Pts',(64.6937034376591,28.934368901987,0.));
#170176=CARTESIAN_POINT('Ctrl Pts',(64.6937034376591,28.934368901987,12.));
#170177=CARTESIAN_POINT('Ctrl Pts',(64.6722053705389,28.9318011239905,0.));
#170178=CARTESIAN_POINT('Ctrl Pts',(64.6722053705389,28.9318011239905,12.));
#170179=CARTESIAN_POINT('Ctrl Pts',(64.6507578895155,28.9292170069219,0.));
#170180=CARTESIAN_POINT('Ctrl Pts',(64.6507578895155,28.9292170069219,12.));
#170181=CARTESIAN_POINT('Ctrl Pts',(64.6293611387753,28.9266166441956,0.));
#170182=CARTESIAN_POINT('Ctrl Pts',(64.6293611387753,28.9266166441956,12.));
#170183=CARTESIAN_POINT('Ctrl Pts',(64.6080152631065,28.9240001297553,0.));
#170184=CARTESIAN_POINT('Ctrl Pts',(64.6080152631065,28.9240001297553,12.));
#170185=CARTESIAN_POINT('Ctrl Pts',(64.5867204079452,28.9213675580996,0.));
#170186=CARTESIAN_POINT('Ctrl Pts',(64.5867204079452,28.9213675580996,12.));
#170187=CARTESIAN_POINT('Ctrl Pts',(64.5654767194487,28.9187190243231,0.));
#170188=CARTESIAN_POINT('Ctrl Pts',(64.5654767194487,28.9187190243231,12.));
#170189=CARTESIAN_POINT('Ctrl Pts',(64.544284344556,28.9160546241538,0.));
#170190=CARTESIAN_POINT('Ctrl Pts',(64.544284344556,28.9160546241538,12.));
#170191=CARTESIAN_POINT('Ctrl Pts',(64.5231434310457,28.9133744539943,0.));
#170192=CARTESIAN_POINT('Ctrl Pts',(64.5231434310457,28.9133744539943,12.));
#170193=CARTESIAN_POINT('Ctrl Pts',(64.5020541275927,28.9106786109639,0.));
#170194=CARTESIAN_POINT('Ctrl Pts',(64.5020541275927,28.9106786109639,12.));
#170195=CARTESIAN_POINT('Ctrl Pts',(64.4810165836568,28.9079671928253,0.));
#170196=CARTESIAN_POINT('Ctrl Pts',(64.4810165836568,28.9079671928253,12.));
#170197=CARTESIAN_POINT('Ctrl Pts',(64.460030949357,28.9052402979055,0.));
#170198=CARTESIAN_POINT('Ctrl Pts',(64.460030949357,28.9052402979055,12.));
#170199=CARTESIAN_POINT('Ctrl Pts',(64.439097375364,28.9024980250309,0.));
#170200=CARTESIAN_POINT('Ctrl Pts',(64.439097375364,28.9024980250309,12.));
#170201=CARTESIAN_POINT('Ctrl Pts',(64.41821601274,28.899740473435,0.));
#170202=CARTESIAN_POINT('Ctrl Pts',(64.41821601274,28.899740473435,12.));
#170203=CARTESIAN_POINT('Ctrl Pts',(64.3973870129201,28.8969677427519,0.));
#170204=CARTESIAN_POINT('Ctrl Pts',(64.3973870129201,28.8969677427519,12.));
#170205=CARTESIAN_POINT('Ctrl Pts',(64.3766105280715,28.8941799332312,0.));
#170206=CARTESIAN_POINT('Ctrl Pts',(64.3766105280715,28.8941799332312,12.));
#170207=CARTESIAN_POINT('Ctrl Pts',(64.3558867114087,28.8913771459327,0.));
#170208=CARTESIAN_POINT('Ctrl Pts',(64.3558867114087,28.8913771459327,12.));
#170209=CARTESIAN_POINT('Ctrl Pts',(64.3352157174606,28.888559482892,0.));
#170210=CARTESIAN_POINT('Ctrl Pts',(64.3352157174606,28.888559482892,12.));
#170211=CARTESIAN_POINT('Ctrl Pts',(64.3145977025005,28.8857270473944,0.));
#170212=CARTESIAN_POINT('Ctrl Pts',(64.3145977025005,28.8857270473944,12.));
#170213=CARTESIAN_POINT('Ctrl Pts',(64.2940328242482,28.8828799437922,0.));
#170214=CARTESIAN_POINT('Ctrl Pts',(64.2940328242482,28.8828799437922,12.));
#170215=CARTESIAN_POINT('Ctrl Pts',(64.2735212410682,28.8800182770052,0.));
#170216=CARTESIAN_POINT('Ctrl Pts',(64.2735212410682,28.8800182770052,12.));
#170217=CARTESIAN_POINT('Ctrl Pts',(64.2530631112926,28.8771421521058,0.));
#170218=CARTESIAN_POINT('Ctrl Pts',(64.2530631112926,28.8771421521058,12.));
#170219=CARTESIAN_POINT('Ctrl Pts',(64.232658592528,28.8742516738959,0.));
#170220=CARTESIAN_POINT('Ctrl Pts',(64.232658592528,28.8742516738959,12.));
#170221=CARTESIAN_POINT('Ctrl Pts',(64.2123078408507,28.8713469464205,0.));
#170222=CARTESIAN_POINT('Ctrl Pts',(64.2123078408507,28.8713469464205,12.));
#170223=CARTESIAN_POINT('Ctrl Pts',(64.1920110123342,28.8684280739033,0.));
#170224=CARTESIAN_POINT('Ctrl Pts',(64.1920110123342,28.8684280739033,12.));
#170225=CARTESIAN_POINT('Ctrl Pts',(64.1717682648708,28.8654951618659,0.));
#170226=CARTESIAN_POINT('Ctrl Pts',(64.1717682648708,28.8654951618659,12.));
#170227=CARTESIAN_POINT('Ctrl Pts',(64.1515797596555,28.8625483180433,0.));
#170228=CARTESIAN_POINT('Ctrl Pts',(64.1515797596555,28.8625483180433,12.));
#170229=CARTESIAN_POINT('Ctrl Pts',(64.1314456633345,28.8595876537132,0.));
#170230=CARTESIAN_POINT('Ctrl Pts',(64.1314456633345,28.8595876537132,12.));
#170231=CARTESIAN_POINT('Ctrl Pts',(64.1113661481918,28.8566132838157,0.));
#170232=CARTESIAN_POINT('Ctrl Pts',(64.1113661481918,28.8566132838157,12.));
#170233=CARTESIAN_POINT('Ctrl Pts',(64.0913413876586,28.8536253241837,0.));
#170234=CARTESIAN_POINT('Ctrl Pts',(64.0913413876586,28.8536253241837,12.));
#170235=CARTESIAN_POINT('Ctrl Pts',(64.0713715523588,28.8506238891087,0.));
#170236=CARTESIAN_POINT('Ctrl Pts',(64.0713715523588,28.8506238891087,12.));
#170237=CARTESIAN_POINT('Ctrl Pts',(64.0514568066659,28.8476090892242,0.));
#170238=CARTESIAN_POINT('Ctrl Pts',(64.0514568066659,28.8476090892242,12.));
#170239=CARTESIAN_POINT('Ctrl Pts',(64.0315973031994,28.8445810281275,0.));
#170240=CARTESIAN_POINT('Ctrl Pts',(64.0315973031994,28.8445810281275,12.));
#170241=CARTESIAN_POINT('Ctrl Pts',(64.0117931881364,28.841539805646,0.));
#170242=CARTESIAN_POINT('Ctrl Pts',(64.0117931881364,28.841539805646,12.));
#170243=CARTESIAN_POINT('Ctrl Pts',(63.9920446117632,28.8384855243267,0.));
#170244=CARTESIAN_POINT('Ctrl Pts',(63.9920446117632,28.8384855243267,12.));
#170245=CARTESIAN_POINT('Ctrl Pts',(63.9723517369614,28.8354182946601,0.));
#170246=CARTESIAN_POINT('Ctrl Pts',(63.9723517369614,28.8354182946601,12.));
#170247=CARTESIAN_POINT('Ctrl Pts',(63.9527147494351,28.8323382413753,0.));
#170248=CARTESIAN_POINT('Ctrl Pts',(63.9527147494351,28.8323382413753,12.));
#170249=CARTESIAN_POINT('Ctrl Pts',(63.9331338646868,28.8292455077494,0.));
#170250=CARTESIAN_POINT('Ctrl Pts',(63.9331338646868,28.8292455077494,12.));
#170251=CARTESIAN_POINT('Ctrl Pts',(63.9136093063647,28.826140242322,0.));
#170252=CARTESIAN_POINT('Ctrl Pts',(63.9136093063647,28.826140242322,12.));
#170253=CARTESIAN_POINT('Ctrl Pts',(63.894141285685,28.8230225863142,0.));
#170254=CARTESIAN_POINT('Ctrl Pts',(63.894141285685,28.8230225863142,12.));
#170255=CARTESIAN_POINT('Ctrl Pts',(63.8747299825383,28.8198926619893,0.));
#170256=CARTESIAN_POINT('Ctrl Pts',(63.8747299825383,28.8198926619893,12.));
#170257=CARTESIAN_POINT('Ctrl Pts',(63.8553755207732,28.8167505576806,0.));
#170258=CARTESIAN_POINT('Ctrl Pts',(63.8553755207732,28.8167505576806,12.));
#170259=CARTESIAN_POINT('Ctrl Pts',(63.8360779670225,28.8135963263557,0.));
#170260=CARTESIAN_POINT('Ctrl Pts',(63.8360779670225,28.8135963263557,12.));
#170261=CARTESIAN_POINT('Ctrl Pts',(63.8206854735372,28.8110632621133,0.));
#170262=CARTESIAN_POINT('Ctrl Pts',(63.8206854735372,28.8110632621133,12.));
#170263=CARTESIAN_POINT('Ctrl Pts',(63.809166727145,28.8091580239664,0.));
#170264=CARTESIAN_POINT('Ctrl Pts',(63.809166727145,28.8091580239664,12.));
#170265=CARTESIAN_POINT('Ctrl Pts',(63.8014989507575,28.8078854475473,0.));
#170266=CARTESIAN_POINT('Ctrl Pts',(63.8014989507575,28.8078854475473,12.));
#170267=CARTESIAN_POINT('Ctrl Pts',(63.7976679095314,28.8072485549236,0.));
#170268=CARTESIAN_POINT('Ctrl Pts',(63.7976679095314,28.8072485549236,12.));
#170269=CARTESIAN_POINT('',(63.7976679095314,28.8072485549236,12.));
#170270=CARTESIAN_POINT('Ctrl Pts',(63.7976679095314,28.8072485549236,12.));
#170271=CARTESIAN_POINT('Ctrl Pts',(63.8014989507575,28.8078854475473,12.));
#170272=CARTESIAN_POINT('Ctrl Pts',(63.809166727145,28.8091580239664,12.));
#170273=CARTESIAN_POINT('Ctrl Pts',(63.8206854735372,28.8110632621133,12.));
#170274=CARTESIAN_POINT('Ctrl Pts',(63.8360779670225,28.8135963263557,12.));
#170275=CARTESIAN_POINT('Ctrl Pts',(63.8553755207732,28.8167505576806,12.));
#170276=CARTESIAN_POINT('Ctrl Pts',(63.8747299825383,28.8198926619893,12.));
#170277=CARTESIAN_POINT('Ctrl Pts',(63.894141285685,28.8230225863142,12.));
#170278=CARTESIAN_POINT('Ctrl Pts',(63.9136093063647,28.826140242322,12.));
#170279=CARTESIAN_POINT('Ctrl Pts',(63.9331338646868,28.8292455077494,12.));
#170280=CARTESIAN_POINT('Ctrl Pts',(63.9527147494351,28.8323382413753,12.));
#170281=CARTESIAN_POINT('Ctrl Pts',(63.9723517369614,28.8354182946601,12.));
#170282=CARTESIAN_POINT('Ctrl Pts',(63.9920446117632,28.8384855243267,12.));
#170283=CARTESIAN_POINT('Ctrl Pts',(64.0117931881364,28.841539805646,12.));
#170284=CARTESIAN_POINT('Ctrl Pts',(64.0315973031994,28.8445810281275,12.));
#170285=CARTESIAN_POINT('Ctrl Pts',(64.0514568066659,28.8476090892242,12.));
#170286=CARTESIAN_POINT('Ctrl Pts',(64.0713715523588,28.8506238891087,12.));
#170287=CARTESIAN_POINT('Ctrl Pts',(64.0913413876586,28.8536253241837,12.));
#170288=CARTESIAN_POINT('Ctrl Pts',(64.1113661481918,28.8566132838157,12.));
#170289=CARTESIAN_POINT('Ctrl Pts',(64.1314456633345,28.8595876537132,12.));
#170290=CARTESIAN_POINT('Ctrl Pts',(64.1515797596555,28.8625483180433,12.));
#170291=CARTESIAN_POINT('Ctrl Pts',(64.1717682648708,28.8654951618659,12.));
#170292=CARTESIAN_POINT('Ctrl Pts',(64.1920110123342,28.8684280739033,12.));
#170293=CARTESIAN_POINT('Ctrl Pts',(64.2123078408507,28.8713469464205,12.));
#170294=CARTESIAN_POINT('Ctrl Pts',(64.232658592528,28.8742516738959,12.));
#170295=CARTESIAN_POINT('Ctrl Pts',(64.2530631112926,28.8771421521058,12.));
#170296=CARTESIAN_POINT('Ctrl Pts',(64.2735212410682,28.8800182770052,12.));
#170297=CARTESIAN_POINT('Ctrl Pts',(64.2940328242482,28.8828799437922,12.));
#170298=CARTESIAN_POINT('Ctrl Pts',(64.3145977025005,28.8857270473944,12.));
#170299=CARTESIAN_POINT('Ctrl Pts',(64.3352157174606,28.888559482892,12.));
#170300=CARTESIAN_POINT('Ctrl Pts',(64.3558867114087,28.8913771459327,12.));
#170301=CARTESIAN_POINT('Ctrl Pts',(64.3766105280715,28.8941799332312,12.));
#170302=CARTESIAN_POINT('Ctrl Pts',(64.3973870129201,28.8969677427519,12.));
#170303=CARTESIAN_POINT('Ctrl Pts',(64.41821601274,28.899740473435,12.));
#170304=CARTESIAN_POINT('Ctrl Pts',(64.439097375364,28.9024980250309,12.));
#170305=CARTESIAN_POINT('Ctrl Pts',(64.460030949357,28.9052402979055,12.));
#170306=CARTESIAN_POINT('Ctrl Pts',(64.4810165836568,28.9079671928253,12.));
#170307=CARTESIAN_POINT('Ctrl Pts',(64.5020541275927,28.9106786109639,12.));
#170308=CARTESIAN_POINT('Ctrl Pts',(64.5231434310457,28.9133744539943,12.));
#170309=CARTESIAN_POINT('Ctrl Pts',(64.544284344556,28.9160546241538,12.));
#170310=CARTESIAN_POINT('Ctrl Pts',(64.5654767194487,28.9187190243231,12.));
#170311=CARTESIAN_POINT('Ctrl Pts',(64.5867204079452,28.9213675580996,12.));
#170312=CARTESIAN_POINT('Ctrl Pts',(64.6080152631065,28.9240001297553,12.));
#170313=CARTESIAN_POINT('Ctrl Pts',(64.6293611387753,28.9266166441956,12.));
#170314=CARTESIAN_POINT('Ctrl Pts',(64.6507578895155,28.9292170069219,12.));
#170315=CARTESIAN_POINT('Ctrl Pts',(64.6722053705389,28.9318011239905,12.));
#170316=CARTESIAN_POINT('Ctrl Pts',(64.6937034376591,28.934368901987,12.));
#170317=CARTESIAN_POINT('Ctrl Pts',(64.715251947327,28.9369202480383,12.));
#170318=CARTESIAN_POINT('Ctrl Pts',(64.7368507566461,28.9394550698201,12.));
#170319=CARTESIAN_POINT('Ctrl Pts',(64.7584997233889,28.9419732755659,12.));
#170320=CARTESIAN_POINT('Ctrl Pts',(64.7801987060097,28.9444747740815,12.));
#170321=CARTESIAN_POINT('Ctrl Pts',(64.8019475636454,28.9469594747436,12.));
#170322=CARTESIAN_POINT('Ctrl Pts',(64.8237461561024,28.9494272874833,12.));
#170323=CARTESIAN_POINT('Ctrl Pts',(64.8455943438423,28.9518781227765,12.));
#170324=CARTESIAN_POINT('Ctrl Pts',(64.8674919879646,28.9543118916327,12.));
#170325=CARTESIAN_POINT('Ctrl Pts',(64.8894389501799,28.9567285055866,12.));
#170326=CARTESIAN_POINT('Ctrl Pts',(64.9114350928124,28.9591278766934,12.));
#170327=CARTESIAN_POINT('Ctrl Pts',(64.9334802788037,28.961509917525,12.));
#170328=CARTESIAN_POINT('Ctrl Pts',(64.955574371711,28.9638745411677,12.));
#170329=CARTESIAN_POINT('Ctrl Pts',(64.9777172357028,28.9662216612216,12.));
#170330=CARTESIAN_POINT('Ctrl Pts',(64.9999087355504,28.9685511918017,12.));
#170331=CARTESIAN_POINT('Ctrl Pts',(65.0221487366279,28.9708630475298,12.));
#170332=CARTESIAN_POINT('Ctrl Pts',(65.0444371049082,28.9731571435281,12.));
#170333=CARTESIAN_POINT('Ctrl Pts',(65.0667737069562,28.9754333954134,12.));
#170334=CARTESIAN_POINT('Ctrl Pts',(65.0891584099174,28.9776917192936,12.));
#170335=CARTESIAN_POINT('Ctrl Pts',(65.111591081505,28.9799320317648,12.));
#170336=CARTESIAN_POINT('Ctrl Pts',(65.1340715900042,28.9821542499049,12.));
#170337=CARTESIAN_POINT('Ctrl Pts',(65.1565998042705,28.9843582912697,12.));
#170338=CARTESIAN_POINT('Ctrl Pts',(65.1791755937254,28.9865440738882,12.));
#170339=CARTESIAN_POINT('Ctrl Pts',(65.2017988283465,28.9887115162626,12.));
#170340=CARTESIAN_POINT('Ctrl Pts',(65.2244693786586,28.9908605373652,12.));
#170341=CARTESIAN_POINT('Ctrl Pts',(65.2471871157375,28.9929910566314,12.));
#170342=CARTESIAN_POINT('Ctrl Pts',(65.2699519112052,28.9951029939551,12.));
#170343=CARTESIAN_POINT('Ctrl Pts',(65.2927636372261,28.9971962696848,12.));
#170344=CARTESIAN_POINT('Ctrl Pts',(65.3156221664942,28.9992708046223,12.));
#170345=CARTESIAN_POINT('Ctrl Pts',(65.3385273722278,29.0013265200201,12.));
#170346=CARTESIAN_POINT('Ctrl Pts',(65.3614791281725,29.0033633375745,12.));
#170347=CARTESIAN_POINT('Ctrl Pts',(65.3844773085976,29.0053811794214,12.));
#170348=CARTESIAN_POINT('Ctrl Pts',(65.4075217882921,29.0073799681336,12.));
#170349=CARTESIAN_POINT('Ctrl Pts',(65.4306124425524,29.0093596267198,12.));
#170350=CARTESIAN_POINT('Ctrl Pts',(65.4537491471782,29.0113200786219,12.));
#170351=CARTESIAN_POINT('Ctrl Pts',(65.4769317784754,29.0132612477075,12.));
#170352=CARTESIAN_POINT('Ctrl Pts',(65.5001602132524,29.015183058267,12.));
#170353=CARTESIAN_POINT('Ctrl Pts',(65.523434328815,29.01708543501,12.));
#170354=CARTESIAN_POINT('Ctrl Pts',(65.5467540029546,29.0189683030654,12.));
#170355=CARTESIAN_POINT('Ctrl Pts',(65.5701191139455,29.0208315879778,12.));
#170356=CARTESIAN_POINT('Ctrl Pts',(65.593529540548,29.0226752157013,12.));
#170357=CARTESIAN_POINT('Ctrl Pts',(65.6169851620054,29.0244991125962,12.));
#170358=CARTESIAN_POINT('Ctrl Pts',(65.6404858580391,29.0263032054261,12.));
#170359=CARTESIAN_POINT('Ctrl Pts',(65.664031508836,29.0280874213584,12.));
#170360=CARTESIAN_POINT('Ctrl Pts',(65.6876219950465,29.0298516879599,12.));
#170361=CARTESIAN_POINT('Ctrl Pts',(65.7112571977874,29.0315959331911,12.));
#170362=CARTESIAN_POINT('Ctrl Pts',(65.7349369986382,29.0333200854026,12.));
#170363=CARTESIAN_POINT('Ctrl Pts',(65.7586612796375,29.0350240733333,12.));
#170364=CARTESIAN_POINT('Ctrl Pts',(65.7824299232715,29.0367078261107,12.));
#170365=CARTESIAN_POINT('Ctrl Pts',(65.8062428124723,29.0383712732473,12.));
#170366=CARTESIAN_POINT('Ctrl Pts',(65.8300998306198,29.0400143446341,12.));
#170367=CARTESIAN_POINT('Ctrl Pts',(65.854000861539,29.0416369705375,12.));
#170368=CARTESIAN_POINT('Ctrl Pts',(65.8779457894959,29.0432390815977,12.));
#170369=CARTESIAN_POINT('Ctrl Pts',(65.9019344991854,29.0448206088288,12.));
#170370=CARTESIAN_POINT('Ctrl Pts',(65.9259668757309,29.0463814836159,12.));
#170371=CARTESIAN_POINT('Ctrl Pts',(65.9500428046873,29.0479216377082,12.));
#170372=CARTESIAN_POINT('Ctrl Pts',(65.9741621720372,29.0494410032173,12.));
#170373=CARTESIAN_POINT('Ctrl Pts',(65.9983248641877,29.0509395126141,12.));
#170374=CARTESIAN_POINT('Ctrl Pts',(66.0225307679584,29.0524170987303,12.));
#170375=CARTESIAN_POINT('Ctrl Pts',(66.0467797705806,29.0538736947547,12.));
#170376=CARTESIAN_POINT('Ctrl Pts',(66.0710717597003,29.0553092342275,12.));
#170377=CARTESIAN_POINT('Ctrl Pts',(66.0954066233752,29.0567236510372,12.));
#170378=CARTESIAN_POINT('Ctrl Pts',(66.1197842500714,29.0581168794191,12.));
#170379=CARTESIAN_POINT('Ctrl Pts',(66.144204528652,29.0594888539558,12.));
#170380=CARTESIAN_POINT('Ctrl Pts',(66.1686673483757,29.0608395095747,12.));
#170381=CARTESIAN_POINT('Ctrl Pts',(66.1931725989008,29.062168781542,12.));
#170382=CARTESIAN_POINT('Ctrl Pts',(66.2177201702818,29.0634766054598,12.));
#170383=CARTESIAN_POINT('Ctrl Pts',(66.2423099529669,29.0647629172645,12.));
#170384=CARTESIAN_POINT('Ctrl Pts',(66.2669418377871,29.0660276532274,12.));
#170385=CARTESIAN_POINT('Ctrl Pts',(66.2916157159536,29.067270749953,12.));
#170386=CARTESIAN_POINT('Ctrl Pts',(66.3163314790615,29.0684921443721,12.));
#170387=CARTESIAN_POINT('Ctrl Pts',(66.3410890190884,29.0696917737399,12.));
#170388=CARTESIAN_POINT('Ctrl Pts',(66.3658882283903,29.0708695756334,12.));
#170389=CARTESIAN_POINT('Ctrl Pts',(66.3907289996932,29.072025487953,12.));
#170390=CARTESIAN_POINT('Ctrl Pts',(66.4156112260887,29.0731594489211,12.));
#170391=CARTESIAN_POINT('Ctrl Pts',(66.4405348010388,29.0742713970755,12.));
#170392=CARTESIAN_POINT('Ctrl Pts',(66.4654996183731,29.0753612712666,12.));
#170393=CARTESIAN_POINT('Ctrl Pts',(66.4905055722868,29.0764290106554,12.));
#170394=CARTESIAN_POINT('Ctrl Pts',(66.5155525573323,29.0774745547152,12.));
#170395=CARTESIAN_POINT('Ctrl Pts',(66.5406404684132,29.0784978432301,12.));
#170396=CARTESIAN_POINT('Ctrl Pts',(66.5657692007906,29.0794988162897,12.));
#170397=CARTESIAN_POINT('Ctrl Pts',(66.59093865008,29.0804774142854,12.));
#170398=CARTESIAN_POINT('Ctrl Pts',(66.6161487122502,29.0814335779084,12.));
#170399=CARTESIAN_POINT('Ctrl Pts',(66.6413992836147,29.0823672481507,12.));
#170400=CARTESIAN_POINT('Ctrl Pts',(66.6666902608249,29.083278366305,12.));
#170401=CARTESIAN_POINT('Ctrl Pts',(66.6920215408751,29.0841668739588,12.));
#170402=CARTESIAN_POINT('Ctrl Pts',(66.7173930211022,29.0850327129916,12.));
#170403=CARTESIAN_POINT('Ctrl Pts',(66.7428045991841,29.0858758255729,12.));
#170404=CARTESIAN_POINT('Ctrl Pts',(66.7682561731341,29.0866961541626,12.));
#170405=CARTESIAN_POINT('Ctrl Pts',(66.793747641293,29.0874936415132,12.));
#170406=CARTESIAN_POINT('Ctrl Pts',(66.8192789023312,29.088268230663,12.));
#170407=CARTESIAN_POINT('Ctrl Pts',(66.8448498552503,29.0890198649323,12.));
#170408=CARTESIAN_POINT('Ctrl Pts',(66.8704603993794,29.0897484879207,12.));
#170409=CARTESIAN_POINT('Ctrl Pts',(66.8961104343707,29.0904540435065,12.));
#170410=CARTESIAN_POINT('Ctrl Pts',(66.9217998601885,29.0911364758487,12.));
#170411=CARTESIAN_POINT('Ctrl Pts',(66.9475285771135,29.0917957293826,12.));
#170412=CARTESIAN_POINT('Ctrl Pts',(66.9732964857466,29.092431748817,12.));
#170413=CARTESIAN_POINT('Ctrl Pts',(66.9991034870083,29.0930444791328,12.));
#170414=CARTESIAN_POINT('Ctrl Pts',(67.0249494821363,29.0936338655828,12.));
#170415=CARTESIAN_POINT('Ctrl Pts',(67.0508343726776,29.0941998536959,12.));
#170416=CARTESIAN_POINT('Ctrl Pts',(67.0767580604879,29.0947423892727,12.));
#170417=CARTESIAN_POINT('Ctrl Pts',(67.1027204477311,29.0952614183779,12.));
#170418=CARTESIAN_POINT('Ctrl Pts',(67.1287214368746,29.0957568873358,12.));
#170419=CARTESIAN_POINT('Ctrl Pts',(67.1547609306843,29.0962287427273,12.));
#170420=CARTESIAN_POINT('Ctrl Pts',(67.1808388322109,29.096676931389,12.));
#170421=CARTESIAN_POINT('Ctrl Pts',(67.2069550447883,29.0971014004131,12.));
#170422=CARTESIAN_POINT('Ctrl Pts',(67.2331094720471,29.097502097147,12.));
#170423=CARTESIAN_POINT('Ctrl Pts',(67.2593020179209,29.0978789691962,12.));
#170424=CARTESIAN_POINT('Ctrl Pts',(67.2855325866517,29.0982319644277,12.));
#170425=CARTESIAN_POINT('Ctrl Pts',(67.311801082792,29.0985610309771,12.));
#170426=CARTESIAN_POINT('Ctrl Pts',(67.3381074112027,29.0988661172531,12.));
#170427=CARTESIAN_POINT('Ctrl Pts',(67.3644514770387,29.0991471719176,12.));
#170428=CARTESIAN_POINT('Ctrl Pts',(67.3908331857323,29.0994041438719,12.));
#170429=CARTESIAN_POINT('Ctrl Pts',(67.4172524429727,29.0996369822418,12.));
#170430=CARTESIAN_POINT('Ctrl Pts',(67.4437091546859,29.0998456363683,12.));
#170431=CARTESIAN_POINT('Ctrl Pts',(67.4702032270048,29.1000300557955,12.));
#170432=CARTESIAN_POINT('Ctrl Pts',(67.4967345663096,29.1001901902909,12.));
#170433=CARTESIAN_POINT('Ctrl Pts',(67.5233030792704,29.1003259898682,12.));
#170434=CARTESIAN_POINT('Ctrl Pts',(67.5499086728888,29.1004374048148,12.));
#170435=CARTESIAN_POINT('Ctrl Pts',(67.5765512545281,29.1005243857139,12.));
#170436=CARTESIAN_POINT('Ctrl Pts',(67.6032307319623,29.1005868834866,12.));
#170437=CARTESIAN_POINT('Ctrl Pts',(67.6299470133295,29.100624849358,12.));
#170438=CARTESIAN_POINT('Ctrl Pts',(67.6567000070326,29.1006382347814,12.));
#170439=CARTESIAN_POINT('Ctrl Pts',(67.6834896216461,29.1006269913747,12.));
#170440=CARTESIAN_POINT('Ctrl Pts',(67.7103157658296,29.1005910708624,12.));
#170441=CARTESIAN_POINT('Ctrl Pts',(67.7371783482035,29.1005304249987,12.));
#170442=CARTESIAN_POINT('Ctrl Pts',(67.7640772773387,29.1004450055643,12.));
#170443=CARTESIAN_POINT('Ctrl Pts',(67.7910124620135,29.1003347645294,12.));
#170444=CARTESIAN_POINT('Ctrl Pts',(67.8179838114099,29.1001996541842,12.));
#170445=CARTESIAN_POINT('Ctrl Pts',(67.8449912353329,29.1000396272867,12.));
#170446=CARTESIAN_POINT('Ctrl Pts',(67.8720346444124,29.0998546372032,12.));
#170447=CARTESIAN_POINT('Ctrl Pts',(67.8991139503193,29.0996446380626,12.));
#170448=CARTESIAN_POINT('Ctrl Pts',(67.9262290652829,29.099409584422,12.));
#170449=CARTESIAN_POINT('Ctrl Pts',(67.9533799016148,29.0991494309404,12.));
#170450=CARTESIAN_POINT('Ctrl Pts',(67.9805663711855,29.0988641320247,12.));
#170451=CARTESIAN_POINT('Ctrl Pts',(68.0077883850121,29.0985536415531,12.));
#170452=CARTESIAN_POINT('Ctrl Pts',(68.0350458525551,29.0982179124097,12.));
#170453=CARTESIAN_POINT('Ctrl Pts',(68.0623386822863,29.0978568968657,12.));
#170454=CARTESIAN_POINT('Ctrl Pts',(68.0896667829567,29.0974705474259,12.));
#170455=CARTESIAN_POINT('Ctrl Pts',(68.1170300646987,29.0970588175728,12.));
#170456=CARTESIAN_POINT('Ctrl Pts',(68.1444284400742,29.0966216624743,12.));
#170457=CARTESIAN_POINT('Ctrl Pts',(68.1718618254281,29.0961590399046,12.));
#170458=CARTESIAN_POINT('Ctrl Pts',(68.1993301412061,29.0956709104627,12.));
#170459=CARTESIAN_POINT('Ctrl Pts',(68.2229056854683,29.095230591515,12.));
#170460=CARTESIAN_POINT('Ctrl Pts',(68.2409993690197,29.094879194787,12.));
#170461=CARTESIAN_POINT('Ctrl Pts',(68.2535957747187,29.0946280433337,12.));
#170462=CARTESIAN_POINT('Ctrl Pts',(68.2606847334987,29.0944846386568,12.));
#170463=CARTESIAN_POINT('Ctrl Pts',(68.2622612910177,29.0944526440266,12.));
#170464=CARTESIAN_POINT('',(63.7976679095314,28.8072485549236,0.));
#170465=CARTESIAN_POINT('',(63.7976679095314,28.8072485549236,0.));
#170466=CARTESIAN_POINT('Ctrl Pts',(68.2622612910177,29.0944526440266,0.));
#170467=CARTESIAN_POINT('Ctrl Pts',(68.2606847334987,29.0944846386568,0.));
#170468=CARTESIAN_POINT('Ctrl Pts',(68.2535957747187,29.0946280433337,0.));
#170469=CARTESIAN_POINT('Ctrl Pts',(68.2409993690197,29.094879194787,0.));
#170470=CARTESIAN_POINT('Ctrl Pts',(68.2229056854683,29.095230591515,0.));
#170471=CARTESIAN_POINT('Ctrl Pts',(68.1993301412061,29.0956709104627,0.));
#170472=CARTESIAN_POINT('Ctrl Pts',(68.1718618254281,29.0961590399046,0.));
#170473=CARTESIAN_POINT('Ctrl Pts',(68.1444284400742,29.0966216624743,0.));
#170474=CARTESIAN_POINT('Ctrl Pts',(68.1170300646987,29.0970588175728,0.));
#170475=CARTESIAN_POINT('Ctrl Pts',(68.0896667829567,29.0974705474259,0.));
#170476=CARTESIAN_POINT('Ctrl Pts',(68.0623386822863,29.0978568968657,0.));
#170477=CARTESIAN_POINT('Ctrl Pts',(68.0350458525551,29.0982179124097,0.));
#170478=CARTESIAN_POINT('Ctrl Pts',(68.0077883850121,29.0985536415531,0.));
#170479=CARTESIAN_POINT('Ctrl Pts',(67.9805663711855,29.0988641320247,0.));
#170480=CARTESIAN_POINT('Ctrl Pts',(67.9533799016148,29.0991494309404,0.));
#170481=CARTESIAN_POINT('Ctrl Pts',(67.9262290652829,29.099409584422,0.));
#170482=CARTESIAN_POINT('Ctrl Pts',(67.8991139503193,29.0996446380626,0.));
#170483=CARTESIAN_POINT('Ctrl Pts',(67.8720346444124,29.0998546372032,0.));
#170484=CARTESIAN_POINT('Ctrl Pts',(67.8449912353329,29.1000396272867,0.));
#170485=CARTESIAN_POINT('Ctrl Pts',(67.8179838114099,29.1001996541842,0.));
#170486=CARTESIAN_POINT('Ctrl Pts',(67.7910124620135,29.1003347645294,0.));
#170487=CARTESIAN_POINT('Ctrl Pts',(67.7640772773387,29.1004450055643,0.));
#170488=CARTESIAN_POINT('Ctrl Pts',(67.7371783482035,29.1005304249987,0.));
#170489=CARTESIAN_POINT('Ctrl Pts',(67.7103157658296,29.1005910708624,0.));
#170490=CARTESIAN_POINT('Ctrl Pts',(67.6834896216461,29.1006269913747,0.));
#170491=CARTESIAN_POINT('Ctrl Pts',(67.6567000070326,29.1006382347814,0.));
#170492=CARTESIAN_POINT('Ctrl Pts',(67.6299470133295,29.100624849358,0.));
#170493=CARTESIAN_POINT('Ctrl Pts',(67.6032307319623,29.1005868834866,0.));
#170494=CARTESIAN_POINT('Ctrl Pts',(67.5765512545281,29.1005243857139,0.));
#170495=CARTESIAN_POINT('Ctrl Pts',(67.5499086728888,29.1004374048148,0.));
#170496=CARTESIAN_POINT('Ctrl Pts',(67.5233030792704,29.1003259898682,0.));
#170497=CARTESIAN_POINT('Ctrl Pts',(67.4967345663096,29.1001901902909,0.));
#170498=CARTESIAN_POINT('Ctrl Pts',(67.4702032270048,29.1000300557955,0.));
#170499=CARTESIAN_POINT('Ctrl Pts',(67.4437091546859,29.0998456363683,0.));
#170500=CARTESIAN_POINT('Ctrl Pts',(67.4172524429727,29.0996369822418,0.));
#170501=CARTESIAN_POINT('Ctrl Pts',(67.3908331857323,29.0994041438719,0.));
#170502=CARTESIAN_POINT('Ctrl Pts',(67.3644514770387,29.0991471719176,0.));
#170503=CARTESIAN_POINT('Ctrl Pts',(67.3381074112027,29.0988661172531,0.));
#170504=CARTESIAN_POINT('Ctrl Pts',(67.311801082792,29.0985610309771,0.));
#170505=CARTESIAN_POINT('Ctrl Pts',(67.2855325866517,29.0982319644277,0.));
#170506=CARTESIAN_POINT('Ctrl Pts',(67.2593020179209,29.0978789691962,0.));
#170507=CARTESIAN_POINT('Ctrl Pts',(67.2331094720471,29.097502097147,0.));
#170508=CARTESIAN_POINT('Ctrl Pts',(67.2069550447883,29.0971014004131,0.));
#170509=CARTESIAN_POINT('Ctrl Pts',(67.1808388322109,29.096676931389,0.));
#170510=CARTESIAN_POINT('Ctrl Pts',(67.1547609306843,29.0962287427273,0.));
#170511=CARTESIAN_POINT('Ctrl Pts',(67.1287214368746,29.0957568873358,0.));
#170512=CARTESIAN_POINT('Ctrl Pts',(67.1027204477311,29.0952614183779,0.));
#170513=CARTESIAN_POINT('Ctrl Pts',(67.0767580604879,29.0947423892727,0.));
#170514=CARTESIAN_POINT('Ctrl Pts',(67.0508343726776,29.0941998536959,0.));
#170515=CARTESIAN_POINT('Ctrl Pts',(67.0249494821363,29.0936338655828,0.));
#170516=CARTESIAN_POINT('Ctrl Pts',(66.9991034870083,29.0930444791328,0.));
#170517=CARTESIAN_POINT('Ctrl Pts',(66.9732964857466,29.092431748817,0.));
#170518=CARTESIAN_POINT('Ctrl Pts',(66.9475285771135,29.0917957293826,0.));
#170519=CARTESIAN_POINT('Ctrl Pts',(66.9217998601885,29.0911364758487,0.));
#170520=CARTESIAN_POINT('Ctrl Pts',(66.8961104343707,29.0904540435065,0.));
#170521=CARTESIAN_POINT('Ctrl Pts',(66.8704603993794,29.0897484879207,0.));
#170522=CARTESIAN_POINT('Ctrl Pts',(66.8448498552503,29.0890198649323,0.));
#170523=CARTESIAN_POINT('Ctrl Pts',(66.8192789023312,29.088268230663,0.));
#170524=CARTESIAN_POINT('Ctrl Pts',(66.793747641293,29.0874936415132,0.));
#170525=CARTESIAN_POINT('Ctrl Pts',(66.7682561731341,29.0866961541626,0.));
#170526=CARTESIAN_POINT('Ctrl Pts',(66.7428045991841,29.0858758255729,0.));
#170527=CARTESIAN_POINT('Ctrl Pts',(66.7173930211022,29.0850327129916,0.));
#170528=CARTESIAN_POINT('Ctrl Pts',(66.6920215408751,29.0841668739588,0.));
#170529=CARTESIAN_POINT('Ctrl Pts',(66.6666902608249,29.083278366305,0.));
#170530=CARTESIAN_POINT('Ctrl Pts',(66.6413992836147,29.0823672481507,0.));
#170531=CARTESIAN_POINT('Ctrl Pts',(66.6161487122502,29.0814335779084,0.));
#170532=CARTESIAN_POINT('Ctrl Pts',(66.59093865008,29.0804774142854,0.));
#170533=CARTESIAN_POINT('Ctrl Pts',(66.5657692007906,29.0794988162897,0.));
#170534=CARTESIAN_POINT('Ctrl Pts',(66.5406404684132,29.0784978432301,0.));
#170535=CARTESIAN_POINT('Ctrl Pts',(66.5155525573323,29.0774745547152,0.));
#170536=CARTESIAN_POINT('Ctrl Pts',(66.4905055722868,29.0764290106554,0.));
#170537=CARTESIAN_POINT('Ctrl Pts',(66.4654996183731,29.0753612712666,0.));
#170538=CARTESIAN_POINT('Ctrl Pts',(66.4405348010388,29.0742713970755,0.));
#170539=CARTESIAN_POINT('Ctrl Pts',(66.4156112260887,29.0731594489211,0.));
#170540=CARTESIAN_POINT('Ctrl Pts',(66.3907289996932,29.072025487953,0.));
#170541=CARTESIAN_POINT('Ctrl Pts',(66.3658882283903,29.0708695756334,0.));
#170542=CARTESIAN_POINT('Ctrl Pts',(66.3410890190884,29.0696917737399,0.));
#170543=CARTESIAN_POINT('Ctrl Pts',(66.3163314790615,29.0684921443721,0.));
#170544=CARTESIAN_POINT('Ctrl Pts',(66.2916157159536,29.067270749953,0.));
#170545=CARTESIAN_POINT('Ctrl Pts',(66.2669418377871,29.0660276532274,0.));
#170546=CARTESIAN_POINT('Ctrl Pts',(66.2423099529669,29.0647629172645,0.));
#170547=CARTESIAN_POINT('Ctrl Pts',(66.2177201702818,29.0634766054598,0.));
#170548=CARTESIAN_POINT('Ctrl Pts',(66.1931725989008,29.062168781542,0.));
#170549=CARTESIAN_POINT('Ctrl Pts',(66.1686673483757,29.0608395095747,0.));
#170550=CARTESIAN_POINT('Ctrl Pts',(66.144204528652,29.0594888539558,0.));
#170551=CARTESIAN_POINT('Ctrl Pts',(66.1197842500714,29.0581168794191,0.));
#170552=CARTESIAN_POINT('Ctrl Pts',(66.0954066233752,29.0567236510372,0.));
#170553=CARTESIAN_POINT('Ctrl Pts',(66.0710717597003,29.0553092342275,0.));
#170554=CARTESIAN_POINT('Ctrl Pts',(66.0467797705806,29.0538736947547,0.));
#170555=CARTESIAN_POINT('Ctrl Pts',(66.0225307679584,29.0524170987303,0.));
#170556=CARTESIAN_POINT('Ctrl Pts',(65.9983248641877,29.0509395126141,0.));
#170557=CARTESIAN_POINT('Ctrl Pts',(65.9741621720372,29.0494410032173,0.));
#170558=CARTESIAN_POINT('Ctrl Pts',(65.9500428046873,29.0479216377082,0.));
#170559=CARTESIAN_POINT('Ctrl Pts',(65.9259668757309,29.0463814836159,0.));
#170560=CARTESIAN_POINT('Ctrl Pts',(65.9019344991854,29.0448206088288,0.));
#170561=CARTESIAN_POINT('Ctrl Pts',(65.8779457894959,29.0432390815977,0.));
#170562=CARTESIAN_POINT('Ctrl Pts',(65.854000861539,29.0416369705375,0.));
#170563=CARTESIAN_POINT('Ctrl Pts',(65.8300998306198,29.0400143446341,0.));
#170564=CARTESIAN_POINT('Ctrl Pts',(65.8062428124723,29.0383712732473,0.));
#170565=CARTESIAN_POINT('Ctrl Pts',(65.7824299232715,29.0367078261107,0.));
#170566=CARTESIAN_POINT('Ctrl Pts',(65.7586612796375,29.0350240733333,0.));
#170567=CARTESIAN_POINT('Ctrl Pts',(65.7349369986382,29.0333200854026,0.));
#170568=CARTESIAN_POINT('Ctrl Pts',(65.7112571977874,29.0315959331911,0.));
#170569=CARTESIAN_POINT('Ctrl Pts',(65.6876219950465,29.0298516879599,0.));
#170570=CARTESIAN_POINT('Ctrl Pts',(65.664031508836,29.0280874213584,0.));
#170571=CARTESIAN_POINT('Ctrl Pts',(65.6404858580391,29.0263032054261,0.));
#170572=CARTESIAN_POINT('Ctrl Pts',(65.6169851620054,29.0244991125962,0.));
#170573=CARTESIAN_POINT('Ctrl Pts',(65.593529540548,29.0226752157013,0.));
#170574=CARTESIAN_POINT('Ctrl Pts',(65.5701191139455,29.0208315879778,0.));
#170575=CARTESIAN_POINT('Ctrl Pts',(65.5467540029546,29.0189683030654,0.));
#170576=CARTESIAN_POINT('Ctrl Pts',(65.523434328815,29.01708543501,0.));
#170577=CARTESIAN_POINT('Ctrl Pts',(65.5001602132524,29.015183058267,0.));
#170578=CARTESIAN_POINT('Ctrl Pts',(65.4769317784754,29.0132612477075,0.));
#170579=CARTESIAN_POINT('Ctrl Pts',(65.4537491471782,29.0113200786219,0.));
#170580=CARTESIAN_POINT('Ctrl Pts',(65.4306124425524,29.0093596267198,0.));
#170581=CARTESIAN_POINT('Ctrl Pts',(65.4075217882921,29.0073799681336,0.));
#170582=CARTESIAN_POINT('Ctrl Pts',(65.3844773085976,29.0053811794214,0.));
#170583=CARTESIAN_POINT('Ctrl Pts',(65.3614791281725,29.0033633375745,0.));
#170584=CARTESIAN_POINT('Ctrl Pts',(65.3385273722278,29.0013265200201,0.));
#170585=CARTESIAN_POINT('Ctrl Pts',(65.3156221664942,28.9992708046223,0.));
#170586=CARTESIAN_POINT('Ctrl Pts',(65.2927636372261,28.9971962696848,0.));
#170587=CARTESIAN_POINT('Ctrl Pts',(65.2699519112052,28.9951029939551,0.));
#170588=CARTESIAN_POINT('Ctrl Pts',(65.2471871157375,28.9929910566314,0.));
#170589=CARTESIAN_POINT('Ctrl Pts',(65.2244693786586,28.9908605373652,0.));
#170590=CARTESIAN_POINT('Ctrl Pts',(65.2017988283465,28.9887115162626,0.));
#170591=CARTESIAN_POINT('Ctrl Pts',(65.1791755937254,28.9865440738882,0.));
#170592=CARTESIAN_POINT('Ctrl Pts',(65.1565998042705,28.9843582912697,0.));
#170593=CARTESIAN_POINT('Ctrl Pts',(65.1340715900042,28.9821542499049,0.));
#170594=CARTESIAN_POINT('Ctrl Pts',(65.111591081505,28.9799320317648,0.));
#170595=CARTESIAN_POINT('Ctrl Pts',(65.0891584099174,28.9776917192936,0.));
#170596=CARTESIAN_POINT('Ctrl Pts',(65.0667737069562,28.9754333954134,0.));
#170597=CARTESIAN_POINT('Ctrl Pts',(65.0444371049082,28.9731571435281,0.));
#170598=CARTESIAN_POINT('Ctrl Pts',(65.0221487366279,28.9708630475298,0.));
#170599=CARTESIAN_POINT('Ctrl Pts',(64.9999087355504,28.9685511918017,0.));
#170600=CARTESIAN_POINT('Ctrl Pts',(64.9777172357028,28.9662216612216,0.));
#170601=CARTESIAN_POINT('Ctrl Pts',(64.955574371711,28.9638745411677,0.));
#170602=CARTESIAN_POINT('Ctrl Pts',(64.9334802788037,28.961509917525,0.));
#170603=CARTESIAN_POINT('Ctrl Pts',(64.9114350928124,28.9591278766934,0.));
#170604=CARTESIAN_POINT('Ctrl Pts',(64.8894389501799,28.9567285055866,0.));
#170605=CARTESIAN_POINT('Ctrl Pts',(64.8674919879646,28.9543118916327,0.));
#170606=CARTESIAN_POINT('Ctrl Pts',(64.8455943438423,28.9518781227765,0.));
#170607=CARTESIAN_POINT('Ctrl Pts',(64.8237461561024,28.9494272874833,0.));
#170608=CARTESIAN_POINT('Ctrl Pts',(64.8019475636454,28.9469594747436,0.));
#170609=CARTESIAN_POINT('Ctrl Pts',(64.7801987060097,28.9444747740815,0.));
#170610=CARTESIAN_POINT('Ctrl Pts',(64.7584997233889,28.9419732755659,0.));
#170611=CARTESIAN_POINT('Ctrl Pts',(64.7368507566461,28.9394550698201,0.));
#170612=CARTESIAN_POINT('Ctrl Pts',(64.715251947327,28.9369202480383,0.));
#170613=CARTESIAN_POINT('Ctrl Pts',(64.6937034376591,28.934368901987,0.));
#170614=CARTESIAN_POINT('Ctrl Pts',(64.6722053705389,28.9318011239905,0.));
#170615=CARTESIAN_POINT('Ctrl Pts',(64.6507578895155,28.9292170069219,0.));
#170616=CARTESIAN_POINT('Ctrl Pts',(64.6293611387753,28.9266166441956,0.));
#170617=CARTESIAN_POINT('Ctrl Pts',(64.6080152631065,28.9240001297553,0.));
#170618=CARTESIAN_POINT('Ctrl Pts',(64.5867204079452,28.9213675580996,0.));
#170619=CARTESIAN_POINT('Ctrl Pts',(64.5654767194487,28.9187190243231,0.));
#170620=CARTESIAN_POINT('Ctrl Pts',(64.544284344556,28.9160546241538,0.));
#170621=CARTESIAN_POINT('Ctrl Pts',(64.5231434310457,28.9133744539943,0.));
#170622=CARTESIAN_POINT('Ctrl Pts',(64.5020541275927,28.9106786109639,0.));
#170623=CARTESIAN_POINT('Ctrl Pts',(64.4810165836568,28.9079671928253,0.));
#170624=CARTESIAN_POINT('Ctrl Pts',(64.460030949357,28.9052402979055,0.));
#170625=CARTESIAN_POINT('Ctrl Pts',(64.439097375364,28.9024980250309,0.));
#170626=CARTESIAN_POINT('Ctrl Pts',(64.41821601274,28.899740473435,0.));
#170627=CARTESIAN_POINT('Ctrl Pts',(64.3973870129201,28.8969677427519,0.));
#170628=CARTESIAN_POINT('Ctrl Pts',(64.3766105280715,28.8941799332312,0.));
#170629=CARTESIAN_POINT('Ctrl Pts',(64.3558867114087,28.8913771459327,0.));
#170630=CARTESIAN_POINT('Ctrl Pts',(64.3352157174606,28.888559482892,0.));
#170631=CARTESIAN_POINT('Ctrl Pts',(64.3145977025005,28.8857270473944,0.));
#170632=CARTESIAN_POINT('Ctrl Pts',(64.2940328242482,28.8828799437922,0.));
#170633=CARTESIAN_POINT('Ctrl Pts',(64.2735212410682,28.8800182770052,0.));
#170634=CARTESIAN_POINT('Ctrl Pts',(64.2530631112926,28.8771421521058,0.));
#170635=CARTESIAN_POINT('Ctrl Pts',(64.232658592528,28.8742516738959,0.));
#170636=CARTESIAN_POINT('Ctrl Pts',(64.2123078408507,28.8713469464205,0.));
#170637=CARTESIAN_POINT('Ctrl Pts',(64.1920110123342,28.8684280739033,0.));
#170638=CARTESIAN_POINT('Ctrl Pts',(64.1717682648708,28.8654951618659,0.));
#170639=CARTESIAN_POINT('Ctrl Pts',(64.1515797596555,28.8625483180433,0.));
#170640=CARTESIAN_POINT('Ctrl Pts',(64.1314456633345,28.8595876537132,0.));
#170641=CARTESIAN_POINT('Ctrl Pts',(64.1113661481918,28.8566132838157,0.));
#170642=CARTESIAN_POINT('Ctrl Pts',(64.0913413876586,28.8536253241837,0.));
#170643=CARTESIAN_POINT('Ctrl Pts',(64.0713715523588,28.8506238891087,0.));
#170644=CARTESIAN_POINT('Ctrl Pts',(64.0514568066659,28.8476090892242,0.));
#170645=CARTESIAN_POINT('Ctrl Pts',(64.0315973031994,28.8445810281275,0.));
#170646=CARTESIAN_POINT('Ctrl Pts',(64.0117931881364,28.841539805646,0.));
#170647=CARTESIAN_POINT('Ctrl Pts',(63.9920446117632,28.8384855243267,0.));
#170648=CARTESIAN_POINT('Ctrl Pts',(63.9723517369614,28.8354182946601,0.));
#170649=CARTESIAN_POINT('Ctrl Pts',(63.9527147494351,28.8323382413753,0.));
#170650=CARTESIAN_POINT('Ctrl Pts',(63.9331338646868,28.8292455077494,0.));
#170651=CARTESIAN_POINT('Ctrl Pts',(63.9136093063647,28.826140242322,0.));
#170652=CARTESIAN_POINT('Ctrl Pts',(63.894141285685,28.8230225863142,0.));
#170653=CARTESIAN_POINT('Ctrl Pts',(63.8747299825383,28.8198926619893,0.));
#170654=CARTESIAN_POINT('Ctrl Pts',(63.8553755207732,28.8167505576806,0.));
#170655=CARTESIAN_POINT('Ctrl Pts',(63.8360779670225,28.8135963263557,0.));
#170656=CARTESIAN_POINT('Ctrl Pts',(63.8206854735372,28.8110632621133,0.));
#170657=CARTESIAN_POINT('Ctrl Pts',(63.809166727145,28.8091580239664,0.));
#170658=CARTESIAN_POINT('Ctrl Pts',(63.8014989507575,28.8078854475473,0.));
#170659=CARTESIAN_POINT('Ctrl Pts',(63.7976679095314,28.8072485549236,0.));
#170660=CARTESIAN_POINT('Ctrl Pts',(70.8615414811571,22.9976507259816,0.));
#170661=CARTESIAN_POINT('Ctrl Pts',(70.8615414811571,22.9976507259816,12.));
#170662=CARTESIAN_POINT('Ctrl Pts',(70.8559846928,22.9983100639391,0.));
#170663=CARTESIAN_POINT('Ctrl Pts',(70.8559846928,22.9983100639391,12.));
#170664=CARTESIAN_POINT('Ctrl Pts',(70.8448742696689,22.9996258555291,0.));
#170665=CARTESIAN_POINT('Ctrl Pts',(70.8448742696689,22.9996258555291,12.));
#170666=CARTESIAN_POINT('Ctrl Pts',(70.8282180957225,23.0015908899394,0.));
#170667=CARTESIAN_POINT('Ctrl Pts',(70.8282180957225,23.0015908899394,12.));
#170668=CARTESIAN_POINT('Ctrl Pts',(70.8060287860585,23.0041936291626,0.));
#170669=CARTESIAN_POINT('Ctrl Pts',(70.8060287860585,23.0041936291626,12.));
#170670=CARTESIAN_POINT('Ctrl Pts',(70.7783236951202,23.0074182063787,0.));
#170671=CARTESIAN_POINT('Ctrl Pts',(70.7783236951202,23.0074182063787,12.));
#170672=CARTESIAN_POINT('Ctrl Pts',(70.750650169619,23.0106139366046,0.));
#170673=CARTESIAN_POINT('Ctrl Pts',(70.750650169619,23.0106139366046,12.));
#170674=CARTESIAN_POINT('Ctrl Pts',(70.7230082425412,23.0137808248924,0.));
#170675=CARTESIAN_POINT('Ctrl Pts',(70.7230082425412,23.0137808248924,12.));
#170676=CARTESIAN_POINT('Ctrl Pts',(70.6953979633426,23.0169188841045,0.));
#170677=CARTESIAN_POINT('Ctrl Pts',(70.6953979633426,23.0169188841045,12.));
#170678=CARTESIAN_POINT('Ctrl Pts',(70.6678194023135,23.0200281385833,0.));
#170679=CARTESIAN_POINT('Ctrl Pts',(70.6678194023135,23.0200281385833,12.));
#170680=CARTESIAN_POINT('Ctrl Pts',(70.6402726486453,23.0231086235186,0.));
#170681=CARTESIAN_POINT('Ctrl Pts',(70.6402726486453,23.0231086235186,12.));
#170682=CARTESIAN_POINT('Ctrl Pts',(70.6127578036673,23.026160381013,0.));
#170683=CARTESIAN_POINT('Ctrl Pts',(70.6127578036673,23.026160381013,12.));
#170684=CARTESIAN_POINT('Ctrl Pts',(70.5852749754082,23.0291834570663,0.));
#170685=CARTESIAN_POINT('Ctrl Pts',(70.5852749754082,23.0291834570663,12.));
#170686=CARTESIAN_POINT('Ctrl Pts',(70.5578242727627,23.0321778982711,0.));
#170687=CARTESIAN_POINT('Ctrl Pts',(70.5578242727627,23.0321778982711,12.));
#170688=CARTESIAN_POINT('Ctrl Pts',(70.5304057994631,23.0351437484336,0.));
#170689=CARTESIAN_POINT('Ctrl Pts',(70.5304057994631,23.0351437484336,12.));
#170690=CARTESIAN_POINT('Ctrl Pts',(70.5030196492003,23.0380810458271,0.));
#170691=CARTESIAN_POINT('Ctrl Pts',(70.5030196492003,23.0380810458271,12.));
#170692=CARTESIAN_POINT('Ctrl Pts',(70.4756659090209,23.0409898250756,0.));
#170693=CARTESIAN_POINT('Ctrl Pts',(70.4756659090209,23.0409898250756,12.));
#170694=CARTESIAN_POINT('Ctrl Pts',(70.4483446617614,23.0438701185013,0.));
#170695=CARTESIAN_POINT('Ctrl Pts',(70.4483446617614,23.0438701185013,12.));
#170696=CARTESIAN_POINT('Ctrl Pts',(70.4210559889348,23.0467219577291,0.));
#170697=CARTESIAN_POINT('Ctrl Pts',(70.4210559889348,23.0467219577291,12.));
#170698=CARTESIAN_POINT('Ctrl Pts',(70.3937999732267,23.0495453750763,0.));
#170699=CARTESIAN_POINT('Ctrl Pts',(70.3937999732267,23.0495453750763,12.));
#170700=CARTESIAN_POINT('Ctrl Pts',(70.3665767016542,23.0523404053172,0.));
#170701=CARTESIAN_POINT('Ctrl Pts',(70.3665767016542,23.0523404053172,12.));
#170702=CARTESIAN_POINT('Ctrl Pts',(70.3393862652297,23.0551070854926,0.));
#170703=CARTESIAN_POINT('Ctrl Pts',(70.3393862652297,23.0551070854926,12.));
#170704=CARTESIAN_POINT('Ctrl Pts',(70.3122287575335,23.0578454541104,0.));
#170705=CARTESIAN_POINT('Ctrl Pts',(70.3122287575335,23.0578454541104,12.));
#170706=CARTESIAN_POINT('Ctrl Pts',(70.2851042736066,23.0605555505321,0.));
#170707=CARTESIAN_POINT('Ctrl Pts',(70.2851042736066,23.0605555505321,12.));
#170708=CARTESIAN_POINT('Ctrl Pts',(70.2580129087888,23.0632374143279,0.));
#170709=CARTESIAN_POINT('Ctrl Pts',(70.2580129087888,23.0632374143279,12.));
#170710=CARTESIAN_POINT('Ctrl Pts',(70.2309547573815,23.0658910845433,0.));
#170711=CARTESIAN_POINT('Ctrl Pts',(70.2309547573815,23.0658910845433,12.));
#170712=CARTESIAN_POINT('Ctrl Pts',(70.2039299120488,23.0685165993691,0.));
#170713=CARTESIAN_POINT('Ctrl Pts',(70.2039299120488,23.0685165993691,12.));
#170714=CARTESIAN_POINT('Ctrl Pts',(70.1769384645586,23.071113996544,0.));
#170715=CARTESIAN_POINT('Ctrl Pts',(70.1769384645586,23.071113996544,12.));
#170716=CARTESIAN_POINT('Ctrl Pts',(70.1499805062172,23.0736833135938,0.));
#170717=CARTESIAN_POINT('Ctrl Pts',(70.1499805062172,23.0736833135938,12.));
#170718=CARTESIAN_POINT('Ctrl Pts',(70.123056128422,23.0762245881389,0.));
#170719=CARTESIAN_POINT('Ctrl Pts',(70.123056128422,23.0762245881389,12.));
#170720=CARTESIAN_POINT('Ctrl Pts',(70.0961654231639,23.0787378581774,0.));
#170721=CARTESIAN_POINT('Ctrl Pts',(70.0961654231639,23.0787378581774,12.));
#170722=CARTESIAN_POINT('Ctrl Pts',(70.0693084835373,23.0812231623765,0.));
#170723=CARTESIAN_POINT('Ctrl Pts',(70.0693084835373,23.0812231623765,12.));
#170724=CARTESIAN_POINT('Ctrl Pts',(70.0424854035115,23.0836805399374,0.));
#170725=CARTESIAN_POINT('Ctrl Pts',(70.0424854035115,23.0836805399374,12.));
#170726=CARTESIAN_POINT('Ctrl Pts',(70.0156962777169,23.0861100304729,0.));
#170727=CARTESIAN_POINT('Ctrl Pts',(70.0156962777169,23.0861100304729,12.));
#170728=CARTESIAN_POINT('Ctrl Pts',(69.9889412012143,23.0885116738798,0.));
#170729=CARTESIAN_POINT('Ctrl Pts',(69.9889412012143,23.0885116738798,12.));
#170730=CARTESIAN_POINT('Ctrl Pts',(69.9622202692873,23.0908855102251,0.));
#170731=CARTESIAN_POINT('Ctrl Pts',(69.9622202692873,23.0908855102251,12.));
#170732=CARTESIAN_POINT('Ctrl Pts',(69.9355335771729,23.0932315796068,0.));
#170733=CARTESIAN_POINT('Ctrl Pts',(69.9355335771729,23.0932315796068,12.));
#170734=CARTESIAN_POINT('Ctrl Pts',(69.9088812200713,23.0955499221558,0.));
#170735=CARTESIAN_POINT('Ctrl Pts',(69.9088812200713,23.0955499221558,12.));
#170736=CARTESIAN_POINT('Ctrl Pts',(69.8822632932768,23.0978405781021,0.));
#170737=CARTESIAN_POINT('Ctrl Pts',(69.8822632932768,23.0978405781021,12.));
#170738=CARTESIAN_POINT('Ctrl Pts',(69.8556798922693,23.1001035878241,0.));
#170739=CARTESIAN_POINT('Ctrl Pts',(69.8556798922693,23.1001035878241,12.));
#170740=CARTESIAN_POINT('Ctrl Pts',(69.8291311128118,23.1023389919051,0.));
#170741=CARTESIAN_POINT('Ctrl Pts',(69.8291311128118,23.1023389919051,12.));
#170742=CARTESIAN_POINT('Ctrl Pts',(69.8026170510572,23.1045468311991,0.));
#170743=CARTESIAN_POINT('Ctrl Pts',(69.8026170510572,23.1045468311991,12.));
#170744=CARTESIAN_POINT('Ctrl Pts',(69.7761378035964,23.106727146861,0.));
#170745=CARTESIAN_POINT('Ctrl Pts',(69.7761378035964,23.106727146861,12.));
#170746=CARTESIAN_POINT('Ctrl Pts',(69.7496934674069,23.1088799803089,0.));
#170747=CARTESIAN_POINT('Ctrl Pts',(69.7496934674069,23.1088799803089,12.));
#170748=CARTESIAN_POINT('Ctrl Pts',(69.7232841398197,23.1110053732046,0.));
#170749=CARTESIAN_POINT('Ctrl Pts',(69.7232841398197,23.1110053732046,12.));
#170750=CARTESIAN_POINT('Ctrl Pts',(69.6969099184767,23.1131033674301,0.));
#170751=CARTESIAN_POINT('Ctrl Pts',(69.6969099184767,23.1131033674301,12.));
#170752=CARTESIAN_POINT('Ctrl Pts',(69.6705709012852,23.1151740050681,0.));
#170753=CARTESIAN_POINT('Ctrl Pts',(69.6705709012852,23.1151740050681,12.));
#170754=CARTESIAN_POINT('Ctrl Pts',(69.6442671863765,23.1172173283859,0.));
#170755=CARTESIAN_POINT('Ctrl Pts',(69.6442671863765,23.1172173283859,12.));
#170756=CARTESIAN_POINT('Ctrl Pts',(69.6179988721365,23.1192333798441,0.));
#170757=CARTESIAN_POINT('Ctrl Pts',(69.6179988721365,23.1192333798441,12.));
#170758=CARTESIAN_POINT('Ctrl Pts',(69.5917660572265,23.1212222021051,0.));
#170759=CARTESIAN_POINT('Ctrl Pts',(69.5917660572265,23.1212222021051,12.));
#170760=CARTESIAN_POINT('Ctrl Pts',(69.5655688406052,23.1231838380452,0.));
#170761=CARTESIAN_POINT('Ctrl Pts',(69.5655688406052,23.1231838380452,12.));
#170762=CARTESIAN_POINT('Ctrl Pts',(69.539407321546,23.1251183307676,0.));
#170763=CARTESIAN_POINT('Ctrl Pts',(69.539407321546,23.1251183307676,12.));
#170764=CARTESIAN_POINT('Ctrl Pts',(69.5132815996537,23.1270257236204,0.));
#170765=CARTESIAN_POINT('Ctrl Pts',(69.5132815996537,23.1270257236204,12.));
#170766=CARTESIAN_POINT('Ctrl Pts',(69.4871917748654,23.1289060601924,0.));
#170767=CARTESIAN_POINT('Ctrl Pts',(69.4871917748654,23.1289060601924,12.));
#170768=CARTESIAN_POINT('Ctrl Pts',(69.4611379474484,23.1307593843061,0.));
#170769=CARTESIAN_POINT('Ctrl Pts',(69.4611379474484,23.1307593843061,12.));
#170770=CARTESIAN_POINT('Ctrl Pts',(69.4351202179946,23.1325857400144,0.));
#170771=CARTESIAN_POINT('Ctrl Pts',(69.4351202179946,23.1325857400144,12.));
#170772=CARTESIAN_POINT('Ctrl Pts',(69.4091386874132,23.1343851715989,0.));
#170773=CARTESIAN_POINT('Ctrl Pts',(69.4091386874132,23.1343851715989,12.));
#170774=CARTESIAN_POINT('Ctrl Pts',(69.3831934569182,23.1361577235709,0.));
#170775=CARTESIAN_POINT('Ctrl Pts',(69.3831934569182,23.1361577235709,12.));
#170776=CARTESIAN_POINT('Ctrl Pts',(69.3572846280297,23.1379034406718,0.));
#170777=CARTESIAN_POINT('Ctrl Pts',(69.3572846280297,23.1379034406718,12.));
#170778=CARTESIAN_POINT('Ctrl Pts',(69.3314123025869,23.1396223678725,0.));
#170779=CARTESIAN_POINT('Ctrl Pts',(69.3314123025869,23.1396223678725,12.));
#170780=CARTESIAN_POINT('Ctrl Pts',(69.3055765827546,23.1413145503762,0.));
#170781=CARTESIAN_POINT('Ctrl Pts',(69.3055765827546,23.1413145503762,12.));
#170782=CARTESIAN_POINT('Ctrl Pts',(69.2797775710273,23.142980033622,0.));
#170783=CARTESIAN_POINT('Ctrl Pts',(69.2797775710273,23.142980033622,12.));
#170784=CARTESIAN_POINT('Ctrl Pts',(69.254015370231,23.1446188632931,0.));
#170785=CARTESIAN_POINT('Ctrl Pts',(69.254015370231,23.1446188632931,12.));
#170786=CARTESIAN_POINT('Ctrl Pts',(69.2282900835235,23.1462310853206,0.));
#170787=CARTESIAN_POINT('Ctrl Pts',(69.2282900835235,23.1462310853206,12.));
#170788=CARTESIAN_POINT('Ctrl Pts',(69.2026018144028,23.147816745879,0.));
#170789=CARTESIAN_POINT('Ctrl Pts',(69.2026018144028,23.147816745879,12.));
#170790=CARTESIAN_POINT('Ctrl Pts',(69.1769506667084,23.1493758913859,0.));
#170791=CARTESIAN_POINT('Ctrl Pts',(69.1769506667084,23.1493758913859,12.));
#170792=CARTESIAN_POINT('Ctrl Pts',(69.1513367446231,23.1509085685032,0.));
#170793=CARTESIAN_POINT('Ctrl Pts',(69.1513367446231,23.1509085685032,12.));
#170794=CARTESIAN_POINT('Ctrl Pts',(69.1257601526687,23.152414824141,0.));
#170795=CARTESIAN_POINT('Ctrl Pts',(69.1257601526687,23.152414824141,12.));
#170796=CARTESIAN_POINT('Ctrl Pts',(69.1002209957025,23.1538947054615,0.));
#170797=CARTESIAN_POINT('Ctrl Pts',(69.1002209957025,23.1538947054615,12.));
#170798=CARTESIAN_POINT('Ctrl Pts',(69.074719378928,23.1553482598762,0.));
#170799=CARTESIAN_POINT('Ctrl Pts',(69.074719378928,23.1553482598762,12.));
#170800=CARTESIAN_POINT('Ctrl Pts',(69.0492554078992,23.1567755350469,0.));
#170801=CARTESIAN_POINT('Ctrl Pts',(69.0492554078992,23.1567755350469,12.));
#170802=CARTESIAN_POINT('Ctrl Pts',(69.0238291885245,23.1581765788869,0.));
#170803=CARTESIAN_POINT('Ctrl Pts',(69.0238291885245,23.1581765788869,12.));
#170804=CARTESIAN_POINT('Ctrl Pts',(68.9984408270659,23.1595514395656,0.));
#170805=CARTESIAN_POINT('Ctrl Pts',(68.9984408270659,23.1595514395656,12.));
#170806=CARTESIAN_POINT('Ctrl Pts',(68.9730904301369,23.1609001655156,0.));
#170807=CARTESIAN_POINT('Ctrl Pts',(68.9730904301369,23.1609001655156,12.));
#170808=CARTESIAN_POINT('Ctrl Pts',(68.9477781047106,23.1622228054291,0.));
#170809=CARTESIAN_POINT('Ctrl Pts',(68.9477781047106,23.1622228054291,12.));
#170810=CARTESIAN_POINT('Ctrl Pts',(68.9225039581248,23.1635194082581,0.));
#170811=CARTESIAN_POINT('Ctrl Pts',(68.9225039581248,23.1635194082581,12.));
#170812=CARTESIAN_POINT('Ctrl Pts',(68.8972680980842,23.164790023215,0.));
#170813=CARTESIAN_POINT('Ctrl Pts',(68.8972680980842,23.164790023215,12.));
#170814=CARTESIAN_POINT('Ctrl Pts',(68.8720706326609,23.1660346997764,0.));
#170815=CARTESIAN_POINT('Ctrl Pts',(68.8720706326609,23.1660346997764,12.));
#170816=CARTESIAN_POINT('Ctrl Pts',(68.8469116702898,23.1672534876889,0.));
#170817=CARTESIAN_POINT('Ctrl Pts',(68.8469116702898,23.1672534876889,12.));
#170818=CARTESIAN_POINT('Ctrl Pts',(68.8217913197752,23.1684464369686,0.));
#170819=CARTESIAN_POINT('Ctrl Pts',(68.8217913197752,23.1684464369686,12.));
#170820=CARTESIAN_POINT('Ctrl Pts',(68.7967096902996,23.1696135978997,0.));
#170821=CARTESIAN_POINT('Ctrl Pts',(68.7967096902996,23.1696135978997,12.));
#170822=CARTESIAN_POINT('Ctrl Pts',(68.771666891425,23.170755021036,0.));
#170823=CARTESIAN_POINT('Ctrl Pts',(68.771666891425,23.170755021036,12.));
#170824=CARTESIAN_POINT('Ctrl Pts',(68.746663033096,23.1718707572043,0.));
#170825=CARTESIAN_POINT('Ctrl Pts',(68.746663033096,23.1718707572043,12.));
#170826=CARTESIAN_POINT('Ctrl Pts',(68.7216982256341,23.172960857511,0.));
#170827=CARTESIAN_POINT('Ctrl Pts',(68.7216982256341,23.172960857511,12.));
#170828=CARTESIAN_POINT('Ctrl Pts',(68.696772579744,23.1740253733417,0.));
#170829=CARTESIAN_POINT('Ctrl Pts',(68.696772579744,23.1740253733417,12.));
#170830=CARTESIAN_POINT('Ctrl Pts',(68.6718862065216,23.1750643563602,0.));
#170831=CARTESIAN_POINT('Ctrl Pts',(68.6718862065216,23.1750643563602,12.));
#170832=CARTESIAN_POINT('Ctrl Pts',(68.6470392174564,23.1760778585092,0.));
#170833=CARTESIAN_POINT('Ctrl Pts',(68.6470392174564,23.1760778585092,12.));
#170834=CARTESIAN_POINT('Ctrl Pts',(68.6222317244341,23.1770659320138,0.));
#170835=CARTESIAN_POINT('Ctrl Pts',(68.6222317244341,23.1770659320138,12.));
#170836=CARTESIAN_POINT('Ctrl Pts',(68.597463839733,23.1780286293875,0.));
#170837=CARTESIAN_POINT('Ctrl Pts',(68.597463839733,23.1780286293875,12.));
#170838=CARTESIAN_POINT('Ctrl Pts',(68.5727356760278,23.1789660034342,0.));
#170839=CARTESIAN_POINT('Ctrl Pts',(68.5727356760278,23.1789660034342,12.));
#170840=CARTESIAN_POINT('Ctrl Pts',(68.5480473463985,23.179878107245,0.));
#170841=CARTESIAN_POINT('Ctrl Pts',(68.5480473463985,23.179878107245,12.));
#170842=CARTESIAN_POINT('Ctrl Pts',(68.5233989643345,23.180764994201,0.));
#170843=CARTESIAN_POINT('Ctrl Pts',(68.5233989643345,23.180764994201,12.));
#170844=CARTESIAN_POINT('Ctrl Pts',(68.4987906437356,23.1816267179751,0.));
#170845=CARTESIAN_POINT('Ctrl Pts',(68.4987906437356,23.1816267179751,12.));
#170846=CARTESIAN_POINT('Ctrl Pts',(68.4742224989098,23.1824633325385,0.));
#170847=CARTESIAN_POINT('Ctrl Pts',(68.4742224989098,23.1824633325385,12.));
#170848=CARTESIAN_POINT('Ctrl Pts',(68.4496946445758,23.183274892163,0.));
#170849=CARTESIAN_POINT('Ctrl Pts',(68.4496946445758,23.183274892163,12.));
#170850=CARTESIAN_POINT('Ctrl Pts',(68.4252071958729,23.1840614514192,0.));
#170851=CARTESIAN_POINT('Ctrl Pts',(68.4252071958729,23.1840614514192,12.));
#170852=CARTESIAN_POINT('Ctrl Pts',(68.4007602683652,23.1848230651776,0.));
#170853=CARTESIAN_POINT('Ctrl Pts',(68.4007602683652,23.1848230651776,12.));
#170854=CARTESIAN_POINT('Ctrl Pts',(68.376353978044,23.1855597886116,0.));
#170855=CARTESIAN_POINT('Ctrl Pts',(68.376353978044,23.1855597886116,12.));
#170856=CARTESIAN_POINT('Ctrl Pts',(68.3519884413246,23.1862716772031,0.));
#170857=CARTESIAN_POINT('Ctrl Pts',(68.3519884413246,23.1862716772031,12.));
#170858=CARTESIAN_POINT('Ctrl Pts',(68.3276637750485,23.1869587867459,0.));
#170859=CARTESIAN_POINT('Ctrl Pts',(68.3276637750485,23.1869587867459,12.));
#170860=CARTESIAN_POINT('Ctrl Pts',(68.3033800964939,23.1876211733436,0.));
#170861=CARTESIAN_POINT('Ctrl Pts',(68.3033800964939,23.1876211733436,12.));
#170862=CARTESIAN_POINT('Ctrl Pts',(68.2791375233795,23.1882588934107,0.));
#170863=CARTESIAN_POINT('Ctrl Pts',(68.2791375233795,23.1882588934107,12.));
#170864=CARTESIAN_POINT('Ctrl Pts',(68.2549361738681,23.1888720036757,0.));
#170865=CARTESIAN_POINT('Ctrl Pts',(68.2549361738681,23.1888720036757,12.));
#170866=CARTESIAN_POINT('Ctrl Pts',(68.2307761665633,23.1894605611871,0.));
#170867=CARTESIAN_POINT('Ctrl Pts',(68.2307761665633,23.1894605611871,12.));
#170868=CARTESIAN_POINT('Ctrl Pts',(68.2066576205116,23.1900246233165,0.));
#170869=CARTESIAN_POINT('Ctrl Pts',(68.2066576205116,23.1900246233165,12.));
#170870=CARTESIAN_POINT('Ctrl Pts',(68.1825806552129,23.1905642477571,0.));
#170871=CARTESIAN_POINT('Ctrl Pts',(68.1825806552129,23.1905642477571,12.));
#170872=CARTESIAN_POINT('Ctrl Pts',(68.1585453906257,23.1910794925251,0.));
#170873=CARTESIAN_POINT('Ctrl Pts',(68.1585453906257,23.1910794925251,12.));
#170874=CARTESIAN_POINT('Ctrl Pts',(68.1345519471695,23.1915704159623,0.));
#170875=CARTESIAN_POINT('Ctrl Pts',(68.1345519471695,23.1915704159623,12.));
#170876=CARTESIAN_POINT('Ctrl Pts',(68.110600445723,23.1920370767426,0.));
#170877=CARTESIAN_POINT('Ctrl Pts',(68.110600445723,23.1920370767426,12.));
#170878=CARTESIAN_POINT('Ctrl Pts',(68.0866910076251,23.1924795338749,0.));
#170879=CARTESIAN_POINT('Ctrl Pts',(68.0866910076251,23.1924795338749,12.));
#170880=CARTESIAN_POINT('Ctrl Pts',(68.0628237546863,23.1928978467021,0.));
#170881=CARTESIAN_POINT('Ctrl Pts',(68.0628237546863,23.1928978467021,12.));
#170882=CARTESIAN_POINT('Ctrl Pts',(68.0389988091933,23.1932920749023,0.));
#170883=CARTESIAN_POINT('Ctrl Pts',(68.0389988091933,23.1932920749023,12.));
#170884=CARTESIAN_POINT('Ctrl Pts',(68.0152162939121,23.1936622784919,0.));
#170885=CARTESIAN_POINT('Ctrl Pts',(68.0152162939121,23.1936622784919,12.));
#170886=CARTESIAN_POINT('Ctrl Pts',(67.991476332086,23.1940085178313,0.));
#170887=CARTESIAN_POINT('Ctrl Pts',(67.991476332086,23.1940085178313,12.));
#170888=CARTESIAN_POINT('Ctrl Pts',(67.9677790474385,23.1943308536297,0.));
#170889=CARTESIAN_POINT('Ctrl Pts',(67.9677790474385,23.1943308536297,12.));
#170890=CARTESIAN_POINT('Ctrl Pts',(67.9441245641842,23.1946293469427,0.));
#170891=CARTESIAN_POINT('Ctrl Pts',(67.9441245641842,23.1946293469427,12.));
#170892=CARTESIAN_POINT('Ctrl Pts',(67.9205130070324,23.1949040591744,0.));
#170893=CARTESIAN_POINT('Ctrl Pts',(67.9205130070324,23.1949040591744,12.));
#170894=CARTESIAN_POINT('Ctrl Pts',(67.8969445011916,23.1951550520802,0.));
#170895=CARTESIAN_POINT('Ctrl Pts',(67.8969445011916,23.1951550520802,12.));
#170896=CARTESIAN_POINT('Ctrl Pts',(67.8734191723667,23.1953823877734,0.));
#170897=CARTESIAN_POINT('Ctrl Pts',(67.8734191723667,23.1953823877734,12.));
#170898=CARTESIAN_POINT('Ctrl Pts',(67.8499371467616,23.1955861287286,0.));
#170899=CARTESIAN_POINT('Ctrl Pts',(67.8499371467616,23.1955861287286,12.));
#170900=CARTESIAN_POINT('Ctrl Pts',(67.8264985510917,23.1957663377806,0.));
#170901=CARTESIAN_POINT('Ctrl Pts',(67.8264985510917,23.1957663377806,12.));
#170902=CARTESIAN_POINT('Ctrl Pts',(67.8031035125887,23.1959230781269,0.));
#170903=CARTESIAN_POINT('Ctrl Pts',(67.8031035125887,23.1959230781269,12.));
#170904=CARTESIAN_POINT('Ctrl Pts',(67.7797521590045,23.1960564133304,0.));
#170905=CARTESIAN_POINT('Ctrl Pts',(67.7797521590045,23.1960564133304,12.));
#170906=CARTESIAN_POINT('Ctrl Pts',(67.7564446186079,23.1961664073262,0.));
#170907=CARTESIAN_POINT('Ctrl Pts',(67.7564446186079,23.1961664073262,12.));
#170908=CARTESIAN_POINT('Ctrl Pts',(67.7331810201883,23.1962531244245,0.));
#170909=CARTESIAN_POINT('Ctrl Pts',(67.7331810201883,23.1962531244245,12.));
#170910=CARTESIAN_POINT('Ctrl Pts',(67.7099614930671,23.1963166293102,0.));
#170911=CARTESIAN_POINT('Ctrl Pts',(67.7099614930671,23.1963166293102,12.));
#170912=CARTESIAN_POINT('Ctrl Pts',(67.6867861671031,23.1963569870451,0.));
#170913=CARTESIAN_POINT('Ctrl Pts',(67.6867861671031,23.1963569870451,12.));
#170914=CARTESIAN_POINT('Ctrl Pts',(67.6636551726964,23.1963742630715,0.));
#170915=CARTESIAN_POINT('Ctrl Pts',(67.6636551726964,23.1963742630715,12.));
#170916=CARTESIAN_POINT('Ctrl Pts',(67.6405686407863,23.1963685232188,0.));
#170917=CARTESIAN_POINT('Ctrl Pts',(67.6405686407863,23.1963685232188,12.));
#170918=CARTESIAN_POINT('Ctrl Pts',(67.6175267028555,23.1963398337069,0.));
#170919=CARTESIAN_POINT('Ctrl Pts',(67.6175267028555,23.1963398337069,12.));
#170920=CARTESIAN_POINT('Ctrl Pts',(67.5945294909426,23.1962882611453,0.));
#170921=CARTESIAN_POINT('Ctrl Pts',(67.5945294909426,23.1962882611453,12.));
#170922=CARTESIAN_POINT('Ctrl Pts',(67.5715771376461,23.196213872536,0.));
#170923=CARTESIAN_POINT('Ctrl Pts',(67.5715771376461,23.196213872536,12.));
#170924=CARTESIAN_POINT('Ctrl Pts',(67.5486697761288,23.1961167352772,0.));
#170925=CARTESIAN_POINT('Ctrl Pts',(67.5486697761288,23.1961167352772,12.));
#170926=CARTESIAN_POINT('Ctrl Pts',(67.5258075401146,23.1959969171701,0.));
#170927=CARTESIAN_POINT('Ctrl Pts',(67.5258075401146,23.1959969171701,12.));
#170928=CARTESIAN_POINT('Ctrl Pts',(67.5029905638949,23.1958544864215,0.));
#170929=CARTESIAN_POINT('Ctrl Pts',(67.5029905638949,23.1958544864215,12.));
#170930=CARTESIAN_POINT('Ctrl Pts',(67.4802189823408,23.195689511644,0.));
#170931=CARTESIAN_POINT('Ctrl Pts',(67.4802189823408,23.195689511644,12.));
#170932=CARTESIAN_POINT('Ctrl Pts',(67.4574929309076,23.195502061859,0.));
#170933=CARTESIAN_POINT('Ctrl Pts',(67.4574929309076,23.195502061859,12.));
#170934=CARTESIAN_POINT('Ctrl Pts',(67.4348125456398,23.1952922065012,0.));
#170935=CARTESIAN_POINT('Ctrl Pts',(67.4348125456398,23.1952922065012,12.));
#170936=CARTESIAN_POINT('Ctrl Pts',(67.412177963168,23.1950600154265,0.));
#170937=CARTESIAN_POINT('Ctrl Pts',(67.412177963168,23.1950600154265,12.));
#170938=CARTESIAN_POINT('Ctrl Pts',(67.3895893207182,23.1948055589129,0.));
#170939=CARTESIAN_POINT('Ctrl Pts',(67.3895893207182,23.1948055589129,12.));
#170940=CARTESIAN_POINT('Ctrl Pts',(67.3670467561212,23.194528907661,0.));
#170941=CARTESIAN_POINT('Ctrl Pts',(67.3670467561212,23.194528907661,12.));
#170942=CARTESIAN_POINT('Ctrl Pts',(67.3445504078176,23.1942301327978,0.));
#170943=CARTESIAN_POINT('Ctrl Pts',(67.3445504078176,23.1942301327978,12.));
#170944=CARTESIAN_POINT('Ctrl Pts',(67.3221004148603,23.1939093058801,0.));
#170945=CARTESIAN_POINT('Ctrl Pts',(67.3221004148603,23.1939093058801,12.));
#170946=CARTESIAN_POINT('Ctrl Pts',(67.2996969169098,23.1935664989018,0.));
#170947=CARTESIAN_POINT('Ctrl Pts',(67.2996969169098,23.1935664989018,12.));
#170948=CARTESIAN_POINT('Ctrl Pts',(67.2773400542477,23.1932017842953,0.));
#170949=CARTESIAN_POINT('Ctrl Pts',(67.2773400542477,23.1932017842953,12.));
#170950=CARTESIAN_POINT('Ctrl Pts',(67.2550299677888,23.1928152349343,0.));
#170951=CARTESIAN_POINT('Ctrl Pts',(67.2550299677888,23.1928152349343,12.));
#170952=CARTESIAN_POINT('Ctrl Pts',(67.232766799088,23.1924069241385,0.));
#170953=CARTESIAN_POINT('Ctrl Pts',(67.232766799088,23.1924069241385,12.));
#170954=CARTESIAN_POINT('Ctrl Pts',(67.2105506903447,23.1919769256803,0.));
#170955=CARTESIAN_POINT('Ctrl Pts',(67.2105506903447,23.1919769256803,12.));
#170956=CARTESIAN_POINT('Ctrl Pts',(67.1883817844038,23.1915253137924,0.));
#170957=CARTESIAN_POINT('Ctrl Pts',(67.1883817844038,23.1915253137924,12.));
#170958=CARTESIAN_POINT('Ctrl Pts',(67.1662602247639,23.1910521631657,0.));
#170959=CARTESIAN_POINT('Ctrl Pts',(67.1662602247639,23.1910521631657,12.));
#170960=CARTESIAN_POINT('Ctrl Pts',(67.1441861555817,23.1905575489505,0.));
#170961=CARTESIAN_POINT('Ctrl Pts',(67.1441861555817,23.1905575489505,12.));
#170962=CARTESIAN_POINT('Ctrl Pts',(67.1221597216741,23.1900415467574,0.));
#170963=CARTESIAN_POINT('Ctrl Pts',(67.1221597216741,23.1900415467574,12.));
#170964=CARTESIAN_POINT('Ctrl Pts',(67.1001810685143,23.1895042326627,0.));
#170965=CARTESIAN_POINT('Ctrl Pts',(67.1001810685143,23.1895042326627,12.));
#170966=CARTESIAN_POINT('Ctrl Pts',(67.0782503422305,23.1889456832119,0.));
#170967=CARTESIAN_POINT('Ctrl Pts',(67.0782503422305,23.1889456832119,12.));
#170968=CARTESIAN_POINT('Ctrl Pts',(67.0563676896325,23.1883659754271,0.));
#170969=CARTESIAN_POINT('Ctrl Pts',(67.0563676896325,23.1883659754271,12.));
#170970=CARTESIAN_POINT('Ctrl Pts',(67.0345332582306,23.1877651868158,0.));
#170971=CARTESIAN_POINT('Ctrl Pts',(67.0345332582306,23.1877651868158,12.));
#170972=CARTESIAN_POINT('Ctrl Pts',(67.0127471962501,23.1871433953793,0.));
#170973=CARTESIAN_POINT('Ctrl Pts',(67.0127471962501,23.1871433953793,12.));
#170974=CARTESIAN_POINT('Ctrl Pts',(66.9910096526462,23.1865006796283,0.));
#170975=CARTESIAN_POINT('Ctrl Pts',(66.9910096526462,23.1865006796283,12.));
#170976=CARTESIAN_POINT('Ctrl Pts',(66.9693207771031,23.1858371185842,0.));
#170977=CARTESIAN_POINT('Ctrl Pts',(66.9693207771031,23.1858371185842,12.));
#170978=CARTESIAN_POINT('Ctrl Pts',(66.9476807200203,23.1851527917657,0.));
#170979=CARTESIAN_POINT('Ctrl Pts',(66.9476807200203,23.1851527917657,12.));
#170980=CARTESIAN_POINT('Ctrl Pts',(66.9260896324949,23.1844477791814,0.));
#170981=CARTESIAN_POINT('Ctrl Pts',(66.9260896324949,23.1844477791814,12.));
#170982=CARTESIAN_POINT('Ctrl Pts',(66.9045476663063,23.1837221613235,0.));
#170983=CARTESIAN_POINT('Ctrl Pts',(66.9045476663063,23.1837221613235,12.));
#170984=CARTESIAN_POINT('Ctrl Pts',(66.8830549738795,23.1829760191591,0.));
#170985=CARTESIAN_POINT('Ctrl Pts',(66.8830549738795,23.1829760191591,12.));
#170986=CARTESIAN_POINT('Ctrl Pts',(66.8616117083331,23.1822094341517,0.));
#170987=CARTESIAN_POINT('Ctrl Pts',(66.8616117083331,23.1822094341517,12.));
#170988=CARTESIAN_POINT('Ctrl Pts',(66.8402180235566,23.1814224882953,0.));
#170989=CARTESIAN_POINT('Ctrl Pts',(66.8402180235566,23.1814224882953,12.));
#170990=CARTESIAN_POINT('Ctrl Pts',(66.8188740742727,23.1806152641475,0.));
#170991=CARTESIAN_POINT('Ctrl Pts',(66.8188740742727,23.1806152641475,12.));
#170992=CARTESIAN_POINT('Ctrl Pts',(66.7975800161,23.1797878448639,0.));
#170993=CARTESIAN_POINT('Ctrl Pts',(66.7975800161,23.1797878448639,12.));
#170994=CARTESIAN_POINT('Ctrl Pts',(66.776336005612,23.1789403142366,0.));
#170995=CARTESIAN_POINT('Ctrl Pts',(66.776336005612,23.1789403142366,12.));
#170996=CARTESIAN_POINT('Ctrl Pts',(66.7551422002204,23.17807275663,0.));
#170997=CARTESIAN_POINT('Ctrl Pts',(66.7551422002204,23.17807275663,12.));
#170998=CARTESIAN_POINT('Ctrl Pts',(66.7339987580427,23.1771852569131,0.));
#170999=CARTESIAN_POINT('Ctrl Pts',(66.7339987580427,23.1771852569131,12.));
#171000=CARTESIAN_POINT('Ctrl Pts',(66.7129058377896,23.1762779004044,0.));
#171001=CARTESIAN_POINT('Ctrl Pts',(66.7129058377896,23.1762779004044,12.));
#171002=CARTESIAN_POINT('Ctrl Pts',(66.6918635985972,23.1753507727939,0.));
#171003=CARTESIAN_POINT('Ctrl Pts',(66.6918635985972,23.1753507727939,12.));
#171004=CARTESIAN_POINT('Ctrl Pts',(66.6708722000079,23.1744039601382,0.));
#171005=CARTESIAN_POINT('Ctrl Pts',(66.6708722000079,23.1744039601382,12.));
#171006=CARTESIAN_POINT('Ctrl Pts',(66.6499318023473,23.1734375490431,0.));
#171007=CARTESIAN_POINT('Ctrl Pts',(66.6499318023473,23.1734375490431,12.));
#171008=CARTESIAN_POINT('Ctrl Pts',(66.6290425670548,23.1724516268302,0.));
#171009=CARTESIAN_POINT('Ctrl Pts',(66.6290425670548,23.1724516268302,12.));
#171010=CARTESIAN_POINT('Ctrl Pts',(66.6082046569644,23.1714462816789,0.));
#171011=CARTESIAN_POINT('Ctrl Pts',(66.6082046569644,23.1714462816789,12.));
#171012=CARTESIAN_POINT('Ctrl Pts',(66.5874182367563,23.1704216028614,0.));
#171013=CARTESIAN_POINT('Ctrl Pts',(66.5874182367563,23.1704216028614,12.));
#171014=CARTESIAN_POINT('Ctrl Pts',(66.5666834726454,23.1693776805866,0.));
#171015=CARTESIAN_POINT('Ctrl Pts',(66.5666834726454,23.1693776805866,12.));
#171016=CARTESIAN_POINT('Ctrl Pts',(66.5460005315376,23.1683146055726,0.));
#171017=CARTESIAN_POINT('Ctrl Pts',(66.5460005315376,23.1683146055726,12.));
#171018=CARTESIAN_POINT('Ctrl Pts',(66.5253695803205,23.1672324686926,0.));
#171019=CARTESIAN_POINT('Ctrl Pts',(66.5253695803205,23.1672324686926,12.));
#171020=CARTESIAN_POINT('Ctrl Pts',(66.5047907851348,23.1661313606132,0.));
#171021=CARTESIAN_POINT('Ctrl Pts',(66.5047907851348,23.1661313606132,12.));
#171022=CARTESIAN_POINT('Ctrl Pts',(66.4842643105311,23.1650113713808,0.));
#171023=CARTESIAN_POINT('Ctrl Pts',(66.4842643105311,23.1650113713808,12.));
#171024=CARTESIAN_POINT('Ctrl Pts',(66.4637903210727,23.1638725912195,0.));
#171025=CARTESIAN_POINT('Ctrl Pts',(66.4637903210727,23.1638725912195,12.));
#171026=CARTESIAN_POINT('Ctrl Pts',(66.4433689832478,23.1627151114883,0.));
#171027=CARTESIAN_POINT('Ctrl Pts',(66.4433689832478,23.1627151114883,12.));
#171028=CARTESIAN_POINT('Ctrl Pts',(66.4230004670278,23.1615390254632,0.));
#171029=CARTESIAN_POINT('Ctrl Pts',(66.4230004670278,23.1615390254632,12.));
#171030=CARTESIAN_POINT('Ctrl Pts',(66.4026849481232,23.160344429474,0.));
#171031=CARTESIAN_POINT('Ctrl Pts',(66.4026849481232,23.160344429474,12.));
#171032=CARTESIAN_POINT('Ctrl Pts',(66.3824226081801,23.1591314230083,0.));
#171033=CARTESIAN_POINT('Ctrl Pts',(66.3824226081801,23.1591314230083,12.));
#171034=CARTESIAN_POINT('Ctrl Pts',(66.3622136300654,23.1579001063424,0.));
#171035=CARTESIAN_POINT('Ctrl Pts',(66.3622136300654,23.1579001063424,12.));
#171036=CARTESIAN_POINT('Ctrl Pts',(66.3420581937147,23.1566505784621,0.));
#171037=CARTESIAN_POINT('Ctrl Pts',(66.3420581937147,23.1566505784621,12.));
#171038=CARTESIAN_POINT('Ctrl Pts',(66.3219564725184,23.1553829352539,0.));
#171039=CARTESIAN_POINT('Ctrl Pts',(66.3219564725184,23.1553829352539,12.));
#171040=CARTESIAN_POINT('Ctrl Pts',(66.3019086275444,23.1540972666191,0.));
#171041=CARTESIAN_POINT('Ctrl Pts',(66.3019086275444,23.1540972666191,12.));
#171042=CARTESIAN_POINT('Ctrl Pts',(66.281914813114,23.1527936592651,0.));
#171043=CARTESIAN_POINT('Ctrl Pts',(66.281914813114,23.1527936592651,12.));
#171044=CARTESIAN_POINT('Ctrl Pts',(66.2619751878793,23.1514722022503,0.));
#171045=CARTESIAN_POINT('Ctrl Pts',(66.2619751878793,23.1514722022503,12.));
#171046=CARTESIAN_POINT('Ctrl Pts',(66.2420899237318,23.1501329914488,0.));
#171047=CARTESIAN_POINT('Ctrl Pts',(66.2420899237318,23.1501329914488,12.));
#171048=CARTESIAN_POINT('Ctrl Pts',(66.2222592165398,23.1487761349298,0.));
#171049=CARTESIAN_POINT('Ctrl Pts',(66.2222592165398,23.1487761349298,12.));
#171050=CARTESIAN_POINT('Ctrl Pts',(66.2024832934733,23.147401756643,0.));
#171051=CARTESIAN_POINT('Ctrl Pts',(66.2024832934733,23.147401756643,12.));
#171052=CARTESIAN_POINT('Ctrl Pts',(66.1827623902755,23.1460099850704,0.));
#171053=CARTESIAN_POINT('Ctrl Pts',(66.1827623902755,23.1460099850704,12.));
#171054=CARTESIAN_POINT('Ctrl Pts',(66.163096729667,23.1446009424871,0.));
#171055=CARTESIAN_POINT('Ctrl Pts',(66.163096729667,23.1446009424871,12.));
#171056=CARTESIAN_POINT('Ctrl Pts',(66.14348650151,23.1431747350127,0.));
#171057=CARTESIAN_POINT('Ctrl Pts',(66.14348650151,23.1431747350127,12.));
#171058=CARTESIAN_POINT('Ctrl Pts',(66.1239318368803,23.1417314398501,0.));
#171059=CARTESIAN_POINT('Ctrl Pts',(66.1239318368803,23.1417314398501,12.));
#171060=CARTESIAN_POINT('Ctrl Pts',(66.1044328067739,23.140271103958,0.));
#171061=CARTESIAN_POINT('Ctrl Pts',(66.1044328067739,23.140271103958,12.));
#171062=CARTESIAN_POINT('Ctrl Pts',(66.0888781152779,23.1390892229923,0.));
#171063=CARTESIAN_POINT('Ctrl Pts',(66.0888781152779,23.1390892229923,12.));
#171064=CARTESIAN_POINT('Ctrl Pts',(66.0772371487475,23.1381951597491,0.));
#171065=CARTESIAN_POINT('Ctrl Pts',(66.0772371487475,23.1381951597491,12.));
#171066=CARTESIAN_POINT('Ctrl Pts',(66.0694876382212,23.1375957166138,0.));
#171067=CARTESIAN_POINT('Ctrl Pts',(66.0694876382212,23.1375957166138,12.));
#171068=CARTESIAN_POINT('Ctrl Pts',(66.0656156664138,23.1372951448024,0.));
#171069=CARTESIAN_POINT('Ctrl Pts',(66.0656156664138,23.1372951448024,12.));
#171070=CARTESIAN_POINT('',(66.0656156664138,23.1372951448024,12.));
#171071=CARTESIAN_POINT('Ctrl Pts',(66.0656156664138,23.1372951448024,12.));
#171072=CARTESIAN_POINT('Ctrl Pts',(66.0694876382212,23.1375957166138,12.));
#171073=CARTESIAN_POINT('Ctrl Pts',(66.0772371487475,23.1381951597491,12.));
#171074=CARTESIAN_POINT('Ctrl Pts',(66.0888781152779,23.1390892229923,12.));
#171075=CARTESIAN_POINT('Ctrl Pts',(66.1044328067739,23.140271103958,12.));
#171076=CARTESIAN_POINT('Ctrl Pts',(66.1239318368803,23.1417314398501,12.));
#171077=CARTESIAN_POINT('Ctrl Pts',(66.14348650151,23.1431747350127,12.));
#171078=CARTESIAN_POINT('Ctrl Pts',(66.163096729667,23.1446009424871,12.));
#171079=CARTESIAN_POINT('Ctrl Pts',(66.1827623902755,23.1460099850704,12.));
#171080=CARTESIAN_POINT('Ctrl Pts',(66.2024832934733,23.147401756643,12.));
#171081=CARTESIAN_POINT('Ctrl Pts',(66.2222592165398,23.1487761349298,12.));
#171082=CARTESIAN_POINT('Ctrl Pts',(66.2420899237318,23.1501329914488,12.));
#171083=CARTESIAN_POINT('Ctrl Pts',(66.2619751878793,23.1514722022503,12.));
#171084=CARTESIAN_POINT('Ctrl Pts',(66.281914813114,23.1527936592651,12.));
#171085=CARTESIAN_POINT('Ctrl Pts',(66.3019086275444,23.1540972666191,12.));
#171086=CARTESIAN_POINT('Ctrl Pts',(66.3219564725184,23.1553829352539,12.));
#171087=CARTESIAN_POINT('Ctrl Pts',(66.3420581937147,23.1566505784621,12.));
#171088=CARTESIAN_POINT('Ctrl Pts',(66.3622136300654,23.1579001063424,12.));
#171089=CARTESIAN_POINT('Ctrl Pts',(66.3824226081801,23.1591314230083,12.));
#171090=CARTESIAN_POINT('Ctrl Pts',(66.4026849481232,23.160344429474,12.));
#171091=CARTESIAN_POINT('Ctrl Pts',(66.4230004670278,23.1615390254632,12.));
#171092=CARTESIAN_POINT('Ctrl Pts',(66.4433689832478,23.1627151114883,12.));
#171093=CARTESIAN_POINT('Ctrl Pts',(66.4637903210727,23.1638725912195,12.));
#171094=CARTESIAN_POINT('Ctrl Pts',(66.4842643105311,23.1650113713808,12.));
#171095=CARTESIAN_POINT('Ctrl Pts',(66.5047907851348,23.1661313606132,12.));
#171096=CARTESIAN_POINT('Ctrl Pts',(66.5253695803205,23.1672324686926,12.));
#171097=CARTESIAN_POINT('Ctrl Pts',(66.5460005315376,23.1683146055726,12.));
#171098=CARTESIAN_POINT('Ctrl Pts',(66.5666834726454,23.1693776805866,12.));
#171099=CARTESIAN_POINT('Ctrl Pts',(66.5874182367563,23.1704216028614,12.));
#171100=CARTESIAN_POINT('Ctrl Pts',(66.6082046569644,23.1714462816789,12.));
#171101=CARTESIAN_POINT('Ctrl Pts',(66.6290425670548,23.1724516268302,12.));
#171102=CARTESIAN_POINT('Ctrl Pts',(66.6499318023473,23.1734375490431,12.));
#171103=CARTESIAN_POINT('Ctrl Pts',(66.6708722000079,23.1744039601382,12.));
#171104=CARTESIAN_POINT('Ctrl Pts',(66.6918635985972,23.1753507727939,12.));
#171105=CARTESIAN_POINT('Ctrl Pts',(66.7129058377896,23.1762779004044,12.));
#171106=CARTESIAN_POINT('Ctrl Pts',(66.7339987580427,23.1771852569131,12.));
#171107=CARTESIAN_POINT('Ctrl Pts',(66.7551422002204,23.17807275663,12.));
#171108=CARTESIAN_POINT('Ctrl Pts',(66.776336005612,23.1789403142366,12.));
#171109=CARTESIAN_POINT('Ctrl Pts',(66.7975800161,23.1797878448639,12.));
#171110=CARTESIAN_POINT('Ctrl Pts',(66.8188740742727,23.1806152641475,12.));
#171111=CARTESIAN_POINT('Ctrl Pts',(66.8402180235566,23.1814224882953,12.));
#171112=CARTESIAN_POINT('Ctrl Pts',(66.8616117083331,23.1822094341517,12.));
#171113=CARTESIAN_POINT('Ctrl Pts',(66.8830549738795,23.1829760191591,12.));
#171114=CARTESIAN_POINT('Ctrl Pts',(66.9045476663063,23.1837221613235,12.));
#171115=CARTESIAN_POINT('Ctrl Pts',(66.9260896324949,23.1844477791814,12.));
#171116=CARTESIAN_POINT('Ctrl Pts',(66.9476807200203,23.1851527917657,12.));
#171117=CARTESIAN_POINT('Ctrl Pts',(66.9693207771031,23.1858371185842,12.));
#171118=CARTESIAN_POINT('Ctrl Pts',(66.9910096526462,23.1865006796283,12.));
#171119=CARTESIAN_POINT('Ctrl Pts',(67.0127471962501,23.1871433953793,12.));
#171120=CARTESIAN_POINT('Ctrl Pts',(67.0345332582306,23.1877651868158,12.));
#171121=CARTESIAN_POINT('Ctrl Pts',(67.0563676896325,23.1883659754271,12.));
#171122=CARTESIAN_POINT('Ctrl Pts',(67.0782503422305,23.1889456832119,12.));
#171123=CARTESIAN_POINT('Ctrl Pts',(67.1001810685143,23.1895042326627,12.));
#171124=CARTESIAN_POINT('Ctrl Pts',(67.1221597216741,23.1900415467574,12.));
#171125=CARTESIAN_POINT('Ctrl Pts',(67.1441861555817,23.1905575489505,12.));
#171126=CARTESIAN_POINT('Ctrl Pts',(67.1662602247639,23.1910521631657,12.));
#171127=CARTESIAN_POINT('Ctrl Pts',(67.1883817844038,23.1915253137924,12.));
#171128=CARTESIAN_POINT('Ctrl Pts',(67.2105506903447,23.1919769256803,12.));
#171129=CARTESIAN_POINT('Ctrl Pts',(67.232766799088,23.1924069241385,12.));
#171130=CARTESIAN_POINT('Ctrl Pts',(67.2550299677888,23.1928152349343,12.));
#171131=CARTESIAN_POINT('Ctrl Pts',(67.2773400542477,23.1932017842953,12.));
#171132=CARTESIAN_POINT('Ctrl Pts',(67.2996969169098,23.1935664989018,12.));
#171133=CARTESIAN_POINT('Ctrl Pts',(67.3221004148603,23.1939093058801,12.));
#171134=CARTESIAN_POINT('Ctrl Pts',(67.3445504078176,23.1942301327978,12.));
#171135=CARTESIAN_POINT('Ctrl Pts',(67.3670467561212,23.194528907661,12.));
#171136=CARTESIAN_POINT('Ctrl Pts',(67.3895893207182,23.1948055589129,12.));
#171137=CARTESIAN_POINT('Ctrl Pts',(67.412177963168,23.1950600154265,12.));
#171138=CARTESIAN_POINT('Ctrl Pts',(67.4348125456398,23.1952922065012,12.));
#171139=CARTESIAN_POINT('Ctrl Pts',(67.4574929309076,23.195502061859,12.));
#171140=CARTESIAN_POINT('Ctrl Pts',(67.4802189823408,23.195689511644,12.));
#171141=CARTESIAN_POINT('Ctrl Pts',(67.5029905638949,23.1958544864215,12.));
#171142=CARTESIAN_POINT('Ctrl Pts',(67.5258075401146,23.1959969171701,12.));
#171143=CARTESIAN_POINT('Ctrl Pts',(67.5486697761288,23.1961167352772,12.));
#171144=CARTESIAN_POINT('Ctrl Pts',(67.5715771376461,23.196213872536,12.));
#171145=CARTESIAN_POINT('Ctrl Pts',(67.5945294909426,23.1962882611453,12.));
#171146=CARTESIAN_POINT('Ctrl Pts',(67.6175267028555,23.1963398337069,12.));
#171147=CARTESIAN_POINT('Ctrl Pts',(67.6405686407863,23.1963685232188,12.));
#171148=CARTESIAN_POINT('Ctrl Pts',(67.6636551726964,23.1963742630715,12.));
#171149=CARTESIAN_POINT('Ctrl Pts',(67.6867861671031,23.1963569870451,12.));
#171150=CARTESIAN_POINT('Ctrl Pts',(67.7099614930671,23.1963166293102,12.));
#171151=CARTESIAN_POINT('Ctrl Pts',(67.7331810201883,23.1962531244245,12.));
#171152=CARTESIAN_POINT('Ctrl Pts',(67.7564446186079,23.1961664073262,12.));
#171153=CARTESIAN_POINT('Ctrl Pts',(67.7797521590045,23.1960564133304,12.));
#171154=CARTESIAN_POINT('Ctrl Pts',(67.8031035125887,23.1959230781269,12.));
#171155=CARTESIAN_POINT('Ctrl Pts',(67.8264985510917,23.1957663377806,12.));
#171156=CARTESIAN_POINT('Ctrl Pts',(67.8499371467616,23.1955861287286,12.));
#171157=CARTESIAN_POINT('Ctrl Pts',(67.8734191723667,23.1953823877734,12.));
#171158=CARTESIAN_POINT('Ctrl Pts',(67.8969445011916,23.1951550520802,12.));
#171159=CARTESIAN_POINT('Ctrl Pts',(67.9205130070324,23.1949040591744,12.));
#171160=CARTESIAN_POINT('Ctrl Pts',(67.9441245641842,23.1946293469427,12.));
#171161=CARTESIAN_POINT('Ctrl Pts',(67.9677790474385,23.1943308536297,12.));
#171162=CARTESIAN_POINT('Ctrl Pts',(67.991476332086,23.1940085178313,12.));
#171163=CARTESIAN_POINT('Ctrl Pts',(68.0152162939121,23.1936622784919,12.));
#171164=CARTESIAN_POINT('Ctrl Pts',(68.0389988091933,23.1932920749023,12.));
#171165=CARTESIAN_POINT('Ctrl Pts',(68.0628237546863,23.1928978467021,12.));
#171166=CARTESIAN_POINT('Ctrl Pts',(68.0866910076251,23.1924795338749,12.));
#171167=CARTESIAN_POINT('Ctrl Pts',(68.110600445723,23.1920370767426,12.));
#171168=CARTESIAN_POINT('Ctrl Pts',(68.1345519471695,23.1915704159623,12.));
#171169=CARTESIAN_POINT('Ctrl Pts',(68.1585453906257,23.1910794925251,12.));
#171170=CARTESIAN_POINT('Ctrl Pts',(68.1825806552129,23.1905642477571,12.));
#171171=CARTESIAN_POINT('Ctrl Pts',(68.2066576205116,23.1900246233165,12.));
#171172=CARTESIAN_POINT('Ctrl Pts',(68.2307761665633,23.1894605611871,12.));
#171173=CARTESIAN_POINT('Ctrl Pts',(68.2549361738681,23.1888720036757,12.));
#171174=CARTESIAN_POINT('Ctrl Pts',(68.2791375233795,23.1882588934107,12.));
#171175=CARTESIAN_POINT('Ctrl Pts',(68.3033800964939,23.1876211733436,12.));
#171176=CARTESIAN_POINT('Ctrl Pts',(68.3276637750485,23.1869587867459,12.));
#171177=CARTESIAN_POINT('Ctrl Pts',(68.3519884413246,23.1862716772031,12.));
#171178=CARTESIAN_POINT('Ctrl Pts',(68.376353978044,23.1855597886116,12.));
#171179=CARTESIAN_POINT('Ctrl Pts',(68.4007602683652,23.1848230651776,12.));
#171180=CARTESIAN_POINT('Ctrl Pts',(68.4252071958729,23.1840614514192,12.));
#171181=CARTESIAN_POINT('Ctrl Pts',(68.4496946445758,23.183274892163,12.));
#171182=CARTESIAN_POINT('Ctrl Pts',(68.4742224989098,23.1824633325385,12.));
#171183=CARTESIAN_POINT('Ctrl Pts',(68.4987906437356,23.1816267179751,12.));
#171184=CARTESIAN_POINT('Ctrl Pts',(68.5233989643345,23.180764994201,12.));
#171185=CARTESIAN_POINT('Ctrl Pts',(68.5480473463985,23.179878107245,12.));
#171186=CARTESIAN_POINT('Ctrl Pts',(68.5727356760278,23.1789660034342,12.));
#171187=CARTESIAN_POINT('Ctrl Pts',(68.597463839733,23.1780286293875,12.));
#171188=CARTESIAN_POINT('Ctrl Pts',(68.6222317244341,23.1770659320138,12.));
#171189=CARTESIAN_POINT('Ctrl Pts',(68.6470392174564,23.1760778585092,12.));
#171190=CARTESIAN_POINT('Ctrl Pts',(68.6718862065216,23.1750643563602,12.));
#171191=CARTESIAN_POINT('Ctrl Pts',(68.696772579744,23.1740253733417,12.));
#171192=CARTESIAN_POINT('Ctrl Pts',(68.7216982256341,23.172960857511,12.));
#171193=CARTESIAN_POINT('Ctrl Pts',(68.746663033096,23.1718707572043,12.));
#171194=CARTESIAN_POINT('Ctrl Pts',(68.771666891425,23.170755021036,12.));
#171195=CARTESIAN_POINT('Ctrl Pts',(68.7967096902996,23.1696135978997,12.));
#171196=CARTESIAN_POINT('Ctrl Pts',(68.8217913197752,23.1684464369686,12.));
#171197=CARTESIAN_POINT('Ctrl Pts',(68.8469116702898,23.1672534876889,12.));
#171198=CARTESIAN_POINT('Ctrl Pts',(68.8720706326609,23.1660346997764,12.));
#171199=CARTESIAN_POINT('Ctrl Pts',(68.8972680980842,23.164790023215,12.));
#171200=CARTESIAN_POINT('Ctrl Pts',(68.9225039581248,23.1635194082581,12.));
#171201=CARTESIAN_POINT('Ctrl Pts',(68.9477781047106,23.1622228054291,12.));
#171202=CARTESIAN_POINT('Ctrl Pts',(68.9730904301369,23.1609001655156,12.));
#171203=CARTESIAN_POINT('Ctrl Pts',(68.9984408270659,23.1595514395656,12.));
#171204=CARTESIAN_POINT('Ctrl Pts',(69.0238291885245,23.1581765788869,12.));
#171205=CARTESIAN_POINT('Ctrl Pts',(69.0492554078992,23.1567755350469,12.));
#171206=CARTESIAN_POINT('Ctrl Pts',(69.074719378928,23.1553482598762,12.));
#171207=CARTESIAN_POINT('Ctrl Pts',(69.1002209957025,23.1538947054615,12.));
#171208=CARTESIAN_POINT('Ctrl Pts',(69.1257601526687,23.152414824141,12.));
#171209=CARTESIAN_POINT('Ctrl Pts',(69.1513367446231,23.1509085685032,12.));
#171210=CARTESIAN_POINT('Ctrl Pts',(69.1769506667084,23.1493758913859,12.));
#171211=CARTESIAN_POINT('Ctrl Pts',(69.2026018144028,23.147816745879,12.));
#171212=CARTESIAN_POINT('Ctrl Pts',(69.2282900835235,23.1462310853206,12.));
#171213=CARTESIAN_POINT('Ctrl Pts',(69.254015370231,23.1446188632931,12.));
#171214=CARTESIAN_POINT('Ctrl Pts',(69.2797775710273,23.142980033622,12.));
#171215=CARTESIAN_POINT('Ctrl Pts',(69.3055765827546,23.1413145503762,12.));
#171216=CARTESIAN_POINT('Ctrl Pts',(69.3314123025869,23.1396223678725,12.));
#171217=CARTESIAN_POINT('Ctrl Pts',(69.3572846280297,23.1379034406718,12.));
#171218=CARTESIAN_POINT('Ctrl Pts',(69.3831934569182,23.1361577235709,12.));
#171219=CARTESIAN_POINT('Ctrl Pts',(69.4091386874132,23.1343851715989,12.));
#171220=CARTESIAN_POINT('Ctrl Pts',(69.4351202179946,23.1325857400144,12.));
#171221=CARTESIAN_POINT('Ctrl Pts',(69.4611379474484,23.1307593843061,12.));
#171222=CARTESIAN_POINT('Ctrl Pts',(69.4871917748654,23.1289060601924,12.));
#171223=CARTESIAN_POINT('Ctrl Pts',(69.5132815996537,23.1270257236204,12.));
#171224=CARTESIAN_POINT('Ctrl Pts',(69.539407321546,23.1251183307676,12.));
#171225=CARTESIAN_POINT('Ctrl Pts',(69.5655688406052,23.1231838380452,12.));
#171226=CARTESIAN_POINT('Ctrl Pts',(69.5917660572265,23.1212222021051,12.));
#171227=CARTESIAN_POINT('Ctrl Pts',(69.6179988721365,23.1192333798441,12.));
#171228=CARTESIAN_POINT('Ctrl Pts',(69.6442671863765,23.1172173283859,12.));
#171229=CARTESIAN_POINT('Ctrl Pts',(69.6705709012852,23.1151740050681,12.));
#171230=CARTESIAN_POINT('Ctrl Pts',(69.6969099184767,23.1131033674301,12.));
#171231=CARTESIAN_POINT('Ctrl Pts',(69.7232841398197,23.1110053732046,12.));
#171232=CARTESIAN_POINT('Ctrl Pts',(69.7496934674069,23.1088799803089,12.));
#171233=CARTESIAN_POINT('Ctrl Pts',(69.7761378035964,23.106727146861,12.));
#171234=CARTESIAN_POINT('Ctrl Pts',(69.8026170510572,23.1045468311991,12.));
#171235=CARTESIAN_POINT('Ctrl Pts',(69.8291311128118,23.1023389919051,12.));
#171236=CARTESIAN_POINT('Ctrl Pts',(69.8556798922693,23.1001035878241,12.));
#171237=CARTESIAN_POINT('Ctrl Pts',(69.8822632932768,23.0978405781021,12.));
#171238=CARTESIAN_POINT('Ctrl Pts',(69.9088812200713,23.0955499221558,12.));
#171239=CARTESIAN_POINT('Ctrl Pts',(69.9355335771729,23.0932315796068,12.));
#171240=CARTESIAN_POINT('Ctrl Pts',(69.9622202692873,23.0908855102251,12.));
#171241=CARTESIAN_POINT('Ctrl Pts',(69.9889412012143,23.0885116738798,12.));
#171242=CARTESIAN_POINT('Ctrl Pts',(70.0156962777169,23.0861100304729,12.));
#171243=CARTESIAN_POINT('Ctrl Pts',(70.0424854035115,23.0836805399374,12.));
#171244=CARTESIAN_POINT('Ctrl Pts',(70.0693084835373,23.0812231623765,12.));
#171245=CARTESIAN_POINT('Ctrl Pts',(70.0961654231639,23.0787378581774,12.));
#171246=CARTESIAN_POINT('Ctrl Pts',(70.123056128422,23.0762245881389,12.));
#171247=CARTESIAN_POINT('Ctrl Pts',(70.1499805062172,23.0736833135938,12.));
#171248=CARTESIAN_POINT('Ctrl Pts',(70.1769384645586,23.071113996544,12.));
#171249=CARTESIAN_POINT('Ctrl Pts',(70.2039299120488,23.0685165993691,12.));
#171250=CARTESIAN_POINT('Ctrl Pts',(70.2309547573815,23.0658910845433,12.));
#171251=CARTESIAN_POINT('Ctrl Pts',(70.2580129087888,23.0632374143279,12.));
#171252=CARTESIAN_POINT('Ctrl Pts',(70.2851042736066,23.0605555505321,12.));
#171253=CARTESIAN_POINT('Ctrl Pts',(70.3122287575335,23.0578454541104,12.));
#171254=CARTESIAN_POINT('Ctrl Pts',(70.3393862652297,23.0551070854926,12.));
#171255=CARTESIAN_POINT('Ctrl Pts',(70.3665767016542,23.0523404053172,12.));
#171256=CARTESIAN_POINT('Ctrl Pts',(70.3937999732267,23.0495453750763,12.));
#171257=CARTESIAN_POINT('Ctrl Pts',(70.4210559889348,23.0467219577291,12.));
#171258=CARTESIAN_POINT('Ctrl Pts',(70.4483446617614,23.0438701185013,12.));
#171259=CARTESIAN_POINT('Ctrl Pts',(70.4756659090209,23.0409898250756,12.));
#171260=CARTESIAN_POINT('Ctrl Pts',(70.4991133648947,23.0384964376036,12.));
#171261=CARTESIAN_POINT('Ctrl Pts',(70.5171075702746,23.0365694096173,12.));
#171262=CARTESIAN_POINT('Ctrl Pts',(70.5296341535556,23.0352213647764,12.));
#171263=CARTESIAN_POINT('Ctrl Pts',(70.5366836381661,23.0344606623299,12.));
#171264=CARTESIAN_POINT('Ctrl Pts',(70.538251407892,23.0342913834073,12.));
#171265=CARTESIAN_POINT('',(66.0656156664138,23.1372951448024,0.));
#171266=CARTESIAN_POINT('',(66.0656156664138,23.1372951448024,0.));
#171267=CARTESIAN_POINT('Ctrl Pts',(70.538251407892,23.0342913834073,0.));
#171268=CARTESIAN_POINT('Ctrl Pts',(70.5366836381661,23.0344606623299,0.));
#171269=CARTESIAN_POINT('Ctrl Pts',(70.5296341535556,23.0352213647764,0.));
#171270=CARTESIAN_POINT('Ctrl Pts',(70.5171075702746,23.0365694096173,0.));
#171271=CARTESIAN_POINT('Ctrl Pts',(70.4991133648947,23.0384964376036,0.));
#171272=CARTESIAN_POINT('Ctrl Pts',(70.4756659090209,23.0409898250756,0.));
#171273=CARTESIAN_POINT('Ctrl Pts',(70.4483446617614,23.0438701185013,0.));
#171274=CARTESIAN_POINT('Ctrl Pts',(70.4210559889348,23.0467219577291,0.));
#171275=CARTESIAN_POINT('Ctrl Pts',(70.3937999732267,23.0495453750763,0.));
#171276=CARTESIAN_POINT('Ctrl Pts',(70.3665767016542,23.0523404053172,0.));
#171277=CARTESIAN_POINT('Ctrl Pts',(70.3393862652297,23.0551070854926,0.));
#171278=CARTESIAN_POINT('Ctrl Pts',(70.3122287575335,23.0578454541104,0.));
#171279=CARTESIAN_POINT('Ctrl Pts',(70.2851042736066,23.0605555505321,0.));
#171280=CARTESIAN_POINT('Ctrl Pts',(70.2580129087888,23.0632374143279,0.));
#171281=CARTESIAN_POINT('Ctrl Pts',(70.2309547573815,23.0658910845433,0.));
#171282=CARTESIAN_POINT('Ctrl Pts',(70.2039299120488,23.0685165993691,0.));
#171283=CARTESIAN_POINT('Ctrl Pts',(70.1769384645586,23.071113996544,0.));
#171284=CARTESIAN_POINT('Ctrl Pts',(70.1499805062172,23.0736833135938,0.));
#171285=CARTESIAN_POINT('Ctrl Pts',(70.123056128422,23.0762245881389,0.));
#171286=CARTESIAN_POINT('Ctrl Pts',(70.0961654231639,23.0787378581774,0.));
#171287=CARTESIAN_POINT('Ctrl Pts',(70.0693084835373,23.0812231623765,0.));
#171288=CARTESIAN_POINT('Ctrl Pts',(70.0424854035115,23.0836805399374,0.));
#171289=CARTESIAN_POINT('Ctrl Pts',(70.0156962777169,23.0861100304729,0.));
#171290=CARTESIAN_POINT('Ctrl Pts',(69.9889412012143,23.0885116738798,0.));
#171291=CARTESIAN_POINT('Ctrl Pts',(69.9622202692873,23.0908855102251,0.));
#171292=CARTESIAN_POINT('Ctrl Pts',(69.9355335771729,23.0932315796068,0.));
#171293=CARTESIAN_POINT('Ctrl Pts',(69.9088812200713,23.0955499221558,0.));
#171294=CARTESIAN_POINT('Ctrl Pts',(69.8822632932768,23.0978405781021,0.));
#171295=CARTESIAN_POINT('Ctrl Pts',(69.8556798922693,23.1001035878241,0.));
#171296=CARTESIAN_POINT('Ctrl Pts',(69.8291311128118,23.1023389919051,0.));
#171297=CARTESIAN_POINT('Ctrl Pts',(69.8026170510572,23.1045468311991,0.));
#171298=CARTESIAN_POINT('Ctrl Pts',(69.7761378035964,23.106727146861,0.));
#171299=CARTESIAN_POINT('Ctrl Pts',(69.7496934674069,23.1088799803089,0.));
#171300=CARTESIAN_POINT('Ctrl Pts',(69.7232841398197,23.1110053732046,0.));
#171301=CARTESIAN_POINT('Ctrl Pts',(69.6969099184767,23.1131033674301,0.));
#171302=CARTESIAN_POINT('Ctrl Pts',(69.6705709012852,23.1151740050681,0.));
#171303=CARTESIAN_POINT('Ctrl Pts',(69.6442671863765,23.1172173283859,0.));
#171304=CARTESIAN_POINT('Ctrl Pts',(69.6179988721365,23.1192333798441,0.));
#171305=CARTESIAN_POINT('Ctrl Pts',(69.5917660572265,23.1212222021051,0.));
#171306=CARTESIAN_POINT('Ctrl Pts',(69.5655688406052,23.1231838380452,0.));
#171307=CARTESIAN_POINT('Ctrl Pts',(69.539407321546,23.1251183307676,0.));
#171308=CARTESIAN_POINT('Ctrl Pts',(69.5132815996537,23.1270257236204,0.));
#171309=CARTESIAN_POINT('Ctrl Pts',(69.4871917748654,23.1289060601924,0.));
#171310=CARTESIAN_POINT('Ctrl Pts',(69.4611379474484,23.1307593843061,0.));
#171311=CARTESIAN_POINT('Ctrl Pts',(69.4351202179946,23.1325857400144,0.));
#171312=CARTESIAN_POINT('Ctrl Pts',(69.4091386874132,23.1343851715989,0.));
#171313=CARTESIAN_POINT('Ctrl Pts',(69.3831934569182,23.1361577235709,0.));
#171314=CARTESIAN_POINT('Ctrl Pts',(69.3572846280297,23.1379034406718,0.));
#171315=CARTESIAN_POINT('Ctrl Pts',(69.3314123025869,23.1396223678725,0.));
#171316=CARTESIAN_POINT('Ctrl Pts',(69.3055765827546,23.1413145503762,0.));
#171317=CARTESIAN_POINT('Ctrl Pts',(69.2797775710273,23.142980033622,0.));
#171318=CARTESIAN_POINT('Ctrl Pts',(69.254015370231,23.1446188632931,0.));
#171319=CARTESIAN_POINT('Ctrl Pts',(69.2282900835235,23.1462310853206,0.));
#171320=CARTESIAN_POINT('Ctrl Pts',(69.2026018144028,23.147816745879,0.));
#171321=CARTESIAN_POINT('Ctrl Pts',(69.1769506667084,23.1493758913859,0.));
#171322=CARTESIAN_POINT('Ctrl Pts',(69.1513367446231,23.1509085685032,0.));
#171323=CARTESIAN_POINT('Ctrl Pts',(69.1257601526687,23.152414824141,0.));
#171324=CARTESIAN_POINT('Ctrl Pts',(69.1002209957025,23.1538947054615,0.));
#171325=CARTESIAN_POINT('Ctrl Pts',(69.074719378928,23.1553482598762,0.));
#171326=CARTESIAN_POINT('Ctrl Pts',(69.0492554078992,23.1567755350469,0.));
#171327=CARTESIAN_POINT('Ctrl Pts',(69.0238291885245,23.1581765788869,0.));
#171328=CARTESIAN_POINT('Ctrl Pts',(68.9984408270659,23.1595514395656,0.));
#171329=CARTESIAN_POINT('Ctrl Pts',(68.9730904301369,23.1609001655156,0.));
#171330=CARTESIAN_POINT('Ctrl Pts',(68.9477781047106,23.1622228054291,0.));
#171331=CARTESIAN_POINT('Ctrl Pts',(68.9225039581248,23.1635194082581,0.));
#171332=CARTESIAN_POINT('Ctrl Pts',(68.8972680980842,23.164790023215,0.));
#171333=CARTESIAN_POINT('Ctrl Pts',(68.8720706326609,23.1660346997764,0.));
#171334=CARTESIAN_POINT('Ctrl Pts',(68.8469116702898,23.1672534876889,0.));
#171335=CARTESIAN_POINT('Ctrl Pts',(68.8217913197752,23.1684464369686,0.));
#171336=CARTESIAN_POINT('Ctrl Pts',(68.7967096902996,23.1696135978997,0.));
#171337=CARTESIAN_POINT('Ctrl Pts',(68.771666891425,23.170755021036,0.));
#171338=CARTESIAN_POINT('Ctrl Pts',(68.746663033096,23.1718707572043,0.));
#171339=CARTESIAN_POINT('Ctrl Pts',(68.7216982256341,23.172960857511,0.));
#171340=CARTESIAN_POINT('Ctrl Pts',(68.696772579744,23.1740253733417,0.));
#171341=CARTESIAN_POINT('Ctrl Pts',(68.6718862065216,23.1750643563602,0.));
#171342=CARTESIAN_POINT('Ctrl Pts',(68.6470392174564,23.1760778585092,0.));
#171343=CARTESIAN_POINT('Ctrl Pts',(68.6222317244341,23.1770659320138,0.));
#171344=CARTESIAN_POINT('Ctrl Pts',(68.597463839733,23.1780286293875,0.));
#171345=CARTESIAN_POINT('Ctrl Pts',(68.5727356760278,23.1789660034342,0.));
#171346=CARTESIAN_POINT('Ctrl Pts',(68.5480473463985,23.179878107245,0.));
#171347=CARTESIAN_POINT('Ctrl Pts',(68.5233989643345,23.180764994201,0.));
#171348=CARTESIAN_POINT('Ctrl Pts',(68.4987906437356,23.1816267179751,0.));
#171349=CARTESIAN_POINT('Ctrl Pts',(68.4742224989098,23.1824633325385,0.));
#171350=CARTESIAN_POINT('Ctrl Pts',(68.4496946445758,23.183274892163,0.));
#171351=CARTESIAN_POINT('Ctrl Pts',(68.4252071958729,23.1840614514192,0.));
#171352=CARTESIAN_POINT('Ctrl Pts',(68.4007602683652,23.1848230651776,0.));
#171353=CARTESIAN_POINT('Ctrl Pts',(68.376353978044,23.1855597886116,0.));
#171354=CARTESIAN_POINT('Ctrl Pts',(68.3519884413246,23.1862716772031,0.));
#171355=CARTESIAN_POINT('Ctrl Pts',(68.3276637750485,23.1869587867459,0.));
#171356=CARTESIAN_POINT('Ctrl Pts',(68.3033800964939,23.1876211733436,0.));
#171357=CARTESIAN_POINT('Ctrl Pts',(68.2791375233795,23.1882588934107,0.));
#171358=CARTESIAN_POINT('Ctrl Pts',(68.2549361738681,23.1888720036757,0.));
#171359=CARTESIAN_POINT('Ctrl Pts',(68.2307761665633,23.1894605611871,0.));
#171360=CARTESIAN_POINT('Ctrl Pts',(68.2066576205116,23.1900246233165,0.));
#171361=CARTESIAN_POINT('Ctrl Pts',(68.1825806552129,23.1905642477571,0.));
#171362=CARTESIAN_POINT('Ctrl Pts',(68.1585453906257,23.1910794925251,0.));
#171363=CARTESIAN_POINT('Ctrl Pts',(68.1345519471695,23.1915704159623,0.));
#171364=CARTESIAN_POINT('Ctrl Pts',(68.110600445723,23.1920370767426,0.));
#171365=CARTESIAN_POINT('Ctrl Pts',(68.0866910076251,23.1924795338749,0.));
#171366=CARTESIAN_POINT('Ctrl Pts',(68.0628237546863,23.1928978467021,0.));
#171367=CARTESIAN_POINT('Ctrl Pts',(68.0389988091933,23.1932920749023,0.));
#171368=CARTESIAN_POINT('Ctrl Pts',(68.0152162939121,23.1936622784919,0.));
#171369=CARTESIAN_POINT('Ctrl Pts',(67.991476332086,23.1940085178313,0.));
#171370=CARTESIAN_POINT('Ctrl Pts',(67.9677790474385,23.1943308536297,0.));
#171371=CARTESIAN_POINT('Ctrl Pts',(67.9441245641842,23.1946293469427,0.));
#171372=CARTESIAN_POINT('Ctrl Pts',(67.9205130070324,23.1949040591744,0.));
#171373=CARTESIAN_POINT('Ctrl Pts',(67.8969445011916,23.1951550520802,0.));
#171374=CARTESIAN_POINT('Ctrl Pts',(67.8734191723667,23.1953823877734,0.));
#171375=CARTESIAN_POINT('Ctrl Pts',(67.8499371467616,23.1955861287286,0.));
#171376=CARTESIAN_POINT('Ctrl Pts',(67.8264985510917,23.1957663377806,0.));
#171377=CARTESIAN_POINT('Ctrl Pts',(67.8031035125887,23.1959230781269,0.));
#171378=CARTESIAN_POINT('Ctrl Pts',(67.7797521590045,23.1960564133304,0.));
#171379=CARTESIAN_POINT('Ctrl Pts',(67.7564446186079,23.1961664073262,0.));
#171380=CARTESIAN_POINT('Ctrl Pts',(67.7331810201883,23.1962531244245,0.));
#171381=CARTESIAN_POINT('Ctrl Pts',(67.7099614930671,23.1963166293102,0.));
#171382=CARTESIAN_POINT('Ctrl Pts',(67.6867861671031,23.1963569870451,0.));
#171383=CARTESIAN_POINT('Ctrl Pts',(67.6636551726964,23.1963742630715,0.));
#171384=CARTESIAN_POINT('Ctrl Pts',(67.6405686407863,23.1963685232188,0.));
#171385=CARTESIAN_POINT('Ctrl Pts',(67.6175267028555,23.1963398337069,0.));
#171386=CARTESIAN_POINT('Ctrl Pts',(67.5945294909426,23.1962882611453,0.));
#171387=CARTESIAN_POINT('Ctrl Pts',(67.5715771376461,23.196213872536,0.));
#171388=CARTESIAN_POINT('Ctrl Pts',(67.5486697761288,23.1961167352772,0.));
#171389=CARTESIAN_POINT('Ctrl Pts',(67.5258075401146,23.1959969171701,0.));
#171390=CARTESIAN_POINT('Ctrl Pts',(67.5029905638949,23.1958544864215,0.));
#171391=CARTESIAN_POINT('Ctrl Pts',(67.4802189823408,23.195689511644,0.));
#171392=CARTESIAN_POINT('Ctrl Pts',(67.4574929309076,23.195502061859,0.));
#171393=CARTESIAN_POINT('Ctrl Pts',(67.4348125456398,23.1952922065012,0.));
#171394=CARTESIAN_POINT('Ctrl Pts',(67.412177963168,23.1950600154265,0.));
#171395=CARTESIAN_POINT('Ctrl Pts',(67.3895893207182,23.1948055589129,0.));
#171396=CARTESIAN_POINT('Ctrl Pts',(67.3670467561212,23.194528907661,0.));
#171397=CARTESIAN_POINT('Ctrl Pts',(67.3445504078176,23.1942301327978,0.));
#171398=CARTESIAN_POINT('Ctrl Pts',(67.3221004148603,23.1939093058801,0.));
#171399=CARTESIAN_POINT('Ctrl Pts',(67.2996969169098,23.1935664989018,0.));
#171400=CARTESIAN_POINT('Ctrl Pts',(67.2773400542477,23.1932017842953,0.));
#171401=CARTESIAN_POINT('Ctrl Pts',(67.2550299677888,23.1928152349343,0.));
#171402=CARTESIAN_POINT('Ctrl Pts',(67.232766799088,23.1924069241385,0.));
#171403=CARTESIAN_POINT('Ctrl Pts',(67.2105506903447,23.1919769256803,0.));
#171404=CARTESIAN_POINT('Ctrl Pts',(67.1883817844038,23.1915253137924,0.));
#171405=CARTESIAN_POINT('Ctrl Pts',(67.1662602247639,23.1910521631657,0.));
#171406=CARTESIAN_POINT('Ctrl Pts',(67.1441861555817,23.1905575489505,0.));
#171407=CARTESIAN_POINT('Ctrl Pts',(67.1221597216741,23.1900415467574,0.));
#171408=CARTESIAN_POINT('Ctrl Pts',(67.1001810685143,23.1895042326627,0.));
#171409=CARTESIAN_POINT('Ctrl Pts',(67.0782503422305,23.1889456832119,0.));
#171410=CARTESIAN_POINT('Ctrl Pts',(67.0563676896325,23.1883659754271,0.));
#171411=CARTESIAN_POINT('Ctrl Pts',(67.0345332582306,23.1877651868158,0.));
#171412=CARTESIAN_POINT('Ctrl Pts',(67.0127471962501,23.1871433953793,0.));
#171413=CARTESIAN_POINT('Ctrl Pts',(66.9910096526462,23.1865006796283,0.));
#171414=CARTESIAN_POINT('Ctrl Pts',(66.9693207771031,23.1858371185842,0.));
#171415=CARTESIAN_POINT('Ctrl Pts',(66.9476807200203,23.1851527917657,0.));
#171416=CARTESIAN_POINT('Ctrl Pts',(66.9260896324949,23.1844477791814,0.));
#171417=CARTESIAN_POINT('Ctrl Pts',(66.9045476663063,23.1837221613235,0.));
#171418=CARTESIAN_POINT('Ctrl Pts',(66.8830549738795,23.1829760191591,0.));
#171419=CARTESIAN_POINT('Ctrl Pts',(66.8616117083331,23.1822094341517,0.));
#171420=CARTESIAN_POINT('Ctrl Pts',(66.8402180235566,23.1814224882953,0.));
#171421=CARTESIAN_POINT('Ctrl Pts',(66.8188740742727,23.1806152641475,0.));
#171422=CARTESIAN_POINT('Ctrl Pts',(66.7975800161,23.1797878448639,0.));
#171423=CARTESIAN_POINT('Ctrl Pts',(66.776336005612,23.1789403142366,0.));
#171424=CARTESIAN_POINT('Ctrl Pts',(66.7551422002204,23.17807275663,0.));
#171425=CARTESIAN_POINT('Ctrl Pts',(66.7339987580427,23.1771852569131,0.));
#171426=CARTESIAN_POINT('Ctrl Pts',(66.7129058377896,23.1762779004044,0.));
#171427=CARTESIAN_POINT('Ctrl Pts',(66.6918635985972,23.1753507727939,0.));
#171428=CARTESIAN_POINT('Ctrl Pts',(66.6708722000079,23.1744039601382,0.));
#171429=CARTESIAN_POINT('Ctrl Pts',(66.6499318023473,23.1734375490431,0.));
#171430=CARTESIAN_POINT('Ctrl Pts',(66.6290425670548,23.1724516268302,0.));
#171431=CARTESIAN_POINT('Ctrl Pts',(66.6082046569644,23.1714462816789,0.));
#171432=CARTESIAN_POINT('Ctrl Pts',(66.5874182367563,23.1704216028614,0.));
#171433=CARTESIAN_POINT('Ctrl Pts',(66.5666834726454,23.1693776805866,0.));
#171434=CARTESIAN_POINT('Ctrl Pts',(66.5460005315376,23.1683146055726,0.));
#171435=CARTESIAN_POINT('Ctrl Pts',(66.5253695803205,23.1672324686926,0.));
#171436=CARTESIAN_POINT('Ctrl Pts',(66.5047907851348,23.1661313606132,0.));
#171437=CARTESIAN_POINT('Ctrl Pts',(66.4842643105311,23.1650113713808,0.));
#171438=CARTESIAN_POINT('Ctrl Pts',(66.4637903210727,23.1638725912195,0.));
#171439=CARTESIAN_POINT('Ctrl Pts',(66.4433689832478,23.1627151114883,0.));
#171440=CARTESIAN_POINT('Ctrl Pts',(66.4230004670278,23.1615390254632,0.));
#171441=CARTESIAN_POINT('Ctrl Pts',(66.4026849481232,23.160344429474,0.));
#171442=CARTESIAN_POINT('Ctrl Pts',(66.3824226081801,23.1591314230083,0.));
#171443=CARTESIAN_POINT('Ctrl Pts',(66.3622136300654,23.1579001063424,0.));
#171444=CARTESIAN_POINT('Ctrl Pts',(66.3420581937147,23.1566505784621,0.));
#171445=CARTESIAN_POINT('Ctrl Pts',(66.3219564725184,23.1553829352539,0.));
#171446=CARTESIAN_POINT('Ctrl Pts',(66.3019086275444,23.1540972666191,0.));
#171447=CARTESIAN_POINT('Ctrl Pts',(66.281914813114,23.1527936592651,0.));
#171448=CARTESIAN_POINT('Ctrl Pts',(66.2619751878793,23.1514722022503,0.));
#171449=CARTESIAN_POINT('Ctrl Pts',(66.2420899237318,23.1501329914488,0.));
#171450=CARTESIAN_POINT('Ctrl Pts',(66.2222592165398,23.1487761349298,0.));
#171451=CARTESIAN_POINT('Ctrl Pts',(66.2024832934733,23.147401756643,0.));
#171452=CARTESIAN_POINT('Ctrl Pts',(66.1827623902755,23.1460099850704,0.));
#171453=CARTESIAN_POINT('Ctrl Pts',(66.163096729667,23.1446009424871,0.));
#171454=CARTESIAN_POINT('Ctrl Pts',(66.14348650151,23.1431747350127,0.));
#171455=CARTESIAN_POINT('Ctrl Pts',(66.1239318368803,23.1417314398501,0.));
#171456=CARTESIAN_POINT('Ctrl Pts',(66.1044328067739,23.140271103958,0.));
#171457=CARTESIAN_POINT('Ctrl Pts',(66.0888781152779,23.1390892229923,0.));
#171458=CARTESIAN_POINT('Ctrl Pts',(66.0772371487475,23.1381951597491,0.));
#171459=CARTESIAN_POINT('Ctrl Pts',(66.0694876382212,23.1375957166138,0.));
#171460=CARTESIAN_POINT('Ctrl Pts',(66.0656156664138,23.1372951448024,0.));
#171461=CARTESIAN_POINT('Ctrl Pts',(72.5962692526112,16.7341474417544,0.));
#171462=CARTESIAN_POINT('Ctrl Pts',(72.5962692526112,16.7341474417544,12.));
#171463=CARTESIAN_POINT('Ctrl Pts',(72.5907910746008,16.7352885767485,0.));
#171464=CARTESIAN_POINT('Ctrl Pts',(72.5907910746008,16.7352885767485,12.));
#171465=CARTESIAN_POINT('Ctrl Pts',(72.5798376087774,16.7375676985344,0.));
#171466=CARTESIAN_POINT('Ctrl Pts',(72.5798376087774,16.7375676985344,12.));
#171467=CARTESIAN_POINT('Ctrl Pts',(72.5634160806351,16.7409769366072,0.));
#171468=CARTESIAN_POINT('Ctrl Pts',(72.5634160806351,16.7409769366072,12.));
#171469=CARTESIAN_POINT('Ctrl Pts',(72.5415380516637,16.7455036973866,0.));
#171470=CARTESIAN_POINT('Ctrl Pts',(72.5415380516637,16.7455036973866,12.));
#171471=CARTESIAN_POINT('Ctrl Pts',(72.514219427383,16.7511306618915,0.));
#171472=CARTESIAN_POINT('Ctrl Pts',(72.514219427383,16.7511306618915,12.));
#171473=CARTESIAN_POINT('Ctrl Pts',(72.4869297342427,16.7567261380687,0.));
#171474=CARTESIAN_POINT('Ctrl Pts',(72.4869297342427,16.7567261380687,12.));
#171475=CARTESIAN_POINT('Ctrl Pts',(72.4596690055437,16.7622901280758,0.));
#171476=CARTESIAN_POINT('Ctrl Pts',(72.4596690055437,16.7622901280758,12.));
#171477=CARTESIAN_POINT('Ctrl Pts',(72.4324372916746,16.7678226404162,0.));
#171478=CARTESIAN_POINT('Ctrl Pts',(72.4324372916746,16.7678226404162,12.));
#171479=CARTESIAN_POINT('Ctrl Pts',(72.4052346647799,16.7733236932135,0.));
#171480=CARTESIAN_POINT('Ctrl Pts',(72.4052346647799,16.7733236932135,12.));
#171481=CARTESIAN_POINT('Ctrl Pts',(72.3780612167786,16.7787933137498,0.));
#171482=CARTESIAN_POINT('Ctrl Pts',(72.3780612167786,16.7787933137498,12.));
#171483=CARTESIAN_POINT('Ctrl Pts',(72.3509170522838,16.7842315351363,0.));
#171484=CARTESIAN_POINT('Ctrl Pts',(72.3509170522838,16.7842315351363,12.));
#171485=CARTESIAN_POINT('Ctrl Pts',(72.3238022829223,16.7896383937822,0.));
#171486=CARTESIAN_POINT('Ctrl Pts',(72.3238022829223,16.7896383937822,12.));
#171487=CARTESIAN_POINT('Ctrl Pts',(72.2967170212353,16.7950139266122,0.));
#171488=CARTESIAN_POINT('Ctrl Pts',(72.2967170212353,16.7950139266122,12.));
#171489=CARTESIAN_POINT('Ctrl Pts',(72.2696613743782,16.8003581682248,0.));
#171490=CARTESIAN_POINT('Ctrl Pts',(72.2696613743782,16.8003581682248,12.));
#171491=CARTESIAN_POINT('Ctrl Pts',(72.2426354390213,16.8056711485821,0.));
#171492=CARTESIAN_POINT('Ctrl Pts',(72.2426354390213,16.8056711485821,12.));
#171493=CARTESIAN_POINT('Ctrl Pts',(72.2156393048975,16.8109528945896,0.));
#171494=CARTESIAN_POINT('Ctrl Pts',(72.2156393048975,16.8109528945896,12.));
#171495=CARTESIAN_POINT('Ctrl Pts',(72.1886730573452,16.8162034312269,0.));
#171496=CARTESIAN_POINT('Ctrl Pts',(72.1886730573452,16.8162034312269,12.));
#171497=CARTESIAN_POINT('Ctrl Pts',(72.1617367803235,16.8214227828943,0.));
#171498=CARTESIAN_POINT('Ctrl Pts',(72.1617367803235,16.8214227828943,12.));
#171499=CARTESIAN_POINT('Ctrl Pts',(72.13483055902,16.8266109745795,0.));
#171500=CARTESIAN_POINT('Ctrl Pts',(72.13483055902,16.8266109745795,12.));
#171501=CARTESIAN_POINT('Ctrl Pts',(72.1079544831513,16.8317680333404,0.));
#171502=CARTESIAN_POINT('Ctrl Pts',(72.1079544831513,16.8317680333404,12.));
#171503=CARTESIAN_POINT('Ctrl Pts',(72.0811086466121,16.8368939881446,0.));
#171504=CARTESIAN_POINT('Ctrl Pts',(72.0811086466121,16.8368939881446,12.));
#171505=CARTESIAN_POINT('Ctrl Pts',(72.0542931459825,16.8419888691976,0.));
#171506=CARTESIAN_POINT('Ctrl Pts',(72.0542931459825,16.8419888691976,12.));
#171507=CARTESIAN_POINT('Ctrl Pts',(72.0275080793727,16.8470527074275,0.));
#171508=CARTESIAN_POINT('Ctrl Pts',(72.0275080793727,16.8470527074275,12.));
#171509=CARTESIAN_POINT('Ctrl Pts',(72.0007535452081,16.8520855339446,0.));
#171510=CARTESIAN_POINT('Ctrl Pts',(72.0007535452081,16.8520855339446,12.));
#171511=CARTESIAN_POINT('Ctrl Pts',(71.9740296408347,16.8570873794269,0.));
#171512=CARTESIAN_POINT('Ctrl Pts',(71.9740296408347,16.8570873794269,12.));
#171513=CARTESIAN_POINT('Ctrl Pts',(71.9473364618922,16.8620582738437,0.));
#171514=CARTESIAN_POINT('Ctrl Pts',(71.9473364618922,16.8620582738437,12.));
#171515=CARTESIAN_POINT('Ctrl Pts',(71.9206741030887,16.866998246792,0.));
#171516=CARTESIAN_POINT('Ctrl Pts',(71.9206741030887,16.866998246792,12.));
#171517=CARTESIAN_POINT('Ctrl Pts',(71.8940426586534,16.871907327697,0.));
#171518=CARTESIAN_POINT('Ctrl Pts',(71.8940426586534,16.871907327697,12.));
#171519=CARTESIAN_POINT('Ctrl Pts',(71.867442222915,16.87678554607,0.));
#171520=CARTESIAN_POINT('Ctrl Pts',(71.867442222915,16.87678554607,12.));
#171521=CARTESIAN_POINT('Ctrl Pts',(71.8408728908258,16.8816329317471,0.));
#171522=CARTESIAN_POINT('Ctrl Pts',(71.8408728908258,16.8816329317471,12.));
#171523=CARTESIAN_POINT('Ctrl Pts',(71.8143347584962,16.8864495151344,0.));
#171524=CARTESIAN_POINT('Ctrl Pts',(71.8143347584962,16.8864495151344,12.));
#171525=CARTESIAN_POINT('Ctrl Pts',(71.7878279229546,16.8912353270942,0.));
#171526=CARTESIAN_POINT('Ctrl Pts',(71.7878279229546,16.8912353270942,12.));
#171527=CARTESIAN_POINT('Ctrl Pts',(71.7613524819235,16.895990398841,0.));
#171528=CARTESIAN_POINT('Ctrl Pts',(71.7613524819235,16.895990398841,12.));
#171529=CARTESIAN_POINT('Ctrl Pts',(71.7349085335796,16.9007147618344,0.));
#171530=CARTESIAN_POINT('Ctrl Pts',(71.7349085335796,16.9007147618344,12.));
#171531=CARTESIAN_POINT('Ctrl Pts',(71.7084961763357,16.9054084476847,0.));
#171532=CARTESIAN_POINT('Ctrl Pts',(71.7084961763357,16.9054084476847,12.));
#171533=CARTESIAN_POINT('Ctrl Pts',(71.6821155085612,16.9100714880368,0.));
#171534=CARTESIAN_POINT('Ctrl Pts',(71.6821155085612,16.9100714880368,12.));
#171535=CARTESIAN_POINT('Ctrl Pts',(71.6557666285917,16.9147039145717,0.));
#171536=CARTESIAN_POINT('Ctrl Pts',(71.6557666285917,16.9147039145717,12.));
#171537=CARTESIAN_POINT('Ctrl Pts',(71.6294496348653,16.9193057590607,0.));
#171538=CARTESIAN_POINT('Ctrl Pts',(71.6294496348653,16.9193057590607,12.));
#171539=CARTESIAN_POINT('Ctrl Pts',(71.6031646260174,16.9238770534071,0.));
#171540=CARTESIAN_POINT('Ctrl Pts',(71.6031646260174,16.9238770534071,12.));
#171541=CARTESIAN_POINT('Ctrl Pts',(71.5769117009842,16.9284178296933,0.));
#171542=CARTESIAN_POINT('Ctrl Pts',(71.5769117009842,16.9284178296933,12.));
#171543=CARTESIAN_POINT('Ctrl Pts',(71.5506909591129,16.9329281202377,0.));
#171544=CARTESIAN_POINT('Ctrl Pts',(71.5506909591129,16.9329281202377,12.));
#171545=CARTESIAN_POINT('Ctrl Pts',(71.5245025002139,16.9374079576201,0.));
#171546=CARTESIAN_POINT('Ctrl Pts',(71.5245025002139,16.9374079576201,12.));
#171547=CARTESIAN_POINT('Ctrl Pts',(71.4983464245055,16.9418573746489,0.));
#171548=CARTESIAN_POINT('Ctrl Pts',(71.4983464245055,16.9418573746489,12.));
#171549=CARTESIAN_POINT('Ctrl Pts',(71.4722228325794,16.9462764043443,0.));
#171550=CARTESIAN_POINT('Ctrl Pts',(71.4722228325794,16.9462764043443,12.));
#171551=CARTESIAN_POINT('Ctrl Pts',(71.4461318253563,16.9506650799189,0.));
#171552=CARTESIAN_POINT('Ctrl Pts',(71.4461318253563,16.9506650799189,12.));
#171553=CARTESIAN_POINT('Ctrl Pts',(71.4200735040384,16.9550234347621,0.));
#171554=CARTESIAN_POINT('Ctrl Pts',(71.4200735040384,16.9550234347621,12.));
#171555=CARTESIAN_POINT('Ctrl Pts',(71.3940479700677,16.9593515024276,0.));
#171556=CARTESIAN_POINT('Ctrl Pts',(71.3940479700677,16.9593515024276,12.));
#171557=CARTESIAN_POINT('Ctrl Pts',(71.3680553251562,16.9636493166397,0.));
#171558=CARTESIAN_POINT('Ctrl Pts',(71.3680553251562,16.9636493166397,12.));
#171559=CARTESIAN_POINT('Ctrl Pts',(71.3420956713082,16.9679169112994,0.));
#171560=CARTESIAN_POINT('Ctrl Pts',(71.3420956713082,16.9679169112994,12.));
#171561=CARTESIAN_POINT('Ctrl Pts',(71.3161691108427,16.9721543204951,0.));
#171562=CARTESIAN_POINT('Ctrl Pts',(71.3161691108427,16.9721543204951,12.));
#171563=CARTESIAN_POINT('Ctrl Pts',(71.290275746412,16.9763615785137,0.));
#171564=CARTESIAN_POINT('Ctrl Pts',(71.290275746412,16.9763615785137,12.));
#171565=CARTESIAN_POINT('Ctrl Pts',(71.2644156810198,16.9805387198571,0.));
#171566=CARTESIAN_POINT('Ctrl Pts',(71.2644156810198,16.9805387198571,12.));
#171567=CARTESIAN_POINT('Ctrl Pts',(71.2385890180221,16.9846857792384,0.));
#171568=CARTESIAN_POINT('Ctrl Pts',(71.2385890180221,16.9846857792384,12.));
#171569=CARTESIAN_POINT('Ctrl Pts',(71.212795861124,16.9888027915742,0.));
#171570=CARTESIAN_POINT('Ctrl Pts',(71.212795861124,16.9888027915742,12.));
#171571=CARTESIAN_POINT('Ctrl Pts',(71.187036314374,16.9928897919828,0.));
#171572=CARTESIAN_POINT('Ctrl Pts',(71.187036314374,16.9928897919828,12.));
#171573=CARTESIAN_POINT('Ctrl Pts',(71.1613104821568,16.9969468157824,0.));
#171574=CARTESIAN_POINT('Ctrl Pts',(71.1613104821568,16.9969468157824,12.));
#171575=CARTESIAN_POINT('Ctrl Pts',(71.1356184691806,17.0009738984936,0.));
#171576=CARTESIAN_POINT('Ctrl Pts',(71.1356184691806,17.0009738984936,12.));
#171577=CARTESIAN_POINT('Ctrl Pts',(71.1099603804786,17.0049710758394,0.));
#171578=CARTESIAN_POINT('Ctrl Pts',(71.1099603804786,17.0049710758394,12.));
#171579=CARTESIAN_POINT('Ctrl Pts',(71.0843363214221,17.0089383837437,0.));
#171580=CARTESIAN_POINT('Ctrl Pts',(71.0843363214221,17.0089383837437,12.));
#171581=CARTESIAN_POINT('Ctrl Pts',(71.0587463977268,17.0128758583335,0.));
#171582=CARTESIAN_POINT('Ctrl Pts',(71.0587463977268,17.0128758583335,12.));
#171583=CARTESIAN_POINT('Ctrl Pts',(71.0331907154574,17.0167835359419,0.));
#171584=CARTESIAN_POINT('Ctrl Pts',(71.0331907154574,17.0167835359419,12.));
#171585=CARTESIAN_POINT('Ctrl Pts',(71.0076693810301,17.0206614531166,0.));
#171586=CARTESIAN_POINT('Ctrl Pts',(71.0076693810301,17.0206614531166,12.));
#171587=CARTESIAN_POINT('Ctrl Pts',(70.9821825012136,17.0245096466229,0.));
#171588=CARTESIAN_POINT('Ctrl Pts',(70.9821825012136,17.0245096466229,12.));
#171589=CARTESIAN_POINT('Ctrl Pts',(70.956730183136,17.0283281534392,0.));
#171590=CARTESIAN_POINT('Ctrl Pts',(70.956730183136,17.0283281534392,12.));
#171591=CARTESIAN_POINT('Ctrl Pts',(70.9313125342876,17.0321170107564,0.));
#171592=CARTESIAN_POINT('Ctrl Pts',(70.9313125342876,17.0321170107564,12.));
#171593=CARTESIAN_POINT('Ctrl Pts',(70.9059296625214,17.0358762559786,0.));
#171594=CARTESIAN_POINT('Ctrl Pts',(70.9059296625214,17.0358762559786,12.));
#171595=CARTESIAN_POINT('Ctrl Pts',(70.8805816760501,17.0396059267277,0.));
#171596=CARTESIAN_POINT('Ctrl Pts',(70.8805816760501,17.0396059267277,12.));
#171597=CARTESIAN_POINT('Ctrl Pts',(70.8552686834423,17.0433060608475,0.));
#171598=CARTESIAN_POINT('Ctrl Pts',(70.8552686834423,17.0433060608475,12.));
#171599=CARTESIAN_POINT('Ctrl Pts',(70.8299907936334,17.0469766964001,0.));
#171600=CARTESIAN_POINT('Ctrl Pts',(70.8299907936334,17.0469766964001,12.));
#171601=CARTESIAN_POINT('Ctrl Pts',(70.8047481159298,17.0506178716662,0.));
#171602=CARTESIAN_POINT('Ctrl Pts',(70.8047481159298,17.0506178716662,12.));
#171603=CARTESIAN_POINT('Ctrl Pts',(70.7795407600127,17.0542296251462,0.));
#171604=CARTESIAN_POINT('Ctrl Pts',(70.7795407600127,17.0542296251462,12.));
#171605=CARTESIAN_POINT('Ctrl Pts',(70.754368835938,17.0578119955651,0.));
#171606=CARTESIAN_POINT('Ctrl Pts',(70.754368835938,17.0578119955651,12.));
#171607=CARTESIAN_POINT('Ctrl Pts',(70.7292324541348,17.0613650218789,0.));
#171608=CARTESIAN_POINT('Ctrl Pts',(70.7292324541348,17.0613650218789,12.));
#171609=CARTESIAN_POINT('Ctrl Pts',(70.7041317254128,17.0648887432714,0.));
#171610=CARTESIAN_POINT('Ctrl Pts',(70.7041317254128,17.0648887432714,12.));
#171611=CARTESIAN_POINT('Ctrl Pts',(70.6790667609678,17.0683831991532,0.));
#171612=CARTESIAN_POINT('Ctrl Pts',(70.6790667609678,17.0683831991532,12.));
#171613=CARTESIAN_POINT('Ctrl Pts',(70.6540376723839,17.0718484291623,0.));
#171614=CARTESIAN_POINT('Ctrl Pts',(70.6540376723839,17.0718484291623,12.));
#171615=CARTESIAN_POINT('Ctrl Pts',(70.6290445716341,17.0752844731679,0.));
#171616=CARTESIAN_POINT('Ctrl Pts',(70.6290445716341,17.0752844731679,12.));
#171617=CARTESIAN_POINT('Ctrl Pts',(70.6040875710762,17.0786913712767,0.));
#171618=CARTESIAN_POINT('Ctrl Pts',(70.6040875710762,17.0786913712767,12.));
#171619=CARTESIAN_POINT('Ctrl Pts',(70.5791667834599,17.0820691638314,0.));
#171620=CARTESIAN_POINT('Ctrl Pts',(70.5791667834599,17.0820691638314,12.));
#171621=CARTESIAN_POINT('Ctrl Pts',(70.5542823219346,17.085417891409,0.));
#171622=CARTESIAN_POINT('Ctrl Pts',(70.5542823219346,17.085417891409,12.));
#171623=CARTESIAN_POINT('Ctrl Pts',(70.5294343000516,17.0887375948221,0.));
#171624=CARTESIAN_POINT('Ctrl Pts',(70.5294343000516,17.0887375948221,12.));
#171625=CARTESIAN_POINT('Ctrl Pts',(70.5046228317669,17.0920283151217,0.));
#171626=CARTESIAN_POINT('Ctrl Pts',(70.5046228317669,17.0920283151217,12.));
#171627=CARTESIAN_POINT('Ctrl Pts',(70.4798480314364,17.0952900936044,0.));
#171628=CARTESIAN_POINT('Ctrl Pts',(70.4798480314364,17.0952900936044,12.));
#171629=CARTESIAN_POINT('Ctrl Pts',(70.4551100138221,17.098522971812,0.));
#171630=CARTESIAN_POINT('Ctrl Pts',(70.4551100138221,17.098522971812,12.));
#171631=CARTESIAN_POINT('Ctrl Pts',(70.4304088940998,17.1017269915289,0.));
#171632=CARTESIAN_POINT('Ctrl Pts',(70.4304088940998,17.1017269915289,12.));
#171633=CARTESIAN_POINT('Ctrl Pts',(70.4057447878621,17.1049021947833,0.));
#171634=CARTESIAN_POINT('Ctrl Pts',(70.4057447878621,17.1049021947833,12.));
#171635=CARTESIAN_POINT('Ctrl Pts',(70.3811178111206,17.10804862385,0.));
#171636=CARTESIAN_POINT('Ctrl Pts',(70.3811178111206,17.10804862385,12.));
#171637=CARTESIAN_POINT('Ctrl Pts',(70.356528080303,17.111166321257,0.));
#171638=CARTESIAN_POINT('Ctrl Pts',(70.356528080303,17.111166321257,12.));
#171639=CARTESIAN_POINT('Ctrl Pts',(70.3319757122577,17.1142553297869,0.));
#171640=CARTESIAN_POINT('Ctrl Pts',(70.3319757122577,17.1142553297869,12.));
#171641=CARTESIAN_POINT('Ctrl Pts',(70.3074608242613,17.1173156924734,0.));
#171642=CARTESIAN_POINT('Ctrl Pts',(70.3074608242613,17.1173156924734,12.));
#171643=CARTESIAN_POINT('Ctrl Pts',(70.2829835340239,17.1203474526031,0.));
#171644=CARTESIAN_POINT('Ctrl Pts',(70.2829835340239,17.1203474526031,12.));
#171645=CARTESIAN_POINT('Ctrl Pts',(70.2585439596899,17.1233506537176,0.));
#171646=CARTESIAN_POINT('Ctrl Pts',(70.2585439596899,17.1233506537176,12.));
#171647=CARTESIAN_POINT('Ctrl Pts',(70.2341422198363,17.1263253396202,0.));
#171648=CARTESIAN_POINT('Ctrl Pts',(70.2341422198363,17.1263253396202,12.));
#171649=CARTESIAN_POINT('Ctrl Pts',(70.2097784334749,17.1292715543779,0.));
#171650=CARTESIAN_POINT('Ctrl Pts',(70.2097784334749,17.1292715543779,12.));
#171651=CARTESIAN_POINT('Ctrl Pts',(70.1854527200636,17.1321893423183,0.));
#171652=CARTESIAN_POINT('Ctrl Pts',(70.1854527200636,17.1321893423183,12.));
#171653=CARTESIAN_POINT('Ctrl Pts',(70.1611651995085,17.1350787480313,0.));
#171654=CARTESIAN_POINT('Ctrl Pts',(70.1611651995085,17.1350787480313,12.));
#171655=CARTESIAN_POINT('Ctrl Pts',(70.1369159921686,17.1379398163708,0.));
#171656=CARTESIAN_POINT('Ctrl Pts',(70.1369159921686,17.1379398163708,12.));
#171657=CARTESIAN_POINT('Ctrl Pts',(70.1127052188515,17.1407725924615,0.));
#171658=CARTESIAN_POINT('Ctrl Pts',(70.1127052188515,17.1407725924615,12.));
#171659=CARTESIAN_POINT('Ctrl Pts',(70.0885330008169,17.1435771217015,0.));
#171660=CARTESIAN_POINT('Ctrl Pts',(70.0885330008169,17.1435771217015,12.));
#171661=CARTESIAN_POINT('Ctrl Pts',(70.0643994597865,17.1463534497592,0.));
#171662=CARTESIAN_POINT('Ctrl Pts',(70.0643994597865,17.1463534497592,12.));
#171663=CARTESIAN_POINT('Ctrl Pts',(70.0403047179481,17.1491016225748,0.));
#171664=CARTESIAN_POINT('Ctrl Pts',(70.0403047179481,17.1491016225748,12.));
#171665=CARTESIAN_POINT('Ctrl Pts',(70.0162488979587,17.1518216863624,0.));
#171666=CARTESIAN_POINT('Ctrl Pts',(70.0162488979587,17.1518216863624,12.));
#171667=CARTESIAN_POINT('Ctrl Pts',(69.9922321229428,17.1545136876162,0.));
#171668=CARTESIAN_POINT('Ctrl Pts',(69.9922321229428,17.1545136876162,12.));
#171669=CARTESIAN_POINT('Ctrl Pts',(69.9682545164942,17.157177673114,0.));
#171670=CARTESIAN_POINT('Ctrl Pts',(69.9682545164942,17.157177673114,12.));
#171671=CARTESIAN_POINT('Ctrl Pts',(69.9443162026865,17.1598136899144,0.));
#171672=CARTESIAN_POINT('Ctrl Pts',(69.9443162026865,17.1598136899144,12.));
#171673=CARTESIAN_POINT('Ctrl Pts',(69.9204173060779,17.1624217853577,0.));
#171674=CARTESIAN_POINT('Ctrl Pts',(69.9204173060779,17.1624217853577,12.));
#171675=CARTESIAN_POINT('Ctrl Pts',(69.8965579517147,17.1650020070686,0.));
#171676=CARTESIAN_POINT('Ctrl Pts',(69.8965579517147,17.1650020070686,12.));
#171677=CARTESIAN_POINT('Ctrl Pts',(69.8727382651292,17.1675544029622,0.));
#171678=CARTESIAN_POINT('Ctrl Pts',(69.8727382651292,17.1675544029622,12.));
#171679=CARTESIAN_POINT('Ctrl Pts',(69.8489583723417,17.1700790212476,0.));
#171680=CARTESIAN_POINT('Ctrl Pts',(69.8489583723417,17.1700790212476,12.));
#171681=CARTESIAN_POINT('Ctrl Pts',(69.8252183998713,17.1725759104254,0.));
#171682=CARTESIAN_POINT('Ctrl Pts',(69.8252183998713,17.1725759104254,12.));
#171683=CARTESIAN_POINT('Ctrl Pts',(69.8015184747404,17.1750451192887,0.));
#171684=CARTESIAN_POINT('Ctrl Pts',(69.8015184747404,17.1750451192887,12.));
#171685=CARTESIAN_POINT('Ctrl Pts',(69.7778587244788,17.1774866969256,0.));
#171686=CARTESIAN_POINT('Ctrl Pts',(69.7778587244788,17.1774866969256,12.));
#171687=CARTESIAN_POINT('Ctrl Pts',(69.7542392771216,17.1799006927256,0.));
#171688=CARTESIAN_POINT('Ctrl Pts',(69.7542392771216,17.1799006927256,12.));
#171689=CARTESIAN_POINT('Ctrl Pts',(69.7306602612125,17.1822871563835,0.));
#171690=CARTESIAN_POINT('Ctrl Pts',(69.7306602612125,17.1822871563835,12.));
#171691=CARTESIAN_POINT('Ctrl Pts',(69.7071218058149,17.1846461378966,0.));
#171692=CARTESIAN_POINT('Ctrl Pts',(69.7071218058149,17.1846461378966,12.));
#171693=CARTESIAN_POINT('Ctrl Pts',(69.6836240405152,17.1869776875663,0.));
#171694=CARTESIAN_POINT('Ctrl Pts',(69.6836240405152,17.1869776875663,12.));
#171695=CARTESIAN_POINT('Ctrl Pts',(69.6601670954277,17.1892818560004,0.));
#171696=CARTESIAN_POINT('Ctrl Pts',(69.6601670954277,17.1892818560004,12.));
#171697=CARTESIAN_POINT('Ctrl Pts',(69.6367511011927,17.1915586941198,0.));
#171698=CARTESIAN_POINT('Ctrl Pts',(69.6367511011927,17.1915586941198,12.));
#171699=CARTESIAN_POINT('Ctrl Pts',(69.6133761889787,17.193808253162,0.));
#171700=CARTESIAN_POINT('Ctrl Pts',(69.6133761889787,17.193808253162,12.));
#171701=CARTESIAN_POINT('Ctrl Pts',(69.5900424904954,17.1960305846787,0.));
#171702=CARTESIAN_POINT('Ctrl Pts',(69.5900424904954,17.1960305846787,12.));
#171703=CARTESIAN_POINT('Ctrl Pts',(69.5667501379984,17.198225740538,0.));
#171704=CARTESIAN_POINT('Ctrl Pts',(69.5667501379984,17.198225740538,12.));
#171705=CARTESIAN_POINT('Ctrl Pts',(69.5434992642932,17.2003937729266,0.));
#171706=CARTESIAN_POINT('Ctrl Pts',(69.5434992642932,17.2003937729266,12.));
#171707=CARTESIAN_POINT('Ctrl Pts',(69.5202900027329,17.2025347343568,0.));
#171708=CARTESIAN_POINT('Ctrl Pts',(69.5202900027329,17.2025347343568,12.));
#171709=CARTESIAN_POINT('Ctrl Pts',(69.497122487222,17.2046486776697,0.));
#171710=CARTESIAN_POINT('Ctrl Pts',(69.497122487222,17.2046486776697,12.));
#171711=CARTESIAN_POINT('Ctrl Pts',(69.4739968522271,17.2067356560326,0.));
#171712=CARTESIAN_POINT('Ctrl Pts',(69.4739968522271,17.2067356560326,12.));
#171713=CARTESIAN_POINT('Ctrl Pts',(69.4509132327836,17.208795722942,0.));
#171714=CARTESIAN_POINT('Ctrl Pts',(69.4509132327836,17.208795722942,12.));
#171715=CARTESIAN_POINT('Ctrl Pts',(69.4278717644989,17.2108289322258,0.));
#171716=CARTESIAN_POINT('Ctrl Pts',(69.4278717644989,17.2108289322258,12.));
#171717=CARTESIAN_POINT('Ctrl Pts',(69.4048725835516,17.2128353380511,0.));
#171718=CARTESIAN_POINT('Ctrl Pts',(69.4048725835516,17.2128353380511,12.));
#171719=CARTESIAN_POINT('Ctrl Pts',(69.3819158266955,17.2148149949261,0.));
#171720=CARTESIAN_POINT('Ctrl Pts',(69.3819158266955,17.2148149949261,12.));
#171721=CARTESIAN_POINT('Ctrl Pts',(69.359001631272,17.2167679576991,0.));
#171722=CARTESIAN_POINT('Ctrl Pts',(69.359001631272,17.2167679576991,12.));
#171723=CARTESIAN_POINT('Ctrl Pts',(69.3361301352149,17.2186942815604,0.));
#171724=CARTESIAN_POINT('Ctrl Pts',(69.3361301352149,17.2186942815604,12.));
#171725=CARTESIAN_POINT('Ctrl Pts',(69.3133014770541,17.2205940220455,0.));
#171726=CARTESIAN_POINT('Ctrl Pts',(69.3133014770541,17.2205940220455,12.));
#171727=CARTESIAN_POINT('Ctrl Pts',(69.2905157959142,17.2224672350432,0.));
#171728=CARTESIAN_POINT('Ctrl Pts',(69.2905157959142,17.2224672350432,12.));
#171729=CARTESIAN_POINT('Ctrl Pts',(69.26777323152,17.2243139767963,0.));
#171730=CARTESIAN_POINT('Ctrl Pts',(69.26777323152,17.2243139767963,12.));
#171731=CARTESIAN_POINT('Ctrl Pts',(69.2450739242092,17.2261343039015,0.));
#171732=CARTESIAN_POINT('Ctrl Pts',(69.2450739242092,17.2261343039015,12.));
#171733=CARTESIAN_POINT('Ctrl Pts',(69.2224180149377,17.2279282733119,0.));
#171734=CARTESIAN_POINT('Ctrl Pts',(69.2224180149377,17.2279282733119,12.));
#171735=CARTESIAN_POINT('Ctrl Pts',(69.1998056452837,17.229695942341,0.));
#171736=CARTESIAN_POINT('Ctrl Pts',(69.1998056452837,17.229695942341,12.));
#171737=CARTESIAN_POINT('Ctrl Pts',(69.1772369574462,17.2314373686705,0.));
#171738=CARTESIAN_POINT('Ctrl Pts',(69.1772369574462,17.2314373686705,12.));
#171739=CARTESIAN_POINT('Ctrl Pts',(69.1547120942542,17.2331526103511,0.));
#171740=CARTESIAN_POINT('Ctrl Pts',(69.1547120942542,17.2331526103511,12.));
#171741=CARTESIAN_POINT('Ctrl Pts',(69.1322311991759,17.2348417258017,0.));
#171742=CARTESIAN_POINT('Ctrl Pts',(69.1322311991759,17.2348417258017,12.));
#171743=CARTESIAN_POINT('Ctrl Pts',(69.1097944163243,17.2365047738125,0.));
#171744=CARTESIAN_POINT('Ctrl Pts',(69.1097944163243,17.2365047738125,12.));
#171745=CARTESIAN_POINT('Ctrl Pts',(69.0874018904598,17.238141813549,0.));
#171746=CARTESIAN_POINT('Ctrl Pts',(69.0874018904598,17.238141813549,12.));
#171747=CARTESIAN_POINT('Ctrl Pts',(69.0650537669859,17.2397529045587,0.));
#171748=CARTESIAN_POINT('Ctrl Pts',(69.0650537669859,17.2397529045587,12.));
#171749=CARTESIAN_POINT('Ctrl Pts',(69.0427501919636,17.2413381067722,0.));
#171750=CARTESIAN_POINT('Ctrl Pts',(69.0427501919636,17.2413381067722,12.));
#171751=CARTESIAN_POINT('Ctrl Pts',(69.0204913121226,17.2428974805043,0.));
#171752=CARTESIAN_POINT('Ctrl Pts',(69.0204913121226,17.2428974805043,12.));
#171753=CARTESIAN_POINT('Ctrl Pts',(68.9982772748694,17.2444310864585,0.));
#171754=CARTESIAN_POINT('Ctrl Pts',(68.9982772748694,17.2444310864585,12.));
#171755=CARTESIAN_POINT('Ctrl Pts',(68.9761082282922,17.2459389857327,0.));
#171756=CARTESIAN_POINT('Ctrl Pts',(68.9761082282922,17.2459389857327,12.));
#171757=CARTESIAN_POINT('Ctrl Pts',(68.9539843211618,17.2474212398275,0.));
#171758=CARTESIAN_POINT('Ctrl Pts',(68.9539843211618,17.2474212398275,12.));
#171759=CARTESIAN_POINT('Ctrl Pts',(68.9319057029407,17.248877910643,0.));
#171760=CARTESIAN_POINT('Ctrl Pts',(68.9319057029407,17.248877910643,12.));
#171761=CARTESIAN_POINT('Ctrl Pts',(68.9098725237868,17.2503090604792,0.));
#171762=CARTESIAN_POINT('Ctrl Pts',(68.9098725237868,17.2503090604792,12.));
#171763=CARTESIAN_POINT('Ctrl Pts',(68.8878849345557,17.2517147520376,0.));
#171764=CARTESIAN_POINT('Ctrl Pts',(68.8878849345557,17.2517147520376,12.));
#171765=CARTESIAN_POINT('Ctrl Pts',(68.8659430867977,17.2530950484259,0.));
#171766=CARTESIAN_POINT('Ctrl Pts',(68.8659430867977,17.2530950484259,12.));
#171767=CARTESIAN_POINT('Ctrl Pts',(68.8440471327563,17.2544500131627,0.));
#171768=CARTESIAN_POINT('Ctrl Pts',(68.8440471327563,17.2544500131627,12.));
#171769=CARTESIAN_POINT('Ctrl Pts',(68.8221972253954,17.2557797101816,0.));
#171770=CARTESIAN_POINT('Ctrl Pts',(68.8221972253954,17.2557797101816,12.));
#171771=CARTESIAN_POINT('Ctrl Pts',(68.8003935184193,17.2570842038386,0.));
#171772=CARTESIAN_POINT('Ctrl Pts',(68.8003935184193,17.2570842038386,12.));
#171773=CARTESIAN_POINT('Ctrl Pts',(68.7786361662876,17.2583635589197,0.));
#171774=CARTESIAN_POINT('Ctrl Pts',(68.7786361662876,17.2583635589197,12.));
#171775=CARTESIAN_POINT('Ctrl Pts',(68.7569253242312,17.2596178406545,0.));
#171776=CARTESIAN_POINT('Ctrl Pts',(68.7569253242312,17.2596178406545,12.));
#171777=CARTESIAN_POINT('Ctrl Pts',(68.7352611482519,17.2608471147178,0.));
#171778=CARTESIAN_POINT('Ctrl Pts',(68.7352611482519,17.2608471147178,12.));
#171779=CARTESIAN_POINT('Ctrl Pts',(68.7136437951075,17.2620514472176,0.));
#171780=CARTESIAN_POINT('Ctrl Pts',(68.7136437951075,17.2620514472176,12.));
#171781=CARTESIAN_POINT('Ctrl Pts',(68.6920734222932,17.263230904689,0.));
#171782=CARTESIAN_POINT('Ctrl Pts',(68.6920734222932,17.263230904689,12.));
#171783=CARTESIAN_POINT('Ctrl Pts',(68.6705501880263,17.2643855540896,0.));
#171784=CARTESIAN_POINT('Ctrl Pts',(68.6705501880263,17.2643855540896,12.));
#171785=CARTESIAN_POINT('Ctrl Pts',(68.6490742512085,17.2655154627935,0.));
#171786=CARTESIAN_POINT('Ctrl Pts',(68.6490742512085,17.2655154627935,12.));
#171787=CARTESIAN_POINT('Ctrl Pts',(68.6276457714757,17.2666206986091,0.));
#171788=CARTESIAN_POINT('Ctrl Pts',(68.6276457714757,17.2666206986091,12.));
#171789=CARTESIAN_POINT('Ctrl Pts',(68.6062649092781,17.2677013298061,0.));
#171790=CARTESIAN_POINT('Ctrl Pts',(68.6062649092781,17.2677013298061,12.));
#171791=CARTESIAN_POINT('Ctrl Pts',(68.5849318259449,17.2687574251429,0.));
#171792=CARTESIAN_POINT('Ctrl Pts',(68.5849318259449,17.2687574251429,12.));
#171793=CARTESIAN_POINT('Ctrl Pts',(68.5636466837502,17.2697890538956,0.));
#171794=CARTESIAN_POINT('Ctrl Pts',(68.5636466837502,17.2697890538956,12.));
#171795=CARTESIAN_POINT('Ctrl Pts',(68.5424096459746,17.2707962858912,0.));
#171796=CARTESIAN_POINT('Ctrl Pts',(68.5424096459746,17.2707962858912,12.));
#171797=CARTESIAN_POINT('Ctrl Pts',(68.5212208767835,17.2717791914538,0.));
#171798=CARTESIAN_POINT('Ctrl Pts',(68.5212208767835,17.2717791914538,12.));
#171799=CARTESIAN_POINT('Ctrl Pts',(68.5000805410897,17.2727378413485,0.));
#171800=CARTESIAN_POINT('Ctrl Pts',(68.5000805410897,17.2727378413485,12.));
#171801=CARTESIAN_POINT('Ctrl Pts',(68.4789888044357,17.2736723067367,0.));
#171802=CARTESIAN_POINT('Ctrl Pts',(68.4789888044357,17.2736723067367,12.));
#171803=CARTESIAN_POINT('Ctrl Pts',(68.4579458328208,17.2745826591125,0.));
#171804=CARTESIAN_POINT('Ctrl Pts',(68.4579458328208,17.2745826591125,12.));
#171805=CARTESIAN_POINT('Ctrl Pts',(68.4369517926803,17.2754689703001,0.));
#171806=CARTESIAN_POINT('Ctrl Pts',(68.4369517926803,17.2754689703001,12.));
#171807=CARTESIAN_POINT('Ctrl Pts',(68.4160068512781,17.2763313126026,0.));
#171808=CARTESIAN_POINT('Ctrl Pts',(68.4160068512781,17.2763313126026,12.));
#171809=CARTESIAN_POINT('Ctrl Pts',(68.3951111770498,17.2771697589387,0.));
#171810=CARTESIAN_POINT('Ctrl Pts',(68.3951111770498,17.2771697589387,12.));
#171811=CARTESIAN_POINT('Ctrl Pts',(68.374264939895,17.2779843829605,0.));
#171812=CARTESIAN_POINT('Ctrl Pts',(68.374264939895,17.2779843829605,12.));
#171813=CARTESIAN_POINT('Ctrl Pts',(68.353468311648,17.2787752592475,0.));
#171814=CARTESIAN_POINT('Ctrl Pts',(68.353468311648,17.2787752592475,12.));
#171815=CARTESIAN_POINT('Ctrl Pts',(68.3327214657533,17.2795424631789,0.));
#171816=CARTESIAN_POINT('Ctrl Pts',(68.3327214657533,17.2795424631789,12.));
#171817=CARTESIAN_POINT('Ctrl Pts',(68.3120245763884,17.2802860705807,0.));
#171818=CARTESIAN_POINT('Ctrl Pts',(68.3120245763884,17.2802860705807,12.));
#171819=CARTESIAN_POINT('Ctrl Pts',(68.2913778177258,17.2810061574352,0.));
#171820=CARTESIAN_POINT('Ctrl Pts',(68.2913778177258,17.2810061574352,12.));
#171821=CARTESIAN_POINT('Ctrl Pts',(68.2707813631761,17.2817027995838,0.));
#171822=CARTESIAN_POINT('Ctrl Pts',(68.2707813631761,17.2817027995838,12.));
#171823=CARTESIAN_POINT('Ctrl Pts',(68.250235384512,17.2823760723886,0.));
#171824=CARTESIAN_POINT('Ctrl Pts',(68.250235384512,17.2823760723886,12.));
#171825=CARTESIAN_POINT('Ctrl Pts',(68.2297400535339,17.2830260513879,0.));
#171826=CARTESIAN_POINT('Ctrl Pts',(68.2297400535339,17.2830260513879,12.));
#171827=CARTESIAN_POINT('Ctrl Pts',(68.2092955440591,17.2836528130825,0.));
#171828=CARTESIAN_POINT('Ctrl Pts',(68.2092955440591,17.2836528130825,12.));
#171829=CARTESIAN_POINT('Ctrl Pts',(68.1889020335418,17.2842564355796,0.));
#171830=CARTESIAN_POINT('Ctrl Pts',(68.1889020335418,17.2842564355796,12.));
#171831=CARTESIAN_POINT('Ctrl Pts',(68.1685597054193,17.2848369995283,0.));
#171832=CARTESIAN_POINT('Ctrl Pts',(68.1685597054193,17.2848369995283,12.));
#171833=CARTESIAN_POINT('Ctrl Pts',(68.1482687493176,17.2853945882059,0.));
#171834=CARTESIAN_POINT('Ctrl Pts',(68.1482687493176,17.2853945882059,12.));
#171835=CARTESIAN_POINT('Ctrl Pts',(68.1280293561473,17.2859292855694,0.));
#171836=CARTESIAN_POINT('Ctrl Pts',(68.1280293561473,17.2859292855694,12.));
#171837=CARTESIAN_POINT('Ctrl Pts',(68.1078417137865,17.2864411745456,0.));
#171838=CARTESIAN_POINT('Ctrl Pts',(68.1078417137865,17.2864411745456,12.));
#171839=CARTESIAN_POINT('Ctrl Pts',(68.0877060033229,17.2869303355438,0.));
#171840=CARTESIAN_POINT('Ctrl Pts',(68.0877060033229,17.2869303355438,12.));
#171841=CARTESIAN_POINT('Ctrl Pts',(68.0676223930469,17.2873968440855,0.));
#171842=CARTESIAN_POINT('Ctrl Pts',(68.0676223930469,17.2873968440855,12.));
#171843=CARTESIAN_POINT('Ctrl Pts',(68.0475910442494,17.2878407730981,0.));
#171844=CARTESIAN_POINT('Ctrl Pts',(68.0475910442494,17.2878407730981,12.));
#171845=CARTESIAN_POINT('Ctrl Pts',(68.027612122741,17.2882621974737,0.));
#171846=CARTESIAN_POINT('Ctrl Pts',(68.027612122741,17.2882621974737,12.));
#171847=CARTESIAN_POINT('Ctrl Pts',(68.007685808115,17.28866119774,0.));
#171848=CARTESIAN_POINT('Ctrl Pts',(68.007685808115,17.28866119774,12.));
#171849=CARTESIAN_POINT('Ctrl Pts',(67.9878123049133,17.2890378644843,0.));
#171850=CARTESIAN_POINT('Ctrl Pts',(67.9878123049133,17.2890378644843,12.));
#171851=CARTESIAN_POINT('Ctrl Pts',(67.9679918502441,17.2893923013852,0.));
#171852=CARTESIAN_POINT('Ctrl Pts',(67.9679918502441,17.2893923013852,12.));
#171853=CARTESIAN_POINT('Ctrl Pts',(67.9482246901517,17.2897246158895,0.));
#171854=CARTESIAN_POINT('Ctrl Pts',(67.9482246901517,17.2897246158895,12.));
#171855=CARTESIAN_POINT('Ctrl Pts',(67.9285110571662,17.2900349103956,0.));
#171856=CARTESIAN_POINT('Ctrl Pts',(67.9285110571662,17.2900349103956,12.));
#171857=CARTESIAN_POINT('Ctrl Pts',(67.908851149676,17.2903232740717,0.));
#171858=CARTESIAN_POINT('Ctrl Pts',(67.908851149676,17.2903232740717,12.));
#171859=CARTESIAN_POINT('Ctrl Pts',(67.8892451049871,17.2905897724029,0.));
#171860=CARTESIAN_POINT('Ctrl Pts',(67.8892451049871,17.2905897724029,12.));
#171861=CARTESIAN_POINT('Ctrl Pts',(67.8696929979178,17.2908344459816,0.));
#171862=CARTESIAN_POINT('Ctrl Pts',(67.8696929979178,17.2908344459816,12.));
#171863=CARTESIAN_POINT('Ctrl Pts',(67.8540944890057,17.2910127431203,0.));
#171864=CARTESIAN_POINT('Ctrl Pts',(67.8540944890057,17.2910127431203,12.));
#171865=CARTESIAN_POINT('Ctrl Pts',(67.8424198971214,17.2911366591419,0.));
#171866=CARTESIAN_POINT('Ctrl Pts',(67.8424198971214,17.2911366591419,12.));
#171867=CARTESIAN_POINT('Ctrl Pts',(67.8346476309106,17.2912149114145,0.));
#171868=CARTESIAN_POINT('Ctrl Pts',(67.8346476309106,17.2912149114145,12.));
#171869=CARTESIAN_POINT('Ctrl Pts',(67.8307641965655,17.2912529479484,0.));
#171870=CARTESIAN_POINT('Ctrl Pts',(67.8307641965655,17.2912529479484,12.));
#171871=CARTESIAN_POINT('',(67.8307641965655,17.2912529479484,12.));
#171872=CARTESIAN_POINT('Ctrl Pts',(67.8307641965655,17.2912529479484,12.));
#171873=CARTESIAN_POINT('Ctrl Pts',(67.8346476309106,17.2912149114145,12.));
#171874=CARTESIAN_POINT('Ctrl Pts',(67.8424198971214,17.2911366591419,12.));
#171875=CARTESIAN_POINT('Ctrl Pts',(67.8540944890057,17.2910127431203,12.));
#171876=CARTESIAN_POINT('Ctrl Pts',(67.8696929979178,17.2908344459816,12.));
#171877=CARTESIAN_POINT('Ctrl Pts',(67.8892451049871,17.2905897724029,12.));
#171878=CARTESIAN_POINT('Ctrl Pts',(67.908851149676,17.2903232740717,12.));
#171879=CARTESIAN_POINT('Ctrl Pts',(67.9285110571662,17.2900349103956,12.));
#171880=CARTESIAN_POINT('Ctrl Pts',(67.9482246901517,17.2897246158895,12.));
#171881=CARTESIAN_POINT('Ctrl Pts',(67.9679918502441,17.2893923013852,12.));
#171882=CARTESIAN_POINT('Ctrl Pts',(67.9878123049133,17.2890378644843,12.));
#171883=CARTESIAN_POINT('Ctrl Pts',(68.007685808115,17.28866119774,12.));
#171884=CARTESIAN_POINT('Ctrl Pts',(68.027612122741,17.2882621974737,12.));
#171885=CARTESIAN_POINT('Ctrl Pts',(68.0475910442494,17.2878407730981,12.));
#171886=CARTESIAN_POINT('Ctrl Pts',(68.0676223930469,17.2873968440855,12.));
#171887=CARTESIAN_POINT('Ctrl Pts',(68.0877060033229,17.2869303355438,12.));
#171888=CARTESIAN_POINT('Ctrl Pts',(68.1078417137865,17.2864411745456,12.));
#171889=CARTESIAN_POINT('Ctrl Pts',(68.1280293561473,17.2859292855694,12.));
#171890=CARTESIAN_POINT('Ctrl Pts',(68.1482687493176,17.2853945882059,12.));
#171891=CARTESIAN_POINT('Ctrl Pts',(68.1685597054193,17.2848369995283,12.));
#171892=CARTESIAN_POINT('Ctrl Pts',(68.1889020335418,17.2842564355796,12.));
#171893=CARTESIAN_POINT('Ctrl Pts',(68.2092955440591,17.2836528130825,12.));
#171894=CARTESIAN_POINT('Ctrl Pts',(68.2297400535339,17.2830260513879,12.));
#171895=CARTESIAN_POINT('Ctrl Pts',(68.250235384512,17.2823760723886,12.));
#171896=CARTESIAN_POINT('Ctrl Pts',(68.2707813631761,17.2817027995838,12.));
#171897=CARTESIAN_POINT('Ctrl Pts',(68.2913778177258,17.2810061574352,12.));
#171898=CARTESIAN_POINT('Ctrl Pts',(68.3120245763884,17.2802860705807,12.));
#171899=CARTESIAN_POINT('Ctrl Pts',(68.3327214657533,17.2795424631789,12.));
#171900=CARTESIAN_POINT('Ctrl Pts',(68.353468311648,17.2787752592475,12.));
#171901=CARTESIAN_POINT('Ctrl Pts',(68.374264939895,17.2779843829605,12.));
#171902=CARTESIAN_POINT('Ctrl Pts',(68.3951111770498,17.2771697589387,12.));
#171903=CARTESIAN_POINT('Ctrl Pts',(68.4160068512781,17.2763313126026,12.));
#171904=CARTESIAN_POINT('Ctrl Pts',(68.4369517926803,17.2754689703001,12.));
#171905=CARTESIAN_POINT('Ctrl Pts',(68.4579458328208,17.2745826591125,12.));
#171906=CARTESIAN_POINT('Ctrl Pts',(68.4789888044357,17.2736723067367,12.));
#171907=CARTESIAN_POINT('Ctrl Pts',(68.5000805410897,17.2727378413485,12.));
#171908=CARTESIAN_POINT('Ctrl Pts',(68.5212208767835,17.2717791914538,12.));
#171909=CARTESIAN_POINT('Ctrl Pts',(68.5424096459746,17.2707962858912,12.));
#171910=CARTESIAN_POINT('Ctrl Pts',(68.5636466837502,17.2697890538956,12.));
#171911=CARTESIAN_POINT('Ctrl Pts',(68.5849318259449,17.2687574251429,12.));
#171912=CARTESIAN_POINT('Ctrl Pts',(68.6062649092781,17.2677013298061,12.));
#171913=CARTESIAN_POINT('Ctrl Pts',(68.6276457714757,17.2666206986091,12.));
#171914=CARTESIAN_POINT('Ctrl Pts',(68.6490742512085,17.2655154627935,12.));
#171915=CARTESIAN_POINT('Ctrl Pts',(68.6705501880263,17.2643855540896,12.));
#171916=CARTESIAN_POINT('Ctrl Pts',(68.6920734222932,17.263230904689,12.));
#171917=CARTESIAN_POINT('Ctrl Pts',(68.7136437951075,17.2620514472176,12.));
#171918=CARTESIAN_POINT('Ctrl Pts',(68.7352611482519,17.2608471147178,12.));
#171919=CARTESIAN_POINT('Ctrl Pts',(68.7569253242312,17.2596178406545,12.));
#171920=CARTESIAN_POINT('Ctrl Pts',(68.7786361662876,17.2583635589197,12.));
#171921=CARTESIAN_POINT('Ctrl Pts',(68.8003935184193,17.2570842038386,12.));
#171922=CARTESIAN_POINT('Ctrl Pts',(68.8221972253954,17.2557797101816,12.));
#171923=CARTESIAN_POINT('Ctrl Pts',(68.8440471327563,17.2544500131627,12.));
#171924=CARTESIAN_POINT('Ctrl Pts',(68.8659430867977,17.2530950484259,12.));
#171925=CARTESIAN_POINT('Ctrl Pts',(68.8878849345557,17.2517147520376,12.));
#171926=CARTESIAN_POINT('Ctrl Pts',(68.9098725237868,17.2503090604792,12.));
#171927=CARTESIAN_POINT('Ctrl Pts',(68.9319057029407,17.248877910643,12.));
#171928=CARTESIAN_POINT('Ctrl Pts',(68.9539843211618,17.2474212398275,12.));
#171929=CARTESIAN_POINT('Ctrl Pts',(68.9761082282922,17.2459389857327,12.));
#171930=CARTESIAN_POINT('Ctrl Pts',(68.9982772748694,17.2444310864585,12.));
#171931=CARTESIAN_POINT('Ctrl Pts',(69.0204913121226,17.2428974805043,12.));
#171932=CARTESIAN_POINT('Ctrl Pts',(69.0427501919636,17.2413381067722,12.));
#171933=CARTESIAN_POINT('Ctrl Pts',(69.0650537669859,17.2397529045587,12.));
#171934=CARTESIAN_POINT('Ctrl Pts',(69.0874018904598,17.238141813549,12.));
#171935=CARTESIAN_POINT('Ctrl Pts',(69.1097944163243,17.2365047738125,12.));
#171936=CARTESIAN_POINT('Ctrl Pts',(69.1322311991759,17.2348417258017,12.));
#171937=CARTESIAN_POINT('Ctrl Pts',(69.1547120942542,17.2331526103511,12.));
#171938=CARTESIAN_POINT('Ctrl Pts',(69.1772369574462,17.2314373686705,12.));
#171939=CARTESIAN_POINT('Ctrl Pts',(69.1998056452837,17.229695942341,12.));
#171940=CARTESIAN_POINT('Ctrl Pts',(69.2224180149377,17.2279282733119,12.));
#171941=CARTESIAN_POINT('Ctrl Pts',(69.2450739242092,17.2261343039015,12.));
#171942=CARTESIAN_POINT('Ctrl Pts',(69.26777323152,17.2243139767963,12.));
#171943=CARTESIAN_POINT('Ctrl Pts',(69.2905157959142,17.2224672350432,12.));
#171944=CARTESIAN_POINT('Ctrl Pts',(69.3133014770541,17.2205940220455,12.));
#171945=CARTESIAN_POINT('Ctrl Pts',(69.3361301352149,17.2186942815604,12.));
#171946=CARTESIAN_POINT('Ctrl Pts',(69.359001631272,17.2167679576991,12.));
#171947=CARTESIAN_POINT('Ctrl Pts',(69.3819158266955,17.2148149949261,12.));
#171948=CARTESIAN_POINT('Ctrl Pts',(69.4048725835516,17.2128353380511,12.));
#171949=CARTESIAN_POINT('Ctrl Pts',(69.4278717644989,17.2108289322258,12.));
#171950=CARTESIAN_POINT('Ctrl Pts',(69.4509132327836,17.208795722942,12.));
#171951=CARTESIAN_POINT('Ctrl Pts',(69.4739968522271,17.2067356560326,12.));
#171952=CARTESIAN_POINT('Ctrl Pts',(69.497122487222,17.2046486776697,12.));
#171953=CARTESIAN_POINT('Ctrl Pts',(69.5202900027329,17.2025347343568,12.));
#171954=CARTESIAN_POINT('Ctrl Pts',(69.5434992642932,17.2003937729266,12.));
#171955=CARTESIAN_POINT('Ctrl Pts',(69.5667501379984,17.198225740538,12.));
#171956=CARTESIAN_POINT('Ctrl Pts',(69.5900424904954,17.1960305846787,12.));
#171957=CARTESIAN_POINT('Ctrl Pts',(69.6133761889787,17.193808253162,12.));
#171958=CARTESIAN_POINT('Ctrl Pts',(69.6367511011927,17.1915586941198,12.));
#171959=CARTESIAN_POINT('Ctrl Pts',(69.6601670954277,17.1892818560004,12.));
#171960=CARTESIAN_POINT('Ctrl Pts',(69.6836240405152,17.1869776875663,12.));
#171961=CARTESIAN_POINT('Ctrl Pts',(69.7071218058149,17.1846461378966,12.));
#171962=CARTESIAN_POINT('Ctrl Pts',(69.7306602612125,17.1822871563835,12.));
#171963=CARTESIAN_POINT('Ctrl Pts',(69.7542392771216,17.1799006927256,12.));
#171964=CARTESIAN_POINT('Ctrl Pts',(69.7778587244788,17.1774866969256,12.));
#171965=CARTESIAN_POINT('Ctrl Pts',(69.8015184747404,17.1750451192887,12.));
#171966=CARTESIAN_POINT('Ctrl Pts',(69.8252183998713,17.1725759104254,12.));
#171967=CARTESIAN_POINT('Ctrl Pts',(69.8489583723417,17.1700790212476,12.));
#171968=CARTESIAN_POINT('Ctrl Pts',(69.8727382651292,17.1675544029622,12.));
#171969=CARTESIAN_POINT('Ctrl Pts',(69.8965579517147,17.1650020070686,12.));
#171970=CARTESIAN_POINT('Ctrl Pts',(69.9204173060779,17.1624217853577,12.));
#171971=CARTESIAN_POINT('Ctrl Pts',(69.9443162026865,17.1598136899144,12.));
#171972=CARTESIAN_POINT('Ctrl Pts',(69.9682545164942,17.157177673114,12.));
#171973=CARTESIAN_POINT('Ctrl Pts',(69.9922321229428,17.1545136876162,12.));
#171974=CARTESIAN_POINT('Ctrl Pts',(70.0162488979587,17.1518216863624,12.));
#171975=CARTESIAN_POINT('Ctrl Pts',(70.0403047179481,17.1491016225748,12.));
#171976=CARTESIAN_POINT('Ctrl Pts',(70.0643994597865,17.1463534497592,12.));
#171977=CARTESIAN_POINT('Ctrl Pts',(70.0885330008169,17.1435771217015,12.));
#171978=CARTESIAN_POINT('Ctrl Pts',(70.1127052188515,17.1407725924615,12.));
#171979=CARTESIAN_POINT('Ctrl Pts',(70.1369159921686,17.1379398163708,12.));
#171980=CARTESIAN_POINT('Ctrl Pts',(70.1611651995085,17.1350787480313,12.));
#171981=CARTESIAN_POINT('Ctrl Pts',(70.1854527200636,17.1321893423183,12.));
#171982=CARTESIAN_POINT('Ctrl Pts',(70.2097784334749,17.1292715543779,12.));
#171983=CARTESIAN_POINT('Ctrl Pts',(70.2341422198363,17.1263253396202,12.));
#171984=CARTESIAN_POINT('Ctrl Pts',(70.2585439596899,17.1233506537176,12.));
#171985=CARTESIAN_POINT('Ctrl Pts',(70.2829835340239,17.1203474526031,12.));
#171986=CARTESIAN_POINT('Ctrl Pts',(70.3074608242613,17.1173156924734,12.));
#171987=CARTESIAN_POINT('Ctrl Pts',(70.3319757122577,17.1142553297869,12.));
#171988=CARTESIAN_POINT('Ctrl Pts',(70.356528080303,17.111166321257,12.));
#171989=CARTESIAN_POINT('Ctrl Pts',(70.3811178111206,17.10804862385,12.));
#171990=CARTESIAN_POINT('Ctrl Pts',(70.4057447878621,17.1049021947833,12.));
#171991=CARTESIAN_POINT('Ctrl Pts',(70.4304088940998,17.1017269915289,12.));
#171992=CARTESIAN_POINT('Ctrl Pts',(70.4551100138221,17.098522971812,12.));
#171993=CARTESIAN_POINT('Ctrl Pts',(70.4798480314364,17.0952900936044,12.));
#171994=CARTESIAN_POINT('Ctrl Pts',(70.5046228317669,17.0920283151217,12.));
#171995=CARTESIAN_POINT('Ctrl Pts',(70.5294343000516,17.0887375948221,12.));
#171996=CARTESIAN_POINT('Ctrl Pts',(70.5542823219346,17.085417891409,12.));
#171997=CARTESIAN_POINT('Ctrl Pts',(70.5791667834599,17.0820691638314,12.));
#171998=CARTESIAN_POINT('Ctrl Pts',(70.6040875710762,17.0786913712767,12.));
#171999=CARTESIAN_POINT('Ctrl Pts',(70.6290445716341,17.0752844731679,12.));
#172000=CARTESIAN_POINT('Ctrl Pts',(70.6540376723839,17.0718484291623,12.));
#172001=CARTESIAN_POINT('Ctrl Pts',(70.6790667609678,17.0683831991532,12.));
#172002=CARTESIAN_POINT('Ctrl Pts',(70.7041317254128,17.0648887432714,12.));
#172003=CARTESIAN_POINT('Ctrl Pts',(70.7292324541348,17.0613650218789,12.));
#172004=CARTESIAN_POINT('Ctrl Pts',(70.754368835938,17.0578119955651,12.));
#172005=CARTESIAN_POINT('Ctrl Pts',(70.7795407600127,17.0542296251462,12.));
#172006=CARTESIAN_POINT('Ctrl Pts',(70.8047481159298,17.0506178716662,12.));
#172007=CARTESIAN_POINT('Ctrl Pts',(70.8299907936334,17.0469766964001,12.));
#172008=CARTESIAN_POINT('Ctrl Pts',(70.8552686834423,17.0433060608475,12.));
#172009=CARTESIAN_POINT('Ctrl Pts',(70.8805816760501,17.0396059267277,12.));
#172010=CARTESIAN_POINT('Ctrl Pts',(70.9059296625214,17.0358762559786,12.));
#172011=CARTESIAN_POINT('Ctrl Pts',(70.9313125342876,17.0321170107564,12.));
#172012=CARTESIAN_POINT('Ctrl Pts',(70.956730183136,17.0283281534392,12.));
#172013=CARTESIAN_POINT('Ctrl Pts',(70.9821825012136,17.0245096466229,12.));
#172014=CARTESIAN_POINT('Ctrl Pts',(71.0076693810301,17.0206614531166,12.));
#172015=CARTESIAN_POINT('Ctrl Pts',(71.0331907154574,17.0167835359419,12.));
#172016=CARTESIAN_POINT('Ctrl Pts',(71.0587463977268,17.0128758583335,12.));
#172017=CARTESIAN_POINT('Ctrl Pts',(71.0843363214221,17.0089383837437,12.));
#172018=CARTESIAN_POINT('Ctrl Pts',(71.1099603804786,17.0049710758394,12.));
#172019=CARTESIAN_POINT('Ctrl Pts',(71.1356184691806,17.0009738984936,12.));
#172020=CARTESIAN_POINT('Ctrl Pts',(71.1613104821568,16.9969468157824,12.));
#172021=CARTESIAN_POINT('Ctrl Pts',(71.187036314374,16.9928897919828,12.));
#172022=CARTESIAN_POINT('Ctrl Pts',(71.212795861124,16.9888027915742,12.));
#172023=CARTESIAN_POINT('Ctrl Pts',(71.2385890180221,16.9846857792384,12.));
#172024=CARTESIAN_POINT('Ctrl Pts',(71.2644156810198,16.9805387198571,12.));
#172025=CARTESIAN_POINT('Ctrl Pts',(71.290275746412,16.9763615785137,12.));
#172026=CARTESIAN_POINT('Ctrl Pts',(71.3161691108427,16.9721543204951,12.));
#172027=CARTESIAN_POINT('Ctrl Pts',(71.3420956713082,16.9679169112994,12.));
#172028=CARTESIAN_POINT('Ctrl Pts',(71.3680553251562,16.9636493166397,12.));
#172029=CARTESIAN_POINT('Ctrl Pts',(71.3940479700677,16.9593515024276,12.));
#172030=CARTESIAN_POINT('Ctrl Pts',(71.4200735040384,16.9550234347621,12.));
#172031=CARTESIAN_POINT('Ctrl Pts',(71.4461318253563,16.9506650799189,12.));
#172032=CARTESIAN_POINT('Ctrl Pts',(71.4722228325794,16.9462764043443,12.));
#172033=CARTESIAN_POINT('Ctrl Pts',(71.4983464245055,16.9418573746489,12.));
#172034=CARTESIAN_POINT('Ctrl Pts',(71.5245025002139,16.9374079576201,12.));
#172035=CARTESIAN_POINT('Ctrl Pts',(71.5506909591129,16.9329281202377,12.));
#172036=CARTESIAN_POINT('Ctrl Pts',(71.5769117009842,16.9284178296933,12.));
#172037=CARTESIAN_POINT('Ctrl Pts',(71.6031646260174,16.9238770534071,12.));
#172038=CARTESIAN_POINT('Ctrl Pts',(71.6294496348653,16.9193057590607,12.));
#172039=CARTESIAN_POINT('Ctrl Pts',(71.6557666285917,16.9147039145717,12.));
#172040=CARTESIAN_POINT('Ctrl Pts',(71.6821155085612,16.9100714880368,12.));
#172041=CARTESIAN_POINT('Ctrl Pts',(71.7084961763357,16.9054084476847,12.));
#172042=CARTESIAN_POINT('Ctrl Pts',(71.7349085335796,16.9007147618344,12.));
#172043=CARTESIAN_POINT('Ctrl Pts',(71.7613524819235,16.895990398841,12.));
#172044=CARTESIAN_POINT('Ctrl Pts',(71.7878279229546,16.8912353270942,12.));
#172045=CARTESIAN_POINT('Ctrl Pts',(71.8143347584962,16.8864495151344,12.));
#172046=CARTESIAN_POINT('Ctrl Pts',(71.8408728908258,16.8816329317471,12.));
#172047=CARTESIAN_POINT('Ctrl Pts',(71.867442222915,16.87678554607,12.));
#172048=CARTESIAN_POINT('Ctrl Pts',(71.8940426586534,16.871907327697,12.));
#172049=CARTESIAN_POINT('Ctrl Pts',(71.9206741030887,16.866998246792,12.));
#172050=CARTESIAN_POINT('Ctrl Pts',(71.9473364618922,16.8620582738437,12.));
#172051=CARTESIAN_POINT('Ctrl Pts',(71.9740296408347,16.8570873794269,12.));
#172052=CARTESIAN_POINT('Ctrl Pts',(72.0007535452081,16.8520855339446,12.));
#172053=CARTESIAN_POINT('Ctrl Pts',(72.0275080793727,16.8470527074275,12.));
#172054=CARTESIAN_POINT('Ctrl Pts',(72.0542931459825,16.8419888691976,12.));
#172055=CARTESIAN_POINT('Ctrl Pts',(72.0811086466121,16.8368939881446,12.));
#172056=CARTESIAN_POINT('Ctrl Pts',(72.1079544831513,16.8317680333404,12.));
#172057=CARTESIAN_POINT('Ctrl Pts',(72.13483055902,16.8266109745795,12.));
#172058=CARTESIAN_POINT('Ctrl Pts',(72.1617367803235,16.8214227828943,12.));
#172059=CARTESIAN_POINT('Ctrl Pts',(72.1886730573452,16.8162034312269,12.));
#172060=CARTESIAN_POINT('Ctrl Pts',(72.2156393048975,16.8109528945896,12.));
#172061=CARTESIAN_POINT('Ctrl Pts',(72.2387802230856,16.8064254147776,12.));
#172062=CARTESIAN_POINT('Ctrl Pts',(72.256538003526,16.8029374213794,12.));
#172063=CARTESIAN_POINT('Ctrl Pts',(72.2688994295263,16.8005027425863,12.));
#172064=CARTESIAN_POINT('Ctrl Pts',(72.2758557891328,16.799130531775,12.));
#172065=CARTESIAN_POINT('Ctrl Pts',(72.2774028393913,16.7988252568749,12.));
#172066=CARTESIAN_POINT('',(67.8307641965655,17.2912529479484,0.));
#172067=CARTESIAN_POINT('',(67.8307641965655,17.2912529479484,0.));
#172068=CARTESIAN_POINT('Ctrl Pts',(72.2774028393913,16.7988252568749,0.));
#172069=CARTESIAN_POINT('Ctrl Pts',(72.2758557891328,16.7991305317749,0.));
#172070=CARTESIAN_POINT('Ctrl Pts',(72.2688994295263,16.8005027425863,0.));
#172071=CARTESIAN_POINT('Ctrl Pts',(72.256538003526,16.8029374213794,0.));
#172072=CARTESIAN_POINT('Ctrl Pts',(72.2387802230856,16.8064254147776,0.));
#172073=CARTESIAN_POINT('Ctrl Pts',(72.2156393048975,16.8109528945896,0.));
#172074=CARTESIAN_POINT('Ctrl Pts',(72.1886730573452,16.8162034312269,0.));
#172075=CARTESIAN_POINT('Ctrl Pts',(72.1617367803235,16.8214227828943,0.));
#172076=CARTESIAN_POINT('Ctrl Pts',(72.13483055902,16.8266109745795,0.));
#172077=CARTESIAN_POINT('Ctrl Pts',(72.1079544831513,16.8317680333404,0.));
#172078=CARTESIAN_POINT('Ctrl Pts',(72.0811086466121,16.8368939881446,0.));
#172079=CARTESIAN_POINT('Ctrl Pts',(72.0542931459825,16.8419888691976,0.));
#172080=CARTESIAN_POINT('Ctrl Pts',(72.0275080793727,16.8470527074275,0.));
#172081=CARTESIAN_POINT('Ctrl Pts',(72.0007535452081,16.8520855339446,0.));
#172082=CARTESIAN_POINT('Ctrl Pts',(71.9740296408347,16.8570873794269,0.));
#172083=CARTESIAN_POINT('Ctrl Pts',(71.9473364618922,16.8620582738437,0.));
#172084=CARTESIAN_POINT('Ctrl Pts',(71.9206741030887,16.866998246792,0.));
#172085=CARTESIAN_POINT('Ctrl Pts',(71.8940426586534,16.871907327697,0.));
#172086=CARTESIAN_POINT('Ctrl Pts',(71.867442222915,16.87678554607,0.));
#172087=CARTESIAN_POINT('Ctrl Pts',(71.8408728908258,16.8816329317471,0.));
#172088=CARTESIAN_POINT('Ctrl Pts',(71.8143347584962,16.8864495151344,0.));
#172089=CARTESIAN_POINT('Ctrl Pts',(71.7878279229546,16.8912353270942,0.));
#172090=CARTESIAN_POINT('Ctrl Pts',(71.7613524819235,16.895990398841,0.));
#172091=CARTESIAN_POINT('Ctrl Pts',(71.7349085335796,16.9007147618344,0.));
#172092=CARTESIAN_POINT('Ctrl Pts',(71.7084961763357,16.9054084476847,0.));
#172093=CARTESIAN_POINT('Ctrl Pts',(71.6821155085612,16.9100714880368,0.));
#172094=CARTESIAN_POINT('Ctrl Pts',(71.6557666285917,16.9147039145717,0.));
#172095=CARTESIAN_POINT('Ctrl Pts',(71.6294496348653,16.9193057590607,0.));
#172096=CARTESIAN_POINT('Ctrl Pts',(71.6031646260174,16.9238770534071,0.));
#172097=CARTESIAN_POINT('Ctrl Pts',(71.5769117009842,16.9284178296933,0.));
#172098=CARTESIAN_POINT('Ctrl Pts',(71.5506909591129,16.9329281202377,0.));
#172099=CARTESIAN_POINT('Ctrl Pts',(71.5245025002139,16.9374079576201,0.));
#172100=CARTESIAN_POINT('Ctrl Pts',(71.4983464245055,16.9418573746489,0.));
#172101=CARTESIAN_POINT('Ctrl Pts',(71.4722228325794,16.9462764043443,0.));
#172102=CARTESIAN_POINT('Ctrl Pts',(71.4461318253563,16.9506650799189,0.));
#172103=CARTESIAN_POINT('Ctrl Pts',(71.4200735040384,16.9550234347621,0.));
#172104=CARTESIAN_POINT('Ctrl Pts',(71.3940479700677,16.9593515024276,0.));
#172105=CARTESIAN_POINT('Ctrl Pts',(71.3680553251562,16.9636493166397,0.));
#172106=CARTESIAN_POINT('Ctrl Pts',(71.3420956713082,16.9679169112994,0.));
#172107=CARTESIAN_POINT('Ctrl Pts',(71.3161691108427,16.9721543204951,0.));
#172108=CARTESIAN_POINT('Ctrl Pts',(71.290275746412,16.9763615785137,0.));
#172109=CARTESIAN_POINT('Ctrl Pts',(71.2644156810198,16.9805387198571,0.));
#172110=CARTESIAN_POINT('Ctrl Pts',(71.2385890180221,16.9846857792384,0.));
#172111=CARTESIAN_POINT('Ctrl Pts',(71.212795861124,16.9888027915742,0.));
#172112=CARTESIAN_POINT('Ctrl Pts',(71.187036314374,16.9928897919828,0.));
#172113=CARTESIAN_POINT('Ctrl Pts',(71.1613104821568,16.9969468157824,0.));
#172114=CARTESIAN_POINT('Ctrl Pts',(71.1356184691806,17.0009738984936,0.));
#172115=CARTESIAN_POINT('Ctrl Pts',(71.1099603804786,17.0049710758394,0.));
#172116=CARTESIAN_POINT('Ctrl Pts',(71.0843363214221,17.0089383837437,0.));
#172117=CARTESIAN_POINT('Ctrl Pts',(71.0587463977268,17.0128758583335,0.));
#172118=CARTESIAN_POINT('Ctrl Pts',(71.0331907154574,17.0167835359419,0.));
#172119=CARTESIAN_POINT('Ctrl Pts',(71.0076693810301,17.0206614531166,0.));
#172120=CARTESIAN_POINT('Ctrl Pts',(70.9821825012136,17.0245096466229,0.));
#172121=CARTESIAN_POINT('Ctrl Pts',(70.956730183136,17.0283281534392,0.));
#172122=CARTESIAN_POINT('Ctrl Pts',(70.9313125342876,17.0321170107564,0.));
#172123=CARTESIAN_POINT('Ctrl Pts',(70.9059296625214,17.0358762559786,0.));
#172124=CARTESIAN_POINT('Ctrl Pts',(70.8805816760501,17.0396059267277,0.));
#172125=CARTESIAN_POINT('Ctrl Pts',(70.8552686834423,17.0433060608475,0.));
#172126=CARTESIAN_POINT('Ctrl Pts',(70.8299907936334,17.0469766964001,0.));
#172127=CARTESIAN_POINT('Ctrl Pts',(70.8047481159298,17.0506178716662,0.));
#172128=CARTESIAN_POINT('Ctrl Pts',(70.7795407600127,17.0542296251462,0.));
#172129=CARTESIAN_POINT('Ctrl Pts',(70.754368835938,17.0578119955651,0.));
#172130=CARTESIAN_POINT('Ctrl Pts',(70.7292324541348,17.0613650218789,0.));
#172131=CARTESIAN_POINT('Ctrl Pts',(70.7041317254128,17.0648887432714,0.));
#172132=CARTESIAN_POINT('Ctrl Pts',(70.6790667609678,17.0683831991532,0.));
#172133=CARTESIAN_POINT('Ctrl Pts',(70.6540376723839,17.0718484291623,0.));
#172134=CARTESIAN_POINT('Ctrl Pts',(70.6290445716341,17.0752844731679,0.));
#172135=CARTESIAN_POINT('Ctrl Pts',(70.6040875710762,17.0786913712767,0.));
#172136=CARTESIAN_POINT('Ctrl Pts',(70.5791667834599,17.0820691638314,0.));
#172137=CARTESIAN_POINT('Ctrl Pts',(70.5542823219346,17.085417891409,0.));
#172138=CARTESIAN_POINT('Ctrl Pts',(70.5294343000516,17.0887375948221,0.));
#172139=CARTESIAN_POINT('Ctrl Pts',(70.5046228317669,17.0920283151217,0.));
#172140=CARTESIAN_POINT('Ctrl Pts',(70.4798480314364,17.0952900936044,0.));
#172141=CARTESIAN_POINT('Ctrl Pts',(70.4551100138221,17.098522971812,0.));
#172142=CARTESIAN_POINT('Ctrl Pts',(70.4304088940998,17.1017269915289,0.));
#172143=CARTESIAN_POINT('Ctrl Pts',(70.4057447878621,17.1049021947833,0.));
#172144=CARTESIAN_POINT('Ctrl Pts',(70.3811178111206,17.10804862385,0.));
#172145=CARTESIAN_POINT('Ctrl Pts',(70.356528080303,17.111166321257,0.));
#172146=CARTESIAN_POINT('Ctrl Pts',(70.3319757122577,17.1142553297869,0.));
#172147=CARTESIAN_POINT('Ctrl Pts',(70.3074608242613,17.1173156924734,0.));
#172148=CARTESIAN_POINT('Ctrl Pts',(70.2829835340239,17.1203474526031,0.));
#172149=CARTESIAN_POINT('Ctrl Pts',(70.2585439596899,17.1233506537176,0.));
#172150=CARTESIAN_POINT('Ctrl Pts',(70.2341422198363,17.1263253396202,0.));
#172151=CARTESIAN_POINT('Ctrl Pts',(70.2097784334749,17.1292715543779,0.));
#172152=CARTESIAN_POINT('Ctrl Pts',(70.1854527200636,17.1321893423183,0.));
#172153=CARTESIAN_POINT('Ctrl Pts',(70.1611651995085,17.1350787480313,0.));
#172154=CARTESIAN_POINT('Ctrl Pts',(70.1369159921686,17.1379398163708,0.));
#172155=CARTESIAN_POINT('Ctrl Pts',(70.1127052188515,17.1407725924615,0.));
#172156=CARTESIAN_POINT('Ctrl Pts',(70.0885330008169,17.1435771217015,0.));
#172157=CARTESIAN_POINT('Ctrl Pts',(70.0643994597865,17.1463534497592,0.));
#172158=CARTESIAN_POINT('Ctrl Pts',(70.0403047179481,17.1491016225748,0.));
#172159=CARTESIAN_POINT('Ctrl Pts',(70.0162488979587,17.1518216863624,0.));
#172160=CARTESIAN_POINT('Ctrl Pts',(69.9922321229428,17.1545136876162,0.));
#172161=CARTESIAN_POINT('Ctrl Pts',(69.9682545164942,17.157177673114,0.));
#172162=CARTESIAN_POINT('Ctrl Pts',(69.9443162026865,17.1598136899144,0.));
#172163=CARTESIAN_POINT('Ctrl Pts',(69.9204173060779,17.1624217853577,0.));
#172164=CARTESIAN_POINT('Ctrl Pts',(69.8965579517147,17.1650020070686,0.));
#172165=CARTESIAN_POINT('Ctrl Pts',(69.8727382651292,17.1675544029622,0.));
#172166=CARTESIAN_POINT('Ctrl Pts',(69.8489583723417,17.1700790212476,0.));
#172167=CARTESIAN_POINT('Ctrl Pts',(69.8252183998713,17.1725759104254,0.));
#172168=CARTESIAN_POINT('Ctrl Pts',(69.8015184747404,17.1750451192887,0.));
#172169=CARTESIAN_POINT('Ctrl Pts',(69.7778587244788,17.1774866969256,0.));
#172170=CARTESIAN_POINT('Ctrl Pts',(69.7542392771216,17.1799006927256,0.));
#172171=CARTESIAN_POINT('Ctrl Pts',(69.7306602612125,17.1822871563835,0.));
#172172=CARTESIAN_POINT('Ctrl Pts',(69.7071218058149,17.1846461378966,0.));
#172173=CARTESIAN_POINT('Ctrl Pts',(69.6836240405152,17.1869776875663,0.));
#172174=CARTESIAN_POINT('Ctrl Pts',(69.6601670954277,17.1892818560004,0.));
#172175=CARTESIAN_POINT('Ctrl Pts',(69.6367511011927,17.1915586941198,0.));
#172176=CARTESIAN_POINT('Ctrl Pts',(69.6133761889787,17.193808253162,0.));
#172177=CARTESIAN_POINT('Ctrl Pts',(69.5900424904954,17.1960305846787,0.));
#172178=CARTESIAN_POINT('Ctrl Pts',(69.5667501379984,17.198225740538,0.));
#172179=CARTESIAN_POINT('Ctrl Pts',(69.5434992642932,17.2003937729266,0.));
#172180=CARTESIAN_POINT('Ctrl Pts',(69.5202900027329,17.2025347343568,0.));
#172181=CARTESIAN_POINT('Ctrl Pts',(69.497122487222,17.2046486776697,0.));
#172182=CARTESIAN_POINT('Ctrl Pts',(69.4739968522271,17.2067356560326,0.));
#172183=CARTESIAN_POINT('Ctrl Pts',(69.4509132327836,17.208795722942,0.));
#172184=CARTESIAN_POINT('Ctrl Pts',(69.4278717644989,17.2108289322258,0.));
#172185=CARTESIAN_POINT('Ctrl Pts',(69.4048725835516,17.2128353380511,0.));
#172186=CARTESIAN_POINT('Ctrl Pts',(69.3819158266955,17.2148149949261,0.));
#172187=CARTESIAN_POINT('Ctrl Pts',(69.359001631272,17.2167679576991,0.));
#172188=CARTESIAN_POINT('Ctrl Pts',(69.3361301352149,17.2186942815604,0.));
#172189=CARTESIAN_POINT('Ctrl Pts',(69.3133014770541,17.2205940220455,0.));
#172190=CARTESIAN_POINT('Ctrl Pts',(69.2905157959142,17.2224672350432,0.));
#172191=CARTESIAN_POINT('Ctrl Pts',(69.26777323152,17.2243139767963,0.));
#172192=CARTESIAN_POINT('Ctrl Pts',(69.2450739242092,17.2261343039015,0.));
#172193=CARTESIAN_POINT('Ctrl Pts',(69.2224180149377,17.2279282733119,0.));
#172194=CARTESIAN_POINT('Ctrl Pts',(69.1998056452837,17.229695942341,0.));
#172195=CARTESIAN_POINT('Ctrl Pts',(69.1772369574462,17.2314373686705,0.));
#172196=CARTESIAN_POINT('Ctrl Pts',(69.1547120942542,17.2331526103511,0.));
#172197=CARTESIAN_POINT('Ctrl Pts',(69.1322311991759,17.2348417258017,0.));
#172198=CARTESIAN_POINT('Ctrl Pts',(69.1097944163243,17.2365047738125,0.));
#172199=CARTESIAN_POINT('Ctrl Pts',(69.0874018904598,17.238141813549,0.));
#172200=CARTESIAN_POINT('Ctrl Pts',(69.0650537669859,17.2397529045587,0.));
#172201=CARTESIAN_POINT('Ctrl Pts',(69.0427501919636,17.2413381067722,0.));
#172202=CARTESIAN_POINT('Ctrl Pts',(69.0204913121226,17.2428974805043,0.));
#172203=CARTESIAN_POINT('Ctrl Pts',(68.9982772748694,17.2444310864585,0.));
#172204=CARTESIAN_POINT('Ctrl Pts',(68.9761082282922,17.2459389857327,0.));
#172205=CARTESIAN_POINT('Ctrl Pts',(68.9539843211618,17.2474212398275,0.));
#172206=CARTESIAN_POINT('Ctrl Pts',(68.9319057029407,17.248877910643,0.));
#172207=CARTESIAN_POINT('Ctrl Pts',(68.9098725237868,17.2503090604792,0.));
#172208=CARTESIAN_POINT('Ctrl Pts',(68.8878849345557,17.2517147520376,0.));
#172209=CARTESIAN_POINT('Ctrl Pts',(68.8659430867977,17.2530950484259,0.));
#172210=CARTESIAN_POINT('Ctrl Pts',(68.8440471327563,17.2544500131627,0.));
#172211=CARTESIAN_POINT('Ctrl Pts',(68.8221972253954,17.2557797101816,0.));
#172212=CARTESIAN_POINT('Ctrl Pts',(68.8003935184193,17.2570842038386,0.));
#172213=CARTESIAN_POINT('Ctrl Pts',(68.7786361662876,17.2583635589197,0.));
#172214=CARTESIAN_POINT('Ctrl Pts',(68.7569253242312,17.2596178406545,0.));
#172215=CARTESIAN_POINT('Ctrl Pts',(68.7352611482519,17.2608471147178,0.));
#172216=CARTESIAN_POINT('Ctrl Pts',(68.7136437951075,17.2620514472176,0.));
#172217=CARTESIAN_POINT('Ctrl Pts',(68.6920734222932,17.263230904689,0.));
#172218=CARTESIAN_POINT('Ctrl Pts',(68.6705501880263,17.2643855540896,0.));
#172219=CARTESIAN_POINT('Ctrl Pts',(68.6490742512085,17.2655154627935,0.));
#172220=CARTESIAN_POINT('Ctrl Pts',(68.6276457714757,17.2666206986091,0.));
#172221=CARTESIAN_POINT('Ctrl Pts',(68.6062649092781,17.2677013298061,0.));
#172222=CARTESIAN_POINT('Ctrl Pts',(68.5849318259449,17.2687574251429,0.));
#172223=CARTESIAN_POINT('Ctrl Pts',(68.5636466837502,17.2697890538956,0.));
#172224=CARTESIAN_POINT('Ctrl Pts',(68.5424096459746,17.2707962858912,0.));
#172225=CARTESIAN_POINT('Ctrl Pts',(68.5212208767835,17.2717791914538,0.));
#172226=CARTESIAN_POINT('Ctrl Pts',(68.5000805410897,17.2727378413485,0.));
#172227=CARTESIAN_POINT('Ctrl Pts',(68.4789888044357,17.2736723067367,0.));
#172228=CARTESIAN_POINT('Ctrl Pts',(68.4579458328208,17.2745826591125,0.));
#172229=CARTESIAN_POINT('Ctrl Pts',(68.4369517926803,17.2754689703001,0.));
#172230=CARTESIAN_POINT('Ctrl Pts',(68.4160068512781,17.2763313126026,0.));
#172231=CARTESIAN_POINT('Ctrl Pts',(68.3951111770498,17.2771697589387,0.));
#172232=CARTESIAN_POINT('Ctrl Pts',(68.374264939895,17.2779843829605,0.));
#172233=CARTESIAN_POINT('Ctrl Pts',(68.353468311648,17.2787752592475,0.));
#172234=CARTESIAN_POINT('Ctrl Pts',(68.3327214657533,17.2795424631789,0.));
#172235=CARTESIAN_POINT('Ctrl Pts',(68.3120245763884,17.2802860705807,0.));
#172236=CARTESIAN_POINT('Ctrl Pts',(68.2913778177258,17.2810061574352,0.));
#172237=CARTESIAN_POINT('Ctrl Pts',(68.2707813631761,17.2817027995838,0.));
#172238=CARTESIAN_POINT('Ctrl Pts',(68.250235384512,17.2823760723886,0.));
#172239=CARTESIAN_POINT('Ctrl Pts',(68.2297400535339,17.2830260513879,0.));
#172240=CARTESIAN_POINT('Ctrl Pts',(68.2092955440591,17.2836528130825,0.));
#172241=CARTESIAN_POINT('Ctrl Pts',(68.1889020335418,17.2842564355796,0.));
#172242=CARTESIAN_POINT('Ctrl Pts',(68.1685597054193,17.2848369995283,0.));
#172243=CARTESIAN_POINT('Ctrl Pts',(68.1482687493176,17.2853945882059,0.));
#172244=CARTESIAN_POINT('Ctrl Pts',(68.1280293561473,17.2859292855694,0.));
#172245=CARTESIAN_POINT('Ctrl Pts',(68.1078417137865,17.2864411745456,0.));
#172246=CARTESIAN_POINT('Ctrl Pts',(68.0877060033229,17.2869303355438,0.));
#172247=CARTESIAN_POINT('Ctrl Pts',(68.0676223930469,17.2873968440855,0.));
#172248=CARTESIAN_POINT('Ctrl Pts',(68.0475910442494,17.2878407730981,0.));
#172249=CARTESIAN_POINT('Ctrl Pts',(68.027612122741,17.2882621974737,0.));
#172250=CARTESIAN_POINT('Ctrl Pts',(68.007685808115,17.28866119774,0.));
#172251=CARTESIAN_POINT('Ctrl Pts',(67.9878123049133,17.2890378644843,0.));
#172252=CARTESIAN_POINT('Ctrl Pts',(67.9679918502441,17.2893923013852,0.));
#172253=CARTESIAN_POINT('Ctrl Pts',(67.9482246901517,17.2897246158895,0.));
#172254=CARTESIAN_POINT('Ctrl Pts',(67.9285110571662,17.2900349103956,0.));
#172255=CARTESIAN_POINT('Ctrl Pts',(67.908851149676,17.2903232740717,0.));
#172256=CARTESIAN_POINT('Ctrl Pts',(67.8892451049871,17.2905897724029,0.));
#172257=CARTESIAN_POINT('Ctrl Pts',(67.8696929979178,17.2908344459816,0.));
#172258=CARTESIAN_POINT('Ctrl Pts',(67.8540944890057,17.2910127431203,0.));
#172259=CARTESIAN_POINT('Ctrl Pts',(67.8424198971214,17.2911366591419,0.));
#172260=CARTESIAN_POINT('Ctrl Pts',(67.8346476309106,17.2912149114145,0.));
#172261=CARTESIAN_POINT('Ctrl Pts',(67.8307641965655,17.2912529479484,0.));
#172262=CARTESIAN_POINT('Ctrl Pts',(73.778495580227,10.343287191141,0.));
#172263=CARTESIAN_POINT('Ctrl Pts',(73.778495580227,10.343287191141,12.));
#172264=CARTESIAN_POINT('Ctrl Pts',(73.7731377048058,10.3449014384453,0.));
#172265=CARTESIAN_POINT('Ctrl Pts',(73.7731377048058,10.3449014384453,12.));
#172266=CARTESIAN_POINT('Ctrl Pts',(73.7624245587789,10.3481265449342,0.));
#172267=CARTESIAN_POINT('Ctrl Pts',(73.7624245587789,10.3481265449342,12.));
#172268=CARTESIAN_POINT('Ctrl Pts',(73.7463626541854,10.3529540403092,0.));
#172269=CARTESIAN_POINT('Ctrl Pts',(73.7463626541854,10.3529540403092,12.));
#172270=CARTESIAN_POINT('Ctrl Pts',(73.7249624109173,10.359370371262,0.));
#172271=CARTESIAN_POINT('Ctrl Pts',(73.7249624109173,10.359370371262,12.));
#172272=CARTESIAN_POINT('Ctrl Pts',(73.6982381645206,10.3673568984582,0.));
#172273=CARTESIAN_POINT('Ctrl Pts',(73.6982381645206,10.3673568984582,12.));
#172274=CARTESIAN_POINT('Ctrl Pts',(73.6715399947839,10.3753095356342,0.));
#172275=CARTESIAN_POINT('Ctrl Pts',(73.6715399947839,10.3753095356342,12.));
#172276=CARTESIAN_POINT('Ctrl Pts',(73.6448679350696,10.3832282820371,0.));
#172277=CARTESIAN_POINT('Ctrl Pts',(73.6448679350696,10.3832282820371,12.));
#172278=CARTESIAN_POINT('Ctrl Pts',(73.6182220363156,10.3911131417463,0.));
#172279=CARTESIAN_POINT('Ctrl Pts',(73.6182220363156,10.3911131417463,12.));
#172280=CARTESIAN_POINT('Ctrl Pts',(73.5916023719713,10.3989641265286,0.));
#172281=CARTESIAN_POINT('Ctrl Pts',(73.5916023719713,10.3989641265286,12.));
#172282=CARTESIAN_POINT('Ctrl Pts',(73.5650090359839,10.406781255551,0.));
#172283=CARTESIAN_POINT('Ctrl Pts',(73.5650090359839,10.406781255551,12.));
#172284=CARTESIAN_POINT('Ctrl Pts',(73.5384421354543,10.414564552681,0.));
#172285=CARTESIAN_POINT('Ctrl Pts',(73.5384421354543,10.414564552681,12.));
#172286=CARTESIAN_POINT('Ctrl Pts',(73.5119017847575,10.4223140444605,0.));
#172287=CARTESIAN_POINT('Ctrl Pts',(73.5119017847575,10.4223140444605,12.));
#172288=CARTESIAN_POINT('Ctrl Pts',(73.485388099225,10.4300297578651,0.));
#172289=CARTESIAN_POINT('Ctrl Pts',(73.485388099225,10.4300297578651,12.));
#172290=CARTESIAN_POINT('Ctrl Pts',(73.4589011886197,10.4377117180223,0.));
#172291=CARTESIAN_POINT('Ctrl Pts',(73.4589011886197,10.4377117180223,12.));
#172292=CARTESIAN_POINT('Ctrl Pts',(73.4324411518554,10.4453599463547,0.));
#172293=CARTESIAN_POINT('Ctrl Pts',(73.4324411518554,10.4453599463547,12.));
#172294=CARTESIAN_POINT('Ctrl Pts',(73.4060080806686,10.452974461845,0.));
#172295=CARTESIAN_POINT('Ctrl Pts',(73.4060080806686,10.452974461845,12.));
#172296=CARTESIAN_POINT('Ctrl Pts',(73.37960206225,10.4605552819397,0.));
#172297=CARTESIAN_POINT('Ctrl Pts',(73.37960206225,10.4605552819397,12.));
#172298=CARTESIAN_POINT('Ctrl Pts',(73.3532231823659,10.4681024236289,0.));
#172299=CARTESIAN_POINT('Ctrl Pts',(73.3532231823659,10.4681024236289,12.));
#172300=CARTESIAN_POINT('Ctrl Pts',(73.3268715280575,10.4756159043806,0.));
#172301=CARTESIAN_POINT('Ctrl Pts',(73.3268715280575,10.4756159043806,12.));
#172302=CARTESIAN_POINT('Ctrl Pts',(73.3005471910583,10.4830957433305,0.));
#172303=CARTESIAN_POINT('Ctrl Pts',(73.3005471910583,10.4830957433305,12.));
#172304=CARTESIAN_POINT('Ctrl Pts',(73.2742502674304,10.4905419611523,0.));
#172305=CARTESIAN_POINT('Ctrl Pts',(73.2742502674304,10.4905419611523,12.));
#172306=CARTESIAN_POINT('Ctrl Pts',(73.2479808560189,10.4979545795192,0.));
#172307=CARTESIAN_POINT('Ctrl Pts',(73.2479808560189,10.4979545795192,12.));
#172308=CARTESIAN_POINT('Ctrl Pts',(73.2217390572562,10.5053336206908,0.));
#172309=CARTESIAN_POINT('Ctrl Pts',(73.2217390572562,10.5053336206908,12.));
#172310=CARTESIAN_POINT('Ctrl Pts',(73.1955249719048,10.5126791070805,0.));
#172311=CARTESIAN_POINT('Ctrl Pts',(73.1955249719048,10.5126791070805,12.));
#172312=CARTESIAN_POINT('Ctrl Pts',(73.1693386996138,10.5199910607655,0.));
#172313=CARTESIAN_POINT('Ctrl Pts',(73.1693386996138,10.5199910607655,12.));
#172314=CARTESIAN_POINT('Ctrl Pts',(73.1431803382711,10.5272695032653,0.));
#172315=CARTESIAN_POINT('Ctrl Pts',(73.1431803382711,10.5272695032653,12.));
#172316=CARTESIAN_POINT('Ctrl Pts',(73.1170499848039,10.53451445581,0.));
#172317=CARTESIAN_POINT('Ctrl Pts',(73.1170499848039,10.53451445581,12.));
#172318=CARTESIAN_POINT('Ctrl Pts',(73.0909477356474,10.5417259395003,0.));
#172319=CARTESIAN_POINT('Ctrl Pts',(73.0909477356474,10.5417259395003,12.));
#172320=CARTESIAN_POINT('Ctrl Pts',(73.0648736873434,10.5489039755138,0.));
#172321=CARTESIAN_POINT('Ctrl Pts',(73.0648736873434,10.5489039755138,12.));
#172322=CARTESIAN_POINT('Ctrl Pts',(73.0388279370834,10.5560485852974,0.));
#172323=CARTESIAN_POINT('Ctrl Pts',(73.0388279370834,10.5560485852974,12.));
#172324=CARTESIAN_POINT('Ctrl Pts',(73.0128105832621,10.5631597907651,0.));
#172325=CARTESIAN_POINT('Ctrl Pts',(73.0128105832621,10.5631597907651,12.));
#172326=CARTESIAN_POINT('Ctrl Pts',(72.9868217252283,10.570237614205,0.));
#172327=CARTESIAN_POINT('Ctrl Pts',(72.9868217252283,10.570237614205,12.));
#172328=CARTESIAN_POINT('Ctrl Pts',(72.9608614630534,10.5772820781958,0.));
#172329=CARTESIAN_POINT('Ctrl Pts',(72.9608614630534,10.5772820781958,12.));
#172330=CARTESIAN_POINT('Ctrl Pts',(72.9349298972822,10.5842932055209,0.));
#172331=CARTESIAN_POINT('Ctrl Pts',(72.9349298972822,10.5842932055209,12.));
#172332=CARTESIAN_POINT('Ctrl Pts',(72.9090271287083,10.5912710190928,0.));
#172333=CARTESIAN_POINT('Ctrl Pts',(72.9090271287083,10.5912710190928,12.));
#172334=CARTESIAN_POINT('Ctrl Pts',(72.8831532580845,10.5982155418626,0.));
#172335=CARTESIAN_POINT('Ctrl Pts',(72.8831532580845,10.5982155418626,12.));
#172336=CARTESIAN_POINT('Ctrl Pts',(72.8573083861337,10.6051267968203,0.));
#172337=CARTESIAN_POINT('Ctrl Pts',(72.8573083861337,10.6051267968203,12.));
#172338=CARTESIAN_POINT('Ctrl Pts',(72.8314926136881,10.6120048070368,0.));
#172339=CARTESIAN_POINT('Ctrl Pts',(72.8314926136881,10.6120048070368,12.));
#172340=CARTESIAN_POINT('Ctrl Pts',(72.8057060417887,10.6188495956973,0.));
#172341=CARTESIAN_POINT('Ctrl Pts',(72.8057060417887,10.6188495956973,12.));
#172342=CARTESIAN_POINT('Ctrl Pts',(72.7799487717911,10.6256611861394,0.));
#172343=CARTESIAN_POINT('Ctrl Pts',(72.7799487717911,10.6256611861394,12.));
#172344=CARTESIAN_POINT('Ctrl Pts',(72.7542209054812,10.6324396018998,0.));
#172345=CARTESIAN_POINT('Ctrl Pts',(72.7542209054812,10.6324396018998,12.));
#172346=CARTESIAN_POINT('Ctrl Pts',(72.7285225451293,10.6391848667352,0.));
#172347=CARTESIAN_POINT('Ctrl Pts',(72.7285225451293,10.6391848667352,12.));
#172348=CARTESIAN_POINT('Ctrl Pts',(72.7028537934317,10.6458970045946,0.));
#172349=CARTESIAN_POINT('Ctrl Pts',(72.7028537934317,10.6458970045946,12.));
#172350=CARTESIAN_POINT('Ctrl Pts',(72.6772147534752,10.6525760396054,0.));
#172351=CARTESIAN_POINT('Ctrl Pts',(72.6772147534752,10.6525760396054,12.));
#172352=CARTESIAN_POINT('Ctrl Pts',(72.651605528691,10.6592219960581,0.));
#172353=CARTESIAN_POINT('Ctrl Pts',(72.651605528691,10.6592219960581,12.));
#172354=CARTESIAN_POINT('Ctrl Pts',(72.6260262228065,10.6658348983945,0.));
#172355=CARTESIAN_POINT('Ctrl Pts',(72.6260262228065,10.6658348983945,12.));
#172356=CARTESIAN_POINT('Ctrl Pts',(72.6004769398019,10.6724147711995,0.));
#172357=CARTESIAN_POINT('Ctrl Pts',(72.6004769398019,10.6724147711995,12.));
#172358=CARTESIAN_POINT('Ctrl Pts',(72.5749577839415,10.6789616392042,0.));
#172359=CARTESIAN_POINT('Ctrl Pts',(72.5749577839415,10.6789616392042,12.));
#172360=CARTESIAN_POINT('Ctrl Pts',(72.5494688597961,10.6854755272904,0.));
#172361=CARTESIAN_POINT('Ctrl Pts',(72.5494688597961,10.6854755272904,12.));
#172362=CARTESIAN_POINT('Ctrl Pts',(72.5240102722664,10.691956460499,0.));
#172363=CARTESIAN_POINT('Ctrl Pts',(72.5240102722664,10.691956460499,12.));
#172364=CARTESIAN_POINT('Ctrl Pts',(72.4985821266023,10.6984044640398,0.));
#172365=CARTESIAN_POINT('Ctrl Pts',(72.4985821266023,10.6984044640398,12.));
#172366=CARTESIAN_POINT('Ctrl Pts',(72.4731845284227,10.7048195633061,0.));
#172367=CARTESIAN_POINT('Ctrl Pts',(72.4731845284227,10.7048195633061,12.));
#172368=CARTESIAN_POINT('Ctrl Pts',(72.4478175837156,10.7112017838706,0.));
#172369=CARTESIAN_POINT('Ctrl Pts',(72.4478175837156,10.7112017838706,12.));
#172370=CARTESIAN_POINT('Ctrl Pts',(72.4224813988347,10.7175511514789,0.));
#172371=CARTESIAN_POINT('Ctrl Pts',(72.4224813988347,10.7175511514789,12.));
#172372=CARTESIAN_POINT('Ctrl Pts',(72.3971760804933,10.7238676920469,0.));
#172373=CARTESIAN_POINT('Ctrl Pts',(72.3971760804933,10.7238676920469,12.));
#172374=CARTESIAN_POINT('Ctrl Pts',(72.3719017357571,10.7301514316607,0.));
#172375=CARTESIAN_POINT('Ctrl Pts',(72.3719017357571,10.7301514316607,12.));
#172376=CARTESIAN_POINT('Ctrl Pts',(72.3466584720318,10.73640239658,0.));
#172377=CARTESIAN_POINT('Ctrl Pts',(72.3466584720318,10.73640239658,12.));
#172378=CARTESIAN_POINT('Ctrl Pts',(72.3214463970641,10.7426206132375,0.));
#172379=CARTESIAN_POINT('Ctrl Pts',(72.3214463970641,10.7426206132375,12.));
#172380=CARTESIAN_POINT('Ctrl Pts',(72.2962656189556,10.7488061082368,0.));
#172381=CARTESIAN_POINT('Ctrl Pts',(72.2962656189556,10.7488061082368,12.));
#172382=CARTESIAN_POINT('Ctrl Pts',(72.2711162461681,10.7549589083535,0.));
#172383=CARTESIAN_POINT('Ctrl Pts',(72.2711162461681,10.7549589083535,12.));
#172384=CARTESIAN_POINT('Ctrl Pts',(72.2459983875296,10.7610790405385,0.));
#172385=CARTESIAN_POINT('Ctrl Pts',(72.2459983875296,10.7610790405385,12.));
#172386=CARTESIAN_POINT('Ctrl Pts',(72.2209121522366,10.7671665319255,0.));
#172387=CARTESIAN_POINT('Ctrl Pts',(72.2209121522366,10.7671665319255,12.));
#172388=CARTESIAN_POINT('Ctrl Pts',(72.1958576498557,10.7732214098345,0.));
#172389=CARTESIAN_POINT('Ctrl Pts',(72.1958576498557,10.7732214098345,12.));
#172390=CARTESIAN_POINT('Ctrl Pts',(72.1708349903305,10.7792437017662,0.));
#172391=CARTESIAN_POINT('Ctrl Pts',(72.1708349903305,10.7792437017662,12.));
#172392=CARTESIAN_POINT('Ctrl Pts',(72.1458442839834,10.7852334354016,0.));
#172393=CARTESIAN_POINT('Ctrl Pts',(72.1458442839834,10.7852334354016,12.));
#172394=CARTESIAN_POINT('Ctrl Pts',(72.1208856415171,10.7911906386027,0.));
#172395=CARTESIAN_POINT('Ctrl Pts',(72.1208856415171,10.7911906386027,12.));
#172396=CARTESIAN_POINT('Ctrl Pts',(72.0959591740114,10.7971153394166,0.));
#172397=CARTESIAN_POINT('Ctrl Pts',(72.0959591740114,10.7971153394166,12.));
#172398=CARTESIAN_POINT('Ctrl Pts',(72.0710649929202,10.8030075660809,0.));
#172399=CARTESIAN_POINT('Ctrl Pts',(72.0710649929202,10.8030075660809,12.));
#172400=CARTESIAN_POINT('Ctrl Pts',(72.0462032100815,10.8088673470184,0.));
#172401=CARTESIAN_POINT('Ctrl Pts',(72.0462032100815,10.8088673470184,12.));
#172402=CARTESIAN_POINT('Ctrl Pts',(72.0213739377223,10.8146947108375,0.));
#172403=CARTESIAN_POINT('Ctrl Pts',(72.0213739377223,10.8146947108375,12.));
#172404=CARTESIAN_POINT('Ctrl Pts',(71.9965772884619,10.8204896863328,0.));
#172405=CARTESIAN_POINT('Ctrl Pts',(71.9965772884619,10.8204896863328,12.));
#172406=CARTESIAN_POINT('Ctrl Pts',(71.9718133753127,10.8262523024898,0.));
#172407=CARTESIAN_POINT('Ctrl Pts',(71.9718133753127,10.8262523024898,12.));
#172408=CARTESIAN_POINT('Ctrl Pts',(71.9470823116785,10.8319825884918,0.));
#172409=CARTESIAN_POINT('Ctrl Pts',(71.9470823116785,10.8319825884918,12.));
#172410=CARTESIAN_POINT('Ctrl Pts',(71.9223842113625,10.8376805737159,0.));
#172411=CARTESIAN_POINT('Ctrl Pts',(71.9223842113625,10.8376805737159,12.));
#172412=CARTESIAN_POINT('Ctrl Pts',(71.8977191885725,10.8433462877312,0.));
#172413=CARTESIAN_POINT('Ctrl Pts',(71.8977191885725,10.8433462877312,12.));
#172414=CARTESIAN_POINT('Ctrl Pts',(71.8730873579224,10.8489797602998,0.));
#172415=CARTESIAN_POINT('Ctrl Pts',(71.8730873579224,10.8489797602998,12.));
#172416=CARTESIAN_POINT('Ctrl Pts',(71.8484888344339,10.8545810213799,0.));
#172417=CARTESIAN_POINT('Ctrl Pts',(71.8484888344339,10.8545810213799,12.));
#172418=CARTESIAN_POINT('Ctrl Pts',(71.8239237335331,10.8601501011332,0.));
#172419=CARTESIAN_POINT('Ctrl Pts',(71.8239237335331,10.8601501011332,12.));
#172420=CARTESIAN_POINT('Ctrl Pts',(71.7993921710564,10.865687029922,0.));
#172421=CARTESIAN_POINT('Ctrl Pts',(71.7993921710564,10.865687029922,12.));
#172422=CARTESIAN_POINT('Ctrl Pts',(71.7748942632593,10.8711918383073,0.));
#172423=CARTESIAN_POINT('Ctrl Pts',(71.7748942632593,10.8711918383073,12.));
#172424=CARTESIAN_POINT('Ctrl Pts',(71.7504301268181,10.8766645570497,0.));
#172425=CARTESIAN_POINT('Ctrl Pts',(71.7504301268181,10.8766645570497,12.));
#172426=CARTESIAN_POINT('Ctrl Pts',(71.7259998788328,10.8821052171121,0.));
#172427=CARTESIAN_POINT('Ctrl Pts',(71.7259998788328,10.8821052171121,12.));
#172428=CARTESIAN_POINT('Ctrl Pts',(71.7016036368236,10.8875138496671,0.));
#172429=CARTESIAN_POINT('Ctrl Pts',(71.7016036368236,10.8875138496671,12.));
#172430=CARTESIAN_POINT('Ctrl Pts',(71.6772415187364,10.8928904860964,0.));
#172431=CARTESIAN_POINT('Ctrl Pts',(71.6772415187364,10.8928904860964,12.));
#172432=CARTESIAN_POINT('Ctrl Pts',(71.6529136429504,10.8982351579871,0.));
#172433=CARTESIAN_POINT('Ctrl Pts',(71.6529136429504,10.8982351579871,12.));
#172434=CARTESIAN_POINT('Ctrl Pts',(71.6286201282812,10.9035478971328,0.));
#172435=CARTESIAN_POINT('Ctrl Pts',(71.6286201282812,10.9035478971328,12.));
#172436=CARTESIAN_POINT('Ctrl Pts',(71.6043610939835,10.9088287355365,0.));
#172437=CARTESIAN_POINT('Ctrl Pts',(71.6043610939835,10.9088287355365,12.));
#172438=CARTESIAN_POINT('Ctrl Pts',(71.5801366597488,10.914077705417,0.));
#172439=CARTESIAN_POINT('Ctrl Pts',(71.5801366597488,10.914077705417,12.));
#172440=CARTESIAN_POINT('Ctrl Pts',(71.5559469457091,10.91929483921,0.));
#172441=CARTESIAN_POINT('Ctrl Pts',(71.5559469457091,10.91929483921,12.));
#172442=CARTESIAN_POINT('Ctrl Pts',(71.5317920724459,10.9244801695642,0.));
#172443=CARTESIAN_POINT('Ctrl Pts',(71.5317920724459,10.9244801695642,12.));
#172444=CARTESIAN_POINT('Ctrl Pts',(71.5076721609936,10.9296337293425,0.));
#172445=CARTESIAN_POINT('Ctrl Pts',(71.5076721609936,10.9296337293425,12.));
#172446=CARTESIAN_POINT('Ctrl Pts',(71.4835873328423,10.9347555516235,0.));
#172447=CARTESIAN_POINT('Ctrl Pts',(71.4835873328423,10.9347555516235,12.));
#172448=CARTESIAN_POINT('Ctrl Pts',(71.4595377099351,10.9398456697095,0.));
#172449=CARTESIAN_POINT('Ctrl Pts',(71.4595377099351,10.9398456697095,12.));
#172450=CARTESIAN_POINT('Ctrl Pts',(71.435523414672,10.944904117127,0.));
#172451=CARTESIAN_POINT('Ctrl Pts',(71.435523414672,10.944904117127,12.));
#172452=CARTESIAN_POINT('Ctrl Pts',(71.4115445699194,10.9499309276237,0.));
#172453=CARTESIAN_POINT('Ctrl Pts',(71.4115445699194,10.9499309276237,12.));
#172454=CARTESIAN_POINT('Ctrl Pts',(71.3876012990138,10.954926135169,0.));
#172455=CARTESIAN_POINT('Ctrl Pts',(71.3876012990138,10.954926135169,12.));
#172456=CARTESIAN_POINT('Ctrl Pts',(71.3636937257649,10.9598897739565,0.));
#172457=CARTESIAN_POINT('Ctrl Pts',(71.3636937257649,10.9598897739565,12.));
#172458=CARTESIAN_POINT('Ctrl Pts',(71.339821974454,10.9648218784098,0.));
#172459=CARTESIAN_POINT('Ctrl Pts',(71.339821974454,10.9648218784098,12.));
#172460=CARTESIAN_POINT('Ctrl Pts',(71.3159861698358,10.969722483186,0.));
#172461=CARTESIAN_POINT('Ctrl Pts',(71.3159861698358,10.969722483186,12.));
#172462=CARTESIAN_POINT('Ctrl Pts',(71.2921864371491,10.9745916231709,0.));
#172463=CARTESIAN_POINT('Ctrl Pts',(71.2921864371491,10.9745916231709,12.));
#172464=CARTESIAN_POINT('Ctrl Pts',(71.2684229021207,10.9794293334805,0.));
#172465=CARTESIAN_POINT('Ctrl Pts',(71.2684229021207,10.9794293334805,12.));
#172466=CARTESIAN_POINT('Ctrl Pts',(71.2446956909687,10.9842356494627,0.));
#172467=CARTESIAN_POINT('Ctrl Pts',(71.2446956909687,10.9842356494627,12.));
#172468=CARTESIAN_POINT('Ctrl Pts',(71.2210049304014,10.9890106067039,0.));
#172469=CARTESIAN_POINT('Ctrl Pts',(71.2210049304014,10.9890106067039,12.));
#172470=CARTESIAN_POINT('Ctrl Pts',(71.1973507476191,10.993754241032,0.));
#172471=CARTESIAN_POINT('Ctrl Pts',(71.1973507476191,10.993754241032,12.));
#172472=CARTESIAN_POINT('Ctrl Pts',(71.1737332703248,10.9984665885127,0.));
#172473=CARTESIAN_POINT('Ctrl Pts',(71.1737332703248,10.9984665885127,12.));
#172474=CARTESIAN_POINT('Ctrl Pts',(71.1501526267286,11.0031476854502,0.));
#172475=CARTESIAN_POINT('Ctrl Pts',(71.1501526267286,11.0031476854502,12.));
#172476=CARTESIAN_POINT('Ctrl Pts',(71.1266089455517,11.0077975683895,0.));
#172477=CARTESIAN_POINT('Ctrl Pts',(71.1266089455517,11.0077975683895,12.));
#172478=CARTESIAN_POINT('Ctrl Pts',(71.1031023560249,11.0124162741225,0.));
#172479=CARTESIAN_POINT('Ctrl Pts',(71.1031023560249,11.0124162741225,12.));
#172480=CARTESIAN_POINT('Ctrl Pts',(71.0796329878907,11.0170038396915,0.));
#172481=CARTESIAN_POINT('Ctrl Pts',(71.0796329878907,11.0170038396915,12.));
#172482=CARTESIAN_POINT('Ctrl Pts',(71.0562009714136,11.0215603023856,0.));
#172483=CARTESIAN_POINT('Ctrl Pts',(71.0562009714136,11.0215603023856,12.));
#172484=CARTESIAN_POINT('Ctrl Pts',(71.0328064373856,11.0260856997415,0.));
#172485=CARTESIAN_POINT('Ctrl Pts',(71.0328064373856,11.0260856997415,12.));
#172486=CARTESIAN_POINT('Ctrl Pts',(71.0094495171292,11.0305800695456,0.));
#172487=CARTESIAN_POINT('Ctrl Pts',(71.0094495171292,11.0305800695456,12.));
#172488=CARTESIAN_POINT('Ctrl Pts',(70.986130342497,11.0350434498405,0.));
#172489=CARTESIAN_POINT('Ctrl Pts',(70.986130342497,11.0350434498405,12.));
#172490=CARTESIAN_POINT('Ctrl Pts',(70.9628490458748,11.0394758789285,0.));
#172491=CARTESIAN_POINT('Ctrl Pts',(70.9628490458748,11.0394758789285,12.));
#172492=CARTESIAN_POINT('Ctrl Pts',(70.9396057601924,11.0438773953682,0.));
#172493=CARTESIAN_POINT('Ctrl Pts',(70.9396057601924,11.0438773953682,12.));
#172494=CARTESIAN_POINT('Ctrl Pts',(70.916400618927,11.048248037975,0.));
#172495=CARTESIAN_POINT('Ctrl Pts',(70.916400618927,11.048248037975,12.));
#172496=CARTESIAN_POINT('Ctrl Pts',(70.8932337561087,11.0525878458243,0.));
#172497=CARTESIAN_POINT('Ctrl Pts',(70.8932337561087,11.0525878458243,12.));
#172498=CARTESIAN_POINT('Ctrl Pts',(70.8701053063186,11.0568968582569,0.));
#172499=CARTESIAN_POINT('Ctrl Pts',(70.8701053063186,11.0568968582569,12.));
#172500=CARTESIAN_POINT('Ctrl Pts',(70.8470154046919,11.0611751148835,0.));
#172501=CARTESIAN_POINT('Ctrl Pts',(70.8470154046919,11.0611751148835,12.));
#172502=CARTESIAN_POINT('Ctrl Pts',(70.8239641869299,11.0654226555802,0.));
#172503=CARTESIAN_POINT('Ctrl Pts',(70.8239641869299,11.0654226555802,12.));
#172504=CARTESIAN_POINT('Ctrl Pts',(70.8009517893057,11.0696395204909,0.));
#172505=CARTESIAN_POINT('Ctrl Pts',(70.8009517893057,11.0696395204909,12.));
#172506=CARTESIAN_POINT('Ctrl Pts',(70.7779783486677,11.0738257500291,0.));
#172507=CARTESIAN_POINT('Ctrl Pts',(70.7779783486677,11.0738257500291,12.));
#172508=CARTESIAN_POINT('Ctrl Pts',(70.7550440024384,11.0779813848846,0.));
#172509=CARTESIAN_POINT('Ctrl Pts',(70.7550440024384,11.0779813848846,12.));
#172510=CARTESIAN_POINT('Ctrl Pts',(70.732148888618,11.0821064660269,0.));
#172511=CARTESIAN_POINT('Ctrl Pts',(70.732148888618,11.0821064660269,12.));
#172512=CARTESIAN_POINT('Ctrl Pts',(70.7092931457954,11.0862010347016,0.));
#172513=CARTESIAN_POINT('Ctrl Pts',(70.7092931457954,11.0862010347016,12.));
#172514=CARTESIAN_POINT('Ctrl Pts',(70.6864769131546,11.0902651324323,0.));
#172515=CARTESIAN_POINT('Ctrl Pts',(70.6864769131546,11.0902651324323,12.));
#172516=CARTESIAN_POINT('Ctrl Pts',(70.6637003304785,11.0942988010233,0.));
#172517=CARTESIAN_POINT('Ctrl Pts',(70.6637003304785,11.0942988010233,12.));
#172518=CARTESIAN_POINT('Ctrl Pts',(70.6409635381482,11.0983020825667,0.));
#172519=CARTESIAN_POINT('Ctrl Pts',(70.6409635381482,11.0983020825667,12.));
#172520=CARTESIAN_POINT('Ctrl Pts',(70.6182666771481,11.1022750194446,0.));
#172521=CARTESIAN_POINT('Ctrl Pts',(70.6182666771481,11.1022750194446,12.));
#172522=CARTESIAN_POINT('Ctrl Pts',(70.5956098890773,11.1062176543262,0.));
#172523=CARTESIAN_POINT('Ctrl Pts',(70.5956098890773,11.1062176543262,12.));
#172524=CARTESIAN_POINT('Ctrl Pts',(70.5729933161546,11.1101300301702,0.));
#172525=CARTESIAN_POINT('Ctrl Pts',(70.5729933161546,11.1101300301702,12.));
#172526=CARTESIAN_POINT('Ctrl Pts',(70.5504171012233,11.1140121902271,0.));
#172527=CARTESIAN_POINT('Ctrl Pts',(70.5504171012233,11.1140121902271,12.));
#172528=CARTESIAN_POINT('Ctrl Pts',(70.5278813877494,11.1178641780476,0.));
#172529=CARTESIAN_POINT('Ctrl Pts',(70.5278813877494,11.1178641780476,12.));
#172530=CARTESIAN_POINT('Ctrl Pts',(70.505386319828,11.1216860374826,0.));
#172531=CARTESIAN_POINT('Ctrl Pts',(70.505386319828,11.1216860374826,12.));
#172532=CARTESIAN_POINT('Ctrl Pts',(70.4829320421957,11.1254778126821,0.));
#172533=CARTESIAN_POINT('Ctrl Pts',(70.4829320421957,11.1254778126821,12.));
#172534=CARTESIAN_POINT('Ctrl Pts',(70.4605187002354,11.1292395480974,0.));
#172535=CARTESIAN_POINT('Ctrl Pts',(70.4605187002354,11.1292395480974,12.));
#172536=CARTESIAN_POINT('Ctrl Pts',(70.4381464399819,11.1329712884847,0.));
#172537=CARTESIAN_POINT('Ctrl Pts',(70.4381464399819,11.1329712884847,12.));
#172538=CARTESIAN_POINT('Ctrl Pts',(70.4158154081205,11.1366730789126,0.));
#172539=CARTESIAN_POINT('Ctrl Pts',(70.4158154081205,11.1366730789126,12.));
#172540=CARTESIAN_POINT('Ctrl Pts',(70.393525751996,11.1403449647625,0.));
#172541=CARTESIAN_POINT('Ctrl Pts',(70.393525751996,11.1403449647625,12.));
#172542=CARTESIAN_POINT('Ctrl Pts',(70.3712776196223,11.143986991727,0.));
#172543=CARTESIAN_POINT('Ctrl Pts',(70.3712776196223,11.143986991727,12.));
#172544=CARTESIAN_POINT('Ctrl Pts',(70.349071159688,11.1475992058124,0.));
#172545=CARTESIAN_POINT('Ctrl Pts',(70.349071159688,11.1475992058124,12.));
#172546=CARTESIAN_POINT('Ctrl Pts',(70.326906521559,11.1511816533421,0.));
#172547=CARTESIAN_POINT('Ctrl Pts',(70.326906521559,11.1511816533421,12.));
#172548=CARTESIAN_POINT('Ctrl Pts',(70.3047838552756,11.1547343809646,0.));
#172549=CARTESIAN_POINT('Ctrl Pts',(70.3047838552756,11.1547343809646,12.));
#172550=CARTESIAN_POINT('Ctrl Pts',(70.2827033115662,11.1582574356521,0.));
#172551=CARTESIAN_POINT('Ctrl Pts',(70.2827033115662,11.1582574356521,12.));
#172552=CARTESIAN_POINT('Ctrl Pts',(70.2606650418589,11.1617508647016,0.));
#172553=CARTESIAN_POINT('Ctrl Pts',(70.2606650418589,11.1617508647016,12.));
#172554=CARTESIAN_POINT('Ctrl Pts',(70.2386691982902,11.1652147157383,0.));
#172555=CARTESIAN_POINT('Ctrl Pts',(70.2386691982902,11.1652147157383,12.));
#172556=CARTESIAN_POINT('Ctrl Pts',(70.2167159337094,11.168649036721,0.));
#172557=CARTESIAN_POINT('Ctrl Pts',(70.2167159337094,11.168649036721,12.));
#172558=CARTESIAN_POINT('Ctrl Pts',(70.1948054016816,11.1720538759499,0.));
#172559=CARTESIAN_POINT('Ctrl Pts',(70.1948054016816,11.1720538759499,12.));
#172560=CARTESIAN_POINT('Ctrl Pts',(70.1729377564954,11.1754292820631,0.));
#172561=CARTESIAN_POINT('Ctrl Pts',(70.1729377564954,11.1754292820631,12.));
#172562=CARTESIAN_POINT('Ctrl Pts',(70.1511131531672,11.1787753040363,0.));
#172563=CARTESIAN_POINT('Ctrl Pts',(70.1511131531672,11.1787753040363,12.));
#172564=CARTESIAN_POINT('Ctrl Pts',(70.1293317474432,11.1820919911846,0.));
#172565=CARTESIAN_POINT('Ctrl Pts',(70.1293317474432,11.1820919911846,12.));
#172566=CARTESIAN_POINT('Ctrl Pts',(70.1075936957973,11.185379393167,0.));
#172567=CARTESIAN_POINT('Ctrl Pts',(70.1075936957973,11.185379393167,12.));
#172568=CARTESIAN_POINT('Ctrl Pts',(70.0858991554295,11.1886375599916,0.));
#172569=CARTESIAN_POINT('Ctrl Pts',(70.0858991554295,11.1886375599916,12.));
#172570=CARTESIAN_POINT('Ctrl Pts',(70.0642482842942,11.1918665420168,0.));
#172571=CARTESIAN_POINT('Ctrl Pts',(70.0642482842942,11.1918665420168,12.));
#172572=CARTESIAN_POINT('Ctrl Pts',(70.0426412411194,11.1950663899578,0.));
#172573=CARTESIAN_POINT('Ctrl Pts',(70.0426412411194,11.1950663899578,12.));
#172574=CARTESIAN_POINT('Ctrl Pts',(70.0210781854236,11.1982371548918,0.));
#172575=CARTESIAN_POINT('Ctrl Pts',(70.0210781854236,11.1982371548918,12.));
#172576=CARTESIAN_POINT('Ctrl Pts',(69.9995592775322,11.2013788882711,0.));
#172577=CARTESIAN_POINT('Ctrl Pts',(69.9995592775322,11.2013788882711,12.));
#172578=CARTESIAN_POINT('Ctrl Pts',(69.9780846785771,11.2044916419239,0.));
#172579=CARTESIAN_POINT('Ctrl Pts',(69.9780846785771,11.2044916419239,12.));
#172580=CARTESIAN_POINT('Ctrl Pts',(69.9566545504813,11.2075754680445,0.));
#172581=CARTESIAN_POINT('Ctrl Pts',(69.9566545504813,11.2075754680445,12.));
#172582=CARTESIAN_POINT('Ctrl Pts',(69.9352690559399,11.2106304191881,0.));
#172583=CARTESIAN_POINT('Ctrl Pts',(69.9352690559399,11.2106304191881,12.));
#172584=CARTESIAN_POINT('Ctrl Pts',(69.9139283584036,11.213656548268,0.));
#172585=CARTESIAN_POINT('Ctrl Pts',(69.9139283584036,11.213656548268,12.));
#172586=CARTESIAN_POINT('Ctrl Pts',(69.8926326220414,11.2166539085527,0.));
#172587=CARTESIAN_POINT('Ctrl Pts',(69.8926326220414,11.2166539085527,12.));
#172588=CARTESIAN_POINT('Ctrl Pts',(69.8713820117918,11.2196225536794,0.));
#172589=CARTESIAN_POINT('Ctrl Pts',(69.8713820117918,11.2196225536794,12.));
#172590=CARTESIAN_POINT('Ctrl Pts',(69.8501766934445,11.2225625376739,0.));
#172591=CARTESIAN_POINT('Ctrl Pts',(69.8501766934445,11.2225625376739,12.));
#172592=CARTESIAN_POINT('Ctrl Pts',(69.8290168337076,11.225473914972,0.));
#172593=CARTESIAN_POINT('Ctrl Pts',(69.8290168337076,11.225473914972,12.));
#172594=CARTESIAN_POINT('Ctrl Pts',(69.8079026002753,11.2283567404434,0.));
#172595=CARTESIAN_POINT('Ctrl Pts',(69.8079026002753,11.2283567404434,12.));
#172596=CARTESIAN_POINT('Ctrl Pts',(69.7868341618927,11.2312110694183,0.));
#172597=CARTESIAN_POINT('Ctrl Pts',(69.7868341618927,11.2312110694183,12.));
#172598=CARTESIAN_POINT('Ctrl Pts',(69.7658116882298,11.2340369576452,0.));
#172599=CARTESIAN_POINT('Ctrl Pts',(69.7658116882298,11.2340369576452,12.));
#172600=CARTESIAN_POINT('Ctrl Pts',(69.7448353497394,11.236834461247,0.));
#172601=CARTESIAN_POINT('Ctrl Pts',(69.7448353497394,11.236834461247,12.));
#172602=CARTESIAN_POINT('Ctrl Pts',(69.7239053175362,11.2396036366861,0.));
#172603=CARTESIAN_POINT('Ctrl Pts',(69.7239053175362,11.2396036366861,12.));
#172604=CARTESIAN_POINT('Ctrl Pts',(69.7030217632187,11.242344540717,0.));
#172605=CARTESIAN_POINT('Ctrl Pts',(69.7030217632187,11.242344540717,12.));
#172606=CARTESIAN_POINT('Ctrl Pts',(69.6821848588492,11.2450572303847,0.));
#172607=CARTESIAN_POINT('Ctrl Pts',(69.6821848588492,11.2450572303847,12.));
#172608=CARTESIAN_POINT('Ctrl Pts',(69.6613947773563,11.2477417631391,0.));
#172609=CARTESIAN_POINT('Ctrl Pts',(69.6613947773563,11.2477417631391,12.));
#172610=CARTESIAN_POINT('Ctrl Pts',(69.6406516928902,11.2503981969414,0.));
#172611=CARTESIAN_POINT('Ctrl Pts',(69.6406516928902,11.2503981969414,12.));
#172612=CARTESIAN_POINT('Ctrl Pts',(69.6199557811231,11.2530265903555,0.));
#172613=CARTESIAN_POINT('Ctrl Pts',(69.6199557811231,11.2530265903555,12.));
#172614=CARTESIAN_POINT('Ctrl Pts',(69.5993072197355,11.255627002701,0.));
#172615=CARTESIAN_POINT('Ctrl Pts',(69.5993072197355,11.255627002701,12.));
#172616=CARTESIAN_POINT('Ctrl Pts',(69.5787061880815,11.2581994939534,0.));
#172617=CARTESIAN_POINT('Ctrl Pts',(69.5787061880815,11.2581994939534,12.));
#172618=CARTESIAN_POINT('Ctrl Pts',(69.5581528662846,11.2607441244698,0.));
#172619=CARTESIAN_POINT('Ctrl Pts',(69.5581528662846,11.2607441244698,12.));
#172620=CARTESIAN_POINT('Ctrl Pts',(69.5376474344768,11.2632609547629,0.));
#172621=CARTESIAN_POINT('Ctrl Pts',(69.5376474344768,11.2632609547629,12.));
#172622=CARTESIAN_POINT('Ctrl Pts',(69.5171900720188,11.2657500452721,0.));
#172623=CARTESIAN_POINT('Ctrl Pts',(69.5171900720188,11.2657500452721,12.));
#172624=CARTESIAN_POINT('Ctrl Pts',(69.4967809565978,11.2682114561015,0.));
#172625=CARTESIAN_POINT('Ctrl Pts',(69.4967809565978,11.2682114561015,12.));
#172626=CARTESIAN_POINT('Ctrl Pts',(69.4764202659443,11.2706452475287,0.));
#172627=CARTESIAN_POINT('Ctrl Pts',(69.4764202659443,11.2706452475287,12.));
#172628=CARTESIAN_POINT('Ctrl Pts',(69.4561081798815,11.2730514806143,0.));
#172629=CARTESIAN_POINT('Ctrl Pts',(69.4561081798815,11.2730514806143,12.));
#172630=CARTESIAN_POINT('Ctrl Pts',(69.4358448819957,11.2754302177019,0.));
#172631=CARTESIAN_POINT('Ctrl Pts',(69.4358448819957,11.2754302177019,12.));
#172632=CARTESIAN_POINT('Ctrl Pts',(69.4156305620554,11.2777815231462,0.));
#172633=CARTESIAN_POINT('Ctrl Pts',(69.4156305620554,11.2777815231462,12.));
#172634=CARTESIAN_POINT('Ctrl Pts',(69.395465416223,11.2801054633807,0.));
#172635=CARTESIAN_POINT('Ctrl Pts',(69.395465416223,11.2801054633807,12.));
#172636=CARTESIAN_POINT('Ctrl Pts',(69.375349642,11.2824021054038,0.));
#172637=CARTESIAN_POINT('Ctrl Pts',(69.375349642,11.2824021054038,12.));
#172638=CARTESIAN_POINT('Ctrl Pts',(69.3552834337771,11.2846715154521,0.));
#172639=CARTESIAN_POINT('Ctrl Pts',(69.3552834337771,11.2846715154521,12.));
#172640=CARTESIAN_POINT('Ctrl Pts',(69.3352669789611,11.2869137578463,0.));
#172641=CARTESIAN_POINT('Ctrl Pts',(69.3352669789611,11.2869137578463,12.));
#172642=CARTESIAN_POINT('Ctrl Pts',(69.315300451784,11.2891288931528,0.));
#172643=CARTESIAN_POINT('Ctrl Pts',(69.315300451784,11.2891288931528,12.));
#172644=CARTESIAN_POINT('Ctrl Pts',(69.2953840192792,11.2913169799642,0.));
#172645=CARTESIAN_POINT('Ctrl Pts',(69.2953840192792,11.2913169799642,12.));
#172646=CARTESIAN_POINT('Ctrl Pts',(69.2755178531534,11.2934780784362,0.));
#172647=CARTESIAN_POINT('Ctrl Pts',(69.2755178531534,11.2934780784362,12.));
#172648=CARTESIAN_POINT('Ctrl Pts',(69.255702139335,11.2956122531375,0.));
#172649=CARTESIAN_POINT('Ctrl Pts',(69.255702139335,11.2956122531375,12.));
#172650=CARTESIAN_POINT('Ctrl Pts',(69.2359370894828,11.2977195764836,0.));
#172651=CARTESIAN_POINT('Ctrl Pts',(69.2359370894828,11.2977195764836,12.));
#172652=CARTESIAN_POINT('Ctrl Pts',(69.216222948839,11.2998001310934,0.));
#172653=CARTESIAN_POINT('Ctrl Pts',(69.216222948839,11.2998001310934,12.));
#172654=CARTESIAN_POINT('Ctrl Pts',(69.1965599718761,11.3018540025605,0.));
#172655=CARTESIAN_POINT('Ctrl Pts',(69.1965599718761,11.3018540025605,12.));
#172656=CARTESIAN_POINT('Ctrl Pts',(69.1769483991639,11.3038812726275,0.));
#172657=CARTESIAN_POINT('Ctrl Pts',(69.1769483991639,11.3038812726275,12.));
#172658=CARTESIAN_POINT('Ctrl Pts',(69.1573884361076,11.3058820128323,0.));
#172659=CARTESIAN_POINT('Ctrl Pts',(69.1573884361076,11.3058820128323,12.));
#172660=CARTESIAN_POINT('Ctrl Pts',(69.137880225198,11.3078562764442,0.));
#172661=CARTESIAN_POINT('Ctrl Pts',(69.137880225198,11.3078562764442,12.));
#172662=CARTESIAN_POINT('Ctrl Pts',(69.1184238445065,11.3098040973799,0.));
#172663=CARTESIAN_POINT('Ctrl Pts',(69.1184238445065,11.3098040973799,12.));
#172664=CARTESIAN_POINT('Ctrl Pts',(69.1029002322497,11.3113412156742,0.));
#172665=CARTESIAN_POINT('Ctrl Pts',(69.1029002322497,11.3113412156742,12.));
#172666=CARTESIAN_POINT('Ctrl Pts',(69.0912808657051,11.3124821678849,0.));
#172667=CARTESIAN_POINT('Ctrl Pts',(69.0912808657051,11.3124821678849,12.));
#172668=CARTESIAN_POINT('Ctrl Pts',(69.0835449954486,11.3132375200184,0.));
#172669=CARTESIAN_POINT('Ctrl Pts',(69.0835449954486,11.3132375200184,12.));
#172670=CARTESIAN_POINT('Ctrl Pts',(69.079679653846,11.3136138754165,0.));
#172671=CARTESIAN_POINT('Ctrl Pts',(69.079679653846,11.3136138754165,12.));
#172672=CARTESIAN_POINT('',(69.079679653846,11.3136138754165,12.));
#172673=CARTESIAN_POINT('Ctrl Pts',(69.079679653846,11.3136138754165,12.));
#172674=CARTESIAN_POINT('Ctrl Pts',(69.0835449954486,11.3132375200184,12.));
#172675=CARTESIAN_POINT('Ctrl Pts',(69.0912808657051,11.3124821678849,12.));
#172676=CARTESIAN_POINT('Ctrl Pts',(69.1029002322497,11.3113412156742,12.));
#172677=CARTESIAN_POINT('Ctrl Pts',(69.1184238445065,11.3098040973799,12.));
#172678=CARTESIAN_POINT('Ctrl Pts',(69.137880225198,11.3078562764442,12.));
#172679=CARTESIAN_POINT('Ctrl Pts',(69.1573884361076,11.3058820128323,12.));
#172680=CARTESIAN_POINT('Ctrl Pts',(69.1769483991639,11.3038812726275,12.));
#172681=CARTESIAN_POINT('Ctrl Pts',(69.1965599718761,11.3018540025605,12.));
#172682=CARTESIAN_POINT('Ctrl Pts',(69.216222948839,11.2998001310934,12.));
#172683=CARTESIAN_POINT('Ctrl Pts',(69.2359370894828,11.2977195764836,12.));
#172684=CARTESIAN_POINT('Ctrl Pts',(69.255702139335,11.2956122531375,12.));
#172685=CARTESIAN_POINT('Ctrl Pts',(69.2755178531534,11.2934780784362,12.));
#172686=CARTESIAN_POINT('Ctrl Pts',(69.2953840192792,11.2913169799642,12.));
#172687=CARTESIAN_POINT('Ctrl Pts',(69.315300451784,11.2891288931528,12.));
#172688=CARTESIAN_POINT('Ctrl Pts',(69.3352669789611,11.2869137578463,12.));
#172689=CARTESIAN_POINT('Ctrl Pts',(69.3552834337771,11.2846715154521,12.));
#172690=CARTESIAN_POINT('Ctrl Pts',(69.375349642,11.2824021054038,12.));
#172691=CARTESIAN_POINT('Ctrl Pts',(69.395465416223,11.2801054633807,12.));
#172692=CARTESIAN_POINT('Ctrl Pts',(69.4156305620554,11.2777815231462,12.));
#172693=CARTESIAN_POINT('Ctrl Pts',(69.4358448819957,11.2754302177019,12.));
#172694=CARTESIAN_POINT('Ctrl Pts',(69.4561081798815,11.2730514806143,12.));
#172695=CARTESIAN_POINT('Ctrl Pts',(69.4764202659443,11.2706452475287,12.));
#172696=CARTESIAN_POINT('Ctrl Pts',(69.4967809565978,11.2682114561015,12.));
#172697=CARTESIAN_POINT('Ctrl Pts',(69.5171900720188,11.2657500452721,12.));
#172698=CARTESIAN_POINT('Ctrl Pts',(69.5376474344768,11.2632609547629,12.));
#172699=CARTESIAN_POINT('Ctrl Pts',(69.5581528662846,11.2607441244698,12.));
#172700=CARTESIAN_POINT('Ctrl Pts',(69.5787061880815,11.2581994939534,12.));
#172701=CARTESIAN_POINT('Ctrl Pts',(69.5993072197355,11.255627002701,12.));
#172702=CARTESIAN_POINT('Ctrl Pts',(69.6199557811231,11.2530265903555,12.));
#172703=CARTESIAN_POINT('Ctrl Pts',(69.6406516928902,11.2503981969414,12.));
#172704=CARTESIAN_POINT('Ctrl Pts',(69.6613947773563,11.2477417631391,12.));
#172705=CARTESIAN_POINT('Ctrl Pts',(69.6821848588492,11.2450572303847,12.));
#172706=CARTESIAN_POINT('Ctrl Pts',(69.7030217632187,11.242344540717,12.));
#172707=CARTESIAN_POINT('Ctrl Pts',(69.7239053175362,11.2396036366861,12.));
#172708=CARTESIAN_POINT('Ctrl Pts',(69.7448353497394,11.236834461247,12.));
#172709=CARTESIAN_POINT('Ctrl Pts',(69.7658116882298,11.2340369576452,12.));
#172710=CARTESIAN_POINT('Ctrl Pts',(69.7868341618927,11.2312110694183,12.));
#172711=CARTESIAN_POINT('Ctrl Pts',(69.8079026002753,11.2283567404434,12.));
#172712=CARTESIAN_POINT('Ctrl Pts',(69.8290168337076,11.225473914972,12.));
#172713=CARTESIAN_POINT('Ctrl Pts',(69.8501766934445,11.2225625376739,12.));
#172714=CARTESIAN_POINT('Ctrl Pts',(69.8713820117918,11.2196225536794,12.));
#172715=CARTESIAN_POINT('Ctrl Pts',(69.8926326220414,11.2166539085527,12.));
#172716=CARTESIAN_POINT('Ctrl Pts',(69.9139283584036,11.213656548268,12.));
#172717=CARTESIAN_POINT('Ctrl Pts',(69.9352690559399,11.2106304191881,12.));
#172718=CARTESIAN_POINT('Ctrl Pts',(69.9566545504813,11.2075754680445,12.));
#172719=CARTESIAN_POINT('Ctrl Pts',(69.9780846785771,11.2044916419239,12.));
#172720=CARTESIAN_POINT('Ctrl Pts',(69.9995592775322,11.2013788882711,12.));
#172721=CARTESIAN_POINT('Ctrl Pts',(70.0210781854236,11.1982371548918,12.));
#172722=CARTESIAN_POINT('Ctrl Pts',(70.0426412411194,11.1950663899578,12.));
#172723=CARTESIAN_POINT('Ctrl Pts',(70.0642482842942,11.1918665420168,12.));
#172724=CARTESIAN_POINT('Ctrl Pts',(70.0858991554295,11.1886375599916,12.));
#172725=CARTESIAN_POINT('Ctrl Pts',(70.1075936957973,11.185379393167,12.));
#172726=CARTESIAN_POINT('Ctrl Pts',(70.1293317474432,11.1820919911846,12.));
#172727=CARTESIAN_POINT('Ctrl Pts',(70.1511131531672,11.1787753040363,12.));
#172728=CARTESIAN_POINT('Ctrl Pts',(70.1729377564954,11.1754292820631,12.));
#172729=CARTESIAN_POINT('Ctrl Pts',(70.1948054016816,11.1720538759499,12.));
#172730=CARTESIAN_POINT('Ctrl Pts',(70.2167159337094,11.168649036721,12.));
#172731=CARTESIAN_POINT('Ctrl Pts',(70.2386691982902,11.1652147157383,12.));
#172732=CARTESIAN_POINT('Ctrl Pts',(70.2606650418589,11.1617508647016,12.));
#172733=CARTESIAN_POINT('Ctrl Pts',(70.2827033115662,11.1582574356521,12.));
#172734=CARTESIAN_POINT('Ctrl Pts',(70.3047838552756,11.1547343809646,12.));
#172735=CARTESIAN_POINT('Ctrl Pts',(70.326906521559,11.1511816533421,12.));
#172736=CARTESIAN_POINT('Ctrl Pts',(70.349071159688,11.1475992058124,12.));
#172737=CARTESIAN_POINT('Ctrl Pts',(70.3712776196223,11.143986991727,12.));
#172738=CARTESIAN_POINT('Ctrl Pts',(70.393525751996,11.1403449647625,12.));
#172739=CARTESIAN_POINT('Ctrl Pts',(70.4158154081205,11.1366730789126,12.));
#172740=CARTESIAN_POINT('Ctrl Pts',(70.4381464399819,11.1329712884847,12.));
#172741=CARTESIAN_POINT('Ctrl Pts',(70.4605187002354,11.1292395480974,12.));
#172742=CARTESIAN_POINT('Ctrl Pts',(70.4829320421957,11.1254778126821,12.));
#172743=CARTESIAN_POINT('Ctrl Pts',(70.505386319828,11.1216860374826,12.));
#172744=CARTESIAN_POINT('Ctrl Pts',(70.5278813877494,11.1178641780476,12.));
#172745=CARTESIAN_POINT('Ctrl Pts',(70.5504171012233,11.1140121902271,12.));
#172746=CARTESIAN_POINT('Ctrl Pts',(70.5729933161546,11.1101300301702,12.));
#172747=CARTESIAN_POINT('Ctrl Pts',(70.5956098890773,11.1062176543262,12.));
#172748=CARTESIAN_POINT('Ctrl Pts',(70.6182666771481,11.1022750194446,12.));
#172749=CARTESIAN_POINT('Ctrl Pts',(70.6409635381482,11.0983020825667,12.));
#172750=CARTESIAN_POINT('Ctrl Pts',(70.6637003304785,11.0942988010233,12.));
#172751=CARTESIAN_POINT('Ctrl Pts',(70.6864769131546,11.0902651324323,12.));
#172752=CARTESIAN_POINT('Ctrl Pts',(70.7092931457954,11.0862010347016,12.));
#172753=CARTESIAN_POINT('Ctrl Pts',(70.732148888618,11.0821064660269,12.));
#172754=CARTESIAN_POINT('Ctrl Pts',(70.7550440024384,11.0779813848846,12.));
#172755=CARTESIAN_POINT('Ctrl Pts',(70.7779783486677,11.0738257500291,12.));
#172756=CARTESIAN_POINT('Ctrl Pts',(70.8009517893057,11.0696395204909,12.));
#172757=CARTESIAN_POINT('Ctrl Pts',(70.8239641869299,11.0654226555802,12.));
#172758=CARTESIAN_POINT('Ctrl Pts',(70.8470154046919,11.0611751148835,12.));
#172759=CARTESIAN_POINT('Ctrl Pts',(70.8701053063186,11.0568968582569,12.));
#172760=CARTESIAN_POINT('Ctrl Pts',(70.8932337561087,11.0525878458243,12.));
#172761=CARTESIAN_POINT('Ctrl Pts',(70.916400618927,11.048248037975,12.));
#172762=CARTESIAN_POINT('Ctrl Pts',(70.9396057601924,11.0438773953682,12.));
#172763=CARTESIAN_POINT('Ctrl Pts',(70.9628490458748,11.0394758789285,12.));
#172764=CARTESIAN_POINT('Ctrl Pts',(70.986130342497,11.0350434498405,12.));
#172765=CARTESIAN_POINT('Ctrl Pts',(71.0094495171292,11.0305800695456,12.));
#172766=CARTESIAN_POINT('Ctrl Pts',(71.0328064373856,11.0260856997415,12.));
#172767=CARTESIAN_POINT('Ctrl Pts',(71.0562009714136,11.0215603023856,12.));
#172768=CARTESIAN_POINT('Ctrl Pts',(71.0796329878907,11.0170038396915,12.));
#172769=CARTESIAN_POINT('Ctrl Pts',(71.1031023560249,11.0124162741225,12.));
#172770=CARTESIAN_POINT('Ctrl Pts',(71.1266089455517,11.0077975683895,12.));
#172771=CARTESIAN_POINT('Ctrl Pts',(71.1501526267286,11.0031476854502,12.));
#172772=CARTESIAN_POINT('Ctrl Pts',(71.1737332703248,10.9984665885127,12.));
#172773=CARTESIAN_POINT('Ctrl Pts',(71.1973507476191,10.993754241032,12.));
#172774=CARTESIAN_POINT('Ctrl Pts',(71.2210049304014,10.9890106067039,12.));
#172775=CARTESIAN_POINT('Ctrl Pts',(71.2446956909687,10.9842356494627,12.));
#172776=CARTESIAN_POINT('Ctrl Pts',(71.2684229021207,10.9794293334805,12.));
#172777=CARTESIAN_POINT('Ctrl Pts',(71.2921864371491,10.9745916231709,12.));
#172778=CARTESIAN_POINT('Ctrl Pts',(71.3159861698358,10.969722483186,12.));
#172779=CARTESIAN_POINT('Ctrl Pts',(71.339821974454,10.9648218784098,12.));
#172780=CARTESIAN_POINT('Ctrl Pts',(71.3636937257649,10.9598897739565,12.));
#172781=CARTESIAN_POINT('Ctrl Pts',(71.3876012990138,10.954926135169,12.));
#172782=CARTESIAN_POINT('Ctrl Pts',(71.4115445699194,10.9499309276237,12.));
#172783=CARTESIAN_POINT('Ctrl Pts',(71.435523414672,10.944904117127,12.));
#172784=CARTESIAN_POINT('Ctrl Pts',(71.4595377099351,10.9398456697095,12.));
#172785=CARTESIAN_POINT('Ctrl Pts',(71.4835873328423,10.9347555516235,12.));
#172786=CARTESIAN_POINT('Ctrl Pts',(71.5076721609936,10.9296337293425,12.));
#172787=CARTESIAN_POINT('Ctrl Pts',(71.5317920724459,10.9244801695642,12.));
#172788=CARTESIAN_POINT('Ctrl Pts',(71.5559469457091,10.91929483921,12.));
#172789=CARTESIAN_POINT('Ctrl Pts',(71.5801366597488,10.914077705417,12.));
#172790=CARTESIAN_POINT('Ctrl Pts',(71.6043610939835,10.9088287355365,12.));
#172791=CARTESIAN_POINT('Ctrl Pts',(71.6286201282812,10.9035478971328,12.));
#172792=CARTESIAN_POINT('Ctrl Pts',(71.6529136429504,10.8982351579871,12.));
#172793=CARTESIAN_POINT('Ctrl Pts',(71.6772415187364,10.8928904860964,12.));
#172794=CARTESIAN_POINT('Ctrl Pts',(71.7016036368236,10.8875138496671,12.));
#172795=CARTESIAN_POINT('Ctrl Pts',(71.7259998788328,10.8821052171121,12.));
#172796=CARTESIAN_POINT('Ctrl Pts',(71.7504301268181,10.8766645570497,12.));
#172797=CARTESIAN_POINT('Ctrl Pts',(71.7748942632593,10.8711918383073,12.));
#172798=CARTESIAN_POINT('Ctrl Pts',(71.7993921710564,10.865687029922,12.));
#172799=CARTESIAN_POINT('Ctrl Pts',(71.8239237335331,10.8601501011332,12.));
#172800=CARTESIAN_POINT('Ctrl Pts',(71.8484888344339,10.8545810213799,12.));
#172801=CARTESIAN_POINT('Ctrl Pts',(71.8730873579224,10.8489797602998,12.));
#172802=CARTESIAN_POINT('Ctrl Pts',(71.8977191885725,10.8433462877312,12.));
#172803=CARTESIAN_POINT('Ctrl Pts',(71.9223842113625,10.8376805737159,12.));
#172804=CARTESIAN_POINT('Ctrl Pts',(71.9470823116785,10.8319825884918,12.));
#172805=CARTESIAN_POINT('Ctrl Pts',(71.9718133753127,10.8262523024898,12.));
#172806=CARTESIAN_POINT('Ctrl Pts',(71.9965772884619,10.8204896863328,12.));
#172807=CARTESIAN_POINT('Ctrl Pts',(72.0213739377223,10.8146947108375,12.));
#172808=CARTESIAN_POINT('Ctrl Pts',(72.0462032100815,10.8088673470184,12.));
#172809=CARTESIAN_POINT('Ctrl Pts',(72.0710649929202,10.8030075660809,12.));
#172810=CARTESIAN_POINT('Ctrl Pts',(72.0959591740114,10.7971153394166,12.));
#172811=CARTESIAN_POINT('Ctrl Pts',(72.1208856415171,10.7911906386027,12.));
#172812=CARTESIAN_POINT('Ctrl Pts',(72.1458442839834,10.7852334354016,12.));
#172813=CARTESIAN_POINT('Ctrl Pts',(72.1708349903305,10.7792437017662,12.));
#172814=CARTESIAN_POINT('Ctrl Pts',(72.1958576498557,10.7732214098345,12.));
#172815=CARTESIAN_POINT('Ctrl Pts',(72.2209121522366,10.7671665319255,12.));
#172816=CARTESIAN_POINT('Ctrl Pts',(72.2459983875296,10.7610790405385,12.));
#172817=CARTESIAN_POINT('Ctrl Pts',(72.2711162461681,10.7549589083535,12.));
#172818=CARTESIAN_POINT('Ctrl Pts',(72.2962656189556,10.7488061082368,12.));
#172819=CARTESIAN_POINT('Ctrl Pts',(72.3214463970641,10.7426206132375,12.));
#172820=CARTESIAN_POINT('Ctrl Pts',(72.3466584720318,10.73640239658,12.));
#172821=CARTESIAN_POINT('Ctrl Pts',(72.3719017357571,10.7301514316607,12.));
#172822=CARTESIAN_POINT('Ctrl Pts',(72.3971760804933,10.7238676920469,12.));
#172823=CARTESIAN_POINT('Ctrl Pts',(72.4224813988347,10.7175511514789,12.));
#172824=CARTESIAN_POINT('Ctrl Pts',(72.4478175837156,10.7112017838706,12.));
#172825=CARTESIAN_POINT('Ctrl Pts',(72.4731845284227,10.7048195633061,12.));
#172826=CARTESIAN_POINT('Ctrl Pts',(72.4985821266023,10.6984044640398,12.));
#172827=CARTESIAN_POINT('Ctrl Pts',(72.5240102722664,10.691956460499,12.));
#172828=CARTESIAN_POINT('Ctrl Pts',(72.5494688597961,10.6854755272904,12.));
#172829=CARTESIAN_POINT('Ctrl Pts',(72.5749577839415,10.6789616392042,12.));
#172830=CARTESIAN_POINT('Ctrl Pts',(72.6004769398019,10.6724147711995,12.));
#172831=CARTESIAN_POINT('Ctrl Pts',(72.6260262228065,10.6658348983945,12.));
#172832=CARTESIAN_POINT('Ctrl Pts',(72.651605528691,10.6592219960581,12.));
#172833=CARTESIAN_POINT('Ctrl Pts',(72.6772147534752,10.6525760396054,12.));
#172834=CARTESIAN_POINT('Ctrl Pts',(72.7028537934317,10.6458970045946,12.));
#172835=CARTESIAN_POINT('Ctrl Pts',(72.7285225451293,10.6391848667352,12.));
#172836=CARTESIAN_POINT('Ctrl Pts',(72.7542209054812,10.6324396018998,12.));
#172837=CARTESIAN_POINT('Ctrl Pts',(72.7799487717911,10.6256611861394,12.));
#172838=CARTESIAN_POINT('Ctrl Pts',(72.8057060417887,10.6188495956973,12.));
#172839=CARTESIAN_POINT('Ctrl Pts',(72.8314926136881,10.6120048070368,12.));
#172840=CARTESIAN_POINT('Ctrl Pts',(72.8573083861337,10.6051267968203,12.));
#172841=CARTESIAN_POINT('Ctrl Pts',(72.8831532580845,10.5982155418626,12.));
#172842=CARTESIAN_POINT('Ctrl Pts',(72.9090271287083,10.5912710190928,12.));
#172843=CARTESIAN_POINT('Ctrl Pts',(72.9349298972822,10.5842932055209,12.));
#172844=CARTESIAN_POINT('Ctrl Pts',(72.9608614630534,10.5772820781958,12.));
#172845=CARTESIAN_POINT('Ctrl Pts',(72.9868217252283,10.570237614205,12.));
#172846=CARTESIAN_POINT('Ctrl Pts',(73.0128105832621,10.5631597907651,12.));
#172847=CARTESIAN_POINT('Ctrl Pts',(73.0388279370834,10.5560485852974,12.));
#172848=CARTESIAN_POINT('Ctrl Pts',(73.0648736873434,10.5489039755138,12.));
#172849=CARTESIAN_POINT('Ctrl Pts',(73.0909477356474,10.5417259395003,12.));
#172850=CARTESIAN_POINT('Ctrl Pts',(73.1170499848039,10.53451445581,12.));
#172851=CARTESIAN_POINT('Ctrl Pts',(73.1431803382711,10.5272695032653,12.));
#172852=CARTESIAN_POINT('Ctrl Pts',(73.1693386996138,10.5199910607655,12.));
#172853=CARTESIAN_POINT('Ctrl Pts',(73.1955249719048,10.5126791070805,12.));
#172854=CARTESIAN_POINT('Ctrl Pts',(73.2217390572562,10.5053336206908,12.));
#172855=CARTESIAN_POINT('Ctrl Pts',(73.2479808560189,10.4979545795192,12.));
#172856=CARTESIAN_POINT('Ctrl Pts',(73.2742502674304,10.4905419611523,12.));
#172857=CARTESIAN_POINT('Ctrl Pts',(73.3005471910583,10.4830957433305,12.));
#172858=CARTESIAN_POINT('Ctrl Pts',(73.3268715280575,10.4756159043806,12.));
#172859=CARTESIAN_POINT('Ctrl Pts',(73.3532231823659,10.4681024236289,12.));
#172860=CARTESIAN_POINT('Ctrl Pts',(73.37960206225,10.4605552819397,12.));
#172861=CARTESIAN_POINT('Ctrl Pts',(73.4060080806686,10.452974461845,12.));
#172862=CARTESIAN_POINT('Ctrl Pts',(73.4286663448108,10.4464473465479,12.));
#172863=CARTESIAN_POINT('Ctrl Pts',(73.44605255288,10.4414249334739,12.));
#172864=CARTESIAN_POINT('Ctrl Pts',(73.4581547436839,10.4379221501041,12.));
#172865=CARTESIAN_POINT('Ctrl Pts',(73.4649650361894,10.4359488742809,12.));
#172866=CARTESIAN_POINT('Ctrl Pts',(73.466479592994,10.4355099267296,12.));
#172867=CARTESIAN_POINT('',(69.079679653846,11.3136138754165,0.));
#172868=CARTESIAN_POINT('',(69.079679653846,11.3136138754165,0.));
#172869=CARTESIAN_POINT('Ctrl Pts',(73.466479592994,10.4355099267296,0.));
#172870=CARTESIAN_POINT('Ctrl Pts',(73.4649650361895,10.4359488742808,0.));
#172871=CARTESIAN_POINT('Ctrl Pts',(73.4581547436839,10.4379221501041,0.));
#172872=CARTESIAN_POINT('Ctrl Pts',(73.4460525528801,10.4414249334739,0.));
#172873=CARTESIAN_POINT('Ctrl Pts',(73.4286663448108,10.4464473465479,0.));
#172874=CARTESIAN_POINT('Ctrl Pts',(73.4060080806686,10.452974461845,0.));
#172875=CARTESIAN_POINT('Ctrl Pts',(73.37960206225,10.4605552819397,0.));
#172876=CARTESIAN_POINT('Ctrl Pts',(73.3532231823659,10.4681024236289,0.));
#172877=CARTESIAN_POINT('Ctrl Pts',(73.3268715280575,10.4756159043806,0.));
#172878=CARTESIAN_POINT('Ctrl Pts',(73.3005471910583,10.4830957433305,0.));
#172879=CARTESIAN_POINT('Ctrl Pts',(73.2742502674304,10.4905419611523,0.));
#172880=CARTESIAN_POINT('Ctrl Pts',(73.2479808560189,10.4979545795192,0.));
#172881=CARTESIAN_POINT('Ctrl Pts',(73.2217390572562,10.5053336206908,0.));
#172882=CARTESIAN_POINT('Ctrl Pts',(73.1955249719048,10.5126791070805,0.));
#172883=CARTESIAN_POINT('Ctrl Pts',(73.1693386996138,10.5199910607655,0.));
#172884=CARTESIAN_POINT('Ctrl Pts',(73.1431803382711,10.5272695032653,0.));
#172885=CARTESIAN_POINT('Ctrl Pts',(73.1170499848039,10.53451445581,0.));
#172886=CARTESIAN_POINT('Ctrl Pts',(73.0909477356474,10.5417259395003,0.));
#172887=CARTESIAN_POINT('Ctrl Pts',(73.0648736873434,10.5489039755138,0.));
#172888=CARTESIAN_POINT('Ctrl Pts',(73.0388279370834,10.5560485852974,0.));
#172889=CARTESIAN_POINT('Ctrl Pts',(73.0128105832621,10.5631597907651,0.));
#172890=CARTESIAN_POINT('Ctrl Pts',(72.9868217252283,10.570237614205,0.));
#172891=CARTESIAN_POINT('Ctrl Pts',(72.9608614630534,10.5772820781958,0.));
#172892=CARTESIAN_POINT('Ctrl Pts',(72.9349298972822,10.5842932055209,0.));
#172893=CARTESIAN_POINT('Ctrl Pts',(72.9090271287083,10.5912710190928,0.));
#172894=CARTESIAN_POINT('Ctrl Pts',(72.8831532580845,10.5982155418626,0.));
#172895=CARTESIAN_POINT('Ctrl Pts',(72.8573083861337,10.6051267968203,0.));
#172896=CARTESIAN_POINT('Ctrl Pts',(72.8314926136881,10.6120048070368,0.));
#172897=CARTESIAN_POINT('Ctrl Pts',(72.8057060417887,10.6188495956973,0.));
#172898=CARTESIAN_POINT('Ctrl Pts',(72.7799487717911,10.6256611861394,0.));
#172899=CARTESIAN_POINT('Ctrl Pts',(72.7542209054812,10.6324396018998,0.));
#172900=CARTESIAN_POINT('Ctrl Pts',(72.7285225451293,10.6391848667352,0.));
#172901=CARTESIAN_POINT('Ctrl Pts',(72.7028537934317,10.6458970045946,0.));
#172902=CARTESIAN_POINT('Ctrl Pts',(72.6772147534752,10.6525760396054,0.));
#172903=CARTESIAN_POINT('Ctrl Pts',(72.651605528691,10.6592219960581,0.));
#172904=CARTESIAN_POINT('Ctrl Pts',(72.6260262228065,10.6658348983945,0.));
#172905=CARTESIAN_POINT('Ctrl Pts',(72.6004769398019,10.6724147711995,0.));
#172906=CARTESIAN_POINT('Ctrl Pts',(72.5749577839415,10.6789616392042,0.));
#172907=CARTESIAN_POINT('Ctrl Pts',(72.5494688597961,10.6854755272904,0.));
#172908=CARTESIAN_POINT('Ctrl Pts',(72.5240102722664,10.691956460499,0.));
#172909=CARTESIAN_POINT('Ctrl Pts',(72.4985821266023,10.6984044640398,0.));
#172910=CARTESIAN_POINT('Ctrl Pts',(72.4731845284227,10.7048195633061,0.));
#172911=CARTESIAN_POINT('Ctrl Pts',(72.4478175837156,10.7112017838706,0.));
#172912=CARTESIAN_POINT('Ctrl Pts',(72.4224813988347,10.7175511514789,0.));
#172913=CARTESIAN_POINT('Ctrl Pts',(72.3971760804933,10.7238676920469,0.));
#172914=CARTESIAN_POINT('Ctrl Pts',(72.3719017357571,10.7301514316607,0.));
#172915=CARTESIAN_POINT('Ctrl Pts',(72.3466584720318,10.73640239658,0.));
#172916=CARTESIAN_POINT('Ctrl Pts',(72.3214463970641,10.7426206132375,0.));
#172917=CARTESIAN_POINT('Ctrl Pts',(72.2962656189556,10.7488061082368,0.));
#172918=CARTESIAN_POINT('Ctrl Pts',(72.2711162461681,10.7549589083535,0.));
#172919=CARTESIAN_POINT('Ctrl Pts',(72.2459983875296,10.7610790405385,0.));
#172920=CARTESIAN_POINT('Ctrl Pts',(72.2209121522366,10.7671665319255,0.));
#172921=CARTESIAN_POINT('Ctrl Pts',(72.1958576498557,10.7732214098345,0.));
#172922=CARTESIAN_POINT('Ctrl Pts',(72.1708349903305,10.7792437017662,0.));
#172923=CARTESIAN_POINT('Ctrl Pts',(72.1458442839834,10.7852334354016,0.));
#172924=CARTESIAN_POINT('Ctrl Pts',(72.1208856415171,10.7911906386027,0.));
#172925=CARTESIAN_POINT('Ctrl Pts',(72.0959591740114,10.7971153394166,0.));
#172926=CARTESIAN_POINT('Ctrl Pts',(72.0710649929202,10.8030075660809,0.));
#172927=CARTESIAN_POINT('Ctrl Pts',(72.0462032100815,10.8088673470184,0.));
#172928=CARTESIAN_POINT('Ctrl Pts',(72.0213739377223,10.8146947108375,0.));
#172929=CARTESIAN_POINT('Ctrl Pts',(71.9965772884619,10.8204896863328,0.));
#172930=CARTESIAN_POINT('Ctrl Pts',(71.9718133753127,10.8262523024898,0.));
#172931=CARTESIAN_POINT('Ctrl Pts',(71.9470823116785,10.8319825884918,0.));
#172932=CARTESIAN_POINT('Ctrl Pts',(71.9223842113625,10.8376805737159,0.));
#172933=CARTESIAN_POINT('Ctrl Pts',(71.8977191885725,10.8433462877312,0.));
#172934=CARTESIAN_POINT('Ctrl Pts',(71.8730873579224,10.8489797602998,0.));
#172935=CARTESIAN_POINT('Ctrl Pts',(71.8484888344339,10.8545810213799,0.));
#172936=CARTESIAN_POINT('Ctrl Pts',(71.8239237335331,10.8601501011332,0.));
#172937=CARTESIAN_POINT('Ctrl Pts',(71.7993921710564,10.865687029922,0.));
#172938=CARTESIAN_POINT('Ctrl Pts',(71.7748942632593,10.8711918383073,0.));
#172939=CARTESIAN_POINT('Ctrl Pts',(71.7504301268181,10.8766645570497,0.));
#172940=CARTESIAN_POINT('Ctrl Pts',(71.7259998788328,10.8821052171121,0.));
#172941=CARTESIAN_POINT('Ctrl Pts',(71.7016036368236,10.8875138496671,0.));
#172942=CARTESIAN_POINT('Ctrl Pts',(71.6772415187364,10.8928904860964,0.));
#172943=CARTESIAN_POINT('Ctrl Pts',(71.6529136429504,10.8982351579871,0.));
#172944=CARTESIAN_POINT('Ctrl Pts',(71.6286201282812,10.9035478971328,0.));
#172945=CARTESIAN_POINT('Ctrl Pts',(71.6043610939835,10.9088287355365,0.));
#172946=CARTESIAN_POINT('Ctrl Pts',(71.5801366597488,10.914077705417,0.));
#172947=CARTESIAN_POINT('Ctrl Pts',(71.5559469457091,10.91929483921,0.));
#172948=CARTESIAN_POINT('Ctrl Pts',(71.5317920724459,10.9244801695642,0.));
#172949=CARTESIAN_POINT('Ctrl Pts',(71.5076721609936,10.9296337293425,0.));
#172950=CARTESIAN_POINT('Ctrl Pts',(71.4835873328423,10.9347555516235,0.));
#172951=CARTESIAN_POINT('Ctrl Pts',(71.4595377099351,10.9398456697095,0.));
#172952=CARTESIAN_POINT('Ctrl Pts',(71.435523414672,10.944904117127,0.));
#172953=CARTESIAN_POINT('Ctrl Pts',(71.4115445699194,10.9499309276237,0.));
#172954=CARTESIAN_POINT('Ctrl Pts',(71.3876012990138,10.954926135169,0.));
#172955=CARTESIAN_POINT('Ctrl Pts',(71.3636937257649,10.9598897739565,0.));
#172956=CARTESIAN_POINT('Ctrl Pts',(71.339821974454,10.9648218784098,0.));
#172957=CARTESIAN_POINT('Ctrl Pts',(71.3159861698358,10.969722483186,0.));
#172958=CARTESIAN_POINT('Ctrl Pts',(71.2921864371491,10.9745916231709,0.));
#172959=CARTESIAN_POINT('Ctrl Pts',(71.2684229021207,10.9794293334805,0.));
#172960=CARTESIAN_POINT('Ctrl Pts',(71.2446956909687,10.9842356494627,0.));
#172961=CARTESIAN_POINT('Ctrl Pts',(71.2210049304014,10.9890106067039,0.));
#172962=CARTESIAN_POINT('Ctrl Pts',(71.1973507476191,10.993754241032,0.));
#172963=CARTESIAN_POINT('Ctrl Pts',(71.1737332703248,10.9984665885127,0.));
#172964=CARTESIAN_POINT('Ctrl Pts',(71.1501526267286,11.0031476854502,0.));
#172965=CARTESIAN_POINT('Ctrl Pts',(71.1266089455517,11.0077975683895,0.));
#172966=CARTESIAN_POINT('Ctrl Pts',(71.1031023560249,11.0124162741225,0.));
#172967=CARTESIAN_POINT('Ctrl Pts',(71.0796329878907,11.0170038396915,0.));
#172968=CARTESIAN_POINT('Ctrl Pts',(71.0562009714136,11.0215603023856,0.));
#172969=CARTESIAN_POINT('Ctrl Pts',(71.0328064373856,11.0260856997415,0.));
#172970=CARTESIAN_POINT('Ctrl Pts',(71.0094495171292,11.0305800695456,0.));
#172971=CARTESIAN_POINT('Ctrl Pts',(70.986130342497,11.0350434498405,0.));
#172972=CARTESIAN_POINT('Ctrl Pts',(70.9628490458748,11.0394758789285,0.));
#172973=CARTESIAN_POINT('Ctrl Pts',(70.9396057601924,11.0438773953682,0.));
#172974=CARTESIAN_POINT('Ctrl Pts',(70.916400618927,11.048248037975,0.));
#172975=CARTESIAN_POINT('Ctrl Pts',(70.8932337561087,11.0525878458243,0.));
#172976=CARTESIAN_POINT('Ctrl Pts',(70.8701053063186,11.0568968582569,0.));
#172977=CARTESIAN_POINT('Ctrl Pts',(70.8470154046919,11.0611751148835,0.));
#172978=CARTESIAN_POINT('Ctrl Pts',(70.8239641869299,11.0654226555802,0.));
#172979=CARTESIAN_POINT('Ctrl Pts',(70.8009517893057,11.0696395204909,0.));
#172980=CARTESIAN_POINT('Ctrl Pts',(70.7779783486677,11.0738257500291,0.));
#172981=CARTESIAN_POINT('Ctrl Pts',(70.7550440024384,11.0779813848846,0.));
#172982=CARTESIAN_POINT('Ctrl Pts',(70.732148888618,11.0821064660269,0.));
#172983=CARTESIAN_POINT('Ctrl Pts',(70.7092931457954,11.0862010347016,0.));
#172984=CARTESIAN_POINT('Ctrl Pts',(70.6864769131546,11.0902651324323,0.));
#172985=CARTESIAN_POINT('Ctrl Pts',(70.6637003304785,11.0942988010233,0.));
#172986=CARTESIAN_POINT('Ctrl Pts',(70.6409635381482,11.0983020825667,0.));
#172987=CARTESIAN_POINT('Ctrl Pts',(70.6182666771481,11.1022750194446,0.));
#172988=CARTESIAN_POINT('Ctrl Pts',(70.5956098890773,11.1062176543262,0.));
#172989=CARTESIAN_POINT('Ctrl Pts',(70.5729933161546,11.1101300301702,0.));
#172990=CARTESIAN_POINT('Ctrl Pts',(70.5504171012233,11.1140121902271,0.));
#172991=CARTESIAN_POINT('Ctrl Pts',(70.5278813877494,11.1178641780476,0.));
#172992=CARTESIAN_POINT('Ctrl Pts',(70.505386319828,11.1216860374826,0.));
#172993=CARTESIAN_POINT('Ctrl Pts',(70.4829320421957,11.1254778126821,0.));
#172994=CARTESIAN_POINT('Ctrl Pts',(70.4605187002354,11.1292395480974,0.));
#172995=CARTESIAN_POINT('Ctrl Pts',(70.4381464399819,11.1329712884847,0.));
#172996=CARTESIAN_POINT('Ctrl Pts',(70.4158154081205,11.1366730789126,0.));
#172997=CARTESIAN_POINT('Ctrl Pts',(70.393525751996,11.1403449647625,0.));
#172998=CARTESIAN_POINT('Ctrl Pts',(70.3712776196223,11.143986991727,0.));
#172999=CARTESIAN_POINT('Ctrl Pts',(70.349071159688,11.1475992058124,0.));
#173000=CARTESIAN_POINT('Ctrl Pts',(70.326906521559,11.1511816533421,0.));
#173001=CARTESIAN_POINT('Ctrl Pts',(70.3047838552756,11.1547343809646,0.));
#173002=CARTESIAN_POINT('Ctrl Pts',(70.2827033115662,11.1582574356521,0.));
#173003=CARTESIAN_POINT('Ctrl Pts',(70.2606650418589,11.1617508647016,0.));
#173004=CARTESIAN_POINT('Ctrl Pts',(70.2386691982902,11.1652147157383,0.));
#173005=CARTESIAN_POINT('Ctrl Pts',(70.2167159337094,11.168649036721,0.));
#173006=CARTESIAN_POINT('Ctrl Pts',(70.1948054016816,11.1720538759499,0.));
#173007=CARTESIAN_POINT('Ctrl Pts',(70.1729377564954,11.1754292820631,0.));
#173008=CARTESIAN_POINT('Ctrl Pts',(70.1511131531672,11.1787753040363,0.));
#173009=CARTESIAN_POINT('Ctrl Pts',(70.1293317474432,11.1820919911846,0.));
#173010=CARTESIAN_POINT('Ctrl Pts',(70.1075936957973,11.185379393167,0.));
#173011=CARTESIAN_POINT('Ctrl Pts',(70.0858991554295,11.1886375599916,0.));
#173012=CARTESIAN_POINT('Ctrl Pts',(70.0642482842942,11.1918665420168,0.));
#173013=CARTESIAN_POINT('Ctrl Pts',(70.0426412411194,11.1950663899578,0.));
#173014=CARTESIAN_POINT('Ctrl Pts',(70.0210781854236,11.1982371548918,0.));
#173015=CARTESIAN_POINT('Ctrl Pts',(69.9995592775322,11.2013788882711,0.));
#173016=CARTESIAN_POINT('Ctrl Pts',(69.9780846785771,11.2044916419239,0.));
#173017=CARTESIAN_POINT('Ctrl Pts',(69.9566545504813,11.2075754680445,0.));
#173018=CARTESIAN_POINT('Ctrl Pts',(69.9352690559399,11.2106304191881,0.));
#173019=CARTESIAN_POINT('Ctrl Pts',(69.9139283584036,11.213656548268,0.));
#173020=CARTESIAN_POINT('Ctrl Pts',(69.8926326220414,11.2166539085527,0.));
#173021=CARTESIAN_POINT('Ctrl Pts',(69.8713820117918,11.2196225536794,0.));
#173022=CARTESIAN_POINT('Ctrl Pts',(69.8501766934445,11.2225625376739,0.));
#173023=CARTESIAN_POINT('Ctrl Pts',(69.8290168337076,11.225473914972,0.));
#173024=CARTESIAN_POINT('Ctrl Pts',(69.8079026002753,11.2283567404434,0.));
#173025=CARTESIAN_POINT('Ctrl Pts',(69.7868341618927,11.2312110694183,0.));
#173026=CARTESIAN_POINT('Ctrl Pts',(69.7658116882298,11.2340369576452,0.));
#173027=CARTESIAN_POINT('Ctrl Pts',(69.7448353497394,11.236834461247,0.));
#173028=CARTESIAN_POINT('Ctrl Pts',(69.7239053175362,11.2396036366861,0.));
#173029=CARTESIAN_POINT('Ctrl Pts',(69.7030217632187,11.242344540717,0.));
#173030=CARTESIAN_POINT('Ctrl Pts',(69.6821848588492,11.2450572303847,0.));
#173031=CARTESIAN_POINT('Ctrl Pts',(69.6613947773563,11.2477417631391,0.));
#173032=CARTESIAN_POINT('Ctrl Pts',(69.6406516928902,11.2503981969414,0.));
#173033=CARTESIAN_POINT('Ctrl Pts',(69.6199557811231,11.2530265903555,0.));
#173034=CARTESIAN_POINT('Ctrl Pts',(69.5993072197355,11.255627002701,0.));
#173035=CARTESIAN_POINT('Ctrl Pts',(69.5787061880815,11.2581994939534,0.));
#173036=CARTESIAN_POINT('Ctrl Pts',(69.5581528662846,11.2607441244698,0.));
#173037=CARTESIAN_POINT('Ctrl Pts',(69.5376474344768,11.2632609547629,0.));
#173038=CARTESIAN_POINT('Ctrl Pts',(69.5171900720188,11.2657500452721,0.));
#173039=CARTESIAN_POINT('Ctrl Pts',(69.4967809565978,11.2682114561015,0.));
#173040=CARTESIAN_POINT('Ctrl Pts',(69.4764202659443,11.2706452475287,0.));
#173041=CARTESIAN_POINT('Ctrl Pts',(69.4561081798815,11.2730514806143,0.));
#173042=CARTESIAN_POINT('Ctrl Pts',(69.4358448819957,11.2754302177019,0.));
#173043=CARTESIAN_POINT('Ctrl Pts',(69.4156305620554,11.2777815231462,0.));
#173044=CARTESIAN_POINT('Ctrl Pts',(69.395465416223,11.2801054633807,0.));
#173045=CARTESIAN_POINT('Ctrl Pts',(69.375349642,11.2824021054038,0.));
#173046=CARTESIAN_POINT('Ctrl Pts',(69.3552834337771,11.2846715154521,0.));
#173047=CARTESIAN_POINT('Ctrl Pts',(69.3352669789611,11.2869137578463,0.));
#173048=CARTESIAN_POINT('Ctrl Pts',(69.315300451784,11.2891288931528,0.));
#173049=CARTESIAN_POINT('Ctrl Pts',(69.2953840192792,11.2913169799642,0.));
#173050=CARTESIAN_POINT('Ctrl Pts',(69.2755178531534,11.2934780784362,0.));
#173051=CARTESIAN_POINT('Ctrl Pts',(69.255702139335,11.2956122531375,0.));
#173052=CARTESIAN_POINT('Ctrl Pts',(69.2359370894828,11.2977195764836,0.));
#173053=CARTESIAN_POINT('Ctrl Pts',(69.216222948839,11.2998001310934,0.));
#173054=CARTESIAN_POINT('Ctrl Pts',(69.1965599718761,11.3018540025605,0.));
#173055=CARTESIAN_POINT('Ctrl Pts',(69.1769483991639,11.3038812726275,0.));
#173056=CARTESIAN_POINT('Ctrl Pts',(69.1573884361076,11.3058820128323,0.));
#173057=CARTESIAN_POINT('Ctrl Pts',(69.137880225198,11.3078562764442,0.));
#173058=CARTESIAN_POINT('Ctrl Pts',(69.1184238445065,11.3098040973799,0.));
#173059=CARTESIAN_POINT('Ctrl Pts',(69.1029002322497,11.3113412156742,0.));
#173060=CARTESIAN_POINT('Ctrl Pts',(69.0912808657051,11.3124821678849,0.));
#173061=CARTESIAN_POINT('Ctrl Pts',(69.0835449954486,11.3132375200184,0.));
#173062=CARTESIAN_POINT('Ctrl Pts',(69.079679653846,11.3136138754165,0.));
#173063=CARTESIAN_POINT('Origin',(0.,0.,0.));
#173064=CARTESIAN_POINT('',(69.8028570375097,5.24987136994592,0.));
#173065=CARTESIAN_POINT('Origin',(0.,0.,0.));
#173066=CARTESIAN_POINT('',(69.8028570375097,5.24987136994592,12.));
#173067=CARTESIAN_POINT('',(69.8028570375097,5.24987136994592,0.));
#173068=CARTESIAN_POINT('Origin',(0.,0.,12.));
#173069=CARTESIAN_POINT('Origin',(0.,0.,0.));
#173070=CARTESIAN_POINT('Origin',(0.,0.,0.));
#173071=CARTESIAN_POINT('Origin',(0.,0.,12.));
#173072=CARTESIAN_POINT('Origin',(0.,0.,0.));
#173073=CARTESIAN_POINT('Origin',(0.,0.,0.));
#173074=CARTESIAN_POINT('Origin',(0.,0.,12.));
#173075=CARTESIAN_POINT('Origin',(0.,0.,0.));
#173076=CARTESIAN_POINT('Origin',(0.,0.,0.));
#173077=CARTESIAN_POINT('Origin',(0.,0.,12.));
#173078=CARTESIAN_POINT('Origin',(0.,0.,0.));
#173079=CARTESIAN_POINT('Origin',(0.,0.,0.));
#173080=CARTESIAN_POINT('Origin',(0.,0.,12.));
#173081=CARTESIAN_POINT('Origin',(0.,0.,0.));
#173082=CARTESIAN_POINT('Origin',(0.,0.,0.));
#173083=CARTESIAN_POINT('Origin',(0.,0.,12.));
#173084=CARTESIAN_POINT('Origin',(0.,0.,0.));
#173085=CARTESIAN_POINT('Origin',(0.,0.,0.));
#173086=CARTESIAN_POINT('Origin',(0.,0.,12.));
#173087=CARTESIAN_POINT('Origin',(0.,0.,0.));
#173088=CARTESIAN_POINT('Origin',(0.,0.,0.));
#173089=CARTESIAN_POINT('Origin',(0.,0.,12.));
#173090=CARTESIAN_POINT('Origin',(0.,0.,0.));
#173091=CARTESIAN_POINT('Origin',(0.,0.,0.));
#173092=CARTESIAN_POINT('Origin',(0.,0.,12.));
#173093=CARTESIAN_POINT('Origin',(0.,0.,0.));
#173094=CARTESIAN_POINT('Origin',(0.,0.,0.));
#173095=CARTESIAN_POINT('Origin',(0.,0.,12.));
#173096=CARTESIAN_POINT('Origin',(0.,0.,0.));
#173097=CARTESIAN_POINT('Origin',(0.,0.,0.));
#173098=CARTESIAN_POINT('Origin',(0.,0.,12.));
#173099=CARTESIAN_POINT('Origin',(0.,0.,0.));
#173100=CARTESIAN_POINT('Origin',(0.,0.,0.));
#173101=CARTESIAN_POINT('Origin',(0.,0.,12.));
#173102=CARTESIAN_POINT('Origin',(0.,0.,0.));
#173103=CARTESIAN_POINT('Origin',(0.,0.,0.));
#173104=CARTESIAN_POINT('Origin',(0.,0.,12.));
#173105=CARTESIAN_POINT('Origin',(0.,0.,0.));
#173106=CARTESIAN_POINT('Origin',(0.,0.,0.));
#173107=CARTESIAN_POINT('Origin',(0.,0.,12.));
#173108=CARTESIAN_POINT('Origin',(0.,0.,0.));
#173109=CARTESIAN_POINT('Origin',(0.,0.,0.));
#173110=CARTESIAN_POINT('Origin',(0.,0.,12.));
#173111=CARTESIAN_POINT('Origin',(0.,0.,0.));
#173112=CARTESIAN_POINT('Origin',(0.,0.,0.));
#173113=CARTESIAN_POINT('Origin',(0.,0.,12.));
#173114=CARTESIAN_POINT('Origin',(0.,0.,0.));
#173115=CARTESIAN_POINT('Origin',(0.,0.,0.));
#173116=CARTESIAN_POINT('Origin',(0.,0.,12.));
#173117=CARTESIAN_POINT('Origin',(0.,0.,0.));
#173118=CARTESIAN_POINT('Origin',(0.,0.,0.));
#173119=CARTESIAN_POINT('Origin',(0.,0.,12.));
#173120=CARTESIAN_POINT('Origin',(0.,0.,0.));
#173121=CARTESIAN_POINT('Origin',(0.,0.,0.));
#173122=CARTESIAN_POINT('Origin',(0.,0.,12.));
#173123=CARTESIAN_POINT('Origin',(0.,0.,0.));
#173124=CARTESIAN_POINT('Origin',(0.,0.,0.));
#173125=CARTESIAN_POINT('Origin',(0.,0.,12.));
#173126=CARTESIAN_POINT('Origin',(0.,0.,0.));
#173127=CARTESIAN_POINT('Origin',(0.,0.,0.));
#173128=CARTESIAN_POINT('Origin',(0.,0.,12.));
#173129=CARTESIAN_POINT('Origin',(0.,0.,0.));
#173130=CARTESIAN_POINT('Origin',(0.,0.,0.));
#173131=CARTESIAN_POINT('Origin',(0.,0.,12.));
#173132=CARTESIAN_POINT('Origin',(0.,0.,0.));
#173133=CARTESIAN_POINT('Origin',(0.,0.,0.));
#173134=CARTESIAN_POINT('Origin',(0.,0.,12.));
#173135=CARTESIAN_POINT('Origin',(0.,0.,0.));
#173136=CARTESIAN_POINT('Origin',(0.,0.,0.));
#173137=CARTESIAN_POINT('Origin',(0.,0.,12.));
#173138=CARTESIAN_POINT('Origin',(0.,0.,0.));
#173139=CARTESIAN_POINT('Origin',(0.,0.,0.));
#173140=CARTESIAN_POINT('Origin',(0.,0.,12.));
#173141=CARTESIAN_POINT('Origin',(0.,0.,0.));
#173142=CARTESIAN_POINT('Origin',(0.,0.,0.));
#173143=CARTESIAN_POINT('Origin',(0.,0.,12.));
#173144=CARTESIAN_POINT('Origin',(0.,0.,0.));
#173145=CARTESIAN_POINT('Origin',(0.,0.,0.));
#173146=CARTESIAN_POINT('Origin',(0.,0.,12.));
#173147=CARTESIAN_POINT('Origin',(0.,0.,0.));
#173148=CARTESIAN_POINT('Origin',(0.,0.,0.));
#173149=CARTESIAN_POINT('Origin',(0.,0.,12.));
#173150=CARTESIAN_POINT('Origin',(0.,0.,0.));
#173151=CARTESIAN_POINT('Origin',(0.,0.,0.));
#173152=CARTESIAN_POINT('Origin',(0.,0.,12.));
#173153=CARTESIAN_POINT('Origin',(0.,0.,0.));
#173154=CARTESIAN_POINT('Origin',(0.,0.,0.));
#173155=CARTESIAN_POINT('Origin',(0.,0.,12.));
#173156=CARTESIAN_POINT('Origin',(0.,0.,0.));
#173157=CARTESIAN_POINT('Origin',(0.,0.,0.));
#173158=CARTESIAN_POINT('Origin',(0.,0.,12.));
#173159=CARTESIAN_POINT('Origin',(0.,0.,0.));
#173160=CARTESIAN_POINT('Origin',(0.,0.,0.));
#173161=CARTESIAN_POINT('Origin',(0.,0.,12.));
#173162=CARTESIAN_POINT('Origin',(0.,0.,0.));
#173163=CARTESIAN_POINT('Origin',(0.,0.,0.));
#173164=CARTESIAN_POINT('Origin',(0.,0.,12.));
#173165=CARTESIAN_POINT('Origin',(0.,0.,0.));
#173166=CARTESIAN_POINT('Origin',(0.,0.,0.));
#173167=CARTESIAN_POINT('Origin',(0.,0.,12.));
#173168=CARTESIAN_POINT('Origin',(0.,0.,0.));
#173169=CARTESIAN_POINT('Origin',(0.,0.,0.));
#173170=CARTESIAN_POINT('Origin',(0.,0.,12.));
#173171=CARTESIAN_POINT('Origin',(0.,0.,0.));
#173172=CARTESIAN_POINT('Origin',(0.,0.,0.));
#173173=CARTESIAN_POINT('Origin',(0.,0.,12.));
#173174=CARTESIAN_POINT('Origin',(0.,0.,0.));
#173175=CARTESIAN_POINT('Origin',(0.,0.,0.));
#173176=CARTESIAN_POINT('Origin',(0.,0.,12.));
#173177=CARTESIAN_POINT('Origin',(0.,0.,0.));
#173178=CARTESIAN_POINT('Origin',(0.,0.,0.));
#173179=CARTESIAN_POINT('Origin',(0.,0.,12.));
#173180=CARTESIAN_POINT('Origin',(0.,0.,0.));
#173181=CARTESIAN_POINT('Origin',(0.,0.,0.));
#173182=CARTESIAN_POINT('Origin',(0.,0.,12.));
#173183=CARTESIAN_POINT('Origin',(0.,0.,0.));
#173184=CARTESIAN_POINT('Origin',(0.,0.,0.));
#173185=CARTESIAN_POINT('Origin',(0.,0.,12.));
#173186=CARTESIAN_POINT('Origin',(0.,0.,0.));
#173187=CARTESIAN_POINT('Origin',(0.,0.,0.));
#173188=CARTESIAN_POINT('Origin',(0.,0.,12.));
#173189=CARTESIAN_POINT('Origin',(0.,0.,0.));
#173190=CARTESIAN_POINT('Origin',(0.,0.,0.));
#173191=CARTESIAN_POINT('Origin',(0.,0.,12.));
#173192=CARTESIAN_POINT('Origin',(0.,0.,0.));
#173193=CARTESIAN_POINT('Origin',(0.,0.,0.));
#173194=CARTESIAN_POINT('Origin',(0.,0.,12.));
#173195=CARTESIAN_POINT('Origin',(0.,0.,0.));
#173196=CARTESIAN_POINT('Origin',(0.,0.,0.));
#173197=CARTESIAN_POINT('Origin',(0.,0.,12.));
#173198=CARTESIAN_POINT('Origin',(0.,0.,0.));
#173199=CARTESIAN_POINT('Origin',(0.,0.,0.));
#173200=CARTESIAN_POINT('Origin',(0.,0.,12.));
#173201=CARTESIAN_POINT('Origin',(0.,0.,0.));
#173202=CARTESIAN_POINT('Origin',(0.,0.,0.));
#173203=CARTESIAN_POINT('Origin',(0.,0.,12.));
#173204=CARTESIAN_POINT('Origin',(0.,0.,0.));
#173205=CARTESIAN_POINT('Origin',(0.,0.,0.));
#173206=CARTESIAN_POINT('Origin',(0.,0.,12.));
#173207=CARTESIAN_POINT('Origin',(0.,0.,0.));
#173208=CARTESIAN_POINT('Origin',(0.,0.,0.));
#173209=CARTESIAN_POINT('Origin',(0.,0.,12.));
#173210=CARTESIAN_POINT('Origin',(0.,0.,0.));
#173211=CARTESIAN_POINT('Origin',(0.,0.,0.));
#173212=CARTESIAN_POINT('Origin',(0.,0.,12.));
#173213=CARTESIAN_POINT('Origin',(0.,0.,0.));
#173214=CARTESIAN_POINT('Origin',(0.,0.,0.));
#173215=CARTESIAN_POINT('Origin',(0.,0.,12.));
#173216=CARTESIAN_POINT('Origin',(0.,0.,0.));
#173217=CARTESIAN_POINT('Origin',(0.,0.,0.));
#173218=CARTESIAN_POINT('Origin',(0.,0.,12.));
#173219=CARTESIAN_POINT('Origin',(0.,0.,0.));
#173220=CARTESIAN_POINT('Origin',(0.,0.,0.));
#173221=CARTESIAN_POINT('Origin',(0.,0.,12.));
#173222=CARTESIAN_POINT('Origin',(0.,0.,0.));
#173223=CARTESIAN_POINT('Origin',(0.,0.,0.));
#173224=CARTESIAN_POINT('Origin',(0.,0.,12.));
#173225=CARTESIAN_POINT('Origin',(0.,0.,0.));
#173226=CARTESIAN_POINT('Origin',(0.,0.,0.));
#173227=CARTESIAN_POINT('Origin',(0.,0.,12.));
#173228=CARTESIAN_POINT('Origin',(0.,0.,0.));
#173229=CARTESIAN_POINT('Origin',(0.,0.,0.));
#173230=CARTESIAN_POINT('Origin',(0.,0.,12.));
#173231=CARTESIAN_POINT('Origin',(0.,0.,0.));
#173232=CARTESIAN_POINT('Origin',(0.,0.,0.));
#173233=CARTESIAN_POINT('Origin',(0.,0.,12.));
#173234=CARTESIAN_POINT('Origin',(0.,0.,0.));
#173235=CARTESIAN_POINT('Origin',(0.,0.,0.));
#173236=CARTESIAN_POINT('Origin',(0.,0.,12.));
#173237=CARTESIAN_POINT('Origin',(0.,0.,0.));
#173238=CARTESIAN_POINT('Origin',(0.,0.,0.));
#173239=CARTESIAN_POINT('Origin',(0.,0.,12.));
#173240=CARTESIAN_POINT('Origin',(0.,0.,0.));
#173241=CARTESIAN_POINT('Origin',(0.,0.,0.));
#173242=CARTESIAN_POINT('Origin',(0.,0.,12.));
#173243=CARTESIAN_POINT('Origin',(0.,0.,0.));
#173244=CARTESIAN_POINT('Origin',(0.,0.,0.));
#173245=CARTESIAN_POINT('Origin',(0.,0.,12.));
#173246=CARTESIAN_POINT('Origin',(0.,0.,0.));
#173247=CARTESIAN_POINT('Origin',(0.,0.,0.));
#173248=CARTESIAN_POINT('Origin',(0.,0.,12.));
#173249=CARTESIAN_POINT('Origin',(0.,0.,0.));
#173250=CARTESIAN_POINT('Origin',(0.,0.,0.));
#173251=CARTESIAN_POINT('Origin',(0.,0.,12.));
#173252=CARTESIAN_POINT('Origin',(0.,0.,0.));
#173253=CARTESIAN_POINT('Origin',(0.,0.,0.));
#173254=CARTESIAN_POINT('Origin',(0.,0.,12.));
#173255=CARTESIAN_POINT('Origin',(0.,0.,0.));
#173256=CARTESIAN_POINT('Origin',(0.,0.,0.));
#173257=CARTESIAN_POINT('Origin',(0.,0.,12.));
#173258=CARTESIAN_POINT('Origin',(0.,0.,0.));
#173259=CARTESIAN_POINT('Origin',(0.,0.,0.));
#173260=CARTESIAN_POINT('Origin',(0.,0.,12.));
#173261=CARTESIAN_POINT('Origin',(0.,0.,0.));
#173262=CARTESIAN_POINT('Origin',(0.,0.,0.));
#173263=CARTESIAN_POINT('Origin',(0.,0.,12.));
#173264=CARTESIAN_POINT('Origin',(0.,0.,0.));
#173265=CARTESIAN_POINT('Origin',(0.,0.,0.));
#173266=CARTESIAN_POINT('Origin',(0.,0.,12.));
#173267=CARTESIAN_POINT('Origin',(0.,0.,0.));
#173268=CARTESIAN_POINT('Origin',(0.,0.,0.));
#173269=CARTESIAN_POINT('Origin',(0.,0.,12.));
#173270=CARTESIAN_POINT('Origin',(0.,0.,0.));
#173271=CARTESIAN_POINT('Origin',(0.,0.,0.));
#173272=CARTESIAN_POINT('Origin',(0.,0.,12.));
#173273=CARTESIAN_POINT('Origin',(0.,0.,0.));
#173274=CARTESIAN_POINT('Origin',(0.,0.,0.));
#173275=CARTESIAN_POINT('Origin',(0.,0.,12.));
#173276=CARTESIAN_POINT('Origin',(0.,0.,0.));
#173277=CARTESIAN_POINT('',(69.9947925310006,0.853825826608988,12.));
#173278=CARTESIAN_POINT('Origin',(0.,0.,12.));
#173279=CARTESIAN_POINT('',(69.9947925310006,0.853825826608988,0.));
#173280=CARTESIAN_POINT('',(69.9947925310006,0.853825826608988,0.));
#173281=CARTESIAN_POINT('Origin',(0.,0.,0.));
#173282=CARTESIAN_POINT('Ctrl Pts',(74.4416140848738,2.94891377268297,0.));
#173283=CARTESIAN_POINT('Ctrl Pts',(74.4416140848738,2.94891377268297,4.));
#173284=CARTESIAN_POINT('Ctrl Pts',(74.4416140848738,2.94891377268294,8.));
#173285=CARTESIAN_POINT('Ctrl Pts',(74.4416140848738,2.94891377268294,12.));
#173286=CARTESIAN_POINT('Ctrl Pts',(74.4459635334396,2.83911742169665,0.));
#173287=CARTESIAN_POINT('Ctrl Pts',(74.4459635334396,2.83911742169665,4.));
#173288=CARTESIAN_POINT('Ctrl Pts',(74.4459635334396,2.8391174216966,8.));
#173289=CARTESIAN_POINT('Ctrl Pts',(74.4459635334396,2.8391174216966,12.));
#173290=CARTESIAN_POINT('Ctrl Pts',(74.3877786926472,2.64498412359347,-7.30788408216183E-17));
#173291=CARTESIAN_POINT('Ctrl Pts',(74.3877786926472,2.64498412359347,4.00000000000001));
#173292=CARTESIAN_POINT('Ctrl Pts',(74.3877786926472,2.64498412359339,8.00000000000001));
#173293=CARTESIAN_POINT('Ctrl Pts',(74.3877786926472,2.64498412359339,12.));
#173294=CARTESIAN_POINT('Ctrl Pts',(74.2364344282701,2.51668625693798,-2.46611180232484E-16));
#173295=CARTESIAN_POINT('Ctrl Pts',(74.2364344282701,2.51668625693798,3.99999999999999));
#173296=CARTESIAN_POINT('Ctrl Pts',(74.2364344282701,2.51668625693788,8.));
#173297=CARTESIAN_POINT('Ctrl Pts',(74.2364344282701,2.51668625693788,12.));
#173298=CARTESIAN_POINT('Ctrl Pts',(74.1624659714555,2.48034921843216,-3.30265160469911E-16));
#173299=CARTESIAN_POINT('Ctrl Pts',(74.1624659714555,2.48034921843216,4.));
#173300=CARTESIAN_POINT('Ctrl Pts',(74.1624659714554,2.48034921843206,8.));
#173301=CARTESIAN_POINT('Ctrl Pts',(74.1624659714554,2.48034921843206,12.));
#173302=CARTESIAN_POINT('',(74.4416140848738,2.94891377268297,0.));
#173303=CARTESIAN_POINT('',(74.1624659714554,2.48034921843225,0.));
#173304=CARTESIAN_POINT('Ctrl Pts',(74.4416140848738,2.94891377268297,6.36152171223239E-17));
#173305=CARTESIAN_POINT('Ctrl Pts',(74.4459635334396,2.83911742169665,6.36152171223239E-17));
#173306=CARTESIAN_POINT('Ctrl Pts',(74.4127150529868,2.72818410849483,2.18558795099707E-17));
#173307=CARTESIAN_POINT('Ctrl Pts',(74.3490471689145,2.63874807903103,-5.27046004988717E-17));
#173308=CARTESIAN_POINT('Ctrl Pts',(74.3012962558603,2.57167105693319,-1.08624960505504E-16));
#173309=CARTESIAN_POINT('Ctrl Pts',(74.2364344282701,2.51668625693798,-1.82995963110161E-16));
#173310=CARTESIAN_POINT('Ctrl Pts',(74.1624659714555,2.48034921843216,-2.66649943347587E-16));
#173311=CARTESIAN_POINT('',(74.1624659714554,2.48034921843222,12.));
#173312=CARTESIAN_POINT('Ctrl Pts',(74.1624659714555,2.48034921843216,-3.30265160469911E-16));
#173313=CARTESIAN_POINT('Ctrl Pts',(74.1624659714555,2.48034921843216,4.));
#173314=CARTESIAN_POINT('Ctrl Pts',(74.1624659714554,2.48034921843206,8.));
#173315=CARTESIAN_POINT('Ctrl Pts',(74.1624659714554,2.48034921843206,12.));
#173316=CARTESIAN_POINT('',(74.4416140848738,2.94891377268294,12.));
#173317=CARTESIAN_POINT('Ctrl Pts',(74.1624659714554,2.48034921843206,12.));
#173318=CARTESIAN_POINT('Ctrl Pts',(74.2364344282701,2.51668625693788,12.));
#173319=CARTESIAN_POINT('Ctrl Pts',(74.3012962558603,2.5716710569331,12.));
#173320=CARTESIAN_POINT('Ctrl Pts',(74.3490471689145,2.63874807903096,12.));
#173321=CARTESIAN_POINT('Ctrl Pts',(74.4127150529868,2.72818410849477,12.));
#173322=CARTESIAN_POINT('Ctrl Pts',(74.4459635334396,2.8391174216966,12.));
#173323=CARTESIAN_POINT('Ctrl Pts',(74.4416140848738,2.94891377268294,12.));
#173324=CARTESIAN_POINT('Ctrl Pts',(74.4416140848738,2.94891377268294,12.));
#173325=CARTESIAN_POINT('Ctrl Pts',(74.4416140848738,2.94891377268294,8.));
#173326=CARTESIAN_POINT('Ctrl Pts',(74.4416140848738,2.94891377268297,4.));
#173327=CARTESIAN_POINT('Ctrl Pts',(74.4416140848738,2.94891377268297,0.));
#173328=CARTESIAN_POINT('Ctrl Pts',(69.9947925310006,0.853825826608988,
0.));
#173329=CARTESIAN_POINT('Ctrl Pts',(69.9947925310006,0.853825826608988,
12.));
#173330=CARTESIAN_POINT('Ctrl Pts',(69.9985337959407,0.854867673848601,
0.));
#173331=CARTESIAN_POINT('Ctrl Pts',(69.9985337959407,0.854867673848601,
12.));
#173332=CARTESIAN_POINT('Ctrl Pts',(70.0060209754087,0.85695487025921,0.));
#173333=CARTESIAN_POINT('Ctrl Pts',(70.0060209754087,0.85695487025921,12.));
#173334=CARTESIAN_POINT('Ctrl Pts',(70.0172656933806,0.86009617066874,0.));
#173335=CARTESIAN_POINT('Ctrl Pts',(70.0172656933806,0.86009617066874,12.));
#173336=CARTESIAN_POINT('Ctrl Pts',(70.0322865492925,0.86430558366155,0.));
#173337=CARTESIAN_POINT('Ctrl Pts',(70.0322865492925,0.86430558366155,12.));
#173338=CARTESIAN_POINT('Ctrl Pts',(70.051109108301,0.869602377871129,0.));
#173339=CARTESIAN_POINT('Ctrl Pts',(70.051109108301,0.869602377871129,12.));
#173340=CARTESIAN_POINT('Ctrl Pts',(70.0699781183935,0.874934213255844,
0.));
#173341=CARTESIAN_POINT('Ctrl Pts',(70.0699781183935,0.874934213255844,
12.));
#173342=CARTESIAN_POINT('Ctrl Pts',(70.0888934967855,0.880301109660733,
0.));
#173343=CARTESIAN_POINT('Ctrl Pts',(70.0888934967855,0.880301109660733,
12.));
#173344=CARTESIAN_POINT('Ctrl Pts',(70.1078550938958,0.88570309480254,0.));
#173345=CARTESIAN_POINT('Ctrl Pts',(70.1078550938958,0.88570309480254,12.));
#173346=CARTESIAN_POINT('Ctrl Pts',(70.1268626950175,0.891140203464248,
0.));
#173347=CARTESIAN_POINT('Ctrl Pts',(70.1268626950175,0.891140203464248,
12.));
#173348=CARTESIAN_POINT('Ctrl Pts',(70.1459160490446,0.896612474371848,
0.));
#173349=CARTESIAN_POINT('Ctrl Pts',(70.1459160490446,0.896612474371848,
12.));
#173350=CARTESIAN_POINT('Ctrl Pts',(70.1650148905109,0.902119947629775,
0.));
#173351=CARTESIAN_POINT('Ctrl Pts',(70.1650148905109,0.902119947629775,
12.));
#173352=CARTESIAN_POINT('Ctrl Pts',(70.1841589635574,0.907662662015791,
0.));
#173353=CARTESIAN_POINT('Ctrl Pts',(70.1841589635574,0.907662662015791,
12.));
#173354=CARTESIAN_POINT('Ctrl Pts',(70.2033480471676,0.913240652090985,
0.));
#173355=CARTESIAN_POINT('Ctrl Pts',(70.2033480471676,0.913240652090985,
12.));
#173356=CARTESIAN_POINT('Ctrl Pts',(70.2225819470248,0.918853949157122,
0.));
#173357=CARTESIAN_POINT('Ctrl Pts',(70.2225819470248,0.918853949157122,
12.));
#173358=CARTESIAN_POINT('Ctrl Pts',(70.2418604835836,0.924502582639461,
0.));
#173359=CARTESIAN_POINT('Ctrl Pts',(70.2418604835836,0.924502582639461,
12.));
#173360=CARTESIAN_POINT('Ctrl Pts',(70.2611834821723,0.930186581235552,
0.));
#173361=CARTESIAN_POINT('Ctrl Pts',(70.2611834821723,0.930186581235552,
12.));
#173362=CARTESIAN_POINT('Ctrl Pts',(70.2805507606872,0.935905974336485,
0.));
#173363=CARTESIAN_POINT('Ctrl Pts',(70.2805507606872,0.935905974336485,
12.));
#173364=CARTESIAN_POINT('Ctrl Pts',(70.299962123399,0.941660792742984,0.));
#173365=CARTESIAN_POINT('Ctrl Pts',(70.299962123399,0.941660792742984,12.));
#173366=CARTESIAN_POINT('Ctrl Pts',(70.3194173673674,0.947451067929609,
0.));
#173367=CARTESIAN_POINT('Ctrl Pts',(70.3194173673674,0.947451067929609,
12.));
#173368=CARTESIAN_POINT('Ctrl Pts',(70.338916286458,0.953276831581247,0.));
#173369=CARTESIAN_POINT('Ctrl Pts',(70.338916286458,0.953276831581247,12.));
#173370=CARTESIAN_POINT('Ctrl Pts',(70.3584586759536,0.959138115058838,
0.));
#173371=CARTESIAN_POINT('Ctrl Pts',(70.3584586759536,0.959138115058838,
12.));
#173372=CARTESIAN_POINT('Ctrl Pts',(70.3780443377956,0.965034948786454,
0.));
#173373=CARTESIAN_POINT('Ctrl Pts',(70.3780443377956,0.965034948786454,
12.));
#173374=CARTESIAN_POINT('Ctrl Pts',(70.3976730803613,0.970967362281179,
0.));
#173375=CARTESIAN_POINT('Ctrl Pts',(70.3976730803613,0.970967362281179,
12.));
#173376=CARTESIAN_POINT('Ctrl Pts',(70.417344715957,0.976935384450047,0.));
#173377=CARTESIAN_POINT('Ctrl Pts',(70.417344715957,0.976935384450047,12.));
#173378=CARTESIAN_POINT('Ctrl Pts',(70.4370590590842,0.982939043792161,
0.));
#173379=CARTESIAN_POINT('Ctrl Pts',(70.4370590590842,0.982939043792161,
12.));
#173380=CARTESIAN_POINT('Ctrl Pts',(70.4568159243163,0.988978368643654,
0.));
#173381=CARTESIAN_POINT('Ctrl Pts',(70.4568159243163,0.988978368643654,
12.));
#173382=CARTESIAN_POINT('Ctrl Pts',(70.4766151245212,0.99505338737976,0.));
#173383=CARTESIAN_POINT('Ctrl Pts',(70.4766151245212,0.99505338737976,12.));
#173384=CARTESIAN_POINT('Ctrl Pts',(70.4964564717953,1.00116412831443,0.));
#173385=CARTESIAN_POINT('Ctrl Pts',(70.4964564717953,1.00116412831443,12.));
#173386=CARTESIAN_POINT('Ctrl Pts',(70.5163397782713,1.00731061960969,0.));
#173387=CARTESIAN_POINT('Ctrl Pts',(70.5163397782713,1.00731061960969,12.));
#173388=CARTESIAN_POINT('Ctrl Pts',(70.5362648569061,1.01349288918538,0.));
#173389=CARTESIAN_POINT('Ctrl Pts',(70.5362648569061,1.01349288918538,12.));
#173390=CARTESIAN_POINT('Ctrl Pts',(70.556231522419,1.01971096460597,0.));
#173391=CARTESIAN_POINT('Ctrl Pts',(70.556231522419,1.01971096460597,12.));
#173392=CARTESIAN_POINT('Ctrl Pts',(70.5762395916377,1.02596487304049,0.));
#173393=CARTESIAN_POINT('Ctrl Pts',(70.5762395916377,1.02596487304049,12.));
#173394=CARTESIAN_POINT('Ctrl Pts',(70.5962888829934,1.03225464132871,0.));
#173395=CARTESIAN_POINT('Ctrl Pts',(70.5962888829934,1.03225464132871,12.));
#173396=CARTESIAN_POINT('Ctrl Pts',(70.6163792162073,1.03858029601904,0.));
#173397=CARTESIAN_POINT('Ctrl Pts',(70.6163792162073,1.03858029601904,12.));
#173398=CARTESIAN_POINT('Ctrl Pts',(70.6365104119252,1.04494186341157,0.));
#173399=CARTESIAN_POINT('Ctrl Pts',(70.6365104119252,1.04494186341157,12.));
#173400=CARTESIAN_POINT('Ctrl Pts',(70.6566822912991,1.05133936960072,0.));
#173401=CARTESIAN_POINT('Ctrl Pts',(70.6566822912991,1.05133936960072,12.));
#173402=CARTESIAN_POINT('Ctrl Pts',(70.676894676009,1.05777284047731,0.));
#173403=CARTESIAN_POINT('Ctrl Pts',(70.676894676009,1.05777284047731,12.));
#173404=CARTESIAN_POINT('Ctrl Pts',(70.6971473884459,1.06424230171281,0.));
#173405=CARTESIAN_POINT('Ctrl Pts',(70.6971473884459,1.06424230171281,12.));
#173406=CARTESIAN_POINT('Ctrl Pts',(70.7174402518378,1.07074777874596,0.));
#173407=CARTESIAN_POINT('Ctrl Pts',(70.7174402518378,1.07074777874596,12.));
#173408=CARTESIAN_POINT('Ctrl Pts',(70.7377730903953,1.07728929676409,0.));
#173409=CARTESIAN_POINT('Ctrl Pts',(70.7377730903953,1.07728929676409,12.));
#173410=CARTESIAN_POINT('Ctrl Pts',(70.7581457294447,1.08386688068343,0.));
#173411=CARTESIAN_POINT('Ctrl Pts',(70.7581457294447,1.08386688068343,12.));
#173412=CARTESIAN_POINT('Ctrl Pts',(70.7785579953583,1.09048055516427,0.));
#173413=CARTESIAN_POINT('Ctrl Pts',(70.7785579953583,1.09048055516427,12.));
#173414=CARTESIAN_POINT('Ctrl Pts',(70.799009715484,1.09713034462266,0.));
#173415=CARTESIAN_POINT('Ctrl Pts',(70.799009715484,1.09713034462266,12.));
#173416=CARTESIAN_POINT('Ctrl Pts',(70.8195007180745,1.10381627323947,0.));
#173417=CARTESIAN_POINT('Ctrl Pts',(70.8195007180745,1.10381627323947,12.));
#173418=CARTESIAN_POINT('Ctrl Pts',(70.8400308322037,1.1105383649664,0.));
#173419=CARTESIAN_POINT('Ctrl Pts',(70.8400308322037,1.1105383649664,12.));
#173420=CARTESIAN_POINT('Ctrl Pts',(70.8605998877149,1.11729664352993,0.));
#173421=CARTESIAN_POINT('Ctrl Pts',(70.8605998877149,1.11729664352993,12.));
#173422=CARTESIAN_POINT('Ctrl Pts',(70.8812077152586,1.12409113243514,0.));
#173423=CARTESIAN_POINT('Ctrl Pts',(70.8812077152586,1.12409113243514,12.));
#173424=CARTESIAN_POINT('Ctrl Pts',(70.9018541463089,1.13092185496565,0.));
#173425=CARTESIAN_POINT('Ctrl Pts',(70.9018541463089,1.13092185496565,12.));
#173426=CARTESIAN_POINT('Ctrl Pts',(70.9225390131826,1.13778883418214,0.));
#173427=CARTESIAN_POINT('Ctrl Pts',(70.9225390131826,1.13778883418214,12.));
#173428=CARTESIAN_POINT('Ctrl Pts',(70.9432621490566,1.14469209291489,0.));
#173429=CARTESIAN_POINT('Ctrl Pts',(70.9432621490566,1.14469209291489,12.));
#173430=CARTESIAN_POINT('Ctrl Pts',(70.9640233879659,1.15163165376525,0.));
#173431=CARTESIAN_POINT('Ctrl Pts',(70.9640233879659,1.15163165376525,12.));
#173432=CARTESIAN_POINT('Ctrl Pts',(70.9848225647871,1.15860753911486,0.));
#173433=CARTESIAN_POINT('Ctrl Pts',(70.9848225647871,1.15860753911486,12.));
#173434=CARTESIAN_POINT('Ctrl Pts',(71.0056595152204,1.16561977112881,0.));
#173435=CARTESIAN_POINT('Ctrl Pts',(71.0056595152204,1.16561977112881,12.));
#173436=CARTESIAN_POINT('Ctrl Pts',(71.0265340757699,1.17266837175778,0.));
#173437=CARTESIAN_POINT('Ctrl Pts',(71.0265340757699,1.17266837175778,12.));
#173438=CARTESIAN_POINT('Ctrl Pts',(71.0474460837159,1.17975336273505,0.));
#173439=CARTESIAN_POINT('Ctrl Pts',(71.0474460837159,1.17975336273505,12.));
#173440=CARTESIAN_POINT('Ctrl Pts',(71.0683953771149,1.18687476558133,0.));
#173441=CARTESIAN_POINT('Ctrl Pts',(71.0683953771149,1.18687476558133,12.));
#173442=CARTESIAN_POINT('Ctrl Pts',(71.089381794801,1.19403260161003,0.));
#173443=CARTESIAN_POINT('Ctrl Pts',(71.089381794801,1.19403260161003,12.));
#173444=CARTESIAN_POINT('Ctrl Pts',(71.1104051763839,1.20122689192837,0.));
#173445=CARTESIAN_POINT('Ctrl Pts',(71.1104051763839,1.20122689192837,12.));
#173446=CARTESIAN_POINT('Ctrl Pts',(71.1314653622442,1.20845765743648,0.));
#173447=CARTESIAN_POINT('Ctrl Pts',(71.1314653622442,1.20845765743648,12.));
#173448=CARTESIAN_POINT('Ctrl Pts',(71.1525621935267,1.21572491882263,0.));
#173449=CARTESIAN_POINT('Ctrl Pts',(71.1525621935267,1.21572491882263,12.));
#173450=CARTESIAN_POINT('Ctrl Pts',(71.1736955121362,1.22302869657018,0.));
#173451=CARTESIAN_POINT('Ctrl Pts',(71.1736955121362,1.22302869657018,12.));
#173452=CARTESIAN_POINT('Ctrl Pts',(71.194865160732,1.2303690109624,0.));
#173453=CARTESIAN_POINT('Ctrl Pts',(71.194865160732,1.2303690109624,12.));
#173454=CARTESIAN_POINT('Ctrl Pts',(71.2160709827191,1.23774588208428,0.));
#173455=CARTESIAN_POINT('Ctrl Pts',(71.2160709827191,1.23774588208428,12.));
#173456=CARTESIAN_POINT('Ctrl Pts',(71.2373128222352,1.24515932982113,0.));
#173457=CARTESIAN_POINT('Ctrl Pts',(71.2373128222352,1.24515932982113,12.));
#173458=CARTESIAN_POINT('Ctrl Pts',(71.2585905241406,1.25260937385569,0.));
#173459=CARTESIAN_POINT('Ctrl Pts',(71.2585905241406,1.25260937385569,12.));
#173460=CARTESIAN_POINT('Ctrl Pts',(71.2799039340175,1.26009603367571,0.));
#173461=CARTESIAN_POINT('Ctrl Pts',(71.2799039340175,1.26009603367571,12.));
#173462=CARTESIAN_POINT('Ctrl Pts',(71.3012528981661,1.26761932857725,0.));
#173463=CARTESIAN_POINT('Ctrl Pts',(71.3012528981661,1.26761932857725,12.));
#173464=CARTESIAN_POINT('Ctrl Pts',(71.3226372635996,1.27517927766609,0.));
#173465=CARTESIAN_POINT('Ctrl Pts',(71.3226372635996,1.27517927766609,12.));
#173466=CARTESIAN_POINT('Ctrl Pts',(71.3440568780347,1.28277589985472,0.));
#173467=CARTESIAN_POINT('Ctrl Pts',(71.3440568780347,1.28277589985472,12.));
#173468=CARTESIAN_POINT('Ctrl Pts',(71.3655115898827,1.2904092138606,0.));
#173469=CARTESIAN_POINT('Ctrl Pts',(71.3655115898827,1.2904092138606,12.));
#173470=CARTESIAN_POINT('Ctrl Pts',(71.3870012482499,1.29807923821414,0.));
#173471=CARTESIAN_POINT('Ctrl Pts',(71.3870012482499,1.29807923821414,12.));
#173472=CARTESIAN_POINT('Ctrl Pts',(71.4085257029322,1.3057859912614,0.));
#173473=CARTESIAN_POINT('Ctrl Pts',(71.4085257029322,1.3057859912614,12.));
#173474=CARTESIAN_POINT('Ctrl Pts',(71.4300848044087,1.31352949116538,0.));
#173475=CARTESIAN_POINT('Ctrl Pts',(71.4300848044087,1.31352949116538,12.));
#173476=CARTESIAN_POINT('Ctrl Pts',(71.4516784038317,1.32130975590226,0.));
#173477=CARTESIAN_POINT('Ctrl Pts',(71.4516784038317,1.32130975590226,12.));
#173478=CARTESIAN_POINT('Ctrl Pts',(71.4733063530187,1.32912680326124,0.));
#173479=CARTESIAN_POINT('Ctrl Pts',(71.4733063530187,1.32912680326124,12.));
#173480=CARTESIAN_POINT('Ctrl Pts',(71.4949685044522,1.3369806508522,0.));
#173481=CARTESIAN_POINT('Ctrl Pts',(71.4949685044522,1.3369806508522,12.));
#173482=CARTESIAN_POINT('Ctrl Pts',(71.516664711275,1.34487131610781,0.));
#173483=CARTESIAN_POINT('Ctrl Pts',(71.516664711275,1.34487131610781,12.));
#173484=CARTESIAN_POINT('Ctrl Pts',(71.5383948272845,1.35279881628455,0.));
#173485=CARTESIAN_POINT('Ctrl Pts',(71.5383948272845,1.35279881628455,12.));
#173486=CARTESIAN_POINT('Ctrl Pts',(71.5601587069217,1.36076316845817,0.));
#173487=CARTESIAN_POINT('Ctrl Pts',(71.5601587069217,1.36076316845817,12.));
#173488=CARTESIAN_POINT('Ctrl Pts',(71.5819562052663,1.36876438952466,0.));
#173489=CARTESIAN_POINT('Ctrl Pts',(71.5819562052663,1.36876438952466,12.));
#173490=CARTESIAN_POINT('Ctrl Pts',(71.6037871780385,1.3768024962078,0.));
#173491=CARTESIAN_POINT('Ctrl Pts',(71.6037871780385,1.3768024962078,12.));
#173492=CARTESIAN_POINT('Ctrl Pts',(71.625651481593,1.38487750506083,0.));
#173493=CARTESIAN_POINT('Ctrl Pts',(71.625651481593,1.38487750506083,12.));
#173494=CARTESIAN_POINT('Ctrl Pts',(71.6475489729134,1.39298943246723,0.));
#173495=CARTESIAN_POINT('Ctrl Pts',(71.6475489729134,1.39298943246723,12.));
#173496=CARTESIAN_POINT('Ctrl Pts',(71.6694795096001,1.40113829463577,0.));
#173497=CARTESIAN_POINT('Ctrl Pts',(71.6694795096001,1.40113829463577,12.));
#173498=CARTESIAN_POINT('Ctrl Pts',(71.6914429498663,1.40932410760249,0.));
#173499=CARTESIAN_POINT('Ctrl Pts',(71.6914429498663,1.40932410760249,12.));
#173500=CARTESIAN_POINT('Ctrl Pts',(71.7134391525389,1.41754688723773,0.));
#173501=CARTESIAN_POINT('Ctrl Pts',(71.7134391525389,1.41754688723773,12.));
#173502=CARTESIAN_POINT('Ctrl Pts',(71.7354679770528,1.4258066492477,0.));
#173503=CARTESIAN_POINT('Ctrl Pts',(71.7354679770528,1.4258066492477,12.));
#173504=CARTESIAN_POINT('Ctrl Pts',(71.7575292834469,1.43410340917496,0.));
#173505=CARTESIAN_POINT('Ctrl Pts',(71.7575292834469,1.43410340917496,12.));
#173506=CARTESIAN_POINT('Ctrl Pts',(71.7796229323526,1.44243718239316,0.));
#173507=CARTESIAN_POINT('Ctrl Pts',(71.7796229323526,1.44243718239316,12.));
#173508=CARTESIAN_POINT('Ctrl Pts',(71.8017487849895,1.45080798410966,0.));
#173509=CARTESIAN_POINT('Ctrl Pts',(71.8017487849895,1.45080798410966,12.));
#173510=CARTESIAN_POINT('Ctrl Pts',(71.8239067031683,1.45921582937232,0.));
#173511=CARTESIAN_POINT('Ctrl Pts',(71.8239067031683,1.45921582937232,12.));
#173512=CARTESIAN_POINT('Ctrl Pts',(71.8460965492838,1.46766073307089,0.));
#173513=CARTESIAN_POINT('Ctrl Pts',(71.8460965492838,1.46766073307089,12.));
#173514=CARTESIAN_POINT('Ctrl Pts',(71.8683181863116,1.47614270993729,0.));
#173515=CARTESIAN_POINT('Ctrl Pts',(71.8683181863116,1.47614270993729,12.));
#173516=CARTESIAN_POINT('Ctrl Pts',(71.8905714777961,1.4846617745402,0.));
#173517=CARTESIAN_POINT('Ctrl Pts',(71.8905714777961,1.4846617745402,12.));
#173518=CARTESIAN_POINT('Ctrl Pts',(71.912856287848,1.49321794128799,0.));
#173519=CARTESIAN_POINT('Ctrl Pts',(71.912856287848,1.49321794128799,12.));
#173520=CARTESIAN_POINT('Ctrl Pts',(71.9351724811443,1.50181122443535,0.));
#173521=CARTESIAN_POINT('Ctrl Pts',(71.9351724811443,1.50181122443535,12.));
#173522=CARTESIAN_POINT('Ctrl Pts',(71.9575199229241,1.51044163808454,0.));
#173523=CARTESIAN_POINT('Ctrl Pts',(71.9575199229241,1.51044163808454,12.));
#173524=CARTESIAN_POINT('Ctrl Pts',(71.979898478983,1.51910919618566,0.));
#173525=CARTESIAN_POINT('Ctrl Pts',(71.979898478983,1.51910919618566,12.));
#173526=CARTESIAN_POINT('Ctrl Pts',(72.0023080156647,1.52781391253102,0.));
#173527=CARTESIAN_POINT('Ctrl Pts',(72.0023080156647,1.52781391253102,12.));
#173528=CARTESIAN_POINT('Ctrl Pts',(72.0247483998578,1.53655580075813,0.));
#173529=CARTESIAN_POINT('Ctrl Pts',(72.0247483998578,1.53655580075813,12.));
#173530=CARTESIAN_POINT('Ctrl Pts',(72.0472194989963,1.54533487435627,0.));
#173531=CARTESIAN_POINT('Ctrl Pts',(72.0472194989963,1.54533487435627,12.));
#173532=CARTESIAN_POINT('Ctrl Pts',(72.0697211810545,1.55415114666774,0.));
#173533=CARTESIAN_POINT('Ctrl Pts',(72.0697211810545,1.55415114666774,12.));
#173534=CARTESIAN_POINT('Ctrl Pts',(72.0922533145433,1.56300463088809,0.));
#173535=CARTESIAN_POINT('Ctrl Pts',(72.0922533145433,1.56300463088809,12.));
#173536=CARTESIAN_POINT('Ctrl Pts',(72.1148157684995,1.57189534006041,0.));
#173537=CARTESIAN_POINT('Ctrl Pts',(72.1148157684995,1.57189534006041,12.));
#173538=CARTESIAN_POINT('Ctrl Pts',(72.1374084124839,1.58082328707804,0.));
#173539=CARTESIAN_POINT('Ctrl Pts',(72.1374084124839,1.58082328707804,12.));
#173540=CARTESIAN_POINT('Ctrl Pts',(72.1600311165821,1.58978848469124,0.));
#173541=CARTESIAN_POINT('Ctrl Pts',(72.1600311165821,1.58978848469124,12.));
#173542=CARTESIAN_POINT('Ctrl Pts',(72.1826837514001,1.59879094550848,0.));
#173543=CARTESIAN_POINT('Ctrl Pts',(72.1826837514001,1.59879094550848,12.));
#173544=CARTESIAN_POINT('Ctrl Pts',(72.2053661880608,1.60783068199664,0.));
#173545=CARTESIAN_POINT('Ctrl Pts',(72.2053661880608,1.60783068199664,12.));
#173546=CARTESIAN_POINT('Ctrl Pts',(72.2280782981937,1.61690770647541,0.));
#173547=CARTESIAN_POINT('Ctrl Pts',(72.2280782981937,1.61690770647541,12.));
#173548=CARTESIAN_POINT('Ctrl Pts',(72.2508199539323,1.62602203111931,0.));
#173549=CARTESIAN_POINT('Ctrl Pts',(72.2508199539323,1.62602203111931,12.));
#173550=CARTESIAN_POINT('Ctrl Pts',(72.2735910279149,1.63517366796464,0.));
#173551=CARTESIAN_POINT('Ctrl Pts',(72.2735910279149,1.63517366796464,12.));
#173552=CARTESIAN_POINT('Ctrl Pts',(72.2963913932813,1.64436262891079,0.));
#173553=CARTESIAN_POINT('Ctrl Pts',(72.2963913932813,1.64436262891079,12.));
#173554=CARTESIAN_POINT('Ctrl Pts',(72.319220923669,1.65358892572063,0.));
#173555=CARTESIAN_POINT('Ctrl Pts',(72.319220923669,1.65358892572063,12.));
#173556=CARTESIAN_POINT('Ctrl Pts',(72.3420794932047,1.66285257001497,0.));
#173557=CARTESIAN_POINT('Ctrl Pts',(72.3420794932047,1.66285257001497,12.));
#173558=CARTESIAN_POINT('Ctrl Pts',(72.3649669765004,1.67215357327366,0.));
#173559=CARTESIAN_POINT('Ctrl Pts',(72.3649669765004,1.67215357327366,12.));
#173560=CARTESIAN_POINT('Ctrl Pts',(72.387883248654,1.68149194684282,0.));
#173561=CARTESIAN_POINT('Ctrl Pts',(72.387883248654,1.68149194684282,12.));
#173562=CARTESIAN_POINT('Ctrl Pts',(72.4108281852467,1.69086770193638,0.));
#173563=CARTESIAN_POINT('Ctrl Pts',(72.4108281852467,1.69086770193638,12.));
#173564=CARTESIAN_POINT('Ctrl Pts',(72.4338016623391,1.70028084963648,0.));
#173565=CARTESIAN_POINT('Ctrl Pts',(72.4338016623391,1.70028084963648,12.));
#173566=CARTESIAN_POINT('Ctrl Pts',(72.456803556463,1.70973140088842,0.));
#173567=CARTESIAN_POINT('Ctrl Pts',(72.456803556463,1.70973140088842,12.));
#173568=CARTESIAN_POINT('Ctrl Pts',(72.479833744618,1.71921936650039,0.));
#173569=CARTESIAN_POINT('Ctrl Pts',(72.479833744618,1.71921936650039,12.));
#173570=CARTESIAN_POINT('Ctrl Pts',(72.5028921042721,1.72874475715104,0.));
#173571=CARTESIAN_POINT('Ctrl Pts',(72.5028921042721,1.72874475715104,12.));
#173572=CARTESIAN_POINT('Ctrl Pts',(72.5259785133595,1.73830758339125,0.));
#173573=CARTESIAN_POINT('Ctrl Pts',(72.5259785133595,1.73830758339125,12.));
#173574=CARTESIAN_POINT('Ctrl Pts',(72.5490928502769,1.74790785564474,0.));
#173575=CARTESIAN_POINT('Ctrl Pts',(72.5490928502769,1.74790785564474,12.));
#173576=CARTESIAN_POINT('Ctrl Pts',(72.5722349938774,1.75754558420345,0.));
#173577=CARTESIAN_POINT('Ctrl Pts',(72.5722349938774,1.75754558420345,12.));
#173578=CARTESIAN_POINT('Ctrl Pts',(72.5954048234638,1.76722077922575,0.));
#173579=CARTESIAN_POINT('Ctrl Pts',(72.5954048234638,1.76722077922575,12.));
#173580=CARTESIAN_POINT('Ctrl Pts',(72.6186022187907,1.77693345074427,0.));
#173581=CARTESIAN_POINT('Ctrl Pts',(72.6186022187907,1.77693345074427,12.));
#173582=CARTESIAN_POINT('Ctrl Pts',(72.6418270600619,1.78668360866812,0.));
#173583=CARTESIAN_POINT('Ctrl Pts',(72.6418270600619,1.78668360866812,12.));
#173584=CARTESIAN_POINT('Ctrl Pts',(72.6650792279274,1.79647126278359,0.));
#173585=CARTESIAN_POINT('Ctrl Pts',(72.6650792279274,1.79647126278359,12.));
#173586=CARTESIAN_POINT('Ctrl Pts',(72.6883586034769,1.80629642275051,0.));
#173587=CARTESIAN_POINT('Ctrl Pts',(72.6883586034769,1.80629642275051,12.));
#173588=CARTESIAN_POINT('Ctrl Pts',(72.7116650682344,1.81615909809871,0.));
#173589=CARTESIAN_POINT('Ctrl Pts',(72.7116650682344,1.81615909809871,12.));
#173590=CARTESIAN_POINT('Ctrl Pts',(72.7349985041592,1.82605929823565,0.));
#173591=CARTESIAN_POINT('Ctrl Pts',(72.7349985041592,1.82605929823565,12.));
#173592=CARTESIAN_POINT('Ctrl Pts',(72.7583587936447,1.83599703244925,0.));
#173593=CARTESIAN_POINT('Ctrl Pts',(72.7583587936447,1.83599703244925,12.));
#173594=CARTESIAN_POINT('Ctrl Pts',(72.7817458195155,1.84597230990858,0.));
#173595=CARTESIAN_POINT('Ctrl Pts',(72.7817458195155,1.84597230990858,12.));
#173596=CARTESIAN_POINT('Ctrl Pts',(72.8051594650222,1.85598513966114,0.));
#173597=CARTESIAN_POINT('Ctrl Pts',(72.8051594650222,1.85598513966114,12.));
#173598=CARTESIAN_POINT('Ctrl Pts',(72.8285996138359,1.86603553062772,0.));
#173599=CARTESIAN_POINT('Ctrl Pts',(72.8285996138359,1.86603553062772,12.));
#173600=CARTESIAN_POINT('Ctrl Pts',(72.8520661500477,1.87612349160945,0.));
#173601=CARTESIAN_POINT('Ctrl Pts',(72.8520661500477,1.87612349160945,12.));
#173602=CARTESIAN_POINT('Ctrl Pts',(72.875558958168,1.88624903129189,0.));
#173603=CARTESIAN_POINT('Ctrl Pts',(72.875558958168,1.88624903129189,12.));
#173604=CARTESIAN_POINT('Ctrl Pts',(72.8990779231226,1.89641215824583,0.));
#173605=CARTESIAN_POINT('Ctrl Pts',(72.8990779231226,1.89641215824583,12.));
#173606=CARTESIAN_POINT('Ctrl Pts',(72.9226229302478,1.90661288092587,0.));
#173607=CARTESIAN_POINT('Ctrl Pts',(72.9226229302478,1.90661288092587,12.));
#173608=CARTESIAN_POINT('Ctrl Pts',(72.9461938652811,1.91685120766437,0.));
#173609=CARTESIAN_POINT('Ctrl Pts',(72.9461938652811,1.91685120766437,12.));
#173610=CARTESIAN_POINT('Ctrl Pts',(72.9697906143636,1.92712714667661,0.));
#173611=CARTESIAN_POINT('Ctrl Pts',(72.9697906143636,1.92712714667661,12.));
#173612=CARTESIAN_POINT('Ctrl Pts',(72.9934130640415,1.93744070606566,0.));
#173613=CARTESIAN_POINT('Ctrl Pts',(72.9934130640415,1.93744070606566,12.));
#173614=CARTESIAN_POINT('Ctrl Pts',(73.0170611012661,1.94779189382303,0.));
#173615=CARTESIAN_POINT('Ctrl Pts',(73.0170611012661,1.94779189382303,12.));
#173616=CARTESIAN_POINT('Ctrl Pts',(73.040734613391,1.95818071782768,0.));
#173617=CARTESIAN_POINT('Ctrl Pts',(73.040734613391,1.95818071782768,12.));
#173618=CARTESIAN_POINT('Ctrl Pts',(73.0644334881673,1.96860718583933,0.));
#173619=CARTESIAN_POINT('Ctrl Pts',(73.0644334881673,1.96860718583933,12.));
#173620=CARTESIAN_POINT('Ctrl Pts',(73.0881576137407,1.97907130550158,0.));
#173621=CARTESIAN_POINT('Ctrl Pts',(73.0881576137407,1.97907130550158,12.));
#173622=CARTESIAN_POINT('Ctrl Pts',(73.1119068786475,1.98957308434919,0.));
#173623=CARTESIAN_POINT('Ctrl Pts',(73.1119068786475,1.98957308434919,12.));
#173624=CARTESIAN_POINT('Ctrl Pts',(73.1356811718091,2.00011252980982,0.));
#173625=CARTESIAN_POINT('Ctrl Pts',(73.1356811718091,2.00011252980982,12.));
#173626=CARTESIAN_POINT('Ctrl Pts',(73.1594803825252,2.01068964920468,0.));
#173627=CARTESIAN_POINT('Ctrl Pts',(73.1594803825252,2.01068964920468,12.));
#173628=CARTESIAN_POINT('Ctrl Pts',(73.183304400462,2.02130444974362,0.));
#173629=CARTESIAN_POINT('Ctrl Pts',(73.183304400462,2.02130444974362,12.));
#173630=CARTESIAN_POINT('Ctrl Pts',(73.2071531156504,2.03195693852455,0.));
#173631=CARTESIAN_POINT('Ctrl Pts',(73.2071531156504,2.03195693852455,12.));
#173632=CARTESIAN_POINT('Ctrl Pts',(73.2310264184976,2.04264712253929,0.));
#173633=CARTESIAN_POINT('Ctrl Pts',(73.2310264184976,2.04264712253929,12.));
#173634=CARTESIAN_POINT('Ctrl Pts',(73.2549241997953,2.05337500867403,0.));
#173635=CARTESIAN_POINT('Ctrl Pts',(73.2549241997953,2.05337500867403,12.));
#173636=CARTESIAN_POINT('Ctrl Pts',(73.2788463507246,2.06414060370835,0.));
#173637=CARTESIAN_POINT('Ctrl Pts',(73.2788463507246,2.06414060370835,12.));
#173638=CARTESIAN_POINT('Ctrl Pts',(73.3027927628626,2.07494391430941,0.));
#173639=CARTESIAN_POINT('Ctrl Pts',(73.3027927628626,2.07494391430941,12.));
#173640=CARTESIAN_POINT('Ctrl Pts',(73.3267633281807,2.08578494702744,0.));
#173641=CARTESIAN_POINT('Ctrl Pts',(73.3267633281807,2.08578494702744,12.));
#173642=CARTESIAN_POINT('Ctrl Pts',(73.3507579390239,2.09666370830717,0.));
#173643=CARTESIAN_POINT('Ctrl Pts',(73.3507579390239,2.09666370830717,12.));
#173644=CARTESIAN_POINT('Ctrl Pts',(73.3747764880893,2.1075802044939,0.));
#173645=CARTESIAN_POINT('Ctrl Pts',(73.3747764880893,2.1075802044939,12.));
#173646=CARTESIAN_POINT('Ctrl Pts',(73.3988188684021,2.11853444183762,0.));
#173647=CARTESIAN_POINT('Ctrl Pts',(73.3988188684021,2.11853444183762,12.));
#173648=CARTESIAN_POINT('Ctrl Pts',(73.4228849732925,2.12952642649368,0.));
#173649=CARTESIAN_POINT('Ctrl Pts',(73.4228849732925,2.12952642649368,12.));
#173650=CARTESIAN_POINT('Ctrl Pts',(73.4469746963637,2.14055616452058,0.));
#173651=CARTESIAN_POINT('Ctrl Pts',(73.4469746963637,2.14055616452058,12.));
#173652=CARTESIAN_POINT('Ctrl Pts',(73.4710879315382,2.15162366187907,0.));
#173653=CARTESIAN_POINT('Ctrl Pts',(73.4710879315382,2.15162366187907,12.));
#173654=CARTESIAN_POINT('Ctrl Pts',(73.4952245731054,2.1627289244292,0.));
#173655=CARTESIAN_POINT('Ctrl Pts',(73.4952245731054,2.1627289244292,12.));
#173656=CARTESIAN_POINT('Ctrl Pts',(73.5193845157708,2.17387195792306,0.));
#173657=CARTESIAN_POINT('Ctrl Pts',(73.5193845157708,2.17387195792306,12.));
#173658=CARTESIAN_POINT('Ctrl Pts',(73.5435676546929,2.18505276799754,0.));
#173659=CARTESIAN_POINT('Ctrl Pts',(73.5435676546929,2.18505276799754,12.));
#173660=CARTESIAN_POINT('Ctrl Pts',(73.5677738855452,2.19627136015679,0.));
#173661=CARTESIAN_POINT('Ctrl Pts',(73.5677738855452,2.19627136015679,12.));
#173662=CARTESIAN_POINT('Ctrl Pts',(73.5920031044595,2.20752773978349,0.));
#173663=CARTESIAN_POINT('Ctrl Pts',(73.5920031044595,2.20752773978349,12.));
#173664=CARTESIAN_POINT('Ctrl Pts',(73.6162552079038,2.21882191216519,0.));
#173665=CARTESIAN_POINT('Ctrl Pts',(73.6162552079038,2.21882191216519,12.));
#173666=CARTESIAN_POINT('Ctrl Pts',(73.6405300925712,2.23015388251288,0.));
#173667=CARTESIAN_POINT('Ctrl Pts',(73.6405300925712,2.23015388251288,12.));
#173668=CARTESIAN_POINT('Ctrl Pts',(73.6648276552767,2.24152365597698,0.));
#173669=CARTESIAN_POINT('Ctrl Pts',(73.6648276552767,2.24152365597698,12.));
#173670=CARTESIAN_POINT('Ctrl Pts',(73.6891477928129,2.25293123766425,0.));
#173671=CARTESIAN_POINT('Ctrl Pts',(73.6891477928129,2.25293123766425,12.));
#173672=CARTESIAN_POINT('Ctrl Pts',(73.7134904019389,2.26437663263667,0.));
#173673=CARTESIAN_POINT('Ctrl Pts',(73.7134904019389,2.26437663263667,12.));
#173674=CARTESIAN_POINT('Ctrl Pts',(73.7378553796807,2.27585984587199,0.));
#173675=CARTESIAN_POINT('Ctrl Pts',(73.7378553796807,2.27585984587199,12.));
#173676=CARTESIAN_POINT('Ctrl Pts',(73.762242623566,2.28738088222864,0.));
#173677=CARTESIAN_POINT('Ctrl Pts',(73.762242623566,2.28738088222864,12.));
#173678=CARTESIAN_POINT('Ctrl Pts',(73.786652031885,2.29893974640435,0.));
#173679=CARTESIAN_POINT('Ctrl Pts',(73.786652031885,2.29893974640435,12.));
#173680=CARTESIAN_POINT('Ctrl Pts',(73.8110835039327,2.31053644289417,0.));
#173681=CARTESIAN_POINT('Ctrl Pts',(73.8110835039327,2.31053644289417,12.));
#173682=CARTESIAN_POINT('Ctrl Pts',(73.8355369402706,2.32217097594198,0.));
#173683=CARTESIAN_POINT('Ctrl Pts',(73.8355369402706,2.32217097594198,12.));
#173684=CARTESIAN_POINT('Ctrl Pts',(73.8600122421468,2.33384334963958,0.));
#173685=CARTESIAN_POINT('Ctrl Pts',(73.8600122421468,2.33384334963958,12.));
#173686=CARTESIAN_POINT('Ctrl Pts',(73.8845093109274,2.34555356802121,0.));
#173687=CARTESIAN_POINT('Ctrl Pts',(73.8845093109274,2.34555356802121,12.));
#173688=CARTESIAN_POINT('Ctrl Pts',(73.9090280474712,2.35730163516316,0.));
#173689=CARTESIAN_POINT('Ctrl Pts',(73.9090280474712,2.35730163516316,12.));
#173690=CARTESIAN_POINT('Ctrl Pts',(73.9335683516404,2.36908755526004,0.));
#173691=CARTESIAN_POINT('Ctrl Pts',(73.9335683516404,2.36908755526004,12.));
#173692=CARTESIAN_POINT('Ctrl Pts',(73.958130121465,2.38091133274961,0.));
#173693=CARTESIAN_POINT('Ctrl Pts',(73.958130121465,2.38091133274961,12.));
#173694=CARTESIAN_POINT('Ctrl Pts',(73.9827132538206,2.39277297220757,0.));
#173695=CARTESIAN_POINT('Ctrl Pts',(73.9827132538206,2.39277297220757,12.));
#173696=CARTESIAN_POINT('Ctrl Pts',(74.0073176459344,2.40467247811537,0.));
#173697=CARTESIAN_POINT('Ctrl Pts',(74.0073176459344,2.40467247811537,12.));
#173698=CARTESIAN_POINT('Ctrl Pts',(74.0319431966989,2.41660985465252,0.));
#173699=CARTESIAN_POINT('Ctrl Pts',(74.0319431966989,2.41660985465252,12.));
#173700=CARTESIAN_POINT('Ctrl Pts',(74.0565898079218,2.42858510549779,0.));
#173701=CARTESIAN_POINT('Ctrl Pts',(74.0565898079218,2.42858510549779,12.));
#173702=CARTESIAN_POINT('Ctrl Pts',(74.0812573859411,2.44059823356676,0.));
#173703=CARTESIAN_POINT('Ctrl Pts',(74.0812573859411,2.44059823356676,12.));
#173704=CARTESIAN_POINT('Ctrl Pts',(74.1059458420067,2.45264924094776,0.));
#173705=CARTESIAN_POINT('Ctrl Pts',(74.1059458420067,2.45264924094776,12.));
#173706=CARTESIAN_POINT('Ctrl Pts',(74.1306550887071,2.4647381294796,0.));
#173707=CARTESIAN_POINT('Ctrl Pts',(74.1306550887071,2.4647381294796,12.));
#173708=CARTESIAN_POINT('Ctrl Pts',(74.155385037148,2.47686490120355,0.));
#173709=CARTESIAN_POINT('Ctrl Pts',(74.155385037148,2.47686490120355,12.));
#173710=CARTESIAN_POINT('Ctrl Pts',(74.1801355936907,2.48902955888385,0.));
#173711=CARTESIAN_POINT('Ctrl Pts',(74.1801355936907,2.48902955888385,12.));
#173712=CARTESIAN_POINT('Ctrl Pts',(74.2049066572031,2.50123210644136,0.));
#173713=CARTESIAN_POINT('Ctrl Pts',(74.2049066572031,2.50123210644136,12.));
#173714=CARTESIAN_POINT('Ctrl Pts',(74.229698115223,2.51347254956168,0.));
#173715=CARTESIAN_POINT('Ctrl Pts',(74.229698115223,2.51347254956168,12.));
#173716=CARTESIAN_POINT('Ctrl Pts',(74.2545098494824,2.52575089478304,0.));
#173717=CARTESIAN_POINT('Ctrl Pts',(74.2545098494824,2.52575089478304,12.));
#173718=CARTESIAN_POINT('Ctrl Pts',(74.2793417427308,2.53806714838287,0.));
#173719=CARTESIAN_POINT('Ctrl Pts',(74.2793417427308,2.53806714838287,12.));
#173720=CARTESIAN_POINT('Ctrl Pts',(74.3041936853468,2.55042131526781,0.));
#173721=CARTESIAN_POINT('Ctrl Pts',(74.3041936853468,2.55042131526781,12.));
#173722=CARTESIAN_POINT('Ctrl Pts',(74.329065581483,2.56281339800018,0.));
#173723=CARTESIAN_POINT('Ctrl Pts',(74.329065581483,2.56281339800018,12.));
#173724=CARTESIAN_POINT('Ctrl Pts',(74.3539573567672,2.5752433954139,0.));
#173725=CARTESIAN_POINT('Ctrl Pts',(74.3539573567672,2.5752433954139,12.));
#173726=CARTESIAN_POINT('Ctrl Pts',(74.3788689603363,2.58771130268176,0.));
#173727=CARTESIAN_POINT('Ctrl Pts',(74.3788689603363,2.58771130268176,12.));
#173728=CARTESIAN_POINT('Ctrl Pts',(74.4038003594771,2.60021711326978,0.));
#173729=CARTESIAN_POINT('Ctrl Pts',(74.4038003594771,2.60021711326978,12.));
#173730=CARTESIAN_POINT('Ctrl Pts',(74.4237613007988,2.61025207898403,0.));
#173731=CARTESIAN_POINT('Ctrl Pts',(74.4237613007988,2.61025207898403,12.));
#173732=CARTESIAN_POINT('Ctrl Pts',(74.4387409032207,2.61779535432113,0.));
#173733=CARTESIAN_POINT('Ctrl Pts',(74.4387409032207,2.61779535432113,12.));
#173734=CARTESIAN_POINT('Ctrl Pts',(74.4487312586464,2.62283178248203,0.));
#173735=CARTESIAN_POINT('Ctrl Pts',(74.4487312586464,2.62283178248203,12.));
#173736=CARTESIAN_POINT('Ctrl Pts',(74.4537274248118,2.62535189104656,0.));
#173737=CARTESIAN_POINT('Ctrl Pts',(74.4537274248118,2.62535189104656,12.));
#173738=CARTESIAN_POINT('Ctrl Pts',(69.9947925310006,0.853825826608988,
0.));
#173739=CARTESIAN_POINT('Ctrl Pts',(69.9985337959407,0.854867673848601,
0.));
#173740=CARTESIAN_POINT('Ctrl Pts',(70.0060209754087,0.85695487025921,0.));
#173741=CARTESIAN_POINT('Ctrl Pts',(70.0172656933806,0.86009617066874,0.));
#173742=CARTESIAN_POINT('Ctrl Pts',(70.0322865492925,0.86430558366155,0.));
#173743=CARTESIAN_POINT('Ctrl Pts',(70.051109108301,0.869602377871129,0.));
#173744=CARTESIAN_POINT('Ctrl Pts',(70.0699781183935,0.874934213255844,
0.));
#173745=CARTESIAN_POINT('Ctrl Pts',(70.0888934967855,0.880301109660733,
0.));
#173746=CARTESIAN_POINT('Ctrl Pts',(70.1078550938958,0.88570309480254,0.));
#173747=CARTESIAN_POINT('Ctrl Pts',(70.1268626950175,0.891140203464248,
0.));
#173748=CARTESIAN_POINT('Ctrl Pts',(70.1459160490446,0.896612474371848,
0.));
#173749=CARTESIAN_POINT('Ctrl Pts',(70.1650148905109,0.902119947629775,
0.));
#173750=CARTESIAN_POINT('Ctrl Pts',(70.1841589635574,0.907662662015791,
0.));
#173751=CARTESIAN_POINT('Ctrl Pts',(70.2033480471676,0.913240652090985,
0.));
#173752=CARTESIAN_POINT('Ctrl Pts',(70.2225819470248,0.918853949157122,
0.));
#173753=CARTESIAN_POINT('Ctrl Pts',(70.2418604835836,0.924502582639461,
0.));
#173754=CARTESIAN_POINT('Ctrl Pts',(70.2611834821723,0.930186581235552,
0.));
#173755=CARTESIAN_POINT('Ctrl Pts',(70.2805507606872,0.935905974336485,
0.));
#173756=CARTESIAN_POINT('Ctrl Pts',(70.299962123399,0.941660792742984,0.));
#173757=CARTESIAN_POINT('Ctrl Pts',(70.3194173673674,0.947451067929609,
0.));
#173758=CARTESIAN_POINT('Ctrl Pts',(70.338916286458,0.953276831581247,0.));
#173759=CARTESIAN_POINT('Ctrl Pts',(70.3584586759536,0.959138115058838,
0.));
#173760=CARTESIAN_POINT('Ctrl Pts',(70.3780443377956,0.965034948786454,
0.));
#173761=CARTESIAN_POINT('Ctrl Pts',(70.3976730803613,0.970967362281179,
0.));
#173762=CARTESIAN_POINT('Ctrl Pts',(70.417344715957,0.976935384450047,0.));
#173763=CARTESIAN_POINT('Ctrl Pts',(70.4370590590842,0.982939043792161,
0.));
#173764=CARTESIAN_POINT('Ctrl Pts',(70.4568159243163,0.988978368643654,
0.));
#173765=CARTESIAN_POINT('Ctrl Pts',(70.4766151245212,0.99505338737976,0.));
#173766=CARTESIAN_POINT('Ctrl Pts',(70.4964564717953,1.00116412831443,0.));
#173767=CARTESIAN_POINT('Ctrl Pts',(70.5163397782713,1.00731061960969,0.));
#173768=CARTESIAN_POINT('Ctrl Pts',(70.5362648569061,1.01349288918538,0.));
#173769=CARTESIAN_POINT('Ctrl Pts',(70.556231522419,1.01971096460597,0.));
#173770=CARTESIAN_POINT('Ctrl Pts',(70.5762395916377,1.02596487304049,0.));
#173771=CARTESIAN_POINT('Ctrl Pts',(70.5962888829934,1.03225464132871,0.));
#173772=CARTESIAN_POINT('Ctrl Pts',(70.6163792162073,1.03858029601904,0.));
#173773=CARTESIAN_POINT('Ctrl Pts',(70.6365104119252,1.04494186341157,0.));
#173774=CARTESIAN_POINT('Ctrl Pts',(70.6566822912991,1.05133936960072,0.));
#173775=CARTESIAN_POINT('Ctrl Pts',(70.676894676009,1.05777284047731,0.));
#173776=CARTESIAN_POINT('Ctrl Pts',(70.6971473884459,1.06424230171281,0.));
#173777=CARTESIAN_POINT('Ctrl Pts',(70.7174402518378,1.07074777874596,0.));
#173778=CARTESIAN_POINT('Ctrl Pts',(70.7377730903953,1.07728929676409,0.));
#173779=CARTESIAN_POINT('Ctrl Pts',(70.7581457294447,1.08386688068343,0.));
#173780=CARTESIAN_POINT('Ctrl Pts',(70.7785579953583,1.09048055516427,0.));
#173781=CARTESIAN_POINT('Ctrl Pts',(70.799009715484,1.09713034462266,0.));
#173782=CARTESIAN_POINT('Ctrl Pts',(70.8195007180745,1.10381627323947,0.));
#173783=CARTESIAN_POINT('Ctrl Pts',(70.8400308322037,1.1105383649664,0.));
#173784=CARTESIAN_POINT('Ctrl Pts',(70.8605998877149,1.11729664352993,0.));
#173785=CARTESIAN_POINT('Ctrl Pts',(70.8812077152586,1.12409113243514,0.));
#173786=CARTESIAN_POINT('Ctrl Pts',(70.9018541463089,1.13092185496565,0.));
#173787=CARTESIAN_POINT('Ctrl Pts',(70.9225390131826,1.13778883418214,0.));
#173788=CARTESIAN_POINT('Ctrl Pts',(70.9432621490566,1.14469209291489,0.));
#173789=CARTESIAN_POINT('Ctrl Pts',(70.9640233879659,1.15163165376525,0.));
#173790=CARTESIAN_POINT('Ctrl Pts',(70.9848225647871,1.15860753911486,0.));
#173791=CARTESIAN_POINT('Ctrl Pts',(71.0056595152204,1.16561977112881,0.));
#173792=CARTESIAN_POINT('Ctrl Pts',(71.0265340757699,1.17266837175778,0.));
#173793=CARTESIAN_POINT('Ctrl Pts',(71.0474460837159,1.17975336273505,0.));
#173794=CARTESIAN_POINT('Ctrl Pts',(71.0683953771149,1.18687476558133,0.));
#173795=CARTESIAN_POINT('Ctrl Pts',(71.089381794801,1.19403260161003,0.));
#173796=CARTESIAN_POINT('Ctrl Pts',(71.1104051763839,1.20122689192837,0.));
#173797=CARTESIAN_POINT('Ctrl Pts',(71.1314653622442,1.20845765743648,0.));
#173798=CARTESIAN_POINT('Ctrl Pts',(71.1525621935267,1.21572491882263,0.));
#173799=CARTESIAN_POINT('Ctrl Pts',(71.1736955121362,1.22302869657018,0.));
#173800=CARTESIAN_POINT('Ctrl Pts',(71.194865160732,1.2303690109624,0.));
#173801=CARTESIAN_POINT('Ctrl Pts',(71.2160709827191,1.23774588208428,0.));
#173802=CARTESIAN_POINT('Ctrl Pts',(71.2373128222352,1.24515932982113,0.));
#173803=CARTESIAN_POINT('Ctrl Pts',(71.2585905241406,1.25260937385569,0.));
#173804=CARTESIAN_POINT('Ctrl Pts',(71.2799039340175,1.26009603367571,0.));
#173805=CARTESIAN_POINT('Ctrl Pts',(71.3012528981661,1.26761932857725,0.));
#173806=CARTESIAN_POINT('Ctrl Pts',(71.3226372635996,1.27517927766609,0.));
#173807=CARTESIAN_POINT('Ctrl Pts',(71.3440568780347,1.28277589985472,0.));
#173808=CARTESIAN_POINT('Ctrl Pts',(71.3655115898827,1.2904092138606,0.));
#173809=CARTESIAN_POINT('Ctrl Pts',(71.3870012482499,1.29807923821414,0.));
#173810=CARTESIAN_POINT('Ctrl Pts',(71.4085257029322,1.3057859912614,0.));
#173811=CARTESIAN_POINT('Ctrl Pts',(71.4300848044087,1.31352949116538,0.));
#173812=CARTESIAN_POINT('Ctrl Pts',(71.4516784038317,1.32130975590226,0.));
#173813=CARTESIAN_POINT('Ctrl Pts',(71.4733063530187,1.32912680326124,0.));
#173814=CARTESIAN_POINT('Ctrl Pts',(71.4949685044522,1.3369806508522,0.));
#173815=CARTESIAN_POINT('Ctrl Pts',(71.516664711275,1.34487131610781,0.));
#173816=CARTESIAN_POINT('Ctrl Pts',(71.5383948272845,1.35279881628455,0.));
#173817=CARTESIAN_POINT('Ctrl Pts',(71.5601587069217,1.36076316845817,0.));
#173818=CARTESIAN_POINT('Ctrl Pts',(71.5819562052663,1.36876438952466,0.));
#173819=CARTESIAN_POINT('Ctrl Pts',(71.6037871780385,1.3768024962078,0.));
#173820=CARTESIAN_POINT('Ctrl Pts',(71.625651481593,1.38487750506083,0.));
#173821=CARTESIAN_POINT('Ctrl Pts',(71.6475489729134,1.39298943246723,0.));
#173822=CARTESIAN_POINT('Ctrl Pts',(71.6694795096001,1.40113829463577,0.));
#173823=CARTESIAN_POINT('Ctrl Pts',(71.6914429498663,1.40932410760249,0.));
#173824=CARTESIAN_POINT('Ctrl Pts',(71.7134391525389,1.41754688723773,0.));
#173825=CARTESIAN_POINT('Ctrl Pts',(71.7354679770528,1.4258066492477,0.));
#173826=CARTESIAN_POINT('Ctrl Pts',(71.7575292834469,1.43410340917496,0.));
#173827=CARTESIAN_POINT('Ctrl Pts',(71.7796229323526,1.44243718239316,0.));
#173828=CARTESIAN_POINT('Ctrl Pts',(71.8017487849895,1.45080798410966,0.));
#173829=CARTESIAN_POINT('Ctrl Pts',(71.8239067031683,1.45921582937232,0.));
#173830=CARTESIAN_POINT('Ctrl Pts',(71.8460965492838,1.46766073307089,0.));
#173831=CARTESIAN_POINT('Ctrl Pts',(71.8683181863116,1.47614270993729,0.));
#173832=CARTESIAN_POINT('Ctrl Pts',(71.8905714777961,1.4846617745402,0.));
#173833=CARTESIAN_POINT('Ctrl Pts',(71.912856287848,1.49321794128799,0.));
#173834=CARTESIAN_POINT('Ctrl Pts',(71.9351724811443,1.50181122443535,0.));
#173835=CARTESIAN_POINT('Ctrl Pts',(71.9575199229241,1.51044163808454,0.));
#173836=CARTESIAN_POINT('Ctrl Pts',(71.979898478983,1.51910919618566,0.));
#173837=CARTESIAN_POINT('Ctrl Pts',(72.0023080156647,1.52781391253102,0.));
#173838=CARTESIAN_POINT('Ctrl Pts',(72.0247483998578,1.53655580075813,0.));
#173839=CARTESIAN_POINT('Ctrl Pts',(72.0472194989963,1.54533487435627,0.));
#173840=CARTESIAN_POINT('Ctrl Pts',(72.0697211810545,1.55415114666774,0.));
#173841=CARTESIAN_POINT('Ctrl Pts',(72.0922533145433,1.56300463088809,0.));
#173842=CARTESIAN_POINT('Ctrl Pts',(72.1148157684995,1.57189534006041,0.));
#173843=CARTESIAN_POINT('Ctrl Pts',(72.1374084124839,1.58082328707804,0.));
#173844=CARTESIAN_POINT('Ctrl Pts',(72.1600311165821,1.58978848469124,0.));
#173845=CARTESIAN_POINT('Ctrl Pts',(72.1826837514001,1.59879094550848,0.));
#173846=CARTESIAN_POINT('Ctrl Pts',(72.2053661880608,1.60783068199664,0.));
#173847=CARTESIAN_POINT('Ctrl Pts',(72.2280782981937,1.61690770647541,0.));
#173848=CARTESIAN_POINT('Ctrl Pts',(72.2508199539323,1.62602203111931,0.));
#173849=CARTESIAN_POINT('Ctrl Pts',(72.2735910279149,1.63517366796464,0.));
#173850=CARTESIAN_POINT('Ctrl Pts',(72.2963913932813,1.64436262891079,0.));
#173851=CARTESIAN_POINT('Ctrl Pts',(72.319220923669,1.65358892572063,0.));
#173852=CARTESIAN_POINT('Ctrl Pts',(72.3420794932047,1.66285257001497,0.));
#173853=CARTESIAN_POINT('Ctrl Pts',(72.3649669765004,1.67215357327366,0.));
#173854=CARTESIAN_POINT('Ctrl Pts',(72.387883248654,1.68149194684282,0.));
#173855=CARTESIAN_POINT('Ctrl Pts',(72.4108281852467,1.69086770193638,0.));
#173856=CARTESIAN_POINT('Ctrl Pts',(72.4338016623391,1.70028084963648,0.));
#173857=CARTESIAN_POINT('Ctrl Pts',(72.456803556463,1.70973140088842,0.));
#173858=CARTESIAN_POINT('Ctrl Pts',(72.479833744618,1.71921936650039,0.));
#173859=CARTESIAN_POINT('Ctrl Pts',(72.5028921042721,1.72874475715104,0.));
#173860=CARTESIAN_POINT('Ctrl Pts',(72.5259785133595,1.73830758339125,0.));
#173861=CARTESIAN_POINT('Ctrl Pts',(72.5490928502769,1.74790785564474,0.));
#173862=CARTESIAN_POINT('Ctrl Pts',(72.5722349938774,1.75754558420345,0.));
#173863=CARTESIAN_POINT('Ctrl Pts',(72.5954048234638,1.76722077922575,0.));
#173864=CARTESIAN_POINT('Ctrl Pts',(72.6186022187907,1.77693345074427,0.));
#173865=CARTESIAN_POINT('Ctrl Pts',(72.6418270600619,1.78668360866812,0.));
#173866=CARTESIAN_POINT('Ctrl Pts',(72.6650792279274,1.79647126278359,0.));
#173867=CARTESIAN_POINT('Ctrl Pts',(72.6883586034769,1.80629642275051,0.));
#173868=CARTESIAN_POINT('Ctrl Pts',(72.7116650682344,1.81615909809871,0.));
#173869=CARTESIAN_POINT('Ctrl Pts',(72.7349985041592,1.82605929823565,0.));
#173870=CARTESIAN_POINT('Ctrl Pts',(72.7583587936447,1.83599703244925,0.));
#173871=CARTESIAN_POINT('Ctrl Pts',(72.7817458195155,1.84597230990858,0.));
#173872=CARTESIAN_POINT('Ctrl Pts',(72.8051594650222,1.85598513966114,0.));
#173873=CARTESIAN_POINT('Ctrl Pts',(72.8285996138359,1.86603553062772,0.));
#173874=CARTESIAN_POINT('Ctrl Pts',(72.8520661500477,1.87612349160945,0.));
#173875=CARTESIAN_POINT('Ctrl Pts',(72.875558958168,1.88624903129189,0.));
#173876=CARTESIAN_POINT('Ctrl Pts',(72.8990779231226,1.89641215824583,0.));
#173877=CARTESIAN_POINT('Ctrl Pts',(72.9226229302478,1.90661288092587,0.));
#173878=CARTESIAN_POINT('Ctrl Pts',(72.9461938652811,1.91685120766437,0.));
#173879=CARTESIAN_POINT('Ctrl Pts',(72.9697906143636,1.92712714667661,0.));
#173880=CARTESIAN_POINT('Ctrl Pts',(72.9934130640415,1.93744070606566,0.));
#173881=CARTESIAN_POINT('Ctrl Pts',(73.0170611012661,1.94779189382303,0.));
#173882=CARTESIAN_POINT('Ctrl Pts',(73.040734613391,1.95818071782768,0.));
#173883=CARTESIAN_POINT('Ctrl Pts',(73.0644334881673,1.96860718583933,0.));
#173884=CARTESIAN_POINT('Ctrl Pts',(73.0881576137407,1.97907130550158,0.));
#173885=CARTESIAN_POINT('Ctrl Pts',(73.1119068786475,1.98957308434919,0.));
#173886=CARTESIAN_POINT('Ctrl Pts',(73.1356811718091,2.00011252980982,0.));
#173887=CARTESIAN_POINT('Ctrl Pts',(73.1594803825252,2.01068964920468,0.));
#173888=CARTESIAN_POINT('Ctrl Pts',(73.183304400462,2.02130444974362,0.));
#173889=CARTESIAN_POINT('Ctrl Pts',(73.2071531156504,2.03195693852455,0.));
#173890=CARTESIAN_POINT('Ctrl Pts',(73.2310264184976,2.04264712253929,0.));
#173891=CARTESIAN_POINT('Ctrl Pts',(73.2549241997953,2.05337500867403,0.));
#173892=CARTESIAN_POINT('Ctrl Pts',(73.2788463507246,2.06414060370835,0.));
#173893=CARTESIAN_POINT('Ctrl Pts',(73.3027927628626,2.07494391430941,0.));
#173894=CARTESIAN_POINT('Ctrl Pts',(73.3267633281807,2.08578494702744,0.));
#173895=CARTESIAN_POINT('Ctrl Pts',(73.3507579390239,2.09666370830717,0.));
#173896=CARTESIAN_POINT('Ctrl Pts',(73.3747764880893,2.1075802044939,0.));
#173897=CARTESIAN_POINT('Ctrl Pts',(73.3988188684021,2.11853444183762,0.));
#173898=CARTESIAN_POINT('Ctrl Pts',(73.4228849732925,2.12952642649368,0.));
#173899=CARTESIAN_POINT('Ctrl Pts',(73.4469746963637,2.14055616452058,0.));
#173900=CARTESIAN_POINT('Ctrl Pts',(73.4710879315382,2.15162366187907,0.));
#173901=CARTESIAN_POINT('Ctrl Pts',(73.4952245731054,2.1627289244292,0.));
#173902=CARTESIAN_POINT('Ctrl Pts',(73.5193845157708,2.17387195792306,0.));
#173903=CARTESIAN_POINT('Ctrl Pts',(73.5435676546929,2.18505276799754,0.));
#173904=CARTESIAN_POINT('Ctrl Pts',(73.5677738855452,2.19627136015679,0.));
#173905=CARTESIAN_POINT('Ctrl Pts',(73.5920031044595,2.20752773978349,0.));
#173906=CARTESIAN_POINT('Ctrl Pts',(73.6162552079038,2.21882191216519,0.));
#173907=CARTESIAN_POINT('Ctrl Pts',(73.6405300925712,2.23015388251288,0.));
#173908=CARTESIAN_POINT('Ctrl Pts',(73.6648276552767,2.24152365597698,0.));
#173909=CARTESIAN_POINT('Ctrl Pts',(73.6891477928129,2.25293123766425,0.));
#173910=CARTESIAN_POINT('Ctrl Pts',(73.7134904019389,2.26437663263667,0.));
#173911=CARTESIAN_POINT('Ctrl Pts',(73.7378553796807,2.27585984587199,0.));
#173912=CARTESIAN_POINT('Ctrl Pts',(73.762242623566,2.28738088222864,0.));
#173913=CARTESIAN_POINT('Ctrl Pts',(73.786652031885,2.29893974640435,0.));
#173914=CARTESIAN_POINT('Ctrl Pts',(73.8110835039327,2.31053644289417,0.));
#173915=CARTESIAN_POINT('Ctrl Pts',(73.8355369402706,2.32217097594198,0.));
#173916=CARTESIAN_POINT('Ctrl Pts',(73.8600122421468,2.33384334963958,0.));
#173917=CARTESIAN_POINT('Ctrl Pts',(73.8845093109274,2.34555356802121,0.));
#173918=CARTESIAN_POINT('Ctrl Pts',(73.9090280474712,2.35730163516316,0.));
#173919=CARTESIAN_POINT('Ctrl Pts',(73.9335683516404,2.36908755526004,0.));
#173920=CARTESIAN_POINT('Ctrl Pts',(73.958130121465,2.38091133274961,0.));
#173921=CARTESIAN_POINT('Ctrl Pts',(73.9827132538206,2.39277297220757,0.));
#173922=CARTESIAN_POINT('Ctrl Pts',(74.0073176459344,2.40467247811537,0.));
#173923=CARTESIAN_POINT('Ctrl Pts',(74.0319431966989,2.41660985465252,0.));
#173924=CARTESIAN_POINT('Ctrl Pts',(74.0565898079218,2.42858510549779,0.));
#173925=CARTESIAN_POINT('Ctrl Pts',(74.0812573859411,2.44059823356676,0.));
#173926=CARTESIAN_POINT('Ctrl Pts',(74.1059458420067,2.45264924094776,0.));
#173927=CARTESIAN_POINT('Ctrl Pts',(74.1271264545189,2.46301176097118,0.));
#173928=CARTESIAN_POINT('Ctrl Pts',(74.143376394138,2.47097695564992,0.));
#173929=CARTESIAN_POINT('Ctrl Pts',(74.1546864735166,2.47652804724536,0.));
#173930=CARTESIAN_POINT('Ctrl Pts',(74.1610506466205,2.47965393945472,0.));
#173931=CARTESIAN_POINT('Ctrl Pts',(74.1624659714554,2.48034921843225,0.));
#173932=CARTESIAN_POINT('Ctrl Pts',(74.1624659714553,2.48034921843222,12.));
#173933=CARTESIAN_POINT('Ctrl Pts',(74.1610506466205,2.4796539394547,12.));
#173934=CARTESIAN_POINT('Ctrl Pts',(74.1546864735166,2.47652804724534,12.));
#173935=CARTESIAN_POINT('Ctrl Pts',(74.1433763941379,2.47097695564991,12.));
#173936=CARTESIAN_POINT('Ctrl Pts',(74.1271264545189,2.46301176097117,12.));
#173937=CARTESIAN_POINT('Ctrl Pts',(74.1059458420067,2.45264924094776,12.));
#173938=CARTESIAN_POINT('Ctrl Pts',(74.0812573859411,2.44059823356676,12.));
#173939=CARTESIAN_POINT('Ctrl Pts',(74.0565898079218,2.42858510549779,12.));
#173940=CARTESIAN_POINT('Ctrl Pts',(74.0319431966989,2.41660985465252,12.));
#173941=CARTESIAN_POINT('Ctrl Pts',(74.0073176459344,2.40467247811537,12.));
#173942=CARTESIAN_POINT('Ctrl Pts',(73.9827132538206,2.39277297220757,12.));
#173943=CARTESIAN_POINT('Ctrl Pts',(73.958130121465,2.38091133274961,12.));
#173944=CARTESIAN_POINT('Ctrl Pts',(73.9335683516404,2.36908755526004,12.));
#173945=CARTESIAN_POINT('Ctrl Pts',(73.9090280474712,2.35730163516316,12.));
#173946=CARTESIAN_POINT('Ctrl Pts',(73.8845093109274,2.34555356802121,12.));
#173947=CARTESIAN_POINT('Ctrl Pts',(73.8600122421468,2.33384334963958,12.));
#173948=CARTESIAN_POINT('Ctrl Pts',(73.8355369402706,2.32217097594198,12.));
#173949=CARTESIAN_POINT('Ctrl Pts',(73.8110835039327,2.31053644289417,12.));
#173950=CARTESIAN_POINT('Ctrl Pts',(73.786652031885,2.29893974640435,12.));
#173951=CARTESIAN_POINT('Ctrl Pts',(73.762242623566,2.28738088222864,12.));
#173952=CARTESIAN_POINT('Ctrl Pts',(73.7378553796807,2.27585984587199,12.));
#173953=CARTESIAN_POINT('Ctrl Pts',(73.7134904019389,2.26437663263667,12.));
#173954=CARTESIAN_POINT('Ctrl Pts',(73.6891477928129,2.25293123766425,12.));
#173955=CARTESIAN_POINT('Ctrl Pts',(73.6648276552767,2.24152365597698,12.));
#173956=CARTESIAN_POINT('Ctrl Pts',(73.6405300925712,2.23015388251288,12.));
#173957=CARTESIAN_POINT('Ctrl Pts',(73.6162552079038,2.21882191216519,12.));
#173958=CARTESIAN_POINT('Ctrl Pts',(73.5920031044595,2.20752773978349,12.));
#173959=CARTESIAN_POINT('Ctrl Pts',(73.5677738855452,2.19627136015679,12.));
#173960=CARTESIAN_POINT('Ctrl Pts',(73.5435676546929,2.18505276799754,12.));
#173961=CARTESIAN_POINT('Ctrl Pts',(73.5193845157708,2.17387195792306,12.));
#173962=CARTESIAN_POINT('Ctrl Pts',(73.4952245731054,2.1627289244292,12.));
#173963=CARTESIAN_POINT('Ctrl Pts',(73.4710879315382,2.15162366187907,12.));
#173964=CARTESIAN_POINT('Ctrl Pts',(73.4469746963637,2.14055616452058,12.));
#173965=CARTESIAN_POINT('Ctrl Pts',(73.4228849732925,2.12952642649368,12.));
#173966=CARTESIAN_POINT('Ctrl Pts',(73.3988188684021,2.11853444183762,12.));
#173967=CARTESIAN_POINT('Ctrl Pts',(73.3747764880893,2.1075802044939,12.));
#173968=CARTESIAN_POINT('Ctrl Pts',(73.3507579390239,2.09666370830717,12.));
#173969=CARTESIAN_POINT('Ctrl Pts',(73.3267633281807,2.08578494702744,12.));
#173970=CARTESIAN_POINT('Ctrl Pts',(73.3027927628626,2.07494391430941,12.));
#173971=CARTESIAN_POINT('Ctrl Pts',(73.2788463507246,2.06414060370835,12.));
#173972=CARTESIAN_POINT('Ctrl Pts',(73.2549241997953,2.05337500867403,12.));
#173973=CARTESIAN_POINT('Ctrl Pts',(73.2310264184976,2.04264712253929,12.));
#173974=CARTESIAN_POINT('Ctrl Pts',(73.2071531156504,2.03195693852455,12.));
#173975=CARTESIAN_POINT('Ctrl Pts',(73.183304400462,2.02130444974362,12.));
#173976=CARTESIAN_POINT('Ctrl Pts',(73.1594803825252,2.01068964920468,12.));
#173977=CARTESIAN_POINT('Ctrl Pts',(73.1356811718091,2.00011252980982,12.));
#173978=CARTESIAN_POINT('Ctrl Pts',(73.1119068786475,1.98957308434919,12.));
#173979=CARTESIAN_POINT('Ctrl Pts',(73.0881576137407,1.97907130550158,12.));
#173980=CARTESIAN_POINT('Ctrl Pts',(73.0644334881673,1.96860718583933,12.));
#173981=CARTESIAN_POINT('Ctrl Pts',(73.040734613391,1.95818071782768,12.));
#173982=CARTESIAN_POINT('Ctrl Pts',(73.0170611012661,1.94779189382303,12.));
#173983=CARTESIAN_POINT('Ctrl Pts',(72.9934130640415,1.93744070606566,12.));
#173984=CARTESIAN_POINT('Ctrl Pts',(72.9697906143636,1.92712714667661,12.));
#173985=CARTESIAN_POINT('Ctrl Pts',(72.9461938652811,1.91685120766437,12.));
#173986=CARTESIAN_POINT('Ctrl Pts',(72.9226229302478,1.90661288092587,12.));
#173987=CARTESIAN_POINT('Ctrl Pts',(72.8990779231226,1.89641215824583,12.));
#173988=CARTESIAN_POINT('Ctrl Pts',(72.875558958168,1.88624903129189,12.));
#173989=CARTESIAN_POINT('Ctrl Pts',(72.8520661500477,1.87612349160945,12.));
#173990=CARTESIAN_POINT('Ctrl Pts',(72.8285996138359,1.86603553062772,12.));
#173991=CARTESIAN_POINT('Ctrl Pts',(72.8051594650222,1.85598513966114,12.));
#173992=CARTESIAN_POINT('Ctrl Pts',(72.7817458195155,1.84597230990858,12.));
#173993=CARTESIAN_POINT('Ctrl Pts',(72.7583587936447,1.83599703244925,12.));
#173994=CARTESIAN_POINT('Ctrl Pts',(72.7349985041592,1.82605929823565,12.));
#173995=CARTESIAN_POINT('Ctrl Pts',(72.7116650682344,1.81615909809871,12.));
#173996=CARTESIAN_POINT('Ctrl Pts',(72.6883586034769,1.80629642275051,12.));
#173997=CARTESIAN_POINT('Ctrl Pts',(72.6650792279274,1.79647126278359,12.));
#173998=CARTESIAN_POINT('Ctrl Pts',(72.6418270600619,1.78668360866812,12.));
#173999=CARTESIAN_POINT('Ctrl Pts',(72.6186022187907,1.77693345074427,12.));
#174000=CARTESIAN_POINT('Ctrl Pts',(72.5954048234638,1.76722077922575,12.));
#174001=CARTESIAN_POINT('Ctrl Pts',(72.5722349938774,1.75754558420345,12.));
#174002=CARTESIAN_POINT('Ctrl Pts',(72.5490928502769,1.74790785564474,12.));
#174003=CARTESIAN_POINT('Ctrl Pts',(72.5259785133595,1.73830758339125,12.));
#174004=CARTESIAN_POINT('Ctrl Pts',(72.5028921042721,1.72874475715104,12.));
#174005=CARTESIAN_POINT('Ctrl Pts',(72.479833744618,1.71921936650039,12.));
#174006=CARTESIAN_POINT('Ctrl Pts',(72.456803556463,1.70973140088842,12.));
#174007=CARTESIAN_POINT('Ctrl Pts',(72.4338016623391,1.70028084963648,12.));
#174008=CARTESIAN_POINT('Ctrl Pts',(72.4108281852467,1.69086770193638,12.));
#174009=CARTESIAN_POINT('Ctrl Pts',(72.387883248654,1.68149194684282,12.));
#174010=CARTESIAN_POINT('Ctrl Pts',(72.3649669765004,1.67215357327366,12.));
#174011=CARTESIAN_POINT('Ctrl Pts',(72.3420794932047,1.66285257001497,12.));
#174012=CARTESIAN_POINT('Ctrl Pts',(72.319220923669,1.65358892572063,12.));
#174013=CARTESIAN_POINT('Ctrl Pts',(72.2963913932813,1.64436262891079,12.));
#174014=CARTESIAN_POINT('Ctrl Pts',(72.2735910279149,1.63517366796464,12.));
#174015=CARTESIAN_POINT('Ctrl Pts',(72.2508199539323,1.62602203111931,12.));
#174016=CARTESIAN_POINT('Ctrl Pts',(72.2280782981937,1.61690770647541,12.));
#174017=CARTESIAN_POINT('Ctrl Pts',(72.2053661880608,1.60783068199664,12.));
#174018=CARTESIAN_POINT('Ctrl Pts',(72.1826837514001,1.59879094550848,12.));
#174019=CARTESIAN_POINT('Ctrl Pts',(72.1600311165821,1.58978848469124,12.));
#174020=CARTESIAN_POINT('Ctrl Pts',(72.1374084124839,1.58082328707804,12.));
#174021=CARTESIAN_POINT('Ctrl Pts',(72.1148157684995,1.57189534006041,12.));
#174022=CARTESIAN_POINT('Ctrl Pts',(72.0922533145433,1.56300463088809,12.));
#174023=CARTESIAN_POINT('Ctrl Pts',(72.0697211810545,1.55415114666774,12.));
#174024=CARTESIAN_POINT('Ctrl Pts',(72.0472194989963,1.54533487435627,12.));
#174025=CARTESIAN_POINT('Ctrl Pts',(72.0247483998578,1.53655580075813,12.));
#174026=CARTESIAN_POINT('Ctrl Pts',(72.0023080156647,1.52781391253102,12.));
#174027=CARTESIAN_POINT('Ctrl Pts',(71.979898478983,1.51910919618566,12.));
#174028=CARTESIAN_POINT('Ctrl Pts',(71.9575199229241,1.51044163808454,12.));
#174029=CARTESIAN_POINT('Ctrl Pts',(71.9351724811443,1.50181122443535,12.));
#174030=CARTESIAN_POINT('Ctrl Pts',(71.912856287848,1.49321794128799,12.));
#174031=CARTESIAN_POINT('Ctrl Pts',(71.8905714777961,1.4846617745402,12.));
#174032=CARTESIAN_POINT('Ctrl Pts',(71.8683181863116,1.47614270993729,12.));
#174033=CARTESIAN_POINT('Ctrl Pts',(71.8460965492838,1.46766073307089,12.));
#174034=CARTESIAN_POINT('Ctrl Pts',(71.8239067031683,1.45921582937232,12.));
#174035=CARTESIAN_POINT('Ctrl Pts',(71.8017487849895,1.45080798410966,12.));
#174036=CARTESIAN_POINT('Ctrl Pts',(71.7796229323526,1.44243718239316,12.));
#174037=CARTESIAN_POINT('Ctrl Pts',(71.7575292834469,1.43410340917496,12.));
#174038=CARTESIAN_POINT('Ctrl Pts',(71.7354679770528,1.4258066492477,12.));
#174039=CARTESIAN_POINT('Ctrl Pts',(71.7134391525389,1.41754688723773,12.));
#174040=CARTESIAN_POINT('Ctrl Pts',(71.6914429498663,1.40932410760249,12.));
#174041=CARTESIAN_POINT('Ctrl Pts',(71.6694795096001,1.40113829463577,12.));
#174042=CARTESIAN_POINT('Ctrl Pts',(71.6475489729134,1.39298943246723,12.));
#174043=CARTESIAN_POINT('Ctrl Pts',(71.625651481593,1.38487750506083,12.));
#174044=CARTESIAN_POINT('Ctrl Pts',(71.6037871780385,1.3768024962078,12.));
#174045=CARTESIAN_POINT('Ctrl Pts',(71.5819562052663,1.36876438952466,12.));
#174046=CARTESIAN_POINT('Ctrl Pts',(71.5601587069217,1.36076316845817,12.));
#174047=CARTESIAN_POINT('Ctrl Pts',(71.5383948272845,1.35279881628455,12.));
#174048=CARTESIAN_POINT('Ctrl Pts',(71.516664711275,1.34487131610781,12.));
#174049=CARTESIAN_POINT('Ctrl Pts',(71.4949685044522,1.3369806508522,12.));
#174050=CARTESIAN_POINT('Ctrl Pts',(71.4733063530187,1.32912680326124,12.));
#174051=CARTESIAN_POINT('Ctrl Pts',(71.4516784038317,1.32130975590226,12.));
#174052=CARTESIAN_POINT('Ctrl Pts',(71.4300848044087,1.31352949116538,12.));
#174053=CARTESIAN_POINT('Ctrl Pts',(71.4085257029322,1.3057859912614,12.));
#174054=CARTESIAN_POINT('Ctrl Pts',(71.3870012482499,1.29807923821414,12.));
#174055=CARTESIAN_POINT('Ctrl Pts',(71.3655115898827,1.2904092138606,12.));
#174056=CARTESIAN_POINT('Ctrl Pts',(71.3440568780347,1.28277589985472,12.));
#174057=CARTESIAN_POINT('Ctrl Pts',(71.3226372635996,1.27517927766609,12.));
#174058=CARTESIAN_POINT('Ctrl Pts',(71.3012528981661,1.26761932857725,12.));
#174059=CARTESIAN_POINT('Ctrl Pts',(71.2799039340175,1.26009603367571,12.));
#174060=CARTESIAN_POINT('Ctrl Pts',(71.2585905241406,1.25260937385569,12.));
#174061=CARTESIAN_POINT('Ctrl Pts',(71.2373128222352,1.24515932982113,12.));
#174062=CARTESIAN_POINT('Ctrl Pts',(71.2160709827191,1.23774588208428,12.));
#174063=CARTESIAN_POINT('Ctrl Pts',(71.194865160732,1.2303690109624,12.));
#174064=CARTESIAN_POINT('Ctrl Pts',(71.1736955121362,1.22302869657018,12.));
#174065=CARTESIAN_POINT('Ctrl Pts',(71.1525621935267,1.21572491882263,12.));
#174066=CARTESIAN_POINT('Ctrl Pts',(71.1314653622442,1.20845765743648,12.));
#174067=CARTESIAN_POINT('Ctrl Pts',(71.1104051763839,1.20122689192837,12.));
#174068=CARTESIAN_POINT('Ctrl Pts',(71.089381794801,1.19403260161003,12.));
#174069=CARTESIAN_POINT('Ctrl Pts',(71.0683953771149,1.18687476558133,12.));
#174070=CARTESIAN_POINT('Ctrl Pts',(71.0474460837159,1.17975336273505,12.));
#174071=CARTESIAN_POINT('Ctrl Pts',(71.0265340757699,1.17266837175778,12.));
#174072=CARTESIAN_POINT('Ctrl Pts',(71.0056595152204,1.16561977112881,12.));
#174073=CARTESIAN_POINT('Ctrl Pts',(70.9848225647871,1.15860753911486,12.));
#174074=CARTESIAN_POINT('Ctrl Pts',(70.9640233879659,1.15163165376525,12.));
#174075=CARTESIAN_POINT('Ctrl Pts',(70.9432621490566,1.14469209291489,12.));
#174076=CARTESIAN_POINT('Ctrl Pts',(70.9225390131826,1.13778883418214,12.));
#174077=CARTESIAN_POINT('Ctrl Pts',(70.9018541463089,1.13092185496565,12.));
#174078=CARTESIAN_POINT('Ctrl Pts',(70.8812077152586,1.12409113243514,12.));
#174079=CARTESIAN_POINT('Ctrl Pts',(70.8605998877149,1.11729664352993,12.));
#174080=CARTESIAN_POINT('Ctrl Pts',(70.8400308322037,1.1105383649664,12.));
#174081=CARTESIAN_POINT('Ctrl Pts',(70.8195007180745,1.10381627323947,12.));
#174082=CARTESIAN_POINT('Ctrl Pts',(70.799009715484,1.09713034462266,12.));
#174083=CARTESIAN_POINT('Ctrl Pts',(70.7785579953583,1.09048055516427,12.));
#174084=CARTESIAN_POINT('Ctrl Pts',(70.7581457294447,1.08386688068343,12.));
#174085=CARTESIAN_POINT('Ctrl Pts',(70.7377730903953,1.07728929676409,12.));
#174086=CARTESIAN_POINT('Ctrl Pts',(70.7174402518378,1.07074777874596,12.));
#174087=CARTESIAN_POINT('Ctrl Pts',(70.6971473884459,1.06424230171281,12.));
#174088=CARTESIAN_POINT('Ctrl Pts',(70.676894676009,1.05777284047731,12.));
#174089=CARTESIAN_POINT('Ctrl Pts',(70.6566822912991,1.05133936960072,12.));
#174090=CARTESIAN_POINT('Ctrl Pts',(70.6365104119252,1.04494186341157,12.));
#174091=CARTESIAN_POINT('Ctrl Pts',(70.6163792162073,1.03858029601904,12.));
#174092=CARTESIAN_POINT('Ctrl Pts',(70.5962888829934,1.03225464132871,12.));
#174093=CARTESIAN_POINT('Ctrl Pts',(70.5762395916377,1.02596487304049,12.));
#174094=CARTESIAN_POINT('Ctrl Pts',(70.556231522419,1.01971096460597,12.));
#174095=CARTESIAN_POINT('Ctrl Pts',(70.5362648569061,1.01349288918538,12.));
#174096=CARTESIAN_POINT('Ctrl Pts',(70.5163397782713,1.00731061960969,12.));
#174097=CARTESIAN_POINT('Ctrl Pts',(70.4964564717953,1.00116412831443,12.));
#174098=CARTESIAN_POINT('Ctrl Pts',(70.4766151245212,0.99505338737976,12.));
#174099=CARTESIAN_POINT('Ctrl Pts',(70.4568159243163,0.988978368643654,
12.));
#174100=CARTESIAN_POINT('Ctrl Pts',(70.4370590590842,0.982939043792161,
12.));
#174101=CARTESIAN_POINT('Ctrl Pts',(70.417344715957,0.976935384450047,12.));
#174102=CARTESIAN_POINT('Ctrl Pts',(70.3976730803613,0.970967362281179,
12.));
#174103=CARTESIAN_POINT('Ctrl Pts',(70.3780443377956,0.965034948786454,
12.));
#174104=CARTESIAN_POINT('Ctrl Pts',(70.3584586759536,0.959138115058838,
12.));
#174105=CARTESIAN_POINT('Ctrl Pts',(70.338916286458,0.953276831581247,12.));
#174106=CARTESIAN_POINT('Ctrl Pts',(70.3194173673674,0.947451067929609,
12.));
#174107=CARTESIAN_POINT('Ctrl Pts',(70.299962123399,0.941660792742984,12.));
#174108=CARTESIAN_POINT('Ctrl Pts',(70.2805507606872,0.935905974336485,
12.));
#174109=CARTESIAN_POINT('Ctrl Pts',(70.2611834821723,0.930186581235552,
12.));
#174110=CARTESIAN_POINT('Ctrl Pts',(70.2418604835836,0.924502582639461,
12.));
#174111=CARTESIAN_POINT('Ctrl Pts',(70.2225819470248,0.918853949157122,
12.));
#174112=CARTESIAN_POINT('Ctrl Pts',(70.2033480471676,0.913240652090985,
12.));
#174113=CARTESIAN_POINT('Ctrl Pts',(70.1841589635574,0.907662662015791,
12.));
#174114=CARTESIAN_POINT('Ctrl Pts',(70.1650148905109,0.902119947629775,
12.));
#174115=CARTESIAN_POINT('Ctrl Pts',(70.1459160490446,0.896612474371848,
12.));
#174116=CARTESIAN_POINT('Ctrl Pts',(70.1268626950175,0.891140203464248,
12.));
#174117=CARTESIAN_POINT('Ctrl Pts',(70.1078550938958,0.88570309480254,12.));
#174118=CARTESIAN_POINT('Ctrl Pts',(70.0888934967855,0.880301109660733,
12.));
#174119=CARTESIAN_POINT('Ctrl Pts',(70.0699781183935,0.874934213255844,
12.));
#174120=CARTESIAN_POINT('Ctrl Pts',(70.051109108301,0.869602377871129,12.));
#174121=CARTESIAN_POINT('Ctrl Pts',(70.0322865492925,0.86430558366155,12.));
#174122=CARTESIAN_POINT('Ctrl Pts',(70.0172656933806,0.86009617066874,12.));
#174123=CARTESIAN_POINT('Ctrl Pts',(70.0060209754087,0.85695487025921,12.));
#174124=CARTESIAN_POINT('Ctrl Pts',(69.9985337959407,0.854867673848601,
12.));
#174125=CARTESIAN_POINT('Ctrl Pts',(69.9947925310006,0.853825826608988,
12.));
#174126=CARTESIAN_POINT('Ctrl Pts',(74.0964320766207,3.99277406490871,0.));
#174127=CARTESIAN_POINT('Ctrl Pts',(74.0964320766207,3.99277406490871,4.));
#174128=CARTESIAN_POINT('Ctrl Pts',(74.0964320766208,3.9927740649087,8.));
#174129=CARTESIAN_POINT('Ctrl Pts',(74.0964320766208,3.9927740649087,12.));
#174130=CARTESIAN_POINT('Ctrl Pts',(74.1989040313893,3.9531047458223,0.));
#174131=CARTESIAN_POINT('Ctrl Pts',(74.1989040313893,3.9531047458223,4.));
#174132=CARTESIAN_POINT('Ctrl Pts',(74.1989040313893,3.95310474582228,8.));
#174133=CARTESIAN_POINT('Ctrl Pts',(74.1989040313893,3.95310474582228,12.));
#174134=CARTESIAN_POINT('Ctrl Pts',(74.3538917248566,3.82252142018533,0.));
#174135=CARTESIAN_POINT('Ctrl Pts',(74.3538917248566,3.82252142018533,4.));
#174136=CARTESIAN_POINT('Ctrl Pts',(74.3538917248566,3.82252142018531,7.99999999999999));
#174137=CARTESIAN_POINT('Ctrl Pts',(74.3538917248566,3.82252142018531,12.));
#174138=CARTESIAN_POINT('Ctrl Pts',(74.4114286752098,3.63264011802873,0.));
#174139=CARTESIAN_POINT('Ctrl Pts',(74.4114286752098,3.63264011802873,4.));
#174140=CARTESIAN_POINT('Ctrl Pts',(74.4114286752098,3.63264011802872,8.00000000000001));
#174141=CARTESIAN_POINT('Ctrl Pts',(74.4114286752098,3.63264011802872,12.));
#174142=CARTESIAN_POINT('Ctrl Pts',(74.4153560388998,3.55032190142809,0.));
#174143=CARTESIAN_POINT('Ctrl Pts',(74.4153560388998,3.55032190142809,4.));
#174144=CARTESIAN_POINT('Ctrl Pts',(74.4153560388998,3.55032190142808,8.));
#174145=CARTESIAN_POINT('Ctrl Pts',(74.4153560388998,3.55032190142808,12.));
#174146=CARTESIAN_POINT('',(74.0964320766207,3.99277406490871,0.));
#174147=CARTESIAN_POINT('',(74.4153560388999,3.5503219014281,0.));
#174148=CARTESIAN_POINT('Ctrl Pts',(74.0964320766207,3.99277406490871,0.));
#174149=CARTESIAN_POINT('Ctrl Pts',(74.1989040313893,3.9531047458223,0.));
#174150=CARTESIAN_POINT('Ctrl Pts',(74.2874684276563,3.87848570260117,0.));
#174151=CARTESIAN_POINT('Ctrl Pts',(74.3442121731106,3.78450405480221,0.));
#174152=CARTESIAN_POINT('Ctrl Pts',(74.3867699822013,3.71401781895299,0.));
#174153=CARTESIAN_POINT('Ctrl Pts',(74.4114286752098,3.63264011802873,0.));
#174154=CARTESIAN_POINT('Ctrl Pts',(74.4153560388998,3.55032190142809,0.));
#174155=CARTESIAN_POINT('',(74.4153560388999,3.55032190142809,12.));
#174156=CARTESIAN_POINT('Ctrl Pts',(74.4153560388998,3.55032190142809,0.));
#174157=CARTESIAN_POINT('Ctrl Pts',(74.4153560388998,3.55032190142809,4.));
#174158=CARTESIAN_POINT('Ctrl Pts',(74.4153560388998,3.55032190142808,8.));
#174159=CARTESIAN_POINT('Ctrl Pts',(74.4153560388998,3.55032190142808,12.));
#174160=CARTESIAN_POINT('',(74.0964320766208,3.99277406490869,12.));
#174161=CARTESIAN_POINT('Ctrl Pts',(74.4153560388998,3.55032190142808,12.));
#174162=CARTESIAN_POINT('Ctrl Pts',(74.4114286752098,3.63264011802872,12.));
#174163=CARTESIAN_POINT('Ctrl Pts',(74.3867699822013,3.71401781895297,12.));
#174164=CARTESIAN_POINT('Ctrl Pts',(74.3442121731106,3.78450405480219,12.));
#174165=CARTESIAN_POINT('Ctrl Pts',(74.2874684276563,3.87848570260115,12.));
#174166=CARTESIAN_POINT('Ctrl Pts',(74.1989040313893,3.95310474582228,12.));
#174167=CARTESIAN_POINT('Ctrl Pts',(74.0964320766208,3.9927740649087,12.));
#174168=CARTESIAN_POINT('Ctrl Pts',(74.0964320766208,3.9927740649087,12.));
#174169=CARTESIAN_POINT('Ctrl Pts',(74.0964320766208,3.9927740649087,8.));
#174170=CARTESIAN_POINT('Ctrl Pts',(74.0964320766207,3.99277406490871,4.));
#174171=CARTESIAN_POINT('Ctrl Pts',(74.0964320766207,3.99277406490871,0.));
#174172=CARTESIAN_POINT('Origin',(3.74482667098164E-10,1.64496194443586E-11,
0.));
#174173=CARTESIAN_POINT('Origin',(3.74482667098164E-10,1.64496194443586E-11,
12.));
#174174=CARTESIAN_POINT('Origin',(3.74482667098164E-10,1.64496194443586E-11,
0.));
#174175=CARTESIAN_POINT('Ctrl Pts',(74.3992230078037,3.87370827955544,0.));
#174176=CARTESIAN_POINT('Ctrl Pts',(74.3992230078037,3.87370827955544,12.));
#174177=CARTESIAN_POINT('Ctrl Pts',(74.3940262116388,3.87578335377326,0.));
#174178=CARTESIAN_POINT('Ctrl Pts',(74.3940262116388,3.87578335377326,12.));
#174179=CARTESIAN_POINT('Ctrl Pts',(74.3836349189184,3.87992989995748,0.));
#174180=CARTESIAN_POINT('Ctrl Pts',(74.3836349189184,3.87992989995748,12.));
#174181=CARTESIAN_POINT('Ctrl Pts',(74.3680548786661,3.88613891247984,0.));
#174182=CARTESIAN_POINT('Ctrl Pts',(74.3680548786661,3.88613891247984,12.));
#174183=CARTESIAN_POINT('Ctrl Pts',(74.3472952898745,3.89439598145329,0.));
#174184=CARTESIAN_POINT('Ctrl Pts',(74.3472952898745,3.89439598145329,12.));
#174185=CARTESIAN_POINT('Ctrl Pts',(74.3213688090133,3.90468128904635,0.));
#174186=CARTESIAN_POINT('Ctrl Pts',(74.3213688090133,3.90468128904635,12.));
#174187=CARTESIAN_POINT('Ctrl Pts',(74.2954653518728,3.91493056285031,0.));
#174188=CARTESIAN_POINT('Ctrl Pts',(74.2954653518728,3.91493056285031,12.));
#174189=CARTESIAN_POINT('Ctrl Pts',(74.2695849516226,3.92514379920744,0.));
#174190=CARTESIAN_POINT('Ctrl Pts',(74.2695849516226,3.92514379920744,12.));
#174191=CARTESIAN_POINT('Ctrl Pts',(74.2437276593623,3.93532099774204,0.));
#174192=CARTESIAN_POINT('Ctrl Pts',(74.2437276593623,3.93532099774204,12.));
#174193=CARTESIAN_POINT('Ctrl Pts',(74.2178935492876,3.94546216377452,0.));
#174194=CARTESIAN_POINT('Ctrl Pts',(74.2178935492876,3.94546216377452,12.));
#174195=CARTESIAN_POINT('Ctrl Pts',(74.1920827166585,3.95556730821111,0.));
#174196=CARTESIAN_POINT('Ctrl Pts',(74.1920827166585,3.95556730821111,12.));
#174197=CARTESIAN_POINT('Ctrl Pts',(74.1662952702485,3.96563644549386,0.));
#174198=CARTESIAN_POINT('Ctrl Pts',(74.1662952702485,3.96563644549386,12.));
#174199=CARTESIAN_POINT('Ctrl Pts',(74.1405313263109,3.97566959209529,0.));
#174200=CARTESIAN_POINT('Ctrl Pts',(74.1405313263109,3.97566959209529,12.));
#174201=CARTESIAN_POINT('Ctrl Pts',(74.1147910020891,3.98566676483642,0.));
#174202=CARTESIAN_POINT('Ctrl Pts',(74.1147910020891,3.98566676483642,12.));
#174203=CARTESIAN_POINT('Ctrl Pts',(74.0890744091186,3.99562797918288,0.));
#174204=CARTESIAN_POINT('Ctrl Pts',(74.0890744091186,3.99562797918288,12.));
#174205=CARTESIAN_POINT('Ctrl Pts',(74.0633816478037,4.00555324785481,0.));
#174206=CARTESIAN_POINT('Ctrl Pts',(74.0633816478037,4.00555324785481,12.));
#174207=CARTESIAN_POINT('Ctrl Pts',(74.0377128111863,4.01544258176711,0.));
#174208=CARTESIAN_POINT('Ctrl Pts',(74.0377128111863,4.01544258176711,12.));
#174209=CARTESIAN_POINT('Ctrl Pts',(74.012067987646,4.02529599070095,0.));
#174210=CARTESIAN_POINT('Ctrl Pts',(74.012067987646,4.02529599070095,12.));
#174211=CARTESIAN_POINT('Ctrl Pts',(73.9864472641033,4.0351134841066,0.));
#174212=CARTESIAN_POINT('Ctrl Pts',(73.9864472641033,4.0351134841066,12.));
#174213=CARTESIAN_POINT('Ctrl Pts',(73.9608507287909,4.04489507179958,0.));
#174214=CARTESIAN_POINT('Ctrl Pts',(73.9608507287909,4.04489507179958,12.));
#174215=CARTESIAN_POINT('Ctrl Pts',(73.9352784747608,4.05464076484752,0.));
#174216=CARTESIAN_POINT('Ctrl Pts',(73.9352784747608,4.05464076484752,12.));
#174217=CARTESIAN_POINT('Ctrl Pts',(73.9097305995115,4.06435057547325,0.));
#174218=CARTESIAN_POINT('Ctrl Pts',(73.9097305995115,4.06435057547325,12.));
#174219=CARTESIAN_POINT('Ctrl Pts',(73.8842072034008,4.07402451665245,0.));
#174220=CARTESIAN_POINT('Ctrl Pts',(73.8842072034008,4.07402451665245,12.));
#174221=CARTESIAN_POINT('Ctrl Pts',(73.8587083884191,4.08366260180675,0.));
#174222=CARTESIAN_POINT('Ctrl Pts',(73.8587083884191,4.08366260180675,12.));
#174223=CARTESIAN_POINT('Ctrl Pts',(73.8332342568989,4.09326484448233,0.));
#174224=CARTESIAN_POINT('Ctrl Pts',(73.8332342568989,4.09326484448233,12.));
#174225=CARTESIAN_POINT('Ctrl Pts',(73.8077849100342,4.1028312579873,0.));
#174226=CARTESIAN_POINT('Ctrl Pts',(73.8077849100342,4.1028312579873,12.));
#174227=CARTESIAN_POINT('Ctrl Pts',(73.7823604472159,4.11236185522788,0.));
#174228=CARTESIAN_POINT('Ctrl Pts',(73.7823604472159,4.11236185522788,12.));
#174229=CARTESIAN_POINT('Ctrl Pts',(73.7569609668528,4.12185664890557,0.));
#174230=CARTESIAN_POINT('Ctrl Pts',(73.7569609668528,4.12185664890557,12.));
#174231=CARTESIAN_POINT('Ctrl Pts',(73.7315865668522,4.13131565163579,0.));
#174232=CARTESIAN_POINT('Ctrl Pts',(73.7315865668522,4.13131565163579,12.));
#174233=CARTESIAN_POINT('Ctrl Pts',(73.7062373452342,4.14073887610154,0.));
#174234=CARTESIAN_POINT('Ctrl Pts',(73.7062373452342,4.14073887610154,12.));
#174235=CARTESIAN_POINT('Ctrl Pts',(73.6809134006897,4.15012633519724,0.));
#174236=CARTESIAN_POINT('Ctrl Pts',(73.6809134006897,4.15012633519724,12.));
#174237=CARTESIAN_POINT('Ctrl Pts',(73.6556148331489,4.15947804217784,0.));
#174238=CARTESIAN_POINT('Ctrl Pts',(73.6556148331489,4.15947804217784,12.));
#174239=CARTESIAN_POINT('Ctrl Pts',(73.6303417435251,4.16879401058781,0.));
#174240=CARTESIAN_POINT('Ctrl Pts',(73.6303417435251,4.16879401058781,12.));
#174241=CARTESIAN_POINT('Ctrl Pts',(73.6050942334768,4.17807425419813,0.));
#174242=CARTESIAN_POINT('Ctrl Pts',(73.6050942334768,4.17807425419813,12.));
#174243=CARTESIAN_POINT('Ctrl Pts',(73.5798724051519,4.18731878694237,0.));
#174244=CARTESIAN_POINT('Ctrl Pts',(73.5798724051519,4.18731878694237,12.));
#174245=CARTESIAN_POINT('Ctrl Pts',(73.5546763609572,4.19652762286128,0.));
#174246=CARTESIAN_POINT('Ctrl Pts',(73.5546763609572,4.19652762286128,12.));
#174247=CARTESIAN_POINT('Ctrl Pts',(73.5295062032628,4.2057007760373,0.));
#174248=CARTESIAN_POINT('Ctrl Pts',(73.5295062032628,4.2057007760373,12.));
#174249=CARTESIAN_POINT('Ctrl Pts',(73.5043620344116,4.21483826059441,0.));
#174250=CARTESIAN_POINT('Ctrl Pts',(73.5043620344116,4.21483826059441,12.));
#174251=CARTESIAN_POINT('Ctrl Pts',(73.4792439568633,4.22394009072757,0.));
#174252=CARTESIAN_POINT('Ctrl Pts',(73.4792439568633,4.22394009072757,12.));
#174253=CARTESIAN_POINT('Ctrl Pts',(73.4541520732948,4.23300628072759,0.));
#174254=CARTESIAN_POINT('Ctrl Pts',(73.4541520732948,4.23300628072759,12.));
#174255=CARTESIAN_POINT('Ctrl Pts',(73.4290864867101,4.24203684500939,0.));
#174256=CARTESIAN_POINT('Ctrl Pts',(73.4290864867101,4.24203684500939,12.));
#174257=CARTESIAN_POINT('Ctrl Pts',(73.4040473005592,4.25103179814887,0.));
#174258=CARTESIAN_POINT('Ctrl Pts',(73.4040473005592,4.25103179814887,12.));
#174259=CARTESIAN_POINT('Ctrl Pts',(73.3790346187938,4.259991154899,0.));
#174260=CARTESIAN_POINT('Ctrl Pts',(73.3790346187938,4.259991154899,12.));
#174261=CARTESIAN_POINT('Ctrl Pts',(73.3540485458065,4.268914930167,0.));
#174262=CARTESIAN_POINT('Ctrl Pts',(73.3540485458065,4.268914930167,12.));
#174263=CARTESIAN_POINT('Ctrl Pts',(73.3290891863949,4.2778031390039,0.));
#174264=CARTESIAN_POINT('Ctrl Pts',(73.3290891863949,4.2778031390039,12.));
#174265=CARTESIAN_POINT('Ctrl Pts',(73.3041566457135,4.28665579659302,0.));
#174266=CARTESIAN_POINT('Ctrl Pts',(73.3041566457135,4.28665579659302,12.));
#174267=CARTESIAN_POINT('Ctrl Pts',(73.2792510292253,4.29547291824287,0.));
#174268=CARTESIAN_POINT('Ctrl Pts',(73.2792510292253,4.29547291824287,12.));
#174269=CARTESIAN_POINT('Ctrl Pts',(73.2543724426577,4.30425451938231,0.));
#174270=CARTESIAN_POINT('Ctrl Pts',(73.2543724426577,4.30425451938231,12.));
#174271=CARTESIAN_POINT('Ctrl Pts',(73.2295209920334,4.31300061556098,0.));
#174272=CARTESIAN_POINT('Ctrl Pts',(73.2295209920334,4.31300061556098,12.));
#174273=CARTESIAN_POINT('Ctrl Pts',(73.204696783694,4.32171122245214,0.));
#174274=CARTESIAN_POINT('Ctrl Pts',(73.204696783694,4.32171122245214,12.));
#174275=CARTESIAN_POINT('Ctrl Pts',(73.1798999243235,4.33038635585877,0.));
#174276=CARTESIAN_POINT('Ctrl Pts',(73.1798999243235,4.33038635585877,12.));
#174277=CARTESIAN_POINT('Ctrl Pts',(73.1551305209685,4.33902603172141,0.));
#174278=CARTESIAN_POINT('Ctrl Pts',(73.1551305209685,4.33902603172141,12.));
#174279=CARTESIAN_POINT('Ctrl Pts',(73.130388681059,4.34763026613158,0.));
#174280=CARTESIAN_POINT('Ctrl Pts',(73.130388681059,4.34763026613158,12.));
#174281=CARTESIAN_POINT('Ctrl Pts',(73.1056745124087,4.3561990753272,0.));
#174282=CARTESIAN_POINT('Ctrl Pts',(73.1056745124087,4.3561990753272,12.));
#174283=CARTESIAN_POINT('Ctrl Pts',(73.0809881232103,4.36473247568642,0.));
#174284=CARTESIAN_POINT('Ctrl Pts',(73.0809881232103,4.36473247568642,12.));
#174285=CARTESIAN_POINT('Ctrl Pts',(73.0563296220299,4.37323048372608,0.));
#174286=CARTESIAN_POINT('Ctrl Pts',(73.0563296220299,4.37323048372608,12.));
#174287=CARTESIAN_POINT('Ctrl Pts',(73.0316991177993,4.38169311610151,0.));
#174288=CARTESIAN_POINT('Ctrl Pts',(73.0316991177993,4.38169311610151,12.));
#174289=CARTESIAN_POINT('Ctrl Pts',(73.007096719804,4.3901203896114,0.));
#174290=CARTESIAN_POINT('Ctrl Pts',(73.007096719804,4.3901203896114,12.));
#174291=CARTESIAN_POINT('Ctrl Pts',(72.9825225376846,4.39851232119723,0.));
#174292=CARTESIAN_POINT('Ctrl Pts',(72.9825225376846,4.39851232119723,12.));
#174293=CARTESIAN_POINT('Ctrl Pts',(72.95797668145,4.40686892793958,0.));
#174294=CARTESIAN_POINT('Ctrl Pts',(72.95797668145,4.40686892793958,12.));
#174295=CARTESIAN_POINT('Ctrl Pts',(72.9334592614829,4.41519022705922,0.));
#174296=CARTESIAN_POINT('Ctrl Pts',(72.9334592614829,4.41519022705922,12.));
#174297=CARTESIAN_POINT('Ctrl Pts',(72.9089703885462,4.42347623591942,0.));
#174298=CARTESIAN_POINT('Ctrl Pts',(72.9089703885462,4.42347623591942,12.));
#174299=CARTESIAN_POINT('Ctrl Pts',(72.8845101737855,4.4317269720335,0.));
#174300=CARTESIAN_POINT('Ctrl Pts',(72.8845101737855,4.4317269720335,12.));
#174301=CARTESIAN_POINT('Ctrl Pts',(72.8600787287318,4.43994245306819,0.));
#174302=CARTESIAN_POINT('Ctrl Pts',(72.8600787287318,4.43994245306819,12.));
#174303=CARTESIAN_POINT('Ctrl Pts',(72.8356761653069,4.44812269683738,0.));
#174304=CARTESIAN_POINT('Ctrl Pts',(72.8356761653069,4.44812269683738,12.));
#174305=CARTESIAN_POINT('Ctrl Pts',(72.8113025958262,4.45626772130147,0.));
#174306=CARTESIAN_POINT('Ctrl Pts',(72.8113025958262,4.45626772130147,12.));
#174307=CARTESIAN_POINT('Ctrl Pts',(72.7869581329994,4.46437754456793,0.));
#174308=CARTESIAN_POINT('Ctrl Pts',(72.7869581329994,4.46437754456793,12.));
#174309=CARTESIAN_POINT('Ctrl Pts',(72.7626428899281,4.4724521848961,0.));
#174310=CARTESIAN_POINT('Ctrl Pts',(72.7626428899281,4.4724521848961,12.));
#174311=CARTESIAN_POINT('Ctrl Pts',(72.738356980103,4.48049166070206,0.));
#174312=CARTESIAN_POINT('Ctrl Pts',(72.738356980103,4.48049166070206,12.));
#174313=CARTESIAN_POINT('Ctrl Pts',(72.714100517414,4.48849599055338,0.));
#174314=CARTESIAN_POINT('Ctrl Pts',(72.714100517414,4.48849599055338,12.));
#174315=CARTESIAN_POINT('Ctrl Pts',(72.6898736161542,4.49646519316813,0.));
#174316=CARTESIAN_POINT('Ctrl Pts',(72.6898736161542,4.49646519316813,12.));
#174317=CARTESIAN_POINT('Ctrl Pts',(72.6656763910241,4.50439928741604,0.));
#174318=CARTESIAN_POINT('Ctrl Pts',(72.6656763910241,4.50439928741604,12.));
#174319=CARTESIAN_POINT('Ctrl Pts',(72.6415089571321,4.51229829232264,0.));
#174320=CARTESIAN_POINT('Ctrl Pts',(72.6415089571321,4.51229829232264,12.));
#174321=CARTESIAN_POINT('Ctrl Pts',(72.6173714299942,4.52016222707638,0.));
#174322=CARTESIAN_POINT('Ctrl Pts',(72.6173714299942,4.52016222707638,12.));
#174323=CARTESIAN_POINT('Ctrl Pts',(72.5932639255409,4.52799111102392,0.));
#174324=CARTESIAN_POINT('Ctrl Pts',(72.5932639255409,4.52799111102392,12.));
#174325=CARTESIAN_POINT('Ctrl Pts',(72.5691865601223,4.535784963668,0.));
#174326=CARTESIAN_POINT('Ctrl Pts',(72.5691865601223,4.535784963668,12.));
#174327=CARTESIAN_POINT('Ctrl Pts',(72.5451394505103,4.54354380466823,0.));
#174328=CARTESIAN_POINT('Ctrl Pts',(72.5451394505103,4.54354380466823,12.));
#174329=CARTESIAN_POINT('Ctrl Pts',(72.5211227139001,4.55126765384405,0.));
#174330=CARTESIAN_POINT('Ctrl Pts',(72.5211227139001,4.55126765384405,12.));
#174331=CARTESIAN_POINT('Ctrl Pts',(72.4971364679068,4.55895653118221,0.));
#174332=CARTESIAN_POINT('Ctrl Pts',(72.4971364679068,4.55895653118221,12.));
#174333=CARTESIAN_POINT('Ctrl Pts',(72.4731808305728,4.56661045683376,0.));
#174334=CARTESIAN_POINT('Ctrl Pts',(72.4731808305728,4.56661045683376,12.));
#174335=CARTESIAN_POINT('Ctrl Pts',(72.4492559203745,4.57422945111103,0.));
#174336=CARTESIAN_POINT('Ctrl Pts',(72.4492559203745,4.57422945111103,12.));
#174337=CARTESIAN_POINT('Ctrl Pts',(72.4253618562252,4.58181353448852,0.));
#174338=CARTESIAN_POINT('Ctrl Pts',(72.4253618562252,4.58181353448852,12.));
#174339=CARTESIAN_POINT('Ctrl Pts',(72.401498757478,4.58936272760545,0.));
#174340=CARTESIAN_POINT('Ctrl Pts',(72.401498757478,4.58936272760545,12.));
#174341=CARTESIAN_POINT('Ctrl Pts',(72.3776667439227,4.5968770512733,0.));
#174342=CARTESIAN_POINT('Ctrl Pts',(72.3776667439227,4.5968770512733,12.));
#174343=CARTESIAN_POINT('Ctrl Pts',(72.3538659357913,4.60435652647454,0.));
#174344=CARTESIAN_POINT('Ctrl Pts',(72.3538659357913,4.60435652647454,12.));
#174345=CARTESIAN_POINT('Ctrl Pts',(72.3300964537658,4.61180117435863,0.));
#174346=CARTESIAN_POINT('Ctrl Pts',(72.3300964537658,4.61180117435863,12.));
#174347=CARTESIAN_POINT('Ctrl Pts',(72.3063584189807,4.61921101624292,0.));
#174348=CARTESIAN_POINT('Ctrl Pts',(72.3063584189807,4.61921101624292,12.));
#174349=CARTESIAN_POINT('Ctrl Pts',(72.2826519530259,4.62658607361466,0.));
#174350=CARTESIAN_POINT('Ctrl Pts',(72.2826519530259,4.62658607361466,12.));
#174351=CARTESIAN_POINT('Ctrl Pts',(72.2589771779456,4.63392636813844,0.));
#174352=CARTESIAN_POINT('Ctrl Pts',(72.2589771779456,4.63392636813844,12.));
#174353=CARTESIAN_POINT('Ctrl Pts',(72.2353342162417,4.64123192165628,0.));
#174354=CARTESIAN_POINT('Ctrl Pts',(72.2353342162417,4.64123192165628,12.));
#174355=CARTESIAN_POINT('Ctrl Pts',(72.2117231908822,4.64850275618324,0.));
#174356=CARTESIAN_POINT('Ctrl Pts',(72.2117231908822,4.64850275618324,12.));
#174357=CARTESIAN_POINT('Ctrl Pts',(72.1881442253053,4.65573889390823,0.));
#174358=CARTESIAN_POINT('Ctrl Pts',(72.1881442253053,4.65573889390823,12.));
#174359=CARTESIAN_POINT('Ctrl Pts',(72.1645974434216,4.6629403571957,0.));
#174360=CARTESIAN_POINT('Ctrl Pts',(72.1645974434216,4.6629403571957,12.));
#174361=CARTESIAN_POINT('Ctrl Pts',(72.1410829696128,4.67010716859286,0.));
#174362=CARTESIAN_POINT('Ctrl Pts',(72.1410829696128,4.67010716859286,12.));
#174363=CARTESIAN_POINT('Ctrl Pts',(72.1176009287351,4.67723935083095,0.));
#174364=CARTESIAN_POINT('Ctrl Pts',(72.1176009287351,4.67723935083095,12.));
#174365=CARTESIAN_POINT('Ctrl Pts',(72.0941514461287,4.68433692682069,0.));
#174366=CARTESIAN_POINT('Ctrl Pts',(72.0941514461287,4.68433692682069,12.));
#174367=CARTESIAN_POINT('Ctrl Pts',(72.0707346476213,4.69139991965284,0.));
#174368=CARTESIAN_POINT('Ctrl Pts',(72.0707346476213,4.69139991965284,12.));
#174369=CARTESIAN_POINT('Ctrl Pts',(72.0473506595318,4.69842835259993,0.));
#174370=CARTESIAN_POINT('Ctrl Pts',(72.0473506595318,4.69842835259993,12.));
#174371=CARTESIAN_POINT('Ctrl Pts',(72.0239996086686,4.70542224912301,0.));
#174372=CARTESIAN_POINT('Ctrl Pts',(72.0239996086686,4.70542224912301,12.));
#174373=CARTESIAN_POINT('Ctrl Pts',(72.0006816223325,4.71238163287397,0.));
#174374=CARTESIAN_POINT('Ctrl Pts',(72.0006816223325,4.71238163287397,12.));
#174375=CARTESIAN_POINT('Ctrl Pts',(71.9773968283259,4.71930652769071,0.));
#174376=CARTESIAN_POINT('Ctrl Pts',(71.9773968283259,4.71930652769071,12.));
#174377=CARTESIAN_POINT('Ctrl Pts',(71.9541453549579,4.72619695759774,0.));
#174378=CARTESIAN_POINT('Ctrl Pts',(71.9541453549579,4.72619695759774,12.));
#174379=CARTESIAN_POINT('Ctrl Pts',(71.9309273310471,4.73305294680786,0.));
#174380=CARTESIAN_POINT('Ctrl Pts',(71.9309273310471,4.73305294680786,12.));
#174381=CARTESIAN_POINT('Ctrl Pts',(71.9077428859212,4.73987451972864,0.));
#174382=CARTESIAN_POINT('Ctrl Pts',(71.9077428859212,4.73987451972864,12.));
#174383=CARTESIAN_POINT('Ctrl Pts',(71.8845921494189,4.74666170096548,0.));
#174384=CARTESIAN_POINT('Ctrl Pts',(71.8845921494189,4.74666170096548,12.));
#174385=CARTESIAN_POINT('Ctrl Pts',(71.8614752519008,4.7534145153167,0.));
#174386=CARTESIAN_POINT('Ctrl Pts',(71.8614752519008,4.7534145153167,12.));
#174387=CARTESIAN_POINT('Ctrl Pts',(71.8383923242531,4.7601329877742,0.));
#174388=CARTESIAN_POINT('Ctrl Pts',(71.8383923242531,4.7601329877742,12.));
#174389=CARTESIAN_POINT('Ctrl Pts',(71.8153434978923,4.76681714352503,0.));
#174390=CARTESIAN_POINT('Ctrl Pts',(71.8153434978923,4.76681714352503,12.));
#174391=CARTESIAN_POINT('Ctrl Pts',(71.7923289047643,4.77346700795792,0.));
#174392=CARTESIAN_POINT('Ctrl Pts',(71.7923289047643,4.77346700795792,12.));
#174393=CARTESIAN_POINT('Ctrl Pts',(71.769348677346,4.78008260666651,0.));
#174394=CARTESIAN_POINT('Ctrl Pts',(71.769348677346,4.78008260666651,12.));
#174395=CARTESIAN_POINT('Ctrl Pts',(71.7464029486563,4.78666396544459,0.));
#174396=CARTESIAN_POINT('Ctrl Pts',(71.7464029486563,4.78666396544459,12.));
#174397=CARTESIAN_POINT('Ctrl Pts',(71.723491852261,4.79321111028676,0.));
#174398=CARTESIAN_POINT('Ctrl Pts',(71.723491852261,4.79321111028676,12.));
#174399=CARTESIAN_POINT('Ctrl Pts',(71.7006155222764,4.79972406739011,0.));
#174400=CARTESIAN_POINT('Ctrl Pts',(71.7006155222764,4.79972406739011,12.));
#174401=CARTESIAN_POINT('Ctrl Pts',(71.6777740933687,4.80620286316076,0.));
#174402=CARTESIAN_POINT('Ctrl Pts',(71.6777740933687,4.80620286316076,12.));
#174403=CARTESIAN_POINT('Ctrl Pts',(71.6549677007582,4.81264752421714,0.));
#174404=CARTESIAN_POINT('Ctrl Pts',(71.6549677007582,4.81264752421714,12.));
#174405=CARTESIAN_POINT('Ctrl Pts',(71.6321964802297,4.81905807738542,0.));
#174406=CARTESIAN_POINT('Ctrl Pts',(71.6321964802297,4.81905807738542,12.));
#174407=CARTESIAN_POINT('Ctrl Pts',(71.6094605681353,4.82543454970021,0.));
#174408=CARTESIAN_POINT('Ctrl Pts',(71.6094605681353,4.82543454970021,12.));
#174409=CARTESIAN_POINT('Ctrl Pts',(71.5867601014008,4.83177696840641,0.));
#174410=CARTESIAN_POINT('Ctrl Pts',(71.5867601014008,4.83177696840641,12.));
#174411=CARTESIAN_POINT('Ctrl Pts',(71.5640952175239,4.8380853609659,0.));
#174412=CARTESIAN_POINT('Ctrl Pts',(71.5640952175239,4.8380853609659,12.));
#174413=CARTESIAN_POINT('Ctrl Pts',(71.5414660545778,4.84435975506057,0.));
#174414=CARTESIAN_POINT('Ctrl Pts',(71.5414660545778,4.84435975506057,12.));
#174415=CARTESIAN_POINT('Ctrl Pts',(71.5188727512231,4.85060017858787,0.));
#174416=CARTESIAN_POINT('Ctrl Pts',(71.5188727512231,4.85060017858787,12.));
#174417=CARTESIAN_POINT('Ctrl Pts',(71.4963154467128,4.85680665966185,0.));
#174418=CARTESIAN_POINT('Ctrl Pts',(71.4963154467128,4.85680665966185,12.));
#174419=CARTESIAN_POINT('Ctrl Pts',(71.4737942808971,4.86297922661499,0.));
#174420=CARTESIAN_POINT('Ctrl Pts',(71.4737942808971,4.86297922661499,12.));
#174421=CARTESIAN_POINT('Ctrl Pts',(71.4513093942216,4.86911790800534,0.));
#174422=CARTESIAN_POINT('Ctrl Pts',(71.4513093942216,4.86911790800534,12.));
#174423=CARTESIAN_POINT('Ctrl Pts',(71.4288609277324,4.87522273261881,0.));
#174424=CARTESIAN_POINT('Ctrl Pts',(71.4288609277324,4.87522273261881,12.));
#174425=CARTESIAN_POINT('Ctrl Pts',(71.4064490230857,4.88129372946525,0.));
#174426=CARTESIAN_POINT('Ctrl Pts',(71.4064490230857,4.88129372946525,12.));
#174427=CARTESIAN_POINT('Ctrl Pts',(71.3840738225547,4.88733092777965,0.));
#174428=CARTESIAN_POINT('Ctrl Pts',(71.3840738225547,4.88733092777965,12.));
#174429=CARTESIAN_POINT('Ctrl Pts',(71.3617354690342,4.89333435702424,0.));
#174430=CARTESIAN_POINT('Ctrl Pts',(71.3617354690342,4.89333435702424,12.));
#174431=CARTESIAN_POINT('Ctrl Pts',(71.3394341060396,4.899304046896,0.));
#174432=CARTESIAN_POINT('Ctrl Pts',(71.3394341060396,4.899304046896,12.));
#174433=CARTESIAN_POINT('Ctrl Pts',(71.3171698777124,4.90524002732806,0.));
#174434=CARTESIAN_POINT('Ctrl Pts',(71.3171698777124,4.90524002732806,12.));
#174435=CARTESIAN_POINT('Ctrl Pts',(71.2949429288319,4.91114232848623,0.));
#174436=CARTESIAN_POINT('Ctrl Pts',(71.2949429288319,4.91114232848623,12.));
#174437=CARTESIAN_POINT('Ctrl Pts',(71.27275340482,4.91701098077042,0.));
#174438=CARTESIAN_POINT('Ctrl Pts',(71.27275340482,4.91701098077042,12.));
#174439=CARTESIAN_POINT('Ctrl Pts',(71.2506014517457,4.92284601481711,0.));
#174440=CARTESIAN_POINT('Ctrl Pts',(71.2506014517457,4.92284601481711,12.));
#174441=CARTESIAN_POINT('Ctrl Pts',(71.2284872163248,4.92864746150711,0.));
#174442=CARTESIAN_POINT('Ctrl Pts',(71.2284872163248,4.92864746150711,12.));
#174443=CARTESIAN_POINT('Ctrl Pts',(71.206410845926,4.93441535196594,0.));
#174444=CARTESIAN_POINT('Ctrl Pts',(71.206410845926,4.93441535196594,12.));
#174445=CARTESIAN_POINT('Ctrl Pts',(71.184372488583,4.94014971756097,0.));
#174446=CARTESIAN_POINT('Ctrl Pts',(71.184372488583,4.94014971756097,12.));
#174447=CARTESIAN_POINT('Ctrl Pts',(71.1623722929998,4.94585058990337,0.));
#174448=CARTESIAN_POINT('Ctrl Pts',(71.1623722929998,4.94585058990337,12.));
#174449=CARTESIAN_POINT('Ctrl Pts',(71.1404104085561,4.95151800085111,0.));
#174450=CARTESIAN_POINT('Ctrl Pts',(71.1404104085561,4.95151800085111,12.));
#174451=CARTESIAN_POINT('Ctrl Pts',(71.1184869853071,4.95715198251704,0.));
#174452=CARTESIAN_POINT('Ctrl Pts',(71.1184869853071,4.95715198251704,12.));
#174453=CARTESIAN_POINT('Ctrl Pts',(71.0966021739922,4.96275256726787,0.));
#174454=CARTESIAN_POINT('Ctrl Pts',(71.0966021739922,4.96275256726787,12.));
#174455=CARTESIAN_POINT('Ctrl Pts',(71.0747561260443,4.96831978772202,0.));
#174456=CARTESIAN_POINT('Ctrl Pts',(71.0747561260443,4.96831978772202,12.));
#174457=CARTESIAN_POINT('Ctrl Pts',(71.0529489935959,4.97385367675158,0.));
#174458=CARTESIAN_POINT('Ctrl Pts',(71.0529489935959,4.97385367675158,12.));
#174459=CARTESIAN_POINT('Ctrl Pts',(71.031180929482,4.97935426748578,0.));
#174460=CARTESIAN_POINT('Ctrl Pts',(71.031180929482,4.97935426748578,12.));
#174461=CARTESIAN_POINT('Ctrl Pts',(71.0094520872375,4.98482159331852,0.));
#174462=CARTESIAN_POINT('Ctrl Pts',(71.0094520872375,4.98482159331852,12.));
#174463=CARTESIAN_POINT('Ctrl Pts',(70.9877626211112,4.99025568790653,0.));
#174464=CARTESIAN_POINT('Ctrl Pts',(70.9877626211112,4.99025568790653,12.));
#174465=CARTESIAN_POINT('Ctrl Pts',(70.9661126860773,4.99565658516906,0.));
#174466=CARTESIAN_POINT('Ctrl Pts',(70.9661126860773,4.99565658516906,12.));
#174467=CARTESIAN_POINT('Ctrl Pts',(70.9445024378439,5.0010243192904,0.));
#174468=CARTESIAN_POINT('Ctrl Pts',(70.9445024378439,5.0010243192904,12.));
#174469=CARTESIAN_POINT('Ctrl Pts',(70.9229320328588,5.00635892472518,0.));
#174470=CARTESIAN_POINT('Ctrl Pts',(70.9229320328588,5.00635892472518,12.));
#174471=CARTESIAN_POINT('Ctrl Pts',(70.9014016283123,5.01166043620574,0.));
#174472=CARTESIAN_POINT('Ctrl Pts',(70.9014016283123,5.01166043620574,12.));
#174473=CARTESIAN_POINT('Ctrl Pts',(70.8799113821449,5.01692888873793,0.));
#174474=CARTESIAN_POINT('Ctrl Pts',(70.8799113821449,5.01692888873793,12.));
#174475=CARTESIAN_POINT('Ctrl Pts',(70.8584614530517,5.02216431760061,0.));
#174476=CARTESIAN_POINT('Ctrl Pts',(70.8584614530517,5.02216431760061,12.));
#174477=CARTESIAN_POINT('Ctrl Pts',(70.8370520004844,5.02736675834692,0.));
#174478=CARTESIAN_POINT('Ctrl Pts',(70.8370520004844,5.02736675834692,12.));
#174479=CARTESIAN_POINT('Ctrl Pts',(70.8156831846493,5.03253624680941,0.));
#174480=CARTESIAN_POINT('Ctrl Pts',(70.8156831846493,5.03253624680941,12.));
#174481=CARTESIAN_POINT('Ctrl Pts',(70.7943551665071,5.03767281910484,0.));
#174482=CARTESIAN_POINT('Ctrl Pts',(70.7943551665071,5.03767281910484,12.));
#174483=CARTESIAN_POINT('Ctrl Pts',(70.7730681077997,5.04277651163357,0.));
#174484=CARTESIAN_POINT('Ctrl Pts',(70.7730681077997,5.04277651163357,12.));
#174485=CARTESIAN_POINT('Ctrl Pts',(70.7518221710715,5.04784736108351,0.));
#174486=CARTESIAN_POINT('Ctrl Pts',(70.7518221710715,5.04784736108351,12.));
#174487=CARTESIAN_POINT('Ctrl Pts',(70.7306175196856,5.05288540443478,0.));
#174488=CARTESIAN_POINT('Ctrl Pts',(70.7306175196856,5.05288540443478,12.));
#174489=CARTESIAN_POINT('Ctrl Pts',(70.7094543178416,5.05789067897041,0.));
#174490=CARTESIAN_POINT('Ctrl Pts',(70.7094543178416,5.05789067897041,12.));
#174491=CARTESIAN_POINT('Ctrl Pts',(70.6883327305755,5.06286322227797,0.));
#174492=CARTESIAN_POINT('Ctrl Pts',(70.6883327305755,5.06286322227797,12.));
#174493=CARTESIAN_POINT('Ctrl Pts',(70.6672529237431,5.06780307224053,0.));
#174494=CARTESIAN_POINT('Ctrl Pts',(70.6672529237431,5.06780307224053,12.));
#174495=CARTESIAN_POINT('Ctrl Pts',(70.6462150640009,5.07271026703351,0.));
#174496=CARTESIAN_POINT('Ctrl Pts',(70.6462150640009,5.07271026703351,12.));
#174497=CARTESIAN_POINT('Ctrl Pts',(70.6252193187892,5.07758484512311,0.));
#174498=CARTESIAN_POINT('Ctrl Pts',(70.6252193187892,5.07758484512311,12.));
#174499=CARTESIAN_POINT('Ctrl Pts',(70.6042658562951,5.08242684526704,0.));
#174500=CARTESIAN_POINT('Ctrl Pts',(70.6042658562951,5.08242684526704,12.));
#174501=CARTESIAN_POINT('Ctrl Pts',(70.5833548455043,5.08723630652291,0.));
#174502=CARTESIAN_POINT('Ctrl Pts',(70.5833548455043,5.08723630652291,12.));
#174503=CARTESIAN_POINT('Ctrl Pts',(70.5624864562841,5.09201326826146,0.));
#174504=CARTESIAN_POINT('Ctrl Pts',(70.5624864562841,5.09201326826146,12.));
#174505=CARTESIAN_POINT('Ctrl Pts',(70.5416608594526,5.09675777018183,0.));
#174506=CARTESIAN_POINT('Ctrl Pts',(70.5416608594526,5.09675777018183,12.));
#174507=CARTESIAN_POINT('Ctrl Pts',(70.5208782268482,5.10146985232929,0.));
#174508=CARTESIAN_POINT('Ctrl Pts',(70.5208782268482,5.10146985232929,12.));
#174509=CARTESIAN_POINT('Ctrl Pts',(70.5001387313963,5.10614955511643,0.));
#174510=CARTESIAN_POINT('Ctrl Pts',(70.5001387313963,5.10614955511643,12.));
#174511=CARTESIAN_POINT('Ctrl Pts',(70.4794425469799,5.11079691929193,0.));
#174512=CARTESIAN_POINT('Ctrl Pts',(70.4794425469799,5.11079691929193,12.));
#174513=CARTESIAN_POINT('Ctrl Pts',(70.4587898482946,5.1154119859092,0.));
#174514=CARTESIAN_POINT('Ctrl Pts',(70.4587898482946,5.1154119859092,12.));
#174515=CARTESIAN_POINT('Ctrl Pts',(70.438180810725,5.11999479630215,0.));
#174516=CARTESIAN_POINT('Ctrl Pts',(70.438180810725,5.11999479630215,12.));
#174517=CARTESIAN_POINT('Ctrl Pts',(70.4176156101633,5.12454539205347,0.));
#174518=CARTESIAN_POINT('Ctrl Pts',(70.4176156101633,5.12454539205347,12.));
#174519=CARTESIAN_POINT('Ctrl Pts',(70.3970944229885,5.12906381499486,0.));
#174520=CARTESIAN_POINT('Ctrl Pts',(70.3970944229885,5.12906381499486,12.));
#174521=CARTESIAN_POINT('Ctrl Pts',(70.3766174264786,5.13355010728591,0.));
#174522=CARTESIAN_POINT('Ctrl Pts',(70.3766174264786,5.13355010728591,12.));
#174523=CARTESIAN_POINT('Ctrl Pts',(70.3561847991725,5.13800431148911,0.));
#174524=CARTESIAN_POINT('Ctrl Pts',(70.3561847991725,5.13800431148911,12.));
#174525=CARTESIAN_POINT('Ctrl Pts',(70.3357967211782,5.14242647063468,0.));
#174526=CARTESIAN_POINT('Ctrl Pts',(70.3357967211782,5.14242647063468,12.));
#174527=CARTESIAN_POINT('Ctrl Pts',(70.31545337467,5.14681662833054,0.));
#174528=CARTESIAN_POINT('Ctrl Pts',(70.31545337467,5.14681662833054,12.));
#174529=CARTESIAN_POINT('Ctrl Pts',(70.2951549435469,5.15117482869225,0.));
#174530=CARTESIAN_POINT('Ctrl Pts',(70.2951549435469,5.15117482869225,12.));
#174531=CARTESIAN_POINT('Ctrl Pts',(70.2749016125073,5.15550111614838,0.));
#174532=CARTESIAN_POINT('Ctrl Pts',(70.2749016125073,5.15550111614838,12.));
#174533=CARTESIAN_POINT('Ctrl Pts',(70.2546935662719,5.15979553528201,0.));
#174534=CARTESIAN_POINT('Ctrl Pts',(70.2546935662719,5.15979553528201,12.));
#174535=CARTESIAN_POINT('Ctrl Pts',(70.2345309887864,5.16405813066995,0.));
#174536=CARTESIAN_POINT('Ctrl Pts',(70.2345309887864,5.16405813066995,12.));
#174537=CARTESIAN_POINT('Ctrl Pts',(70.2144140623004,5.1682889467014,0.));
#174538=CARTESIAN_POINT('Ctrl Pts',(70.2144140623004,5.1682889467014,12.));
#174539=CARTESIAN_POINT('Ctrl Pts',(70.1943429691214,5.1724880279342,0.));
#174540=CARTESIAN_POINT('Ctrl Pts',(70.1943429691214,5.1724880279342,12.));
#174541=CARTESIAN_POINT('Ctrl Pts',(70.1743178937102,5.176655419524,0.));
#174542=CARTESIAN_POINT('Ctrl Pts',(70.1743178937102,5.176655419524,12.));
#174543=CARTESIAN_POINT('Ctrl Pts',(70.1543390243882,5.18079116757659,0.));
#174544=CARTESIAN_POINT('Ctrl Pts',(70.1543390243882,5.18079116757659,12.));
#174545=CARTESIAN_POINT('Ctrl Pts',(70.1344065558106,5.18489531966235,0.));
#174546=CARTESIAN_POINT('Ctrl Pts',(70.1344065558106,5.18489531966235,12.));
#174547=CARTESIAN_POINT('Ctrl Pts',(70.1145206891833,5.18896792486523,0.));
#174548=CARTESIAN_POINT('Ctrl Pts',(70.1145206891833,5.18896792486523,12.));
#174549=CARTESIAN_POINT('Ctrl Pts',(70.0946816270957,5.19300903271544,0.));
#174550=CARTESIAN_POINT('Ctrl Pts',(70.0946816270957,5.19300903271544,12.));
#174551=CARTESIAN_POINT('Ctrl Pts',(70.0748895689716,5.19701869225515,0.));
#174552=CARTESIAN_POINT('Ctrl Pts',(70.0748895689716,5.19701869225515,12.));
#174553=CARTESIAN_POINT('Ctrl Pts',(70.0551447071106,5.20099695122678,0.));
#174554=CARTESIAN_POINT('Ctrl Pts',(70.0551447071106,5.20099695122678,12.));
#174555=CARTESIAN_POINT('Ctrl Pts',(70.0354472203604,5.20494385478084,0.));
#174556=CARTESIAN_POINT('Ctrl Pts',(70.0354472203604,5.20494385478084,12.));
#174557=CARTESIAN_POINT('Ctrl Pts',(70.0157972802255,5.20885944672915,0.));
#174558=CARTESIAN_POINT('Ctrl Pts',(70.0157972802255,5.20885944672915,12.));
#174559=CARTESIAN_POINT('Ctrl Pts',(69.996195063002,5.21274377203322,0.));
#174560=CARTESIAN_POINT('Ctrl Pts',(69.996195063002,5.21274377203322,12.));
#174561=CARTESIAN_POINT('Ctrl Pts',(69.9766407595385,5.21659687881139,0.));
#174562=CARTESIAN_POINT('Ctrl Pts',(69.9766407595385,5.21659687881139,12.));
#174563=CARTESIAN_POINT('Ctrl Pts',(69.9571345869996,5.22041882075627,0.));
#174564=CARTESIAN_POINT('Ctrl Pts',(69.9571345869996,5.22041882075627,12.));
#174565=CARTESIAN_POINT('Ctrl Pts',(69.9376767968951,5.22420965879808,0.));
#174566=CARTESIAN_POINT('Ctrl Pts',(69.9376767968951,5.22420965879808,12.));
#174567=CARTESIAN_POINT('Ctrl Pts',(69.9182676501892,5.22796945602603,0.));
#174568=CARTESIAN_POINT('Ctrl Pts',(69.9182676501892,5.22796945602603,12.));
#174569=CARTESIAN_POINT('Ctrl Pts',(69.8989073936606,5.23169827290452,0.));
#174570=CARTESIAN_POINT('Ctrl Pts',(69.8989073936606,5.23169827290452,12.));
#174571=CARTESIAN_POINT('Ctrl Pts',(69.8795962381676,5.23539616279715,0.));
#174572=CARTESIAN_POINT('Ctrl Pts',(69.8795962381676,5.23539616279715,12.));
#174573=CARTESIAN_POINT('Ctrl Pts',(69.8603343303016,5.23906316635141,0.));
#174574=CARTESIAN_POINT('Ctrl Pts',(69.8603343303016,5.23906316635141,12.));
#174575=CARTESIAN_POINT('Ctrl Pts',(69.8411217507931,5.24269931055076,0.));
#174576=CARTESIAN_POINT('Ctrl Pts',(69.8411217507931,5.24269931055076,12.));
#174577=CARTESIAN_POINT('Ctrl Pts',(69.8257911792542,5.24558355160221,0.));
#174578=CARTESIAN_POINT('Ctrl Pts',(69.8257911792542,5.24558355160221,12.));
#174579=CARTESIAN_POINT('Ctrl Pts',(69.8143154684447,5.24773285666674,0.));
#174580=CARTESIAN_POINT('Ctrl Pts',(69.8143154684447,5.24773285666674,12.));
#174581=CARTESIAN_POINT('Ctrl Pts',(69.8066748687863,5.24915955997537,0.));
#174582=CARTESIAN_POINT('Ctrl Pts',(69.8066748687863,5.24915955997537,12.));
#174583=CARTESIAN_POINT('Ctrl Pts',(69.8028570375097,5.24987136994592,0.));
#174584=CARTESIAN_POINT('Ctrl Pts',(69.8028570375097,5.24987136994592,12.));
#174585=CARTESIAN_POINT('Ctrl Pts',(69.8028570375097,5.24987136994592,12.));
#174586=CARTESIAN_POINT('Ctrl Pts',(69.8066748687863,5.24915955997537,12.));
#174587=CARTESIAN_POINT('Ctrl Pts',(69.8143154684447,5.24773285666674,12.));
#174588=CARTESIAN_POINT('Ctrl Pts',(69.8257911792542,5.24558355160221,12.));
#174589=CARTESIAN_POINT('Ctrl Pts',(69.8411217507931,5.24269931055076,12.));
#174590=CARTESIAN_POINT('Ctrl Pts',(69.8603343303016,5.23906316635141,12.));
#174591=CARTESIAN_POINT('Ctrl Pts',(69.8795962381676,5.23539616279715,12.));
#174592=CARTESIAN_POINT('Ctrl Pts',(69.8989073936606,5.23169827290452,12.));
#174593=CARTESIAN_POINT('Ctrl Pts',(69.9182676501892,5.22796945602603,12.));
#174594=CARTESIAN_POINT('Ctrl Pts',(69.9376767968951,5.22420965879808,12.));
#174595=CARTESIAN_POINT('Ctrl Pts',(69.9571345869996,5.22041882075627,12.));
#174596=CARTESIAN_POINT('Ctrl Pts',(69.9766407595385,5.21659687881139,12.));
#174597=CARTESIAN_POINT('Ctrl Pts',(69.996195063002,5.21274377203322,12.));
#174598=CARTESIAN_POINT('Ctrl Pts',(70.0157972802255,5.20885944672915,12.));
#174599=CARTESIAN_POINT('Ctrl Pts',(70.0354472203604,5.20494385478084,12.));
#174600=CARTESIAN_POINT('Ctrl Pts',(70.0551447071106,5.20099695122678,12.));
#174601=CARTESIAN_POINT('Ctrl Pts',(70.0748895689716,5.19701869225515,12.));
#174602=CARTESIAN_POINT('Ctrl Pts',(70.0946816270957,5.19300903271544,12.));
#174603=CARTESIAN_POINT('Ctrl Pts',(70.1145206891833,5.18896792486523,12.));
#174604=CARTESIAN_POINT('Ctrl Pts',(70.1344065558106,5.18489531966235,12.));
#174605=CARTESIAN_POINT('Ctrl Pts',(70.1543390243882,5.18079116757659,12.));
#174606=CARTESIAN_POINT('Ctrl Pts',(70.1743178937102,5.176655419524,12.));
#174607=CARTESIAN_POINT('Ctrl Pts',(70.1943429691214,5.1724880279342,12.));
#174608=CARTESIAN_POINT('Ctrl Pts',(70.2144140623004,5.1682889467014,12.));
#174609=CARTESIAN_POINT('Ctrl Pts',(70.2345309887864,5.16405813066995,12.));
#174610=CARTESIAN_POINT('Ctrl Pts',(70.2546935662719,5.15979553528201,12.));
#174611=CARTESIAN_POINT('Ctrl Pts',(70.2749016125073,5.15550111614838,12.));
#174612=CARTESIAN_POINT('Ctrl Pts',(70.2951549435469,5.15117482869225,12.));
#174613=CARTESIAN_POINT('Ctrl Pts',(70.31545337467,5.14681662833054,12.));
#174614=CARTESIAN_POINT('Ctrl Pts',(70.3357967211782,5.14242647063468,12.));
#174615=CARTESIAN_POINT('Ctrl Pts',(70.3561847991725,5.13800431148911,12.));
#174616=CARTESIAN_POINT('Ctrl Pts',(70.3766174264786,5.13355010728591,12.));
#174617=CARTESIAN_POINT('Ctrl Pts',(70.3970944229885,5.12906381499486,12.));
#174618=CARTESIAN_POINT('Ctrl Pts',(70.4176156101633,5.12454539205347,12.));
#174619=CARTESIAN_POINT('Ctrl Pts',(70.438180810725,5.11999479630215,12.));
#174620=CARTESIAN_POINT('Ctrl Pts',(70.4587898482946,5.1154119859092,12.));
#174621=CARTESIAN_POINT('Ctrl Pts',(70.4794425469799,5.11079691929193,12.));
#174622=CARTESIAN_POINT('Ctrl Pts',(70.5001387313963,5.10614955511643,12.));
#174623=CARTESIAN_POINT('Ctrl Pts',(70.5208782268482,5.10146985232929,12.));
#174624=CARTESIAN_POINT('Ctrl Pts',(70.5416608594526,5.09675777018183,12.));
#174625=CARTESIAN_POINT('Ctrl Pts',(70.5624864562841,5.09201326826146,12.));
#174626=CARTESIAN_POINT('Ctrl Pts',(70.5833548455043,5.08723630652291,12.));
#174627=CARTESIAN_POINT('Ctrl Pts',(70.6042658562951,5.08242684526704,12.));
#174628=CARTESIAN_POINT('Ctrl Pts',(70.6252193187892,5.07758484512311,12.));
#174629=CARTESIAN_POINT('Ctrl Pts',(70.6462150640009,5.07271026703351,12.));
#174630=CARTESIAN_POINT('Ctrl Pts',(70.6672529237431,5.06780307224053,12.));
#174631=CARTESIAN_POINT('Ctrl Pts',(70.6883327305755,5.06286322227797,12.));
#174632=CARTESIAN_POINT('Ctrl Pts',(70.7094543178416,5.05789067897041,12.));
#174633=CARTESIAN_POINT('Ctrl Pts',(70.7306175196856,5.05288540443478,12.));
#174634=CARTESIAN_POINT('Ctrl Pts',(70.7518221710715,5.04784736108351,12.));
#174635=CARTESIAN_POINT('Ctrl Pts',(70.7730681077997,5.04277651163357,12.));
#174636=CARTESIAN_POINT('Ctrl Pts',(70.7943551665071,5.03767281910484,12.));
#174637=CARTESIAN_POINT('Ctrl Pts',(70.8156831846493,5.03253624680941,12.));
#174638=CARTESIAN_POINT('Ctrl Pts',(70.8370520004844,5.02736675834692,12.));
#174639=CARTESIAN_POINT('Ctrl Pts',(70.8584614530517,5.02216431760061,12.));
#174640=CARTESIAN_POINT('Ctrl Pts',(70.8799113821449,5.01692888873793,12.));
#174641=CARTESIAN_POINT('Ctrl Pts',(70.9014016283123,5.01166043620574,12.));
#174642=CARTESIAN_POINT('Ctrl Pts',(70.9229320328588,5.00635892472518,12.));
#174643=CARTESIAN_POINT('Ctrl Pts',(70.9445024378439,5.0010243192904,12.));
#174644=CARTESIAN_POINT('Ctrl Pts',(70.9661126860773,4.99565658516906,12.));
#174645=CARTESIAN_POINT('Ctrl Pts',(70.9877626211112,4.99025568790653,12.));
#174646=CARTESIAN_POINT('Ctrl Pts',(71.0094520872375,4.98482159331852,12.));
#174647=CARTESIAN_POINT('Ctrl Pts',(71.031180929482,4.97935426748578,12.));
#174648=CARTESIAN_POINT('Ctrl Pts',(71.0529489935959,4.97385367675158,12.));
#174649=CARTESIAN_POINT('Ctrl Pts',(71.0747561260443,4.96831978772202,12.));
#174650=CARTESIAN_POINT('Ctrl Pts',(71.0966021739922,4.96275256726787,12.));
#174651=CARTESIAN_POINT('Ctrl Pts',(71.1184869853071,4.95715198251704,12.));
#174652=CARTESIAN_POINT('Ctrl Pts',(71.1404104085561,4.95151800085111,12.));
#174653=CARTESIAN_POINT('Ctrl Pts',(71.1623722929998,4.94585058990337,12.));
#174654=CARTESIAN_POINT('Ctrl Pts',(71.184372488583,4.94014971756097,12.));
#174655=CARTESIAN_POINT('Ctrl Pts',(71.206410845926,4.93441535196594,12.));
#174656=CARTESIAN_POINT('Ctrl Pts',(71.2284872163248,4.92864746150711,12.));
#174657=CARTESIAN_POINT('Ctrl Pts',(71.2506014517457,4.92284601481711,12.));
#174658=CARTESIAN_POINT('Ctrl Pts',(71.27275340482,4.91701098077042,12.));
#174659=CARTESIAN_POINT('Ctrl Pts',(71.2949429288319,4.91114232848623,12.));
#174660=CARTESIAN_POINT('Ctrl Pts',(71.3171698777124,4.90524002732806,12.));
#174661=CARTESIAN_POINT('Ctrl Pts',(71.3394341060396,4.899304046896,12.));
#174662=CARTESIAN_POINT('Ctrl Pts',(71.3617354690342,4.89333435702424,12.));
#174663=CARTESIAN_POINT('Ctrl Pts',(71.3840738225547,4.88733092777965,12.));
#174664=CARTESIAN_POINT('Ctrl Pts',(71.4064490230857,4.88129372946525,12.));
#174665=CARTESIAN_POINT('Ctrl Pts',(71.4288609277324,4.87522273261881,12.));
#174666=CARTESIAN_POINT('Ctrl Pts',(71.4513093942216,4.86911790800534,12.));
#174667=CARTESIAN_POINT('Ctrl Pts',(71.4737942808971,4.86297922661499,12.));
#174668=CARTESIAN_POINT('Ctrl Pts',(71.4963154467128,4.85680665966185,12.));
#174669=CARTESIAN_POINT('Ctrl Pts',(71.5188727512231,4.85060017858787,12.));
#174670=CARTESIAN_POINT('Ctrl Pts',(71.5414660545778,4.84435975506057,12.));
#174671=CARTESIAN_POINT('Ctrl Pts',(71.5640952175239,4.8380853609659,12.));
#174672=CARTESIAN_POINT('Ctrl Pts',(71.5867601014008,4.83177696840641,12.));
#174673=CARTESIAN_POINT('Ctrl Pts',(71.6094605681353,4.82543454970021,12.));
#174674=CARTESIAN_POINT('Ctrl Pts',(71.6321964802297,4.81905807738542,12.));
#174675=CARTESIAN_POINT('Ctrl Pts',(71.6549677007582,4.81264752421714,12.));
#174676=CARTESIAN_POINT('Ctrl Pts',(71.6777740933687,4.80620286316076,12.));
#174677=CARTESIAN_POINT('Ctrl Pts',(71.7006155222764,4.79972406739011,12.));
#174678=CARTESIAN_POINT('Ctrl Pts',(71.723491852261,4.79321111028676,12.));
#174679=CARTESIAN_POINT('Ctrl Pts',(71.7464029486563,4.78666396544459,12.));
#174680=CARTESIAN_POINT('Ctrl Pts',(71.769348677346,4.78008260666651,12.));
#174681=CARTESIAN_POINT('Ctrl Pts',(71.7923289047643,4.77346700795792,12.));
#174682=CARTESIAN_POINT('Ctrl Pts',(71.8153434978923,4.76681714352503,12.));
#174683=CARTESIAN_POINT('Ctrl Pts',(71.8383923242531,4.7601329877742,12.));
#174684=CARTESIAN_POINT('Ctrl Pts',(71.8614752519008,4.7534145153167,12.));
#174685=CARTESIAN_POINT('Ctrl Pts',(71.8845921494189,4.74666170096548,12.));
#174686=CARTESIAN_POINT('Ctrl Pts',(71.9077428859212,4.73987451972864,12.));
#174687=CARTESIAN_POINT('Ctrl Pts',(71.9309273310471,4.73305294680786,12.));
#174688=CARTESIAN_POINT('Ctrl Pts',(71.9541453549579,4.72619695759774,12.));
#174689=CARTESIAN_POINT('Ctrl Pts',(71.9773968283259,4.71930652769071,12.));
#174690=CARTESIAN_POINT('Ctrl Pts',(72.0006816223325,4.71238163287397,12.));
#174691=CARTESIAN_POINT('Ctrl Pts',(72.0239996086686,4.70542224912301,12.));
#174692=CARTESIAN_POINT('Ctrl Pts',(72.0473506595318,4.69842835259993,12.));
#174693=CARTESIAN_POINT('Ctrl Pts',(72.0707346476213,4.69139991965284,12.));
#174694=CARTESIAN_POINT('Ctrl Pts',(72.0941514461287,4.68433692682069,12.));
#174695=CARTESIAN_POINT('Ctrl Pts',(72.1176009287351,4.67723935083095,12.));
#174696=CARTESIAN_POINT('Ctrl Pts',(72.1410829696128,4.67010716859286,12.));
#174697=CARTESIAN_POINT('Ctrl Pts',(72.1645974434216,4.6629403571957,12.));
#174698=CARTESIAN_POINT('Ctrl Pts',(72.1881442253053,4.65573889390823,12.));
#174699=CARTESIAN_POINT('Ctrl Pts',(72.2117231908822,4.64850275618324,12.));
#174700=CARTESIAN_POINT('Ctrl Pts',(72.2353342162417,4.64123192165628,12.));
#174701=CARTESIAN_POINT('Ctrl Pts',(72.2589771779456,4.63392636813844,12.));
#174702=CARTESIAN_POINT('Ctrl Pts',(72.2826519530259,4.62658607361466,12.));
#174703=CARTESIAN_POINT('Ctrl Pts',(72.3063584189807,4.61921101624292,12.));
#174704=CARTESIAN_POINT('Ctrl Pts',(72.3300964537658,4.61180117435863,12.));
#174705=CARTESIAN_POINT('Ctrl Pts',(72.3538659357913,4.60435652647454,12.));
#174706=CARTESIAN_POINT('Ctrl Pts',(72.3776667439227,4.5968770512733,12.));
#174707=CARTESIAN_POINT('Ctrl Pts',(72.401498757478,4.58936272760545,12.));
#174708=CARTESIAN_POINT('Ctrl Pts',(72.4253618562252,4.58181353448852,12.));
#174709=CARTESIAN_POINT('Ctrl Pts',(72.4492559203745,4.57422945111103,12.));
#174710=CARTESIAN_POINT('Ctrl Pts',(72.4731808305728,4.56661045683376,12.));
#174711=CARTESIAN_POINT('Ctrl Pts',(72.4971364679068,4.55895653118221,12.));
#174712=CARTESIAN_POINT('Ctrl Pts',(72.5211227139001,4.55126765384405,12.));
#174713=CARTESIAN_POINT('Ctrl Pts',(72.5451394505103,4.54354380466823,12.));
#174714=CARTESIAN_POINT('Ctrl Pts',(72.5691865601223,4.535784963668,12.));
#174715=CARTESIAN_POINT('Ctrl Pts',(72.5932639255409,4.52799111102392,12.));
#174716=CARTESIAN_POINT('Ctrl Pts',(72.6173714299942,4.52016222707638,12.));
#174717=CARTESIAN_POINT('Ctrl Pts',(72.6415089571321,4.51229829232264,12.));
#174718=CARTESIAN_POINT('Ctrl Pts',(72.6656763910241,4.50439928741604,12.));
#174719=CARTESIAN_POINT('Ctrl Pts',(72.6898736161542,4.49646519316813,12.));
#174720=CARTESIAN_POINT('Ctrl Pts',(72.714100517414,4.48849599055338,12.));
#174721=CARTESIAN_POINT('Ctrl Pts',(72.738356980103,4.48049166070206,12.));
#174722=CARTESIAN_POINT('Ctrl Pts',(72.7626428899281,4.4724521848961,12.));
#174723=CARTESIAN_POINT('Ctrl Pts',(72.7869581329994,4.46437754456793,12.));
#174724=CARTESIAN_POINT('Ctrl Pts',(72.8113025958262,4.45626772130147,12.));
#174725=CARTESIAN_POINT('Ctrl Pts',(72.8356761653069,4.44812269683738,12.));
#174726=CARTESIAN_POINT('Ctrl Pts',(72.8600787287318,4.43994245306819,12.));
#174727=CARTESIAN_POINT('Ctrl Pts',(72.8845101737855,4.4317269720335,12.));
#174728=CARTESIAN_POINT('Ctrl Pts',(72.9089703885462,4.42347623591942,12.));
#174729=CARTESIAN_POINT('Ctrl Pts',(72.9334592614829,4.41519022705922,12.));
#174730=CARTESIAN_POINT('Ctrl Pts',(72.95797668145,4.40686892793958,12.));
#174731=CARTESIAN_POINT('Ctrl Pts',(72.9825225376846,4.39851232119723,12.));
#174732=CARTESIAN_POINT('Ctrl Pts',(73.007096719804,4.3901203896114,12.));
#174733=CARTESIAN_POINT('Ctrl Pts',(73.0316991177993,4.38169311610151,12.));
#174734=CARTESIAN_POINT('Ctrl Pts',(73.0563296220299,4.37323048372608,12.));
#174735=CARTESIAN_POINT('Ctrl Pts',(73.0809881232103,4.36473247568642,12.));
#174736=CARTESIAN_POINT('Ctrl Pts',(73.1056745124087,4.3561990753272,12.));
#174737=CARTESIAN_POINT('Ctrl Pts',(73.130388681059,4.34763026613158,12.));
#174738=CARTESIAN_POINT('Ctrl Pts',(73.1551305209685,4.33902603172141,12.));
#174739=CARTESIAN_POINT('Ctrl Pts',(73.1798999243235,4.33038635585877,12.));
#174740=CARTESIAN_POINT('Ctrl Pts',(73.204696783694,4.32171122245214,12.));
#174741=CARTESIAN_POINT('Ctrl Pts',(73.2295209920334,4.31300061556098,12.));
#174742=CARTESIAN_POINT('Ctrl Pts',(73.2543724426577,4.30425451938231,12.));
#174743=CARTESIAN_POINT('Ctrl Pts',(73.2792510292253,4.29547291824287,12.));
#174744=CARTESIAN_POINT('Ctrl Pts',(73.3041566457135,4.28665579659302,12.));
#174745=CARTESIAN_POINT('Ctrl Pts',(73.3290891863949,4.2778031390039,12.));
#174746=CARTESIAN_POINT('Ctrl Pts',(73.3540485458065,4.268914930167,12.));
#174747=CARTESIAN_POINT('Ctrl Pts',(73.3790346187938,4.259991154899,12.));
#174748=CARTESIAN_POINT('Ctrl Pts',(73.4040473005592,4.25103179814887,12.));
#174749=CARTESIAN_POINT('Ctrl Pts',(73.4290864867101,4.24203684500939,12.));
#174750=CARTESIAN_POINT('Ctrl Pts',(73.4541520732948,4.23300628072759,12.));
#174751=CARTESIAN_POINT('Ctrl Pts',(73.4792439568633,4.22394009072757,12.));
#174752=CARTESIAN_POINT('Ctrl Pts',(73.5043620344116,4.21483826059441,12.));
#174753=CARTESIAN_POINT('Ctrl Pts',(73.5295062032628,4.2057007760373,12.));
#174754=CARTESIAN_POINT('Ctrl Pts',(73.5546763609572,4.19652762286128,12.));
#174755=CARTESIAN_POINT('Ctrl Pts',(73.5798724051519,4.18731878694237,12.));
#174756=CARTESIAN_POINT('Ctrl Pts',(73.6050942334768,4.17807425419813,12.));
#174757=CARTESIAN_POINT('Ctrl Pts',(73.6303417435251,4.16879401058781,12.));
#174758=CARTESIAN_POINT('Ctrl Pts',(73.6556148331489,4.15947804217784,12.));
#174759=CARTESIAN_POINT('Ctrl Pts',(73.6809134006897,4.15012633519724,12.));
#174760=CARTESIAN_POINT('Ctrl Pts',(73.7062373452342,4.14073887610154,12.));
#174761=CARTESIAN_POINT('Ctrl Pts',(73.7315865668522,4.13131565163579,12.));
#174762=CARTESIAN_POINT('Ctrl Pts',(73.7569609668528,4.12185664890557,12.));
#174763=CARTESIAN_POINT('Ctrl Pts',(73.7823604472159,4.11236185522788,12.));
#174764=CARTESIAN_POINT('Ctrl Pts',(73.8077849100342,4.1028312579873,12.));
#174765=CARTESIAN_POINT('Ctrl Pts',(73.8332342568989,4.09326484448233,12.));
#174766=CARTESIAN_POINT('Ctrl Pts',(73.8587083884191,4.08366260180675,12.));
#174767=CARTESIAN_POINT('Ctrl Pts',(73.8842072034008,4.07402451665245,12.));
#174768=CARTESIAN_POINT('Ctrl Pts',(73.9097305995115,4.06435057547325,12.));
#174769=CARTESIAN_POINT('Ctrl Pts',(73.9352784747608,4.05464076484752,12.));
#174770=CARTESIAN_POINT('Ctrl Pts',(73.9608507287909,4.04489507179958,12.));
#174771=CARTESIAN_POINT('Ctrl Pts',(73.9864472641033,4.0351134841066,12.));
#174772=CARTESIAN_POINT('Ctrl Pts',(74.012067987646,4.02529599070095,12.));
#174773=CARTESIAN_POINT('Ctrl Pts',(74.0377128111863,4.01544258176711,12.));
#174774=CARTESIAN_POINT('Ctrl Pts',(74.059715978211,4.00696550627364,12.));
#174775=CARTESIAN_POINT('Ctrl Pts',(74.0765982943677,4.00044689711983,12.));
#174776=CARTESIAN_POINT('Ctrl Pts',(74.0883491449955,3.9959026674699,12.));
#174777=CARTESIAN_POINT('Ctrl Pts',(74.094961539962,3.99334334445527,12.));
#174778=CARTESIAN_POINT('Ctrl Pts',(74.0964320766208,3.9927740649087,12.));
#174779=CARTESIAN_POINT('Ctrl Pts',(74.0964320766207,3.99277406490872,0.));
#174780=CARTESIAN_POINT('Ctrl Pts',(74.0949615399619,3.99334334445528,0.));
#174781=CARTESIAN_POINT('Ctrl Pts',(74.0883491449955,3.99590266746991,0.));
#174782=CARTESIAN_POINT('Ctrl Pts',(74.0765982943677,4.00044689711983,0.));
#174783=CARTESIAN_POINT('Ctrl Pts',(74.0597159782109,4.00696550627365,0.));
#174784=CARTESIAN_POINT('Ctrl Pts',(74.0377128111863,4.01544258176711,0.));
#174785=CARTESIAN_POINT('Ctrl Pts',(74.012067987646,4.02529599070095,0.));
#174786=CARTESIAN_POINT('Ctrl Pts',(73.9864472641033,4.0351134841066,0.));
#174787=CARTESIAN_POINT('Ctrl Pts',(73.9608507287909,4.04489507179958,0.));
#174788=CARTESIAN_POINT('Ctrl Pts',(73.9352784747608,4.05464076484752,0.));
#174789=CARTESIAN_POINT('Ctrl Pts',(73.9097305995115,4.06435057547325,0.));
#174790=CARTESIAN_POINT('Ctrl Pts',(73.8842072034008,4.07402451665245,0.));
#174791=CARTESIAN_POINT('Ctrl Pts',(73.8587083884191,4.08366260180675,0.));
#174792=CARTESIAN_POINT('Ctrl Pts',(73.8332342568989,4.09326484448233,0.));
#174793=CARTESIAN_POINT('Ctrl Pts',(73.8077849100342,4.1028312579873,0.));
#174794=CARTESIAN_POINT('Ctrl Pts',(73.7823604472159,4.11236185522788,0.));
#174795=CARTESIAN_POINT('Ctrl Pts',(73.7569609668528,4.12185664890557,0.));
#174796=CARTESIAN_POINT('Ctrl Pts',(73.7315865668522,4.13131565163579,0.));
#174797=CARTESIAN_POINT('Ctrl Pts',(73.7062373452342,4.14073887610154,0.));
#174798=CARTESIAN_POINT('Ctrl Pts',(73.6809134006897,4.15012633519724,0.));
#174799=CARTESIAN_POINT('Ctrl Pts',(73.6556148331489,4.15947804217784,0.));
#174800=CARTESIAN_POINT('Ctrl Pts',(73.6303417435251,4.16879401058781,0.));
#174801=CARTESIAN_POINT('Ctrl Pts',(73.6050942334768,4.17807425419813,0.));
#174802=CARTESIAN_POINT('Ctrl Pts',(73.5798724051519,4.18731878694237,0.));
#174803=CARTESIAN_POINT('Ctrl Pts',(73.5546763609572,4.19652762286128,0.));
#174804=CARTESIAN_POINT('Ctrl Pts',(73.5295062032628,4.2057007760373,0.));
#174805=CARTESIAN_POINT('Ctrl Pts',(73.5043620344116,4.21483826059441,0.));
#174806=CARTESIAN_POINT('Ctrl Pts',(73.4792439568633,4.22394009072757,0.));
#174807=CARTESIAN_POINT('Ctrl Pts',(73.4541520732948,4.23300628072759,0.));
#174808=CARTESIAN_POINT('Ctrl Pts',(73.4290864867101,4.24203684500939,0.));
#174809=CARTESIAN_POINT('Ctrl Pts',(73.4040473005592,4.25103179814887,0.));
#174810=CARTESIAN_POINT('Ctrl Pts',(73.3790346187938,4.259991154899,0.));
#174811=CARTESIAN_POINT('Ctrl Pts',(73.3540485458065,4.268914930167,0.));
#174812=CARTESIAN_POINT('Ctrl Pts',(73.3290891863949,4.2778031390039,0.));
#174813=CARTESIAN_POINT('Ctrl Pts',(73.3041566457135,4.28665579659302,0.));
#174814=CARTESIAN_POINT('Ctrl Pts',(73.2792510292253,4.29547291824287,0.));
#174815=CARTESIAN_POINT('Ctrl Pts',(73.2543724426577,4.30425451938231,0.));
#174816=CARTESIAN_POINT('Ctrl Pts',(73.2295209920334,4.31300061556098,0.));
#174817=CARTESIAN_POINT('Ctrl Pts',(73.204696783694,4.32171122245214,0.));
#174818=CARTESIAN_POINT('Ctrl Pts',(73.1798999243235,4.33038635585877,0.));
#174819=CARTESIAN_POINT('Ctrl Pts',(73.1551305209685,4.33902603172141,0.));
#174820=CARTESIAN_POINT('Ctrl Pts',(73.130388681059,4.34763026613158,0.));
#174821=CARTESIAN_POINT('Ctrl Pts',(73.1056745124087,4.3561990753272,0.));
#174822=CARTESIAN_POINT('Ctrl Pts',(73.0809881232103,4.36473247568642,0.));
#174823=CARTESIAN_POINT('Ctrl Pts',(73.0563296220299,4.37323048372608,0.));
#174824=CARTESIAN_POINT('Ctrl Pts',(73.0316991177993,4.38169311610151,0.));
#174825=CARTESIAN_POINT('Ctrl Pts',(73.007096719804,4.3901203896114,0.));
#174826=CARTESIAN_POINT('Ctrl Pts',(72.9825225376846,4.39851232119723,0.));
#174827=CARTESIAN_POINT('Ctrl Pts',(72.95797668145,4.40686892793958,0.));
#174828=CARTESIAN_POINT('Ctrl Pts',(72.9334592614829,4.41519022705922,0.));
#174829=CARTESIAN_POINT('Ctrl Pts',(72.9089703885462,4.42347623591942,0.));
#174830=CARTESIAN_POINT('Ctrl Pts',(72.8845101737855,4.4317269720335,0.));
#174831=CARTESIAN_POINT('Ctrl Pts',(72.8600787287318,4.43994245306819,0.));
#174832=CARTESIAN_POINT('Ctrl Pts',(72.8356761653069,4.44812269683738,0.));
#174833=CARTESIAN_POINT('Ctrl Pts',(72.8113025958262,4.45626772130147,0.));
#174834=CARTESIAN_POINT('Ctrl Pts',(72.7869581329994,4.46437754456793,0.));
#174835=CARTESIAN_POINT('Ctrl Pts',(72.7626428899281,4.4724521848961,0.));
#174836=CARTESIAN_POINT('Ctrl Pts',(72.738356980103,4.48049166070206,0.));
#174837=CARTESIAN_POINT('Ctrl Pts',(72.714100517414,4.48849599055338,0.));
#174838=CARTESIAN_POINT('Ctrl Pts',(72.6898736161542,4.49646519316813,0.));
#174839=CARTESIAN_POINT('Ctrl Pts',(72.6656763910241,4.50439928741604,0.));
#174840=CARTESIAN_POINT('Ctrl Pts',(72.6415089571321,4.51229829232264,0.));
#174841=CARTESIAN_POINT('Ctrl Pts',(72.6173714299942,4.52016222707638,0.));
#174842=CARTESIAN_POINT('Ctrl Pts',(72.5932639255409,4.52799111102392,0.));
#174843=CARTESIAN_POINT('Ctrl Pts',(72.5691865601223,4.535784963668,0.));
#174844=CARTESIAN_POINT('Ctrl Pts',(72.5451394505103,4.54354380466823,0.));
#174845=CARTESIAN_POINT('Ctrl Pts',(72.5211227139001,4.55126765384405,0.));
#174846=CARTESIAN_POINT('Ctrl Pts',(72.4971364679068,4.55895653118221,0.));
#174847=CARTESIAN_POINT('Ctrl Pts',(72.4731808305728,4.56661045683376,0.));
#174848=CARTESIAN_POINT('Ctrl Pts',(72.4492559203745,4.57422945111103,0.));
#174849=CARTESIAN_POINT('Ctrl Pts',(72.4253618562252,4.58181353448852,0.));
#174850=CARTESIAN_POINT('Ctrl Pts',(72.401498757478,4.58936272760545,0.));
#174851=CARTESIAN_POINT('Ctrl Pts',(72.3776667439227,4.5968770512733,0.));
#174852=CARTESIAN_POINT('Ctrl Pts',(72.3538659357913,4.60435652647454,0.));
#174853=CARTESIAN_POINT('Ctrl Pts',(72.3300964537658,4.61180117435863,0.));
#174854=CARTESIAN_POINT('Ctrl Pts',(72.3063584189807,4.61921101624292,0.));
#174855=CARTESIAN_POINT('Ctrl Pts',(72.2826519530259,4.62658607361466,0.));
#174856=CARTESIAN_POINT('Ctrl Pts',(72.2589771779456,4.63392636813844,0.));
#174857=CARTESIAN_POINT('Ctrl Pts',(72.2353342162417,4.64123192165628,0.));
#174858=CARTESIAN_POINT('Ctrl Pts',(72.2117231908822,4.64850275618324,0.));
#174859=CARTESIAN_POINT('Ctrl Pts',(72.1881442253053,4.65573889390823,0.));
#174860=CARTESIAN_POINT('Ctrl Pts',(72.1645974434216,4.6629403571957,0.));
#174861=CARTESIAN_POINT('Ctrl Pts',(72.1410829696128,4.67010716859286,0.));
#174862=CARTESIAN_POINT('Ctrl Pts',(72.1176009287351,4.67723935083095,0.));
#174863=CARTESIAN_POINT('Ctrl Pts',(72.0941514461287,4.68433692682069,0.));
#174864=CARTESIAN_POINT('Ctrl Pts',(72.0707346476213,4.69139991965284,0.));
#174865=CARTESIAN_POINT('Ctrl Pts',(72.0473506595318,4.69842835259993,0.));
#174866=CARTESIAN_POINT('Ctrl Pts',(72.0239996086686,4.70542224912301,0.));
#174867=CARTESIAN_POINT('Ctrl Pts',(72.0006816223325,4.71238163287397,0.));
#174868=CARTESIAN_POINT('Ctrl Pts',(71.9773968283259,4.71930652769071,0.));
#174869=CARTESIAN_POINT('Ctrl Pts',(71.9541453549579,4.72619695759774,0.));
#174870=CARTESIAN_POINT('Ctrl Pts',(71.9309273310471,4.73305294680786,0.));
#174871=CARTESIAN_POINT('Ctrl Pts',(71.9077428859212,4.73987451972864,0.));
#174872=CARTESIAN_POINT('Ctrl Pts',(71.8845921494189,4.74666170096548,0.));
#174873=CARTESIAN_POINT('Ctrl Pts',(71.8614752519008,4.7534145153167,0.));
#174874=CARTESIAN_POINT('Ctrl Pts',(71.8383923242531,4.7601329877742,0.));
#174875=CARTESIAN_POINT('Ctrl Pts',(71.8153434978923,4.76681714352503,0.));
#174876=CARTESIAN_POINT('Ctrl Pts',(71.7923289047643,4.77346700795792,0.));
#174877=CARTESIAN_POINT('Ctrl Pts',(71.769348677346,4.78008260666651,0.));
#174878=CARTESIAN_POINT('Ctrl Pts',(71.7464029486563,4.78666396544459,0.));
#174879=CARTESIAN_POINT('Ctrl Pts',(71.723491852261,4.79321111028676,0.));
#174880=CARTESIAN_POINT('Ctrl Pts',(71.7006155222764,4.79972406739011,0.));
#174881=CARTESIAN_POINT('Ctrl Pts',(71.6777740933687,4.80620286316076,0.));
#174882=CARTESIAN_POINT('Ctrl Pts',(71.6549677007582,4.81264752421714,0.));
#174883=CARTESIAN_POINT('Ctrl Pts',(71.6321964802297,4.81905807738542,0.));
#174884=CARTESIAN_POINT('Ctrl Pts',(71.6094605681353,4.82543454970021,0.));
#174885=CARTESIAN_POINT('Ctrl Pts',(71.5867601014008,4.83177696840641,0.));
#174886=CARTESIAN_POINT('Ctrl Pts',(71.5640952175239,4.8380853609659,0.));
#174887=CARTESIAN_POINT('Ctrl Pts',(71.5414660545778,4.84435975506057,0.));
#174888=CARTESIAN_POINT('Ctrl Pts',(71.5188727512231,4.85060017858787,0.));
#174889=CARTESIAN_POINT('Ctrl Pts',(71.4963154467128,4.85680665966185,0.));
#174890=CARTESIAN_POINT('Ctrl Pts',(71.4737942808971,4.86297922661499,0.));
#174891=CARTESIAN_POINT('Ctrl Pts',(71.4513093942216,4.86911790800534,0.));
#174892=CARTESIAN_POINT('Ctrl Pts',(71.4288609277324,4.87522273261881,0.));
#174893=CARTESIAN_POINT('Ctrl Pts',(71.4064490230857,4.88129372946525,0.));
#174894=CARTESIAN_POINT('Ctrl Pts',(71.3840738225547,4.88733092777965,0.));
#174895=CARTESIAN_POINT('Ctrl Pts',(71.3617354690342,4.89333435702424,0.));
#174896=CARTESIAN_POINT('Ctrl Pts',(71.3394341060396,4.899304046896,0.));
#174897=CARTESIAN_POINT('Ctrl Pts',(71.3171698777124,4.90524002732806,0.));
#174898=CARTESIAN_POINT('Ctrl Pts',(71.2949429288319,4.91114232848623,0.));
#174899=CARTESIAN_POINT('Ctrl Pts',(71.27275340482,4.91701098077042,0.));
#174900=CARTESIAN_POINT('Ctrl Pts',(71.2506014517457,4.92284601481711,0.));
#174901=CARTESIAN_POINT('Ctrl Pts',(71.2284872163248,4.92864746150711,0.));
#174902=CARTESIAN_POINT('Ctrl Pts',(71.206410845926,4.93441535196594,0.));
#174903=CARTESIAN_POINT('Ctrl Pts',(71.184372488583,4.94014971756097,0.));
#174904=CARTESIAN_POINT('Ctrl Pts',(71.1623722929998,4.94585058990337,0.));
#174905=CARTESIAN_POINT('Ctrl Pts',(71.1404104085561,4.95151800085111,0.));
#174906=CARTESIAN_POINT('Ctrl Pts',(71.1184869853071,4.95715198251704,0.));
#174907=CARTESIAN_POINT('Ctrl Pts',(71.0966021739922,4.96275256726787,0.));
#174908=CARTESIAN_POINT('Ctrl Pts',(71.0747561260443,4.96831978772202,0.));
#174909=CARTESIAN_POINT('Ctrl Pts',(71.0529489935959,4.97385367675158,0.));
#174910=CARTESIAN_POINT('Ctrl Pts',(71.031180929482,4.97935426748578,0.));
#174911=CARTESIAN_POINT('Ctrl Pts',(71.0094520872375,4.98482159331852,0.));
#174912=CARTESIAN_POINT('Ctrl Pts',(70.9877626211112,4.99025568790653,0.));
#174913=CARTESIAN_POINT('Ctrl Pts',(70.9661126860773,4.99565658516906,0.));
#174914=CARTESIAN_POINT('Ctrl Pts',(70.9445024378439,5.0010243192904,0.));
#174915=CARTESIAN_POINT('Ctrl Pts',(70.9229320328588,5.00635892472518,0.));
#174916=CARTESIAN_POINT('Ctrl Pts',(70.9014016283123,5.01166043620574,0.));
#174917=CARTESIAN_POINT('Ctrl Pts',(70.8799113821449,5.01692888873793,0.));
#174918=CARTESIAN_POINT('Ctrl Pts',(70.8584614530517,5.02216431760061,0.));
#174919=CARTESIAN_POINT('Ctrl Pts',(70.8370520004844,5.02736675834692,0.));
#174920=CARTESIAN_POINT('Ctrl Pts',(70.8156831846493,5.03253624680941,0.));
#174921=CARTESIAN_POINT('Ctrl Pts',(70.7943551665071,5.03767281910484,0.));
#174922=CARTESIAN_POINT('Ctrl Pts',(70.7730681077997,5.04277651163357,0.));
#174923=CARTESIAN_POINT('Ctrl Pts',(70.7518221710715,5.04784736108351,0.));
#174924=CARTESIAN_POINT('Ctrl Pts',(70.7306175196856,5.05288540443478,0.));
#174925=CARTESIAN_POINT('Ctrl Pts',(70.7094543178416,5.05789067897041,0.));
#174926=CARTESIAN_POINT('Ctrl Pts',(70.6883327305755,5.06286322227797,0.));
#174927=CARTESIAN_POINT('Ctrl Pts',(70.6672529237431,5.06780307224053,0.));
#174928=CARTESIAN_POINT('Ctrl Pts',(70.6462150640009,5.07271026703351,0.));
#174929=CARTESIAN_POINT('Ctrl Pts',(70.6252193187892,5.07758484512311,0.));
#174930=CARTESIAN_POINT('Ctrl Pts',(70.6042658562951,5.08242684526704,0.));
#174931=CARTESIAN_POINT('Ctrl Pts',(70.5833548455043,5.08723630652291,0.));
#174932=CARTESIAN_POINT('Ctrl Pts',(70.5624864562841,5.09201326826146,0.));
#174933=CARTESIAN_POINT('Ctrl Pts',(70.5416608594526,5.09675777018183,0.));
#174934=CARTESIAN_POINT('Ctrl Pts',(70.5208782268482,5.10146985232929,0.));
#174935=CARTESIAN_POINT('Ctrl Pts',(70.5001387313963,5.10614955511643,0.));
#174936=CARTESIAN_POINT('Ctrl Pts',(70.4794425469799,5.11079691929193,0.));
#174937=CARTESIAN_POINT('Ctrl Pts',(70.4587898482946,5.1154119859092,0.));
#174938=CARTESIAN_POINT('Ctrl Pts',(70.438180810725,5.11999479630215,0.));
#174939=CARTESIAN_POINT('Ctrl Pts',(70.4176156101633,5.12454539205347,0.));
#174940=CARTESIAN_POINT('Ctrl Pts',(70.3970944229885,5.12906381499486,0.));
#174941=CARTESIAN_POINT('Ctrl Pts',(70.3766174264786,5.13355010728591,0.));
#174942=CARTESIAN_POINT('Ctrl Pts',(70.3561847991725,5.13800431148911,0.));
#174943=CARTESIAN_POINT('Ctrl Pts',(70.3357967211782,5.14242647063468,0.));
#174944=CARTESIAN_POINT('Ctrl Pts',(70.31545337467,5.14681662833054,0.));
#174945=CARTESIAN_POINT('Ctrl Pts',(70.2951549435469,5.15117482869225,0.));
#174946=CARTESIAN_POINT('Ctrl Pts',(70.2749016125073,5.15550111614838,0.));
#174947=CARTESIAN_POINT('Ctrl Pts',(70.2546935662719,5.15979553528201,0.));
#174948=CARTESIAN_POINT('Ctrl Pts',(70.2345309887864,5.16405813066995,0.));
#174949=CARTESIAN_POINT('Ctrl Pts',(70.2144140623004,5.1682889467014,0.));
#174950=CARTESIAN_POINT('Ctrl Pts',(70.1943429691214,5.1724880279342,0.));
#174951=CARTESIAN_POINT('Ctrl Pts',(70.1743178937102,5.176655419524,0.));
#174952=CARTESIAN_POINT('Ctrl Pts',(70.1543390243882,5.18079116757659,0.));
#174953=CARTESIAN_POINT('Ctrl Pts',(70.1344065558106,5.18489531966235,0.));
#174954=CARTESIAN_POINT('Ctrl Pts',(70.1145206891833,5.18896792486523,0.));
#174955=CARTESIAN_POINT('Ctrl Pts',(70.0946816270957,5.19300903271544,0.));
#174956=CARTESIAN_POINT('Ctrl Pts',(70.0748895689716,5.19701869225515,0.));
#174957=CARTESIAN_POINT('Ctrl Pts',(70.0551447071106,5.20099695122678,0.));
#174958=CARTESIAN_POINT('Ctrl Pts',(70.0354472203604,5.20494385478084,0.));
#174959=CARTESIAN_POINT('Ctrl Pts',(70.0157972802255,5.20885944672915,0.));
#174960=CARTESIAN_POINT('Ctrl Pts',(69.996195063002,5.21274377203322,0.));
#174961=CARTESIAN_POINT('Ctrl Pts',(69.9766407595385,5.21659687881139,0.));
#174962=CARTESIAN_POINT('Ctrl Pts',(69.9571345869996,5.22041882075627,0.));
#174963=CARTESIAN_POINT('Ctrl Pts',(69.9376767968951,5.22420965879808,0.));
#174964=CARTESIAN_POINT('Ctrl Pts',(69.9182676501892,5.22796945602603,0.));
#174965=CARTESIAN_POINT('Ctrl Pts',(69.8989073936606,5.23169827290452,0.));
#174966=CARTESIAN_POINT('Ctrl Pts',(69.8795962381676,5.23539616279715,0.));
#174967=CARTESIAN_POINT('Ctrl Pts',(69.8603343303016,5.23906316635141,0.));
#174968=CARTESIAN_POINT('Ctrl Pts',(69.8411217507931,5.24269931055076,0.));
#174969=CARTESIAN_POINT('Ctrl Pts',(69.8257911792542,5.24558355160221,0.));
#174970=CARTESIAN_POINT('Ctrl Pts',(69.8143154684447,5.24773285666674,0.));
#174971=CARTESIAN_POINT('Ctrl Pts',(69.8066748687863,5.24915955997537,0.));
#174972=CARTESIAN_POINT('Ctrl Pts',(69.8028570375097,5.24987136994592,0.));
#174973=CARTESIAN_POINT('Origin',(0.,0.,12.));
#174974=CARTESIAN_POINT('',(-90.,-1.10218211923262E-14,12.));
#174975=CARTESIAN_POINT('Origin',(0.,0.,12.));
#174976=CARTESIAN_POINT('Origin',(0.,0.,12.));
#174977=CARTESIAN_POINT('Origin',(0.,0.,0.));
#174978=CARTESIAN_POINT('Origin',(0.,0.,0.));
#174979=CARTESIAN_POINT('Origin',(0.,0.,0.));
#174980=CARTESIAN_POINT('',(-90.,-1.10218211923262E-14,0.));
#174981=CARTESIAN_POINT('',(-90.,-1.10218211923262E-14,0.));
#174982=CARTESIAN_POINT('',(-90.,-1.10218211923262E-14,0.));
#174983=CARTESIAN_POINT('Origin',(0.,0.,0.));
#174984=CARTESIAN_POINT('Origin',(0.,0.,0.));
#174985=CARTESIAN_POINT('',(0.,0.,0.));
#174986=CARTESIAN_POINT('Origin',(5.,3.,12.));
#174987=CARTESIAN_POINT('',(7.41619848709566,3.,0.));
#174988=CARTESIAN_POINT('',(7.41619848709566,3.,12.));
#174989=CARTESIAN_POINT('',(7.41619848709566,3.,0.));
#174990=CARTESIAN_POINT('',(11.,3.,0.));
#174991=CARTESIAN_POINT('',(2.5,3.,0.));
#174992=CARTESIAN_POINT('',(11.,3.,12.));
#174993=CARTESIAN_POINT('',(11.,3.,12.));
#174994=CARTESIAN_POINT('',(2.5,3.,12.));
#174995=CARTESIAN_POINT('Origin',(11.,-3.,12.));
#174996=CARTESIAN_POINT('',(7.41619848709566,-3.,12.));
#174997=CARTESIAN_POINT('',(7.41619848709566,-3.,0.));
#174998=CARTESIAN_POINT('',(7.41619848709566,-3.,0.));
#174999=CARTESIAN_POINT('',(11.,-3.,12.));
#175000=CARTESIAN_POINT('',(5.5,-3.,12.));
#175001=CARTESIAN_POINT('',(11.,-3.,0.));
#175002=CARTESIAN_POINT('',(11.,-3.,12.));
#175003=CARTESIAN_POINT('',(5.5,-3.,0.));
#175004=CARTESIAN_POINT('Origin',(11.,3.,12.));
#175005=CARTESIAN_POINT('',(11.,1.5,12.));
#175006=CARTESIAN_POINT('',(11.,1.5,0.));
#175007=CARTESIAN_POINT('Origin',(0.,0.,0.));
#175008=CARTESIAN_POINT('Origin',(0.,0.,12.));
#175009=CARTESIAN_POINT('Origin',(0.,0.,0.));
#175010=CARTESIAN_POINT('Origin',(0.,0.,12.));
#175011=CARTESIAN_POINT('',(22.4835757167854,-1.76341220531181,12.));
#175012=CARTESIAN_POINT('',(25.991588367311,-0.661312440730916,12.));
#175013=CARTESIAN_POINT('Ctrl Pts',(22.4835757167854,-1.76341220531181,
12.));
#175014=CARTESIAN_POINT('Ctrl Pts',(22.4835819929788,-1.76341415538792,
12.));
#175015=CARTESIAN_POINT('Ctrl Pts',(22.4836387052228,-1.76342064263638,
12.));
#175016=CARTESIAN_POINT('Ctrl Pts',(22.4838562517064,-1.7634381343466,12.));
#175017=CARTESIAN_POINT('Ctrl Pts',(22.4844112933125,-1.76347698284863,
12.));
#175018=CARTESIAN_POINT('Ctrl Pts',(22.4855446605991,-1.7635507604555,12.));
#175019=CARTESIAN_POINT('Ctrl Pts',(22.4871115206572,-1.76364784232927,
12.));
#175020=CARTESIAN_POINT('Ctrl Pts',(22.4890991659479,-1.76376424879469,
12.));
#175021=CARTESIAN_POINT('Ctrl Pts',(22.4914909094908,-1.76389475965715,
12.));
#175022=CARTESIAN_POINT('Ctrl Pts',(22.4942693792449,-1.76403393880317,
12.));
#175023=CARTESIAN_POINT('Ctrl Pts',(22.4974203063191,-1.76417731243484,
12.));
#175024=CARTESIAN_POINT('Ctrl Pts',(22.5009332677316,-1.76432160068739,
12.));
#175025=CARTESIAN_POINT('Ctrl Pts',(22.5047996391978,-1.76446408210366,
12.));
#175026=CARTESIAN_POINT('Ctrl Pts',(22.5090112700212,-1.76460218257314,
12.));
#175027=CARTESIAN_POINT('Ctrl Pts',(22.5135590569554,-1.7647330328115,12.));
#175028=CARTESIAN_POINT('Ctrl Pts',(22.5184336670207,-1.76485369319896,
12.));
#175029=CARTESIAN_POINT('Ctrl Pts',(22.5236259635515,-1.76496128643376,
12.));
#175030=CARTESIAN_POINT('Ctrl Pts',(22.529127665298,-1.7650532026276,12.));
#175031=CARTESIAN_POINT('Ctrl Pts',(22.5349313983571,-1.76512711563255,
12.));
#175032=CARTESIAN_POINT('Ctrl Pts',(22.5410303590892,-1.76518087841494,
12.));
#175033=CARTESIAN_POINT('Ctrl Pts',(22.5474180954006,-1.76521245524048,
12.));
#175034=CARTESIAN_POINT('Ctrl Pts',(22.5540882235837,-1.76521983384064,
12.));
#175035=CARTESIAN_POINT('Ctrl Pts',(22.5610344912501,-1.76520104500451,
12.));
#175036=CARTESIAN_POINT('Ctrl Pts',(22.5682508499873,-1.76515418518832,
12.));
#175037=CARTESIAN_POINT('Ctrl Pts',(22.5757315316353,-1.76507744026747,
12.));
#175038=CARTESIAN_POINT('Ctrl Pts',(22.5834711038022,-1.76496910283089,
12.));
#175039=CARTESIAN_POINT('Ctrl Pts',(22.5914644078105,-1.76482755288412,
12.));
#175040=CARTESIAN_POINT('Ctrl Pts',(22.5997065145638,-1.76465124413558,
12.));
#175041=CARTESIAN_POINT('Ctrl Pts',(22.6081926681343,-1.76443868648017,
12.));
#175042=CARTESIAN_POINT('Ctrl Pts',(22.6169182517694,-1.76418843543741,
12.));
#175043=CARTESIAN_POINT('Ctrl Pts',(22.6258787994848,-1.76389909571404,
12.));
#175044=CARTESIAN_POINT('Ctrl Pts',(22.6350699979359,-1.76356932176274,
12.));
#175045=CARTESIAN_POINT('Ctrl Pts',(22.6444876940423,-1.76319782013917,
12.));
#175046=CARTESIAN_POINT('Ctrl Pts',(22.6541278938409,-1.76278334912562,
12.));
#175047=CARTESIAN_POINT('Ctrl Pts',(22.6639867471753,-1.7623247139257,12.));
#175048=CARTESIAN_POINT('Ctrl Pts',(22.67406053567,-1.76182076289527,12.));
#175049=CARTESIAN_POINT('Ctrl Pts',(22.684345658525,-1.76127038310615,12.));
#175050=CARTESIAN_POINT('Ctrl Pts',(22.6948386219851,-1.76067249704888,
12.));
#175051=CARTESIAN_POINT('Ctrl Pts',(22.7055360375485,-1.76002606202402,
12.));
#175052=CARTESIAN_POINT('Ctrl Pts',(22.7164346186006,-1.75933006905926,
12.));
#175053=CARTESIAN_POINT('Ctrl Pts',(22.72753117773,-1.75858354204634,12.));
#175054=CARTESIAN_POINT('Ctrl Pts',(22.7388226235559,-1.75778553673245,
12.));
#175055=CARTESIAN_POINT('Ctrl Pts',(22.750305955645,-1.75693513908908,12.));
#175056=CARTESIAN_POINT('Ctrl Pts',(22.7619782595013,-1.75603146371642,
12.));
#175057=CARTESIAN_POINT('Ctrl Pts',(22.7738367016118,-1.75507365227133,
12.));
#175058=CARTESIAN_POINT('Ctrl Pts',(22.7858785242361,-1.75406087182937,
12.));
#175059=CARTESIAN_POINT('Ctrl Pts',(22.7981010424314,-1.75299231391468,
12.));
#175060=CARTESIAN_POINT('Ctrl Pts',(22.8105016414713,-1.75186719365593,
12.));
#175061=CARTESIAN_POINT('Ctrl Pts',(22.8230777741284,-1.75068474890884,
12.));
#175062=CARTESIAN_POINT('Ctrl Pts',(22.8358269579853,-1.74944423940117,
12.));
#175063=CARTESIAN_POINT('Ctrl Pts',(22.8487467728076,-1.74814494588494,
12.));
#175064=CARTESIAN_POINT('Ctrl Pts',(22.8618348580235,-1.74678616930666,
12.));
#175065=CARTESIAN_POINT('Ctrl Pts',(22.8750889101696,-1.74536722998202,
12.));
#175066=CARTESIAN_POINT('Ctrl Pts',(22.888506680335,-1.74388746677704,12.));
#175067=CARTESIAN_POINT('Ctrl Pts',(22.9020859716141,-1.74234623630081,
12.));
#175068=CARTESIAN_POINT('Ctrl Pts',(22.9158246373363,-1.7407429123106,12.));
#175069=CARTESIAN_POINT('Ctrl Pts',(22.9297205792586,-1.73907688511667,
12.));
#175070=CARTESIAN_POINT('Ctrl Pts',(22.9437717457826,-1.7373475610004,12.));
#175071=CARTESIAN_POINT('Ctrl Pts',(22.9579761301063,-1.73555436162771,
12.));
#175072=CARTESIAN_POINT('Ctrl Pts',(22.9723317685688,-1.73369672350816,
12.));
#175073=CARTESIAN_POINT('Ctrl Pts',(22.9868367391978,-1.73177409750192,
12.));
#175074=CARTESIAN_POINT('Ctrl Pts',(23.001489160189,-1.72978594832137,12.));
#175075=CARTESIAN_POINT('Ctrl Pts',(23.0162871884168,-1.7277317540471,12.));
#175076=CARTESIAN_POINT('Ctrl Pts',(23.0312290178883,-1.72561100564047,
12.));
#175077=CARTESIAN_POINT('Ctrl Pts',(23.0463128785531,-1.72342320653748,
12.));
#175078=CARTESIAN_POINT('Ctrl Pts',(23.0615370351562,-1.72116787225993,
12.));
#175079=CARTESIAN_POINT('Ctrl Pts',(23.0768997860708,-1.71884453003028,
12.));
#175080=CARTESIAN_POINT('Ctrl Pts',(23.0923994621213,-1.71645271839298,
12.));
#175081=CARTESIAN_POINT('Ctrl Pts',(23.1080344254286,-1.71399198684705,
12.));
#175082=CARTESIAN_POINT('Ctrl Pts',(23.1238030684925,-1.71146189552175,
12.));
#175083=CARTESIAN_POINT('Ctrl Pts',(23.1397038132356,-1.70886201485453,
12.));
#175084=CARTESIAN_POINT('Ctrl Pts',(23.1557351100614,-1.70619192527853,
12.));
#175085=CARTESIAN_POINT('Ctrl Pts',(23.1718954368751,-1.70345121691278,
12.));
#175086=CARTESIAN_POINT('Ctrl Pts',(23.1881832981851,-1.70063948927011,
12.));
#175087=CARTESIAN_POINT('Ctrl Pts',(23.2045972243767,-1.69775635099444,
12.));
#175088=CARTESIAN_POINT('Ctrl Pts',(23.2211357709374,-1.69480141959954,
12.));
#175089=CARTESIAN_POINT('Ctrl Pts',(23.2377975177013,-1.69177432121712,
12.));
#175090=CARTESIAN_POINT('Ctrl Pts',(23.2545810680537,-1.68867469034897,
12.));
#175091=CARTESIAN_POINT('Ctrl Pts',(23.2714850482246,-1.68550216963259,
12.));
#175092=CARTESIAN_POINT('Ctrl Pts',(23.2885081066951,-1.68225640962169,
12.));
#175093=CARTESIAN_POINT('Ctrl Pts',(23.3056489135611,-1.67893706857118,
12.));
#175094=CARTESIAN_POINT('Ctrl Pts',(23.3229061599144,-1.67554381222995,
12.));
#175095=CARTESIAN_POINT('Ctrl Pts',(23.3402785571865,-1.67207631363923,
12.));
#175096=CARTESIAN_POINT('Ctrl Pts',(23.3577648365744,-1.66853425293997,
12.));
#175097=CARTESIAN_POINT('Ctrl Pts',(23.3753637485545,-1.66491731718878,
12.));
#175098=CARTESIAN_POINT('Ctrl Pts',(23.3930740623619,-1.66122520018012,
12.));
#175099=CARTESIAN_POINT('Ctrl Pts',(23.4108945654805,-1.65745760227506,
12.));
#175100=CARTESIAN_POINT('Ctrl Pts',(23.4288240631043,-1.6536142302373,12.));
#175101=CARTESIAN_POINT('Ctrl Pts',(23.4468613776574,-1.64969479707341,
12.));
#175102=CARTESIAN_POINT('Ctrl Pts',(23.4650053483932,-1.64569902187612,
12.));
#175103=CARTESIAN_POINT('Ctrl Pts',(23.4832548309645,-1.64162662967529,
12.));
#175104=CARTESIAN_POINT('Ctrl Pts',(23.5016086970003,-1.63747735129475,
12.));
#175105=CARTESIAN_POINT('Ctrl Pts',(23.5200658336612,-1.63325092321727,
12.));
#175106=CARTESIAN_POINT('Ctrl Pts',(23.538625143226,-1.62894708745224,12.));
#175107=CARTESIAN_POINT('Ctrl Pts',(23.5572855427601,-1.62456559140066,
12.));
#175108=CARTESIAN_POINT('Ctrl Pts',(23.57604596376,-1.62010618772867,12.));
#175109=CARTESIAN_POINT('Ctrl Pts',(23.5949053517997,-1.61556863424699,
12.));
#175110=CARTESIAN_POINT('Ctrl Pts',(23.6138626661653,-1.61095269379779,
12.));
#175111=CARTESIAN_POINT('Ctrl Pts',(23.6329168794929,-1.60625813414674,
12.));
#175112=CARTESIAN_POINT('Ctrl Pts',(23.6520669774876,-1.60148472786596,
12.));
#175113=CARTESIAN_POINT('Ctrl Pts',(23.671311958631,-1.59663225222464,12.));
#175114=CARTESIAN_POINT('Ctrl Pts',(23.6906508338833,-1.59170048908634,
12.));
#175115=CARTESIAN_POINT('Ctrl Pts',(23.710082626383,-1.58668922481222,12.));
#175116=CARTESIAN_POINT('Ctrl Pts',(23.72960637113,-1.58159825017359,12.));
#175117=CARTESIAN_POINT('Ctrl Pts',(23.749221114736,-1.57642736025247,12.));
#175118=CARTESIAN_POINT('Ctrl Pts',(23.7689259151862,-1.57117635434409,
12.));
#175119=CARTESIAN_POINT('Ctrl Pts',(23.7887198415878,-1.56584503586844,
12.));
#175120=CARTESIAN_POINT('Ctrl Pts',(23.8086019739194,-1.56043321228635,
12.));
#175121=CARTESIAN_POINT('Ctrl Pts',(23.8285714027636,-1.55494069502636,
12.));
#175122=CARTESIAN_POINT('Ctrl Pts',(23.8486272290705,-1.54936729940542,
12.));
#175123=CARTESIAN_POINT('Ctrl Pts',(23.8687685639642,-1.54371284453992,
12.));
#175124=CARTESIAN_POINT('Ctrl Pts',(23.8889945285318,-1.53797715326759,
12.));
#175125=CARTESIAN_POINT('Ctrl Pts',(23.9093042536119,-1.53216005207464,
12.));
#175126=CARTESIAN_POINT('Ctrl Pts',(23.9296968795757,-1.52626137103033,
12.));
#175127=CARTESIAN_POINT('Ctrl Pts',(23.9501715561033,-1.52028094372793,
12.));
#175128=CARTESIAN_POINT('Ctrl Pts',(23.970727442014,-1.51421860720616,12.));
#175129=CARTESIAN_POINT('Ctrl Pts',(23.9913637050927,-1.50807420187695,
12.));
#175130=CARTESIAN_POINT('Ctrl Pts',(24.0120795219086,-1.501847571461,12.));
#175131=CARTESIAN_POINT('Ctrl Pts',(24.0328740776331,-1.49553856292802,
12.));
#175132=CARTESIAN_POINT('Ctrl Pts',(24.0537465658429,-1.48914702644889,
12.));
#175133=CARTESIAN_POINT('Ctrl Pts',(24.0746961883528,-1.48267281533684,
12.));
#175134=CARTESIAN_POINT('Ctrl Pts',(24.0957221550778,-1.47611578597743,
12.));
#175135=CARTESIAN_POINT('Ctrl Pts',(24.1168236838824,-1.46947579776993,
12.));
#175136=CARTESIAN_POINT('Ctrl Pts',(24.1380000004272,-1.46275271307399,
12.));
#175137=CARTESIAN_POINT('Ctrl Pts',(24.1592503380107,-1.45594639716319,
12.));
#175138=CARTESIAN_POINT('Ctrl Pts',(24.1805739374038,-1.44905671818729,
12.));
#175139=CARTESIAN_POINT('Ctrl Pts',(24.201970046722,-1.44208354711083,12.));
#175140=CARTESIAN_POINT('Ctrl Pts',(24.2234379212984,-1.4350267576551,12.));
#175141=CARTESIAN_POINT('Ctrl Pts',(24.2449768235488,-1.42788622624855,
12.));
#175142=CARTESIAN_POINT('Ctrl Pts',(24.2665860228356,-1.42066183198254,
12.));
#175143=CARTESIAN_POINT('Ctrl Pts',(24.288264795321,-1.41335345657684,12.));
#175144=CARTESIAN_POINT('Ctrl Pts',(24.3100124238311,-1.40596098434339,
12.));
#175145=CARTESIAN_POINT('Ctrl Pts',(24.3318281977643,-1.39848430212808,
12.));
#175146=CARTESIAN_POINT('Ctrl Pts',(24.3537114129875,-1.3909232992639,12.));
#175147=CARTESIAN_POINT('Ctrl Pts',(24.3756613717299,-1.38327786753,12.));
#175148=CARTESIAN_POINT('Ctrl Pts',(24.3976773824732,-1.37554790111611,
12.));
#175149=CARTESIAN_POINT('Ctrl Pts',(24.4197587598337,-1.36773329659958,
12.));
#175150=CARTESIAN_POINT('Ctrl Pts',(24.4419048244523,-1.35983395290629,
12.));
#175151=CARTESIAN_POINT('Ctrl Pts',(24.4641149028892,-1.35184977125649,
12.));
#175152=CARTESIAN_POINT('Ctrl Pts',(24.4863883275134,-1.34378065512339,
12.));
#175153=CARTESIAN_POINT('Ctrl Pts',(24.5087244363856,-1.33562651019687,
12.));
#175154=CARTESIAN_POINT('Ctrl Pts',(24.5311225731435,-1.32738724435327,
12.));
#175155=CARTESIAN_POINT('Ctrl Pts',(24.5535820868674,-1.31906276763669,
12.));
#175156=CARTESIAN_POINT('Ctrl Pts',(24.5761023320183,-1.31065299222023,
12.));
#175157=CARTESIAN_POINT('Ctrl Pts',(24.5986826684027,-1.30215783236363,
12.));
#175158=CARTESIAN_POINT('Ctrl Pts',(24.6213224611229,-1.29357720438108,
12.));
#175159=CARTESIAN_POINT('Ctrl Pts',(24.6440210805278,-1.28491102661515,
12.));
#175160=CARTESIAN_POINT('Ctrl Pts',(24.6667779021559,-1.27615921941643,
12.));
#175161=CARTESIAN_POINT('Ctrl Pts',(24.6895923066836,-1.26732170513501,
12.));
#175162=CARTESIAN_POINT('Ctrl Pts',(24.7124636797894,-1.25839840807419,
12.));
#175163=CARTESIAN_POINT('Ctrl Pts',(24.7353914120011,-1.24938925444327,
12.));
#175164=CARTESIAN_POINT('Ctrl Pts',(24.7583748985438,-1.2402941723199,12.));
#175165=CARTESIAN_POINT('Ctrl Pts',(24.7814135391799,-1.23111309161845,
12.));
#175166=CARTESIAN_POINT('Ctrl Pts',(24.8045067380536,-1.22184594406529,
12.));
#175167=CARTESIAN_POINT('Ctrl Pts',(24.8276539035092,-1.21249266318209,
12.));
#175168=CARTESIAN_POINT('Ctrl Pts',(24.8508544481974,-1.20305318426021,
12.));
#175169=CARTESIAN_POINT('Ctrl Pts',(24.8741077892075,-1.19352744434066,
12.));
#175170=CARTESIAN_POINT('Ctrl Pts',(24.8974133481829,-1.18391538220104,
12.));
#175171=CARTESIAN_POINT('Ctrl Pts',(24.9207705514448,-1.17421693835042,
12.));
#175172=CARTESIAN_POINT('Ctrl Pts',(24.9441788300932,-1.16443205502851,
12.));
#175173=CARTESIAN_POINT('Ctrl Pts',(24.9676376201502,-1.15456067621891,
12.));
#175174=CARTESIAN_POINT('Ctrl Pts',(24.9911463621433,-1.14460274758202,
12.));
#175175=CARTESIAN_POINT('Ctrl Pts',(25.0147045006195,-1.13455821638531,
12.));
#175176=CARTESIAN_POINT('Ctrl Pts',(25.0383114836899,-1.12442703144453,
12.));
#175177=CARTESIAN_POINT('Ctrl Pts',(25.0619667625336,-1.11420914306891,
12.));
#175178=CARTESIAN_POINT('Ctrl Pts',(25.0856697909679,-1.10390450301747,
12.));
#175179=CARTESIAN_POINT('Ctrl Pts',(25.1094200248446,-1.09351306445309,
12.));
#175180=CARTESIAN_POINT('Ctrl Pts',(25.1332169227413,-1.08303478197189,
12.));
#175181=CARTESIAN_POINT('Ctrl Pts',(25.157059946931,-1.07246961165477,12.));
#175182=CARTESIAN_POINT('Ctrl Pts',(25.1809485642192,-1.06181751111769,
12.));
#175183=CARTESIAN_POINT('Ctrl Pts',(25.2048822469028,-1.05107843957933,
12.));
#175184=CARTESIAN_POINT('Ctrl Pts',(25.2288604735086,-1.04025235791508,
12.));
#175185=CARTESIAN_POINT('Ctrl Pts',(25.2528827300422,-1.02933922876807,
12.));
#175186=CARTESIAN_POINT('Ctrl Pts',(25.276948508726,-1.01833901642238,12.));
#175187=CARTESIAN_POINT('Ctrl Pts',(25.3010573055547,-1.00725168656897,
12.));
#175188=CARTESIAN_POINT('Ctrl Pts',(25.3252086182968,-0.996077206120637,
12.));
#175189=CARTESIAN_POINT('Ctrl Pts',(25.3494019441441,-0.984815543003986,
12.));
#175190=CARTESIAN_POINT('Ctrl Pts',(25.3736367778845,-0.973466666000178,
12.));
#175191=CARTESIAN_POINT('Ctrl Pts',(25.3979126089163,-0.962030544503156,
12.));
#175192=CARTESIAN_POINT('Ctrl Pts',(25.4222289223167,-0.950507148597483,
12.));
#175193=CARTESIAN_POINT('Ctrl Pts',(25.4465852044849,-0.938896449496205,
12.));
#175194=CARTESIAN_POINT('Ctrl Pts',(25.4709809475009,-0.927198419886108,
12.));
#175195=CARTESIAN_POINT('Ctrl Pts',(25.4954156541795,-0.915413034335626,
12.));
#175196=CARTESIAN_POINT('Ctrl Pts',(25.5198888424194,-0.903540269651121,
12.));
#175197=CARTESIAN_POINT('Ctrl Pts',(25.5444000508211,-0.891580105349052,
12.));
#175198=CARTESIAN_POINT('Ctrl Pts',(25.5689488408156,-0.879532523834308,
12.));
#175199=CARTESIAN_POINT('Ctrl Pts',(25.5935347843585,-0.867397509338443,
12.));
#175200=CARTESIAN_POINT('Ctrl Pts',(25.6181574536049,-0.855175047036563,
12.));
#175201=CARTESIAN_POINT('Ctrl Pts',(25.6428164100055,-0.842865122120773,
12.));
#175202=CARTESIAN_POINT('Ctrl Pts',(25.6675111931952,-0.830467718864221,
12.));
#175203=CARTESIAN_POINT('Ctrl Pts',(25.6922413110194,-0.817982819787478,
12.));
#175204=CARTESIAN_POINT('Ctrl Pts',(25.7170062262525,-0.805410404554366,
12.));
#175205=CARTESIAN_POINT('Ctrl Pts',(25.7418053757746,-0.79275045161614,
12.));
#175206=CARTESIAN_POINT('Ctrl Pts',(25.7666381946955,-0.780002940291977,
12.));
#175207=CARTESIAN_POINT('Ctrl Pts',(25.7915041383376,-0.767167852651183,
12.));
#175208=CARTESIAN_POINT('Ctrl Pts',(25.8164027059984,-0.754245175609537,
12.));
#175209=CARTESIAN_POINT('Ctrl Pts',(25.8413334619054,-0.74123490266382,
12.));
#175210=CARTESIAN_POINT('Ctrl Pts',(25.8662960624185,-0.728137036482349,
12.));
#175211=CARTESIAN_POINT('Ctrl Pts',(25.8912902614969,-0.714951588527653,
12.));
#175212=CARTESIAN_POINT('Ctrl Pts',(25.9163158909426,-0.701678575228769,
12.));
#175213=CARTESIAN_POINT('Ctrl Pts',(25.9413728471909,-0.688318015057744,
12.));
#175214=CARTESIAN_POINT('Ctrl Pts',(25.9614434297919,-0.67755954320974,
12.));
#175215=CARTESIAN_POINT('Ctrl Pts',(25.9765104298071,-0.669451306780839,
12.));
#175216=CARTESIAN_POINT('Ctrl Pts',(25.9865613464773,-0.66402831318764,
12.));
#175217=CARTESIAN_POINT('Ctrl Pts',(25.991588367311,-0.661312440730916,
12.));
#175218=CARTESIAN_POINT('',(25.991588367311,0.661312440730894,12.));
#175219=CARTESIAN_POINT('Origin',(0.,0.,12.));
#175220=CARTESIAN_POINT('',(22.4835757167854,1.76341220531179,12.));
#175221=CARTESIAN_POINT('Ctrl Pts',(25.991588367311,0.661312440730894,12.));
#175222=CARTESIAN_POINT('Ctrl Pts',(25.9865613464809,0.664028313188916,
12.));
#175223=CARTESIAN_POINT('Ctrl Pts',(25.9765104298171,0.669451306784419,
12.));
#175224=CARTESIAN_POINT('Ctrl Pts',(25.9614434298092,0.677559543215907,
12.));
#175225=CARTESIAN_POINT('Ctrl Pts',(25.941372847213,0.68831801506568,12.));
#175226=CARTESIAN_POINT('Ctrl Pts',(25.9163158909645,0.701678575236605,
12.));
#175227=CARTESIAN_POINT('Ctrl Pts',(25.8912902615141,0.714951588533756,
12.));
#175228=CARTESIAN_POINT('Ctrl Pts',(25.8662960624285,0.728137036485881,
12.));
#175229=CARTESIAN_POINT('Ctrl Pts',(25.841333461908,0.741234902664698,12.));
#175230=CARTESIAN_POINT('Ctrl Pts',(25.816402705995,0.754245175608291,12.));
#175231=CARTESIAN_POINT('Ctrl Pts',(25.7915041383304,0.767167852648643,
12.));
#175232=CARTESIAN_POINT('Ctrl Pts',(25.7666381946871,0.780002940289028,
12.));
#175233=CARTESIAN_POINT('Ctrl Pts',(25.7418053757671,0.792750451613538,
12.));
#175234=CARTESIAN_POINT('Ctrl Pts',(25.7170062262474,0.805410404552597,
12.));
#175235=CARTESIAN_POINT('Ctrl Pts',(25.6922413110172,0.817982819786722,
12.));
#175236=CARTESIAN_POINT('Ctrl Pts',(25.6675111931957,0.83046771886437,12.));
#175237=CARTESIAN_POINT('Ctrl Pts',(25.6428164100078,0.842865122121547,
12.));
#175238=CARTESIAN_POINT('Ctrl Pts',(25.618157453608,0.855175047037618,12.));
#175239=CARTESIAN_POINT('Ctrl Pts',(25.5935347843616,0.867397509339473,
12.));
#175240=CARTESIAN_POINT('Ctrl Pts',(25.568948840818,0.879532523835094,12.));
#175241=CARTESIAN_POINT('Ctrl Pts',(25.5444000508223,0.891580105349469,
12.));
#175242=CARTESIAN_POINT('Ctrl Pts',(25.5198888424195,0.903540269651155,
12.));
#175243=CARTESIAN_POINT('Ctrl Pts',(25.4954156541787,0.915413034335334,
12.));
#175244=CARTESIAN_POINT('Ctrl Pts',(25.4709809474996,0.927198419885607,
12.));
#175245=CARTESIAN_POINT('Ctrl Pts',(25.4465852044835,0.938896449495636,
12.));
#175246=CARTESIAN_POINT('Ctrl Pts',(25.4222289223155,0.950507148596971,
12.));
#175247=CARTESIAN_POINT('Ctrl Pts',(25.3979126089155,0.962030544502806,
12.));
#175248=CARTESIAN_POINT('Ctrl Pts',(25.3736367778842,0.97346666600005,12.));
#175249=CARTESIAN_POINT('Ctrl Pts',(25.3494019441444,0.984815543004091,
12.));
#175250=CARTESIAN_POINT('Ctrl Pts',(25.3252086182976,0.996077206120921,
12.));
#175251=CARTESIAN_POINT('Ctrl Pts',(25.3010573055557,1.00725168656934,12.));
#175252=CARTESIAN_POINT('Ctrl Pts',(25.2769485087268,1.01833901642273,12.));
#175253=CARTESIAN_POINT('Ctrl Pts',(25.2528827300427,1.0293392287683,12.));
#175254=CARTESIAN_POINT('Ctrl Pts',(25.2288604735087,1.04025235791515,12.));
#175255=CARTESIAN_POINT('Ctrl Pts',(25.2048822469027,1.05107843957926,12.));
#175256=CARTESIAN_POINT('Ctrl Pts',(25.1809485642191,1.06181751111754,12.));
#175257=CARTESIAN_POINT('Ctrl Pts',(25.1570599469311,1.0724696116546,12.));
#175258=CARTESIAN_POINT('Ctrl Pts',(25.1332169227415,1.08303478197174,12.));
#175259=CARTESIAN_POINT('Ctrl Pts',(25.1094200248448,1.09351306445299,12.));
#175260=CARTESIAN_POINT('Ctrl Pts',(25.085669790968,1.10390450301741,12.));
#175261=CARTESIAN_POINT('Ctrl Pts',(25.0619667625336,1.1142091430689,12.));
#175262=CARTESIAN_POINT('Ctrl Pts',(25.0383114836898,1.12442703144455,12.));
#175263=CARTESIAN_POINT('Ctrl Pts',(25.0147045006193,1.13455821638536,12.));
#175264=CARTESIAN_POINT('Ctrl Pts',(24.9911463621431,1.14460274758206,12.));
#175265=CARTESIAN_POINT('Ctrl Pts',(24.9676376201501,1.15456067621894,12.));
#175266=CARTESIAN_POINT('Ctrl Pts',(24.9441788300932,1.16443205502852,12.));
#175267=CARTESIAN_POINT('Ctrl Pts',(24.9207705514449,1.1742169383504,12.));
#175268=CARTESIAN_POINT('Ctrl Pts',(24.8974133481829,1.18391538220098,12.));
#175269=CARTESIAN_POINT('Ctrl Pts',(24.8741077892074,1.19352744434059,12.));
#175270=CARTESIAN_POINT('Ctrl Pts',(24.8508544481973,1.20305318426016,12.));
#175271=CARTESIAN_POINT('Ctrl Pts',(24.8276539035092,1.21249266318205,12.));
#175272=CARTESIAN_POINT('Ctrl Pts',(24.8045067380536,1.22184594406527,12.));
#175273=CARTESIAN_POINT('Ctrl Pts',(24.78141353918,1.23111309161843,12.));
#175274=CARTESIAN_POINT('Ctrl Pts',(24.7583748985439,1.24029417231988,12.));
#175275=CARTESIAN_POINT('Ctrl Pts',(24.7353914120012,1.24938925444324,12.));
#175276=CARTESIAN_POINT('Ctrl Pts',(24.7124636797895,1.25839840807415,12.));
#175277=CARTESIAN_POINT('Ctrl Pts',(24.6895923066837,1.26732170513497,12.));
#175278=CARTESIAN_POINT('Ctrl Pts',(24.666777902156,1.2761592194164,12.));
#175279=CARTESIAN_POINT('Ctrl Pts',(24.6440210805278,1.28491102661514,12.));
#175280=CARTESIAN_POINT('Ctrl Pts',(24.6213224611228,1.29357720438108,12.));
#175281=CARTESIAN_POINT('Ctrl Pts',(24.5986826684025,1.30215783236364,12.));
#175282=CARTESIAN_POINT('Ctrl Pts',(24.576102332018,1.31065299222023,12.));
#175283=CARTESIAN_POINT('Ctrl Pts',(24.5535820868671,1.31906276763669,12.));
#175284=CARTESIAN_POINT('Ctrl Pts',(24.5311225731434,1.32738724435326,12.));
#175285=CARTESIAN_POINT('Ctrl Pts',(24.5087244363856,1.33562651019684,12.));
#175286=CARTESIAN_POINT('Ctrl Pts',(24.4863883275135,1.34378065512335,12.));
#175287=CARTESIAN_POINT('Ctrl Pts',(24.4641149028894,1.35184977125645,12.));
#175288=CARTESIAN_POINT('Ctrl Pts',(24.4419048244524,1.35983395290624,12.));
#175289=CARTESIAN_POINT('Ctrl Pts',(24.4197587598337,1.36773329659954,12.));
#175290=CARTESIAN_POINT('Ctrl Pts',(24.3976773824731,1.37554790111608,12.));
#175291=CARTESIAN_POINT('Ctrl Pts',(24.37566137173,1.38327786752998,12.));
#175292=CARTESIAN_POINT('Ctrl Pts',(24.3537114129877,1.3909232992639,12.));
#175293=CARTESIAN_POINT('Ctrl Pts',(24.3318281977647,1.3984843021281,12.));
#175294=CARTESIAN_POINT('Ctrl Pts',(24.3100124238316,1.40596098434341,12.));
#175295=CARTESIAN_POINT('Ctrl Pts',(24.2882647953214,1.41335345657685,12.));
#175296=CARTESIAN_POINT('Ctrl Pts',(24.2665860228357,1.42066183198252,12.));
#175297=CARTESIAN_POINT('Ctrl Pts',(24.2449768235485,1.42788622624851,12.));
#175298=CARTESIAN_POINT('Ctrl Pts',(24.2234379212978,1.43502675765502,12.));
#175299=CARTESIAN_POINT('Ctrl Pts',(24.2019700467214,1.44208354711074,12.));
#175300=CARTESIAN_POINT('Ctrl Pts',(24.1805739374033,1.44905671818721,12.));
#175301=CARTESIAN_POINT('Ctrl Pts',(24.1592503380105,1.45594639716314,12.));
#175302=CARTESIAN_POINT('Ctrl Pts',(24.1380000004272,1.46275271307398,12.));
#175303=CARTESIAN_POINT('Ctrl Pts',(24.1168236838827,1.46947579776992,12.));
#175304=CARTESIAN_POINT('Ctrl Pts',(24.0957221550782,1.47611578597742,12.));
#175305=CARTESIAN_POINT('Ctrl Pts',(24.074696188353,1.4826728153368,12.));
#175306=CARTESIAN_POINT('Ctrl Pts',(24.053746565843,1.48914702644883,12.));
#175307=CARTESIAN_POINT('Ctrl Pts',(24.0328740776331,1.49553856292798,12.));
#175308=CARTESIAN_POINT('Ctrl Pts',(24.0120795219086,1.50184757146099,12.));
#175309=CARTESIAN_POINT('Ctrl Pts',(23.991363705093,1.50807420187703,12.));
#175310=CARTESIAN_POINT('Ctrl Pts',(23.9707274420145,1.51421860720628,12.));
#175311=CARTESIAN_POINT('Ctrl Pts',(23.9501715561038,1.52028094372806,12.));
#175312=CARTESIAN_POINT('Ctrl Pts',(23.9296968795761,1.5262613710304,12.));
#175313=CARTESIAN_POINT('Ctrl Pts',(23.9093042536119,1.53216005207462,12.));
#175314=CARTESIAN_POINT('Ctrl Pts',(23.8889945285313,1.53797715326748,12.));
#175315=CARTESIAN_POINT('Ctrl Pts',(23.8687685639635,1.54371284453978,12.));
#175316=CARTESIAN_POINT('Ctrl Pts',(23.8486272290698,1.5493672994053,12.));
#175317=CARTESIAN_POINT('Ctrl Pts',(23.8285714027631,1.55494069502628,12.));
#175318=CARTESIAN_POINT('Ctrl Pts',(23.8086019739192,1.56043321228631,12.));
#175319=CARTESIAN_POINT('Ctrl Pts',(23.788719841588,1.56584503586844,12.));
#175320=CARTESIAN_POINT('Ctrl Pts',(23.7689259151869,1.57117635434412,12.));
#175321=CARTESIAN_POINT('Ctrl Pts',(23.7492211147369,1.57642736025251,12.));
#175322=CARTESIAN_POINT('Ctrl Pts',(23.7296063711308,1.58159825017362,12.));
#175323=CARTESIAN_POINT('Ctrl Pts',(23.7100826263835,1.58668922481222,12.));
#175324=CARTESIAN_POINT('Ctrl Pts',(23.6906508338832,1.59170048908631,12.));
#175325=CARTESIAN_POINT('Ctrl Pts',(23.6713119586302,1.59663225222459,12.));
#175326=CARTESIAN_POINT('Ctrl Pts',(23.6520669774863,1.60148472786588,12.));
#175327=CARTESIAN_POINT('Ctrl Pts',(23.6329168794916,1.60625813414666,12.));
#175328=CARTESIAN_POINT('Ctrl Pts',(23.6138626661644,1.61095269379773,12.));
#175329=CARTESIAN_POINT('Ctrl Pts',(23.5949053517996,1.61556863424697,12.));
#175330=CARTESIAN_POINT('Ctrl Pts',(23.5760459637608,1.62010618772869,12.));
#175331=CARTESIAN_POINT('Ctrl Pts',(23.5572855427617,1.62456559140072,12.));
#175332=CARTESIAN_POINT('Ctrl Pts',(23.5386251432278,1.62894708745231,12.));
#175333=CARTESIAN_POINT('Ctrl Pts',(23.5200658336624,1.63325092321731,12.));
#175334=CARTESIAN_POINT('Ctrl Pts',(23.5016086970006,1.63747735129474,12.));
#175335=CARTESIAN_POINT('Ctrl Pts',(23.4832548309638,1.64162662967525,12.));
#175336=CARTESIAN_POINT('Ctrl Pts',(23.4650053483919,1.64569902187608,12.));
#175337=CARTESIAN_POINT('Ctrl Pts',(23.446861377656,1.6496947970734,12.));
#175338=CARTESIAN_POINT('Ctrl Pts',(23.4288240631034,1.6536142302373,12.));
#175339=CARTESIAN_POINT('Ctrl Pts',(23.4108945654803,1.65745760227507,12.));
#175340=CARTESIAN_POINT('Ctrl Pts',(23.3930740623622,1.66122520018008,12.));
#175341=CARTESIAN_POINT('Ctrl Pts',(23.375363748555,1.66491731718864,12.));
#175342=CARTESIAN_POINT('Ctrl Pts',(23.3577648365747,1.66853425293978,12.));
#175343=CARTESIAN_POINT('Ctrl Pts',(23.3402785571866,1.67207631363905,12.));
#175344=CARTESIAN_POINT('Ctrl Pts',(23.3229061599145,1.67554381222988,12.));
#175345=CARTESIAN_POINT('Ctrl Pts',(23.3056489135611,1.67893706857123,12.));
#175346=CARTESIAN_POINT('Ctrl Pts',(23.2885081066949,1.68225640962181,12.));
#175347=CARTESIAN_POINT('Ctrl Pts',(23.2714850482245,1.68550216963275,12.));
#175348=CARTESIAN_POINT('Ctrl Pts',(23.2545810680536,1.6886746903491,12.));
#175349=CARTESIAN_POINT('Ctrl Pts',(23.2377975177014,1.69177432121716,12.));
#175350=CARTESIAN_POINT('Ctrl Pts',(23.2211357709374,1.69480141959946,12.));
#175351=CARTESIAN_POINT('Ctrl Pts',(23.2045972243765,1.69775635099425,12.));
#175352=CARTESIAN_POINT('Ctrl Pts',(23.1881832981848,1.70063948926988,12.));
#175353=CARTESIAN_POINT('Ctrl Pts',(23.1718954368749,1.70345121691259,12.));
#175354=CARTESIAN_POINT('Ctrl Pts',(23.1557351100613,1.70619192527847,12.));
#175355=CARTESIAN_POINT('Ctrl Pts',(23.1397038132358,1.7088620148546,12.));
#175356=CARTESIAN_POINT('Ctrl Pts',(23.1238030684929,1.71146189552192,12.));
#175357=CARTESIAN_POINT('Ctrl Pts',(23.1080344254291,1.71399198684725,12.));
#175358=CARTESIAN_POINT('Ctrl Pts',(23.0923994621216,1.71645271839311,12.));
#175359=CARTESIAN_POINT('Ctrl Pts',(23.0768997860709,1.71884453003027,12.));
#175360=CARTESIAN_POINT('Ctrl Pts',(23.0615370351559,1.72116787225981,12.));
#175361=CARTESIAN_POINT('Ctrl Pts',(23.0463128785528,1.72342320653731,12.));
#175362=CARTESIAN_POINT('Ctrl Pts',(23.031229017888,1.72561100564033,12.));
#175363=CARTESIAN_POINT('Ctrl Pts',(23.0162871884167,1.72773175404703,12.));
#175364=CARTESIAN_POINT('Ctrl Pts',(23.0014891601891,1.72978594832137,12.));
#175365=CARTESIAN_POINT('Ctrl Pts',(22.9868367391978,1.73177409750194,12.));
#175366=CARTESIAN_POINT('Ctrl Pts',(22.9723317685688,1.73369672350818,12.));
#175367=CARTESIAN_POINT('Ctrl Pts',(22.9579761301062,1.73555436162771,12.));
#175368=CARTESIAN_POINT('Ctrl Pts',(22.9437717457825,1.73734756100038,12.));
#175369=CARTESIAN_POINT('Ctrl Pts',(22.9297205792587,1.73907688511665,12.));
#175370=CARTESIAN_POINT('Ctrl Pts',(22.9158246373365,1.74074291231057,12.));
#175371=CARTESIAN_POINT('Ctrl Pts',(22.9020859716144,1.74234623630079,12.));
#175372=CARTESIAN_POINT('Ctrl Pts',(22.8885066803351,1.74388746677702,12.));
#175373=CARTESIAN_POINT('Ctrl Pts',(22.8750889101696,1.745367229982,12.));
#175374=CARTESIAN_POINT('Ctrl Pts',(22.8618348580234,1.74678616930663,12.));
#175375=CARTESIAN_POINT('Ctrl Pts',(22.8487467728075,1.74814494588492,12.));
#175376=CARTESIAN_POINT('Ctrl Pts',(22.8358269579854,1.74944423940117,12.));
#175377=CARTESIAN_POINT('Ctrl Pts',(22.8230777741285,1.75068474890884,12.));
#175378=CARTESIAN_POINT('Ctrl Pts',(22.8105016414712,1.7518671936559,12.));
#175379=CARTESIAN_POINT('Ctrl Pts',(22.7981010424312,1.75299231391461,12.));
#175380=CARTESIAN_POINT('Ctrl Pts',(22.7858785242358,1.7540608718293,12.));
#175381=CARTESIAN_POINT('Ctrl Pts',(22.7738367016115,1.75507365227127,12.));
#175382=CARTESIAN_POINT('Ctrl Pts',(22.7619782595013,1.75603146371641,12.));
#175383=CARTESIAN_POINT('Ctrl Pts',(22.7503059556455,1.75693513908911,12.));
#175384=CARTESIAN_POINT('Ctrl Pts',(22.7388226235565,1.75778553673249,12.));
#175385=CARTESIAN_POINT('Ctrl Pts',(22.7275311777305,1.75858354204635,12.));
#175386=CARTESIAN_POINT('Ctrl Pts',(22.7164346186007,1.75933006905924,12.));
#175387=CARTESIAN_POINT('Ctrl Pts',(22.7055360375481,1.76002606202399,12.));
#175388=CARTESIAN_POINT('Ctrl Pts',(22.6948386219843,1.76067249704884,12.));
#175389=CARTESIAN_POINT('Ctrl Pts',(22.6843456585245,1.76127038310613,12.));
#175390=CARTESIAN_POINT('Ctrl Pts',(22.6740605356699,1.76182076289525,12.));
#175391=CARTESIAN_POINT('Ctrl Pts',(22.6639867471756,1.76232471392568,12.));
#175392=CARTESIAN_POINT('Ctrl Pts',(22.6541278938413,1.76278334912559,12.));
#175393=CARTESIAN_POINT('Ctrl Pts',(22.6444876940425,1.76319782013914,12.));
#175394=CARTESIAN_POINT('Ctrl Pts',(22.635069997936,1.76356932176272,12.));
#175395=CARTESIAN_POINT('Ctrl Pts',(22.6258787994847,1.76389909571402,12.));
#175396=CARTESIAN_POINT('Ctrl Pts',(22.6169182517693,1.76418843543739,12.));
#175397=CARTESIAN_POINT('Ctrl Pts',(22.6081926681342,1.76443868648015,12.));
#175398=CARTESIAN_POINT('Ctrl Pts',(22.5997065145638,1.76465124413556,12.));
#175399=CARTESIAN_POINT('Ctrl Pts',(22.5914644078106,1.76482755288411,12.));
#175400=CARTESIAN_POINT('Ctrl Pts',(22.5834711038024,1.76496910283089,12.));
#175401=CARTESIAN_POINT('Ctrl Pts',(22.5757315316355,1.76507744026747,12.));
#175402=CARTESIAN_POINT('Ctrl Pts',(22.5682508499873,1.76515418518829,12.));
#175403=CARTESIAN_POINT('Ctrl Pts',(22.5610344912501,1.7652010450045,12.));
#175404=CARTESIAN_POINT('Ctrl Pts',(22.5540882235837,1.76521983384063,12.));
#175405=CARTESIAN_POINT('Ctrl Pts',(22.5474180954006,1.76521245524047,12.));
#175406=CARTESIAN_POINT('Ctrl Pts',(22.5410303590891,1.76518087841493,12.));
#175407=CARTESIAN_POINT('Ctrl Pts',(22.5349313983571,1.7651271156325,12.));
#175408=CARTESIAN_POINT('Ctrl Pts',(22.529127665298,1.76505320262752,12.));
#175409=CARTESIAN_POINT('Ctrl Pts',(22.5236259635515,1.76496128643369,12.));
#175410=CARTESIAN_POINT('Ctrl Pts',(22.5184336670207,1.76485369319896,12.));
#175411=CARTESIAN_POINT('Ctrl Pts',(22.5135590569554,1.76473303281159,12.));
#175412=CARTESIAN_POINT('Ctrl Pts',(22.5090112700212,1.76460218257323,12.));
#175413=CARTESIAN_POINT('Ctrl Pts',(22.5047996391978,1.76446408210366,12.));
#175414=CARTESIAN_POINT('Ctrl Pts',(22.5009332677316,1.76432160068726,12.));
#175415=CARTESIAN_POINT('Ctrl Pts',(22.4974203063191,1.76417731243462,12.));
#175416=CARTESIAN_POINT('Ctrl Pts',(22.4942693792449,1.76403393880301,12.));
#175417=CARTESIAN_POINT('Ctrl Pts',(22.4914909094908,1.76389475965724,12.));
#175418=CARTESIAN_POINT('Ctrl Pts',(22.4890991659478,1.76376424879505,12.));
#175419=CARTESIAN_POINT('Ctrl Pts',(22.4871115206571,1.76364784232963,12.));
#175420=CARTESIAN_POINT('Ctrl Pts',(22.4855446605991,1.76355076045546,12.));
#175421=CARTESIAN_POINT('Ctrl Pts',(22.4844112933129,1.76347698284792,12.));
#175422=CARTESIAN_POINT('Ctrl Pts',(22.4838562517069,1.76343813434565,12.));
#175423=CARTESIAN_POINT('Ctrl Pts',(22.4836387052232,1.7634206426357,12.));
#175424=CARTESIAN_POINT('Ctrl Pts',(22.483581992979,1.76341415538764,12.));
#175425=CARTESIAN_POINT('Ctrl Pts',(22.4835757167854,1.76341220531179,12.));
#175426=CARTESIAN_POINT('',(21.9269795755927,1.71975774210841,12.));
#175427=CARTESIAN_POINT('',(10.7170877657712,0.840553282521227,12.));
#175428=CARTESIAN_POINT('',(21.3904321633055,2.16781269186828,12.));
#175429=CARTESIAN_POINT('Origin',(21.8878840740801,2.21822694051638,12.));
#175430=CARTESIAN_POINT('',(21.2226420728916,3.44230496120419,12.));
#175431=CARTESIAN_POINT('Origin',(7.7715611723761E-13,7.16093850883226E-14,
12.));
#175432=CARTESIAN_POINT('',(21.624941921198,4.01396149767428,12.));
#175433=CARTESIAN_POINT('Origin',(21.7161918885402,3.52235856495312,12.));
#175434=CARTESIAN_POINT('',(22.1738711152697,4.11585220600461,12.));
#175435=CARTESIAN_POINT('',(11.0869355576349,2.05792610300232,12.));
#175436=CARTESIAN_POINT('',(25.2771067246846,6.08833931617698,12.));
#175437=CARTESIAN_POINT('Ctrl Pts',(22.1738711152697,4.11585220600461,12.));
#175438=CARTESIAN_POINT('Ctrl Pts',(22.1738776823239,4.11585194677412,12.));
#175439=CARTESIAN_POINT('Ctrl Pts',(22.1739341411684,4.1158603587821,12.));
#175440=CARTESIAN_POINT('Ctrl Pts',(22.174148802123,4.11589976826061,12.));
#175441=CARTESIAN_POINT('Ctrl Pts',(22.1746949858773,4.11600589882768,12.));
#175442=CARTESIAN_POINT('Ctrl Pts',(22.1758088296598,4.11622797217066,12.));
#175443=CARTESIAN_POINT('Ctrl Pts',(22.177347426894,4.11653973150558,12.));
#175444=CARTESIAN_POINT('Ctrl Pts',(22.179297473024,4.11694173195041,12.));
#175445=CARTESIAN_POINT('Ctrl Pts',(22.1816414985788,4.11743469691765,12.));
#175446=CARTESIAN_POINT('Ctrl Pts',(22.1843613164855,4.11801938107464,12.));
#175447=CARTESIAN_POINT('Ctrl Pts',(22.1874419861496,4.11869641271752,12.));
#175448=CARTESIAN_POINT('Ctrl Pts',(22.1908725908525,4.11946626228623,12.));
#175449=CARTESIAN_POINT('Ctrl Pts',(22.1946440958098,4.12032932637738,12.));
#175450=CARTESIAN_POINT('Ctrl Pts',(22.1987479618246,4.12128598183533,12.));
#175451=CARTESIAN_POINT('Ctrl Pts',(22.2031746532106,4.12233664408237,12.));
#175452=CARTESIAN_POINT('Ctrl Pts',(22.2079143941719,4.12348173702025,12.));
#175453=CARTESIAN_POINT('Ctrl Pts',(22.2129576146671,4.12472167516602,12.));
#175454=CARTESIAN_POINT('Ctrl Pts',(22.2182956401341,4.126056836133,12.));
#175455=CARTESIAN_POINT('Ctrl Pts',(22.2239207458781,4.127487558301,12.));
#175456=CARTESIAN_POINT('Ctrl Pts',(22.2298258043947,4.12901415463379,12.));
#175457=CARTESIAN_POINT('Ctrl Pts',(22.2360040565534,4.13063692157499,12.));
#175458=CARTESIAN_POINT('Ctrl Pts',(22.2424488153523,4.1323561506016,12.));
#175459=CARTESIAN_POINT('Ctrl Pts',(22.2491535317789,4.13417212558809,12.));
#175460=CARTESIAN_POINT('Ctrl Pts',(22.2561118708422,4.13608511977226,12.));
#175461=CARTESIAN_POINT('Ctrl Pts',(22.263317791397,4.13809539255419,12.));
#175462=CARTESIAN_POINT('Ctrl Pts',(22.2707656042456,4.14020318715988,12.));
#175463=CARTESIAN_POINT('Ctrl Pts',(22.2784499072026,4.14240873321982,12.));
#175464=CARTESIAN_POINT('Ctrl Pts',(22.2863655389167,4.14471224859295,12.));
#175465=CARTESIAN_POINT('Ctrl Pts',(22.2945075198468,4.14711394168559,12.));
#175466=CARTESIAN_POINT('Ctrl Pts',(22.3028710166935,4.14961401285526,12.));
#175467=CARTESIAN_POINT('Ctrl Pts',(22.3114513545186,4.15221265396993,12.));
#175468=CARTESIAN_POINT('Ctrl Pts',(22.3202440186979,4.15491004835278,12.));
#175469=CARTESIAN_POINT('Ctrl Pts',(22.3292446628957,4.15770637047882,12.));
#175470=CARTESIAN_POINT('Ctrl Pts',(22.3384491078599,4.16060178604154,12.));
#175471=CARTESIAN_POINT('Ctrl Pts',(22.3478533253886,4.1635964526318,12.));
#175472=CARTESIAN_POINT('Ctrl Pts',(22.3574534257397,4.16669052026602,12.));
#175473=CARTESIAN_POINT('Ctrl Pts',(22.3672456427605,4.1698841319947,12.));
#175474=CARTESIAN_POINT('Ctrl Pts',(22.3772263228624,4.17317742436162,12.));
#175475=CARTESIAN_POINT('Ctrl Pts',(22.3873919231339,4.17657052752834,12.));
#175476=CARTESIAN_POINT('Ctrl Pts',(22.3977390078074,4.18006356544879,12.));
#175477=CARTESIAN_POINT('Ctrl Pts',(22.4082642454448,4.18365665600839,12.));
#175478=CARTESIAN_POINT('Ctrl Pts',(22.4189644056109,4.18734991117707,12.));
#175479=CARTESIAN_POINT('Ctrl Pts',(22.4298363535416,4.19114343726932,12.));
#175480=CARTESIAN_POINT('Ctrl Pts',(22.4408770448917,4.1950373351886,12.));
#175481=CARTESIAN_POINT('Ctrl Pts',(22.4520835205422,4.19903170066358,12.));
#175482=CARTESIAN_POINT('Ctrl Pts',(22.4634529011437,4.20312662448174,12.));
#175483=CARTESIAN_POINT('Ctrl Pts',(22.4749823839917,4.20732219265649,12.));
#175484=CARTESIAN_POINT('Ctrl Pts',(22.4866692403147,4.21161848657428,12.));
#175485=CARTESIAN_POINT('Ctrl Pts',(22.4985108124228,4.21601558313906,12.));
#175486=CARTESIAN_POINT('Ctrl Pts',(22.5105045108881,4.22051355490196,12.));
#175487=CARTESIAN_POINT('Ctrl Pts',(22.5226478117886,4.22511247020041,12.));
#175488=CARTESIAN_POINT('Ctrl Pts',(22.5349382540588,4.22981239330733,12.));
#175489=CARTESIAN_POINT('Ctrl Pts',(22.5473734368086,4.23461338456712,12.));
#175490=CARTESIAN_POINT('Ctrl Pts',(22.5599510166429,4.23951550052523,12.));
#175491=CARTESIAN_POINT('Ctrl Pts',(22.572668704992,4.24451879404851,12.));
#175492=CARTESIAN_POINT('Ctrl Pts',(22.5855242662477,4.24962331444177,12.));
#175493=CARTESIAN_POINT('Ctrl Pts',(22.5985155158636,4.25482910755481,12.));
#175494=CARTESIAN_POINT('Ctrl Pts',(22.6116403184821,4.26013621588305,12.));
#175495=CARTESIAN_POINT('Ctrl Pts',(22.6248965859977,4.26554467865576,12.));
#175496=CARTESIAN_POINT('Ctrl Pts',(22.6382822758172,4.27105453193004,12.));
#175497=CARTESIAN_POINT('Ctrl Pts',(22.6517953893303,4.2766658086912,12.));
#175498=CARTESIAN_POINT('Ctrl Pts',(22.6654339703109,4.28237853894059,12.));
#175499=CARTESIAN_POINT('Ctrl Pts',(22.6791961033537,4.28819274977763,12.));
#175500=CARTESIAN_POINT('Ctrl Pts',(22.6930799122548,4.29410846547056,12.));
#175501=CARTESIAN_POINT('Ctrl Pts',(22.7070835587564,4.3001257075406,12.));
#175502=CARTESIAN_POINT('Ctrl Pts',(22.7212052413386,4.30624449484069,12.));
#175503=CARTESIAN_POINT('Ctrl Pts',(22.7354431939926,4.31246484362549,12.));
#175504=CARTESIAN_POINT('Ctrl Pts',(22.7497956849848,4.31878676761235,12.));
#175505=CARTESIAN_POINT('Ctrl Pts',(22.7642610156475,4.32521027803754,12.));
#175506=CARTESIAN_POINT('Ctrl Pts',(22.7788375194076,4.3317353837319,12.));
#175507=CARTESIAN_POINT('Ctrl Pts',(22.7935235607806,4.33836209118446,12.));
#175508=CARTESIAN_POINT('Ctrl Pts',(22.8083175343791,4.34509040460062,12.));
#175509=CARTESIAN_POINT('Ctrl Pts',(22.8232178638876,4.35192032594791,12.));
#175510=CARTESIAN_POINT('Ctrl Pts',(22.8382230011184,4.35885185500546,12.));
#175511=CARTESIAN_POINT('Ctrl Pts',(22.8533314252422,4.36588498942997,12.));
#175512=CARTESIAN_POINT('Ctrl Pts',(22.8685416419725,4.37301972480746,12.));
#175513=CARTESIAN_POINT('Ctrl Pts',(22.8838521827701,4.38025605470093,12.));
#175514=CARTESIAN_POINT('Ctrl Pts',(22.8992616040108,4.38759397068406,12.));
#175515=CARTESIAN_POINT('Ctrl Pts',(22.9147684862426,4.39503346238473,12.));
#175516=CARTESIAN_POINT('Ctrl Pts',(22.930371433555,4.40257451754324,12.));
#175517=CARTESIAN_POINT('Ctrl Pts',(22.9460690729093,4.41021712205554,12.));
#175518=CARTESIAN_POINT('Ctrl Pts',(22.9618600534866,4.41796126001302,12.));
#175519=CARTESIAN_POINT('Ctrl Pts',(22.977743046002,4.42580691372752,12.));
#175520=CARTESIAN_POINT('Ctrl Pts',(22.9937167421006,4.43375406376879,12.));
#175521=CARTESIAN_POINT('Ctrl Pts',(23.0097798538395,4.44180268901643,12.));
#175522=CARTESIAN_POINT('Ctrl Pts',(23.0259311131392,4.44995276669687,12.));
#175523=CARTESIAN_POINT('Ctrl Pts',(23.0421692712467,4.45820427241683,12.));
#175524=CARTESIAN_POINT('Ctrl Pts',(23.0584930981732,4.46655718018231,12.));
#175525=CARTESIAN_POINT('Ctrl Pts',(23.0749013821881,4.47501146242856,12.));
#175526=CARTESIAN_POINT('Ctrl Pts',(23.0913929293922,4.48356709006788,12.));
#175527=CARTESIAN_POINT('Ctrl Pts',(23.1079665632636,4.49222403252216,12.));
#175528=CARTESIAN_POINT('Ctrl Pts',(23.1246211242115,4.50098225775171,12.));
#175529=CARTESIAN_POINT('Ctrl Pts',(23.1413554691123,4.5098417322706,12.));
#175530=CARTESIAN_POINT('Ctrl Pts',(23.1581684708761,4.51880242116748,12.));
#175531=CARTESIAN_POINT('Ctrl Pts',(23.1750590180908,4.52786428815015,12.));
#175532=CARTESIAN_POINT('Ctrl Pts',(23.1920260146465,4.53702729557566,12.));
#175533=CARTESIAN_POINT('Ctrl Pts',(23.2090683793629,4.54629140447544,12.));
#175534=CARTESIAN_POINT('Ctrl Pts',(23.2261850456064,4.55565657456975,12.));
#175535=CARTESIAN_POINT('Ctrl Pts',(23.2433749609131,4.56512276427839,12.));
#175536=CARTESIAN_POINT('Ctrl Pts',(23.2606370866866,4.57468993076097,12.));
#175537=CARTESIAN_POINT('Ctrl Pts',(23.2779703978876,4.5843580299469,12.));
#175538=CARTESIAN_POINT('Ctrl Pts',(23.2953738827191,4.5941270165575,12.));
#175539=CARTESIAN_POINT('Ctrl Pts',(23.3128465423115,4.60399684412163,12.));
#175540=CARTESIAN_POINT('Ctrl Pts',(23.3303873903938,4.6139674649783,12.));
#175541=CARTESIAN_POINT('Ctrl Pts',(23.3479954530272,4.62403883030805,12.));
#175542=CARTESIAN_POINT('Ctrl Pts',(23.3656697683489,4.63421089016541,12.));
#175543=CARTESIAN_POINT('Ctrl Pts',(23.3834093863068,4.6444835934993,12.));
#175544=CARTESIAN_POINT('Ctrl Pts',(23.4012133683959,4.65485688816924,12.));
#175545=CARTESIAN_POINT('Ctrl Pts',(23.4190807873803,4.6653307209467,12.));
#175546=CARTESIAN_POINT('Ctrl Pts',(23.4370107270451,4.67590503753059,12.));
#175547=CARTESIAN_POINT('Ctrl Pts',(23.455002281986,4.68657978258303,12.));
#175548=CARTESIAN_POINT('Ctrl Pts',(23.4730545573853,4.69735489975024,12.));
#175549=CARTESIAN_POINT('Ctrl Pts',(23.491166668789,4.70823033167819,12.));
#175550=CARTESIAN_POINT('Ctrl Pts',(23.509337741878,4.71920602001902,12.));
#175551=CARTESIAN_POINT('Ctrl Pts',(23.5275669122372,4.7302819054303,12.));
#175552=CARTESIAN_POINT('Ctrl Pts',(23.545853325171,4.74145792760699,12.));
#175553=CARTESIAN_POINT('Ctrl Pts',(23.5641961355168,4.75273402530617,12.));
#175554=CARTESIAN_POINT('Ctrl Pts',(23.5825945074535,4.76411013636251,12.));
#175555=CARTESIAN_POINT('Ctrl Pts',(23.6010476143099,4.77558619769872,12.));
#175556=CARTESIAN_POINT('Ctrl Pts',(23.6195546383624,4.78716214532098,12.));
#175557=CARTESIAN_POINT('Ctrl Pts',(23.6381147706579,4.7988379143322,12.));
#175558=CARTESIAN_POINT('Ctrl Pts',(23.6567272108628,4.81061343896432,12.));
#175559=CARTESIAN_POINT('Ctrl Pts',(23.675391167102,4.82248865259562,12.));
#175560=CARTESIAN_POINT('Ctrl Pts',(23.6941058557971,4.83446348776266,12.));
#175561=CARTESIAN_POINT('Ctrl Pts',(23.7128705015017,4.84653787616426,12.));
#175562=CARTESIAN_POINT('Ctrl Pts',(23.7316843367313,4.85871174865499,12.));
#175563=CARTESIAN_POINT('Ctrl Pts',(23.7505466018245,4.87098503527152,12.));
#175564=CARTESIAN_POINT('Ctrl Pts',(23.7694565448049,4.88335766525573,12.));
#175565=CARTESIAN_POINT('Ctrl Pts',(23.7884134212384,4.89582956706775,12.));
#175566=CARTESIAN_POINT('Ctrl Pts',(23.8074164940896,4.90840066839344,12.));
#175567=CARTESIAN_POINT('Ctrl Pts',(23.8264650335717,4.92107089613969,12.));
#175568=CARTESIAN_POINT('Ctrl Pts',(23.8455583170057,4.93384017643432,12.));
#175569=CARTESIAN_POINT('Ctrl Pts',(23.8646956287168,4.9467084346586,12.));
#175570=CARTESIAN_POINT('Ctrl Pts',(23.8838762599218,4.95967559546561,12.));
#175571=CARTESIAN_POINT('Ctrl Pts',(23.9030995086163,4.97274158279227,12.));
#175572=CARTESIAN_POINT('Ctrl Pts',(23.9223646794592,4.98590631986533,12.));
#175573=CARTESIAN_POINT('Ctrl Pts',(23.9416710836529,4.99916972919307,12.));
#175574=CARTESIAN_POINT('Ctrl Pts',(23.961018038827,5.01253173257453,12.));
#175575=CARTESIAN_POINT('Ctrl Pts',(23.9804048689227,5.02599225112454,12.));
#175576=CARTESIAN_POINT('Ctrl Pts',(23.9998309040746,5.03955120528521,12.));
#175577=CARTESIAN_POINT('Ctrl Pts',(24.0192954804896,5.05320851483065,12.));
#175578=CARTESIAN_POINT('Ctrl Pts',(24.0387979403268,5.06696409886641,12.));
#175579=CARTESIAN_POINT('Ctrl Pts',(24.0583376315638,5.08081787581277,12.));
#175580=CARTESIAN_POINT('Ctrl Pts',(24.0779139079266,5.09476976342625,12.));
#175581=CARTESIAN_POINT('Ctrl Pts',(24.0975261288446,5.10881967883132,12.));
#175582=CARTESIAN_POINT('Ctrl Pts',(24.117173659394,5.1229675385386,12.));
#175583=CARTESIAN_POINT('Ctrl Pts',(24.1368558702443,5.13721325845745,12.));
#175584=CARTESIAN_POINT('Ctrl Pts',(24.156572137597,5.15155675390075,12.));
#175585=CARTESIAN_POINT('Ctrl Pts',(24.1763218431343,5.16599793957979,12.));
#175586=CARTESIAN_POINT('Ctrl Pts',(24.1961043738754,5.18053672961392,12.));
#175587=CARTESIAN_POINT('Ctrl Pts',(24.215919122017,5.19517303753643,12.));
#175588=CARTESIAN_POINT('Ctrl Pts',(24.2357654847765,5.20990677629173,12.));
#175589=CARTESIAN_POINT('Ctrl Pts',(24.2556428642294,5.22473785822441,12.));
#175590=CARTESIAN_POINT('Ctrl Pts',(24.2755506671526,5.23966619506289,12.));
#175591=CARTESIAN_POINT('Ctrl Pts',(24.2954883048448,5.25469169788856,12.));
#175592=CARTESIAN_POINT('Ctrl Pts',(24.3154551932222,5.26981427718796,12.));
#175593=CARTESIAN_POINT('Ctrl Pts',(24.3354507529415,5.28503384290644,12.));
#175594=CARTESIAN_POINT('Ctrl Pts',(24.3554744095075,5.30035030449059,12.));
#175595=CARTESIAN_POINT('Ctrl Pts',(24.3755255933917,5.31576357092525,12.));
#175596=CARTESIAN_POINT('Ctrl Pts',(24.3956037401293,5.33127355076037,12.));
#175597=CARTESIAN_POINT('Ctrl Pts',(24.4157082904615,5.34688015213546,12.));
#175598=CARTESIAN_POINT('Ctrl Pts',(24.4358386899152,5.36258328273639,12.));
#175599=CARTESIAN_POINT('Ctrl Pts',(24.4559943883159,5.37838284973706,12.));
#175600=CARTESIAN_POINT('Ctrl Pts',(24.4761748393322,5.39427875973831,12.));
#175601=CARTESIAN_POINT('Ctrl Pts',(24.4963794999831,5.41027091869242,12.));
#175602=CARTESIAN_POINT('Ctrl Pts',(24.5166078302107,5.42635923183411,12.));
#175603=CARTESIAN_POINT('Ctrl Pts',(24.5368592922861,5.44254360356866,12.));
#175604=CARTESIAN_POINT('Ctrl Pts',(24.5571333514841,5.45882393762244,12.));
#175605=CARTESIAN_POINT('Ctrl Pts',(24.5774294770329,5.47520013724403,12.));
#175606=CARTESIAN_POINT('Ctrl Pts',(24.5977471429365,5.49167210537235,12.));
#175607=CARTESIAN_POINT('Ctrl Pts',(24.618085828918,5.50823974481959,12.));
#175608=CARTESIAN_POINT('Ctrl Pts',(24.6384450211466,5.52490295840996,12.));
#175609=CARTESIAN_POINT('Ctrl Pts',(24.6588242134733,5.54166164919593,12.));
#175610=CARTESIAN_POINT('Ctrl Pts',(24.6792229061785,5.55851572025389,12.));
#175611=CARTESIAN_POINT('Ctrl Pts',(24.6996406035507,5.57546507427767,12.));
#175612=CARTESIAN_POINT('Ctrl Pts',(24.7200768119079,5.59250961323995,12.));
#175613=CARTESIAN_POINT('Ctrl Pts',(24.7405310372736,5.60964923798495,12.));
#175614=CARTESIAN_POINT('Ctrl Pts',(24.76100278357,5.62688384790919,12.));
#175615=CARTESIAN_POINT('Ctrl Pts',(24.7814915496728,5.64421334042248,12.));
#175616=CARTESIAN_POINT('Ctrl Pts',(24.8019968304618,5.66163761114903,12.));
#175617=CARTESIAN_POINT('Ctrl Pts',(24.822518122386,5.67915655496524,12.));
#175618=CARTESIAN_POINT('Ctrl Pts',(24.8430549277634,5.6967700667943,12.));
#175619=CARTESIAN_POINT('Ctrl Pts',(24.8636067597677,5.71447804252019,12.));
#175620=CARTESIAN_POINT('Ctrl Pts',(24.8841731467219,5.73228037976927,12.));
#175621=CARTESIAN_POINT('Ctrl Pts',(24.9047536376467,5.75017697890813,12.));
#175622=CARTESIAN_POINT('Ctrl Pts',(24.9253478043632,5.76816774342236,12.));
#175623=CARTESIAN_POINT('Ctrl Pts',(24.9459552293308,5.78625257775703,12.));
#175624=CARTESIAN_POINT('Ctrl Pts',(24.9665754954462,5.80443138549747,12.));
#175625=CARTESIAN_POINT('Ctrl Pts',(24.9872081752709,5.82270406744214,12.));
#175626=CARTESIAN_POINT('Ctrl Pts',(25.0078528200558,5.84107051963074,12.));
#175627=CARTESIAN_POINT('Ctrl Pts',(25.0285089498922,5.8595306315681,12.));
#175628=CARTESIAN_POINT('Ctrl Pts',(25.0491760405965,5.87808428385329,12.));
#175629=CARTESIAN_POINT('Ctrl Pts',(25.0698535426593,5.89673135155459,12.));
#175630=CARTESIAN_POINT('Ctrl Pts',(25.0905409050863,5.91547170844382,12.));
#175631=CARTESIAN_POINT('Ctrl Pts',(25.1112375971182,5.93430523086776,12.));
#175632=CARTESIAN_POINT('Ctrl Pts',(25.1319431317273,5.95323180187348,12.));
#175633=CARTESIAN_POINT('Ctrl Pts',(25.1526570863065,5.97225131495636,12.));
#175634=CARTESIAN_POINT('Ctrl Pts',(25.1733791296154,5.99136367859839,12.));
#175635=CARTESIAN_POINT('Ctrl Pts',(25.1941090269638,6.0105688180476,12.));
#175636=CARTESIAN_POINT('Ctrl Pts',(25.2148466201368,6.02986667390187,12.));
#175637=CARTESIAN_POINT('Ctrl Pts',(25.2355918138798,6.04925720151412,12.));
#175638=CARTESIAN_POINT('Ctrl Pts',(25.2521940105523,6.06484373634697,12.));
#175639=CARTESIAN_POINT('Ctrl Pts',(25.2646490489816,6.07657531787578,12.));
#175640=CARTESIAN_POINT('Ctrl Pts',(25.2729539149479,6.08441489609824,12.));
#175641=CARTESIAN_POINT('Ctrl Pts',(25.2771067246846,6.08833931617698,12.));
#175642=CARTESIAN_POINT('',(24.9347862158358,7.36589684767344,12.));
#175643=CARTESIAN_POINT('Origin',(0.,0.,12.));
#175644=CARTESIAN_POINT('',(21.2610617890679,7.52250298901264,12.));
#175645=CARTESIAN_POINT('Ctrl Pts',(24.9347862158358,7.36589684767344,12.));
#175646=CARTESIAN_POINT('Ctrl Pts',(24.9292275670705,7.3672190902906,12.));
#175647=CARTESIAN_POINT('Ctrl Pts',(24.9181155530631,7.36985593120697,12.));
#175648=CARTESIAN_POINT('Ctrl Pts',(24.9014633826201,7.37378825962718,12.));
#175649=CARTESIAN_POINT('Ctrl Pts',(24.8792921911309,7.3789854964161,12.));
#175650=CARTESIAN_POINT('Ctrl Pts',(24.8516310625367,7.38540558904946,12.));
#175651=CARTESIAN_POINT('Ctrl Pts',(24.8240228521042,7.39174922586841,12.));
#175652=CARTESIAN_POINT('Ctrl Pts',(24.7964676646518,7.39801641583613,12.));
#175653=CARTESIAN_POINT('Ctrl Pts',(24.7689656669005,7.40420718661755,12.));
#175654=CARTESIAN_POINT('Ctrl Pts',(24.7415170994754,7.41032159082173,12.));
#175655=CARTESIAN_POINT('Ctrl Pts',(24.7141222949988,7.41635971481243,12.));
#175656=CARTESIAN_POINT('Ctrl Pts',(24.6867816727118,7.42232167765763,12.));
#175657=CARTESIAN_POINT('Ctrl Pts',(24.659495712869,7.42820762158681,12.));
#175658=CARTESIAN_POINT('Ctrl Pts',(24.6322649369472,7.43401770489221,12.));
#175659=CARTESIAN_POINT('Ctrl Pts',(24.6050898852349,7.43975209375375,12.));
#175660=CARTESIAN_POINT('Ctrl Pts',(24.5779710960865,7.44541095473163,12.));
#175661=CARTESIAN_POINT('Ctrl Pts',(24.5509090831579,7.45099444651296,12.));
#175662=CARTESIAN_POINT('Ctrl Pts',(24.52390431731,7.45650271336046,12.));
#175663=CARTESIAN_POINT('Ctrl Pts',(24.4969572391509,7.46193588961642,12.));
#175664=CARTESIAN_POINT('Ctrl Pts',(24.4700682684544,7.46729410308923,12.));
#175665=CARTESIAN_POINT('Ctrl Pts',(24.4432378146501,7.47257747883319,12.));
#175666=CARTESIAN_POINT('Ctrl Pts',(24.4164662871165,7.47778614286574,12.));
#175667=CARTESIAN_POINT('Ctrl Pts',(24.3897541049248,7.48292022569254,12.));
#175668=CARTESIAN_POINT('Ctrl Pts',(24.3631017084513,7.48797986651828,12.));
#175669=CARTESIAN_POINT('Ctrl Pts',(24.3365095573673,7.4929652125233,12.));
#175670=CARTESIAN_POINT('Ctrl Pts',(24.3099781253345,7.49787641695359,12.));
#175671=CARTESIAN_POINT('Ctrl Pts',(24.2835078958966,7.50271363765099,12.));
#175672=CARTESIAN_POINT('Ctrl Pts',(24.2570993577032,7.50747703535115,12.));
#175673=CARTESIAN_POINT('Ctrl Pts',(24.230753000389,7.51216677222199,12.));
#175674=CARTESIAN_POINT('Ctrl Pts',(24.2044693092356,7.51678300997998,12.));
#175675=CARTESIAN_POINT('Ctrl Pts',(24.1782487641602,7.52132590953863,12.));
#175676=CARTESIAN_POINT('Ctrl Pts',(24.152091842537,7.52579563201479,12.));
#175677=CARTESIAN_POINT('Ctrl Pts',(24.1259990209211,7.53019233935537,12.));
#175678=CARTESIAN_POINT('Ctrl Pts',(24.0999707772642,7.53451619514659,12.));
#175679=CARTESIAN_POINT('Ctrl Pts',(24.0740075927984,7.53876736531005,12.));
#175680=CARTESIAN_POINT('Ctrl Pts',(24.0481099543353,7.54294601896128,12.));
#175681=CARTESIAN_POINT('Ctrl Pts',(24.0222783554531,7.54705232885895,12.));
#175682=CARTESIAN_POINT('Ctrl Pts',(23.9965132953187,7.55108647097432,12.));
#175683=CARTESIAN_POINT('Ctrl Pts',(23.9708152779886,7.55504862424808,12.));
#175684=CARTESIAN_POINT('Ctrl Pts',(23.9451848115002,7.5589389702768,12.));
#175685=CARTESIAN_POINT('Ctrl Pts',(23.9196224070759,7.56275769304773,12.));
#175686=CARTESIAN_POINT('Ctrl Pts',(23.8941285782002,7.56650497863791,12.));
#175687=CARTESIAN_POINT('Ctrl Pts',(23.8687038399595,7.57018101500709,12.));
#175688=CARTESIAN_POINT('Ctrl Pts',(23.8433487096132,7.57378599219814,12.));
#175689=CARTESIAN_POINT('Ctrl Pts',(23.8180637069976,7.57732010249066,12.));
#175690=CARTESIAN_POINT('Ctrl Pts',(23.7928493549908,7.58078354058213,12.));
#175691=CARTESIAN_POINT('Ctrl Pts',(23.7677061799376,7.58417650376271,12.));
#175692=CARTESIAN_POINT('Ctrl Pts',(23.7426347121006,7.58749919210826,12.));
#175693=CARTESIAN_POINT('Ctrl Pts',(23.7176354860456,7.59075180865321,12.));
#175694=CARTESIAN_POINT('Ctrl Pts',(23.6927090405066,7.59393455934035,12.));
#175695=CARTESIAN_POINT('Ctrl Pts',(23.6678559182875,7.59704765299567,12.));
#175696=CARTESIAN_POINT('Ctrl Pts',(23.6430766661418,7.60009130130126,12.));
#175697=CARTESIAN_POINT('Ctrl Pts',(23.6183718346576,7.60306571877806,12.));
#175698=CARTESIAN_POINT('Ctrl Pts',(23.5937419781245,7.60597112277094,12.));
#175699=CARTESIAN_POINT('Ctrl Pts',(23.5691876544244,7.608807733446,12.));
#175700=CARTESIAN_POINT('Ctrl Pts',(23.544709425203,7.61157577385372,12.));
#175701=CARTESIAN_POINT('Ctrl Pts',(23.5203078560129,7.61427546999298,12.));
#175702=CARTESIAN_POINT('Ctrl Pts',(23.4959835164609,7.61690705088319,12.));
#175703=CARTESIAN_POINT('Ctrl Pts',(23.4717369803438,7.61947074863977,12.));
#175704=CARTESIAN_POINT('Ctrl Pts',(23.4475688257854,7.62196679855955,12.));
#175705=CARTESIAN_POINT('Ctrl Pts',(23.4234796353542,7.6243954392005,12.));
#175706=CARTESIAN_POINT('Ctrl Pts',(23.399469996112,7.62675691240329,12.));
#175707=CARTESIAN_POINT('Ctrl Pts',(23.3755404996636,7.62905146332593,12.));
#175708=CARTESIAN_POINT('Ctrl Pts',(23.3516917421972,7.63127934048137,12.));
#175709=CARTESIAN_POINT('Ctrl Pts',(23.3279243245241,7.63344079578162,12.));
#175710=CARTESIAN_POINT('Ctrl Pts',(23.3042388521022,7.63553608458783,12.));
#175711=CARTESIAN_POINT('Ctrl Pts',(23.2806359350855,7.63756546576374,12.));
#175712=CARTESIAN_POINT('Ctrl Pts',(23.2571161884488,7.63952920172835,12.));
#175713=CARTESIAN_POINT('Ctrl Pts',(23.2336802320912,7.64142755851505,12.));
#175714=CARTESIAN_POINT('Ctrl Pts',(23.2103286909398,7.6432608058368,12.));
#175715=CARTESIAN_POINT('Ctrl Pts',(23.1870621950452,7.64502921715483,12.));
#175716=CARTESIAN_POINT('Ctrl Pts',(23.1638813796694,7.64673306975805,12.));
#175717=CARTESIAN_POINT('Ctrl Pts',(23.1407868853819,7.64837264482943,12.));
#175718=CARTESIAN_POINT('Ctrl Pts',(23.1177793581679,7.6499482274986,12.));
#175719=CARTESIAN_POINT('Ctrl Pts',(23.094859449525,7.65146010690476,12.));
#175720=CARTESIAN_POINT('Ctrl Pts',(23.072027816555,7.65290857626358,12.));
#175721=CARTESIAN_POINT('Ctrl Pts',(23.0492851220528,7.65429393293946,12.));
#175722=CARTESIAN_POINT('Ctrl Pts',(23.0266320345787,7.65561647852534,12.));
#175723=CARTESIAN_POINT('Ctrl Pts',(23.0040692285814,7.65687651891305,12.));
#175724=CARTESIAN_POINT('Ctrl Pts',(22.9815973845296,7.65807436436432,12.));
#175725=CARTESIAN_POINT('Ctrl Pts',(22.959217189033,7.65921032958902,12.));
#175726=CARTESIAN_POINT('Ctrl Pts',(22.9369293349593,7.66028473382778,12.));
#175727=CARTESIAN_POINT('Ctrl Pts',(22.9147345215421,7.66129790094108,12.));
#175728=CARTESIAN_POINT('Ctrl Pts',(22.8926334544883,7.66225015950156,12.));
#175729=CARTESIAN_POINT('Ctrl Pts',(22.8706268461283,7.66314184287337,12.));
#175730=CARTESIAN_POINT('Ctrl Pts',(22.848715415557,7.66397328929803,12.));
#175731=CARTESIAN_POINT('Ctrl Pts',(22.8268998887678,7.66474484198549,12.));
#175732=CARTESIAN_POINT('Ctrl Pts',(22.8051809987833,7.66545684920987,12.));
#175733=CARTESIAN_POINT('Ctrl Pts',(22.7835594857699,7.66610966441273,12.));
#175734=CARTESIAN_POINT('Ctrl Pts',(22.7620360971843,7.66670364630299,12.));
#175735=CARTESIAN_POINT('Ctrl Pts',(22.7406115879513,7.6672391589544,12.));
#175736=CARTESIAN_POINT('Ctrl Pts',(22.7192867206245,7.66771657191028,12.));
#175737=CARTESIAN_POINT('Ctrl Pts',(22.6980622655446,7.66813626029275,12.));
#175738=CARTESIAN_POINT('Ctrl Pts',(22.6769390009885,7.66849860491743,12.));
#175739=CARTESIAN_POINT('Ctrl Pts',(22.6559177133127,7.66880399241323,12.));
#175740=CARTESIAN_POINT('Ctrl Pts',(22.6349991971541,7.66905281533715,12.));
#175741=CARTESIAN_POINT('Ctrl Pts',(22.6141842556243,7.66924547229414,12.));
#175742=CARTESIAN_POINT('Ctrl Pts',(22.5934737004953,7.66938236806233,12.));
#175743=CARTESIAN_POINT('Ctrl Pts',(22.5728683523831,7.66946391372306,12.));
#175744=CARTESIAN_POINT('Ctrl Pts',(22.5523690409116,7.66949052679693,12.));
#175745=CARTESIAN_POINT('Ctrl Pts',(22.53197660492,7.66946263138144,12.));
#175746=CARTESIAN_POINT('Ctrl Pts',(22.5116918927031,7.66938065829108,12.));
#175747=CARTESIAN_POINT('Ctrl Pts',(22.4915157622312,7.66924504520315,12.));
#175748=CARTESIAN_POINT('Ctrl Pts',(22.4714490813699,7.66905623680831,12.));
#175749=CARTESIAN_POINT('Ctrl Pts',(22.4514927280855,7.66881468496635,12.));
#175750=CARTESIAN_POINT('Ctrl Pts',(22.4316475906603,7.66852084886704,12.));
#175751=CARTESIAN_POINT('Ctrl Pts',(22.4119145679758,7.6681751951964,12.));
#175752=CARTESIAN_POINT('Ctrl Pts',(22.3922945697773,7.6677781983079,12.));
#175753=CARTESIAN_POINT('Ctrl Pts',(22.372788516936,7.66733034039883,12.));
#175754=CARTESIAN_POINT('Ctrl Pts',(22.3533973417021,7.66683211169159,12.));
#175755=CARTESIAN_POINT('Ctrl Pts',(22.3341219879469,7.66628401061952,12.));
#175756=CARTESIAN_POINT('Ctrl Pts',(22.314963411484,7.66568654402494,12.));
#175757=CARTESIAN_POINT('Ctrl Pts',(22.2959225803937,7.66504022736299,12.));
#175758=CARTESIAN_POINT('Ctrl Pts',(22.2770004753335,7.66434558490979,12.));
#175759=CARTESIAN_POINT('Ctrl Pts',(22.258198089848,7.66360314997641,12.));
#175760=CARTESIAN_POINT('Ctrl Pts',(22.2395164306547,7.66281346512509,12.));
#175761=CARTESIAN_POINT('Ctrl Pts',(22.2209565180085,7.661977082404,12.));
#175762=CARTESIAN_POINT('Ctrl Pts',(22.2025193860964,7.66109456359271,12.));
#175763=CARTESIAN_POINT('Ctrl Pts',(22.1842060834091,7.66016648045005,12.));
#175764=CARTESIAN_POINT('Ctrl Pts',(22.1660176731178,7.65919341496931,12.));
#175765=CARTESIAN_POINT('Ctrl Pts',(22.1479552334211,7.65817595963349,12.));
#175766=CARTESIAN_POINT('Ctrl Pts',(22.1300198579675,7.65711471769397,12.));
#175767=CARTESIAN_POINT('Ctrl Pts',(22.1122126563329,7.65601030346807,12.));
#175768=CARTESIAN_POINT('Ctrl Pts',(22.094534754469,7.65486334263644,12.));
#175769=CARTESIAN_POINT('Ctrl Pts',(22.0769872951596,7.65367447254949,12.));
#175770=CARTESIAN_POINT('Ctrl Pts',(22.0595714384431,7.65244434253113,12.));
#175771=CARTESIAN_POINT('Ctrl Pts',(22.0422883621174,7.65117361421359,12.));
#175772=CARTESIAN_POINT('Ctrl Pts',(22.0251392623209,7.64986296190169,12.));
#175773=CARTESIAN_POINT('Ctrl Pts',(22.0081253540774,7.64851307293352,12.));
#175774=CARTESIAN_POINT('Ctrl Pts',(21.9912478718542,7.6471246480525,12.));
#175775=CARTESIAN_POINT('Ctrl Pts',(21.9745080700798,7.64569840177336,12.));
#175776=CARTESIAN_POINT('Ctrl Pts',(21.9579072237651,7.64423506279123,12.));
#175777=CARTESIAN_POINT('Ctrl Pts',(21.9414466292072,7.64273537442682,12.));
#175778=CARTESIAN_POINT('Ctrl Pts',(21.9251276046545,7.64120009506532,12.));
#175779=CARTESIAN_POINT('Ctrl Pts',(21.9089514909874,7.63962999860927,12.));
#175780=CARTESIAN_POINT('Ctrl Pts',(21.8929196523514,7.63802587492035,12.));
#175781=CARTESIAN_POINT('Ctrl Pts',(21.8770334769496,7.636388530334,12.));
#175782=CARTESIAN_POINT('Ctrl Pts',(21.8612943779089,7.63471878821226,12.));
#175783=CARTESIAN_POINT('Ctrl Pts',(21.8457037941084,7.63301748948936,12.));
#175784=CARTESIAN_POINT('Ctrl Pts',(21.8302631910195,7.63128549323023,12.));
#175785=CARTESIAN_POINT('Ctrl Pts',(21.814974061509,7.62952367718127,12.));
#175786=CARTESIAN_POINT('Ctrl Pts',(21.799837926858,7.62773293842389,12.));
#175787=CARTESIAN_POINT('Ctrl Pts',(21.7848563378021,7.62591419404513,12.));
#175788=CARTESIAN_POINT('Ctrl Pts',(21.7700308755584,7.62406838181166,12.));
#175789=CARTESIAN_POINT('Ctrl Pts',(21.7553631528328,7.62219646084229,12.));
#175790=CARTESIAN_POINT('Ctrl Pts',(21.7408548148656,7.62029941230855,12.));
#175791=CARTESIAN_POINT('Ctrl Pts',(21.7265075407975,7.61837824030538,12.));
#175792=CARTESIAN_POINT('Ctrl Pts',(21.7123230449834,7.61643397270421,12.));
#175793=CARTESIAN_POINT('Ctrl Pts',(21.6983030783322,7.61446766202787,12.));
#175794=CARTESIAN_POINT('Ctrl Pts',(21.6844494295815,7.61248038630269,12.));
#175795=CARTESIAN_POINT('Ctrl Pts',(21.6707639267576,7.61047325000956,12.));
#175796=CARTESIAN_POINT('Ctrl Pts',(21.6572484388081,7.60844738512874,12.));
#175797=CARTESIAN_POINT('Ctrl Pts',(21.6439048771743,7.60640395216357,12.));
#175798=CARTESIAN_POINT('Ctrl Pts',(21.6307351973822,7.60434414118296,12.));
#175799=CARTESIAN_POINT('Ctrl Pts',(21.617741400599,7.60226917285429,12.));
#175800=CARTESIAN_POINT('Ctrl Pts',(21.6049255358843,7.60018029988241,12.));
#175801=CARTESIAN_POINT('Ctrl Pts',(21.5922897024466,7.59807880846195,12.));
#175802=CARTESIAN_POINT('Ctrl Pts',(21.5798360518978,7.59596601973584,12.));
#175803=CARTESIAN_POINT('Ctrl Pts',(21.5675667904726,7.59384329124918,12.));
#175804=CARTESIAN_POINT('Ctrl Pts',(21.5554841813462,7.59171201844777,12.));
#175805=CARTESIAN_POINT('Ctrl Pts',(21.543590547011,7.58957363620014,12.));
#175806=CARTESIAN_POINT('Ctrl Pts',(21.5318882716736,7.58742962034834,12.));
#175807=CARTESIAN_POINT('Ctrl Pts',(21.5203798035299,7.5852814891913,12.));
#175808=CARTESIAN_POINT('Ctrl Pts',(21.5090676573873,7.5831308051918,12.));
#175809=CARTESIAN_POINT('Ctrl Pts',(21.4979544192744,7.58097917790744,12.));
#175810=CARTESIAN_POINT('Ctrl Pts',(21.4870427508194,7.57882826679132,12.));
#175811=CARTESIAN_POINT('Ctrl Pts',(21.4763353936762,7.57667978402987,12.));
#175812=CARTESIAN_POINT('Ctrl Pts',(21.4658351740128,7.57453549743412,12.));
#175813=CARTESIAN_POINT('Ctrl Pts',(21.4555450053142,7.57239723223506,12.));
#175814=CARTESIAN_POINT('Ctrl Pts',(21.4454678907509,7.57026687261166,12.));
#175815=CARTESIAN_POINT('Ctrl Pts',(21.4356069261513,7.56814636360848,12.));
#175816=CARTESIAN_POINT('Ctrl Pts',(21.4259653015736,7.56603771218712,12.));
#175817=CARTESIAN_POINT('Ctrl Pts',(21.4165463106254,7.56394299313685,12.));
#175818=CARTESIAN_POINT('Ctrl Pts',(21.4073533630365,7.56186435703622,12.));
#175819=CARTESIAN_POINT('Ctrl Pts',(21.3983899952987,7.55980403700611,12.));
#175820=CARTESIAN_POINT('Ctrl Pts',(21.3896598842117,7.55776435731417,12.));
#175821=CARTESIAN_POINT('Ctrl Pts',(21.3811668478932,7.55574773403503,12.));
#175822=CARTESIAN_POINT('Ctrl Pts',(21.3729148390243,7.55375667080029,12.));
#175823=CARTESIAN_POINT('Ctrl Pts',(21.3649079431865,7.55179375777444,12.));
#175824=CARTESIAN_POINT('Ctrl Pts',(21.3571503685855,7.5498616652131,12.));
#175825=CARTESIAN_POINT('Ctrl Pts',(21.3496464761531,7.54796316246331,12.));
#175826=CARTESIAN_POINT('Ctrl Pts',(21.3424008295038,7.54610114948347,12.));
#175827=CARTESIAN_POINT('Ctrl Pts',(21.3354182340149,7.54427868151268,12.));
#175828=CARTESIAN_POINT('Ctrl Pts',(21.328703791771,7.54249900377031,12.));
#175829=CARTESIAN_POINT('Ctrl Pts',(21.3222628524165,7.54076552038279,12.));
#175830=CARTESIAN_POINT('Ctrl Pts',(21.3161009456256,7.53908175169899,12.));
#175831=CARTESIAN_POINT('Ctrl Pts',(21.310223716773,7.53745129364616,12.));
#175832=CARTESIAN_POINT('Ctrl Pts',(21.3046368712157,7.53587778251736,12.));
#175833=CARTESIAN_POINT('Ctrl Pts',(21.2993464250717,7.53436505309943,12.));
#175834=CARTESIAN_POINT('Ctrl Pts',(21.2943588989331,7.53291726078527,12.));
#175835=CARTESIAN_POINT('Ctrl Pts',(21.2896816163842,7.53153906987856,12.));
#175836=CARTESIAN_POINT('Ctrl Pts',(21.2853226580657,7.5302356243823,12.));
#175837=CARTESIAN_POINT('Ctrl Pts',(21.2812902781143,7.52901217930408,12.));
#175838=CARTESIAN_POINT('Ctrl Pts',(21.2775925269652,7.52787386225333,12.));
#175839=CARTESIAN_POINT('Ctrl Pts',(21.2742366113579,7.52682526918541,12.));
#175840=CARTESIAN_POINT('Ctrl Pts',(21.2712301573466,7.5258712609553,12.));
#175841=CARTESIAN_POINT('Ctrl Pts',(21.2685823838671,7.52501770333531,12.));
#175842=CARTESIAN_POINT('Ctrl Pts',(21.2663059157058,7.52427261074298,12.));
#175843=CARTESIAN_POINT('Ctrl Pts',(21.2644161259962,7.52364573027553,12.));
#175844=CARTESIAN_POINT('Ctrl Pts',(21.262927782038,7.52314642316199,12.));
#175845=CARTESIAN_POINT('Ctrl Pts',(21.2618521283555,7.5227818224267,12.));
#175846=CARTESIAN_POINT('Ctrl Pts',(21.261326054066,7.52260064231661,12.));
#175847=CARTESIAN_POINT('Ctrl Pts',(21.2611204474866,7.52252744144904,12.));
#175848=CARTESIAN_POINT('Ctrl Pts',(21.2610673466886,7.5225064970397,12.));
#175849=CARTESIAN_POINT('Ctrl Pts',(21.2610617890679,7.52250298901264,12.));
#175850=CARTESIAN_POINT('',(20.7347298079577,7.33627833380046,12.));
#175851=CARTESIAN_POINT('',(10.1343606576251,3.58569854577611,12.));
#175852=CARTESIAN_POINT('',(20.1004996511507,7.63019749246977,12.));
#175853=CARTESIAN_POINT('Origin',(20.56795313141,7.80764394578302,12.));
#175854=CARTESIAN_POINT('',(19.6085639972844,8.8178352198485,12.));
#175855=CARTESIAN_POINT('Origin',(7.32141292029404E-13,2.70312158620511E-13,
12.));
#175856=CARTESIAN_POINT('',(19.84920021178,9.47413589477548,12.));
#175857=CARTESIAN_POINT('Origin',(20.0645771135003,9.02290115519381,12.));
#175858=CARTESIAN_POINT('',(20.353053841303,9.71462809124916,12.));
#175859=CARTESIAN_POINT('',(10.1765269206515,4.85731404562459,12.));
#175860=CARTESIAN_POINT('',(22.8400320311648,12.4230808101438,12.));
#175861=CARTESIAN_POINT('Ctrl Pts',(20.353053841303,9.71462809124916,12.));
#175862=CARTESIAN_POINT('Ctrl Pts',(20.353060251684,9.71462954053042,12.));
#175863=CARTESIAN_POINT('Ctrl Pts',(20.3531126095522,9.71465227853042,12.));
#175864=CARTESIAN_POINT('Ctrl Pts',(20.3533097561886,9.71474590350681,12.));
#175865=CARTESIAN_POINT('Ctrl Pts',(20.3538098605706,9.71498978052021,12.));
#175866=CARTESIAN_POINT('Ctrl Pts',(20.3548282742361,9.71549257088173,12.));
#175867=CARTESIAN_POINT('Ctrl Pts',(20.3562337557875,9.71619192554186,12.));
#175868=CARTESIAN_POINT('Ctrl Pts',(20.3580133103356,9.71708493723096,12.));
#175869=CARTESIAN_POINT('Ctrl Pts',(20.3601498764344,9.71816778328007,12.));
#175870=CARTESIAN_POINT('Ctrl Pts',(20.3626256913981,9.71943648548099,12.));
#175871=CARTESIAN_POINT('Ctrl Pts',(20.3654261611056,9.72088778381081,12.));
#175872=CARTESIAN_POINT('Ctrl Pts',(20.3685406190576,9.7225193072249,12.));
#175873=CARTESIAN_POINT('Ctrl Pts',(20.371960235676,9.72432910043194,12.));
#175874=CARTESIAN_POINT('Ctrl Pts',(20.3756766651951,9.72631531732881,12.));
#175875=CARTESIAN_POINT('Ctrl Pts',(20.3796805893304,9.72847589116542,12.));
#175876=CARTESIAN_POINT('Ctrl Pts',(20.3839624556742,9.73080870123727,12.));
#175877=CARTESIAN_POINT('Ctrl Pts',(20.3885129129912,9.73331167102808,12.));
#175878=CARTESIAN_POINT('Ctrl Pts',(20.3933234845647,9.73598292014243,12.));
#175879=CARTESIAN_POINT('Ctrl Pts',(20.3983866213331,9.73882077613201,12.));
#175880=CARTESIAN_POINT('Ctrl Pts',(20.4036953576549,9.74182369656272,12.));
#175881=CARTESIAN_POINT('Ctrl Pts',(20.4092430879861,9.74499021838538,12.));
#175882=CARTESIAN_POINT('Ctrl Pts',(20.4150232777393,9.74831889242174,12.));
#175883=CARTESIAN_POINT('Ctrl Pts',(20.4210295275817,9.7518082978643,12.));
#175884=CARTESIAN_POINT('Ctrl Pts',(20.4272556476629,9.75545705902418,12.));
#175885=CARTESIAN_POINT('Ctrl Pts',(20.4336957355473,9.75926386289923,12.));
#175886=CARTESIAN_POINT('Ctrl Pts',(20.44034423294,9.76322747195495,12.));
#175887=CARTESIAN_POINT('Ctrl Pts',(20.447195862298,9.76734670980892,12.));
#175888=CARTESIAN_POINT('Ctrl Pts',(20.4542455817527,9.7716204510407,12.));
#175889=CARTESIAN_POINT('Ctrl Pts',(20.4614885274975,9.77604760815529,12.));
#175890=CARTESIAN_POINT('Ctrl Pts',(20.4689199790669,9.78062712373321,12.));
#175891=CARTESIAN_POINT('Ctrl Pts',(20.4765353711586,9.78535797314167,12.));
#175892=CARTESIAN_POINT('Ctrl Pts',(20.4843302955329,9.79023916498656,12.));
#175893=CARTESIAN_POINT('Ctrl Pts',(20.4923005087943,9.79526974288331,12.));
#175894=CARTESIAN_POINT('Ctrl Pts',(20.5004419312107,9.80044878520949,12.));
#175895=CARTESIAN_POINT('Ctrl Pts',(20.5087506310505,9.80577540161088,12.));
#175896=CARTESIAN_POINT('Ctrl Pts',(20.517222812284,9.81124873025282,12.));
#175897=CARTESIAN_POINT('Ctrl Pts',(20.5258548000629,9.81686793455943,12.));
#175898=CARTESIAN_POINT('Ctrl Pts',(20.5346430299517,9.82263220080363,12.));
#175899=CARTESIAN_POINT('Ctrl Pts',(20.5435840460721,9.82854073773878,12.));
#175900=CARTESIAN_POINT('Ctrl Pts',(20.552674497646,9.83459277585315,12.));
#175901=CARTESIAN_POINT('Ctrl Pts',(20.5619111362402,9.84078756677565,12.));
#175902=CARTESIAN_POINT('Ctrl Pts',(20.5712908125139,9.84712438256278,12.));
#175903=CARTESIAN_POINT('Ctrl Pts',(20.5808104710015,9.85360251456981,12.));
#175904=CARTESIAN_POINT('Ctrl Pts',(20.5904671449754,9.86022127232748,12.));
#175905=CARTESIAN_POINT('Ctrl Pts',(20.6002579513699,9.86697998242623,12.));
#175906=CARTESIAN_POINT('Ctrl Pts',(20.6101800854494,9.87387798732956,12.));
#175907=CARTESIAN_POINT('Ctrl Pts',(20.6202308177474,9.88091464472676,12.));
#175908=CARTESIAN_POINT('Ctrl Pts',(20.6304074914087,9.88808932697306,12.));
#175909=CARTESIAN_POINT('Ctrl Pts',(20.6407075193976,9.8954014204912,12.));
#175910=CARTESIAN_POINT('Ctrl Pts',(20.6511283817414,9.90285032516693,12.));
#175911=CARTESIAN_POINT('Ctrl Pts',(20.6616676228315,9.91043545377008,12.));
#175912=CARTESIAN_POINT('Ctrl Pts',(20.6723228488263,9.91815623141289,12.));
#175913=CARTESIAN_POINT('Ctrl Pts',(20.6830917250255,9.92601209498749,12.));
#175914=CARTESIAN_POINT('Ctrl Pts',(20.6939719732484,9.9340024925973,12.));
#175915=CARTESIAN_POINT('Ctrl Pts',(20.7049613692234,9.94212688298236,12.));
#175916=CARTESIAN_POINT('Ctrl Pts',(20.7160577407579,9.95038473514949,12.));
#175917=CARTESIAN_POINT('Ctrl Pts',(20.7272589658751,9.95877552798398,12.));
#175918=CARTESIAN_POINT('Ctrl Pts',(20.7385629709795,9.96729874986202,12.));
#175919=CARTESIAN_POINT('Ctrl Pts',(20.7499677289627,9.9759538982347,12.));
#175920=CARTESIAN_POINT('Ctrl Pts',(20.761471257499,9.98474047926853,12.));
#175921=CARTESIAN_POINT('Ctrl Pts',(20.7730716175417,9.9936580075464,12.));
#175922=CARTESIAN_POINT('Ctrl Pts',(20.7847669117568,10.0027060057389,12.));
#175923=CARTESIAN_POINT('Ctrl Pts',(20.7965552829908,10.0118840042786,12.));
#175924=CARTESIAN_POINT('Ctrl Pts',(20.8084349126888,10.0211915410095,12.));
#175925=CARTESIAN_POINT('Ctrl Pts',(20.8204040196602,10.0306281609435,12.));
#175926=CARTESIAN_POINT('Ctrl Pts',(20.8324608588909,10.0401934160234,12.));
#175927=CARTESIAN_POINT('Ctrl Pts',(20.8446037203402,10.0498868648733,12.));
#175928=CARTESIAN_POINT('Ctrl Pts',(20.8568309277316,10.0597080725375,12.));
#175929=CARTESIAN_POINT('Ctrl Pts',(20.86914083737,10.0696566102218,12.));
#175930=CARTESIAN_POINT('Ctrl Pts',(20.881531837184,10.0797320551154,12.));
#175931=CARTESIAN_POINT('Ctrl Pts',(20.894002345737,10.0899339901916,12.));
#175932=CARTESIAN_POINT('Ctrl Pts',(20.9065508112557,10.1002620040076,12.));
#175933=CARTESIAN_POINT('Ctrl Pts',(20.919175710627,10.1107156904836,12.));
#175934=CARTESIAN_POINT('Ctrl Pts',(20.9318755484734,10.1212946487057,12.));
#175935=CARTESIAN_POINT('Ctrl Pts',(20.9446488563933,10.1319984827908,12.));
#175936=CARTESIAN_POINT('Ctrl Pts',(20.9574941921591,10.1428268017256,12.));
#175937=CARTESIAN_POINT('Ctrl Pts',(20.9704101389369,10.1537792192065,12.));
#175938=CARTESIAN_POINT('Ctrl Pts',(20.9833953044736,10.1648553534568,12.));
#175939=CARTESIAN_POINT('Ctrl Pts',(20.9964483203686,10.1760548270767,12.));
#175940=CARTESIAN_POINT('Ctrl Pts',(21.0095678414486,10.187377266936,12.));
#175941=CARTESIAN_POINT('Ctrl Pts',(21.0227525451107,10.1988223040425,12.));
#175942=CARTESIAN_POINT('Ctrl Pts',(21.0360011306815,10.2103895734123,12.));
#175943=CARTESIAN_POINT('Ctrl Pts',(21.0493123187483,10.2220787139155,12.));
#175944=CARTESIAN_POINT('Ctrl Pts',(21.0626848505663,10.2338893681567,12.));
#175945=CARTESIAN_POINT('Ctrl Pts',(21.0761174875444,10.2458211823912,12.));
#175946=CARTESIAN_POINT('Ctrl Pts',(21.0896090107063,10.2578738064181,12.));
#175947=CARTESIAN_POINT('Ctrl Pts',(21.1031582201627,10.2700468934744,12.));
#175948=CARTESIAN_POINT('Ctrl Pts',(21.1167639345631,10.2823401001072,12.));
#175949=CARTESIAN_POINT('Ctrl Pts',(21.1304249906002,10.2947530860721,12.));
#175950=CARTESIAN_POINT('Ctrl Pts',(21.1441402425843,10.3072855142687,12.));
#175951=CARTESIAN_POINT('Ctrl Pts',(21.1579085619965,10.3199370506544,12.));
#175952=CARTESIAN_POINT('Ctrl Pts',(21.1717288370509,10.3327073641572,12.));
#175953=CARTESIAN_POINT('Ctrl Pts',(21.1855999722416,10.3455961265701,12.));
#175954=CARTESIAN_POINT('Ctrl Pts',(21.199520887919,10.3586030124587,12.));
#175955=CARTESIAN_POINT('Ctrl Pts',(21.2134905199345,10.371727699113,12.));
#175956=CARTESIAN_POINT('Ctrl Pts',(21.22750781927,10.3849698664786,12.));
#175957=CARTESIAN_POINT('Ctrl Pts',(21.2415717516714,10.3983291970846,12.));
#175958=CARTESIAN_POINT('Ctrl Pts',(21.255681297275,10.4118053759588,12.));
#175959=CARTESIAN_POINT('Ctrl Pts',(21.2698354502403,10.42539809054,12.));
#175960=CARTESIAN_POINT('Ctrl Pts',(21.2840332184483,10.4391070306391,12.));
#175961=CARTESIAN_POINT('Ctrl Pts',(21.2982736231931,10.4529318883874,12.));
#175962=CARTESIAN_POINT('Ctrl Pts',(21.3125556988731,10.4668723581768,12.));
#175963=CARTESIAN_POINT('Ctrl Pts',(21.3268784926819,10.4809281365931,12.));
#175964=CARTESIAN_POINT('Ctrl Pts',(21.3412410642904,10.4950989223337,12.));
#175965=CARTESIAN_POINT('Ctrl Pts',(21.3556424855814,10.5093844161685,12.));
#175966=CARTESIAN_POINT('Ctrl Pts',(21.3700818403936,10.5237843209057,12.));
#175967=CARTESIAN_POINT('Ctrl Pts',(21.3845582242602,10.5382983413421,12.));
#175968=CARTESIAN_POINT('Ctrl Pts',(21.3990707441497,10.5529261842108,12.));
#175969=CARTESIAN_POINT('Ctrl Pts',(21.4136185181979,10.5676675581108,12.));
#175970=CARTESIAN_POINT('Ctrl Pts',(21.4282006754631,10.5825221734573,12.));
#175971=CARTESIAN_POINT('Ctrl Pts',(21.4428163557144,10.5974897424622,12.));
#175972=CARTESIAN_POINT('Ctrl Pts',(21.4574647092097,10.6125699790961,12.));
#175973=CARTESIAN_POINT('Ctrl Pts',(21.4721448964766,10.6277625990456,12.));
#175974=CARTESIAN_POINT('Ctrl Pts',(21.4868560880889,10.6430673196607,12.));
#175975=CARTESIAN_POINT('Ctrl Pts',(21.5015974644449,10.6584838598939,12.));
#175976=CARTESIAN_POINT('Ctrl Pts',(21.51636821558,10.6740119402834,12.));
#175977=CARTESIAN_POINT('Ctrl Pts',(21.5311675409807,10.689651282929,12.));
#175978=CARTESIAN_POINT('Ctrl Pts',(21.5459946493955,10.7054016114571,12.));
#175979=CARTESIAN_POINT('Ctrl Pts',(21.5608487586468,10.7212626509816,12.));
#175980=CARTESIAN_POINT('Ctrl Pts',(21.5757290954371,10.7372341280467,12.));
#175981=CARTESIAN_POINT('Ctrl Pts',(21.5906348951743,10.7533157705941,12.));
#175982=CARTESIAN_POINT('Ctrl Pts',(21.6055654018176,10.7695073079552,12.));
#175983=CARTESIAN_POINT('Ctrl Pts',(21.6205198677173,10.7858084708261,12.));
#175984=CARTESIAN_POINT('Ctrl Pts',(21.6354975534557,10.8022189912369,12.));
#175985=CARTESIAN_POINT('Ctrl Pts',(21.6504977276866,10.8187386025136,12.));
#175986=CARTESIAN_POINT('Ctrl Pts',(21.6655196669732,10.8353670392272,12.));
#175987=CARTESIAN_POINT('Ctrl Pts',(21.6805626556467,10.8521040371835,12.));
#175988=CARTESIAN_POINT('Ctrl Pts',(21.6956259856672,10.8689493334095,12.));
#175989=CARTESIAN_POINT('Ctrl Pts',(21.7107089564825,10.8859026661293,12.));
#175990=CARTESIAN_POINT('Ctrl Pts',(21.7258108748873,10.902963774734,12.));
#175991=CARTESIAN_POINT('Ctrl Pts',(21.7409310548797,10.9201323997384,12.));
#175992=CARTESIAN_POINT('Ctrl Pts',(21.7560688175247,10.9374082827444,12.));
#175993=CARTESIAN_POINT('Ctrl Pts',(21.7712234908464,10.9547911664455,12.));
#175994=CARTESIAN_POINT('Ctrl Pts',(21.7863944097141,10.9722807946156,12.));
#175995=CARTESIAN_POINT('Ctrl Pts',(21.8015809157301,10.9898769120912,12.));
#175996=CARTESIAN_POINT('Ctrl Pts',(21.8167823571168,11.0075792647477,12.));
#175997=CARTESIAN_POINT('Ctrl Pts',(21.8319980886033,11.0253875994598,12.));
#175998=CARTESIAN_POINT('Ctrl Pts',(21.8472274713103,11.0433016640807,12.));
#175999=CARTESIAN_POINT('Ctrl Pts',(21.8624698726318,11.0613212074363,12.));
#176000=CARTESIAN_POINT('Ctrl Pts',(21.877724666119,11.0794459793057,12.));
#176001=CARTESIAN_POINT('Ctrl Pts',(21.8929912313608,11.0976757303944,12.));
#176002=CARTESIAN_POINT('Ctrl Pts',(21.9082689538688,11.1160102123024,12.));
#176003=CARTESIAN_POINT('Ctrl Pts',(21.923557224952,11.1344491774741,12.));
#176004=CARTESIAN_POINT('Ctrl Pts',(21.9388554416439,11.1529923792003,12.));
#176005=CARTESIAN_POINT('Ctrl Pts',(21.9541630066506,11.1716395716376,12.));
#176006=CARTESIAN_POINT('Ctrl Pts',(21.9694793282914,11.190390509811,12.));
#176007=CARTESIAN_POINT('Ctrl Pts',(21.9848038204439,11.2092449496125,12.));
#176008=CARTESIAN_POINT('Ctrl Pts',(22.0001359024839,11.2282026477896,12.));
#176009=CARTESIAN_POINT('Ctrl Pts',(22.0154749992363,11.2472633619275,12.));
#176010=CARTESIAN_POINT('Ctrl Pts',(22.030820540835,11.2664268504206,12.));
#176011=CARTESIAN_POINT('Ctrl Pts',(22.046171962566,11.2856928724374,12.));
#176012=CARTESIAN_POINT('Ctrl Pts',(22.0615287047179,11.3050611878771,12.));
#176013=CARTESIAN_POINT('Ctrl Pts',(22.0768902124267,11.3245315573168,12.));
#176014=CARTESIAN_POINT('Ctrl Pts',(22.0922559355294,11.3441037419553,12.));
#176015=CARTESIAN_POINT('Ctrl Pts',(22.1076253283979,11.3637775035367,12.));
#176016=CARTESIAN_POINT('Ctrl Pts',(22.1229978500186,11.3835526044256,12.));
#176017=CARTESIAN_POINT('Ctrl Pts',(22.1383729640964,11.4034288076908,12.));
#176018=CARTESIAN_POINT('Ctrl Pts',(22.1537501391487,11.4234058771742,12.));
#176019=CARTESIAN_POINT('Ctrl Pts',(22.1691288486096,11.443483577557,12.));
#176020=CARTESIAN_POINT('Ctrl Pts',(22.184508570917,11.463661674411,12.));
#176021=CARTESIAN_POINT('Ctrl Pts',(22.1998887896436,11.483939934259,12.));
#176022=CARTESIAN_POINT('Ctrl Pts',(22.2152689931022,11.5043181244242,12.));
#176023=CARTESIAN_POINT('Ctrl Pts',(22.2306486738901,11.5247960128477,12.));
#176024=CARTESIAN_POINT('Ctrl Pts',(22.2460273284654,11.5453733679121,12.));
#176025=CARTESIAN_POINT('Ctrl Pts',(22.2614044566898,11.5660499582403,12.));
#176026=CARTESIAN_POINT('Ctrl Pts',(22.2767795614348,11.5868255525188,12.));
#176027=CARTESIAN_POINT('Ctrl Pts',(22.2921521480356,11.6076999192357,12.));
#176028=CARTESIAN_POINT('Ctrl Pts',(22.3075217249049,11.6286728270009,12.));
#176029=CARTESIAN_POINT('Ctrl Pts',(22.3228878043976,11.6497440449857,12.));
#176030=CARTESIAN_POINT('Ctrl Pts',(22.3382499035619,11.6709133432985,12.));
#176031=CARTESIAN_POINT('Ctrl Pts',(22.3536075450029,11.6921804934056,12.));
#176032=CARTESIAN_POINT('Ctrl Pts',(22.3689602575491,11.7135452684532,12.));
#176033=CARTESIAN_POINT('Ctrl Pts',(22.3843075773899,11.7350074437961,12.));
#176034=CARTESIAN_POINT('Ctrl Pts',(22.3996490469191,11.7565667964764,12.));
#176035=CARTESIAN_POINT('Ctrl Pts',(22.4149842125008,11.7782231042039,12.));
#176036=CARTESIAN_POINT('Ctrl Pts',(22.430312622646,11.7999761445173,12.));
#176037=CARTESIAN_POINT('Ctrl Pts',(22.4456338258735,11.8218256937889,12.));
#176038=CARTESIAN_POINT('Ctrl Pts',(22.4609473690471,11.8437715264487,12.));
#176039=CARTESIAN_POINT('Ctrl Pts',(22.4762527946702,11.8658134137019,12.));
#176040=CARTESIAN_POINT('Ctrl Pts',(22.4915496418485,11.8879511239943,12.));
#176041=CARTESIAN_POINT('Ctrl Pts',(22.5068374513973,11.9101844254557,12.));
#176042=CARTESIAN_POINT('Ctrl Pts',(22.5221157697883,11.9325130877803,12.));
#176043=CARTESIAN_POINT('Ctrl Pts',(22.5373841537307,11.9549368843997,12.));
#176044=CARTESIAN_POINT('Ctrl Pts',(22.5526421741158,11.9774555943496,12.));
#176045=CARTESIAN_POINT('Ctrl Pts',(22.5678894211181,12.0000690046695,12.));
#176046=CARTESIAN_POINT('Ctrl Pts',(22.5831255061282,12.0227769113127,12.));
#176047=CARTESIAN_POINT('Ctrl Pts',(22.5983500505644,12.0455791139128,12.));
#176048=CARTESIAN_POINT('Ctrl Pts',(22.6135626764898,12.0684754113862,12.));
#176049=CARTESIAN_POINT('Ctrl Pts',(22.6287629967056,12.0914655972823,12.));
#176050=CARTESIAN_POINT('Ctrl Pts',(22.6439506046605,12.1145494550383,12.));
#176051=CARTESIAN_POINT('Ctrl Pts',(22.6591250653965,12.1377267537145,12.));
#176052=CARTESIAN_POINT('Ctrl Pts',(22.6742859034944,12.1609972423099,12.));
#176053=CARTESIAN_POINT('Ctrl Pts',(22.6894326205037,12.1843606579262,12.));
#176054=CARTESIAN_POINT('Ctrl Pts',(22.7045647168747,12.2078167360284,12.));
#176055=CARTESIAN_POINT('Ctrl Pts',(22.7196817119374,12.2313652198061,12.));
#176056=CARTESIAN_POINT('Ctrl Pts',(22.7347831655287,12.2550058702395,12.));
#176057=CARTESIAN_POINT('Ctrl Pts',(22.7498686970069,12.2787384750742,12.));
#176058=CARTESIAN_POINT('Ctrl Pts',(22.764938010105,12.3025628601792,12.));
#176059=CARTESIAN_POINT('Ctrl Pts',(22.7799908974768,12.3264788926075,12.));
#176060=CARTESIAN_POINT('Ctrl Pts',(22.795027221673,12.3504864740319,12.));
#176061=CARTESIAN_POINT('Ctrl Pts',(22.81004690224,12.374585536673,12.));
#176062=CARTESIAN_POINT('Ctrl Pts',(22.8220493007173,12.3939379378998,12.));
#176063=CARTESIAN_POINT('Ctrl Pts',(22.8310435872747,12.4084933766347,12.));
#176064=CARTESIAN_POINT('Ctrl Pts',(22.8370364396459,12.418215285186,12.));
#176065=CARTESIAN_POINT('Ctrl Pts',(22.8400320311648,12.4230808101438,12.));
#176066=CARTESIAN_POINT('',(22.1787195904339,13.5685075571671,12.));
#176067=CARTESIAN_POINT('Origin',(0.,0.,12.));
#176068=CARTESIAN_POINT('',(18.5896416359912,12.7689476255363,12.));
#176069=CARTESIAN_POINT('Ctrl Pts',(22.1787195904339,13.5685075571671,12.));
#176070=CARTESIAN_POINT('Ctrl Pts',(22.1730081264608,13.5683460612942,12.));
#176071=CARTESIAN_POINT('Ctrl Pts',(22.1615922805008,13.5680170531805,12.));
#176072=CARTESIAN_POINT('Ctrl Pts',(22.1444897575194,13.5675054919061,12.));
#176073=CARTESIAN_POINT('Ctrl Pts',(22.1217288871975,13.5667873105359,12.));
#176074=CARTESIAN_POINT('Ctrl Pts',(22.0933486464593,13.5658294169284,12.));
#176075=CARTESIAN_POINT('Ctrl Pts',(22.0650393089609,13.5648113689033,12.));
#176076=CARTESIAN_POINT('Ctrl Pts',(22.0368009736295,13.5637332022473,12.));
#176077=CARTESIAN_POINT('Ctrl Pts',(22.0086337943449,13.5625949868333,12.));
#176078=CARTESIAN_POINT('Ctrl Pts',(21.9805379899168,13.5613968357561,12.));
#176079=CARTESIAN_POINT('Ctrl Pts',(21.9525138592813,13.5601389185257,12.));
#176080=CARTESIAN_POINT('Ctrl Pts',(21.9245617765769,13.5588214586604,12.));
#176081=CARTESIAN_POINT('Ctrl Pts',(21.8966821688824,13.5574447178425,12.));
#176082=CARTESIAN_POINT('Ctrl Pts',(21.8688754989365,13.5560089839385,12.));
#176083=CARTESIAN_POINT('Ctrl Pts',(21.8411422456075,13.5545145573031,12.));
#176084=CARTESIAN_POINT('Ctrl Pts',(21.8134828857967,13.5529617381573,12.));
#176085=CARTESIAN_POINT('Ctrl Pts',(21.7858978745865,13.551350812725,12.));
#176086=CARTESIAN_POINT('Ctrl Pts',(21.7583876294554,13.5496820422211,12.));
#176087=CARTESIAN_POINT('Ctrl Pts',(21.7309525412281,13.5479556704481,12.));
#176088=CARTESIAN_POINT('Ctrl Pts',(21.7035929822955,13.5461719295048,12.));
#176089=CARTESIAN_POINT('Ctrl Pts',(21.6763093157699,13.5443310461526,12.));
#176090=CARTESIAN_POINT('Ctrl Pts',(21.6491019044648,13.5424332480699,12.));
#176091=CARTESIAN_POINT('Ctrl Pts',(21.6219711193946,13.5404787697792,12.));
#176092=CARTESIAN_POINT('Ctrl Pts',(21.5949173499013,13.5384678597195,12.));
#176093=CARTESIAN_POINT('Ctrl Pts',(21.5679410019001,13.536400779028,12.));
#176094=CARTESIAN_POINT('Ctrl Pts',(21.5410424932503,13.5342777983215,12.));
#176095=CARTESIAN_POINT('Ctrl Pts',(21.5142222501666,13.5320991952138,12.));
#176096=CARTESIAN_POINT('Ctrl Pts',(21.4874807030468,13.5298652514355,12.));
#176097=CARTESIAN_POINT('Ctrl Pts',(21.4608182828697,13.5275762503555,12.));
#176098=CARTESIAN_POINT('Ctrl Pts',(21.4342354165259,13.5252324737802,12.));
#176099=CARTESIAN_POINT('Ctrl Pts',(21.4077325259324,13.5228342013516,12.));
#176100=CARTESIAN_POINT('Ctrl Pts',(21.3813100304973,13.5203817122504,12.));
#176101=CARTESIAN_POINT('Ctrl Pts',(21.3549683486222,13.5178752862466,12.));
#176102=CARTESIAN_POINT('Ctrl Pts',(21.3287078996341,13.5153152050555,12.));
#176103=CARTESIAN_POINT('Ctrl Pts',(21.3025291054235,13.5127017534971,12.));
#176104=CARTESIAN_POINT('Ctrl Pts',(21.2764323924442,13.5100352209205,12.));
#176105=CARTESIAN_POINT('Ctrl Pts',(21.250418192743,13.5073159019452,12.));
#176106=CARTESIAN_POINT('Ctrl Pts',(21.2244869429332,13.5045440957404,12.));
#176107=CARTESIAN_POINT('Ctrl Pts',(21.1986390835828,13.5017201056088,12.));
#176108=CARTESIAN_POINT('Ctrl Pts',(21.1728750584175,13.4988442384491,12.));
#176109=CARTESIAN_POINT('Ctrl Pts',(21.1471953136209,13.4959168042934,12.));
#176110=CARTESIAN_POINT('Ctrl Pts',(21.1216002970207,13.4929381157778,12.));
#176111=CARTESIAN_POINT('Ctrl Pts',(21.0960904575046,13.4899084877717,12.));
#176112=CARTESIAN_POINT('Ctrl Pts',(21.0706662455199,13.4868282377191,12.));
#176113=CARTESIAN_POINT('Ctrl Pts',(21.0453281134245,13.4836976858912,12.));
#176114=CARTESIAN_POINT('Ctrl Pts',(21.0200765158884,13.4805171556822,12.));
#176115=CARTESIAN_POINT('Ctrl Pts',(20.9949119102592,13.4772869738879,12.));
#176116=CARTESIAN_POINT('Ctrl Pts',(20.9698347569477,13.4740074710086,12.));
#176117=CARTESIAN_POINT('Ctrl Pts',(20.9448455197557,13.4706789815166,12.));
#176118=CARTESIAN_POINT('Ctrl Pts',(20.9199446657583,13.4673018437717,12.));
#176119=CARTESIAN_POINT('Ctrl Pts',(20.8951326652158,13.4638763999725,12.));
#176120=CARTESIAN_POINT('Ctrl Pts',(20.8704099914641,13.4604029960983,12.));
#176121=CARTESIAN_POINT('Ctrl Pts',(20.8457771208083,13.4568819818631,12.));
#176122=CARTESIAN_POINT('Ctrl Pts',(20.821234532398,13.4533137106667,12.));
#176123=CARTESIAN_POINT('Ctrl Pts',(20.7967827081228,13.4496985395637,12.));
#176124=CARTESIAN_POINT('Ctrl Pts',(20.7724221327609,13.4460368293689,12.));
#176125=CARTESIAN_POINT('Ctrl Pts',(20.7481532941014,13.4423289447561,12.));
#176126=CARTESIAN_POINT('Ctrl Pts',(20.7239766830675,13.4385752543663,12.));
#176127=CARTESIAN_POINT('Ctrl Pts',(20.6998927938288,13.4347761309154,12.));
#176128=CARTESIAN_POINT('Ctrl Pts',(20.6759021239102,13.4309319513119,12.));
#176129=CARTESIAN_POINT('Ctrl Pts',(20.6520051742867,13.4270430967651,12.));
#176130=CARTESIAN_POINT('Ctrl Pts',(20.6282024494234,13.4231099528178,12.));
#176131=CARTESIAN_POINT('Ctrl Pts',(20.6044944573151,13.4191329093932,12.));
#176132=CARTESIAN_POINT('Ctrl Pts',(20.5808817095155,13.4151123608411,12.));
#176133=CARTESIAN_POINT('Ctrl Pts',(20.557364721164,13.4110487059912,12.));
#176134=CARTESIAN_POINT('Ctrl Pts',(20.5339440109957,13.4069423482077,12.));
#176135=CARTESIAN_POINT('Ctrl Pts',(20.5106201013755,13.4027936954529,12.));
#176136=CARTESIAN_POINT('Ctrl Pts',(20.4873935184041,13.3986031603716,12.));
#176137=CARTESIAN_POINT('Ctrl Pts',(20.4642647920038,13.3943711603739,12.));
#176138=CARTESIAN_POINT('Ctrl Pts',(20.4412344560007,13.3900981177254,12.));
#176139=CARTESIAN_POINT('Ctrl Pts',(20.4183030482002,13.3857844596387,12.));
#176140=CARTESIAN_POINT('Ctrl Pts',(20.3954711104504,13.3814306183721,12.));
#176141=CARTESIAN_POINT('Ctrl Pts',(20.3727391887187,13.377037031319,12.));
#176142=CARTESIAN_POINT('Ctrl Pts',(20.3501078331818,13.372604141087,12.));
#176143=CARTESIAN_POINT('Ctrl Pts',(20.3275775983032,13.3681323955828,12.));
#176144=CARTESIAN_POINT('Ctrl Pts',(20.3051490429049,13.3636222481017,12.));
#176145=CARTESIAN_POINT('Ctrl Pts',(20.2828227302337,13.3590741574194,12.));
#176146=CARTESIAN_POINT('Ctrl Pts',(20.2605992280117,13.3544885878886,12.));
#176147=CARTESIAN_POINT('Ctrl Pts',(20.2384791085354,13.3498660095382,12.));
#176148=CARTESIAN_POINT('Ctrl Pts',(20.2164629487855,13.3452068981763,12.));
#176149=CARTESIAN_POINT('Ctrl Pts',(20.1945513305233,13.3405117354969,12.));
#176150=CARTESIAN_POINT('Ctrl Pts',(20.1727448403818,13.3357810091903,12.));
#176151=CARTESIAN_POINT('Ctrl Pts',(20.1510440699477,13.3310152130565,12.));
#176152=CARTESIAN_POINT('Ctrl Pts',(20.1294496158405,13.3262148471228,12.));
#176153=CARTESIAN_POINT('Ctrl Pts',(20.1079620798377,13.3213804177588,12.));
#176154=CARTESIAN_POINT('Ctrl Pts',(20.0865820689883,13.3165124377963,12.));
#176155=CARTESIAN_POINT('Ctrl Pts',(20.0653101957188,13.3116114266514,12.));
#176156=CARTESIAN_POINT('Ctrl Pts',(20.0441470779345,13.3066779104515,12.));
#176157=CARTESIAN_POINT('Ctrl Pts',(20.0230933391039,13.3017124221639,12.));
#176158=CARTESIAN_POINT('Ctrl Pts',(20.0021496083742,13.296715501731,12.));
#176159=CARTESIAN_POINT('Ctrl Pts',(19.9813165207174,13.2916876962098,12.));
#176160=CARTESIAN_POINT('Ctrl Pts',(19.9605947170589,13.2866295599152,12.));
#176161=CARTESIAN_POINT('Ctrl Pts',(19.9399848444019,13.2815416545663,12.));
#176162=CARTESIAN_POINT('Ctrl Pts',(19.9194875559419,13.2764245494354,12.));
#176163=CARTESIAN_POINT('Ctrl Pts',(19.8991035111739,13.2712788215015,12.));
#176164=CARTESIAN_POINT('Ctrl Pts',(19.8788333760571,13.2661050556128,12.));
#176165=CARTESIAN_POINT('Ctrl Pts',(19.8586778231711,13.2609038446525,12.));
#176166=CARTESIAN_POINT('Ctrl Pts',(19.8386375318632,13.2556757897085,12.));
#176167=CARTESIAN_POINT('Ctrl Pts',(19.8187131883919,13.2504215002458,12.));
#176168=CARTESIAN_POINT('Ctrl Pts',(19.7989054860501,13.2451415942809,12.));
#176169=CARTESIAN_POINT('Ctrl Pts',(19.7792151253297,13.239836698568,12.));
#176170=CARTESIAN_POINT('Ctrl Pts',(19.7596428141176,13.2345074487968,12.));
#176171=CARTESIAN_POINT('Ctrl Pts',(19.7401892678701,13.2291544897902,12.));
#176172=CARTESIAN_POINT('Ctrl Pts',(19.7208552097867,13.2237784757065,12.));
#176173=CARTESIAN_POINT('Ctrl Pts',(19.7016413709678,13.2183800702431,12.));
#176174=CARTESIAN_POINT('Ctrl Pts',(19.6825484905812,13.2129599468478,12.));
#176175=CARTESIAN_POINT('Ctrl Pts',(19.6635773160924,13.2075187889522,12.));
#176176=CARTESIAN_POINT('Ctrl Pts',(19.6447286034764,13.202057290206,12.));
#176177=CARTESIAN_POINT('Ctrl Pts',(19.6260031174244,13.196576154715,12.));
#176178=CARTESIAN_POINT('Ctrl Pts',(19.6074016315421,13.1910760972818,12.));
#176179=CARTESIAN_POINT('Ctrl Pts',(19.5889249285352,13.185557843648,12.));
#176180=CARTESIAN_POINT('Ctrl Pts',(19.5705738004682,13.1800221307683,12.));
#176181=CARTESIAN_POINT('Ctrl Pts',(19.5523490490254,13.1744697070918,12.));
#176182=CARTESIAN_POINT('Ctrl Pts',(19.5342514857564,13.1689013328432,12.));
#176183=CARTESIAN_POINT('Ctrl Pts',(19.5162819323207,13.1633177803097,12.));
#176184=CARTESIAN_POINT('Ctrl Pts',(19.498441220707,13.1577198341238,12.));
#176185=CARTESIAN_POINT('Ctrl Pts',(19.4807301935256,13.1521082915846,12.));
#176186=CARTESIAN_POINT('Ctrl Pts',(19.463149704325,13.1464839629966,12.));
#176187=CARTESIAN_POINT('Ctrl Pts',(19.4457006178875,13.140847672006,12.));
#176188=CARTESIAN_POINT('Ctrl Pts',(19.4283838105265,13.135200255944,12.));
#176189=CARTESIAN_POINT('Ctrl Pts',(19.4112001703561,13.1295425661635,12.));
#176190=CARTESIAN_POINT('Ctrl Pts',(19.3941505976267,13.1238754684177,12.));
#176191=CARTESIAN_POINT('Ctrl Pts',(19.3772360051093,13.118199843271,12.));
#176192=CARTESIAN_POINT('Ctrl Pts',(19.3604573184516,13.1125165865021,12.));
#176193=CARTESIAN_POINT('Ctrl Pts',(19.3438154765395,13.1068266095186,12.));
#176194=CARTESIAN_POINT('Ctrl Pts',(19.3273114318268,13.1011308397592,12.));
#176195=CARTESIAN_POINT('Ctrl Pts',(19.3109461507358,13.095430221148,12.));
#176196=CARTESIAN_POINT('Ctrl Pts',(19.2947206141246,13.089725714597,12.));
#176197=CARTESIAN_POINT('Ctrl Pts',(19.2786358177198,13.0840182984949,12.));
#176198=CARTESIAN_POINT('Ctrl Pts',(19.2626927725596,13.0783089692118,12.));
#176199=CARTESIAN_POINT('Ctrl Pts',(19.2468925053988,13.0725987415856,12.));
#176200=CARTESIAN_POINT('Ctrl Pts',(19.2312360592031,13.0668886494791,12.));
#176201=CARTESIAN_POINT('Ctrl Pts',(19.2157244937141,13.0611797463913,12.));
#176202=CARTESIAN_POINT('Ctrl Pts',(19.2003588859771,13.0554731060537,12.));
#176203=CARTESIAN_POINT('Ctrl Pts',(19.1851403308825,13.0497698230442,12.));
#176204=CARTESIAN_POINT('Ctrl Pts',(19.1700699416625,13.0440710133775,12.));
#176205=CARTESIAN_POINT('Ctrl Pts',(19.1551488505233,13.0383778152072,12.));
#176206=CARTESIAN_POINT('Ctrl Pts',(19.1403782093389,13.0326913895841,12.));
#176207=CARTESIAN_POINT('Ctrl Pts',(19.1257591903099,13.0270129211976,12.));
#176208=CARTESIAN_POINT('Ctrl Pts',(19.1112929866308,13.0213436191326,12.));
#176209=CARTESIAN_POINT('Ctrl Pts',(19.0969808131226,13.0156847176094,12.));
#176210=CARTESIAN_POINT('Ctrl Pts',(19.0828239070482,13.0100374768786,12.));
#176211=CARTESIAN_POINT('Ctrl Pts',(19.0688235289437,13.0044031841381,12.));
#176212=CARTESIAN_POINT('Ctrl Pts',(19.0549809634355,12.9987831544502,12.));
#176213=CARTESIAN_POINT('Ctrl Pts',(19.0412975200398,12.9931787316515,12.));
#176214=CARTESIAN_POINT('Ctrl Pts',(19.0277745339908,12.9875912893003,12.));
#176215=CARTESIAN_POINT('Ctrl Pts',(19.0144133673348,12.9820222318716,12.));
#176216=CARTESIAN_POINT('Ctrl Pts',(19.0012154099791,12.9764729959205,12.));
#176217=CARTESIAN_POINT('Ctrl Pts',(18.9881820807585,12.9709450512747,12.));
#176218=CARTESIAN_POINT('Ctrl Pts',(18.9753148284475,12.9654399021869,12.));
#176219=CARTESIAN_POINT('Ctrl Pts',(18.9626151329229,12.9599590886319,12.));
#176220=CARTESIAN_POINT('Ctrl Pts',(18.9500845064715,12.9545041877377,12.));
#176221=CARTESIAN_POINT('Ctrl Pts',(18.9377244950435,12.9490768151821,12.));
#176222=CARTESIAN_POINT('Ctrl Pts',(18.9255366795195,12.9436786266105,12.));
#176223=CARTESIAN_POINT('Ctrl Pts',(18.9135226769465,12.9383113190375,12.));
#176224=CARTESIAN_POINT('Ctrl Pts',(18.9016841423403,12.9329766328185,12.));
#176225=CARTESIAN_POINT('Ctrl Pts',(18.8900227704889,12.9276763536373,12.));
#176226=CARTESIAN_POINT('Ctrl Pts',(18.8785402977527,12.9224123144982,12.));
#176227=CARTESIAN_POINT('Ctrl Pts',(18.8672385038326,12.9171863977045,12.));
#176228=CARTESIAN_POINT('Ctrl Pts',(18.8561192136198,12.9120005369063,12.));
#176229=CARTESIAN_POINT('Ctrl Pts',(18.8451842990984,12.9068567191854,12.));
#176230=CARTESIAN_POINT('Ctrl Pts',(18.834435681259,12.9017569871738,12.));
#176231=CARTESIAN_POINT('Ctrl Pts',(18.8238753319129,12.8967034410755,12.));
#176232=CARTESIAN_POINT('Ctrl Pts',(18.813505275782,12.8916982409935,12.));
#176233=CARTESIAN_POINT('Ctrl Pts',(18.8033275941943,12.8867436109546,12.));
#176234=CARTESIAN_POINT('Ctrl Pts',(18.7933444285868,12.8818418427475,12.));
#176235=CARTESIAN_POINT('Ctrl Pts',(18.7835579840477,12.8769952998095,12.));
#176236=CARTESIAN_POINT('Ctrl Pts',(18.7739705329022,12.872206421181,12.));
#176237=CARTESIAN_POINT('Ctrl Pts',(18.7645844169564,12.8674777239653,12.));
#176238=CARTESIAN_POINT('Ctrl Pts',(18.7554020493887,12.8628118054171,12.));
#176239=CARTESIAN_POINT('Ctrl Pts',(18.7464259171251,12.8582113455646,12.));
#176240=CARTESIAN_POINT('Ctrl Pts',(18.7376585820854,12.8536791086316,12.));
#176241=CARTESIAN_POINT('Ctrl Pts',(18.7291026886554,12.8492179511591,12.));
#176242=CARTESIAN_POINT('Ctrl Pts',(18.7207609737702,12.8448308329494,12.));
#176243=CARTESIAN_POINT('Ctrl Pts',(18.7126362754445,12.8405208263431,12.));
#176244=CARTESIAN_POINT('Ctrl Pts',(18.7047315436294,12.8362911280361,12.));
#176245=CARTESIAN_POINT('Ctrl Pts',(18.6970498410172,12.8321450599789,12.));
#176246=CARTESIAN_POINT('Ctrl Pts',(18.6895943376171,12.8280860635231,12.));
#176247=CARTESIAN_POINT('Ctrl Pts',(18.6823683094139,12.8241176980017,12.));
#176248=CARTESIAN_POINT('Ctrl Pts',(18.6753751301092,12.8202436318474,12.));
#176249=CARTESIAN_POINT('Ctrl Pts',(18.6686182952799,12.8164676687362,12.));
#176250=CARTESIAN_POINT('Ctrl Pts',(18.6621014624746,12.8127937909631,12.));
#176251=CARTESIAN_POINT('Ctrl Pts',(18.6558284825773,12.8092261933858,12.));
#176252=CARTESIAN_POINT('Ctrl Pts',(18.6498034438987,12.805769331162,12.));
#176253=CARTESIAN_POINT('Ctrl Pts',(18.6440306327456,12.8024278770153,12.));
#176254=CARTESIAN_POINT('Ctrl Pts',(18.63851447924,12.7992066625264,12.));
#176255=CARTESIAN_POINT('Ctrl Pts',(18.6332595057006,12.7961106222251,12.));
#176256=CARTESIAN_POINT('Ctrl Pts',(18.6282702819371,12.7931447451555,12.));
#176257=CARTESIAN_POINT('Ctrl Pts',(18.6235516265575,12.7903142925234,12.));
#176258=CARTESIAN_POINT('Ctrl Pts',(18.6191087624752,12.7876249657834,12.));
#176259=CARTESIAN_POINT('Ctrl Pts',(18.6149475565188,12.7850831657901,12.));
#176260=CARTESIAN_POINT('Ctrl Pts',(18.6110744826219,12.7826959526925,12.));
#176261=CARTESIAN_POINT('Ctrl Pts',(18.6074961535723,12.7804705387658,12.));
#176262=CARTESIAN_POINT('Ctrl Pts',(18.6042190183704,12.7784139605066,12.));
#176263=CARTESIAN_POINT('Ctrl Pts',(18.6012488486709,12.7765325225081,12.));
#176264=CARTESIAN_POINT('Ctrl Pts',(18.598591752595,12.7748328937638,12.));
#176265=CARTESIAN_POINT('Ctrl Pts',(18.5962551167772,12.7733231262108,12.));
#176266=CARTESIAN_POINT('Ctrl Pts',(18.5942490615407,12.7720142287172,12.));
#176267=CARTESIAN_POINT('Ctrl Pts',(18.5925859134579,12.7709195951156,12.));
#176268=CARTESIAN_POINT('Ctrl Pts',(18.5912775137806,12.7700520897173,12.));
#176269=CARTESIAN_POINT('Ctrl Pts',(18.5903328777227,12.7694215127919,12.));
#176270=CARTESIAN_POINT('Ctrl Pts',(18.589871621843,12.769110348199,12.));
#176271=CARTESIAN_POINT('Ctrl Pts',(18.5896919669165,12.768986426692,12.));
#176272=CARTESIAN_POINT('Ctrl Pts',(18.5896460962964,12.7689524524483,12.));
#176273=CARTESIAN_POINT('Ctrl Pts',(18.5896416359912,12.7689476255363,12.));
#176274=CARTESIAN_POINT('',(18.1294424696716,12.4528436808172,12.));
#176275=CARTESIAN_POINT('',(8.86099361848466,6.08648437878338,12.));
#176276=CARTESIAN_POINT('',(17.4407513054162,12.572596943457,12.));
#176277=CARTESIAN_POINT('Origin',(17.846350172984,12.8649829188862,12.));
#176278=CARTESIAN_POINT('',(16.6581946899465,13.5924445804218,12.));
#176279=CARTESIAN_POINT('Origin',(6.37232247690086E-13,4.50593605254675E-13,
12.));
#176280=CARTESIAN_POINT('',(16.7207683102834,14.2886635873976,12.));
#176281=CARTESIAN_POINT('Origin',(17.0455945664569,13.9085479427572,12.));
#176282=CARTESIAN_POINT('',(17.1452095830633,14.6513681262571,12.));
#176283=CARTESIAN_POINT('',(8.57260479153162,7.32568406312855,12.));
#176284=CARTESIAN_POINT('',(18.8464468996588,17.9112098770111,12.));
#176285=CARTESIAN_POINT('Ctrl Pts',(17.1452095830633,14.6513681262571,12.));
#176286=CARTESIAN_POINT('Ctrl Pts',(17.1452153999142,14.651371185284,12.));
#176287=CARTESIAN_POINT('Ctrl Pts',(17.1452600887039,14.6514066997188,12.));
#176288=CARTESIAN_POINT('Ctrl Pts',(17.1454262858045,14.6515481598057,12.));
#176289=CARTESIAN_POINT('Ctrl Pts',(17.1458462295273,14.65191316345,12.));
#176290=CARTESIAN_POINT('Ctrl Pts',(17.1466998098673,14.6526624064978,12.));
#176291=CARTESIAN_POINT('Ctrl Pts',(17.1478763944909,14.6537016966188,12.));
#176292=CARTESIAN_POINT('Ctrl Pts',(17.1493641837556,14.6550248622813,12.));
#176293=CARTESIAN_POINT('Ctrl Pts',(17.1511476869495,14.6566237952435,12.));
#176294=CARTESIAN_POINT('Ctrl Pts',(17.1532107762719,14.6584900555301,12.));
#176295=CARTESIAN_POINT('Ctrl Pts',(17.1555401986403,14.660616716964,12.));
#176296=CARTESIAN_POINT('Ctrl Pts',(17.1581262646789,14.662998728599,12.));
#176297=CARTESIAN_POINT('Ctrl Pts',(17.1609609517369,14.6656319165057,12.));
#176298=CARTESIAN_POINT('Ctrl Pts',(17.1640366762304,14.6685123374424,12.));
#176299=CARTESIAN_POINT('Ctrl Pts',(17.1673449723019,14.6716355833321,12.));
#176300=CARTESIAN_POINT('Ctrl Pts',(17.1708771619129,14.6749971333867,12.));
#176301=CARTESIAN_POINT('Ctrl Pts',(17.1746247499057,14.6785925615676,12.));
#176302=CARTESIAN_POINT('Ctrl Pts',(17.1785800350827,14.6824178576167,12.));
#176303=CARTESIAN_POINT('Ctrl Pts',(17.182736158472,14.6864694522319,12.));
#176304=CARTESIAN_POINT('Ctrl Pts',(17.1870867909918,14.6907440526958,12.));
#176305=CARTESIAN_POINT('Ctrl Pts',(17.1916259308415,14.6952385361706,12.));
#176306=CARTESIAN_POINT('Ctrl Pts',(17.1963476411694,14.699949811582,12.));
#176307=CARTESIAN_POINT('Ctrl Pts',(17.2012461084268,14.7048748502663,12.));
#176308=CARTESIAN_POINT('Ctrl Pts',(17.2063157097316,14.7100107213587,12.));
#176309=CARTESIAN_POINT('Ctrl Pts',(17.2115510835988,14.7153546289338,12.));
#176310=CARTESIAN_POINT('Ctrl Pts',(17.2169471814255,14.7209039390326,12.));
#176311=CARTESIAN_POINT('Ctrl Pts',(17.2224992099666,14.7266561494282,12.));
#176312=CARTESIAN_POINT('Ctrl Pts',(17.2282025904314,14.7326088681163,12.));
#176313=CARTESIAN_POINT('Ctrl Pts',(17.2340529062077,14.7387597858117,12.));
#176314=CARTESIAN_POINT('Ctrl Pts',(17.2400458713566,14.7451066593793,12.));
#176315=CARTESIAN_POINT('Ctrl Pts',(17.2461773413289,14.7516473175125,12.));
#176316=CARTESIAN_POINT('Ctrl Pts',(17.2524433146837,14.7583796616617,12.));
#176317=CARTESIAN_POINT('Ctrl Pts',(17.2588399401464,14.7653016697589,12.));
#176318=CARTESIAN_POINT('Ctrl Pts',(17.2653635155317,14.7724113956728,12.));
#176319=CARTESIAN_POINT('Ctrl Pts',(17.2720104735192,14.7797069617802,12.));
#176320=CARTESIAN_POINT('Ctrl Pts',(17.278777370485,14.787186553128,12.));
#176321=CARTESIAN_POINT('Ctrl Pts',(17.28566087332,14.7948484105253,12.));
#176322=CARTESIAN_POINT('Ctrl Pts',(17.2926577496519,14.8026908254281,12.));
#176323=CARTESIAN_POINT('Ctrl Pts',(17.2997648661483,14.8107121391038,12.));
#176324=CARTESIAN_POINT('Ctrl Pts',(17.3069791853705,14.8189107410161,12.));
#176325=CARTESIAN_POINT('Ctrl Pts',(17.3142977632656,14.8272850675375,12.));
#176326=CARTESIAN_POINT('Ctrl Pts',(17.3217177462096,14.8358336004193,12.));
#176327=CARTESIAN_POINT('Ctrl Pts',(17.3292363662601,14.8445548643505,12.));
#176328=CARTESIAN_POINT('Ctrl Pts',(17.336850936485,14.8534474245433,12.));
#176329=CARTESIAN_POINT('Ctrl Pts',(17.3445588463477,14.8625098843419,12.));
#176330=CARTESIAN_POINT('Ctrl Pts',(17.3523575568648,14.8717408826958,12.));
#176331=CARTESIAN_POINT('Ctrl Pts',(17.3602445978163,14.8811390927424,12.));
#176332=CARTESIAN_POINT('Ctrl Pts',(17.3682175653236,14.8907032205789,12.));
#176333=CARTESIAN_POINT('Ctrl Pts',(17.3762741193075,14.9004320039609,12.));
#176334=CARTESIAN_POINT('Ctrl Pts',(17.3844119809823,14.9103242110057,12.));
#176335=CARTESIAN_POINT('Ctrl Pts',(17.3926289303987,14.9203786389343,12.));
#176336=CARTESIAN_POINT('Ctrl Pts',(17.400922804075,14.9305941128758,12.));
#176337=CARTESIAN_POINT('Ctrl Pts',(17.4092914926071,14.940969484645,12.));
#176338=CARTESIAN_POINT('Ctrl Pts',(17.4177329382827,14.9515036315142,12.));
#176339=CARTESIAN_POINT('Ctrl Pts',(17.4262451327088,14.9621954549825,12.));
#176340=CARTESIAN_POINT('Ctrl Pts',(17.4348261151395,14.973043879945,12.));
#176341=CARTESIAN_POINT('Ctrl Pts',(17.4434739707773,14.9840478538357,12.));
#176342=CARTESIAN_POINT('Ctrl Pts',(17.4521868291005,14.9952063457779,12.));
#176343=CARTESIAN_POINT('Ctrl Pts',(17.4609628621419,15.0065183456923,12.));
#176344=CARTESIAN_POINT('Ctrl Pts',(17.4698002829357,15.0179828635087,12.));
#176345=CARTESIAN_POINT('Ctrl Pts',(17.4786973441417,15.029598928488,12.));
#176346=CARTESIAN_POINT('Ctrl Pts',(17.4876523366178,15.0413655884993,12.));
#176347=CARTESIAN_POINT('Ctrl Pts',(17.4966635880246,15.0532819093085,12.));
#176348=CARTESIAN_POINT('Ctrl Pts',(17.5057294613877,15.0653469738307,12.));
#176349=CARTESIAN_POINT('Ctrl Pts',(17.5148483539687,15.0775598815749,12.));
#176350=CARTESIAN_POINT('Ctrl Pts',(17.524018696179,15.0899197481082,12.));
#176351=CARTESIAN_POINT('Ctrl Pts',(17.5332389504829,15.1024257045033,12.));
#176352=CARTESIAN_POINT('Ctrl Pts',(17.5425076102963,15.1150768967728,12.));
#176353=CARTESIAN_POINT('Ctrl Pts',(17.5518231989117,15.1278724853138,12.));
#176354=CARTESIAN_POINT('Ctrl Pts',(17.5611842686192,15.1408116444876,12.));
#176355=CARTESIAN_POINT('Ctrl Pts',(17.5705893998029,15.1538935621714,12.));
#176356=CARTESIAN_POINT('Ctrl Pts',(17.580037200054,15.1671174393137,12.));
#176357=CARTESIAN_POINT('Ctrl Pts',(17.5895263032595,15.1804824894605,12.));
#176358=CARTESIAN_POINT('Ctrl Pts',(17.5990553687599,15.1939879383268,12.));
#176359=CARTESIAN_POINT('Ctrl Pts',(17.60862308065,15.2076330234686,12.));
#176360=CARTESIAN_POINT('Ctrl Pts',(17.6182281470468,15.22141699392,12.));
#176361=CARTESIAN_POINT('Ctrl Pts',(17.6278692993764,15.2353391098367,12.));
#176362=CARTESIAN_POINT('Ctrl Pts',(17.6375452916369,15.2493986421092,12.));
#176363=CARTESIAN_POINT('Ctrl Pts',(17.6472548997328,15.2635948720292,12.));
#176364=CARTESIAN_POINT('Ctrl Pts',(17.6569969209,15.2779270910239,12.));
#176365=CARTESIAN_POINT('Ctrl Pts',(17.6667701731041,15.2923946003598,12.));
#176366=CARTESIAN_POINT('Ctrl Pts',(17.676573494456,15.3069967108501,12.));
#176367=CARTESIAN_POINT('Ctrl Pts',(17.6864057426052,15.3217327425338,12.));
#176368=CARTESIAN_POINT('Ctrl Pts',(17.6962657941983,15.3366020244066,12.));
#176369=CARTESIAN_POINT('Ctrl Pts',(17.7061525444042,15.351603894206,12.));
#176370=CARTESIAN_POINT('Ctrl Pts',(17.7160649064206,15.3667376981699,12.));
#176371=CARTESIAN_POINT('Ctrl Pts',(17.7260018109924,15.3820027907967,12.));
#176372=CARTESIAN_POINT('Ctrl Pts',(17.7359622059149,15.3973985345802,12.));
#176373=CARTESIAN_POINT('Ctrl Pts',(17.7459450555812,15.4129242997837,12.));
#176374=CARTESIAN_POINT('Ctrl Pts',(17.7559493405881,15.4285794642668,12.));
#176375=CARTESIAN_POINT('Ctrl Pts',(17.7659740573265,15.4443634132869,12.));
#176376=CARTESIAN_POINT('Ctrl Pts',(17.7760182175815,15.4602755393018,12.));
#176377=CARTESIAN_POINT('Ctrl Pts',(17.7860808481219,15.4763152417497,12.));
#176378=CARTESIAN_POINT('Ctrl Pts',(17.7961609903148,15.4924819268517,12.));
#176379=CARTESIAN_POINT('Ctrl Pts',(17.8062576997952,15.5087750074718,12.));
#176380=CARTESIAN_POINT('Ctrl Pts',(17.8163700461256,15.5251939029552,12.));
#176381=CARTESIAN_POINT('Ctrl Pts',(17.8264971124606,15.541738038964,12.));
#176382=CARTESIAN_POINT('Ctrl Pts',(17.8366379952085,15.5584068472982,12.));
#176383=CARTESIAN_POINT('Ctrl Pts',(17.8467918036987,15.5751997657163,12.));
#176384=CARTESIAN_POINT('Ctrl Pts',(17.8569576599006,15.5921162378192,12.));
#176385=CARTESIAN_POINT('Ctrl Pts',(17.8671346981394,15.609155712921,12.));
#176386=CARTESIAN_POINT('Ctrl Pts',(17.8773220648125,15.6263176459108,12.));
#176387=CARTESIAN_POINT('Ctrl Pts',(17.8875189181091,15.6436014971085,12.));
#176388=CARTESIAN_POINT('Ctrl Pts',(17.897724427724,15.661006732103,12.));
#176389=CARTESIAN_POINT('Ctrl Pts',(17.9079377746111,15.6785328216461,12.));
#176390=CARTESIAN_POINT('Ctrl Pts',(17.9181581507455,15.6961792415522,12.));
#176391=CARTESIAN_POINT('Ctrl Pts',(17.9283847588836,15.7139454725839,12.));
#176392=CARTESIAN_POINT('Ctrl Pts',(17.9386168123262,15.7318310003335,12.));
#176393=CARTESIAN_POINT('Ctrl Pts',(17.9488535346781,15.749835315086,12.));
#176394=CARTESIAN_POINT('Ctrl Pts',(17.9590941596242,15.7679579117077,12.));
#176395=CARTESIAN_POINT('Ctrl Pts',(17.9693379307303,15.7861982895724,12.));
#176396=CARTESIAN_POINT('Ctrl Pts',(17.9795841012386,15.8045559524677,12.));
#176397=CARTESIAN_POINT('Ctrl Pts',(17.9898319338664,15.8230304084962,12.));
#176398=CARTESIAN_POINT('Ctrl Pts',(18.0000807006052,15.8416211699679,12.));
#176399=CARTESIAN_POINT('Ctrl Pts',(18.0103296825205,15.8603277532831,12.));
#176400=CARTESIAN_POINT('Ctrl Pts',(18.0205781695769,15.8791496788683,12.));
#176401=CARTESIAN_POINT('Ctrl Pts',(18.0308254604636,15.8980864711042,12.));
#176402=CARTESIAN_POINT('Ctrl Pts',(18.0410708624208,15.9171376582436,12.));
#176403=CARTESIAN_POINT('Ctrl Pts',(18.0513136910691,15.9363027723244,12.));
#176404=CARTESIAN_POINT('Ctrl Pts',(18.061553270236,15.9555813490644,12.));
#176405=CARTESIAN_POINT('Ctrl Pts',(18.0717889317958,15.9749729277846,12.));
#176406=CARTESIAN_POINT('Ctrl Pts',(18.0820200155236,15.9944770513613,12.));
#176407=CARTESIAN_POINT('Ctrl Pts',(18.0922458689462,16.014093266161,12.));
#176408=CARTESIAN_POINT('Ctrl Pts',(18.1024658471966,16.0338211219693,12.));
#176409=CARTESIAN_POINT('Ctrl Pts',(18.112679312869,16.0536601719126,12.));
#176410=CARTESIAN_POINT('Ctrl Pts',(18.1228856358751,16.0736099723668,12.));
#176411=CARTESIAN_POINT('Ctrl Pts',(18.1330841933105,16.0936700829112,12.));
#176412=CARTESIAN_POINT('Ctrl Pts',(18.1432743693235,16.1138400662794,12.));
#176413=CARTESIAN_POINT('Ctrl Pts',(18.1534555549852,16.1341194882988,12.));
#176414=CARTESIAN_POINT('Ctrl Pts',(18.1636271481615,16.154507917826,12.));
#176415=CARTESIAN_POINT('Ctrl Pts',(18.1737885533849,16.1750049266671,12.));
#176416=CARTESIAN_POINT('Ctrl Pts',(18.1839391817331,16.1956100895073,12.));
#176417=CARTESIAN_POINT('Ctrl Pts',(18.1940784507229,16.2163229838875,12.));
#176418=CARTESIAN_POINT('Ctrl Pts',(18.2042057842035,16.2371431901638,12.));
#176419=CARTESIAN_POINT('Ctrl Pts',(18.2143206122529,16.2580702914615,12.));
#176420=CARTESIAN_POINT('Ctrl Pts',(18.2244223710745,16.2791038736223,12.));
#176421=CARTESIAN_POINT('Ctrl Pts',(18.2345105028982,16.3002435251378,12.));
#176422=CARTESIAN_POINT('Ctrl Pts',(18.2445844558742,16.3214888370987,12.));
#176423=CARTESIAN_POINT('Ctrl Pts',(18.2546436839608,16.3428394031589,12.));
#176424=CARTESIAN_POINT('Ctrl Pts',(18.2646876468169,16.3642948194868,12.));
#176425=CARTESIAN_POINT('Ctrl Pts',(18.2747158096934,16.385854684708,12.));
#176426=CARTESIAN_POINT('Ctrl Pts',(18.2847276433309,16.4075185998455,12.));
#176427=CARTESIAN_POINT('Ctrl Pts',(18.294722623851,16.4292861682379,12.));
#176428=CARTESIAN_POINT('Ctrl Pts',(18.304700232686,16.4511569955233,12.));
#176429=CARTESIAN_POINT('Ctrl Pts',(18.3146599565231,16.4731306896441,12.));
#176430=CARTESIAN_POINT('Ctrl Pts',(18.3246012872469,16.4952068608345,12.));
#176431=CARTESIAN_POINT('Ctrl Pts',(18.3345237218864,16.5173851216045,12.));
#176432=CARTESIAN_POINT('Ctrl Pts',(18.34442676256,16.5396650867139,12.));
#176433=CARTESIAN_POINT('Ctrl Pts',(18.354309916433,16.5620463731413,12.));
#176434=CARTESIAN_POINT('Ctrl Pts',(18.3641726955889,16.5845286000217,12.));
#176435=CARTESIAN_POINT('Ctrl Pts',(18.3740146168879,16.607111388571,12.));
#176436=CARTESIAN_POINT('Ctrl Pts',(18.3838352018327,16.6297943620056,12.));
#176437=CARTESIAN_POINT('Ctrl Pts',(18.3936339764332,16.6525771454513,12.));
#176438=CARTESIAN_POINT('Ctrl Pts',(18.403410471079,16.6754593658513,12.));
#176439=CARTESIAN_POINT('Ctrl Pts',(18.413164220399,16.6984406518491,12.));
#176440=CARTESIAN_POINT('Ctrl Pts',(18.4228947633187,16.7215206338818,12.));
#176441=CARTESIAN_POINT('Ctrl Pts',(18.4326016431392,16.7446989442882,12.));
#176442=CARTESIAN_POINT('Ctrl Pts',(18.44228440761,16.7679752173992,12.));
#176443=CARTESIAN_POINT('Ctrl Pts',(18.4519426090123,16.791349089629,12.));
#176444=CARTESIAN_POINT('Ctrl Pts',(18.4615758042305,16.8148201995472,12.));
#176445=CARTESIAN_POINT('Ctrl Pts',(18.4711835548623,16.8383881879709,12.));
#176446=CARTESIAN_POINT('Ctrl Pts',(18.4807654268771,16.8620526977171,12.));
#176447=CARTESIAN_POINT('Ctrl Pts',(18.4903209902227,16.8858133733088,12.));
#176448=CARTESIAN_POINT('Ctrl Pts',(18.499849818462,16.9096698606943,12.));
#176449=CARTESIAN_POINT('Ctrl Pts',(18.5093514883835,16.9336218069353,12.));
#176450=CARTESIAN_POINT('Ctrl Pts',(18.5188255796659,16.9576688599339,12.));
#176451=CARTESIAN_POINT('Ctrl Pts',(18.5282716744197,16.981810668038,12.));
#176452=CARTESIAN_POINT('Ctrl Pts',(18.5376893576961,17.0060468805097,12.));
#176453=CARTESIAN_POINT('Ctrl Pts',(18.547078218209,17.0303771481738,12.));
#176454=CARTESIAN_POINT('Ctrl Pts',(18.556437848963,17.0548011239751,12.));
#176455=CARTESIAN_POINT('Ctrl Pts',(18.5657678479789,17.0793184636079,12.));
#176456=CARTESIAN_POINT('Ctrl Pts',(18.5750678188542,17.1039288260001,12.));
#176457=CARTESIAN_POINT('Ctrl Pts',(18.5843373717247,17.1286318741183,12.));
#176458=CARTESIAN_POINT('Ctrl Pts',(18.5935761222825,17.1534272741643,12.));
#176459=CARTESIAN_POINT('Ctrl Pts',(18.6027836898817,17.1783146940127,12.));
#176460=CARTESIAN_POINT('Ctrl Pts',(18.6119596959949,17.2032938019284,12.));
#176461=CARTESIAN_POINT('Ctrl Pts',(18.6211037624038,17.2283642650518,12.));
#176462=CARTESIAN_POINT('Ctrl Pts',(18.6302155097943,17.2535257482187,12.));
#176463=CARTESIAN_POINT('Ctrl Pts',(18.6392945554748,17.2787779120213,12.));
#176464=CARTESIAN_POINT('Ctrl Pts',(18.6483405141865,17.3041204135074,12.));
#176465=CARTESIAN_POINT('Ctrl Pts',(18.6573530024033,17.3295529098618,12.));
#176466=CARTESIAN_POINT('Ctrl Pts',(18.6663316416582,17.3550750612443,12.));
#176467=CARTESIAN_POINT('Ctrl Pts',(18.6752760624052,17.3806865340747,12.));
#176468=CARTESIAN_POINT('Ctrl Pts',(18.6841859073471,17.4063870038562,12.));
#176469=CARTESIAN_POINT('Ctrl Pts',(18.6930608357409,17.4321761588142,12.));
#176470=CARTESIAN_POINT('Ctrl Pts',(18.70190052503,17.4580537012753,12.));
#176471=CARTESIAN_POINT('Ctrl Pts',(18.7107046613912,17.4840193397162,12.));
#176472=CARTESIAN_POINT('Ctrl Pts',(18.7194729318098,17.5100727820876,12.));
#176473=CARTESIAN_POINT('Ctrl Pts',(18.7282050157138,17.5362137287593,12.));
#176474=CARTESIAN_POINT('Ctrl Pts',(18.7369005764553,17.5624418653245,12.));
#176475=CARTESIAN_POINT('Ctrl Pts',(18.7455592536687,17.5887568561371,12.));
#176476=CARTESIAN_POINT('Ctrl Pts',(18.7541806530984,17.6151583357012,12.));
#176477=CARTESIAN_POINT('Ctrl Pts',(18.762764361321,17.6416459210681,12.));
#176478=CARTESIAN_POINT('Ctrl Pts',(18.7713099642754,17.6682192274236,12.));
#176479=CARTESIAN_POINT('Ctrl Pts',(18.7798170641374,17.6948778823014,12.));
#176480=CARTESIAN_POINT('Ctrl Pts',(18.7882852976049,17.7216215409035,12.));
#176481=CARTESIAN_POINT('Ctrl Pts',(18.7967143519419,17.7484498996905,12.));
#176482=CARTESIAN_POINT('Ctrl Pts',(18.8051039860448,17.7753627137853,12.));
#176483=CARTESIAN_POINT('Ctrl Pts',(18.8134540340417,17.8023598011057,12.));
#176484=CARTESIAN_POINT('Ctrl Pts',(18.8217643886157,17.8294410311006,12.));
#176485=CARTESIAN_POINT('Ctrl Pts',(18.8300349895974,17.8566063174771,12.));
#176486=CARTESIAN_POINT('Ctrl Pts',(18.8366196462581,17.8784057509356,12.));
#176487=CARTESIAN_POINT('Ctrl Pts',(18.8415402351786,17.8947931177807,12.));
#176488=CARTESIAN_POINT('Ctrl Pts',(18.8448126709691,17.9057348246595,12.));
#176489=CARTESIAN_POINT('Ctrl Pts',(18.8464468996588,17.9112098770111,12.));
#176490=CARTESIAN_POINT('',(17.9112098770111,18.8464468996588,12.));
#176491=CARTESIAN_POINT('Origin',(0.,0.,12.));
#176492=CARTESIAN_POINT('',(14.6513681262571,17.1452095830633,12.));
#176493=CARTESIAN_POINT('Ctrl Pts',(17.9112098770111,18.8464468996588,12.));
#176494=CARTESIAN_POINT('Ctrl Pts',(17.9057348246611,18.8448126709726,12.));
#176495=CARTESIAN_POINT('Ctrl Pts',(17.8947931177853,18.8415402351882,12.));
#176496=CARTESIAN_POINT('Ctrl Pts',(17.8784057509434,18.8366196462746,12.));
#176497=CARTESIAN_POINT('Ctrl Pts',(17.8566063174871,18.8300349896187,12.));
#176498=CARTESIAN_POINT('Ctrl Pts',(17.8294410311105,18.8217643886368,12.));
#176499=CARTESIAN_POINT('Ctrl Pts',(17.8023598011135,18.8134540340581,12.));
#176500=CARTESIAN_POINT('Ctrl Pts',(17.7753627137898,18.8051039860543,12.));
#176501=CARTESIAN_POINT('Ctrl Pts',(17.7484498996916,18.7967143519444,12.));
#176502=CARTESIAN_POINT('Ctrl Pts',(17.7216215409019,18.7882852976016,12.));
#176503=CARTESIAN_POINT('Ctrl Pts',(17.6948778822981,18.7798170641305,12.));
#176504=CARTESIAN_POINT('Ctrl Pts',(17.6682192274197,18.7713099642673,12.));
#176505=CARTESIAN_POINT('Ctrl Pts',(17.6416459210646,18.7627643613139,12.));
#176506=CARTESIAN_POINT('Ctrl Pts',(17.6151583356988,18.7541806530935,12.));
#176507=CARTESIAN_POINT('Ctrl Pts',(17.5887568561361,18.7455592536667,12.));
#176508=CARTESIAN_POINT('Ctrl Pts',(17.5624418653248,18.7369005764558,12.));
#176509=CARTESIAN_POINT('Ctrl Pts',(17.5362137287604,18.728205015716,12.));
#176510=CARTESIAN_POINT('Ctrl Pts',(17.5100727820891,18.7194729318128,12.));
#176511=CARTESIAN_POINT('Ctrl Pts',(17.4840193397176,18.7107046613941,12.));
#176512=CARTESIAN_POINT('Ctrl Pts',(17.4580537012764,18.7019005250322,12.));
#176513=CARTESIAN_POINT('Ctrl Pts',(17.4321761588148,18.6930608357421,12.));
#176514=CARTESIAN_POINT('Ctrl Pts',(17.4063870038563,18.6841859073472,12.));
#176515=CARTESIAN_POINT('Ctrl Pts',(17.3806865340744,18.6752760624045,12.));
#176516=CARTESIAN_POINT('Ctrl Pts',(17.3550750612438,18.6663316416569,12.));
#176517=CARTESIAN_POINT('Ctrl Pts',(17.3295529098612,18.6573530024019,12.));
#176518=CARTESIAN_POINT('Ctrl Pts',(17.3041204135069,18.6483405141853,12.));
#176519=CARTESIAN_POINT('Ctrl Pts',(17.278777912021,18.639294555474,12.));
#176520=CARTESIAN_POINT('Ctrl Pts',(17.2535257482186,18.630215509794,12.));
#176521=CARTESIAN_POINT('Ctrl Pts',(17.2283642650519,18.6211037624041,12.));
#176522=CARTESIAN_POINT('Ctrl Pts',(17.2032938019288,18.6119596959957,12.));
#176523=CARTESIAN_POINT('Ctrl Pts',(17.1783146940131,18.6027836898826,12.));
#176524=CARTESIAN_POINT('Ctrl Pts',(17.1534272741646,18.5935761222833,12.));
#176525=CARTESIAN_POINT('Ctrl Pts',(17.1286318741185,18.5843373717253,12.));
#176526=CARTESIAN_POINT('Ctrl Pts',(17.1039288260001,18.5750678188543,12.));
#176527=CARTESIAN_POINT('Ctrl Pts',(17.0793184636079,18.5657678479788,12.));
#176528=CARTESIAN_POINT('Ctrl Pts',(17.0548011239751,18.5564378489628,12.));
#176529=CARTESIAN_POINT('Ctrl Pts',(17.030377148174,18.5470782182089,12.));
#176530=CARTESIAN_POINT('Ctrl Pts',(17.0060468805099,18.5376893576961,12.));
#176531=CARTESIAN_POINT('Ctrl Pts',(16.9818106680382,18.5282716744198,12.));
#176532=CARTESIAN_POINT('Ctrl Pts',(16.957668859934,18.518825579666,12.));
#176533=CARTESIAN_POINT('Ctrl Pts',(16.9336218069353,18.5093514883835,12.));
#176534=CARTESIAN_POINT('Ctrl Pts',(16.9096698606942,18.4998498184619,12.));
#176535=CARTESIAN_POINT('Ctrl Pts',(16.8858133733086,18.4903209902226,12.));
#176536=CARTESIAN_POINT('Ctrl Pts',(16.8620526977169,18.4807654268769,12.));
#176537=CARTESIAN_POINT('Ctrl Pts',(16.8383881879707,18.4711835548622,12.));
#176538=CARTESIAN_POINT('Ctrl Pts',(16.8148201995472,18.4615758042305,12.));
#176539=CARTESIAN_POINT('Ctrl Pts',(16.791349089629,18.4519426090124,12.));
#176540=CARTESIAN_POINT('Ctrl Pts',(16.7679752173992,18.4422844076099,12.));
#176541=CARTESIAN_POINT('Ctrl Pts',(16.7446989442882,18.4326016431392,12.));
#176542=CARTESIAN_POINT('Ctrl Pts',(16.7215206338818,18.4228947633186,12.));
#176543=CARTESIAN_POINT('Ctrl Pts',(16.698440651849,18.413164220399,12.));
#176544=CARTESIAN_POINT('Ctrl Pts',(16.6754593658513,18.4034104710789,12.));
#176545=CARTESIAN_POINT('Ctrl Pts',(16.6525771454513,18.3936339764332,12.));
#176546=CARTESIAN_POINT('Ctrl Pts',(16.6297943620056,18.3838352018327,12.));
#176547=CARTESIAN_POINT('Ctrl Pts',(16.6071113885711,18.3740146168879,12.));
#176548=CARTESIAN_POINT('Ctrl Pts',(16.5845286000218,18.364172695589,12.));
#176549=CARTESIAN_POINT('Ctrl Pts',(16.5620463731414,18.3543099164331,12.));
#176550=CARTESIAN_POINT('Ctrl Pts',(16.5396650867139,18.3444267625601,12.));
#176551=CARTESIAN_POINT('Ctrl Pts',(16.5173851216045,18.3345237218864,12.));
#176552=CARTESIAN_POINT('Ctrl Pts',(16.4952068608344,18.3246012872468,12.));
#176553=CARTESIAN_POINT('Ctrl Pts',(16.4731306896439,18.3146599565229,12.));
#176554=CARTESIAN_POINT('Ctrl Pts',(16.4511569955231,18.3047002326858,12.));
#176555=CARTESIAN_POINT('Ctrl Pts',(16.4292861682377,18.2947226238509,12.));
#176556=CARTESIAN_POINT('Ctrl Pts',(16.4075185998454,18.2847276433308,12.));
#176557=CARTESIAN_POINT('Ctrl Pts',(16.385854684708,18.2747158096934,12.));
#176558=CARTESIAN_POINT('Ctrl Pts',(16.3642948194869,18.2646876468169,12.));
#176559=CARTESIAN_POINT('Ctrl Pts',(16.342839403159,18.2546436839609,12.));
#176560=CARTESIAN_POINT('Ctrl Pts',(16.3214888370988,18.2445844558742,12.));
#176561=CARTESIAN_POINT('Ctrl Pts',(16.3002435251378,18.2345105028981,12.));
#176562=CARTESIAN_POINT('Ctrl Pts',(16.2791038736223,18.2244223710745,12.));
#176563=CARTESIAN_POINT('Ctrl Pts',(16.2580702914615,18.214320612253,12.));
#176564=CARTESIAN_POINT('Ctrl Pts',(16.237143190164,18.2042057842037,12.));
#176565=CARTESIAN_POINT('Ctrl Pts',(16.2163229838878,18.1940784507232,12.));
#176566=CARTESIAN_POINT('Ctrl Pts',(16.1956100895076,18.1839391817335,12.));
#176567=CARTESIAN_POINT('Ctrl Pts',(16.1750049266673,18.1737885533852,12.));
#176568=CARTESIAN_POINT('Ctrl Pts',(16.1545079178261,18.1636271481616,12.));
#176569=CARTESIAN_POINT('Ctrl Pts',(16.1341194882987,18.1534555549851,12.));
#176570=CARTESIAN_POINT('Ctrl Pts',(16.113840066279,18.1432743693231,12.));
#176571=CARTESIAN_POINT('Ctrl Pts',(16.0936700829108,18.1330841933099,12.));
#176572=CARTESIAN_POINT('Ctrl Pts',(16.0736099723664,18.1228856358746,12.));
#176573=CARTESIAN_POINT('Ctrl Pts',(16.0536601719124,18.1126793128688,12.));
#176574=CARTESIAN_POINT('Ctrl Pts',(16.0338211219693,18.1024658471966,12.));
#176575=CARTESIAN_POINT('Ctrl Pts',(16.0140932661612,18.0922458689464,12.));
#176576=CARTESIAN_POINT('Ctrl Pts',(15.9944770513616,18.0820200155239,12.));
#176577=CARTESIAN_POINT('Ctrl Pts',(15.9749729277848,18.071788931796,12.));
#176578=CARTESIAN_POINT('Ctrl Pts',(15.9555813490645,18.061553270236,12.));
#176579=CARTESIAN_POINT('Ctrl Pts',(15.9363027723244,18.0513136910691,12.));
#176580=CARTESIAN_POINT('Ctrl Pts',(15.9171376582436,18.0410708624208,12.));
#176581=CARTESIAN_POINT('Ctrl Pts',(15.8980864711043,18.0308254604638,12.));
#176582=CARTESIAN_POINT('Ctrl Pts',(15.8791496788685,18.0205781695773,12.));
#176583=CARTESIAN_POINT('Ctrl Pts',(15.8603277532834,18.010329682521,12.));
#176584=CARTESIAN_POINT('Ctrl Pts',(15.8416211699681,18.0000807006055,12.));
#176585=CARTESIAN_POINT('Ctrl Pts',(15.8230304084963,17.9898319338664,12.));
#176586=CARTESIAN_POINT('Ctrl Pts',(15.8045559524674,17.9795841012383,12.));
#176587=CARTESIAN_POINT('Ctrl Pts',(15.786198289572,17.9693379307297,12.));
#176588=CARTESIAN_POINT('Ctrl Pts',(15.7679579117072,17.9590941596236,12.));
#176589=CARTESIAN_POINT('Ctrl Pts',(15.7498353150856,17.9488535346776,12.));
#176590=CARTESIAN_POINT('Ctrl Pts',(15.7318310003334,17.9386168123261,12.));
#176591=CARTESIAN_POINT('Ctrl Pts',(15.713945472584,17.9283847588837,12.));
#176592=CARTESIAN_POINT('Ctrl Pts',(15.6961792415526,17.918158150746,12.));
#176593=CARTESIAN_POINT('Ctrl Pts',(15.6785328216467,17.9079377746118,12.));
#176594=CARTESIAN_POINT('Ctrl Pts',(15.6610067321036,17.8977244277247,12.));
#176595=CARTESIAN_POINT('Ctrl Pts',(15.6436014971088,17.8875189181095,12.));
#176596=CARTESIAN_POINT('Ctrl Pts',(15.6263176459107,17.8773220648125,12.));
#176597=CARTESIAN_POINT('Ctrl Pts',(15.6091557129205,17.8671346981388,12.));
#176598=CARTESIAN_POINT('Ctrl Pts',(15.5921162378183,17.8569576598996,12.));
#176599=CARTESIAN_POINT('Ctrl Pts',(15.5751997657153,17.8467918036977,12.));
#176600=CARTESIAN_POINT('Ctrl Pts',(15.5584068472976,17.8366379952078,12.));
#176601=CARTESIAN_POINT('Ctrl Pts',(15.5417380389639,17.8264971124606,12.));
#176602=CARTESIAN_POINT('Ctrl Pts',(15.5251939029558,17.8163700461263,12.));
#176603=CARTESIAN_POINT('Ctrl Pts',(15.5087750074728,17.8062576997964,12.));
#176604=CARTESIAN_POINT('Ctrl Pts',(15.4924819268529,17.7961609903161,12.));
#176605=CARTESIAN_POINT('Ctrl Pts',(15.4763152417506,17.7860808481229,12.));
#176606=CARTESIAN_POINT('Ctrl Pts',(15.4602755393019,17.7760182175817,12.));
#176607=CARTESIAN_POINT('Ctrl Pts',(15.4443634132865,17.765974057326,12.));
#176608=CARTESIAN_POINT('Ctrl Pts',(15.4285794642658,17.7559493405871,12.));
#176609=CARTESIAN_POINT('Ctrl Pts',(15.4129242997828,17.7459450555803,12.));
#176610=CARTESIAN_POINT('Ctrl Pts',(15.3973985345796,17.7359622059143,12.));
#176611=CARTESIAN_POINT('Ctrl Pts',(15.3820027907965,17.7260018109923,12.));
#176612=CARTESIAN_POINT('Ctrl Pts',(15.3667376981702,17.7160649064208,12.));
#176613=CARTESIAN_POINT('Ctrl Pts',(15.3516038942064,17.7061525444044,12.));
#176614=CARTESIAN_POINT('Ctrl Pts',(15.3366020244069,17.6962657941984,12.));
#176615=CARTESIAN_POINT('Ctrl Pts',(15.3217327425341,17.6864057426052,12.));
#176616=CARTESIAN_POINT('Ctrl Pts',(15.3069967108501,17.6765734944559,12.));
#176617=CARTESIAN_POINT('Ctrl Pts',(15.2923946003598,17.6667701731041,12.));
#176618=CARTESIAN_POINT('Ctrl Pts',(15.2779270910238,17.6569969209,12.));
#176619=CARTESIAN_POINT('Ctrl Pts',(15.263594872029,17.6472548997329,12.));
#176620=CARTESIAN_POINT('Ctrl Pts',(15.2493986421091,17.637545291637,12.));
#176621=CARTESIAN_POINT('Ctrl Pts',(15.2353391098367,17.6278692993765,12.));
#176622=CARTESIAN_POINT('Ctrl Pts',(15.22141699392,17.6182281470467,12.));
#176623=CARTESIAN_POINT('Ctrl Pts',(15.2076330234686,17.6086230806497,12.));
#176624=CARTESIAN_POINT('Ctrl Pts',(15.1939879383268,17.5990553687595,12.));
#176625=CARTESIAN_POINT('Ctrl Pts',(15.1804824894605,17.5895263032592,12.));
#176626=CARTESIAN_POINT('Ctrl Pts',(15.1671174393136,17.5800372000539,12.));
#176627=CARTESIAN_POINT('Ctrl Pts',(15.1538935621714,17.570589399803,12.));
#176628=CARTESIAN_POINT('Ctrl Pts',(15.1408116444877,17.5611842686196,12.));
#176629=CARTESIAN_POINT('Ctrl Pts',(15.127872485314,17.5518231989122,12.));
#176630=CARTESIAN_POINT('Ctrl Pts',(15.1150768967729,17.5425076102966,12.));
#176631=CARTESIAN_POINT('Ctrl Pts',(15.1024257045033,17.5332389504829,12.));
#176632=CARTESIAN_POINT('Ctrl Pts',(15.0899197481082,17.5240186961788,12.));
#176633=CARTESIAN_POINT('Ctrl Pts',(15.0775598815748,17.5148483539684,12.));
#176634=CARTESIAN_POINT('Ctrl Pts',(15.0653469738306,17.5057294613874,12.));
#176635=CARTESIAN_POINT('Ctrl Pts',(15.0532819093085,17.4966635880245,12.));
#176636=CARTESIAN_POINT('Ctrl Pts',(15.0413655884993,17.4876523366178,12.));
#176637=CARTESIAN_POINT('Ctrl Pts',(15.029598928488,17.4786973441417,12.));
#176638=CARTESIAN_POINT('Ctrl Pts',(15.0179828635086,17.4698002829357,12.));
#176639=CARTESIAN_POINT('Ctrl Pts',(15.0065183456921,17.4609628621418,12.));
#176640=CARTESIAN_POINT('Ctrl Pts',(14.9952063457778,17.4521868291004,12.));
#176641=CARTESIAN_POINT('Ctrl Pts',(14.9840478538358,17.4434739707773,12.));
#176642=CARTESIAN_POINT('Ctrl Pts',(14.9730438799452,17.4348261151396,12.));
#176643=CARTESIAN_POINT('Ctrl Pts',(14.9621954549827,17.426245132709,12.));
#176644=CARTESIAN_POINT('Ctrl Pts',(14.9515036315143,17.4177329382828,12.));
#176645=CARTESIAN_POINT('Ctrl Pts',(14.940969484645,17.4092914926071,12.));
#176646=CARTESIAN_POINT('Ctrl Pts',(14.9305941128757,17.4009228040749,12.));
#176647=CARTESIAN_POINT('Ctrl Pts',(14.9203786389342,17.3926289303986,12.));
#176648=CARTESIAN_POINT('Ctrl Pts',(14.9103242110057,17.3844119809824,12.));
#176649=CARTESIAN_POINT('Ctrl Pts',(14.900432003961,17.3762741193076,12.));
#176650=CARTESIAN_POINT('Ctrl Pts',(14.8907032205788,17.3682175653235,12.));
#176651=CARTESIAN_POINT('Ctrl Pts',(14.8811390927423,17.3602445978161,12.));
#176652=CARTESIAN_POINT('Ctrl Pts',(14.8717408826955,17.3523575568645,12.));
#176653=CARTESIAN_POINT('Ctrl Pts',(14.8625098843417,17.3445588463475,12.));
#176654=CARTESIAN_POINT('Ctrl Pts',(14.8534474245433,17.336850936485,12.));
#176655=CARTESIAN_POINT('Ctrl Pts',(14.8445548643508,17.3292363662605,12.));
#176656=CARTESIAN_POINT('Ctrl Pts',(14.8358336004197,17.3217177462101,12.));
#176657=CARTESIAN_POINT('Ctrl Pts',(14.8272850675379,17.3142977632659,12.));
#176658=CARTESIAN_POINT('Ctrl Pts',(14.8189107410162,17.3069791853706,12.));
#176659=CARTESIAN_POINT('Ctrl Pts',(14.8107121391035,17.299764866148,12.));
#176660=CARTESIAN_POINT('Ctrl Pts',(14.8026908254276,17.2926577496513,12.));
#176661=CARTESIAN_POINT('Ctrl Pts',(14.7948484105249,17.2856608733196,12.));
#176662=CARTESIAN_POINT('Ctrl Pts',(14.787186553128,17.2787773704849,12.));
#176663=CARTESIAN_POINT('Ctrl Pts',(14.7797069617804,17.2720104735194,12.));
#176664=CARTESIAN_POINT('Ctrl Pts',(14.7724113956731,17.2653635155319,12.));
#176665=CARTESIAN_POINT('Ctrl Pts',(14.7653016697591,17.2588399401465,12.));
#176666=CARTESIAN_POINT('Ctrl Pts',(14.7583796616617,17.2524433146837,12.));
#176667=CARTESIAN_POINT('Ctrl Pts',(14.7516473175124,17.2461773413288,12.));
#176668=CARTESIAN_POINT('Ctrl Pts',(14.7451066593792,17.2400458713565,12.));
#176669=CARTESIAN_POINT('Ctrl Pts',(14.7387597858116,17.2340529062076,12.));
#176670=CARTESIAN_POINT('Ctrl Pts',(14.7326088681163,17.2282025904314,12.));
#176671=CARTESIAN_POINT('Ctrl Pts',(14.7266561494282,17.2224992099667,12.));
#176672=CARTESIAN_POINT('Ctrl Pts',(14.7209039390327,17.2169471814256,12.));
#176673=CARTESIAN_POINT('Ctrl Pts',(14.7153546289339,17.2115510835989,12.));
#176674=CARTESIAN_POINT('Ctrl Pts',(14.7100107213586,17.2063157097315,12.));
#176675=CARTESIAN_POINT('Ctrl Pts',(14.7048748502663,17.2012461084268,12.));
#176676=CARTESIAN_POINT('Ctrl Pts',(14.699949811582,17.1963476411694,12.));
#176677=CARTESIAN_POINT('Ctrl Pts',(14.6952385361705,17.1916259308415,12.));
#176678=CARTESIAN_POINT('Ctrl Pts',(14.6907440526958,17.1870867909918,12.));
#176679=CARTESIAN_POINT('Ctrl Pts',(14.686469452232,17.182736158472,12.));
#176680=CARTESIAN_POINT('Ctrl Pts',(14.6824178576167,17.1785800350826,12.));
#176681=CARTESIAN_POINT('Ctrl Pts',(14.6785925615677,17.1746247499057,12.));
#176682=CARTESIAN_POINT('Ctrl Pts',(14.6749971333867,17.1708771619129,12.));
#176683=CARTESIAN_POINT('Ctrl Pts',(14.671635583332,17.167344972302,12.));
#176684=CARTESIAN_POINT('Ctrl Pts',(14.6685123374423,17.1640366762305,12.));
#176685=CARTESIAN_POINT('Ctrl Pts',(14.6656319165057,17.1609609517369,12.));
#176686=CARTESIAN_POINT('Ctrl Pts',(14.6629987285992,17.1581262646789,12.));
#176687=CARTESIAN_POINT('Ctrl Pts',(14.6606167169642,17.1555401986401,12.));
#176688=CARTESIAN_POINT('Ctrl Pts',(14.6584900555302,17.1532107762718,12.));
#176689=CARTESIAN_POINT('Ctrl Pts',(14.6566237952435,17.1511476869496,12.));
#176690=CARTESIAN_POINT('Ctrl Pts',(14.655024862281,17.1493641837558,12.));
#176691=CARTESIAN_POINT('Ctrl Pts',(14.6537016966184,17.147876394491,12.));
#176692=CARTESIAN_POINT('Ctrl Pts',(14.6526624064978,17.1466998098673,12.));
#176693=CARTESIAN_POINT('Ctrl Pts',(14.6519131634508,17.1458462295271,12.));
#176694=CARTESIAN_POINT('Ctrl Pts',(14.6515481598068,17.1454262858043,12.));
#176695=CARTESIAN_POINT('Ctrl Pts',(14.6514066997196,17.1452600887037,12.));
#176696=CARTESIAN_POINT('Ctrl Pts',(14.6513711852843,17.1452153999142,12.));
#176697=CARTESIAN_POINT('Ctrl Pts',(14.6513681262571,17.1452095830633,12.));
#176698=CARTESIAN_POINT('',(14.2886635873976,16.7207683102834,12.));
#176699=CARTESIAN_POINT('',(6.98376450772883,8.17248635976757,12.));
#176700=CARTESIAN_POINT('',(13.5924445804218,16.6581946899465,12.));
#176701=CARTESIAN_POINT('Origin',(13.9085479427572,17.0455945664569,12.));
#176702=CARTESIAN_POINT('',(12.572596943457,17.4407513054162,12.));
#176703=CARTESIAN_POINT('Origin',(4.9889687874677E-13,6.00167842331873E-13,
12.));
#176704=CARTESIAN_POINT('',(12.4528436808172,18.1294424696716,12.));
#176705=CARTESIAN_POINT('Origin',(12.8649829188862,17.846350172984,12.));
#176706=CARTESIAN_POINT('',(12.7689476255363,18.5896416359912,12.));
#176707=CARTESIAN_POINT('',(6.38447381276812,9.29482081799561,12.));
#176708=CARTESIAN_POINT('',(13.5685075571671,22.1787195904339,12.));
#176709=CARTESIAN_POINT('Ctrl Pts',(12.7689476255363,18.5896416359912,12.));
#176710=CARTESIAN_POINT('Ctrl Pts',(12.7689524524484,18.5896460962961,12.));
#176711=CARTESIAN_POINT('Ctrl Pts',(12.7689864266924,18.5896919669158,12.));
#176712=CARTESIAN_POINT('Ctrl Pts',(12.7691103481996,18.589871621842,12.));
#176713=CARTESIAN_POINT('Ctrl Pts',(12.7694215127923,18.590332877722,12.));
#176714=CARTESIAN_POINT('Ctrl Pts',(12.7700520897174,18.5912775137806,12.));
#176715=CARTESIAN_POINT('Ctrl Pts',(12.7709195951153,18.5925859134582,12.));
#176716=CARTESIAN_POINT('Ctrl Pts',(12.7720142287169,18.5942490615409,12.));
#176717=CARTESIAN_POINT('Ctrl Pts',(12.7733231262107,18.5962551167772,12.));
#176718=CARTESIAN_POINT('Ctrl Pts',(12.7748328937639,18.5985917525949,12.));
#176719=CARTESIAN_POINT('Ctrl Pts',(12.7765325225082,18.6012488486708,12.));
#176720=CARTESIAN_POINT('Ctrl Pts',(12.7784139605067,18.6042190183703,12.));
#176721=CARTESIAN_POINT('Ctrl Pts',(12.7804705387658,18.6074961535723,12.));
#176722=CARTESIAN_POINT('Ctrl Pts',(12.7826959526924,18.611074482622,12.));
#176723=CARTESIAN_POINT('Ctrl Pts',(12.78508316579,18.6149475565189,12.));
#176724=CARTESIAN_POINT('Ctrl Pts',(12.7876249657834,18.6191087624752,12.));
#176725=CARTESIAN_POINT('Ctrl Pts',(12.7903142925234,18.6235516265575,12.));
#176726=CARTESIAN_POINT('Ctrl Pts',(12.7931447451556,18.6282702819371,12.));
#176727=CARTESIAN_POINT('Ctrl Pts',(12.7961106222251,18.6332595057005,12.));
#176728=CARTESIAN_POINT('Ctrl Pts',(12.7992066625264,18.63851447924,12.));
#176729=CARTESIAN_POINT('Ctrl Pts',(12.8024278770153,18.6440306327457,12.));
#176730=CARTESIAN_POINT('Ctrl Pts',(12.805769331162,18.6498034438986,12.));
#176731=CARTESIAN_POINT('Ctrl Pts',(12.8092261933858,18.6558284825772,12.));
#176732=CARTESIAN_POINT('Ctrl Pts',(12.8127937909632,18.6621014624746,12.));
#176733=CARTESIAN_POINT('Ctrl Pts',(12.8164676687361,18.6686182952798,12.));
#176734=CARTESIAN_POINT('Ctrl Pts',(12.8202436318473,18.6753751301091,12.));
#176735=CARTESIAN_POINT('Ctrl Pts',(12.8241176980016,18.6823683094139,12.));
#176736=CARTESIAN_POINT('Ctrl Pts',(12.8280860635231,18.6895943376172,12.));
#176737=CARTESIAN_POINT('Ctrl Pts',(12.832145059979,18.6970498410173,12.));
#176738=CARTESIAN_POINT('Ctrl Pts',(12.8362911280362,18.7047315436296,12.));
#176739=CARTESIAN_POINT('Ctrl Pts',(12.8405208263432,18.7126362754446,12.));
#176740=CARTESIAN_POINT('Ctrl Pts',(12.8448308329494,18.7207609737701,12.));
#176741=CARTESIAN_POINT('Ctrl Pts',(12.849217951159,18.7291026886552,12.));
#176742=CARTESIAN_POINT('Ctrl Pts',(12.8536791086315,18.7376585820851,12.));
#176743=CARTESIAN_POINT('Ctrl Pts',(12.8582113455644,18.7464259171248,12.));
#176744=CARTESIAN_POINT('Ctrl Pts',(12.8628118054172,18.7554020493888,12.));
#176745=CARTESIAN_POINT('Ctrl Pts',(12.8674777239656,18.7645844169568,12.));
#176746=CARTESIAN_POINT('Ctrl Pts',(12.8722064211814,18.7739705329029,12.));
#176747=CARTESIAN_POINT('Ctrl Pts',(12.8769952998097,18.7835579840481,12.));
#176748=CARTESIAN_POINT('Ctrl Pts',(12.8818418427474,18.7933444285867,12.));
#176749=CARTESIAN_POINT('Ctrl Pts',(12.8867436109543,18.8033275941939,12.));
#176750=CARTESIAN_POINT('Ctrl Pts',(12.8916982409931,18.8135052757815,12.));
#176751=CARTESIAN_POINT('Ctrl Pts',(12.8967034410752,18.8238753319124,12.));
#176752=CARTESIAN_POINT('Ctrl Pts',(12.9017569871738,18.834435681259,12.));
#176753=CARTESIAN_POINT('Ctrl Pts',(12.9068567191856,18.8451842990986,12.));
#176754=CARTESIAN_POINT('Ctrl Pts',(12.9120005369066,18.8561192136201,12.));
#176755=CARTESIAN_POINT('Ctrl Pts',(12.9171863977047,18.8672385038328,12.));
#176756=CARTESIAN_POINT('Ctrl Pts',(12.9224123144982,18.8785402977528,12.));
#176757=CARTESIAN_POINT('Ctrl Pts',(12.9276763536372,18.8900227704888,12.));
#176758=CARTESIAN_POINT('Ctrl Pts',(12.9329766328184,18.9016841423402,12.));
#176759=CARTESIAN_POINT('Ctrl Pts',(12.9383113190375,18.9135226769466,12.));
#176760=CARTESIAN_POINT('Ctrl Pts',(12.9436786266106,18.9255366795196,12.));
#176761=CARTESIAN_POINT('Ctrl Pts',(12.9490768151821,18.9377244950435,12.));
#176762=CARTESIAN_POINT('Ctrl Pts',(12.9545041877377,18.9500845064714,12.));
#176763=CARTESIAN_POINT('Ctrl Pts',(12.9599590886317,18.9626151329226,12.));
#176764=CARTESIAN_POINT('Ctrl Pts',(12.9654399021868,18.9753148284473,12.));
#176765=CARTESIAN_POINT('Ctrl Pts',(12.9709450512747,18.9881820807585,12.));
#176766=CARTESIAN_POINT('Ctrl Pts',(12.9764729959206,19.0012154099792,12.));
#176767=CARTESIAN_POINT('Ctrl Pts',(12.9820222318716,19.014413367335,12.));
#176768=CARTESIAN_POINT('Ctrl Pts',(12.9875912893003,19.0277745339909,12.));
#176769=CARTESIAN_POINT('Ctrl Pts',(12.9931787316514,19.0412975200398,12.));
#176770=CARTESIAN_POINT('Ctrl Pts',(12.9987831544502,19.0549809634354,12.));
#176771=CARTESIAN_POINT('Ctrl Pts',(13.0044031841382,19.0688235289437,12.));
#176772=CARTESIAN_POINT('Ctrl Pts',(13.0100374768788,19.0828239070484,12.));
#176773=CARTESIAN_POINT('Ctrl Pts',(13.0156847176096,19.0969808131228,12.));
#176774=CARTESIAN_POINT('Ctrl Pts',(13.0213436191328,19.111292986631,12.));
#176775=CARTESIAN_POINT('Ctrl Pts',(13.0270129211976,19.1257591903099,12.));
#176776=CARTESIAN_POINT('Ctrl Pts',(13.0326913895838,19.1403782093386,12.));
#176777=CARTESIAN_POINT('Ctrl Pts',(13.0383778152068,19.155148850523,12.));
#176778=CARTESIAN_POINT('Ctrl Pts',(13.0440710133772,19.1700699416622,12.));
#176779=CARTESIAN_POINT('Ctrl Pts',(13.0497698230441,19.1851403308825,12.));
#176780=CARTESIAN_POINT('Ctrl Pts',(13.0554731060538,19.2003588859772,12.));
#176781=CARTESIAN_POINT('Ctrl Pts',(13.0611797463915,19.2157244937142,12.));
#176782=CARTESIAN_POINT('Ctrl Pts',(13.0668886494795,19.2312360592033,12.));
#176783=CARTESIAN_POINT('Ctrl Pts',(13.0725987415859,19.2468925053989,12.));
#176784=CARTESIAN_POINT('Ctrl Pts',(13.0783089692118,19.2626927725596,12.));
#176785=CARTESIAN_POINT('Ctrl Pts',(13.0840182984949,19.2786358177198,12.));
#176786=CARTESIAN_POINT('Ctrl Pts',(13.0897257145968,19.2947206141247,12.));
#176787=CARTESIAN_POINT('Ctrl Pts',(13.0954302211479,19.310946150736,12.));
#176788=CARTESIAN_POINT('Ctrl Pts',(13.1011308397591,19.3273114318269,12.));
#176789=CARTESIAN_POINT('Ctrl Pts',(13.1068266095186,19.3438154765395,12.));
#176790=CARTESIAN_POINT('Ctrl Pts',(13.1125165865022,19.3604573184515,12.));
#176791=CARTESIAN_POINT('Ctrl Pts',(13.118199843271,19.3772360051091,12.));
#176792=CARTESIAN_POINT('Ctrl Pts',(13.1238754684177,19.3941505976263,12.));
#176793=CARTESIAN_POINT('Ctrl Pts',(13.1295425661634,19.4112001703557,12.));
#176794=CARTESIAN_POINT('Ctrl Pts',(13.1352002559438,19.4283838105262,12.));
#176795=CARTESIAN_POINT('Ctrl Pts',(13.1408476720061,19.4457006178876,12.));
#176796=CARTESIAN_POINT('Ctrl Pts',(13.1464839629971,19.4631497043258,12.));
#176797=CARTESIAN_POINT('Ctrl Pts',(13.1521082915853,19.4807301935268,12.));
#176798=CARTESIAN_POINT('Ctrl Pts',(13.1577198341245,19.4984412207082,12.));
#176799=CARTESIAN_POINT('Ctrl Pts',(13.1633177803101,19.5162819323213,12.));
#176800=CARTESIAN_POINT('Ctrl Pts',(13.168901332843,19.5342514857562,12.));
#176801=CARTESIAN_POINT('Ctrl Pts',(13.1744697070911,19.5523490490244,12.));
#176802=CARTESIAN_POINT('Ctrl Pts',(13.1800221307673,19.5705738004667,12.));
#176803=CARTESIAN_POINT('Ctrl Pts',(13.1855578436471,19.5889249285338,12.));
#176804=CARTESIAN_POINT('Ctrl Pts',(13.1910760972814,19.6074016315414,12.));
#176805=CARTESIAN_POINT('Ctrl Pts',(13.1965761547151,19.6260031174244,12.));
#176806=CARTESIAN_POINT('Ctrl Pts',(13.2020572902065,19.6447286034772,12.));
#176807=CARTESIAN_POINT('Ctrl Pts',(13.2075187889529,19.6635773160936,12.));
#176808=CARTESIAN_POINT('Ctrl Pts',(13.2129599468485,19.6825484905823,12.));
#176809=CARTESIAN_POINT('Ctrl Pts',(13.2183800702436,19.7016413709685,12.));
#176810=CARTESIAN_POINT('Ctrl Pts',(13.2237784757065,19.7208552097868,12.));
#176811=CARTESIAN_POINT('Ctrl Pts',(13.2291544897899,19.7401892678697,12.));
#176812=CARTESIAN_POINT('Ctrl Pts',(13.2345074487963,19.7596428141168,12.));
#176813=CARTESIAN_POINT('Ctrl Pts',(13.2398366985675,19.7792151253289,12.));
#176814=CARTESIAN_POINT('Ctrl Pts',(13.2451415942805,19.7989054860495,12.));
#176815=CARTESIAN_POINT('Ctrl Pts',(13.2504215002457,19.8187131883917,12.));
#176816=CARTESIAN_POINT('Ctrl Pts',(13.2556757897086,19.8386375318634,12.));
#176817=CARTESIAN_POINT('Ctrl Pts',(13.2609038446529,19.8586778231715,12.));
#176818=CARTESIAN_POINT('Ctrl Pts',(13.2661050556132,19.8788333760577,12.));
#176819=CARTESIAN_POINT('Ctrl Pts',(13.271278821502,19.8991035111745,12.));
#176820=CARTESIAN_POINT('Ctrl Pts',(13.2764245494357,19.9194875559422,12.));
#176821=CARTESIAN_POINT('Ctrl Pts',(13.2815416545663,19.9399848444019,12.));
#176822=CARTESIAN_POINT('Ctrl Pts',(13.286629559915,19.9605947170586,12.));
#176823=CARTESIAN_POINT('Ctrl Pts',(13.2916876962094,19.981316520717,12.));
#176824=CARTESIAN_POINT('Ctrl Pts',(13.2967155017306,20.0021496083738,12.));
#176825=CARTESIAN_POINT('Ctrl Pts',(13.3017124221637,20.0230933391038,12.));
#176826=CARTESIAN_POINT('Ctrl Pts',(13.3066779104515,20.0441470779345,12.));
#176827=CARTESIAN_POINT('Ctrl Pts',(13.3116114266515,20.0653101957188,12.));
#176828=CARTESIAN_POINT('Ctrl Pts',(13.3165124377962,20.0865820689883,12.));
#176829=CARTESIAN_POINT('Ctrl Pts',(13.3213804177587,20.1079620798375,12.));
#176830=CARTESIAN_POINT('Ctrl Pts',(13.3262148471226,20.1294496158402,12.));
#176831=CARTESIAN_POINT('Ctrl Pts',(13.3310152130564,20.1510440699474,12.));
#176832=CARTESIAN_POINT('Ctrl Pts',(13.3357810091903,20.1727448403817,12.));
#176833=CARTESIAN_POINT('Ctrl Pts',(13.3405117354971,20.1945513305235,12.));
#176834=CARTESIAN_POINT('Ctrl Pts',(13.3452068981766,20.216462948786,12.));
#176835=CARTESIAN_POINT('Ctrl Pts',(13.3498660095386,20.2384791085359,12.));
#176836=CARTESIAN_POINT('Ctrl Pts',(13.3544885878889,20.2605992280122,12.));
#176837=CARTESIAN_POINT('Ctrl Pts',(13.3590741574195,20.2828227302339,12.));
#176838=CARTESIAN_POINT('Ctrl Pts',(13.3636222481016,20.3051490429048,12.));
#176839=CARTESIAN_POINT('Ctrl Pts',(13.3681323955826,20.3275775983029,12.));
#176840=CARTESIAN_POINT('Ctrl Pts',(13.3726041410867,20.3501078331814,12.));
#176841=CARTESIAN_POINT('Ctrl Pts',(13.3770370313188,20.3727391887184,12.));
#176842=CARTESIAN_POINT('Ctrl Pts',(13.3814306183719,20.3954711104502,12.));
#176843=CARTESIAN_POINT('Ctrl Pts',(13.3857844596387,20.4183030482002,12.));
#176844=CARTESIAN_POINT('Ctrl Pts',(13.3900981177255,20.4412344560008,12.));
#176845=CARTESIAN_POINT('Ctrl Pts',(13.3943711603739,20.4642647920038,12.));
#176846=CARTESIAN_POINT('Ctrl Pts',(13.3986031603716,20.487393518404,12.));
#176847=CARTESIAN_POINT('Ctrl Pts',(13.4027936954529,20.5106201013753,12.));
#176848=CARTESIAN_POINT('Ctrl Pts',(13.4069423482076,20.5339440109956,12.));
#176849=CARTESIAN_POINT('Ctrl Pts',(13.4110487059912,20.5573647211639,12.));
#176850=CARTESIAN_POINT('Ctrl Pts',(13.4151123608411,20.5808817095155,12.));
#176851=CARTESIAN_POINT('Ctrl Pts',(13.4191329093932,20.6044944573153,12.));
#176852=CARTESIAN_POINT('Ctrl Pts',(13.4231099528179,20.6282024494237,12.));
#176853=CARTESIAN_POINT('Ctrl Pts',(13.4270430967651,20.6520051742869,12.));
#176854=CARTESIAN_POINT('Ctrl Pts',(13.4309319513119,20.6759021239103,12.));
#176855=CARTESIAN_POINT('Ctrl Pts',(13.4347761309154,20.6998927938288,12.));
#176856=CARTESIAN_POINT('Ctrl Pts',(13.4385752543663,20.7239766830675,12.));
#176857=CARTESIAN_POINT('Ctrl Pts',(13.4423289447561,20.7481532941013,12.));
#176858=CARTESIAN_POINT('Ctrl Pts',(13.4460368293688,20.7724221327608,12.));
#176859=CARTESIAN_POINT('Ctrl Pts',(13.4496985395637,20.7967827081227,12.));
#176860=CARTESIAN_POINT('Ctrl Pts',(13.4533137106667,20.821234532398,12.));
#176861=CARTESIAN_POINT('Ctrl Pts',(13.4568819818631,20.8457771208082,12.));
#176862=CARTESIAN_POINT('Ctrl Pts',(13.4604029960983,20.8704099914641,12.));
#176863=CARTESIAN_POINT('Ctrl Pts',(13.4638763999725,20.8951326652158,12.));
#176864=CARTESIAN_POINT('Ctrl Pts',(13.4673018437718,20.9199446657584,12.));
#176865=CARTESIAN_POINT('Ctrl Pts',(13.4706789815166,20.9448455197557,12.));
#176866=CARTESIAN_POINT('Ctrl Pts',(13.4740074710087,20.9698347569476,12.));
#176867=CARTESIAN_POINT('Ctrl Pts',(13.4772869738879,20.9949119102592,12.));
#176868=CARTESIAN_POINT('Ctrl Pts',(13.4805171556822,21.0200765158885,12.));
#176869=CARTESIAN_POINT('Ctrl Pts',(13.4836976858912,21.0453281134247,12.));
#176870=CARTESIAN_POINT('Ctrl Pts',(13.4868282377191,21.0706662455202,12.));
#176871=CARTESIAN_POINT('Ctrl Pts',(13.4899084877718,21.0960904575048,12.));
#176872=CARTESIAN_POINT('Ctrl Pts',(13.4929381157778,21.1216002970209,12.));
#176873=CARTESIAN_POINT('Ctrl Pts',(13.4959168042934,21.1471953136209,12.));
#176874=CARTESIAN_POINT('Ctrl Pts',(13.4988442384491,21.1728750584173,12.));
#176875=CARTESIAN_POINT('Ctrl Pts',(13.5017201056088,21.1986390835825,12.));
#176876=CARTESIAN_POINT('Ctrl Pts',(13.5045440957404,21.224486942933,12.));
#176877=CARTESIAN_POINT('Ctrl Pts',(13.5073159019454,21.2504181927429,12.));
#176878=CARTESIAN_POINT('Ctrl Pts',(13.5100352209207,21.2764323924442,12.));
#176879=CARTESIAN_POINT('Ctrl Pts',(13.5127017534972,21.3025291054236,12.));
#176880=CARTESIAN_POINT('Ctrl Pts',(13.5153152050554,21.328707899634,12.));
#176881=CARTESIAN_POINT('Ctrl Pts',(13.5178752862461,21.3549683486219,12.));
#176882=CARTESIAN_POINT('Ctrl Pts',(13.5203817122496,21.3813100304967,12.));
#176883=CARTESIAN_POINT('Ctrl Pts',(13.5228342013508,21.4077325259318,12.));
#176884=CARTESIAN_POINT('Ctrl Pts',(13.5252324737795,21.4342354165254,12.));
#176885=CARTESIAN_POINT('Ctrl Pts',(13.5275762503553,21.4608182828695,12.));
#176886=CARTESIAN_POINT('Ctrl Pts',(13.5298652514357,21.487480703047,12.));
#176887=CARTESIAN_POINT('Ctrl Pts',(13.5320991952145,21.5142222501671,12.));
#176888=CARTESIAN_POINT('Ctrl Pts',(13.5342777983225,21.5410424932511,12.));
#176889=CARTESIAN_POINT('Ctrl Pts',(13.5364007790292,21.5679410019011,12.));
#176890=CARTESIAN_POINT('Ctrl Pts',(13.5384678597206,21.5949173499022,12.));
#176891=CARTESIAN_POINT('Ctrl Pts',(13.5404787697798,21.6219711193951,12.));
#176892=CARTESIAN_POINT('Ctrl Pts',(13.5424332480698,21.6491019044647,12.));
#176893=CARTESIAN_POINT('Ctrl Pts',(13.5443310461516,21.676309315769,12.));
#176894=CARTESIAN_POINT('Ctrl Pts',(13.546171929503,21.7035929822939,12.));
#176895=CARTESIAN_POINT('Ctrl Pts',(13.5479556704457,21.730952541226,12.));
#176896=CARTESIAN_POINT('Ctrl Pts',(13.5496820422186,21.7583876294532,12.));
#176897=CARTESIAN_POINT('Ctrl Pts',(13.5513508127232,21.7858978745848,12.));
#176898=CARTESIAN_POINT('Ctrl Pts',(13.5529617381569,21.8134828857963,12.));
#176899=CARTESIAN_POINT('Ctrl Pts',(13.5545145573048,21.841142245609,12.));
#176900=CARTESIAN_POINT('Ctrl Pts',(13.5560089839426,21.8688754989401,12.));
#176901=CARTESIAN_POINT('Ctrl Pts',(13.5574447178484,21.8966821688876,12.));
#176902=CARTESIAN_POINT('Ctrl Pts',(13.5588214586672,21.9245617765827,12.));
#176903=CARTESIAN_POINT('Ctrl Pts',(13.5601389185315,21.9525138592862,12.));
#176904=CARTESIAN_POINT('Ctrl Pts',(13.5613968357589,21.9805379899192,12.));
#176905=CARTESIAN_POINT('Ctrl Pts',(13.5625949868313,22.0086337943431,12.));
#176906=CARTESIAN_POINT('Ctrl Pts',(13.5637332022393,22.0368009736227,12.));
#176907=CARTESIAN_POINT('Ctrl Pts',(13.5648113688894,22.0650393089492,12.));
#176908=CARTESIAN_POINT('Ctrl Pts',(13.5658294169106,22.0933486464442,12.));
#176909=CARTESIAN_POINT('Ctrl Pts',(13.5667873105179,22.1217288871823,12.));
#176910=CARTESIAN_POINT('Ctrl Pts',(13.5675054918922,22.1444897575076,12.));
#176911=CARTESIAN_POINT('Ctrl Pts',(13.5680170531724,22.1615922804939,12.));
#176912=CARTESIAN_POINT('Ctrl Pts',(13.5683460612913,22.1730081264583,12.));
#176913=CARTESIAN_POINT('Ctrl Pts',(13.5685075571671,22.1787195904339,12.));
#176914=CARTESIAN_POINT('',(12.4230808101438,22.8400320311648,12.));
#176915=CARTESIAN_POINT('Origin',(0.,0.,12.));
#176916=CARTESIAN_POINT('',(9.71462809124917,20.353053841303,12.));
#176917=CARTESIAN_POINT('Ctrl Pts',(12.4230808101438,22.8400320311648,12.));
#176918=CARTESIAN_POINT('Ctrl Pts',(12.4182152851867,22.8370364396497,12.));
#176919=CARTESIAN_POINT('Ctrl Pts',(12.4084933766366,22.8310435872852,12.));
#176920=CARTESIAN_POINT('Ctrl Pts',(12.393937937903,22.8220493007353,12.));
#176921=CARTESIAN_POINT('Ctrl Pts',(12.3745855366772,22.8100469022632,12.));
#176922=CARTESIAN_POINT('Ctrl Pts',(12.3504864740361,22.7950272216959,12.));
#176923=CARTESIAN_POINT('Ctrl Pts',(12.3264788926108,22.7799908974947,12.));
#176924=CARTESIAN_POINT('Ctrl Pts',(12.3025628601811,22.7649380101154,12.));
#176925=CARTESIAN_POINT('Ctrl Pts',(12.2787384750747,22.7498686970096,12.));
#176926=CARTESIAN_POINT('Ctrl Pts',(12.2550058702389,22.7347831655251,12.));
#176927=CARTESIAN_POINT('Ctrl Pts',(12.2313652198047,22.7196817119299,12.));
#176928=CARTESIAN_POINT('Ctrl Pts',(12.2078167360267,22.7045647168659,12.));
#176929=CARTESIAN_POINT('Ctrl Pts',(12.1843606579246,22.6894326204959,12.));
#176930=CARTESIAN_POINT('Ctrl Pts',(12.1609972423088,22.6742859034891,12.));
#176931=CARTESIAN_POINT('Ctrl Pts',(12.1377267537141,22.6591250653942,12.));
#176932=CARTESIAN_POINT('Ctrl Pts',(12.1145494550384,22.6439506046611,12.));
#176933=CARTESIAN_POINT('Ctrl Pts',(12.0914655972828,22.628762996708,12.));
#176934=CARTESIAN_POINT('Ctrl Pts',(12.0684754113869,22.613562676493,12.));
#176935=CARTESIAN_POINT('Ctrl Pts',(12.0455791139135,22.5983500505675,12.));
#176936=CARTESIAN_POINT('Ctrl Pts',(12.0227769113132,22.5831255061306,12.));
#176937=CARTESIAN_POINT('Ctrl Pts',(12.0000690046697,22.5678894211194,12.));
#176938=CARTESIAN_POINT('Ctrl Pts',(11.9774555943496,22.5526421741159,12.));
#176939=CARTESIAN_POINT('Ctrl Pts',(11.9549368843996,22.5373841537299,12.));
#176940=CARTESIAN_POINT('Ctrl Pts',(11.9325130877801,22.5221157697869,12.));
#176941=CARTESIAN_POINT('Ctrl Pts',(11.9101844254555,22.5068374513958,12.));
#176942=CARTESIAN_POINT('Ctrl Pts',(11.8879511239941,22.4915496418472,12.));
#176943=CARTESIAN_POINT('Ctrl Pts',(11.8658134137018,22.4762527946694,12.));
#176944=CARTESIAN_POINT('Ctrl Pts',(11.8437715264487,22.4609473690469,12.));
#176945=CARTESIAN_POINT('Ctrl Pts',(11.8218256937889,22.4456338258738,12.));
#176946=CARTESIAN_POINT('Ctrl Pts',(11.7999761445175,22.4303126226468,12.));
#176947=CARTESIAN_POINT('Ctrl Pts',(11.7782231042041,22.4149842125018,12.));
#176948=CARTESIAN_POINT('Ctrl Pts',(11.7565667964765,22.39964904692,12.));
#176949=CARTESIAN_POINT('Ctrl Pts',(11.7350074437961,22.3843075773905,12.));
#176950=CARTESIAN_POINT('Ctrl Pts',(11.7135452684532,22.3689602575492,12.));
#176951=CARTESIAN_POINT('Ctrl Pts',(11.6921804934056,22.3536075450028,12.));
#176952=CARTESIAN_POINT('Ctrl Pts',(11.6709133432986,22.3382499035618,12.));
#176953=CARTESIAN_POINT('Ctrl Pts',(11.6497440449858,22.3228878043976,12.));
#176954=CARTESIAN_POINT('Ctrl Pts',(11.6286728270011,22.3075217249049,12.));
#176955=CARTESIAN_POINT('Ctrl Pts',(11.6076999192359,22.2921521480358,12.));
#176956=CARTESIAN_POINT('Ctrl Pts',(11.5868255525189,22.2767795614349,12.));
#176957=CARTESIAN_POINT('Ctrl Pts',(11.5660499582403,22.2614044566898,12.));
#176958=CARTESIAN_POINT('Ctrl Pts',(11.545373367912,22.2460273284653,12.));
#176959=CARTESIAN_POINT('Ctrl Pts',(11.5247960128476,22.2306486738899,12.));
#176960=CARTESIAN_POINT('Ctrl Pts',(11.504318124424,22.215268993102,12.));
#176961=CARTESIAN_POINT('Ctrl Pts',(11.4839399342589,22.1998887896435,12.));
#176962=CARTESIAN_POINT('Ctrl Pts',(11.463661674411,22.184508570917,12.));
#176963=CARTESIAN_POINT('Ctrl Pts',(11.443483577557,22.1691288486096,12.));
#176964=CARTESIAN_POINT('Ctrl Pts',(11.4234058771742,22.1537501391486,12.));
#176965=CARTESIAN_POINT('Ctrl Pts',(11.4034288076908,22.1383729640963,12.));
#176966=CARTESIAN_POINT('Ctrl Pts',(11.3835526044256,22.1229978500185,12.));
#176967=CARTESIAN_POINT('Ctrl Pts',(11.3637775035367,22.1076253283978,12.));
#176968=CARTESIAN_POINT('Ctrl Pts',(11.3441037419553,22.0922559355293,12.));
#176969=CARTESIAN_POINT('Ctrl Pts',(11.3245315573168,22.0768902124267,12.));
#176970=CARTESIAN_POINT('Ctrl Pts',(11.3050611878771,22.0615287047179,12.));
#176971=CARTESIAN_POINT('Ctrl Pts',(11.2856928724374,22.0461719625661,12.));
#176972=CARTESIAN_POINT('Ctrl Pts',(11.2664268504207,22.0308205408351,12.));
#176973=CARTESIAN_POINT('Ctrl Pts',(11.2472633619276,22.0154749992364,12.));
#176974=CARTESIAN_POINT('Ctrl Pts',(11.2282026477897,22.000135902484,12.));
#176975=CARTESIAN_POINT('Ctrl Pts',(11.2092449496125,21.9848038204439,12.));
#176976=CARTESIAN_POINT('Ctrl Pts',(11.1903905098109,21.9694793282913,12.));
#176977=CARTESIAN_POINT('Ctrl Pts',(11.1716395716375,21.9541630066504,12.));
#176978=CARTESIAN_POINT('Ctrl Pts',(11.1529923792002,21.9388554416437,12.));
#176979=CARTESIAN_POINT('Ctrl Pts',(11.134449177474,21.9235572249518,12.));
#176980=CARTESIAN_POINT('Ctrl Pts',(11.1160102123024,21.9082689538687,12.));
#176981=CARTESIAN_POINT('Ctrl Pts',(11.0976757303944,21.8929912313608,12.));
#176982=CARTESIAN_POINT('Ctrl Pts',(11.0794459793058,21.8777246661191,12.));
#176983=CARTESIAN_POINT('Ctrl Pts',(11.0613212074364,21.8624698726319,12.));
#176984=CARTESIAN_POINT('Ctrl Pts',(11.0433016640808,21.8472274713103,12.));
#176985=CARTESIAN_POINT('Ctrl Pts',(11.0253875994598,21.8319980886033,12.));
#176986=CARTESIAN_POINT('Ctrl Pts',(11.0075792647477,21.8167823571168,12.));
#176987=CARTESIAN_POINT('Ctrl Pts',(10.9898769120913,21.8015809157302,12.));
#176988=CARTESIAN_POINT('Ctrl Pts',(10.9722807946157,21.7863944097143,12.));
#176989=CARTESIAN_POINT('Ctrl Pts',(10.9547911664457,21.7712234908468,12.));
#176990=CARTESIAN_POINT('Ctrl Pts',(10.9374082827446,21.7560688175252,12.));
#176991=CARTESIAN_POINT('Ctrl Pts',(10.9201323997386,21.74093105488,12.));
#176992=CARTESIAN_POINT('Ctrl Pts',(10.9029637747341,21.7258108748874,12.));
#176993=CARTESIAN_POINT('Ctrl Pts',(10.8859026661292,21.7107089564822,12.));
#176994=CARTESIAN_POINT('Ctrl Pts',(10.8689493334093,21.6956259856667,12.));
#176995=CARTESIAN_POINT('Ctrl Pts',(10.8521040371832,21.6805626556461,12.));
#176996=CARTESIAN_POINT('Ctrl Pts',(10.835367039227,21.6655196669727,12.));
#176997=CARTESIAN_POINT('Ctrl Pts',(10.8187386025135,21.6504977276864,12.));
#176998=CARTESIAN_POINT('Ctrl Pts',(10.8022189912369,21.6354975534558,12.));
#176999=CARTESIAN_POINT('Ctrl Pts',(10.7858084708262,21.6205198677176,12.));
#177000=CARTESIAN_POINT('Ctrl Pts',(10.7695073079554,21.6055654018179,12.));
#177001=CARTESIAN_POINT('Ctrl Pts',(10.7533157705943,21.5906348951745,12.));
#177002=CARTESIAN_POINT('Ctrl Pts',(10.7372341280468,21.5757290954372,12.));
#177003=CARTESIAN_POINT('Ctrl Pts',(10.7212626509816,21.5608487586467,12.));
#177004=CARTESIAN_POINT('Ctrl Pts',(10.7054016114571,21.5459946493955,12.));
#177005=CARTESIAN_POINT('Ctrl Pts',(10.689651282929,21.531167540981,12.));
#177006=CARTESIAN_POINT('Ctrl Pts',(10.6740119402835,21.5163682155805,12.));
#177007=CARTESIAN_POINT('Ctrl Pts',(10.658483859894,21.5015974644454,12.));
#177008=CARTESIAN_POINT('Ctrl Pts',(10.6430673196609,21.4868560880893,12.));
#177009=CARTESIAN_POINT('Ctrl Pts',(10.6277625990456,21.4721448964766,12.));
#177010=CARTESIAN_POINT('Ctrl Pts',(10.612569979096,21.4574647092093,12.));
#177011=CARTESIAN_POINT('Ctrl Pts',(10.597489742462,21.4428163557137,12.));
#177012=CARTESIAN_POINT('Ctrl Pts',(10.582522173457,21.4282006754624,12.));
#177013=CARTESIAN_POINT('Ctrl Pts',(10.5676675581106,21.4136185181974,12.));
#177014=CARTESIAN_POINT('Ctrl Pts',(10.5529261842107,21.3990707441495,12.));
#177015=CARTESIAN_POINT('Ctrl Pts',(10.5382983413422,21.3845582242604,12.));
#177016=CARTESIAN_POINT('Ctrl Pts',(10.523784320906,21.3700818403942,12.));
#177017=CARTESIAN_POINT('Ctrl Pts',(10.5093844161689,21.3556424855822,12.));
#177018=CARTESIAN_POINT('Ctrl Pts',(10.4950989223341,21.3412410642912,12.));
#177019=CARTESIAN_POINT('Ctrl Pts',(10.4809281365933,21.3268784926823,12.));
#177020=CARTESIAN_POINT('Ctrl Pts',(10.4668723581768,21.312555698873,12.));
#177021=CARTESIAN_POINT('Ctrl Pts',(10.452931888387,21.2982736231924,12.));
#177022=CARTESIAN_POINT('Ctrl Pts',(10.4391070306385,21.2840332184471,12.));
#177023=CARTESIAN_POINT('Ctrl Pts',(10.4253980905394,21.2698354502391,12.));
#177024=CARTESIAN_POINT('Ctrl Pts',(10.4118053759584,21.2556812972741,12.));
#177025=CARTESIAN_POINT('Ctrl Pts',(10.3983291970846,21.2415717516713,12.));
#177026=CARTESIAN_POINT('Ctrl Pts',(10.384969866479,21.2275078192708,12.));
#177027=CARTESIAN_POINT('Ctrl Pts',(10.3717276991137,21.2134905199359,12.));
#177028=CARTESIAN_POINT('Ctrl Pts',(10.3586030124595,21.1995208879205,12.));
#177029=CARTESIAN_POINT('Ctrl Pts',(10.3455961265706,21.1855999722427,12.));
#177030=CARTESIAN_POINT('Ctrl Pts',(10.3327073641574,21.1717288370512,12.));
#177031=CARTESIAN_POINT('Ctrl Pts',(10.3199370506541,21.1579085619959,12.));
#177032=CARTESIAN_POINT('Ctrl Pts',(10.307285514268,21.1441402425831,12.));
#177033=CARTESIAN_POINT('Ctrl Pts',(10.2947530860714,21.130424990599,12.));
#177034=CARTESIAN_POINT('Ctrl Pts',(10.2823401001067,21.1167639345623,12.));
#177035=CARTESIAN_POINT('Ctrl Pts',(10.2700468934743,21.1031582201625,12.));
#177036=CARTESIAN_POINT('Ctrl Pts',(10.2578738064183,21.0896090107066,12.));
#177037=CARTESIAN_POINT('Ctrl Pts',(10.2458211823915,21.0761174875448,12.));
#177038=CARTESIAN_POINT('Ctrl Pts',(10.233889368157,21.0626848505665,12.));
#177039=CARTESIAN_POINT('Ctrl Pts',(10.2220787139157,21.0493123187484,12.));
#177040=CARTESIAN_POINT('Ctrl Pts',(10.2103895734123,21.0360011306814,12.));
#177041=CARTESIAN_POINT('Ctrl Pts',(10.1988223040425,21.0227525451107,12.));
#177042=CARTESIAN_POINT('Ctrl Pts',(10.1873772669358,21.0095678414486,12.));
#177043=CARTESIAN_POINT('Ctrl Pts',(10.1760548270765,20.9964483203685,12.));
#177044=CARTESIAN_POINT('Ctrl Pts',(10.1648553534567,20.9833953044737,12.));
#177045=CARTESIAN_POINT('Ctrl Pts',(10.1537792192065,20.970410138937,12.));
#177046=CARTESIAN_POINT('Ctrl Pts',(10.1428268017257,20.9574941921591,12.));
#177047=CARTESIAN_POINT('Ctrl Pts',(10.1319984827909,20.944648856393,12.));
#177048=CARTESIAN_POINT('Ctrl Pts',(10.1212946487057,20.931875548473,12.));
#177049=CARTESIAN_POINT('Ctrl Pts',(10.1107156904836,20.9191757106266,12.));
#177050=CARTESIAN_POINT('Ctrl Pts',(10.1002620040076,20.9065508112556,12.));
#177051=CARTESIAN_POINT('Ctrl Pts',(10.0899339901916,20.8940023457371,12.));
#177052=CARTESIAN_POINT('Ctrl Pts',(10.0797320551154,20.8815318371844,12.));
#177053=CARTESIAN_POINT('Ctrl Pts',(10.0696566102219,20.8691408373705,12.));
#177054=CARTESIAN_POINT('Ctrl Pts',(10.0597080725375,20.856830927732,12.));
#177055=CARTESIAN_POINT('Ctrl Pts',(10.0498868648733,20.8446037203402,12.));
#177056=CARTESIAN_POINT('Ctrl Pts',(10.0401934160234,20.8324608588906,12.));
#177057=CARTESIAN_POINT('Ctrl Pts',(10.0306281609435,20.8204040196599,12.));
#177058=CARTESIAN_POINT('Ctrl Pts',(10.0211915410095,20.8084349126885,12.));
#177059=CARTESIAN_POINT('Ctrl Pts',(10.0118840042786,20.7965552829907,12.));
#177060=CARTESIAN_POINT('Ctrl Pts',(10.0027060057389,20.7847669117568,12.));
#177061=CARTESIAN_POINT('Ctrl Pts',(9.99365800754637,20.7730716175417,12.));
#177062=CARTESIAN_POINT('Ctrl Pts',(9.98474047926846,20.7614712574989,12.));
#177063=CARTESIAN_POINT('Ctrl Pts',(9.97595389823461,20.7499677289626,12.));
#177064=CARTESIAN_POINT('Ctrl Pts',(9.96729874986198,20.7385629709795,12.));
#177065=CARTESIAN_POINT('Ctrl Pts',(9.95877552798403,20.7272589658752,12.));
#177066=CARTESIAN_POINT('Ctrl Pts',(9.95038473514962,20.7160577407581,12.));
#177067=CARTESIAN_POINT('Ctrl Pts',(9.9421268829825,20.7049613692237,12.));
#177068=CARTESIAN_POINT('Ctrl Pts',(9.93400249259736,20.6939719732485,12.));
#177069=CARTESIAN_POINT('Ctrl Pts',(9.9260120949875,20.6830917250255,12.));
#177070=CARTESIAN_POINT('Ctrl Pts',(9.91815623141284,20.6723228488262,12.));
#177071=CARTESIAN_POINT('Ctrl Pts',(9.91043545377004,20.6616676228315,12.));
#177072=CARTESIAN_POINT('Ctrl Pts',(9.90285032516695,20.6511283817415,12.));
#177073=CARTESIAN_POINT('Ctrl Pts',(9.89540142049123,20.6407075193977,12.));
#177074=CARTESIAN_POINT('Ctrl Pts',(9.88808932697304,20.6304074914086,12.));
#177075=CARTESIAN_POINT('Ctrl Pts',(9.88091464472669,20.6202308177472,12.));
#177076=CARTESIAN_POINT('Ctrl Pts',(9.87387798732943,20.6101800854491,12.));
#177077=CARTESIAN_POINT('Ctrl Pts',(9.86697998242612,20.6002579513696,12.));
#177078=CARTESIAN_POINT('Ctrl Pts',(9.86022127232749,20.5904671449755,12.));
#177079=CARTESIAN_POINT('Ctrl Pts',(9.85360251457004,20.580810471002,12.));
#177080=CARTESIAN_POINT('Ctrl Pts',(9.84712438256308,20.5712908125145,12.));
#177081=CARTESIAN_POINT('Ctrl Pts',(9.84078756677589,20.5619111362406,12.));
#177082=CARTESIAN_POINT('Ctrl Pts',(9.8345927758532,20.5526744976461,12.));
#177083=CARTESIAN_POINT('Ctrl Pts',(9.82854073773857,20.5435840460717,12.));
#177084=CARTESIAN_POINT('Ctrl Pts',(9.82263220080327,20.534643029951,12.));
#177085=CARTESIAN_POINT('Ctrl Pts',(9.81686793455918,20.5258548000625,12.));
#177086=CARTESIAN_POINT('Ctrl Pts',(9.81124873025278,20.5172228122839,12.));
#177087=CARTESIAN_POINT('Ctrl Pts',(9.80577540161102,20.5087506310507,12.));
#177088=CARTESIAN_POINT('Ctrl Pts',(9.80044878520967,20.500441931211,12.));
#177089=CARTESIAN_POINT('Ctrl Pts',(9.79526974288343,20.4923005087945,12.));
#177090=CARTESIAN_POINT('Ctrl Pts',(9.79023916498659,20.4843302955329,12.));
#177091=CARTESIAN_POINT('Ctrl Pts',(9.78535797314162,20.4765353711585,12.));
#177092=CARTESIAN_POINT('Ctrl Pts',(9.78062712373313,20.4689199790668,12.));
#177093=CARTESIAN_POINT('Ctrl Pts',(9.77604760815522,20.4614885274973,12.));
#177094=CARTESIAN_POINT('Ctrl Pts',(9.77162045104069,20.4542455817527,12.));
#177095=CARTESIAN_POINT('Ctrl Pts',(9.76734670980896,20.447195862298,12.));
#177096=CARTESIAN_POINT('Ctrl Pts',(9.76322747195502,20.4403442329401,12.));
#177097=CARTESIAN_POINT('Ctrl Pts',(9.75926386289929,20.4336957355474,12.));
#177098=CARTESIAN_POINT('Ctrl Pts',(9.75545705902416,20.4272556476629,12.));
#177099=CARTESIAN_POINT('Ctrl Pts',(9.75180829786433,20.4210295275818,12.));
#177100=CARTESIAN_POINT('Ctrl Pts',(9.74831889242174,20.4150232777393,12.));
#177101=CARTESIAN_POINT('Ctrl Pts',(9.74499021838536,20.4092430879861,12.));
#177102=CARTESIAN_POINT('Ctrl Pts',(9.74182369656272,20.4036953576549,12.));
#177103=CARTESIAN_POINT('Ctrl Pts',(9.73882077613206,20.3983866213331,12.));
#177104=CARTESIAN_POINT('Ctrl Pts',(9.73598292014249,20.3933234845646,12.));
#177105=CARTESIAN_POINT('Ctrl Pts',(9.73331167102812,20.3885129129912,12.));
#177106=CARTESIAN_POINT('Ctrl Pts',(9.73080870123726,20.3839624556742,12.));
#177107=CARTESIAN_POINT('Ctrl Pts',(9.72847589116532,20.3796805893304,12.));
#177108=CARTESIAN_POINT('Ctrl Pts',(9.7263153173287,20.3756766651952,12.));
#177109=CARTESIAN_POINT('Ctrl Pts',(9.72432910043192,20.371960235676,12.));
#177110=CARTESIAN_POINT('Ctrl Pts',(9.72251930722503,20.3685406190576,12.));
#177111=CARTESIAN_POINT('Ctrl Pts',(9.72088778381101,20.3654261611055,12.));
#177112=CARTESIAN_POINT('Ctrl Pts',(9.71943648548114,20.362625691398,12.));
#177113=CARTESIAN_POINT('Ctrl Pts',(9.71816778327998,20.3601498764344,12.));
#177114=CARTESIAN_POINT('Ctrl Pts',(9.71708493723061,20.3580133103357,12.));
#177115=CARTESIAN_POINT('Ctrl Pts',(9.71619192554146,20.3562337557875,12.));
#177116=CARTESIAN_POINT('Ctrl Pts',(9.71549257088174,20.3548282742361,12.));
#177117=CARTESIAN_POINT('Ctrl Pts',(9.714989780521,20.3538098605706,12.));
#177118=CARTESIAN_POINT('Ctrl Pts',(9.71474590350791,20.3533097561886,12.));
#177119=CARTESIAN_POINT('Ctrl Pts',(9.71465227853122,20.3531126095522,12.));
#177120=CARTESIAN_POINT('Ctrl Pts',(9.71462954053074,20.353060251684,12.));
#177121=CARTESIAN_POINT('Ctrl Pts',(9.71462809124917,20.353053841303,12.));
#177122=CARTESIAN_POINT('',(9.47413589477549,19.84920021178,12.));
#177123=CARTESIAN_POINT('',(4.63060338698782,9.70154690100589,12.));
#177124=CARTESIAN_POINT('',(8.8178352198485,19.6085639972844,12.));
#177125=CARTESIAN_POINT('Origin',(9.02290115519382,20.0645771135003,12.));
#177126=CARTESIAN_POINT('',(7.63019749246978,20.1004996511507,12.));
#177127=CARTESIAN_POINT('Origin',(3.26562511982935E-13,7.08841632778409E-13,
12.));
#177128=CARTESIAN_POINT('',(7.33627833380047,20.7347298079577,12.));
#177129=CARTESIAN_POINT('Origin',(7.80764394578303,20.56795313141,12.));
#177130=CARTESIAN_POINT('',(7.52250298901265,21.2610617890679,12.));
#177131=CARTESIAN_POINT('',(3.76125149450631,10.6305308945339,12.));
#177132=CARTESIAN_POINT('',(7.36589684767344,24.9347862158358,12.));
#177133=CARTESIAN_POINT('Ctrl Pts',(7.52250298901265,21.2610617890679,12.));
#177134=CARTESIAN_POINT('Ctrl Pts',(7.52250649703991,21.2610673466883,12.));
#177135=CARTESIAN_POINT('Ctrl Pts',(7.52252744144957,21.261120447486,12.));
#177136=CARTESIAN_POINT('Ctrl Pts',(7.52260064231736,21.2613260540651,12.));
#177137=CARTESIAN_POINT('Ctrl Pts',(7.52278182242727,21.261852128355,12.));
#177138=CARTESIAN_POINT('Ctrl Pts',(7.52314642316202,21.262927782038,12.));
#177139=CARTESIAN_POINT('Ctrl Pts',(7.52364573027521,21.2644161259965,12.));
#177140=CARTESIAN_POINT('Ctrl Pts',(7.52427261074263,21.266305915706,12.));
#177141=CARTESIAN_POINT('Ctrl Pts',(7.52501770333521,21.2685823838672,12.));
#177142=CARTESIAN_POINT('Ctrl Pts',(7.52587126095544,21.2712301573465,12.));
#177143=CARTESIAN_POINT('Ctrl Pts',(7.5268252691856,21.2742366113578,12.));
#177144=CARTESIAN_POINT('Ctrl Pts',(7.52787386225343,21.2775925269652,12.));
#177145=CARTESIAN_POINT('Ctrl Pts',(7.52901217930407,21.2812902781143,12.));
#177146=CARTESIAN_POINT('Ctrl Pts',(7.5302356243822,21.2853226580658,12.));
#177147=CARTESIAN_POINT('Ctrl Pts',(7.53153906987846,21.2896816163843,12.));
#177148=CARTESIAN_POINT('Ctrl Pts',(7.53291726078526,21.2943588989331,12.));
#177149=CARTESIAN_POINT('Ctrl Pts',(7.53436505309948,21.2993464250717,12.));
#177150=CARTESIAN_POINT('Ctrl Pts',(7.53587778251743,21.3046368712157,12.));
#177151=CARTESIAN_POINT('Ctrl Pts',(7.53745129364619,21.3102237167729,12.));
#177152=CARTESIAN_POINT('Ctrl Pts',(7.53908175169898,21.3161009456256,12.));
#177153=CARTESIAN_POINT('Ctrl Pts',(7.54076552038279,21.3222628524165,12.));
#177154=CARTESIAN_POINT('Ctrl Pts',(7.54249900377031,21.328703791771,12.));
#177155=CARTESIAN_POINT('Ctrl Pts',(7.54427868151268,21.3354182340149,12.));
#177156=CARTESIAN_POINT('Ctrl Pts',(7.5461011494835,21.3424008295038,12.));
#177157=CARTESIAN_POINT('Ctrl Pts',(7.54796316246326,21.349646476153,12.));
#177158=CARTESIAN_POINT('Ctrl Pts',(7.54986166521306,21.3571503685853,12.));
#177159=CARTESIAN_POINT('Ctrl Pts',(7.55179375777441,21.3649079431864,12.));
#177160=CARTESIAN_POINT('Ctrl Pts',(7.55375667080031,21.3729148390244,12.));
#177161=CARTESIAN_POINT('Ctrl Pts',(7.55574773403507,21.3811668478933,12.));
#177162=CARTESIAN_POINT('Ctrl Pts',(7.55776435731421,21.3896598842119,12.));
#177163=CARTESIAN_POINT('Ctrl Pts',(7.55980403700614,21.3983899952988,12.));
#177164=CARTESIAN_POINT('Ctrl Pts',(7.56186435703622,21.4073533630364,12.));
#177165=CARTESIAN_POINT('Ctrl Pts',(7.56394299313682,21.4165463106252,12.));
#177166=CARTESIAN_POINT('Ctrl Pts',(7.56603771218706,21.4259653015732,12.));
#177167=CARTESIAN_POINT('Ctrl Pts',(7.56814636360841,21.435606926151,12.));
#177168=CARTESIAN_POINT('Ctrl Pts',(7.57026687261169,21.445467890751,12.));
#177169=CARTESIAN_POINT('Ctrl Pts',(7.57239723223521,21.4555450053147,12.));
#177170=CARTESIAN_POINT('Ctrl Pts',(7.57453549743434,21.4658351740135,12.));
#177171=CARTESIAN_POINT('Ctrl Pts',(7.57667978403001,21.4763353936766,12.));
#177172=CARTESIAN_POINT('Ctrl Pts',(7.57882826679131,21.4870427508193,12.));
#177173=CARTESIAN_POINT('Ctrl Pts',(7.58097917790729,21.497954419274,12.));
#177174=CARTESIAN_POINT('Ctrl Pts',(7.58313080519158,21.5090676573866,12.));
#177175=CARTESIAN_POINT('Ctrl Pts',(7.58528148919113,21.5203798035294,12.));
#177176=CARTESIAN_POINT('Ctrl Pts',(7.58742962034834,21.5318882716736,12.));
#177177=CARTESIAN_POINT('Ctrl Pts',(7.58957363620026,21.5435905470113,12.));
#177178=CARTESIAN_POINT('Ctrl Pts',(7.59171201844792,21.5554841813466,12.));
#177179=CARTESIAN_POINT('Ctrl Pts',(7.59384329124929,21.5675667904728,12.));
#177180=CARTESIAN_POINT('Ctrl Pts',(7.59596601973588,21.5798360518978,12.));
#177181=CARTESIAN_POINT('Ctrl Pts',(7.59807880846192,21.5922897024466,12.));
#177182=CARTESIAN_POINT('Ctrl Pts',(7.60018029988238,21.6049255358843,12.));
#177183=CARTESIAN_POINT('Ctrl Pts',(7.60226917285431,21.6177414005991,12.));
#177184=CARTESIAN_POINT('Ctrl Pts',(7.60434414118299,21.6307351973823,12.));
#177185=CARTESIAN_POINT('Ctrl Pts',(7.60640395216358,21.6439048771743,12.));
#177186=CARTESIAN_POINT('Ctrl Pts',(7.60844738512871,21.6572484388079,12.));
#177187=CARTESIAN_POINT('Ctrl Pts',(7.61047325000949,21.6707639267573,12.));
#177188=CARTESIAN_POINT('Ctrl Pts',(7.61248038630264,21.6844494295813,12.));
#177189=CARTESIAN_POINT('Ctrl Pts',(7.61446766202786,21.6983030783321,12.));
#177190=CARTESIAN_POINT('Ctrl Pts',(7.61643397270424,21.7123230449835,12.));
#177191=CARTESIAN_POINT('Ctrl Pts',(7.61837824030541,21.7265075407977,12.));
#177192=CARTESIAN_POINT('Ctrl Pts',(7.62029941230854,21.7408548148657,12.));
#177193=CARTESIAN_POINT('Ctrl Pts',(7.62219646084225,21.7553631528329,12.));
#177194=CARTESIAN_POINT('Ctrl Pts',(7.62406838181164,21.7700308755584,12.));
#177195=CARTESIAN_POINT('Ctrl Pts',(7.6259141940452,21.7848563378022,12.));
#177196=CARTESIAN_POINT('Ctrl Pts',(7.62773293842409,21.7998379268583,12.));
#177197=CARTESIAN_POINT('Ctrl Pts',(7.62952367718151,21.8149740615093,12.));
#177198=CARTESIAN_POINT('Ctrl Pts',(7.6312854932304,21.8302631910197,12.));
#177199=CARTESIAN_POINT('Ctrl Pts',(7.63301748948936,21.8457037941084,12.));
#177200=CARTESIAN_POINT('Ctrl Pts',(7.63471878821203,21.8612943779086,12.));
#177201=CARTESIAN_POINT('Ctrl Pts',(7.63638853033367,21.8770334769492,12.));
#177202=CARTESIAN_POINT('Ctrl Pts',(7.63802587492007,21.8929196523511,12.));
#177203=CARTESIAN_POINT('Ctrl Pts',(7.63962999860916,21.9089514909873,12.));
#177204=CARTESIAN_POINT('Ctrl Pts',(7.64120009506539,21.9251276046546,12.));
#177205=CARTESIAN_POINT('Ctrl Pts',(7.64273537442706,21.9414466292074,12.));
#177206=CARTESIAN_POINT('Ctrl Pts',(7.64423506279153,21.9579072237653,12.));
#177207=CARTESIAN_POINT('Ctrl Pts',(7.64569840177359,21.97450807008,12.));
#177208=CARTESIAN_POINT('Ctrl Pts',(7.64712464805257,21.9912478718542,12.));
#177209=CARTESIAN_POINT('Ctrl Pts',(7.64851307293345,22.0081253540774,12.));
#177210=CARTESIAN_POINT('Ctrl Pts',(7.64986296190156,22.025139262321,12.));
#177211=CARTESIAN_POINT('Ctrl Pts',(7.65117361421346,22.0422883621176,12.));
#177212=CARTESIAN_POINT('Ctrl Pts',(7.65244434253103,22.0595714384432,12.));
#177213=CARTESIAN_POINT('Ctrl Pts',(7.65367447254944,22.0769872951596,12.));
#177214=CARTESIAN_POINT('Ctrl Pts',(7.6548633426365,22.094534754469,12.));
#177215=CARTESIAN_POINT('Ctrl Pts',(7.65601030346818,22.1122126563327,12.));
#177216=CARTESIAN_POINT('Ctrl Pts',(7.65711471769406,22.1300198579671,12.));
#177217=CARTESIAN_POINT('Ctrl Pts',(7.6581759596335,22.1479552334206,12.));
#177218=CARTESIAN_POINT('Ctrl Pts',(7.65919341496925,22.1660176731174,12.));
#177219=CARTESIAN_POINT('Ctrl Pts',(7.66016648045007,22.1842060834093,12.));
#177220=CARTESIAN_POINT('Ctrl Pts',(7.66109456359292,22.2025193860972,12.));
#177221=CARTESIAN_POINT('Ctrl Pts',(7.66197708240435,22.2209565180098,12.));
#177222=CARTESIAN_POINT('Ctrl Pts',(7.66281346512545,22.239516430656,12.));
#177223=CARTESIAN_POINT('Ctrl Pts',(7.66360314997661,22.2581980898487,12.));
#177224=CARTESIAN_POINT('Ctrl Pts',(7.66434558490972,22.2770004753332,12.));
#177225=CARTESIAN_POINT('Ctrl Pts',(7.66504022736262,22.2959225803925,12.));
#177226=CARTESIAN_POINT('Ctrl Pts',(7.66568654402441,22.3149634114823,12.));
#177227=CARTESIAN_POINT('Ctrl Pts',(7.66628401061905,22.3341219879454,12.));
#177228=CARTESIAN_POINT('Ctrl Pts',(7.66683211169133,22.3533973417013,12.));
#177229=CARTESIAN_POINT('Ctrl Pts',(7.66733034039887,22.3727885169361,12.));
#177230=CARTESIAN_POINT('Ctrl Pts',(7.66777819830819,22.3922945697782,12.));
#177231=CARTESIAN_POINT('Ctrl Pts',(7.66817519519681,22.411914567977,12.));
#177232=CARTESIAN_POINT('Ctrl Pts',(7.66852084886745,22.4316475906616,12.));
#177233=CARTESIAN_POINT('Ctrl Pts',(7.66881468496659,22.4514927280863,12.));
#177234=CARTESIAN_POINT('Ctrl Pts',(7.66905623680835,22.47144908137,12.));
#177235=CARTESIAN_POINT('Ctrl Pts',(7.66924504520301,22.4915157622308,12.));
#177236=CARTESIAN_POINT('Ctrl Pts',(7.66938065829082,22.5116918927023,12.));
#177237=CARTESIAN_POINT('Ctrl Pts',(7.66946263138115,22.5319766049191,12.));
#177238=CARTESIAN_POINT('Ctrl Pts',(7.66949052679671,22.5523690409109,12.));
#177239=CARTESIAN_POINT('Ctrl Pts',(7.66946391372299,22.5728683523829,12.));
#177240=CARTESIAN_POINT('Ctrl Pts',(7.6693823680624,22.5934737004955,12.));
#177241=CARTESIAN_POINT('Ctrl Pts',(7.66924547229434,22.6141842556248,12.));
#177242=CARTESIAN_POINT('Ctrl Pts',(7.66905281533744,22.6349991971548,12.));
#177243=CARTESIAN_POINT('Ctrl Pts',(7.66880399241353,22.6559177133133,12.));
#177244=CARTESIAN_POINT('Ctrl Pts',(7.66849860491762,22.6769390009889,12.));
#177245=CARTESIAN_POINT('Ctrl Pts',(7.66813626029276,22.6980622655446,12.));
#177246=CARTESIAN_POINT('Ctrl Pts',(7.6677165719101,22.7192867206242,12.));
#177247=CARTESIAN_POINT('Ctrl Pts',(7.66723915895412,22.7406115879508,12.));
#177248=CARTESIAN_POINT('Ctrl Pts',(7.66670364630273,22.7620360971839,12.));
#177249=CARTESIAN_POINT('Ctrl Pts',(7.66610966441259,22.7835594857697,12.));
#177250=CARTESIAN_POINT('Ctrl Pts',(7.66545684920987,22.8051809987834,12.));
#177251=CARTESIAN_POINT('Ctrl Pts',(7.66474484198552,22.8268998887679,12.));
#177252=CARTESIAN_POINT('Ctrl Pts',(7.66397328929805,22.8487154155569,12.));
#177253=CARTESIAN_POINT('Ctrl Pts',(7.66314184287333,22.870626846128,12.));
#177254=CARTESIAN_POINT('Ctrl Pts',(7.66225015950147,22.8926334544879,12.));
#177255=CARTESIAN_POINT('Ctrl Pts',(7.66129790094099,22.9147345215418,12.));
#177256=CARTESIAN_POINT('Ctrl Pts',(7.66028473382776,22.9369293349592,12.));
#177257=CARTESIAN_POINT('Ctrl Pts',(7.65921032958911,22.9592171890332,12.));
#177258=CARTESIAN_POINT('Ctrl Pts',(7.65807436436452,22.9815973845301,12.));
#177259=CARTESIAN_POINT('Ctrl Pts',(7.6568765189133,23.004069228582,12.));
#177260=CARTESIAN_POINT('Ctrl Pts',(7.65561647852554,23.0266320345792,12.));
#177261=CARTESIAN_POINT('Ctrl Pts',(7.65429393293955,23.049285122053,12.));
#177262=CARTESIAN_POINT('Ctrl Pts',(7.65290857626356,23.072027816555,12.));
#177263=CARTESIAN_POINT('Ctrl Pts',(7.65146010690464,23.0948594495246,12.));
#177264=CARTESIAN_POINT('Ctrl Pts',(7.64994822749844,23.1177793581674,12.));
#177265=CARTESIAN_POINT('Ctrl Pts',(7.64837264482929,23.1407868853815,12.));
#177266=CARTESIAN_POINT('Ctrl Pts',(7.64673306975796,23.1638813796691,12.));
#177267=CARTESIAN_POINT('Ctrl Pts',(7.64502921715482,23.1870621950452,12.));
#177268=CARTESIAN_POINT('Ctrl Pts',(7.64326080583683,23.2103286909399,12.));
#177269=CARTESIAN_POINT('Ctrl Pts',(7.64142755851507,23.2336802320912,12.));
#177270=CARTESIAN_POINT('Ctrl Pts',(7.63952920172837,23.2571161884487,12.));
#177271=CARTESIAN_POINT('Ctrl Pts',(7.63756546576374,23.2806359350853,12.));
#177272=CARTESIAN_POINT('Ctrl Pts',(7.63553608458783,23.3042388521021,12.));
#177273=CARTESIAN_POINT('Ctrl Pts',(7.63344079578162,23.3279243245241,12.));
#177274=CARTESIAN_POINT('Ctrl Pts',(7.63127934048138,23.3516917421973,12.));
#177275=CARTESIAN_POINT('Ctrl Pts',(7.62905146332597,23.3755404996638,12.));
#177276=CARTESIAN_POINT('Ctrl Pts',(7.62675691240334,23.3994699961122,12.));
#177277=CARTESIAN_POINT('Ctrl Pts',(7.62439543920053,23.4234796353544,12.));
#177278=CARTESIAN_POINT('Ctrl Pts',(7.62196679855957,23.4475688257855,12.));
#177279=CARTESIAN_POINT('Ctrl Pts',(7.61947074863977,23.4717369803438,12.));
#177280=CARTESIAN_POINT('Ctrl Pts',(7.61690705088318,23.4959835164608,12.));
#177281=CARTESIAN_POINT('Ctrl Pts',(7.61427546999298,23.5203078560128,12.));
#177282=CARTESIAN_POINT('Ctrl Pts',(7.61157577385371,23.5447094252029,12.));
#177283=CARTESIAN_POINT('Ctrl Pts',(7.60880773344599,23.5691876544243,12.));
#177284=CARTESIAN_POINT('Ctrl Pts',(7.60597112277094,23.5937419781244,12.));
#177285=CARTESIAN_POINT('Ctrl Pts',(7.60306571877806,23.6183718346576,12.));
#177286=CARTESIAN_POINT('Ctrl Pts',(7.60009130130129,23.6430766661419,12.));
#177287=CARTESIAN_POINT('Ctrl Pts',(7.59704765299572,23.6678559182876,12.));
#177288=CARTESIAN_POINT('Ctrl Pts',(7.59393455934041,23.6927090405067,12.));
#177289=CARTESIAN_POINT('Ctrl Pts',(7.59075180865326,23.7176354860457,12.));
#177290=CARTESIAN_POINT('Ctrl Pts',(7.58749919210831,23.7426347121006,12.));
#177291=CARTESIAN_POINT('Ctrl Pts',(7.58417650376271,23.7677061799376,12.));
#177292=CARTESIAN_POINT('Ctrl Pts',(7.58078354058211,23.7928493549908,12.));
#177293=CARTESIAN_POINT('Ctrl Pts',(7.57732010249065,23.8180637069977,12.));
#177294=CARTESIAN_POINT('Ctrl Pts',(7.57378599219816,23.8433487096134,12.));
#177295=CARTESIAN_POINT('Ctrl Pts',(7.5701810150071,23.8687038399598,12.));
#177296=CARTESIAN_POINT('Ctrl Pts',(7.56650497863791,23.8941285782003,12.));
#177297=CARTESIAN_POINT('Ctrl Pts',(7.56275769304773,23.9196224070759,12.));
#177298=CARTESIAN_POINT('Ctrl Pts',(7.55893897027682,23.9451848115,12.));
#177299=CARTESIAN_POINT('Ctrl Pts',(7.55504862424811,23.9708152779884,12.));
#177300=CARTESIAN_POINT('Ctrl Pts',(7.5510864709744,23.9965132953185,12.));
#177301=CARTESIAN_POINT('Ctrl Pts',(7.5470523288591,24.022278355453,12.));
#177302=CARTESIAN_POINT('Ctrl Pts',(7.54294601896144,24.0481099543353,12.));
#177303=CARTESIAN_POINT('Ctrl Pts',(7.53876736531013,24.0740075927985,12.));
#177304=CARTESIAN_POINT('Ctrl Pts',(7.53451619514649,24.0999707772642,12.));
#177305=CARTESIAN_POINT('Ctrl Pts',(7.53019233935501,24.1259990209207,12.));
#177306=CARTESIAN_POINT('Ctrl Pts',(7.52579563201423,24.1520918425364,12.));
#177307=CARTESIAN_POINT('Ctrl Pts',(7.52132590953801,24.1782487641594,12.));
#177308=CARTESIAN_POINT('Ctrl Pts',(7.51678300997949,24.2044693092349,12.));
#177309=CARTESIAN_POINT('Ctrl Pts',(7.5121667722218,24.2307530003887,12.));
#177310=CARTESIAN_POINT('Ctrl Pts',(7.50747703535133,24.2570993577034,12.));
#177311=CARTESIAN_POINT('Ctrl Pts',(7.50271363765151,24.2835078958973,12.));
#177312=CARTESIAN_POINT('Ctrl Pts',(7.49787641695438,24.3099781253355,12.));
#177313=CARTESIAN_POINT('Ctrl Pts',(7.4929652125242,24.3365095573685,12.));
#177314=CARTESIAN_POINT('Ctrl Pts',(7.48797986651908,24.3631017084524,12.));
#177315=CARTESIAN_POINT('Ctrl Pts',(7.482920225693,24.3897541049254,12.));
#177316=CARTESIAN_POINT('Ctrl Pts',(7.47778614286564,24.4164662871163,12.));
#177317=CARTESIAN_POINT('Ctrl Pts',(7.47257747883246,24.443237814649,12.));
#177318=CARTESIAN_POINT('Ctrl Pts',(7.46729410308786,24.4700682684524,12.));
#177319=CARTESIAN_POINT('Ctrl Pts',(7.46193588961463,24.4969572391483,12.));
#177320=CARTESIAN_POINT('Ctrl Pts',(7.45650271335861,24.5239043173072,12.));
#177321=CARTESIAN_POINT('Ctrl Pts',(7.4509944465116,24.5509090831559,12.));
#177322=CARTESIAN_POINT('Ctrl Pts',(7.44541095473134,24.577971096086,12.));
#177323=CARTESIAN_POINT('Ctrl Pts',(7.43975209375503,24.6050898852368,12.));
#177324=CARTESIAN_POINT('Ctrl Pts',(7.43401770489523,24.6322649369517,12.));
#177325=CARTESIAN_POINT('Ctrl Pts',(7.42820762159125,24.6594957128756,12.));
#177326=CARTESIAN_POINT('Ctrl Pts',(7.42232167766265,24.6867816727192,12.));
#177327=CARTESIAN_POINT('Ctrl Pts',(7.41635971481674,24.7141222950051,12.));
#177328=CARTESIAN_POINT('Ctrl Pts',(7.41032159082381,24.7415170994784,12.));
#177329=CARTESIAN_POINT('Ctrl Pts',(7.40420718661602,24.7689656668983,12.));
#177330=CARTESIAN_POINT('Ctrl Pts',(7.39801641583012,24.7964676646431,12.));
#177331=CARTESIAN_POINT('Ctrl Pts',(7.39174922585808,24.8240228520893,12.));
#177332=CARTESIAN_POINT('Ctrl Pts',(7.3854055890362,24.8516310625176,12.));
#177333=CARTESIAN_POINT('Ctrl Pts',(7.37898549640269,24.8792921911115,12.));
#177334=CARTESIAN_POINT('Ctrl Pts',(7.37378825961676,24.901463382605,12.));
#177335=CARTESIAN_POINT('Ctrl Pts',(7.3698559312009,24.9181155530543,12.));
#177336=CARTESIAN_POINT('Ctrl Pts',(7.36721909028842,24.9292275670674,12.));
#177337=CARTESIAN_POINT('Ctrl Pts',(7.36589684767344,24.9347862158358,12.));
#177338=CARTESIAN_POINT('',(6.08833931617699,25.2771067246846,12.));
#177339=CARTESIAN_POINT('Origin',(0.,0.,12.));
#177340=CARTESIAN_POINT('',(4.11585220600461,22.1738711152697,12.));
#177341=CARTESIAN_POINT('Ctrl Pts',(6.08833931617699,25.2771067246846,12.));
#177342=CARTESIAN_POINT('Ctrl Pts',(6.08441489609793,25.2729539149517,12.));
#177343=CARTESIAN_POINT('Ctrl Pts',(6.0765753178749,25.2646490489923,12.));
#177344=CARTESIAN_POINT('Ctrl Pts',(6.06484373634546,25.2521940105705,12.));
#177345=CARTESIAN_POINT('Ctrl Pts',(6.04925720151218,25.2355918139032,12.));
#177346=CARTESIAN_POINT('Ctrl Pts',(6.02986667389996,25.21484662016,12.));
#177347=CARTESIAN_POINT('Ctrl Pts',(6.01056881804612,25.1941090269819,12.));
#177348=CARTESIAN_POINT('Ctrl Pts',(5.99136367859754,25.1733791296259,12.));
#177349=CARTESIAN_POINT('Ctrl Pts',(5.97225131495616,25.1526570863092,12.));
#177350=CARTESIAN_POINT('Ctrl Pts',(5.95323180187378,25.1319431317237,12.));
#177351=CARTESIAN_POINT('Ctrl Pts',(5.93430523086834,25.1112375971106,12.));
#177352=CARTESIAN_POINT('Ctrl Pts',(5.91547170844447,25.0905409050773,12.));
#177353=CARTESIAN_POINT('Ctrl Pts',(5.89673135155514,25.0698535426514,12.));
#177354=CARTESIAN_POINT('Ctrl Pts',(5.87808428385365,25.0491760405911,12.));
#177355=CARTESIAN_POINT('Ctrl Pts',(5.85953063156826,25.0285089498899,12.));
#177356=CARTESIAN_POINT('Ctrl Pts',(5.84107051963071,25.0078528200564,12.));
#177357=CARTESIAN_POINT('Ctrl Pts',(5.82270406744198,24.9872081752734,12.));
#177358=CARTESIAN_POINT('Ctrl Pts',(5.80443138549726,24.9665754954496,12.));
#177359=CARTESIAN_POINT('Ctrl Pts',(5.78625257775681,24.945955229334,12.));
#177360=CARTESIAN_POINT('Ctrl Pts',(5.76816774342219,24.9253478043656,12.));
#177361=CARTESIAN_POINT('Ctrl Pts',(5.75017697890804,24.904753637648,12.));
#177362=CARTESIAN_POINT('Ctrl Pts',(5.73228037976926,24.884173146722,12.));
#177363=CARTESIAN_POINT('Ctrl Pts',(5.71447804252027,24.8636067597669,12.));
#177364=CARTESIAN_POINT('Ctrl Pts',(5.69677006679444,24.8430549277621,12.));
#177365=CARTESIAN_POINT('Ctrl Pts',(5.67915655496542,24.8225181223845,12.));
#177366=CARTESIAN_POINT('Ctrl Pts',(5.66163761114921,24.8019968304605,12.));
#177367=CARTESIAN_POINT('Ctrl Pts',(5.6442133404226,24.781491549672,12.));
#177368=CARTESIAN_POINT('Ctrl Pts',(5.62688384790923,24.7610027835697,12.));
#177369=CARTESIAN_POINT('Ctrl Pts',(5.60964923798491,24.7405310372739,12.));
#177370=CARTESIAN_POINT('Ctrl Pts',(5.59250961323987,24.7200768119088,12.));
#177371=CARTESIAN_POINT('Ctrl Pts',(5.57546507427754,24.6996406035517,12.));
#177372=CARTESIAN_POINT('Ctrl Pts',(5.55851572025376,24.6792229061794,12.));
#177373=CARTESIAN_POINT('Ctrl Pts',(5.54166164919583,24.6588242134738,12.));
#177374=CARTESIAN_POINT('Ctrl Pts',(5.52490295840991,24.6384450211467,12.));
#177375=CARTESIAN_POINT('Ctrl Pts',(5.50823974481962,24.6180858289179,12.));
#177376=CARTESIAN_POINT('Ctrl Pts',(5.49167210537246,24.5977471429364,12.));
#177377=CARTESIAN_POINT('Ctrl Pts',(5.47520013724419,24.5774294770329,12.));
#177378=CARTESIAN_POINT('Ctrl Pts',(5.45882393762261,24.5571333514842,12.));
#177379=CARTESIAN_POINT('Ctrl Pts',(5.4425436035688,24.5368592922863,12.));
#177380=CARTESIAN_POINT('Ctrl Pts',(5.42635923183419,24.5166078302108,12.));
#177381=CARTESIAN_POINT('Ctrl Pts',(5.41027091869241,24.4963794999831,12.));
#177382=CARTESIAN_POINT('Ctrl Pts',(5.39427875973824,24.4761748393321,12.));
#177383=CARTESIAN_POINT('Ctrl Pts',(5.37838284973695,24.4559943883157,12.));
#177384=CARTESIAN_POINT('Ctrl Pts',(5.36258328273627,24.435838689915,12.));
#177385=CARTESIAN_POINT('Ctrl Pts',(5.34688015213537,24.4157082904614,12.));
#177386=CARTESIAN_POINT('Ctrl Pts',(5.33127355076033,24.3956037401293,12.));
#177387=CARTESIAN_POINT('Ctrl Pts',(5.31576357092526,24.3755255933917,12.));
#177388=CARTESIAN_POINT('Ctrl Pts',(5.30035030449063,24.3554744095075,12.));
#177389=CARTESIAN_POINT('Ctrl Pts',(5.28503384290648,24.3354507529414,12.));
#177390=CARTESIAN_POINT('Ctrl Pts',(5.26981427718798,24.3154551932221,12.));
#177391=CARTESIAN_POINT('Ctrl Pts',(5.25469169788856,24.2954883048447,12.));
#177392=CARTESIAN_POINT('Ctrl Pts',(5.23966619506289,24.2755506671525,12.));
#177393=CARTESIAN_POINT('Ctrl Pts',(5.22473785822442,24.2556428642294,12.));
#177394=CARTESIAN_POINT('Ctrl Pts',(5.20990677629176,24.2357654847766,12.));
#177395=CARTESIAN_POINT('Ctrl Pts',(5.19517303753647,24.2159191220171,12.));
#177396=CARTESIAN_POINT('Ctrl Pts',(5.18053672961398,24.1961043738756,12.));
#177397=CARTESIAN_POINT('Ctrl Pts',(5.16599793957985,24.1763218431344,12.));
#177398=CARTESIAN_POINT('Ctrl Pts',(5.15155675390079,24.1565721375971,12.));
#177399=CARTESIAN_POINT('Ctrl Pts',(5.13721325845745,24.1368558702443,12.));
#177400=CARTESIAN_POINT('Ctrl Pts',(5.12296753853857,24.117173659394,12.));
#177401=CARTESIAN_POINT('Ctrl Pts',(5.10881967883124,24.0975261288444,12.));
#177402=CARTESIAN_POINT('Ctrl Pts',(5.09476976342616,24.0779139079264,12.));
#177403=CARTESIAN_POINT('Ctrl Pts',(5.0808178758127,24.0583376315636,12.));
#177404=CARTESIAN_POINT('Ctrl Pts',(5.06696409886639,24.0387979403268,12.));
#177405=CARTESIAN_POINT('Ctrl Pts',(5.05320851483068,24.0192954804896,12.));
#177406=CARTESIAN_POINT('Ctrl Pts',(5.03955120528527,23.9998309040747,12.));
#177407=CARTESIAN_POINT('Ctrl Pts',(5.02599225112461,23.9804048689228,12.));
#177408=CARTESIAN_POINT('Ctrl Pts',(5.01253173257458,23.9610180388271,12.));
#177409=CARTESIAN_POINT('Ctrl Pts',(4.99916972919309,23.9416710836529,12.));
#177410=CARTESIAN_POINT('Ctrl Pts',(4.98590631986532,23.9223646794591,12.));
#177411=CARTESIAN_POINT('Ctrl Pts',(4.97274158279228,23.9030995086164,12.));
#177412=CARTESIAN_POINT('Ctrl Pts',(4.95967559546565,23.883876259922,12.));
#177413=CARTESIAN_POINT('Ctrl Pts',(4.94670843465868,23.8646956287172,12.));
#177414=CARTESIAN_POINT('Ctrl Pts',(4.93384017643441,23.8455583170062,12.));
#177415=CARTESIAN_POINT('Ctrl Pts',(4.92107089613976,23.8264650335721,12.));
#177416=CARTESIAN_POINT('Ctrl Pts',(4.90840066839346,23.8074164940897,12.));
#177417=CARTESIAN_POINT('Ctrl Pts',(4.89582956706771,23.7884134212381,12.));
#177418=CARTESIAN_POINT('Ctrl Pts',(4.88335766525565,23.7694565448044,12.));
#177419=CARTESIAN_POINT('Ctrl Pts',(4.87098503527142,23.7505466018239,12.));
#177420=CARTESIAN_POINT('Ctrl Pts',(4.85871174865491,23.7316843367308,12.));
#177421=CARTESIAN_POINT('Ctrl Pts',(4.84653787616422,23.7128705015014,12.));
#177422=CARTESIAN_POINT('Ctrl Pts',(4.83446348776267,23.6941058557971,12.));
#177423=CARTESIAN_POINT('Ctrl Pts',(4.82248865259569,23.6753911671023,12.));
#177424=CARTESIAN_POINT('Ctrl Pts',(4.81061343896442,23.6567272108631,12.));
#177425=CARTESIAN_POINT('Ctrl Pts',(4.79883791433229,23.6381147706581,12.));
#177426=CARTESIAN_POINT('Ctrl Pts',(4.78716214532104,23.6195546383625,12.));
#177427=CARTESIAN_POINT('Ctrl Pts',(4.77558619769875,23.6010476143099,12.));
#177428=CARTESIAN_POINT('Ctrl Pts',(4.7641101363625,23.5825945074535,12.));
#177429=CARTESIAN_POINT('Ctrl Pts',(4.75273402530615,23.564196135517,12.));
#177430=CARTESIAN_POINT('Ctrl Pts',(4.74145792760698,23.5458533251715,12.));
#177431=CARTESIAN_POINT('Ctrl Pts',(4.73028190543031,23.5275669122378,12.));
#177432=CARTESIAN_POINT('Ctrl Pts',(4.71920602001904,23.5093377418784,12.));
#177433=CARTESIAN_POINT('Ctrl Pts',(4.7082303316782,23.491166668789,12.));
#177434=CARTESIAN_POINT('Ctrl Pts',(4.69735489975023,23.4730545573849,12.));
#177435=CARTESIAN_POINT('Ctrl Pts',(4.68657978258297,23.4550022819853,12.));
#177436=CARTESIAN_POINT('Ctrl Pts',(4.6759050375305,23.4370107270444,12.));
#177437=CARTESIAN_POINT('Ctrl Pts',(4.66533072094663,23.4190807873798,12.));
#177438=CARTESIAN_POINT('Ctrl Pts',(4.65485688816921,23.4012133683957,12.));
#177439=CARTESIAN_POINT('Ctrl Pts',(4.64448359349935,23.383409386307,12.));
#177440=CARTESIAN_POINT('Ctrl Pts',(4.63421089016554,23.3656697683496,12.));
#177441=CARTESIAN_POINT('Ctrl Pts',(4.62403883030823,23.3479954530281,12.));
#177442=CARTESIAN_POINT('Ctrl Pts',(4.61396746497848,23.3303873903947,12.));
#177443=CARTESIAN_POINT('Ctrl Pts',(4.60399684412174,23.3128465423119,12.));
#177444=CARTESIAN_POINT('Ctrl Pts',(4.59412701655749,23.295373882719,12.));
#177445=CARTESIAN_POINT('Ctrl Pts',(4.58435802994674,23.2779703978868,12.));
#177446=CARTESIAN_POINT('Ctrl Pts',(4.5746899307607,23.2606370866853,12.));
#177447=CARTESIAN_POINT('Ctrl Pts',(4.5651227642781,23.2433749609117,12.));
#177448=CARTESIAN_POINT('Ctrl Pts',(4.55565657456956,23.2261850456055,12.));
#177449=CARTESIAN_POINT('Ctrl Pts',(4.54629140447542,23.2090683793627,12.));
#177450=CARTESIAN_POINT('Ctrl Pts',(4.53702729557585,23.1920260146474,12.));
#177451=CARTESIAN_POINT('Ctrl Pts',(4.52786428815047,23.1750590180923,12.));
#177452=CARTESIAN_POINT('Ctrl Pts',(4.51880242116785,23.1581684708778,12.));
#177453=CARTESIAN_POINT('Ctrl Pts',(4.50984173227087,23.1413554691136,12.));
#177454=CARTESIAN_POINT('Ctrl Pts',(4.50098225775178,23.1246211242117,12.));
#177455=CARTESIAN_POINT('Ctrl Pts',(4.49222403252201,23.1079665632629,12.));
#177456=CARTESIAN_POINT('Ctrl Pts',(4.48356709006756,23.0913929293909,12.));
#177457=CARTESIAN_POINT('Ctrl Pts',(4.47501146242821,23.0749013821868,12.));
#177458=CARTESIAN_POINT('Ctrl Pts',(4.46655718018205,23.0584930981723,12.));
#177459=CARTESIAN_POINT('Ctrl Pts',(4.45820427241676,23.0421692712466,12.));
#177460=CARTESIAN_POINT('Ctrl Pts',(4.44995276669698,23.0259311131395,12.));
#177461=CARTESIAN_POINT('Ctrl Pts',(4.44180268901666,23.0097798538399,12.));
#177462=CARTESIAN_POINT('Ctrl Pts',(4.43375406376904,22.9937167421009,12.));
#177463=CARTESIAN_POINT('Ctrl Pts',(4.42580691372771,22.9777430460021,12.));
#177464=CARTESIAN_POINT('Ctrl Pts',(4.41796126001309,22.9618600534866,12.));
#177465=CARTESIAN_POINT('Ctrl Pts',(4.41021712205547,22.9460690729093,12.));
#177466=CARTESIAN_POINT('Ctrl Pts',(4.40257451754307,22.9303714335549,12.));
#177467=CARTESIAN_POINT('Ctrl Pts',(4.39503346238454,22.9147684862425,12.));
#177468=CARTESIAN_POINT('Ctrl Pts',(4.38759397068391,22.8992616040108,12.));
#177469=CARTESIAN_POINT('Ctrl Pts',(4.38025605470089,22.8838521827702,12.));
#177470=CARTESIAN_POINT('Ctrl Pts',(4.37301972480752,22.8685416419725,12.));
#177471=CARTESIAN_POINT('Ctrl Pts',(4.36588498943009,22.8533314252419,12.));
#177472=CARTESIAN_POINT('Ctrl Pts',(4.35885185500559,22.838223001118,12.));
#177473=CARTESIAN_POINT('Ctrl Pts',(4.35192032594801,22.8232178638873,12.));
#177474=CARTESIAN_POINT('Ctrl Pts',(4.34509040460065,22.808317534379,12.));
#177475=CARTESIAN_POINT('Ctrl Pts',(4.33836209118442,22.7935235607807,12.));
#177476=CARTESIAN_POINT('Ctrl Pts',(4.33173538373182,22.7788375194081,12.));
#177477=CARTESIAN_POINT('Ctrl Pts',(4.32521027803747,22.764261015648,12.));
#177478=CARTESIAN_POINT('Ctrl Pts',(4.3187867676123,22.7497956849852,12.));
#177479=CARTESIAN_POINT('Ctrl Pts',(4.3124648436255,22.7354431939927,12.));
#177480=CARTESIAN_POINT('Ctrl Pts',(4.30624449484074,22.7212052413384,12.));
#177481=CARTESIAN_POINT('Ctrl Pts',(4.30012570754066,22.707083558756,12.));
#177482=CARTESIAN_POINT('Ctrl Pts',(4.29410846547061,22.6930799122545,12.));
#177483=CARTESIAN_POINT('Ctrl Pts',(4.28819274977766,22.6791961033537,12.));
#177484=CARTESIAN_POINT('Ctrl Pts',(4.28237853894059,22.665433970311,12.));
#177485=CARTESIAN_POINT('Ctrl Pts',(4.27666580869117,22.6517953893303,12.));
#177486=CARTESIAN_POINT('Ctrl Pts',(4.27105453192999,22.6382822758171,12.));
#177487=CARTESIAN_POINT('Ctrl Pts',(4.26554467865571,22.6248965859975,12.));
#177488=CARTESIAN_POINT('Ctrl Pts',(4.26013621588303,22.611640318482,12.));
#177489=CARTESIAN_POINT('Ctrl Pts',(4.25482910755485,22.5985155158637,12.));
#177490=CARTESIAN_POINT('Ctrl Pts',(4.24962331444184,22.5855242662479,12.));
#177491=CARTESIAN_POINT('Ctrl Pts',(4.24451879404858,22.5726687049922,12.));
#177492=CARTESIAN_POINT('Ctrl Pts',(4.23951550052526,22.559951016643,12.));
#177493=CARTESIAN_POINT('Ctrl Pts',(4.23461338456713,22.5473734368086,12.));
#177494=CARTESIAN_POINT('Ctrl Pts',(4.22981239330731,22.5349382540587,12.));
#177495=CARTESIAN_POINT('Ctrl Pts',(4.2251124702004,22.5226478117885,12.));
#177496=CARTESIAN_POINT('Ctrl Pts',(4.22051355490196,22.5105045108882,12.));
#177497=CARTESIAN_POINT('Ctrl Pts',(4.21601558313908,22.4985108124229,12.));
#177498=CARTESIAN_POINT('Ctrl Pts',(4.21161848657428,22.4866692403147,12.));
#177499=CARTESIAN_POINT('Ctrl Pts',(4.20732219265648,22.4749823839915,12.));
#177500=CARTESIAN_POINT('Ctrl Pts',(4.2031266244817,22.4634529011433,12.));
#177501=CARTESIAN_POINT('Ctrl Pts',(4.19903170066354,22.4520835205419,12.));
#177502=CARTESIAN_POINT('Ctrl Pts',(4.1950373351886,22.4408770448917,12.));
#177503=CARTESIAN_POINT('Ctrl Pts',(4.19114343726941,22.4298363535421,12.));
#177504=CARTESIAN_POINT('Ctrl Pts',(4.1873499111772,22.4189644056115,12.));
#177505=CARTESIAN_POINT('Ctrl Pts',(4.1836566560085,22.4082642454453,12.));
#177506=CARTESIAN_POINT('Ctrl Pts',(4.18006356544882,22.3977390078075,12.));
#177507=CARTESIAN_POINT('Ctrl Pts',(4.17657052752825,22.3873919231334,12.));
#177508=CARTESIAN_POINT('Ctrl Pts',(4.17317742436145,22.3772263228617,12.));
#177509=CARTESIAN_POINT('Ctrl Pts',(4.16988413199457,22.36724564276,12.));
#177510=CARTESIAN_POINT('Ctrl Pts',(4.166690520266,22.3574534257396,12.));
#177511=CARTESIAN_POINT('Ctrl Pts',(4.16359645263187,22.3478533253889,12.));
#177512=CARTESIAN_POINT('Ctrl Pts',(4.16060178604164,22.3384491078602,12.));
#177513=CARTESIAN_POINT('Ctrl Pts',(4.15770637047889,22.3292446628959,12.));
#177514=CARTESIAN_POINT('Ctrl Pts',(4.15491004835281,22.3202440186979,12.));
#177515=CARTESIAN_POINT('Ctrl Pts',(4.1522126539699,22.3114513545185,12.));
#177516=CARTESIAN_POINT('Ctrl Pts',(4.14961401285522,22.3028710166933,12.));
#177517=CARTESIAN_POINT('Ctrl Pts',(4.14711394168556,22.2945075198467,12.));
#177518=CARTESIAN_POINT('Ctrl Pts',(4.14471224859295,22.2863655389166,12.));
#177519=CARTESIAN_POINT('Ctrl Pts',(4.14240873321984,22.2784499072027,12.));
#177520=CARTESIAN_POINT('Ctrl Pts',(4.14020318715991,22.2707656042457,12.));
#177521=CARTESIAN_POINT('Ctrl Pts',(4.13809539255421,22.2633177913972,12.));
#177522=CARTESIAN_POINT('Ctrl Pts',(4.13608511977225,22.2561118708421,12.));
#177523=CARTESIAN_POINT('Ctrl Pts',(4.1341721255881,22.249153531779,12.));
#177524=CARTESIAN_POINT('Ctrl Pts',(4.1323561506016,22.2424488153523,12.));
#177525=CARTESIAN_POINT('Ctrl Pts',(4.13063692157498,22.2360040565533,12.));
#177526=CARTESIAN_POINT('Ctrl Pts',(4.12901415463379,22.2298258043947,12.));
#177527=CARTESIAN_POINT('Ctrl Pts',(4.12748755830104,22.2239207458781,12.));
#177528=CARTESIAN_POINT('Ctrl Pts',(4.12605683613307,22.2182956401341,12.));
#177529=CARTESIAN_POINT('Ctrl Pts',(4.12472167516607,22.2129576146671,12.));
#177530=CARTESIAN_POINT('Ctrl Pts',(4.12348173702023,22.2079143941719,12.));
#177531=CARTESIAN_POINT('Ctrl Pts',(4.12233664408227,22.2031746532106,12.));
#177532=CARTESIAN_POINT('Ctrl Pts',(4.12128598183522,22.1987479618246,12.));
#177533=CARTESIAN_POINT('Ctrl Pts',(4.12032932637736,22.1946440958098,12.));
#177534=CARTESIAN_POINT('Ctrl Pts',(4.11946626228636,22.1908725908525,12.));
#177535=CARTESIAN_POINT('Ctrl Pts',(4.11869641271773,22.1874419861496,12.));
#177536=CARTESIAN_POINT('Ctrl Pts',(4.11801938107479,22.1843613164855,12.));
#177537=CARTESIAN_POINT('Ctrl Pts',(4.11743469691756,22.1816414985788,12.));
#177538=CARTESIAN_POINT('Ctrl Pts',(4.11694173195003,22.179297473024,12.));
#177539=CARTESIAN_POINT('Ctrl Pts',(4.11653973150518,22.177347426894,12.));
#177540=CARTESIAN_POINT('Ctrl Pts',(4.11622797217068,22.1758088296598,12.));
#177541=CARTESIAN_POINT('Ctrl Pts',(4.11600589882845,22.1746949858775,12.));
#177542=CARTESIAN_POINT('Ctrl Pts',(4.11589976826166,22.1741488021234,12.));
#177543=CARTESIAN_POINT('Ctrl Pts',(4.11586035878287,22.1739341411687,12.));
#177544=CARTESIAN_POINT('Ctrl Pts',(4.11585194677442,22.173877682324,12.));
#177545=CARTESIAN_POINT('Ctrl Pts',(4.11585220600461,22.1738711152697,12.));
#177546=CARTESIAN_POINT('',(4.01396149767429,21.624941921198,12.));
#177547=CARTESIAN_POINT('',(1.96187429785751,10.5694630535049,12.));
#177548=CARTESIAN_POINT('',(3.44230496120419,21.2226420728916,12.));
#177549=CARTESIAN_POINT('Origin',(3.52235856495312,21.7161918885402,12.));
#177550=CARTESIAN_POINT('',(2.16781269186828,21.3904321633055,12.));
#177551=CARTESIAN_POINT('Origin',(1.31973449697531E-13,7.6920903736728E-13,
12.));
#177552=CARTESIAN_POINT('',(1.71975774210842,21.9269795755927,12.));
#177553=CARTESIAN_POINT('Origin',(2.21822694051638,21.8878840740801,12.));
#177554=CARTESIAN_POINT('',(1.7634122053118,22.4835757167854,12.));
#177555=CARTESIAN_POINT('',(0.881706102655883,11.2417878583927,12.));
#177556=CARTESIAN_POINT('',(0.661312440730901,25.991588367311,12.));
#177557=CARTESIAN_POINT('Ctrl Pts',(1.7634122053118,22.4835757167854,12.));
#177558=CARTESIAN_POINT('Ctrl Pts',(1.7634141553879,22.4835819929788,12.));
#177559=CARTESIAN_POINT('Ctrl Pts',(1.76342064263637,22.4836387052228,12.));
#177560=CARTESIAN_POINT('Ctrl Pts',(1.76343813434659,22.4838562517064,12.));
#177561=CARTESIAN_POINT('Ctrl Pts',(1.76347698284861,22.4844112933125,12.));
#177562=CARTESIAN_POINT('Ctrl Pts',(1.76355076045549,22.4855446605991,12.));
#177563=CARTESIAN_POINT('Ctrl Pts',(1.76364784232925,22.4871115206572,12.));
#177564=CARTESIAN_POINT('Ctrl Pts',(1.76376424879468,22.4890991659479,12.));
#177565=CARTESIAN_POINT('Ctrl Pts',(1.76389475965714,22.4914909094908,12.));
#177566=CARTESIAN_POINT('Ctrl Pts',(1.76403393880316,22.4942693792449,12.));
#177567=CARTESIAN_POINT('Ctrl Pts',(1.76417731243483,22.4974203063191,12.));
#177568=CARTESIAN_POINT('Ctrl Pts',(1.76432160068737,22.5009332677316,12.));
#177569=CARTESIAN_POINT('Ctrl Pts',(1.76446408210364,22.5047996391978,12.));
#177570=CARTESIAN_POINT('Ctrl Pts',(1.76460218257313,22.5090112700212,12.));
#177571=CARTESIAN_POINT('Ctrl Pts',(1.76473303281149,22.5135590569554,12.));
#177572=CARTESIAN_POINT('Ctrl Pts',(1.76485369319895,22.5184336670207,12.));
#177573=CARTESIAN_POINT('Ctrl Pts',(1.76496128643375,22.5236259635515,12.));
#177574=CARTESIAN_POINT('Ctrl Pts',(1.76505320262759,22.529127665298,12.));
#177575=CARTESIAN_POINT('Ctrl Pts',(1.76512711563254,22.5349313983571,12.));
#177576=CARTESIAN_POINT('Ctrl Pts',(1.76518087841493,22.5410303590892,12.));
#177577=CARTESIAN_POINT('Ctrl Pts',(1.76521245524047,22.5474180954006,12.));
#177578=CARTESIAN_POINT('Ctrl Pts',(1.76521983384062,22.5540882235837,12.));
#177579=CARTESIAN_POINT('Ctrl Pts',(1.7652010450045,22.5610344912501,12.));
#177580=CARTESIAN_POINT('Ctrl Pts',(1.76515418518831,22.5682508499873,12.));
#177581=CARTESIAN_POINT('Ctrl Pts',(1.76507744026746,22.5757315316353,12.));
#177582=CARTESIAN_POINT('Ctrl Pts',(1.76496910283088,22.5834711038022,12.));
#177583=CARTESIAN_POINT('Ctrl Pts',(1.76482755288411,22.5914644078106,12.));
#177584=CARTESIAN_POINT('Ctrl Pts',(1.76465124413557,22.5997065145638,12.));
#177585=CARTESIAN_POINT('Ctrl Pts',(1.76443868648015,22.6081926681343,12.));
#177586=CARTESIAN_POINT('Ctrl Pts',(1.76418843543739,22.6169182517694,12.));
#177587=CARTESIAN_POINT('Ctrl Pts',(1.76389909571403,22.6258787994848,12.));
#177588=CARTESIAN_POINT('Ctrl Pts',(1.76356932176273,22.6350699979359,12.));
#177589=CARTESIAN_POINT('Ctrl Pts',(1.76319782013916,22.6444876940423,12.));
#177590=CARTESIAN_POINT('Ctrl Pts',(1.76278334912561,22.6541278938409,12.));
#177591=CARTESIAN_POINT('Ctrl Pts',(1.76232471392568,22.6639867471753,12.));
#177592=CARTESIAN_POINT('Ctrl Pts',(1.76182076289525,22.67406053567,12.));
#177593=CARTESIAN_POINT('Ctrl Pts',(1.76127038310614,22.684345658525,12.));
#177594=CARTESIAN_POINT('Ctrl Pts',(1.76067249704886,22.6948386219851,12.));
#177595=CARTESIAN_POINT('Ctrl Pts',(1.76002606202401,22.7055360375485,12.));
#177596=CARTESIAN_POINT('Ctrl Pts',(1.75933006905925,22.7164346186006,12.));
#177597=CARTESIAN_POINT('Ctrl Pts',(1.75858354204633,22.72753117773,12.));
#177598=CARTESIAN_POINT('Ctrl Pts',(1.75778553673244,22.7388226235559,12.));
#177599=CARTESIAN_POINT('Ctrl Pts',(1.75693513908907,22.750305955645,12.));
#177600=CARTESIAN_POINT('Ctrl Pts',(1.75603146371641,22.7619782595013,12.));
#177601=CARTESIAN_POINT('Ctrl Pts',(1.75507365227131,22.7738367016118,12.));
#177602=CARTESIAN_POINT('Ctrl Pts',(1.75406087182936,22.7858785242361,12.));
#177603=CARTESIAN_POINT('Ctrl Pts',(1.75299231391466,22.7981010424314,12.));
#177604=CARTESIAN_POINT('Ctrl Pts',(1.75186719365592,22.8105016414713,12.));
#177605=CARTESIAN_POINT('Ctrl Pts',(1.75068474890883,22.8230777741284,12.));
#177606=CARTESIAN_POINT('Ctrl Pts',(1.74944423940115,22.8358269579853,12.));
#177607=CARTESIAN_POINT('Ctrl Pts',(1.74814494588492,22.8487467728076,12.));
#177608=CARTESIAN_POINT('Ctrl Pts',(1.74678616930664,22.8618348580235,12.));
#177609=CARTESIAN_POINT('Ctrl Pts',(1.74536722998201,22.8750889101696,12.));
#177610=CARTESIAN_POINT('Ctrl Pts',(1.74388746677702,22.888506680335,12.));
#177611=CARTESIAN_POINT('Ctrl Pts',(1.7423462363008,22.9020859716141,12.));
#177612=CARTESIAN_POINT('Ctrl Pts',(1.74074291231058,22.9158246373363,12.));
#177613=CARTESIAN_POINT('Ctrl Pts',(1.73907688511666,22.9297205792586,12.));
#177614=CARTESIAN_POINT('Ctrl Pts',(1.73734756100039,22.9437717457826,12.));
#177615=CARTESIAN_POINT('Ctrl Pts',(1.73555436162769,22.9579761301063,12.));
#177616=CARTESIAN_POINT('Ctrl Pts',(1.73369672350814,22.9723317685688,12.));
#177617=CARTESIAN_POINT('Ctrl Pts',(1.7317740975019,22.9868367391978,12.));
#177618=CARTESIAN_POINT('Ctrl Pts',(1.72978594832136,23.001489160189,12.));
#177619=CARTESIAN_POINT('Ctrl Pts',(1.72773175404708,23.0162871884168,12.));
#177620=CARTESIAN_POINT('Ctrl Pts',(1.72561100564045,23.0312290178883,12.));
#177621=CARTESIAN_POINT('Ctrl Pts',(1.72342320653746,23.0463128785531,12.));
#177622=CARTESIAN_POINT('Ctrl Pts',(1.72116787225991,23.0615370351562,12.));
#177623=CARTESIAN_POINT('Ctrl Pts',(1.71884453003027,23.0768997860709,12.));
#177624=CARTESIAN_POINT('Ctrl Pts',(1.71645271839296,23.0923994621213,12.));
#177625=CARTESIAN_POINT('Ctrl Pts',(1.71399198684704,23.1080344254286,12.));
#177626=CARTESIAN_POINT('Ctrl Pts',(1.71146189552174,23.1238030684925,12.));
#177627=CARTESIAN_POINT('Ctrl Pts',(1.70886201485452,23.1397038132356,12.));
#177628=CARTESIAN_POINT('Ctrl Pts',(1.70619192527852,23.1557351100614,12.));
#177629=CARTESIAN_POINT('Ctrl Pts',(1.70345121691276,23.1718954368751,12.));
#177630=CARTESIAN_POINT('Ctrl Pts',(1.7006394892701,23.1881832981851,12.));
#177631=CARTESIAN_POINT('Ctrl Pts',(1.69775635099443,23.2045972243767,12.));
#177632=CARTESIAN_POINT('Ctrl Pts',(1.69480141959953,23.2211357709374,12.));
#177633=CARTESIAN_POINT('Ctrl Pts',(1.69177432121711,23.2377975177013,12.));
#177634=CARTESIAN_POINT('Ctrl Pts',(1.68867469034896,23.2545810680537,12.));
#177635=CARTESIAN_POINT('Ctrl Pts',(1.68550216963258,23.2714850482246,12.));
#177636=CARTESIAN_POINT('Ctrl Pts',(1.68225640962168,23.2885081066951,12.));
#177637=CARTESIAN_POINT('Ctrl Pts',(1.67893706857117,23.3056489135611,12.));
#177638=CARTESIAN_POINT('Ctrl Pts',(1.67554381222994,23.3229061599145,12.));
#177639=CARTESIAN_POINT('Ctrl Pts',(1.67207631363921,23.3402785571865,12.));
#177640=CARTESIAN_POINT('Ctrl Pts',(1.66853425293995,23.3577648365744,12.));
#177641=CARTESIAN_POINT('Ctrl Pts',(1.66491731718876,23.3753637485545,12.));
#177642=CARTESIAN_POINT('Ctrl Pts',(1.66122520018011,23.3930740623619,12.));
#177643=CARTESIAN_POINT('Ctrl Pts',(1.65745760227505,23.4108945654805,12.));
#177644=CARTESIAN_POINT('Ctrl Pts',(1.65361423023728,23.4288240631043,12.));
#177645=CARTESIAN_POINT('Ctrl Pts',(1.6496947970734,23.4468613776574,12.));
#177646=CARTESIAN_POINT('Ctrl Pts',(1.64569902187611,23.4650053483932,12.));
#177647=CARTESIAN_POINT('Ctrl Pts',(1.64162662967528,23.4832548309645,12.));
#177648=CARTESIAN_POINT('Ctrl Pts',(1.63747735129474,23.5016086970003,12.));
#177649=CARTESIAN_POINT('Ctrl Pts',(1.63325092321725,23.5200658336612,12.));
#177650=CARTESIAN_POINT('Ctrl Pts',(1.62894708745223,23.538625143226,12.));
#177651=CARTESIAN_POINT('Ctrl Pts',(1.62456559140064,23.5572855427601,12.));
#177652=CARTESIAN_POINT('Ctrl Pts',(1.62010618772866,23.57604596376,12.));
#177653=CARTESIAN_POINT('Ctrl Pts',(1.61556863424698,23.5949053517997,12.));
#177654=CARTESIAN_POINT('Ctrl Pts',(1.61095269379778,23.6138626661653,12.));
#177655=CARTESIAN_POINT('Ctrl Pts',(1.60625813414672,23.6329168794929,12.));
#177656=CARTESIAN_POINT('Ctrl Pts',(1.60148472786595,23.6520669774876,12.));
#177657=CARTESIAN_POINT('Ctrl Pts',(1.59663225222463,23.671311958631,12.));
#177658=CARTESIAN_POINT('Ctrl Pts',(1.59170048908633,23.6906508338833,12.));
#177659=CARTESIAN_POINT('Ctrl Pts',(1.58668922481221,23.710082626383,12.));
#177660=CARTESIAN_POINT('Ctrl Pts',(1.58159825017358,23.72960637113,12.));
#177661=CARTESIAN_POINT('Ctrl Pts',(1.57642736025246,23.749221114736,12.));
#177662=CARTESIAN_POINT('Ctrl Pts',(1.57117635434408,23.7689259151862,12.));
#177663=CARTESIAN_POINT('Ctrl Pts',(1.56584503586843,23.7887198415878,12.));
#177664=CARTESIAN_POINT('Ctrl Pts',(1.56043321228633,23.8086019739194,12.));
#177665=CARTESIAN_POINT('Ctrl Pts',(1.55494069502635,23.8285714027636,12.));
#177666=CARTESIAN_POINT('Ctrl Pts',(1.54936729940541,23.8486272290705,12.));
#177667=CARTESIAN_POINT('Ctrl Pts',(1.5437128445399,23.8687685639642,12.));
#177668=CARTESIAN_POINT('Ctrl Pts',(1.53797715326758,23.8889945285318,12.));
#177669=CARTESIAN_POINT('Ctrl Pts',(1.53216005207463,23.9093042536119,12.));
#177670=CARTESIAN_POINT('Ctrl Pts',(1.52626137103032,23.9296968795757,12.));
#177671=CARTESIAN_POINT('Ctrl Pts',(1.52028094372792,23.9501715561033,12.));
#177672=CARTESIAN_POINT('Ctrl Pts',(1.51421860720614,23.970727442014,12.));
#177673=CARTESIAN_POINT('Ctrl Pts',(1.50807420187694,23.9913637050927,12.));
#177674=CARTESIAN_POINT('Ctrl Pts',(1.50184757146098,24.0120795219086,12.));
#177675=CARTESIAN_POINT('Ctrl Pts',(1.49553856292801,24.0328740776331,12.));
#177676=CARTESIAN_POINT('Ctrl Pts',(1.48914702644887,24.0537465658429,12.));
#177677=CARTESIAN_POINT('Ctrl Pts',(1.48267281533683,24.0746961883528,12.));
#177678=CARTESIAN_POINT('Ctrl Pts',(1.47611578597742,24.0957221550778,12.));
#177679=CARTESIAN_POINT('Ctrl Pts',(1.46947579776991,24.1168236838824,12.));
#177680=CARTESIAN_POINT('Ctrl Pts',(1.46275271307397,24.1380000004272,12.));
#177681=CARTESIAN_POINT('Ctrl Pts',(1.45594639716317,24.1592503380107,12.));
#177682=CARTESIAN_POINT('Ctrl Pts',(1.44905671818727,24.1805739374038,12.));
#177683=CARTESIAN_POINT('Ctrl Pts',(1.44208354711082,24.201970046722,12.));
#177684=CARTESIAN_POINT('Ctrl Pts',(1.43502675765508,24.2234379212984,12.));
#177685=CARTESIAN_POINT('Ctrl Pts',(1.42788622624854,24.2449768235488,12.));
#177686=CARTESIAN_POINT('Ctrl Pts',(1.42066183198252,24.2665860228356,12.));
#177687=CARTESIAN_POINT('Ctrl Pts',(1.41335345657682,24.288264795321,12.));
#177688=CARTESIAN_POINT('Ctrl Pts',(1.40596098434337,24.3100124238311,12.));
#177689=CARTESIAN_POINT('Ctrl Pts',(1.39848430212807,24.3318281977643,12.));
#177690=CARTESIAN_POINT('Ctrl Pts',(1.39092329926388,24.3537114129875,12.));
#177691=CARTESIAN_POINT('Ctrl Pts',(1.38327786752998,24.3756613717299,12.));
#177692=CARTESIAN_POINT('Ctrl Pts',(1.37554790111609,24.3976773824732,12.));
#177693=CARTESIAN_POINT('Ctrl Pts',(1.36773329659956,24.4197587598337,12.));
#177694=CARTESIAN_POINT('Ctrl Pts',(1.35983395290627,24.4419048244523,12.));
#177695=CARTESIAN_POINT('Ctrl Pts',(1.35184977125648,24.4641149028892,12.));
#177696=CARTESIAN_POINT('Ctrl Pts',(1.34378065512337,24.4863883275134,12.));
#177697=CARTESIAN_POINT('Ctrl Pts',(1.33562651019686,24.5087244363856,12.));
#177698=CARTESIAN_POINT('Ctrl Pts',(1.32738724435326,24.5311225731435,12.));
#177699=CARTESIAN_POINT('Ctrl Pts',(1.31906276763668,24.5535820868674,12.));
#177700=CARTESIAN_POINT('Ctrl Pts',(1.31065299222021,24.5761023320183,12.));
#177701=CARTESIAN_POINT('Ctrl Pts',(1.30215783236362,24.5986826684027,12.));
#177702=CARTESIAN_POINT('Ctrl Pts',(1.29357720438107,24.6213224611229,12.));
#177703=CARTESIAN_POINT('Ctrl Pts',(1.28491102661514,24.6440210805278,12.));
#177704=CARTESIAN_POINT('Ctrl Pts',(1.27615921941642,24.666777902156,12.));
#177705=CARTESIAN_POINT('Ctrl Pts',(1.267321705135,24.6895923066836,12.));
#177706=CARTESIAN_POINT('Ctrl Pts',(1.25839840807418,24.7124636797894,12.));
#177707=CARTESIAN_POINT('Ctrl Pts',(1.24938925444325,24.7353914120011,12.));
#177708=CARTESIAN_POINT('Ctrl Pts',(1.24029417231989,24.7583748985438,12.));
#177709=CARTESIAN_POINT('Ctrl Pts',(1.23111309161843,24.7814135391799,12.));
#177710=CARTESIAN_POINT('Ctrl Pts',(1.22184594406528,24.8045067380536,12.));
#177711=CARTESIAN_POINT('Ctrl Pts',(1.21249266318208,24.8276539035092,12.));
#177712=CARTESIAN_POINT('Ctrl Pts',(1.2030531842602,24.8508544481974,12.));
#177713=CARTESIAN_POINT('Ctrl Pts',(1.19352744434064,24.8741077892075,12.));
#177714=CARTESIAN_POINT('Ctrl Pts',(1.18391538220103,24.8974133481829,12.));
#177715=CARTESIAN_POINT('Ctrl Pts',(1.17421693835041,24.9207705514449,12.));
#177716=CARTESIAN_POINT('Ctrl Pts',(1.16443205502849,24.9441788300932,12.));
#177717=CARTESIAN_POINT('Ctrl Pts',(1.15456067621889,24.9676376201502,12.));
#177718=CARTESIAN_POINT('Ctrl Pts',(1.144602747582,24.9911463621433,12.));
#177719=CARTESIAN_POINT('Ctrl Pts',(1.1345582163853,25.0147045006196,12.));
#177720=CARTESIAN_POINT('Ctrl Pts',(1.12442703144451,25.0383114836899,12.));
#177721=CARTESIAN_POINT('Ctrl Pts',(1.11420914306889,25.0619667625336,12.));
#177722=CARTESIAN_POINT('Ctrl Pts',(1.10390450301745,25.0856697909679,12.));
#177723=CARTESIAN_POINT('Ctrl Pts',(1.09351306445308,25.1094200248446,12.));
#177724=CARTESIAN_POINT('Ctrl Pts',(1.08303478197187,25.1332169227413,12.));
#177725=CARTESIAN_POINT('Ctrl Pts',(1.07246961165475,25.157059946931,12.));
#177726=CARTESIAN_POINT('Ctrl Pts',(1.06181751111768,25.1809485642192,12.));
#177727=CARTESIAN_POINT('Ctrl Pts',(1.05107843957931,25.2048822469028,12.));
#177728=CARTESIAN_POINT('Ctrl Pts',(1.04025235791507,25.2288604735086,12.));
#177729=CARTESIAN_POINT('Ctrl Pts',(1.02933922876806,25.2528827300422,12.));
#177730=CARTESIAN_POINT('Ctrl Pts',(1.01833901642237,25.276948508726,12.));
#177731=CARTESIAN_POINT('Ctrl Pts',(1.00725168656896,25.3010573055547,12.));
#177732=CARTESIAN_POINT('Ctrl Pts',(0.996077206120624,25.3252086182968,
12.));
#177733=CARTESIAN_POINT('Ctrl Pts',(0.984815543003973,25.3494019441441,
12.));
#177734=CARTESIAN_POINT('Ctrl Pts',(0.973466666000163,25.3736367778845,
12.));
#177735=CARTESIAN_POINT('Ctrl Pts',(0.962030544503142,25.3979126089163,
12.));
#177736=CARTESIAN_POINT('Ctrl Pts',(0.950507148597468,25.4222289223167,
12.));
#177737=CARTESIAN_POINT('Ctrl Pts',(0.938896449496192,25.4465852044849,
12.));
#177738=CARTESIAN_POINT('Ctrl Pts',(0.927198419886094,25.4709809475009,
12.));
#177739=CARTESIAN_POINT('Ctrl Pts',(0.915413034335613,25.4954156541795,
12.));
#177740=CARTESIAN_POINT('Ctrl Pts',(0.903540269651106,25.5198888424194,
12.));
#177741=CARTESIAN_POINT('Ctrl Pts',(0.89158010534904,25.5444000508211,12.));
#177742=CARTESIAN_POINT('Ctrl Pts',(0.879532523834294,25.5689488408156,
12.));
#177743=CARTESIAN_POINT('Ctrl Pts',(0.867397509338431,25.5935347843585,
12.));
#177744=CARTESIAN_POINT('Ctrl Pts',(0.855175047036549,25.6181574536049,
12.));
#177745=CARTESIAN_POINT('Ctrl Pts',(0.842865122120758,25.6428164100055,
12.));
#177746=CARTESIAN_POINT('Ctrl Pts',(0.830467718864205,25.6675111931952,
12.));
#177747=CARTESIAN_POINT('Ctrl Pts',(0.817982819787464,25.6922413110194,
12.));
#177748=CARTESIAN_POINT('Ctrl Pts',(0.805410404554352,25.7170062262525,
12.));
#177749=CARTESIAN_POINT('Ctrl Pts',(0.792750451616127,25.7418053757746,
12.));
#177750=CARTESIAN_POINT('Ctrl Pts',(0.780002940291965,25.7666381946955,
12.));
#177751=CARTESIAN_POINT('Ctrl Pts',(0.767167852651168,25.7915041383376,
12.));
#177752=CARTESIAN_POINT('Ctrl Pts',(0.754245175609524,25.8164027059984,
12.));
#177753=CARTESIAN_POINT('Ctrl Pts',(0.741234902663807,25.8413334619055,
12.));
#177754=CARTESIAN_POINT('Ctrl Pts',(0.728137036482335,25.8662960624185,
12.));
#177755=CARTESIAN_POINT('Ctrl Pts',(0.714951588527638,25.891290261497,12.));
#177756=CARTESIAN_POINT('Ctrl Pts',(0.701678575228756,25.9163158909426,
12.));
#177757=CARTESIAN_POINT('Ctrl Pts',(0.688318015057729,25.9413728471909,
12.));
#177758=CARTESIAN_POINT('Ctrl Pts',(0.677559543209725,25.9614434297919,
12.));
#177759=CARTESIAN_POINT('Ctrl Pts',(0.669451306780825,25.9765104298071,
12.));
#177760=CARTESIAN_POINT('Ctrl Pts',(0.664028313187627,25.9865613464773,
12.));
#177761=CARTESIAN_POINT('Ctrl Pts',(0.661312440730901,25.991588367311,12.));
#177762=CARTESIAN_POINT('',(-0.661312440730891,25.991588367311,12.));
#177763=CARTESIAN_POINT('Origin',(0.,0.,12.));
#177764=CARTESIAN_POINT('',(-1.76341220531179,22.4835757167854,12.));
#177765=CARTESIAN_POINT('Ctrl Pts',(-0.661312440730891,25.991588367311,
12.));
#177766=CARTESIAN_POINT('Ctrl Pts',(-0.664028313188914,25.9865613464809,
12.));
#177767=CARTESIAN_POINT('Ctrl Pts',(-0.669451306784418,25.9765104298171,
12.));
#177768=CARTESIAN_POINT('Ctrl Pts',(-0.677559543215903,25.9614434298092,
12.));
#177769=CARTESIAN_POINT('Ctrl Pts',(-0.688318015065679,25.941372847213,
12.));
#177770=CARTESIAN_POINT('Ctrl Pts',(-0.701678575236603,25.9163158909645,
12.));
#177771=CARTESIAN_POINT('Ctrl Pts',(-0.714951588533753,25.8912902615141,
12.));
#177772=CARTESIAN_POINT('Ctrl Pts',(-0.728137036485879,25.8662960624285,
12.));
#177773=CARTESIAN_POINT('Ctrl Pts',(-0.741234902664698,25.841333461908,
12.));
#177774=CARTESIAN_POINT('Ctrl Pts',(-0.75424517560829,25.816402705995,12.));
#177775=CARTESIAN_POINT('Ctrl Pts',(-0.767167852648641,25.7915041383304,
12.));
#177776=CARTESIAN_POINT('Ctrl Pts',(-0.780002940289027,25.7666381946871,
12.));
#177777=CARTESIAN_POINT('Ctrl Pts',(-0.792750451613536,25.7418053757671,
12.));
#177778=CARTESIAN_POINT('Ctrl Pts',(-0.805410404552596,25.7170062262474,
12.));
#177779=CARTESIAN_POINT('Ctrl Pts',(-0.81798281978672,25.6922413110172,
12.));
#177780=CARTESIAN_POINT('Ctrl Pts',(-0.830467718864369,25.6675111931957,
12.));
#177781=CARTESIAN_POINT('Ctrl Pts',(-0.842865122121547,25.6428164100078,
12.));
#177782=CARTESIAN_POINT('Ctrl Pts',(-0.855175047037615,25.618157453608,
12.));
#177783=CARTESIAN_POINT('Ctrl Pts',(-0.86739750933947,25.5935347843616,
12.));
#177784=CARTESIAN_POINT('Ctrl Pts',(-0.879532523835092,25.568948840818,
12.));
#177785=CARTESIAN_POINT('Ctrl Pts',(-0.891580105349468,25.5444000508223,
12.));
#177786=CARTESIAN_POINT('Ctrl Pts',(-0.903540269651155,25.5198888424195,
12.));
#177787=CARTESIAN_POINT('Ctrl Pts',(-0.915413034335334,25.4954156541787,
12.));
#177788=CARTESIAN_POINT('Ctrl Pts',(-0.927198419885605,25.4709809474996,
12.));
#177789=CARTESIAN_POINT('Ctrl Pts',(-0.938896449495633,25.4465852044835,
12.));
#177790=CARTESIAN_POINT('Ctrl Pts',(-0.95050714859697,25.4222289223155,
12.));
#177791=CARTESIAN_POINT('Ctrl Pts',(-0.962030544502803,25.3979126089155,
12.));
#177792=CARTESIAN_POINT('Ctrl Pts',(-0.973466666000049,25.3736367778842,
12.));
#177793=CARTESIAN_POINT('Ctrl Pts',(-0.984815543004092,25.3494019441444,
12.));
#177794=CARTESIAN_POINT('Ctrl Pts',(-0.99607720612092,25.3252086182976,
12.));
#177795=CARTESIAN_POINT('Ctrl Pts',(-1.00725168656934,25.3010573055557,
12.));
#177796=CARTESIAN_POINT('Ctrl Pts',(-1.01833901642272,25.2769485087268,
12.));
#177797=CARTESIAN_POINT('Ctrl Pts',(-1.0293392287683,25.2528827300427,12.));
#177798=CARTESIAN_POINT('Ctrl Pts',(-1.04025235791515,25.2288604735087,
12.));
#177799=CARTESIAN_POINT('Ctrl Pts',(-1.05107843957926,25.2048822469027,
12.));
#177800=CARTESIAN_POINT('Ctrl Pts',(-1.06181751111754,25.1809485642191,
12.));
#177801=CARTESIAN_POINT('Ctrl Pts',(-1.0724696116546,25.1570599469311,12.));
#177802=CARTESIAN_POINT('Ctrl Pts',(-1.08303478197174,25.1332169227415,
12.));
#177803=CARTESIAN_POINT('Ctrl Pts',(-1.09351306445299,25.1094200248448,
12.));
#177804=CARTESIAN_POINT('Ctrl Pts',(-1.1039045030174,25.085669790968,12.));
#177805=CARTESIAN_POINT('Ctrl Pts',(-1.1142091430689,25.0619667625336,12.));
#177806=CARTESIAN_POINT('Ctrl Pts',(-1.12442703144455,25.0383114836898,
12.));
#177807=CARTESIAN_POINT('Ctrl Pts',(-1.13455821638536,25.0147045006193,
12.));
#177808=CARTESIAN_POINT('Ctrl Pts',(-1.14460274758206,24.9911463621431,
12.));
#177809=CARTESIAN_POINT('Ctrl Pts',(-1.15456067621894,24.9676376201501,
12.));
#177810=CARTESIAN_POINT('Ctrl Pts',(-1.16443205502852,24.9441788300932,
12.));
#177811=CARTESIAN_POINT('Ctrl Pts',(-1.17421693835039,24.9207705514449,
12.));
#177812=CARTESIAN_POINT('Ctrl Pts',(-1.18391538220098,24.8974133481829,
12.));
#177813=CARTESIAN_POINT('Ctrl Pts',(-1.19352744434059,24.8741077892074,
12.));
#177814=CARTESIAN_POINT('Ctrl Pts',(-1.20305318426015,24.8508544481973,
12.));
#177815=CARTESIAN_POINT('Ctrl Pts',(-1.21249266318205,24.8276539035092,
12.));
#177816=CARTESIAN_POINT('Ctrl Pts',(-1.22184594406526,24.8045067380536,
12.));
#177817=CARTESIAN_POINT('Ctrl Pts',(-1.23111309161843,24.78141353918,12.));
#177818=CARTESIAN_POINT('Ctrl Pts',(-1.24029417231988,24.7583748985439,
12.));
#177819=CARTESIAN_POINT('Ctrl Pts',(-1.24938925444324,24.7353914120012,
12.));
#177820=CARTESIAN_POINT('Ctrl Pts',(-1.25839840807415,24.7124636797895,
12.));
#177821=CARTESIAN_POINT('Ctrl Pts',(-1.26732170513497,24.6895923066837,
12.));
#177822=CARTESIAN_POINT('Ctrl Pts',(-1.2761592194164,24.666777902156,12.));
#177823=CARTESIAN_POINT('Ctrl Pts',(-1.28491102661514,24.6440210805278,
12.));
#177824=CARTESIAN_POINT('Ctrl Pts',(-1.29357720438108,24.6213224611228,
12.));
#177825=CARTESIAN_POINT('Ctrl Pts',(-1.30215783236364,24.5986826684025,
12.));
#177826=CARTESIAN_POINT('Ctrl Pts',(-1.31065299222023,24.576102332018,12.));
#177827=CARTESIAN_POINT('Ctrl Pts',(-1.31906276763669,24.5535820868671,
12.));
#177828=CARTESIAN_POINT('Ctrl Pts',(-1.32738724435326,24.5311225731434,
12.));
#177829=CARTESIAN_POINT('Ctrl Pts',(-1.33562651019684,24.5087244363856,
12.));
#177830=CARTESIAN_POINT('Ctrl Pts',(-1.34378065512335,24.4863883275135,
12.));
#177831=CARTESIAN_POINT('Ctrl Pts',(-1.35184977125645,24.4641149028894,
12.));
#177832=CARTESIAN_POINT('Ctrl Pts',(-1.35983395290624,24.4419048244524,
12.));
#177833=CARTESIAN_POINT('Ctrl Pts',(-1.36773329659954,24.4197587598337,
12.));
#177834=CARTESIAN_POINT('Ctrl Pts',(-1.37554790111608,24.3976773824731,
12.));
#177835=CARTESIAN_POINT('Ctrl Pts',(-1.38327786752998,24.37566137173,12.));
#177836=CARTESIAN_POINT('Ctrl Pts',(-1.3909232992639,24.3537114129877,12.));
#177837=CARTESIAN_POINT('Ctrl Pts',(-1.3984843021281,24.3318281977647,12.));
#177838=CARTESIAN_POINT('Ctrl Pts',(-1.40596098434341,24.3100124238316,
12.));
#177839=CARTESIAN_POINT('Ctrl Pts',(-1.41335345657685,24.2882647953214,
12.));
#177840=CARTESIAN_POINT('Ctrl Pts',(-1.42066183198252,24.2665860228357,
12.));
#177841=CARTESIAN_POINT('Ctrl Pts',(-1.42788622624851,24.2449768235485,
12.));
#177842=CARTESIAN_POINT('Ctrl Pts',(-1.43502675765502,24.2234379212978,
12.));
#177843=CARTESIAN_POINT('Ctrl Pts',(-1.44208354711074,24.2019700467214,
12.));
#177844=CARTESIAN_POINT('Ctrl Pts',(-1.44905671818721,24.1805739374033,
12.));
#177845=CARTESIAN_POINT('Ctrl Pts',(-1.45594639716314,24.1592503380105,
12.));
#177846=CARTESIAN_POINT('Ctrl Pts',(-1.46275271307398,24.1380000004272,
12.));
#177847=CARTESIAN_POINT('Ctrl Pts',(-1.46947579776992,24.1168236838827,
12.));
#177848=CARTESIAN_POINT('Ctrl Pts',(-1.47611578597741,24.0957221550782,
12.));
#177849=CARTESIAN_POINT('Ctrl Pts',(-1.4826728153368,24.074696188353,12.));
#177850=CARTESIAN_POINT('Ctrl Pts',(-1.48914702644883,24.053746565843,12.));
#177851=CARTESIAN_POINT('Ctrl Pts',(-1.49553856292798,24.0328740776331,
12.));
#177852=CARTESIAN_POINT('Ctrl Pts',(-1.50184757146099,24.0120795219086,
12.));
#177853=CARTESIAN_POINT('Ctrl Pts',(-1.50807420187703,23.991363705093,12.));
#177854=CARTESIAN_POINT('Ctrl Pts',(-1.51421860720628,23.9707274420145,
12.));
#177855=CARTESIAN_POINT('Ctrl Pts',(-1.52028094372806,23.9501715561038,
12.));
#177856=CARTESIAN_POINT('Ctrl Pts',(-1.5262613710304,23.9296968795761,12.));
#177857=CARTESIAN_POINT('Ctrl Pts',(-1.53216005207462,23.9093042536119,
12.));
#177858=CARTESIAN_POINT('Ctrl Pts',(-1.53797715326748,23.8889945285313,
12.));
#177859=CARTESIAN_POINT('Ctrl Pts',(-1.54371284453978,23.8687685639635,
12.));
#177860=CARTESIAN_POINT('Ctrl Pts',(-1.5493672994053,23.8486272290698,12.));
#177861=CARTESIAN_POINT('Ctrl Pts',(-1.55494069502628,23.8285714027631,
12.));
#177862=CARTESIAN_POINT('Ctrl Pts',(-1.56043321228631,23.8086019739192,
12.));
#177863=CARTESIAN_POINT('Ctrl Pts',(-1.56584503586844,23.788719841588,12.));
#177864=CARTESIAN_POINT('Ctrl Pts',(-1.57117635434412,23.7689259151869,
12.));
#177865=CARTESIAN_POINT('Ctrl Pts',(-1.57642736025251,23.7492211147369,
12.));
#177866=CARTESIAN_POINT('Ctrl Pts',(-1.58159825017362,23.7296063711308,
12.));
#177867=CARTESIAN_POINT('Ctrl Pts',(-1.58668922481222,23.7100826263835,
12.));
#177868=CARTESIAN_POINT('Ctrl Pts',(-1.59170048908632,23.6906508338833,
12.));
#177869=CARTESIAN_POINT('Ctrl Pts',(-1.59663225222458,23.6713119586302,
12.));
#177870=CARTESIAN_POINT('Ctrl Pts',(-1.60148472786588,23.6520669774863,
12.));
#177871=CARTESIAN_POINT('Ctrl Pts',(-1.60625813414666,23.6329168794916,
12.));
#177872=CARTESIAN_POINT('Ctrl Pts',(-1.61095269379773,23.6138626661644,
12.));
#177873=CARTESIAN_POINT('Ctrl Pts',(-1.61556863424697,23.5949053517996,
12.));
#177874=CARTESIAN_POINT('Ctrl Pts',(-1.62010618772869,23.5760459637608,
12.));
#177875=CARTESIAN_POINT('Ctrl Pts',(-1.62456559140072,23.5572855427617,
12.));
#177876=CARTESIAN_POINT('Ctrl Pts',(-1.62894708745231,23.5386251432278,
12.));
#177877=CARTESIAN_POINT('Ctrl Pts',(-1.63325092321731,23.5200658336624,
12.));
#177878=CARTESIAN_POINT('Ctrl Pts',(-1.63747735129474,23.5016086970006,
12.));
#177879=CARTESIAN_POINT('Ctrl Pts',(-1.64162662967525,23.4832548309638,
12.));
#177880=CARTESIAN_POINT('Ctrl Pts',(-1.64569902187608,23.4650053483919,
12.));
#177881=CARTESIAN_POINT('Ctrl Pts',(-1.6496947970734,23.446861377656,12.));
#177882=CARTESIAN_POINT('Ctrl Pts',(-1.6536142302373,23.4288240631034,12.));
#177883=CARTESIAN_POINT('Ctrl Pts',(-1.65745760227507,23.4108945654803,
12.));
#177884=CARTESIAN_POINT('Ctrl Pts',(-1.66122520018008,23.3930740623622,
12.));
#177885=CARTESIAN_POINT('Ctrl Pts',(-1.66491731718864,23.375363748555,12.));
#177886=CARTESIAN_POINT('Ctrl Pts',(-1.66853425293978,23.3577648365747,
12.));
#177887=CARTESIAN_POINT('Ctrl Pts',(-1.67207631363905,23.3402785571866,
12.));
#177888=CARTESIAN_POINT('Ctrl Pts',(-1.67554381222987,23.3229061599145,
12.));
#177889=CARTESIAN_POINT('Ctrl Pts',(-1.67893706857123,23.3056489135611,
12.));
#177890=CARTESIAN_POINT('Ctrl Pts',(-1.68225640962181,23.2885081066949,
12.));
#177891=CARTESIAN_POINT('Ctrl Pts',(-1.68550216963275,23.2714850482245,
12.));
#177892=CARTESIAN_POINT('Ctrl Pts',(-1.6886746903491,23.2545810680536,12.));
#177893=CARTESIAN_POINT('Ctrl Pts',(-1.69177432121716,23.2377975177014,
12.));
#177894=CARTESIAN_POINT('Ctrl Pts',(-1.69480141959946,23.2211357709374,
12.));
#177895=CARTESIAN_POINT('Ctrl Pts',(-1.69775635099425,23.2045972243765,
12.));
#177896=CARTESIAN_POINT('Ctrl Pts',(-1.70063948926987,23.1881832981848,
12.));
#177897=CARTESIAN_POINT('Ctrl Pts',(-1.70345121691259,23.1718954368749,
12.));
#177898=CARTESIAN_POINT('Ctrl Pts',(-1.70619192527847,23.1557351100613,
12.));
#177899=CARTESIAN_POINT('Ctrl Pts',(-1.7088620148546,23.1397038132358,12.));
#177900=CARTESIAN_POINT('Ctrl Pts',(-1.71146189552192,23.1238030684929,
12.));
#177901=CARTESIAN_POINT('Ctrl Pts',(-1.71399198684725,23.1080344254291,
12.));
#177902=CARTESIAN_POINT('Ctrl Pts',(-1.71645271839311,23.0923994621216,
12.));
#177903=CARTESIAN_POINT('Ctrl Pts',(-1.71884453003027,23.0768997860709,
12.));
#177904=CARTESIAN_POINT('Ctrl Pts',(-1.7211678722598,23.061537035156,12.));
#177905=CARTESIAN_POINT('Ctrl Pts',(-1.72342320653731,23.0463128785528,
12.));
#177906=CARTESIAN_POINT('Ctrl Pts',(-1.72561100564033,23.031229017888,12.));
#177907=CARTESIAN_POINT('Ctrl Pts',(-1.72773175404703,23.0162871884167,
12.));
#177908=CARTESIAN_POINT('Ctrl Pts',(-1.72978594832137,23.0014891601891,
12.));
#177909=CARTESIAN_POINT('Ctrl Pts',(-1.73177409750194,22.9868367391978,
12.));
#177910=CARTESIAN_POINT('Ctrl Pts',(-1.73369672350818,22.9723317685688,
12.));
#177911=CARTESIAN_POINT('Ctrl Pts',(-1.73555436162771,22.9579761301062,
12.));
#177912=CARTESIAN_POINT('Ctrl Pts',(-1.73734756100038,22.9437717457825,
12.));
#177913=CARTESIAN_POINT('Ctrl Pts',(-1.73907688511664,22.9297205792587,
12.));
#177914=CARTESIAN_POINT('Ctrl Pts',(-1.74074291231057,22.9158246373365,
12.));
#177915=CARTESIAN_POINT('Ctrl Pts',(-1.74234623630079,22.9020859716144,
12.));
#177916=CARTESIAN_POINT('Ctrl Pts',(-1.74388746677702,22.8885066803351,
12.));
#177917=CARTESIAN_POINT('Ctrl Pts',(-1.745367229982,22.8750889101696,12.));
#177918=CARTESIAN_POINT('Ctrl Pts',(-1.74678616930663,22.8618348580234,
12.));
#177919=CARTESIAN_POINT('Ctrl Pts',(-1.74814494588492,22.8487467728075,
12.));
#177920=CARTESIAN_POINT('Ctrl Pts',(-1.74944423940117,22.8358269579854,
12.));
#177921=CARTESIAN_POINT('Ctrl Pts',(-1.75068474890884,22.8230777741285,
12.));
#177922=CARTESIAN_POINT('Ctrl Pts',(-1.7518671936559,22.8105016414712,12.));
#177923=CARTESIAN_POINT('Ctrl Pts',(-1.75299231391461,22.7981010424312,
12.));
#177924=CARTESIAN_POINT('Ctrl Pts',(-1.7540608718293,22.7858785242358,12.));
#177925=CARTESIAN_POINT('Ctrl Pts',(-1.75507365227127,22.7738367016115,
12.));
#177926=CARTESIAN_POINT('Ctrl Pts',(-1.7560314637164,22.7619782595013,12.));
#177927=CARTESIAN_POINT('Ctrl Pts',(-1.75693513908911,22.7503059556455,
12.));
#177928=CARTESIAN_POINT('Ctrl Pts',(-1.75778553673249,22.7388226235565,
12.));
#177929=CARTESIAN_POINT('Ctrl Pts',(-1.75858354204635,22.7275311777305,
12.));
#177930=CARTESIAN_POINT('Ctrl Pts',(-1.75933006905924,22.7164346186007,
12.));
#177931=CARTESIAN_POINT('Ctrl Pts',(-1.76002606202399,22.7055360375481,
12.));
#177932=CARTESIAN_POINT('Ctrl Pts',(-1.76067249704884,22.6948386219843,
12.));
#177933=CARTESIAN_POINT('Ctrl Pts',(-1.76127038310613,22.6843456585245,
12.));
#177934=CARTESIAN_POINT('Ctrl Pts',(-1.76182076289525,22.6740605356699,
12.));
#177935=CARTESIAN_POINT('Ctrl Pts',(-1.76232471392567,22.6639867471756,
12.));
#177936=CARTESIAN_POINT('Ctrl Pts',(-1.76278334912559,22.6541278938413,
12.));
#177937=CARTESIAN_POINT('Ctrl Pts',(-1.76319782013914,22.6444876940425,
12.));
#177938=CARTESIAN_POINT('Ctrl Pts',(-1.76356932176272,22.635069997936,12.));
#177939=CARTESIAN_POINT('Ctrl Pts',(-1.76389909571402,22.6258787994847,
12.));
#177940=CARTESIAN_POINT('Ctrl Pts',(-1.76418843543739,22.6169182517693,
12.));
#177941=CARTESIAN_POINT('Ctrl Pts',(-1.76443868648015,22.6081926681342,
12.));
#177942=CARTESIAN_POINT('Ctrl Pts',(-1.76465124413556,22.5997065145638,
12.));
#177943=CARTESIAN_POINT('Ctrl Pts',(-1.76482755288411,22.5914644078106,
12.));
#177944=CARTESIAN_POINT('Ctrl Pts',(-1.76496910283088,22.5834711038024,
12.));
#177945=CARTESIAN_POINT('Ctrl Pts',(-1.76507744026747,22.5757315316355,
12.));
#177946=CARTESIAN_POINT('Ctrl Pts',(-1.76515418518829,22.5682508499873,
12.));
#177947=CARTESIAN_POINT('Ctrl Pts',(-1.76520104500449,22.5610344912501,
12.));
#177948=CARTESIAN_POINT('Ctrl Pts',(-1.76521983384063,22.5540882235837,
12.));
#177949=CARTESIAN_POINT('Ctrl Pts',(-1.76521245524047,22.5474180954006,
12.));
#177950=CARTESIAN_POINT('Ctrl Pts',(-1.76518087841493,22.5410303590891,
12.));
#177951=CARTESIAN_POINT('Ctrl Pts',(-1.7651271156325,22.5349313983571,12.));
#177952=CARTESIAN_POINT('Ctrl Pts',(-1.76505320262752,22.529127665298,12.));
#177953=CARTESIAN_POINT('Ctrl Pts',(-1.76496128643369,22.5236259635515,
12.));
#177954=CARTESIAN_POINT('Ctrl Pts',(-1.76485369319896,22.5184336670207,
12.));
#177955=CARTESIAN_POINT('Ctrl Pts',(-1.76473303281159,22.5135590569554,
12.));
#177956=CARTESIAN_POINT('Ctrl Pts',(-1.76460218257323,22.5090112700212,
12.));
#177957=CARTESIAN_POINT('Ctrl Pts',(-1.76446408210366,22.5047996391978,
12.));
#177958=CARTESIAN_POINT('Ctrl Pts',(-1.76432160068725,22.5009332677316,
12.));
#177959=CARTESIAN_POINT('Ctrl Pts',(-1.76417731243462,22.4974203063191,
12.));
#177960=CARTESIAN_POINT('Ctrl Pts',(-1.76403393880301,22.4942693792449,
12.));
#177961=CARTESIAN_POINT('Ctrl Pts',(-1.76389475965724,22.4914909094908,
12.));
#177962=CARTESIAN_POINT('Ctrl Pts',(-1.76376424879505,22.4890991659478,
12.));
#177963=CARTESIAN_POINT('Ctrl Pts',(-1.76364784232963,22.4871115206571,
12.));
#177964=CARTESIAN_POINT('Ctrl Pts',(-1.76355076045546,22.4855446605991,
12.));
#177965=CARTESIAN_POINT('Ctrl Pts',(-1.76347698284792,22.4844112933129,
12.));
#177966=CARTESIAN_POINT('Ctrl Pts',(-1.76343813434565,22.483856251707,12.));
#177967=CARTESIAN_POINT('Ctrl Pts',(-1.7634206426357,22.4836387052232,12.));
#177968=CARTESIAN_POINT('Ctrl Pts',(-1.76341415538764,22.483581992979,12.));
#177969=CARTESIAN_POINT('Ctrl Pts',(-1.76341220531179,22.4835757167854,
12.));
#177970=CARTESIAN_POINT('',(-1.71975774210841,21.9269795755927,12.));
#177971=CARTESIAN_POINT('',(-0.840553282521227,10.7170877657712,12.));
#177972=CARTESIAN_POINT('',(-2.16781269186828,21.3904321633055,12.));
#177973=CARTESIAN_POINT('Origin',(-2.21822694051637,21.8878840740801,12.));
#177974=CARTESIAN_POINT('',(-3.44230496120418,21.2226420728916,12.));
#177975=CARTESIAN_POINT('Origin',(-7.16093850883226E-14,7.7715611723761E-13,
12.));
#177976=CARTESIAN_POINT('',(-4.01396149767428,21.624941921198,12.));
#177977=CARTESIAN_POINT('Origin',(-3.52235856495312,21.7161918885402,12.));
#177978=CARTESIAN_POINT('',(-4.11585220600461,22.1738711152697,12.));
#177979=CARTESIAN_POINT('',(-2.05792610300232,11.0869355576349,12.));
#177980=CARTESIAN_POINT('',(-6.08833931617698,25.2771067246846,12.));
#177981=CARTESIAN_POINT('Ctrl Pts',(-4.11585220600461,22.1738711152697,
12.));
#177982=CARTESIAN_POINT('Ctrl Pts',(-4.11585194677412,22.1738776823239,
12.));
#177983=CARTESIAN_POINT('Ctrl Pts',(-4.1158603587821,22.1739341411684,12.));
#177984=CARTESIAN_POINT('Ctrl Pts',(-4.11589976826061,22.174148802123,12.));
#177985=CARTESIAN_POINT('Ctrl Pts',(-4.11600589882767,22.1746949858773,
12.));
#177986=CARTESIAN_POINT('Ctrl Pts',(-4.11622797217066,22.1758088296598,
12.));
#177987=CARTESIAN_POINT('Ctrl Pts',(-4.11653973150558,22.177347426894,12.));
#177988=CARTESIAN_POINT('Ctrl Pts',(-4.11694173195041,22.179297473024,12.));
#177989=CARTESIAN_POINT('Ctrl Pts',(-4.11743469691765,22.1816414985788,
12.));
#177990=CARTESIAN_POINT('Ctrl Pts',(-4.11801938107464,22.1843613164855,
12.));
#177991=CARTESIAN_POINT('Ctrl Pts',(-4.11869641271752,22.1874419861496,
12.));
#177992=CARTESIAN_POINT('Ctrl Pts',(-4.11946626228623,22.1908725908525,
12.));
#177993=CARTESIAN_POINT('Ctrl Pts',(-4.12032932637738,22.1946440958098,
12.));
#177994=CARTESIAN_POINT('Ctrl Pts',(-4.12128598183533,22.1987479618246,
12.));
#177995=CARTESIAN_POINT('Ctrl Pts',(-4.12233664408237,22.2031746532106,
12.));
#177996=CARTESIAN_POINT('Ctrl Pts',(-4.12348173702025,22.2079143941719,
12.));
#177997=CARTESIAN_POINT('Ctrl Pts',(-4.12472167516602,22.2129576146671,
12.));
#177998=CARTESIAN_POINT('Ctrl Pts',(-4.126056836133,22.2182956401341,12.));
#177999=CARTESIAN_POINT('Ctrl Pts',(-4.12748755830099,22.2239207458781,
12.));
#178000=CARTESIAN_POINT('Ctrl Pts',(-4.12901415463379,22.2298258043947,
12.));
#178001=CARTESIAN_POINT('Ctrl Pts',(-4.13063692157499,22.2360040565534,
12.));
#178002=CARTESIAN_POINT('Ctrl Pts',(-4.1323561506016,22.2424488153523,12.));
#178003=CARTESIAN_POINT('Ctrl Pts',(-4.13417212558808,22.2491535317789,
12.));
#178004=CARTESIAN_POINT('Ctrl Pts',(-4.13608511977226,22.2561118708422,
12.));
#178005=CARTESIAN_POINT('Ctrl Pts',(-4.13809539255419,22.263317791397,12.));
#178006=CARTESIAN_POINT('Ctrl Pts',(-4.14020318715988,22.2707656042456,
12.));
#178007=CARTESIAN_POINT('Ctrl Pts',(-4.14240873321982,22.2784499072026,
12.));
#178008=CARTESIAN_POINT('Ctrl Pts',(-4.14471224859295,22.2863655389166,
12.));
#178009=CARTESIAN_POINT('Ctrl Pts',(-4.14711394168559,22.2945075198468,
12.));
#178010=CARTESIAN_POINT('Ctrl Pts',(-4.14961401285526,22.3028710166935,
12.));
#178011=CARTESIAN_POINT('Ctrl Pts',(-4.15221265396992,22.3114513545186,
12.));
#178012=CARTESIAN_POINT('Ctrl Pts',(-4.15491004835278,22.3202440186979,
12.));
#178013=CARTESIAN_POINT('Ctrl Pts',(-4.15770637047882,22.3292446628957,
12.));
#178014=CARTESIAN_POINT('Ctrl Pts',(-4.16060178604154,22.3384491078599,
12.));
#178015=CARTESIAN_POINT('Ctrl Pts',(-4.1635964526318,22.3478533253886,12.));
#178016=CARTESIAN_POINT('Ctrl Pts',(-4.16669052026602,22.3574534257397,
12.));
#178017=CARTESIAN_POINT('Ctrl Pts',(-4.1698841319947,22.3672456427605,12.));
#178018=CARTESIAN_POINT('Ctrl Pts',(-4.17317742436162,22.3772263228624,
12.));
#178019=CARTESIAN_POINT('Ctrl Pts',(-4.17657052752834,22.3873919231339,
12.));
#178020=CARTESIAN_POINT('Ctrl Pts',(-4.18006356544879,22.3977390078074,
12.));
#178021=CARTESIAN_POINT('Ctrl Pts',(-4.18365665600839,22.4082642454448,
12.));
#178022=CARTESIAN_POINT('Ctrl Pts',(-4.18734991117707,22.4189644056109,
12.));
#178023=CARTESIAN_POINT('Ctrl Pts',(-4.19114343726932,22.4298363535416,
12.));
#178024=CARTESIAN_POINT('Ctrl Pts',(-4.1950373351886,22.4408770448917,12.));
#178025=CARTESIAN_POINT('Ctrl Pts',(-4.19903170066358,22.4520835205422,
12.));
#178026=CARTESIAN_POINT('Ctrl Pts',(-4.20312662448174,22.4634529011437,
12.));
#178027=CARTESIAN_POINT('Ctrl Pts',(-4.20732219265649,22.4749823839917,
12.));
#178028=CARTESIAN_POINT('Ctrl Pts',(-4.21161848657428,22.4866692403147,
12.));
#178029=CARTESIAN_POINT('Ctrl Pts',(-4.21601558313906,22.4985108124228,
12.));
#178030=CARTESIAN_POINT('Ctrl Pts',(-4.22051355490196,22.5105045108881,
12.));
#178031=CARTESIAN_POINT('Ctrl Pts',(-4.22511247020041,22.5226478117886,
12.));
#178032=CARTESIAN_POINT('Ctrl Pts',(-4.22981239330733,22.5349382540588,
12.));
#178033=CARTESIAN_POINT('Ctrl Pts',(-4.23461338456712,22.5473734368086,
12.));
#178034=CARTESIAN_POINT('Ctrl Pts',(-4.23951550052523,22.5599510166429,
12.));
#178035=CARTESIAN_POINT('Ctrl Pts',(-4.24451879404851,22.572668704992,12.));
#178036=CARTESIAN_POINT('Ctrl Pts',(-4.24962331444177,22.5855242662477,
12.));
#178037=CARTESIAN_POINT('Ctrl Pts',(-4.25482910755481,22.5985155158636,
12.));
#178038=CARTESIAN_POINT('Ctrl Pts',(-4.26013621588305,22.6116403184821,
12.));
#178039=CARTESIAN_POINT('Ctrl Pts',(-4.26554467865576,22.6248965859977,
12.));
#178040=CARTESIAN_POINT('Ctrl Pts',(-4.27105453193004,22.6382822758172,
12.));
#178041=CARTESIAN_POINT('Ctrl Pts',(-4.2766658086912,22.6517953893303,12.));
#178042=CARTESIAN_POINT('Ctrl Pts',(-4.28237853894059,22.6654339703109,
12.));
#178043=CARTESIAN_POINT('Ctrl Pts',(-4.28819274977763,22.6791961033538,
12.));
#178044=CARTESIAN_POINT('Ctrl Pts',(-4.29410846547056,22.6930799122548,
12.));
#178045=CARTESIAN_POINT('Ctrl Pts',(-4.3001257075406,22.7070835587564,12.));
#178046=CARTESIAN_POINT('Ctrl Pts',(-4.30624449484069,22.7212052413386,
12.));
#178047=CARTESIAN_POINT('Ctrl Pts',(-4.31246484362549,22.7354431939926,
12.));
#178048=CARTESIAN_POINT('Ctrl Pts',(-4.31878676761235,22.7497956849848,
12.));
#178049=CARTESIAN_POINT('Ctrl Pts',(-4.32521027803754,22.7642610156475,
12.));
#178050=CARTESIAN_POINT('Ctrl Pts',(-4.3317353837319,22.7788375194076,12.));
#178051=CARTESIAN_POINT('Ctrl Pts',(-4.33836209118446,22.7935235607806,
12.));
#178052=CARTESIAN_POINT('Ctrl Pts',(-4.34509040460062,22.8083175343791,
12.));
#178053=CARTESIAN_POINT('Ctrl Pts',(-4.35192032594791,22.8232178638876,
12.));
#178054=CARTESIAN_POINT('Ctrl Pts',(-4.35885185500546,22.8382230011184,
12.));
#178055=CARTESIAN_POINT('Ctrl Pts',(-4.36588498942997,22.8533314252422,
12.));
#178056=CARTESIAN_POINT('Ctrl Pts',(-4.37301972480746,22.8685416419725,
12.));
#178057=CARTESIAN_POINT('Ctrl Pts',(-4.38025605470093,22.8838521827701,
12.));
#178058=CARTESIAN_POINT('Ctrl Pts',(-4.38759397068406,22.8992616040108,
12.));
#178059=CARTESIAN_POINT('Ctrl Pts',(-4.39503346238473,22.9147684862426,
12.));
#178060=CARTESIAN_POINT('Ctrl Pts',(-4.40257451754323,22.930371433555,12.));
#178061=CARTESIAN_POINT('Ctrl Pts',(-4.41021712205553,22.9460690729093,
12.));
#178062=CARTESIAN_POINT('Ctrl Pts',(-4.41796126001302,22.9618600534866,
12.));
#178063=CARTESIAN_POINT('Ctrl Pts',(-4.42580691372751,22.977743046002,12.));
#178064=CARTESIAN_POINT('Ctrl Pts',(-4.43375406376879,22.9937167421006,
12.));
#178065=CARTESIAN_POINT('Ctrl Pts',(-4.44180268901643,23.0097798538395,
12.));
#178066=CARTESIAN_POINT('Ctrl Pts',(-4.44995276669686,23.0259311131392,
12.));
#178067=CARTESIAN_POINT('Ctrl Pts',(-4.45820427241683,23.0421692712467,
12.));
#178068=CARTESIAN_POINT('Ctrl Pts',(-4.4665571801823,23.0584930981732,12.));
#178069=CARTESIAN_POINT('Ctrl Pts',(-4.47501146242856,23.0749013821881,
12.));
#178070=CARTESIAN_POINT('Ctrl Pts',(-4.48356709006788,23.0913929293922,
12.));
#178071=CARTESIAN_POINT('Ctrl Pts',(-4.49222403252216,23.1079665632636,
12.));
#178072=CARTESIAN_POINT('Ctrl Pts',(-4.50098225775171,23.1246211242115,
12.));
#178073=CARTESIAN_POINT('Ctrl Pts',(-4.5098417322706,23.1413554691123,12.));
#178074=CARTESIAN_POINT('Ctrl Pts',(-4.51880242116748,23.1581684708761,
12.));
#178075=CARTESIAN_POINT('Ctrl Pts',(-4.52786428815015,23.1750590180908,
12.));
#178076=CARTESIAN_POINT('Ctrl Pts',(-4.53702729557566,23.1920260146465,
12.));
#178077=CARTESIAN_POINT('Ctrl Pts',(-4.54629140447544,23.2090683793629,
12.));
#178078=CARTESIAN_POINT('Ctrl Pts',(-4.55565657456975,23.2261850456064,
12.));
#178079=CARTESIAN_POINT('Ctrl Pts',(-4.56512276427839,23.2433749609131,
12.));
#178080=CARTESIAN_POINT('Ctrl Pts',(-4.57468993076097,23.2606370866866,
12.));
#178081=CARTESIAN_POINT('Ctrl Pts',(-4.5843580299469,23.2779703978876,12.));
#178082=CARTESIAN_POINT('Ctrl Pts',(-4.5941270165575,23.2953738827191,12.));
#178083=CARTESIAN_POINT('Ctrl Pts',(-4.60399684412163,23.3128465423115,
12.));
#178084=CARTESIAN_POINT('Ctrl Pts',(-4.6139674649783,23.3303873903938,12.));
#178085=CARTESIAN_POINT('Ctrl Pts',(-4.62403883030805,23.3479954530272,
12.));
#178086=CARTESIAN_POINT('Ctrl Pts',(-4.63421089016541,23.3656697683489,
12.));
#178087=CARTESIAN_POINT('Ctrl Pts',(-4.6444835934993,23.3834093863068,12.));
#178088=CARTESIAN_POINT('Ctrl Pts',(-4.65485688816924,23.4012133683959,
12.));
#178089=CARTESIAN_POINT('Ctrl Pts',(-4.6653307209467,23.4190807873803,12.));
#178090=CARTESIAN_POINT('Ctrl Pts',(-4.67590503753058,23.4370107270451,
12.));
#178091=CARTESIAN_POINT('Ctrl Pts',(-4.68657978258303,23.455002281986,12.));
#178092=CARTESIAN_POINT('Ctrl Pts',(-4.69735489975024,23.4730545573853,
12.));
#178093=CARTESIAN_POINT('Ctrl Pts',(-4.70823033167819,23.491166668789,12.));
#178094=CARTESIAN_POINT('Ctrl Pts',(-4.71920602001902,23.509337741878,12.));
#178095=CARTESIAN_POINT('Ctrl Pts',(-4.7302819054303,23.5275669122372,12.));
#178096=CARTESIAN_POINT('Ctrl Pts',(-4.74145792760698,23.545853325171,12.));
#178097=CARTESIAN_POINT('Ctrl Pts',(-4.75273402530617,23.5641961355168,
12.));
#178098=CARTESIAN_POINT('Ctrl Pts',(-4.76411013636251,23.5825945074535,
12.));
#178099=CARTESIAN_POINT('Ctrl Pts',(-4.77558619769872,23.6010476143099,
12.));
#178100=CARTESIAN_POINT('Ctrl Pts',(-4.78716214532098,23.6195546383624,
12.));
#178101=CARTESIAN_POINT('Ctrl Pts',(-4.7988379143322,23.6381147706579,12.));
#178102=CARTESIAN_POINT('Ctrl Pts',(-4.81061343896432,23.6567272108628,
12.));
#178103=CARTESIAN_POINT('Ctrl Pts',(-4.82248865259562,23.675391167102,12.));
#178104=CARTESIAN_POINT('Ctrl Pts',(-4.83446348776266,23.6941058557971,
12.));
#178105=CARTESIAN_POINT('Ctrl Pts',(-4.84653787616425,23.7128705015017,
12.));
#178106=CARTESIAN_POINT('Ctrl Pts',(-4.85871174865499,23.7316843367313,
12.));
#178107=CARTESIAN_POINT('Ctrl Pts',(-4.87098503527152,23.7505466018245,
12.));
#178108=CARTESIAN_POINT('Ctrl Pts',(-4.88335766525573,23.7694565448049,
12.));
#178109=CARTESIAN_POINT('Ctrl Pts',(-4.89582956706775,23.7884134212384,
12.));
#178110=CARTESIAN_POINT('Ctrl Pts',(-4.90840066839344,23.8074164940896,
12.));
#178111=CARTESIAN_POINT('Ctrl Pts',(-4.92107089613969,23.8264650335717,
12.));
#178112=CARTESIAN_POINT('Ctrl Pts',(-4.93384017643432,23.8455583170057,
12.));
#178113=CARTESIAN_POINT('Ctrl Pts',(-4.9467084346586,23.8646956287168,12.));
#178114=CARTESIAN_POINT('Ctrl Pts',(-4.95967559546561,23.8838762599218,
12.));
#178115=CARTESIAN_POINT('Ctrl Pts',(-4.97274158279227,23.9030995086163,
12.));
#178116=CARTESIAN_POINT('Ctrl Pts',(-4.98590631986533,23.9223646794592,
12.));
#178117=CARTESIAN_POINT('Ctrl Pts',(-4.99916972919307,23.9416710836529,
12.));
#178118=CARTESIAN_POINT('Ctrl Pts',(-5.01253173257453,23.9610180388271,
12.));
#178119=CARTESIAN_POINT('Ctrl Pts',(-5.02599225112454,23.9804048689227,
12.));
#178120=CARTESIAN_POINT('Ctrl Pts',(-5.03955120528521,23.9998309040746,
12.));
#178121=CARTESIAN_POINT('Ctrl Pts',(-5.05320851483065,24.0192954804896,
12.));
#178122=CARTESIAN_POINT('Ctrl Pts',(-5.06696409886641,24.0387979403268,
12.));
#178123=CARTESIAN_POINT('Ctrl Pts',(-5.08081787581276,24.0583376315638,
12.));
#178124=CARTESIAN_POINT('Ctrl Pts',(-5.09476976342625,24.0779139079266,
12.));
#178125=CARTESIAN_POINT('Ctrl Pts',(-5.10881967883132,24.0975261288446,
12.));
#178126=CARTESIAN_POINT('Ctrl Pts',(-5.12296753853859,24.117173659394,12.));
#178127=CARTESIAN_POINT('Ctrl Pts',(-5.13721325845745,24.1368558702443,
12.));
#178128=CARTESIAN_POINT('Ctrl Pts',(-5.15155675390075,24.156572137597,12.));
#178129=CARTESIAN_POINT('Ctrl Pts',(-5.16599793957979,24.1763218431343,
12.));
#178130=CARTESIAN_POINT('Ctrl Pts',(-5.18053672961392,24.1961043738754,
12.));
#178131=CARTESIAN_POINT('Ctrl Pts',(-5.19517303753643,24.215919122017,12.));
#178132=CARTESIAN_POINT('Ctrl Pts',(-5.20990677629173,24.2357654847765,
12.));
#178133=CARTESIAN_POINT('Ctrl Pts',(-5.22473785822441,24.2556428642294,
12.));
#178134=CARTESIAN_POINT('Ctrl Pts',(-5.23966619506289,24.2755506671526,
12.));
#178135=CARTESIAN_POINT('Ctrl Pts',(-5.25469169788856,24.2954883048448,
12.));
#178136=CARTESIAN_POINT('Ctrl Pts',(-5.26981427718796,24.3154551932222,
12.));
#178137=CARTESIAN_POINT('Ctrl Pts',(-5.28503384290644,24.3354507529415,
12.));
#178138=CARTESIAN_POINT('Ctrl Pts',(-5.30035030449059,24.3554744095075,
12.));
#178139=CARTESIAN_POINT('Ctrl Pts',(-5.31576357092524,24.3755255933917,
12.));
#178140=CARTESIAN_POINT('Ctrl Pts',(-5.33127355076037,24.3956037401293,
12.));
#178141=CARTESIAN_POINT('Ctrl Pts',(-5.34688015213546,24.4157082904615,
12.));
#178142=CARTESIAN_POINT('Ctrl Pts',(-5.36258328273639,24.4358386899152,
12.));
#178143=CARTESIAN_POINT('Ctrl Pts',(-5.37838284973706,24.4559943883159,
12.));
#178144=CARTESIAN_POINT('Ctrl Pts',(-5.3942787597383,24.4761748393322,12.));
#178145=CARTESIAN_POINT('Ctrl Pts',(-5.41027091869242,24.4963794999831,
12.));
#178146=CARTESIAN_POINT('Ctrl Pts',(-5.42635923183411,24.5166078302107,
12.));
#178147=CARTESIAN_POINT('Ctrl Pts',(-5.44254360356865,24.5368592922861,
12.));
#178148=CARTESIAN_POINT('Ctrl Pts',(-5.45882393762244,24.5571333514841,
12.));
#178149=CARTESIAN_POINT('Ctrl Pts',(-5.47520013724403,24.5774294770329,
12.));
#178150=CARTESIAN_POINT('Ctrl Pts',(-5.49167210537235,24.5977471429365,
12.));
#178151=CARTESIAN_POINT('Ctrl Pts',(-5.50823974481959,24.618085828918,12.));
#178152=CARTESIAN_POINT('Ctrl Pts',(-5.52490295840996,24.6384450211466,
12.));
#178153=CARTESIAN_POINT('Ctrl Pts',(-5.54166164919593,24.6588242134733,
12.));
#178154=CARTESIAN_POINT('Ctrl Pts',(-5.55851572025389,24.6792229061785,
12.));
#178155=CARTESIAN_POINT('Ctrl Pts',(-5.57546507427767,24.6996406035507,
12.));
#178156=CARTESIAN_POINT('Ctrl Pts',(-5.59250961323995,24.7200768119079,
12.));
#178157=CARTESIAN_POINT('Ctrl Pts',(-5.60964923798495,24.7405310372736,
12.));
#178158=CARTESIAN_POINT('Ctrl Pts',(-5.62688384790919,24.76100278357,12.));
#178159=CARTESIAN_POINT('Ctrl Pts',(-5.64421334042248,24.7814915496728,
12.));
#178160=CARTESIAN_POINT('Ctrl Pts',(-5.66163761114903,24.8019968304618,
12.));
#178161=CARTESIAN_POINT('Ctrl Pts',(-5.67915655496524,24.822518122386,12.));
#178162=CARTESIAN_POINT('Ctrl Pts',(-5.69677006679429,24.8430549277634,
12.));
#178163=CARTESIAN_POINT('Ctrl Pts',(-5.71447804252019,24.8636067597677,
12.));
#178164=CARTESIAN_POINT('Ctrl Pts',(-5.73228037976927,24.8841731467219,
12.));
#178165=CARTESIAN_POINT('Ctrl Pts',(-5.75017697890813,24.9047536376467,
12.));
#178166=CARTESIAN_POINT('Ctrl Pts',(-5.76816774342236,24.9253478043632,
12.));
#178167=CARTESIAN_POINT('Ctrl Pts',(-5.78625257775703,24.9459552293308,
12.));
#178168=CARTESIAN_POINT('Ctrl Pts',(-5.80443138549747,24.9665754954462,
12.));
#178169=CARTESIAN_POINT('Ctrl Pts',(-5.82270406744214,24.9872081752709,
12.));
#178170=CARTESIAN_POINT('Ctrl Pts',(-5.84107051963073,25.0078528200558,
12.));
#178171=CARTESIAN_POINT('Ctrl Pts',(-5.8595306315681,25.0285089498922,12.));
#178172=CARTESIAN_POINT('Ctrl Pts',(-5.87808428385329,25.0491760405965,
12.));
#178173=CARTESIAN_POINT('Ctrl Pts',(-5.89673135155459,25.0698535426593,
12.));
#178174=CARTESIAN_POINT('Ctrl Pts',(-5.91547170844382,25.0905409050863,
12.));
#178175=CARTESIAN_POINT('Ctrl Pts',(-5.93430523086776,25.1112375971182,
12.));
#178176=CARTESIAN_POINT('Ctrl Pts',(-5.95323180187348,25.1319431317273,
12.));
#178177=CARTESIAN_POINT('Ctrl Pts',(-5.97225131495636,25.1526570863065,
12.));
#178178=CARTESIAN_POINT('Ctrl Pts',(-5.99136367859838,25.1733791296154,
12.));
#178179=CARTESIAN_POINT('Ctrl Pts',(-6.0105688180476,25.1941090269638,12.));
#178180=CARTESIAN_POINT('Ctrl Pts',(-6.02986667390187,25.2148466201368,
12.));
#178181=CARTESIAN_POINT('Ctrl Pts',(-6.04925720151412,25.2355918138798,
12.));
#178182=CARTESIAN_POINT('Ctrl Pts',(-6.06484373634697,25.2521940105523,
12.));
#178183=CARTESIAN_POINT('Ctrl Pts',(-6.07657531787578,25.2646490489816,
12.));
#178184=CARTESIAN_POINT('Ctrl Pts',(-6.08441489609824,25.2729539149479,
12.));
#178185=CARTESIAN_POINT('Ctrl Pts',(-6.08833931617698,25.2771067246846,
12.));
#178186=CARTESIAN_POINT('',(-7.36589684767344,24.9347862158358,12.));
#178187=CARTESIAN_POINT('Origin',(0.,0.,12.));
#178188=CARTESIAN_POINT('',(-7.52250298901264,21.2610617890679,12.));
#178189=CARTESIAN_POINT('Ctrl Pts',(-7.36589684767344,24.9347862158358,
12.));
#178190=CARTESIAN_POINT('Ctrl Pts',(-7.3672190902906,24.9292275670705,12.));
#178191=CARTESIAN_POINT('Ctrl Pts',(-7.36985593120696,24.9181155530631,
12.));
#178192=CARTESIAN_POINT('Ctrl Pts',(-7.37378825962718,24.9014633826201,
12.));
#178193=CARTESIAN_POINT('Ctrl Pts',(-7.3789854964161,24.8792921911309,12.));
#178194=CARTESIAN_POINT('Ctrl Pts',(-7.38540558904946,24.8516310625367,
12.));
#178195=CARTESIAN_POINT('Ctrl Pts',(-7.39174922586841,24.8240228521042,
12.));
#178196=CARTESIAN_POINT('Ctrl Pts',(-7.39801641583612,24.7964676646518,
12.));
#178197=CARTESIAN_POINT('Ctrl Pts',(-7.40420718661754,24.7689656669005,
12.));
#178198=CARTESIAN_POINT('Ctrl Pts',(-7.41032159082173,24.7415170994754,
12.));
#178199=CARTESIAN_POINT('Ctrl Pts',(-7.41635971481243,24.7141222949988,
12.));
#178200=CARTESIAN_POINT('Ctrl Pts',(-7.42232167765763,24.6867816727118,
12.));
#178201=CARTESIAN_POINT('Ctrl Pts',(-7.42820762158681,24.659495712869,12.));
#178202=CARTESIAN_POINT('Ctrl Pts',(-7.4340177048922,24.6322649369472,12.));
#178203=CARTESIAN_POINT('Ctrl Pts',(-7.43975209375375,24.6050898852349,
12.));
#178204=CARTESIAN_POINT('Ctrl Pts',(-7.44541095473163,24.5779710960865,
12.));
#178205=CARTESIAN_POINT('Ctrl Pts',(-7.45099444651296,24.5509090831579,
12.));
#178206=CARTESIAN_POINT('Ctrl Pts',(-7.45650271336045,24.52390431731,12.));
#178207=CARTESIAN_POINT('Ctrl Pts',(-7.46193588961642,24.4969572391509,
12.));
#178208=CARTESIAN_POINT('Ctrl Pts',(-7.46729410308923,24.4700682684544,
12.));
#178209=CARTESIAN_POINT('Ctrl Pts',(-7.47257747883319,24.4432378146501,
12.));
#178210=CARTESIAN_POINT('Ctrl Pts',(-7.47778614286573,24.4164662871165,
12.));
#178211=CARTESIAN_POINT('Ctrl Pts',(-7.48292022569254,24.3897541049248,
12.));
#178212=CARTESIAN_POINT('Ctrl Pts',(-7.48797986651828,24.3631017084513,
12.));
#178213=CARTESIAN_POINT('Ctrl Pts',(-7.4929652125233,24.3365095573673,12.));
#178214=CARTESIAN_POINT('Ctrl Pts',(-7.49787641695359,24.3099781253345,
12.));
#178215=CARTESIAN_POINT('Ctrl Pts',(-7.50271363765098,24.2835078958966,
12.));
#178216=CARTESIAN_POINT('Ctrl Pts',(-7.50747703535115,24.2570993577032,
12.));
#178217=CARTESIAN_POINT('Ctrl Pts',(-7.51216677222199,24.230753000389,12.));
#178218=CARTESIAN_POINT('Ctrl Pts',(-7.51678300997998,24.2044693092356,
12.));
#178219=CARTESIAN_POINT('Ctrl Pts',(-7.52132590953862,24.1782487641602,
12.));
#178220=CARTESIAN_POINT('Ctrl Pts',(-7.52579563201479,24.152091842537,12.));
#178221=CARTESIAN_POINT('Ctrl Pts',(-7.53019233935536,24.1259990209211,
12.));
#178222=CARTESIAN_POINT('Ctrl Pts',(-7.53451619514658,24.0999707772643,
12.));
#178223=CARTESIAN_POINT('Ctrl Pts',(-7.53876736531005,24.0740075927984,
12.));
#178224=CARTESIAN_POINT('Ctrl Pts',(-7.54294601896128,24.0481099543353,
12.));
#178225=CARTESIAN_POINT('Ctrl Pts',(-7.54705232885895,24.0222783554531,
12.));
#178226=CARTESIAN_POINT('Ctrl Pts',(-7.55108647097432,23.9965132953187,
12.));
#178227=CARTESIAN_POINT('Ctrl Pts',(-7.55504862424808,23.9708152779886,
12.));
#178228=CARTESIAN_POINT('Ctrl Pts',(-7.5589389702768,23.9451848115002,12.));
#178229=CARTESIAN_POINT('Ctrl Pts',(-7.56275769304773,23.9196224070759,
12.));
#178230=CARTESIAN_POINT('Ctrl Pts',(-7.56650497863791,23.8941285782002,
12.));
#178231=CARTESIAN_POINT('Ctrl Pts',(-7.57018101500709,23.8687038399595,
12.));
#178232=CARTESIAN_POINT('Ctrl Pts',(-7.57378599219814,23.8433487096132,
12.));
#178233=CARTESIAN_POINT('Ctrl Pts',(-7.57732010249066,23.8180637069976,
12.));
#178234=CARTESIAN_POINT('Ctrl Pts',(-7.58078354058213,23.7928493549908,
12.));
#178235=CARTESIAN_POINT('Ctrl Pts',(-7.58417650376271,23.7677061799376,
12.));
#178236=CARTESIAN_POINT('Ctrl Pts',(-7.58749919210826,23.7426347121006,
12.));
#178237=CARTESIAN_POINT('Ctrl Pts',(-7.5907518086532,23.7176354860456,12.));
#178238=CARTESIAN_POINT('Ctrl Pts',(-7.59393455934035,23.6927090405066,
12.));
#178239=CARTESIAN_POINT('Ctrl Pts',(-7.59704765299567,23.6678559182875,
12.));
#178240=CARTESIAN_POINT('Ctrl Pts',(-7.60009130130126,23.6430766661418,
12.));
#178241=CARTESIAN_POINT('Ctrl Pts',(-7.60306571877806,23.6183718346576,
12.));
#178242=CARTESIAN_POINT('Ctrl Pts',(-7.60597112277094,23.5937419781245,
12.));
#178243=CARTESIAN_POINT('Ctrl Pts',(-7.608807733446,23.5691876544244,12.));
#178244=CARTESIAN_POINT('Ctrl Pts',(-7.61157577385372,23.544709425203,12.));
#178245=CARTESIAN_POINT('Ctrl Pts',(-7.61427546999298,23.5203078560129,
12.));
#178246=CARTESIAN_POINT('Ctrl Pts',(-7.61690705088319,23.4959835164609,
12.));
#178247=CARTESIAN_POINT('Ctrl Pts',(-7.61947074863977,23.4717369803438,
12.));
#178248=CARTESIAN_POINT('Ctrl Pts',(-7.62196679855955,23.4475688257854,
12.));
#178249=CARTESIAN_POINT('Ctrl Pts',(-7.6243954392005,23.4234796353542,12.));
#178250=CARTESIAN_POINT('Ctrl Pts',(-7.62675691240329,23.399469996112,12.));
#178251=CARTESIAN_POINT('Ctrl Pts',(-7.62905146332593,23.3755404996636,
12.));
#178252=CARTESIAN_POINT('Ctrl Pts',(-7.63127934048136,23.3516917421972,
12.));
#178253=CARTESIAN_POINT('Ctrl Pts',(-7.63344079578161,23.3279243245241,
12.));
#178254=CARTESIAN_POINT('Ctrl Pts',(-7.63553608458783,23.3042388521022,
12.));
#178255=CARTESIAN_POINT('Ctrl Pts',(-7.63756546576374,23.2806359350855,
12.));
#178256=CARTESIAN_POINT('Ctrl Pts',(-7.63952920172835,23.2571161884488,
12.));
#178257=CARTESIAN_POINT('Ctrl Pts',(-7.64142755851504,23.2336802320912,
12.));
#178258=CARTESIAN_POINT('Ctrl Pts',(-7.6432608058368,23.2103286909398,12.));
#178259=CARTESIAN_POINT('Ctrl Pts',(-7.64502921715483,23.1870621950452,
12.));
#178260=CARTESIAN_POINT('Ctrl Pts',(-7.64673306975805,23.1638813796694,
12.));
#178261=CARTESIAN_POINT('Ctrl Pts',(-7.64837264482943,23.1407868853819,
12.));
#178262=CARTESIAN_POINT('Ctrl Pts',(-7.6499482274986,23.1177793581679,12.));
#178263=CARTESIAN_POINT('Ctrl Pts',(-7.65146010690476,23.094859449525,12.));
#178264=CARTESIAN_POINT('Ctrl Pts',(-7.65290857626358,23.072027816555,12.));
#178265=CARTESIAN_POINT('Ctrl Pts',(-7.65429393293946,23.0492851220528,
12.));
#178266=CARTESIAN_POINT('Ctrl Pts',(-7.65561647852534,23.0266320345787,
12.));
#178267=CARTESIAN_POINT('Ctrl Pts',(-7.65687651891304,23.0040692285814,
12.));
#178268=CARTESIAN_POINT('Ctrl Pts',(-7.65807436436432,22.9815973845296,
12.));
#178269=CARTESIAN_POINT('Ctrl Pts',(-7.65921032958902,22.959217189033,12.));
#178270=CARTESIAN_POINT('Ctrl Pts',(-7.66028473382778,22.9369293349593,
12.));
#178271=CARTESIAN_POINT('Ctrl Pts',(-7.66129790094108,22.9147345215421,
12.));
#178272=CARTESIAN_POINT('Ctrl Pts',(-7.66225015950156,22.8926334544883,
12.));
#178273=CARTESIAN_POINT('Ctrl Pts',(-7.66314184287337,22.8706268461283,
12.));
#178274=CARTESIAN_POINT('Ctrl Pts',(-7.66397328929803,22.848715415557,12.));
#178275=CARTESIAN_POINT('Ctrl Pts',(-7.66474484198549,22.8268998887678,
12.));
#178276=CARTESIAN_POINT('Ctrl Pts',(-7.66545684920987,22.8051809987833,
12.));
#178277=CARTESIAN_POINT('Ctrl Pts',(-7.66610966441273,22.7835594857699,
12.));
#178278=CARTESIAN_POINT('Ctrl Pts',(-7.66670364630299,22.7620360971843,
12.));
#178279=CARTESIAN_POINT('Ctrl Pts',(-7.6672391589544,22.7406115879513,12.));
#178280=CARTESIAN_POINT('Ctrl Pts',(-7.66771657191027,22.7192867206245,
12.));
#178281=CARTESIAN_POINT('Ctrl Pts',(-7.66813626029275,22.6980622655446,
12.));
#178282=CARTESIAN_POINT('Ctrl Pts',(-7.66849860491743,22.6769390009885,
12.));
#178283=CARTESIAN_POINT('Ctrl Pts',(-7.66880399241323,22.6559177133127,
12.));
#178284=CARTESIAN_POINT('Ctrl Pts',(-7.66905281533715,22.6349991971541,
12.));
#178285=CARTESIAN_POINT('Ctrl Pts',(-7.66924547229414,22.6141842556243,
12.));
#178286=CARTESIAN_POINT('Ctrl Pts',(-7.66938236806233,22.5934737004953,
12.));
#178287=CARTESIAN_POINT('Ctrl Pts',(-7.66946391372306,22.5728683523831,
12.));
#178288=CARTESIAN_POINT('Ctrl Pts',(-7.66949052679693,22.5523690409116,
12.));
#178289=CARTESIAN_POINT('Ctrl Pts',(-7.66946263138144,22.53197660492,12.));
#178290=CARTESIAN_POINT('Ctrl Pts',(-7.66938065829108,22.5116918927031,
12.));
#178291=CARTESIAN_POINT('Ctrl Pts',(-7.66924504520315,22.4915157622312,
12.));
#178292=CARTESIAN_POINT('Ctrl Pts',(-7.66905623680831,22.47144908137,12.));
#178293=CARTESIAN_POINT('Ctrl Pts',(-7.66881468496635,22.4514927280855,
12.));
#178294=CARTESIAN_POINT('Ctrl Pts',(-7.66852084886704,22.4316475906603,
12.));
#178295=CARTESIAN_POINT('Ctrl Pts',(-7.6681751951964,22.4119145679758,12.));
#178296=CARTESIAN_POINT('Ctrl Pts',(-7.6677781983079,22.3922945697773,12.));
#178297=CARTESIAN_POINT('Ctrl Pts',(-7.66733034039883,22.372788516936,12.));
#178298=CARTESIAN_POINT('Ctrl Pts',(-7.66683211169158,22.3533973417021,
12.));
#178299=CARTESIAN_POINT('Ctrl Pts',(-7.66628401061952,22.3341219879469,
12.));
#178300=CARTESIAN_POINT('Ctrl Pts',(-7.66568654402494,22.314963411484,12.));
#178301=CARTESIAN_POINT('Ctrl Pts',(-7.66504022736299,22.2959225803937,
12.));
#178302=CARTESIAN_POINT('Ctrl Pts',(-7.66434558490979,22.2770004753335,
12.));
#178303=CARTESIAN_POINT('Ctrl Pts',(-7.66360314997641,22.258198089848,12.));
#178304=CARTESIAN_POINT('Ctrl Pts',(-7.66281346512509,22.2395164306547,
12.));
#178305=CARTESIAN_POINT('Ctrl Pts',(-7.661977082404,22.2209565180085,12.));
#178306=CARTESIAN_POINT('Ctrl Pts',(-7.66109456359271,22.2025193860964,
12.));
#178307=CARTESIAN_POINT('Ctrl Pts',(-7.66016648045005,22.1842060834091,
12.));
#178308=CARTESIAN_POINT('Ctrl Pts',(-7.6591934149693,22.1660176731178,12.));
#178309=CARTESIAN_POINT('Ctrl Pts',(-7.65817595963349,22.1479552334211,
12.));
#178310=CARTESIAN_POINT('Ctrl Pts',(-7.65711471769397,22.1300198579675,
12.));
#178311=CARTESIAN_POINT('Ctrl Pts',(-7.65601030346807,22.1122126563329,
12.));
#178312=CARTESIAN_POINT('Ctrl Pts',(-7.65486334263644,22.094534754469,12.));
#178313=CARTESIAN_POINT('Ctrl Pts',(-7.65367447254949,22.0769872951596,
12.));
#178314=CARTESIAN_POINT('Ctrl Pts',(-7.65244434253113,22.0595714384431,
12.));
#178315=CARTESIAN_POINT('Ctrl Pts',(-7.65117361421358,22.0422883621174,
12.));
#178316=CARTESIAN_POINT('Ctrl Pts',(-7.64986296190168,22.0251392623209,
12.));
#178317=CARTESIAN_POINT('Ctrl Pts',(-7.64851307293352,22.0081253540774,
12.));
#178318=CARTESIAN_POINT('Ctrl Pts',(-7.6471246480525,21.9912478718542,12.));
#178319=CARTESIAN_POINT('Ctrl Pts',(-7.64569840177336,21.9745080700798,
12.));
#178320=CARTESIAN_POINT('Ctrl Pts',(-7.64423506279123,21.9579072237651,
12.));
#178321=CARTESIAN_POINT('Ctrl Pts',(-7.64273537442682,21.9414466292072,
12.));
#178322=CARTESIAN_POINT('Ctrl Pts',(-7.64120009506532,21.9251276046546,
12.));
#178323=CARTESIAN_POINT('Ctrl Pts',(-7.63962999860927,21.9089514909874,
12.));
#178324=CARTESIAN_POINT('Ctrl Pts',(-7.63802587492035,21.8929196523514,
12.));
#178325=CARTESIAN_POINT('Ctrl Pts',(-7.636388530334,21.8770334769496,12.));
#178326=CARTESIAN_POINT('Ctrl Pts',(-7.63471878821226,21.8612943779089,
12.));
#178327=CARTESIAN_POINT('Ctrl Pts',(-7.63301748948936,21.8457037941084,
12.));
#178328=CARTESIAN_POINT('Ctrl Pts',(-7.63128549323023,21.8302631910195,
12.));
#178329=CARTESIAN_POINT('Ctrl Pts',(-7.62952367718127,21.814974061509,12.));
#178330=CARTESIAN_POINT('Ctrl Pts',(-7.62773293842389,21.799837926858,12.));
#178331=CARTESIAN_POINT('Ctrl Pts',(-7.62591419404512,21.7848563378021,
12.));
#178332=CARTESIAN_POINT('Ctrl Pts',(-7.62406838181166,21.7700308755584,
12.));
#178333=CARTESIAN_POINT('Ctrl Pts',(-7.62219646084228,21.7553631528328,
12.));
#178334=CARTESIAN_POINT('Ctrl Pts',(-7.62029941230855,21.7408548148656,
12.));
#178335=CARTESIAN_POINT('Ctrl Pts',(-7.61837824030538,21.7265075407975,
12.));
#178336=CARTESIAN_POINT('Ctrl Pts',(-7.61643397270421,21.7123230449834,
12.));
#178337=CARTESIAN_POINT('Ctrl Pts',(-7.61446766202787,21.6983030783322,
12.));
#178338=CARTESIAN_POINT('Ctrl Pts',(-7.61248038630268,21.6844494295815,
12.));
#178339=CARTESIAN_POINT('Ctrl Pts',(-7.61047325000956,21.6707639267576,
12.));
#178340=CARTESIAN_POINT('Ctrl Pts',(-7.60844738512874,21.6572484388081,
12.));
#178341=CARTESIAN_POINT('Ctrl Pts',(-7.60640395216357,21.6439048771743,
12.));
#178342=CARTESIAN_POINT('Ctrl Pts',(-7.60434414118296,21.6307351973822,
12.));
#178343=CARTESIAN_POINT('Ctrl Pts',(-7.60226917285429,21.617741400599,12.));
#178344=CARTESIAN_POINT('Ctrl Pts',(-7.60018029988241,21.6049255358843,
12.));
#178345=CARTESIAN_POINT('Ctrl Pts',(-7.59807880846195,21.5922897024466,
12.));
#178346=CARTESIAN_POINT('Ctrl Pts',(-7.59596601973584,21.5798360518978,
12.));
#178347=CARTESIAN_POINT('Ctrl Pts',(-7.59384329124918,21.5675667904726,
12.));
#178348=CARTESIAN_POINT('Ctrl Pts',(-7.59171201844777,21.5554841813462,
12.));
#178349=CARTESIAN_POINT('Ctrl Pts',(-7.58957363620014,21.543590547011,12.));
#178350=CARTESIAN_POINT('Ctrl Pts',(-7.58742962034834,21.5318882716736,
12.));
#178351=CARTESIAN_POINT('Ctrl Pts',(-7.5852814891913,21.5203798035299,12.));
#178352=CARTESIAN_POINT('Ctrl Pts',(-7.5831308051918,21.5090676573873,12.));
#178353=CARTESIAN_POINT('Ctrl Pts',(-7.58097917790744,21.4979544192744,
12.));
#178354=CARTESIAN_POINT('Ctrl Pts',(-7.57882826679132,21.4870427508194,
12.));
#178355=CARTESIAN_POINT('Ctrl Pts',(-7.57667978402987,21.4763353936762,
12.));
#178356=CARTESIAN_POINT('Ctrl Pts',(-7.57453549743412,21.4658351740128,
12.));
#178357=CARTESIAN_POINT('Ctrl Pts',(-7.57239723223506,21.4555450053142,
12.));
#178358=CARTESIAN_POINT('Ctrl Pts',(-7.57026687261166,21.4454678907509,
12.));
#178359=CARTESIAN_POINT('Ctrl Pts',(-7.56814636360847,21.4356069261513,
12.));
#178360=CARTESIAN_POINT('Ctrl Pts',(-7.56603771218712,21.4259653015736,
12.));
#178361=CARTESIAN_POINT('Ctrl Pts',(-7.56394299313685,21.4165463106254,
12.));
#178362=CARTESIAN_POINT('Ctrl Pts',(-7.56186435703622,21.4073533630365,
12.));
#178363=CARTESIAN_POINT('Ctrl Pts',(-7.55980403700611,21.3983899952987,
12.));
#178364=CARTESIAN_POINT('Ctrl Pts',(-7.55776435731417,21.3896598842117,
12.));
#178365=CARTESIAN_POINT('Ctrl Pts',(-7.55574773403503,21.3811668478932,
12.));
#178366=CARTESIAN_POINT('Ctrl Pts',(-7.55375667080029,21.3729148390243,
12.));
#178367=CARTESIAN_POINT('Ctrl Pts',(-7.55179375777444,21.3649079431865,
12.));
#178368=CARTESIAN_POINT('Ctrl Pts',(-7.5498616652131,21.3571503685855,12.));
#178369=CARTESIAN_POINT('Ctrl Pts',(-7.5479631624633,21.3496464761531,12.));
#178370=CARTESIAN_POINT('Ctrl Pts',(-7.54610114948347,21.3424008295038,
12.));
#178371=CARTESIAN_POINT('Ctrl Pts',(-7.54427868151268,21.3354182340149,
12.));
#178372=CARTESIAN_POINT('Ctrl Pts',(-7.54249900377031,21.328703791771,12.));
#178373=CARTESIAN_POINT('Ctrl Pts',(-7.54076552038279,21.3222628524165,
12.));
#178374=CARTESIAN_POINT('Ctrl Pts',(-7.53908175169898,21.3161009456256,
12.));
#178375=CARTESIAN_POINT('Ctrl Pts',(-7.53745129364616,21.310223716773,12.));
#178376=CARTESIAN_POINT('Ctrl Pts',(-7.53587778251736,21.3046368712157,
12.));
#178377=CARTESIAN_POINT('Ctrl Pts',(-7.53436505309943,21.2993464250717,
12.));
#178378=CARTESIAN_POINT('Ctrl Pts',(-7.53291726078527,21.2943588989331,
12.));
#178379=CARTESIAN_POINT('Ctrl Pts',(-7.53153906987855,21.2896816163842,
12.));
#178380=CARTESIAN_POINT('Ctrl Pts',(-7.53023562438229,21.2853226580657,
12.));
#178381=CARTESIAN_POINT('Ctrl Pts',(-7.52901217930408,21.2812902781143,
12.));
#178382=CARTESIAN_POINT('Ctrl Pts',(-7.52787386225333,21.2775925269652,
12.));
#178383=CARTESIAN_POINT('Ctrl Pts',(-7.52682526918541,21.2742366113579,
12.));
#178384=CARTESIAN_POINT('Ctrl Pts',(-7.5258712609553,21.2712301573466,12.));
#178385=CARTESIAN_POINT('Ctrl Pts',(-7.5250177033353,21.2685823838671,12.));
#178386=CARTESIAN_POINT('Ctrl Pts',(-7.52427261074298,21.2663059157058,
12.));
#178387=CARTESIAN_POINT('Ctrl Pts',(-7.52364573027553,21.2644161259962,
12.));
#178388=CARTESIAN_POINT('Ctrl Pts',(-7.52314642316199,21.262927782038,12.));
#178389=CARTESIAN_POINT('Ctrl Pts',(-7.5227818224267,21.2618521283555,12.));
#178390=CARTESIAN_POINT('Ctrl Pts',(-7.52260064231661,21.261326054066,12.));
#178391=CARTESIAN_POINT('Ctrl Pts',(-7.52252744144904,21.2611204474866,
12.));
#178392=CARTESIAN_POINT('Ctrl Pts',(-7.5225064970397,21.2610673466886,12.));
#178393=CARTESIAN_POINT('Ctrl Pts',(-7.52250298901264,21.2610617890679,
12.));
#178394=CARTESIAN_POINT('',(-7.33627833380046,20.7347298079577,12.));
#178395=CARTESIAN_POINT('',(-3.58569854577611,10.1343606576251,12.));
#178396=CARTESIAN_POINT('',(-7.63019749246977,20.1004996511507,12.));
#178397=CARTESIAN_POINT('Origin',(-7.80764394578302,20.56795313141,12.));
#178398=CARTESIAN_POINT('',(-8.8178352198485,19.6085639972844,12.));
#178399=CARTESIAN_POINT('Origin',(-2.70312158620511E-13,7.32141292029404E-13,
12.));
#178400=CARTESIAN_POINT('',(-9.47413589477548,19.84920021178,12.));
#178401=CARTESIAN_POINT('Origin',(-9.02290115519381,20.0645771135003,12.));
#178402=CARTESIAN_POINT('',(-9.71462809124916,20.353053841303,12.));
#178403=CARTESIAN_POINT('',(-4.85731404562459,10.1765269206515,12.));
#178404=CARTESIAN_POINT('',(-12.4230808101438,22.8400320311648,12.));
#178405=CARTESIAN_POINT('Ctrl Pts',(-9.71462809124916,20.353053841303,12.));
#178406=CARTESIAN_POINT('Ctrl Pts',(-9.71462954053042,20.353060251684,12.));
#178407=CARTESIAN_POINT('Ctrl Pts',(-9.71465227853041,20.3531126095522,
12.));
#178408=CARTESIAN_POINT('Ctrl Pts',(-9.71474590350681,20.3533097561886,
12.));
#178409=CARTESIAN_POINT('Ctrl Pts',(-9.71498978052021,20.3538098605706,
12.));
#178410=CARTESIAN_POINT('Ctrl Pts',(-9.71549257088172,20.3548282742361,
12.));
#178411=CARTESIAN_POINT('Ctrl Pts',(-9.71619192554186,20.3562337557875,
12.));
#178412=CARTESIAN_POINT('Ctrl Pts',(-9.71708493723096,20.3580133103356,
12.));
#178413=CARTESIAN_POINT('Ctrl Pts',(-9.71816778328006,20.3601498764344,
12.));
#178414=CARTESIAN_POINT('Ctrl Pts',(-9.71943648548099,20.3626256913981,
12.));
#178415=CARTESIAN_POINT('Ctrl Pts',(-9.72088778381081,20.3654261611056,
12.));
#178416=CARTESIAN_POINT('Ctrl Pts',(-9.7225193072249,20.3685406190576,12.));
#178417=CARTESIAN_POINT('Ctrl Pts',(-9.72432910043194,20.371960235676,12.));
#178418=CARTESIAN_POINT('Ctrl Pts',(-9.7263153173288,20.3756766651951,12.));
#178419=CARTESIAN_POINT('Ctrl Pts',(-9.72847589116542,20.3796805893304,
12.));
#178420=CARTESIAN_POINT('Ctrl Pts',(-9.73080870123727,20.3839624556742,
12.));
#178421=CARTESIAN_POINT('Ctrl Pts',(-9.73331167102808,20.3885129129912,
12.));
#178422=CARTESIAN_POINT('Ctrl Pts',(-9.73598292014243,20.3933234845647,
12.));
#178423=CARTESIAN_POINT('Ctrl Pts',(-9.73882077613201,20.3983866213331,
12.));
#178424=CARTESIAN_POINT('Ctrl Pts',(-9.74182369656272,20.4036953576549,
12.));
#178425=CARTESIAN_POINT('Ctrl Pts',(-9.74499021838538,20.4092430879861,
12.));
#178426=CARTESIAN_POINT('Ctrl Pts',(-9.74831889242174,20.4150232777393,
12.));
#178427=CARTESIAN_POINT('Ctrl Pts',(-9.7518082978643,20.4210295275817,12.));
#178428=CARTESIAN_POINT('Ctrl Pts',(-9.75545705902418,20.4272556476629,
12.));
#178429=CARTESIAN_POINT('Ctrl Pts',(-9.75926386289923,20.4336957355473,
12.));
#178430=CARTESIAN_POINT('Ctrl Pts',(-9.76322747195495,20.44034423294,12.));
#178431=CARTESIAN_POINT('Ctrl Pts',(-9.76734670980892,20.447195862298,12.));
#178432=CARTESIAN_POINT('Ctrl Pts',(-9.7716204510407,20.4542455817527,12.));
#178433=CARTESIAN_POINT('Ctrl Pts',(-9.77604760815529,20.4614885274975,
12.));
#178434=CARTESIAN_POINT('Ctrl Pts',(-9.78062712373321,20.4689199790669,
12.));
#178435=CARTESIAN_POINT('Ctrl Pts',(-9.78535797314167,20.4765353711586,
12.));
#178436=CARTESIAN_POINT('Ctrl Pts',(-9.79023916498656,20.4843302955329,
12.));
#178437=CARTESIAN_POINT('Ctrl Pts',(-9.79526974288331,20.4923005087943,
12.));
#178438=CARTESIAN_POINT('Ctrl Pts',(-9.80044878520949,20.5004419312107,
12.));
#178439=CARTESIAN_POINT('Ctrl Pts',(-9.80577540161088,20.5087506310505,
12.));
#178440=CARTESIAN_POINT('Ctrl Pts',(-9.81124873025282,20.517222812284,12.));
#178441=CARTESIAN_POINT('Ctrl Pts',(-9.81686793455943,20.5258548000629,
12.));
#178442=CARTESIAN_POINT('Ctrl Pts',(-9.82263220080363,20.5346430299517,
12.));
#178443=CARTESIAN_POINT('Ctrl Pts',(-9.82854073773877,20.5435840460721,
12.));
#178444=CARTESIAN_POINT('Ctrl Pts',(-9.83459277585315,20.552674497646,12.));
#178445=CARTESIAN_POINT('Ctrl Pts',(-9.84078756677565,20.5619111362402,
12.));
#178446=CARTESIAN_POINT('Ctrl Pts',(-9.84712438256278,20.5712908125139,
12.));
#178447=CARTESIAN_POINT('Ctrl Pts',(-9.85360251456981,20.5808104710015,
12.));
#178448=CARTESIAN_POINT('Ctrl Pts',(-9.86022127232748,20.5904671449754,
12.));
#178449=CARTESIAN_POINT('Ctrl Pts',(-9.86697998242623,20.6002579513699,
12.));
#178450=CARTESIAN_POINT('Ctrl Pts',(-9.87387798732956,20.6101800854494,
12.));
#178451=CARTESIAN_POINT('Ctrl Pts',(-9.88091464472676,20.6202308177474,
12.));
#178452=CARTESIAN_POINT('Ctrl Pts',(-9.88808932697306,20.6304074914087,
12.));
#178453=CARTESIAN_POINT('Ctrl Pts',(-9.8954014204912,20.6407075193976,12.));
#178454=CARTESIAN_POINT('Ctrl Pts',(-9.90285032516693,20.6511283817414,
12.));
#178455=CARTESIAN_POINT('Ctrl Pts',(-9.91043545377007,20.6616676228315,
12.));
#178456=CARTESIAN_POINT('Ctrl Pts',(-9.91815623141289,20.6723228488263,
12.));
#178457=CARTESIAN_POINT('Ctrl Pts',(-9.92601209498749,20.6830917250255,
12.));
#178458=CARTESIAN_POINT('Ctrl Pts',(-9.9340024925973,20.6939719732484,12.));
#178459=CARTESIAN_POINT('Ctrl Pts',(-9.94212688298236,20.7049613692234,
12.));
#178460=CARTESIAN_POINT('Ctrl Pts',(-9.95038473514949,20.7160577407579,
12.));
#178461=CARTESIAN_POINT('Ctrl Pts',(-9.95877552798398,20.7272589658751,
12.));
#178462=CARTESIAN_POINT('Ctrl Pts',(-9.96729874986202,20.7385629709795,
12.));
#178463=CARTESIAN_POINT('Ctrl Pts',(-9.9759538982347,20.7499677289627,12.));
#178464=CARTESIAN_POINT('Ctrl Pts',(-9.98474047926852,20.761471257499,12.));
#178465=CARTESIAN_POINT('Ctrl Pts',(-9.9936580075464,20.7730716175417,12.));
#178466=CARTESIAN_POINT('Ctrl Pts',(-10.0027060057389,20.7847669117568,
12.));
#178467=CARTESIAN_POINT('Ctrl Pts',(-10.0118840042786,20.7965552829908,
12.));
#178468=CARTESIAN_POINT('Ctrl Pts',(-10.0211915410095,20.8084349126888,
12.));
#178469=CARTESIAN_POINT('Ctrl Pts',(-10.0306281609435,20.8204040196602,
12.));
#178470=CARTESIAN_POINT('Ctrl Pts',(-10.0401934160234,20.8324608588909,
12.));
#178471=CARTESIAN_POINT('Ctrl Pts',(-10.0498868648733,20.8446037203402,
12.));
#178472=CARTESIAN_POINT('Ctrl Pts',(-10.0597080725375,20.8568309277316,
12.));
#178473=CARTESIAN_POINT('Ctrl Pts',(-10.0696566102218,20.86914083737,12.));
#178474=CARTESIAN_POINT('Ctrl Pts',(-10.0797320551154,20.881531837184,12.));
#178475=CARTESIAN_POINT('Ctrl Pts',(-10.0899339901916,20.894002345737,12.));
#178476=CARTESIAN_POINT('Ctrl Pts',(-10.1002620040076,20.9065508112557,
12.));
#178477=CARTESIAN_POINT('Ctrl Pts',(-10.1107156904836,20.919175710627,12.));
#178478=CARTESIAN_POINT('Ctrl Pts',(-10.1212946487057,20.9318755484734,
12.));
#178479=CARTESIAN_POINT('Ctrl Pts',(-10.1319984827908,20.9446488563933,
12.));
#178480=CARTESIAN_POINT('Ctrl Pts',(-10.1428268017256,20.9574941921591,
12.));
#178481=CARTESIAN_POINT('Ctrl Pts',(-10.1537792192065,20.9704101389369,
12.));
#178482=CARTESIAN_POINT('Ctrl Pts',(-10.1648553534568,20.9833953044736,
12.));
#178483=CARTESIAN_POINT('Ctrl Pts',(-10.1760548270767,20.9964483203686,
12.));
#178484=CARTESIAN_POINT('Ctrl Pts',(-10.187377266936,21.0095678414486,12.));
#178485=CARTESIAN_POINT('Ctrl Pts',(-10.1988223040425,21.0227525451107,
12.));
#178486=CARTESIAN_POINT('Ctrl Pts',(-10.2103895734123,21.0360011306815,
12.));
#178487=CARTESIAN_POINT('Ctrl Pts',(-10.2220787139155,21.0493123187483,
12.));
#178488=CARTESIAN_POINT('Ctrl Pts',(-10.2338893681567,21.0626848505663,
12.));
#178489=CARTESIAN_POINT('Ctrl Pts',(-10.2458211823912,21.0761174875445,
12.));
#178490=CARTESIAN_POINT('Ctrl Pts',(-10.2578738064181,21.0896090107063,
12.));
#178491=CARTESIAN_POINT('Ctrl Pts',(-10.2700468934744,21.1031582201627,
12.));
#178492=CARTESIAN_POINT('Ctrl Pts',(-10.2823401001072,21.1167639345631,
12.));
#178493=CARTESIAN_POINT('Ctrl Pts',(-10.2947530860721,21.1304249906002,
12.));
#178494=CARTESIAN_POINT('Ctrl Pts',(-10.3072855142687,21.1441402425843,
12.));
#178495=CARTESIAN_POINT('Ctrl Pts',(-10.3199370506544,21.1579085619965,
12.));
#178496=CARTESIAN_POINT('Ctrl Pts',(-10.3327073641572,21.1717288370509,
12.));
#178497=CARTESIAN_POINT('Ctrl Pts',(-10.3455961265701,21.1855999722416,
12.));
#178498=CARTESIAN_POINT('Ctrl Pts',(-10.3586030124587,21.199520887919,12.));
#178499=CARTESIAN_POINT('Ctrl Pts',(-10.371727699113,21.2134905199345,12.));
#178500=CARTESIAN_POINT('Ctrl Pts',(-10.3849698664786,21.22750781927,12.));
#178501=CARTESIAN_POINT('Ctrl Pts',(-10.3983291970846,21.2415717516714,
12.));
#178502=CARTESIAN_POINT('Ctrl Pts',(-10.4118053759588,21.255681297275,12.));
#178503=CARTESIAN_POINT('Ctrl Pts',(-10.42539809054,21.2698354502403,12.));
#178504=CARTESIAN_POINT('Ctrl Pts',(-10.4391070306391,21.2840332184483,
12.));
#178505=CARTESIAN_POINT('Ctrl Pts',(-10.4529318883874,21.2982736231931,
12.));
#178506=CARTESIAN_POINT('Ctrl Pts',(-10.4668723581768,21.3125556988731,
12.));
#178507=CARTESIAN_POINT('Ctrl Pts',(-10.4809281365931,21.3268784926819,
12.));
#178508=CARTESIAN_POINT('Ctrl Pts',(-10.4950989223337,21.3412410642904,
12.));
#178509=CARTESIAN_POINT('Ctrl Pts',(-10.5093844161685,21.3556424855814,
12.));
#178510=CARTESIAN_POINT('Ctrl Pts',(-10.5237843209057,21.3700818403936,
12.));
#178511=CARTESIAN_POINT('Ctrl Pts',(-10.5382983413421,21.3845582242602,
12.));
#178512=CARTESIAN_POINT('Ctrl Pts',(-10.5529261842108,21.3990707441497,
12.));
#178513=CARTESIAN_POINT('Ctrl Pts',(-10.5676675581108,21.4136185181979,
12.));
#178514=CARTESIAN_POINT('Ctrl Pts',(-10.5825221734573,21.4282006754631,
12.));
#178515=CARTESIAN_POINT('Ctrl Pts',(-10.5974897424622,21.4428163557144,
12.));
#178516=CARTESIAN_POINT('Ctrl Pts',(-10.6125699790961,21.4574647092097,
12.));
#178517=CARTESIAN_POINT('Ctrl Pts',(-10.6277625990456,21.4721448964766,
12.));
#178518=CARTESIAN_POINT('Ctrl Pts',(-10.6430673196607,21.4868560880889,
12.));
#178519=CARTESIAN_POINT('Ctrl Pts',(-10.6584838598939,21.5015974644449,
12.));
#178520=CARTESIAN_POINT('Ctrl Pts',(-10.6740119402834,21.51636821558,12.));
#178521=CARTESIAN_POINT('Ctrl Pts',(-10.689651282929,21.5311675409807,12.));
#178522=CARTESIAN_POINT('Ctrl Pts',(-10.7054016114571,21.5459946493955,
12.));
#178523=CARTESIAN_POINT('Ctrl Pts',(-10.7212626509816,21.5608487586468,
12.));
#178524=CARTESIAN_POINT('Ctrl Pts',(-10.7372341280467,21.5757290954371,
12.));
#178525=CARTESIAN_POINT('Ctrl Pts',(-10.7533157705941,21.5906348951743,
12.));
#178526=CARTESIAN_POINT('Ctrl Pts',(-10.7695073079552,21.6055654018176,
12.));
#178527=CARTESIAN_POINT('Ctrl Pts',(-10.7858084708261,21.6205198677173,
12.));
#178528=CARTESIAN_POINT('Ctrl Pts',(-10.8022189912369,21.6354975534557,
12.));
#178529=CARTESIAN_POINT('Ctrl Pts',(-10.8187386025136,21.6504977276866,
12.));
#178530=CARTESIAN_POINT('Ctrl Pts',(-10.8353670392272,21.6655196669732,
12.));
#178531=CARTESIAN_POINT('Ctrl Pts',(-10.8521040371835,21.6805626556467,
12.));
#178532=CARTESIAN_POINT('Ctrl Pts',(-10.8689493334095,21.6956259856672,
12.));
#178533=CARTESIAN_POINT('Ctrl Pts',(-10.8859026661293,21.7107089564825,
12.));
#178534=CARTESIAN_POINT('Ctrl Pts',(-10.902963774734,21.7258108748873,12.));
#178535=CARTESIAN_POINT('Ctrl Pts',(-10.9201323997384,21.7409310548797,
12.));
#178536=CARTESIAN_POINT('Ctrl Pts',(-10.9374082827444,21.7560688175247,
12.));
#178537=CARTESIAN_POINT('Ctrl Pts',(-10.9547911664455,21.7712234908464,
12.));
#178538=CARTESIAN_POINT('Ctrl Pts',(-10.9722807946156,21.7863944097141,
12.));
#178539=CARTESIAN_POINT('Ctrl Pts',(-10.9898769120912,21.8015809157301,
12.));
#178540=CARTESIAN_POINT('Ctrl Pts',(-11.0075792647477,21.8167823571168,
12.));
#178541=CARTESIAN_POINT('Ctrl Pts',(-11.0253875994598,21.8319980886033,
12.));
#178542=CARTESIAN_POINT('Ctrl Pts',(-11.0433016640807,21.8472274713103,
12.));
#178543=CARTESIAN_POINT('Ctrl Pts',(-11.0613212074363,21.8624698726318,
12.));
#178544=CARTESIAN_POINT('Ctrl Pts',(-11.0794459793057,21.877724666119,12.));
#178545=CARTESIAN_POINT('Ctrl Pts',(-11.0976757303944,21.8929912313608,
12.));
#178546=CARTESIAN_POINT('Ctrl Pts',(-11.1160102123024,21.9082689538688,
12.));
#178547=CARTESIAN_POINT('Ctrl Pts',(-11.1344491774741,21.923557224952,12.));
#178548=CARTESIAN_POINT('Ctrl Pts',(-11.1529923792003,21.9388554416439,
12.));
#178549=CARTESIAN_POINT('Ctrl Pts',(-11.1716395716376,21.9541630066506,
12.));
#178550=CARTESIAN_POINT('Ctrl Pts',(-11.190390509811,21.9694793282914,12.));
#178551=CARTESIAN_POINT('Ctrl Pts',(-11.2092449496125,21.9848038204439,
12.));
#178552=CARTESIAN_POINT('Ctrl Pts',(-11.2282026477896,22.0001359024839,
12.));
#178553=CARTESIAN_POINT('Ctrl Pts',(-11.2472633619275,22.0154749992363,
12.));
#178554=CARTESIAN_POINT('Ctrl Pts',(-11.2664268504206,22.030820540835,12.));
#178555=CARTESIAN_POINT('Ctrl Pts',(-11.2856928724374,22.046171962566,12.));
#178556=CARTESIAN_POINT('Ctrl Pts',(-11.3050611878771,22.0615287047179,
12.));
#178557=CARTESIAN_POINT('Ctrl Pts',(-11.3245315573168,22.0768902124267,
12.));
#178558=CARTESIAN_POINT('Ctrl Pts',(-11.3441037419553,22.0922559355294,
12.));
#178559=CARTESIAN_POINT('Ctrl Pts',(-11.3637775035367,22.1076253283979,
12.));
#178560=CARTESIAN_POINT('Ctrl Pts',(-11.3835526044256,22.1229978500186,
12.));
#178561=CARTESIAN_POINT('Ctrl Pts',(-11.4034288076908,22.1383729640964,
12.));
#178562=CARTESIAN_POINT('Ctrl Pts',(-11.4234058771742,22.1537501391487,
12.));
#178563=CARTESIAN_POINT('Ctrl Pts',(-11.443483577557,22.1691288486096,12.));
#178564=CARTESIAN_POINT('Ctrl Pts',(-11.463661674411,22.184508570917,12.));
#178565=CARTESIAN_POINT('Ctrl Pts',(-11.483939934259,22.1998887896436,12.));
#178566=CARTESIAN_POINT('Ctrl Pts',(-11.5043181244242,22.2152689931022,
12.));
#178567=CARTESIAN_POINT('Ctrl Pts',(-11.5247960128477,22.2306486738901,
12.));
#178568=CARTESIAN_POINT('Ctrl Pts',(-11.5453733679121,22.2460273284654,
12.));
#178569=CARTESIAN_POINT('Ctrl Pts',(-11.5660499582403,22.2614044566898,
12.));
#178570=CARTESIAN_POINT('Ctrl Pts',(-11.5868255525188,22.2767795614348,
12.));
#178571=CARTESIAN_POINT('Ctrl Pts',(-11.6076999192357,22.2921521480356,
12.));
#178572=CARTESIAN_POINT('Ctrl Pts',(-11.6286728270009,22.3075217249049,
12.));
#178573=CARTESIAN_POINT('Ctrl Pts',(-11.6497440449857,22.3228878043976,
12.));
#178574=CARTESIAN_POINT('Ctrl Pts',(-11.6709133432985,22.3382499035619,
12.));
#178575=CARTESIAN_POINT('Ctrl Pts',(-11.6921804934056,22.3536075450029,
12.));
#178576=CARTESIAN_POINT('Ctrl Pts',(-11.7135452684532,22.3689602575491,
12.));
#178577=CARTESIAN_POINT('Ctrl Pts',(-11.7350074437961,22.3843075773899,
12.));
#178578=CARTESIAN_POINT('Ctrl Pts',(-11.7565667964764,22.3996490469191,
12.));
#178579=CARTESIAN_POINT('Ctrl Pts',(-11.7782231042039,22.4149842125008,
12.));
#178580=CARTESIAN_POINT('Ctrl Pts',(-11.7999761445173,22.430312622646,12.));
#178581=CARTESIAN_POINT('Ctrl Pts',(-11.8218256937889,22.4456338258735,
12.));
#178582=CARTESIAN_POINT('Ctrl Pts',(-11.8437715264487,22.4609473690471,
12.));
#178583=CARTESIAN_POINT('Ctrl Pts',(-11.8658134137019,22.4762527946702,
12.));
#178584=CARTESIAN_POINT('Ctrl Pts',(-11.8879511239943,22.4915496418485,
12.));
#178585=CARTESIAN_POINT('Ctrl Pts',(-11.9101844254557,22.5068374513973,
12.));
#178586=CARTESIAN_POINT('Ctrl Pts',(-11.9325130877803,22.5221157697883,
12.));
#178587=CARTESIAN_POINT('Ctrl Pts',(-11.9549368843997,22.5373841537307,
12.));
#178588=CARTESIAN_POINT('Ctrl Pts',(-11.9774555943496,22.5526421741158,
12.));
#178589=CARTESIAN_POINT('Ctrl Pts',(-12.0000690046695,22.5678894211181,
12.));
#178590=CARTESIAN_POINT('Ctrl Pts',(-12.0227769113127,22.5831255061282,
12.));
#178591=CARTESIAN_POINT('Ctrl Pts',(-12.0455791139128,22.5983500505644,
12.));
#178592=CARTESIAN_POINT('Ctrl Pts',(-12.0684754113862,22.6135626764898,
12.));
#178593=CARTESIAN_POINT('Ctrl Pts',(-12.0914655972823,22.6287629967056,
12.));
#178594=CARTESIAN_POINT('Ctrl Pts',(-12.1145494550383,22.6439506046605,
12.));
#178595=CARTESIAN_POINT('Ctrl Pts',(-12.1377267537145,22.6591250653965,
12.));
#178596=CARTESIAN_POINT('Ctrl Pts',(-12.1609972423099,22.6742859034944,
12.));
#178597=CARTESIAN_POINT('Ctrl Pts',(-12.1843606579262,22.6894326205037,
12.));
#178598=CARTESIAN_POINT('Ctrl Pts',(-12.2078167360284,22.7045647168747,
12.));
#178599=CARTESIAN_POINT('Ctrl Pts',(-12.2313652198061,22.7196817119374,
12.));
#178600=CARTESIAN_POINT('Ctrl Pts',(-12.2550058702395,22.7347831655287,
12.));
#178601=CARTESIAN_POINT('Ctrl Pts',(-12.2787384750742,22.7498686970069,
12.));
#178602=CARTESIAN_POINT('Ctrl Pts',(-12.3025628601792,22.764938010105,12.));
#178603=CARTESIAN_POINT('Ctrl Pts',(-12.3264788926075,22.7799908974768,
12.));
#178604=CARTESIAN_POINT('Ctrl Pts',(-12.3504864740319,22.795027221673,12.));
#178605=CARTESIAN_POINT('Ctrl Pts',(-12.374585536673,22.81004690224,12.));
#178606=CARTESIAN_POINT('Ctrl Pts',(-12.3939379378998,22.8220493007173,
12.));
#178607=CARTESIAN_POINT('Ctrl Pts',(-12.4084933766347,22.8310435872747,
12.));
#178608=CARTESIAN_POINT('Ctrl Pts',(-12.418215285186,22.8370364396459,12.));
#178609=CARTESIAN_POINT('Ctrl Pts',(-12.4230808101438,22.8400320311648,
12.));
#178610=CARTESIAN_POINT('',(-13.5685075571671,22.1787195904339,12.));
#178611=CARTESIAN_POINT('Origin',(0.,0.,12.));
#178612=CARTESIAN_POINT('',(-12.7689476255363,18.5896416359912,12.));
#178613=CARTESIAN_POINT('Ctrl Pts',(-13.5685075571671,22.1787195904339,
12.));
#178614=CARTESIAN_POINT('Ctrl Pts',(-13.5683460612942,22.1730081264608,
12.));
#178615=CARTESIAN_POINT('Ctrl Pts',(-13.5680170531805,22.1615922805008,
12.));
#178616=CARTESIAN_POINT('Ctrl Pts',(-13.5675054919061,22.1444897575194,
12.));
#178617=CARTESIAN_POINT('Ctrl Pts',(-13.5667873105359,22.1217288871975,
12.));
#178618=CARTESIAN_POINT('Ctrl Pts',(-13.5658294169284,22.0933486464593,
12.));
#178619=CARTESIAN_POINT('Ctrl Pts',(-13.5648113689033,22.0650393089609,
12.));
#178620=CARTESIAN_POINT('Ctrl Pts',(-13.5637332022473,22.0368009736295,
12.));
#178621=CARTESIAN_POINT('Ctrl Pts',(-13.5625949868333,22.0086337943449,
12.));
#178622=CARTESIAN_POINT('Ctrl Pts',(-13.5613968357561,21.9805379899168,
12.));
#178623=CARTESIAN_POINT('Ctrl Pts',(-13.5601389185257,21.9525138592813,
12.));
#178624=CARTESIAN_POINT('Ctrl Pts',(-13.5588214586604,21.9245617765769,
12.));
#178625=CARTESIAN_POINT('Ctrl Pts',(-13.5574447178424,21.8966821688824,
12.));
#178626=CARTESIAN_POINT('Ctrl Pts',(-13.5560089839385,21.8688754989365,
12.));
#178627=CARTESIAN_POINT('Ctrl Pts',(-13.5545145573031,21.8411422456075,
12.));
#178628=CARTESIAN_POINT('Ctrl Pts',(-13.5529617381573,21.8134828857967,
12.));
#178629=CARTESIAN_POINT('Ctrl Pts',(-13.551350812725,21.7858978745865,12.));
#178630=CARTESIAN_POINT('Ctrl Pts',(-13.5496820422211,21.7583876294554,
12.));
#178631=CARTESIAN_POINT('Ctrl Pts',(-13.5479556704481,21.7309525412281,
12.));
#178632=CARTESIAN_POINT('Ctrl Pts',(-13.5461719295048,21.7035929822955,
12.));
#178633=CARTESIAN_POINT('Ctrl Pts',(-13.5443310461526,21.6763093157699,
12.));
#178634=CARTESIAN_POINT('Ctrl Pts',(-13.5424332480699,21.6491019044648,
12.));
#178635=CARTESIAN_POINT('Ctrl Pts',(-13.5404787697792,21.6219711193946,
12.));
#178636=CARTESIAN_POINT('Ctrl Pts',(-13.5384678597195,21.5949173499013,
12.));
#178637=CARTESIAN_POINT('Ctrl Pts',(-13.536400779028,21.5679410019001,12.));
#178638=CARTESIAN_POINT('Ctrl Pts',(-13.5342777983215,21.5410424932503,
12.));
#178639=CARTESIAN_POINT('Ctrl Pts',(-13.5320991952138,21.5142222501666,
12.));
#178640=CARTESIAN_POINT('Ctrl Pts',(-13.5298652514355,21.4874807030468,
12.));
#178641=CARTESIAN_POINT('Ctrl Pts',(-13.5275762503555,21.4608182828697,
12.));
#178642=CARTESIAN_POINT('Ctrl Pts',(-13.5252324737802,21.4342354165259,
12.));
#178643=CARTESIAN_POINT('Ctrl Pts',(-13.5228342013516,21.4077325259324,
12.));
#178644=CARTESIAN_POINT('Ctrl Pts',(-13.5203817122504,21.3813100304973,
12.));
#178645=CARTESIAN_POINT('Ctrl Pts',(-13.5178752862466,21.3549683486222,
12.));
#178646=CARTESIAN_POINT('Ctrl Pts',(-13.5153152050555,21.328707899634,12.));
#178647=CARTESIAN_POINT('Ctrl Pts',(-13.5127017534971,21.3025291054235,
12.));
#178648=CARTESIAN_POINT('Ctrl Pts',(-13.5100352209205,21.2764323924442,
12.));
#178649=CARTESIAN_POINT('Ctrl Pts',(-13.5073159019452,21.250418192743,12.));
#178650=CARTESIAN_POINT('Ctrl Pts',(-13.5045440957404,21.2244869429332,
12.));
#178651=CARTESIAN_POINT('Ctrl Pts',(-13.5017201056088,21.1986390835828,
12.));
#178652=CARTESIAN_POINT('Ctrl Pts',(-13.4988442384491,21.1728750584175,
12.));
#178653=CARTESIAN_POINT('Ctrl Pts',(-13.4959168042934,21.1471953136209,
12.));
#178654=CARTESIAN_POINT('Ctrl Pts',(-13.4929381157778,21.1216002970207,
12.));
#178655=CARTESIAN_POINT('Ctrl Pts',(-13.4899084877717,21.0960904575046,
12.));
#178656=CARTESIAN_POINT('Ctrl Pts',(-13.4868282377191,21.0706662455199,
12.));
#178657=CARTESIAN_POINT('Ctrl Pts',(-13.4836976858912,21.0453281134245,
12.));
#178658=CARTESIAN_POINT('Ctrl Pts',(-13.4805171556822,21.0200765158884,
12.));
#178659=CARTESIAN_POINT('Ctrl Pts',(-13.4772869738879,20.9949119102592,
12.));
#178660=CARTESIAN_POINT('Ctrl Pts',(-13.4740074710086,20.9698347569476,
12.));
#178661=CARTESIAN_POINT('Ctrl Pts',(-13.4706789815166,20.9448455197557,
12.));
#178662=CARTESIAN_POINT('Ctrl Pts',(-13.4673018437717,20.9199446657583,
12.));
#178663=CARTESIAN_POINT('Ctrl Pts',(-13.4638763999725,20.8951326652158,
12.));
#178664=CARTESIAN_POINT('Ctrl Pts',(-13.4604029960983,20.8704099914641,
12.));
#178665=CARTESIAN_POINT('Ctrl Pts',(-13.4568819818631,20.8457771208083,
12.));
#178666=CARTESIAN_POINT('Ctrl Pts',(-13.4533137106667,20.821234532398,12.));
#178667=CARTESIAN_POINT('Ctrl Pts',(-13.4496985395637,20.7967827081228,
12.));
#178668=CARTESIAN_POINT('Ctrl Pts',(-13.4460368293689,20.7724221327609,
12.));
#178669=CARTESIAN_POINT('Ctrl Pts',(-13.4423289447561,20.7481532941014,
12.));
#178670=CARTESIAN_POINT('Ctrl Pts',(-13.4385752543663,20.7239766830675,
12.));
#178671=CARTESIAN_POINT('Ctrl Pts',(-13.4347761309154,20.6998927938288,
12.));
#178672=CARTESIAN_POINT('Ctrl Pts',(-13.4309319513119,20.6759021239102,
12.));
#178673=CARTESIAN_POINT('Ctrl Pts',(-13.427043096765,20.6520051742867,12.));
#178674=CARTESIAN_POINT('Ctrl Pts',(-13.4231099528178,20.6282024494234,
12.));
#178675=CARTESIAN_POINT('Ctrl Pts',(-13.4191329093932,20.6044944573151,
12.));
#178676=CARTESIAN_POINT('Ctrl Pts',(-13.4151123608411,20.5808817095155,
12.));
#178677=CARTESIAN_POINT('Ctrl Pts',(-13.4110487059912,20.557364721164,12.));
#178678=CARTESIAN_POINT('Ctrl Pts',(-13.4069423482076,20.5339440109957,
12.));
#178679=CARTESIAN_POINT('Ctrl Pts',(-13.4027936954529,20.5106201013755,
12.));
#178680=CARTESIAN_POINT('Ctrl Pts',(-13.3986031603716,20.4873935184041,
12.));
#178681=CARTESIAN_POINT('Ctrl Pts',(-13.3943711603739,20.4642647920038,
12.));
#178682=CARTESIAN_POINT('Ctrl Pts',(-13.3900981177254,20.4412344560007,
12.));
#178683=CARTESIAN_POINT('Ctrl Pts',(-13.3857844596387,20.4183030482002,
12.));
#178684=CARTESIAN_POINT('Ctrl Pts',(-13.3814306183721,20.3954711104504,
12.));
#178685=CARTESIAN_POINT('Ctrl Pts',(-13.377037031319,20.3727391887187,12.));
#178686=CARTESIAN_POINT('Ctrl Pts',(-13.3726041410869,20.3501078331818,
12.));
#178687=CARTESIAN_POINT('Ctrl Pts',(-13.3681323955828,20.3275775983032,
12.));
#178688=CARTESIAN_POINT('Ctrl Pts',(-13.3636222481017,20.3051490429049,
12.));
#178689=CARTESIAN_POINT('Ctrl Pts',(-13.3590741574194,20.2828227302337,
12.));
#178690=CARTESIAN_POINT('Ctrl Pts',(-13.3544885878886,20.2605992280117,
12.));
#178691=CARTESIAN_POINT('Ctrl Pts',(-13.3498660095382,20.2384791085354,
12.));
#178692=CARTESIAN_POINT('Ctrl Pts',(-13.3452068981763,20.2164629487855,
12.));
#178693=CARTESIAN_POINT('Ctrl Pts',(-13.3405117354969,20.1945513305233,
12.));
#178694=CARTESIAN_POINT('Ctrl Pts',(-13.3357810091903,20.1727448403818,
12.));
#178695=CARTESIAN_POINT('Ctrl Pts',(-13.3310152130565,20.1510440699477,
12.));
#178696=CARTESIAN_POINT('Ctrl Pts',(-13.3262148471228,20.1294496158405,
12.));
#178697=CARTESIAN_POINT('Ctrl Pts',(-13.3213804177588,20.1079620798377,
12.));
#178698=CARTESIAN_POINT('Ctrl Pts',(-13.3165124377963,20.0865820689883,
12.));
#178699=CARTESIAN_POINT('Ctrl Pts',(-13.3116114266514,20.0653101957188,
12.));
#178700=CARTESIAN_POINT('Ctrl Pts',(-13.3066779104515,20.0441470779345,
12.));
#178701=CARTESIAN_POINT('Ctrl Pts',(-13.3017124221639,20.0230933391039,
12.));
#178702=CARTESIAN_POINT('Ctrl Pts',(-13.296715501731,20.0021496083742,12.));
#178703=CARTESIAN_POINT('Ctrl Pts',(-13.2916876962098,19.9813165207174,
12.));
#178704=CARTESIAN_POINT('Ctrl Pts',(-13.2866295599152,19.9605947170589,
12.));
#178705=CARTESIAN_POINT('Ctrl Pts',(-13.2815416545663,19.9399848444019,
12.));
#178706=CARTESIAN_POINT('Ctrl Pts',(-13.2764245494354,19.9194875559419,
12.));
#178707=CARTESIAN_POINT('Ctrl Pts',(-13.2712788215015,19.8991035111739,
12.));
#178708=CARTESIAN_POINT('Ctrl Pts',(-13.2661050556128,19.8788333760571,
12.));
#178709=CARTESIAN_POINT('Ctrl Pts',(-13.2609038446525,19.8586778231711,
12.));
#178710=CARTESIAN_POINT('Ctrl Pts',(-13.2556757897085,19.8386375318632,
12.));
#178711=CARTESIAN_POINT('Ctrl Pts',(-13.2504215002458,19.8187131883919,
12.));
#178712=CARTESIAN_POINT('Ctrl Pts',(-13.2451415942809,19.7989054860501,
12.));
#178713=CARTESIAN_POINT('Ctrl Pts',(-13.239836698568,19.7792151253297,12.));
#178714=CARTESIAN_POINT('Ctrl Pts',(-13.2345074487968,19.7596428141176,
12.));
#178715=CARTESIAN_POINT('Ctrl Pts',(-13.2291544897902,19.7401892678701,
12.));
#178716=CARTESIAN_POINT('Ctrl Pts',(-13.2237784757065,19.7208552097867,
12.));
#178717=CARTESIAN_POINT('Ctrl Pts',(-13.2183800702431,19.7016413709678,
12.));
#178718=CARTESIAN_POINT('Ctrl Pts',(-13.2129599468478,19.6825484905812,
12.));
#178719=CARTESIAN_POINT('Ctrl Pts',(-13.2075187889522,19.6635773160924,
12.));
#178720=CARTESIAN_POINT('Ctrl Pts',(-13.202057290206,19.6447286034764,12.));
#178721=CARTESIAN_POINT('Ctrl Pts',(-13.196576154715,19.6260031174244,12.));
#178722=CARTESIAN_POINT('Ctrl Pts',(-13.1910760972818,19.6074016315421,
12.));
#178723=CARTESIAN_POINT('Ctrl Pts',(-13.1855578436479,19.5889249285351,
12.));
#178724=CARTESIAN_POINT('Ctrl Pts',(-13.1800221307683,19.5705738004682,
12.));
#178725=CARTESIAN_POINT('Ctrl Pts',(-13.1744697070918,19.5523490490254,
12.));
#178726=CARTESIAN_POINT('Ctrl Pts',(-13.1689013328432,19.5342514857564,
12.));
#178727=CARTESIAN_POINT('Ctrl Pts',(-13.1633177803097,19.5162819323207,
12.));
#178728=CARTESIAN_POINT('Ctrl Pts',(-13.1577198341238,19.498441220707,12.));
#178729=CARTESIAN_POINT('Ctrl Pts',(-13.1521082915846,19.4807301935256,
12.));
#178730=CARTESIAN_POINT('Ctrl Pts',(-13.1464839629966,19.463149704325,12.));
#178731=CARTESIAN_POINT('Ctrl Pts',(-13.140847672006,19.4457006178875,12.));
#178732=CARTESIAN_POINT('Ctrl Pts',(-13.1352002559439,19.4283838105265,
12.));
#178733=CARTESIAN_POINT('Ctrl Pts',(-13.1295425661635,19.4112001703561,
12.));
#178734=CARTESIAN_POINT('Ctrl Pts',(-13.1238754684177,19.3941505976267,
12.));
#178735=CARTESIAN_POINT('Ctrl Pts',(-13.118199843271,19.3772360051093,12.));
#178736=CARTESIAN_POINT('Ctrl Pts',(-13.1125165865021,19.3604573184516,
12.));
#178737=CARTESIAN_POINT('Ctrl Pts',(-13.1068266095186,19.3438154765395,
12.));
#178738=CARTESIAN_POINT('Ctrl Pts',(-13.1011308397592,19.3273114318268,
12.));
#178739=CARTESIAN_POINT('Ctrl Pts',(-13.095430221148,19.3109461507358,12.));
#178740=CARTESIAN_POINT('Ctrl Pts',(-13.089725714597,19.2947206141246,12.));
#178741=CARTESIAN_POINT('Ctrl Pts',(-13.0840182984949,19.2786358177198,
12.));
#178742=CARTESIAN_POINT('Ctrl Pts',(-13.0783089692118,19.2626927725596,
12.));
#178743=CARTESIAN_POINT('Ctrl Pts',(-13.0725987415856,19.2468925053988,
12.));
#178744=CARTESIAN_POINT('Ctrl Pts',(-13.0668886494791,19.2312360592031,
12.));
#178745=CARTESIAN_POINT('Ctrl Pts',(-13.0611797463913,19.2157244937141,
12.));
#178746=CARTESIAN_POINT('Ctrl Pts',(-13.0554731060537,19.2003588859771,
12.));
#178747=CARTESIAN_POINT('Ctrl Pts',(-13.0497698230442,19.1851403308825,
12.));
#178748=CARTESIAN_POINT('Ctrl Pts',(-13.0440710133775,19.1700699416625,
12.));
#178749=CARTESIAN_POINT('Ctrl Pts',(-13.0383778152072,19.1551488505233,
12.));
#178750=CARTESIAN_POINT('Ctrl Pts',(-13.0326913895841,19.1403782093389,
12.));
#178751=CARTESIAN_POINT('Ctrl Pts',(-13.0270129211976,19.1257591903099,
12.));
#178752=CARTESIAN_POINT('Ctrl Pts',(-13.0213436191326,19.1112929866308,
12.));
#178753=CARTESIAN_POINT('Ctrl Pts',(-13.0156847176093,19.0969808131225,
12.));
#178754=CARTESIAN_POINT('Ctrl Pts',(-13.0100374768785,19.0828239070482,
12.));
#178755=CARTESIAN_POINT('Ctrl Pts',(-13.0044031841381,19.0688235289437,
12.));
#178756=CARTESIAN_POINT('Ctrl Pts',(-12.9987831544502,19.0549809634355,
12.));
#178757=CARTESIAN_POINT('Ctrl Pts',(-12.9931787316515,19.0412975200398,
12.));
#178758=CARTESIAN_POINT('Ctrl Pts',(-12.9875912893003,19.0277745339908,
12.));
#178759=CARTESIAN_POINT('Ctrl Pts',(-12.9820222318716,19.0144133673348,
12.));
#178760=CARTESIAN_POINT('Ctrl Pts',(-12.9764729959205,19.0012154099791,
12.));
#178761=CARTESIAN_POINT('Ctrl Pts',(-12.9709450512747,18.9881820807585,
12.));
#178762=CARTESIAN_POINT('Ctrl Pts',(-12.9654399021869,18.9753148284475,
12.));
#178763=CARTESIAN_POINT('Ctrl Pts',(-12.9599590886319,18.9626151329229,
12.));
#178764=CARTESIAN_POINT('Ctrl Pts',(-12.9545041877377,18.9500845064715,
12.));
#178765=CARTESIAN_POINT('Ctrl Pts',(-12.9490768151821,18.9377244950435,
12.));
#178766=CARTESIAN_POINT('Ctrl Pts',(-12.9436786266105,18.9255366795195,
12.));
#178767=CARTESIAN_POINT('Ctrl Pts',(-12.9383113190375,18.9135226769465,
12.));
#178768=CARTESIAN_POINT('Ctrl Pts',(-12.9329766328185,18.9016841423403,
12.));
#178769=CARTESIAN_POINT('Ctrl Pts',(-12.9276763536373,18.8900227704889,
12.));
#178770=CARTESIAN_POINT('Ctrl Pts',(-12.9224123144982,18.8785402977527,
12.));
#178771=CARTESIAN_POINT('Ctrl Pts',(-12.9171863977045,18.8672385038326,
12.));
#178772=CARTESIAN_POINT('Ctrl Pts',(-12.9120005369063,18.8561192136198,
12.));
#178773=CARTESIAN_POINT('Ctrl Pts',(-12.9068567191854,18.8451842990984,
12.));
#178774=CARTESIAN_POINT('Ctrl Pts',(-12.9017569871738,18.834435681259,12.));
#178775=CARTESIAN_POINT('Ctrl Pts',(-12.8967034410755,18.8238753319128,
12.));
#178776=CARTESIAN_POINT('Ctrl Pts',(-12.8916982409935,18.813505275782,12.));
#178777=CARTESIAN_POINT('Ctrl Pts',(-12.8867436109546,18.8033275941943,
12.));
#178778=CARTESIAN_POINT('Ctrl Pts',(-12.8818418427475,18.7933444285868,
12.));
#178779=CARTESIAN_POINT('Ctrl Pts',(-12.8769952998095,18.7835579840477,
12.));
#178780=CARTESIAN_POINT('Ctrl Pts',(-12.872206421181,18.7739705329022,12.));
#178781=CARTESIAN_POINT('Ctrl Pts',(-12.8674777239653,18.7645844169564,
12.));
#178782=CARTESIAN_POINT('Ctrl Pts',(-12.8628118054171,18.7554020493887,
12.));
#178783=CARTESIAN_POINT('Ctrl Pts',(-12.8582113455646,18.7464259171251,
12.));
#178784=CARTESIAN_POINT('Ctrl Pts',(-12.8536791086316,18.7376585820854,
12.));
#178785=CARTESIAN_POINT('Ctrl Pts',(-12.8492179511591,18.7291026886554,
12.));
#178786=CARTESIAN_POINT('Ctrl Pts',(-12.8448308329494,18.7207609737702,
12.));
#178787=CARTESIAN_POINT('Ctrl Pts',(-12.8405208263431,18.7126362754445,
12.));
#178788=CARTESIAN_POINT('Ctrl Pts',(-12.8362911280361,18.7047315436294,
12.));
#178789=CARTESIAN_POINT('Ctrl Pts',(-12.8321450599789,18.6970498410172,
12.));
#178790=CARTESIAN_POINT('Ctrl Pts',(-12.8280860635231,18.6895943376171,
12.));
#178791=CARTESIAN_POINT('Ctrl Pts',(-12.8241176980017,18.6823683094139,
12.));
#178792=CARTESIAN_POINT('Ctrl Pts',(-12.8202436318474,18.6753751301092,
12.));
#178793=CARTESIAN_POINT('Ctrl Pts',(-12.8164676687362,18.6686182952799,
12.));
#178794=CARTESIAN_POINT('Ctrl Pts',(-12.8127937909631,18.6621014624746,
12.));
#178795=CARTESIAN_POINT('Ctrl Pts',(-12.8092261933858,18.6558284825773,
12.));
#178796=CARTESIAN_POINT('Ctrl Pts',(-12.805769331162,18.6498034438986,12.));
#178797=CARTESIAN_POINT('Ctrl Pts',(-12.8024278770152,18.6440306327456,
12.));
#178798=CARTESIAN_POINT('Ctrl Pts',(-12.7992066625264,18.63851447924,12.));
#178799=CARTESIAN_POINT('Ctrl Pts',(-12.7961106222251,18.6332595057006,
12.));
#178800=CARTESIAN_POINT('Ctrl Pts',(-12.7931447451555,18.6282702819371,
12.));
#178801=CARTESIAN_POINT('Ctrl Pts',(-12.7903142925234,18.6235516265575,
12.));
#178802=CARTESIAN_POINT('Ctrl Pts',(-12.7876249657834,18.6191087624752,
12.));
#178803=CARTESIAN_POINT('Ctrl Pts',(-12.7850831657901,18.6149475565188,
12.));
#178804=CARTESIAN_POINT('Ctrl Pts',(-12.7826959526925,18.6110744826219,
12.));
#178805=CARTESIAN_POINT('Ctrl Pts',(-12.7804705387658,18.6074961535723,
12.));
#178806=CARTESIAN_POINT('Ctrl Pts',(-12.7784139605066,18.6042190183704,
12.));
#178807=CARTESIAN_POINT('Ctrl Pts',(-12.7765325225081,18.6012488486709,
12.));
#178808=CARTESIAN_POINT('Ctrl Pts',(-12.7748328937638,18.598591752595,12.));
#178809=CARTESIAN_POINT('Ctrl Pts',(-12.7733231262108,18.5962551167772,
12.));
#178810=CARTESIAN_POINT('Ctrl Pts',(-12.7720142287172,18.5942490615407,
12.));
#178811=CARTESIAN_POINT('Ctrl Pts',(-12.7709195951156,18.5925859134579,
12.));
#178812=CARTESIAN_POINT('Ctrl Pts',(-12.7700520897173,18.5912775137806,
12.));
#178813=CARTESIAN_POINT('Ctrl Pts',(-12.7694215127919,18.5903328777227,
12.));
#178814=CARTESIAN_POINT('Ctrl Pts',(-12.769110348199,18.589871621843,12.));
#178815=CARTESIAN_POINT('Ctrl Pts',(-12.768986426692,18.5896919669165,12.));
#178816=CARTESIAN_POINT('Ctrl Pts',(-12.7689524524483,18.5896460962964,
12.));
#178817=CARTESIAN_POINT('Ctrl Pts',(-12.7689476255363,18.5896416359912,
12.));
#178818=CARTESIAN_POINT('',(-12.4528436808172,18.1294424696716,12.));
#178819=CARTESIAN_POINT('',(-6.08648437878338,8.86099361848466,12.));
#178820=CARTESIAN_POINT('',(-12.572596943457,17.4407513054162,12.));
#178821=CARTESIAN_POINT('Origin',(-12.8649829188862,17.846350172984,12.));
#178822=CARTESIAN_POINT('',(-13.5924445804218,16.6581946899465,12.));
#178823=CARTESIAN_POINT('Origin',(-4.50593605254675E-13,6.37232247690086E-13,
12.));
#178824=CARTESIAN_POINT('',(-14.2886635873976,16.7207683102834,12.));
#178825=CARTESIAN_POINT('Origin',(-13.9085479427572,17.0455945664569,12.));
#178826=CARTESIAN_POINT('',(-14.6513681262571,17.1452095830633,12.));
#178827=CARTESIAN_POINT('',(-7.32568406312854,8.57260479153162,12.));
#178828=CARTESIAN_POINT('',(-17.9112098770111,18.8464468996588,12.));
#178829=CARTESIAN_POINT('Ctrl Pts',(-14.6513681262571,17.1452095830633,
12.));
#178830=CARTESIAN_POINT('Ctrl Pts',(-14.651371185284,17.1452153999142,12.));
#178831=CARTESIAN_POINT('Ctrl Pts',(-14.6514066997188,17.1452600887039,
12.));
#178832=CARTESIAN_POINT('Ctrl Pts',(-14.6515481598057,17.1454262858045,
12.));
#178833=CARTESIAN_POINT('Ctrl Pts',(-14.65191316345,17.1458462295273,12.));
#178834=CARTESIAN_POINT('Ctrl Pts',(-14.6526624064978,17.1466998098673,
12.));
#178835=CARTESIAN_POINT('Ctrl Pts',(-14.6537016966188,17.1478763944909,
12.));
#178836=CARTESIAN_POINT('Ctrl Pts',(-14.6550248622813,17.1493641837556,
12.));
#178837=CARTESIAN_POINT('Ctrl Pts',(-14.6566237952435,17.1511476869495,
12.));
#178838=CARTESIAN_POINT('Ctrl Pts',(-14.6584900555301,17.1532107762719,
12.));
#178839=CARTESIAN_POINT('Ctrl Pts',(-14.660616716964,17.1555401986403,12.));
#178840=CARTESIAN_POINT('Ctrl Pts',(-14.662998728599,17.1581262646789,12.));
#178841=CARTESIAN_POINT('Ctrl Pts',(-14.6656319165057,17.1609609517369,
12.));
#178842=CARTESIAN_POINT('Ctrl Pts',(-14.6685123374424,17.1640366762304,
12.));
#178843=CARTESIAN_POINT('Ctrl Pts',(-14.6716355833321,17.1673449723019,
12.));
#178844=CARTESIAN_POINT('Ctrl Pts',(-14.6749971333867,17.1708771619129,
12.));
#178845=CARTESIAN_POINT('Ctrl Pts',(-14.6785925615676,17.1746247499057,
12.));
#178846=CARTESIAN_POINT('Ctrl Pts',(-14.6824178576167,17.1785800350827,
12.));
#178847=CARTESIAN_POINT('Ctrl Pts',(-14.6864694522319,17.182736158472,12.));
#178848=CARTESIAN_POINT('Ctrl Pts',(-14.6907440526958,17.1870867909918,
12.));
#178849=CARTESIAN_POINT('Ctrl Pts',(-14.6952385361706,17.1916259308415,
12.));
#178850=CARTESIAN_POINT('Ctrl Pts',(-14.699949811582,17.1963476411694,12.));
#178851=CARTESIAN_POINT('Ctrl Pts',(-14.7048748502663,17.2012461084268,
12.));
#178852=CARTESIAN_POINT('Ctrl Pts',(-14.7100107213586,17.2063157097316,
12.));
#178853=CARTESIAN_POINT('Ctrl Pts',(-14.7153546289338,17.2115510835988,
12.));
#178854=CARTESIAN_POINT('Ctrl Pts',(-14.7209039390326,17.2169471814255,
12.));
#178855=CARTESIAN_POINT('Ctrl Pts',(-14.7266561494282,17.2224992099666,
12.));
#178856=CARTESIAN_POINT('Ctrl Pts',(-14.7326088681163,17.2282025904314,
12.));
#178857=CARTESIAN_POINT('Ctrl Pts',(-14.7387597858117,17.2340529062077,
12.));
#178858=CARTESIAN_POINT('Ctrl Pts',(-14.7451066593793,17.2400458713566,
12.));
#178859=CARTESIAN_POINT('Ctrl Pts',(-14.7516473175125,17.2461773413289,
12.));
#178860=CARTESIAN_POINT('Ctrl Pts',(-14.7583796616617,17.2524433146837,
12.));
#178861=CARTESIAN_POINT('Ctrl Pts',(-14.7653016697589,17.2588399401464,
12.));
#178862=CARTESIAN_POINT('Ctrl Pts',(-14.7724113956728,17.2653635155317,
12.));
#178863=CARTESIAN_POINT('Ctrl Pts',(-14.7797069617802,17.2720104735192,
12.));
#178864=CARTESIAN_POINT('Ctrl Pts',(-14.787186553128,17.278777370485,12.));
#178865=CARTESIAN_POINT('Ctrl Pts',(-14.7948484105253,17.28566087332,12.));
#178866=CARTESIAN_POINT('Ctrl Pts',(-14.8026908254281,17.2926577496519,
12.));
#178867=CARTESIAN_POINT('Ctrl Pts',(-14.8107121391038,17.2997648661483,
12.));
#178868=CARTESIAN_POINT('Ctrl Pts',(-14.8189107410161,17.3069791853705,
12.));
#178869=CARTESIAN_POINT('Ctrl Pts',(-14.8272850675375,17.3142977632656,
12.));
#178870=CARTESIAN_POINT('Ctrl Pts',(-14.8358336004193,17.3217177462096,
12.));
#178871=CARTESIAN_POINT('Ctrl Pts',(-14.8445548643504,17.3292363662601,
12.));
#178872=CARTESIAN_POINT('Ctrl Pts',(-14.8534474245433,17.336850936485,12.));
#178873=CARTESIAN_POINT('Ctrl Pts',(-14.8625098843419,17.3445588463477,
12.));
#178874=CARTESIAN_POINT('Ctrl Pts',(-14.8717408826958,17.3523575568648,
12.));
#178875=CARTESIAN_POINT('Ctrl Pts',(-14.8811390927424,17.3602445978163,
12.));
#178876=CARTESIAN_POINT('Ctrl Pts',(-14.8907032205789,17.3682175653236,
12.));
#178877=CARTESIAN_POINT('Ctrl Pts',(-14.9004320039609,17.3762741193075,
12.));
#178878=CARTESIAN_POINT('Ctrl Pts',(-14.9103242110057,17.3844119809823,
12.));
#178879=CARTESIAN_POINT('Ctrl Pts',(-14.9203786389343,17.3926289303987,
12.));
#178880=CARTESIAN_POINT('Ctrl Pts',(-14.9305941128758,17.400922804075,12.));
#178881=CARTESIAN_POINT('Ctrl Pts',(-14.940969484645,17.4092914926071,12.));
#178882=CARTESIAN_POINT('Ctrl Pts',(-14.9515036315142,17.4177329382827,
12.));
#178883=CARTESIAN_POINT('Ctrl Pts',(-14.9621954549825,17.4262451327088,
12.));
#178884=CARTESIAN_POINT('Ctrl Pts',(-14.973043879945,17.4348261151395,12.));
#178885=CARTESIAN_POINT('Ctrl Pts',(-14.9840478538357,17.4434739707773,
12.));
#178886=CARTESIAN_POINT('Ctrl Pts',(-14.9952063457779,17.4521868291005,
12.));
#178887=CARTESIAN_POINT('Ctrl Pts',(-15.0065183456922,17.4609628621419,
12.));
#178888=CARTESIAN_POINT('Ctrl Pts',(-15.0179828635087,17.4698002829357,
12.));
#178889=CARTESIAN_POINT('Ctrl Pts',(-15.029598928488,17.4786973441417,12.));
#178890=CARTESIAN_POINT('Ctrl Pts',(-15.0413655884993,17.4876523366178,
12.));
#178891=CARTESIAN_POINT('Ctrl Pts',(-15.0532819093085,17.4966635880246,
12.));
#178892=CARTESIAN_POINT('Ctrl Pts',(-15.0653469738307,17.5057294613877,
12.));
#178893=CARTESIAN_POINT('Ctrl Pts',(-15.0775598815749,17.5148483539687,
12.));
#178894=CARTESIAN_POINT('Ctrl Pts',(-15.0899197481082,17.524018696179,12.));
#178895=CARTESIAN_POINT('Ctrl Pts',(-15.1024257045033,17.5332389504829,
12.));
#178896=CARTESIAN_POINT('Ctrl Pts',(-15.1150768967728,17.5425076102963,
12.));
#178897=CARTESIAN_POINT('Ctrl Pts',(-15.1278724853138,17.5518231989117,
12.));
#178898=CARTESIAN_POINT('Ctrl Pts',(-15.1408116444876,17.5611842686192,
12.));
#178899=CARTESIAN_POINT('Ctrl Pts',(-15.1538935621714,17.5705893998029,
12.));
#178900=CARTESIAN_POINT('Ctrl Pts',(-15.1671174393137,17.580037200054,12.));
#178901=CARTESIAN_POINT('Ctrl Pts',(-15.1804824894605,17.5895263032595,
12.));
#178902=CARTESIAN_POINT('Ctrl Pts',(-15.1939879383268,17.5990553687599,
12.));
#178903=CARTESIAN_POINT('Ctrl Pts',(-15.2076330234686,17.60862308065,12.));
#178904=CARTESIAN_POINT('Ctrl Pts',(-15.2214169939199,17.6182281470468,
12.));
#178905=CARTESIAN_POINT('Ctrl Pts',(-15.2353391098366,17.6278692993764,
12.));
#178906=CARTESIAN_POINT('Ctrl Pts',(-15.2493986421092,17.6375452916369,
12.));
#178907=CARTESIAN_POINT('Ctrl Pts',(-15.2635948720292,17.6472548997328,
12.));
#178908=CARTESIAN_POINT('Ctrl Pts',(-15.2779270910239,17.6569969209,12.));
#178909=CARTESIAN_POINT('Ctrl Pts',(-15.2923946003598,17.6667701731041,
12.));
#178910=CARTESIAN_POINT('Ctrl Pts',(-15.3069967108501,17.676573494456,12.));
#178911=CARTESIAN_POINT('Ctrl Pts',(-15.3217327425338,17.6864057426052,
12.));
#178912=CARTESIAN_POINT('Ctrl Pts',(-15.3366020244066,17.6962657941983,
12.));
#178913=CARTESIAN_POINT('Ctrl Pts',(-15.351603894206,17.7061525444042,12.));
#178914=CARTESIAN_POINT('Ctrl Pts',(-15.3667376981699,17.7160649064206,
12.));
#178915=CARTESIAN_POINT('Ctrl Pts',(-15.3820027907967,17.7260018109924,
12.));
#178916=CARTESIAN_POINT('Ctrl Pts',(-15.3973985345802,17.7359622059149,
12.));
#178917=CARTESIAN_POINT('Ctrl Pts',(-15.4129242997837,17.7459450555812,
12.));
#178918=CARTESIAN_POINT('Ctrl Pts',(-15.4285794642668,17.7559493405881,
12.));
#178919=CARTESIAN_POINT('Ctrl Pts',(-15.4443634132869,17.7659740573265,
12.));
#178920=CARTESIAN_POINT('Ctrl Pts',(-15.4602755393017,17.7760182175815,
12.));
#178921=CARTESIAN_POINT('Ctrl Pts',(-15.4763152417497,17.7860808481219,
12.));
#178922=CARTESIAN_POINT('Ctrl Pts',(-15.4924819268517,17.7961609903148,
12.));
#178923=CARTESIAN_POINT('Ctrl Pts',(-15.5087750074718,17.8062576997952,
12.));
#178924=CARTESIAN_POINT('Ctrl Pts',(-15.5251939029552,17.8163700461256,
12.));
#178925=CARTESIAN_POINT('Ctrl Pts',(-15.541738038964,17.8264971124606,12.));
#178926=CARTESIAN_POINT('Ctrl Pts',(-15.5584068472982,17.8366379952085,
12.));
#178927=CARTESIAN_POINT('Ctrl Pts',(-15.5751997657163,17.8467918036987,
12.));
#178928=CARTESIAN_POINT('Ctrl Pts',(-15.5921162378192,17.8569576599006,
12.));
#178929=CARTESIAN_POINT('Ctrl Pts',(-15.609155712921,17.8671346981394,12.));
#178930=CARTESIAN_POINT('Ctrl Pts',(-15.6263176459108,17.8773220648125,
12.));
#178931=CARTESIAN_POINT('Ctrl Pts',(-15.6436014971084,17.8875189181091,
12.));
#178932=CARTESIAN_POINT('Ctrl Pts',(-15.661006732103,17.897724427724,12.));
#178933=CARTESIAN_POINT('Ctrl Pts',(-15.678532821646,17.9079377746111,12.));
#178934=CARTESIAN_POINT('Ctrl Pts',(-15.6961792415522,17.9181581507455,
12.));
#178935=CARTESIAN_POINT('Ctrl Pts',(-15.7139454725838,17.9283847588835,
12.));
#178936=CARTESIAN_POINT('Ctrl Pts',(-15.7318310003335,17.9386168123262,
12.));
#178937=CARTESIAN_POINT('Ctrl Pts',(-15.749835315086,17.9488535346781,12.));
#178938=CARTESIAN_POINT('Ctrl Pts',(-15.7679579117077,17.9590941596242,
12.));
#178939=CARTESIAN_POINT('Ctrl Pts',(-15.7861982895724,17.9693379307303,
12.));
#178940=CARTESIAN_POINT('Ctrl Pts',(-15.8045559524676,17.9795841012386,
12.));
#178941=CARTESIAN_POINT('Ctrl Pts',(-15.8230304084962,17.9898319338664,
12.));
#178942=CARTESIAN_POINT('Ctrl Pts',(-15.8416211699679,18.0000807006052,
12.));
#178943=CARTESIAN_POINT('Ctrl Pts',(-15.8603277532831,18.0103296825205,
12.));
#178944=CARTESIAN_POINT('Ctrl Pts',(-15.8791496788683,18.0205781695769,
12.));
#178945=CARTESIAN_POINT('Ctrl Pts',(-15.8980864711042,18.0308254604636,
12.));
#178946=CARTESIAN_POINT('Ctrl Pts',(-15.9171376582436,18.0410708624208,
12.));
#178947=CARTESIAN_POINT('Ctrl Pts',(-15.9363027723244,18.0513136910691,
12.));
#178948=CARTESIAN_POINT('Ctrl Pts',(-15.9555813490644,18.0615532702359,
12.));
#178949=CARTESIAN_POINT('Ctrl Pts',(-15.9749729277846,18.0717889317958,
12.));
#178950=CARTESIAN_POINT('Ctrl Pts',(-15.9944770513613,18.0820200155236,
12.));
#178951=CARTESIAN_POINT('Ctrl Pts',(-16.014093266161,18.0922458689462,12.));
#178952=CARTESIAN_POINT('Ctrl Pts',(-16.0338211219693,18.1024658471966,
12.));
#178953=CARTESIAN_POINT('Ctrl Pts',(-16.0536601719126,18.112679312869,12.));
#178954=CARTESIAN_POINT('Ctrl Pts',(-16.0736099723668,18.1228856358751,
12.));
#178955=CARTESIAN_POINT('Ctrl Pts',(-16.0936700829112,18.1330841933105,
12.));
#178956=CARTESIAN_POINT('Ctrl Pts',(-16.1138400662794,18.1432743693235,
12.));
#178957=CARTESIAN_POINT('Ctrl Pts',(-16.1341194882988,18.1534555549852,
12.));
#178958=CARTESIAN_POINT('Ctrl Pts',(-16.154507917826,18.1636271481615,12.));
#178959=CARTESIAN_POINT('Ctrl Pts',(-16.1750049266671,18.1737885533849,
12.));
#178960=CARTESIAN_POINT('Ctrl Pts',(-16.1956100895073,18.1839391817331,
12.));
#178961=CARTESIAN_POINT('Ctrl Pts',(-16.2163229838875,18.1940784507229,
12.));
#178962=CARTESIAN_POINT('Ctrl Pts',(-16.2371431901638,18.2042057842035,
12.));
#178963=CARTESIAN_POINT('Ctrl Pts',(-16.2580702914615,18.2143206122529,
12.));
#178964=CARTESIAN_POINT('Ctrl Pts',(-16.2791038736223,18.2244223710745,
12.));
#178965=CARTESIAN_POINT('Ctrl Pts',(-16.3002435251378,18.2345105028982,
12.));
#178966=CARTESIAN_POINT('Ctrl Pts',(-16.3214888370987,18.2445844558741,
12.));
#178967=CARTESIAN_POINT('Ctrl Pts',(-16.3428394031589,18.2546436839608,
12.));
#178968=CARTESIAN_POINT('Ctrl Pts',(-16.3642948194868,18.2646876468169,
12.));
#178969=CARTESIAN_POINT('Ctrl Pts',(-16.385854684708,18.2747158096934,12.));
#178970=CARTESIAN_POINT('Ctrl Pts',(-16.4075185998455,18.2847276433309,
12.));
#178971=CARTESIAN_POINT('Ctrl Pts',(-16.4292861682379,18.294722623851,12.));
#178972=CARTESIAN_POINT('Ctrl Pts',(-16.4511569955233,18.304700232686,12.));
#178973=CARTESIAN_POINT('Ctrl Pts',(-16.4731306896441,18.3146599565231,
12.));
#178974=CARTESIAN_POINT('Ctrl Pts',(-16.4952068608345,18.3246012872469,
12.));
#178975=CARTESIAN_POINT('Ctrl Pts',(-16.5173851216045,18.3345237218864,
12.));
#178976=CARTESIAN_POINT('Ctrl Pts',(-16.5396650867139,18.34442676256,12.));
#178977=CARTESIAN_POINT('Ctrl Pts',(-16.5620463731413,18.354309916433,12.));
#178978=CARTESIAN_POINT('Ctrl Pts',(-16.5845286000217,18.3641726955889,
12.));
#178979=CARTESIAN_POINT('Ctrl Pts',(-16.607111388571,18.3740146168879,12.));
#178980=CARTESIAN_POINT('Ctrl Pts',(-16.6297943620056,18.3838352018327,
12.));
#178981=CARTESIAN_POINT('Ctrl Pts',(-16.6525771454513,18.3936339764332,
12.));
#178982=CARTESIAN_POINT('Ctrl Pts',(-16.6754593658513,18.403410471079,12.));
#178983=CARTESIAN_POINT('Ctrl Pts',(-16.6984406518491,18.413164220399,12.));
#178984=CARTESIAN_POINT('Ctrl Pts',(-16.7215206338818,18.4228947633187,
12.));
#178985=CARTESIAN_POINT('Ctrl Pts',(-16.7446989442882,18.4326016431392,
12.));
#178986=CARTESIAN_POINT('Ctrl Pts',(-16.7679752173992,18.44228440761,12.));
#178987=CARTESIAN_POINT('Ctrl Pts',(-16.791349089629,18.4519426090123,12.));
#178988=CARTESIAN_POINT('Ctrl Pts',(-16.8148201995472,18.4615758042305,
12.));
#178989=CARTESIAN_POINT('Ctrl Pts',(-16.8383881879709,18.4711835548623,
12.));
#178990=CARTESIAN_POINT('Ctrl Pts',(-16.8620526977171,18.480765426877,12.));
#178991=CARTESIAN_POINT('Ctrl Pts',(-16.8858133733088,18.4903209902227,
12.));
#178992=CARTESIAN_POINT('Ctrl Pts',(-16.9096698606943,18.499849818462,12.));
#178993=CARTESIAN_POINT('Ctrl Pts',(-16.9336218069353,18.5093514883835,
12.));
#178994=CARTESIAN_POINT('Ctrl Pts',(-16.9576688599339,18.5188255796659,
12.));
#178995=CARTESIAN_POINT('Ctrl Pts',(-16.981810668038,18.5282716744197,12.));
#178996=CARTESIAN_POINT('Ctrl Pts',(-17.0060468805097,18.5376893576961,
12.));
#178997=CARTESIAN_POINT('Ctrl Pts',(-17.0303771481738,18.547078218209,12.));
#178998=CARTESIAN_POINT('Ctrl Pts',(-17.0548011239751,18.556437848963,12.));
#178999=CARTESIAN_POINT('Ctrl Pts',(-17.0793184636079,18.5657678479789,
12.));
#179000=CARTESIAN_POINT('Ctrl Pts',(-17.1039288260001,18.5750678188542,
12.));
#179001=CARTESIAN_POINT('Ctrl Pts',(-17.1286318741183,18.5843373717247,
12.));
#179002=CARTESIAN_POINT('Ctrl Pts',(-17.1534272741643,18.5935761222825,
12.));
#179003=CARTESIAN_POINT('Ctrl Pts',(-17.1783146940127,18.6027836898817,
12.));
#179004=CARTESIAN_POINT('Ctrl Pts',(-17.2032938019284,18.6119596959949,
12.));
#179005=CARTESIAN_POINT('Ctrl Pts',(-17.2283642650518,18.6211037624038,
12.));
#179006=CARTESIAN_POINT('Ctrl Pts',(-17.2535257482187,18.6302155097943,
12.));
#179007=CARTESIAN_POINT('Ctrl Pts',(-17.2787779120213,18.6392945554748,
12.));
#179008=CARTESIAN_POINT('Ctrl Pts',(-17.3041204135074,18.6483405141865,
12.));
#179009=CARTESIAN_POINT('Ctrl Pts',(-17.3295529098618,18.6573530024033,
12.));
#179010=CARTESIAN_POINT('Ctrl Pts',(-17.3550750612443,18.6663316416582,
12.));
#179011=CARTESIAN_POINT('Ctrl Pts',(-17.3806865340747,18.6752760624052,
12.));
#179012=CARTESIAN_POINT('Ctrl Pts',(-17.4063870038562,18.6841859073471,
12.));
#179013=CARTESIAN_POINT('Ctrl Pts',(-17.4321761588142,18.6930608357409,
12.));
#179014=CARTESIAN_POINT('Ctrl Pts',(-17.4580537012753,18.70190052503,12.));
#179015=CARTESIAN_POINT('Ctrl Pts',(-17.4840193397162,18.7107046613912,
12.));
#179016=CARTESIAN_POINT('Ctrl Pts',(-17.5100727820876,18.7194729318098,
12.));
#179017=CARTESIAN_POINT('Ctrl Pts',(-17.5362137287593,18.7282050157138,
12.));
#179018=CARTESIAN_POINT('Ctrl Pts',(-17.5624418653245,18.7369005764553,
12.));
#179019=CARTESIAN_POINT('Ctrl Pts',(-17.5887568561371,18.7455592536687,
12.));
#179020=CARTESIAN_POINT('Ctrl Pts',(-17.6151583357012,18.7541806530984,
12.));
#179021=CARTESIAN_POINT('Ctrl Pts',(-17.6416459210681,18.762764361321,12.));
#179022=CARTESIAN_POINT('Ctrl Pts',(-17.6682192274236,18.7713099642754,
12.));
#179023=CARTESIAN_POINT('Ctrl Pts',(-17.6948778823014,18.7798170641374,
12.));
#179024=CARTESIAN_POINT('Ctrl Pts',(-17.7216215409035,18.7882852976049,
12.));
#179025=CARTESIAN_POINT('Ctrl Pts',(-17.7484498996905,18.7967143519419,
12.));
#179026=CARTESIAN_POINT('Ctrl Pts',(-17.7753627137853,18.8051039860448,
12.));
#179027=CARTESIAN_POINT('Ctrl Pts',(-17.8023598011057,18.8134540340417,
12.));
#179028=CARTESIAN_POINT('Ctrl Pts',(-17.8294410311006,18.8217643886157,
12.));
#179029=CARTESIAN_POINT('Ctrl Pts',(-17.8566063174771,18.8300349895974,
12.));
#179030=CARTESIAN_POINT('Ctrl Pts',(-17.8784057509356,18.8366196462581,
12.));
#179031=CARTESIAN_POINT('Ctrl Pts',(-17.8947931177807,18.8415402351786,
12.));
#179032=CARTESIAN_POINT('Ctrl Pts',(-17.9057348246595,18.8448126709691,
12.));
#179033=CARTESIAN_POINT('Ctrl Pts',(-17.9112098770111,18.8464468996588,
12.));
#179034=CARTESIAN_POINT('',(-18.8464468996588,17.9112098770111,12.));
#179035=CARTESIAN_POINT('Origin',(0.,0.,12.));
#179036=CARTESIAN_POINT('',(-17.1452095830633,14.6513681262571,12.));
#179037=CARTESIAN_POINT('Ctrl Pts',(-18.8464468996588,17.9112098770111,
12.));
#179038=CARTESIAN_POINT('Ctrl Pts',(-18.8448126709726,17.9057348246611,
12.));
#179039=CARTESIAN_POINT('Ctrl Pts',(-18.8415402351882,17.8947931177853,
12.));
#179040=CARTESIAN_POINT('Ctrl Pts',(-18.8366196462746,17.8784057509434,
12.));
#179041=CARTESIAN_POINT('Ctrl Pts',(-18.8300349896187,17.8566063174871,
12.));
#179042=CARTESIAN_POINT('Ctrl Pts',(-18.8217643886368,17.8294410311105,
12.));
#179043=CARTESIAN_POINT('Ctrl Pts',(-18.8134540340581,17.8023598011135,
12.));
#179044=CARTESIAN_POINT('Ctrl Pts',(-18.8051039860543,17.7753627137898,
12.));
#179045=CARTESIAN_POINT('Ctrl Pts',(-18.7967143519444,17.7484498996916,
12.));
#179046=CARTESIAN_POINT('Ctrl Pts',(-18.7882852976016,17.7216215409019,
12.));
#179047=CARTESIAN_POINT('Ctrl Pts',(-18.7798170641305,17.6948778822981,
12.));
#179048=CARTESIAN_POINT('Ctrl Pts',(-18.7713099642673,17.6682192274197,
12.));
#179049=CARTESIAN_POINT('Ctrl Pts',(-18.7627643613139,17.6416459210646,
12.));
#179050=CARTESIAN_POINT('Ctrl Pts',(-18.7541806530935,17.6151583356988,
12.));
#179051=CARTESIAN_POINT('Ctrl Pts',(-18.7455592536667,17.5887568561361,
12.));
#179052=CARTESIAN_POINT('Ctrl Pts',(-18.7369005764558,17.5624418653248,
12.));
#179053=CARTESIAN_POINT('Ctrl Pts',(-18.728205015716,17.5362137287604,12.));
#179054=CARTESIAN_POINT('Ctrl Pts',(-18.7194729318128,17.5100727820891,
12.));
#179055=CARTESIAN_POINT('Ctrl Pts',(-18.7107046613941,17.4840193397176,
12.));
#179056=CARTESIAN_POINT('Ctrl Pts',(-18.7019005250322,17.4580537012764,
12.));
#179057=CARTESIAN_POINT('Ctrl Pts',(-18.6930608357421,17.4321761588148,
12.));
#179058=CARTESIAN_POINT('Ctrl Pts',(-18.6841859073472,17.4063870038563,
12.));
#179059=CARTESIAN_POINT('Ctrl Pts',(-18.6752760624045,17.3806865340744,
12.));
#179060=CARTESIAN_POINT('Ctrl Pts',(-18.6663316416569,17.3550750612438,
12.));
#179061=CARTESIAN_POINT('Ctrl Pts',(-18.6573530024019,17.3295529098612,
12.));
#179062=CARTESIAN_POINT('Ctrl Pts',(-18.6483405141853,17.3041204135069,
12.));
#179063=CARTESIAN_POINT('Ctrl Pts',(-18.639294555474,17.278777912021,12.));
#179064=CARTESIAN_POINT('Ctrl Pts',(-18.630215509794,17.2535257482186,12.));
#179065=CARTESIAN_POINT('Ctrl Pts',(-18.6211037624041,17.2283642650519,
12.));
#179066=CARTESIAN_POINT('Ctrl Pts',(-18.6119596959957,17.2032938019288,
12.));
#179067=CARTESIAN_POINT('Ctrl Pts',(-18.6027836898826,17.1783146940131,
12.));
#179068=CARTESIAN_POINT('Ctrl Pts',(-18.5935761222833,17.1534272741646,
12.));
#179069=CARTESIAN_POINT('Ctrl Pts',(-18.5843373717253,17.1286318741185,
12.));
#179070=CARTESIAN_POINT('Ctrl Pts',(-18.5750678188543,17.1039288260001,
12.));
#179071=CARTESIAN_POINT('Ctrl Pts',(-18.5657678479788,17.0793184636079,
12.));
#179072=CARTESIAN_POINT('Ctrl Pts',(-18.5564378489628,17.0548011239751,
12.));
#179073=CARTESIAN_POINT('Ctrl Pts',(-18.5470782182089,17.030377148174,12.));
#179074=CARTESIAN_POINT('Ctrl Pts',(-18.5376893576961,17.0060468805099,
12.));
#179075=CARTESIAN_POINT('Ctrl Pts',(-18.5282716744198,16.9818106680382,
12.));
#179076=CARTESIAN_POINT('Ctrl Pts',(-18.518825579666,16.957668859934,12.));
#179077=CARTESIAN_POINT('Ctrl Pts',(-18.5093514883835,16.9336218069353,
12.));
#179078=CARTESIAN_POINT('Ctrl Pts',(-18.4998498184619,16.9096698606942,
12.));
#179079=CARTESIAN_POINT('Ctrl Pts',(-18.4903209902226,16.8858133733086,
12.));
#179080=CARTESIAN_POINT('Ctrl Pts',(-18.4807654268769,16.8620526977169,
12.));
#179081=CARTESIAN_POINT('Ctrl Pts',(-18.4711835548622,16.8383881879707,
12.));
#179082=CARTESIAN_POINT('Ctrl Pts',(-18.4615758042305,16.8148201995472,
12.));
#179083=CARTESIAN_POINT('Ctrl Pts',(-18.4519426090124,16.791349089629,12.));
#179084=CARTESIAN_POINT('Ctrl Pts',(-18.4422844076099,16.7679752173992,
12.));
#179085=CARTESIAN_POINT('Ctrl Pts',(-18.4326016431392,16.7446989442882,
12.));
#179086=CARTESIAN_POINT('Ctrl Pts',(-18.4228947633186,16.7215206338818,
12.));
#179087=CARTESIAN_POINT('Ctrl Pts',(-18.413164220399,16.698440651849,12.));
#179088=CARTESIAN_POINT('Ctrl Pts',(-18.4034104710789,16.6754593658513,
12.));
#179089=CARTESIAN_POINT('Ctrl Pts',(-18.3936339764332,16.6525771454513,
12.));
#179090=CARTESIAN_POINT('Ctrl Pts',(-18.3838352018327,16.6297943620056,
12.));
#179091=CARTESIAN_POINT('Ctrl Pts',(-18.3740146168879,16.6071113885711,
12.));
#179092=CARTESIAN_POINT('Ctrl Pts',(-18.364172695589,16.5845286000218,12.));
#179093=CARTESIAN_POINT('Ctrl Pts',(-18.3543099164331,16.5620463731414,
12.));
#179094=CARTESIAN_POINT('Ctrl Pts',(-18.3444267625601,16.5396650867139,
12.));
#179095=CARTESIAN_POINT('Ctrl Pts',(-18.3345237218864,16.5173851216045,
12.));
#179096=CARTESIAN_POINT('Ctrl Pts',(-18.3246012872468,16.4952068608344,
12.));
#179097=CARTESIAN_POINT('Ctrl Pts',(-18.3146599565229,16.4731306896439,
12.));
#179098=CARTESIAN_POINT('Ctrl Pts',(-18.3047002326858,16.4511569955231,
12.));
#179099=CARTESIAN_POINT('Ctrl Pts',(-18.2947226238509,16.4292861682377,
12.));
#179100=CARTESIAN_POINT('Ctrl Pts',(-18.2847276433308,16.4075185998454,
12.));
#179101=CARTESIAN_POINT('Ctrl Pts',(-18.2747158096934,16.385854684708,12.));
#179102=CARTESIAN_POINT('Ctrl Pts',(-18.2646876468169,16.3642948194869,
12.));
#179103=CARTESIAN_POINT('Ctrl Pts',(-18.2546436839609,16.342839403159,12.));
#179104=CARTESIAN_POINT('Ctrl Pts',(-18.2445844558742,16.3214888370988,
12.));
#179105=CARTESIAN_POINT('Ctrl Pts',(-18.2345105028981,16.3002435251378,
12.));
#179106=CARTESIAN_POINT('Ctrl Pts',(-18.2244223710745,16.2791038736223,
12.));
#179107=CARTESIAN_POINT('Ctrl Pts',(-18.214320612253,16.2580702914615,12.));
#179108=CARTESIAN_POINT('Ctrl Pts',(-18.2042057842037,16.237143190164,12.));
#179109=CARTESIAN_POINT('Ctrl Pts',(-18.1940784507232,16.2163229838878,
12.));
#179110=CARTESIAN_POINT('Ctrl Pts',(-18.1839391817335,16.1956100895076,
12.));
#179111=CARTESIAN_POINT('Ctrl Pts',(-18.1737885533852,16.1750049266673,
12.));
#179112=CARTESIAN_POINT('Ctrl Pts',(-18.1636271481616,16.1545079178261,
12.));
#179113=CARTESIAN_POINT('Ctrl Pts',(-18.1534555549851,16.1341194882987,
12.));
#179114=CARTESIAN_POINT('Ctrl Pts',(-18.1432743693231,16.113840066279,12.));
#179115=CARTESIAN_POINT('Ctrl Pts',(-18.1330841933099,16.0936700829108,
12.));
#179116=CARTESIAN_POINT('Ctrl Pts',(-18.1228856358746,16.0736099723664,
12.));
#179117=CARTESIAN_POINT('Ctrl Pts',(-18.1126793128688,16.0536601719124,
12.));
#179118=CARTESIAN_POINT('Ctrl Pts',(-18.1024658471966,16.0338211219693,
12.));
#179119=CARTESIAN_POINT('Ctrl Pts',(-18.0922458689464,16.0140932661612,
12.));
#179120=CARTESIAN_POINT('Ctrl Pts',(-18.0820200155239,15.9944770513616,
12.));
#179121=CARTESIAN_POINT('Ctrl Pts',(-18.071788931796,15.9749729277848,12.));
#179122=CARTESIAN_POINT('Ctrl Pts',(-18.061553270236,15.9555813490645,12.));
#179123=CARTESIAN_POINT('Ctrl Pts',(-18.0513136910691,15.9363027723244,
12.));
#179124=CARTESIAN_POINT('Ctrl Pts',(-18.0410708624208,15.9171376582436,
12.));
#179125=CARTESIAN_POINT('Ctrl Pts',(-18.0308254604638,15.8980864711043,
12.));
#179126=CARTESIAN_POINT('Ctrl Pts',(-18.0205781695773,15.8791496788685,
12.));
#179127=CARTESIAN_POINT('Ctrl Pts',(-18.010329682521,15.8603277532834,12.));
#179128=CARTESIAN_POINT('Ctrl Pts',(-18.0000807006055,15.8416211699681,
12.));
#179129=CARTESIAN_POINT('Ctrl Pts',(-17.9898319338664,15.8230304084963,
12.));
#179130=CARTESIAN_POINT('Ctrl Pts',(-17.9795841012383,15.8045559524674,
12.));
#179131=CARTESIAN_POINT('Ctrl Pts',(-17.9693379307297,15.786198289572,12.));
#179132=CARTESIAN_POINT('Ctrl Pts',(-17.9590941596236,15.7679579117072,
12.));
#179133=CARTESIAN_POINT('Ctrl Pts',(-17.9488535346776,15.7498353150856,
12.));
#179134=CARTESIAN_POINT('Ctrl Pts',(-17.9386168123261,15.7318310003334,
12.));
#179135=CARTESIAN_POINT('Ctrl Pts',(-17.9283847588837,15.713945472584,12.));
#179136=CARTESIAN_POINT('Ctrl Pts',(-17.918158150746,15.6961792415526,12.));
#179137=CARTESIAN_POINT('Ctrl Pts',(-17.9079377746118,15.6785328216467,
12.));
#179138=CARTESIAN_POINT('Ctrl Pts',(-17.8977244277247,15.6610067321036,
12.));
#179139=CARTESIAN_POINT('Ctrl Pts',(-17.8875189181095,15.6436014971088,
12.));
#179140=CARTESIAN_POINT('Ctrl Pts',(-17.8773220648125,15.6263176459107,
12.));
#179141=CARTESIAN_POINT('Ctrl Pts',(-17.8671346981388,15.6091557129205,
12.));
#179142=CARTESIAN_POINT('Ctrl Pts',(-17.8569576598996,15.5921162378183,
12.));
#179143=CARTESIAN_POINT('Ctrl Pts',(-17.8467918036977,15.5751997657153,
12.));
#179144=CARTESIAN_POINT('Ctrl Pts',(-17.8366379952078,15.5584068472976,
12.));
#179145=CARTESIAN_POINT('Ctrl Pts',(-17.8264971124606,15.5417380389639,
12.));
#179146=CARTESIAN_POINT('Ctrl Pts',(-17.8163700461263,15.5251939029558,
12.));
#179147=CARTESIAN_POINT('Ctrl Pts',(-17.8062576997964,15.5087750074728,
12.));
#179148=CARTESIAN_POINT('Ctrl Pts',(-17.7961609903161,15.4924819268529,
12.));
#179149=CARTESIAN_POINT('Ctrl Pts',(-17.7860808481229,15.4763152417506,
12.));
#179150=CARTESIAN_POINT('Ctrl Pts',(-17.7760182175817,15.4602755393019,
12.));
#179151=CARTESIAN_POINT('Ctrl Pts',(-17.765974057326,15.4443634132865,12.));
#179152=CARTESIAN_POINT('Ctrl Pts',(-17.7559493405871,15.4285794642658,
12.));
#179153=CARTESIAN_POINT('Ctrl Pts',(-17.7459450555803,15.4129242997828,
12.));
#179154=CARTESIAN_POINT('Ctrl Pts',(-17.7359622059143,15.3973985345796,
12.));
#179155=CARTESIAN_POINT('Ctrl Pts',(-17.7260018109923,15.3820027907965,
12.));
#179156=CARTESIAN_POINT('Ctrl Pts',(-17.7160649064208,15.3667376981702,
12.));
#179157=CARTESIAN_POINT('Ctrl Pts',(-17.7061525444044,15.3516038942064,
12.));
#179158=CARTESIAN_POINT('Ctrl Pts',(-17.6962657941984,15.3366020244069,
12.));
#179159=CARTESIAN_POINT('Ctrl Pts',(-17.6864057426052,15.3217327425341,
12.));
#179160=CARTESIAN_POINT('Ctrl Pts',(-17.6765734944559,15.3069967108501,
12.));
#179161=CARTESIAN_POINT('Ctrl Pts',(-17.6667701731041,15.2923946003598,
12.));
#179162=CARTESIAN_POINT('Ctrl Pts',(-17.6569969209,15.2779270910238,12.));
#179163=CARTESIAN_POINT('Ctrl Pts',(-17.6472548997329,15.263594872029,12.));
#179164=CARTESIAN_POINT('Ctrl Pts',(-17.637545291637,15.2493986421091,12.));
#179165=CARTESIAN_POINT('Ctrl Pts',(-17.6278692993765,15.2353391098367,
12.));
#179166=CARTESIAN_POINT('Ctrl Pts',(-17.6182281470467,15.22141699392,12.));
#179167=CARTESIAN_POINT('Ctrl Pts',(-17.6086230806497,15.2076330234686,
12.));
#179168=CARTESIAN_POINT('Ctrl Pts',(-17.5990553687595,15.1939879383268,
12.));
#179169=CARTESIAN_POINT('Ctrl Pts',(-17.5895263032592,15.1804824894605,
12.));
#179170=CARTESIAN_POINT('Ctrl Pts',(-17.5800372000539,15.1671174393136,
12.));
#179171=CARTESIAN_POINT('Ctrl Pts',(-17.570589399803,15.1538935621714,12.));
#179172=CARTESIAN_POINT('Ctrl Pts',(-17.5611842686196,15.1408116444877,
12.));
#179173=CARTESIAN_POINT('Ctrl Pts',(-17.5518231989122,15.127872485314,12.));
#179174=CARTESIAN_POINT('Ctrl Pts',(-17.5425076102966,15.1150768967729,
12.));
#179175=CARTESIAN_POINT('Ctrl Pts',(-17.5332389504829,15.1024257045033,
12.));
#179176=CARTESIAN_POINT('Ctrl Pts',(-17.5240186961788,15.0899197481082,
12.));
#179177=CARTESIAN_POINT('Ctrl Pts',(-17.5148483539684,15.0775598815748,
12.));
#179178=CARTESIAN_POINT('Ctrl Pts',(-17.5057294613874,15.0653469738306,
12.));
#179179=CARTESIAN_POINT('Ctrl Pts',(-17.4966635880245,15.0532819093085,
12.));
#179180=CARTESIAN_POINT('Ctrl Pts',(-17.4876523366178,15.0413655884993,
12.));
#179181=CARTESIAN_POINT('Ctrl Pts',(-17.4786973441417,15.029598928488,12.));
#179182=CARTESIAN_POINT('Ctrl Pts',(-17.4698002829357,15.0179828635086,
12.));
#179183=CARTESIAN_POINT('Ctrl Pts',(-17.4609628621418,15.0065183456921,
12.));
#179184=CARTESIAN_POINT('Ctrl Pts',(-17.4521868291004,14.9952063457778,
12.));
#179185=CARTESIAN_POINT('Ctrl Pts',(-17.4434739707773,14.9840478538358,
12.));
#179186=CARTESIAN_POINT('Ctrl Pts',(-17.4348261151396,14.9730438799452,
12.));
#179187=CARTESIAN_POINT('Ctrl Pts',(-17.426245132709,14.9621954549827,12.));
#179188=CARTESIAN_POINT('Ctrl Pts',(-17.4177329382828,14.9515036315143,
12.));
#179189=CARTESIAN_POINT('Ctrl Pts',(-17.4092914926071,14.940969484645,12.));
#179190=CARTESIAN_POINT('Ctrl Pts',(-17.4009228040749,14.9305941128757,
12.));
#179191=CARTESIAN_POINT('Ctrl Pts',(-17.3926289303986,14.9203786389342,
12.));
#179192=CARTESIAN_POINT('Ctrl Pts',(-17.3844119809824,14.9103242110057,
12.));
#179193=CARTESIAN_POINT('Ctrl Pts',(-17.3762741193076,14.900432003961,12.));
#179194=CARTESIAN_POINT('Ctrl Pts',(-17.3682175653235,14.8907032205788,
12.));
#179195=CARTESIAN_POINT('Ctrl Pts',(-17.3602445978161,14.8811390927423,
12.));
#179196=CARTESIAN_POINT('Ctrl Pts',(-17.3523575568645,14.8717408826955,
12.));
#179197=CARTESIAN_POINT('Ctrl Pts',(-17.3445588463475,14.8625098843417,
12.));
#179198=CARTESIAN_POINT('Ctrl Pts',(-17.336850936485,14.8534474245433,12.));
#179199=CARTESIAN_POINT('Ctrl Pts',(-17.3292363662605,14.8445548643508,
12.));
#179200=CARTESIAN_POINT('Ctrl Pts',(-17.3217177462101,14.8358336004197,
12.));
#179201=CARTESIAN_POINT('Ctrl Pts',(-17.3142977632659,14.8272850675379,
12.));
#179202=CARTESIAN_POINT('Ctrl Pts',(-17.3069791853706,14.8189107410162,
12.));
#179203=CARTESIAN_POINT('Ctrl Pts',(-17.299764866148,14.8107121391035,12.));
#179204=CARTESIAN_POINT('Ctrl Pts',(-17.2926577496513,14.8026908254276,
12.));
#179205=CARTESIAN_POINT('Ctrl Pts',(-17.2856608733196,14.7948484105249,
12.));
#179206=CARTESIAN_POINT('Ctrl Pts',(-17.2787773704849,14.787186553128,12.));
#179207=CARTESIAN_POINT('Ctrl Pts',(-17.2720104735194,14.7797069617804,
12.));
#179208=CARTESIAN_POINT('Ctrl Pts',(-17.2653635155319,14.7724113956731,
12.));
#179209=CARTESIAN_POINT('Ctrl Pts',(-17.2588399401465,14.7653016697591,
12.));
#179210=CARTESIAN_POINT('Ctrl Pts',(-17.2524433146837,14.7583796616617,
12.));
#179211=CARTESIAN_POINT('Ctrl Pts',(-17.2461773413288,14.7516473175124,
12.));
#179212=CARTESIAN_POINT('Ctrl Pts',(-17.2400458713565,14.7451066593792,
12.));
#179213=CARTESIAN_POINT('Ctrl Pts',(-17.2340529062076,14.7387597858116,
12.));
#179214=CARTESIAN_POINT('Ctrl Pts',(-17.2282025904314,14.7326088681163,
12.));
#179215=CARTESIAN_POINT('Ctrl Pts',(-17.2224992099667,14.7266561494282,
12.));
#179216=CARTESIAN_POINT('Ctrl Pts',(-17.2169471814256,14.7209039390327,
12.));
#179217=CARTESIAN_POINT('Ctrl Pts',(-17.2115510835989,14.7153546289339,
12.));
#179218=CARTESIAN_POINT('Ctrl Pts',(-17.2063157097315,14.7100107213586,
12.));
#179219=CARTESIAN_POINT('Ctrl Pts',(-17.2012461084268,14.7048748502663,
12.));
#179220=CARTESIAN_POINT('Ctrl Pts',(-17.1963476411694,14.699949811582,12.));
#179221=CARTESIAN_POINT('Ctrl Pts',(-17.1916259308415,14.6952385361705,
12.));
#179222=CARTESIAN_POINT('Ctrl Pts',(-17.1870867909918,14.6907440526958,
12.));
#179223=CARTESIAN_POINT('Ctrl Pts',(-17.182736158472,14.686469452232,12.));
#179224=CARTESIAN_POINT('Ctrl Pts',(-17.1785800350826,14.6824178576167,
12.));
#179225=CARTESIAN_POINT('Ctrl Pts',(-17.1746247499057,14.6785925615677,
12.));
#179226=CARTESIAN_POINT('Ctrl Pts',(-17.1708771619129,14.6749971333867,
12.));
#179227=CARTESIAN_POINT('Ctrl Pts',(-17.167344972302,14.671635583332,12.));
#179228=CARTESIAN_POINT('Ctrl Pts',(-17.1640366762305,14.6685123374423,
12.));
#179229=CARTESIAN_POINT('Ctrl Pts',(-17.1609609517369,14.6656319165057,
12.));
#179230=CARTESIAN_POINT('Ctrl Pts',(-17.1581262646789,14.6629987285992,
12.));
#179231=CARTESIAN_POINT('Ctrl Pts',(-17.1555401986401,14.6606167169642,
12.));
#179232=CARTESIAN_POINT('Ctrl Pts',(-17.1532107762718,14.6584900555302,
12.));
#179233=CARTESIAN_POINT('Ctrl Pts',(-17.1511476869496,14.6566237952435,
12.));
#179234=CARTESIAN_POINT('Ctrl Pts',(-17.1493641837558,14.655024862281,12.));
#179235=CARTESIAN_POINT('Ctrl Pts',(-17.147876394491,14.6537016966184,12.));
#179236=CARTESIAN_POINT('Ctrl Pts',(-17.1466998098673,14.6526624064978,
12.));
#179237=CARTESIAN_POINT('Ctrl Pts',(-17.1458462295271,14.6519131634508,
12.));
#179238=CARTESIAN_POINT('Ctrl Pts',(-17.1454262858043,14.6515481598068,
12.));
#179239=CARTESIAN_POINT('Ctrl Pts',(-17.1452600887037,14.6514066997196,
12.));
#179240=CARTESIAN_POINT('Ctrl Pts',(-17.1452153999142,14.6513711852843,
12.));
#179241=CARTESIAN_POINT('Ctrl Pts',(-17.1452095830633,14.6513681262571,
12.));
#179242=CARTESIAN_POINT('',(-16.7207683102834,14.2886635873976,12.));
#179243=CARTESIAN_POINT('',(-8.17248635976757,6.98376450772883,12.));
#179244=CARTESIAN_POINT('',(-16.6581946899465,13.5924445804218,12.));
#179245=CARTESIAN_POINT('Origin',(-17.0455945664569,13.9085479427572,12.));
#179246=CARTESIAN_POINT('',(-17.4407513054162,12.572596943457,12.));
#179247=CARTESIAN_POINT('Origin',(-6.00167842331873E-13,4.9889687874677E-13,
12.));
#179248=CARTESIAN_POINT('',(-18.1294424696716,12.4528436808172,12.));
#179249=CARTESIAN_POINT('Origin',(-17.846350172984,12.8649829188862,12.));
#179250=CARTESIAN_POINT('',(-18.5896416359912,12.7689476255363,12.));
#179251=CARTESIAN_POINT('',(-9.29482081799561,6.38447381276812,12.));
#179252=CARTESIAN_POINT('',(-22.1787195904339,13.5685075571671,12.));
#179253=CARTESIAN_POINT('Ctrl Pts',(-18.5896416359912,12.7689476255363,
12.));
#179254=CARTESIAN_POINT('Ctrl Pts',(-18.5896460962961,12.7689524524484,
12.));
#179255=CARTESIAN_POINT('Ctrl Pts',(-18.5896919669158,12.7689864266924,
12.));
#179256=CARTESIAN_POINT('Ctrl Pts',(-18.589871621842,12.7691103481996,12.));
#179257=CARTESIAN_POINT('Ctrl Pts',(-18.590332877722,12.7694215127923,12.));
#179258=CARTESIAN_POINT('Ctrl Pts',(-18.5912775137806,12.7700520897174,
12.));
#179259=CARTESIAN_POINT('Ctrl Pts',(-18.5925859134582,12.7709195951153,
12.));
#179260=CARTESIAN_POINT('Ctrl Pts',(-18.5942490615409,12.7720142287169,
12.));
#179261=CARTESIAN_POINT('Ctrl Pts',(-18.5962551167772,12.7733231262107,
12.));
#179262=CARTESIAN_POINT('Ctrl Pts',(-18.5985917525949,12.7748328937639,
12.));
#179263=CARTESIAN_POINT('Ctrl Pts',(-18.6012488486708,12.7765325225082,
12.));
#179264=CARTESIAN_POINT('Ctrl Pts',(-18.6042190183703,12.7784139605067,
12.));
#179265=CARTESIAN_POINT('Ctrl Pts',(-18.6074961535723,12.7804705387658,
12.));
#179266=CARTESIAN_POINT('Ctrl Pts',(-18.611074482622,12.7826959526924,12.));
#179267=CARTESIAN_POINT('Ctrl Pts',(-18.6149475565189,12.78508316579,12.));
#179268=CARTESIAN_POINT('Ctrl Pts',(-18.6191087624752,12.7876249657834,
12.));
#179269=CARTESIAN_POINT('Ctrl Pts',(-18.6235516265575,12.7903142925234,
12.));
#179270=CARTESIAN_POINT('Ctrl Pts',(-18.6282702819371,12.7931447451556,
12.));
#179271=CARTESIAN_POINT('Ctrl Pts',(-18.6332595057005,12.7961106222251,
12.));
#179272=CARTESIAN_POINT('Ctrl Pts',(-18.63851447924,12.7992066625264,12.));
#179273=CARTESIAN_POINT('Ctrl Pts',(-18.6440306327457,12.8024278770153,
12.));
#179274=CARTESIAN_POINT('Ctrl Pts',(-18.6498034438986,12.805769331162,12.));
#179275=CARTESIAN_POINT('Ctrl Pts',(-18.6558284825772,12.8092261933858,
12.));
#179276=CARTESIAN_POINT('Ctrl Pts',(-18.6621014624746,12.8127937909632,
12.));
#179277=CARTESIAN_POINT('Ctrl Pts',(-18.6686182952798,12.8164676687361,
12.));
#179278=CARTESIAN_POINT('Ctrl Pts',(-18.6753751301091,12.8202436318473,
12.));
#179279=CARTESIAN_POINT('Ctrl Pts',(-18.6823683094139,12.8241176980016,
12.));
#179280=CARTESIAN_POINT('Ctrl Pts',(-18.6895943376172,12.8280860635231,
12.));
#179281=CARTESIAN_POINT('Ctrl Pts',(-18.6970498410173,12.832145059979,12.));
#179282=CARTESIAN_POINT('Ctrl Pts',(-18.7047315436296,12.8362911280362,
12.));
#179283=CARTESIAN_POINT('Ctrl Pts',(-18.7126362754446,12.8405208263432,
12.));
#179284=CARTESIAN_POINT('Ctrl Pts',(-18.7207609737701,12.8448308329494,
12.));
#179285=CARTESIAN_POINT('Ctrl Pts',(-18.7291026886552,12.849217951159,12.));
#179286=CARTESIAN_POINT('Ctrl Pts',(-18.7376585820851,12.8536791086315,
12.));
#179287=CARTESIAN_POINT('Ctrl Pts',(-18.7464259171248,12.8582113455644,
12.));
#179288=CARTESIAN_POINT('Ctrl Pts',(-18.7554020493888,12.8628118054172,
12.));
#179289=CARTESIAN_POINT('Ctrl Pts',(-18.7645844169568,12.8674777239656,
12.));
#179290=CARTESIAN_POINT('Ctrl Pts',(-18.7739705329029,12.8722064211814,
12.));
#179291=CARTESIAN_POINT('Ctrl Pts',(-18.7835579840481,12.8769952998097,
12.));
#179292=CARTESIAN_POINT('Ctrl Pts',(-18.7933444285867,12.8818418427474,
12.));
#179293=CARTESIAN_POINT('Ctrl Pts',(-18.8033275941939,12.8867436109543,
12.));
#179294=CARTESIAN_POINT('Ctrl Pts',(-18.8135052757815,12.8916982409931,
12.));
#179295=CARTESIAN_POINT('Ctrl Pts',(-18.8238753319124,12.8967034410752,
12.));
#179296=CARTESIAN_POINT('Ctrl Pts',(-18.834435681259,12.9017569871738,12.));
#179297=CARTESIAN_POINT('Ctrl Pts',(-18.8451842990986,12.9068567191856,
12.));
#179298=CARTESIAN_POINT('Ctrl Pts',(-18.8561192136201,12.9120005369066,
12.));
#179299=CARTESIAN_POINT('Ctrl Pts',(-18.8672385038328,12.9171863977047,
12.));
#179300=CARTESIAN_POINT('Ctrl Pts',(-18.8785402977528,12.9224123144982,
12.));
#179301=CARTESIAN_POINT('Ctrl Pts',(-18.8900227704888,12.9276763536372,
12.));
#179302=CARTESIAN_POINT('Ctrl Pts',(-18.9016841423402,12.9329766328184,
12.));
#179303=CARTESIAN_POINT('Ctrl Pts',(-18.9135226769466,12.9383113190375,
12.));
#179304=CARTESIAN_POINT('Ctrl Pts',(-18.9255366795196,12.9436786266106,
12.));
#179305=CARTESIAN_POINT('Ctrl Pts',(-18.9377244950435,12.9490768151821,
12.));
#179306=CARTESIAN_POINT('Ctrl Pts',(-18.9500845064714,12.9545041877377,
12.));
#179307=CARTESIAN_POINT('Ctrl Pts',(-18.9626151329226,12.9599590886317,
12.));
#179308=CARTESIAN_POINT('Ctrl Pts',(-18.9753148284473,12.9654399021868,
12.));
#179309=CARTESIAN_POINT('Ctrl Pts',(-18.9881820807585,12.9709450512747,
12.));
#179310=CARTESIAN_POINT('Ctrl Pts',(-19.0012154099792,12.9764729959206,
12.));
#179311=CARTESIAN_POINT('Ctrl Pts',(-19.014413367335,12.9820222318716,12.));
#179312=CARTESIAN_POINT('Ctrl Pts',(-19.0277745339909,12.9875912893003,
12.));
#179313=CARTESIAN_POINT('Ctrl Pts',(-19.0412975200398,12.9931787316514,
12.));
#179314=CARTESIAN_POINT('Ctrl Pts',(-19.0549809634354,12.9987831544502,
12.));
#179315=CARTESIAN_POINT('Ctrl Pts',(-19.0688235289437,13.0044031841382,
12.));
#179316=CARTESIAN_POINT('Ctrl Pts',(-19.0828239070484,13.0100374768788,
12.));
#179317=CARTESIAN_POINT('Ctrl Pts',(-19.0969808131228,13.0156847176096,
12.));
#179318=CARTESIAN_POINT('Ctrl Pts',(-19.111292986631,13.0213436191328,12.));
#179319=CARTESIAN_POINT('Ctrl Pts',(-19.1257591903099,13.0270129211976,
12.));
#179320=CARTESIAN_POINT('Ctrl Pts',(-19.1403782093386,13.0326913895838,
12.));
#179321=CARTESIAN_POINT('Ctrl Pts',(-19.155148850523,13.0383778152068,12.));
#179322=CARTESIAN_POINT('Ctrl Pts',(-19.1700699416622,13.0440710133772,
12.));
#179323=CARTESIAN_POINT('Ctrl Pts',(-19.1851403308825,13.0497698230441,
12.));
#179324=CARTESIAN_POINT('Ctrl Pts',(-19.2003588859772,13.0554731060538,
12.));
#179325=CARTESIAN_POINT('Ctrl Pts',(-19.2157244937142,13.0611797463915,
12.));
#179326=CARTESIAN_POINT('Ctrl Pts',(-19.2312360592033,13.0668886494795,
12.));
#179327=CARTESIAN_POINT('Ctrl Pts',(-19.2468925053989,13.0725987415859,
12.));
#179328=CARTESIAN_POINT('Ctrl Pts',(-19.2626927725596,13.0783089692118,
12.));
#179329=CARTESIAN_POINT('Ctrl Pts',(-19.2786358177198,13.0840182984949,
12.));
#179330=CARTESIAN_POINT('Ctrl Pts',(-19.2947206141247,13.0897257145968,
12.));
#179331=CARTESIAN_POINT('Ctrl Pts',(-19.310946150736,13.0954302211479,12.));
#179332=CARTESIAN_POINT('Ctrl Pts',(-19.3273114318269,13.1011308397591,
12.));
#179333=CARTESIAN_POINT('Ctrl Pts',(-19.3438154765395,13.1068266095186,
12.));
#179334=CARTESIAN_POINT('Ctrl Pts',(-19.3604573184515,13.1125165865022,
12.));
#179335=CARTESIAN_POINT('Ctrl Pts',(-19.3772360051091,13.118199843271,12.));
#179336=CARTESIAN_POINT('Ctrl Pts',(-19.3941505976263,13.1238754684177,
12.));
#179337=CARTESIAN_POINT('Ctrl Pts',(-19.4112001703557,13.1295425661634,
12.));
#179338=CARTESIAN_POINT('Ctrl Pts',(-19.4283838105262,13.1352002559438,
12.));
#179339=CARTESIAN_POINT('Ctrl Pts',(-19.4457006178876,13.1408476720061,
12.));
#179340=CARTESIAN_POINT('Ctrl Pts',(-19.4631497043258,13.1464839629971,
12.));
#179341=CARTESIAN_POINT('Ctrl Pts',(-19.4807301935268,13.1521082915853,
12.));
#179342=CARTESIAN_POINT('Ctrl Pts',(-19.4984412207082,13.1577198341245,
12.));
#179343=CARTESIAN_POINT('Ctrl Pts',(-19.5162819323213,13.1633177803101,
12.));
#179344=CARTESIAN_POINT('Ctrl Pts',(-19.5342514857562,13.168901332843,12.));
#179345=CARTESIAN_POINT('Ctrl Pts',(-19.5523490490244,13.1744697070911,
12.));
#179346=CARTESIAN_POINT('Ctrl Pts',(-19.5705738004667,13.1800221307673,
12.));
#179347=CARTESIAN_POINT('Ctrl Pts',(-19.5889249285338,13.1855578436471,
12.));
#179348=CARTESIAN_POINT('Ctrl Pts',(-19.6074016315414,13.1910760972814,
12.));
#179349=CARTESIAN_POINT('Ctrl Pts',(-19.6260031174244,13.1965761547151,
12.));
#179350=CARTESIAN_POINT('Ctrl Pts',(-19.6447286034772,13.2020572902065,
12.));
#179351=CARTESIAN_POINT('Ctrl Pts',(-19.6635773160936,13.2075187889529,
12.));
#179352=CARTESIAN_POINT('Ctrl Pts',(-19.6825484905823,13.2129599468485,
12.));
#179353=CARTESIAN_POINT('Ctrl Pts',(-19.7016413709685,13.2183800702436,
12.));
#179354=CARTESIAN_POINT('Ctrl Pts',(-19.7208552097868,13.2237784757065,
12.));
#179355=CARTESIAN_POINT('Ctrl Pts',(-19.7401892678697,13.2291544897899,
12.));
#179356=CARTESIAN_POINT('Ctrl Pts',(-19.7596428141168,13.2345074487963,
12.));
#179357=CARTESIAN_POINT('Ctrl Pts',(-19.7792151253289,13.2398366985675,
12.));
#179358=CARTESIAN_POINT('Ctrl Pts',(-19.7989054860495,13.2451415942805,
12.));
#179359=CARTESIAN_POINT('Ctrl Pts',(-19.8187131883917,13.2504215002457,
12.));
#179360=CARTESIAN_POINT('Ctrl Pts',(-19.8386375318634,13.2556757897086,
12.));
#179361=CARTESIAN_POINT('Ctrl Pts',(-19.8586778231715,13.2609038446529,
12.));
#179362=CARTESIAN_POINT('Ctrl Pts',(-19.8788333760577,13.2661050556132,
12.));
#179363=CARTESIAN_POINT('Ctrl Pts',(-19.8991035111745,13.271278821502,12.));
#179364=CARTESIAN_POINT('Ctrl Pts',(-19.9194875559422,13.2764245494357,
12.));
#179365=CARTESIAN_POINT('Ctrl Pts',(-19.9399848444019,13.2815416545663,
12.));
#179366=CARTESIAN_POINT('Ctrl Pts',(-19.9605947170586,13.286629559915,12.));
#179367=CARTESIAN_POINT('Ctrl Pts',(-19.981316520717,13.2916876962094,12.));
#179368=CARTESIAN_POINT('Ctrl Pts',(-20.0021496083738,13.2967155017306,
12.));
#179369=CARTESIAN_POINT('Ctrl Pts',(-20.0230933391038,13.3017124221637,
12.));
#179370=CARTESIAN_POINT('Ctrl Pts',(-20.0441470779345,13.3066779104515,
12.));
#179371=CARTESIAN_POINT('Ctrl Pts',(-20.0653101957188,13.3116114266515,
12.));
#179372=CARTESIAN_POINT('Ctrl Pts',(-20.0865820689883,13.3165124377962,
12.));
#179373=CARTESIAN_POINT('Ctrl Pts',(-20.1079620798375,13.3213804177587,
12.));
#179374=CARTESIAN_POINT('Ctrl Pts',(-20.1294496158402,13.3262148471226,
12.));
#179375=CARTESIAN_POINT('Ctrl Pts',(-20.1510440699474,13.3310152130564,
12.));
#179376=CARTESIAN_POINT('Ctrl Pts',(-20.1727448403817,13.3357810091903,
12.));
#179377=CARTESIAN_POINT('Ctrl Pts',(-20.1945513305235,13.3405117354971,
12.));
#179378=CARTESIAN_POINT('Ctrl Pts',(-20.216462948786,13.3452068981766,12.));
#179379=CARTESIAN_POINT('Ctrl Pts',(-20.2384791085359,13.3498660095386,
12.));
#179380=CARTESIAN_POINT('Ctrl Pts',(-20.2605992280122,13.3544885878889,
12.));
#179381=CARTESIAN_POINT('Ctrl Pts',(-20.2828227302339,13.3590741574195,
12.));
#179382=CARTESIAN_POINT('Ctrl Pts',(-20.3051490429048,13.3636222481016,
12.));
#179383=CARTESIAN_POINT('Ctrl Pts',(-20.3275775983029,13.3681323955826,
12.));
#179384=CARTESIAN_POINT('Ctrl Pts',(-20.3501078331814,13.3726041410867,
12.));
#179385=CARTESIAN_POINT('Ctrl Pts',(-20.3727391887184,13.3770370313188,
12.));
#179386=CARTESIAN_POINT('Ctrl Pts',(-20.3954711104502,13.3814306183719,
12.));
#179387=CARTESIAN_POINT('Ctrl Pts',(-20.4183030482002,13.3857844596387,
12.));
#179388=CARTESIAN_POINT('Ctrl Pts',(-20.4412344560008,13.3900981177255,
12.));
#179389=CARTESIAN_POINT('Ctrl Pts',(-20.4642647920038,13.3943711603739,
12.));
#179390=CARTESIAN_POINT('Ctrl Pts',(-20.487393518404,13.3986031603716,12.));
#179391=CARTESIAN_POINT('Ctrl Pts',(-20.5106201013753,13.4027936954529,
12.));
#179392=CARTESIAN_POINT('Ctrl Pts',(-20.5339440109956,13.4069423482076,
12.));
#179393=CARTESIAN_POINT('Ctrl Pts',(-20.5573647211639,13.4110487059912,
12.));
#179394=CARTESIAN_POINT('Ctrl Pts',(-20.5808817095155,13.4151123608411,
12.));
#179395=CARTESIAN_POINT('Ctrl Pts',(-20.6044944573153,13.4191329093932,
12.));
#179396=CARTESIAN_POINT('Ctrl Pts',(-20.6282024494237,13.4231099528179,
12.));
#179397=CARTESIAN_POINT('Ctrl Pts',(-20.6520051742869,13.4270430967651,
12.));
#179398=CARTESIAN_POINT('Ctrl Pts',(-20.6759021239103,13.4309319513119,
12.));
#179399=CARTESIAN_POINT('Ctrl Pts',(-20.6998927938288,13.4347761309154,
12.));
#179400=CARTESIAN_POINT('Ctrl Pts',(-20.7239766830675,13.4385752543663,
12.));
#179401=CARTESIAN_POINT('Ctrl Pts',(-20.7481532941013,13.4423289447561,
12.));
#179402=CARTESIAN_POINT('Ctrl Pts',(-20.7724221327608,13.4460368293688,
12.));
#179403=CARTESIAN_POINT('Ctrl Pts',(-20.7967827081227,13.4496985395637,
12.));
#179404=CARTESIAN_POINT('Ctrl Pts',(-20.821234532398,13.4533137106667,12.));
#179405=CARTESIAN_POINT('Ctrl Pts',(-20.8457771208082,13.4568819818631,
12.));
#179406=CARTESIAN_POINT('Ctrl Pts',(-20.8704099914641,13.4604029960983,
12.));
#179407=CARTESIAN_POINT('Ctrl Pts',(-20.8951326652158,13.4638763999725,
12.));
#179408=CARTESIAN_POINT('Ctrl Pts',(-20.9199446657584,13.4673018437718,
12.));
#179409=CARTESIAN_POINT('Ctrl Pts',(-20.9448455197557,13.4706789815166,
12.));
#179410=CARTESIAN_POINT('Ctrl Pts',(-20.9698347569476,13.4740074710087,
12.));
#179411=CARTESIAN_POINT('Ctrl Pts',(-20.9949119102592,13.4772869738879,
12.));
#179412=CARTESIAN_POINT('Ctrl Pts',(-21.0200765158885,13.4805171556822,
12.));
#179413=CARTESIAN_POINT('Ctrl Pts',(-21.0453281134247,13.4836976858912,
12.));
#179414=CARTESIAN_POINT('Ctrl Pts',(-21.0706662455202,13.4868282377191,
12.));
#179415=CARTESIAN_POINT('Ctrl Pts',(-21.0960904575048,13.4899084877718,
12.));
#179416=CARTESIAN_POINT('Ctrl Pts',(-21.1216002970209,13.4929381157778,
12.));
#179417=CARTESIAN_POINT('Ctrl Pts',(-21.1471953136209,13.4959168042934,
12.));
#179418=CARTESIAN_POINT('Ctrl Pts',(-21.1728750584173,13.4988442384491,
12.));
#179419=CARTESIAN_POINT('Ctrl Pts',(-21.1986390835825,13.5017201056088,
12.));
#179420=CARTESIAN_POINT('Ctrl Pts',(-21.224486942933,13.5045440957404,12.));
#179421=CARTESIAN_POINT('Ctrl Pts',(-21.2504181927429,13.5073159019454,
12.));
#179422=CARTESIAN_POINT('Ctrl Pts',(-21.2764323924442,13.5100352209207,
12.));
#179423=CARTESIAN_POINT('Ctrl Pts',(-21.3025291054236,13.5127017534972,
12.));
#179424=CARTESIAN_POINT('Ctrl Pts',(-21.328707899634,13.5153152050554,12.));
#179425=CARTESIAN_POINT('Ctrl Pts',(-21.3549683486219,13.5178752862461,
12.));
#179426=CARTESIAN_POINT('Ctrl Pts',(-21.3813100304967,13.5203817122496,
12.));
#179427=CARTESIAN_POINT('Ctrl Pts',(-21.4077325259318,13.5228342013508,
12.));
#179428=CARTESIAN_POINT('Ctrl Pts',(-21.4342354165254,13.5252324737795,
12.));
#179429=CARTESIAN_POINT('Ctrl Pts',(-21.4608182828695,13.5275762503553,
12.));
#179430=CARTESIAN_POINT('Ctrl Pts',(-21.487480703047,13.5298652514357,12.));
#179431=CARTESIAN_POINT('Ctrl Pts',(-21.5142222501671,13.5320991952145,
12.));
#179432=CARTESIAN_POINT('Ctrl Pts',(-21.5410424932511,13.5342777983225,
12.));
#179433=CARTESIAN_POINT('Ctrl Pts',(-21.5679410019011,13.5364007790292,
12.));
#179434=CARTESIAN_POINT('Ctrl Pts',(-21.5949173499022,13.5384678597206,
12.));
#179435=CARTESIAN_POINT('Ctrl Pts',(-21.6219711193951,13.5404787697798,
12.));
#179436=CARTESIAN_POINT('Ctrl Pts',(-21.6491019044647,13.5424332480698,
12.));
#179437=CARTESIAN_POINT('Ctrl Pts',(-21.676309315769,13.5443310461516,12.));
#179438=CARTESIAN_POINT('Ctrl Pts',(-21.7035929822939,13.546171929503,12.));
#179439=CARTESIAN_POINT('Ctrl Pts',(-21.730952541226,13.5479556704457,12.));
#179440=CARTESIAN_POINT('Ctrl Pts',(-21.7583876294532,13.5496820422186,
12.));
#179441=CARTESIAN_POINT('Ctrl Pts',(-21.7858978745848,13.5513508127232,
12.));
#179442=CARTESIAN_POINT('Ctrl Pts',(-21.8134828857963,13.5529617381569,
12.));
#179443=CARTESIAN_POINT('Ctrl Pts',(-21.841142245609,13.5545145573048,12.));
#179444=CARTESIAN_POINT('Ctrl Pts',(-21.8688754989401,13.5560089839426,
12.));
#179445=CARTESIAN_POINT('Ctrl Pts',(-21.8966821688876,13.5574447178484,
12.));
#179446=CARTESIAN_POINT('Ctrl Pts',(-21.9245617765827,13.5588214586672,
12.));
#179447=CARTESIAN_POINT('Ctrl Pts',(-21.9525138592862,13.5601389185315,
12.));
#179448=CARTESIAN_POINT('Ctrl Pts',(-21.9805379899192,13.5613968357589,
12.));
#179449=CARTESIAN_POINT('Ctrl Pts',(-22.0086337943431,13.5625949868313,
12.));
#179450=CARTESIAN_POINT('Ctrl Pts',(-22.0368009736227,13.5637332022393,
12.));
#179451=CARTESIAN_POINT('Ctrl Pts',(-22.0650393089492,13.5648113688894,
12.));
#179452=CARTESIAN_POINT('Ctrl Pts',(-22.0933486464442,13.5658294169106,
12.));
#179453=CARTESIAN_POINT('Ctrl Pts',(-22.1217288871823,13.5667873105179,
12.));
#179454=CARTESIAN_POINT('Ctrl Pts',(-22.1444897575076,13.5675054918922,
12.));
#179455=CARTESIAN_POINT('Ctrl Pts',(-22.1615922804939,13.5680170531724,
12.));
#179456=CARTESIAN_POINT('Ctrl Pts',(-22.1730081264583,13.5683460612913,
12.));
#179457=CARTESIAN_POINT('Ctrl Pts',(-22.1787195904339,13.5685075571671,
12.));
#179458=CARTESIAN_POINT('',(-22.8400320311648,12.4230808101438,12.));
#179459=CARTESIAN_POINT('Origin',(0.,0.,12.));
#179460=CARTESIAN_POINT('',(-20.353053841303,9.71462809124917,12.));
#179461=CARTESIAN_POINT('Ctrl Pts',(-22.8400320311648,12.4230808101438,
12.));
#179462=CARTESIAN_POINT('Ctrl Pts',(-22.8370364396497,12.4182152851867,
12.));
#179463=CARTESIAN_POINT('Ctrl Pts',(-22.8310435872852,12.4084933766366,
12.));
#179464=CARTESIAN_POINT('Ctrl Pts',(-22.8220493007353,12.393937937903,12.));
#179465=CARTESIAN_POINT('Ctrl Pts',(-22.8100469022632,12.3745855366772,
12.));
#179466=CARTESIAN_POINT('Ctrl Pts',(-22.7950272216959,12.3504864740361,
12.));
#179467=CARTESIAN_POINT('Ctrl Pts',(-22.7799908974947,12.3264788926108,
12.));
#179468=CARTESIAN_POINT('Ctrl Pts',(-22.7649380101154,12.3025628601812,
12.));
#179469=CARTESIAN_POINT('Ctrl Pts',(-22.7498686970096,12.2787384750747,
12.));
#179470=CARTESIAN_POINT('Ctrl Pts',(-22.7347831655251,12.2550058702389,
12.));
#179471=CARTESIAN_POINT('Ctrl Pts',(-22.7196817119299,12.2313652198047,
12.));
#179472=CARTESIAN_POINT('Ctrl Pts',(-22.7045647168659,12.2078167360267,
12.));
#179473=CARTESIAN_POINT('Ctrl Pts',(-22.6894326204959,12.1843606579246,
12.));
#179474=CARTESIAN_POINT('Ctrl Pts',(-22.6742859034891,12.1609972423088,
12.));
#179475=CARTESIAN_POINT('Ctrl Pts',(-22.6591250653942,12.1377267537141,
12.));
#179476=CARTESIAN_POINT('Ctrl Pts',(-22.6439506046611,12.1145494550384,
12.));
#179477=CARTESIAN_POINT('Ctrl Pts',(-22.628762996708,12.0914655972828,12.));
#179478=CARTESIAN_POINT('Ctrl Pts',(-22.613562676493,12.0684754113869,12.));
#179479=CARTESIAN_POINT('Ctrl Pts',(-22.5983500505675,12.0455791139135,
12.));
#179480=CARTESIAN_POINT('Ctrl Pts',(-22.5831255061306,12.0227769113132,
12.));
#179481=CARTESIAN_POINT('Ctrl Pts',(-22.5678894211194,12.0000690046697,
12.));
#179482=CARTESIAN_POINT('Ctrl Pts',(-22.5526421741159,11.9774555943496,
12.));
#179483=CARTESIAN_POINT('Ctrl Pts',(-22.5373841537299,11.9549368843996,
12.));
#179484=CARTESIAN_POINT('Ctrl Pts',(-22.5221157697869,11.9325130877801,
12.));
#179485=CARTESIAN_POINT('Ctrl Pts',(-22.5068374513958,11.9101844254555,
12.));
#179486=CARTESIAN_POINT('Ctrl Pts',(-22.4915496418472,11.8879511239941,
12.));
#179487=CARTESIAN_POINT('Ctrl Pts',(-22.4762527946694,11.8658134137018,
12.));
#179488=CARTESIAN_POINT('Ctrl Pts',(-22.4609473690469,11.8437715264487,
12.));
#179489=CARTESIAN_POINT('Ctrl Pts',(-22.4456338258738,11.8218256937889,
12.));
#179490=CARTESIAN_POINT('Ctrl Pts',(-22.4303126226468,11.7999761445175,
12.));
#179491=CARTESIAN_POINT('Ctrl Pts',(-22.4149842125018,11.7782231042041,
12.));
#179492=CARTESIAN_POINT('Ctrl Pts',(-22.39964904692,11.7565667964765,12.));
#179493=CARTESIAN_POINT('Ctrl Pts',(-22.3843075773905,11.7350074437961,
12.));
#179494=CARTESIAN_POINT('Ctrl Pts',(-22.3689602575492,11.7135452684532,
12.));
#179495=CARTESIAN_POINT('Ctrl Pts',(-22.3536075450028,11.6921804934056,
12.));
#179496=CARTESIAN_POINT('Ctrl Pts',(-22.3382499035618,11.6709133432986,
12.));
#179497=CARTESIAN_POINT('Ctrl Pts',(-22.3228878043976,11.6497440449858,
12.));
#179498=CARTESIAN_POINT('Ctrl Pts',(-22.3075217249049,11.6286728270011,
12.));
#179499=CARTESIAN_POINT('Ctrl Pts',(-22.2921521480358,11.6076999192359,
12.));
#179500=CARTESIAN_POINT('Ctrl Pts',(-22.2767795614349,11.5868255525189,
12.));
#179501=CARTESIAN_POINT('Ctrl Pts',(-22.2614044566898,11.5660499582403,
12.));
#179502=CARTESIAN_POINT('Ctrl Pts',(-22.2460273284653,11.545373367912,12.));
#179503=CARTESIAN_POINT('Ctrl Pts',(-22.2306486738899,11.5247960128476,
12.));
#179504=CARTESIAN_POINT('Ctrl Pts',(-22.215268993102,11.504318124424,12.));
#179505=CARTESIAN_POINT('Ctrl Pts',(-22.1998887896435,11.4839399342589,
12.));
#179506=CARTESIAN_POINT('Ctrl Pts',(-22.184508570917,11.463661674411,12.));
#179507=CARTESIAN_POINT('Ctrl Pts',(-22.1691288486096,11.443483577557,12.));
#179508=CARTESIAN_POINT('Ctrl Pts',(-22.1537501391486,11.4234058771742,
12.));
#179509=CARTESIAN_POINT('Ctrl Pts',(-22.1383729640963,11.4034288076908,
12.));
#179510=CARTESIAN_POINT('Ctrl Pts',(-22.1229978500185,11.3835526044256,
12.));
#179511=CARTESIAN_POINT('Ctrl Pts',(-22.1076253283978,11.3637775035367,
12.));
#179512=CARTESIAN_POINT('Ctrl Pts',(-22.0922559355293,11.3441037419553,
12.));
#179513=CARTESIAN_POINT('Ctrl Pts',(-22.0768902124267,11.3245315573168,
12.));
#179514=CARTESIAN_POINT('Ctrl Pts',(-22.0615287047179,11.3050611878771,
12.));
#179515=CARTESIAN_POINT('Ctrl Pts',(-22.046171962566,11.2856928724374,12.));
#179516=CARTESIAN_POINT('Ctrl Pts',(-22.0308205408351,11.2664268504207,
12.));
#179517=CARTESIAN_POINT('Ctrl Pts',(-22.0154749992364,11.2472633619276,
12.));
#179518=CARTESIAN_POINT('Ctrl Pts',(-22.0001359024839,11.2282026477897,
12.));
#179519=CARTESIAN_POINT('Ctrl Pts',(-21.9848038204439,11.2092449496125,
12.));
#179520=CARTESIAN_POINT('Ctrl Pts',(-21.9694793282913,11.1903905098109,
12.));
#179521=CARTESIAN_POINT('Ctrl Pts',(-21.9541630066504,11.1716395716375,
12.));
#179522=CARTESIAN_POINT('Ctrl Pts',(-21.9388554416437,11.1529923792002,
12.));
#179523=CARTESIAN_POINT('Ctrl Pts',(-21.9235572249518,11.134449177474,12.));
#179524=CARTESIAN_POINT('Ctrl Pts',(-21.9082689538687,11.1160102123024,
12.));
#179525=CARTESIAN_POINT('Ctrl Pts',(-21.8929912313608,11.0976757303944,
12.));
#179526=CARTESIAN_POINT('Ctrl Pts',(-21.8777246661191,11.0794459793058,
12.));
#179527=CARTESIAN_POINT('Ctrl Pts',(-21.8624698726319,11.0613212074364,
12.));
#179528=CARTESIAN_POINT('Ctrl Pts',(-21.8472274713103,11.0433016640808,
12.));
#179529=CARTESIAN_POINT('Ctrl Pts',(-21.8319980886033,11.0253875994598,
12.));
#179530=CARTESIAN_POINT('Ctrl Pts',(-21.8167823571168,11.0075792647477,
12.));
#179531=CARTESIAN_POINT('Ctrl Pts',(-21.8015809157302,10.9898769120913,
12.));
#179532=CARTESIAN_POINT('Ctrl Pts',(-21.7863944097143,10.9722807946157,
12.));
#179533=CARTESIAN_POINT('Ctrl Pts',(-21.7712234908468,10.9547911664457,
12.));
#179534=CARTESIAN_POINT('Ctrl Pts',(-21.7560688175252,10.9374082827446,
12.));
#179535=CARTESIAN_POINT('Ctrl Pts',(-21.74093105488,10.9201323997386,12.));
#179536=CARTESIAN_POINT('Ctrl Pts',(-21.7258108748874,10.9029637747341,
12.));
#179537=CARTESIAN_POINT('Ctrl Pts',(-21.7107089564822,10.8859026661292,
12.));
#179538=CARTESIAN_POINT('Ctrl Pts',(-21.6956259856667,10.8689493334093,
12.));
#179539=CARTESIAN_POINT('Ctrl Pts',(-21.6805626556461,10.8521040371832,
12.));
#179540=CARTESIAN_POINT('Ctrl Pts',(-21.6655196669727,10.835367039227,12.));
#179541=CARTESIAN_POINT('Ctrl Pts',(-21.6504977276864,10.8187386025135,
12.));
#179542=CARTESIAN_POINT('Ctrl Pts',(-21.6354975534557,10.8022189912369,
12.));
#179543=CARTESIAN_POINT('Ctrl Pts',(-21.6205198677176,10.7858084708262,
12.));
#179544=CARTESIAN_POINT('Ctrl Pts',(-21.6055654018179,10.7695073079554,
12.));
#179545=CARTESIAN_POINT('Ctrl Pts',(-21.5906348951745,10.7533157705943,
12.));
#179546=CARTESIAN_POINT('Ctrl Pts',(-21.5757290954372,10.7372341280468,
12.));
#179547=CARTESIAN_POINT('Ctrl Pts',(-21.5608487586467,10.7212626509816,
12.));
#179548=CARTESIAN_POINT('Ctrl Pts',(-21.5459946493955,10.7054016114571,
12.));
#179549=CARTESIAN_POINT('Ctrl Pts',(-21.531167540981,10.689651282929,12.));
#179550=CARTESIAN_POINT('Ctrl Pts',(-21.5163682155805,10.6740119402835,
12.));
#179551=CARTESIAN_POINT('Ctrl Pts',(-21.5015974644454,10.658483859894,12.));
#179552=CARTESIAN_POINT('Ctrl Pts',(-21.4868560880893,10.6430673196609,
12.));
#179553=CARTESIAN_POINT('Ctrl Pts',(-21.4721448964766,10.6277625990457,
12.));
#179554=CARTESIAN_POINT('Ctrl Pts',(-21.4574647092093,10.612569979096,12.));
#179555=CARTESIAN_POINT('Ctrl Pts',(-21.4428163557137,10.597489742462,12.));
#179556=CARTESIAN_POINT('Ctrl Pts',(-21.4282006754624,10.582522173457,12.));
#179557=CARTESIAN_POINT('Ctrl Pts',(-21.4136185181974,10.5676675581106,
12.));
#179558=CARTESIAN_POINT('Ctrl Pts',(-21.3990707441495,10.5529261842107,
12.));
#179559=CARTESIAN_POINT('Ctrl Pts',(-21.3845582242604,10.5382983413422,
12.));
#179560=CARTESIAN_POINT('Ctrl Pts',(-21.3700818403942,10.523784320906,12.));
#179561=CARTESIAN_POINT('Ctrl Pts',(-21.3556424855822,10.5093844161689,
12.));
#179562=CARTESIAN_POINT('Ctrl Pts',(-21.3412410642912,10.4950989223341,
12.));
#179563=CARTESIAN_POINT('Ctrl Pts',(-21.3268784926823,10.4809281365933,
12.));
#179564=CARTESIAN_POINT('Ctrl Pts',(-21.312555698873,10.4668723581768,12.));
#179565=CARTESIAN_POINT('Ctrl Pts',(-21.2982736231924,10.452931888387,12.));
#179566=CARTESIAN_POINT('Ctrl Pts',(-21.2840332184471,10.4391070306385,
12.));
#179567=CARTESIAN_POINT('Ctrl Pts',(-21.2698354502391,10.4253980905394,
12.));
#179568=CARTESIAN_POINT('Ctrl Pts',(-21.2556812972741,10.4118053759584,
12.));
#179569=CARTESIAN_POINT('Ctrl Pts',(-21.2415717516713,10.3983291970846,
12.));
#179570=CARTESIAN_POINT('Ctrl Pts',(-21.2275078192708,10.384969866479,12.));
#179571=CARTESIAN_POINT('Ctrl Pts',(-21.2134905199359,10.3717276991137,
12.));
#179572=CARTESIAN_POINT('Ctrl Pts',(-21.1995208879205,10.3586030124595,
12.));
#179573=CARTESIAN_POINT('Ctrl Pts',(-21.1855999722427,10.3455961265706,
12.));
#179574=CARTESIAN_POINT('Ctrl Pts',(-21.1717288370512,10.3327073641574,
12.));
#179575=CARTESIAN_POINT('Ctrl Pts',(-21.1579085619959,10.3199370506541,
12.));
#179576=CARTESIAN_POINT('Ctrl Pts',(-21.1441402425831,10.307285514268,12.));
#179577=CARTESIAN_POINT('Ctrl Pts',(-21.130424990599,10.2947530860714,12.));
#179578=CARTESIAN_POINT('Ctrl Pts',(-21.1167639345623,10.2823401001067,
12.));
#179579=CARTESIAN_POINT('Ctrl Pts',(-21.1031582201625,10.2700468934743,
12.));
#179580=CARTESIAN_POINT('Ctrl Pts',(-21.0896090107066,10.2578738064183,
12.));
#179581=CARTESIAN_POINT('Ctrl Pts',(-21.0761174875448,10.2458211823915,
12.));
#179582=CARTESIAN_POINT('Ctrl Pts',(-21.0626848505665,10.233889368157,12.));
#179583=CARTESIAN_POINT('Ctrl Pts',(-21.0493123187483,10.2220787139157,
12.));
#179584=CARTESIAN_POINT('Ctrl Pts',(-21.0360011306814,10.2103895734123,
12.));
#179585=CARTESIAN_POINT('Ctrl Pts',(-21.0227525451107,10.1988223040425,
12.));
#179586=CARTESIAN_POINT('Ctrl Pts',(-21.0095678414486,10.1873772669358,
12.));
#179587=CARTESIAN_POINT('Ctrl Pts',(-20.9964483203685,10.1760548270765,
12.));
#179588=CARTESIAN_POINT('Ctrl Pts',(-20.9833953044737,10.1648553534567,
12.));
#179589=CARTESIAN_POINT('Ctrl Pts',(-20.970410138937,10.1537792192065,12.));
#179590=CARTESIAN_POINT('Ctrl Pts',(-20.9574941921591,10.1428268017257,
12.));
#179591=CARTESIAN_POINT('Ctrl Pts',(-20.944648856393,10.1319984827909,12.));
#179592=CARTESIAN_POINT('Ctrl Pts',(-20.931875548473,10.1212946487057,12.));
#179593=CARTESIAN_POINT('Ctrl Pts',(-20.9191757106266,10.1107156904836,
12.));
#179594=CARTESIAN_POINT('Ctrl Pts',(-20.9065508112556,10.1002620040076,
12.));
#179595=CARTESIAN_POINT('Ctrl Pts',(-20.8940023457371,10.0899339901916,
12.));
#179596=CARTESIAN_POINT('Ctrl Pts',(-20.8815318371844,10.0797320551154,
12.));
#179597=CARTESIAN_POINT('Ctrl Pts',(-20.8691408373705,10.0696566102219,
12.));
#179598=CARTESIAN_POINT('Ctrl Pts',(-20.856830927732,10.0597080725375,12.));
#179599=CARTESIAN_POINT('Ctrl Pts',(-20.8446037203402,10.0498868648733,
12.));
#179600=CARTESIAN_POINT('Ctrl Pts',(-20.8324608588906,10.0401934160234,
12.));
#179601=CARTESIAN_POINT('Ctrl Pts',(-20.8204040196599,10.0306281609435,
12.));
#179602=CARTESIAN_POINT('Ctrl Pts',(-20.8084349126885,10.0211915410095,
12.));
#179603=CARTESIAN_POINT('Ctrl Pts',(-20.7965552829907,10.0118840042786,
12.));
#179604=CARTESIAN_POINT('Ctrl Pts',(-20.7847669117568,10.0027060057389,
12.));
#179605=CARTESIAN_POINT('Ctrl Pts',(-20.7730716175417,9.99365800754638,
12.));
#179606=CARTESIAN_POINT('Ctrl Pts',(-20.7614712574989,9.98474047926846,
12.));
#179607=CARTESIAN_POINT('Ctrl Pts',(-20.7499677289625,9.97595389823461,
12.));
#179608=CARTESIAN_POINT('Ctrl Pts',(-20.7385629709795,9.96729874986198,
12.));
#179609=CARTESIAN_POINT('Ctrl Pts',(-20.7272589658752,9.95877552798403,
12.));
#179610=CARTESIAN_POINT('Ctrl Pts',(-20.716057740758,9.95038473514962,12.));
#179611=CARTESIAN_POINT('Ctrl Pts',(-20.7049613692237,9.94212688298251,
12.));
#179612=CARTESIAN_POINT('Ctrl Pts',(-20.6939719732485,9.93400249259736,
12.));
#179613=CARTESIAN_POINT('Ctrl Pts',(-20.6830917250255,9.9260120949875,12.));
#179614=CARTESIAN_POINT('Ctrl Pts',(-20.6723228488262,9.91815623141284,
12.));
#179615=CARTESIAN_POINT('Ctrl Pts',(-20.6616676228315,9.91043545377004,
12.));
#179616=CARTESIAN_POINT('Ctrl Pts',(-20.6511283817415,9.90285032516696,
12.));
#179617=CARTESIAN_POINT('Ctrl Pts',(-20.6407075193977,9.89540142049124,
12.));
#179618=CARTESIAN_POINT('Ctrl Pts',(-20.6304074914086,9.88808932697305,
12.));
#179619=CARTESIAN_POINT('Ctrl Pts',(-20.6202308177472,9.88091464472669,
12.));
#179620=CARTESIAN_POINT('Ctrl Pts',(-20.6101800854491,9.87387798732944,
12.));
#179621=CARTESIAN_POINT('Ctrl Pts',(-20.6002579513696,9.86697998242612,
12.));
#179622=CARTESIAN_POINT('Ctrl Pts',(-20.5904671449754,9.86022127232749,
12.));
#179623=CARTESIAN_POINT('Ctrl Pts',(-20.580810471002,9.85360251457004,12.));
#179624=CARTESIAN_POINT('Ctrl Pts',(-20.5712908125145,9.84712438256308,
12.));
#179625=CARTESIAN_POINT('Ctrl Pts',(-20.5619111362406,9.84078756677589,
12.));
#179626=CARTESIAN_POINT('Ctrl Pts',(-20.5526744976461,9.83459277585321,
12.));
#179627=CARTESIAN_POINT('Ctrl Pts',(-20.5435840460717,9.82854073773857,
12.));
#179628=CARTESIAN_POINT('Ctrl Pts',(-20.534643029951,9.82263220080328,12.));
#179629=CARTESIAN_POINT('Ctrl Pts',(-20.5258548000625,9.81686793455918,
12.));
#179630=CARTESIAN_POINT('Ctrl Pts',(-20.5172228122839,9.81124873025278,
12.));
#179631=CARTESIAN_POINT('Ctrl Pts',(-20.5087506310507,9.80577540161103,
12.));
#179632=CARTESIAN_POINT('Ctrl Pts',(-20.500441931211,9.80044878520967,12.));
#179633=CARTESIAN_POINT('Ctrl Pts',(-20.4923005087945,9.79526974288344,
12.));
#179634=CARTESIAN_POINT('Ctrl Pts',(-20.4843302955329,9.7902391649866,12.));
#179635=CARTESIAN_POINT('Ctrl Pts',(-20.4765353711585,9.78535797314162,
12.));
#179636=CARTESIAN_POINT('Ctrl Pts',(-20.4689199790668,9.78062712373313,
12.));
#179637=CARTESIAN_POINT('Ctrl Pts',(-20.4614885274973,9.77604760815523,
12.));
#179638=CARTESIAN_POINT('Ctrl Pts',(-20.4542455817527,9.7716204510407,12.));
#179639=CARTESIAN_POINT('Ctrl Pts',(-20.447195862298,9.76734670980897,12.));
#179640=CARTESIAN_POINT('Ctrl Pts',(-20.4403442329401,9.76322747195502,
12.));
#179641=CARTESIAN_POINT('Ctrl Pts',(-20.4336957355474,9.7592638628993,12.));
#179642=CARTESIAN_POINT('Ctrl Pts',(-20.4272556476629,9.75545705902416,
12.));
#179643=CARTESIAN_POINT('Ctrl Pts',(-20.4210295275818,9.75180829786433,
12.));
#179644=CARTESIAN_POINT('Ctrl Pts',(-20.4150232777393,9.74831889242175,
12.));
#179645=CARTESIAN_POINT('Ctrl Pts',(-20.4092430879861,9.74499021838536,
12.));
#179646=CARTESIAN_POINT('Ctrl Pts',(-20.4036953576549,9.74182369656272,
12.));
#179647=CARTESIAN_POINT('Ctrl Pts',(-20.3983866213331,9.73882077613206,
12.));
#179648=CARTESIAN_POINT('Ctrl Pts',(-20.3933234845646,9.7359829201425,12.));
#179649=CARTESIAN_POINT('Ctrl Pts',(-20.3885129129912,9.73331167102812,
12.));
#179650=CARTESIAN_POINT('Ctrl Pts',(-20.3839624556742,9.73080870123726,
12.));
#179651=CARTESIAN_POINT('Ctrl Pts',(-20.3796805893304,9.72847589116533,
12.));
#179652=CARTESIAN_POINT('Ctrl Pts',(-20.3756766651952,9.72631531732871,
12.));
#179653=CARTESIAN_POINT('Ctrl Pts',(-20.371960235676,9.72432910043193,12.));
#179654=CARTESIAN_POINT('Ctrl Pts',(-20.3685406190576,9.72251930722504,
12.));
#179655=CARTESIAN_POINT('Ctrl Pts',(-20.3654261611055,9.72088778381102,
12.));
#179656=CARTESIAN_POINT('Ctrl Pts',(-20.362625691398,9.71943648548114,12.));
#179657=CARTESIAN_POINT('Ctrl Pts',(-20.3601498764344,9.71816778327999,
12.));
#179658=CARTESIAN_POINT('Ctrl Pts',(-20.3580133103357,9.71708493723061,
12.));
#179659=CARTESIAN_POINT('Ctrl Pts',(-20.3562337557875,9.71619192554147,
12.));
#179660=CARTESIAN_POINT('Ctrl Pts',(-20.3548282742361,9.71549257088175,
12.));
#179661=CARTESIAN_POINT('Ctrl Pts',(-20.3538098605706,9.71498978052101,
12.));
#179662=CARTESIAN_POINT('Ctrl Pts',(-20.3533097561886,9.71474590350791,
12.));
#179663=CARTESIAN_POINT('Ctrl Pts',(-20.3531126095522,9.71465227853122,
12.));
#179664=CARTESIAN_POINT('Ctrl Pts',(-20.353060251684,9.71462954053074,12.));
#179665=CARTESIAN_POINT('Ctrl Pts',(-20.353053841303,9.71462809124917,12.));
#179666=CARTESIAN_POINT('',(-19.84920021178,9.47413589477549,12.));
#179667=CARTESIAN_POINT('',(-9.70154690100589,4.63060338698782,12.));
#179668=CARTESIAN_POINT('',(-19.6085639972844,8.81783521984851,12.));
#179669=CARTESIAN_POINT('Origin',(-20.0645771135003,9.02290115519382,12.));
#179670=CARTESIAN_POINT('',(-20.1004996511507,7.63019749246978,12.));
#179671=CARTESIAN_POINT('Origin',(-7.08841632778408E-13,3.26562511982935E-13,
12.));
#179672=CARTESIAN_POINT('',(-20.7347298079577,7.33627833380047,12.));
#179673=CARTESIAN_POINT('Origin',(-20.56795313141,7.80764394578303,12.));
#179674=CARTESIAN_POINT('',(-21.2610617890679,7.52250298901265,12.));
#179675=CARTESIAN_POINT('',(-10.6305308945339,3.76125149450631,12.));
#179676=CARTESIAN_POINT('',(-24.9347862158358,7.36589684767345,12.));
#179677=CARTESIAN_POINT('Ctrl Pts',(-21.2610617890679,7.52250298901265,
12.));
#179678=CARTESIAN_POINT('Ctrl Pts',(-21.2610673466883,7.52250649703992,
12.));
#179679=CARTESIAN_POINT('Ctrl Pts',(-21.261120447486,7.52252744144958,12.));
#179680=CARTESIAN_POINT('Ctrl Pts',(-21.2613260540651,7.52260064231736,
12.));
#179681=CARTESIAN_POINT('Ctrl Pts',(-21.261852128355,7.52278182242727,12.));
#179682=CARTESIAN_POINT('Ctrl Pts',(-21.262927782038,7.52314642316202,12.));
#179683=CARTESIAN_POINT('Ctrl Pts',(-21.2644161259965,7.52364573027521,
12.));
#179684=CARTESIAN_POINT('Ctrl Pts',(-21.266305915706,7.52427261074264,12.));
#179685=CARTESIAN_POINT('Ctrl Pts',(-21.2685823838672,7.52501770333522,
12.));
#179686=CARTESIAN_POINT('Ctrl Pts',(-21.2712301573465,7.52587126095544,
12.));
#179687=CARTESIAN_POINT('Ctrl Pts',(-21.2742366113578,7.5268252691856,12.));
#179688=CARTESIAN_POINT('Ctrl Pts',(-21.2775925269651,7.52787386225343,
12.));
#179689=CARTESIAN_POINT('Ctrl Pts',(-21.2812902781143,7.52901217930407,
12.));
#179690=CARTESIAN_POINT('Ctrl Pts',(-21.2853226580658,7.53023562438221,
12.));
#179691=CARTESIAN_POINT('Ctrl Pts',(-21.2896816163843,7.53153906987847,
12.));
#179692=CARTESIAN_POINT('Ctrl Pts',(-21.2943588989331,7.53291726078526,
12.));
#179693=CARTESIAN_POINT('Ctrl Pts',(-21.2993464250717,7.53436505309949,
12.));
#179694=CARTESIAN_POINT('Ctrl Pts',(-21.3046368712156,7.53587778251743,
12.));
#179695=CARTESIAN_POINT('Ctrl Pts',(-21.3102237167729,7.53745129364619,
12.));
#179696=CARTESIAN_POINT('Ctrl Pts',(-21.3161009456256,7.53908175169899,
12.));
#179697=CARTESIAN_POINT('Ctrl Pts',(-21.3222628524165,7.5407655203828,12.));
#179698=CARTESIAN_POINT('Ctrl Pts',(-21.328703791771,7.54249900377031,12.));
#179699=CARTESIAN_POINT('Ctrl Pts',(-21.3354182340149,7.54427868151268,
12.));
#179700=CARTESIAN_POINT('Ctrl Pts',(-21.3424008295038,7.54610114948351,
12.));
#179701=CARTESIAN_POINT('Ctrl Pts',(-21.349646476153,7.54796316246327,12.));
#179702=CARTESIAN_POINT('Ctrl Pts',(-21.3571503685853,7.54986166521306,
12.));
#179703=CARTESIAN_POINT('Ctrl Pts',(-21.3649079431864,7.55179375777441,
12.));
#179704=CARTESIAN_POINT('Ctrl Pts',(-21.3729148390244,7.55375667080032,
12.));
#179705=CARTESIAN_POINT('Ctrl Pts',(-21.3811668478933,7.55574773403507,
12.));
#179706=CARTESIAN_POINT('Ctrl Pts',(-21.3896598842119,7.55776435731422,
12.));
#179707=CARTESIAN_POINT('Ctrl Pts',(-21.3983899952988,7.55980403700615,
12.));
#179708=CARTESIAN_POINT('Ctrl Pts',(-21.4073533630364,7.56186435703622,
12.));
#179709=CARTESIAN_POINT('Ctrl Pts',(-21.4165463106252,7.56394299313682,
12.));
#179710=CARTESIAN_POINT('Ctrl Pts',(-21.4259653015732,7.56603771218706,
12.));
#179711=CARTESIAN_POINT('Ctrl Pts',(-21.435606926151,7.56814636360842,12.));
#179712=CARTESIAN_POINT('Ctrl Pts',(-21.445467890751,7.57026687261169,12.));
#179713=CARTESIAN_POINT('Ctrl Pts',(-21.4555450053147,7.57239723223521,
12.));
#179714=CARTESIAN_POINT('Ctrl Pts',(-21.4658351740135,7.57453549743435,
12.));
#179715=CARTESIAN_POINT('Ctrl Pts',(-21.4763353936766,7.57667978403002,
12.));
#179716=CARTESIAN_POINT('Ctrl Pts',(-21.4870427508193,7.57882826679131,
12.));
#179717=CARTESIAN_POINT('Ctrl Pts',(-21.497954419274,7.5809791779073,12.));
#179718=CARTESIAN_POINT('Ctrl Pts',(-21.5090676573866,7.58313080519158,
12.));
#179719=CARTESIAN_POINT('Ctrl Pts',(-21.5203798035294,7.58528148919113,
12.));
#179720=CARTESIAN_POINT('Ctrl Pts',(-21.5318882716735,7.58742962034834,
12.));
#179721=CARTESIAN_POINT('Ctrl Pts',(-21.5435905470113,7.58957363620026,
12.));
#179722=CARTESIAN_POINT('Ctrl Pts',(-21.5554841813465,7.59171201844793,
12.));
#179723=CARTESIAN_POINT('Ctrl Pts',(-21.5675667904728,7.5938432912493,12.));
#179724=CARTESIAN_POINT('Ctrl Pts',(-21.5798360518978,7.59596601973588,
12.));
#179725=CARTESIAN_POINT('Ctrl Pts',(-21.5922897024466,7.59807880846192,
12.));
#179726=CARTESIAN_POINT('Ctrl Pts',(-21.6049255358843,7.60018029988238,
12.));
#179727=CARTESIAN_POINT('Ctrl Pts',(-21.6177414005991,7.60226917285432,
12.));
#179728=CARTESIAN_POINT('Ctrl Pts',(-21.6307351973823,7.604344141183,12.));
#179729=CARTESIAN_POINT('Ctrl Pts',(-21.6439048771743,7.60640395216358,
12.));
#179730=CARTESIAN_POINT('Ctrl Pts',(-21.6572484388079,7.60844738512872,
12.));
#179731=CARTESIAN_POINT('Ctrl Pts',(-21.6707639267573,7.6104732500095,12.));
#179732=CARTESIAN_POINT('Ctrl Pts',(-21.6844494295813,7.61248038630265,
12.));
#179733=CARTESIAN_POINT('Ctrl Pts',(-21.6983030783321,7.61446766202787,
12.));
#179734=CARTESIAN_POINT('Ctrl Pts',(-21.7123230449835,7.61643397270425,
12.));
#179735=CARTESIAN_POINT('Ctrl Pts',(-21.7265075407977,7.61837824030541,
12.));
#179736=CARTESIAN_POINT('Ctrl Pts',(-21.7408548148657,7.62029941230855,
12.));
#179737=CARTESIAN_POINT('Ctrl Pts',(-21.7553631528329,7.62219646084226,
12.));
#179738=CARTESIAN_POINT('Ctrl Pts',(-21.7700308755583,7.62406838181164,
12.));
#179739=CARTESIAN_POINT('Ctrl Pts',(-21.7848563378022,7.62591419404521,
12.));
#179740=CARTESIAN_POINT('Ctrl Pts',(-21.7998379268583,7.62773293842409,
12.));
#179741=CARTESIAN_POINT('Ctrl Pts',(-21.8149740615093,7.62952367718151,
12.));
#179742=CARTESIAN_POINT('Ctrl Pts',(-21.8302631910197,7.6312854932304,12.));
#179743=CARTESIAN_POINT('Ctrl Pts',(-21.8457037941084,7.63301748948936,
12.));
#179744=CARTESIAN_POINT('Ctrl Pts',(-21.8612943779086,7.63471878821203,
12.));
#179745=CARTESIAN_POINT('Ctrl Pts',(-21.8770334769492,7.63638853033367,
12.));
#179746=CARTESIAN_POINT('Ctrl Pts',(-21.8929196523511,7.63802587492007,
12.));
#179747=CARTESIAN_POINT('Ctrl Pts',(-21.9089514909873,7.63962999860916,
12.));
#179748=CARTESIAN_POINT('Ctrl Pts',(-21.9251276046546,7.6412000950654,12.));
#179749=CARTESIAN_POINT('Ctrl Pts',(-21.9414466292074,7.64273537442706,
12.));
#179750=CARTESIAN_POINT('Ctrl Pts',(-21.9579072237653,7.64423506279153,
12.));
#179751=CARTESIAN_POINT('Ctrl Pts',(-21.97450807008,7.64569840177359,12.));
#179752=CARTESIAN_POINT('Ctrl Pts',(-21.9912478718542,7.64712464805258,
12.));
#179753=CARTESIAN_POINT('Ctrl Pts',(-22.0081253540773,7.64851307293346,
12.));
#179754=CARTESIAN_POINT('Ctrl Pts',(-22.0251392623209,7.64986296190156,
12.));
#179755=CARTESIAN_POINT('Ctrl Pts',(-22.0422883621176,7.65117361421346,
12.));
#179756=CARTESIAN_POINT('Ctrl Pts',(-22.0595714384432,7.65244434253104,
12.));
#179757=CARTESIAN_POINT('Ctrl Pts',(-22.0769872951596,7.65367447254945,
12.));
#179758=CARTESIAN_POINT('Ctrl Pts',(-22.094534754469,7.6548633426365,12.));
#179759=CARTESIAN_POINT('Ctrl Pts',(-22.1122126563327,7.65601030346819,
12.));
#179760=CARTESIAN_POINT('Ctrl Pts',(-22.1300198579671,7.65711471769407,
12.));
#179761=CARTESIAN_POINT('Ctrl Pts',(-22.1479552334206,7.65817595963351,
12.));
#179762=CARTESIAN_POINT('Ctrl Pts',(-22.1660176731174,7.65919341496925,
12.));
#179763=CARTESIAN_POINT('Ctrl Pts',(-22.1842060834092,7.66016648045008,
12.));
#179764=CARTESIAN_POINT('Ctrl Pts',(-22.2025193860972,7.66109456359292,
12.));
#179765=CARTESIAN_POINT('Ctrl Pts',(-22.2209565180098,7.66197708240435,
12.));
#179766=CARTESIAN_POINT('Ctrl Pts',(-22.239516430656,7.66281346512545,12.));
#179767=CARTESIAN_POINT('Ctrl Pts',(-22.2581980898487,7.66360314997662,
12.));
#179768=CARTESIAN_POINT('Ctrl Pts',(-22.2770004753332,7.66434558490972,
12.));
#179769=CARTESIAN_POINT('Ctrl Pts',(-22.2959225803925,7.66504022736262,
12.));
#179770=CARTESIAN_POINT('Ctrl Pts',(-22.3149634114823,7.66568654402441,
12.));
#179771=CARTESIAN_POINT('Ctrl Pts',(-22.3341219879454,7.66628401061905,
12.));
#179772=CARTESIAN_POINT('Ctrl Pts',(-22.3533973417013,7.66683211169134,
12.));
#179773=CARTESIAN_POINT('Ctrl Pts',(-22.3727885169361,7.66733034039887,
12.));
#179774=CARTESIAN_POINT('Ctrl Pts',(-22.3922945697782,7.66777819830819,
12.));
#179775=CARTESIAN_POINT('Ctrl Pts',(-22.411914567977,7.66817519519682,12.));
#179776=CARTESIAN_POINT('Ctrl Pts',(-22.4316475906616,7.66852084886745,
12.));
#179777=CARTESIAN_POINT('Ctrl Pts',(-22.4514927280863,7.6688146849666,12.));
#179778=CARTESIAN_POINT('Ctrl Pts',(-22.47144908137,7.66905623680835,12.));
#179779=CARTESIAN_POINT('Ctrl Pts',(-22.4915157622308,7.66924504520302,
12.));
#179780=CARTESIAN_POINT('Ctrl Pts',(-22.5116918927023,7.66938065829082,
12.));
#179781=CARTESIAN_POINT('Ctrl Pts',(-22.5319766049191,7.66946263138116,
12.));
#179782=CARTESIAN_POINT('Ctrl Pts',(-22.5523690409109,7.66949052679671,
12.));
#179783=CARTESIAN_POINT('Ctrl Pts',(-22.5728683523829,7.66946391372299,
12.));
#179784=CARTESIAN_POINT('Ctrl Pts',(-22.5934737004955,7.66938236806241,
12.));
#179785=CARTESIAN_POINT('Ctrl Pts',(-22.6141842556248,7.66924547229435,
12.));
#179786=CARTESIAN_POINT('Ctrl Pts',(-22.6349991971547,7.66905281533745,
12.));
#179787=CARTESIAN_POINT('Ctrl Pts',(-22.6559177133133,7.66880399241354,
12.));
#179788=CARTESIAN_POINT('Ctrl Pts',(-22.6769390009889,7.66849860491763,
12.));
#179789=CARTESIAN_POINT('Ctrl Pts',(-22.6980622655446,7.66813626029276,
12.));
#179790=CARTESIAN_POINT('Ctrl Pts',(-22.7192867206242,7.6677165719101,12.));
#179791=CARTESIAN_POINT('Ctrl Pts',(-22.7406115879508,7.66723915895412,
12.));
#179792=CARTESIAN_POINT('Ctrl Pts',(-22.7620360971839,7.66670364630273,
12.));
#179793=CARTESIAN_POINT('Ctrl Pts',(-22.7835594857697,7.66610966441259,
12.));
#179794=CARTESIAN_POINT('Ctrl Pts',(-22.8051809987834,7.66545684920987,
12.));
#179795=CARTESIAN_POINT('Ctrl Pts',(-22.8268998887679,7.66474484198553,
12.));
#179796=CARTESIAN_POINT('Ctrl Pts',(-22.8487154155569,7.66397328929805,
12.));
#179797=CARTESIAN_POINT('Ctrl Pts',(-22.870626846128,7.66314184287334,12.));
#179798=CARTESIAN_POINT('Ctrl Pts',(-22.8926334544879,7.66225015950147,
12.));
#179799=CARTESIAN_POINT('Ctrl Pts',(-22.9147345215418,7.661297900941,12.));
#179800=CARTESIAN_POINT('Ctrl Pts',(-22.9369293349592,7.66028473382777,
12.));
#179801=CARTESIAN_POINT('Ctrl Pts',(-22.9592171890332,7.65921032958912,
12.));
#179802=CARTESIAN_POINT('Ctrl Pts',(-22.9815973845301,7.65807436436453,
12.));
#179803=CARTESIAN_POINT('Ctrl Pts',(-23.004069228582,7.6568765189133,12.));
#179804=CARTESIAN_POINT('Ctrl Pts',(-23.0266320345792,7.65561647852555,
12.));
#179805=CARTESIAN_POINT('Ctrl Pts',(-23.049285122053,7.65429393293955,12.));
#179806=CARTESIAN_POINT('Ctrl Pts',(-23.072027816555,7.65290857626356,12.));
#179807=CARTESIAN_POINT('Ctrl Pts',(-23.0948594495246,7.65146010690464,
12.));
#179808=CARTESIAN_POINT('Ctrl Pts',(-23.1177793581674,7.64994822749845,
12.));
#179809=CARTESIAN_POINT('Ctrl Pts',(-23.1407868853815,7.64837264482929,
12.));
#179810=CARTESIAN_POINT('Ctrl Pts',(-23.1638813796691,7.64673306975797,
12.));
#179811=CARTESIAN_POINT('Ctrl Pts',(-23.1870621950452,7.64502921715483,
12.));
#179812=CARTESIAN_POINT('Ctrl Pts',(-23.2103286909399,7.64326080583684,
12.));
#179813=CARTESIAN_POINT('Ctrl Pts',(-23.2336802320912,7.64142755851508,
12.));
#179814=CARTESIAN_POINT('Ctrl Pts',(-23.2571161884487,7.63952920172837,
12.));
#179815=CARTESIAN_POINT('Ctrl Pts',(-23.2806359350853,7.63756546576375,
12.));
#179816=CARTESIAN_POINT('Ctrl Pts',(-23.3042388521021,7.63553608458784,
12.));
#179817=CARTESIAN_POINT('Ctrl Pts',(-23.3279243245241,7.63344079578162,
12.));
#179818=CARTESIAN_POINT('Ctrl Pts',(-23.3516917421973,7.63127934048139,
12.));
#179819=CARTESIAN_POINT('Ctrl Pts',(-23.3755404996638,7.62905146332598,
12.));
#179820=CARTESIAN_POINT('Ctrl Pts',(-23.3994699961122,7.62675691240335,
12.));
#179821=CARTESIAN_POINT('Ctrl Pts',(-23.4234796353544,7.62439543920054,
12.));
#179822=CARTESIAN_POINT('Ctrl Pts',(-23.4475688257854,7.62196679855957,
12.));
#179823=CARTESIAN_POINT('Ctrl Pts',(-23.4717369803438,7.61947074863977,
12.));
#179824=CARTESIAN_POINT('Ctrl Pts',(-23.4959835164608,7.61690705088319,
12.));
#179825=CARTESIAN_POINT('Ctrl Pts',(-23.5203078560128,7.61427546999299,
12.));
#179826=CARTESIAN_POINT('Ctrl Pts',(-23.5447094252029,7.61157577385372,
12.));
#179827=CARTESIAN_POINT('Ctrl Pts',(-23.5691876544243,7.60880773344599,
12.));
#179828=CARTESIAN_POINT('Ctrl Pts',(-23.5937419781244,7.60597112277094,
12.));
#179829=CARTESIAN_POINT('Ctrl Pts',(-23.6183718346576,7.60306571877806,
12.));
#179830=CARTESIAN_POINT('Ctrl Pts',(-23.6430766661419,7.60009130130129,
12.));
#179831=CARTESIAN_POINT('Ctrl Pts',(-23.6678559182876,7.59704765299572,
12.));
#179832=CARTESIAN_POINT('Ctrl Pts',(-23.6927090405067,7.59393455934042,
12.));
#179833=CARTESIAN_POINT('Ctrl Pts',(-23.7176354860457,7.59075180865327,
12.));
#179834=CARTESIAN_POINT('Ctrl Pts',(-23.7426347121006,7.58749919210832,
12.));
#179835=CARTESIAN_POINT('Ctrl Pts',(-23.7677061799376,7.58417650376272,
12.));
#179836=CARTESIAN_POINT('Ctrl Pts',(-23.7928493549908,7.58078354058212,
12.));
#179837=CARTESIAN_POINT('Ctrl Pts',(-23.8180637069977,7.57732010249066,
12.));
#179838=CARTESIAN_POINT('Ctrl Pts',(-23.8433487096134,7.57378599219816,
12.));
#179839=CARTESIAN_POINT('Ctrl Pts',(-23.8687038399598,7.57018101500711,
12.));
#179840=CARTESIAN_POINT('Ctrl Pts',(-23.8941285782003,7.56650497863792,
12.));
#179841=CARTESIAN_POINT('Ctrl Pts',(-23.9196224070759,7.56275769304773,
12.));
#179842=CARTESIAN_POINT('Ctrl Pts',(-23.9451848115,7.55893897027682,12.));
#179843=CARTESIAN_POINT('Ctrl Pts',(-23.9708152779884,7.55504862424812,
12.));
#179844=CARTESIAN_POINT('Ctrl Pts',(-23.9965132953185,7.55108647097441,
12.));
#179845=CARTESIAN_POINT('Ctrl Pts',(-24.022278355453,7.5470523288591,12.));
#179846=CARTESIAN_POINT('Ctrl Pts',(-24.0481099543353,7.54294601896144,
12.));
#179847=CARTESIAN_POINT('Ctrl Pts',(-24.0740075927985,7.53876736531014,
12.));
#179848=CARTESIAN_POINT('Ctrl Pts',(-24.0999707772642,7.53451619514649,
12.));
#179849=CARTESIAN_POINT('Ctrl Pts',(-24.1259990209207,7.53019233935501,
12.));
#179850=CARTESIAN_POINT('Ctrl Pts',(-24.1520918425364,7.52579563201424,
12.));
#179851=CARTESIAN_POINT('Ctrl Pts',(-24.1782487641594,7.52132590953802,
12.));
#179852=CARTESIAN_POINT('Ctrl Pts',(-24.2044693092349,7.51678300997949,
12.));
#179853=CARTESIAN_POINT('Ctrl Pts',(-24.2307530003887,7.51216677222181,
12.));
#179854=CARTESIAN_POINT('Ctrl Pts',(-24.2570993577034,7.50747703535133,
12.));
#179855=CARTESIAN_POINT('Ctrl Pts',(-24.2835078958973,7.50271363765152,
12.));
#179856=CARTESIAN_POINT('Ctrl Pts',(-24.3099781253355,7.49787641695439,
12.));
#179857=CARTESIAN_POINT('Ctrl Pts',(-24.3365095573685,7.4929652125242,12.));
#179858=CARTESIAN_POINT('Ctrl Pts',(-24.3631017084524,7.48797986651908,
12.));
#179859=CARTESIAN_POINT('Ctrl Pts',(-24.3897541049254,7.48292022569301,
12.));
#179860=CARTESIAN_POINT('Ctrl Pts',(-24.4164662871163,7.47778614286565,
12.));
#179861=CARTESIAN_POINT('Ctrl Pts',(-24.443237814649,7.47257747883246,12.));
#179862=CARTESIAN_POINT('Ctrl Pts',(-24.4700682684524,7.46729410308786,
12.));
#179863=CARTESIAN_POINT('Ctrl Pts',(-24.4969572391483,7.46193588961463,
12.));
#179864=CARTESIAN_POINT('Ctrl Pts',(-24.5239043173072,7.45650271335862,
12.));
#179865=CARTESIAN_POINT('Ctrl Pts',(-24.5509090831559,7.4509944465116,12.));
#179866=CARTESIAN_POINT('Ctrl Pts',(-24.577971096086,7.44541095473134,12.));
#179867=CARTESIAN_POINT('Ctrl Pts',(-24.6050898852368,7.43975209375504,
12.));
#179868=CARTESIAN_POINT('Ctrl Pts',(-24.6322649369517,7.43401770489524,
12.));
#179869=CARTESIAN_POINT('Ctrl Pts',(-24.6594957128756,7.42820762159126,
12.));
#179870=CARTESIAN_POINT('Ctrl Pts',(-24.6867816727192,7.42232167766265,
12.));
#179871=CARTESIAN_POINT('Ctrl Pts',(-24.7141222950051,7.41635971481674,
12.));
#179872=CARTESIAN_POINT('Ctrl Pts',(-24.7415170994784,7.41032159082382,
12.));
#179873=CARTESIAN_POINT('Ctrl Pts',(-24.7689656668983,7.40420718661603,
12.));
#179874=CARTESIAN_POINT('Ctrl Pts',(-24.7964676646431,7.39801641583013,
12.));
#179875=CARTESIAN_POINT('Ctrl Pts',(-24.8240228520893,7.39174922585808,
12.));
#179876=CARTESIAN_POINT('Ctrl Pts',(-24.8516310625176,7.38540558903621,
12.));
#179877=CARTESIAN_POINT('Ctrl Pts',(-24.8792921911115,7.3789854964027,12.));
#179878=CARTESIAN_POINT('Ctrl Pts',(-24.901463382605,7.37378825961676,12.));
#179879=CARTESIAN_POINT('Ctrl Pts',(-24.9181155530543,7.3698559312009,12.));
#179880=CARTESIAN_POINT('Ctrl Pts',(-24.9292275670674,7.36721909028843,
12.));
#179881=CARTESIAN_POINT('Ctrl Pts',(-24.9347862158358,7.36589684767345,
12.));
#179882=CARTESIAN_POINT('',(-25.2771067246846,6.08833931617699,12.));
#179883=CARTESIAN_POINT('Origin',(0.,0.,12.));
#179884=CARTESIAN_POINT('',(-22.1738711152697,4.11585220600461,12.));
#179885=CARTESIAN_POINT('Ctrl Pts',(-25.2771067246846,6.08833931617699,
12.));
#179886=CARTESIAN_POINT('Ctrl Pts',(-25.2729539149517,6.08441489609793,
12.));
#179887=CARTESIAN_POINT('Ctrl Pts',(-25.2646490489923,6.0765753178749,12.));
#179888=CARTESIAN_POINT('Ctrl Pts',(-25.2521940105705,6.06484373634546,
12.));
#179889=CARTESIAN_POINT('Ctrl Pts',(-25.2355918139032,6.04925720151218,
12.));
#179890=CARTESIAN_POINT('Ctrl Pts',(-25.21484662016,6.02986667389996,12.));
#179891=CARTESIAN_POINT('Ctrl Pts',(-25.1941090269819,6.01056881804612,
12.));
#179892=CARTESIAN_POINT('Ctrl Pts',(-25.1733791296259,5.99136367859754,
12.));
#179893=CARTESIAN_POINT('Ctrl Pts',(-25.1526570863092,5.97225131495616,
12.));
#179894=CARTESIAN_POINT('Ctrl Pts',(-25.1319431317237,5.95323180187378,
12.));
#179895=CARTESIAN_POINT('Ctrl Pts',(-25.1112375971106,5.93430523086834,
12.));
#179896=CARTESIAN_POINT('Ctrl Pts',(-25.0905409050773,5.91547170844447,
12.));
#179897=CARTESIAN_POINT('Ctrl Pts',(-25.0698535426514,5.89673135155514,
12.));
#179898=CARTESIAN_POINT('Ctrl Pts',(-25.0491760405911,5.87808428385365,
12.));
#179899=CARTESIAN_POINT('Ctrl Pts',(-25.0285089498899,5.85953063156826,
12.));
#179900=CARTESIAN_POINT('Ctrl Pts',(-25.0078528200564,5.84107051963071,
12.));
#179901=CARTESIAN_POINT('Ctrl Pts',(-24.9872081752734,5.82270406744198,
12.));
#179902=CARTESIAN_POINT('Ctrl Pts',(-24.9665754954496,5.80443138549726,
12.));
#179903=CARTESIAN_POINT('Ctrl Pts',(-24.945955229334,5.78625257775681,12.));
#179904=CARTESIAN_POINT('Ctrl Pts',(-24.9253478043656,5.76816774342219,
12.));
#179905=CARTESIAN_POINT('Ctrl Pts',(-24.904753637648,5.75017697890804,12.));
#179906=CARTESIAN_POINT('Ctrl Pts',(-24.884173146722,5.73228037976926,12.));
#179907=CARTESIAN_POINT('Ctrl Pts',(-24.8636067597669,5.71447804252027,
12.));
#179908=CARTESIAN_POINT('Ctrl Pts',(-24.8430549277621,5.69677006679444,
12.));
#179909=CARTESIAN_POINT('Ctrl Pts',(-24.8225181223845,5.67915655496542,
12.));
#179910=CARTESIAN_POINT('Ctrl Pts',(-24.8019968304605,5.66163761114921,
12.));
#179911=CARTESIAN_POINT('Ctrl Pts',(-24.781491549672,5.6442133404226,12.));
#179912=CARTESIAN_POINT('Ctrl Pts',(-24.7610027835697,5.62688384790923,
12.));
#179913=CARTESIAN_POINT('Ctrl Pts',(-24.7405310372739,5.60964923798491,
12.));
#179914=CARTESIAN_POINT('Ctrl Pts',(-24.7200768119088,5.59250961323987,
12.));
#179915=CARTESIAN_POINT('Ctrl Pts',(-24.6996406035517,5.57546507427754,
12.));
#179916=CARTESIAN_POINT('Ctrl Pts',(-24.6792229061794,5.55851572025376,
12.));
#179917=CARTESIAN_POINT('Ctrl Pts',(-24.6588242134738,5.54166164919583,
12.));
#179918=CARTESIAN_POINT('Ctrl Pts',(-24.6384450211467,5.52490295840991,
12.));
#179919=CARTESIAN_POINT('Ctrl Pts',(-24.6180858289179,5.50823974481962,
12.));
#179920=CARTESIAN_POINT('Ctrl Pts',(-24.5977471429364,5.49167210537246,
12.));
#179921=CARTESIAN_POINT('Ctrl Pts',(-24.5774294770329,5.47520013724419,
12.));
#179922=CARTESIAN_POINT('Ctrl Pts',(-24.5571333514842,5.45882393762261,
12.));
#179923=CARTESIAN_POINT('Ctrl Pts',(-24.5368592922863,5.4425436035688,12.));
#179924=CARTESIAN_POINT('Ctrl Pts',(-24.5166078302108,5.42635923183419,
12.));
#179925=CARTESIAN_POINT('Ctrl Pts',(-24.4963794999831,5.41027091869241,
12.));
#179926=CARTESIAN_POINT('Ctrl Pts',(-24.4761748393321,5.39427875973824,
12.));
#179927=CARTESIAN_POINT('Ctrl Pts',(-24.4559943883157,5.37838284973695,
12.));
#179928=CARTESIAN_POINT('Ctrl Pts',(-24.435838689915,5.36258328273627,12.));
#179929=CARTESIAN_POINT('Ctrl Pts',(-24.4157082904614,5.34688015213537,
12.));
#179930=CARTESIAN_POINT('Ctrl Pts',(-24.3956037401293,5.33127355076033,
12.));
#179931=CARTESIAN_POINT('Ctrl Pts',(-24.3755255933917,5.31576357092526,
12.));
#179932=CARTESIAN_POINT('Ctrl Pts',(-24.3554744095075,5.30035030449063,
12.));
#179933=CARTESIAN_POINT('Ctrl Pts',(-24.3354507529414,5.28503384290648,
12.));
#179934=CARTESIAN_POINT('Ctrl Pts',(-24.3154551932221,5.26981427718798,
12.));
#179935=CARTESIAN_POINT('Ctrl Pts',(-24.2954883048447,5.25469169788856,
12.));
#179936=CARTESIAN_POINT('Ctrl Pts',(-24.2755506671525,5.23966619506289,
12.));
#179937=CARTESIAN_POINT('Ctrl Pts',(-24.2556428642294,5.22473785822442,
12.));
#179938=CARTESIAN_POINT('Ctrl Pts',(-24.2357654847766,5.20990677629176,
12.));
#179939=CARTESIAN_POINT('Ctrl Pts',(-24.2159191220171,5.19517303753647,
12.));
#179940=CARTESIAN_POINT('Ctrl Pts',(-24.1961043738756,5.18053672961398,
12.));
#179941=CARTESIAN_POINT('Ctrl Pts',(-24.1763218431344,5.16599793957985,
12.));
#179942=CARTESIAN_POINT('Ctrl Pts',(-24.1565721375971,5.15155675390079,
12.));
#179943=CARTESIAN_POINT('Ctrl Pts',(-24.1368558702443,5.13721325845745,
12.));
#179944=CARTESIAN_POINT('Ctrl Pts',(-24.117173659394,5.12296753853857,12.));
#179945=CARTESIAN_POINT('Ctrl Pts',(-24.0975261288444,5.10881967883124,
12.));
#179946=CARTESIAN_POINT('Ctrl Pts',(-24.0779139079264,5.09476976342616,
12.));
#179947=CARTESIAN_POINT('Ctrl Pts',(-24.0583376315636,5.0808178758127,12.));
#179948=CARTESIAN_POINT('Ctrl Pts',(-24.0387979403268,5.06696409886639,
12.));
#179949=CARTESIAN_POINT('Ctrl Pts',(-24.0192954804896,5.05320851483068,
12.));
#179950=CARTESIAN_POINT('Ctrl Pts',(-23.9998309040747,5.03955120528527,
12.));
#179951=CARTESIAN_POINT('Ctrl Pts',(-23.9804048689228,5.02599225112461,
12.));
#179952=CARTESIAN_POINT('Ctrl Pts',(-23.9610180388271,5.01253173257458,
12.));
#179953=CARTESIAN_POINT('Ctrl Pts',(-23.9416710836529,4.99916972919309,
12.));
#179954=CARTESIAN_POINT('Ctrl Pts',(-23.9223646794591,4.98590631986532,
12.));
#179955=CARTESIAN_POINT('Ctrl Pts',(-23.9030995086164,4.97274158279228,
12.));
#179956=CARTESIAN_POINT('Ctrl Pts',(-23.883876259922,4.95967559546565,12.));
#179957=CARTESIAN_POINT('Ctrl Pts',(-23.8646956287172,4.94670843465868,
12.));
#179958=CARTESIAN_POINT('Ctrl Pts',(-23.8455583170062,4.93384017643441,
12.));
#179959=CARTESIAN_POINT('Ctrl Pts',(-23.8264650335721,4.92107089613976,
12.));
#179960=CARTESIAN_POINT('Ctrl Pts',(-23.8074164940897,4.90840066839346,
12.));
#179961=CARTESIAN_POINT('Ctrl Pts',(-23.7884134212381,4.89582956706771,
12.));
#179962=CARTESIAN_POINT('Ctrl Pts',(-23.7694565448044,4.88335766525565,
12.));
#179963=CARTESIAN_POINT('Ctrl Pts',(-23.7505466018239,4.87098503527142,
12.));
#179964=CARTESIAN_POINT('Ctrl Pts',(-23.7316843367308,4.85871174865491,
12.));
#179965=CARTESIAN_POINT('Ctrl Pts',(-23.7128705015014,4.84653787616422,
12.));
#179966=CARTESIAN_POINT('Ctrl Pts',(-23.6941058557971,4.83446348776267,
12.));
#179967=CARTESIAN_POINT('Ctrl Pts',(-23.6753911671023,4.82248865259569,
12.));
#179968=CARTESIAN_POINT('Ctrl Pts',(-23.6567272108631,4.81061343896442,
12.));
#179969=CARTESIAN_POINT('Ctrl Pts',(-23.6381147706581,4.79883791433229,
12.));
#179970=CARTESIAN_POINT('Ctrl Pts',(-23.6195546383625,4.78716214532104,
12.));
#179971=CARTESIAN_POINT('Ctrl Pts',(-23.6010476143099,4.77558619769875,
12.));
#179972=CARTESIAN_POINT('Ctrl Pts',(-23.5825945074535,4.7641101363625,12.));
#179973=CARTESIAN_POINT('Ctrl Pts',(-23.564196135517,4.75273402530615,12.));
#179974=CARTESIAN_POINT('Ctrl Pts',(-23.5458533251715,4.74145792760698,
12.));
#179975=CARTESIAN_POINT('Ctrl Pts',(-23.5275669122378,4.73028190543031,
12.));
#179976=CARTESIAN_POINT('Ctrl Pts',(-23.5093377418784,4.71920602001904,
12.));
#179977=CARTESIAN_POINT('Ctrl Pts',(-23.491166668789,4.7082303316782,12.));
#179978=CARTESIAN_POINT('Ctrl Pts',(-23.4730545573849,4.69735489975023,
12.));
#179979=CARTESIAN_POINT('Ctrl Pts',(-23.4550022819853,4.68657978258297,
12.));
#179980=CARTESIAN_POINT('Ctrl Pts',(-23.4370107270444,4.6759050375305,12.));
#179981=CARTESIAN_POINT('Ctrl Pts',(-23.4190807873798,4.66533072094663,
12.));
#179982=CARTESIAN_POINT('Ctrl Pts',(-23.4012133683957,4.65485688816921,
12.));
#179983=CARTESIAN_POINT('Ctrl Pts',(-23.383409386307,4.64448359349935,12.));
#179984=CARTESIAN_POINT('Ctrl Pts',(-23.3656697683496,4.63421089016554,
12.));
#179985=CARTESIAN_POINT('Ctrl Pts',(-23.3479954530281,4.62403883030823,
12.));
#179986=CARTESIAN_POINT('Ctrl Pts',(-23.3303873903947,4.61396746497848,
12.));
#179987=CARTESIAN_POINT('Ctrl Pts',(-23.3128465423119,4.60399684412174,
12.));
#179988=CARTESIAN_POINT('Ctrl Pts',(-23.295373882719,4.59412701655749,12.));
#179989=CARTESIAN_POINT('Ctrl Pts',(-23.2779703978868,4.58435802994674,
12.));
#179990=CARTESIAN_POINT('Ctrl Pts',(-23.2606370866853,4.5746899307607,12.));
#179991=CARTESIAN_POINT('Ctrl Pts',(-23.2433749609117,4.5651227642781,12.));
#179992=CARTESIAN_POINT('Ctrl Pts',(-23.2261850456055,4.55565657456956,
12.));
#179993=CARTESIAN_POINT('Ctrl Pts',(-23.2090683793627,4.54629140447542,
12.));
#179994=CARTESIAN_POINT('Ctrl Pts',(-23.1920260146474,4.53702729557585,
12.));
#179995=CARTESIAN_POINT('Ctrl Pts',(-23.1750590180923,4.52786428815047,
12.));
#179996=CARTESIAN_POINT('Ctrl Pts',(-23.1581684708778,4.51880242116785,
12.));
#179997=CARTESIAN_POINT('Ctrl Pts',(-23.1413554691136,4.50984173227087,
12.));
#179998=CARTESIAN_POINT('Ctrl Pts',(-23.1246211242117,4.50098225775178,
12.));
#179999=CARTESIAN_POINT('Ctrl Pts',(-23.1079665632629,4.49222403252201,
12.));
#180000=CARTESIAN_POINT('Ctrl Pts',(-23.0913929293909,4.48356709006756,
12.));
#180001=CARTESIAN_POINT('Ctrl Pts',(-23.0749013821868,4.47501146242821,
12.));
#180002=CARTESIAN_POINT('Ctrl Pts',(-23.0584930981723,4.46655718018205,
12.));
#180003=CARTESIAN_POINT('Ctrl Pts',(-23.0421692712466,4.45820427241676,
12.));
#180004=CARTESIAN_POINT('Ctrl Pts',(-23.0259311131395,4.44995276669698,
12.));
#180005=CARTESIAN_POINT('Ctrl Pts',(-23.0097798538399,4.44180268901666,
12.));
#180006=CARTESIAN_POINT('Ctrl Pts',(-22.9937167421009,4.43375406376904,
12.));
#180007=CARTESIAN_POINT('Ctrl Pts',(-22.9777430460021,4.42580691372771,
12.));
#180008=CARTESIAN_POINT('Ctrl Pts',(-22.9618600534866,4.41796126001309,
12.));
#180009=CARTESIAN_POINT('Ctrl Pts',(-22.9460690729093,4.41021712205547,
12.));
#180010=CARTESIAN_POINT('Ctrl Pts',(-22.9303714335549,4.40257451754307,
12.));
#180011=CARTESIAN_POINT('Ctrl Pts',(-22.9147684862425,4.39503346238454,
12.));
#180012=CARTESIAN_POINT('Ctrl Pts',(-22.8992616040108,4.38759397068391,
12.));
#180013=CARTESIAN_POINT('Ctrl Pts',(-22.8838521827702,4.38025605470089,
12.));
#180014=CARTESIAN_POINT('Ctrl Pts',(-22.8685416419725,4.37301972480752,
12.));
#180015=CARTESIAN_POINT('Ctrl Pts',(-22.8533314252419,4.36588498943009,
12.));
#180016=CARTESIAN_POINT('Ctrl Pts',(-22.838223001118,4.35885185500559,12.));
#180017=CARTESIAN_POINT('Ctrl Pts',(-22.8232178638873,4.35192032594801,
12.));
#180018=CARTESIAN_POINT('Ctrl Pts',(-22.808317534379,4.34509040460065,12.));
#180019=CARTESIAN_POINT('Ctrl Pts',(-22.7935235607807,4.33836209118442,
12.));
#180020=CARTESIAN_POINT('Ctrl Pts',(-22.7788375194081,4.33173538373182,
12.));
#180021=CARTESIAN_POINT('Ctrl Pts',(-22.764261015648,4.32521027803747,12.));
#180022=CARTESIAN_POINT('Ctrl Pts',(-22.7497956849852,4.3187867676123,12.));
#180023=CARTESIAN_POINT('Ctrl Pts',(-22.7354431939927,4.3124648436255,12.));
#180024=CARTESIAN_POINT('Ctrl Pts',(-22.7212052413384,4.30624449484074,
12.));
#180025=CARTESIAN_POINT('Ctrl Pts',(-22.707083558756,4.30012570754066,12.));
#180026=CARTESIAN_POINT('Ctrl Pts',(-22.6930799122545,4.29410846547061,
12.));
#180027=CARTESIAN_POINT('Ctrl Pts',(-22.6791961033537,4.28819274977766,
12.));
#180028=CARTESIAN_POINT('Ctrl Pts',(-22.665433970311,4.28237853894059,12.));
#180029=CARTESIAN_POINT('Ctrl Pts',(-22.6517953893303,4.27666580869117,
12.));
#180030=CARTESIAN_POINT('Ctrl Pts',(-22.6382822758171,4.27105453192999,
12.));
#180031=CARTESIAN_POINT('Ctrl Pts',(-22.6248965859975,4.26554467865571,
12.));
#180032=CARTESIAN_POINT('Ctrl Pts',(-22.611640318482,4.26013621588303,12.));
#180033=CARTESIAN_POINT('Ctrl Pts',(-22.5985155158637,4.25482910755485,
12.));
#180034=CARTESIAN_POINT('Ctrl Pts',(-22.5855242662479,4.24962331444184,
12.));
#180035=CARTESIAN_POINT('Ctrl Pts',(-22.5726687049922,4.24451879404858,
12.));
#180036=CARTESIAN_POINT('Ctrl Pts',(-22.559951016643,4.23951550052526,12.));
#180037=CARTESIAN_POINT('Ctrl Pts',(-22.5473734368086,4.23461338456713,
12.));
#180038=CARTESIAN_POINT('Ctrl Pts',(-22.5349382540587,4.22981239330731,
12.));
#180039=CARTESIAN_POINT('Ctrl Pts',(-22.5226478117885,4.2251124702004,12.));
#180040=CARTESIAN_POINT('Ctrl Pts',(-22.5105045108882,4.22051355490196,
12.));
#180041=CARTESIAN_POINT('Ctrl Pts',(-22.4985108124229,4.21601558313908,
12.));
#180042=CARTESIAN_POINT('Ctrl Pts',(-22.4866692403147,4.21161848657428,
12.));
#180043=CARTESIAN_POINT('Ctrl Pts',(-22.4749823839915,4.20732219265648,
12.));
#180044=CARTESIAN_POINT('Ctrl Pts',(-22.4634529011433,4.2031266244817,12.));
#180045=CARTESIAN_POINT('Ctrl Pts',(-22.4520835205419,4.19903170066354,
12.));
#180046=CARTESIAN_POINT('Ctrl Pts',(-22.4408770448917,4.1950373351886,12.));
#180047=CARTESIAN_POINT('Ctrl Pts',(-22.4298363535421,4.19114343726941,
12.));
#180048=CARTESIAN_POINT('Ctrl Pts',(-22.4189644056115,4.1873499111772,12.));
#180049=CARTESIAN_POINT('Ctrl Pts',(-22.4082642454453,4.1836566560085,12.));
#180050=CARTESIAN_POINT('Ctrl Pts',(-22.3977390078075,4.18006356544882,
12.));
#180051=CARTESIAN_POINT('Ctrl Pts',(-22.3873919231334,4.17657052752825,
12.));
#180052=CARTESIAN_POINT('Ctrl Pts',(-22.3772263228617,4.17317742436145,
12.));
#180053=CARTESIAN_POINT('Ctrl Pts',(-22.36724564276,4.16988413199457,12.));
#180054=CARTESIAN_POINT('Ctrl Pts',(-22.3574534257396,4.166690520266,12.));
#180055=CARTESIAN_POINT('Ctrl Pts',(-22.3478533253889,4.16359645263187,
12.));
#180056=CARTESIAN_POINT('Ctrl Pts',(-22.3384491078602,4.16060178604164,
12.));
#180057=CARTESIAN_POINT('Ctrl Pts',(-22.3292446628959,4.15770637047889,
12.));
#180058=CARTESIAN_POINT('Ctrl Pts',(-22.3202440186979,4.15491004835281,
12.));
#180059=CARTESIAN_POINT('Ctrl Pts',(-22.3114513545185,4.1522126539699,12.));
#180060=CARTESIAN_POINT('Ctrl Pts',(-22.3028710166933,4.14961401285522,
12.));
#180061=CARTESIAN_POINT('Ctrl Pts',(-22.2945075198467,4.14711394168556,
12.));
#180062=CARTESIAN_POINT('Ctrl Pts',(-22.2863655389166,4.14471224859295,
12.));
#180063=CARTESIAN_POINT('Ctrl Pts',(-22.2784499072027,4.14240873321984,
12.));
#180064=CARTESIAN_POINT('Ctrl Pts',(-22.2707656042457,4.14020318715991,
12.));
#180065=CARTESIAN_POINT('Ctrl Pts',(-22.2633177913972,4.13809539255421,
12.));
#180066=CARTESIAN_POINT('Ctrl Pts',(-22.2561118708421,4.13608511977225,
12.));
#180067=CARTESIAN_POINT('Ctrl Pts',(-22.249153531779,4.1341721255881,12.));
#180068=CARTESIAN_POINT('Ctrl Pts',(-22.2424488153523,4.1323561506016,12.));
#180069=CARTESIAN_POINT('Ctrl Pts',(-22.2360040565533,4.13063692157498,
12.));
#180070=CARTESIAN_POINT('Ctrl Pts',(-22.2298258043947,4.12901415463379,
12.));
#180071=CARTESIAN_POINT('Ctrl Pts',(-22.2239207458781,4.12748755830104,
12.));
#180072=CARTESIAN_POINT('Ctrl Pts',(-22.2182956401341,4.12605683613307,
12.));
#180073=CARTESIAN_POINT('Ctrl Pts',(-22.2129576146671,4.12472167516607,
12.));
#180074=CARTESIAN_POINT('Ctrl Pts',(-22.2079143941719,4.12348173702023,
12.));
#180075=CARTESIAN_POINT('Ctrl Pts',(-22.2031746532106,4.12233664408227,
12.));
#180076=CARTESIAN_POINT('Ctrl Pts',(-22.1987479618246,4.12128598183522,
12.));
#180077=CARTESIAN_POINT('Ctrl Pts',(-22.1946440958098,4.12032932637736,
12.));
#180078=CARTESIAN_POINT('Ctrl Pts',(-22.1908725908525,4.11946626228636,
12.));
#180079=CARTESIAN_POINT('Ctrl Pts',(-22.1874419861496,4.11869641271773,
12.));
#180080=CARTESIAN_POINT('Ctrl Pts',(-22.1843613164855,4.11801938107479,
12.));
#180081=CARTESIAN_POINT('Ctrl Pts',(-22.1816414985788,4.11743469691756,
12.));
#180082=CARTESIAN_POINT('Ctrl Pts',(-22.179297473024,4.11694173195003,12.));
#180083=CARTESIAN_POINT('Ctrl Pts',(-22.177347426894,4.11653973150518,12.));
#180084=CARTESIAN_POINT('Ctrl Pts',(-22.1758088296598,4.11622797217068,
12.));
#180085=CARTESIAN_POINT('Ctrl Pts',(-22.1746949858775,4.11600589882845,
12.));
#180086=CARTESIAN_POINT('Ctrl Pts',(-22.1741488021234,4.11589976826166,
12.));
#180087=CARTESIAN_POINT('Ctrl Pts',(-22.1739341411687,4.11586035878287,
12.));
#180088=CARTESIAN_POINT('Ctrl Pts',(-22.173877682324,4.11585194677442,12.));
#180089=CARTESIAN_POINT('Ctrl Pts',(-22.1738711152697,4.11585220600461,
12.));
#180090=CARTESIAN_POINT('',(-21.624941921198,4.01396149767429,12.));
#180091=CARTESIAN_POINT('',(-10.5694630535049,1.96187429785751,12.));
#180092=CARTESIAN_POINT('',(-21.2226420728916,3.44230496120419,12.));
#180093=CARTESIAN_POINT('Origin',(-21.7161918885402,3.52235856495312,12.));
#180094=CARTESIAN_POINT('',(-21.3904321633055,2.16781269186828,12.));
#180095=CARTESIAN_POINT('Origin',(-7.6920903736728E-13,1.31973449697531E-13,
12.));
#180096=CARTESIAN_POINT('',(-21.9269795755927,1.71975774210842,12.));
#180097=CARTESIAN_POINT('Origin',(-21.8878840740801,2.21822694051638,12.));
#180098=CARTESIAN_POINT('',(-22.4835757167854,1.7634122053118,12.));
#180099=CARTESIAN_POINT('',(-11.2417878583927,0.881706102655883,12.));
#180100=CARTESIAN_POINT('',(-25.991588367311,0.661312440730901,12.));
#180101=CARTESIAN_POINT('Ctrl Pts',(-22.4835757167854,1.7634122053118,12.));
#180102=CARTESIAN_POINT('Ctrl Pts',(-22.4835819929788,1.7634141553879,12.));
#180103=CARTESIAN_POINT('Ctrl Pts',(-22.4836387052228,1.76342064263637,
12.));
#180104=CARTESIAN_POINT('Ctrl Pts',(-22.4838562517064,1.76343813434659,
12.));
#180105=CARTESIAN_POINT('Ctrl Pts',(-22.4844112933125,1.76347698284861,
12.));
#180106=CARTESIAN_POINT('Ctrl Pts',(-22.4855446605991,1.76355076045549,
12.));
#180107=CARTESIAN_POINT('Ctrl Pts',(-22.4871115206572,1.76364784232925,
12.));
#180108=CARTESIAN_POINT('Ctrl Pts',(-22.4890991659479,1.76376424879468,
12.));
#180109=CARTESIAN_POINT('Ctrl Pts',(-22.4914909094908,1.76389475965714,
12.));
#180110=CARTESIAN_POINT('Ctrl Pts',(-22.4942693792449,1.76403393880316,
12.));
#180111=CARTESIAN_POINT('Ctrl Pts',(-22.4974203063191,1.76417731243483,
12.));
#180112=CARTESIAN_POINT('Ctrl Pts',(-22.5009332677316,1.76432160068737,
12.));
#180113=CARTESIAN_POINT('Ctrl Pts',(-22.5047996391978,1.76446408210364,
12.));
#180114=CARTESIAN_POINT('Ctrl Pts',(-22.5090112700212,1.76460218257313,
12.));
#180115=CARTESIAN_POINT('Ctrl Pts',(-22.5135590569554,1.76473303281149,
12.));
#180116=CARTESIAN_POINT('Ctrl Pts',(-22.5184336670207,1.76485369319895,
12.));
#180117=CARTESIAN_POINT('Ctrl Pts',(-22.5236259635515,1.76496128643375,
12.));
#180118=CARTESIAN_POINT('Ctrl Pts',(-22.529127665298,1.76505320262759,12.));
#180119=CARTESIAN_POINT('Ctrl Pts',(-22.5349313983571,1.76512711563254,
12.));
#180120=CARTESIAN_POINT('Ctrl Pts',(-22.5410303590892,1.76518087841493,
12.));
#180121=CARTESIAN_POINT('Ctrl Pts',(-22.5474180954006,1.76521245524047,
12.));
#180122=CARTESIAN_POINT('Ctrl Pts',(-22.5540882235837,1.76521983384062,
12.));
#180123=CARTESIAN_POINT('Ctrl Pts',(-22.5610344912501,1.7652010450045,12.));
#180124=CARTESIAN_POINT('Ctrl Pts',(-22.5682508499873,1.76515418518831,
12.));
#180125=CARTESIAN_POINT('Ctrl Pts',(-22.5757315316353,1.76507744026746,
12.));
#180126=CARTESIAN_POINT('Ctrl Pts',(-22.5834711038022,1.76496910283088,
12.));
#180127=CARTESIAN_POINT('Ctrl Pts',(-22.5914644078106,1.76482755288411,
12.));
#180128=CARTESIAN_POINT('Ctrl Pts',(-22.5997065145638,1.76465124413557,
12.));
#180129=CARTESIAN_POINT('Ctrl Pts',(-22.6081926681343,1.76443868648015,
12.));
#180130=CARTESIAN_POINT('Ctrl Pts',(-22.6169182517694,1.76418843543739,
12.));
#180131=CARTESIAN_POINT('Ctrl Pts',(-22.6258787994848,1.76389909571403,
12.));
#180132=CARTESIAN_POINT('Ctrl Pts',(-22.6350699979359,1.76356932176273,
12.));
#180133=CARTESIAN_POINT('Ctrl Pts',(-22.6444876940423,1.76319782013916,
12.));
#180134=CARTESIAN_POINT('Ctrl Pts',(-22.6541278938409,1.76278334912561,
12.));
#180135=CARTESIAN_POINT('Ctrl Pts',(-22.6639867471753,1.76232471392568,
12.));
#180136=CARTESIAN_POINT('Ctrl Pts',(-22.67406053567,1.76182076289525,12.));
#180137=CARTESIAN_POINT('Ctrl Pts',(-22.684345658525,1.76127038310614,12.));
#180138=CARTESIAN_POINT('Ctrl Pts',(-22.6948386219851,1.76067249704886,
12.));
#180139=CARTESIAN_POINT('Ctrl Pts',(-22.7055360375485,1.76002606202401,
12.));
#180140=CARTESIAN_POINT('Ctrl Pts',(-22.7164346186006,1.75933006905925,
12.));
#180141=CARTESIAN_POINT('Ctrl Pts',(-22.72753117773,1.75858354204633,12.));
#180142=CARTESIAN_POINT('Ctrl Pts',(-22.7388226235559,1.75778553673244,
12.));
#180143=CARTESIAN_POINT('Ctrl Pts',(-22.750305955645,1.75693513908907,12.));
#180144=CARTESIAN_POINT('Ctrl Pts',(-22.7619782595013,1.75603146371641,
12.));
#180145=CARTESIAN_POINT('Ctrl Pts',(-22.7738367016118,1.75507365227131,
12.));
#180146=CARTESIAN_POINT('Ctrl Pts',(-22.7858785242361,1.75406087182936,
12.));
#180147=CARTESIAN_POINT('Ctrl Pts',(-22.7981010424314,1.75299231391466,
12.));
#180148=CARTESIAN_POINT('Ctrl Pts',(-22.8105016414713,1.75186719365592,
12.));
#180149=CARTESIAN_POINT('Ctrl Pts',(-22.8230777741284,1.75068474890883,
12.));
#180150=CARTESIAN_POINT('Ctrl Pts',(-22.8358269579853,1.74944423940115,
12.));
#180151=CARTESIAN_POINT('Ctrl Pts',(-22.8487467728076,1.74814494588492,
12.));
#180152=CARTESIAN_POINT('Ctrl Pts',(-22.8618348580235,1.74678616930664,
12.));
#180153=CARTESIAN_POINT('Ctrl Pts',(-22.8750889101696,1.74536722998201,
12.));
#180154=CARTESIAN_POINT('Ctrl Pts',(-22.888506680335,1.74388746677702,12.));
#180155=CARTESIAN_POINT('Ctrl Pts',(-22.9020859716141,1.7423462363008,12.));
#180156=CARTESIAN_POINT('Ctrl Pts',(-22.9158246373363,1.74074291231058,
12.));
#180157=CARTESIAN_POINT('Ctrl Pts',(-22.9297205792586,1.73907688511666,
12.));
#180158=CARTESIAN_POINT('Ctrl Pts',(-22.9437717457826,1.73734756100039,
12.));
#180159=CARTESIAN_POINT('Ctrl Pts',(-22.9579761301063,1.73555436162769,
12.));
#180160=CARTESIAN_POINT('Ctrl Pts',(-22.9723317685688,1.73369672350814,
12.));
#180161=CARTESIAN_POINT('Ctrl Pts',(-22.9868367391978,1.7317740975019,12.));
#180162=CARTESIAN_POINT('Ctrl Pts',(-23.001489160189,1.72978594832136,12.));
#180163=CARTESIAN_POINT('Ctrl Pts',(-23.0162871884168,1.72773175404708,
12.));
#180164=CARTESIAN_POINT('Ctrl Pts',(-23.0312290178883,1.72561100564045,
12.));
#180165=CARTESIAN_POINT('Ctrl Pts',(-23.0463128785531,1.72342320653746,
12.));
#180166=CARTESIAN_POINT('Ctrl Pts',(-23.0615370351562,1.72116787225991,
12.));
#180167=CARTESIAN_POINT('Ctrl Pts',(-23.0768997860709,1.71884453003027,
12.));
#180168=CARTESIAN_POINT('Ctrl Pts',(-23.0923994621213,1.71645271839296,
12.));
#180169=CARTESIAN_POINT('Ctrl Pts',(-23.1080344254286,1.71399198684704,
12.));
#180170=CARTESIAN_POINT('Ctrl Pts',(-23.1238030684925,1.71146189552174,
12.));
#180171=CARTESIAN_POINT('Ctrl Pts',(-23.1397038132356,1.70886201485452,
12.));
#180172=CARTESIAN_POINT('Ctrl Pts',(-23.1557351100614,1.70619192527852,
12.));
#180173=CARTESIAN_POINT('Ctrl Pts',(-23.1718954368751,1.70345121691276,
12.));
#180174=CARTESIAN_POINT('Ctrl Pts',(-23.1881832981851,1.7006394892701,12.));
#180175=CARTESIAN_POINT('Ctrl Pts',(-23.2045972243767,1.69775635099443,
12.));
#180176=CARTESIAN_POINT('Ctrl Pts',(-23.2211357709374,1.69480141959953,
12.));
#180177=CARTESIAN_POINT('Ctrl Pts',(-23.2377975177013,1.69177432121711,
12.));
#180178=CARTESIAN_POINT('Ctrl Pts',(-23.2545810680537,1.68867469034896,
12.));
#180179=CARTESIAN_POINT('Ctrl Pts',(-23.2714850482246,1.68550216963258,
12.));
#180180=CARTESIAN_POINT('Ctrl Pts',(-23.2885081066951,1.68225640962168,
12.));
#180181=CARTESIAN_POINT('Ctrl Pts',(-23.3056489135611,1.67893706857117,
12.));
#180182=CARTESIAN_POINT('Ctrl Pts',(-23.3229061599145,1.67554381222994,
12.));
#180183=CARTESIAN_POINT('Ctrl Pts',(-23.3402785571865,1.67207631363921,
12.));
#180184=CARTESIAN_POINT('Ctrl Pts',(-23.3577648365744,1.66853425293995,
12.));
#180185=CARTESIAN_POINT('Ctrl Pts',(-23.3753637485545,1.66491731718876,
12.));
#180186=CARTESIAN_POINT('Ctrl Pts',(-23.3930740623619,1.66122520018011,
12.));
#180187=CARTESIAN_POINT('Ctrl Pts',(-23.4108945654805,1.65745760227505,
12.));
#180188=CARTESIAN_POINT('Ctrl Pts',(-23.4288240631043,1.65361423023728,
12.));
#180189=CARTESIAN_POINT('Ctrl Pts',(-23.4468613776574,1.6496947970734,12.));
#180190=CARTESIAN_POINT('Ctrl Pts',(-23.4650053483932,1.64569902187611,
12.));
#180191=CARTESIAN_POINT('Ctrl Pts',(-23.4832548309645,1.64162662967528,
12.));
#180192=CARTESIAN_POINT('Ctrl Pts',(-23.5016086970003,1.63747735129474,
12.));
#180193=CARTESIAN_POINT('Ctrl Pts',(-23.5200658336612,1.63325092321725,
12.));
#180194=CARTESIAN_POINT('Ctrl Pts',(-23.538625143226,1.62894708745223,12.));
#180195=CARTESIAN_POINT('Ctrl Pts',(-23.5572855427601,1.62456559140064,
12.));
#180196=CARTESIAN_POINT('Ctrl Pts',(-23.57604596376,1.62010618772866,12.));
#180197=CARTESIAN_POINT('Ctrl Pts',(-23.5949053517997,1.61556863424698,
12.));
#180198=CARTESIAN_POINT('Ctrl Pts',(-23.6138626661653,1.61095269379778,
12.));
#180199=CARTESIAN_POINT('Ctrl Pts',(-23.6329168794929,1.60625813414672,
12.));
#180200=CARTESIAN_POINT('Ctrl Pts',(-23.6520669774876,1.60148472786595,
12.));
#180201=CARTESIAN_POINT('Ctrl Pts',(-23.671311958631,1.59663225222463,12.));
#180202=CARTESIAN_POINT('Ctrl Pts',(-23.6906508338833,1.59170048908633,
12.));
#180203=CARTESIAN_POINT('Ctrl Pts',(-23.710082626383,1.58668922481221,12.));
#180204=CARTESIAN_POINT('Ctrl Pts',(-23.72960637113,1.58159825017358,12.));
#180205=CARTESIAN_POINT('Ctrl Pts',(-23.749221114736,1.57642736025246,12.));
#180206=CARTESIAN_POINT('Ctrl Pts',(-23.7689259151862,1.57117635434408,
12.));
#180207=CARTESIAN_POINT('Ctrl Pts',(-23.7887198415878,1.56584503586843,
12.));
#180208=CARTESIAN_POINT('Ctrl Pts',(-23.8086019739194,1.56043321228633,
12.));
#180209=CARTESIAN_POINT('Ctrl Pts',(-23.8285714027636,1.55494069502635,
12.));
#180210=CARTESIAN_POINT('Ctrl Pts',(-23.8486272290705,1.54936729940541,
12.));
#180211=CARTESIAN_POINT('Ctrl Pts',(-23.8687685639642,1.5437128445399,12.));
#180212=CARTESIAN_POINT('Ctrl Pts',(-23.8889945285318,1.53797715326758,
12.));
#180213=CARTESIAN_POINT('Ctrl Pts',(-23.9093042536119,1.53216005207463,
12.));
#180214=CARTESIAN_POINT('Ctrl Pts',(-23.9296968795757,1.52626137103032,
12.));
#180215=CARTESIAN_POINT('Ctrl Pts',(-23.9501715561033,1.52028094372792,
12.));
#180216=CARTESIAN_POINT('Ctrl Pts',(-23.970727442014,1.51421860720614,12.));
#180217=CARTESIAN_POINT('Ctrl Pts',(-23.9913637050927,1.50807420187694,
12.));
#180218=CARTESIAN_POINT('Ctrl Pts',(-24.0120795219086,1.50184757146098,
12.));
#180219=CARTESIAN_POINT('Ctrl Pts',(-24.0328740776331,1.49553856292801,
12.));
#180220=CARTESIAN_POINT('Ctrl Pts',(-24.0537465658429,1.48914702644887,
12.));
#180221=CARTESIAN_POINT('Ctrl Pts',(-24.0746961883528,1.48267281533683,
12.));
#180222=CARTESIAN_POINT('Ctrl Pts',(-24.0957221550778,1.47611578597742,
12.));
#180223=CARTESIAN_POINT('Ctrl Pts',(-24.1168236838824,1.46947579776991,
12.));
#180224=CARTESIAN_POINT('Ctrl Pts',(-24.1380000004272,1.46275271307397,
12.));
#180225=CARTESIAN_POINT('Ctrl Pts',(-24.1592503380107,1.45594639716317,
12.));
#180226=CARTESIAN_POINT('Ctrl Pts',(-24.1805739374038,1.44905671818727,
12.));
#180227=CARTESIAN_POINT('Ctrl Pts',(-24.201970046722,1.44208354711082,12.));
#180228=CARTESIAN_POINT('Ctrl Pts',(-24.2234379212984,1.43502675765508,
12.));
#180229=CARTESIAN_POINT('Ctrl Pts',(-24.2449768235488,1.42788622624854,
12.));
#180230=CARTESIAN_POINT('Ctrl Pts',(-24.2665860228356,1.42066183198252,
12.));
#180231=CARTESIAN_POINT('Ctrl Pts',(-24.288264795321,1.41335345657682,12.));
#180232=CARTESIAN_POINT('Ctrl Pts',(-24.3100124238311,1.40596098434337,
12.));
#180233=CARTESIAN_POINT('Ctrl Pts',(-24.3318281977643,1.39848430212807,
12.));
#180234=CARTESIAN_POINT('Ctrl Pts',(-24.3537114129875,1.39092329926388,
12.));
#180235=CARTESIAN_POINT('Ctrl Pts',(-24.3756613717299,1.38327786752998,
12.));
#180236=CARTESIAN_POINT('Ctrl Pts',(-24.3976773824732,1.37554790111609,
12.));
#180237=CARTESIAN_POINT('Ctrl Pts',(-24.4197587598337,1.36773329659956,
12.));
#180238=CARTESIAN_POINT('Ctrl Pts',(-24.4419048244523,1.35983395290627,
12.));
#180239=CARTESIAN_POINT('Ctrl Pts',(-24.4641149028892,1.35184977125648,
12.));
#180240=CARTESIAN_POINT('Ctrl Pts',(-24.4863883275134,1.34378065512337,
12.));
#180241=CARTESIAN_POINT('Ctrl Pts',(-24.5087244363856,1.33562651019686,
12.));
#180242=CARTESIAN_POINT('Ctrl Pts',(-24.5311225731435,1.32738724435326,
12.));
#180243=CARTESIAN_POINT('Ctrl Pts',(-24.5535820868674,1.31906276763668,
12.));
#180244=CARTESIAN_POINT('Ctrl Pts',(-24.5761023320183,1.31065299222021,
12.));
#180245=CARTESIAN_POINT('Ctrl Pts',(-24.5986826684027,1.30215783236362,
12.));
#180246=CARTESIAN_POINT('Ctrl Pts',(-24.6213224611229,1.29357720438107,
12.));
#180247=CARTESIAN_POINT('Ctrl Pts',(-24.6440210805278,1.28491102661514,
12.));
#180248=CARTESIAN_POINT('Ctrl Pts',(-24.666777902156,1.27615921941642,12.));
#180249=CARTESIAN_POINT('Ctrl Pts',(-24.6895923066836,1.267321705135,12.));
#180250=CARTESIAN_POINT('Ctrl Pts',(-24.7124636797894,1.25839840807418,
12.));
#180251=CARTESIAN_POINT('Ctrl Pts',(-24.7353914120011,1.24938925444325,
12.));
#180252=CARTESIAN_POINT('Ctrl Pts',(-24.7583748985438,1.24029417231989,
12.));
#180253=CARTESIAN_POINT('Ctrl Pts',(-24.7814135391799,1.23111309161843,
12.));
#180254=CARTESIAN_POINT('Ctrl Pts',(-24.8045067380536,1.22184594406528,
12.));
#180255=CARTESIAN_POINT('Ctrl Pts',(-24.8276539035092,1.21249266318208,
12.));
#180256=CARTESIAN_POINT('Ctrl Pts',(-24.8508544481974,1.2030531842602,12.));
#180257=CARTESIAN_POINT('Ctrl Pts',(-24.8741077892075,1.19352744434064,
12.));
#180258=CARTESIAN_POINT('Ctrl Pts',(-24.8974133481829,1.18391538220103,
12.));
#180259=CARTESIAN_POINT('Ctrl Pts',(-24.9207705514449,1.17421693835041,
12.));
#180260=CARTESIAN_POINT('Ctrl Pts',(-24.9441788300932,1.16443205502849,
12.));
#180261=CARTESIAN_POINT('Ctrl Pts',(-24.9676376201502,1.15456067621889,
12.));
#180262=CARTESIAN_POINT('Ctrl Pts',(-24.9911463621433,1.144602747582,12.));
#180263=CARTESIAN_POINT('Ctrl Pts',(-25.0147045006196,1.1345582163853,12.));
#180264=CARTESIAN_POINT('Ctrl Pts',(-25.0383114836899,1.12442703144451,
12.));
#180265=CARTESIAN_POINT('Ctrl Pts',(-25.0619667625336,1.11420914306889,
12.));
#180266=CARTESIAN_POINT('Ctrl Pts',(-25.0856697909679,1.10390450301745,
12.));
#180267=CARTESIAN_POINT('Ctrl Pts',(-25.1094200248446,1.09351306445308,
12.));
#180268=CARTESIAN_POINT('Ctrl Pts',(-25.1332169227413,1.08303478197187,
12.));
#180269=CARTESIAN_POINT('Ctrl Pts',(-25.157059946931,1.07246961165475,12.));
#180270=CARTESIAN_POINT('Ctrl Pts',(-25.1809485642192,1.06181751111768,
12.));
#180271=CARTESIAN_POINT('Ctrl Pts',(-25.2048822469028,1.05107843957931,
12.));
#180272=CARTESIAN_POINT('Ctrl Pts',(-25.2288604735086,1.04025235791507,
12.));
#180273=CARTESIAN_POINT('Ctrl Pts',(-25.2528827300422,1.02933922876806,
12.));
#180274=CARTESIAN_POINT('Ctrl Pts',(-25.276948508726,1.01833901642237,12.));
#180275=CARTESIAN_POINT('Ctrl Pts',(-25.3010573055547,1.00725168656896,
12.));
#180276=CARTESIAN_POINT('Ctrl Pts',(-25.3252086182968,0.996077206120624,
12.));
#180277=CARTESIAN_POINT('Ctrl Pts',(-25.3494019441441,0.984815543003973,
12.));
#180278=CARTESIAN_POINT('Ctrl Pts',(-25.3736367778845,0.973466666000163,
12.));
#180279=CARTESIAN_POINT('Ctrl Pts',(-25.3979126089163,0.962030544503142,
12.));
#180280=CARTESIAN_POINT('Ctrl Pts',(-25.4222289223167,0.950507148597468,
12.));
#180281=CARTESIAN_POINT('Ctrl Pts',(-25.4465852044849,0.938896449496192,
12.));
#180282=CARTESIAN_POINT('Ctrl Pts',(-25.4709809475009,0.927198419886094,
12.));
#180283=CARTESIAN_POINT('Ctrl Pts',(-25.4954156541795,0.915413034335613,
12.));
#180284=CARTESIAN_POINT('Ctrl Pts',(-25.5198888424194,0.903540269651106,
12.));
#180285=CARTESIAN_POINT('Ctrl Pts',(-25.5444000508211,0.89158010534904,
12.));
#180286=CARTESIAN_POINT('Ctrl Pts',(-25.5689488408156,0.879532523834294,
12.));
#180287=CARTESIAN_POINT('Ctrl Pts',(-25.5935347843585,0.867397509338431,
12.));
#180288=CARTESIAN_POINT('Ctrl Pts',(-25.6181574536049,0.855175047036549,
12.));
#180289=CARTESIAN_POINT('Ctrl Pts',(-25.6428164100055,0.842865122120758,
12.));
#180290=CARTESIAN_POINT('Ctrl Pts',(-25.6675111931952,0.830467718864205,
12.));
#180291=CARTESIAN_POINT('Ctrl Pts',(-25.6922413110194,0.817982819787464,
12.));
#180292=CARTESIAN_POINT('Ctrl Pts',(-25.7170062262525,0.805410404554352,
12.));
#180293=CARTESIAN_POINT('Ctrl Pts',(-25.7418053757746,0.792750451616127,
12.));
#180294=CARTESIAN_POINT('Ctrl Pts',(-25.7666381946955,0.780002940291965,
12.));
#180295=CARTESIAN_POINT('Ctrl Pts',(-25.7915041383376,0.767167852651168,
12.));
#180296=CARTESIAN_POINT('Ctrl Pts',(-25.8164027059984,0.754245175609524,
12.));
#180297=CARTESIAN_POINT('Ctrl Pts',(-25.8413334619055,0.741234902663807,
12.));
#180298=CARTESIAN_POINT('Ctrl Pts',(-25.8662960624185,0.728137036482335,
12.));
#180299=CARTESIAN_POINT('Ctrl Pts',(-25.891290261497,0.714951588527638,
12.));
#180300=CARTESIAN_POINT('Ctrl Pts',(-25.9163158909426,0.701678575228756,
12.));
#180301=CARTESIAN_POINT('Ctrl Pts',(-25.9413728471909,0.688318015057729,
12.));
#180302=CARTESIAN_POINT('Ctrl Pts',(-25.9614434297919,0.677559543209725,
12.));
#180303=CARTESIAN_POINT('Ctrl Pts',(-25.9765104298071,0.669451306780825,
12.));
#180304=CARTESIAN_POINT('Ctrl Pts',(-25.9865613464773,0.664028313187627,
12.));
#180305=CARTESIAN_POINT('Ctrl Pts',(-25.991588367311,0.661312440730901,
12.));
#180306=CARTESIAN_POINT('',(-25.991588367311,-0.661312440730891,12.));
#180307=CARTESIAN_POINT('Origin',(0.,0.,12.));
#180308=CARTESIAN_POINT('',(-22.4835757167854,-1.76341220531179,12.));
#180309=CARTESIAN_POINT('Ctrl Pts',(-25.991588367311,-0.661312440730891,
12.));
#180310=CARTESIAN_POINT('Ctrl Pts',(-25.9865613464809,-0.664028313188912,
12.));
#180311=CARTESIAN_POINT('Ctrl Pts',(-25.9765104298171,-0.669451306784415,
12.));
#180312=CARTESIAN_POINT('Ctrl Pts',(-25.9614434298092,-0.677559543215902,
12.));
#180313=CARTESIAN_POINT('Ctrl Pts',(-25.941372847213,-0.688318015065678,
12.));
#180314=CARTESIAN_POINT('Ctrl Pts',(-25.9163158909645,-0.701678575236602,
12.));
#180315=CARTESIAN_POINT('Ctrl Pts',(-25.8912902615141,-0.714951588533753,
12.));
#180316=CARTESIAN_POINT('Ctrl Pts',(-25.8662960624285,-0.728137036485877,
12.));
#180317=CARTESIAN_POINT('Ctrl Pts',(-25.841333461908,-0.741234902664697,
12.));
#180318=CARTESIAN_POINT('Ctrl Pts',(-25.816402705995,-0.754245175608288,
12.));
#180319=CARTESIAN_POINT('Ctrl Pts',(-25.7915041383304,-0.767167852648639,
12.));
#180320=CARTESIAN_POINT('Ctrl Pts',(-25.7666381946871,-0.780002940289025,
12.));
#180321=CARTESIAN_POINT('Ctrl Pts',(-25.7418053757671,-0.792750451613534,
12.));
#180322=CARTESIAN_POINT('Ctrl Pts',(-25.7170062262474,-0.805410404552594,
12.));
#180323=CARTESIAN_POINT('Ctrl Pts',(-25.6922413110172,-0.817982819786719,
12.));
#180324=CARTESIAN_POINT('Ctrl Pts',(-25.6675111931957,-0.830467718864367,
12.));
#180325=CARTESIAN_POINT('Ctrl Pts',(-25.6428164100078,-0.842865122121544,
12.));
#180326=CARTESIAN_POINT('Ctrl Pts',(-25.618157453608,-0.855175047037614,
12.));
#180327=CARTESIAN_POINT('Ctrl Pts',(-25.5935347843616,-0.86739750933947,
12.));
#180328=CARTESIAN_POINT('Ctrl Pts',(-25.568948840818,-0.87953252383509,
12.));
#180329=CARTESIAN_POINT('Ctrl Pts',(-25.5444000508223,-0.891580105349467,
12.));
#180330=CARTESIAN_POINT('Ctrl Pts',(-25.5198888424195,-0.903540269651154,
12.));
#180331=CARTESIAN_POINT('Ctrl Pts',(-25.4954156541787,-0.915413034335333,
12.));
#180332=CARTESIAN_POINT('Ctrl Pts',(-25.4709809474996,-0.927198419885604,
12.));
#180333=CARTESIAN_POINT('Ctrl Pts',(-25.4465852044835,-0.938896449495632,
12.));
#180334=CARTESIAN_POINT('Ctrl Pts',(-25.4222289223155,-0.950507148596968,
12.));
#180335=CARTESIAN_POINT('Ctrl Pts',(-25.3979126089155,-0.962030544502802,
12.));
#180336=CARTESIAN_POINT('Ctrl Pts',(-25.3736367778842,-0.973466666000048,
12.));
#180337=CARTESIAN_POINT('Ctrl Pts',(-25.3494019441444,-0.984815543004089,
12.));
#180338=CARTESIAN_POINT('Ctrl Pts',(-25.3252086182976,-0.996077206120919,
12.));
#180339=CARTESIAN_POINT('Ctrl Pts',(-25.3010573055557,-1.00725168656933,
12.));
#180340=CARTESIAN_POINT('Ctrl Pts',(-25.2769485087268,-1.01833901642272,
12.));
#180341=CARTESIAN_POINT('Ctrl Pts',(-25.2528827300427,-1.0293392287683,
12.));
#180342=CARTESIAN_POINT('Ctrl Pts',(-25.2288604735087,-1.04025235791515,
12.));
#180343=CARTESIAN_POINT('Ctrl Pts',(-25.2048822469027,-1.05107843957925,
12.));
#180344=CARTESIAN_POINT('Ctrl Pts',(-25.1809485642191,-1.06181751111754,
12.));
#180345=CARTESIAN_POINT('Ctrl Pts',(-25.1570599469311,-1.0724696116546,
12.));
#180346=CARTESIAN_POINT('Ctrl Pts',(-25.1332169227415,-1.08303478197174,
12.));
#180347=CARTESIAN_POINT('Ctrl Pts',(-25.1094200248448,-1.09351306445299,
12.));
#180348=CARTESIAN_POINT('Ctrl Pts',(-25.085669790968,-1.1039045030174,12.));
#180349=CARTESIAN_POINT('Ctrl Pts',(-25.0619667625336,-1.1142091430689,
12.));
#180350=CARTESIAN_POINT('Ctrl Pts',(-25.0383114836898,-1.12442703144455,
12.));
#180351=CARTESIAN_POINT('Ctrl Pts',(-25.0147045006193,-1.13455821638535,
12.));
#180352=CARTESIAN_POINT('Ctrl Pts',(-24.9911463621431,-1.14460274758206,
12.));
#180353=CARTESIAN_POINT('Ctrl Pts',(-24.9676376201501,-1.15456067621894,
12.));
#180354=CARTESIAN_POINT('Ctrl Pts',(-24.9441788300932,-1.16443205502852,
12.));
#180355=CARTESIAN_POINT('Ctrl Pts',(-24.9207705514449,-1.17421693835039,
12.));
#180356=CARTESIAN_POINT('Ctrl Pts',(-24.8974133481829,-1.18391538220098,
12.));
#180357=CARTESIAN_POINT('Ctrl Pts',(-24.8741077892074,-1.19352744434059,
12.));
#180358=CARTESIAN_POINT('Ctrl Pts',(-24.8508544481973,-1.20305318426015,
12.));
#180359=CARTESIAN_POINT('Ctrl Pts',(-24.8276539035092,-1.21249266318205,
12.));
#180360=CARTESIAN_POINT('Ctrl Pts',(-24.8045067380536,-1.22184594406526,
12.));
#180361=CARTESIAN_POINT('Ctrl Pts',(-24.78141353918,-1.23111309161843,12.));
#180362=CARTESIAN_POINT('Ctrl Pts',(-24.7583748985439,-1.24029417231988,
12.));
#180363=CARTESIAN_POINT('Ctrl Pts',(-24.7353914120012,-1.24938925444323,
12.));
#180364=CARTESIAN_POINT('Ctrl Pts',(-24.7124636797895,-1.25839840807415,
12.));
#180365=CARTESIAN_POINT('Ctrl Pts',(-24.6895923066837,-1.26732170513497,
12.));
#180366=CARTESIAN_POINT('Ctrl Pts',(-24.666777902156,-1.2761592194164,12.));
#180367=CARTESIAN_POINT('Ctrl Pts',(-24.6440210805278,-1.28491102661513,
12.));
#180368=CARTESIAN_POINT('Ctrl Pts',(-24.6213224611228,-1.29357720438107,
12.));
#180369=CARTESIAN_POINT('Ctrl Pts',(-24.5986826684025,-1.30215783236364,
12.));
#180370=CARTESIAN_POINT('Ctrl Pts',(-24.576102332018,-1.31065299222023,
12.));
#180371=CARTESIAN_POINT('Ctrl Pts',(-24.5535820868671,-1.31906276763669,
12.));
#180372=CARTESIAN_POINT('Ctrl Pts',(-24.5311225731434,-1.32738724435326,
12.));
#180373=CARTESIAN_POINT('Ctrl Pts',(-24.5087244363856,-1.33562651019684,
12.));
#180374=CARTESIAN_POINT('Ctrl Pts',(-24.4863883275135,-1.34378065512335,
12.));
#180375=CARTESIAN_POINT('Ctrl Pts',(-24.4641149028894,-1.35184977125644,
12.));
#180376=CARTESIAN_POINT('Ctrl Pts',(-24.4419048244524,-1.35983395290624,
12.));
#180377=CARTESIAN_POINT('Ctrl Pts',(-24.4197587598337,-1.36773329659954,
12.));
#180378=CARTESIAN_POINT('Ctrl Pts',(-24.3976773824731,-1.37554790111607,
12.));
#180379=CARTESIAN_POINT('Ctrl Pts',(-24.37566137173,-1.38327786752998,12.));
#180380=CARTESIAN_POINT('Ctrl Pts',(-24.3537114129877,-1.3909232992639,
12.));
#180381=CARTESIAN_POINT('Ctrl Pts',(-24.3318281977647,-1.3984843021281,
12.));
#180382=CARTESIAN_POINT('Ctrl Pts',(-24.3100124238316,-1.4059609843434,
12.));
#180383=CARTESIAN_POINT('Ctrl Pts',(-24.2882647953214,-1.41335345657685,
12.));
#180384=CARTESIAN_POINT('Ctrl Pts',(-24.2665860228357,-1.42066183198252,
12.));
#180385=CARTESIAN_POINT('Ctrl Pts',(-24.2449768235485,-1.42788622624851,
12.));
#180386=CARTESIAN_POINT('Ctrl Pts',(-24.2234379212978,-1.43502675765502,
12.));
#180387=CARTESIAN_POINT('Ctrl Pts',(-24.2019700467214,-1.44208354711074,
12.));
#180388=CARTESIAN_POINT('Ctrl Pts',(-24.1805739374033,-1.44905671818721,
12.));
#180389=CARTESIAN_POINT('Ctrl Pts',(-24.1592503380105,-1.45594639716314,
12.));
#180390=CARTESIAN_POINT('Ctrl Pts',(-24.1380000004272,-1.46275271307398,
12.));
#180391=CARTESIAN_POINT('Ctrl Pts',(-24.1168236838827,-1.46947579776992,
12.));
#180392=CARTESIAN_POINT('Ctrl Pts',(-24.0957221550782,-1.47611578597741,
12.));
#180393=CARTESIAN_POINT('Ctrl Pts',(-24.074696188353,-1.4826728153368,12.));
#180394=CARTESIAN_POINT('Ctrl Pts',(-24.053746565843,-1.48914702644883,
12.));
#180395=CARTESIAN_POINT('Ctrl Pts',(-24.0328740776331,-1.49553856292798,
12.));
#180396=CARTESIAN_POINT('Ctrl Pts',(-24.0120795219086,-1.50184757146099,
12.));
#180397=CARTESIAN_POINT('Ctrl Pts',(-23.991363705093,-1.50807420187702,
12.));
#180398=CARTESIAN_POINT('Ctrl Pts',(-23.9707274420145,-1.51421860720628,
12.));
#180399=CARTESIAN_POINT('Ctrl Pts',(-23.9501715561038,-1.52028094372806,
12.));
#180400=CARTESIAN_POINT('Ctrl Pts',(-23.9296968795761,-1.52626137103039,
12.));
#180401=CARTESIAN_POINT('Ctrl Pts',(-23.9093042536119,-1.53216005207462,
12.));
#180402=CARTESIAN_POINT('Ctrl Pts',(-23.8889945285313,-1.53797715326748,
12.));
#180403=CARTESIAN_POINT('Ctrl Pts',(-23.8687685639635,-1.54371284453978,
12.));
#180404=CARTESIAN_POINT('Ctrl Pts',(-23.8486272290698,-1.5493672994053,
12.));
#180405=CARTESIAN_POINT('Ctrl Pts',(-23.8285714027631,-1.55494069502628,
12.));
#180406=CARTESIAN_POINT('Ctrl Pts',(-23.8086019739192,-1.56043321228631,
12.));
#180407=CARTESIAN_POINT('Ctrl Pts',(-23.788719841588,-1.56584503586844,
12.));
#180408=CARTESIAN_POINT('Ctrl Pts',(-23.7689259151869,-1.57117635434412,
12.));
#180409=CARTESIAN_POINT('Ctrl Pts',(-23.7492211147369,-1.57642736025251,
12.));
#180410=CARTESIAN_POINT('Ctrl Pts',(-23.7296063711308,-1.58159825017362,
12.));
#180411=CARTESIAN_POINT('Ctrl Pts',(-23.7100826263835,-1.58668922481222,
12.));
#180412=CARTESIAN_POINT('Ctrl Pts',(-23.6906508338833,-1.59170048908631,
12.));
#180413=CARTESIAN_POINT('Ctrl Pts',(-23.6713119586302,-1.59663225222458,
12.));
#180414=CARTESIAN_POINT('Ctrl Pts',(-23.6520669774863,-1.60148472786588,
12.));
#180415=CARTESIAN_POINT('Ctrl Pts',(-23.6329168794916,-1.60625813414666,
12.));
#180416=CARTESIAN_POINT('Ctrl Pts',(-23.6138626661644,-1.61095269379773,
12.));
#180417=CARTESIAN_POINT('Ctrl Pts',(-23.5949053517996,-1.61556863424697,
12.));
#180418=CARTESIAN_POINT('Ctrl Pts',(-23.5760459637608,-1.62010618772869,
12.));
#180419=CARTESIAN_POINT('Ctrl Pts',(-23.5572855427617,-1.62456559140072,
12.));
#180420=CARTESIAN_POINT('Ctrl Pts',(-23.5386251432278,-1.62894708745231,
12.));
#180421=CARTESIAN_POINT('Ctrl Pts',(-23.5200658336624,-1.63325092321731,
12.));
#180422=CARTESIAN_POINT('Ctrl Pts',(-23.5016086970006,-1.63747735129474,
12.));
#180423=CARTESIAN_POINT('Ctrl Pts',(-23.4832548309638,-1.64162662967524,
12.));
#180424=CARTESIAN_POINT('Ctrl Pts',(-23.4650053483919,-1.64569902187608,
12.));
#180425=CARTESIAN_POINT('Ctrl Pts',(-23.446861377656,-1.64969479707339,
12.));
#180426=CARTESIAN_POINT('Ctrl Pts',(-23.4288240631034,-1.6536142302373,
12.));
#180427=CARTESIAN_POINT('Ctrl Pts',(-23.4108945654803,-1.65745760227507,
12.));
#180428=CARTESIAN_POINT('Ctrl Pts',(-23.3930740623622,-1.66122520018008,
12.));
#180429=CARTESIAN_POINT('Ctrl Pts',(-23.375363748555,-1.66491731718864,
12.));
#180430=CARTESIAN_POINT('Ctrl Pts',(-23.3577648365747,-1.66853425293977,
12.));
#180431=CARTESIAN_POINT('Ctrl Pts',(-23.3402785571866,-1.67207631363905,
12.));
#180432=CARTESIAN_POINT('Ctrl Pts',(-23.3229061599145,-1.67554381222987,
12.));
#180433=CARTESIAN_POINT('Ctrl Pts',(-23.3056489135611,-1.67893706857123,
12.));
#180434=CARTESIAN_POINT('Ctrl Pts',(-23.2885081066949,-1.68225640962181,
12.));
#180435=CARTESIAN_POINT('Ctrl Pts',(-23.2714850482245,-1.68550216963275,
12.));
#180436=CARTESIAN_POINT('Ctrl Pts',(-23.2545810680536,-1.6886746903491,
12.));
#180437=CARTESIAN_POINT('Ctrl Pts',(-23.2377975177014,-1.69177432121716,
12.));
#180438=CARTESIAN_POINT('Ctrl Pts',(-23.2211357709374,-1.69480141959945,
12.));
#180439=CARTESIAN_POINT('Ctrl Pts',(-23.2045972243765,-1.69775635099425,
12.));
#180440=CARTESIAN_POINT('Ctrl Pts',(-23.1881832981848,-1.70063948926987,
12.));
#180441=CARTESIAN_POINT('Ctrl Pts',(-23.1718954368749,-1.70345121691259,
12.));
#180442=CARTESIAN_POINT('Ctrl Pts',(-23.1557351100613,-1.70619192527847,
12.));
#180443=CARTESIAN_POINT('Ctrl Pts',(-23.1397038132358,-1.7088620148546,
12.));
#180444=CARTESIAN_POINT('Ctrl Pts',(-23.1238030684929,-1.71146189552192,
12.));
#180445=CARTESIAN_POINT('Ctrl Pts',(-23.1080344254291,-1.71399198684724,
12.));
#180446=CARTESIAN_POINT('Ctrl Pts',(-23.0923994621216,-1.71645271839311,
12.));
#180447=CARTESIAN_POINT('Ctrl Pts',(-23.0768997860709,-1.71884453003027,
12.));
#180448=CARTESIAN_POINT('Ctrl Pts',(-23.061537035156,-1.7211678722598,12.));
#180449=CARTESIAN_POINT('Ctrl Pts',(-23.0463128785528,-1.72342320653731,
12.));
#180450=CARTESIAN_POINT('Ctrl Pts',(-23.031229017888,-1.72561100564033,
12.));
#180451=CARTESIAN_POINT('Ctrl Pts',(-23.0162871884167,-1.72773175404702,
12.));
#180452=CARTESIAN_POINT('Ctrl Pts',(-23.0014891601891,-1.72978594832137,
12.));
#180453=CARTESIAN_POINT('Ctrl Pts',(-22.9868367391978,-1.73177409750193,
12.));
#180454=CARTESIAN_POINT('Ctrl Pts',(-22.9723317685688,-1.73369672350817,
12.));
#180455=CARTESIAN_POINT('Ctrl Pts',(-22.9579761301062,-1.73555436162771,
12.));
#180456=CARTESIAN_POINT('Ctrl Pts',(-22.9437717457825,-1.73734756100038,
12.));
#180457=CARTESIAN_POINT('Ctrl Pts',(-22.9297205792587,-1.73907688511664,
12.));
#180458=CARTESIAN_POINT('Ctrl Pts',(-22.9158246373365,-1.74074291231057,
12.));
#180459=CARTESIAN_POINT('Ctrl Pts',(-22.9020859716144,-1.74234623630079,
12.));
#180460=CARTESIAN_POINT('Ctrl Pts',(-22.8885066803351,-1.74388746677702,
12.));
#180461=CARTESIAN_POINT('Ctrl Pts',(-22.8750889101696,-1.745367229982,12.));
#180462=CARTESIAN_POINT('Ctrl Pts',(-22.8618348580234,-1.74678616930663,
12.));
#180463=CARTESIAN_POINT('Ctrl Pts',(-22.8487467728075,-1.74814494588492,
12.));
#180464=CARTESIAN_POINT('Ctrl Pts',(-22.8358269579854,-1.74944423940117,
12.));
#180465=CARTESIAN_POINT('Ctrl Pts',(-22.8230777741285,-1.75068474890884,
12.));
#180466=CARTESIAN_POINT('Ctrl Pts',(-22.8105016414712,-1.75186719365589,
12.));
#180467=CARTESIAN_POINT('Ctrl Pts',(-22.7981010424312,-1.75299231391461,
12.));
#180468=CARTESIAN_POINT('Ctrl Pts',(-22.7858785242358,-1.75406087182929,
12.));
#180469=CARTESIAN_POINT('Ctrl Pts',(-22.7738367016115,-1.75507365227127,
12.));
#180470=CARTESIAN_POINT('Ctrl Pts',(-22.7619782595013,-1.7560314637164,
12.));
#180471=CARTESIAN_POINT('Ctrl Pts',(-22.7503059556455,-1.75693513908911,
12.));
#180472=CARTESIAN_POINT('Ctrl Pts',(-22.7388226235565,-1.75778553673249,
12.));
#180473=CARTESIAN_POINT('Ctrl Pts',(-22.7275311777305,-1.75858354204635,
12.));
#180474=CARTESIAN_POINT('Ctrl Pts',(-22.7164346186007,-1.75933006905924,
12.));
#180475=CARTESIAN_POINT('Ctrl Pts',(-22.7055360375481,-1.76002606202399,
12.));
#180476=CARTESIAN_POINT('Ctrl Pts',(-22.6948386219843,-1.76067249704884,
12.));
#180477=CARTESIAN_POINT('Ctrl Pts',(-22.6843456585245,-1.76127038310612,
12.));
#180478=CARTESIAN_POINT('Ctrl Pts',(-22.6740605356699,-1.76182076289525,
12.));
#180479=CARTESIAN_POINT('Ctrl Pts',(-22.6639867471756,-1.76232471392567,
12.));
#180480=CARTESIAN_POINT('Ctrl Pts',(-22.6541278938413,-1.76278334912559,
12.));
#180481=CARTESIAN_POINT('Ctrl Pts',(-22.6444876940425,-1.76319782013914,
12.));
#180482=CARTESIAN_POINT('Ctrl Pts',(-22.635069997936,-1.76356932176272,
12.));
#180483=CARTESIAN_POINT('Ctrl Pts',(-22.6258787994847,-1.76389909571402,
12.));
#180484=CARTESIAN_POINT('Ctrl Pts',(-22.6169182517693,-1.76418843543739,
12.));
#180485=CARTESIAN_POINT('Ctrl Pts',(-22.6081926681342,-1.76443868648015,
12.));
#180486=CARTESIAN_POINT('Ctrl Pts',(-22.5997065145638,-1.76465124413556,
12.));
#180487=CARTESIAN_POINT('Ctrl Pts',(-22.5914644078106,-1.76482755288411,
12.));
#180488=CARTESIAN_POINT('Ctrl Pts',(-22.5834711038024,-1.76496910283088,
12.));
#180489=CARTESIAN_POINT('Ctrl Pts',(-22.5757315316355,-1.76507744026747,
12.));
#180490=CARTESIAN_POINT('Ctrl Pts',(-22.5682508499873,-1.76515418518829,
12.));
#180491=CARTESIAN_POINT('Ctrl Pts',(-22.5610344912501,-1.76520104500449,
12.));
#180492=CARTESIAN_POINT('Ctrl Pts',(-22.5540882235837,-1.76521983384063,
12.));
#180493=CARTESIAN_POINT('Ctrl Pts',(-22.5474180954006,-1.76521245524047,
12.));
#180494=CARTESIAN_POINT('Ctrl Pts',(-22.5410303590891,-1.76518087841492,
12.));
#180495=CARTESIAN_POINT('Ctrl Pts',(-22.5349313983571,-1.7651271156325,
12.));
#180496=CARTESIAN_POINT('Ctrl Pts',(-22.529127665298,-1.76505320262751,
12.));
#180497=CARTESIAN_POINT('Ctrl Pts',(-22.5236259635515,-1.76496128643369,
12.));
#180498=CARTESIAN_POINT('Ctrl Pts',(-22.5184336670207,-1.76485369319896,
12.));
#180499=CARTESIAN_POINT('Ctrl Pts',(-22.5135590569554,-1.76473303281159,
12.));
#180500=CARTESIAN_POINT('Ctrl Pts',(-22.5090112700212,-1.76460218257323,
12.));
#180501=CARTESIAN_POINT('Ctrl Pts',(-22.5047996391978,-1.76446408210366,
12.));
#180502=CARTESIAN_POINT('Ctrl Pts',(-22.5009332677316,-1.76432160068725,
12.));
#180503=CARTESIAN_POINT('Ctrl Pts',(-22.4974203063191,-1.76417731243462,
12.));
#180504=CARTESIAN_POINT('Ctrl Pts',(-22.4942693792449,-1.764033938803,12.));
#180505=CARTESIAN_POINT('Ctrl Pts',(-22.4914909094908,-1.76389475965724,
12.));
#180506=CARTESIAN_POINT('Ctrl Pts',(-22.4890991659478,-1.76376424879505,
12.));
#180507=CARTESIAN_POINT('Ctrl Pts',(-22.4871115206571,-1.76364784232963,
12.));
#180508=CARTESIAN_POINT('Ctrl Pts',(-22.4855446605991,-1.76355076045546,
12.));
#180509=CARTESIAN_POINT('Ctrl Pts',(-22.4844112933129,-1.76347698284792,
12.));
#180510=CARTESIAN_POINT('Ctrl Pts',(-22.483856251707,-1.76343813434565,
12.));
#180511=CARTESIAN_POINT('Ctrl Pts',(-22.4836387052232,-1.7634206426357,
12.));
#180512=CARTESIAN_POINT('Ctrl Pts',(-22.483581992979,-1.76341415538764,
12.));
#180513=CARTESIAN_POINT('Ctrl Pts',(-22.4835757167854,-1.76341220531179,
12.));
#180514=CARTESIAN_POINT('',(-21.9269795755927,-1.71975774210841,12.));
#180515=CARTESIAN_POINT('',(-10.7170877657712,-0.840553282521227,12.));
#180516=CARTESIAN_POINT('',(-21.3904321633055,-2.16781269186828,12.));
#180517=CARTESIAN_POINT('Origin',(-21.8878840740801,-2.21822694051637,12.));
#180518=CARTESIAN_POINT('',(-21.2226420728916,-3.44230496120418,12.));
#180519=CARTESIAN_POINT('Origin',(-7.7715611723761E-13,-7.16093850883225E-14,
12.));
#180520=CARTESIAN_POINT('',(-21.624941921198,-4.01396149767428,12.));
#180521=CARTESIAN_POINT('Origin',(-21.7161918885403,-3.52235856495312,12.));
#180522=CARTESIAN_POINT('',(-22.1738711152697,-4.11585220600461,12.));
#180523=CARTESIAN_POINT('',(-11.0869355576349,-2.05792610300232,12.));
#180524=CARTESIAN_POINT('',(-25.2771067246846,-6.08833931617698,12.));
#180525=CARTESIAN_POINT('Ctrl Pts',(-22.1738711152697,-4.11585220600461,
12.));
#180526=CARTESIAN_POINT('Ctrl Pts',(-22.1738776823239,-4.11585194677412,
12.));
#180527=CARTESIAN_POINT('Ctrl Pts',(-22.1739341411684,-4.1158603587821,
12.));
#180528=CARTESIAN_POINT('Ctrl Pts',(-22.174148802123,-4.11589976826061,
12.));
#180529=CARTESIAN_POINT('Ctrl Pts',(-22.1746949858773,-4.11600589882767,
12.));
#180530=CARTESIAN_POINT('Ctrl Pts',(-22.1758088296598,-4.11622797217066,
12.));
#180531=CARTESIAN_POINT('Ctrl Pts',(-22.177347426894,-4.11653973150558,
12.));
#180532=CARTESIAN_POINT('Ctrl Pts',(-22.179297473024,-4.11694173195041,
12.));
#180533=CARTESIAN_POINT('Ctrl Pts',(-22.1816414985788,-4.11743469691765,
12.));
#180534=CARTESIAN_POINT('Ctrl Pts',(-22.1843613164855,-4.11801938107464,
12.));
#180535=CARTESIAN_POINT('Ctrl Pts',(-22.1874419861496,-4.11869641271752,
12.));
#180536=CARTESIAN_POINT('Ctrl Pts',(-22.1908725908525,-4.11946626228623,
12.));
#180537=CARTESIAN_POINT('Ctrl Pts',(-22.1946440958098,-4.12032932637738,
12.));
#180538=CARTESIAN_POINT('Ctrl Pts',(-22.1987479618246,-4.12128598183533,
12.));
#180539=CARTESIAN_POINT('Ctrl Pts',(-22.2031746532106,-4.12233664408237,
12.));
#180540=CARTESIAN_POINT('Ctrl Pts',(-22.2079143941719,-4.12348173702024,
12.));
#180541=CARTESIAN_POINT('Ctrl Pts',(-22.2129576146671,-4.12472167516602,
12.));
#180542=CARTESIAN_POINT('Ctrl Pts',(-22.2182956401341,-4.126056836133,12.));
#180543=CARTESIAN_POINT('Ctrl Pts',(-22.2239207458781,-4.12748755830099,
12.));
#180544=CARTESIAN_POINT('Ctrl Pts',(-22.2298258043947,-4.12901415463379,
12.));
#180545=CARTESIAN_POINT('Ctrl Pts',(-22.2360040565534,-4.13063692157499,
12.));
#180546=CARTESIAN_POINT('Ctrl Pts',(-22.2424488153523,-4.1323561506016,
12.));
#180547=CARTESIAN_POINT('Ctrl Pts',(-22.2491535317789,-4.13417212558808,
12.));
#180548=CARTESIAN_POINT('Ctrl Pts',(-22.2561118708422,-4.13608511977226,
12.));
#180549=CARTESIAN_POINT('Ctrl Pts',(-22.263317791397,-4.13809539255418,
12.));
#180550=CARTESIAN_POINT('Ctrl Pts',(-22.2707656042456,-4.14020318715988,
12.));
#180551=CARTESIAN_POINT('Ctrl Pts',(-22.2784499072026,-4.14240873321982,
12.));
#180552=CARTESIAN_POINT('Ctrl Pts',(-22.2863655389167,-4.14471224859295,
12.));
#180553=CARTESIAN_POINT('Ctrl Pts',(-22.2945075198468,-4.14711394168559,
12.));
#180554=CARTESIAN_POINT('Ctrl Pts',(-22.3028710166935,-4.14961401285525,
12.));
#180555=CARTESIAN_POINT('Ctrl Pts',(-22.3114513545186,-4.15221265396993,
12.));
#180556=CARTESIAN_POINT('Ctrl Pts',(-22.3202440186979,-4.15491004835278,
12.));
#180557=CARTESIAN_POINT('Ctrl Pts',(-22.3292446628957,-4.15770637047882,
12.));
#180558=CARTESIAN_POINT('Ctrl Pts',(-22.3384491078599,-4.16060178604154,
12.));
#180559=CARTESIAN_POINT('Ctrl Pts',(-22.3478533253886,-4.1635964526318,
12.));
#180560=CARTESIAN_POINT('Ctrl Pts',(-22.3574534257397,-4.16669052026602,
12.));
#180561=CARTESIAN_POINT('Ctrl Pts',(-22.3672456427605,-4.16988413199469,
12.));
#180562=CARTESIAN_POINT('Ctrl Pts',(-22.3772263228624,-4.17317742436162,
12.));
#180563=CARTESIAN_POINT('Ctrl Pts',(-22.3873919231339,-4.17657052752834,
12.));
#180564=CARTESIAN_POINT('Ctrl Pts',(-22.3977390078074,-4.18006356544879,
12.));
#180565=CARTESIAN_POINT('Ctrl Pts',(-22.4082642454448,-4.18365665600839,
12.));
#180566=CARTESIAN_POINT('Ctrl Pts',(-22.4189644056109,-4.18734991117707,
12.));
#180567=CARTESIAN_POINT('Ctrl Pts',(-22.4298363535416,-4.19114343726932,
12.));
#180568=CARTESIAN_POINT('Ctrl Pts',(-22.4408770448917,-4.1950373351886,
12.));
#180569=CARTESIAN_POINT('Ctrl Pts',(-22.4520835205422,-4.19903170066358,
12.));
#180570=CARTESIAN_POINT('Ctrl Pts',(-22.4634529011437,-4.20312662448174,
12.));
#180571=CARTESIAN_POINT('Ctrl Pts',(-22.4749823839917,-4.20732219265649,
12.));
#180572=CARTESIAN_POINT('Ctrl Pts',(-22.4866692403147,-4.21161848657428,
12.));
#180573=CARTESIAN_POINT('Ctrl Pts',(-22.4985108124228,-4.21601558313906,
12.));
#180574=CARTESIAN_POINT('Ctrl Pts',(-22.5105045108881,-4.22051355490196,
12.));
#180575=CARTESIAN_POINT('Ctrl Pts',(-22.5226478117886,-4.22511247020041,
12.));
#180576=CARTESIAN_POINT('Ctrl Pts',(-22.5349382540588,-4.22981239330733,
12.));
#180577=CARTESIAN_POINT('Ctrl Pts',(-22.5473734368086,-4.23461338456712,
12.));
#180578=CARTESIAN_POINT('Ctrl Pts',(-22.5599510166429,-4.23951550052522,
12.));
#180579=CARTESIAN_POINT('Ctrl Pts',(-22.572668704992,-4.24451879404851,
12.));
#180580=CARTESIAN_POINT('Ctrl Pts',(-22.5855242662477,-4.24962331444177,
12.));
#180581=CARTESIAN_POINT('Ctrl Pts',(-22.5985155158636,-4.25482910755481,
12.));
#180582=CARTESIAN_POINT('Ctrl Pts',(-22.6116403184821,-4.26013621588305,
12.));
#180583=CARTESIAN_POINT('Ctrl Pts',(-22.6248965859977,-4.26554467865576,
12.));
#180584=CARTESIAN_POINT('Ctrl Pts',(-22.6382822758172,-4.27105453193004,
12.));
#180585=CARTESIAN_POINT('Ctrl Pts',(-22.6517953893303,-4.2766658086912,
12.));
#180586=CARTESIAN_POINT('Ctrl Pts',(-22.6654339703109,-4.28237853894059,
12.));
#180587=CARTESIAN_POINT('Ctrl Pts',(-22.6791961033538,-4.28819274977763,
12.));
#180588=CARTESIAN_POINT('Ctrl Pts',(-22.6930799122548,-4.29410846547056,
12.));
#180589=CARTESIAN_POINT('Ctrl Pts',(-22.7070835587564,-4.3001257075406,
12.));
#180590=CARTESIAN_POINT('Ctrl Pts',(-22.7212052413386,-4.30624449484069,
12.));
#180591=CARTESIAN_POINT('Ctrl Pts',(-22.7354431939926,-4.31246484362549,
12.));
#180592=CARTESIAN_POINT('Ctrl Pts',(-22.7497956849848,-4.31878676761235,
12.));
#180593=CARTESIAN_POINT('Ctrl Pts',(-22.7642610156475,-4.32521027803754,
12.));
#180594=CARTESIAN_POINT('Ctrl Pts',(-22.7788375194076,-4.3317353837319,
12.));
#180595=CARTESIAN_POINT('Ctrl Pts',(-22.7935235607806,-4.33836209118446,
12.));
#180596=CARTESIAN_POINT('Ctrl Pts',(-22.8083175343791,-4.34509040460062,
12.));
#180597=CARTESIAN_POINT('Ctrl Pts',(-22.8232178638876,-4.35192032594791,
12.));
#180598=CARTESIAN_POINT('Ctrl Pts',(-22.8382230011184,-4.35885185500546,
12.));
#180599=CARTESIAN_POINT('Ctrl Pts',(-22.8533314252422,-4.36588498942997,
12.));
#180600=CARTESIAN_POINT('Ctrl Pts',(-22.8685416419725,-4.37301972480745,
12.));
#180601=CARTESIAN_POINT('Ctrl Pts',(-22.8838521827701,-4.38025605470093,
12.));
#180602=CARTESIAN_POINT('Ctrl Pts',(-22.8992616040108,-4.38759397068406,
12.));
#180603=CARTESIAN_POINT('Ctrl Pts',(-22.9147684862426,-4.39503346238473,
12.));
#180604=CARTESIAN_POINT('Ctrl Pts',(-22.930371433555,-4.40257451754323,
12.));
#180605=CARTESIAN_POINT('Ctrl Pts',(-22.9460690729093,-4.41021712205553,
12.));
#180606=CARTESIAN_POINT('Ctrl Pts',(-22.9618600534866,-4.41796126001302,
12.));
#180607=CARTESIAN_POINT('Ctrl Pts',(-22.977743046002,-4.42580691372751,
12.));
#180608=CARTESIAN_POINT('Ctrl Pts',(-22.9937167421006,-4.43375406376879,
12.));
#180609=CARTESIAN_POINT('Ctrl Pts',(-23.0097798538395,-4.44180268901643,
12.));
#180610=CARTESIAN_POINT('Ctrl Pts',(-23.0259311131392,-4.44995276669686,
12.));
#180611=CARTESIAN_POINT('Ctrl Pts',(-23.0421692712467,-4.45820427241683,
12.));
#180612=CARTESIAN_POINT('Ctrl Pts',(-23.0584930981732,-4.4665571801823,
12.));
#180613=CARTESIAN_POINT('Ctrl Pts',(-23.0749013821881,-4.47501146242856,
12.));
#180614=CARTESIAN_POINT('Ctrl Pts',(-23.0913929293922,-4.48356709006788,
12.));
#180615=CARTESIAN_POINT('Ctrl Pts',(-23.1079665632636,-4.49222403252216,
12.));
#180616=CARTESIAN_POINT('Ctrl Pts',(-23.1246211242115,-4.50098225775171,
12.));
#180617=CARTESIAN_POINT('Ctrl Pts',(-23.1413554691123,-4.5098417322706,
12.));
#180618=CARTESIAN_POINT('Ctrl Pts',(-23.1581684708761,-4.51880242116748,
12.));
#180619=CARTESIAN_POINT('Ctrl Pts',(-23.1750590180908,-4.52786428815014,
12.));
#180620=CARTESIAN_POINT('Ctrl Pts',(-23.1920260146465,-4.53702729557566,
12.));
#180621=CARTESIAN_POINT('Ctrl Pts',(-23.2090683793629,-4.54629140447544,
12.));
#180622=CARTESIAN_POINT('Ctrl Pts',(-23.2261850456064,-4.55565657456975,
12.));
#180623=CARTESIAN_POINT('Ctrl Pts',(-23.2433749609131,-4.56512276427839,
12.));
#180624=CARTESIAN_POINT('Ctrl Pts',(-23.2606370866866,-4.57468993076097,
12.));
#180625=CARTESIAN_POINT('Ctrl Pts',(-23.2779703978876,-4.5843580299469,
12.));
#180626=CARTESIAN_POINT('Ctrl Pts',(-23.2953738827191,-4.5941270165575,
12.));
#180627=CARTESIAN_POINT('Ctrl Pts',(-23.3128465423115,-4.60399684412163,
12.));
#180628=CARTESIAN_POINT('Ctrl Pts',(-23.3303873903938,-4.6139674649783,
12.));
#180629=CARTESIAN_POINT('Ctrl Pts',(-23.3479954530272,-4.62403883030805,
12.));
#180630=CARTESIAN_POINT('Ctrl Pts',(-23.3656697683489,-4.63421089016541,
12.));
#180631=CARTESIAN_POINT('Ctrl Pts',(-23.3834093863068,-4.6444835934993,
12.));
#180632=CARTESIAN_POINT('Ctrl Pts',(-23.4012133683959,-4.65485688816924,
12.));
#180633=CARTESIAN_POINT('Ctrl Pts',(-23.4190807873803,-4.6653307209467,
12.));
#180634=CARTESIAN_POINT('Ctrl Pts',(-23.4370107270451,-4.67590503753058,
12.));
#180635=CARTESIAN_POINT('Ctrl Pts',(-23.455002281986,-4.68657978258303,
12.));
#180636=CARTESIAN_POINT('Ctrl Pts',(-23.4730545573853,-4.69735489975024,
12.));
#180637=CARTESIAN_POINT('Ctrl Pts',(-23.491166668789,-4.70823033167818,
12.));
#180638=CARTESIAN_POINT('Ctrl Pts',(-23.509337741878,-4.71920602001901,
12.));
#180639=CARTESIAN_POINT('Ctrl Pts',(-23.5275669122372,-4.7302819054303,
12.));
#180640=CARTESIAN_POINT('Ctrl Pts',(-23.545853325171,-4.74145792760698,
12.));
#180641=CARTESIAN_POINT('Ctrl Pts',(-23.5641961355168,-4.75273402530617,
12.));
#180642=CARTESIAN_POINT('Ctrl Pts',(-23.5825945074535,-4.76411013636251,
12.));
#180643=CARTESIAN_POINT('Ctrl Pts',(-23.6010476143099,-4.77558619769872,
12.));
#180644=CARTESIAN_POINT('Ctrl Pts',(-23.6195546383624,-4.78716214532098,
12.));
#180645=CARTESIAN_POINT('Ctrl Pts',(-23.6381147706579,-4.7988379143322,
12.));
#180646=CARTESIAN_POINT('Ctrl Pts',(-23.6567272108628,-4.81061343896432,
12.));
#180647=CARTESIAN_POINT('Ctrl Pts',(-23.675391167102,-4.82248865259562,
12.));
#180648=CARTESIAN_POINT('Ctrl Pts',(-23.6941058557971,-4.83446348776265,
12.));
#180649=CARTESIAN_POINT('Ctrl Pts',(-23.7128705015017,-4.84653787616425,
12.));
#180650=CARTESIAN_POINT('Ctrl Pts',(-23.7316843367313,-4.85871174865499,
12.));
#180651=CARTESIAN_POINT('Ctrl Pts',(-23.7505466018245,-4.87098503527152,
12.));
#180652=CARTESIAN_POINT('Ctrl Pts',(-23.7694565448049,-4.88335766525573,
12.));
#180653=CARTESIAN_POINT('Ctrl Pts',(-23.7884134212384,-4.89582956706775,
12.));
#180654=CARTESIAN_POINT('Ctrl Pts',(-23.8074164940896,-4.90840066839344,
12.));
#180655=CARTESIAN_POINT('Ctrl Pts',(-23.8264650335717,-4.92107089613969,
12.));
#180656=CARTESIAN_POINT('Ctrl Pts',(-23.8455583170057,-4.93384017643432,
12.));
#180657=CARTESIAN_POINT('Ctrl Pts',(-23.8646956287168,-4.9467084346586,
12.));
#180658=CARTESIAN_POINT('Ctrl Pts',(-23.8838762599218,-4.9596755954656,
12.));
#180659=CARTESIAN_POINT('Ctrl Pts',(-23.9030995086163,-4.97274158279226,
12.));
#180660=CARTESIAN_POINT('Ctrl Pts',(-23.9223646794592,-4.98590631986532,
12.));
#180661=CARTESIAN_POINT('Ctrl Pts',(-23.9416710836529,-4.99916972919306,
12.));
#180662=CARTESIAN_POINT('Ctrl Pts',(-23.9610180388271,-5.01253173257453,
12.));
#180663=CARTESIAN_POINT('Ctrl Pts',(-23.9804048689227,-5.02599225112454,
12.));
#180664=CARTESIAN_POINT('Ctrl Pts',(-23.9998309040746,-5.03955120528521,
12.));
#180665=CARTESIAN_POINT('Ctrl Pts',(-24.0192954804896,-5.05320851483065,
12.));
#180666=CARTESIAN_POINT('Ctrl Pts',(-24.0387979403268,-5.06696409886641,
12.));
#180667=CARTESIAN_POINT('Ctrl Pts',(-24.0583376315638,-5.08081787581276,
12.));
#180668=CARTESIAN_POINT('Ctrl Pts',(-24.0779139079266,-5.09476976342625,
12.));
#180669=CARTESIAN_POINT('Ctrl Pts',(-24.0975261288446,-5.10881967883132,
12.));
#180670=CARTESIAN_POINT('Ctrl Pts',(-24.117173659394,-5.12296753853859,
12.));
#180671=CARTESIAN_POINT('Ctrl Pts',(-24.1368558702443,-5.13721325845744,
12.));
#180672=CARTESIAN_POINT('Ctrl Pts',(-24.156572137597,-5.15155675390075,
12.));
#180673=CARTESIAN_POINT('Ctrl Pts',(-24.1763218431343,-5.16599793957979,
12.));
#180674=CARTESIAN_POINT('Ctrl Pts',(-24.1961043738754,-5.18053672961392,
12.));
#180675=CARTESIAN_POINT('Ctrl Pts',(-24.215919122017,-5.19517303753643,
12.));
#180676=CARTESIAN_POINT('Ctrl Pts',(-24.2357654847765,-5.20990677629173,
12.));
#180677=CARTESIAN_POINT('Ctrl Pts',(-24.2556428642294,-5.22473785822441,
12.));
#180678=CARTESIAN_POINT('Ctrl Pts',(-24.2755506671526,-5.23966619506289,
12.));
#180679=CARTESIAN_POINT('Ctrl Pts',(-24.2954883048448,-5.25469169788856,
12.));
#180680=CARTESIAN_POINT('Ctrl Pts',(-24.3154551932222,-5.26981427718796,
12.));
#180681=CARTESIAN_POINT('Ctrl Pts',(-24.3354507529415,-5.28503384290644,
12.));
#180682=CARTESIAN_POINT('Ctrl Pts',(-24.3554744095075,-5.30035030449058,
12.));
#180683=CARTESIAN_POINT('Ctrl Pts',(-24.3755255933917,-5.31576357092524,
12.));
#180684=CARTESIAN_POINT('Ctrl Pts',(-24.3956037401293,-5.33127355076036,
12.));
#180685=CARTESIAN_POINT('Ctrl Pts',(-24.4157082904615,-5.34688015213546,
12.));
#180686=CARTESIAN_POINT('Ctrl Pts',(-24.4358386899152,-5.36258328273639,
12.));
#180687=CARTESIAN_POINT('Ctrl Pts',(-24.4559943883159,-5.37838284973706,
12.));
#180688=CARTESIAN_POINT('Ctrl Pts',(-24.4761748393322,-5.3942787597383,
12.));
#180689=CARTESIAN_POINT('Ctrl Pts',(-24.4963794999831,-5.41027091869242,
12.));
#180690=CARTESIAN_POINT('Ctrl Pts',(-24.5166078302107,-5.42635923183411,
12.));
#180691=CARTESIAN_POINT('Ctrl Pts',(-24.5368592922861,-5.44254360356865,
12.));
#180692=CARTESIAN_POINT('Ctrl Pts',(-24.5571333514841,-5.45882393762244,
12.));
#180693=CARTESIAN_POINT('Ctrl Pts',(-24.5774294770329,-5.47520013724403,
12.));
#180694=CARTESIAN_POINT('Ctrl Pts',(-24.5977471429365,-5.49167210537235,
12.));
#180695=CARTESIAN_POINT('Ctrl Pts',(-24.618085828918,-5.50823974481959,
12.));
#180696=CARTESIAN_POINT('Ctrl Pts',(-24.6384450211466,-5.52490295840996,
12.));
#180697=CARTESIAN_POINT('Ctrl Pts',(-24.6588242134733,-5.54166164919593,
12.));
#180698=CARTESIAN_POINT('Ctrl Pts',(-24.6792229061785,-5.55851572025389,
12.));
#180699=CARTESIAN_POINT('Ctrl Pts',(-24.6996406035507,-5.57546507427766,
12.));
#180700=CARTESIAN_POINT('Ctrl Pts',(-24.7200768119079,-5.59250961323995,
12.));
#180701=CARTESIAN_POINT('Ctrl Pts',(-24.7405310372736,-5.60964923798495,
12.));
#180702=CARTESIAN_POINT('Ctrl Pts',(-24.76100278357,-5.62688384790919,12.));
#180703=CARTESIAN_POINT('Ctrl Pts',(-24.7814915496728,-5.64421334042247,
12.));
#180704=CARTESIAN_POINT('Ctrl Pts',(-24.8019968304618,-5.66163761114903,
12.));
#180705=CARTESIAN_POINT('Ctrl Pts',(-24.822518122386,-5.67915655496524,
12.));
#180706=CARTESIAN_POINT('Ctrl Pts',(-24.8430549277634,-5.69677006679429,
12.));
#180707=CARTESIAN_POINT('Ctrl Pts',(-24.8636067597677,-5.71447804252019,
12.));
#180708=CARTESIAN_POINT('Ctrl Pts',(-24.8841731467219,-5.73228037976926,
12.));
#180709=CARTESIAN_POINT('Ctrl Pts',(-24.9047536376467,-5.75017697890813,
12.));
#180710=CARTESIAN_POINT('Ctrl Pts',(-24.9253478043632,-5.76816774342236,
12.));
#180711=CARTESIAN_POINT('Ctrl Pts',(-24.9459552293308,-5.78625257775703,
12.));
#180712=CARTESIAN_POINT('Ctrl Pts',(-24.9665754954462,-5.80443138549747,
12.));
#180713=CARTESIAN_POINT('Ctrl Pts',(-24.9872081752709,-5.82270406744214,
12.));
#180714=CARTESIAN_POINT('Ctrl Pts',(-25.0078528200558,-5.84107051963073,
12.));
#180715=CARTESIAN_POINT('Ctrl Pts',(-25.0285089498922,-5.8595306315681,
12.));
#180716=CARTESIAN_POINT('Ctrl Pts',(-25.0491760405965,-5.87808428385329,
12.));
#180717=CARTESIAN_POINT('Ctrl Pts',(-25.0698535426593,-5.89673135155459,
12.));
#180718=CARTESIAN_POINT('Ctrl Pts',(-25.0905409050863,-5.91547170844382,
12.));
#180719=CARTESIAN_POINT('Ctrl Pts',(-25.1112375971182,-5.93430523086776,
12.));
#180720=CARTESIAN_POINT('Ctrl Pts',(-25.1319431317273,-5.95323180187348,
12.));
#180721=CARTESIAN_POINT('Ctrl Pts',(-25.1526570863065,-5.97225131495636,
12.));
#180722=CARTESIAN_POINT('Ctrl Pts',(-25.1733791296154,-5.99136367859838,
12.));
#180723=CARTESIAN_POINT('Ctrl Pts',(-25.1941090269638,-6.0105688180476,
12.));
#180724=CARTESIAN_POINT('Ctrl Pts',(-25.2148466201368,-6.02986667390187,
12.));
#180725=CARTESIAN_POINT('Ctrl Pts',(-25.2355918138798,-6.04925720151412,
12.));
#180726=CARTESIAN_POINT('Ctrl Pts',(-25.2521940105523,-6.06484373634696,
12.));
#180727=CARTESIAN_POINT('Ctrl Pts',(-25.2646490489816,-6.07657531787577,
12.));
#180728=CARTESIAN_POINT('Ctrl Pts',(-25.2729539149479,-6.08441489609824,
12.));
#180729=CARTESIAN_POINT('Ctrl Pts',(-25.2771067246846,-6.08833931617698,
12.));
#180730=CARTESIAN_POINT('',(-24.9347862158358,-7.36589684767343,12.));
#180731=CARTESIAN_POINT('Origin',(0.,0.,12.));
#180732=CARTESIAN_POINT('',(-21.2610617890679,-7.52250298901264,12.));
#180733=CARTESIAN_POINT('Ctrl Pts',(-24.9347862158358,-7.36589684767343,
12.));
#180734=CARTESIAN_POINT('Ctrl Pts',(-24.9292275670705,-7.36721909029059,
12.));
#180735=CARTESIAN_POINT('Ctrl Pts',(-24.9181155530631,-7.36985593120696,
12.));
#180736=CARTESIAN_POINT('Ctrl Pts',(-24.9014633826201,-7.37378825962717,
12.));
#180737=CARTESIAN_POINT('Ctrl Pts',(-24.8792921911309,-7.3789854964161,
12.));
#180738=CARTESIAN_POINT('Ctrl Pts',(-24.8516310625367,-7.38540558904945,
12.));
#180739=CARTESIAN_POINT('Ctrl Pts',(-24.8240228521042,-7.39174922586841,
12.));
#180740=CARTESIAN_POINT('Ctrl Pts',(-24.7964676646518,-7.39801641583612,
12.));
#180741=CARTESIAN_POINT('Ctrl Pts',(-24.7689656669005,-7.40420718661754,
12.));
#180742=CARTESIAN_POINT('Ctrl Pts',(-24.7415170994754,-7.41032159082173,
12.));
#180743=CARTESIAN_POINT('Ctrl Pts',(-24.7141222949988,-7.41635971481243,
12.));
#180744=CARTESIAN_POINT('Ctrl Pts',(-24.6867816727118,-7.42232167765762,
12.));
#180745=CARTESIAN_POINT('Ctrl Pts',(-24.659495712869,-7.4282076215868,12.));
#180746=CARTESIAN_POINT('Ctrl Pts',(-24.6322649369472,-7.4340177048922,
12.));
#180747=CARTESIAN_POINT('Ctrl Pts',(-24.6050898852349,-7.43975209375374,
12.));
#180748=CARTESIAN_POINT('Ctrl Pts',(-24.5779710960865,-7.44541095473162,
12.));
#180749=CARTESIAN_POINT('Ctrl Pts',(-24.5509090831579,-7.45099444651295,
12.));
#180750=CARTESIAN_POINT('Ctrl Pts',(-24.52390431731,-7.45650271336045,12.));
#180751=CARTESIAN_POINT('Ctrl Pts',(-24.4969572391509,-7.46193588961641,
12.));
#180752=CARTESIAN_POINT('Ctrl Pts',(-24.4700682684544,-7.46729410308922,
12.));
#180753=CARTESIAN_POINT('Ctrl Pts',(-24.4432378146501,-7.47257747883318,
12.));
#180754=CARTESIAN_POINT('Ctrl Pts',(-24.4164662871165,-7.47778614286573,
12.));
#180755=CARTESIAN_POINT('Ctrl Pts',(-24.3897541049248,-7.48292022569253,
12.));
#180756=CARTESIAN_POINT('Ctrl Pts',(-24.3631017084513,-7.48797986651827,
12.));
#180757=CARTESIAN_POINT('Ctrl Pts',(-24.3365095573673,-7.49296521252329,
12.));
#180758=CARTESIAN_POINT('Ctrl Pts',(-24.3099781253345,-7.49787641695358,
12.));
#180759=CARTESIAN_POINT('Ctrl Pts',(-24.2835078958966,-7.50271363765098,
12.));
#180760=CARTESIAN_POINT('Ctrl Pts',(-24.2570993577032,-7.50747703535114,
12.));
#180761=CARTESIAN_POINT('Ctrl Pts',(-24.230753000389,-7.51216677222198,
12.));
#180762=CARTESIAN_POINT('Ctrl Pts',(-24.2044693092356,-7.51678300997997,
12.));
#180763=CARTESIAN_POINT('Ctrl Pts',(-24.1782487641602,-7.52132590953862,
12.));
#180764=CARTESIAN_POINT('Ctrl Pts',(-24.152091842537,-7.52579563201478,
12.));
#180765=CARTESIAN_POINT('Ctrl Pts',(-24.1259990209211,-7.53019233935536,
12.));
#180766=CARTESIAN_POINT('Ctrl Pts',(-24.0999707772643,-7.53451619514658,
12.));
#180767=CARTESIAN_POINT('Ctrl Pts',(-24.0740075927984,-7.53876736531004,
12.));
#180768=CARTESIAN_POINT('Ctrl Pts',(-24.0481099543353,-7.54294601896127,
12.));
#180769=CARTESIAN_POINT('Ctrl Pts',(-24.0222783554531,-7.54705232885894,
12.));
#180770=CARTESIAN_POINT('Ctrl Pts',(-23.9965132953187,-7.55108647097431,
12.));
#180771=CARTESIAN_POINT('Ctrl Pts',(-23.9708152779886,-7.55504862424807,
12.));
#180772=CARTESIAN_POINT('Ctrl Pts',(-23.9451848115002,-7.55893897027679,
12.));
#180773=CARTESIAN_POINT('Ctrl Pts',(-23.9196224070759,-7.56275769304772,
12.));
#180774=CARTESIAN_POINT('Ctrl Pts',(-23.8941285782002,-7.5665049786379,
12.));
#180775=CARTESIAN_POINT('Ctrl Pts',(-23.8687038399595,-7.57018101500709,
12.));
#180776=CARTESIAN_POINT('Ctrl Pts',(-23.8433487096132,-7.57378599219814,
12.));
#180777=CARTESIAN_POINT('Ctrl Pts',(-23.8180637069976,-7.57732010249065,
12.));
#180778=CARTESIAN_POINT('Ctrl Pts',(-23.7928493549908,-7.58078354058212,
12.));
#180779=CARTESIAN_POINT('Ctrl Pts',(-23.7677061799376,-7.5841765037627,
12.));
#180780=CARTESIAN_POINT('Ctrl Pts',(-23.7426347121006,-7.58749919210825,
12.));
#180781=CARTESIAN_POINT('Ctrl Pts',(-23.7176354860457,-7.5907518086532,
12.));
#180782=CARTESIAN_POINT('Ctrl Pts',(-23.6927090405066,-7.59393455934034,
12.));
#180783=CARTESIAN_POINT('Ctrl Pts',(-23.6678559182875,-7.59704765299566,
12.));
#180784=CARTESIAN_POINT('Ctrl Pts',(-23.6430766661418,-7.60009130130125,
12.));
#180785=CARTESIAN_POINT('Ctrl Pts',(-23.6183718346576,-7.60306571877805,
12.));
#180786=CARTESIAN_POINT('Ctrl Pts',(-23.5937419781245,-7.60597112277093,
12.));
#180787=CARTESIAN_POINT('Ctrl Pts',(-23.5691876544244,-7.60880773344599,
12.));
#180788=CARTESIAN_POINT('Ctrl Pts',(-23.544709425203,-7.61157577385371,
12.));
#180789=CARTESIAN_POINT('Ctrl Pts',(-23.5203078560129,-7.61427546999297,
12.));
#180790=CARTESIAN_POINT('Ctrl Pts',(-23.4959835164609,-7.61690705088318,
12.));
#180791=CARTESIAN_POINT('Ctrl Pts',(-23.4717369803438,-7.61947074863976,
12.));
#180792=CARTESIAN_POINT('Ctrl Pts',(-23.4475688257854,-7.62196679855954,
12.));
#180793=CARTESIAN_POINT('Ctrl Pts',(-23.4234796353542,-7.62439543920049,
12.));
#180794=CARTESIAN_POINT('Ctrl Pts',(-23.399469996112,-7.62675691240328,
12.));
#180795=CARTESIAN_POINT('Ctrl Pts',(-23.3755404996636,-7.62905146332592,
12.));
#180796=CARTESIAN_POINT('Ctrl Pts',(-23.3516917421972,-7.63127934048136,
12.));
#180797=CARTESIAN_POINT('Ctrl Pts',(-23.3279243245241,-7.63344079578161,
12.));
#180798=CARTESIAN_POINT('Ctrl Pts',(-23.3042388521022,-7.63553608458782,
12.));
#180799=CARTESIAN_POINT('Ctrl Pts',(-23.2806359350855,-7.63756546576374,
12.));
#180800=CARTESIAN_POINT('Ctrl Pts',(-23.2571161884488,-7.63952920172835,
12.));
#180801=CARTESIAN_POINT('Ctrl Pts',(-23.2336802320912,-7.64142755851504,
12.));
#180802=CARTESIAN_POINT('Ctrl Pts',(-23.2103286909398,-7.64326080583679,
12.));
#180803=CARTESIAN_POINT('Ctrl Pts',(-23.1870621950452,-7.64502921715482,
12.));
#180804=CARTESIAN_POINT('Ctrl Pts',(-23.1638813796694,-7.64673306975804,
12.));
#180805=CARTESIAN_POINT('Ctrl Pts',(-23.1407868853819,-7.64837264482942,
12.));
#180806=CARTESIAN_POINT('Ctrl Pts',(-23.1177793581679,-7.64994822749859,
12.));
#180807=CARTESIAN_POINT('Ctrl Pts',(-23.094859449525,-7.65146010690475,
12.));
#180808=CARTESIAN_POINT('Ctrl Pts',(-23.072027816555,-7.65290857626357,
12.));
#180809=CARTESIAN_POINT('Ctrl Pts',(-23.0492851220528,-7.65429393293945,
12.));
#180810=CARTESIAN_POINT('Ctrl Pts',(-23.0266320345787,-7.65561647852533,
12.));
#180811=CARTESIAN_POINT('Ctrl Pts',(-23.0040692285814,-7.65687651891304,
12.));
#180812=CARTESIAN_POINT('Ctrl Pts',(-22.9815973845296,-7.65807436436431,
12.));
#180813=CARTESIAN_POINT('Ctrl Pts',(-22.959217189033,-7.65921032958901,
12.));
#180814=CARTESIAN_POINT('Ctrl Pts',(-22.9369293349593,-7.66028473382777,
12.));
#180815=CARTESIAN_POINT('Ctrl Pts',(-22.9147345215421,-7.66129790094107,
12.));
#180816=CARTESIAN_POINT('Ctrl Pts',(-22.8926334544883,-7.66225015950155,
12.));
#180817=CARTESIAN_POINT('Ctrl Pts',(-22.8706268461283,-7.66314184287336,
12.));
#180818=CARTESIAN_POINT('Ctrl Pts',(-22.848715415557,-7.66397328929802,
12.));
#180819=CARTESIAN_POINT('Ctrl Pts',(-22.8268998887678,-7.66474484198548,
12.));
#180820=CARTESIAN_POINT('Ctrl Pts',(-22.8051809987833,-7.66545684920987,
12.));
#180821=CARTESIAN_POINT('Ctrl Pts',(-22.7835594857699,-7.66610966441272,
12.));
#180822=CARTESIAN_POINT('Ctrl Pts',(-22.7620360971843,-7.66670364630298,
12.));
#180823=CARTESIAN_POINT('Ctrl Pts',(-22.7406115879513,-7.66723915895439,
12.));
#180824=CARTESIAN_POINT('Ctrl Pts',(-22.7192867206245,-7.66771657191027,
12.));
#180825=CARTESIAN_POINT('Ctrl Pts',(-22.6980622655446,-7.66813626029274,
12.));
#180826=CARTESIAN_POINT('Ctrl Pts',(-22.6769390009885,-7.66849860491742,
12.));
#180827=CARTESIAN_POINT('Ctrl Pts',(-22.6559177133127,-7.66880399241322,
12.));
#180828=CARTESIAN_POINT('Ctrl Pts',(-22.6349991971541,-7.66905281533714,
12.));
#180829=CARTESIAN_POINT('Ctrl Pts',(-22.6141842556243,-7.66924547229413,
12.));
#180830=CARTESIAN_POINT('Ctrl Pts',(-22.5934737004953,-7.66938236806232,
12.));
#180831=CARTESIAN_POINT('Ctrl Pts',(-22.5728683523831,-7.66946391372305,
12.));
#180832=CARTESIAN_POINT('Ctrl Pts',(-22.5523690409116,-7.66949052679692,
12.));
#180833=CARTESIAN_POINT('Ctrl Pts',(-22.53197660492,-7.66946263138143,12.));
#180834=CARTESIAN_POINT('Ctrl Pts',(-22.5116918927032,-7.66938065829107,
12.));
#180835=CARTESIAN_POINT('Ctrl Pts',(-22.4915157622312,-7.66924504520314,
12.));
#180836=CARTESIAN_POINT('Ctrl Pts',(-22.47144908137,-7.6690562368083,12.));
#180837=CARTESIAN_POINT('Ctrl Pts',(-22.4514927280855,-7.66881468496634,
12.));
#180838=CARTESIAN_POINT('Ctrl Pts',(-22.4316475906603,-7.66852084886704,
12.));
#180839=CARTESIAN_POINT('Ctrl Pts',(-22.4119145679758,-7.66817519519639,
12.));
#180840=CARTESIAN_POINT('Ctrl Pts',(-22.3922945697773,-7.66777819830789,
12.));
#180841=CARTESIAN_POINT('Ctrl Pts',(-22.372788516936,-7.66733034039882,
12.));
#180842=CARTESIAN_POINT('Ctrl Pts',(-22.3533973417021,-7.66683211169158,
12.));
#180843=CARTESIAN_POINT('Ctrl Pts',(-22.3341219879469,-7.66628401061952,
12.));
#180844=CARTESIAN_POINT('Ctrl Pts',(-22.314963411484,-7.66568654402493,
12.));
#180845=CARTESIAN_POINT('Ctrl Pts',(-22.2959225803937,-7.66504022736298,
12.));
#180846=CARTESIAN_POINT('Ctrl Pts',(-22.2770004753335,-7.66434558490978,
12.));
#180847=CARTESIAN_POINT('Ctrl Pts',(-22.258198089848,-7.6636031499764,12.));
#180848=CARTESIAN_POINT('Ctrl Pts',(-22.2395164306547,-7.66281346512508,
12.));
#180849=CARTESIAN_POINT('Ctrl Pts',(-22.2209565180085,-7.66197708240399,
12.));
#180850=CARTESIAN_POINT('Ctrl Pts',(-22.2025193860964,-7.6610945635927,
12.));
#180851=CARTESIAN_POINT('Ctrl Pts',(-22.1842060834091,-7.66016648045004,
12.));
#180852=CARTESIAN_POINT('Ctrl Pts',(-22.1660176731178,-7.6591934149693,
12.));
#180853=CARTESIAN_POINT('Ctrl Pts',(-22.1479552334211,-7.65817595963349,
12.));
#180854=CARTESIAN_POINT('Ctrl Pts',(-22.1300198579675,-7.65711471769396,
12.));
#180855=CARTESIAN_POINT('Ctrl Pts',(-22.1122126563329,-7.65601030346806,
12.));
#180856=CARTESIAN_POINT('Ctrl Pts',(-22.094534754469,-7.65486334263643,
12.));
#180857=CARTESIAN_POINT('Ctrl Pts',(-22.0769872951596,-7.65367447254949,
12.));
#180858=CARTESIAN_POINT('Ctrl Pts',(-22.0595714384431,-7.65244434253112,
12.));
#180859=CARTESIAN_POINT('Ctrl Pts',(-22.0422883621174,-7.65117361421358,
12.));
#180860=CARTESIAN_POINT('Ctrl Pts',(-22.0251392623209,-7.64986296190168,
12.));
#180861=CARTESIAN_POINT('Ctrl Pts',(-22.0081253540774,-7.64851307293351,
12.));
#180862=CARTESIAN_POINT('Ctrl Pts',(-21.9912478718542,-7.64712464805249,
12.));
#180863=CARTESIAN_POINT('Ctrl Pts',(-21.9745080700798,-7.64569840177335,
12.));
#180864=CARTESIAN_POINT('Ctrl Pts',(-21.9579072237651,-7.64423506279122,
12.));
#180865=CARTESIAN_POINT('Ctrl Pts',(-21.9414466292072,-7.64273537442682,
12.));
#180866=CARTESIAN_POINT('Ctrl Pts',(-21.9251276046546,-7.64120009506531,
12.));
#180867=CARTESIAN_POINT('Ctrl Pts',(-21.9089514909874,-7.63962999860927,
12.));
#180868=CARTESIAN_POINT('Ctrl Pts',(-21.8929196523514,-7.63802587492034,
12.));
#180869=CARTESIAN_POINT('Ctrl Pts',(-21.8770334769496,-7.63638853033399,
12.));
#180870=CARTESIAN_POINT('Ctrl Pts',(-21.8612943779089,-7.63471878821225,
12.));
#180871=CARTESIAN_POINT('Ctrl Pts',(-21.8457037941084,-7.63301748948935,
12.));
#180872=CARTESIAN_POINT('Ctrl Pts',(-21.8302631910195,-7.63128549323022,
12.));
#180873=CARTESIAN_POINT('Ctrl Pts',(-21.814974061509,-7.62952367718126,
12.));
#180874=CARTESIAN_POINT('Ctrl Pts',(-21.799837926858,-7.62773293842389,
12.));
#180875=CARTESIAN_POINT('Ctrl Pts',(-21.7848563378021,-7.62591419404512,
12.));
#180876=CARTESIAN_POINT('Ctrl Pts',(-21.7700308755584,-7.62406838181166,
12.));
#180877=CARTESIAN_POINT('Ctrl Pts',(-21.7553631528328,-7.62219646084228,
12.));
#180878=CARTESIAN_POINT('Ctrl Pts',(-21.7408548148656,-7.62029941230854,
12.));
#180879=CARTESIAN_POINT('Ctrl Pts',(-21.7265075407975,-7.61837824030537,
12.));
#180880=CARTESIAN_POINT('Ctrl Pts',(-21.7123230449834,-7.6164339727042,
12.));
#180881=CARTESIAN_POINT('Ctrl Pts',(-21.6983030783322,-7.61446766202786,
12.));
#180882=CARTESIAN_POINT('Ctrl Pts',(-21.6844494295815,-7.61248038630268,
12.));
#180883=CARTESIAN_POINT('Ctrl Pts',(-21.6707639267576,-7.61047325000955,
12.));
#180884=CARTESIAN_POINT('Ctrl Pts',(-21.6572484388081,-7.60844738512873,
12.));
#180885=CARTESIAN_POINT('Ctrl Pts',(-21.6439048771743,-7.60640395216356,
12.));
#180886=CARTESIAN_POINT('Ctrl Pts',(-21.6307351973822,-7.60434414118295,
12.));
#180887=CARTESIAN_POINT('Ctrl Pts',(-21.617741400599,-7.60226917285428,
12.));
#180888=CARTESIAN_POINT('Ctrl Pts',(-21.6049255358843,-7.6001802998824,
12.));
#180889=CARTESIAN_POINT('Ctrl Pts',(-21.5922897024466,-7.59807880846194,
12.));
#180890=CARTESIAN_POINT('Ctrl Pts',(-21.5798360518978,-7.59596601973583,
12.));
#180891=CARTESIAN_POINT('Ctrl Pts',(-21.5675667904726,-7.59384329124918,
12.));
#180892=CARTESIAN_POINT('Ctrl Pts',(-21.5554841813462,-7.59171201844776,
12.));
#180893=CARTESIAN_POINT('Ctrl Pts',(-21.543590547011,-7.58957363620013,
12.));
#180894=CARTESIAN_POINT('Ctrl Pts',(-21.5318882716736,-7.58742962034833,
12.));
#180895=CARTESIAN_POINT('Ctrl Pts',(-21.5203798035299,-7.58528148919129,
12.));
#180896=CARTESIAN_POINT('Ctrl Pts',(-21.5090676573873,-7.58313080519179,
12.));
#180897=CARTESIAN_POINT('Ctrl Pts',(-21.4979544192744,-7.58097917790744,
12.));
#180898=CARTESIAN_POINT('Ctrl Pts',(-21.4870427508194,-7.57882826679131,
12.));
#180899=CARTESIAN_POINT('Ctrl Pts',(-21.4763353936762,-7.57667978402987,
12.));
#180900=CARTESIAN_POINT('Ctrl Pts',(-21.4658351740128,-7.57453549743411,
12.));
#180901=CARTESIAN_POINT('Ctrl Pts',(-21.4555450053142,-7.57239723223505,
12.));
#180902=CARTESIAN_POINT('Ctrl Pts',(-21.4454678907509,-7.57026687261165,
12.));
#180903=CARTESIAN_POINT('Ctrl Pts',(-21.4356069261513,-7.56814636360847,
12.));
#180904=CARTESIAN_POINT('Ctrl Pts',(-21.4259653015736,-7.56603771218712,
12.));
#180905=CARTESIAN_POINT('Ctrl Pts',(-21.4165463106254,-7.56394299313684,
12.));
#180906=CARTESIAN_POINT('Ctrl Pts',(-21.4073533630365,-7.56186435703621,
12.));
#180907=CARTESIAN_POINT('Ctrl Pts',(-21.3983899952987,-7.5598040370061,
12.));
#180908=CARTESIAN_POINT('Ctrl Pts',(-21.3896598842117,-7.55776435731416,
12.));
#180909=CARTESIAN_POINT('Ctrl Pts',(-21.3811668478932,-7.55574773403502,
12.));
#180910=CARTESIAN_POINT('Ctrl Pts',(-21.3729148390243,-7.55375667080028,
12.));
#180911=CARTESIAN_POINT('Ctrl Pts',(-21.3649079431865,-7.55179375777443,
12.));
#180912=CARTESIAN_POINT('Ctrl Pts',(-21.3571503685855,-7.54986166521309,
12.));
#180913=CARTESIAN_POINT('Ctrl Pts',(-21.3496464761531,-7.5479631624633,
12.));
#180914=CARTESIAN_POINT('Ctrl Pts',(-21.3424008295038,-7.54610114948346,
12.));
#180915=CARTESIAN_POINT('Ctrl Pts',(-21.3354182340149,-7.54427868151267,
12.));
#180916=CARTESIAN_POINT('Ctrl Pts',(-21.328703791771,-7.5424990037703,12.));
#180917=CARTESIAN_POINT('Ctrl Pts',(-21.3222628524165,-7.54076552038278,
12.));
#180918=CARTESIAN_POINT('Ctrl Pts',(-21.3161009456256,-7.53908175169898,
12.));
#180919=CARTESIAN_POINT('Ctrl Pts',(-21.310223716773,-7.53745129364616,
12.));
#180920=CARTESIAN_POINT('Ctrl Pts',(-21.3046368712157,-7.53587778251735,
12.));
#180921=CARTESIAN_POINT('Ctrl Pts',(-21.2993464250717,-7.53436505309942,
12.));
#180922=CARTESIAN_POINT('Ctrl Pts',(-21.2943588989331,-7.53291726078526,
12.));
#180923=CARTESIAN_POINT('Ctrl Pts',(-21.2896816163842,-7.53153906987855,
12.));
#180924=CARTESIAN_POINT('Ctrl Pts',(-21.2853226580657,-7.53023562438229,
12.));
#180925=CARTESIAN_POINT('Ctrl Pts',(-21.2812902781143,-7.52901217930407,
12.));
#180926=CARTESIAN_POINT('Ctrl Pts',(-21.2775925269652,-7.52787386225332,
12.));
#180927=CARTESIAN_POINT('Ctrl Pts',(-21.2742366113579,-7.5268252691854,
12.));
#180928=CARTESIAN_POINT('Ctrl Pts',(-21.2712301573466,-7.52587126095529,
12.));
#180929=CARTESIAN_POINT('Ctrl Pts',(-21.2685823838671,-7.5250177033353,
12.));
#180930=CARTESIAN_POINT('Ctrl Pts',(-21.2663059157058,-7.52427261074297,
12.));
#180931=CARTESIAN_POINT('Ctrl Pts',(-21.2644161259962,-7.52364573027552,
12.));
#180932=CARTESIAN_POINT('Ctrl Pts',(-21.262927782038,-7.52314642316199,
12.));
#180933=CARTESIAN_POINT('Ctrl Pts',(-21.2618521283555,-7.52278182242669,
12.));
#180934=CARTESIAN_POINT('Ctrl Pts',(-21.261326054066,-7.5226006423166,12.));
#180935=CARTESIAN_POINT('Ctrl Pts',(-21.2611204474866,-7.52252744144903,
12.));
#180936=CARTESIAN_POINT('Ctrl Pts',(-21.2610673466886,-7.5225064970397,
12.));
#180937=CARTESIAN_POINT('Ctrl Pts',(-21.2610617890679,-7.52250298901264,
12.));
#180938=CARTESIAN_POINT('',(-20.7347298079577,-7.33627833380045,12.));
#180939=CARTESIAN_POINT('',(-10.1343606576251,-3.58569854577611,12.));
#180940=CARTESIAN_POINT('',(-20.1004996511507,-7.63019749246977,12.));
#180941=CARTESIAN_POINT('Origin',(-20.56795313141,-7.80764394578302,12.));
#180942=CARTESIAN_POINT('',(-19.6085639972844,-8.81783521984849,12.));
#180943=CARTESIAN_POINT('Origin',(-7.32141292029404E-13,-2.70312158620511E-13,
12.));
#180944=CARTESIAN_POINT('',(-19.84920021178,-9.47413589477548,12.));
#180945=CARTESIAN_POINT('Origin',(-20.0645771135004,-9.0229011551938,12.));
#180946=CARTESIAN_POINT('',(-20.353053841303,-9.71462809124915,12.));
#180947=CARTESIAN_POINT('',(-10.1765269206515,-4.85731404562459,12.));
#180948=CARTESIAN_POINT('',(-22.8400320311649,-12.4230808101438,12.));
#180949=CARTESIAN_POINT('Ctrl Pts',(-20.353053841303,-9.71462809124915,
12.));
#180950=CARTESIAN_POINT('Ctrl Pts',(-20.353060251684,-9.71462954053041,
12.));
#180951=CARTESIAN_POINT('Ctrl Pts',(-20.3531126095522,-9.71465227853041,
12.));
#180952=CARTESIAN_POINT('Ctrl Pts',(-20.3533097561886,-9.7147459035068,
12.));
#180953=CARTESIAN_POINT('Ctrl Pts',(-20.3538098605706,-9.7149897805202,
12.));
#180954=CARTESIAN_POINT('Ctrl Pts',(-20.3548282742361,-9.71549257088172,
12.));
#180955=CARTESIAN_POINT('Ctrl Pts',(-20.3562337557875,-9.71619192554185,
12.));
#180956=CARTESIAN_POINT('Ctrl Pts',(-20.3580133103356,-9.71708493723096,
12.));
#180957=CARTESIAN_POINT('Ctrl Pts',(-20.3601498764344,-9.71816778328006,
12.));
#180958=CARTESIAN_POINT('Ctrl Pts',(-20.3626256913981,-9.71943648548099,
12.));
#180959=CARTESIAN_POINT('Ctrl Pts',(-20.3654261611056,-9.7208877838108,
12.));
#180960=CARTESIAN_POINT('Ctrl Pts',(-20.3685406190576,-9.72251930722489,
12.));
#180961=CARTESIAN_POINT('Ctrl Pts',(-20.371960235676,-9.72432910043194,
12.));
#180962=CARTESIAN_POINT('Ctrl Pts',(-20.3756766651951,-9.7263153173288,
12.));
#180963=CARTESIAN_POINT('Ctrl Pts',(-20.3796805893304,-9.72847589116541,
12.));
#180964=CARTESIAN_POINT('Ctrl Pts',(-20.3839624556742,-9.73080870123727,
12.));
#180965=CARTESIAN_POINT('Ctrl Pts',(-20.3885129129912,-9.73331167102807,
12.));
#180966=CARTESIAN_POINT('Ctrl Pts',(-20.3933234845647,-9.73598292014242,
12.));
#180967=CARTESIAN_POINT('Ctrl Pts',(-20.3983866213331,-9.738820776132,12.));
#180968=CARTESIAN_POINT('Ctrl Pts',(-20.4036953576549,-9.74182369656271,
12.));
#180969=CARTESIAN_POINT('Ctrl Pts',(-20.4092430879861,-9.74499021838537,
12.));
#180970=CARTESIAN_POINT('Ctrl Pts',(-20.4150232777393,-9.74831889242174,
12.));
#180971=CARTESIAN_POINT('Ctrl Pts',(-20.4210295275817,-9.7518082978643,
12.));
#180972=CARTESIAN_POINT('Ctrl Pts',(-20.4272556476629,-9.75545705902417,
12.));
#180973=CARTESIAN_POINT('Ctrl Pts',(-20.4336957355473,-9.75926386289922,
12.));
#180974=CARTESIAN_POINT('Ctrl Pts',(-20.44034423294,-9.76322747195494,12.));
#180975=CARTESIAN_POINT('Ctrl Pts',(-20.447195862298,-9.76734670980891,
12.));
#180976=CARTESIAN_POINT('Ctrl Pts',(-20.4542455817527,-9.77162045104069,
12.));
#180977=CARTESIAN_POINT('Ctrl Pts',(-20.4614885274975,-9.77604760815528,
12.));
#180978=CARTESIAN_POINT('Ctrl Pts',(-20.4689199790669,-9.7806271237332,
12.));
#180979=CARTESIAN_POINT('Ctrl Pts',(-20.4765353711586,-9.78535797314166,
12.));
#180980=CARTESIAN_POINT('Ctrl Pts',(-20.4843302955329,-9.79023916498655,
12.));
#180981=CARTESIAN_POINT('Ctrl Pts',(-20.4923005087943,-9.7952697428833,
12.));
#180982=CARTESIAN_POINT('Ctrl Pts',(-20.5004419312107,-9.80044878520948,
12.));
#180983=CARTESIAN_POINT('Ctrl Pts',(-20.5087506310505,-9.80577540161087,
12.));
#180984=CARTESIAN_POINT('Ctrl Pts',(-20.517222812284,-9.81124873025281,
12.));
#180985=CARTESIAN_POINT('Ctrl Pts',(-20.5258548000629,-9.81686793455942,
12.));
#180986=CARTESIAN_POINT('Ctrl Pts',(-20.5346430299517,-9.82263220080362,
12.));
#180987=CARTESIAN_POINT('Ctrl Pts',(-20.5435840460721,-9.82854073773877,
12.));
#180988=CARTESIAN_POINT('Ctrl Pts',(-20.552674497646,-9.83459277585315,
12.));
#180989=CARTESIAN_POINT('Ctrl Pts',(-20.5619111362402,-9.84078756677565,
12.));
#180990=CARTESIAN_POINT('Ctrl Pts',(-20.5712908125139,-9.84712438256277,
12.));
#180991=CARTESIAN_POINT('Ctrl Pts',(-20.5808104710015,-9.8536025145698,
12.));
#180992=CARTESIAN_POINT('Ctrl Pts',(-20.5904671449754,-9.86022127232747,
12.));
#180993=CARTESIAN_POINT('Ctrl Pts',(-20.6002579513699,-9.86697998242622,
12.));
#180994=CARTESIAN_POINT('Ctrl Pts',(-20.6101800854494,-9.87387798732956,
12.));
#180995=CARTESIAN_POINT('Ctrl Pts',(-20.6202308177474,-9.88091464472675,
12.));
#180996=CARTESIAN_POINT('Ctrl Pts',(-20.6304074914087,-9.88808932697306,
12.));
#180997=CARTESIAN_POINT('Ctrl Pts',(-20.6407075193976,-9.89540142049119,
12.));
#180998=CARTESIAN_POINT('Ctrl Pts',(-20.6511283817414,-9.90285032516692,
12.));
#180999=CARTESIAN_POINT('Ctrl Pts',(-20.6616676228315,-9.91043545377007,
12.));
#181000=CARTESIAN_POINT('Ctrl Pts',(-20.6723228488263,-9.91815623141288,
12.));
#181001=CARTESIAN_POINT('Ctrl Pts',(-20.6830917250255,-9.92601209498748,
12.));
#181002=CARTESIAN_POINT('Ctrl Pts',(-20.6939719732484,-9.93400249259729,
12.));
#181003=CARTESIAN_POINT('Ctrl Pts',(-20.7049613692234,-9.94212688298236,
12.));
#181004=CARTESIAN_POINT('Ctrl Pts',(-20.7160577407579,-9.95038473514948,
12.));
#181005=CARTESIAN_POINT('Ctrl Pts',(-20.7272589658751,-9.95877552798397,
12.));
#181006=CARTESIAN_POINT('Ctrl Pts',(-20.7385629709795,-9.96729874986201,
12.));
#181007=CARTESIAN_POINT('Ctrl Pts',(-20.7499677289627,-9.9759538982347,
12.));
#181008=CARTESIAN_POINT('Ctrl Pts',(-20.761471257499,-9.98474047926852,
12.));
#181009=CARTESIAN_POINT('Ctrl Pts',(-20.7730716175417,-9.9936580075464,
12.));
#181010=CARTESIAN_POINT('Ctrl Pts',(-20.7847669117568,-10.0027060057389,
12.));
#181011=CARTESIAN_POINT('Ctrl Pts',(-20.7965552829908,-10.0118840042786,
12.));
#181012=CARTESIAN_POINT('Ctrl Pts',(-20.8084349126888,-10.0211915410095,
12.));
#181013=CARTESIAN_POINT('Ctrl Pts',(-20.8204040196602,-10.0306281609435,
12.));
#181014=CARTESIAN_POINT('Ctrl Pts',(-20.8324608588909,-10.0401934160234,
12.));
#181015=CARTESIAN_POINT('Ctrl Pts',(-20.8446037203402,-10.0498868648733,
12.));
#181016=CARTESIAN_POINT('Ctrl Pts',(-20.8568309277316,-10.0597080725375,
12.));
#181017=CARTESIAN_POINT('Ctrl Pts',(-20.86914083737,-10.0696566102218,12.));
#181018=CARTESIAN_POINT('Ctrl Pts',(-20.881531837184,-10.0797320551154,
12.));
#181019=CARTESIAN_POINT('Ctrl Pts',(-20.894002345737,-10.0899339901915,
12.));
#181020=CARTESIAN_POINT('Ctrl Pts',(-20.9065508112557,-10.1002620040076,
12.));
#181021=CARTESIAN_POINT('Ctrl Pts',(-20.919175710627,-10.1107156904836,
12.));
#181022=CARTESIAN_POINT('Ctrl Pts',(-20.9318755484734,-10.1212946487057,
12.));
#181023=CARTESIAN_POINT('Ctrl Pts',(-20.9446488563933,-10.1319984827908,
12.));
#181024=CARTESIAN_POINT('Ctrl Pts',(-20.9574941921591,-10.1428268017256,
12.));
#181025=CARTESIAN_POINT('Ctrl Pts',(-20.9704101389369,-10.1537792192065,
12.));
#181026=CARTESIAN_POINT('Ctrl Pts',(-20.9833953044736,-10.1648553534568,
12.));
#181027=CARTESIAN_POINT('Ctrl Pts',(-20.9964483203686,-10.1760548270767,
12.));
#181028=CARTESIAN_POINT('Ctrl Pts',(-21.0095678414486,-10.187377266936,
12.));
#181029=CARTESIAN_POINT('Ctrl Pts',(-21.0227525451107,-10.1988223040425,
12.));
#181030=CARTESIAN_POINT('Ctrl Pts',(-21.0360011306815,-10.2103895734123,
12.));
#181031=CARTESIAN_POINT('Ctrl Pts',(-21.0493123187483,-10.2220787139154,
12.));
#181032=CARTESIAN_POINT('Ctrl Pts',(-21.0626848505663,-10.2338893681567,
12.));
#181033=CARTESIAN_POINT('Ctrl Pts',(-21.0761174875445,-10.2458211823912,
12.));
#181034=CARTESIAN_POINT('Ctrl Pts',(-21.0896090107063,-10.2578738064181,
12.));
#181035=CARTESIAN_POINT('Ctrl Pts',(-21.1031582201627,-10.2700468934744,
12.));
#181036=CARTESIAN_POINT('Ctrl Pts',(-21.1167639345631,-10.2823401001072,
12.));
#181037=CARTESIAN_POINT('Ctrl Pts',(-21.1304249906002,-10.2947530860721,
12.));
#181038=CARTESIAN_POINT('Ctrl Pts',(-21.1441402425843,-10.3072855142687,
12.));
#181039=CARTESIAN_POINT('Ctrl Pts',(-21.1579085619965,-10.3199370506544,
12.));
#181040=CARTESIAN_POINT('Ctrl Pts',(-21.1717288370509,-10.3327073641572,
12.));
#181041=CARTESIAN_POINT('Ctrl Pts',(-21.1855999722416,-10.34559612657,12.));
#181042=CARTESIAN_POINT('Ctrl Pts',(-21.199520887919,-10.3586030124587,
12.));
#181043=CARTESIAN_POINT('Ctrl Pts',(-21.2134905199345,-10.371727699113,
12.));
#181044=CARTESIAN_POINT('Ctrl Pts',(-21.22750781927,-10.3849698664786,12.));
#181045=CARTESIAN_POINT('Ctrl Pts',(-21.2415717516714,-10.3983291970846,
12.));
#181046=CARTESIAN_POINT('Ctrl Pts',(-21.255681297275,-10.4118053759588,
12.));
#181047=CARTESIAN_POINT('Ctrl Pts',(-21.2698354502403,-10.42539809054,12.));
#181048=CARTESIAN_POINT('Ctrl Pts',(-21.2840332184483,-10.4391070306391,
12.));
#181049=CARTESIAN_POINT('Ctrl Pts',(-21.2982736231931,-10.4529318883874,
12.));
#181050=CARTESIAN_POINT('Ctrl Pts',(-21.3125556988731,-10.4668723581768,
12.));
#181051=CARTESIAN_POINT('Ctrl Pts',(-21.3268784926819,-10.4809281365931,
12.));
#181052=CARTESIAN_POINT('Ctrl Pts',(-21.3412410642904,-10.4950989223337,
12.));
#181053=CARTESIAN_POINT('Ctrl Pts',(-21.3556424855814,-10.5093844161685,
12.));
#181054=CARTESIAN_POINT('Ctrl Pts',(-21.3700818403936,-10.5237843209057,
12.));
#181055=CARTESIAN_POINT('Ctrl Pts',(-21.3845582242602,-10.5382983413421,
12.));
#181056=CARTESIAN_POINT('Ctrl Pts',(-21.3990707441497,-10.5529261842108,
12.));
#181057=CARTESIAN_POINT('Ctrl Pts',(-21.4136185181979,-10.5676675581108,
12.));
#181058=CARTESIAN_POINT('Ctrl Pts',(-21.4282006754631,-10.5825221734573,
12.));
#181059=CARTESIAN_POINT('Ctrl Pts',(-21.4428163557144,-10.5974897424622,
12.));
#181060=CARTESIAN_POINT('Ctrl Pts',(-21.4574647092097,-10.6125699790961,
12.));
#181061=CARTESIAN_POINT('Ctrl Pts',(-21.4721448964766,-10.6277625990456,
12.));
#181062=CARTESIAN_POINT('Ctrl Pts',(-21.4868560880889,-10.6430673196607,
12.));
#181063=CARTESIAN_POINT('Ctrl Pts',(-21.5015974644449,-10.6584838598939,
12.));
#181064=CARTESIAN_POINT('Ctrl Pts',(-21.51636821558,-10.6740119402834,12.));
#181065=CARTESIAN_POINT('Ctrl Pts',(-21.5311675409807,-10.689651282929,
12.));
#181066=CARTESIAN_POINT('Ctrl Pts',(-21.5459946493955,-10.7054016114571,
12.));
#181067=CARTESIAN_POINT('Ctrl Pts',(-21.5608487586468,-10.7212626509816,
12.));
#181068=CARTESIAN_POINT('Ctrl Pts',(-21.5757290954371,-10.7372341280467,
12.));
#181069=CARTESIAN_POINT('Ctrl Pts',(-21.5906348951743,-10.7533157705941,
12.));
#181070=CARTESIAN_POINT('Ctrl Pts',(-21.6055654018176,-10.7695073079552,
12.));
#181071=CARTESIAN_POINT('Ctrl Pts',(-21.6205198677173,-10.7858084708261,
12.));
#181072=CARTESIAN_POINT('Ctrl Pts',(-21.6354975534557,-10.8022189912369,
12.));
#181073=CARTESIAN_POINT('Ctrl Pts',(-21.6504977276866,-10.8187386025136,
12.));
#181074=CARTESIAN_POINT('Ctrl Pts',(-21.6655196669732,-10.8353670392272,
12.));
#181075=CARTESIAN_POINT('Ctrl Pts',(-21.6805626556467,-10.8521040371835,
12.));
#181076=CARTESIAN_POINT('Ctrl Pts',(-21.6956259856672,-10.8689493334095,
12.));
#181077=CARTESIAN_POINT('Ctrl Pts',(-21.7107089564825,-10.8859026661293,
12.));
#181078=CARTESIAN_POINT('Ctrl Pts',(-21.7258108748873,-10.902963774734,
12.));
#181079=CARTESIAN_POINT('Ctrl Pts',(-21.7409310548797,-10.9201323997384,
12.));
#181080=CARTESIAN_POINT('Ctrl Pts',(-21.7560688175247,-10.9374082827444,
12.));
#181081=CARTESIAN_POINT('Ctrl Pts',(-21.7712234908464,-10.9547911664455,
12.));
#181082=CARTESIAN_POINT('Ctrl Pts',(-21.7863944097141,-10.9722807946155,
12.));
#181083=CARTESIAN_POINT('Ctrl Pts',(-21.8015809157301,-10.9898769120912,
12.));
#181084=CARTESIAN_POINT('Ctrl Pts',(-21.8167823571168,-11.0075792647477,
12.));
#181085=CARTESIAN_POINT('Ctrl Pts',(-21.8319980886033,-11.0253875994598,
12.));
#181086=CARTESIAN_POINT('Ctrl Pts',(-21.8472274713103,-11.0433016640807,
12.));
#181087=CARTESIAN_POINT('Ctrl Pts',(-21.8624698726318,-11.0613212074363,
12.));
#181088=CARTESIAN_POINT('Ctrl Pts',(-21.877724666119,-11.0794459793057,
12.));
#181089=CARTESIAN_POINT('Ctrl Pts',(-21.8929912313608,-11.0976757303944,
12.));
#181090=CARTESIAN_POINT('Ctrl Pts',(-21.9082689538688,-11.1160102123024,
12.));
#181091=CARTESIAN_POINT('Ctrl Pts',(-21.923557224952,-11.1344491774741,
12.));
#181092=CARTESIAN_POINT('Ctrl Pts',(-21.9388554416439,-11.1529923792003,
12.));
#181093=CARTESIAN_POINT('Ctrl Pts',(-21.9541630066506,-11.1716395716376,
12.));
#181094=CARTESIAN_POINT('Ctrl Pts',(-21.9694793282914,-11.190390509811,
12.));
#181095=CARTESIAN_POINT('Ctrl Pts',(-21.9848038204439,-11.2092449496125,
12.));
#181096=CARTESIAN_POINT('Ctrl Pts',(-22.0001359024839,-11.2282026477896,
12.));
#181097=CARTESIAN_POINT('Ctrl Pts',(-22.0154749992363,-11.2472633619275,
12.));
#181098=CARTESIAN_POINT('Ctrl Pts',(-22.030820540835,-11.2664268504206,
12.));
#181099=CARTESIAN_POINT('Ctrl Pts',(-22.046171962566,-11.2856928724374,
12.));
#181100=CARTESIAN_POINT('Ctrl Pts',(-22.0615287047179,-11.3050611878771,
12.));
#181101=CARTESIAN_POINT('Ctrl Pts',(-22.0768902124267,-11.3245315573168,
12.));
#181102=CARTESIAN_POINT('Ctrl Pts',(-22.0922559355294,-11.3441037419553,
12.));
#181103=CARTESIAN_POINT('Ctrl Pts',(-22.1076253283979,-11.3637775035367,
12.));
#181104=CARTESIAN_POINT('Ctrl Pts',(-22.1229978500186,-11.3835526044256,
12.));
#181105=CARTESIAN_POINT('Ctrl Pts',(-22.1383729640964,-11.4034288076908,
12.));
#181106=CARTESIAN_POINT('Ctrl Pts',(-22.1537501391487,-11.4234058771742,
12.));
#181107=CARTESIAN_POINT('Ctrl Pts',(-22.1691288486096,-11.443483577557,
12.));
#181108=CARTESIAN_POINT('Ctrl Pts',(-22.184508570917,-11.463661674411,12.));
#181109=CARTESIAN_POINT('Ctrl Pts',(-22.1998887896436,-11.483939934259,
12.));
#181110=CARTESIAN_POINT('Ctrl Pts',(-22.2152689931022,-11.5043181244242,
12.));
#181111=CARTESIAN_POINT('Ctrl Pts',(-22.2306486738901,-11.5247960128477,
12.));
#181112=CARTESIAN_POINT('Ctrl Pts',(-22.2460273284654,-11.5453733679121,
12.));
#181113=CARTESIAN_POINT('Ctrl Pts',(-22.2614044566898,-11.5660499582403,
12.));
#181114=CARTESIAN_POINT('Ctrl Pts',(-22.2767795614348,-11.5868255525188,
12.));
#181115=CARTESIAN_POINT('Ctrl Pts',(-22.2921521480356,-11.6076999192357,
12.));
#181116=CARTESIAN_POINT('Ctrl Pts',(-22.3075217249049,-11.6286728270009,
12.));
#181117=CARTESIAN_POINT('Ctrl Pts',(-22.3228878043976,-11.6497440449857,
12.));
#181118=CARTESIAN_POINT('Ctrl Pts',(-22.3382499035619,-11.6709133432985,
12.));
#181119=CARTESIAN_POINT('Ctrl Pts',(-22.3536075450029,-11.6921804934056,
12.));
#181120=CARTESIAN_POINT('Ctrl Pts',(-22.3689602575491,-11.7135452684532,
12.));
#181121=CARTESIAN_POINT('Ctrl Pts',(-22.3843075773899,-11.7350074437961,
12.));
#181122=CARTESIAN_POINT('Ctrl Pts',(-22.3996490469191,-11.7565667964764,
12.));
#181123=CARTESIAN_POINT('Ctrl Pts',(-22.4149842125008,-11.7782231042039,
12.));
#181124=CARTESIAN_POINT('Ctrl Pts',(-22.430312622646,-11.7999761445173,
12.));
#181125=CARTESIAN_POINT('Ctrl Pts',(-22.4456338258735,-11.8218256937889,
12.));
#181126=CARTESIAN_POINT('Ctrl Pts',(-22.4609473690471,-11.8437715264487,
12.));
#181127=CARTESIAN_POINT('Ctrl Pts',(-22.4762527946702,-11.8658134137019,
12.));
#181128=CARTESIAN_POINT('Ctrl Pts',(-22.4915496418485,-11.8879511239942,
12.));
#181129=CARTESIAN_POINT('Ctrl Pts',(-22.5068374513973,-11.9101844254557,
12.));
#181130=CARTESIAN_POINT('Ctrl Pts',(-22.5221157697883,-11.9325130877803,
12.));
#181131=CARTESIAN_POINT('Ctrl Pts',(-22.5373841537307,-11.9549368843997,
12.));
#181132=CARTESIAN_POINT('Ctrl Pts',(-22.5526421741158,-11.9774555943496,
12.));
#181133=CARTESIAN_POINT('Ctrl Pts',(-22.5678894211181,-12.0000690046695,
12.));
#181134=CARTESIAN_POINT('Ctrl Pts',(-22.5831255061282,-12.0227769113127,
12.));
#181135=CARTESIAN_POINT('Ctrl Pts',(-22.5983500505644,-12.0455791139128,
12.));
#181136=CARTESIAN_POINT('Ctrl Pts',(-22.6135626764898,-12.0684754113862,
12.));
#181137=CARTESIAN_POINT('Ctrl Pts',(-22.6287629967056,-12.0914655972823,
12.));
#181138=CARTESIAN_POINT('Ctrl Pts',(-22.6439506046605,-12.1145494550383,
12.));
#181139=CARTESIAN_POINT('Ctrl Pts',(-22.6591250653965,-12.1377267537145,
12.));
#181140=CARTESIAN_POINT('Ctrl Pts',(-22.6742859034944,-12.1609972423099,
12.));
#181141=CARTESIAN_POINT('Ctrl Pts',(-22.6894326205037,-12.1843606579261,
12.));
#181142=CARTESIAN_POINT('Ctrl Pts',(-22.7045647168747,-12.2078167360284,
12.));
#181143=CARTESIAN_POINT('Ctrl Pts',(-22.7196817119374,-12.2313652198061,
12.));
#181144=CARTESIAN_POINT('Ctrl Pts',(-22.7347831655287,-12.2550058702395,
12.));
#181145=CARTESIAN_POINT('Ctrl Pts',(-22.7498686970069,-12.2787384750742,
12.));
#181146=CARTESIAN_POINT('Ctrl Pts',(-22.764938010105,-12.3025628601792,
12.));
#181147=CARTESIAN_POINT('Ctrl Pts',(-22.7799908974768,-12.3264788926075,
12.));
#181148=CARTESIAN_POINT('Ctrl Pts',(-22.795027221673,-12.3504864740319,
12.));
#181149=CARTESIAN_POINT('Ctrl Pts',(-22.81004690224,-12.374585536673,12.));
#181150=CARTESIAN_POINT('Ctrl Pts',(-22.8220493007173,-12.3939379378998,
12.));
#181151=CARTESIAN_POINT('Ctrl Pts',(-22.8310435872748,-12.4084933766346,
12.));
#181152=CARTESIAN_POINT('Ctrl Pts',(-22.8370364396459,-12.418215285186,
12.));
#181153=CARTESIAN_POINT('Ctrl Pts',(-22.8400320311649,-12.4230808101438,
12.));
#181154=CARTESIAN_POINT('',(-22.1787195904339,-13.5685075571671,12.));
#181155=CARTESIAN_POINT('Origin',(0.,0.,12.));
#181156=CARTESIAN_POINT('',(-18.5896416359912,-12.7689476255363,12.));
#181157=CARTESIAN_POINT('Ctrl Pts',(-22.1787195904339,-13.5685075571671,
12.));
#181158=CARTESIAN_POINT('Ctrl Pts',(-22.1730081264608,-13.5683460612942,
12.));
#181159=CARTESIAN_POINT('Ctrl Pts',(-22.1615922805008,-13.5680170531805,
12.));
#181160=CARTESIAN_POINT('Ctrl Pts',(-22.1444897575194,-13.5675054919061,
12.));
#181161=CARTESIAN_POINT('Ctrl Pts',(-22.1217288871975,-13.5667873105359,
12.));
#181162=CARTESIAN_POINT('Ctrl Pts',(-22.0933486464593,-13.5658294169284,
12.));
#181163=CARTESIAN_POINT('Ctrl Pts',(-22.0650393089609,-13.5648113689033,
12.));
#181164=CARTESIAN_POINT('Ctrl Pts',(-22.0368009736295,-13.5637332022473,
12.));
#181165=CARTESIAN_POINT('Ctrl Pts',(-22.0086337943449,-13.5625949868333,
12.));
#181166=CARTESIAN_POINT('Ctrl Pts',(-21.9805379899168,-13.5613968357561,
12.));
#181167=CARTESIAN_POINT('Ctrl Pts',(-21.9525138592813,-13.5601389185257,
12.));
#181168=CARTESIAN_POINT('Ctrl Pts',(-21.9245617765769,-13.5588214586604,
12.));
#181169=CARTESIAN_POINT('Ctrl Pts',(-21.8966821688824,-13.5574447178424,
12.));
#181170=CARTESIAN_POINT('Ctrl Pts',(-21.8688754989365,-13.5560089839385,
12.));
#181171=CARTESIAN_POINT('Ctrl Pts',(-21.8411422456075,-13.5545145573031,
12.));
#181172=CARTESIAN_POINT('Ctrl Pts',(-21.8134828857967,-13.5529617381573,
12.));
#181173=CARTESIAN_POINT('Ctrl Pts',(-21.7858978745865,-13.551350812725,
12.));
#181174=CARTESIAN_POINT('Ctrl Pts',(-21.7583876294554,-13.5496820422211,
12.));
#181175=CARTESIAN_POINT('Ctrl Pts',(-21.7309525412281,-13.5479556704481,
12.));
#181176=CARTESIAN_POINT('Ctrl Pts',(-21.7035929822955,-13.5461719295048,
12.));
#181177=CARTESIAN_POINT('Ctrl Pts',(-21.6763093157699,-13.5443310461526,
12.));
#181178=CARTESIAN_POINT('Ctrl Pts',(-21.6491019044648,-13.5424332480699,
12.));
#181179=CARTESIAN_POINT('Ctrl Pts',(-21.6219711193946,-13.5404787697792,
12.));
#181180=CARTESIAN_POINT('Ctrl Pts',(-21.5949173499013,-13.5384678597195,
12.));
#181181=CARTESIAN_POINT('Ctrl Pts',(-21.5679410019001,-13.536400779028,
12.));
#181182=CARTESIAN_POINT('Ctrl Pts',(-21.5410424932503,-13.5342777983215,
12.));
#181183=CARTESIAN_POINT('Ctrl Pts',(-21.5142222501666,-13.5320991952138,
12.));
#181184=CARTESIAN_POINT('Ctrl Pts',(-21.4874807030468,-13.5298652514355,
12.));
#181185=CARTESIAN_POINT('Ctrl Pts',(-21.4608182828697,-13.5275762503555,
12.));
#181186=CARTESIAN_POINT('Ctrl Pts',(-21.4342354165259,-13.5252324737802,
12.));
#181187=CARTESIAN_POINT('Ctrl Pts',(-21.4077325259324,-13.5228342013516,
12.));
#181188=CARTESIAN_POINT('Ctrl Pts',(-21.3813100304973,-13.5203817122504,
12.));
#181189=CARTESIAN_POINT('Ctrl Pts',(-21.3549683486222,-13.5178752862466,
12.));
#181190=CARTESIAN_POINT('Ctrl Pts',(-21.3287078996341,-13.5153152050555,
12.));
#181191=CARTESIAN_POINT('Ctrl Pts',(-21.3025291054235,-13.5127017534971,
12.));
#181192=CARTESIAN_POINT('Ctrl Pts',(-21.2764323924442,-13.5100352209205,
12.));
#181193=CARTESIAN_POINT('Ctrl Pts',(-21.250418192743,-13.5073159019452,
12.));
#181194=CARTESIAN_POINT('Ctrl Pts',(-21.2244869429332,-13.5045440957404,
12.));
#181195=CARTESIAN_POINT('Ctrl Pts',(-21.1986390835828,-13.5017201056088,
12.));
#181196=CARTESIAN_POINT('Ctrl Pts',(-21.1728750584175,-13.4988442384491,
12.));
#181197=CARTESIAN_POINT('Ctrl Pts',(-21.1471953136209,-13.4959168042934,
12.));
#181198=CARTESIAN_POINT('Ctrl Pts',(-21.1216002970207,-13.4929381157778,
12.));
#181199=CARTESIAN_POINT('Ctrl Pts',(-21.0960904575046,-13.4899084877717,
12.));
#181200=CARTESIAN_POINT('Ctrl Pts',(-21.0706662455199,-13.4868282377191,
12.));
#181201=CARTESIAN_POINT('Ctrl Pts',(-21.0453281134245,-13.4836976858912,
12.));
#181202=CARTESIAN_POINT('Ctrl Pts',(-21.0200765158884,-13.4805171556822,
12.));
#181203=CARTESIAN_POINT('Ctrl Pts',(-20.9949119102592,-13.4772869738879,
12.));
#181204=CARTESIAN_POINT('Ctrl Pts',(-20.9698347569477,-13.4740074710086,
12.));
#181205=CARTESIAN_POINT('Ctrl Pts',(-20.9448455197557,-13.4706789815166,
12.));
#181206=CARTESIAN_POINT('Ctrl Pts',(-20.9199446657583,-13.4673018437717,
12.));
#181207=CARTESIAN_POINT('Ctrl Pts',(-20.8951326652158,-13.4638763999725,
12.));
#181208=CARTESIAN_POINT('Ctrl Pts',(-20.8704099914641,-13.4604029960983,
12.));
#181209=CARTESIAN_POINT('Ctrl Pts',(-20.8457771208083,-13.4568819818631,
12.));
#181210=CARTESIAN_POINT('Ctrl Pts',(-20.821234532398,-13.4533137106667,
12.));
#181211=CARTESIAN_POINT('Ctrl Pts',(-20.7967827081228,-13.4496985395637,
12.));
#181212=CARTESIAN_POINT('Ctrl Pts',(-20.7724221327609,-13.4460368293689,
12.));
#181213=CARTESIAN_POINT('Ctrl Pts',(-20.7481532941014,-13.4423289447561,
12.));
#181214=CARTESIAN_POINT('Ctrl Pts',(-20.7239766830675,-13.4385752543663,
12.));
#181215=CARTESIAN_POINT('Ctrl Pts',(-20.6998927938288,-13.4347761309154,
12.));
#181216=CARTESIAN_POINT('Ctrl Pts',(-20.6759021239102,-13.4309319513119,
12.));
#181217=CARTESIAN_POINT('Ctrl Pts',(-20.6520051742868,-13.427043096765,
12.));
#181218=CARTESIAN_POINT('Ctrl Pts',(-20.6282024494234,-13.4231099528178,
12.));
#181219=CARTESIAN_POINT('Ctrl Pts',(-20.6044944573151,-13.4191329093932,
12.));
#181220=CARTESIAN_POINT('Ctrl Pts',(-20.5808817095155,-13.4151123608411,
12.));
#181221=CARTESIAN_POINT('Ctrl Pts',(-20.557364721164,-13.4110487059912,
12.));
#181222=CARTESIAN_POINT('Ctrl Pts',(-20.5339440109958,-13.4069423482076,
12.));
#181223=CARTESIAN_POINT('Ctrl Pts',(-20.5106201013755,-13.4027936954529,
12.));
#181224=CARTESIAN_POINT('Ctrl Pts',(-20.4873935184041,-13.3986031603716,
12.));
#181225=CARTESIAN_POINT('Ctrl Pts',(-20.4642647920038,-13.3943711603739,
12.));
#181226=CARTESIAN_POINT('Ctrl Pts',(-20.4412344560007,-13.3900981177254,
12.));
#181227=CARTESIAN_POINT('Ctrl Pts',(-20.4183030482002,-13.3857844596387,
12.));
#181228=CARTESIAN_POINT('Ctrl Pts',(-20.3954711104505,-13.3814306183721,
12.));
#181229=CARTESIAN_POINT('Ctrl Pts',(-20.3727391887187,-13.377037031319,
12.));
#181230=CARTESIAN_POINT('Ctrl Pts',(-20.3501078331818,-13.3726041410869,
12.));
#181231=CARTESIAN_POINT('Ctrl Pts',(-20.3275775983032,-13.3681323955828,
12.));
#181232=CARTESIAN_POINT('Ctrl Pts',(-20.3051490429049,-13.3636222481017,
12.));
#181233=CARTESIAN_POINT('Ctrl Pts',(-20.2828227302337,-13.3590741574194,
12.));
#181234=CARTESIAN_POINT('Ctrl Pts',(-20.2605992280117,-13.3544885878886,
12.));
#181235=CARTESIAN_POINT('Ctrl Pts',(-20.2384791085354,-13.3498660095382,
12.));
#181236=CARTESIAN_POINT('Ctrl Pts',(-20.2164629487855,-13.3452068981763,
12.));
#181237=CARTESIAN_POINT('Ctrl Pts',(-20.1945513305233,-13.3405117354969,
12.));
#181238=CARTESIAN_POINT('Ctrl Pts',(-20.1727448403818,-13.3357810091903,
12.));
#181239=CARTESIAN_POINT('Ctrl Pts',(-20.1510440699477,-13.3310152130565,
12.));
#181240=CARTESIAN_POINT('Ctrl Pts',(-20.1294496158405,-13.3262148471228,
12.));
#181241=CARTESIAN_POINT('Ctrl Pts',(-20.1079620798377,-13.3213804177588,
12.));
#181242=CARTESIAN_POINT('Ctrl Pts',(-20.0865820689883,-13.3165124377963,
12.));
#181243=CARTESIAN_POINT('Ctrl Pts',(-20.0653101957188,-13.3116114266514,
12.));
#181244=CARTESIAN_POINT('Ctrl Pts',(-20.0441470779345,-13.3066779104515,
12.));
#181245=CARTESIAN_POINT('Ctrl Pts',(-20.023093339104,-13.3017124221639,
12.));
#181246=CARTESIAN_POINT('Ctrl Pts',(-20.0021496083742,-13.296715501731,
12.));
#181247=CARTESIAN_POINT('Ctrl Pts',(-19.9813165207174,-13.2916876962098,
12.));
#181248=CARTESIAN_POINT('Ctrl Pts',(-19.9605947170589,-13.2866295599152,
12.));
#181249=CARTESIAN_POINT('Ctrl Pts',(-19.9399848444019,-13.2815416545663,
12.));
#181250=CARTESIAN_POINT('Ctrl Pts',(-19.9194875559419,-13.2764245494354,
12.));
#181251=CARTESIAN_POINT('Ctrl Pts',(-19.8991035111739,-13.2712788215015,
12.));
#181252=CARTESIAN_POINT('Ctrl Pts',(-19.8788333760571,-13.2661050556128,
12.));
#181253=CARTESIAN_POINT('Ctrl Pts',(-19.8586778231711,-13.2609038446525,
12.));
#181254=CARTESIAN_POINT('Ctrl Pts',(-19.8386375318632,-13.2556757897085,
12.));
#181255=CARTESIAN_POINT('Ctrl Pts',(-19.8187131883919,-13.2504215002458,
12.));
#181256=CARTESIAN_POINT('Ctrl Pts',(-19.7989054860501,-13.2451415942809,
12.));
#181257=CARTESIAN_POINT('Ctrl Pts',(-19.7792151253297,-13.239836698568,
12.));
#181258=CARTESIAN_POINT('Ctrl Pts',(-19.7596428141176,-13.2345074487968,
12.));
#181259=CARTESIAN_POINT('Ctrl Pts',(-19.7401892678701,-13.2291544897902,
12.));
#181260=CARTESIAN_POINT('Ctrl Pts',(-19.7208552097867,-13.2237784757065,
12.));
#181261=CARTESIAN_POINT('Ctrl Pts',(-19.7016413709678,-13.2183800702431,
12.));
#181262=CARTESIAN_POINT('Ctrl Pts',(-19.6825484905812,-13.2129599468478,
12.));
#181263=CARTESIAN_POINT('Ctrl Pts',(-19.6635773160924,-13.2075187889522,
12.));
#181264=CARTESIAN_POINT('Ctrl Pts',(-19.6447286034764,-13.202057290206,
12.));
#181265=CARTESIAN_POINT('Ctrl Pts',(-19.6260031174244,-13.196576154715,
12.));
#181266=CARTESIAN_POINT('Ctrl Pts',(-19.6074016315421,-13.1910760972818,
12.));
#181267=CARTESIAN_POINT('Ctrl Pts',(-19.5889249285352,-13.1855578436479,
12.));
#181268=CARTESIAN_POINT('Ctrl Pts',(-19.5705738004682,-13.1800221307682,
12.));
#181269=CARTESIAN_POINT('Ctrl Pts',(-19.5523490490254,-13.1744697070918,
12.));
#181270=CARTESIAN_POINT('Ctrl Pts',(-19.5342514857564,-13.1689013328432,
12.));
#181271=CARTESIAN_POINT('Ctrl Pts',(-19.5162819323207,-13.1633177803097,
12.));
#181272=CARTESIAN_POINT('Ctrl Pts',(-19.498441220707,-13.1577198341238,
12.));
#181273=CARTESIAN_POINT('Ctrl Pts',(-19.4807301935256,-13.1521082915846,
12.));
#181274=CARTESIAN_POINT('Ctrl Pts',(-19.463149704325,-13.1464839629966,
12.));
#181275=CARTESIAN_POINT('Ctrl Pts',(-19.4457006178875,-13.140847672006,
12.));
#181276=CARTESIAN_POINT('Ctrl Pts',(-19.4283838105265,-13.1352002559439,
12.));
#181277=CARTESIAN_POINT('Ctrl Pts',(-19.4112001703561,-13.1295425661635,
12.));
#181278=CARTESIAN_POINT('Ctrl Pts',(-19.3941505976267,-13.1238754684177,
12.));
#181279=CARTESIAN_POINT('Ctrl Pts',(-19.3772360051093,-13.118199843271,
12.));
#181280=CARTESIAN_POINT('Ctrl Pts',(-19.3604573184516,-13.1125165865021,
12.));
#181281=CARTESIAN_POINT('Ctrl Pts',(-19.3438154765395,-13.1068266095186,
12.));
#181282=CARTESIAN_POINT('Ctrl Pts',(-19.3273114318268,-13.1011308397592,
12.));
#181283=CARTESIAN_POINT('Ctrl Pts',(-19.3109461507358,-13.095430221148,
12.));
#181284=CARTESIAN_POINT('Ctrl Pts',(-19.2947206141246,-13.0897257145969,
12.));
#181285=CARTESIAN_POINT('Ctrl Pts',(-19.2786358177198,-13.0840182984949,
12.));
#181286=CARTESIAN_POINT('Ctrl Pts',(-19.2626927725596,-13.0783089692118,
12.));
#181287=CARTESIAN_POINT('Ctrl Pts',(-19.2468925053988,-13.0725987415856,
12.));
#181288=CARTESIAN_POINT('Ctrl Pts',(-19.2312360592031,-13.0668886494791,
12.));
#181289=CARTESIAN_POINT('Ctrl Pts',(-19.2157244937141,-13.0611797463913,
12.));
#181290=CARTESIAN_POINT('Ctrl Pts',(-19.2003588859771,-13.0554731060537,
12.));
#181291=CARTESIAN_POINT('Ctrl Pts',(-19.1851403308825,-13.0497698230442,
12.));
#181292=CARTESIAN_POINT('Ctrl Pts',(-19.1700699416625,-13.0440710133775,
12.));
#181293=CARTESIAN_POINT('Ctrl Pts',(-19.1551488505233,-13.0383778152072,
12.));
#181294=CARTESIAN_POINT('Ctrl Pts',(-19.1403782093389,-13.0326913895841,
12.));
#181295=CARTESIAN_POINT('Ctrl Pts',(-19.1257591903099,-13.0270129211976,
12.));
#181296=CARTESIAN_POINT('Ctrl Pts',(-19.1112929866308,-13.0213436191326,
12.));
#181297=CARTESIAN_POINT('Ctrl Pts',(-19.0969808131226,-13.0156847176093,
12.));
#181298=CARTESIAN_POINT('Ctrl Pts',(-19.0828239070482,-13.0100374768785,
12.));
#181299=CARTESIAN_POINT('Ctrl Pts',(-19.0688235289437,-13.0044031841381,
12.));
#181300=CARTESIAN_POINT('Ctrl Pts',(-19.0549809634355,-12.9987831544502,
12.));
#181301=CARTESIAN_POINT('Ctrl Pts',(-19.0412975200398,-12.9931787316515,
12.));
#181302=CARTESIAN_POINT('Ctrl Pts',(-19.0277745339908,-12.9875912893003,
12.));
#181303=CARTESIAN_POINT('Ctrl Pts',(-19.0144133673348,-12.9820222318716,
12.));
#181304=CARTESIAN_POINT('Ctrl Pts',(-19.0012154099791,-12.9764729959205,
12.));
#181305=CARTESIAN_POINT('Ctrl Pts',(-18.9881820807586,-12.9709450512747,
12.));
#181306=CARTESIAN_POINT('Ctrl Pts',(-18.9753148284475,-12.9654399021869,
12.));
#181307=CARTESIAN_POINT('Ctrl Pts',(-18.9626151329229,-12.9599590886319,
12.));
#181308=CARTESIAN_POINT('Ctrl Pts',(-18.9500845064715,-12.9545041877377,
12.));
#181309=CARTESIAN_POINT('Ctrl Pts',(-18.9377244950435,-12.9490768151821,
12.));
#181310=CARTESIAN_POINT('Ctrl Pts',(-18.9255366795195,-12.9436786266105,
12.));
#181311=CARTESIAN_POINT('Ctrl Pts',(-18.9135226769465,-12.9383113190375,
12.));
#181312=CARTESIAN_POINT('Ctrl Pts',(-18.9016841423403,-12.9329766328185,
12.));
#181313=CARTESIAN_POINT('Ctrl Pts',(-18.8900227704889,-12.9276763536373,
12.));
#181314=CARTESIAN_POINT('Ctrl Pts',(-18.8785402977527,-12.9224123144982,
12.));
#181315=CARTESIAN_POINT('Ctrl Pts',(-18.8672385038326,-12.9171863977045,
12.));
#181316=CARTESIAN_POINT('Ctrl Pts',(-18.8561192136198,-12.9120005369063,
12.));
#181317=CARTESIAN_POINT('Ctrl Pts',(-18.8451842990984,-12.9068567191854,
12.));
#181318=CARTESIAN_POINT('Ctrl Pts',(-18.834435681259,-12.9017569871738,
12.));
#181319=CARTESIAN_POINT('Ctrl Pts',(-18.8238753319129,-12.8967034410755,
12.));
#181320=CARTESIAN_POINT('Ctrl Pts',(-18.813505275782,-12.8916982409935,
12.));
#181321=CARTESIAN_POINT('Ctrl Pts',(-18.8033275941943,-12.8867436109546,
12.));
#181322=CARTESIAN_POINT('Ctrl Pts',(-18.7933444285868,-12.8818418427475,
12.));
#181323=CARTESIAN_POINT('Ctrl Pts',(-18.7835579840477,-12.8769952998095,
12.));
#181324=CARTESIAN_POINT('Ctrl Pts',(-18.7739705329022,-12.872206421181,
12.));
#181325=CARTESIAN_POINT('Ctrl Pts',(-18.7645844169564,-12.8674777239653,
12.));
#181326=CARTESIAN_POINT('Ctrl Pts',(-18.7554020493887,-12.8628118054171,
12.));
#181327=CARTESIAN_POINT('Ctrl Pts',(-18.7464259171251,-12.8582113455646,
12.));
#181328=CARTESIAN_POINT('Ctrl Pts',(-18.7376585820854,-12.8536791086316,
12.));
#181329=CARTESIAN_POINT('Ctrl Pts',(-18.7291026886554,-12.8492179511591,
12.));
#181330=CARTESIAN_POINT('Ctrl Pts',(-18.7207609737702,-12.8448308329494,
12.));
#181331=CARTESIAN_POINT('Ctrl Pts',(-18.7126362754445,-12.8405208263431,
12.));
#181332=CARTESIAN_POINT('Ctrl Pts',(-18.7047315436294,-12.8362911280361,
12.));
#181333=CARTESIAN_POINT('Ctrl Pts',(-18.6970498410172,-12.8321450599789,
12.));
#181334=CARTESIAN_POINT('Ctrl Pts',(-18.6895943376171,-12.8280860635231,
12.));
#181335=CARTESIAN_POINT('Ctrl Pts',(-18.6823683094139,-12.8241176980017,
12.));
#181336=CARTESIAN_POINT('Ctrl Pts',(-18.6753751301092,-12.8202436318474,
12.));
#181337=CARTESIAN_POINT('Ctrl Pts',(-18.6686182952799,-12.8164676687362,
12.));
#181338=CARTESIAN_POINT('Ctrl Pts',(-18.6621014624746,-12.8127937909631,
12.));
#181339=CARTESIAN_POINT('Ctrl Pts',(-18.6558284825773,-12.8092261933858,
12.));
#181340=CARTESIAN_POINT('Ctrl Pts',(-18.6498034438987,-12.805769331162,
12.));
#181341=CARTESIAN_POINT('Ctrl Pts',(-18.6440306327456,-12.8024278770152,
12.));
#181342=CARTESIAN_POINT('Ctrl Pts',(-18.63851447924,-12.7992066625264,12.));
#181343=CARTESIAN_POINT('Ctrl Pts',(-18.6332595057006,-12.7961106222251,
12.));
#181344=CARTESIAN_POINT('Ctrl Pts',(-18.6282702819371,-12.7931447451555,
12.));
#181345=CARTESIAN_POINT('Ctrl Pts',(-18.6235516265575,-12.7903142925234,
12.));
#181346=CARTESIAN_POINT('Ctrl Pts',(-18.6191087624752,-12.7876249657834,
12.));
#181347=CARTESIAN_POINT('Ctrl Pts',(-18.6149475565188,-12.7850831657901,
12.));
#181348=CARTESIAN_POINT('Ctrl Pts',(-18.6110744826219,-12.7826959526925,
12.));
#181349=CARTESIAN_POINT('Ctrl Pts',(-18.6074961535723,-12.7804705387658,
12.));
#181350=CARTESIAN_POINT('Ctrl Pts',(-18.6042190183704,-12.7784139605066,
12.));
#181351=CARTESIAN_POINT('Ctrl Pts',(-18.6012488486709,-12.7765325225081,
12.));
#181352=CARTESIAN_POINT('Ctrl Pts',(-18.598591752595,-12.7748328937638,
12.));
#181353=CARTESIAN_POINT('Ctrl Pts',(-18.5962551167772,-12.7733231262108,
12.));
#181354=CARTESIAN_POINT('Ctrl Pts',(-18.5942490615407,-12.7720142287172,
12.));
#181355=CARTESIAN_POINT('Ctrl Pts',(-18.5925859134579,-12.7709195951156,
12.));
#181356=CARTESIAN_POINT('Ctrl Pts',(-18.5912775137806,-12.7700520897173,
12.));
#181357=CARTESIAN_POINT('Ctrl Pts',(-18.5903328777227,-12.7694215127919,
12.));
#181358=CARTESIAN_POINT('Ctrl Pts',(-18.589871621843,-12.769110348199,12.));
#181359=CARTESIAN_POINT('Ctrl Pts',(-18.5896919669165,-12.768986426692,
12.));
#181360=CARTESIAN_POINT('Ctrl Pts',(-18.5896460962964,-12.7689524524483,
12.));
#181361=CARTESIAN_POINT('Ctrl Pts',(-18.5896416359912,-12.7689476255363,
12.));
#181362=CARTESIAN_POINT('',(-18.1294424696716,-12.4528436808172,12.));
#181363=CARTESIAN_POINT('',(-8.86099361848466,-6.08648437878338,12.));
#181364=CARTESIAN_POINT('',(-17.4407513054162,-12.572596943457,12.));
#181365=CARTESIAN_POINT('Origin',(-17.846350172984,-12.8649829188862,12.));
#181366=CARTESIAN_POINT('',(-16.6581946899465,-13.5924445804218,12.));
#181367=CARTESIAN_POINT('Origin',(-6.37232247690086E-13,-4.50593605254675E-13,
12.));
#181368=CARTESIAN_POINT('',(-16.7207683102834,-14.2886635873976,12.));
#181369=CARTESIAN_POINT('Origin',(-17.0455945664569,-13.9085479427572,12.));
#181370=CARTESIAN_POINT('',(-17.1452095830633,-14.6513681262571,12.));
#181371=CARTESIAN_POINT('',(-8.57260479153162,-7.32568406312855,12.));
#181372=CARTESIAN_POINT('',(-18.8464468996588,-17.9112098770111,12.));
#181373=CARTESIAN_POINT('Ctrl Pts',(-17.1452095830633,-14.6513681262571,
12.));
#181374=CARTESIAN_POINT('Ctrl Pts',(-17.1452153999142,-14.651371185284,
12.));
#181375=CARTESIAN_POINT('Ctrl Pts',(-17.1452600887039,-14.6514066997188,
12.));
#181376=CARTESIAN_POINT('Ctrl Pts',(-17.1454262858045,-14.6515481598057,
12.));
#181377=CARTESIAN_POINT('Ctrl Pts',(-17.1458462295273,-14.65191316345,12.));
#181378=CARTESIAN_POINT('Ctrl Pts',(-17.1466998098673,-14.6526624064978,
12.));
#181379=CARTESIAN_POINT('Ctrl Pts',(-17.1478763944909,-14.6537016966188,
12.));
#181380=CARTESIAN_POINT('Ctrl Pts',(-17.1493641837556,-14.6550248622813,
12.));
#181381=CARTESIAN_POINT('Ctrl Pts',(-17.1511476869495,-14.6566237952435,
12.));
#181382=CARTESIAN_POINT('Ctrl Pts',(-17.1532107762719,-14.6584900555301,
12.));
#181383=CARTESIAN_POINT('Ctrl Pts',(-17.1555401986403,-14.660616716964,
12.));
#181384=CARTESIAN_POINT('Ctrl Pts',(-17.1581262646789,-14.662998728599,
12.));
#181385=CARTESIAN_POINT('Ctrl Pts',(-17.1609609517369,-14.6656319165057,
12.));
#181386=CARTESIAN_POINT('Ctrl Pts',(-17.1640366762304,-14.6685123374424,
12.));
#181387=CARTESIAN_POINT('Ctrl Pts',(-17.1673449723019,-14.6716355833321,
12.));
#181388=CARTESIAN_POINT('Ctrl Pts',(-17.1708771619129,-14.6749971333867,
12.));
#181389=CARTESIAN_POINT('Ctrl Pts',(-17.1746247499057,-14.6785925615676,
12.));
#181390=CARTESIAN_POINT('Ctrl Pts',(-17.1785800350827,-14.6824178576167,
12.));
#181391=CARTESIAN_POINT('Ctrl Pts',(-17.182736158472,-14.6864694522319,
12.));
#181392=CARTESIAN_POINT('Ctrl Pts',(-17.1870867909918,-14.6907440526958,
12.));
#181393=CARTESIAN_POINT('Ctrl Pts',(-17.1916259308416,-14.6952385361706,
12.));
#181394=CARTESIAN_POINT('Ctrl Pts',(-17.1963476411694,-14.699949811582,
12.));
#181395=CARTESIAN_POINT('Ctrl Pts',(-17.2012461084268,-14.7048748502663,
12.));
#181396=CARTESIAN_POINT('Ctrl Pts',(-17.2063157097316,-14.7100107213586,
12.));
#181397=CARTESIAN_POINT('Ctrl Pts',(-17.2115510835988,-14.7153546289338,
12.));
#181398=CARTESIAN_POINT('Ctrl Pts',(-17.2169471814255,-14.7209039390326,
12.));
#181399=CARTESIAN_POINT('Ctrl Pts',(-17.2224992099666,-14.7266561494282,
12.));
#181400=CARTESIAN_POINT('Ctrl Pts',(-17.2282025904314,-14.7326088681163,
12.));
#181401=CARTESIAN_POINT('Ctrl Pts',(-17.2340529062077,-14.7387597858117,
12.));
#181402=CARTESIAN_POINT('Ctrl Pts',(-17.2400458713566,-14.7451066593793,
12.));
#181403=CARTESIAN_POINT('Ctrl Pts',(-17.2461773413289,-14.7516473175125,
12.));
#181404=CARTESIAN_POINT('Ctrl Pts',(-17.2524433146837,-14.7583796616617,
12.));
#181405=CARTESIAN_POINT('Ctrl Pts',(-17.2588399401464,-14.7653016697589,
12.));
#181406=CARTESIAN_POINT('Ctrl Pts',(-17.2653635155317,-14.7724113956728,
12.));
#181407=CARTESIAN_POINT('Ctrl Pts',(-17.2720104735192,-14.7797069617802,
12.));
#181408=CARTESIAN_POINT('Ctrl Pts',(-17.278777370485,-14.787186553128,12.));
#181409=CARTESIAN_POINT('Ctrl Pts',(-17.28566087332,-14.7948484105253,12.));
#181410=CARTESIAN_POINT('Ctrl Pts',(-17.2926577496519,-14.8026908254281,
12.));
#181411=CARTESIAN_POINT('Ctrl Pts',(-17.2997648661483,-14.8107121391038,
12.));
#181412=CARTESIAN_POINT('Ctrl Pts',(-17.3069791853705,-14.8189107410161,
12.));
#181413=CARTESIAN_POINT('Ctrl Pts',(-17.3142977632656,-14.8272850675375,
12.));
#181414=CARTESIAN_POINT('Ctrl Pts',(-17.3217177462096,-14.8358336004193,
12.));
#181415=CARTESIAN_POINT('Ctrl Pts',(-17.3292363662601,-14.8445548643505,
12.));
#181416=CARTESIAN_POINT('Ctrl Pts',(-17.336850936485,-14.8534474245433,
12.));
#181417=CARTESIAN_POINT('Ctrl Pts',(-17.3445588463477,-14.8625098843419,
12.));
#181418=CARTESIAN_POINT('Ctrl Pts',(-17.3523575568648,-14.8717408826958,
12.));
#181419=CARTESIAN_POINT('Ctrl Pts',(-17.3602445978163,-14.8811390927424,
12.));
#181420=CARTESIAN_POINT('Ctrl Pts',(-17.3682175653236,-14.8907032205789,
12.));
#181421=CARTESIAN_POINT('Ctrl Pts',(-17.3762741193075,-14.9004320039609,
12.));
#181422=CARTESIAN_POINT('Ctrl Pts',(-17.3844119809823,-14.9103242110057,
12.));
#181423=CARTESIAN_POINT('Ctrl Pts',(-17.3926289303987,-14.9203786389343,
12.));
#181424=CARTESIAN_POINT('Ctrl Pts',(-17.400922804075,-14.9305941128758,
12.));
#181425=CARTESIAN_POINT('Ctrl Pts',(-17.4092914926071,-14.940969484645,
12.));
#181426=CARTESIAN_POINT('Ctrl Pts',(-17.4177329382827,-14.9515036315142,
12.));
#181427=CARTESIAN_POINT('Ctrl Pts',(-17.4262451327088,-14.9621954549825,
12.));
#181428=CARTESIAN_POINT('Ctrl Pts',(-17.4348261151395,-14.973043879945,
12.));
#181429=CARTESIAN_POINT('Ctrl Pts',(-17.4434739707773,-14.9840478538357,
12.));
#181430=CARTESIAN_POINT('Ctrl Pts',(-17.4521868291005,-14.9952063457779,
12.));
#181431=CARTESIAN_POINT('Ctrl Pts',(-17.4609628621419,-15.0065183456922,
12.));
#181432=CARTESIAN_POINT('Ctrl Pts',(-17.4698002829357,-15.0179828635087,
12.));
#181433=CARTESIAN_POINT('Ctrl Pts',(-17.4786973441417,-15.029598928488,
12.));
#181434=CARTESIAN_POINT('Ctrl Pts',(-17.4876523366178,-15.0413655884993,
12.));
#181435=CARTESIAN_POINT('Ctrl Pts',(-17.4966635880246,-15.0532819093085,
12.));
#181436=CARTESIAN_POINT('Ctrl Pts',(-17.5057294613877,-15.0653469738307,
12.));
#181437=CARTESIAN_POINT('Ctrl Pts',(-17.5148483539687,-15.0775598815749,
12.));
#181438=CARTESIAN_POINT('Ctrl Pts',(-17.5240186961791,-15.0899197481082,
12.));
#181439=CARTESIAN_POINT('Ctrl Pts',(-17.5332389504829,-15.1024257045033,
12.));
#181440=CARTESIAN_POINT('Ctrl Pts',(-17.5425076102963,-15.1150768967728,
12.));
#181441=CARTESIAN_POINT('Ctrl Pts',(-17.5518231989117,-15.1278724853138,
12.));
#181442=CARTESIAN_POINT('Ctrl Pts',(-17.5611842686192,-15.1408116444876,
12.));
#181443=CARTESIAN_POINT('Ctrl Pts',(-17.5705893998029,-15.1538935621714,
12.));
#181444=CARTESIAN_POINT('Ctrl Pts',(-17.580037200054,-15.1671174393137,
12.));
#181445=CARTESIAN_POINT('Ctrl Pts',(-17.5895263032595,-15.1804824894605,
12.));
#181446=CARTESIAN_POINT('Ctrl Pts',(-17.5990553687599,-15.1939879383268,
12.));
#181447=CARTESIAN_POINT('Ctrl Pts',(-17.60862308065,-15.2076330234686,12.));
#181448=CARTESIAN_POINT('Ctrl Pts',(-17.6182281470468,-15.2214169939199,
12.));
#181449=CARTESIAN_POINT('Ctrl Pts',(-17.6278692993764,-15.2353391098366,
12.));
#181450=CARTESIAN_POINT('Ctrl Pts',(-17.6375452916369,-15.2493986421092,
12.));
#181451=CARTESIAN_POINT('Ctrl Pts',(-17.6472548997328,-15.2635948720292,
12.));
#181452=CARTESIAN_POINT('Ctrl Pts',(-17.6569969209,-15.2779270910239,12.));
#181453=CARTESIAN_POINT('Ctrl Pts',(-17.6667701731041,-15.2923946003598,
12.));
#181454=CARTESIAN_POINT('Ctrl Pts',(-17.676573494456,-15.3069967108501,
12.));
#181455=CARTESIAN_POINT('Ctrl Pts',(-17.6864057426052,-15.3217327425338,
12.));
#181456=CARTESIAN_POINT('Ctrl Pts',(-17.6962657941983,-15.3366020244066,
12.));
#181457=CARTESIAN_POINT('Ctrl Pts',(-17.7061525444042,-15.351603894206,
12.));
#181458=CARTESIAN_POINT('Ctrl Pts',(-17.7160649064206,-15.3667376981699,
12.));
#181459=CARTESIAN_POINT('Ctrl Pts',(-17.7260018109924,-15.3820027907967,
12.));
#181460=CARTESIAN_POINT('Ctrl Pts',(-17.735962205915,-15.3973985345802,
12.));
#181461=CARTESIAN_POINT('Ctrl Pts',(-17.7459450555812,-15.4129242997837,
12.));
#181462=CARTESIAN_POINT('Ctrl Pts',(-17.7559493405881,-15.4285794642668,
12.));
#181463=CARTESIAN_POINT('Ctrl Pts',(-17.7659740573265,-15.4443634132869,
12.));
#181464=CARTESIAN_POINT('Ctrl Pts',(-17.7760182175815,-15.4602755393017,
12.));
#181465=CARTESIAN_POINT('Ctrl Pts',(-17.786080848122,-15.4763152417497,
12.));
#181466=CARTESIAN_POINT('Ctrl Pts',(-17.7961609903148,-15.4924819268517,
12.));
#181467=CARTESIAN_POINT('Ctrl Pts',(-17.8062576997952,-15.5087750074718,
12.));
#181468=CARTESIAN_POINT('Ctrl Pts',(-17.8163700461256,-15.5251939029552,
12.));
#181469=CARTESIAN_POINT('Ctrl Pts',(-17.8264971124607,-15.541738038964,
12.));
#181470=CARTESIAN_POINT('Ctrl Pts',(-17.8366379952085,-15.5584068472982,
12.));
#181471=CARTESIAN_POINT('Ctrl Pts',(-17.8467918036987,-15.5751997657163,
12.));
#181472=CARTESIAN_POINT('Ctrl Pts',(-17.8569576599006,-15.5921162378192,
12.));
#181473=CARTESIAN_POINT('Ctrl Pts',(-17.8671346981394,-15.609155712921,
12.));
#181474=CARTESIAN_POINT('Ctrl Pts',(-17.8773220648125,-15.6263176459108,
12.));
#181475=CARTESIAN_POINT('Ctrl Pts',(-17.8875189181091,-15.6436014971084,
12.));
#181476=CARTESIAN_POINT('Ctrl Pts',(-17.897724427724,-15.661006732103,12.));
#181477=CARTESIAN_POINT('Ctrl Pts',(-17.9079377746111,-15.678532821646,
12.));
#181478=CARTESIAN_POINT('Ctrl Pts',(-17.9181581507455,-15.6961792415522,
12.));
#181479=CARTESIAN_POINT('Ctrl Pts',(-17.9283847588836,-15.7139454725838,
12.));
#181480=CARTESIAN_POINT('Ctrl Pts',(-17.9386168123262,-15.7318310003335,
12.));
#181481=CARTESIAN_POINT('Ctrl Pts',(-17.9488535346781,-15.749835315086,
12.));
#181482=CARTESIAN_POINT('Ctrl Pts',(-17.9590941596242,-15.7679579117077,
12.));
#181483=CARTESIAN_POINT('Ctrl Pts',(-17.9693379307303,-15.7861982895724,
12.));
#181484=CARTESIAN_POINT('Ctrl Pts',(-17.9795841012386,-15.8045559524676,
12.));
#181485=CARTESIAN_POINT('Ctrl Pts',(-17.9898319338664,-15.8230304084962,
12.));
#181486=CARTESIAN_POINT('Ctrl Pts',(-18.0000807006052,-15.8416211699679,
12.));
#181487=CARTESIAN_POINT('Ctrl Pts',(-18.0103296825205,-15.8603277532831,
12.));
#181488=CARTESIAN_POINT('Ctrl Pts',(-18.0205781695769,-15.8791496788682,
12.));
#181489=CARTESIAN_POINT('Ctrl Pts',(-18.0308254604636,-15.8980864711042,
12.));
#181490=CARTESIAN_POINT('Ctrl Pts',(-18.0410708624208,-15.9171376582436,
12.));
#181491=CARTESIAN_POINT('Ctrl Pts',(-18.0513136910691,-15.9363027723244,
12.));
#181492=CARTESIAN_POINT('Ctrl Pts',(-18.061553270236,-15.9555813490644,
12.));
#181493=CARTESIAN_POINT('Ctrl Pts',(-18.0717889317958,-15.9749729277846,
12.));
#181494=CARTESIAN_POINT('Ctrl Pts',(-18.0820200155236,-15.9944770513613,
12.));
#181495=CARTESIAN_POINT('Ctrl Pts',(-18.0922458689462,-16.014093266161,
12.));
#181496=CARTESIAN_POINT('Ctrl Pts',(-18.1024658471966,-16.0338211219693,
12.));
#181497=CARTESIAN_POINT('Ctrl Pts',(-18.112679312869,-16.0536601719126,
12.));
#181498=CARTESIAN_POINT('Ctrl Pts',(-18.1228856358751,-16.0736099723668,
12.));
#181499=CARTESIAN_POINT('Ctrl Pts',(-18.1330841933105,-16.0936700829112,
12.));
#181500=CARTESIAN_POINT('Ctrl Pts',(-18.1432743693235,-16.1138400662794,
12.));
#181501=CARTESIAN_POINT('Ctrl Pts',(-18.1534555549852,-16.1341194882988,
12.));
#181502=CARTESIAN_POINT('Ctrl Pts',(-18.1636271481615,-16.154507917826,
12.));
#181503=CARTESIAN_POINT('Ctrl Pts',(-18.1737885533849,-16.1750049266671,
12.));
#181504=CARTESIAN_POINT('Ctrl Pts',(-18.1839391817331,-16.1956100895073,
12.));
#181505=CARTESIAN_POINT('Ctrl Pts',(-18.1940784507229,-16.2163229838875,
12.));
#181506=CARTESIAN_POINT('Ctrl Pts',(-18.2042057842035,-16.2371431901638,
12.));
#181507=CARTESIAN_POINT('Ctrl Pts',(-18.2143206122529,-16.2580702914615,
12.));
#181508=CARTESIAN_POINT('Ctrl Pts',(-18.2244223710746,-16.2791038736223,
12.));
#181509=CARTESIAN_POINT('Ctrl Pts',(-18.2345105028982,-16.3002435251378,
12.));
#181510=CARTESIAN_POINT('Ctrl Pts',(-18.2445844558742,-16.3214888370987,
12.));
#181511=CARTESIAN_POINT('Ctrl Pts',(-18.2546436839608,-16.3428394031589,
12.));
#181512=CARTESIAN_POINT('Ctrl Pts',(-18.2646876468169,-16.3642948194868,
12.));
#181513=CARTESIAN_POINT('Ctrl Pts',(-18.2747158096934,-16.385854684708,
12.));
#181514=CARTESIAN_POINT('Ctrl Pts',(-18.2847276433309,-16.4075185998455,
12.));
#181515=CARTESIAN_POINT('Ctrl Pts',(-18.294722623851,-16.4292861682379,
12.));
#181516=CARTESIAN_POINT('Ctrl Pts',(-18.304700232686,-16.4511569955233,
12.));
#181517=CARTESIAN_POINT('Ctrl Pts',(-18.3146599565231,-16.4731306896441,
12.));
#181518=CARTESIAN_POINT('Ctrl Pts',(-18.3246012872469,-16.4952068608345,
12.));
#181519=CARTESIAN_POINT('Ctrl Pts',(-18.3345237218864,-16.5173851216045,
12.));
#181520=CARTESIAN_POINT('Ctrl Pts',(-18.34442676256,-16.5396650867139,12.));
#181521=CARTESIAN_POINT('Ctrl Pts',(-18.354309916433,-16.5620463731413,
12.));
#181522=CARTESIAN_POINT('Ctrl Pts',(-18.3641726955889,-16.5845286000217,
12.));
#181523=CARTESIAN_POINT('Ctrl Pts',(-18.3740146168879,-16.607111388571,
12.));
#181524=CARTESIAN_POINT('Ctrl Pts',(-18.3838352018327,-16.6297943620056,
12.));
#181525=CARTESIAN_POINT('Ctrl Pts',(-18.3936339764332,-16.6525771454513,
12.));
#181526=CARTESIAN_POINT('Ctrl Pts',(-18.403410471079,-16.6754593658513,
12.));
#181527=CARTESIAN_POINT('Ctrl Pts',(-18.413164220399,-16.6984406518491,
12.));
#181528=CARTESIAN_POINT('Ctrl Pts',(-18.4228947633187,-16.7215206338818,
12.));
#181529=CARTESIAN_POINT('Ctrl Pts',(-18.4326016431392,-16.7446989442882,
12.));
#181530=CARTESIAN_POINT('Ctrl Pts',(-18.44228440761,-16.7679752173992,12.));
#181531=CARTESIAN_POINT('Ctrl Pts',(-18.4519426090124,-16.791349089629,
12.));
#181532=CARTESIAN_POINT('Ctrl Pts',(-18.4615758042305,-16.8148201995472,
12.));
#181533=CARTESIAN_POINT('Ctrl Pts',(-18.4711835548623,-16.8383881879709,
12.));
#181534=CARTESIAN_POINT('Ctrl Pts',(-18.4807654268771,-16.8620526977171,
12.));
#181535=CARTESIAN_POINT('Ctrl Pts',(-18.4903209902227,-16.8858133733088,
12.));
#181536=CARTESIAN_POINT('Ctrl Pts',(-18.499849818462,-16.9096698606943,
12.));
#181537=CARTESIAN_POINT('Ctrl Pts',(-18.5093514883835,-16.9336218069353,
12.));
#181538=CARTESIAN_POINT('Ctrl Pts',(-18.5188255796659,-16.9576688599339,
12.));
#181539=CARTESIAN_POINT('Ctrl Pts',(-18.5282716744197,-16.981810668038,
12.));
#181540=CARTESIAN_POINT('Ctrl Pts',(-18.5376893576961,-17.0060468805097,
12.));
#181541=CARTESIAN_POINT('Ctrl Pts',(-18.547078218209,-17.0303771481738,
12.));
#181542=CARTESIAN_POINT('Ctrl Pts',(-18.556437848963,-17.0548011239751,
12.));
#181543=CARTESIAN_POINT('Ctrl Pts',(-18.5657678479789,-17.0793184636079,
12.));
#181544=CARTESIAN_POINT('Ctrl Pts',(-18.5750678188542,-17.1039288260001,
12.));
#181545=CARTESIAN_POINT('Ctrl Pts',(-18.5843373717247,-17.1286318741183,
12.));
#181546=CARTESIAN_POINT('Ctrl Pts',(-18.5935761222825,-17.1534272741643,
12.));
#181547=CARTESIAN_POINT('Ctrl Pts',(-18.6027836898817,-17.1783146940127,
12.));
#181548=CARTESIAN_POINT('Ctrl Pts',(-18.6119596959949,-17.2032938019284,
12.));
#181549=CARTESIAN_POINT('Ctrl Pts',(-18.6211037624038,-17.2283642650518,
12.));
#181550=CARTESIAN_POINT('Ctrl Pts',(-18.6302155097943,-17.2535257482187,
12.));
#181551=CARTESIAN_POINT('Ctrl Pts',(-18.6392945554748,-17.2787779120213,
12.));
#181552=CARTESIAN_POINT('Ctrl Pts',(-18.6483405141865,-17.3041204135074,
12.));
#181553=CARTESIAN_POINT('Ctrl Pts',(-18.6573530024033,-17.3295529098618,
12.));
#181554=CARTESIAN_POINT('Ctrl Pts',(-18.6663316416582,-17.3550750612443,
12.));
#181555=CARTESIAN_POINT('Ctrl Pts',(-18.6752760624052,-17.3806865340747,
12.));
#181556=CARTESIAN_POINT('Ctrl Pts',(-18.6841859073471,-17.4063870038562,
12.));
#181557=CARTESIAN_POINT('Ctrl Pts',(-18.6930608357409,-17.4321761588142,
12.));
#181558=CARTESIAN_POINT('Ctrl Pts',(-18.70190052503,-17.4580537012753,12.));
#181559=CARTESIAN_POINT('Ctrl Pts',(-18.7107046613912,-17.4840193397162,
12.));
#181560=CARTESIAN_POINT('Ctrl Pts',(-18.7194729318098,-17.5100727820876,
12.));
#181561=CARTESIAN_POINT('Ctrl Pts',(-18.7282050157138,-17.5362137287593,
12.));
#181562=CARTESIAN_POINT('Ctrl Pts',(-18.7369005764553,-17.5624418653245,
12.));
#181563=CARTESIAN_POINT('Ctrl Pts',(-18.7455592536687,-17.5887568561371,
12.));
#181564=CARTESIAN_POINT('Ctrl Pts',(-18.7541806530984,-17.6151583357012,
12.));
#181565=CARTESIAN_POINT('Ctrl Pts',(-18.762764361321,-17.6416459210681,
12.));
#181566=CARTESIAN_POINT('Ctrl Pts',(-18.7713099642754,-17.6682192274236,
12.));
#181567=CARTESIAN_POINT('Ctrl Pts',(-18.7798170641374,-17.6948778823014,
12.));
#181568=CARTESIAN_POINT('Ctrl Pts',(-18.788285297605,-17.7216215409035,
12.));
#181569=CARTESIAN_POINT('Ctrl Pts',(-18.7967143519419,-17.7484498996905,
12.));
#181570=CARTESIAN_POINT('Ctrl Pts',(-18.8051039860448,-17.7753627137853,
12.));
#181571=CARTESIAN_POINT('Ctrl Pts',(-18.8134540340417,-17.8023598011057,
12.));
#181572=CARTESIAN_POINT('Ctrl Pts',(-18.8217643886157,-17.8294410311006,
12.));
#181573=CARTESIAN_POINT('Ctrl Pts',(-18.8300349895974,-17.8566063174771,
12.));
#181574=CARTESIAN_POINT('Ctrl Pts',(-18.8366196462581,-17.8784057509356,
12.));
#181575=CARTESIAN_POINT('Ctrl Pts',(-18.8415402351786,-17.8947931177807,
12.));
#181576=CARTESIAN_POINT('Ctrl Pts',(-18.8448126709692,-17.9057348246595,
12.));
#181577=CARTESIAN_POINT('Ctrl Pts',(-18.8464468996588,-17.9112098770111,
12.));
#181578=CARTESIAN_POINT('',(-17.9112098770111,-18.8464468996588,12.));
#181579=CARTESIAN_POINT('Origin',(0.,0.,12.));
#181580=CARTESIAN_POINT('',(-14.6513681262571,-17.1452095830632,12.));
#181581=CARTESIAN_POINT('Ctrl Pts',(-17.9112098770111,-18.8464468996588,
12.));
#181582=CARTESIAN_POINT('Ctrl Pts',(-17.9057348246611,-18.8448126709726,
12.));
#181583=CARTESIAN_POINT('Ctrl Pts',(-17.8947931177853,-18.8415402351882,
12.));
#181584=CARTESIAN_POINT('Ctrl Pts',(-17.8784057509434,-18.8366196462746,
12.));
#181585=CARTESIAN_POINT('Ctrl Pts',(-17.8566063174871,-18.8300349896187,
12.));
#181586=CARTESIAN_POINT('Ctrl Pts',(-17.8294410311105,-18.8217643886368,
12.));
#181587=CARTESIAN_POINT('Ctrl Pts',(-17.8023598011135,-18.8134540340581,
12.));
#181588=CARTESIAN_POINT('Ctrl Pts',(-17.7753627137898,-18.8051039860543,
12.));
#181589=CARTESIAN_POINT('Ctrl Pts',(-17.7484498996917,-18.7967143519444,
12.));
#181590=CARTESIAN_POINT('Ctrl Pts',(-17.7216215409019,-18.7882852976016,
12.));
#181591=CARTESIAN_POINT('Ctrl Pts',(-17.6948778822982,-18.7798170641305,
12.));
#181592=CARTESIAN_POINT('Ctrl Pts',(-17.6682192274197,-18.7713099642673,
12.));
#181593=CARTESIAN_POINT('Ctrl Pts',(-17.6416459210646,-18.7627643613138,
12.));
#181594=CARTESIAN_POINT('Ctrl Pts',(-17.6151583356989,-18.7541806530935,
12.));
#181595=CARTESIAN_POINT('Ctrl Pts',(-17.5887568561361,-18.7455592536667,
12.));
#181596=CARTESIAN_POINT('Ctrl Pts',(-17.5624418653248,-18.7369005764558,
12.));
#181597=CARTESIAN_POINT('Ctrl Pts',(-17.5362137287604,-18.728205015716,
12.));
#181598=CARTESIAN_POINT('Ctrl Pts',(-17.5100727820891,-18.7194729318127,
12.));
#181599=CARTESIAN_POINT('Ctrl Pts',(-17.4840193397176,-18.7107046613941,
12.));
#181600=CARTESIAN_POINT('Ctrl Pts',(-17.4580537012764,-18.7019005250322,
12.));
#181601=CARTESIAN_POINT('Ctrl Pts',(-17.4321761588148,-18.6930608357421,
12.));
#181602=CARTESIAN_POINT('Ctrl Pts',(-17.4063870038563,-18.6841859073472,
12.));
#181603=CARTESIAN_POINT('Ctrl Pts',(-17.3806865340744,-18.6752760624045,
12.));
#181604=CARTESIAN_POINT('Ctrl Pts',(-17.3550750612438,-18.6663316416569,
12.));
#181605=CARTESIAN_POINT('Ctrl Pts',(-17.3295529098612,-18.6573530024019,
12.));
#181606=CARTESIAN_POINT('Ctrl Pts',(-17.3041204135069,-18.6483405141853,
12.));
#181607=CARTESIAN_POINT('Ctrl Pts',(-17.278777912021,-18.639294555474,12.));
#181608=CARTESIAN_POINT('Ctrl Pts',(-17.2535257482186,-18.630215509794,
12.));
#181609=CARTESIAN_POINT('Ctrl Pts',(-17.2283642650519,-18.6211037624041,
12.));
#181610=CARTESIAN_POINT('Ctrl Pts',(-17.2032938019288,-18.6119596959957,
12.));
#181611=CARTESIAN_POINT('Ctrl Pts',(-17.1783146940131,-18.6027836898826,
12.));
#181612=CARTESIAN_POINT('Ctrl Pts',(-17.1534272741646,-18.5935761222833,
12.));
#181613=CARTESIAN_POINT('Ctrl Pts',(-17.1286318741185,-18.5843373717253,
12.));
#181614=CARTESIAN_POINT('Ctrl Pts',(-17.1039288260002,-18.5750678188543,
12.));
#181615=CARTESIAN_POINT('Ctrl Pts',(-17.0793184636079,-18.5657678479788,
12.));
#181616=CARTESIAN_POINT('Ctrl Pts',(-17.0548011239751,-18.5564378489628,
12.));
#181617=CARTESIAN_POINT('Ctrl Pts',(-17.030377148174,-18.5470782182089,
12.));
#181618=CARTESIAN_POINT('Ctrl Pts',(-17.0060468805099,-18.5376893576961,
12.));
#181619=CARTESIAN_POINT('Ctrl Pts',(-16.9818106680382,-18.5282716744198,
12.));
#181620=CARTESIAN_POINT('Ctrl Pts',(-16.957668859934,-18.518825579666,12.));
#181621=CARTESIAN_POINT('Ctrl Pts',(-16.9336218069353,-18.5093514883835,
12.));
#181622=CARTESIAN_POINT('Ctrl Pts',(-16.9096698606942,-18.4998498184619,
12.));
#181623=CARTESIAN_POINT('Ctrl Pts',(-16.8858133733086,-18.4903209902226,
12.));
#181624=CARTESIAN_POINT('Ctrl Pts',(-16.8620526977169,-18.4807654268769,
12.));
#181625=CARTESIAN_POINT('Ctrl Pts',(-16.8383881879707,-18.4711835548622,
12.));
#181626=CARTESIAN_POINT('Ctrl Pts',(-16.8148201995472,-18.4615758042305,
12.));
#181627=CARTESIAN_POINT('Ctrl Pts',(-16.791349089629,-18.4519426090124,
12.));
#181628=CARTESIAN_POINT('Ctrl Pts',(-16.7679752173992,-18.4422844076099,
12.));
#181629=CARTESIAN_POINT('Ctrl Pts',(-16.7446989442882,-18.4326016431392,
12.));
#181630=CARTESIAN_POINT('Ctrl Pts',(-16.7215206338818,-18.4228947633186,
12.));
#181631=CARTESIAN_POINT('Ctrl Pts',(-16.698440651849,-18.4131642203989,
12.));
#181632=CARTESIAN_POINT('Ctrl Pts',(-16.6754593658513,-18.4034104710789,
12.));
#181633=CARTESIAN_POINT('Ctrl Pts',(-16.6525771454513,-18.3936339764332,
12.));
#181634=CARTESIAN_POINT('Ctrl Pts',(-16.6297943620056,-18.3838352018327,
12.));
#181635=CARTESIAN_POINT('Ctrl Pts',(-16.6071113885711,-18.3740146168879,
12.));
#181636=CARTESIAN_POINT('Ctrl Pts',(-16.5845286000219,-18.364172695589,
12.));
#181637=CARTESIAN_POINT('Ctrl Pts',(-16.5620463731414,-18.3543099164331,
12.));
#181638=CARTESIAN_POINT('Ctrl Pts',(-16.539665086714,-18.3444267625601,
12.));
#181639=CARTESIAN_POINT('Ctrl Pts',(-16.5173851216045,-18.3345237218864,
12.));
#181640=CARTESIAN_POINT('Ctrl Pts',(-16.4952068608344,-18.3246012872468,
12.));
#181641=CARTESIAN_POINT('Ctrl Pts',(-16.4731306896439,-18.3146599565229,
12.));
#181642=CARTESIAN_POINT('Ctrl Pts',(-16.4511569955231,-18.3047002326858,
12.));
#181643=CARTESIAN_POINT('Ctrl Pts',(-16.4292861682377,-18.2947226238509,
12.));
#181644=CARTESIAN_POINT('Ctrl Pts',(-16.4075185998454,-18.2847276433308,
12.));
#181645=CARTESIAN_POINT('Ctrl Pts',(-16.385854684708,-18.2747158096934,
12.));
#181646=CARTESIAN_POINT('Ctrl Pts',(-16.3642948194869,-18.2646876468169,
12.));
#181647=CARTESIAN_POINT('Ctrl Pts',(-16.342839403159,-18.2546436839609,
12.));
#181648=CARTESIAN_POINT('Ctrl Pts',(-16.3214888370988,-18.2445844558742,
12.));
#181649=CARTESIAN_POINT('Ctrl Pts',(-16.3002435251378,-18.2345105028981,
12.));
#181650=CARTESIAN_POINT('Ctrl Pts',(-16.2791038736223,-18.2244223710745,
12.));
#181651=CARTESIAN_POINT('Ctrl Pts',(-16.2580702914615,-18.214320612253,
12.));
#181652=CARTESIAN_POINT('Ctrl Pts',(-16.237143190164,-18.2042057842037,
12.));
#181653=CARTESIAN_POINT('Ctrl Pts',(-16.2163229838878,-18.1940784507232,
12.));
#181654=CARTESIAN_POINT('Ctrl Pts',(-16.1956100895076,-18.1839391817335,
12.));
#181655=CARTESIAN_POINT('Ctrl Pts',(-16.1750049266673,-18.1737885533852,
12.));
#181656=CARTESIAN_POINT('Ctrl Pts',(-16.1545079178261,-18.1636271481616,
12.));
#181657=CARTESIAN_POINT('Ctrl Pts',(-16.1341194882987,-18.153455554985,
12.));
#181658=CARTESIAN_POINT('Ctrl Pts',(-16.1138400662791,-18.1432743693231,
12.));
#181659=CARTESIAN_POINT('Ctrl Pts',(-16.0936700829108,-18.1330841933099,
12.));
#181660=CARTESIAN_POINT('Ctrl Pts',(-16.0736099723665,-18.1228856358746,
12.));
#181661=CARTESIAN_POINT('Ctrl Pts',(-16.0536601719124,-18.1126793128688,
12.));
#181662=CARTESIAN_POINT('Ctrl Pts',(-16.0338211219694,-18.1024658471966,
12.));
#181663=CARTESIAN_POINT('Ctrl Pts',(-16.0140932661612,-18.0922458689464,
12.));
#181664=CARTESIAN_POINT('Ctrl Pts',(-15.9944770513616,-18.0820200155238,
12.));
#181665=CARTESIAN_POINT('Ctrl Pts',(-15.9749729277848,-18.071788931796,
12.));
#181666=CARTESIAN_POINT('Ctrl Pts',(-15.9555813490645,-18.061553270236,
12.));
#181667=CARTESIAN_POINT('Ctrl Pts',(-15.9363027723244,-18.0513136910691,
12.));
#181668=CARTESIAN_POINT('Ctrl Pts',(-15.9171376582436,-18.0410708624208,
12.));
#181669=CARTESIAN_POINT('Ctrl Pts',(-15.8980864711043,-18.0308254604638,
12.));
#181670=CARTESIAN_POINT('Ctrl Pts',(-15.8791496788685,-18.0205781695773,
12.));
#181671=CARTESIAN_POINT('Ctrl Pts',(-15.8603277532834,-18.010329682521,
12.));
#181672=CARTESIAN_POINT('Ctrl Pts',(-15.8416211699682,-18.0000807006055,
12.));
#181673=CARTESIAN_POINT('Ctrl Pts',(-15.8230304084963,-17.9898319338664,
12.));
#181674=CARTESIAN_POINT('Ctrl Pts',(-15.8045559524674,-17.9795841012383,
12.));
#181675=CARTESIAN_POINT('Ctrl Pts',(-15.786198289572,-17.9693379307297,
12.));
#181676=CARTESIAN_POINT('Ctrl Pts',(-15.7679579117072,-17.9590941596236,
12.));
#181677=CARTESIAN_POINT('Ctrl Pts',(-15.7498353150856,-17.9488535346776,
12.));
#181678=CARTESIAN_POINT('Ctrl Pts',(-15.7318310003334,-17.9386168123261,
12.));
#181679=CARTESIAN_POINT('Ctrl Pts',(-15.713945472584,-17.9283847588837,
12.));
#181680=CARTESIAN_POINT('Ctrl Pts',(-15.6961792415526,-17.918158150746,
12.));
#181681=CARTESIAN_POINT('Ctrl Pts',(-15.6785328216467,-17.9079377746118,
12.));
#181682=CARTESIAN_POINT('Ctrl Pts',(-15.6610067321036,-17.8977244277247,
12.));
#181683=CARTESIAN_POINT('Ctrl Pts',(-15.6436014971088,-17.8875189181095,
12.));
#181684=CARTESIAN_POINT('Ctrl Pts',(-15.6263176459107,-17.8773220648125,
12.));
#181685=CARTESIAN_POINT('Ctrl Pts',(-15.6091557129205,-17.8671346981388,
12.));
#181686=CARTESIAN_POINT('Ctrl Pts',(-15.5921162378183,-17.8569576598996,
12.));
#181687=CARTESIAN_POINT('Ctrl Pts',(-15.5751997657154,-17.8467918036976,
12.));
#181688=CARTESIAN_POINT('Ctrl Pts',(-15.5584068472976,-17.8366379952078,
12.));
#181689=CARTESIAN_POINT('Ctrl Pts',(-15.5417380389639,-17.8264971124606,
12.));
#181690=CARTESIAN_POINT('Ctrl Pts',(-15.5251939029558,-17.8163700461262,
12.));
#181691=CARTESIAN_POINT('Ctrl Pts',(-15.5087750074728,-17.8062576997964,
12.));
#181692=CARTESIAN_POINT('Ctrl Pts',(-15.4924819268529,-17.7961609903161,
12.));
#181693=CARTESIAN_POINT('Ctrl Pts',(-15.4763152417506,-17.7860808481229,
12.));
#181694=CARTESIAN_POINT('Ctrl Pts',(-15.460275539302,-17.7760182175817,
12.));
#181695=CARTESIAN_POINT('Ctrl Pts',(-15.4443634132865,-17.765974057326,
12.));
#181696=CARTESIAN_POINT('Ctrl Pts',(-15.4285794642658,-17.7559493405871,
12.));
#181697=CARTESIAN_POINT('Ctrl Pts',(-15.4129242997828,-17.7459450555803,
12.));
#181698=CARTESIAN_POINT('Ctrl Pts',(-15.3973985345796,-17.7359622059143,
12.));
#181699=CARTESIAN_POINT('Ctrl Pts',(-15.3820027907965,-17.7260018109923,
12.));
#181700=CARTESIAN_POINT('Ctrl Pts',(-15.3667376981702,-17.7160649064208,
12.));
#181701=CARTESIAN_POINT('Ctrl Pts',(-15.3516038942064,-17.7061525444044,
12.));
#181702=CARTESIAN_POINT('Ctrl Pts',(-15.3366020244069,-17.6962657941984,
12.));
#181703=CARTESIAN_POINT('Ctrl Pts',(-15.3217327425341,-17.6864057426052,
12.));
#181704=CARTESIAN_POINT('Ctrl Pts',(-15.3069967108501,-17.6765734944559,
12.));
#181705=CARTESIAN_POINT('Ctrl Pts',(-15.2923946003598,-17.6667701731041,
12.));
#181706=CARTESIAN_POINT('Ctrl Pts',(-15.2779270910238,-17.6569969209,12.));
#181707=CARTESIAN_POINT('Ctrl Pts',(-15.263594872029,-17.6472548997329,
12.));
#181708=CARTESIAN_POINT('Ctrl Pts',(-15.2493986421091,-17.637545291637,
12.));
#181709=CARTESIAN_POINT('Ctrl Pts',(-15.2353391098367,-17.6278692993765,
12.));
#181710=CARTESIAN_POINT('Ctrl Pts',(-15.22141699392,-17.6182281470467,12.));
#181711=CARTESIAN_POINT('Ctrl Pts',(-15.2076330234686,-17.6086230806497,
12.));
#181712=CARTESIAN_POINT('Ctrl Pts',(-15.1939879383268,-17.5990553687595,
12.));
#181713=CARTESIAN_POINT('Ctrl Pts',(-15.1804824894605,-17.5895263032592,
12.));
#181714=CARTESIAN_POINT('Ctrl Pts',(-15.1671174393137,-17.5800372000539,
12.));
#181715=CARTESIAN_POINT('Ctrl Pts',(-15.1538935621715,-17.570589399803,
12.));
#181716=CARTESIAN_POINT('Ctrl Pts',(-15.1408116444877,-17.5611842686196,
12.));
#181717=CARTESIAN_POINT('Ctrl Pts',(-15.127872485314,-17.5518231989122,
12.));
#181718=CARTESIAN_POINT('Ctrl Pts',(-15.1150768967729,-17.5425076102966,
12.));
#181719=CARTESIAN_POINT('Ctrl Pts',(-15.1024257045033,-17.5332389504829,
12.));
#181720=CARTESIAN_POINT('Ctrl Pts',(-15.0899197481082,-17.5240186961788,
12.));
#181721=CARTESIAN_POINT('Ctrl Pts',(-15.0775598815748,-17.5148483539683,
12.));
#181722=CARTESIAN_POINT('Ctrl Pts',(-15.0653469738306,-17.5057294613874,
12.));
#181723=CARTESIAN_POINT('Ctrl Pts',(-15.0532819093085,-17.4966635880245,
12.));
#181724=CARTESIAN_POINT('Ctrl Pts',(-15.0413655884993,-17.4876523366178,
12.));
#181725=CARTESIAN_POINT('Ctrl Pts',(-15.029598928488,-17.4786973441417,
12.));
#181726=CARTESIAN_POINT('Ctrl Pts',(-15.0179828635086,-17.4698002829356,
12.));
#181727=CARTESIAN_POINT('Ctrl Pts',(-15.0065183456921,-17.4609628621418,
12.));
#181728=CARTESIAN_POINT('Ctrl Pts',(-14.9952063457778,-17.4521868291004,
12.));
#181729=CARTESIAN_POINT('Ctrl Pts',(-14.9840478538358,-17.4434739707773,
12.));
#181730=CARTESIAN_POINT('Ctrl Pts',(-14.9730438799452,-17.4348261151396,
12.));
#181731=CARTESIAN_POINT('Ctrl Pts',(-14.9621954549827,-17.426245132709,
12.));
#181732=CARTESIAN_POINT('Ctrl Pts',(-14.9515036315143,-17.4177329382828,
12.));
#181733=CARTESIAN_POINT('Ctrl Pts',(-14.940969484645,-17.4092914926071,
12.));
#181734=CARTESIAN_POINT('Ctrl Pts',(-14.9305941128757,-17.4009228040749,
12.));
#181735=CARTESIAN_POINT('Ctrl Pts',(-14.9203786389342,-17.3926289303986,
12.));
#181736=CARTESIAN_POINT('Ctrl Pts',(-14.9103242110058,-17.3844119809824,
12.));
#181737=CARTESIAN_POINT('Ctrl Pts',(-14.900432003961,-17.3762741193076,
12.));
#181738=CARTESIAN_POINT('Ctrl Pts',(-14.8907032205788,-17.3682175653235,
12.));
#181739=CARTESIAN_POINT('Ctrl Pts',(-14.8811390927423,-17.3602445978161,
12.));
#181740=CARTESIAN_POINT('Ctrl Pts',(-14.8717408826956,-17.3523575568645,
12.));
#181741=CARTESIAN_POINT('Ctrl Pts',(-14.8625098843417,-17.3445588463474,
12.));
#181742=CARTESIAN_POINT('Ctrl Pts',(-14.8534474245434,-17.336850936485,
12.));
#181743=CARTESIAN_POINT('Ctrl Pts',(-14.8445548643508,-17.3292363662605,
12.));
#181744=CARTESIAN_POINT('Ctrl Pts',(-14.8358336004197,-17.3217177462101,
12.));
#181745=CARTESIAN_POINT('Ctrl Pts',(-14.8272850675379,-17.3142977632659,
12.));
#181746=CARTESIAN_POINT('Ctrl Pts',(-14.8189107410162,-17.3069791853706,
12.));
#181747=CARTESIAN_POINT('Ctrl Pts',(-14.8107121391036,-17.299764866148,
12.));
#181748=CARTESIAN_POINT('Ctrl Pts',(-14.8026908254276,-17.2926577496513,
12.));
#181749=CARTESIAN_POINT('Ctrl Pts',(-14.7948484105249,-17.2856608733196,
12.));
#181750=CARTESIAN_POINT('Ctrl Pts',(-14.787186553128,-17.2787773704849,
12.));
#181751=CARTESIAN_POINT('Ctrl Pts',(-14.7797069617804,-17.2720104735194,
12.));
#181752=CARTESIAN_POINT('Ctrl Pts',(-14.7724113956731,-17.2653635155319,
12.));
#181753=CARTESIAN_POINT('Ctrl Pts',(-14.7653016697591,-17.2588399401465,
12.));
#181754=CARTESIAN_POINT('Ctrl Pts',(-14.7583796616617,-17.2524433146837,
12.));
#181755=CARTESIAN_POINT('Ctrl Pts',(-14.7516473175124,-17.2461773413288,
12.));
#181756=CARTESIAN_POINT('Ctrl Pts',(-14.7451066593792,-17.2400458713565,
12.));
#181757=CARTESIAN_POINT('Ctrl Pts',(-14.7387597858117,-17.2340529062076,
12.));
#181758=CARTESIAN_POINT('Ctrl Pts',(-14.7326088681163,-17.2282025904314,
12.));
#181759=CARTESIAN_POINT('Ctrl Pts',(-14.7266561494282,-17.2224992099666,
12.));
#181760=CARTESIAN_POINT('Ctrl Pts',(-14.7209039390327,-17.2169471814256,
12.));
#181761=CARTESIAN_POINT('Ctrl Pts',(-14.7153546289339,-17.2115510835989,
12.));
#181762=CARTESIAN_POINT('Ctrl Pts',(-14.7100107213586,-17.2063157097315,
12.));
#181763=CARTESIAN_POINT('Ctrl Pts',(-14.7048748502663,-17.2012461084268,
12.));
#181764=CARTESIAN_POINT('Ctrl Pts',(-14.699949811582,-17.1963476411694,
12.));
#181765=CARTESIAN_POINT('Ctrl Pts',(-14.6952385361706,-17.1916259308415,
12.));
#181766=CARTESIAN_POINT('Ctrl Pts',(-14.6907440526958,-17.1870867909918,
12.));
#181767=CARTESIAN_POINT('Ctrl Pts',(-14.686469452232,-17.1827361584719,
12.));
#181768=CARTESIAN_POINT('Ctrl Pts',(-14.6824178576167,-17.1785800350826,
12.));
#181769=CARTESIAN_POINT('Ctrl Pts',(-14.6785925615677,-17.1746247499056,
12.));
#181770=CARTESIAN_POINT('Ctrl Pts',(-14.6749971333867,-17.1708771619129,
12.));
#181771=CARTESIAN_POINT('Ctrl Pts',(-14.671635583332,-17.167344972302,12.));
#181772=CARTESIAN_POINT('Ctrl Pts',(-14.6685123374423,-17.1640366762305,
12.));
#181773=CARTESIAN_POINT('Ctrl Pts',(-14.6656319165057,-17.1609609517369,
12.));
#181774=CARTESIAN_POINT('Ctrl Pts',(-14.6629987285992,-17.1581262646789,
12.));
#181775=CARTESIAN_POINT('Ctrl Pts',(-14.6606167169642,-17.1555401986401,
12.));
#181776=CARTESIAN_POINT('Ctrl Pts',(-14.6584900555302,-17.1532107762718,
12.));
#181777=CARTESIAN_POINT('Ctrl Pts',(-14.6566237952435,-17.1511476869496,
12.));
#181778=CARTESIAN_POINT('Ctrl Pts',(-14.655024862281,-17.1493641837558,
12.));
#181779=CARTESIAN_POINT('Ctrl Pts',(-14.6537016966184,-17.147876394491,
12.));
#181780=CARTESIAN_POINT('Ctrl Pts',(-14.6526624064978,-17.1466998098673,
12.));
#181781=CARTESIAN_POINT('Ctrl Pts',(-14.6519131634508,-17.1458462295271,
12.));
#181782=CARTESIAN_POINT('Ctrl Pts',(-14.6515481598068,-17.1454262858043,
12.));
#181783=CARTESIAN_POINT('Ctrl Pts',(-14.6514066997196,-17.1452600887037,
12.));
#181784=CARTESIAN_POINT('Ctrl Pts',(-14.6513711852843,-17.1452153999142,
12.));
#181785=CARTESIAN_POINT('Ctrl Pts',(-14.6513681262571,-17.1452095830632,
12.));
#181786=CARTESIAN_POINT('',(-14.2886635873976,-16.7207683102834,12.));
#181787=CARTESIAN_POINT('',(-6.98376450772884,-8.17248635976757,12.));
#181788=CARTESIAN_POINT('',(-13.5924445804218,-16.6581946899465,12.));
#181789=CARTESIAN_POINT('Origin',(-13.9085479427572,-17.0455945664569,12.));
#181790=CARTESIAN_POINT('',(-12.572596943457,-17.4407513054161,12.));
#181791=CARTESIAN_POINT('Origin',(-4.9889687874677E-13,-6.00167842331873E-13,
12.));
#181792=CARTESIAN_POINT('',(-12.4528436808172,-18.1294424696716,12.));
#181793=CARTESIAN_POINT('Origin',(-12.8649829188863,-17.846350172984,12.));
#181794=CARTESIAN_POINT('',(-12.7689476255363,-18.5896416359912,12.));
#181795=CARTESIAN_POINT('',(-6.38447381276812,-9.29482081799561,12.));
#181796=CARTESIAN_POINT('',(-13.5685075571671,-22.1787195904339,12.));
#181797=CARTESIAN_POINT('Ctrl Pts',(-12.7689476255363,-18.5896416359912,
12.));
#181798=CARTESIAN_POINT('Ctrl Pts',(-12.7689524524484,-18.5896460962961,
12.));
#181799=CARTESIAN_POINT('Ctrl Pts',(-12.7689864266924,-18.5896919669158,
12.));
#181800=CARTESIAN_POINT('Ctrl Pts',(-12.7691103481996,-18.589871621842,
12.));
#181801=CARTESIAN_POINT('Ctrl Pts',(-12.7694215127923,-18.590332877722,
12.));
#181802=CARTESIAN_POINT('Ctrl Pts',(-12.7700520897174,-18.5912775137806,
12.));
#181803=CARTESIAN_POINT('Ctrl Pts',(-12.7709195951154,-18.5925859134582,
12.));
#181804=CARTESIAN_POINT('Ctrl Pts',(-12.7720142287169,-18.5942490615409,
12.));
#181805=CARTESIAN_POINT('Ctrl Pts',(-12.7733231262107,-18.5962551167772,
12.));
#181806=CARTESIAN_POINT('Ctrl Pts',(-12.7748328937639,-18.5985917525949,
12.));
#181807=CARTESIAN_POINT('Ctrl Pts',(-12.7765325225083,-18.6012488486708,
12.));
#181808=CARTESIAN_POINT('Ctrl Pts',(-12.7784139605067,-18.6042190183703,
12.));
#181809=CARTESIAN_POINT('Ctrl Pts',(-12.7804705387658,-18.6074961535723,
12.));
#181810=CARTESIAN_POINT('Ctrl Pts',(-12.7826959526924,-18.611074482622,
12.));
#181811=CARTESIAN_POINT('Ctrl Pts',(-12.78508316579,-18.6149475565189,12.));
#181812=CARTESIAN_POINT('Ctrl Pts',(-12.7876249657834,-18.6191087624752,
12.));
#181813=CARTESIAN_POINT('Ctrl Pts',(-12.7903142925235,-18.6235516265575,
12.));
#181814=CARTESIAN_POINT('Ctrl Pts',(-12.7931447451556,-18.6282702819371,
12.));
#181815=CARTESIAN_POINT('Ctrl Pts',(-12.7961106222251,-18.6332595057005,
12.));
#181816=CARTESIAN_POINT('Ctrl Pts',(-12.7992066625264,-18.63851447924,12.));
#181817=CARTESIAN_POINT('Ctrl Pts',(-12.8024278770153,-18.6440306327457,
12.));
#181818=CARTESIAN_POINT('Ctrl Pts',(-12.805769331162,-18.6498034438986,
12.));
#181819=CARTESIAN_POINT('Ctrl Pts',(-12.8092261933858,-18.6558284825772,
12.));
#181820=CARTESIAN_POINT('Ctrl Pts',(-12.8127937909632,-18.6621014624746,
12.));
#181821=CARTESIAN_POINT('Ctrl Pts',(-12.8164676687361,-18.6686182952798,
12.));
#181822=CARTESIAN_POINT('Ctrl Pts',(-12.8202436318473,-18.6753751301091,
12.));
#181823=CARTESIAN_POINT('Ctrl Pts',(-12.8241176980016,-18.6823683094138,
12.));
#181824=CARTESIAN_POINT('Ctrl Pts',(-12.8280860635231,-18.6895943376172,
12.));
#181825=CARTESIAN_POINT('Ctrl Pts',(-12.832145059979,-18.6970498410173,
12.));
#181826=CARTESIAN_POINT('Ctrl Pts',(-12.8362911280362,-18.7047315436296,
12.));
#181827=CARTESIAN_POINT('Ctrl Pts',(-12.8405208263432,-18.7126362754446,
12.));
#181828=CARTESIAN_POINT('Ctrl Pts',(-12.8448308329494,-18.7207609737701,
12.));
#181829=CARTESIAN_POINT('Ctrl Pts',(-12.849217951159,-18.7291026886552,
12.));
#181830=CARTESIAN_POINT('Ctrl Pts',(-12.8536791086315,-18.7376585820851,
12.));
#181831=CARTESIAN_POINT('Ctrl Pts',(-12.8582113455645,-18.7464259171248,
12.));
#181832=CARTESIAN_POINT('Ctrl Pts',(-12.8628118054172,-18.7554020493888,
12.));
#181833=CARTESIAN_POINT('Ctrl Pts',(-12.8674777239656,-18.7645844169568,
12.));
#181834=CARTESIAN_POINT('Ctrl Pts',(-12.8722064211814,-18.7739705329028,
12.));
#181835=CARTESIAN_POINT('Ctrl Pts',(-12.8769952998097,-18.7835579840481,
12.));
#181836=CARTESIAN_POINT('Ctrl Pts',(-12.8818418427474,-18.7933444285867,
12.));
#181837=CARTESIAN_POINT('Ctrl Pts',(-12.8867436109543,-18.8033275941939,
12.));
#181838=CARTESIAN_POINT('Ctrl Pts',(-12.8916982409931,-18.8135052757815,
12.));
#181839=CARTESIAN_POINT('Ctrl Pts',(-12.8967034410752,-18.8238753319124,
12.));
#181840=CARTESIAN_POINT('Ctrl Pts',(-12.9017569871738,-18.834435681259,
12.));
#181841=CARTESIAN_POINT('Ctrl Pts',(-12.9068567191856,-18.8451842990986,
12.));
#181842=CARTESIAN_POINT('Ctrl Pts',(-12.9120005369066,-18.8561192136201,
12.));
#181843=CARTESIAN_POINT('Ctrl Pts',(-12.9171863977047,-18.8672385038328,
12.));
#181844=CARTESIAN_POINT('Ctrl Pts',(-12.9224123144982,-18.8785402977528,
12.));
#181845=CARTESIAN_POINT('Ctrl Pts',(-12.9276763536373,-18.8900227704888,
12.));
#181846=CARTESIAN_POINT('Ctrl Pts',(-12.9329766328184,-18.9016841423402,
12.));
#181847=CARTESIAN_POINT('Ctrl Pts',(-12.9383113190375,-18.9135226769466,
12.));
#181848=CARTESIAN_POINT('Ctrl Pts',(-12.9436786266106,-18.9255366795196,
12.));
#181849=CARTESIAN_POINT('Ctrl Pts',(-12.9490768151821,-18.9377244950435,
12.));
#181850=CARTESIAN_POINT('Ctrl Pts',(-12.9545041877377,-18.9500845064714,
12.));
#181851=CARTESIAN_POINT('Ctrl Pts',(-12.9599590886318,-18.9626151329226,
12.));
#181852=CARTESIAN_POINT('Ctrl Pts',(-12.9654399021868,-18.9753148284473,
12.));
#181853=CARTESIAN_POINT('Ctrl Pts',(-12.9709450512747,-18.9881820807585,
12.));
#181854=CARTESIAN_POINT('Ctrl Pts',(-12.9764729959206,-19.0012154099792,
12.));
#181855=CARTESIAN_POINT('Ctrl Pts',(-12.9820222318716,-19.014413367335,
12.));
#181856=CARTESIAN_POINT('Ctrl Pts',(-12.9875912893003,-19.0277745339908,
12.));
#181857=CARTESIAN_POINT('Ctrl Pts',(-12.9931787316514,-19.0412975200398,
12.));
#181858=CARTESIAN_POINT('Ctrl Pts',(-12.9987831544502,-19.0549809634354,
12.));
#181859=CARTESIAN_POINT('Ctrl Pts',(-13.0044031841382,-19.0688235289437,
12.));
#181860=CARTESIAN_POINT('Ctrl Pts',(-13.0100374768788,-19.0828239070484,
12.));
#181861=CARTESIAN_POINT('Ctrl Pts',(-13.0156847176097,-19.0969808131228,
12.));
#181862=CARTESIAN_POINT('Ctrl Pts',(-13.0213436191328,-19.111292986631,
12.));
#181863=CARTESIAN_POINT('Ctrl Pts',(-13.0270129211976,-19.1257591903099,
12.));
#181864=CARTESIAN_POINT('Ctrl Pts',(-13.0326913895838,-19.1403782093386,
12.));
#181865=CARTESIAN_POINT('Ctrl Pts',(-13.0383778152068,-19.155148850523,
12.));
#181866=CARTESIAN_POINT('Ctrl Pts',(-13.0440710133772,-19.1700699416622,
12.));
#181867=CARTESIAN_POINT('Ctrl Pts',(-13.0497698230441,-19.1851403308825,
12.));
#181868=CARTESIAN_POINT('Ctrl Pts',(-13.0554731060538,-19.2003588859772,
12.));
#181869=CARTESIAN_POINT('Ctrl Pts',(-13.0611797463915,-19.2157244937142,
12.));
#181870=CARTESIAN_POINT('Ctrl Pts',(-13.0668886494795,-19.2312360592033,
12.));
#181871=CARTESIAN_POINT('Ctrl Pts',(-13.0725987415859,-19.2468925053989,
12.));
#181872=CARTESIAN_POINT('Ctrl Pts',(-13.0783089692118,-19.2626927725596,
12.));
#181873=CARTESIAN_POINT('Ctrl Pts',(-13.0840182984949,-19.2786358177198,
12.));
#181874=CARTESIAN_POINT('Ctrl Pts',(-13.0897257145969,-19.2947206141247,
12.));
#181875=CARTESIAN_POINT('Ctrl Pts',(-13.0954302211479,-19.310946150736,
12.));
#181876=CARTESIAN_POINT('Ctrl Pts',(-13.1011308397591,-19.3273114318269,
12.));
#181877=CARTESIAN_POINT('Ctrl Pts',(-13.1068266095186,-19.3438154765395,
12.));
#181878=CARTESIAN_POINT('Ctrl Pts',(-13.1125165865022,-19.3604573184515,
12.));
#181879=CARTESIAN_POINT('Ctrl Pts',(-13.118199843271,-19.3772360051091,
12.));
#181880=CARTESIAN_POINT('Ctrl Pts',(-13.1238754684177,-19.3941505976263,
12.));
#181881=CARTESIAN_POINT('Ctrl Pts',(-13.1295425661634,-19.4112001703557,
12.));
#181882=CARTESIAN_POINT('Ctrl Pts',(-13.1352002559438,-19.4283838105262,
12.));
#181883=CARTESIAN_POINT('Ctrl Pts',(-13.1408476720061,-19.4457006178876,
12.));
#181884=CARTESIAN_POINT('Ctrl Pts',(-13.1464839629971,-19.4631497043258,
12.));
#181885=CARTESIAN_POINT('Ctrl Pts',(-13.1521082915853,-19.4807301935268,
12.));
#181886=CARTESIAN_POINT('Ctrl Pts',(-13.1577198341245,-19.4984412207081,
12.));
#181887=CARTESIAN_POINT('Ctrl Pts',(-13.1633177803101,-19.5162819323213,
12.));
#181888=CARTESIAN_POINT('Ctrl Pts',(-13.1689013328431,-19.5342514857562,
12.));
#181889=CARTESIAN_POINT('Ctrl Pts',(-13.1744697070911,-19.5523490490244,
12.));
#181890=CARTESIAN_POINT('Ctrl Pts',(-13.1800221307673,-19.5705738004667,
12.));
#181891=CARTESIAN_POINT('Ctrl Pts',(-13.1855578436471,-19.5889249285338,
12.));
#181892=CARTESIAN_POINT('Ctrl Pts',(-13.1910760972814,-19.6074016315414,
12.));
#181893=CARTESIAN_POINT('Ctrl Pts',(-13.1965761547151,-19.6260031174244,
12.));
#181894=CARTESIAN_POINT('Ctrl Pts',(-13.2020572902065,-19.6447286034772,
12.));
#181895=CARTESIAN_POINT('Ctrl Pts',(-13.2075187889529,-19.6635773160936,
12.));
#181896=CARTESIAN_POINT('Ctrl Pts',(-13.2129599468485,-19.6825484905823,
12.));
#181897=CARTESIAN_POINT('Ctrl Pts',(-13.2183800702436,-19.7016413709685,
12.));
#181898=CARTESIAN_POINT('Ctrl Pts',(-13.2237784757066,-19.7208552097868,
12.));
#181899=CARTESIAN_POINT('Ctrl Pts',(-13.2291544897899,-19.7401892678697,
12.));
#181900=CARTESIAN_POINT('Ctrl Pts',(-13.2345074487963,-19.7596428141168,
12.));
#181901=CARTESIAN_POINT('Ctrl Pts',(-13.2398366985675,-19.7792151253289,
12.));
#181902=CARTESIAN_POINT('Ctrl Pts',(-13.2451415942805,-19.7989054860495,
12.));
#181903=CARTESIAN_POINT('Ctrl Pts',(-13.2504215002457,-19.8187131883917,
12.));
#181904=CARTESIAN_POINT('Ctrl Pts',(-13.2556757897086,-19.8386375318634,
12.));
#181905=CARTESIAN_POINT('Ctrl Pts',(-13.2609038446529,-19.8586778231715,
12.));
#181906=CARTESIAN_POINT('Ctrl Pts',(-13.2661050556132,-19.8788333760577,
12.));
#181907=CARTESIAN_POINT('Ctrl Pts',(-13.271278821502,-19.8991035111745,
12.));
#181908=CARTESIAN_POINT('Ctrl Pts',(-13.2764245494357,-19.9194875559422,
12.));
#181909=CARTESIAN_POINT('Ctrl Pts',(-13.2815416545663,-19.9399848444019,
12.));
#181910=CARTESIAN_POINT('Ctrl Pts',(-13.286629559915,-19.9605947170586,
12.));
#181911=CARTESIAN_POINT('Ctrl Pts',(-13.2916876962094,-19.981316520717,
12.));
#181912=CARTESIAN_POINT('Ctrl Pts',(-13.2967155017306,-20.0021496083738,
12.));
#181913=CARTESIAN_POINT('Ctrl Pts',(-13.3017124221637,-20.0230933391038,
12.));
#181914=CARTESIAN_POINT('Ctrl Pts',(-13.3066779104515,-20.0441470779345,
12.));
#181915=CARTESIAN_POINT('Ctrl Pts',(-13.3116114266515,-20.0653101957188,
12.));
#181916=CARTESIAN_POINT('Ctrl Pts',(-13.3165124377963,-20.0865820689882,
12.));
#181917=CARTESIAN_POINT('Ctrl Pts',(-13.3213804177587,-20.1079620798375,
12.));
#181918=CARTESIAN_POINT('Ctrl Pts',(-13.3262148471226,-20.1294496158402,
12.));
#181919=CARTESIAN_POINT('Ctrl Pts',(-13.3310152130564,-20.1510440699474,
12.));
#181920=CARTESIAN_POINT('Ctrl Pts',(-13.3357810091903,-20.1727448403817,
12.));
#181921=CARTESIAN_POINT('Ctrl Pts',(-13.3405117354971,-20.1945513305235,
12.));
#181922=CARTESIAN_POINT('Ctrl Pts',(-13.3452068981766,-20.216462948786,
12.));
#181923=CARTESIAN_POINT('Ctrl Pts',(-13.3498660095386,-20.2384791085359,
12.));
#181924=CARTESIAN_POINT('Ctrl Pts',(-13.3544885878889,-20.2605992280122,
12.));
#181925=CARTESIAN_POINT('Ctrl Pts',(-13.3590741574195,-20.2828227302339,
12.));
#181926=CARTESIAN_POINT('Ctrl Pts',(-13.3636222481016,-20.3051490429048,
12.));
#181927=CARTESIAN_POINT('Ctrl Pts',(-13.3681323955826,-20.3275775983029,
12.));
#181928=CARTESIAN_POINT('Ctrl Pts',(-13.3726041410867,-20.3501078331814,
12.));
#181929=CARTESIAN_POINT('Ctrl Pts',(-13.3770370313188,-20.3727391887184,
12.));
#181930=CARTESIAN_POINT('Ctrl Pts',(-13.3814306183719,-20.3954711104502,
12.));
#181931=CARTESIAN_POINT('Ctrl Pts',(-13.3857844596387,-20.4183030482002,
12.));
#181932=CARTESIAN_POINT('Ctrl Pts',(-13.3900981177255,-20.4412344560007,
12.));
#181933=CARTESIAN_POINT('Ctrl Pts',(-13.3943711603739,-20.4642647920037,
12.));
#181934=CARTESIAN_POINT('Ctrl Pts',(-13.3986031603716,-20.487393518404,
12.));
#181935=CARTESIAN_POINT('Ctrl Pts',(-13.4027936954529,-20.5106201013753,
12.));
#181936=CARTESIAN_POINT('Ctrl Pts',(-13.4069423482076,-20.5339440109956,
12.));
#181937=CARTESIAN_POINT('Ctrl Pts',(-13.4110487059912,-20.5573647211639,
12.));
#181938=CARTESIAN_POINT('Ctrl Pts',(-13.4151123608411,-20.5808817095155,
12.));
#181939=CARTESIAN_POINT('Ctrl Pts',(-13.4191329093933,-20.6044944573153,
12.));
#181940=CARTESIAN_POINT('Ctrl Pts',(-13.4231099528179,-20.6282024494237,
12.));
#181941=CARTESIAN_POINT('Ctrl Pts',(-13.4270430967652,-20.6520051742869,
12.));
#181942=CARTESIAN_POINT('Ctrl Pts',(-13.4309319513119,-20.6759021239103,
12.));
#181943=CARTESIAN_POINT('Ctrl Pts',(-13.4347761309154,-20.6998927938288,
12.));
#181944=CARTESIAN_POINT('Ctrl Pts',(-13.4385752543663,-20.7239766830675,
12.));
#181945=CARTESIAN_POINT('Ctrl Pts',(-13.4423289447561,-20.7481532941013,
12.));
#181946=CARTESIAN_POINT('Ctrl Pts',(-13.4460368293688,-20.7724221327608,
12.));
#181947=CARTESIAN_POINT('Ctrl Pts',(-13.4496985395637,-20.7967827081227,
12.));
#181948=CARTESIAN_POINT('Ctrl Pts',(-13.4533137106667,-20.821234532398,
12.));
#181949=CARTESIAN_POINT('Ctrl Pts',(-13.4568819818631,-20.8457771208082,
12.));
#181950=CARTESIAN_POINT('Ctrl Pts',(-13.4604029960983,-20.8704099914641,
12.));
#181951=CARTESIAN_POINT('Ctrl Pts',(-13.4638763999726,-20.8951326652158,
12.));
#181952=CARTESIAN_POINT('Ctrl Pts',(-13.4673018437718,-20.9199446657584,
12.));
#181953=CARTESIAN_POINT('Ctrl Pts',(-13.4706789815167,-20.9448455197557,
12.));
#181954=CARTESIAN_POINT('Ctrl Pts',(-13.4740074710087,-20.9698347569476,
12.));
#181955=CARTESIAN_POINT('Ctrl Pts',(-13.4772869738879,-20.9949119102592,
12.));
#181956=CARTESIAN_POINT('Ctrl Pts',(-13.4805171556822,-21.0200765158885,
12.));
#181957=CARTESIAN_POINT('Ctrl Pts',(-13.4836976858912,-21.0453281134247,
12.));
#181958=CARTESIAN_POINT('Ctrl Pts',(-13.4868282377192,-21.0706662455202,
12.));
#181959=CARTESIAN_POINT('Ctrl Pts',(-13.4899084877718,-21.0960904575048,
12.));
#181960=CARTESIAN_POINT('Ctrl Pts',(-13.4929381157778,-21.1216002970209,
12.));
#181961=CARTESIAN_POINT('Ctrl Pts',(-13.4959168042934,-21.1471953136209,
12.));
#181962=CARTESIAN_POINT('Ctrl Pts',(-13.4988442384491,-21.1728750584173,
12.));
#181963=CARTESIAN_POINT('Ctrl Pts',(-13.5017201056088,-21.1986390835825,
12.));
#181964=CARTESIAN_POINT('Ctrl Pts',(-13.5045440957404,-21.224486942933,
12.));
#181965=CARTESIAN_POINT('Ctrl Pts',(-13.5073159019454,-21.2504181927429,
12.));
#181966=CARTESIAN_POINT('Ctrl Pts',(-13.5100352209207,-21.2764323924442,
12.));
#181967=CARTESIAN_POINT('Ctrl Pts',(-13.5127017534972,-21.3025291054236,
12.));
#181968=CARTESIAN_POINT('Ctrl Pts',(-13.5153152050554,-21.328707899634,
12.));
#181969=CARTESIAN_POINT('Ctrl Pts',(-13.5178752862461,-21.3549683486219,
12.));
#181970=CARTESIAN_POINT('Ctrl Pts',(-13.5203817122497,-21.3813100304967,
12.));
#181971=CARTESIAN_POINT('Ctrl Pts',(-13.5228342013508,-21.4077325259318,
12.));
#181972=CARTESIAN_POINT('Ctrl Pts',(-13.5252324737795,-21.4342354165253,
12.));
#181973=CARTESIAN_POINT('Ctrl Pts',(-13.5275762503553,-21.4608182828695,
12.));
#181974=CARTESIAN_POINT('Ctrl Pts',(-13.5298652514357,-21.487480703047,
12.));
#181975=CARTESIAN_POINT('Ctrl Pts',(-13.5320991952145,-21.5142222501671,
12.));
#181976=CARTESIAN_POINT('Ctrl Pts',(-13.5342777983225,-21.5410424932511,
12.));
#181977=CARTESIAN_POINT('Ctrl Pts',(-13.5364007790292,-21.5679410019011,
12.));
#181978=CARTESIAN_POINT('Ctrl Pts',(-13.5384678597206,-21.5949173499022,
12.));
#181979=CARTESIAN_POINT('Ctrl Pts',(-13.5404787697798,-21.6219711193951,
12.));
#181980=CARTESIAN_POINT('Ctrl Pts',(-13.5424332480698,-21.6491019044647,
12.));
#181981=CARTESIAN_POINT('Ctrl Pts',(-13.5443310461516,-21.676309315769,
12.));
#181982=CARTESIAN_POINT('Ctrl Pts',(-13.546171929503,-21.7035929822939,
12.));
#181983=CARTESIAN_POINT('Ctrl Pts',(-13.5479556704457,-21.730952541226,
12.));
#181984=CARTESIAN_POINT('Ctrl Pts',(-13.5496820422187,-21.7583876294532,
12.));
#181985=CARTESIAN_POINT('Ctrl Pts',(-13.5513508127232,-21.7858978745848,
12.));
#181986=CARTESIAN_POINT('Ctrl Pts',(-13.5529617381569,-21.8134828857963,
12.));
#181987=CARTESIAN_POINT('Ctrl Pts',(-13.5545145573049,-21.841142245609,
12.));
#181988=CARTESIAN_POINT('Ctrl Pts',(-13.5560089839426,-21.8688754989401,
12.));
#181989=CARTESIAN_POINT('Ctrl Pts',(-13.5574447178485,-21.8966821688876,
12.));
#181990=CARTESIAN_POINT('Ctrl Pts',(-13.5588214586672,-21.9245617765827,
12.));
#181991=CARTESIAN_POINT('Ctrl Pts',(-13.5601389185315,-21.9525138592862,
12.));
#181992=CARTESIAN_POINT('Ctrl Pts',(-13.5613968357589,-21.9805379899192,
12.));
#181993=CARTESIAN_POINT('Ctrl Pts',(-13.5625949868313,-22.0086337943431,
12.));
#181994=CARTESIAN_POINT('Ctrl Pts',(-13.5637332022393,-22.0368009736227,
12.));
#181995=CARTESIAN_POINT('Ctrl Pts',(-13.5648113688895,-22.0650393089492,
12.));
#181996=CARTESIAN_POINT('Ctrl Pts',(-13.5658294169107,-22.0933486464442,
12.));
#181997=CARTESIAN_POINT('Ctrl Pts',(-13.5667873105179,-22.1217288871823,
12.));
#181998=CARTESIAN_POINT('Ctrl Pts',(-13.5675054918922,-22.1444897575076,
12.));
#181999=CARTESIAN_POINT('Ctrl Pts',(-13.5680170531724,-22.1615922804939,
12.));
#182000=CARTESIAN_POINT('Ctrl Pts',(-13.5683460612913,-22.1730081264583,
12.));
#182001=CARTESIAN_POINT('Ctrl Pts',(-13.5685075571671,-22.1787195904339,
12.));
#182002=CARTESIAN_POINT('',(-12.4230808101438,-22.8400320311648,12.));
#182003=CARTESIAN_POINT('Origin',(0.,0.,12.));
#182004=CARTESIAN_POINT('',(-9.71462809124917,-20.353053841303,12.));
#182005=CARTESIAN_POINT('Ctrl Pts',(-12.4230808101438,-22.8400320311648,
12.));
#182006=CARTESIAN_POINT('Ctrl Pts',(-12.4182152851867,-22.8370364396497,
12.));
#182007=CARTESIAN_POINT('Ctrl Pts',(-12.4084933766366,-22.8310435872852,
12.));
#182008=CARTESIAN_POINT('Ctrl Pts',(-12.393937937903,-22.8220493007353,
12.));
#182009=CARTESIAN_POINT('Ctrl Pts',(-12.3745855366772,-22.8100469022632,
12.));
#182010=CARTESIAN_POINT('Ctrl Pts',(-12.3504864740361,-22.7950272216959,
12.));
#182011=CARTESIAN_POINT('Ctrl Pts',(-12.3264788926108,-22.7799908974947,
12.));
#182012=CARTESIAN_POINT('Ctrl Pts',(-12.3025628601812,-22.7649380101154,
12.));
#182013=CARTESIAN_POINT('Ctrl Pts',(-12.2787384750747,-22.7498686970096,
12.));
#182014=CARTESIAN_POINT('Ctrl Pts',(-12.2550058702389,-22.7347831655251,
12.));
#182015=CARTESIAN_POINT('Ctrl Pts',(-12.2313652198047,-22.7196817119299,
12.));
#182016=CARTESIAN_POINT('Ctrl Pts',(-12.2078167360267,-22.7045647168659,
12.));
#182017=CARTESIAN_POINT('Ctrl Pts',(-12.1843606579246,-22.6894326204959,
12.));
#182018=CARTESIAN_POINT('Ctrl Pts',(-12.1609972423089,-22.6742859034891,
12.));
#182019=CARTESIAN_POINT('Ctrl Pts',(-12.1377267537141,-22.6591250653942,
12.));
#182020=CARTESIAN_POINT('Ctrl Pts',(-12.1145494550384,-22.6439506046611,
12.));
#182021=CARTESIAN_POINT('Ctrl Pts',(-12.0914655972828,-22.628762996708,
12.));
#182022=CARTESIAN_POINT('Ctrl Pts',(-12.0684754113869,-22.613562676493,
12.));
#182023=CARTESIAN_POINT('Ctrl Pts',(-12.0455791139135,-22.5983500505675,
12.));
#182024=CARTESIAN_POINT('Ctrl Pts',(-12.0227769113132,-22.5831255061306,
12.));
#182025=CARTESIAN_POINT('Ctrl Pts',(-12.0000690046697,-22.5678894211194,
12.));
#182026=CARTESIAN_POINT('Ctrl Pts',(-11.9774555943496,-22.5526421741159,
12.));
#182027=CARTESIAN_POINT('Ctrl Pts',(-11.9549368843996,-22.5373841537299,
12.));
#182028=CARTESIAN_POINT('Ctrl Pts',(-11.9325130877801,-22.5221157697869,
12.));
#182029=CARTESIAN_POINT('Ctrl Pts',(-11.9101844254555,-22.5068374513958,
12.));
#182030=CARTESIAN_POINT('Ctrl Pts',(-11.8879511239941,-22.4915496418472,
12.));
#182031=CARTESIAN_POINT('Ctrl Pts',(-11.8658134137018,-22.4762527946694,
12.));
#182032=CARTESIAN_POINT('Ctrl Pts',(-11.8437715264487,-22.4609473690469,
12.));
#182033=CARTESIAN_POINT('Ctrl Pts',(-11.8218256937889,-22.4456338258738,
12.));
#182034=CARTESIAN_POINT('Ctrl Pts',(-11.7999761445175,-22.4303126226468,
12.));
#182035=CARTESIAN_POINT('Ctrl Pts',(-11.7782231042041,-22.4149842125018,
12.));
#182036=CARTESIAN_POINT('Ctrl Pts',(-11.7565667964765,-22.39964904692,12.));
#182037=CARTESIAN_POINT('Ctrl Pts',(-11.7350074437961,-22.3843075773905,
12.));
#182038=CARTESIAN_POINT('Ctrl Pts',(-11.7135452684532,-22.3689602575492,
12.));
#182039=CARTESIAN_POINT('Ctrl Pts',(-11.6921804934056,-22.3536075450028,
12.));
#182040=CARTESIAN_POINT('Ctrl Pts',(-11.6709133432986,-22.3382499035618,
12.));
#182041=CARTESIAN_POINT('Ctrl Pts',(-11.6497440449858,-22.3228878043976,
12.));
#182042=CARTESIAN_POINT('Ctrl Pts',(-11.6286728270011,-22.3075217249049,
12.));
#182043=CARTESIAN_POINT('Ctrl Pts',(-11.6076999192359,-22.2921521480357,
12.));
#182044=CARTESIAN_POINT('Ctrl Pts',(-11.5868255525189,-22.2767795614349,
12.));
#182045=CARTESIAN_POINT('Ctrl Pts',(-11.5660499582403,-22.2614044566898,
12.));
#182046=CARTESIAN_POINT('Ctrl Pts',(-11.545373367912,-22.2460273284653,
12.));
#182047=CARTESIAN_POINT('Ctrl Pts',(-11.5247960128476,-22.2306486738899,
12.));
#182048=CARTESIAN_POINT('Ctrl Pts',(-11.504318124424,-22.215268993102,12.));
#182049=CARTESIAN_POINT('Ctrl Pts',(-11.4839399342589,-22.1998887896435,
12.));
#182050=CARTESIAN_POINT('Ctrl Pts',(-11.463661674411,-22.1845085709169,
12.));
#182051=CARTESIAN_POINT('Ctrl Pts',(-11.443483577557,-22.1691288486096,
12.));
#182052=CARTESIAN_POINT('Ctrl Pts',(-11.4234058771742,-22.1537501391486,
12.));
#182053=CARTESIAN_POINT('Ctrl Pts',(-11.4034288076909,-22.1383729640963,
12.));
#182054=CARTESIAN_POINT('Ctrl Pts',(-11.3835526044256,-22.1229978500185,
12.));
#182055=CARTESIAN_POINT('Ctrl Pts',(-11.3637775035367,-22.1076253283978,
12.));
#182056=CARTESIAN_POINT('Ctrl Pts',(-11.3441037419553,-22.0922559355293,
12.));
#182057=CARTESIAN_POINT('Ctrl Pts',(-11.3245315573168,-22.0768902124267,
12.));
#182058=CARTESIAN_POINT('Ctrl Pts',(-11.3050611878771,-22.0615287047179,
12.));
#182059=CARTESIAN_POINT('Ctrl Pts',(-11.2856928724374,-22.046171962566,
12.));
#182060=CARTESIAN_POINT('Ctrl Pts',(-11.2664268504207,-22.0308205408351,
12.));
#182061=CARTESIAN_POINT('Ctrl Pts',(-11.2472633619276,-22.0154749992364,
12.));
#182062=CARTESIAN_POINT('Ctrl Pts',(-11.2282026477897,-22.0001359024839,
12.));
#182063=CARTESIAN_POINT('Ctrl Pts',(-11.2092449496125,-21.9848038204439,
12.));
#182064=CARTESIAN_POINT('Ctrl Pts',(-11.190390509811,-21.9694793282913,
12.));
#182065=CARTESIAN_POINT('Ctrl Pts',(-11.1716395716375,-21.9541630066504,
12.));
#182066=CARTESIAN_POINT('Ctrl Pts',(-11.1529923792002,-21.9388554416437,
12.));
#182067=CARTESIAN_POINT('Ctrl Pts',(-11.134449177474,-21.9235572249518,
12.));
#182068=CARTESIAN_POINT('Ctrl Pts',(-11.1160102123024,-21.9082689538687,
12.));
#182069=CARTESIAN_POINT('Ctrl Pts',(-11.0976757303944,-21.8929912313608,
12.));
#182070=CARTESIAN_POINT('Ctrl Pts',(-11.0794459793058,-21.8777246661191,
12.));
#182071=CARTESIAN_POINT('Ctrl Pts',(-11.0613212074364,-21.8624698726319,
12.));
#182072=CARTESIAN_POINT('Ctrl Pts',(-11.0433016640808,-21.8472274713103,
12.));
#182073=CARTESIAN_POINT('Ctrl Pts',(-11.0253875994598,-21.8319980886033,
12.));
#182074=CARTESIAN_POINT('Ctrl Pts',(-11.0075792647477,-21.8167823571168,
12.));
#182075=CARTESIAN_POINT('Ctrl Pts',(-10.9898769120913,-21.8015809157302,
12.));
#182076=CARTESIAN_POINT('Ctrl Pts',(-10.9722807946157,-21.7863944097143,
12.));
#182077=CARTESIAN_POINT('Ctrl Pts',(-10.9547911664457,-21.7712234908468,
12.));
#182078=CARTESIAN_POINT('Ctrl Pts',(-10.9374082827446,-21.7560688175252,
12.));
#182079=CARTESIAN_POINT('Ctrl Pts',(-10.9201323997386,-21.74093105488,12.));
#182080=CARTESIAN_POINT('Ctrl Pts',(-10.9029637747341,-21.7258108748874,
12.));
#182081=CARTESIAN_POINT('Ctrl Pts',(-10.8859026661292,-21.7107089564822,
12.));
#182082=CARTESIAN_POINT('Ctrl Pts',(-10.8689493334093,-21.6956259856667,
12.));
#182083=CARTESIAN_POINT('Ctrl Pts',(-10.8521040371832,-21.6805626556461,
12.));
#182084=CARTESIAN_POINT('Ctrl Pts',(-10.835367039227,-21.6655196669727,
12.));
#182085=CARTESIAN_POINT('Ctrl Pts',(-10.8187386025135,-21.6504977276864,
12.));
#182086=CARTESIAN_POINT('Ctrl Pts',(-10.802218991237,-21.6354975534557,
12.));
#182087=CARTESIAN_POINT('Ctrl Pts',(-10.7858084708262,-21.6205198677176,
12.));
#182088=CARTESIAN_POINT('Ctrl Pts',(-10.7695073079554,-21.6055654018179,
12.));
#182089=CARTESIAN_POINT('Ctrl Pts',(-10.7533157705943,-21.5906348951745,
12.));
#182090=CARTESIAN_POINT('Ctrl Pts',(-10.7372341280468,-21.5757290954372,
12.));
#182091=CARTESIAN_POINT('Ctrl Pts',(-10.7212626509816,-21.5608487586467,
12.));
#182092=CARTESIAN_POINT('Ctrl Pts',(-10.7054016114571,-21.5459946493955,
12.));
#182093=CARTESIAN_POINT('Ctrl Pts',(-10.689651282929,-21.531167540981,12.));
#182094=CARTESIAN_POINT('Ctrl Pts',(-10.6740119402835,-21.5163682155805,
12.));
#182095=CARTESIAN_POINT('Ctrl Pts',(-10.6584838598941,-21.5015974644454,
12.));
#182096=CARTESIAN_POINT('Ctrl Pts',(-10.6430673196609,-21.4868560880893,
12.));
#182097=CARTESIAN_POINT('Ctrl Pts',(-10.6277625990457,-21.4721448964766,
12.));
#182098=CARTESIAN_POINT('Ctrl Pts',(-10.612569979096,-21.4574647092093,
12.));
#182099=CARTESIAN_POINT('Ctrl Pts',(-10.597489742462,-21.4428163557137,
12.));
#182100=CARTESIAN_POINT('Ctrl Pts',(-10.582522173457,-21.4282006754624,
12.));
#182101=CARTESIAN_POINT('Ctrl Pts',(-10.5676675581106,-21.4136185181974,
12.));
#182102=CARTESIAN_POINT('Ctrl Pts',(-10.5529261842107,-21.3990707441495,
12.));
#182103=CARTESIAN_POINT('Ctrl Pts',(-10.5382983413422,-21.3845582242604,
12.));
#182104=CARTESIAN_POINT('Ctrl Pts',(-10.523784320906,-21.3700818403942,
12.));
#182105=CARTESIAN_POINT('Ctrl Pts',(-10.509384416169,-21.3556424855822,
12.));
#182106=CARTESIAN_POINT('Ctrl Pts',(-10.4950989223341,-21.3412410642912,
12.));
#182107=CARTESIAN_POINT('Ctrl Pts',(-10.4809281365933,-21.3268784926823,
12.));
#182108=CARTESIAN_POINT('Ctrl Pts',(-10.4668723581768,-21.312555698873,
12.));
#182109=CARTESIAN_POINT('Ctrl Pts',(-10.452931888387,-21.2982736231924,
12.));
#182110=CARTESIAN_POINT('Ctrl Pts',(-10.4391070306385,-21.2840332184471,
12.));
#182111=CARTESIAN_POINT('Ctrl Pts',(-10.4253980905394,-21.2698354502391,
12.));
#182112=CARTESIAN_POINT('Ctrl Pts',(-10.4118053759584,-21.2556812972741,
12.));
#182113=CARTESIAN_POINT('Ctrl Pts',(-10.3983291970846,-21.2415717516713,
12.));
#182114=CARTESIAN_POINT('Ctrl Pts',(-10.384969866479,-21.2275078192708,
12.));
#182115=CARTESIAN_POINT('Ctrl Pts',(-10.3717276991137,-21.2134905199359,
12.));
#182116=CARTESIAN_POINT('Ctrl Pts',(-10.3586030124595,-21.1995208879205,
12.));
#182117=CARTESIAN_POINT('Ctrl Pts',(-10.3455961265706,-21.1855999722427,
12.));
#182118=CARTESIAN_POINT('Ctrl Pts',(-10.3327073641574,-21.1717288370512,
12.));
#182119=CARTESIAN_POINT('Ctrl Pts',(-10.3199370506541,-21.1579085619959,
12.));
#182120=CARTESIAN_POINT('Ctrl Pts',(-10.307285514268,-21.1441402425831,
12.));
#182121=CARTESIAN_POINT('Ctrl Pts',(-10.2947530860714,-21.130424990599,
12.));
#182122=CARTESIAN_POINT('Ctrl Pts',(-10.2823401001067,-21.1167639345623,
12.));
#182123=CARTESIAN_POINT('Ctrl Pts',(-10.2700468934743,-21.1031582201625,
12.));
#182124=CARTESIAN_POINT('Ctrl Pts',(-10.2578738064183,-21.0896090107066,
12.));
#182125=CARTESIAN_POINT('Ctrl Pts',(-10.2458211823915,-21.0761174875448,
12.));
#182126=CARTESIAN_POINT('Ctrl Pts',(-10.233889368157,-21.0626848505665,
12.));
#182127=CARTESIAN_POINT('Ctrl Pts',(-10.2220787139157,-21.0493123187483,
12.));
#182128=CARTESIAN_POINT('Ctrl Pts',(-10.2103895734124,-21.0360011306814,
12.));
#182129=CARTESIAN_POINT('Ctrl Pts',(-10.1988223040425,-21.0227525451107,
12.));
#182130=CARTESIAN_POINT('Ctrl Pts',(-10.1873772669358,-21.0095678414486,
12.));
#182131=CARTESIAN_POINT('Ctrl Pts',(-10.1760548270765,-20.9964483203685,
12.));
#182132=CARTESIAN_POINT('Ctrl Pts',(-10.1648553534567,-20.9833953044736,
12.));
#182133=CARTESIAN_POINT('Ctrl Pts',(-10.1537792192065,-20.970410138937,
12.));
#182134=CARTESIAN_POINT('Ctrl Pts',(-10.1428268017257,-20.9574941921591,
12.));
#182135=CARTESIAN_POINT('Ctrl Pts',(-10.1319984827909,-20.944648856393,
12.));
#182136=CARTESIAN_POINT('Ctrl Pts',(-10.1212946487057,-20.931875548473,
12.));
#182137=CARTESIAN_POINT('Ctrl Pts',(-10.1107156904836,-20.9191757106266,
12.));
#182138=CARTESIAN_POINT('Ctrl Pts',(-10.1002620040076,-20.9065508112556,
12.));
#182139=CARTESIAN_POINT('Ctrl Pts',(-10.0899339901916,-20.8940023457371,
12.));
#182140=CARTESIAN_POINT('Ctrl Pts',(-10.0797320551154,-20.8815318371844,
12.));
#182141=CARTESIAN_POINT('Ctrl Pts',(-10.0696566102219,-20.8691408373705,
12.));
#182142=CARTESIAN_POINT('Ctrl Pts',(-10.0597080725375,-20.856830927732,
12.));
#182143=CARTESIAN_POINT('Ctrl Pts',(-10.0498868648733,-20.8446037203402,
12.));
#182144=CARTESIAN_POINT('Ctrl Pts',(-10.0401934160234,-20.8324608588906,
12.));
#182145=CARTESIAN_POINT('Ctrl Pts',(-10.0306281609435,-20.8204040196599,
12.));
#182146=CARTESIAN_POINT('Ctrl Pts',(-10.0211915410095,-20.8084349126885,
12.));
#182147=CARTESIAN_POINT('Ctrl Pts',(-10.0118840042786,-20.7965552829907,
12.));
#182148=CARTESIAN_POINT('Ctrl Pts',(-10.0027060057389,-20.7847669117568,
12.));
#182149=CARTESIAN_POINT('Ctrl Pts',(-9.99365800754638,-20.7730716175417,
12.));
#182150=CARTESIAN_POINT('Ctrl Pts',(-9.98474047926846,-20.7614712574989,
12.));
#182151=CARTESIAN_POINT('Ctrl Pts',(-9.97595389823461,-20.7499677289625,
12.));
#182152=CARTESIAN_POINT('Ctrl Pts',(-9.96729874986199,-20.7385629709795,
12.));
#182153=CARTESIAN_POINT('Ctrl Pts',(-9.95877552798403,-20.7272589658752,
12.));
#182154=CARTESIAN_POINT('Ctrl Pts',(-9.95038473514962,-20.716057740758,
12.));
#182155=CARTESIAN_POINT('Ctrl Pts',(-9.94212688298251,-20.7049613692237,
12.));
#182156=CARTESIAN_POINT('Ctrl Pts',(-9.93400249259737,-20.6939719732485,
12.));
#182157=CARTESIAN_POINT('Ctrl Pts',(-9.92601209498751,-20.6830917250255,
12.));
#182158=CARTESIAN_POINT('Ctrl Pts',(-9.91815623141285,-20.6723228488261,
12.));
#182159=CARTESIAN_POINT('Ctrl Pts',(-9.91043545377005,-20.6616676228315,
12.));
#182160=CARTESIAN_POINT('Ctrl Pts',(-9.90285032516696,-20.6511283817415,
12.));
#182161=CARTESIAN_POINT('Ctrl Pts',(-9.89540142049124,-20.6407075193977,
12.));
#182162=CARTESIAN_POINT('Ctrl Pts',(-9.88808932697305,-20.6304074914086,
12.));
#182163=CARTESIAN_POINT('Ctrl Pts',(-9.88091464472669,-20.6202308177472,
12.));
#182164=CARTESIAN_POINT('Ctrl Pts',(-9.87387798732944,-20.6101800854491,
12.));
#182165=CARTESIAN_POINT('Ctrl Pts',(-9.86697998242612,-20.6002579513696,
12.));
#182166=CARTESIAN_POINT('Ctrl Pts',(-9.8602212723275,-20.5904671449754,
12.));
#182167=CARTESIAN_POINT('Ctrl Pts',(-9.85360251457004,-20.580810471002,
12.));
#182168=CARTESIAN_POINT('Ctrl Pts',(-9.84712438256308,-20.5712908125145,
12.));
#182169=CARTESIAN_POINT('Ctrl Pts',(-9.84078756677589,-20.5619111362406,
12.));
#182170=CARTESIAN_POINT('Ctrl Pts',(-9.83459277585321,-20.5526744976461,
12.));
#182171=CARTESIAN_POINT('Ctrl Pts',(-9.82854073773858,-20.5435840460717,
12.));
#182172=CARTESIAN_POINT('Ctrl Pts',(-9.82263220080328,-20.534643029951,
12.));
#182173=CARTESIAN_POINT('Ctrl Pts',(-9.81686793455918,-20.5258548000625,
12.));
#182174=CARTESIAN_POINT('Ctrl Pts',(-9.81124873025278,-20.5172228122839,
12.));
#182175=CARTESIAN_POINT('Ctrl Pts',(-9.80577540161103,-20.5087506310507,
12.));
#182176=CARTESIAN_POINT('Ctrl Pts',(-9.80044878520968,-20.500441931211,
12.));
#182177=CARTESIAN_POINT('Ctrl Pts',(-9.79526974288344,-20.4923005087945,
12.));
#182178=CARTESIAN_POINT('Ctrl Pts',(-9.7902391649866,-20.4843302955329,
12.));
#182179=CARTESIAN_POINT('Ctrl Pts',(-9.78535797314162,-20.4765353711585,
12.));
#182180=CARTESIAN_POINT('Ctrl Pts',(-9.78062712373313,-20.4689199790668,
12.));
#182181=CARTESIAN_POINT('Ctrl Pts',(-9.77604760815523,-20.4614885274973,
12.));
#182182=CARTESIAN_POINT('Ctrl Pts',(-9.7716204510407,-20.4542455817527,
12.));
#182183=CARTESIAN_POINT('Ctrl Pts',(-9.76734670980897,-20.447195862298,
12.));
#182184=CARTESIAN_POINT('Ctrl Pts',(-9.76322747195502,-20.4403442329401,
12.));
#182185=CARTESIAN_POINT('Ctrl Pts',(-9.7592638628993,-20.4336957355474,
12.));
#182186=CARTESIAN_POINT('Ctrl Pts',(-9.75545705902416,-20.4272556476629,
12.));
#182187=CARTESIAN_POINT('Ctrl Pts',(-9.75180829786433,-20.4210295275818,
12.));
#182188=CARTESIAN_POINT('Ctrl Pts',(-9.74831889242175,-20.4150232777393,
12.));
#182189=CARTESIAN_POINT('Ctrl Pts',(-9.74499021838537,-20.4092430879861,
12.));
#182190=CARTESIAN_POINT('Ctrl Pts',(-9.74182369656273,-20.4036953576549,
12.));
#182191=CARTESIAN_POINT('Ctrl Pts',(-9.73882077613206,-20.3983866213331,
12.));
#182192=CARTESIAN_POINT('Ctrl Pts',(-9.7359829201425,-20.3933234845646,
12.));
#182193=CARTESIAN_POINT('Ctrl Pts',(-9.73331167102812,-20.3885129129912,
12.));
#182194=CARTESIAN_POINT('Ctrl Pts',(-9.73080870123726,-20.3839624556742,
12.));
#182195=CARTESIAN_POINT('Ctrl Pts',(-9.72847589116533,-20.3796805893304,
12.));
#182196=CARTESIAN_POINT('Ctrl Pts',(-9.72631531732871,-20.3756766651952,
12.));
#182197=CARTESIAN_POINT('Ctrl Pts',(-9.72432910043193,-20.371960235676,
12.));
#182198=CARTESIAN_POINT('Ctrl Pts',(-9.72251930722504,-20.3685406190576,
12.));
#182199=CARTESIAN_POINT('Ctrl Pts',(-9.72088778381102,-20.3654261611055,
12.));
#182200=CARTESIAN_POINT('Ctrl Pts',(-9.71943648548115,-20.362625691398,
12.));
#182201=CARTESIAN_POINT('Ctrl Pts',(-9.71816778327999,-20.3601498764344,
12.));
#182202=CARTESIAN_POINT('Ctrl Pts',(-9.71708493723062,-20.3580133103357,
12.));
#182203=CARTESIAN_POINT('Ctrl Pts',(-9.71619192554147,-20.3562337557875,
12.));
#182204=CARTESIAN_POINT('Ctrl Pts',(-9.71549257088175,-20.3548282742361,
12.));
#182205=CARTESIAN_POINT('Ctrl Pts',(-9.71498978052101,-20.3538098605706,
12.));
#182206=CARTESIAN_POINT('Ctrl Pts',(-9.71474590350792,-20.3533097561886,
12.));
#182207=CARTESIAN_POINT('Ctrl Pts',(-9.71465227853122,-20.3531126095522,
12.));
#182208=CARTESIAN_POINT('Ctrl Pts',(-9.71462954053074,-20.353060251684,
12.));
#182209=CARTESIAN_POINT('Ctrl Pts',(-9.71462809124917,-20.353053841303,
12.));
#182210=CARTESIAN_POINT('',(-9.47413589477549,-19.84920021178,12.));
#182211=CARTESIAN_POINT('',(-4.63060338698782,-9.70154690100589,12.));
#182212=CARTESIAN_POINT('',(-8.81783521984851,-19.6085639972844,12.));
#182213=CARTESIAN_POINT('Origin',(-9.02290115519382,-20.0645771135003,12.));
#182214=CARTESIAN_POINT('',(-7.63019749246979,-20.1004996511507,12.));
#182215=CARTESIAN_POINT('Origin',(-3.26562511982935E-13,-7.08841632778409E-13,
12.));
#182216=CARTESIAN_POINT('',(-7.33627833380047,-20.7347298079577,12.));
#182217=CARTESIAN_POINT('Origin',(-7.80764394578304,-20.56795313141,12.));
#182218=CARTESIAN_POINT('',(-7.52250298901266,-21.2610617890679,12.));
#182219=CARTESIAN_POINT('',(-3.76125149450632,-10.6305308945339,12.));
#182220=CARTESIAN_POINT('',(-7.36589684767345,-24.9347862158358,12.));
#182221=CARTESIAN_POINT('Ctrl Pts',(-7.52250298901266,-21.2610617890679,
12.));
#182222=CARTESIAN_POINT('Ctrl Pts',(-7.52250649703992,-21.2610673466883,
12.));
#182223=CARTESIAN_POINT('Ctrl Pts',(-7.52252744144958,-21.261120447486,
12.));
#182224=CARTESIAN_POINT('Ctrl Pts',(-7.52260064231736,-21.2613260540651,
12.));
#182225=CARTESIAN_POINT('Ctrl Pts',(-7.52278182242728,-21.261852128355,
12.));
#182226=CARTESIAN_POINT('Ctrl Pts',(-7.52314642316203,-21.262927782038,
12.));
#182227=CARTESIAN_POINT('Ctrl Pts',(-7.52364573027521,-21.2644161259965,
12.));
#182228=CARTESIAN_POINT('Ctrl Pts',(-7.52427261074264,-21.266305915706,
12.));
#182229=CARTESIAN_POINT('Ctrl Pts',(-7.52501770333522,-21.2685823838672,
12.));
#182230=CARTESIAN_POINT('Ctrl Pts',(-7.52587126095544,-21.2712301573465,
12.));
#182231=CARTESIAN_POINT('Ctrl Pts',(-7.52682526918561,-21.2742366113578,
12.));
#182232=CARTESIAN_POINT('Ctrl Pts',(-7.52787386225344,-21.2775925269651,
12.));
#182233=CARTESIAN_POINT('Ctrl Pts',(-7.52901217930407,-21.2812902781143,
12.));
#182234=CARTESIAN_POINT('Ctrl Pts',(-7.53023562438221,-21.2853226580658,
12.));
#182235=CARTESIAN_POINT('Ctrl Pts',(-7.53153906987847,-21.2896816163843,
12.));
#182236=CARTESIAN_POINT('Ctrl Pts',(-7.53291726078527,-21.2943588989331,
12.));
#182237=CARTESIAN_POINT('Ctrl Pts',(-7.53436505309949,-21.2993464250717,
12.));
#182238=CARTESIAN_POINT('Ctrl Pts',(-7.53587778251743,-21.3046368712156,
12.));
#182239=CARTESIAN_POINT('Ctrl Pts',(-7.5374512936462,-21.3102237167729,
12.));
#182240=CARTESIAN_POINT('Ctrl Pts',(-7.53908175169899,-21.3161009456256,
12.));
#182241=CARTESIAN_POINT('Ctrl Pts',(-7.5407655203828,-21.3222628524165,
12.));
#182242=CARTESIAN_POINT('Ctrl Pts',(-7.54249900377032,-21.328703791771,
12.));
#182243=CARTESIAN_POINT('Ctrl Pts',(-7.54427868151269,-21.3354182340149,
12.));
#182244=CARTESIAN_POINT('Ctrl Pts',(-7.54610114948351,-21.3424008295038,
12.));
#182245=CARTESIAN_POINT('Ctrl Pts',(-7.54796316246327,-21.349646476153,
12.));
#182246=CARTESIAN_POINT('Ctrl Pts',(-7.54986166521307,-21.3571503685853,
12.));
#182247=CARTESIAN_POINT('Ctrl Pts',(-7.55179375777442,-21.3649079431864,
12.));
#182248=CARTESIAN_POINT('Ctrl Pts',(-7.55375667080032,-21.3729148390244,
12.));
#182249=CARTESIAN_POINT('Ctrl Pts',(-7.55574773403508,-21.3811668478933,
12.));
#182250=CARTESIAN_POINT('Ctrl Pts',(-7.55776435731422,-21.3896598842119,
12.));
#182251=CARTESIAN_POINT('Ctrl Pts',(-7.55980403700615,-21.3983899952988,
12.));
#182252=CARTESIAN_POINT('Ctrl Pts',(-7.56186435703622,-21.4073533630364,
12.));
#182253=CARTESIAN_POINT('Ctrl Pts',(-7.56394299313683,-21.4165463106252,
12.));
#182254=CARTESIAN_POINT('Ctrl Pts',(-7.56603771218706,-21.4259653015732,
12.));
#182255=CARTESIAN_POINT('Ctrl Pts',(-7.56814636360842,-21.435606926151,
12.));
#182256=CARTESIAN_POINT('Ctrl Pts',(-7.5702668726117,-21.445467890751,12.));
#182257=CARTESIAN_POINT('Ctrl Pts',(-7.57239723223521,-21.4555450053147,
12.));
#182258=CARTESIAN_POINT('Ctrl Pts',(-7.57453549743435,-21.4658351740135,
12.));
#182259=CARTESIAN_POINT('Ctrl Pts',(-7.57667978403003,-21.4763353936766,
12.));
#182260=CARTESIAN_POINT('Ctrl Pts',(-7.57882826679131,-21.4870427508193,
12.));
#182261=CARTESIAN_POINT('Ctrl Pts',(-7.5809791779073,-21.4979544192739,
12.));
#182262=CARTESIAN_POINT('Ctrl Pts',(-7.58313080519159,-21.5090676573866,
12.));
#182263=CARTESIAN_POINT('Ctrl Pts',(-7.58528148919114,-21.5203798035294,
12.));
#182264=CARTESIAN_POINT('Ctrl Pts',(-7.58742962034834,-21.5318882716735,
12.));
#182265=CARTESIAN_POINT('Ctrl Pts',(-7.58957363620026,-21.5435905470113,
12.));
#182266=CARTESIAN_POINT('Ctrl Pts',(-7.59171201844793,-21.5554841813465,
12.));
#182267=CARTESIAN_POINT('Ctrl Pts',(-7.5938432912493,-21.5675667904728,
12.));
#182268=CARTESIAN_POINT('Ctrl Pts',(-7.59596601973589,-21.5798360518978,
12.));
#182269=CARTESIAN_POINT('Ctrl Pts',(-7.59807880846193,-21.5922897024466,
12.));
#182270=CARTESIAN_POINT('Ctrl Pts',(-7.60018029988238,-21.6049255358842,
12.));
#182271=CARTESIAN_POINT('Ctrl Pts',(-7.60226917285432,-21.6177414005991,
12.));
#182272=CARTESIAN_POINT('Ctrl Pts',(-7.604344141183,-21.6307351973823,12.));
#182273=CARTESIAN_POINT('Ctrl Pts',(-7.60640395216359,-21.6439048771743,
12.));
#182274=CARTESIAN_POINT('Ctrl Pts',(-7.60844738512872,-21.6572484388079,
12.));
#182275=CARTESIAN_POINT('Ctrl Pts',(-7.6104732500095,-21.6707639267573,
12.));
#182276=CARTESIAN_POINT('Ctrl Pts',(-7.61248038630265,-21.6844494295813,
12.));
#182277=CARTESIAN_POINT('Ctrl Pts',(-7.61446766202787,-21.6983030783321,
12.));
#182278=CARTESIAN_POINT('Ctrl Pts',(-7.61643397270425,-21.7123230449835,
12.));
#182279=CARTESIAN_POINT('Ctrl Pts',(-7.61837824030542,-21.7265075407977,
12.));
#182280=CARTESIAN_POINT('Ctrl Pts',(-7.62029941230855,-21.7408548148657,
12.));
#182281=CARTESIAN_POINT('Ctrl Pts',(-7.62219646084226,-21.7553631528329,
12.));
#182282=CARTESIAN_POINT('Ctrl Pts',(-7.62406838181164,-21.7700308755583,
12.));
#182283=CARTESIAN_POINT('Ctrl Pts',(-7.62591419404521,-21.7848563378022,
12.));
#182284=CARTESIAN_POINT('Ctrl Pts',(-7.62773293842409,-21.7998379268583,
12.));
#182285=CARTESIAN_POINT('Ctrl Pts',(-7.62952367718151,-21.8149740615093,
12.));
#182286=CARTESIAN_POINT('Ctrl Pts',(-7.6312854932304,-21.8302631910197,
12.));
#182287=CARTESIAN_POINT('Ctrl Pts',(-7.63301748948936,-21.8457037941084,
12.));
#182288=CARTESIAN_POINT('Ctrl Pts',(-7.63471878821204,-21.8612943779086,
12.));
#182289=CARTESIAN_POINT('Ctrl Pts',(-7.63638853033368,-21.8770334769492,
12.));
#182290=CARTESIAN_POINT('Ctrl Pts',(-7.63802587492008,-21.8929196523511,
12.));
#182291=CARTESIAN_POINT('Ctrl Pts',(-7.63962999860917,-21.9089514909873,
12.));
#182292=CARTESIAN_POINT('Ctrl Pts',(-7.6412000950654,-21.9251276046546,
12.));
#182293=CARTESIAN_POINT('Ctrl Pts',(-7.64273537442707,-21.9414466292074,
12.));
#182294=CARTESIAN_POINT('Ctrl Pts',(-7.64423506279154,-21.9579072237653,
12.));
#182295=CARTESIAN_POINT('Ctrl Pts',(-7.64569840177359,-21.97450807008,12.));
#182296=CARTESIAN_POINT('Ctrl Pts',(-7.64712464805258,-21.9912478718542,
12.));
#182297=CARTESIAN_POINT('Ctrl Pts',(-7.64851307293346,-22.0081253540773,
12.));
#182298=CARTESIAN_POINT('Ctrl Pts',(-7.64986296190157,-22.0251392623209,
12.));
#182299=CARTESIAN_POINT('Ctrl Pts',(-7.65117361421347,-22.0422883621176,
12.));
#182300=CARTESIAN_POINT('Ctrl Pts',(-7.65244434253104,-22.0595714384432,
12.));
#182301=CARTESIAN_POINT('Ctrl Pts',(-7.65367447254945,-22.0769872951596,
12.));
#182302=CARTESIAN_POINT('Ctrl Pts',(-7.65486334263651,-22.094534754469,
12.));
#182303=CARTESIAN_POINT('Ctrl Pts',(-7.65601030346819,-22.1122126563327,
12.));
#182304=CARTESIAN_POINT('Ctrl Pts',(-7.65711471769407,-22.1300198579671,
12.));
#182305=CARTESIAN_POINT('Ctrl Pts',(-7.65817595963351,-22.1479552334206,
12.));
#182306=CARTESIAN_POINT('Ctrl Pts',(-7.65919341496926,-22.1660176731174,
12.));
#182307=CARTESIAN_POINT('Ctrl Pts',(-7.66016648045008,-22.1842060834092,
12.));
#182308=CARTESIAN_POINT('Ctrl Pts',(-7.66109456359292,-22.2025193860972,
12.));
#182309=CARTESIAN_POINT('Ctrl Pts',(-7.66197708240436,-22.2209565180098,
12.));
#182310=CARTESIAN_POINT('Ctrl Pts',(-7.66281346512546,-22.239516430656,
12.));
#182311=CARTESIAN_POINT('Ctrl Pts',(-7.66360314997662,-22.2581980898487,
12.));
#182312=CARTESIAN_POINT('Ctrl Pts',(-7.66434558490973,-22.2770004753332,
12.));
#182313=CARTESIAN_POINT('Ctrl Pts',(-7.66504022736263,-22.2959225803925,
12.));
#182314=CARTESIAN_POINT('Ctrl Pts',(-7.66568654402442,-22.3149634114823,
12.));
#182315=CARTESIAN_POINT('Ctrl Pts',(-7.66628401061906,-22.3341219879454,
12.));
#182316=CARTESIAN_POINT('Ctrl Pts',(-7.66683211169134,-22.3533973417013,
12.));
#182317=CARTESIAN_POINT('Ctrl Pts',(-7.66733034039887,-22.3727885169361,
12.));
#182318=CARTESIAN_POINT('Ctrl Pts',(-7.6677781983082,-22.3922945697782,
12.));
#182319=CARTESIAN_POINT('Ctrl Pts',(-7.66817519519682,-22.411914567977,
12.));
#182320=CARTESIAN_POINT('Ctrl Pts',(-7.66852084886746,-22.4316475906616,
12.));
#182321=CARTESIAN_POINT('Ctrl Pts',(-7.6688146849666,-22.4514927280862,
12.));
#182322=CARTESIAN_POINT('Ctrl Pts',(-7.66905623680836,-22.47144908137,12.));
#182323=CARTESIAN_POINT('Ctrl Pts',(-7.66924504520302,-22.4915157622308,
12.));
#182324=CARTESIAN_POINT('Ctrl Pts',(-7.66938065829083,-22.5116918927023,
12.));
#182325=CARTESIAN_POINT('Ctrl Pts',(-7.66946263138116,-22.5319766049191,
12.));
#182326=CARTESIAN_POINT('Ctrl Pts',(-7.66949052679672,-22.5523690409109,
12.));
#182327=CARTESIAN_POINT('Ctrl Pts',(-7.66946391372299,-22.5728683523828,
12.));
#182328=CARTESIAN_POINT('Ctrl Pts',(-7.66938236806241,-22.5934737004955,
12.));
#182329=CARTESIAN_POINT('Ctrl Pts',(-7.66924547229435,-22.6141842556248,
12.));
#182330=CARTESIAN_POINT('Ctrl Pts',(-7.66905281533745,-22.6349991971547,
12.));
#182331=CARTESIAN_POINT('Ctrl Pts',(-7.66880399241354,-22.6559177133133,
12.));
#182332=CARTESIAN_POINT('Ctrl Pts',(-7.66849860491763,-22.6769390009889,
12.));
#182333=CARTESIAN_POINT('Ctrl Pts',(-7.66813626029277,-22.6980622655446,
12.));
#182334=CARTESIAN_POINT('Ctrl Pts',(-7.6677165719101,-22.7192867206242,
12.));
#182335=CARTESIAN_POINT('Ctrl Pts',(-7.66723915895413,-22.7406115879508,
12.));
#182336=CARTESIAN_POINT('Ctrl Pts',(-7.66670364630273,-22.7620360971839,
12.));
#182337=CARTESIAN_POINT('Ctrl Pts',(-7.66610966441259,-22.7835594857697,
12.));
#182338=CARTESIAN_POINT('Ctrl Pts',(-7.66545684920988,-22.8051809987833,
12.));
#182339=CARTESIAN_POINT('Ctrl Pts',(-7.66474484198553,-22.8268998887678,
12.));
#182340=CARTESIAN_POINT('Ctrl Pts',(-7.66397328929805,-22.8487154155569,
12.));
#182341=CARTESIAN_POINT('Ctrl Pts',(-7.66314184287334,-22.870626846128,
12.));
#182342=CARTESIAN_POINT('Ctrl Pts',(-7.66225015950148,-22.8926334544879,
12.));
#182343=CARTESIAN_POINT('Ctrl Pts',(-7.661297900941,-22.9147345215418,12.));
#182344=CARTESIAN_POINT('Ctrl Pts',(-7.66028473382777,-22.9369293349592,
12.));
#182345=CARTESIAN_POINT('Ctrl Pts',(-7.65921032958912,-22.9592171890332,
12.));
#182346=CARTESIAN_POINT('Ctrl Pts',(-7.65807436436453,-22.9815973845301,
12.));
#182347=CARTESIAN_POINT('Ctrl Pts',(-7.6568765189133,-23.004069228582,12.));
#182348=CARTESIAN_POINT('Ctrl Pts',(-7.65561647852555,-23.0266320345792,
12.));
#182349=CARTESIAN_POINT('Ctrl Pts',(-7.65429393293955,-23.049285122053,
12.));
#182350=CARTESIAN_POINT('Ctrl Pts',(-7.65290857626357,-23.072027816555,
12.));
#182351=CARTESIAN_POINT('Ctrl Pts',(-7.65146010690465,-23.0948594495246,
12.));
#182352=CARTESIAN_POINT('Ctrl Pts',(-7.64994822749845,-23.1177793581674,
12.));
#182353=CARTESIAN_POINT('Ctrl Pts',(-7.64837264482929,-23.1407868853815,
12.));
#182354=CARTESIAN_POINT('Ctrl Pts',(-7.64673306975797,-23.1638813796691,
12.));
#182355=CARTESIAN_POINT('Ctrl Pts',(-7.64502921715483,-23.1870621950452,
12.));
#182356=CARTESIAN_POINT('Ctrl Pts',(-7.64326080583684,-23.2103286909399,
12.));
#182357=CARTESIAN_POINT('Ctrl Pts',(-7.64142755851508,-23.2336802320912,
12.));
#182358=CARTESIAN_POINT('Ctrl Pts',(-7.63952920172837,-23.2571161884487,
12.));
#182359=CARTESIAN_POINT('Ctrl Pts',(-7.63756546576375,-23.2806359350853,
12.));
#182360=CARTESIAN_POINT('Ctrl Pts',(-7.63553608458784,-23.3042388521021,
12.));
#182361=CARTESIAN_POINT('Ctrl Pts',(-7.63344079578163,-23.3279243245241,
12.));
#182362=CARTESIAN_POINT('Ctrl Pts',(-7.63127934048139,-23.3516917421973,
12.));
#182363=CARTESIAN_POINT('Ctrl Pts',(-7.62905146332598,-23.3755404996638,
12.));
#182364=CARTESIAN_POINT('Ctrl Pts',(-7.62675691240335,-23.3994699961122,
12.));
#182365=CARTESIAN_POINT('Ctrl Pts',(-7.62439543920055,-23.4234796353544,
12.));
#182366=CARTESIAN_POINT('Ctrl Pts',(-7.62196679855957,-23.4475688257854,
12.));
#182367=CARTESIAN_POINT('Ctrl Pts',(-7.61947074863978,-23.4717369803438,
12.));
#182368=CARTESIAN_POINT('Ctrl Pts',(-7.61690705088319,-23.4959835164608,
12.));
#182369=CARTESIAN_POINT('Ctrl Pts',(-7.61427546999299,-23.5203078560128,
12.));
#182370=CARTESIAN_POINT('Ctrl Pts',(-7.61157577385372,-23.5447094252028,
12.));
#182371=CARTESIAN_POINT('Ctrl Pts',(-7.608807733446,-23.5691876544243,12.));
#182372=CARTESIAN_POINT('Ctrl Pts',(-7.60597112277094,-23.5937419781244,
12.));
#182373=CARTESIAN_POINT('Ctrl Pts',(-7.60306571877806,-23.6183718346576,
12.));
#182374=CARTESIAN_POINT('Ctrl Pts',(-7.6000913013013,-23.6430766661419,
12.));
#182375=CARTESIAN_POINT('Ctrl Pts',(-7.59704765299572,-23.6678559182876,
12.));
#182376=CARTESIAN_POINT('Ctrl Pts',(-7.59393455934042,-23.6927090405067,
12.));
#182377=CARTESIAN_POINT('Ctrl Pts',(-7.59075180865327,-23.7176354860457,
12.));
#182378=CARTESIAN_POINT('Ctrl Pts',(-7.58749919210832,-23.7426347121006,
12.));
#182379=CARTESIAN_POINT('Ctrl Pts',(-7.58417650376272,-23.7677061799376,
12.));
#182380=CARTESIAN_POINT('Ctrl Pts',(-7.58078354058212,-23.7928493549908,
12.));
#182381=CARTESIAN_POINT('Ctrl Pts',(-7.57732010249066,-23.8180637069977,
12.));
#182382=CARTESIAN_POINT('Ctrl Pts',(-7.57378599219817,-23.8433487096134,
12.));
#182383=CARTESIAN_POINT('Ctrl Pts',(-7.57018101500711,-23.8687038399597,
12.));
#182384=CARTESIAN_POINT('Ctrl Pts',(-7.56650497863792,-23.8941285782003,
12.));
#182385=CARTESIAN_POINT('Ctrl Pts',(-7.56275769304773,-23.9196224070759,
12.));
#182386=CARTESIAN_POINT('Ctrl Pts',(-7.55893897027683,-23.9451848115,12.));
#182387=CARTESIAN_POINT('Ctrl Pts',(-7.55504862424812,-23.9708152779884,
12.));
#182388=CARTESIAN_POINT('Ctrl Pts',(-7.55108647097441,-23.9965132953185,
12.));
#182389=CARTESIAN_POINT('Ctrl Pts',(-7.5470523288591,-24.022278355453,12.));
#182390=CARTESIAN_POINT('Ctrl Pts',(-7.54294601896145,-24.0481099543353,
12.));
#182391=CARTESIAN_POINT('Ctrl Pts',(-7.53876736531014,-24.0740075927985,
12.));
#182392=CARTESIAN_POINT('Ctrl Pts',(-7.53451619514649,-24.0999707772642,
12.));
#182393=CARTESIAN_POINT('Ctrl Pts',(-7.53019233935502,-24.1259990209207,
12.));
#182394=CARTESIAN_POINT('Ctrl Pts',(-7.52579563201424,-24.1520918425364,
12.));
#182395=CARTESIAN_POINT('Ctrl Pts',(-7.52132590953802,-24.1782487641594,
12.));
#182396=CARTESIAN_POINT('Ctrl Pts',(-7.51678300997949,-24.2044693092349,
12.));
#182397=CARTESIAN_POINT('Ctrl Pts',(-7.51216677222181,-24.2307530003887,
12.));
#182398=CARTESIAN_POINT('Ctrl Pts',(-7.50747703535134,-24.2570993577034,
12.));
#182399=CARTESIAN_POINT('Ctrl Pts',(-7.50271363765152,-24.2835078958973,
12.));
#182400=CARTESIAN_POINT('Ctrl Pts',(-7.49787641695439,-24.3099781253355,
12.));
#182401=CARTESIAN_POINT('Ctrl Pts',(-7.49296521252421,-24.3365095573685,
12.));
#182402=CARTESIAN_POINT('Ctrl Pts',(-7.48797986651909,-24.3631017084524,
12.));
#182403=CARTESIAN_POINT('Ctrl Pts',(-7.48292022569301,-24.3897541049254,
12.));
#182404=CARTESIAN_POINT('Ctrl Pts',(-7.47778614286565,-24.4164662871163,
12.));
#182405=CARTESIAN_POINT('Ctrl Pts',(-7.47257747883246,-24.443237814649,
12.));
#182406=CARTESIAN_POINT('Ctrl Pts',(-7.46729410308787,-24.4700682684524,
12.));
#182407=CARTESIAN_POINT('Ctrl Pts',(-7.46193588961464,-24.4969572391483,
12.));
#182408=CARTESIAN_POINT('Ctrl Pts',(-7.45650271335862,-24.5239043173072,
12.));
#182409=CARTESIAN_POINT('Ctrl Pts',(-7.4509944465116,-24.5509090831559,
12.));
#182410=CARTESIAN_POINT('Ctrl Pts',(-7.44541095473135,-24.577971096086,
12.));
#182411=CARTESIAN_POINT('Ctrl Pts',(-7.43975209375504,-24.6050898852368,
12.));
#182412=CARTESIAN_POINT('Ctrl Pts',(-7.43401770489524,-24.6322649369517,
12.));
#182413=CARTESIAN_POINT('Ctrl Pts',(-7.42820762159126,-24.6594957128756,
12.));
#182414=CARTESIAN_POINT('Ctrl Pts',(-7.42232167766266,-24.6867816727192,
12.));
#182415=CARTESIAN_POINT('Ctrl Pts',(-7.41635971481674,-24.7141222950051,
12.));
#182416=CARTESIAN_POINT('Ctrl Pts',(-7.41032159082382,-24.7415170994784,
12.));
#182417=CARTESIAN_POINT('Ctrl Pts',(-7.40420718661603,-24.7689656668983,
12.));
#182418=CARTESIAN_POINT('Ctrl Pts',(-7.39801641583013,-24.7964676646431,
12.));
#182419=CARTESIAN_POINT('Ctrl Pts',(-7.39174922585809,-24.8240228520893,
12.));
#182420=CARTESIAN_POINT('Ctrl Pts',(-7.38540558903621,-24.8516310625176,
12.));
#182421=CARTESIAN_POINT('Ctrl Pts',(-7.3789854964027,-24.8792921911115,
12.));
#182422=CARTESIAN_POINT('Ctrl Pts',(-7.37378825961676,-24.901463382605,
12.));
#182423=CARTESIAN_POINT('Ctrl Pts',(-7.36985593120091,-24.9181155530543,
12.));
#182424=CARTESIAN_POINT('Ctrl Pts',(-7.36721909028843,-24.9292275670674,
12.));
#182425=CARTESIAN_POINT('Ctrl Pts',(-7.36589684767345,-24.9347862158358,
12.));
#182426=CARTESIAN_POINT('',(-6.088339316177,-25.2771067246846,12.));
#182427=CARTESIAN_POINT('Origin',(0.,0.,12.));
#182428=CARTESIAN_POINT('',(-4.11585220600463,-22.1738711152697,12.));
#182429=CARTESIAN_POINT('Ctrl Pts',(-6.088339316177,-25.2771067246846,12.));
#182430=CARTESIAN_POINT('Ctrl Pts',(-6.08441489609794,-25.2729539149517,
12.));
#182431=CARTESIAN_POINT('Ctrl Pts',(-6.07657531787491,-25.2646490489922,
12.));
#182432=CARTESIAN_POINT('Ctrl Pts',(-6.06484373634547,-25.2521940105705,
12.));
#182433=CARTESIAN_POINT('Ctrl Pts',(-6.04925720151219,-25.2355918139032,
12.));
#182434=CARTESIAN_POINT('Ctrl Pts',(-6.02986667389998,-25.21484662016,12.));
#182435=CARTESIAN_POINT('Ctrl Pts',(-6.01056881804614,-25.1941090269819,
12.));
#182436=CARTESIAN_POINT('Ctrl Pts',(-5.99136367859755,-25.1733791296259,
12.));
#182437=CARTESIAN_POINT('Ctrl Pts',(-5.97225131495618,-25.1526570863092,
12.));
#182438=CARTESIAN_POINT('Ctrl Pts',(-5.95323180187379,-25.1319431317237,
12.));
#182439=CARTESIAN_POINT('Ctrl Pts',(-5.93430523086836,-25.1112375971106,
12.));
#182440=CARTESIAN_POINT('Ctrl Pts',(-5.91547170844448,-25.0905409050773,
12.));
#182441=CARTESIAN_POINT('Ctrl Pts',(-5.89673135155515,-25.0698535426514,
12.));
#182442=CARTESIAN_POINT('Ctrl Pts',(-5.87808428385367,-25.049176040591,
12.));
#182443=CARTESIAN_POINT('Ctrl Pts',(-5.85953063156827,-25.0285089498899,
12.));
#182444=CARTESIAN_POINT('Ctrl Pts',(-5.84107051963072,-25.0078528200564,
12.));
#182445=CARTESIAN_POINT('Ctrl Pts',(-5.822704067442,-24.9872081752734,12.));
#182446=CARTESIAN_POINT('Ctrl Pts',(-5.80443138549727,-24.9665754954496,
12.));
#182447=CARTESIAN_POINT('Ctrl Pts',(-5.78625257775682,-24.945955229334,
12.));
#182448=CARTESIAN_POINT('Ctrl Pts',(-5.76816774342221,-24.9253478043656,
12.));
#182449=CARTESIAN_POINT('Ctrl Pts',(-5.75017697890805,-24.904753637648,
12.));
#182450=CARTESIAN_POINT('Ctrl Pts',(-5.73228037976928,-24.884173146722,
12.));
#182451=CARTESIAN_POINT('Ctrl Pts',(-5.71447804252028,-24.8636067597669,
12.));
#182452=CARTESIAN_POINT('Ctrl Pts',(-5.69677006679445,-24.8430549277621,
12.));
#182453=CARTESIAN_POINT('Ctrl Pts',(-5.67915655496543,-24.8225181223845,
12.));
#182454=CARTESIAN_POINT('Ctrl Pts',(-5.66163761114922,-24.8019968304605,
12.));
#182455=CARTESIAN_POINT('Ctrl Pts',(-5.64421334042262,-24.781491549672,
12.));
#182456=CARTESIAN_POINT('Ctrl Pts',(-5.62688384790924,-24.7610027835697,
12.));
#182457=CARTESIAN_POINT('Ctrl Pts',(-5.60964923798492,-24.7405310372739,
12.));
#182458=CARTESIAN_POINT('Ctrl Pts',(-5.59250961323988,-24.7200768119088,
12.));
#182459=CARTESIAN_POINT('Ctrl Pts',(-5.57546507427756,-24.6996406035517,
12.));
#182460=CARTESIAN_POINT('Ctrl Pts',(-5.55851572025377,-24.6792229061794,
12.));
#182461=CARTESIAN_POINT('Ctrl Pts',(-5.54166164919584,-24.6588242134738,
12.));
#182462=CARTESIAN_POINT('Ctrl Pts',(-5.52490295840993,-24.6384450211467,
12.));
#182463=CARTESIAN_POINT('Ctrl Pts',(-5.50823974481963,-24.6180858289179,
12.));
#182464=CARTESIAN_POINT('Ctrl Pts',(-5.49167210537248,-24.5977471429364,
12.));
#182465=CARTESIAN_POINT('Ctrl Pts',(-5.4752001372442,-24.5774294770329,
12.));
#182466=CARTESIAN_POINT('Ctrl Pts',(-5.45882393762262,-24.5571333514842,
12.));
#182467=CARTESIAN_POINT('Ctrl Pts',(-5.44254360356881,-24.5368592922863,
12.));
#182468=CARTESIAN_POINT('Ctrl Pts',(-5.4263592318342,-24.5166078302108,
12.));
#182469=CARTESIAN_POINT('Ctrl Pts',(-5.41027091869242,-24.496379499983,
12.));
#182470=CARTESIAN_POINT('Ctrl Pts',(-5.39427875973825,-24.4761748393321,
12.));
#182471=CARTESIAN_POINT('Ctrl Pts',(-5.37838284973696,-24.4559943883157,
12.));
#182472=CARTESIAN_POINT('Ctrl Pts',(-5.36258328273628,-24.435838689915,
12.));
#182473=CARTESIAN_POINT('Ctrl Pts',(-5.34688015213538,-24.4157082904614,
12.));
#182474=CARTESIAN_POINT('Ctrl Pts',(-5.33127355076035,-24.3956037401293,
12.));
#182475=CARTESIAN_POINT('Ctrl Pts',(-5.31576357092527,-24.3755255933917,
12.));
#182476=CARTESIAN_POINT('Ctrl Pts',(-5.30035030449064,-24.3554744095075,
12.));
#182477=CARTESIAN_POINT('Ctrl Pts',(-5.28503384290649,-24.3354507529414,
12.));
#182478=CARTESIAN_POINT('Ctrl Pts',(-5.269814277188,-24.3154551932221,12.));
#182479=CARTESIAN_POINT('Ctrl Pts',(-5.25469169788857,-24.2954883048447,
12.));
#182480=CARTESIAN_POINT('Ctrl Pts',(-5.2396661950629,-24.2755506671525,
12.));
#182481=CARTESIAN_POINT('Ctrl Pts',(-5.22473785822443,-24.2556428642294,
12.));
#182482=CARTESIAN_POINT('Ctrl Pts',(-5.20990677629177,-24.2357654847766,
12.));
#182483=CARTESIAN_POINT('Ctrl Pts',(-5.19517303753648,-24.2159191220171,
12.));
#182484=CARTESIAN_POINT('Ctrl Pts',(-5.180536729614,-24.1961043738756,12.));
#182485=CARTESIAN_POINT('Ctrl Pts',(-5.16599793957987,-24.1763218431344,
12.));
#182486=CARTESIAN_POINT('Ctrl Pts',(-5.1515567539008,-24.1565721375971,
12.));
#182487=CARTESIAN_POINT('Ctrl Pts',(-5.13721325845746,-24.1368558702443,
12.));
#182488=CARTESIAN_POINT('Ctrl Pts',(-5.12296753853858,-24.117173659394,
12.));
#182489=CARTESIAN_POINT('Ctrl Pts',(-5.10881967883126,-24.0975261288444,
12.));
#182490=CARTESIAN_POINT('Ctrl Pts',(-5.09476976342618,-24.0779139079264,
12.));
#182491=CARTESIAN_POINT('Ctrl Pts',(-5.08081787581271,-24.0583376315636,
12.));
#182492=CARTESIAN_POINT('Ctrl Pts',(-5.0669640988664,-24.0387979403268,
12.));
#182493=CARTESIAN_POINT('Ctrl Pts',(-5.05320851483069,-24.0192954804896,
12.));
#182494=CARTESIAN_POINT('Ctrl Pts',(-5.03955120528528,-23.9998309040747,
12.));
#182495=CARTESIAN_POINT('Ctrl Pts',(-5.02599225112462,-23.9804048689228,
12.));
#182496=CARTESIAN_POINT('Ctrl Pts',(-5.01253173257459,-23.9610180388271,
12.));
#182497=CARTESIAN_POINT('Ctrl Pts',(-4.9991697291931,-23.9416710836529,
12.));
#182498=CARTESIAN_POINT('Ctrl Pts',(-4.98590631986534,-23.9223646794591,
12.));
#182499=CARTESIAN_POINT('Ctrl Pts',(-4.9727415827923,-23.9030995086164,
12.));
#182500=CARTESIAN_POINT('Ctrl Pts',(-4.95967559546566,-23.883876259922,
12.));
#182501=CARTESIAN_POINT('Ctrl Pts',(-4.94670843465869,-23.8646956287172,
12.));
#182502=CARTESIAN_POINT('Ctrl Pts',(-4.93384017643442,-23.8455583170062,
12.));
#182503=CARTESIAN_POINT('Ctrl Pts',(-4.92107089613977,-23.8264650335721,
12.));
#182504=CARTESIAN_POINT('Ctrl Pts',(-4.90840066839348,-23.8074164940897,
12.));
#182505=CARTESIAN_POINT('Ctrl Pts',(-4.89582956706772,-23.7884134212381,
12.));
#182506=CARTESIAN_POINT('Ctrl Pts',(-4.88335766525566,-23.7694565448044,
12.));
#182507=CARTESIAN_POINT('Ctrl Pts',(-4.87098503527144,-23.7505466018239,
12.));
#182508=CARTESIAN_POINT('Ctrl Pts',(-4.85871174865492,-23.7316843367308,
12.));
#182509=CARTESIAN_POINT('Ctrl Pts',(-4.84653787616424,-23.7128705015014,
12.));
#182510=CARTESIAN_POINT('Ctrl Pts',(-4.83446348776268,-23.6941058557971,
12.));
#182511=CARTESIAN_POINT('Ctrl Pts',(-4.82248865259571,-23.6753911671023,
12.));
#182512=CARTESIAN_POINT('Ctrl Pts',(-4.81061343896443,-23.6567272108631,
12.));
#182513=CARTESIAN_POINT('Ctrl Pts',(-4.79883791433231,-23.6381147706581,
12.));
#182514=CARTESIAN_POINT('Ctrl Pts',(-4.78716214532105,-23.6195546383625,
12.));
#182515=CARTESIAN_POINT('Ctrl Pts',(-4.77558619769876,-23.6010476143099,
12.));
#182516=CARTESIAN_POINT('Ctrl Pts',(-4.76411013636252,-23.5825945074535,
12.));
#182517=CARTESIAN_POINT('Ctrl Pts',(-4.75273402530616,-23.564196135517,
12.));
#182518=CARTESIAN_POINT('Ctrl Pts',(-4.74145792760699,-23.5458533251715,
12.));
#182519=CARTESIAN_POINT('Ctrl Pts',(-4.73028190543032,-23.5275669122378,
12.));
#182520=CARTESIAN_POINT('Ctrl Pts',(-4.71920602001905,-23.5093377418784,
12.));
#182521=CARTESIAN_POINT('Ctrl Pts',(-4.70823033167821,-23.491166668789,
12.));
#182522=CARTESIAN_POINT('Ctrl Pts',(-4.69735489975024,-23.4730545573849,
12.));
#182523=CARTESIAN_POINT('Ctrl Pts',(-4.68657978258298,-23.4550022819852,
12.));
#182524=CARTESIAN_POINT('Ctrl Pts',(-4.67590503753051,-23.4370107270444,
12.));
#182525=CARTESIAN_POINT('Ctrl Pts',(-4.66533072094664,-23.4190807873798,
12.));
#182526=CARTESIAN_POINT('Ctrl Pts',(-4.65485688816923,-23.4012133683957,
12.));
#182527=CARTESIAN_POINT('Ctrl Pts',(-4.64448359349936,-23.383409386307,
12.));
#182528=CARTESIAN_POINT('Ctrl Pts',(-4.63421089016555,-23.3656697683496,
12.));
#182529=CARTESIAN_POINT('Ctrl Pts',(-4.62403883030825,-23.3479954530281,
12.));
#182530=CARTESIAN_POINT('Ctrl Pts',(-4.61396746497849,-23.3303873903947,
12.));
#182531=CARTESIAN_POINT('Ctrl Pts',(-4.60399684412176,-23.3128465423119,
12.));
#182532=CARTESIAN_POINT('Ctrl Pts',(-4.5941270165575,-23.295373882719,12.));
#182533=CARTESIAN_POINT('Ctrl Pts',(-4.58435802994675,-23.2779703978868,
12.));
#182534=CARTESIAN_POINT('Ctrl Pts',(-4.57468993076071,-23.2606370866854,
12.));
#182535=CARTESIAN_POINT('Ctrl Pts',(-4.56512276427812,-23.2433749609117,
12.));
#182536=CARTESIAN_POINT('Ctrl Pts',(-4.55565657456957,-23.2261850456055,
12.));
#182537=CARTESIAN_POINT('Ctrl Pts',(-4.54629140447543,-23.2090683793627,
12.));
#182538=CARTESIAN_POINT('Ctrl Pts',(-4.53702729557586,-23.1920260146474,
12.));
#182539=CARTESIAN_POINT('Ctrl Pts',(-4.52786428815049,-23.1750590180923,
12.));
#182540=CARTESIAN_POINT('Ctrl Pts',(-4.51880242116786,-23.1581684708778,
12.));
#182541=CARTESIAN_POINT('Ctrl Pts',(-4.50984173227088,-23.1413554691136,
12.));
#182542=CARTESIAN_POINT('Ctrl Pts',(-4.50098225775179,-23.1246211242117,
12.));
#182543=CARTESIAN_POINT('Ctrl Pts',(-4.49222403252202,-23.1079665632629,
12.));
#182544=CARTESIAN_POINT('Ctrl Pts',(-4.48356709006757,-23.0913929293909,
12.));
#182545=CARTESIAN_POINT('Ctrl Pts',(-4.47501146242822,-23.0749013821867,
12.));
#182546=CARTESIAN_POINT('Ctrl Pts',(-4.46655718018206,-23.0584930981723,
12.));
#182547=CARTESIAN_POINT('Ctrl Pts',(-4.45820427241677,-23.0421692712466,
12.));
#182548=CARTESIAN_POINT('Ctrl Pts',(-4.44995276669699,-23.0259311131395,
12.));
#182549=CARTESIAN_POINT('Ctrl Pts',(-4.44180268901667,-23.0097798538399,
12.));
#182550=CARTESIAN_POINT('Ctrl Pts',(-4.43375406376906,-22.9937167421009,
12.));
#182551=CARTESIAN_POINT('Ctrl Pts',(-4.42580691372772,-22.9777430460021,
12.));
#182552=CARTESIAN_POINT('Ctrl Pts',(-4.41796126001311,-22.9618600534866,
12.));
#182553=CARTESIAN_POINT('Ctrl Pts',(-4.41021712205549,-22.9460690729093,
12.));
#182554=CARTESIAN_POINT('Ctrl Pts',(-4.40257451754308,-22.9303714335549,
12.));
#182555=CARTESIAN_POINT('Ctrl Pts',(-4.39503346238455,-22.9147684862425,
12.));
#182556=CARTESIAN_POINT('Ctrl Pts',(-4.38759397068393,-22.8992616040108,
12.));
#182557=CARTESIAN_POINT('Ctrl Pts',(-4.38025605470091,-22.8838521827702,
12.));
#182558=CARTESIAN_POINT('Ctrl Pts',(-4.37301972480753,-22.8685416419725,
12.));
#182559=CARTESIAN_POINT('Ctrl Pts',(-4.36588498943011,-22.8533314252419,
12.));
#182560=CARTESIAN_POINT('Ctrl Pts',(-4.3588518550056,-22.838223001118,12.));
#182561=CARTESIAN_POINT('Ctrl Pts',(-4.35192032594802,-22.8232178638873,
12.));
#182562=CARTESIAN_POINT('Ctrl Pts',(-4.34509040460066,-22.808317534379,
12.));
#182563=CARTESIAN_POINT('Ctrl Pts',(-4.33836209118444,-22.7935235607807,
12.));
#182564=CARTESIAN_POINT('Ctrl Pts',(-4.33173538373183,-22.7788375194081,
12.));
#182565=CARTESIAN_POINT('Ctrl Pts',(-4.32521027803748,-22.764261015648,
12.));
#182566=CARTESIAN_POINT('Ctrl Pts',(-4.31878676761231,-22.7497956849852,
12.));
#182567=CARTESIAN_POINT('Ctrl Pts',(-4.31246484362551,-22.7354431939926,
12.));
#182568=CARTESIAN_POINT('Ctrl Pts',(-4.30624449484075,-22.7212052413384,
12.));
#182569=CARTESIAN_POINT('Ctrl Pts',(-4.30012570754067,-22.707083558756,
12.));
#182570=CARTESIAN_POINT('Ctrl Pts',(-4.29410846547062,-22.6930799122545,
12.));
#182571=CARTESIAN_POINT('Ctrl Pts',(-4.28819274977767,-22.6791961033536,
12.));
#182572=CARTESIAN_POINT('Ctrl Pts',(-4.2823785389406,-22.665433970311,12.));
#182573=CARTESIAN_POINT('Ctrl Pts',(-4.27666580869118,-22.6517953893303,
12.));
#182574=CARTESIAN_POINT('Ctrl Pts',(-4.27105453193,-22.6382822758171,12.));
#182575=CARTESIAN_POINT('Ctrl Pts',(-4.26554467865572,-22.6248965859975,
12.));
#182576=CARTESIAN_POINT('Ctrl Pts',(-4.26013621588304,-22.611640318482,
12.));
#182577=CARTESIAN_POINT('Ctrl Pts',(-4.25482910755486,-22.5985155158637,
12.));
#182578=CARTESIAN_POINT('Ctrl Pts',(-4.24962331444186,-22.5855242662479,
12.));
#182579=CARTESIAN_POINT('Ctrl Pts',(-4.2445187940486,-22.5726687049922,
12.));
#182580=CARTESIAN_POINT('Ctrl Pts',(-4.23951550052527,-22.559951016643,
12.));
#182581=CARTESIAN_POINT('Ctrl Pts',(-4.23461338456714,-22.5473734368086,
12.));
#182582=CARTESIAN_POINT('Ctrl Pts',(-4.22981239330732,-22.5349382540587,
12.));
#182583=CARTESIAN_POINT('Ctrl Pts',(-4.22511247020041,-22.5226478117885,
12.));
#182584=CARTESIAN_POINT('Ctrl Pts',(-4.22051355490198,-22.5105045108882,
12.));
#182585=CARTESIAN_POINT('Ctrl Pts',(-4.21601558313909,-22.4985108124229,
12.));
#182586=CARTESIAN_POINT('Ctrl Pts',(-4.21161848657429,-22.4866692403147,
12.));
#182587=CARTESIAN_POINT('Ctrl Pts',(-4.20732219265649,-22.4749823839915,
12.));
#182588=CARTESIAN_POINT('Ctrl Pts',(-4.20312662448172,-22.4634529011433,
12.));
#182589=CARTESIAN_POINT('Ctrl Pts',(-4.19903170066356,-22.4520835205419,
12.));
#182590=CARTESIAN_POINT('Ctrl Pts',(-4.19503733518862,-22.4408770448917,
12.));
#182591=CARTESIAN_POINT('Ctrl Pts',(-4.19114343726943,-22.4298363535421,
12.));
#182592=CARTESIAN_POINT('Ctrl Pts',(-4.18734991117722,-22.4189644056115,
12.));
#182593=CARTESIAN_POINT('Ctrl Pts',(-4.18365665600851,-22.4082642454453,
12.));
#182594=CARTESIAN_POINT('Ctrl Pts',(-4.18006356544883,-22.3977390078075,
12.));
#182595=CARTESIAN_POINT('Ctrl Pts',(-4.17657052752826,-22.3873919231334,
12.));
#182596=CARTESIAN_POINT('Ctrl Pts',(-4.17317742436146,-22.3772263228617,
12.));
#182597=CARTESIAN_POINT('Ctrl Pts',(-4.16988413199458,-22.36724564276,12.));
#182598=CARTESIAN_POINT('Ctrl Pts',(-4.16669052026601,-22.3574534257396,
12.));
#182599=CARTESIAN_POINT('Ctrl Pts',(-4.16359645263189,-22.3478533253889,
12.));
#182600=CARTESIAN_POINT('Ctrl Pts',(-4.16060178604165,-22.3384491078602,
12.));
#182601=CARTESIAN_POINT('Ctrl Pts',(-4.15770637047891,-22.3292446628959,
12.));
#182602=CARTESIAN_POINT('Ctrl Pts',(-4.15491004835282,-22.320244018698,
12.));
#182603=CARTESIAN_POINT('Ctrl Pts',(-4.15221265396991,-22.3114513545185,
12.));
#182604=CARTESIAN_POINT('Ctrl Pts',(-4.14961401285523,-22.3028710166933,
12.));
#182605=CARTESIAN_POINT('Ctrl Pts',(-4.14711394168557,-22.2945075198467,
12.));
#182606=CARTESIAN_POINT('Ctrl Pts',(-4.14471224859296,-22.2863655389166,
12.));
#182607=CARTESIAN_POINT('Ctrl Pts',(-4.14240873321985,-22.2784499072027,
12.));
#182608=CARTESIAN_POINT('Ctrl Pts',(-4.14020318715992,-22.2707656042457,
12.));
#182609=CARTESIAN_POINT('Ctrl Pts',(-4.13809539255423,-22.2633177913972,
12.));
#182610=CARTESIAN_POINT('Ctrl Pts',(-4.13608511977226,-22.2561118708421,
12.));
#182611=CARTESIAN_POINT('Ctrl Pts',(-4.13417212558811,-22.249153531779,
12.));
#182612=CARTESIAN_POINT('Ctrl Pts',(-4.13235615060161,-22.2424488153523,
12.));
#182613=CARTESIAN_POINT('Ctrl Pts',(-4.13063692157499,-22.2360040565533,
12.));
#182614=CARTESIAN_POINT('Ctrl Pts',(-4.1290141546338,-22.2298258043947,
12.));
#182615=CARTESIAN_POINT('Ctrl Pts',(-4.12748755830105,-22.2239207458781,
12.));
#182616=CARTESIAN_POINT('Ctrl Pts',(-4.12605683613308,-22.2182956401341,
12.));
#182617=CARTESIAN_POINT('Ctrl Pts',(-4.12472167516608,-22.2129576146671,
12.));
#182618=CARTESIAN_POINT('Ctrl Pts',(-4.12348173702024,-22.2079143941719,
12.));
#182619=CARTESIAN_POINT('Ctrl Pts',(-4.12233664408228,-22.2031746532106,
12.));
#182620=CARTESIAN_POINT('Ctrl Pts',(-4.12128598183523,-22.1987479618246,
12.));
#182621=CARTESIAN_POINT('Ctrl Pts',(-4.12032932637737,-22.1946440958098,
12.));
#182622=CARTESIAN_POINT('Ctrl Pts',(-4.11946626228637,-22.1908725908525,
12.));
#182623=CARTESIAN_POINT('Ctrl Pts',(-4.11869641271774,-22.1874419861496,
12.));
#182624=CARTESIAN_POINT('Ctrl Pts',(-4.11801938107481,-22.1843613164855,
12.));
#182625=CARTESIAN_POINT('Ctrl Pts',(-4.11743469691757,-22.1816414985788,
12.));
#182626=CARTESIAN_POINT('Ctrl Pts',(-4.11694173195005,-22.179297473024,
12.));
#182627=CARTESIAN_POINT('Ctrl Pts',(-4.11653973150519,-22.177347426894,
12.));
#182628=CARTESIAN_POINT('Ctrl Pts',(-4.11622797217069,-22.1758088296598,
12.));
#182629=CARTESIAN_POINT('Ctrl Pts',(-4.11600589882846,-22.1746949858775,
12.));
#182630=CARTESIAN_POINT('Ctrl Pts',(-4.11589976826167,-22.1741488021234,
12.));
#182631=CARTESIAN_POINT('Ctrl Pts',(-4.11586035878288,-22.1739341411687,
12.));
#182632=CARTESIAN_POINT('Ctrl Pts',(-4.11585194677443,-22.173877682324,
12.));
#182633=CARTESIAN_POINT('Ctrl Pts',(-4.11585220600463,-22.1738711152697,
12.));
#182634=CARTESIAN_POINT('',(-4.0139614976743,-21.624941921198,12.));
#182635=CARTESIAN_POINT('',(-1.96187429785751,-10.5694630535049,12.));
#182636=CARTESIAN_POINT('',(-3.4423049612042,-21.2226420728916,12.));
#182637=CARTESIAN_POINT('Origin',(-3.52235856495314,-21.7161918885402,12.));
#182638=CARTESIAN_POINT('',(-2.16781269186829,-21.3904321633055,12.));
#182639=CARTESIAN_POINT('Origin',(-1.31973449697531E-13,-7.6920903736728E-13,
12.));
#182640=CARTESIAN_POINT('',(-1.71975774210843,-21.9269795755927,12.));
#182641=CARTESIAN_POINT('Origin',(-2.21822694051639,-21.88788407408,12.));
#182642=CARTESIAN_POINT('',(-1.76341220531181,-22.4835757167854,12.));
#182643=CARTESIAN_POINT('',(-0.881706102655891,-11.2417878583927,12.));
#182644=CARTESIAN_POINT('',(-0.661312440730913,-25.991588367311,12.));
#182645=CARTESIAN_POINT('Ctrl Pts',(-1.76341220531181,-22.4835757167854,
12.));
#182646=CARTESIAN_POINT('Ctrl Pts',(-1.76341415538792,-22.4835819929788,
12.));
#182647=CARTESIAN_POINT('Ctrl Pts',(-1.76342064263638,-22.4836387052228,
12.));
#182648=CARTESIAN_POINT('Ctrl Pts',(-1.7634381343466,-22.4838562517064,
12.));
#182649=CARTESIAN_POINT('Ctrl Pts',(-1.76347698284863,-22.4844112933125,
12.));
#182650=CARTESIAN_POINT('Ctrl Pts',(-1.7635507604555,-22.4855446605991,
12.));
#182651=CARTESIAN_POINT('Ctrl Pts',(-1.76364784232926,-22.4871115206572,
12.));
#182652=CARTESIAN_POINT('Ctrl Pts',(-1.76376424879469,-22.4890991659479,
12.));
#182653=CARTESIAN_POINT('Ctrl Pts',(-1.76389475965715,-22.4914909094908,
12.));
#182654=CARTESIAN_POINT('Ctrl Pts',(-1.76403393880317,-22.4942693792449,
12.));
#182655=CARTESIAN_POINT('Ctrl Pts',(-1.76417731243484,-22.4974203063191,
12.));
#182656=CARTESIAN_POINT('Ctrl Pts',(-1.76432160068739,-22.5009332677316,
12.));
#182657=CARTESIAN_POINT('Ctrl Pts',(-1.76446408210366,-22.5047996391978,
12.));
#182658=CARTESIAN_POINT('Ctrl Pts',(-1.76460218257314,-22.5090112700212,
12.));
#182659=CARTESIAN_POINT('Ctrl Pts',(-1.7647330328115,-22.5135590569554,
12.));
#182660=CARTESIAN_POINT('Ctrl Pts',(-1.76485369319896,-22.5184336670207,
12.));
#182661=CARTESIAN_POINT('Ctrl Pts',(-1.76496128643376,-22.5236259635515,
12.));
#182662=CARTESIAN_POINT('Ctrl Pts',(-1.7650532026276,-22.529127665298,12.));
#182663=CARTESIAN_POINT('Ctrl Pts',(-1.76512711563255,-22.5349313983571,
12.));
#182664=CARTESIAN_POINT('Ctrl Pts',(-1.76518087841494,-22.5410303590892,
12.));
#182665=CARTESIAN_POINT('Ctrl Pts',(-1.76521245524048,-22.5474180954006,
12.));
#182666=CARTESIAN_POINT('Ctrl Pts',(-1.76521983384063,-22.5540882235837,
12.));
#182667=CARTESIAN_POINT('Ctrl Pts',(-1.76520104500451,-22.5610344912501,
12.));
#182668=CARTESIAN_POINT('Ctrl Pts',(-1.76515418518832,-22.5682508499874,
12.));
#182669=CARTESIAN_POINT('Ctrl Pts',(-1.76507744026747,-22.5757315316353,
12.));
#182670=CARTESIAN_POINT('Ctrl Pts',(-1.76496910283089,-22.5834711038022,
12.));
#182671=CARTESIAN_POINT('Ctrl Pts',(-1.76482755288412,-22.5914644078106,
12.));
#182672=CARTESIAN_POINT('Ctrl Pts',(-1.76465124413558,-22.5997065145638,
12.));
#182673=CARTESIAN_POINT('Ctrl Pts',(-1.76443868648017,-22.6081926681343,
12.));
#182674=CARTESIAN_POINT('Ctrl Pts',(-1.7641884354374,-22.6169182517694,
12.));
#182675=CARTESIAN_POINT('Ctrl Pts',(-1.76389909571404,-22.6258787994848,
12.));
#182676=CARTESIAN_POINT('Ctrl Pts',(-1.76356932176274,-22.6350699979359,
12.));
#182677=CARTESIAN_POINT('Ctrl Pts',(-1.76319782013917,-22.6444876940423,
12.));
#182678=CARTESIAN_POINT('Ctrl Pts',(-1.76278334912562,-22.654127893841,
12.));
#182679=CARTESIAN_POINT('Ctrl Pts',(-1.7623247139257,-22.6639867471753,
12.));
#182680=CARTESIAN_POINT('Ctrl Pts',(-1.76182076289527,-22.67406053567,12.));
#182681=CARTESIAN_POINT('Ctrl Pts',(-1.76127038310615,-22.684345658525,
12.));
#182682=CARTESIAN_POINT('Ctrl Pts',(-1.76067249704888,-22.6948386219851,
12.));
#182683=CARTESIAN_POINT('Ctrl Pts',(-1.76002606202402,-22.7055360375485,
12.));
#182684=CARTESIAN_POINT('Ctrl Pts',(-1.75933006905926,-22.7164346186006,
12.));
#182685=CARTESIAN_POINT('Ctrl Pts',(-1.75858354204634,-22.72753117773,12.));
#182686=CARTESIAN_POINT('Ctrl Pts',(-1.75778553673245,-22.7388226235559,
12.));
#182687=CARTESIAN_POINT('Ctrl Pts',(-1.75693513908908,-22.750305955645,
12.));
#182688=CARTESIAN_POINT('Ctrl Pts',(-1.75603146371642,-22.7619782595013,
12.));
#182689=CARTESIAN_POINT('Ctrl Pts',(-1.75507365227133,-22.7738367016118,
12.));
#182690=CARTESIAN_POINT('Ctrl Pts',(-1.75406087182937,-22.7858785242361,
12.));
#182691=CARTESIAN_POINT('Ctrl Pts',(-1.75299231391467,-22.7981010424314,
12.));
#182692=CARTESIAN_POINT('Ctrl Pts',(-1.75186719365593,-22.8105016414713,
12.));
#182693=CARTESIAN_POINT('Ctrl Pts',(-1.75068474890884,-22.8230777741284,
12.));
#182694=CARTESIAN_POINT('Ctrl Pts',(-1.74944423940117,-22.8358269579853,
12.));
#182695=CARTESIAN_POINT('Ctrl Pts',(-1.74814494588494,-22.8487467728076,
12.));
#182696=CARTESIAN_POINT('Ctrl Pts',(-1.74678616930666,-22.8618348580235,
12.));
#182697=CARTESIAN_POINT('Ctrl Pts',(-1.74536722998202,-22.8750889101696,
12.));
#182698=CARTESIAN_POINT('Ctrl Pts',(-1.74388746677703,-22.888506680335,
12.));
#182699=CARTESIAN_POINT('Ctrl Pts',(-1.74234623630081,-22.9020859716141,
12.));
#182700=CARTESIAN_POINT('Ctrl Pts',(-1.74074291231059,-22.9158246373363,
12.));
#182701=CARTESIAN_POINT('Ctrl Pts',(-1.73907688511667,-22.9297205792586,
12.));
#182702=CARTESIAN_POINT('Ctrl Pts',(-1.7373475610004,-22.9437717457826,
12.));
#182703=CARTESIAN_POINT('Ctrl Pts',(-1.7355543616277,-22.9579761301063,
12.));
#182704=CARTESIAN_POINT('Ctrl Pts',(-1.73369672350816,-22.9723317685688,
12.));
#182705=CARTESIAN_POINT('Ctrl Pts',(-1.73177409750192,-22.9868367391978,
12.));
#182706=CARTESIAN_POINT('Ctrl Pts',(-1.72978594832137,-23.001489160189,
12.));
#182707=CARTESIAN_POINT('Ctrl Pts',(-1.7277317540471,-23.0162871884168,
12.));
#182708=CARTESIAN_POINT('Ctrl Pts',(-1.72561100564047,-23.0312290178883,
12.));
#182709=CARTESIAN_POINT('Ctrl Pts',(-1.72342320653748,-23.0463128785531,
12.));
#182710=CARTESIAN_POINT('Ctrl Pts',(-1.72116787225993,-23.0615370351562,
12.));
#182711=CARTESIAN_POINT('Ctrl Pts',(-1.71884453003028,-23.0768997860709,
12.));
#182712=CARTESIAN_POINT('Ctrl Pts',(-1.71645271839298,-23.0923994621213,
12.));
#182713=CARTESIAN_POINT('Ctrl Pts',(-1.71399198684705,-23.1080344254286,
12.));
#182714=CARTESIAN_POINT('Ctrl Pts',(-1.71146189552175,-23.1238030684925,
12.));
#182715=CARTESIAN_POINT('Ctrl Pts',(-1.70886201485453,-23.1397038132356,
12.));
#182716=CARTESIAN_POINT('Ctrl Pts',(-1.70619192527853,-23.1557351100614,
12.));
#182717=CARTESIAN_POINT('Ctrl Pts',(-1.70345121691277,-23.1718954368751,
12.));
#182718=CARTESIAN_POINT('Ctrl Pts',(-1.70063948927011,-23.1881832981851,
12.));
#182719=CARTESIAN_POINT('Ctrl Pts',(-1.69775635099444,-23.2045972243767,
12.));
#182720=CARTESIAN_POINT('Ctrl Pts',(-1.69480141959954,-23.2211357709374,
12.));
#182721=CARTESIAN_POINT('Ctrl Pts',(-1.69177432121712,-23.2377975177013,
12.));
#182722=CARTESIAN_POINT('Ctrl Pts',(-1.68867469034897,-23.2545810680537,
12.));
#182723=CARTESIAN_POINT('Ctrl Pts',(-1.68550216963259,-23.2714850482246,
12.));
#182724=CARTESIAN_POINT('Ctrl Pts',(-1.68225640962169,-23.2885081066951,
12.));
#182725=CARTESIAN_POINT('Ctrl Pts',(-1.67893706857118,-23.3056489135611,
12.));
#182726=CARTESIAN_POINT('Ctrl Pts',(-1.67554381222995,-23.3229061599145,
12.));
#182727=CARTESIAN_POINT('Ctrl Pts',(-1.67207631363923,-23.3402785571865,
12.));
#182728=CARTESIAN_POINT('Ctrl Pts',(-1.66853425293997,-23.3577648365744,
12.));
#182729=CARTESIAN_POINT('Ctrl Pts',(-1.66491731718878,-23.3753637485545,
12.));
#182730=CARTESIAN_POINT('Ctrl Pts',(-1.66122520018012,-23.3930740623619,
12.));
#182731=CARTESIAN_POINT('Ctrl Pts',(-1.65745760227506,-23.4108945654805,
12.));
#182732=CARTESIAN_POINT('Ctrl Pts',(-1.65361423023729,-23.4288240631043,
12.));
#182733=CARTESIAN_POINT('Ctrl Pts',(-1.64969479707341,-23.4468613776574,
12.));
#182734=CARTESIAN_POINT('Ctrl Pts',(-1.64569902187612,-23.4650053483932,
12.));
#182735=CARTESIAN_POINT('Ctrl Pts',(-1.64162662967529,-23.4832548309645,
12.));
#182736=CARTESIAN_POINT('Ctrl Pts',(-1.63747735129475,-23.5016086970003,
12.));
#182737=CARTESIAN_POINT('Ctrl Pts',(-1.63325092321727,-23.5200658336612,
12.));
#182738=CARTESIAN_POINT('Ctrl Pts',(-1.62894708745224,-23.538625143226,
12.));
#182739=CARTESIAN_POINT('Ctrl Pts',(-1.62456559140065,-23.5572855427601,
12.));
#182740=CARTESIAN_POINT('Ctrl Pts',(-1.62010618772867,-23.57604596376,12.));
#182741=CARTESIAN_POINT('Ctrl Pts',(-1.61556863424699,-23.5949053517997,
12.));
#182742=CARTESIAN_POINT('Ctrl Pts',(-1.61095269379779,-23.6138626661653,
12.));
#182743=CARTESIAN_POINT('Ctrl Pts',(-1.60625813414674,-23.6329168794929,
12.));
#182744=CARTESIAN_POINT('Ctrl Pts',(-1.60148472786596,-23.6520669774876,
12.));
#182745=CARTESIAN_POINT('Ctrl Pts',(-1.59663225222464,-23.671311958631,
12.));
#182746=CARTESIAN_POINT('Ctrl Pts',(-1.59170048908634,-23.6906508338833,
12.));
#182747=CARTESIAN_POINT('Ctrl Pts',(-1.58668922481222,-23.710082626383,
12.));
#182748=CARTESIAN_POINT('Ctrl Pts',(-1.58159825017359,-23.72960637113,12.));
#182749=CARTESIAN_POINT('Ctrl Pts',(-1.57642736025247,-23.749221114736,
12.));
#182750=CARTESIAN_POINT('Ctrl Pts',(-1.57117635434409,-23.7689259151862,
12.));
#182751=CARTESIAN_POINT('Ctrl Pts',(-1.56584503586844,-23.7887198415878,
12.));
#182752=CARTESIAN_POINT('Ctrl Pts',(-1.56043321228635,-23.8086019739194,
12.));
#182753=CARTESIAN_POINT('Ctrl Pts',(-1.55494069502636,-23.8285714027636,
12.));
#182754=CARTESIAN_POINT('Ctrl Pts',(-1.54936729940542,-23.8486272290705,
12.));
#182755=CARTESIAN_POINT('Ctrl Pts',(-1.54371284453991,-23.8687685639642,
12.));
#182756=CARTESIAN_POINT('Ctrl Pts',(-1.53797715326759,-23.8889945285318,
12.));
#182757=CARTESIAN_POINT('Ctrl Pts',(-1.53216005207464,-23.9093042536119,
12.));
#182758=CARTESIAN_POINT('Ctrl Pts',(-1.52626137103033,-23.9296968795757,
12.));
#182759=CARTESIAN_POINT('Ctrl Pts',(-1.52028094372793,-23.9501715561033,
12.));
#182760=CARTESIAN_POINT('Ctrl Pts',(-1.51421860720615,-23.970727442014,
12.));
#182761=CARTESIAN_POINT('Ctrl Pts',(-1.50807420187695,-23.9913637050927,
12.));
#182762=CARTESIAN_POINT('Ctrl Pts',(-1.501847571461,-24.0120795219086,12.));
#182763=CARTESIAN_POINT('Ctrl Pts',(-1.49553856292802,-24.0328740776331,
12.));
#182764=CARTESIAN_POINT('Ctrl Pts',(-1.48914702644888,-24.0537465658429,
12.));
#182765=CARTESIAN_POINT('Ctrl Pts',(-1.48267281533684,-24.0746961883528,
12.));
#182766=CARTESIAN_POINT('Ctrl Pts',(-1.47611578597743,-24.0957221550778,
12.));
#182767=CARTESIAN_POINT('Ctrl Pts',(-1.46947579776992,-24.1168236838824,
12.));
#182768=CARTESIAN_POINT('Ctrl Pts',(-1.46275271307399,-24.1380000004272,
12.));
#182769=CARTESIAN_POINT('Ctrl Pts',(-1.45594639716319,-24.1592503380107,
12.));
#182770=CARTESIAN_POINT('Ctrl Pts',(-1.44905671818729,-24.1805739374038,
12.));
#182771=CARTESIAN_POINT('Ctrl Pts',(-1.44208354711083,-24.201970046722,
12.));
#182772=CARTESIAN_POINT('Ctrl Pts',(-1.43502675765509,-24.2234379212984,
12.));
#182773=CARTESIAN_POINT('Ctrl Pts',(-1.42788622624855,-24.2449768235488,
12.));
#182774=CARTESIAN_POINT('Ctrl Pts',(-1.42066183198254,-24.2665860228356,
12.));
#182775=CARTESIAN_POINT('Ctrl Pts',(-1.41335345657684,-24.288264795321,
12.));
#182776=CARTESIAN_POINT('Ctrl Pts',(-1.40596098434338,-24.3100124238311,
12.));
#182777=CARTESIAN_POINT('Ctrl Pts',(-1.39848430212808,-24.3318281977643,
12.));
#182778=CARTESIAN_POINT('Ctrl Pts',(-1.39092329926389,-24.3537114129875,
12.));
#182779=CARTESIAN_POINT('Ctrl Pts',(-1.38327786753,-24.3756613717299,12.));
#182780=CARTESIAN_POINT('Ctrl Pts',(-1.3755479011161,-24.3976773824732,
12.));
#182781=CARTESIAN_POINT('Ctrl Pts',(-1.36773329659957,-24.4197587598337,
12.));
#182782=CARTESIAN_POINT('Ctrl Pts',(-1.35983395290628,-24.4419048244523,
12.));
#182783=CARTESIAN_POINT('Ctrl Pts',(-1.35184977125649,-24.4641149028892,
12.));
#182784=CARTESIAN_POINT('Ctrl Pts',(-1.34378065512339,-24.4863883275134,
12.));
#182785=CARTESIAN_POINT('Ctrl Pts',(-1.33562651019687,-24.5087244363856,
12.));
#182786=CARTESIAN_POINT('Ctrl Pts',(-1.32738724435327,-24.5311225731435,
12.));
#182787=CARTESIAN_POINT('Ctrl Pts',(-1.31906276763669,-24.5535820868674,
12.));
#182788=CARTESIAN_POINT('Ctrl Pts',(-1.31065299222023,-24.5761023320183,
12.));
#182789=CARTESIAN_POINT('Ctrl Pts',(-1.30215783236363,-24.5986826684027,
12.));
#182790=CARTESIAN_POINT('Ctrl Pts',(-1.29357720438108,-24.6213224611229,
12.));
#182791=CARTESIAN_POINT('Ctrl Pts',(-1.28491102661515,-24.6440210805278,
12.));
#182792=CARTESIAN_POINT('Ctrl Pts',(-1.27615921941643,-24.6667779021559,
12.));
#182793=CARTESIAN_POINT('Ctrl Pts',(-1.26732170513501,-24.6895923066836,
12.));
#182794=CARTESIAN_POINT('Ctrl Pts',(-1.25839840807419,-24.7124636797894,
12.));
#182795=CARTESIAN_POINT('Ctrl Pts',(-1.24938925444327,-24.7353914120011,
12.));
#182796=CARTESIAN_POINT('Ctrl Pts',(-1.2402941723199,-24.7583748985438,
12.));
#182797=CARTESIAN_POINT('Ctrl Pts',(-1.23111309161845,-24.7814135391799,
12.));
#182798=CARTESIAN_POINT('Ctrl Pts',(-1.22184594406529,-24.8045067380536,
12.));
#182799=CARTESIAN_POINT('Ctrl Pts',(-1.21249266318209,-24.8276539035092,
12.));
#182800=CARTESIAN_POINT('Ctrl Pts',(-1.20305318426021,-24.8508544481974,
12.));
#182801=CARTESIAN_POINT('Ctrl Pts',(-1.19352744434065,-24.8741077892075,
12.));
#182802=CARTESIAN_POINT('Ctrl Pts',(-1.18391538220104,-24.8974133481829,
12.));
#182803=CARTESIAN_POINT('Ctrl Pts',(-1.17421693835042,-24.9207705514448,
12.));
#182804=CARTESIAN_POINT('Ctrl Pts',(-1.16443205502851,-24.9441788300932,
12.));
#182805=CARTESIAN_POINT('Ctrl Pts',(-1.1545606762189,-24.9676376201502,
12.));
#182806=CARTESIAN_POINT('Ctrl Pts',(-1.14460274758202,-24.9911463621433,
12.));
#182807=CARTESIAN_POINT('Ctrl Pts',(-1.13455821638531,-25.0147045006196,
12.));
#182808=CARTESIAN_POINT('Ctrl Pts',(-1.12442703144453,-25.0383114836899,
12.));
#182809=CARTESIAN_POINT('Ctrl Pts',(-1.1142091430689,-25.0619667625336,
12.));
#182810=CARTESIAN_POINT('Ctrl Pts',(-1.10390450301746,-25.0856697909679,
12.));
#182811=CARTESIAN_POINT('Ctrl Pts',(-1.09351306445309,-25.1094200248446,
12.));
#182812=CARTESIAN_POINT('Ctrl Pts',(-1.08303478197189,-25.1332169227413,
12.));
#182813=CARTESIAN_POINT('Ctrl Pts',(-1.07246961165477,-25.157059946931,
12.));
#182814=CARTESIAN_POINT('Ctrl Pts',(-1.06181751111769,-25.1809485642192,
12.));
#182815=CARTESIAN_POINT('Ctrl Pts',(-1.05107843957933,-25.2048822469028,
12.));
#182816=CARTESIAN_POINT('Ctrl Pts',(-1.04025235791508,-25.2288604735086,
12.));
#182817=CARTESIAN_POINT('Ctrl Pts',(-1.02933922876807,-25.2528827300422,
12.));
#182818=CARTESIAN_POINT('Ctrl Pts',(-1.01833901642238,-25.276948508726,
12.));
#182819=CARTESIAN_POINT('Ctrl Pts',(-1.00725168656897,-25.3010573055548,
12.));
#182820=CARTESIAN_POINT('Ctrl Pts',(-0.996077206120636,-25.3252086182968,
12.));
#182821=CARTESIAN_POINT('Ctrl Pts',(-0.984815543003984,-25.3494019441441,
12.));
#182822=CARTESIAN_POINT('Ctrl Pts',(-0.973466666000176,-25.3736367778845,
12.));
#182823=CARTESIAN_POINT('Ctrl Pts',(-0.962030544503155,-25.3979126089163,
12.));
#182824=CARTESIAN_POINT('Ctrl Pts',(-0.950507148597481,-25.4222289223167,
12.));
#182825=CARTESIAN_POINT('Ctrl Pts',(-0.938896449496205,-25.4465852044849,
12.));
#182826=CARTESIAN_POINT('Ctrl Pts',(-0.927198419886107,-25.4709809475009,
12.));
#182827=CARTESIAN_POINT('Ctrl Pts',(-0.915413034335626,-25.4954156541795,
12.));
#182828=CARTESIAN_POINT('Ctrl Pts',(-0.903540269651119,-25.5198888424194,
12.));
#182829=CARTESIAN_POINT('Ctrl Pts',(-0.891580105349052,-25.5444000508211,
12.));
#182830=CARTESIAN_POINT('Ctrl Pts',(-0.879532523834307,-25.5689488408156,
12.));
#182831=CARTESIAN_POINT('Ctrl Pts',(-0.867397509338443,-25.5935347843585,
12.));
#182832=CARTESIAN_POINT('Ctrl Pts',(-0.85517504703656,-25.6181574536049,
12.));
#182833=CARTESIAN_POINT('Ctrl Pts',(-0.842865122120771,-25.6428164100055,
12.));
#182834=CARTESIAN_POINT('Ctrl Pts',(-0.830467718864218,-25.6675111931952,
12.));
#182835=CARTESIAN_POINT('Ctrl Pts',(-0.817982819787476,-25.6922413110194,
12.));
#182836=CARTESIAN_POINT('Ctrl Pts',(-0.805410404554365,-25.7170062262525,
12.));
#182837=CARTESIAN_POINT('Ctrl Pts',(-0.792750451616139,-25.7418053757746,
12.));
#182838=CARTESIAN_POINT('Ctrl Pts',(-0.780002940291976,-25.7666381946955,
12.));
#182839=CARTESIAN_POINT('Ctrl Pts',(-0.76716785265118,-25.7915041383376,
12.));
#182840=CARTESIAN_POINT('Ctrl Pts',(-0.754245175609535,-25.8164027059984,
12.));
#182841=CARTESIAN_POINT('Ctrl Pts',(-0.741234902663818,-25.8413334619055,
12.));
#182842=CARTESIAN_POINT('Ctrl Pts',(-0.728137036482348,-25.8662960624185,
12.));
#182843=CARTESIAN_POINT('Ctrl Pts',(-0.714951588527651,-25.891290261497,
12.));
#182844=CARTESIAN_POINT('Ctrl Pts',(-0.701678575228768,-25.9163158909426,
12.));
#182845=CARTESIAN_POINT('Ctrl Pts',(-0.688318015057743,-25.9413728471909,
12.));
#182846=CARTESIAN_POINT('Ctrl Pts',(-0.677559543209739,-25.9614434297919,
12.));
#182847=CARTESIAN_POINT('Ctrl Pts',(-0.669451306780837,-25.9765104298071,
12.));
#182848=CARTESIAN_POINT('Ctrl Pts',(-0.664028313187638,-25.9865613464773,
12.));
#182849=CARTESIAN_POINT('Ctrl Pts',(-0.661312440730913,-25.991588367311,
12.));
#182850=CARTESIAN_POINT('',(0.66131244073089,-25.991588367311,12.));
#182851=CARTESIAN_POINT('Origin',(0.,0.,12.));
#182852=CARTESIAN_POINT('',(1.76341220531179,-22.4835757167854,12.));
#182853=CARTESIAN_POINT('Ctrl Pts',(0.66131244073089,-25.991588367311,12.));
#182854=CARTESIAN_POINT('Ctrl Pts',(0.664028313188911,-25.9865613464809,
12.));
#182855=CARTESIAN_POINT('Ctrl Pts',(0.669451306784414,-25.9765104298171,
12.));
#182856=CARTESIAN_POINT('Ctrl Pts',(0.677559543215902,-25.9614434298092,
12.));
#182857=CARTESIAN_POINT('Ctrl Pts',(0.688318015065675,-25.941372847213,
12.));
#182858=CARTESIAN_POINT('Ctrl Pts',(0.701678575236601,-25.9163158909645,
12.));
#182859=CARTESIAN_POINT('Ctrl Pts',(0.714951588533752,-25.8912902615141,
12.));
#182860=CARTESIAN_POINT('Ctrl Pts',(0.728137036485876,-25.8662960624285,
12.));
#182861=CARTESIAN_POINT('Ctrl Pts',(0.741234902664695,-25.841333461908,
12.));
#182862=CARTESIAN_POINT('Ctrl Pts',(0.754245175608287,-25.816402705995,
12.));
#182863=CARTESIAN_POINT('Ctrl Pts',(0.767167852648638,-25.7915041383304,
12.));
#182864=CARTESIAN_POINT('Ctrl Pts',(0.780002940289024,-25.7666381946871,
12.));
#182865=CARTESIAN_POINT('Ctrl Pts',(0.792750451613533,-25.7418053757671,
12.));
#182866=CARTESIAN_POINT('Ctrl Pts',(0.805410404552592,-25.7170062262474,
12.));
#182867=CARTESIAN_POINT('Ctrl Pts',(0.817982819786718,-25.6922413110172,
12.));
#182868=CARTESIAN_POINT('Ctrl Pts',(0.830467718864366,-25.6675111931957,
12.));
#182869=CARTESIAN_POINT('Ctrl Pts',(0.842865122121542,-25.6428164100078,
12.));
#182870=CARTESIAN_POINT('Ctrl Pts',(0.855175047037614,-25.618157453608,
12.));
#182871=CARTESIAN_POINT('Ctrl Pts',(0.867397509339468,-25.5935347843616,
12.));
#182872=CARTESIAN_POINT('Ctrl Pts',(0.879532523835088,-25.568948840818,
12.));
#182873=CARTESIAN_POINT('Ctrl Pts',(0.891580105349464,-25.5444000508223,
12.));
#182874=CARTESIAN_POINT('Ctrl Pts',(0.903540269651152,-25.5198888424195,
12.));
#182875=CARTESIAN_POINT('Ctrl Pts',(0.915413034335331,-25.4954156541787,
12.));
#182876=CARTESIAN_POINT('Ctrl Pts',(0.927198419885603,-25.4709809474996,
12.));
#182877=CARTESIAN_POINT('Ctrl Pts',(0.938896449495631,-25.4465852044835,
12.));
#182878=CARTESIAN_POINT('Ctrl Pts',(0.950507148596967,-25.4222289223155,
12.));
#182879=CARTESIAN_POINT('Ctrl Pts',(0.962030544502801,-25.3979126089155,
12.));
#182880=CARTESIAN_POINT('Ctrl Pts',(0.973466666000047,-25.3736367778842,
12.));
#182881=CARTESIAN_POINT('Ctrl Pts',(0.984815543004088,-25.3494019441444,
12.));
#182882=CARTESIAN_POINT('Ctrl Pts',(0.996077206120918,-25.3252086182976,
12.));
#182883=CARTESIAN_POINT('Ctrl Pts',(1.00725168656933,-25.3010573055557,
12.));
#182884=CARTESIAN_POINT('Ctrl Pts',(1.01833901642272,-25.2769485087268,
12.));
#182885=CARTESIAN_POINT('Ctrl Pts',(1.0293392287683,-25.2528827300427,12.));
#182886=CARTESIAN_POINT('Ctrl Pts',(1.04025235791514,-25.2288604735087,
12.));
#182887=CARTESIAN_POINT('Ctrl Pts',(1.05107843957925,-25.2048822469027,
12.));
#182888=CARTESIAN_POINT('Ctrl Pts',(1.06181751111754,-25.1809485642191,
12.));
#182889=CARTESIAN_POINT('Ctrl Pts',(1.07246961165459,-25.1570599469311,
12.));
#182890=CARTESIAN_POINT('Ctrl Pts',(1.08303478197174,-25.1332169227415,
12.));
#182891=CARTESIAN_POINT('Ctrl Pts',(1.09351306445299,-25.1094200248448,
12.));
#182892=CARTESIAN_POINT('Ctrl Pts',(1.1039045030174,-25.085669790968,12.));
#182893=CARTESIAN_POINT('Ctrl Pts',(1.1142091430689,-25.0619667625336,12.));
#182894=CARTESIAN_POINT('Ctrl Pts',(1.12442703144455,-25.0383114836898,
12.));
#182895=CARTESIAN_POINT('Ctrl Pts',(1.13455821638535,-25.0147045006193,
12.));
#182896=CARTESIAN_POINT('Ctrl Pts',(1.14460274758206,-24.9911463621431,
12.));
#182897=CARTESIAN_POINT('Ctrl Pts',(1.15456067621894,-24.9676376201501,
12.));
#182898=CARTESIAN_POINT('Ctrl Pts',(1.16443205502852,-24.9441788300932,
12.));
#182899=CARTESIAN_POINT('Ctrl Pts',(1.17421693835039,-24.9207705514449,
12.));
#182900=CARTESIAN_POINT('Ctrl Pts',(1.18391538220098,-24.8974133481829,
12.));
#182901=CARTESIAN_POINT('Ctrl Pts',(1.19352744434059,-24.8741077892074,
12.));
#182902=CARTESIAN_POINT('Ctrl Pts',(1.20305318426015,-24.8508544481973,
12.));
#182903=CARTESIAN_POINT('Ctrl Pts',(1.21249266318205,-24.8276539035092,
12.));
#182904=CARTESIAN_POINT('Ctrl Pts',(1.22184594406526,-24.8045067380536,
12.));
#182905=CARTESIAN_POINT('Ctrl Pts',(1.23111309161843,-24.78141353918,12.));
#182906=CARTESIAN_POINT('Ctrl Pts',(1.24029417231987,-24.7583748985439,
12.));
#182907=CARTESIAN_POINT('Ctrl Pts',(1.24938925444323,-24.7353914120012,
12.));
#182908=CARTESIAN_POINT('Ctrl Pts',(1.25839840807414,-24.7124636797895,
12.));
#182909=CARTESIAN_POINT('Ctrl Pts',(1.26732170513497,-24.6895923066837,
12.));
#182910=CARTESIAN_POINT('Ctrl Pts',(1.2761592194164,-24.666777902156,12.));
#182911=CARTESIAN_POINT('Ctrl Pts',(1.28491102661513,-24.6440210805278,
12.));
#182912=CARTESIAN_POINT('Ctrl Pts',(1.29357720438107,-24.6213224611228,
12.));
#182913=CARTESIAN_POINT('Ctrl Pts',(1.30215783236363,-24.5986826684025,
12.));
#182914=CARTESIAN_POINT('Ctrl Pts',(1.31065299222023,-24.576102332018,12.));
#182915=CARTESIAN_POINT('Ctrl Pts',(1.31906276763669,-24.5535820868671,
12.));
#182916=CARTESIAN_POINT('Ctrl Pts',(1.32738724435326,-24.5311225731434,
12.));
#182917=CARTESIAN_POINT('Ctrl Pts',(1.33562651019684,-24.5087244363856,
12.));
#182918=CARTESIAN_POINT('Ctrl Pts',(1.34378065512335,-24.4863883275135,
12.));
#182919=CARTESIAN_POINT('Ctrl Pts',(1.35184977125644,-24.4641149028894,
12.));
#182920=CARTESIAN_POINT('Ctrl Pts',(1.35983395290624,-24.4419048244524,
12.));
#182921=CARTESIAN_POINT('Ctrl Pts',(1.36773329659954,-24.4197587598337,
12.));
#182922=CARTESIAN_POINT('Ctrl Pts',(1.37554790111607,-24.3976773824731,
12.));
#182923=CARTESIAN_POINT('Ctrl Pts',(1.38327786752998,-24.37566137173,12.));
#182924=CARTESIAN_POINT('Ctrl Pts',(1.3909232992639,-24.3537114129877,12.));
#182925=CARTESIAN_POINT('Ctrl Pts',(1.3984843021281,-24.3318281977647,12.));
#182926=CARTESIAN_POINT('Ctrl Pts',(1.4059609843434,-24.3100124238316,12.));
#182927=CARTESIAN_POINT('Ctrl Pts',(1.41335345657684,-24.2882647953214,
12.));
#182928=CARTESIAN_POINT('Ctrl Pts',(1.42066183198252,-24.2665860228357,
12.));
#182929=CARTESIAN_POINT('Ctrl Pts',(1.42788622624851,-24.2449768235485,
12.));
#182930=CARTESIAN_POINT('Ctrl Pts',(1.43502675765502,-24.2234379212978,
12.));
#182931=CARTESIAN_POINT('Ctrl Pts',(1.44208354711074,-24.2019700467214,
12.));
#182932=CARTESIAN_POINT('Ctrl Pts',(1.4490567181872,-24.1805739374033,12.));
#182933=CARTESIAN_POINT('Ctrl Pts',(1.45594639716314,-24.1592503380105,
12.));
#182934=CARTESIAN_POINT('Ctrl Pts',(1.46275271307398,-24.1380000004272,
12.));
#182935=CARTESIAN_POINT('Ctrl Pts',(1.46947579776991,-24.1168236838827,
12.));
#182936=CARTESIAN_POINT('Ctrl Pts',(1.47611578597741,-24.0957221550782,
12.));
#182937=CARTESIAN_POINT('Ctrl Pts',(1.4826728153368,-24.074696188353,12.));
#182938=CARTESIAN_POINT('Ctrl Pts',(1.48914702644883,-24.053746565843,12.));
#182939=CARTESIAN_POINT('Ctrl Pts',(1.49553856292798,-24.0328740776331,
12.));
#182940=CARTESIAN_POINT('Ctrl Pts',(1.50184757146099,-24.0120795219086,
12.));
#182941=CARTESIAN_POINT('Ctrl Pts',(1.50807420187702,-23.991363705093,12.));
#182942=CARTESIAN_POINT('Ctrl Pts',(1.51421860720628,-23.9707274420145,
12.));
#182943=CARTESIAN_POINT('Ctrl Pts',(1.52028094372806,-23.9501715561038,
12.));
#182944=CARTESIAN_POINT('Ctrl Pts',(1.52626137103039,-23.9296968795761,
12.));
#182945=CARTESIAN_POINT('Ctrl Pts',(1.53216005207462,-23.9093042536119,
12.));
#182946=CARTESIAN_POINT('Ctrl Pts',(1.53797715326748,-23.8889945285313,
12.));
#182947=CARTESIAN_POINT('Ctrl Pts',(1.54371284453977,-23.8687685639635,
12.));
#182948=CARTESIAN_POINT('Ctrl Pts',(1.5493672994053,-23.8486272290698,12.));
#182949=CARTESIAN_POINT('Ctrl Pts',(1.55494069502627,-23.8285714027631,
12.));
#182950=CARTESIAN_POINT('Ctrl Pts',(1.56043321228631,-23.8086019739192,
12.));
#182951=CARTESIAN_POINT('Ctrl Pts',(1.56584503586844,-23.788719841588,12.));
#182952=CARTESIAN_POINT('Ctrl Pts',(1.57117635434412,-23.7689259151869,
12.));
#182953=CARTESIAN_POINT('Ctrl Pts',(1.57642736025251,-23.7492211147369,
12.));
#182954=CARTESIAN_POINT('Ctrl Pts',(1.58159825017362,-23.7296063711308,
12.));
#182955=CARTESIAN_POINT('Ctrl Pts',(1.58668922481222,-23.7100826263835,
12.));
#182956=CARTESIAN_POINT('Ctrl Pts',(1.59170048908631,-23.6906508338833,
12.));
#182957=CARTESIAN_POINT('Ctrl Pts',(1.59663225222458,-23.6713119586302,
12.));
#182958=CARTESIAN_POINT('Ctrl Pts',(1.60148472786588,-23.6520669774863,
12.));
#182959=CARTESIAN_POINT('Ctrl Pts',(1.60625813414666,-23.6329168794916,
12.));
#182960=CARTESIAN_POINT('Ctrl Pts',(1.61095269379773,-23.6138626661644,
12.));
#182961=CARTESIAN_POINT('Ctrl Pts',(1.61556863424697,-23.5949053517996,
12.));
#182962=CARTESIAN_POINT('Ctrl Pts',(1.62010618772869,-23.5760459637608,
12.));
#182963=CARTESIAN_POINT('Ctrl Pts',(1.62456559140071,-23.5572855427617,
12.));
#182964=CARTESIAN_POINT('Ctrl Pts',(1.62894708745231,-23.5386251432278,
12.));
#182965=CARTESIAN_POINT('Ctrl Pts',(1.63325092321731,-23.5200658336624,
12.));
#182966=CARTESIAN_POINT('Ctrl Pts',(1.63747735129474,-23.5016086970006,
12.));
#182967=CARTESIAN_POINT('Ctrl Pts',(1.64162662967524,-23.4832548309638,
12.));
#182968=CARTESIAN_POINT('Ctrl Pts',(1.64569902187608,-23.4650053483919,
12.));
#182969=CARTESIAN_POINT('Ctrl Pts',(1.64969479707339,-23.446861377656,12.));
#182970=CARTESIAN_POINT('Ctrl Pts',(1.6536142302373,-23.4288240631034,12.));
#182971=CARTESIAN_POINT('Ctrl Pts',(1.65745760227507,-23.4108945654803,
12.));
#182972=CARTESIAN_POINT('Ctrl Pts',(1.66122520018008,-23.3930740623622,
12.));
#182973=CARTESIAN_POINT('Ctrl Pts',(1.66491731718864,-23.375363748555,12.));
#182974=CARTESIAN_POINT('Ctrl Pts',(1.66853425293977,-23.3577648365747,
12.));
#182975=CARTESIAN_POINT('Ctrl Pts',(1.67207631363905,-23.3402785571866,
12.));
#182976=CARTESIAN_POINT('Ctrl Pts',(1.67554381222987,-23.3229061599145,
12.));
#182977=CARTESIAN_POINT('Ctrl Pts',(1.67893706857123,-23.3056489135611,
12.));
#182978=CARTESIAN_POINT('Ctrl Pts',(1.68225640962181,-23.2885081066949,
12.));
#182979=CARTESIAN_POINT('Ctrl Pts',(1.68550216963274,-23.2714850482245,
12.));
#182980=CARTESIAN_POINT('Ctrl Pts',(1.6886746903491,-23.2545810680536,12.));
#182981=CARTESIAN_POINT('Ctrl Pts',(1.69177432121716,-23.2377975177014,
12.));
#182982=CARTESIAN_POINT('Ctrl Pts',(1.69480141959945,-23.2211357709374,
12.));
#182983=CARTESIAN_POINT('Ctrl Pts',(1.69775635099425,-23.2045972243765,
12.));
#182984=CARTESIAN_POINT('Ctrl Pts',(1.70063948926987,-23.1881832981848,
12.));
#182985=CARTESIAN_POINT('Ctrl Pts',(1.70345121691259,-23.1718954368749,
12.));
#182986=CARTESIAN_POINT('Ctrl Pts',(1.70619192527846,-23.1557351100613,
12.));
#182987=CARTESIAN_POINT('Ctrl Pts',(1.70886201485459,-23.1397038132358,
12.));
#182988=CARTESIAN_POINT('Ctrl Pts',(1.71146189552192,-23.1238030684929,
12.));
#182989=CARTESIAN_POINT('Ctrl Pts',(1.71399198684724,-23.1080344254291,
12.));
#182990=CARTESIAN_POINT('Ctrl Pts',(1.71645271839311,-23.0923994621216,
12.));
#182991=CARTESIAN_POINT('Ctrl Pts',(1.71884453003027,-23.0768997860709,
12.));
#182992=CARTESIAN_POINT('Ctrl Pts',(1.7211678722598,-23.061537035156,12.));
#182993=CARTESIAN_POINT('Ctrl Pts',(1.72342320653731,-23.0463128785528,
12.));
#182994=CARTESIAN_POINT('Ctrl Pts',(1.72561100564033,-23.031229017888,12.));
#182995=CARTESIAN_POINT('Ctrl Pts',(1.72773175404702,-23.0162871884167,
12.));
#182996=CARTESIAN_POINT('Ctrl Pts',(1.72978594832137,-23.0014891601891,
12.));
#182997=CARTESIAN_POINT('Ctrl Pts',(1.73177409750193,-22.9868367391978,
12.));
#182998=CARTESIAN_POINT('Ctrl Pts',(1.73369672350817,-22.9723317685688,
12.));
#182999=CARTESIAN_POINT('Ctrl Pts',(1.73555436162771,-22.9579761301062,
12.));
#183000=CARTESIAN_POINT('Ctrl Pts',(1.73734756100038,-22.9437717457825,
12.));
#183001=CARTESIAN_POINT('Ctrl Pts',(1.73907688511664,-22.9297205792587,
12.));
#183002=CARTESIAN_POINT('Ctrl Pts',(1.74074291231056,-22.9158246373365,
12.));
#183003=CARTESIAN_POINT('Ctrl Pts',(1.74234623630079,-22.9020859716144,
12.));
#183004=CARTESIAN_POINT('Ctrl Pts',(1.74388746677702,-22.8885066803351,
12.));
#183005=CARTESIAN_POINT('Ctrl Pts',(1.74536722998199,-22.8750889101696,
12.));
#183006=CARTESIAN_POINT('Ctrl Pts',(1.74678616930663,-22.8618348580234,
12.));
#183007=CARTESIAN_POINT('Ctrl Pts',(1.74814494588491,-22.8487467728075,
12.));
#183008=CARTESIAN_POINT('Ctrl Pts',(1.74944423940117,-22.8358269579854,
12.));
#183009=CARTESIAN_POINT('Ctrl Pts',(1.75068474890883,-22.8230777741285,
12.));
#183010=CARTESIAN_POINT('Ctrl Pts',(1.75186719365589,-22.8105016414712,
12.));
#183011=CARTESIAN_POINT('Ctrl Pts',(1.75299231391461,-22.7981010424312,
12.));
#183012=CARTESIAN_POINT('Ctrl Pts',(1.75406087182929,-22.7858785242358,
12.));
#183013=CARTESIAN_POINT('Ctrl Pts',(1.75507365227127,-22.7738367016115,
12.));
#183014=CARTESIAN_POINT('Ctrl Pts',(1.7560314637164,-22.7619782595013,12.));
#183015=CARTESIAN_POINT('Ctrl Pts',(1.75693513908911,-22.7503059556455,
12.));
#183016=CARTESIAN_POINT('Ctrl Pts',(1.75778553673249,-22.7388226235565,
12.));
#183017=CARTESIAN_POINT('Ctrl Pts',(1.75858354204634,-22.7275311777305,
12.));
#183018=CARTESIAN_POINT('Ctrl Pts',(1.75933006905924,-22.7164346186007,
12.));
#183019=CARTESIAN_POINT('Ctrl Pts',(1.76002606202398,-22.7055360375481,
12.));
#183020=CARTESIAN_POINT('Ctrl Pts',(1.76067249704884,-22.6948386219843,
12.));
#183021=CARTESIAN_POINT('Ctrl Pts',(1.76127038310612,-22.6843456585245,
12.));
#183022=CARTESIAN_POINT('Ctrl Pts',(1.76182076289525,-22.6740605356699,
12.));
#183023=CARTESIAN_POINT('Ctrl Pts',(1.76232471392567,-22.6639867471756,
12.));
#183024=CARTESIAN_POINT('Ctrl Pts',(1.76278334912559,-22.6541278938413,
12.));
#183025=CARTESIAN_POINT('Ctrl Pts',(1.76319782013913,-22.6444876940425,
12.));
#183026=CARTESIAN_POINT('Ctrl Pts',(1.76356932176272,-22.635069997936,12.));
#183027=CARTESIAN_POINT('Ctrl Pts',(1.76389909571402,-22.6258787994847,
12.));
#183028=CARTESIAN_POINT('Ctrl Pts',(1.76418843543739,-22.6169182517693,
12.));
#183029=CARTESIAN_POINT('Ctrl Pts',(1.76443868648015,-22.6081926681342,
12.));
#183030=CARTESIAN_POINT('Ctrl Pts',(1.76465124413556,-22.5997065145638,
12.));
#183031=CARTESIAN_POINT('Ctrl Pts',(1.76482755288411,-22.5914644078106,
12.));
#183032=CARTESIAN_POINT('Ctrl Pts',(1.76496910283088,-22.5834711038024,
12.));
#183033=CARTESIAN_POINT('Ctrl Pts',(1.76507744026747,-22.5757315316355,
12.));
#183034=CARTESIAN_POINT('Ctrl Pts',(1.76515418518829,-22.5682508499873,
12.));
#183035=CARTESIAN_POINT('Ctrl Pts',(1.76520104500449,-22.5610344912501,
12.));
#183036=CARTESIAN_POINT('Ctrl Pts',(1.76521983384062,-22.5540882235837,
12.));
#183037=CARTESIAN_POINT('Ctrl Pts',(1.76521245524047,-22.5474180954006,
12.));
#183038=CARTESIAN_POINT('Ctrl Pts',(1.76518087841492,-22.5410303590891,
12.));
#183039=CARTESIAN_POINT('Ctrl Pts',(1.7651271156325,-22.5349313983571,12.));
#183040=CARTESIAN_POINT('Ctrl Pts',(1.76505320262751,-22.529127665298,12.));
#183041=CARTESIAN_POINT('Ctrl Pts',(1.76496128643369,-22.5236259635515,
12.));
#183042=CARTESIAN_POINT('Ctrl Pts',(1.76485369319896,-22.5184336670207,
12.));
#183043=CARTESIAN_POINT('Ctrl Pts',(1.76473303281158,-22.5135590569554,
12.));
#183044=CARTESIAN_POINT('Ctrl Pts',(1.76460218257323,-22.5090112700212,
12.));
#183045=CARTESIAN_POINT('Ctrl Pts',(1.76446408210366,-22.5047996391978,
12.));
#183046=CARTESIAN_POINT('Ctrl Pts',(1.76432160068725,-22.5009332677316,
12.));
#183047=CARTESIAN_POINT('Ctrl Pts',(1.76417731243462,-22.4974203063191,
12.));
#183048=CARTESIAN_POINT('Ctrl Pts',(1.764033938803,-22.4942693792449,12.));
#183049=CARTESIAN_POINT('Ctrl Pts',(1.76389475965723,-22.4914909094908,
12.));
#183050=CARTESIAN_POINT('Ctrl Pts',(1.76376424879504,-22.4890991659478,
12.));
#183051=CARTESIAN_POINT('Ctrl Pts',(1.76364784232963,-22.4871115206571,
12.));
#183052=CARTESIAN_POINT('Ctrl Pts',(1.76355076045546,-22.4855446605991,
12.));
#183053=CARTESIAN_POINT('Ctrl Pts',(1.76347698284791,-22.4844112933129,
12.));
#183054=CARTESIAN_POINT('Ctrl Pts',(1.76343813434565,-22.483856251707,12.));
#183055=CARTESIAN_POINT('Ctrl Pts',(1.7634206426357,-22.4836387052232,12.));
#183056=CARTESIAN_POINT('Ctrl Pts',(1.76341415538764,-22.483581992979,12.));
#183057=CARTESIAN_POINT('Ctrl Pts',(1.76341220531179,-22.4835757167854,
12.));
#183058=CARTESIAN_POINT('',(1.71975774210841,-21.9269795755927,12.));
#183059=CARTESIAN_POINT('',(0.840553282521226,-10.7170877657712,12.));
#183060=CARTESIAN_POINT('',(2.16781269186827,-21.3904321633055,12.));
#183061=CARTESIAN_POINT('Origin',(2.21822694051637,-21.8878840740801,12.));
#183062=CARTESIAN_POINT('',(3.44230496120418,-21.2226420728916,12.));
#183063=CARTESIAN_POINT('Origin',(7.16093850883225E-14,-7.7715611723761E-13,
12.));
#183064=CARTESIAN_POINT('',(4.01396149767428,-21.624941921198,12.));
#183065=CARTESIAN_POINT('Origin',(3.52235856495312,-21.7161918885403,12.));
#183066=CARTESIAN_POINT('',(4.11585220600461,-22.1738711152697,12.));
#183067=CARTESIAN_POINT('',(2.05792610300232,-11.0869355576349,12.));
#183068=CARTESIAN_POINT('',(6.08833931617698,-25.2771067246846,12.));
#183069=CARTESIAN_POINT('Ctrl Pts',(4.11585220600461,-22.1738711152697,
12.));
#183070=CARTESIAN_POINT('Ctrl Pts',(4.11585194677412,-22.1738776823239,
12.));
#183071=CARTESIAN_POINT('Ctrl Pts',(4.1158603587821,-22.1739341411684,12.));
#183072=CARTESIAN_POINT('Ctrl Pts',(4.11589976826061,-22.174148802123,12.));
#183073=CARTESIAN_POINT('Ctrl Pts',(4.11600589882767,-22.1746949858773,
12.));
#183074=CARTESIAN_POINT('Ctrl Pts',(4.11622797217066,-22.1758088296598,
12.));
#183075=CARTESIAN_POINT('Ctrl Pts',(4.11653973150558,-22.177347426894,12.));
#183076=CARTESIAN_POINT('Ctrl Pts',(4.11694173195041,-22.179297473024,12.));
#183077=CARTESIAN_POINT('Ctrl Pts',(4.11743469691765,-22.1816414985788,
12.));
#183078=CARTESIAN_POINT('Ctrl Pts',(4.11801938107464,-22.1843613164855,
12.));
#183079=CARTESIAN_POINT('Ctrl Pts',(4.11869641271752,-22.1874419861496,
12.));
#183080=CARTESIAN_POINT('Ctrl Pts',(4.11946626228623,-22.1908725908525,
12.));
#183081=CARTESIAN_POINT('Ctrl Pts',(4.12032932637738,-22.1946440958098,
12.));
#183082=CARTESIAN_POINT('Ctrl Pts',(4.12128598183533,-22.1987479618246,
12.));
#183083=CARTESIAN_POINT('Ctrl Pts',(4.12233664408237,-22.2031746532106,
12.));
#183084=CARTESIAN_POINT('Ctrl Pts',(4.12348173702024,-22.2079143941719,
12.));
#183085=CARTESIAN_POINT('Ctrl Pts',(4.12472167516602,-22.2129576146671,
12.));
#183086=CARTESIAN_POINT('Ctrl Pts',(4.12605683613299,-22.2182956401341,
12.));
#183087=CARTESIAN_POINT('Ctrl Pts',(4.12748755830099,-22.2239207458781,
12.));
#183088=CARTESIAN_POINT('Ctrl Pts',(4.12901415463378,-22.2298258043947,
12.));
#183089=CARTESIAN_POINT('Ctrl Pts',(4.13063692157499,-22.2360040565534,
12.));
#183090=CARTESIAN_POINT('Ctrl Pts',(4.1323561506016,-22.2424488153523,12.));
#183091=CARTESIAN_POINT('Ctrl Pts',(4.13417212558808,-22.2491535317789,
12.));
#183092=CARTESIAN_POINT('Ctrl Pts',(4.13608511977226,-22.2561118708422,
12.));
#183093=CARTESIAN_POINT('Ctrl Pts',(4.13809539255418,-22.263317791397,12.));
#183094=CARTESIAN_POINT('Ctrl Pts',(4.14020318715987,-22.2707656042456,
12.));
#183095=CARTESIAN_POINT('Ctrl Pts',(4.14240873321982,-22.2784499072026,
12.));
#183096=CARTESIAN_POINT('Ctrl Pts',(4.14471224859295,-22.2863655389167,
12.));
#183097=CARTESIAN_POINT('Ctrl Pts',(4.14711394168559,-22.2945075198468,
12.));
#183098=CARTESIAN_POINT('Ctrl Pts',(4.14961401285525,-22.3028710166935,
12.));
#183099=CARTESIAN_POINT('Ctrl Pts',(4.15221265396992,-22.3114513545186,
12.));
#183100=CARTESIAN_POINT('Ctrl Pts',(4.15491004835278,-22.3202440186979,
12.));
#183101=CARTESIAN_POINT('Ctrl Pts',(4.15770637047882,-22.3292446628957,
12.));
#183102=CARTESIAN_POINT('Ctrl Pts',(4.16060178604153,-22.3384491078599,
12.));
#183103=CARTESIAN_POINT('Ctrl Pts',(4.1635964526318,-22.3478533253886,12.));
#183104=CARTESIAN_POINT('Ctrl Pts',(4.16669052026602,-22.3574534257397,
12.));
#183105=CARTESIAN_POINT('Ctrl Pts',(4.16988413199469,-22.3672456427605,
12.));
#183106=CARTESIAN_POINT('Ctrl Pts',(4.17317742436162,-22.3772263228624,
12.));
#183107=CARTESIAN_POINT('Ctrl Pts',(4.17657052752834,-22.3873919231339,
12.));
#183108=CARTESIAN_POINT('Ctrl Pts',(4.18006356544879,-22.3977390078074,
12.));
#183109=CARTESIAN_POINT('Ctrl Pts',(4.18365665600839,-22.4082642454448,
12.));
#183110=CARTESIAN_POINT('Ctrl Pts',(4.18734991117707,-22.4189644056109,
12.));
#183111=CARTESIAN_POINT('Ctrl Pts',(4.19114343726932,-22.4298363535416,
12.));
#183112=CARTESIAN_POINT('Ctrl Pts',(4.1950373351886,-22.4408770448917,12.));
#183113=CARTESIAN_POINT('Ctrl Pts',(4.19903170066358,-22.4520835205422,
12.));
#183114=CARTESIAN_POINT('Ctrl Pts',(4.20312662448174,-22.4634529011437,
12.));
#183115=CARTESIAN_POINT('Ctrl Pts',(4.20732219265648,-22.4749823839917,
12.));
#183116=CARTESIAN_POINT('Ctrl Pts',(4.21161848657428,-22.4866692403147,
12.));
#183117=CARTESIAN_POINT('Ctrl Pts',(4.21601558313906,-22.4985108124228,
12.));
#183118=CARTESIAN_POINT('Ctrl Pts',(4.22051355490196,-22.5105045108881,
12.));
#183119=CARTESIAN_POINT('Ctrl Pts',(4.22511247020041,-22.5226478117886,
12.));
#183120=CARTESIAN_POINT('Ctrl Pts',(4.22981239330733,-22.5349382540588,
12.));
#183121=CARTESIAN_POINT('Ctrl Pts',(4.23461338456712,-22.5473734368086,
12.));
#183122=CARTESIAN_POINT('Ctrl Pts',(4.23951550052522,-22.5599510166429,
12.));
#183123=CARTESIAN_POINT('Ctrl Pts',(4.24451879404851,-22.572668704992,12.));
#183124=CARTESIAN_POINT('Ctrl Pts',(4.24962331444177,-22.5855242662477,
12.));
#183125=CARTESIAN_POINT('Ctrl Pts',(4.25482910755481,-22.5985155158636,
12.));
#183126=CARTESIAN_POINT('Ctrl Pts',(4.26013621588305,-22.6116403184821,
12.));
#183127=CARTESIAN_POINT('Ctrl Pts',(4.26554467865576,-22.6248965859977,
12.));
#183128=CARTESIAN_POINT('Ctrl Pts',(4.27105453193004,-22.6382822758172,
12.));
#183129=CARTESIAN_POINT('Ctrl Pts',(4.2766658086912,-22.6517953893303,12.));
#183130=CARTESIAN_POINT('Ctrl Pts',(4.28237853894058,-22.6654339703109,
12.));
#183131=CARTESIAN_POINT('Ctrl Pts',(4.28819274977763,-22.6791961033538,
12.));
#183132=CARTESIAN_POINT('Ctrl Pts',(4.29410846547056,-22.6930799122548,
12.));
#183133=CARTESIAN_POINT('Ctrl Pts',(4.3001257075406,-22.7070835587564,12.));
#183134=CARTESIAN_POINT('Ctrl Pts',(4.30624449484069,-22.7212052413386,
12.));
#183135=CARTESIAN_POINT('Ctrl Pts',(4.31246484362549,-22.7354431939926,
12.));
#183136=CARTESIAN_POINT('Ctrl Pts',(4.31878676761235,-22.7497956849848,
12.));
#183137=CARTESIAN_POINT('Ctrl Pts',(4.32521027803754,-22.7642610156475,
12.));
#183138=CARTESIAN_POINT('Ctrl Pts',(4.33173538373189,-22.7788375194076,
12.));
#183139=CARTESIAN_POINT('Ctrl Pts',(4.33836209118446,-22.7935235607806,
12.));
#183140=CARTESIAN_POINT('Ctrl Pts',(4.34509040460062,-22.8083175343791,
12.));
#183141=CARTESIAN_POINT('Ctrl Pts',(4.3519203259479,-22.8232178638876,12.));
#183142=CARTESIAN_POINT('Ctrl Pts',(4.35885185500546,-22.8382230011184,
12.));
#183143=CARTESIAN_POINT('Ctrl Pts',(4.36588498942997,-22.8533314252422,
12.));
#183144=CARTESIAN_POINT('Ctrl Pts',(4.37301972480745,-22.8685416419725,
12.));
#183145=CARTESIAN_POINT('Ctrl Pts',(4.38025605470092,-22.8838521827701,
12.));
#183146=CARTESIAN_POINT('Ctrl Pts',(4.38759397068405,-22.8992616040108,
12.));
#183147=CARTESIAN_POINT('Ctrl Pts',(4.39503346238473,-22.9147684862426,
12.));
#183148=CARTESIAN_POINT('Ctrl Pts',(4.40257451754323,-22.930371433555,12.));
#183149=CARTESIAN_POINT('Ctrl Pts',(4.41021712205553,-22.9460690729093,
12.));
#183150=CARTESIAN_POINT('Ctrl Pts',(4.41796126001302,-22.9618600534866,
12.));
#183151=CARTESIAN_POINT('Ctrl Pts',(4.42580691372751,-22.977743046002,12.));
#183152=CARTESIAN_POINT('Ctrl Pts',(4.43375406376879,-22.9937167421006,
12.));
#183153=CARTESIAN_POINT('Ctrl Pts',(4.44180268901643,-23.0097798538395,
12.));
#183154=CARTESIAN_POINT('Ctrl Pts',(4.44995276669686,-23.0259311131392,
12.));
#183155=CARTESIAN_POINT('Ctrl Pts',(4.45820427241683,-23.0421692712467,
12.));
#183156=CARTESIAN_POINT('Ctrl Pts',(4.4665571801823,-23.0584930981732,12.));
#183157=CARTESIAN_POINT('Ctrl Pts',(4.47501146242856,-23.0749013821881,
12.));
#183158=CARTESIAN_POINT('Ctrl Pts',(4.48356709006788,-23.0913929293922,
12.));
#183159=CARTESIAN_POINT('Ctrl Pts',(4.49222403252216,-23.1079665632636,
12.));
#183160=CARTESIAN_POINT('Ctrl Pts',(4.50098225775171,-23.1246211242115,
12.));
#183161=CARTESIAN_POINT('Ctrl Pts',(4.5098417322706,-23.1413554691123,12.));
#183162=CARTESIAN_POINT('Ctrl Pts',(4.51880242116748,-23.1581684708761,
12.));
#183163=CARTESIAN_POINT('Ctrl Pts',(4.52786428815014,-23.1750590180908,
12.));
#183164=CARTESIAN_POINT('Ctrl Pts',(4.53702729557566,-23.1920260146465,
12.));
#183165=CARTESIAN_POINT('Ctrl Pts',(4.54629140447544,-23.2090683793629,
12.));
#183166=CARTESIAN_POINT('Ctrl Pts',(4.55565657456975,-23.2261850456064,
12.));
#183167=CARTESIAN_POINT('Ctrl Pts',(4.56512276427839,-23.2433749609131,
12.));
#183168=CARTESIAN_POINT('Ctrl Pts',(4.57468993076097,-23.2606370866866,
12.));
#183169=CARTESIAN_POINT('Ctrl Pts',(4.5843580299469,-23.2779703978876,12.));
#183170=CARTESIAN_POINT('Ctrl Pts',(4.5941270165575,-23.2953738827191,12.));
#183171=CARTESIAN_POINT('Ctrl Pts',(4.60399684412163,-23.3128465423115,
12.));
#183172=CARTESIAN_POINT('Ctrl Pts',(4.6139674649783,-23.3303873903938,12.));
#183173=CARTESIAN_POINT('Ctrl Pts',(4.62403883030805,-23.3479954530272,
12.));
#183174=CARTESIAN_POINT('Ctrl Pts',(4.63421089016541,-23.3656697683489,
12.));
#183175=CARTESIAN_POINT('Ctrl Pts',(4.6444835934993,-23.3834093863068,12.));
#183176=CARTESIAN_POINT('Ctrl Pts',(4.65485688816924,-23.4012133683959,
12.));
#183177=CARTESIAN_POINT('Ctrl Pts',(4.6653307209467,-23.4190807873803,12.));
#183178=CARTESIAN_POINT('Ctrl Pts',(4.67590503753058,-23.4370107270451,
12.));
#183179=CARTESIAN_POINT('Ctrl Pts',(4.68657978258303,-23.455002281986,12.));
#183180=CARTESIAN_POINT('Ctrl Pts',(4.69735489975024,-23.4730545573853,
12.));
#183181=CARTESIAN_POINT('Ctrl Pts',(4.70823033167818,-23.491166668789,12.));
#183182=CARTESIAN_POINT('Ctrl Pts',(4.71920602001901,-23.509337741878,12.));
#183183=CARTESIAN_POINT('Ctrl Pts',(4.73028190543029,-23.5275669122372,
12.));
#183184=CARTESIAN_POINT('Ctrl Pts',(4.74145792760698,-23.545853325171,12.));
#183185=CARTESIAN_POINT('Ctrl Pts',(4.75273402530617,-23.5641961355168,
12.));
#183186=CARTESIAN_POINT('Ctrl Pts',(4.76411013636251,-23.5825945074535,
12.));
#183187=CARTESIAN_POINT('Ctrl Pts',(4.77558619769872,-23.6010476143099,
12.));
#183188=CARTESIAN_POINT('Ctrl Pts',(4.78716214532097,-23.6195546383624,
12.));
#183189=CARTESIAN_POINT('Ctrl Pts',(4.7988379143322,-23.6381147706579,12.));
#183190=CARTESIAN_POINT('Ctrl Pts',(4.81061343896432,-23.6567272108628,
12.));
#183191=CARTESIAN_POINT('Ctrl Pts',(4.82248865259562,-23.675391167102,12.));
#183192=CARTESIAN_POINT('Ctrl Pts',(4.83446348776265,-23.6941058557971,
12.));
#183193=CARTESIAN_POINT('Ctrl Pts',(4.84653787616425,-23.7128705015017,
12.));
#183194=CARTESIAN_POINT('Ctrl Pts',(4.85871174865499,-23.7316843367313,
12.));
#183195=CARTESIAN_POINT('Ctrl Pts',(4.87098503527152,-23.7505466018245,
12.));
#183196=CARTESIAN_POINT('Ctrl Pts',(4.88335766525573,-23.7694565448049,
12.));
#183197=CARTESIAN_POINT('Ctrl Pts',(4.89582956706775,-23.7884134212384,
12.));
#183198=CARTESIAN_POINT('Ctrl Pts',(4.90840066839344,-23.8074164940896,
12.));
#183199=CARTESIAN_POINT('Ctrl Pts',(4.92107089613968,-23.8264650335717,
12.));
#183200=CARTESIAN_POINT('Ctrl Pts',(4.93384017643432,-23.8455583170057,
12.));
#183201=CARTESIAN_POINT('Ctrl Pts',(4.9467084346586,-23.8646956287168,12.));
#183202=CARTESIAN_POINT('Ctrl Pts',(4.9596755954656,-23.8838762599218,12.));
#183203=CARTESIAN_POINT('Ctrl Pts',(4.97274158279226,-23.9030995086163,
12.));
#183204=CARTESIAN_POINT('Ctrl Pts',(4.98590631986532,-23.9223646794592,
12.));
#183205=CARTESIAN_POINT('Ctrl Pts',(4.99916972919306,-23.9416710836529,
12.));
#183206=CARTESIAN_POINT('Ctrl Pts',(5.01253173257452,-23.9610180388271,
12.));
#183207=CARTESIAN_POINT('Ctrl Pts',(5.02599225112454,-23.9804048689227,
12.));
#183208=CARTESIAN_POINT('Ctrl Pts',(5.03955120528521,-23.9998309040746,
12.));
#183209=CARTESIAN_POINT('Ctrl Pts',(5.05320851483065,-24.0192954804896,
12.));
#183210=CARTESIAN_POINT('Ctrl Pts',(5.06696409886641,-24.0387979403268,
12.));
#183211=CARTESIAN_POINT('Ctrl Pts',(5.08081787581276,-24.0583376315638,
12.));
#183212=CARTESIAN_POINT('Ctrl Pts',(5.09476976342625,-24.0779139079266,
12.));
#183213=CARTESIAN_POINT('Ctrl Pts',(5.10881967883132,-24.0975261288446,
12.));
#183214=CARTESIAN_POINT('Ctrl Pts',(5.12296753853859,-24.117173659394,12.));
#183215=CARTESIAN_POINT('Ctrl Pts',(5.13721325845744,-24.1368558702443,
12.));
#183216=CARTESIAN_POINT('Ctrl Pts',(5.15155675390075,-24.1565721375971,
12.));
#183217=CARTESIAN_POINT('Ctrl Pts',(5.16599793957979,-24.1763218431343,
12.));
#183218=CARTESIAN_POINT('Ctrl Pts',(5.18053672961392,-24.1961043738754,
12.));
#183219=CARTESIAN_POINT('Ctrl Pts',(5.19517303753642,-24.215919122017,12.));
#183220=CARTESIAN_POINT('Ctrl Pts',(5.20990677629173,-24.2357654847765,
12.));
#183221=CARTESIAN_POINT('Ctrl Pts',(5.22473785822441,-24.2556428642294,
12.));
#183222=CARTESIAN_POINT('Ctrl Pts',(5.23966619506289,-24.2755506671526,
12.));
#183223=CARTESIAN_POINT('Ctrl Pts',(5.25469169788855,-24.2954883048448,
12.));
#183224=CARTESIAN_POINT('Ctrl Pts',(5.26981427718796,-24.3154551932222,
12.));
#183225=CARTESIAN_POINT('Ctrl Pts',(5.28503384290644,-24.3354507529415,
12.));
#183226=CARTESIAN_POINT('Ctrl Pts',(5.30035030449058,-24.3554744095075,
12.));
#183227=CARTESIAN_POINT('Ctrl Pts',(5.31576357092524,-24.3755255933917,
12.));
#183228=CARTESIAN_POINT('Ctrl Pts',(5.33127355076036,-24.3956037401293,
12.));
#183229=CARTESIAN_POINT('Ctrl Pts',(5.34688015213546,-24.4157082904615,
12.));
#183230=CARTESIAN_POINT('Ctrl Pts',(5.36258328273639,-24.4358386899152,
12.));
#183231=CARTESIAN_POINT('Ctrl Pts',(5.37838284973706,-24.4559943883159,
12.));
#183232=CARTESIAN_POINT('Ctrl Pts',(5.3942787597383,-24.4761748393322,12.));
#183233=CARTESIAN_POINT('Ctrl Pts',(5.41027091869242,-24.4963794999831,
12.));
#183234=CARTESIAN_POINT('Ctrl Pts',(5.42635923183411,-24.5166078302107,
12.));
#183235=CARTESIAN_POINT('Ctrl Pts',(5.44254360356865,-24.5368592922861,
12.));
#183236=CARTESIAN_POINT('Ctrl Pts',(5.45882393762244,-24.5571333514841,
12.));
#183237=CARTESIAN_POINT('Ctrl Pts',(5.47520013724403,-24.5774294770329,
12.));
#183238=CARTESIAN_POINT('Ctrl Pts',(5.49167210537235,-24.5977471429365,
12.));
#183239=CARTESIAN_POINT('Ctrl Pts',(5.50823974481959,-24.618085828918,12.));
#183240=CARTESIAN_POINT('Ctrl Pts',(5.52490295840996,-24.6384450211466,
12.));
#183241=CARTESIAN_POINT('Ctrl Pts',(5.54166164919592,-24.6588242134733,
12.));
#183242=CARTESIAN_POINT('Ctrl Pts',(5.55851572025389,-24.6792229061785,
12.));
#183243=CARTESIAN_POINT('Ctrl Pts',(5.57546507427766,-24.6996406035507,
12.));
#183244=CARTESIAN_POINT('Ctrl Pts',(5.59250961323995,-24.7200768119079,
12.));
#183245=CARTESIAN_POINT('Ctrl Pts',(5.60964923798494,-24.7405310372736,
12.));
#183246=CARTESIAN_POINT('Ctrl Pts',(5.62688384790918,-24.76100278357,12.));
#183247=CARTESIAN_POINT('Ctrl Pts',(5.64421334042247,-24.7814915496728,
12.));
#183248=CARTESIAN_POINT('Ctrl Pts',(5.66163761114903,-24.8019968304618,
12.));
#183249=CARTESIAN_POINT('Ctrl Pts',(5.67915655496524,-24.822518122386,12.));
#183250=CARTESIAN_POINT('Ctrl Pts',(5.69677006679429,-24.8430549277634,
12.));
#183251=CARTESIAN_POINT('Ctrl Pts',(5.71447804252019,-24.8636067597677,
12.));
#183252=CARTESIAN_POINT('Ctrl Pts',(5.73228037976926,-24.8841731467219,
12.));
#183253=CARTESIAN_POINT('Ctrl Pts',(5.75017697890812,-24.9047536376467,
12.));
#183254=CARTESIAN_POINT('Ctrl Pts',(5.76816774342236,-24.9253478043632,
12.));
#183255=CARTESIAN_POINT('Ctrl Pts',(5.78625257775702,-24.9459552293308,
12.));
#183256=CARTESIAN_POINT('Ctrl Pts',(5.80443138549747,-24.9665754954463,
12.));
#183257=CARTESIAN_POINT('Ctrl Pts',(5.82270406744213,-24.9872081752709,
12.));
#183258=CARTESIAN_POINT('Ctrl Pts',(5.84107051963073,-25.0078528200558,
12.));
#183259=CARTESIAN_POINT('Ctrl Pts',(5.8595306315681,-25.0285089498922,12.));
#183260=CARTESIAN_POINT('Ctrl Pts',(5.87808428385329,-25.0491760405965,
12.));
#183261=CARTESIAN_POINT('Ctrl Pts',(5.89673135155458,-25.0698535426593,
12.));
#183262=CARTESIAN_POINT('Ctrl Pts',(5.91547170844382,-25.0905409050863,
12.));
#183263=CARTESIAN_POINT('Ctrl Pts',(5.93430523086776,-25.1112375971182,
12.));
#183264=CARTESIAN_POINT('Ctrl Pts',(5.95323180187347,-25.1319431317273,
12.));
#183265=CARTESIAN_POINT('Ctrl Pts',(5.97225131495636,-25.1526570863065,
12.));
#183266=CARTESIAN_POINT('Ctrl Pts',(5.99136367859838,-25.1733791296154,
12.));
#183267=CARTESIAN_POINT('Ctrl Pts',(6.0105688180476,-25.1941090269638,12.));
#183268=CARTESIAN_POINT('Ctrl Pts',(6.02986667390187,-25.2148466201368,
12.));
#183269=CARTESIAN_POINT('Ctrl Pts',(6.04925720151412,-25.2355918138798,
12.));
#183270=CARTESIAN_POINT('Ctrl Pts',(6.06484373634696,-25.2521940105523,
12.));
#183271=CARTESIAN_POINT('Ctrl Pts',(6.07657531787577,-25.2646490489816,
12.));
#183272=CARTESIAN_POINT('Ctrl Pts',(6.08441489609824,-25.2729539149479,
12.));
#183273=CARTESIAN_POINT('Ctrl Pts',(6.08833931617698,-25.2771067246846,
12.));
#183274=CARTESIAN_POINT('',(7.36589684767343,-24.9347862158358,12.));
#183275=CARTESIAN_POINT('Origin',(0.,0.,12.));
#183276=CARTESIAN_POINT('',(7.52250298901263,-21.2610617890679,12.));
#183277=CARTESIAN_POINT('Ctrl Pts',(7.36589684767343,-24.9347862158358,
12.));
#183278=CARTESIAN_POINT('Ctrl Pts',(7.36721909029059,-24.9292275670705,
12.));
#183279=CARTESIAN_POINT('Ctrl Pts',(7.36985593120695,-24.9181155530631,
12.));
#183280=CARTESIAN_POINT('Ctrl Pts',(7.37378825962717,-24.9014633826201,
12.));
#183281=CARTESIAN_POINT('Ctrl Pts',(7.37898549641609,-24.8792921911309,
12.));
#183282=CARTESIAN_POINT('Ctrl Pts',(7.38540558904945,-24.8516310625367,
12.));
#183283=CARTESIAN_POINT('Ctrl Pts',(7.3917492258684,-24.8240228521042,12.));
#183284=CARTESIAN_POINT('Ctrl Pts',(7.39801641583612,-24.7964676646518,
12.));
#183285=CARTESIAN_POINT('Ctrl Pts',(7.40420718661754,-24.7689656669005,
12.));
#183286=CARTESIAN_POINT('Ctrl Pts',(7.41032159082172,-24.7415170994754,
12.));
#183287=CARTESIAN_POINT('Ctrl Pts',(7.41635971481242,-24.7141222949988,
12.));
#183288=CARTESIAN_POINT('Ctrl Pts',(7.42232167765762,-24.6867816727118,
12.));
#183289=CARTESIAN_POINT('Ctrl Pts',(7.4282076215868,-24.659495712869,12.));
#183290=CARTESIAN_POINT('Ctrl Pts',(7.4340177048922,-24.6322649369472,12.));
#183291=CARTESIAN_POINT('Ctrl Pts',(7.43975209375374,-24.6050898852349,
12.));
#183292=CARTESIAN_POINT('Ctrl Pts',(7.44541095473162,-24.5779710960865,
12.));
#183293=CARTESIAN_POINT('Ctrl Pts',(7.45099444651295,-24.550909083158,12.));
#183294=CARTESIAN_POINT('Ctrl Pts',(7.45650271336044,-24.52390431731,12.));
#183295=CARTESIAN_POINT('Ctrl Pts',(7.46193588961641,-24.4969572391509,
12.));
#183296=CARTESIAN_POINT('Ctrl Pts',(7.46729410308922,-24.4700682684544,
12.));
#183297=CARTESIAN_POINT('Ctrl Pts',(7.47257747883318,-24.4432378146501,
12.));
#183298=CARTESIAN_POINT('Ctrl Pts',(7.47778614286572,-24.4164662871165,
12.));
#183299=CARTESIAN_POINT('Ctrl Pts',(7.48292022569253,-24.3897541049248,
12.));
#183300=CARTESIAN_POINT('Ctrl Pts',(7.48797986651827,-24.3631017084513,
12.));
#183301=CARTESIAN_POINT('Ctrl Pts',(7.49296521252329,-24.3365095573673,
12.));
#183302=CARTESIAN_POINT('Ctrl Pts',(7.49787641695358,-24.3099781253345,
12.));
#183303=CARTESIAN_POINT('Ctrl Pts',(7.50271363765098,-24.2835078958966,
12.));
#183304=CARTESIAN_POINT('Ctrl Pts',(7.50747703535114,-24.2570993577032,
12.));
#183305=CARTESIAN_POINT('Ctrl Pts',(7.51216677222198,-24.230753000389,12.));
#183306=CARTESIAN_POINT('Ctrl Pts',(7.51678300997997,-24.2044693092356,
12.));
#183307=CARTESIAN_POINT('Ctrl Pts',(7.52132590953862,-24.1782487641602,
12.));
#183308=CARTESIAN_POINT('Ctrl Pts',(7.52579563201478,-24.152091842537,12.));
#183309=CARTESIAN_POINT('Ctrl Pts',(7.53019233935536,-24.1259990209211,
12.));
#183310=CARTESIAN_POINT('Ctrl Pts',(7.53451619514658,-24.0999707772643,
12.));
#183311=CARTESIAN_POINT('Ctrl Pts',(7.53876736531004,-24.0740075927984,
12.));
#183312=CARTESIAN_POINT('Ctrl Pts',(7.54294601896127,-24.0481099543353,
12.));
#183313=CARTESIAN_POINT('Ctrl Pts',(7.54705232885894,-24.0222783554531,
12.));
#183314=CARTESIAN_POINT('Ctrl Pts',(7.55108647097431,-23.9965132953187,
12.));
#183315=CARTESIAN_POINT('Ctrl Pts',(7.55504862424807,-23.9708152779886,
12.));
#183316=CARTESIAN_POINT('Ctrl Pts',(7.55893897027679,-23.9451848115002,
12.));
#183317=CARTESIAN_POINT('Ctrl Pts',(7.56275769304772,-23.9196224070759,
12.));
#183318=CARTESIAN_POINT('Ctrl Pts',(7.5665049786379,-23.8941285782002,12.));
#183319=CARTESIAN_POINT('Ctrl Pts',(7.57018101500708,-23.8687038399595,
12.));
#183320=CARTESIAN_POINT('Ctrl Pts',(7.57378599219813,-23.8433487096132,
12.));
#183321=CARTESIAN_POINT('Ctrl Pts',(7.57732010249065,-23.8180637069976,
12.));
#183322=CARTESIAN_POINT('Ctrl Pts',(7.58078354058212,-23.7928493549908,
12.));
#183323=CARTESIAN_POINT('Ctrl Pts',(7.5841765037627,-23.7677061799376,12.));
#183324=CARTESIAN_POINT('Ctrl Pts',(7.58749919210825,-23.7426347121006,
12.));
#183325=CARTESIAN_POINT('Ctrl Pts',(7.5907518086532,-23.7176354860457,12.));
#183326=CARTESIAN_POINT('Ctrl Pts',(7.59393455934034,-23.6927090405066,
12.));
#183327=CARTESIAN_POINT('Ctrl Pts',(7.59704765299566,-23.6678559182875,
12.));
#183328=CARTESIAN_POINT('Ctrl Pts',(7.60009130130125,-23.6430766661418,
12.));
#183329=CARTESIAN_POINT('Ctrl Pts',(7.60306571877805,-23.6183718346576,
12.));
#183330=CARTESIAN_POINT('Ctrl Pts',(7.60597112277093,-23.5937419781245,
12.));
#183331=CARTESIAN_POINT('Ctrl Pts',(7.60880773344599,-23.5691876544244,
12.));
#183332=CARTESIAN_POINT('Ctrl Pts',(7.61157577385371,-23.544709425203,12.));
#183333=CARTESIAN_POINT('Ctrl Pts',(7.61427546999297,-23.5203078560129,
12.));
#183334=CARTESIAN_POINT('Ctrl Pts',(7.61690705088318,-23.4959835164609,
12.));
#183335=CARTESIAN_POINT('Ctrl Pts',(7.61947074863976,-23.4717369803438,
12.));
#183336=CARTESIAN_POINT('Ctrl Pts',(7.62196679855954,-23.4475688257854,
12.));
#183337=CARTESIAN_POINT('Ctrl Pts',(7.62439543920049,-23.4234796353542,
12.));
#183338=CARTESIAN_POINT('Ctrl Pts',(7.62675691240328,-23.399469996112,12.));
#183339=CARTESIAN_POINT('Ctrl Pts',(7.62905146332592,-23.3755404996636,
12.));
#183340=CARTESIAN_POINT('Ctrl Pts',(7.63127934048136,-23.3516917421972,
12.));
#183341=CARTESIAN_POINT('Ctrl Pts',(7.63344079578161,-23.3279243245241,
12.));
#183342=CARTESIAN_POINT('Ctrl Pts',(7.63553608458782,-23.3042388521022,
12.));
#183343=CARTESIAN_POINT('Ctrl Pts',(7.63756546576373,-23.2806359350855,
12.));
#183344=CARTESIAN_POINT('Ctrl Pts',(7.63952920172834,-23.2571161884488,
12.));
#183345=CARTESIAN_POINT('Ctrl Pts',(7.64142755851504,-23.2336802320912,
12.));
#183346=CARTESIAN_POINT('Ctrl Pts',(7.64326080583679,-23.2103286909398,
12.));
#183347=CARTESIAN_POINT('Ctrl Pts',(7.64502921715482,-23.1870621950452,
12.));
#183348=CARTESIAN_POINT('Ctrl Pts',(7.64673306975804,-23.1638813796694,
12.));
#183349=CARTESIAN_POINT('Ctrl Pts',(7.64837264482942,-23.1407868853819,
12.));
#183350=CARTESIAN_POINT('Ctrl Pts',(7.64994822749859,-23.1177793581679,
12.));
#183351=CARTESIAN_POINT('Ctrl Pts',(7.65146010690475,-23.094859449525,12.));
#183352=CARTESIAN_POINT('Ctrl Pts',(7.65290857626357,-23.072027816555,12.));
#183353=CARTESIAN_POINT('Ctrl Pts',(7.65429393293945,-23.0492851220528,
12.));
#183354=CARTESIAN_POINT('Ctrl Pts',(7.65561647852533,-23.0266320345787,
12.));
#183355=CARTESIAN_POINT('Ctrl Pts',(7.65687651891303,-23.0040692285814,
12.));
#183356=CARTESIAN_POINT('Ctrl Pts',(7.65807436436431,-22.9815973845296,
12.));
#183357=CARTESIAN_POINT('Ctrl Pts',(7.65921032958901,-22.959217189033,12.));
#183358=CARTESIAN_POINT('Ctrl Pts',(7.66028473382777,-22.9369293349593,
12.));
#183359=CARTESIAN_POINT('Ctrl Pts',(7.66129790094107,-22.9147345215421,
12.));
#183360=CARTESIAN_POINT('Ctrl Pts',(7.66225015950155,-22.8926334544883,
12.));
#183361=CARTESIAN_POINT('Ctrl Pts',(7.66314184287336,-22.8706268461283,
12.));
#183362=CARTESIAN_POINT('Ctrl Pts',(7.66397328929802,-22.848715415557,12.));
#183363=CARTESIAN_POINT('Ctrl Pts',(7.66474484198548,-22.8268998887678,
12.));
#183364=CARTESIAN_POINT('Ctrl Pts',(7.66545684920986,-22.8051809987833,
12.));
#183365=CARTESIAN_POINT('Ctrl Pts',(7.66610966441272,-22.7835594857699,
12.));
#183366=CARTESIAN_POINT('Ctrl Pts',(7.66670364630298,-22.7620360971843,
12.));
#183367=CARTESIAN_POINT('Ctrl Pts',(7.66723915895439,-22.7406115879513,
12.));
#183368=CARTESIAN_POINT('Ctrl Pts',(7.66771657191027,-22.7192867206245,
12.));
#183369=CARTESIAN_POINT('Ctrl Pts',(7.66813626029274,-22.6980622655446,
12.));
#183370=CARTESIAN_POINT('Ctrl Pts',(7.66849860491742,-22.6769390009885,
12.));
#183371=CARTESIAN_POINT('Ctrl Pts',(7.66880399241322,-22.6559177133127,
12.));
#183372=CARTESIAN_POINT('Ctrl Pts',(7.66905281533714,-22.6349991971541,
12.));
#183373=CARTESIAN_POINT('Ctrl Pts',(7.66924547229413,-22.6141842556243,
12.));
#183374=CARTESIAN_POINT('Ctrl Pts',(7.66938236806232,-22.5934737004953,
12.));
#183375=CARTESIAN_POINT('Ctrl Pts',(7.66946391372305,-22.5728683523831,
12.));
#183376=CARTESIAN_POINT('Ctrl Pts',(7.66949052679692,-22.5523690409116,
12.));
#183377=CARTESIAN_POINT('Ctrl Pts',(7.66946263138143,-22.53197660492,12.));
#183378=CARTESIAN_POINT('Ctrl Pts',(7.66938065829107,-22.5116918927032,
12.));
#183379=CARTESIAN_POINT('Ctrl Pts',(7.66924504520314,-22.4915157622312,
12.));
#183380=CARTESIAN_POINT('Ctrl Pts',(7.6690562368083,-22.47144908137,12.));
#183381=CARTESIAN_POINT('Ctrl Pts',(7.66881468496634,-22.4514927280855,
12.));
#183382=CARTESIAN_POINT('Ctrl Pts',(7.66852084886703,-22.4316475906603,
12.));
#183383=CARTESIAN_POINT('Ctrl Pts',(7.66817519519639,-22.4119145679758,
12.));
#183384=CARTESIAN_POINT('Ctrl Pts',(7.66777819830789,-22.3922945697773,
12.));
#183385=CARTESIAN_POINT('Ctrl Pts',(7.66733034039882,-22.372788516936,12.));
#183386=CARTESIAN_POINT('Ctrl Pts',(7.66683211169157,-22.3533973417021,
12.));
#183387=CARTESIAN_POINT('Ctrl Pts',(7.66628401061951,-22.3341219879469,
12.));
#183388=CARTESIAN_POINT('Ctrl Pts',(7.66568654402493,-22.314963411484,12.));
#183389=CARTESIAN_POINT('Ctrl Pts',(7.66504022736298,-22.2959225803937,
12.));
#183390=CARTESIAN_POINT('Ctrl Pts',(7.66434558490978,-22.2770004753335,
12.));
#183391=CARTESIAN_POINT('Ctrl Pts',(7.6636031499764,-22.258198089848,12.));
#183392=CARTESIAN_POINT('Ctrl Pts',(7.66281346512508,-22.2395164306547,
12.));
#183393=CARTESIAN_POINT('Ctrl Pts',(7.66197708240399,-22.2209565180085,
12.));
#183394=CARTESIAN_POINT('Ctrl Pts',(7.6610945635927,-22.2025193860964,12.));
#183395=CARTESIAN_POINT('Ctrl Pts',(7.66016648045004,-22.1842060834091,
12.));
#183396=CARTESIAN_POINT('Ctrl Pts',(7.6591934149693,-22.1660176731178,12.));
#183397=CARTESIAN_POINT('Ctrl Pts',(7.65817595963348,-22.1479552334211,
12.));
#183398=CARTESIAN_POINT('Ctrl Pts',(7.65711471769396,-22.1300198579675,
12.));
#183399=CARTESIAN_POINT('Ctrl Pts',(7.65601030346806,-22.1122126563329,
12.));
#183400=CARTESIAN_POINT('Ctrl Pts',(7.65486334263643,-22.094534754469,12.));
#183401=CARTESIAN_POINT('Ctrl Pts',(7.65367447254949,-22.0769872951596,
12.));
#183402=CARTESIAN_POINT('Ctrl Pts',(7.65244434253112,-22.0595714384431,
12.));
#183403=CARTESIAN_POINT('Ctrl Pts',(7.65117361421358,-22.0422883621174,
12.));
#183404=CARTESIAN_POINT('Ctrl Pts',(7.64986296190168,-22.0251392623209,
12.));
#183405=CARTESIAN_POINT('Ctrl Pts',(7.64851307293351,-22.0081253540774,
12.));
#183406=CARTESIAN_POINT('Ctrl Pts',(7.64712464805249,-21.9912478718542,
12.));
#183407=CARTESIAN_POINT('Ctrl Pts',(7.64569840177335,-21.9745080700798,
12.));
#183408=CARTESIAN_POINT('Ctrl Pts',(7.64423506279122,-21.9579072237651,
12.));
#183409=CARTESIAN_POINT('Ctrl Pts',(7.64273537442681,-21.9414466292072,
12.));
#183410=CARTESIAN_POINT('Ctrl Pts',(7.64120009506531,-21.9251276046546,
12.));
#183411=CARTESIAN_POINT('Ctrl Pts',(7.63962999860926,-21.9089514909874,
12.));
#183412=CARTESIAN_POINT('Ctrl Pts',(7.63802587492034,-21.8929196523514,
12.));
#183413=CARTESIAN_POINT('Ctrl Pts',(7.63638853033399,-21.8770334769496,
12.));
#183414=CARTESIAN_POINT('Ctrl Pts',(7.63471878821225,-21.8612943779089,
12.));
#183415=CARTESIAN_POINT('Ctrl Pts',(7.63301748948935,-21.8457037941084,
12.));
#183416=CARTESIAN_POINT('Ctrl Pts',(7.63128549323022,-21.8302631910195,
12.));
#183417=CARTESIAN_POINT('Ctrl Pts',(7.62952367718126,-21.814974061509,12.));
#183418=CARTESIAN_POINT('Ctrl Pts',(7.62773293842388,-21.799837926858,12.));
#183419=CARTESIAN_POINT('Ctrl Pts',(7.62591419404512,-21.7848563378021,
12.));
#183420=CARTESIAN_POINT('Ctrl Pts',(7.62406838181165,-21.7700308755584,
12.));
#183421=CARTESIAN_POINT('Ctrl Pts',(7.62219646084228,-21.7553631528328,
12.));
#183422=CARTESIAN_POINT('Ctrl Pts',(7.62029941230854,-21.7408548148656,
12.));
#183423=CARTESIAN_POINT('Ctrl Pts',(7.61837824030537,-21.7265075407975,
12.));
#183424=CARTESIAN_POINT('Ctrl Pts',(7.6164339727042,-21.7123230449834,12.));
#183425=CARTESIAN_POINT('Ctrl Pts',(7.61446766202786,-21.6983030783322,
12.));
#183426=CARTESIAN_POINT('Ctrl Pts',(7.61248038630268,-21.6844494295815,
12.));
#183427=CARTESIAN_POINT('Ctrl Pts',(7.61047325000955,-21.6707639267576,
12.));
#183428=CARTESIAN_POINT('Ctrl Pts',(7.60844738512873,-21.6572484388081,
12.));
#183429=CARTESIAN_POINT('Ctrl Pts',(7.60640395216356,-21.6439048771743,
12.));
#183430=CARTESIAN_POINT('Ctrl Pts',(7.60434414118295,-21.6307351973822,
12.));
#183431=CARTESIAN_POINT('Ctrl Pts',(7.60226917285428,-21.617741400599,12.));
#183432=CARTESIAN_POINT('Ctrl Pts',(7.6001802998824,-21.6049255358843,12.));
#183433=CARTESIAN_POINT('Ctrl Pts',(7.59807880846194,-21.5922897024466,
12.));
#183434=CARTESIAN_POINT('Ctrl Pts',(7.59596601973583,-21.5798360518978,
12.));
#183435=CARTESIAN_POINT('Ctrl Pts',(7.59384329124918,-21.5675667904726,
12.));
#183436=CARTESIAN_POINT('Ctrl Pts',(7.59171201844776,-21.5554841813462,
12.));
#183437=CARTESIAN_POINT('Ctrl Pts',(7.58957363620013,-21.543590547011,12.));
#183438=CARTESIAN_POINT('Ctrl Pts',(7.58742962034833,-21.5318882716736,
12.));
#183439=CARTESIAN_POINT('Ctrl Pts',(7.58528148919129,-21.5203798035299,
12.));
#183440=CARTESIAN_POINT('Ctrl Pts',(7.58313080519179,-21.5090676573873,
12.));
#183441=CARTESIAN_POINT('Ctrl Pts',(7.58097917790743,-21.4979544192744,
12.));
#183442=CARTESIAN_POINT('Ctrl Pts',(7.57882826679131,-21.4870427508194,
12.));
#183443=CARTESIAN_POINT('Ctrl Pts',(7.57667978402986,-21.4763353936762,
12.));
#183444=CARTESIAN_POINT('Ctrl Pts',(7.57453549743411,-21.4658351740128,
12.));
#183445=CARTESIAN_POINT('Ctrl Pts',(7.57239723223505,-21.4555450053142,
12.));
#183446=CARTESIAN_POINT('Ctrl Pts',(7.57026687261165,-21.4454678907509,
12.));
#183447=CARTESIAN_POINT('Ctrl Pts',(7.56814636360847,-21.4356069261513,
12.));
#183448=CARTESIAN_POINT('Ctrl Pts',(7.56603771218711,-21.4259653015736,
12.));
#183449=CARTESIAN_POINT('Ctrl Pts',(7.56394299313684,-21.4165463106254,
12.));
#183450=CARTESIAN_POINT('Ctrl Pts',(7.56186435703621,-21.4073533630365,
12.));
#183451=CARTESIAN_POINT('Ctrl Pts',(7.5598040370061,-21.3983899952987,12.));
#183452=CARTESIAN_POINT('Ctrl Pts',(7.55776435731416,-21.3896598842117,
12.));
#183453=CARTESIAN_POINT('Ctrl Pts',(7.55574773403502,-21.3811668478932,
12.));
#183454=CARTESIAN_POINT('Ctrl Pts',(7.55375667080028,-21.3729148390243,
12.));
#183455=CARTESIAN_POINT('Ctrl Pts',(7.55179375777443,-21.3649079431865,
12.));
#183456=CARTESIAN_POINT('Ctrl Pts',(7.54986166521309,-21.3571503685855,
12.));
#183457=CARTESIAN_POINT('Ctrl Pts',(7.5479631624633,-21.3496464761531,12.));
#183458=CARTESIAN_POINT('Ctrl Pts',(7.54610114948346,-21.3424008295038,
12.));
#183459=CARTESIAN_POINT('Ctrl Pts',(7.54427868151267,-21.3354182340149,
12.));
#183460=CARTESIAN_POINT('Ctrl Pts',(7.5424990037703,-21.328703791771,12.));
#183461=CARTESIAN_POINT('Ctrl Pts',(7.54076552038278,-21.3222628524165,
12.));
#183462=CARTESIAN_POINT('Ctrl Pts',(7.53908175169898,-21.3161009456256,
12.));
#183463=CARTESIAN_POINT('Ctrl Pts',(7.53745129364615,-21.310223716773,12.));
#183464=CARTESIAN_POINT('Ctrl Pts',(7.53587778251735,-21.3046368712157,
12.));
#183465=CARTESIAN_POINT('Ctrl Pts',(7.53436505309942,-21.2993464250717,
12.));
#183466=CARTESIAN_POINT('Ctrl Pts',(7.53291726078526,-21.2943588989331,
12.));
#183467=CARTESIAN_POINT('Ctrl Pts',(7.53153906987855,-21.2896816163842,
12.));
#183468=CARTESIAN_POINT('Ctrl Pts',(7.53023562438229,-21.2853226580657,
12.));
#183469=CARTESIAN_POINT('Ctrl Pts',(7.52901217930407,-21.2812902781143,
12.));
#183470=CARTESIAN_POINT('Ctrl Pts',(7.52787386225332,-21.2775925269652,
12.));
#183471=CARTESIAN_POINT('Ctrl Pts',(7.5268252691854,-21.2742366113579,12.));
#183472=CARTESIAN_POINT('Ctrl Pts',(7.52587126095529,-21.2712301573466,
12.));
#183473=CARTESIAN_POINT('Ctrl Pts',(7.5250177033353,-21.2685823838671,12.));
#183474=CARTESIAN_POINT('Ctrl Pts',(7.52427261074297,-21.2663059157058,
12.));
#183475=CARTESIAN_POINT('Ctrl Pts',(7.52364573027552,-21.2644161259962,
12.));
#183476=CARTESIAN_POINT('Ctrl Pts',(7.52314642316199,-21.262927782038,12.));
#183477=CARTESIAN_POINT('Ctrl Pts',(7.52278182242669,-21.2618521283555,
12.));
#183478=CARTESIAN_POINT('Ctrl Pts',(7.5226006423166,-21.261326054066,12.));
#183479=CARTESIAN_POINT('Ctrl Pts',(7.52252744144903,-21.2611204474866,
12.));
#183480=CARTESIAN_POINT('Ctrl Pts',(7.52250649703969,-21.2610673466886,
12.));
#183481=CARTESIAN_POINT('Ctrl Pts',(7.52250298901263,-21.2610617890679,
12.));
#183482=CARTESIAN_POINT('',(7.33627833380045,-20.7347298079577,12.));
#183483=CARTESIAN_POINT('',(3.58569854577611,-10.1343606576251,12.));
#183484=CARTESIAN_POINT('',(7.63019749246977,-20.1004996511507,12.));
#183485=CARTESIAN_POINT('Origin',(7.80764394578302,-20.56795313141,12.));
#183486=CARTESIAN_POINT('',(8.81783521984849,-19.6085639972844,12.));
#183487=CARTESIAN_POINT('Origin',(2.70312158620511E-13,-7.32141292029404E-13,
12.));
#183488=CARTESIAN_POINT('',(9.47413589477548,-19.84920021178,12.));
#183489=CARTESIAN_POINT('Origin',(9.02290115519381,-20.0645771135004,12.));
#183490=CARTESIAN_POINT('',(9.71462809124915,-20.353053841303,12.));
#183491=CARTESIAN_POINT('',(4.85731404562459,-10.1765269206515,12.));
#183492=CARTESIAN_POINT('',(12.4230808101438,-22.8400320311649,12.));
#183493=CARTESIAN_POINT('Ctrl Pts',(9.71462809124915,-20.353053841303,12.));
#183494=CARTESIAN_POINT('Ctrl Pts',(9.71462954053041,-20.353060251684,12.));
#183495=CARTESIAN_POINT('Ctrl Pts',(9.71465227853041,-20.3531126095522,
12.));
#183496=CARTESIAN_POINT('Ctrl Pts',(9.7147459035068,-20.3533097561886,12.));
#183497=CARTESIAN_POINT('Ctrl Pts',(9.7149897805202,-20.3538098605706,12.));
#183498=CARTESIAN_POINT('Ctrl Pts',(9.71549257088172,-20.3548282742361,
12.));
#183499=CARTESIAN_POINT('Ctrl Pts',(9.71619192554185,-20.3562337557875,
12.));
#183500=CARTESIAN_POINT('Ctrl Pts',(9.71708493723096,-20.3580133103356,
12.));
#183501=CARTESIAN_POINT('Ctrl Pts',(9.71816778328006,-20.3601498764344,
12.));
#183502=CARTESIAN_POINT('Ctrl Pts',(9.71943648548099,-20.3626256913981,
12.));
#183503=CARTESIAN_POINT('Ctrl Pts',(9.7208877838108,-20.3654261611056,12.));
#183504=CARTESIAN_POINT('Ctrl Pts',(9.72251930722489,-20.3685406190576,
12.));
#183505=CARTESIAN_POINT('Ctrl Pts',(9.72432910043194,-20.371960235676,12.));
#183506=CARTESIAN_POINT('Ctrl Pts',(9.7263153173288,-20.3756766651951,12.));
#183507=CARTESIAN_POINT('Ctrl Pts',(9.72847589116541,-20.3796805893304,
12.));
#183508=CARTESIAN_POINT('Ctrl Pts',(9.73080870123726,-20.3839624556742,
12.));
#183509=CARTESIAN_POINT('Ctrl Pts',(9.73331167102807,-20.3885129129912,
12.));
#183510=CARTESIAN_POINT('Ctrl Pts',(9.73598292014242,-20.3933234845647,
12.));
#183511=CARTESIAN_POINT('Ctrl Pts',(9.738820776132,-20.3983866213331,12.));
#183512=CARTESIAN_POINT('Ctrl Pts',(9.74182369656271,-20.4036953576549,
12.));
#183513=CARTESIAN_POINT('Ctrl Pts',(9.74499021838537,-20.4092430879861,
12.));
#183514=CARTESIAN_POINT('Ctrl Pts',(9.74831889242173,-20.4150232777393,
12.));
#183515=CARTESIAN_POINT('Ctrl Pts',(9.75180829786429,-20.4210295275817,
12.));
#183516=CARTESIAN_POINT('Ctrl Pts',(9.75545705902417,-20.4272556476629,
12.));
#183517=CARTESIAN_POINT('Ctrl Pts',(9.75926386289922,-20.4336957355473,
12.));
#183518=CARTESIAN_POINT('Ctrl Pts',(9.76322747195494,-20.44034423294,12.));
#183519=CARTESIAN_POINT('Ctrl Pts',(9.76734670980891,-20.447195862298,12.));
#183520=CARTESIAN_POINT('Ctrl Pts',(9.77162045104069,-20.4542455817527,
12.));
#183521=CARTESIAN_POINT('Ctrl Pts',(9.77604760815528,-20.4614885274975,
12.));
#183522=CARTESIAN_POINT('Ctrl Pts',(9.7806271237332,-20.4689199790669,12.));
#183523=CARTESIAN_POINT('Ctrl Pts',(9.78535797314166,-20.4765353711586,
12.));
#183524=CARTESIAN_POINT('Ctrl Pts',(9.79023916498655,-20.4843302955329,
12.));
#183525=CARTESIAN_POINT('Ctrl Pts',(9.7952697428833,-20.4923005087943,12.));
#183526=CARTESIAN_POINT('Ctrl Pts',(9.80044878520948,-20.5004419312107,
12.));
#183527=CARTESIAN_POINT('Ctrl Pts',(9.80577540161087,-20.5087506310505,
12.));
#183528=CARTESIAN_POINT('Ctrl Pts',(9.81124873025281,-20.517222812284,12.));
#183529=CARTESIAN_POINT('Ctrl Pts',(9.81686793455942,-20.5258548000629,
12.));
#183530=CARTESIAN_POINT('Ctrl Pts',(9.82263220080362,-20.5346430299517,
12.));
#183531=CARTESIAN_POINT('Ctrl Pts',(9.82854073773876,-20.5435840460721,
12.));
#183532=CARTESIAN_POINT('Ctrl Pts',(9.83459277585315,-20.552674497646,12.));
#183533=CARTESIAN_POINT('Ctrl Pts',(9.84078756677565,-20.5619111362402,
12.));
#183534=CARTESIAN_POINT('Ctrl Pts',(9.84712438256277,-20.5712908125139,
12.));
#183535=CARTESIAN_POINT('Ctrl Pts',(9.8536025145698,-20.5808104710015,12.));
#183536=CARTESIAN_POINT('Ctrl Pts',(9.86022127232747,-20.5904671449754,
12.));
#183537=CARTESIAN_POINT('Ctrl Pts',(9.86697998242622,-20.6002579513699,
12.));
#183538=CARTESIAN_POINT('Ctrl Pts',(9.87387798732955,-20.6101800854494,
12.));
#183539=CARTESIAN_POINT('Ctrl Pts',(9.88091464472675,-20.6202308177475,
12.));
#183540=CARTESIAN_POINT('Ctrl Pts',(9.88808932697305,-20.6304074914087,
12.));
#183541=CARTESIAN_POINT('Ctrl Pts',(9.89540142049119,-20.6407075193976,
12.));
#183542=CARTESIAN_POINT('Ctrl Pts',(9.90285032516692,-20.6511283817414,
12.));
#183543=CARTESIAN_POINT('Ctrl Pts',(9.91043545377007,-20.6616676228315,
12.));
#183544=CARTESIAN_POINT('Ctrl Pts',(9.91815623141288,-20.6723228488263,
12.));
#183545=CARTESIAN_POINT('Ctrl Pts',(9.92601209498748,-20.6830917250255,
12.));
#183546=CARTESIAN_POINT('Ctrl Pts',(9.93400249259729,-20.6939719732484,
12.));
#183547=CARTESIAN_POINT('Ctrl Pts',(9.94212688298236,-20.7049613692234,
12.));
#183548=CARTESIAN_POINT('Ctrl Pts',(9.95038473514948,-20.7160577407579,
12.));
#183549=CARTESIAN_POINT('Ctrl Pts',(9.95877552798397,-20.7272589658751,
12.));
#183550=CARTESIAN_POINT('Ctrl Pts',(9.96729874986201,-20.7385629709795,
12.));
#183551=CARTESIAN_POINT('Ctrl Pts',(9.97595389823469,-20.7499677289627,
12.));
#183552=CARTESIAN_POINT('Ctrl Pts',(9.98474047926852,-20.761471257499,12.));
#183553=CARTESIAN_POINT('Ctrl Pts',(9.9936580075464,-20.7730716175417,12.));
#183554=CARTESIAN_POINT('Ctrl Pts',(10.0027060057389,-20.7847669117568,
12.));
#183555=CARTESIAN_POINT('Ctrl Pts',(10.0118840042786,-20.7965552829908,
12.));
#183556=CARTESIAN_POINT('Ctrl Pts',(10.0211915410095,-20.8084349126888,
12.));
#183557=CARTESIAN_POINT('Ctrl Pts',(10.0306281609435,-20.8204040196602,
12.));
#183558=CARTESIAN_POINT('Ctrl Pts',(10.0401934160234,-20.8324608588909,
12.));
#183559=CARTESIAN_POINT('Ctrl Pts',(10.0498868648733,-20.8446037203402,
12.));
#183560=CARTESIAN_POINT('Ctrl Pts',(10.0597080725375,-20.8568309277316,
12.));
#183561=CARTESIAN_POINT('Ctrl Pts',(10.0696566102218,-20.86914083737,12.));
#183562=CARTESIAN_POINT('Ctrl Pts',(10.0797320551154,-20.881531837184,12.));
#183563=CARTESIAN_POINT('Ctrl Pts',(10.0899339901915,-20.894002345737,12.));
#183564=CARTESIAN_POINT('Ctrl Pts',(10.1002620040076,-20.9065508112557,
12.));
#183565=CARTESIAN_POINT('Ctrl Pts',(10.1107156904836,-20.919175710627,12.));
#183566=CARTESIAN_POINT('Ctrl Pts',(10.1212946487057,-20.9318755484734,
12.));
#183567=CARTESIAN_POINT('Ctrl Pts',(10.1319984827908,-20.9446488563933,
12.));
#183568=CARTESIAN_POINT('Ctrl Pts',(10.1428268017256,-20.9574941921591,
12.));
#183569=CARTESIAN_POINT('Ctrl Pts',(10.1537792192065,-20.9704101389369,
12.));
#183570=CARTESIAN_POINT('Ctrl Pts',(10.1648553534568,-20.9833953044736,
12.));
#183571=CARTESIAN_POINT('Ctrl Pts',(10.1760548270767,-20.9964483203686,
12.));
#183572=CARTESIAN_POINT('Ctrl Pts',(10.187377266936,-21.0095678414486,12.));
#183573=CARTESIAN_POINT('Ctrl Pts',(10.1988223040425,-21.0227525451107,
12.));
#183574=CARTESIAN_POINT('Ctrl Pts',(10.2103895734123,-21.0360011306815,
12.));
#183575=CARTESIAN_POINT('Ctrl Pts',(10.2220787139154,-21.0493123187483,
12.));
#183576=CARTESIAN_POINT('Ctrl Pts',(10.2338893681567,-21.0626848505663,
12.));
#183577=CARTESIAN_POINT('Ctrl Pts',(10.2458211823912,-21.0761174875445,
12.));
#183578=CARTESIAN_POINT('Ctrl Pts',(10.2578738064181,-21.0896090107063,
12.));
#183579=CARTESIAN_POINT('Ctrl Pts',(10.2700468934744,-21.1031582201627,
12.));
#183580=CARTESIAN_POINT('Ctrl Pts',(10.2823401001072,-21.1167639345631,
12.));
#183581=CARTESIAN_POINT('Ctrl Pts',(10.2947530860721,-21.1304249906002,
12.));
#183582=CARTESIAN_POINT('Ctrl Pts',(10.3072855142687,-21.1441402425843,
12.));
#183583=CARTESIAN_POINT('Ctrl Pts',(10.3199370506544,-21.1579085619965,
12.));
#183584=CARTESIAN_POINT('Ctrl Pts',(10.3327073641572,-21.1717288370509,
12.));
#183585=CARTESIAN_POINT('Ctrl Pts',(10.34559612657,-21.1855999722416,12.));
#183586=CARTESIAN_POINT('Ctrl Pts',(10.3586030124587,-21.199520887919,12.));
#183587=CARTESIAN_POINT('Ctrl Pts',(10.371727699113,-21.2134905199345,12.));
#183588=CARTESIAN_POINT('Ctrl Pts',(10.3849698664786,-21.22750781927,12.));
#183589=CARTESIAN_POINT('Ctrl Pts',(10.3983291970846,-21.2415717516714,
12.));
#183590=CARTESIAN_POINT('Ctrl Pts',(10.4118053759588,-21.255681297275,12.));
#183591=CARTESIAN_POINT('Ctrl Pts',(10.42539809054,-21.2698354502403,12.));
#183592=CARTESIAN_POINT('Ctrl Pts',(10.4391070306391,-21.2840332184483,
12.));
#183593=CARTESIAN_POINT('Ctrl Pts',(10.4529318883874,-21.2982736231931,
12.));
#183594=CARTESIAN_POINT('Ctrl Pts',(10.4668723581768,-21.3125556988731,
12.));
#183595=CARTESIAN_POINT('Ctrl Pts',(10.4809281365931,-21.3268784926819,
12.));
#183596=CARTESIAN_POINT('Ctrl Pts',(10.4950989223336,-21.3412410642904,
12.));
#183597=CARTESIAN_POINT('Ctrl Pts',(10.5093844161685,-21.3556424855814,
12.));
#183598=CARTESIAN_POINT('Ctrl Pts',(10.5237843209057,-21.3700818403936,
12.));
#183599=CARTESIAN_POINT('Ctrl Pts',(10.5382983413421,-21.3845582242602,
12.));
#183600=CARTESIAN_POINT('Ctrl Pts',(10.5529261842108,-21.3990707441497,
12.));
#183601=CARTESIAN_POINT('Ctrl Pts',(10.5676675581108,-21.4136185181979,
12.));
#183602=CARTESIAN_POINT('Ctrl Pts',(10.5825221734573,-21.4282006754631,
12.));
#183603=CARTESIAN_POINT('Ctrl Pts',(10.5974897424622,-21.4428163557144,
12.));
#183604=CARTESIAN_POINT('Ctrl Pts',(10.6125699790961,-21.4574647092097,
12.));
#183605=CARTESIAN_POINT('Ctrl Pts',(10.6277625990456,-21.4721448964766,
12.));
#183606=CARTESIAN_POINT('Ctrl Pts',(10.6430673196607,-21.4868560880889,
12.));
#183607=CARTESIAN_POINT('Ctrl Pts',(10.6584838598939,-21.5015974644449,
12.));
#183608=CARTESIAN_POINT('Ctrl Pts',(10.6740119402834,-21.51636821558,12.));
#183609=CARTESIAN_POINT('Ctrl Pts',(10.689651282929,-21.5311675409807,12.));
#183610=CARTESIAN_POINT('Ctrl Pts',(10.7054016114571,-21.5459946493955,
12.));
#183611=CARTESIAN_POINT('Ctrl Pts',(10.7212626509816,-21.5608487586468,
12.));
#183612=CARTESIAN_POINT('Ctrl Pts',(10.7372341280467,-21.5757290954371,
12.));
#183613=CARTESIAN_POINT('Ctrl Pts',(10.7533157705941,-21.5906348951743,
12.));
#183614=CARTESIAN_POINT('Ctrl Pts',(10.7695073079552,-21.6055654018176,
12.));
#183615=CARTESIAN_POINT('Ctrl Pts',(10.7858084708261,-21.6205198677173,
12.));
#183616=CARTESIAN_POINT('Ctrl Pts',(10.8022189912369,-21.6354975534557,
12.));
#183617=CARTESIAN_POINT('Ctrl Pts',(10.8187386025136,-21.6504977276866,
12.));
#183618=CARTESIAN_POINT('Ctrl Pts',(10.8353670392272,-21.6655196669732,
12.));
#183619=CARTESIAN_POINT('Ctrl Pts',(10.8521040371835,-21.6805626556467,
12.));
#183620=CARTESIAN_POINT('Ctrl Pts',(10.8689493334095,-21.6956259856672,
12.));
#183621=CARTESIAN_POINT('Ctrl Pts',(10.8859026661293,-21.7107089564825,
12.));
#183622=CARTESIAN_POINT('Ctrl Pts',(10.902963774734,-21.7258108748873,12.));
#183623=CARTESIAN_POINT('Ctrl Pts',(10.9201323997384,-21.7409310548797,
12.));
#183624=CARTESIAN_POINT('Ctrl Pts',(10.9374082827444,-21.7560688175247,
12.));
#183625=CARTESIAN_POINT('Ctrl Pts',(10.9547911664455,-21.7712234908464,
12.));
#183626=CARTESIAN_POINT('Ctrl Pts',(10.9722807946155,-21.7863944097141,
12.));
#183627=CARTESIAN_POINT('Ctrl Pts',(10.9898769120912,-21.8015809157301,
12.));
#183628=CARTESIAN_POINT('Ctrl Pts',(11.0075792647477,-21.8167823571168,
12.));
#183629=CARTESIAN_POINT('Ctrl Pts',(11.0253875994598,-21.8319980886033,
12.));
#183630=CARTESIAN_POINT('Ctrl Pts',(11.0433016640807,-21.8472274713103,
12.));
#183631=CARTESIAN_POINT('Ctrl Pts',(11.0613212074363,-21.8624698726318,
12.));
#183632=CARTESIAN_POINT('Ctrl Pts',(11.0794459793057,-21.877724666119,12.));
#183633=CARTESIAN_POINT('Ctrl Pts',(11.0976757303944,-21.8929912313608,
12.));
#183634=CARTESIAN_POINT('Ctrl Pts',(11.1160102123024,-21.9082689538688,
12.));
#183635=CARTESIAN_POINT('Ctrl Pts',(11.1344491774741,-21.923557224952,12.));
#183636=CARTESIAN_POINT('Ctrl Pts',(11.1529923792003,-21.9388554416439,
12.));
#183637=CARTESIAN_POINT('Ctrl Pts',(11.1716395716376,-21.9541630066506,
12.));
#183638=CARTESIAN_POINT('Ctrl Pts',(11.190390509811,-21.9694793282914,12.));
#183639=CARTESIAN_POINT('Ctrl Pts',(11.2092449496125,-21.9848038204439,
12.));
#183640=CARTESIAN_POINT('Ctrl Pts',(11.2282026477896,-22.0001359024839,
12.));
#183641=CARTESIAN_POINT('Ctrl Pts',(11.2472633619275,-22.0154749992363,
12.));
#183642=CARTESIAN_POINT('Ctrl Pts',(11.2664268504206,-22.030820540835,12.));
#183643=CARTESIAN_POINT('Ctrl Pts',(11.2856928724374,-22.046171962566,12.));
#183644=CARTESIAN_POINT('Ctrl Pts',(11.3050611878771,-22.0615287047179,
12.));
#183645=CARTESIAN_POINT('Ctrl Pts',(11.3245315573168,-22.0768902124267,
12.));
#183646=CARTESIAN_POINT('Ctrl Pts',(11.3441037419553,-22.0922559355294,
12.));
#183647=CARTESIAN_POINT('Ctrl Pts',(11.3637775035367,-22.1076253283979,
12.));
#183648=CARTESIAN_POINT('Ctrl Pts',(11.3835526044256,-22.1229978500186,
12.));
#183649=CARTESIAN_POINT('Ctrl Pts',(11.4034288076908,-22.1383729640964,
12.));
#183650=CARTESIAN_POINT('Ctrl Pts',(11.4234058771742,-22.1537501391487,
12.));
#183651=CARTESIAN_POINT('Ctrl Pts',(11.443483577557,-22.1691288486096,12.));
#183652=CARTESIAN_POINT('Ctrl Pts',(11.463661674411,-22.184508570917,12.));
#183653=CARTESIAN_POINT('Ctrl Pts',(11.483939934259,-22.1998887896436,12.));
#183654=CARTESIAN_POINT('Ctrl Pts',(11.5043181244242,-22.2152689931022,
12.));
#183655=CARTESIAN_POINT('Ctrl Pts',(11.5247960128477,-22.2306486738901,
12.));
#183656=CARTESIAN_POINT('Ctrl Pts',(11.5453733679121,-22.2460273284654,
12.));
#183657=CARTESIAN_POINT('Ctrl Pts',(11.5660499582403,-22.2614044566898,
12.));
#183658=CARTESIAN_POINT('Ctrl Pts',(11.5868255525188,-22.2767795614348,
12.));
#183659=CARTESIAN_POINT('Ctrl Pts',(11.6076999192357,-22.2921521480356,
12.));
#183660=CARTESIAN_POINT('Ctrl Pts',(11.6286728270009,-22.3075217249049,
12.));
#183661=CARTESIAN_POINT('Ctrl Pts',(11.6497440449857,-22.3228878043976,
12.));
#183662=CARTESIAN_POINT('Ctrl Pts',(11.6709133432985,-22.3382499035619,
12.));
#183663=CARTESIAN_POINT('Ctrl Pts',(11.6921804934056,-22.3536075450029,
12.));
#183664=CARTESIAN_POINT('Ctrl Pts',(11.7135452684532,-22.3689602575491,
12.));
#183665=CARTESIAN_POINT('Ctrl Pts',(11.7350074437961,-22.3843075773899,
12.));
#183666=CARTESIAN_POINT('Ctrl Pts',(11.7565667964764,-22.3996490469191,
12.));
#183667=CARTESIAN_POINT('Ctrl Pts',(11.7782231042039,-22.4149842125008,
12.));
#183668=CARTESIAN_POINT('Ctrl Pts',(11.7999761445173,-22.430312622646,12.));
#183669=CARTESIAN_POINT('Ctrl Pts',(11.8218256937889,-22.4456338258735,
12.));
#183670=CARTESIAN_POINT('Ctrl Pts',(11.8437715264487,-22.4609473690472,
12.));
#183671=CARTESIAN_POINT('Ctrl Pts',(11.8658134137019,-22.4762527946702,
12.));
#183672=CARTESIAN_POINT('Ctrl Pts',(11.8879511239942,-22.4915496418485,
12.));
#183673=CARTESIAN_POINT('Ctrl Pts',(11.9101844254557,-22.5068374513973,
12.));
#183674=CARTESIAN_POINT('Ctrl Pts',(11.9325130877803,-22.5221157697883,
12.));
#183675=CARTESIAN_POINT('Ctrl Pts',(11.9549368843997,-22.5373841537307,
12.));
#183676=CARTESIAN_POINT('Ctrl Pts',(11.9774555943496,-22.5526421741158,
12.));
#183677=CARTESIAN_POINT('Ctrl Pts',(12.0000690046694,-22.5678894211181,
12.));
#183678=CARTESIAN_POINT('Ctrl Pts',(12.0227769113127,-22.5831255061282,
12.));
#183679=CARTESIAN_POINT('Ctrl Pts',(12.0455791139128,-22.5983500505644,
12.));
#183680=CARTESIAN_POINT('Ctrl Pts',(12.0684754113862,-22.6135626764898,
12.));
#183681=CARTESIAN_POINT('Ctrl Pts',(12.0914655972823,-22.6287629967056,
12.));
#183682=CARTESIAN_POINT('Ctrl Pts',(12.1145494550383,-22.6439506046605,
12.));
#183683=CARTESIAN_POINT('Ctrl Pts',(12.1377267537145,-22.6591250653965,
12.));
#183684=CARTESIAN_POINT('Ctrl Pts',(12.1609972423099,-22.6742859034944,
12.));
#183685=CARTESIAN_POINT('Ctrl Pts',(12.1843606579261,-22.6894326205037,
12.));
#183686=CARTESIAN_POINT('Ctrl Pts',(12.2078167360284,-22.7045647168747,
12.));
#183687=CARTESIAN_POINT('Ctrl Pts',(12.2313652198061,-22.7196817119374,
12.));
#183688=CARTESIAN_POINT('Ctrl Pts',(12.2550058702395,-22.7347831655287,
12.));
#183689=CARTESIAN_POINT('Ctrl Pts',(12.2787384750742,-22.7498686970069,
12.));
#183690=CARTESIAN_POINT('Ctrl Pts',(12.3025628601792,-22.764938010105,12.));
#183691=CARTESIAN_POINT('Ctrl Pts',(12.3264788926075,-22.7799908974768,
12.));
#183692=CARTESIAN_POINT('Ctrl Pts',(12.3504864740319,-22.795027221673,12.));
#183693=CARTESIAN_POINT('Ctrl Pts',(12.374585536673,-22.81004690224,12.));
#183694=CARTESIAN_POINT('Ctrl Pts',(12.3939379378998,-22.8220493007173,
12.));
#183695=CARTESIAN_POINT('Ctrl Pts',(12.4084933766346,-22.8310435872748,
12.));
#183696=CARTESIAN_POINT('Ctrl Pts',(12.418215285186,-22.8370364396459,12.));
#183697=CARTESIAN_POINT('Ctrl Pts',(12.4230808101438,-22.8400320311649,
12.));
#183698=CARTESIAN_POINT('',(13.5685075571671,-22.178719590434,12.));
#183699=CARTESIAN_POINT('Origin',(0.,0.,12.));
#183700=CARTESIAN_POINT('',(12.7689476255362,-18.5896416359912,12.));
#183701=CARTESIAN_POINT('Ctrl Pts',(13.5685075571671,-22.178719590434,12.));
#183702=CARTESIAN_POINT('Ctrl Pts',(13.5683460612942,-22.1730081264608,
12.));
#183703=CARTESIAN_POINT('Ctrl Pts',(13.5680170531805,-22.1615922805008,
12.));
#183704=CARTESIAN_POINT('Ctrl Pts',(13.5675054919061,-22.1444897575194,
12.));
#183705=CARTESIAN_POINT('Ctrl Pts',(13.5667873105359,-22.1217288871975,
12.));
#183706=CARTESIAN_POINT('Ctrl Pts',(13.5658294169284,-22.0933486464593,
12.));
#183707=CARTESIAN_POINT('Ctrl Pts',(13.5648113689033,-22.065039308961,12.));
#183708=CARTESIAN_POINT('Ctrl Pts',(13.5637332022473,-22.0368009736295,
12.));
#183709=CARTESIAN_POINT('Ctrl Pts',(13.5625949868333,-22.0086337943449,
12.));
#183710=CARTESIAN_POINT('Ctrl Pts',(13.5613968357561,-21.9805379899168,
12.));
#183711=CARTESIAN_POINT('Ctrl Pts',(13.5601389185257,-21.9525138592813,
12.));
#183712=CARTESIAN_POINT('Ctrl Pts',(13.5588214586604,-21.9245617765769,
12.));
#183713=CARTESIAN_POINT('Ctrl Pts',(13.5574447178424,-21.8966821688824,
12.));
#183714=CARTESIAN_POINT('Ctrl Pts',(13.5560089839385,-21.8688754989365,
12.));
#183715=CARTESIAN_POINT('Ctrl Pts',(13.5545145573031,-21.8411422456075,
12.));
#183716=CARTESIAN_POINT('Ctrl Pts',(13.5529617381573,-21.8134828857967,
12.));
#183717=CARTESIAN_POINT('Ctrl Pts',(13.551350812725,-21.7858978745865,12.));
#183718=CARTESIAN_POINT('Ctrl Pts',(13.5496820422211,-21.7583876294554,
12.));
#183719=CARTESIAN_POINT('Ctrl Pts',(13.5479556704481,-21.7309525412281,
12.));
#183720=CARTESIAN_POINT('Ctrl Pts',(13.5461719295048,-21.7035929822955,
12.));
#183721=CARTESIAN_POINT('Ctrl Pts',(13.5443310461526,-21.6763093157699,
12.));
#183722=CARTESIAN_POINT('Ctrl Pts',(13.5424332480699,-21.6491019044648,
12.));
#183723=CARTESIAN_POINT('Ctrl Pts',(13.5404787697791,-21.6219711193946,
12.));
#183724=CARTESIAN_POINT('Ctrl Pts',(13.5384678597195,-21.5949173499013,
12.));
#183725=CARTESIAN_POINT('Ctrl Pts',(13.536400779028,-21.5679410019002,12.));
#183726=CARTESIAN_POINT('Ctrl Pts',(13.5342777983214,-21.5410424932503,
12.));
#183727=CARTESIAN_POINT('Ctrl Pts',(13.5320991952138,-21.5142222501666,
12.));
#183728=CARTESIAN_POINT('Ctrl Pts',(13.5298652514355,-21.4874807030468,
12.));
#183729=CARTESIAN_POINT('Ctrl Pts',(13.5275762503555,-21.4608182828697,
12.));
#183730=CARTESIAN_POINT('Ctrl Pts',(13.5252324737801,-21.4342354165259,
12.));
#183731=CARTESIAN_POINT('Ctrl Pts',(13.5228342013516,-21.4077325259324,
12.));
#183732=CARTESIAN_POINT('Ctrl Pts',(13.5203817122503,-21.3813100304973,
12.));
#183733=CARTESIAN_POINT('Ctrl Pts',(13.5178752862466,-21.3549683486222,
12.));
#183734=CARTESIAN_POINT('Ctrl Pts',(13.5153152050555,-21.3287078996341,
12.));
#183735=CARTESIAN_POINT('Ctrl Pts',(13.5127017534971,-21.3025291054235,
12.));
#183736=CARTESIAN_POINT('Ctrl Pts',(13.5100352209205,-21.2764323924442,
12.));
#183737=CARTESIAN_POINT('Ctrl Pts',(13.5073159019452,-21.250418192743,12.));
#183738=CARTESIAN_POINT('Ctrl Pts',(13.5045440957404,-21.2244869429332,
12.));
#183739=CARTESIAN_POINT('Ctrl Pts',(13.5017201056088,-21.1986390835828,
12.));
#183740=CARTESIAN_POINT('Ctrl Pts',(13.4988442384491,-21.1728750584175,
12.));
#183741=CARTESIAN_POINT('Ctrl Pts',(13.4959168042934,-21.1471953136209,
12.));
#183742=CARTESIAN_POINT('Ctrl Pts',(13.4929381157778,-21.1216002970207,
12.));
#183743=CARTESIAN_POINT('Ctrl Pts',(13.4899084877717,-21.0960904575046,
12.));
#183744=CARTESIAN_POINT('Ctrl Pts',(13.4868282377191,-21.0706662455199,
12.));
#183745=CARTESIAN_POINT('Ctrl Pts',(13.4836976858912,-21.0453281134245,
12.));
#183746=CARTESIAN_POINT('Ctrl Pts',(13.4805171556822,-21.0200765158884,
12.));
#183747=CARTESIAN_POINT('Ctrl Pts',(13.4772869738878,-20.9949119102592,
12.));
#183748=CARTESIAN_POINT('Ctrl Pts',(13.4740074710086,-20.9698347569477,
12.));
#183749=CARTESIAN_POINT('Ctrl Pts',(13.4706789815166,-20.9448455197557,
12.));
#183750=CARTESIAN_POINT('Ctrl Pts',(13.4673018437717,-20.9199446657583,
12.));
#183751=CARTESIAN_POINT('Ctrl Pts',(13.4638763999725,-20.8951326652158,
12.));
#183752=CARTESIAN_POINT('Ctrl Pts',(13.4604029960983,-20.8704099914641,
12.));
#183753=CARTESIAN_POINT('Ctrl Pts',(13.4568819818631,-20.8457771208083,
12.));
#183754=CARTESIAN_POINT('Ctrl Pts',(13.4533137106667,-20.821234532398,12.));
#183755=CARTESIAN_POINT('Ctrl Pts',(13.4496985395637,-20.7967827081228,
12.));
#183756=CARTESIAN_POINT('Ctrl Pts',(13.4460368293689,-20.7724221327609,
12.));
#183757=CARTESIAN_POINT('Ctrl Pts',(13.4423289447561,-20.7481532941014,
12.));
#183758=CARTESIAN_POINT('Ctrl Pts',(13.4385752543663,-20.7239766830676,
12.));
#183759=CARTESIAN_POINT('Ctrl Pts',(13.4347761309154,-20.6998927938288,
12.));
#183760=CARTESIAN_POINT('Ctrl Pts',(13.4309319513119,-20.6759021239102,
12.));
#183761=CARTESIAN_POINT('Ctrl Pts',(13.427043096765,-20.6520051742868,12.));
#183762=CARTESIAN_POINT('Ctrl Pts',(13.4231099528178,-20.6282024494234,
12.));
#183763=CARTESIAN_POINT('Ctrl Pts',(13.4191329093931,-20.6044944573151,
12.));
#183764=CARTESIAN_POINT('Ctrl Pts',(13.415112360841,-20.5808817095155,12.));
#183765=CARTESIAN_POINT('Ctrl Pts',(13.4110487059912,-20.557364721164,12.));
#183766=CARTESIAN_POINT('Ctrl Pts',(13.4069423482076,-20.5339440109958,
12.));
#183767=CARTESIAN_POINT('Ctrl Pts',(13.4027936954529,-20.5106201013755,
12.));
#183768=CARTESIAN_POINT('Ctrl Pts',(13.3986031603716,-20.4873935184041,
12.));
#183769=CARTESIAN_POINT('Ctrl Pts',(13.3943711603739,-20.4642647920038,
12.));
#183770=CARTESIAN_POINT('Ctrl Pts',(13.3900981177254,-20.4412344560007,
12.));
#183771=CARTESIAN_POINT('Ctrl Pts',(13.3857844596387,-20.4183030482002,
12.));
#183772=CARTESIAN_POINT('Ctrl Pts',(13.3814306183721,-20.3954711104505,
12.));
#183773=CARTESIAN_POINT('Ctrl Pts',(13.377037031319,-20.3727391887187,12.));
#183774=CARTESIAN_POINT('Ctrl Pts',(13.3726041410869,-20.3501078331818,
12.));
#183775=CARTESIAN_POINT('Ctrl Pts',(13.3681323955828,-20.3275775983032,
12.));
#183776=CARTESIAN_POINT('Ctrl Pts',(13.3636222481016,-20.3051490429049,
12.));
#183777=CARTESIAN_POINT('Ctrl Pts',(13.3590741574194,-20.2828227302337,
12.));
#183778=CARTESIAN_POINT('Ctrl Pts',(13.3544885878886,-20.2605992280117,
12.));
#183779=CARTESIAN_POINT('Ctrl Pts',(13.3498660095381,-20.2384791085354,
12.));
#183780=CARTESIAN_POINT('Ctrl Pts',(13.3452068981762,-20.2164629487855,
12.));
#183781=CARTESIAN_POINT('Ctrl Pts',(13.3405117354969,-20.1945513305233,
12.));
#183782=CARTESIAN_POINT('Ctrl Pts',(13.3357810091903,-20.1727448403818,
12.));
#183783=CARTESIAN_POINT('Ctrl Pts',(13.3310152130565,-20.1510440699477,
12.));
#183784=CARTESIAN_POINT('Ctrl Pts',(13.3262148471228,-20.1294496158405,
12.));
#183785=CARTESIAN_POINT('Ctrl Pts',(13.3213804177588,-20.1079620798377,
12.));
#183786=CARTESIAN_POINT('Ctrl Pts',(13.3165124377962,-20.0865820689884,
12.));
#183787=CARTESIAN_POINT('Ctrl Pts',(13.3116114266514,-20.0653101957188,
12.));
#183788=CARTESIAN_POINT('Ctrl Pts',(13.3066779104515,-20.0441470779345,
12.));
#183789=CARTESIAN_POINT('Ctrl Pts',(13.3017124221639,-20.023093339104,12.));
#183790=CARTESIAN_POINT('Ctrl Pts',(13.296715501731,-20.0021496083742,12.));
#183791=CARTESIAN_POINT('Ctrl Pts',(13.2916876962098,-19.9813165207174,
12.));
#183792=CARTESIAN_POINT('Ctrl Pts',(13.2866295599152,-19.9605947170589,
12.));
#183793=CARTESIAN_POINT('Ctrl Pts',(13.2815416545662,-19.939984844402,12.));
#183794=CARTESIAN_POINT('Ctrl Pts',(13.2764245494354,-19.9194875559419,
12.));
#183795=CARTESIAN_POINT('Ctrl Pts',(13.2712788215015,-19.8991035111739,
12.));
#183796=CARTESIAN_POINT('Ctrl Pts',(13.2661050556128,-19.8788333760571,
12.));
#183797=CARTESIAN_POINT('Ctrl Pts',(13.2609038446525,-19.8586778231711,
12.));
#183798=CARTESIAN_POINT('Ctrl Pts',(13.2556757897085,-19.8386375318632,
12.));
#183799=CARTESIAN_POINT('Ctrl Pts',(13.2504215002458,-19.8187131883919,
12.));
#183800=CARTESIAN_POINT('Ctrl Pts',(13.2451415942809,-19.7989054860501,
12.));
#183801=CARTESIAN_POINT('Ctrl Pts',(13.239836698568,-19.7792151253297,12.));
#183802=CARTESIAN_POINT('Ctrl Pts',(13.2345074487968,-19.7596428141176,
12.));
#183803=CARTESIAN_POINT('Ctrl Pts',(13.2291544897902,-19.7401892678701,
12.));
#183804=CARTESIAN_POINT('Ctrl Pts',(13.2237784757065,-19.7208552097867,
12.));
#183805=CARTESIAN_POINT('Ctrl Pts',(13.2183800702431,-19.7016413709678,
12.));
#183806=CARTESIAN_POINT('Ctrl Pts',(13.2129599468478,-19.6825484905812,
12.));
#183807=CARTESIAN_POINT('Ctrl Pts',(13.2075187889522,-19.6635773160924,
12.));
#183808=CARTESIAN_POINT('Ctrl Pts',(13.202057290206,-19.6447286034764,12.));
#183809=CARTESIAN_POINT('Ctrl Pts',(13.196576154715,-19.6260031174244,12.));
#183810=CARTESIAN_POINT('Ctrl Pts',(13.1910760972818,-19.6074016315421,
12.));
#183811=CARTESIAN_POINT('Ctrl Pts',(13.1855578436479,-19.5889249285352,
12.));
#183812=CARTESIAN_POINT('Ctrl Pts',(13.1800221307682,-19.5705738004682,
12.));
#183813=CARTESIAN_POINT('Ctrl Pts',(13.1744697070918,-19.5523490490254,
12.));
#183814=CARTESIAN_POINT('Ctrl Pts',(13.1689013328432,-19.5342514857564,
12.));
#183815=CARTESIAN_POINT('Ctrl Pts',(13.1633177803097,-19.5162819323207,
12.));
#183816=CARTESIAN_POINT('Ctrl Pts',(13.1577198341238,-19.498441220707,12.));
#183817=CARTESIAN_POINT('Ctrl Pts',(13.1521082915846,-19.4807301935256,
12.));
#183818=CARTESIAN_POINT('Ctrl Pts',(13.1464839629966,-19.463149704325,12.));
#183819=CARTESIAN_POINT('Ctrl Pts',(13.140847672006,-19.4457006178875,12.));
#183820=CARTESIAN_POINT('Ctrl Pts',(13.1352002559439,-19.4283838105265,
12.));
#183821=CARTESIAN_POINT('Ctrl Pts',(13.1295425661635,-19.4112001703561,
12.));
#183822=CARTESIAN_POINT('Ctrl Pts',(13.1238754684177,-19.3941505976267,
12.));
#183823=CARTESIAN_POINT('Ctrl Pts',(13.118199843271,-19.3772360051093,12.));
#183824=CARTESIAN_POINT('Ctrl Pts',(13.1125165865021,-19.3604573184516,
12.));
#183825=CARTESIAN_POINT('Ctrl Pts',(13.1068266095186,-19.3438154765395,
12.));
#183826=CARTESIAN_POINT('Ctrl Pts',(13.1011308397591,-19.3273114318268,
12.));
#183827=CARTESIAN_POINT('Ctrl Pts',(13.095430221148,-19.3109461507358,12.));
#183828=CARTESIAN_POINT('Ctrl Pts',(13.0897257145969,-19.2947206141246,
12.));
#183829=CARTESIAN_POINT('Ctrl Pts',(13.0840182984949,-19.2786358177198,
12.));
#183830=CARTESIAN_POINT('Ctrl Pts',(13.0783089692117,-19.2626927725596,
12.));
#183831=CARTESIAN_POINT('Ctrl Pts',(13.0725987415856,-19.2468925053988,
12.));
#183832=CARTESIAN_POINT('Ctrl Pts',(13.0668886494791,-19.2312360592031,
12.));
#183833=CARTESIAN_POINT('Ctrl Pts',(13.0611797463912,-19.2157244937141,
12.));
#183834=CARTESIAN_POINT('Ctrl Pts',(13.0554731060537,-19.2003588859771,
12.));
#183835=CARTESIAN_POINT('Ctrl Pts',(13.0497698230442,-19.1851403308826,
12.));
#183836=CARTESIAN_POINT('Ctrl Pts',(13.0440710133775,-19.1700699416625,
12.));
#183837=CARTESIAN_POINT('Ctrl Pts',(13.0383778152072,-19.1551488505233,
12.));
#183838=CARTESIAN_POINT('Ctrl Pts',(13.0326913895841,-19.1403782093389,
12.));
#183839=CARTESIAN_POINT('Ctrl Pts',(13.0270129211976,-19.1257591903099,
12.));
#183840=CARTESIAN_POINT('Ctrl Pts',(13.0213436191326,-19.1112929866308,
12.));
#183841=CARTESIAN_POINT('Ctrl Pts',(13.0156847176093,-19.0969808131226,
12.));
#183842=CARTESIAN_POINT('Ctrl Pts',(13.0100374768785,-19.0828239070482,
12.));
#183843=CARTESIAN_POINT('Ctrl Pts',(13.0044031841381,-19.0688235289437,
12.));
#183844=CARTESIAN_POINT('Ctrl Pts',(12.9987831544502,-19.0549809634355,
12.));
#183845=CARTESIAN_POINT('Ctrl Pts',(12.9931787316514,-19.0412975200398,
12.));
#183846=CARTESIAN_POINT('Ctrl Pts',(12.9875912893003,-19.0277745339908,
12.));
#183847=CARTESIAN_POINT('Ctrl Pts',(12.9820222318715,-19.0144133673348,
12.));
#183848=CARTESIAN_POINT('Ctrl Pts',(12.9764729959205,-19.0012154099791,
12.));
#183849=CARTESIAN_POINT('Ctrl Pts',(12.9709450512747,-18.9881820807586,
12.));
#183850=CARTESIAN_POINT('Ctrl Pts',(12.9654399021869,-18.9753148284475,
12.));
#183851=CARTESIAN_POINT('Ctrl Pts',(12.9599590886319,-18.9626151329229,
12.));
#183852=CARTESIAN_POINT('Ctrl Pts',(12.9545041877377,-18.9500845064715,
12.));
#183853=CARTESIAN_POINT('Ctrl Pts',(12.9490768151821,-18.9377244950435,
12.));
#183854=CARTESIAN_POINT('Ctrl Pts',(12.9436786266105,-18.9255366795195,
12.));
#183855=CARTESIAN_POINT('Ctrl Pts',(12.9383113190374,-18.9135226769466,
12.));
#183856=CARTESIAN_POINT('Ctrl Pts',(12.9329766328184,-18.9016841423403,
12.));
#183857=CARTESIAN_POINT('Ctrl Pts',(12.9276763536373,-18.8900227704889,
12.));
#183858=CARTESIAN_POINT('Ctrl Pts',(12.9224123144981,-18.8785402977528,
12.));
#183859=CARTESIAN_POINT('Ctrl Pts',(12.9171863977045,-18.8672385038326,
12.));
#183860=CARTESIAN_POINT('Ctrl Pts',(12.9120005369063,-18.8561192136198,
12.));
#183861=CARTESIAN_POINT('Ctrl Pts',(12.9068567191854,-18.8451842990984,
12.));
#183862=CARTESIAN_POINT('Ctrl Pts',(12.9017569871738,-18.8344356812591,
12.));
#183863=CARTESIAN_POINT('Ctrl Pts',(12.8967034410754,-18.8238753319129,
12.));
#183864=CARTESIAN_POINT('Ctrl Pts',(12.8916982409935,-18.813505275782,12.));
#183865=CARTESIAN_POINT('Ctrl Pts',(12.8867436109546,-18.8033275941943,
12.));
#183866=CARTESIAN_POINT('Ctrl Pts',(12.8818418427475,-18.7933444285868,
12.));
#183867=CARTESIAN_POINT('Ctrl Pts',(12.8769952998095,-18.7835579840477,
12.));
#183868=CARTESIAN_POINT('Ctrl Pts',(12.872206421181,-18.7739705329022,12.));
#183869=CARTESIAN_POINT('Ctrl Pts',(12.8674777239653,-18.7645844169564,
12.));
#183870=CARTESIAN_POINT('Ctrl Pts',(12.8628118054171,-18.7554020493887,
12.));
#183871=CARTESIAN_POINT('Ctrl Pts',(12.8582113455646,-18.7464259171251,
12.));
#183872=CARTESIAN_POINT('Ctrl Pts',(12.8536791086316,-18.7376585820854,
12.));
#183873=CARTESIAN_POINT('Ctrl Pts',(12.8492179511591,-18.7291026886554,
12.));
#183874=CARTESIAN_POINT('Ctrl Pts',(12.8448308329494,-18.7207609737702,
12.));
#183875=CARTESIAN_POINT('Ctrl Pts',(12.8405208263431,-18.7126362754445,
12.));
#183876=CARTESIAN_POINT('Ctrl Pts',(12.8362911280361,-18.7047315436294,
12.));
#183877=CARTESIAN_POINT('Ctrl Pts',(12.8321450599789,-18.6970498410172,
12.));
#183878=CARTESIAN_POINT('Ctrl Pts',(12.8280860635231,-18.6895943376172,
12.));
#183879=CARTESIAN_POINT('Ctrl Pts',(12.8241176980017,-18.6823683094139,
12.));
#183880=CARTESIAN_POINT('Ctrl Pts',(12.8202436318474,-18.6753751301092,
12.));
#183881=CARTESIAN_POINT('Ctrl Pts',(12.8164676687362,-18.66861829528,12.));
#183882=CARTESIAN_POINT('Ctrl Pts',(12.8127937909631,-18.6621014624746,
12.));
#183883=CARTESIAN_POINT('Ctrl Pts',(12.8092261933858,-18.6558284825773,
12.));
#183884=CARTESIAN_POINT('Ctrl Pts',(12.805769331162,-18.6498034438987,12.));
#183885=CARTESIAN_POINT('Ctrl Pts',(12.8024278770152,-18.6440306327456,
12.));
#183886=CARTESIAN_POINT('Ctrl Pts',(12.7992066625264,-18.63851447924,12.));
#183887=CARTESIAN_POINT('Ctrl Pts',(12.796110622225,-18.6332595057006,12.));
#183888=CARTESIAN_POINT('Ctrl Pts',(12.7931447451555,-18.6282702819371,
12.));
#183889=CARTESIAN_POINT('Ctrl Pts',(12.7903142925234,-18.6235516265575,
12.));
#183890=CARTESIAN_POINT('Ctrl Pts',(12.7876249657834,-18.6191087624752,
12.));
#183891=CARTESIAN_POINT('Ctrl Pts',(12.7850831657901,-18.6149475565188,
12.));
#183892=CARTESIAN_POINT('Ctrl Pts',(12.7826959526924,-18.611074482622,12.));
#183893=CARTESIAN_POINT('Ctrl Pts',(12.7804705387658,-18.6074961535723,
12.));
#183894=CARTESIAN_POINT('Ctrl Pts',(12.7784139605066,-18.6042190183704,
12.));
#183895=CARTESIAN_POINT('Ctrl Pts',(12.7765325225081,-18.6012488486709,
12.));
#183896=CARTESIAN_POINT('Ctrl Pts',(12.7748328937638,-18.598591752595,12.));
#183897=CARTESIAN_POINT('Ctrl Pts',(12.7733231262108,-18.5962551167772,
12.));
#183898=CARTESIAN_POINT('Ctrl Pts',(12.7720142287172,-18.5942490615407,
12.));
#183899=CARTESIAN_POINT('Ctrl Pts',(12.7709195951156,-18.5925859134579,
12.));
#183900=CARTESIAN_POINT('Ctrl Pts',(12.7700520897173,-18.5912775137806,
12.));
#183901=CARTESIAN_POINT('Ctrl Pts',(12.7694215127918,-18.5903328777227,
12.));
#183902=CARTESIAN_POINT('Ctrl Pts',(12.769110348199,-18.589871621843,12.));
#183903=CARTESIAN_POINT('Ctrl Pts',(12.768986426692,-18.5896919669165,12.));
#183904=CARTESIAN_POINT('Ctrl Pts',(12.7689524524483,-18.5896460962964,
12.));
#183905=CARTESIAN_POINT('Ctrl Pts',(12.7689476255362,-18.5896416359912,
12.));
#183906=CARTESIAN_POINT('',(12.4528436808172,-18.1294424696716,12.));
#183907=CARTESIAN_POINT('',(6.08648437878337,-8.86099361848466,12.));
#183908=CARTESIAN_POINT('',(12.572596943457,-17.4407513054162,12.));
#183909=CARTESIAN_POINT('Origin',(12.8649829188862,-17.846350172984,12.));
#183910=CARTESIAN_POINT('',(13.5924445804218,-16.6581946899465,12.));
#183911=CARTESIAN_POINT('Origin',(4.50593605254674E-13,-6.37232247690087E-13,
12.));
#183912=CARTESIAN_POINT('',(14.2886635873976,-16.7207683102834,12.));
#183913=CARTESIAN_POINT('Origin',(13.9085479427572,-17.0455945664569,12.));
#183914=CARTESIAN_POINT('',(14.6513681262571,-17.1452095830633,12.));
#183915=CARTESIAN_POINT('',(7.32568406312854,-8.57260479153162,12.));
#183916=CARTESIAN_POINT('',(17.9112098770111,-18.8464468996588,12.));
#183917=CARTESIAN_POINT('Ctrl Pts',(14.6513681262571,-17.1452095830633,
12.));
#183918=CARTESIAN_POINT('Ctrl Pts',(14.6513711852839,-17.1452153999142,
12.));
#183919=CARTESIAN_POINT('Ctrl Pts',(14.6514066997188,-17.1452600887039,
12.));
#183920=CARTESIAN_POINT('Ctrl Pts',(14.6515481598057,-17.1454262858045,
12.));
#183921=CARTESIAN_POINT('Ctrl Pts',(14.65191316345,-17.1458462295273,12.));
#183922=CARTESIAN_POINT('Ctrl Pts',(14.6526624064978,-17.1466998098673,
12.));
#183923=CARTESIAN_POINT('Ctrl Pts',(14.6537016966188,-17.1478763944909,
12.));
#183924=CARTESIAN_POINT('Ctrl Pts',(14.6550248622813,-17.1493641837556,
12.));
#183925=CARTESIAN_POINT('Ctrl Pts',(14.6566237952435,-17.1511476869495,
12.));
#183926=CARTESIAN_POINT('Ctrl Pts',(14.65849005553,-17.1532107762719,12.));
#183927=CARTESIAN_POINT('Ctrl Pts',(14.660616716964,-17.1555401986403,12.));
#183928=CARTESIAN_POINT('Ctrl Pts',(14.662998728599,-17.1581262646789,12.));
#183929=CARTESIAN_POINT('Ctrl Pts',(14.6656319165057,-17.1609609517369,
12.));
#183930=CARTESIAN_POINT('Ctrl Pts',(14.6685123374424,-17.1640366762304,
12.));
#183931=CARTESIAN_POINT('Ctrl Pts',(14.6716355833321,-17.1673449723019,
12.));
#183932=CARTESIAN_POINT('Ctrl Pts',(14.6749971333867,-17.1708771619129,
12.));
#183933=CARTESIAN_POINT('Ctrl Pts',(14.6785925615676,-17.1746247499057,
12.));
#183934=CARTESIAN_POINT('Ctrl Pts',(14.6824178576166,-17.1785800350827,
12.));
#183935=CARTESIAN_POINT('Ctrl Pts',(14.6864694522319,-17.182736158472,12.));
#183936=CARTESIAN_POINT('Ctrl Pts',(14.6907440526957,-17.1870867909918,
12.));
#183937=CARTESIAN_POINT('Ctrl Pts',(14.6952385361706,-17.1916259308416,
12.));
#183938=CARTESIAN_POINT('Ctrl Pts',(14.699949811582,-17.1963476411694,12.));
#183939=CARTESIAN_POINT('Ctrl Pts',(14.7048748502662,-17.2012461084268,
12.));
#183940=CARTESIAN_POINT('Ctrl Pts',(14.7100107213586,-17.2063157097316,
12.));
#183941=CARTESIAN_POINT('Ctrl Pts',(14.7153546289338,-17.2115510835988,
12.));
#183942=CARTESIAN_POINT('Ctrl Pts',(14.7209039390325,-17.2169471814255,
12.));
#183943=CARTESIAN_POINT('Ctrl Pts',(14.7266561494282,-17.2224992099666,
12.));
#183944=CARTESIAN_POINT('Ctrl Pts',(14.7326088681163,-17.2282025904314,
12.));
#183945=CARTESIAN_POINT('Ctrl Pts',(14.7387597858117,-17.2340529062078,
12.));
#183946=CARTESIAN_POINT('Ctrl Pts',(14.7451066593793,-17.2400458713566,
12.));
#183947=CARTESIAN_POINT('Ctrl Pts',(14.7516473175124,-17.2461773413289,
12.));
#183948=CARTESIAN_POINT('Ctrl Pts',(14.7583796616617,-17.2524433146837,
12.));
#183949=CARTESIAN_POINT('Ctrl Pts',(14.7653016697589,-17.2588399401464,
12.));
#183950=CARTESIAN_POINT('Ctrl Pts',(14.7724113956728,-17.2653635155317,
12.));
#183951=CARTESIAN_POINT('Ctrl Pts',(14.7797069617802,-17.2720104735192,
12.));
#183952=CARTESIAN_POINT('Ctrl Pts',(14.787186553128,-17.278777370485,12.));
#183953=CARTESIAN_POINT('Ctrl Pts',(14.7948484105252,-17.28566087332,12.));
#183954=CARTESIAN_POINT('Ctrl Pts',(14.8026908254281,-17.2926577496519,
12.));
#183955=CARTESIAN_POINT('Ctrl Pts',(14.8107121391038,-17.2997648661483,
12.));
#183956=CARTESIAN_POINT('Ctrl Pts',(14.8189107410161,-17.3069791853705,
12.));
#183957=CARTESIAN_POINT('Ctrl Pts',(14.8272850675375,-17.3142977632656,
12.));
#183958=CARTESIAN_POINT('Ctrl Pts',(14.8358336004193,-17.3217177462096,
12.));
#183959=CARTESIAN_POINT('Ctrl Pts',(14.8445548643504,-17.3292363662601,
12.));
#183960=CARTESIAN_POINT('Ctrl Pts',(14.8534474245433,-17.336850936485,12.));
#183961=CARTESIAN_POINT('Ctrl Pts',(14.8625098843419,-17.3445588463477,
12.));
#183962=CARTESIAN_POINT('Ctrl Pts',(14.8717408826957,-17.3523575568648,
12.));
#183963=CARTESIAN_POINT('Ctrl Pts',(14.8811390927424,-17.3602445978163,
12.));
#183964=CARTESIAN_POINT('Ctrl Pts',(14.8907032205789,-17.3682175653236,
12.));
#183965=CARTESIAN_POINT('Ctrl Pts',(14.9004320039609,-17.3762741193075,
12.));
#183966=CARTESIAN_POINT('Ctrl Pts',(14.9103242110057,-17.3844119809823,
12.));
#183967=CARTESIAN_POINT('Ctrl Pts',(14.9203786389343,-17.3926289303987,
12.));
#183968=CARTESIAN_POINT('Ctrl Pts',(14.9305941128758,-17.400922804075,12.));
#183969=CARTESIAN_POINT('Ctrl Pts',(14.940969484645,-17.4092914926072,12.));
#183970=CARTESIAN_POINT('Ctrl Pts',(14.9515036315142,-17.4177329382827,
12.));
#183971=CARTESIAN_POINT('Ctrl Pts',(14.9621954549825,-17.4262451327088,
12.));
#183972=CARTESIAN_POINT('Ctrl Pts',(14.973043879945,-17.4348261151395,12.));
#183973=CARTESIAN_POINT('Ctrl Pts',(14.9840478538357,-17.4434739707773,
12.));
#183974=CARTESIAN_POINT('Ctrl Pts',(14.9952063457779,-17.4521868291005,
12.));
#183975=CARTESIAN_POINT('Ctrl Pts',(15.0065183456922,-17.4609628621419,
12.));
#183976=CARTESIAN_POINT('Ctrl Pts',(15.0179828635087,-17.4698002829357,
12.));
#183977=CARTESIAN_POINT('Ctrl Pts',(15.029598928488,-17.4786973441417,12.));
#183978=CARTESIAN_POINT('Ctrl Pts',(15.0413655884993,-17.4876523366178,
12.));
#183979=CARTESIAN_POINT('Ctrl Pts',(15.0532819093085,-17.4966635880246,
12.));
#183980=CARTESIAN_POINT('Ctrl Pts',(15.0653469738307,-17.5057294613877,
12.));
#183981=CARTESIAN_POINT('Ctrl Pts',(15.0775598815749,-17.5148483539687,
12.));
#183982=CARTESIAN_POINT('Ctrl Pts',(15.0899197481082,-17.5240186961791,
12.));
#183983=CARTESIAN_POINT('Ctrl Pts',(15.1024257045033,-17.5332389504829,
12.));
#183984=CARTESIAN_POINT('Ctrl Pts',(15.1150768967728,-17.5425076102963,
12.));
#183985=CARTESIAN_POINT('Ctrl Pts',(15.1278724853138,-17.5518231989117,
12.));
#183986=CARTESIAN_POINT('Ctrl Pts',(15.1408116444876,-17.5611842686192,
12.));
#183987=CARTESIAN_POINT('Ctrl Pts',(15.1538935621714,-17.5705893998029,
12.));
#183988=CARTESIAN_POINT('Ctrl Pts',(15.1671174393137,-17.580037200054,12.));
#183989=CARTESIAN_POINT('Ctrl Pts',(15.1804824894605,-17.5895263032595,
12.));
#183990=CARTESIAN_POINT('Ctrl Pts',(15.1939879383268,-17.5990553687599,
12.));
#183991=CARTESIAN_POINT('Ctrl Pts',(15.2076330234686,-17.60862308065,12.));
#183992=CARTESIAN_POINT('Ctrl Pts',(15.2214169939199,-17.6182281470468,
12.));
#183993=CARTESIAN_POINT('Ctrl Pts',(15.2353391098366,-17.6278692993764,
12.));
#183994=CARTESIAN_POINT('Ctrl Pts',(15.2493986421092,-17.6375452916369,
12.));
#183995=CARTESIAN_POINT('Ctrl Pts',(15.2635948720292,-17.6472548997328,
12.));
#183996=CARTESIAN_POINT('Ctrl Pts',(15.2779270910239,-17.6569969209,12.));
#183997=CARTESIAN_POINT('Ctrl Pts',(15.2923946003598,-17.6667701731041,
12.));
#183998=CARTESIAN_POINT('Ctrl Pts',(15.30699671085,-17.676573494456,12.));
#183999=CARTESIAN_POINT('Ctrl Pts',(15.3217327425338,-17.6864057426052,
12.));
#184000=CARTESIAN_POINT('Ctrl Pts',(15.3366020244066,-17.6962657941983,
12.));
#184001=CARTESIAN_POINT('Ctrl Pts',(15.351603894206,-17.7061525444042,12.));
#184002=CARTESIAN_POINT('Ctrl Pts',(15.3667376981699,-17.7160649064206,
12.));
#184003=CARTESIAN_POINT('Ctrl Pts',(15.3820027907966,-17.7260018109924,
12.));
#184004=CARTESIAN_POINT('Ctrl Pts',(15.3973985345802,-17.735962205915,12.));
#184005=CARTESIAN_POINT('Ctrl Pts',(15.4129242997837,-17.7459450555813,
12.));
#184006=CARTESIAN_POINT('Ctrl Pts',(15.4285794642667,-17.7559493405881,
12.));
#184007=CARTESIAN_POINT('Ctrl Pts',(15.4443634132869,-17.7659740573265,
12.));
#184008=CARTESIAN_POINT('Ctrl Pts',(15.4602755393017,-17.7760182175815,
12.));
#184009=CARTESIAN_POINT('Ctrl Pts',(15.4763152417497,-17.786080848122,12.));
#184010=CARTESIAN_POINT('Ctrl Pts',(15.4924819268517,-17.7961609903148,
12.));
#184011=CARTESIAN_POINT('Ctrl Pts',(15.5087750074718,-17.8062576997952,
12.));
#184012=CARTESIAN_POINT('Ctrl Pts',(15.5251939029552,-17.8163700461256,
12.));
#184013=CARTESIAN_POINT('Ctrl Pts',(15.541738038964,-17.8264971124607,12.));
#184014=CARTESIAN_POINT('Ctrl Pts',(15.5584068472982,-17.8366379952085,
12.));
#184015=CARTESIAN_POINT('Ctrl Pts',(15.5751997657162,-17.8467918036987,
12.));
#184016=CARTESIAN_POINT('Ctrl Pts',(15.5921162378192,-17.8569576599006,
12.));
#184017=CARTESIAN_POINT('Ctrl Pts',(15.609155712921,-17.8671346981394,12.));
#184018=CARTESIAN_POINT('Ctrl Pts',(15.6263176459108,-17.8773220648125,
12.));
#184019=CARTESIAN_POINT('Ctrl Pts',(15.6436014971084,-17.8875189181091,
12.));
#184020=CARTESIAN_POINT('Ctrl Pts',(15.661006732103,-17.897724427724,12.));
#184021=CARTESIAN_POINT('Ctrl Pts',(15.678532821646,-17.9079377746111,12.));
#184022=CARTESIAN_POINT('Ctrl Pts',(15.6961792415522,-17.9181581507455,
12.));
#184023=CARTESIAN_POINT('Ctrl Pts',(15.7139454725838,-17.9283847588836,
12.));
#184024=CARTESIAN_POINT('Ctrl Pts',(15.7318310003335,-17.9386168123262,
12.));
#184025=CARTESIAN_POINT('Ctrl Pts',(15.749835315086,-17.9488535346781,12.));
#184026=CARTESIAN_POINT('Ctrl Pts',(15.7679579117077,-17.9590941596242,
12.));
#184027=CARTESIAN_POINT('Ctrl Pts',(15.7861982895724,-17.9693379307303,
12.));
#184028=CARTESIAN_POINT('Ctrl Pts',(15.8045559524676,-17.9795841012386,
12.));
#184029=CARTESIAN_POINT('Ctrl Pts',(15.8230304084962,-17.9898319338665,
12.));
#184030=CARTESIAN_POINT('Ctrl Pts',(15.8416211699679,-18.0000807006052,
12.));
#184031=CARTESIAN_POINT('Ctrl Pts',(15.8603277532831,-18.0103296825205,
12.));
#184032=CARTESIAN_POINT('Ctrl Pts',(15.8791496788682,-18.0205781695769,
12.));
#184033=CARTESIAN_POINT('Ctrl Pts',(15.8980864711042,-18.0308254604636,
12.));
#184034=CARTESIAN_POINT('Ctrl Pts',(15.9171376582436,-18.0410708624209,
12.));
#184035=CARTESIAN_POINT('Ctrl Pts',(15.9363027723244,-18.0513136910691,
12.));
#184036=CARTESIAN_POINT('Ctrl Pts',(15.9555813490644,-18.061553270236,12.));
#184037=CARTESIAN_POINT('Ctrl Pts',(15.9749729277846,-18.0717889317958,
12.));
#184038=CARTESIAN_POINT('Ctrl Pts',(15.9944770513613,-18.0820200155236,
12.));
#184039=CARTESIAN_POINT('Ctrl Pts',(16.014093266161,-18.0922458689462,12.));
#184040=CARTESIAN_POINT('Ctrl Pts',(16.0338211219693,-18.1024658471966,
12.));
#184041=CARTESIAN_POINT('Ctrl Pts',(16.0536601719125,-18.112679312869,12.));
#184042=CARTESIAN_POINT('Ctrl Pts',(16.0736099723668,-18.1228856358751,
12.));
#184043=CARTESIAN_POINT('Ctrl Pts',(16.0936700829112,-18.1330841933105,
12.));
#184044=CARTESIAN_POINT('Ctrl Pts',(16.1138400662794,-18.1432743693235,
12.));
#184045=CARTESIAN_POINT('Ctrl Pts',(16.1341194882988,-18.1534555549853,
12.));
#184046=CARTESIAN_POINT('Ctrl Pts',(16.154507917826,-18.1636271481615,12.));
#184047=CARTESIAN_POINT('Ctrl Pts',(16.1750049266671,-18.1737885533849,
12.));
#184048=CARTESIAN_POINT('Ctrl Pts',(16.1956100895073,-18.1839391817331,
12.));
#184049=CARTESIAN_POINT('Ctrl Pts',(16.2163229838875,-18.1940784507229,
12.));
#184050=CARTESIAN_POINT('Ctrl Pts',(16.2371431901638,-18.2042057842035,
12.));
#184051=CARTESIAN_POINT('Ctrl Pts',(16.2580702914615,-18.2143206122529,
12.));
#184052=CARTESIAN_POINT('Ctrl Pts',(16.2791038736223,-18.2244223710746,
12.));
#184053=CARTESIAN_POINT('Ctrl Pts',(16.3002435251378,-18.2345105028982,
12.));
#184054=CARTESIAN_POINT('Ctrl Pts',(16.3214888370987,-18.2445844558742,
12.));
#184055=CARTESIAN_POINT('Ctrl Pts',(16.3428394031589,-18.2546436839608,
12.));
#184056=CARTESIAN_POINT('Ctrl Pts',(16.3642948194868,-18.2646876468169,
12.));
#184057=CARTESIAN_POINT('Ctrl Pts',(16.385854684708,-18.2747158096934,12.));
#184058=CARTESIAN_POINT('Ctrl Pts',(16.4075185998454,-18.2847276433309,
12.));
#184059=CARTESIAN_POINT('Ctrl Pts',(16.4292861682378,-18.294722623851,12.));
#184060=CARTESIAN_POINT('Ctrl Pts',(16.4511569955233,-18.304700232686,12.));
#184061=CARTESIAN_POINT('Ctrl Pts',(16.4731306896441,-18.3146599565231,
12.));
#184062=CARTESIAN_POINT('Ctrl Pts',(16.4952068608345,-18.3246012872469,
12.));
#184063=CARTESIAN_POINT('Ctrl Pts',(16.5173851216045,-18.3345237218864,
12.));
#184064=CARTESIAN_POINT('Ctrl Pts',(16.5396650867139,-18.34442676256,12.));
#184065=CARTESIAN_POINT('Ctrl Pts',(16.5620463731413,-18.354309916433,12.));
#184066=CARTESIAN_POINT('Ctrl Pts',(16.5845286000217,-18.3641726955889,
12.));
#184067=CARTESIAN_POINT('Ctrl Pts',(16.607111388571,-18.3740146168879,12.));
#184068=CARTESIAN_POINT('Ctrl Pts',(16.6297943620056,-18.3838352018327,
12.));
#184069=CARTESIAN_POINT('Ctrl Pts',(16.6525771454513,-18.3936339764332,
12.));
#184070=CARTESIAN_POINT('Ctrl Pts',(16.6754593658513,-18.403410471079,12.));
#184071=CARTESIAN_POINT('Ctrl Pts',(16.698440651849,-18.413164220399,12.));
#184072=CARTESIAN_POINT('Ctrl Pts',(16.7215206338818,-18.4228947633187,
12.));
#184073=CARTESIAN_POINT('Ctrl Pts',(16.7446989442882,-18.4326016431392,
12.));
#184074=CARTESIAN_POINT('Ctrl Pts',(16.7679752173992,-18.44228440761,12.));
#184075=CARTESIAN_POINT('Ctrl Pts',(16.791349089629,-18.4519426090124,12.));
#184076=CARTESIAN_POINT('Ctrl Pts',(16.8148201995472,-18.4615758042305,
12.));
#184077=CARTESIAN_POINT('Ctrl Pts',(16.8383881879709,-18.4711835548623,
12.));
#184078=CARTESIAN_POINT('Ctrl Pts',(16.8620526977171,-18.4807654268771,
12.));
#184079=CARTESIAN_POINT('Ctrl Pts',(16.8858133733088,-18.4903209902227,
12.));
#184080=CARTESIAN_POINT('Ctrl Pts',(16.9096698606943,-18.499849818462,12.));
#184081=CARTESIAN_POINT('Ctrl Pts',(16.9336218069353,-18.5093514883835,
12.));
#184082=CARTESIAN_POINT('Ctrl Pts',(16.9576688599339,-18.5188255796659,
12.));
#184083=CARTESIAN_POINT('Ctrl Pts',(16.981810668038,-18.5282716744197,12.));
#184084=CARTESIAN_POINT('Ctrl Pts',(17.0060468805097,-18.5376893576961,
12.));
#184085=CARTESIAN_POINT('Ctrl Pts',(17.0303771481738,-18.547078218209,12.));
#184086=CARTESIAN_POINT('Ctrl Pts',(17.0548011239751,-18.556437848963,12.));
#184087=CARTESIAN_POINT('Ctrl Pts',(17.0793184636079,-18.5657678479789,
12.));
#184088=CARTESIAN_POINT('Ctrl Pts',(17.1039288260001,-18.5750678188542,
12.));
#184089=CARTESIAN_POINT('Ctrl Pts',(17.1286318741183,-18.5843373717247,
12.));
#184090=CARTESIAN_POINT('Ctrl Pts',(17.1534272741643,-18.5935761222825,
12.));
#184091=CARTESIAN_POINT('Ctrl Pts',(17.1783146940127,-18.6027836898817,
12.));
#184092=CARTESIAN_POINT('Ctrl Pts',(17.2032938019284,-18.6119596959949,
12.));
#184093=CARTESIAN_POINT('Ctrl Pts',(17.2283642650517,-18.6211037624038,
12.));
#184094=CARTESIAN_POINT('Ctrl Pts',(17.2535257482187,-18.6302155097943,
12.));
#184095=CARTESIAN_POINT('Ctrl Pts',(17.2787779120213,-18.6392945554748,
12.));
#184096=CARTESIAN_POINT('Ctrl Pts',(17.3041204135074,-18.6483405141865,
12.));
#184097=CARTESIAN_POINT('Ctrl Pts',(17.3295529098618,-18.6573530024033,
12.));
#184098=CARTESIAN_POINT('Ctrl Pts',(17.3550750612443,-18.6663316416582,
12.));
#184099=CARTESIAN_POINT('Ctrl Pts',(17.3806865340747,-18.6752760624052,
12.));
#184100=CARTESIAN_POINT('Ctrl Pts',(17.4063870038562,-18.6841859073471,
12.));
#184101=CARTESIAN_POINT('Ctrl Pts',(17.4321761588142,-18.6930608357409,
12.));
#184102=CARTESIAN_POINT('Ctrl Pts',(17.4580537012753,-18.70190052503,12.));
#184103=CARTESIAN_POINT('Ctrl Pts',(17.4840193397162,-18.7107046613912,
12.));
#184104=CARTESIAN_POINT('Ctrl Pts',(17.5100727820876,-18.7194729318098,
12.));
#184105=CARTESIAN_POINT('Ctrl Pts',(17.5362137287593,-18.7282050157138,
12.));
#184106=CARTESIAN_POINT('Ctrl Pts',(17.5624418653245,-18.7369005764553,
12.));
#184107=CARTESIAN_POINT('Ctrl Pts',(17.5887568561371,-18.7455592536688,
12.));
#184108=CARTESIAN_POINT('Ctrl Pts',(17.6151583357012,-18.7541806530984,
12.));
#184109=CARTESIAN_POINT('Ctrl Pts',(17.6416459210681,-18.762764361321,12.));
#184110=CARTESIAN_POINT('Ctrl Pts',(17.6682192274236,-18.7713099642754,
12.));
#184111=CARTESIAN_POINT('Ctrl Pts',(17.6948778823014,-18.7798170641374,
12.));
#184112=CARTESIAN_POINT('Ctrl Pts',(17.7216215409035,-18.788285297605,12.));
#184113=CARTESIAN_POINT('Ctrl Pts',(17.7484498996905,-18.7967143519419,
12.));
#184114=CARTESIAN_POINT('Ctrl Pts',(17.7753627137853,-18.8051039860448,
12.));
#184115=CARTESIAN_POINT('Ctrl Pts',(17.8023598011057,-18.8134540340417,
12.));
#184116=CARTESIAN_POINT('Ctrl Pts',(17.8294410311006,-18.8217643886157,
12.));
#184117=CARTESIAN_POINT('Ctrl Pts',(17.856606317477,-18.8300349895974,12.));
#184118=CARTESIAN_POINT('Ctrl Pts',(17.8784057509355,-18.8366196462581,
12.));
#184119=CARTESIAN_POINT('Ctrl Pts',(17.8947931177807,-18.8415402351786,
12.));
#184120=CARTESIAN_POINT('Ctrl Pts',(17.9057348246595,-18.8448126709692,
12.));
#184121=CARTESIAN_POINT('Ctrl Pts',(17.9112098770111,-18.8464468996588,
12.));
#184122=CARTESIAN_POINT('',(18.8464468996588,-17.9112098770111,12.));
#184123=CARTESIAN_POINT('Origin',(0.,0.,12.));
#184124=CARTESIAN_POINT('',(17.1452095830632,-14.6513681262571,12.));
#184125=CARTESIAN_POINT('Ctrl Pts',(18.8464468996588,-17.9112098770111,
12.));
#184126=CARTESIAN_POINT('Ctrl Pts',(18.8448126709726,-17.9057348246611,
12.));
#184127=CARTESIAN_POINT('Ctrl Pts',(18.8415402351882,-17.8947931177853,
12.));
#184128=CARTESIAN_POINT('Ctrl Pts',(18.8366196462746,-17.8784057509434,
12.));
#184129=CARTESIAN_POINT('Ctrl Pts',(18.8300349896187,-17.8566063174871,
12.));
#184130=CARTESIAN_POINT('Ctrl Pts',(18.8217643886368,-17.8294410311105,
12.));
#184131=CARTESIAN_POINT('Ctrl Pts',(18.8134540340581,-17.8023598011135,
12.));
#184132=CARTESIAN_POINT('Ctrl Pts',(18.8051039860543,-17.7753627137898,
12.));
#184133=CARTESIAN_POINT('Ctrl Pts',(18.7967143519444,-17.7484498996916,
12.));
#184134=CARTESIAN_POINT('Ctrl Pts',(18.7882852976016,-17.7216215409019,
12.));
#184135=CARTESIAN_POINT('Ctrl Pts',(18.7798170641305,-17.6948778822982,
12.));
#184136=CARTESIAN_POINT('Ctrl Pts',(18.7713099642673,-17.6682192274197,
12.));
#184137=CARTESIAN_POINT('Ctrl Pts',(18.7627643613139,-17.6416459210646,
12.));
#184138=CARTESIAN_POINT('Ctrl Pts',(18.7541806530935,-17.6151583356989,
12.));
#184139=CARTESIAN_POINT('Ctrl Pts',(18.7455592536667,-17.5887568561361,
12.));
#184140=CARTESIAN_POINT('Ctrl Pts',(18.7369005764558,-17.5624418653248,
12.));
#184141=CARTESIAN_POINT('Ctrl Pts',(18.728205015716,-17.5362137287604,12.));
#184142=CARTESIAN_POINT('Ctrl Pts',(18.7194729318127,-17.5100727820891,
12.));
#184143=CARTESIAN_POINT('Ctrl Pts',(18.7107046613941,-17.4840193397176,
12.));
#184144=CARTESIAN_POINT('Ctrl Pts',(18.7019005250322,-17.4580537012764,
12.));
#184145=CARTESIAN_POINT('Ctrl Pts',(18.6930608357421,-17.4321761588148,
12.));
#184146=CARTESIAN_POINT('Ctrl Pts',(18.6841859073472,-17.4063870038563,
12.));
#184147=CARTESIAN_POINT('Ctrl Pts',(18.6752760624045,-17.3806865340744,
12.));
#184148=CARTESIAN_POINT('Ctrl Pts',(18.6663316416569,-17.3550750612438,
12.));
#184149=CARTESIAN_POINT('Ctrl Pts',(18.6573530024019,-17.3295529098612,
12.));
#184150=CARTESIAN_POINT('Ctrl Pts',(18.6483405141853,-17.3041204135069,
12.));
#184151=CARTESIAN_POINT('Ctrl Pts',(18.639294555474,-17.278777912021,12.));
#184152=CARTESIAN_POINT('Ctrl Pts',(18.630215509794,-17.2535257482186,12.));
#184153=CARTESIAN_POINT('Ctrl Pts',(18.6211037624041,-17.2283642650519,
12.));
#184154=CARTESIAN_POINT('Ctrl Pts',(18.6119596959957,-17.2032938019288,
12.));
#184155=CARTESIAN_POINT('Ctrl Pts',(18.6027836898826,-17.1783146940131,
12.));
#184156=CARTESIAN_POINT('Ctrl Pts',(18.5935761222833,-17.1534272741646,
12.));
#184157=CARTESIAN_POINT('Ctrl Pts',(18.5843373717253,-17.1286318741185,
12.));
#184158=CARTESIAN_POINT('Ctrl Pts',(18.5750678188543,-17.1039288260002,
12.));
#184159=CARTESIAN_POINT('Ctrl Pts',(18.5657678479788,-17.0793184636079,
12.));
#184160=CARTESIAN_POINT('Ctrl Pts',(18.5564378489628,-17.0548011239751,
12.));
#184161=CARTESIAN_POINT('Ctrl Pts',(18.5470782182089,-17.030377148174,12.));
#184162=CARTESIAN_POINT('Ctrl Pts',(18.5376893576961,-17.0060468805099,
12.));
#184163=CARTESIAN_POINT('Ctrl Pts',(18.5282716744198,-16.9818106680382,
12.));
#184164=CARTESIAN_POINT('Ctrl Pts',(18.518825579666,-16.957668859934,12.));
#184165=CARTESIAN_POINT('Ctrl Pts',(18.5093514883835,-16.9336218069353,
12.));
#184166=CARTESIAN_POINT('Ctrl Pts',(18.4998498184619,-16.9096698606942,
12.));
#184167=CARTESIAN_POINT('Ctrl Pts',(18.4903209902226,-16.8858133733086,
12.));
#184168=CARTESIAN_POINT('Ctrl Pts',(18.4807654268769,-16.8620526977169,
12.));
#184169=CARTESIAN_POINT('Ctrl Pts',(18.4711835548622,-16.8383881879707,
12.));
#184170=CARTESIAN_POINT('Ctrl Pts',(18.4615758042305,-16.8148201995472,
12.));
#184171=CARTESIAN_POINT('Ctrl Pts',(18.4519426090124,-16.791349089629,12.));
#184172=CARTESIAN_POINT('Ctrl Pts',(18.4422844076099,-16.7679752173992,
12.));
#184173=CARTESIAN_POINT('Ctrl Pts',(18.4326016431392,-16.7446989442882,
12.));
#184174=CARTESIAN_POINT('Ctrl Pts',(18.4228947633186,-16.7215206338818,
12.));
#184175=CARTESIAN_POINT('Ctrl Pts',(18.4131642203989,-16.698440651849,12.));
#184176=CARTESIAN_POINT('Ctrl Pts',(18.4034104710789,-16.6754593658513,
12.));
#184177=CARTESIAN_POINT('Ctrl Pts',(18.3936339764332,-16.6525771454513,
12.));
#184178=CARTESIAN_POINT('Ctrl Pts',(18.3838352018327,-16.6297943620056,
12.));
#184179=CARTESIAN_POINT('Ctrl Pts',(18.3740146168879,-16.6071113885711,
12.));
#184180=CARTESIAN_POINT('Ctrl Pts',(18.364172695589,-16.5845286000218,12.));
#184181=CARTESIAN_POINT('Ctrl Pts',(18.3543099164331,-16.5620463731414,
12.));
#184182=CARTESIAN_POINT('Ctrl Pts',(18.3444267625601,-16.5396650867139,
12.));
#184183=CARTESIAN_POINT('Ctrl Pts',(18.3345237218864,-16.5173851216045,
12.));
#184184=CARTESIAN_POINT('Ctrl Pts',(18.3246012872468,-16.4952068608344,
12.));
#184185=CARTESIAN_POINT('Ctrl Pts',(18.3146599565229,-16.4731306896439,
12.));
#184186=CARTESIAN_POINT('Ctrl Pts',(18.3047002326858,-16.4511569955231,
12.));
#184187=CARTESIAN_POINT('Ctrl Pts',(18.2947226238509,-16.4292861682377,
12.));
#184188=CARTESIAN_POINT('Ctrl Pts',(18.2847276433308,-16.4075185998454,
12.));
#184189=CARTESIAN_POINT('Ctrl Pts',(18.2747158096934,-16.385854684708,12.));
#184190=CARTESIAN_POINT('Ctrl Pts',(18.2646876468169,-16.3642948194869,
12.));
#184191=CARTESIAN_POINT('Ctrl Pts',(18.2546436839609,-16.342839403159,12.));
#184192=CARTESIAN_POINT('Ctrl Pts',(18.2445844558742,-16.3214888370988,
12.));
#184193=CARTESIAN_POINT('Ctrl Pts',(18.2345105028981,-16.3002435251378,
12.));
#184194=CARTESIAN_POINT('Ctrl Pts',(18.2244223710745,-16.2791038736223,
12.));
#184195=CARTESIAN_POINT('Ctrl Pts',(18.214320612253,-16.2580702914615,12.));
#184196=CARTESIAN_POINT('Ctrl Pts',(18.2042057842037,-16.237143190164,12.));
#184197=CARTESIAN_POINT('Ctrl Pts',(18.1940784507232,-16.2163229838878,
12.));
#184198=CARTESIAN_POINT('Ctrl Pts',(18.1839391817335,-16.1956100895076,
12.));
#184199=CARTESIAN_POINT('Ctrl Pts',(18.1737885533852,-16.1750049266673,
12.));
#184200=CARTESIAN_POINT('Ctrl Pts',(18.1636271481616,-16.1545079178261,
12.));
#184201=CARTESIAN_POINT('Ctrl Pts',(18.153455554985,-16.1341194882987,12.));
#184202=CARTESIAN_POINT('Ctrl Pts',(18.1432743693231,-16.113840066279,12.));
#184203=CARTESIAN_POINT('Ctrl Pts',(18.1330841933099,-16.0936700829108,
12.));
#184204=CARTESIAN_POINT('Ctrl Pts',(18.1228856358746,-16.0736099723664,
12.));
#184205=CARTESIAN_POINT('Ctrl Pts',(18.1126793128688,-16.0536601719124,
12.));
#184206=CARTESIAN_POINT('Ctrl Pts',(18.1024658471966,-16.0338211219694,
12.));
#184207=CARTESIAN_POINT('Ctrl Pts',(18.0922458689464,-16.0140932661612,
12.));
#184208=CARTESIAN_POINT('Ctrl Pts',(18.0820200155239,-15.9944770513616,
12.));
#184209=CARTESIAN_POINT('Ctrl Pts',(18.071788931796,-15.9749729277848,12.));
#184210=CARTESIAN_POINT('Ctrl Pts',(18.061553270236,-15.9555813490645,12.));
#184211=CARTESIAN_POINT('Ctrl Pts',(18.0513136910691,-15.9363027723244,
12.));
#184212=CARTESIAN_POINT('Ctrl Pts',(18.0410708624208,-15.9171376582436,
12.));
#184213=CARTESIAN_POINT('Ctrl Pts',(18.0308254604638,-15.8980864711043,
12.));
#184214=CARTESIAN_POINT('Ctrl Pts',(18.0205781695773,-15.8791496788685,
12.));
#184215=CARTESIAN_POINT('Ctrl Pts',(18.010329682521,-15.8603277532834,12.));
#184216=CARTESIAN_POINT('Ctrl Pts',(18.0000807006055,-15.8416211699682,
12.));
#184217=CARTESIAN_POINT('Ctrl Pts',(17.9898319338664,-15.8230304084963,
12.));
#184218=CARTESIAN_POINT('Ctrl Pts',(17.9795841012383,-15.8045559524674,
12.));
#184219=CARTESIAN_POINT('Ctrl Pts',(17.9693379307297,-15.786198289572,12.));
#184220=CARTESIAN_POINT('Ctrl Pts',(17.9590941596236,-15.7679579117072,
12.));
#184221=CARTESIAN_POINT('Ctrl Pts',(17.9488535346776,-15.7498353150856,
12.));
#184222=CARTESIAN_POINT('Ctrl Pts',(17.9386168123261,-15.7318310003334,
12.));
#184223=CARTESIAN_POINT('Ctrl Pts',(17.9283847588837,-15.713945472584,12.));
#184224=CARTESIAN_POINT('Ctrl Pts',(17.918158150746,-15.6961792415526,12.));
#184225=CARTESIAN_POINT('Ctrl Pts',(17.9079377746118,-15.6785328216467,
12.));
#184226=CARTESIAN_POINT('Ctrl Pts',(17.8977244277247,-15.6610067321036,
12.));
#184227=CARTESIAN_POINT('Ctrl Pts',(17.8875189181095,-15.6436014971088,
12.));
#184228=CARTESIAN_POINT('Ctrl Pts',(17.8773220648125,-15.6263176459107,
12.));
#184229=CARTESIAN_POINT('Ctrl Pts',(17.8671346981388,-15.6091557129205,
12.));
#184230=CARTESIAN_POINT('Ctrl Pts',(17.8569576598996,-15.5921162378183,
12.));
#184231=CARTESIAN_POINT('Ctrl Pts',(17.8467918036976,-15.5751997657153,
12.));
#184232=CARTESIAN_POINT('Ctrl Pts',(17.8366379952078,-15.5584068472976,
12.));
#184233=CARTESIAN_POINT('Ctrl Pts',(17.8264971124606,-15.5417380389639,
12.));
#184234=CARTESIAN_POINT('Ctrl Pts',(17.8163700461263,-15.5251939029558,
12.));
#184235=CARTESIAN_POINT('Ctrl Pts',(17.8062576997964,-15.5087750074728,
12.));
#184236=CARTESIAN_POINT('Ctrl Pts',(17.7961609903161,-15.4924819268529,
12.));
#184237=CARTESIAN_POINT('Ctrl Pts',(17.7860808481229,-15.4763152417506,
12.));
#184238=CARTESIAN_POINT('Ctrl Pts',(17.7760182175817,-15.4602755393019,
12.));
#184239=CARTESIAN_POINT('Ctrl Pts',(17.765974057326,-15.4443634132865,12.));
#184240=CARTESIAN_POINT('Ctrl Pts',(17.7559493405871,-15.4285794642658,
12.));
#184241=CARTESIAN_POINT('Ctrl Pts',(17.7459450555803,-15.4129242997828,
12.));
#184242=CARTESIAN_POINT('Ctrl Pts',(17.7359622059143,-15.3973985345796,
12.));
#184243=CARTESIAN_POINT('Ctrl Pts',(17.7260018109923,-15.3820027907965,
12.));
#184244=CARTESIAN_POINT('Ctrl Pts',(17.7160649064208,-15.3667376981702,
12.));
#184245=CARTESIAN_POINT('Ctrl Pts',(17.7061525444044,-15.3516038942064,
12.));
#184246=CARTESIAN_POINT('Ctrl Pts',(17.6962657941984,-15.3366020244069,
12.));
#184247=CARTESIAN_POINT('Ctrl Pts',(17.6864057426052,-15.3217327425341,
12.));
#184248=CARTESIAN_POINT('Ctrl Pts',(17.6765734944559,-15.3069967108501,
12.));
#184249=CARTESIAN_POINT('Ctrl Pts',(17.6667701731041,-15.2923946003598,
12.));
#184250=CARTESIAN_POINT('Ctrl Pts',(17.6569969209,-15.2779270910238,12.));
#184251=CARTESIAN_POINT('Ctrl Pts',(17.6472548997329,-15.263594872029,12.));
#184252=CARTESIAN_POINT('Ctrl Pts',(17.637545291637,-15.2493986421091,12.));
#184253=CARTESIAN_POINT('Ctrl Pts',(17.6278692993765,-15.2353391098367,
12.));
#184254=CARTESIAN_POINT('Ctrl Pts',(17.6182281470467,-15.22141699392,12.));
#184255=CARTESIAN_POINT('Ctrl Pts',(17.6086230806497,-15.2076330234686,
12.));
#184256=CARTESIAN_POINT('Ctrl Pts',(17.5990553687595,-15.1939879383268,
12.));
#184257=CARTESIAN_POINT('Ctrl Pts',(17.5895263032592,-15.1804824894605,
12.));
#184258=CARTESIAN_POINT('Ctrl Pts',(17.5800372000539,-15.1671174393136,
12.));
#184259=CARTESIAN_POINT('Ctrl Pts',(17.570589399803,-15.1538935621715,12.));
#184260=CARTESIAN_POINT('Ctrl Pts',(17.5611842686196,-15.1408116444877,
12.));
#184261=CARTESIAN_POINT('Ctrl Pts',(17.5518231989122,-15.127872485314,12.));
#184262=CARTESIAN_POINT('Ctrl Pts',(17.5425076102966,-15.1150768967729,
12.));
#184263=CARTESIAN_POINT('Ctrl Pts',(17.5332389504829,-15.1024257045033,
12.));
#184264=CARTESIAN_POINT('Ctrl Pts',(17.5240186961788,-15.0899197481082,
12.));
#184265=CARTESIAN_POINT('Ctrl Pts',(17.5148483539683,-15.0775598815748,
12.));
#184266=CARTESIAN_POINT('Ctrl Pts',(17.5057294613874,-15.0653469738306,
12.));
#184267=CARTESIAN_POINT('Ctrl Pts',(17.4966635880245,-15.0532819093085,
12.));
#184268=CARTESIAN_POINT('Ctrl Pts',(17.4876523366178,-15.0413655884993,
12.));
#184269=CARTESIAN_POINT('Ctrl Pts',(17.4786973441417,-15.029598928488,12.));
#184270=CARTESIAN_POINT('Ctrl Pts',(17.4698002829357,-15.0179828635086,
12.));
#184271=CARTESIAN_POINT('Ctrl Pts',(17.4609628621418,-15.0065183456921,
12.));
#184272=CARTESIAN_POINT('Ctrl Pts',(17.4521868291004,-14.9952063457778,
12.));
#184273=CARTESIAN_POINT('Ctrl Pts',(17.4434739707773,-14.9840478538358,
12.));
#184274=CARTESIAN_POINT('Ctrl Pts',(17.4348261151396,-14.9730438799452,
12.));
#184275=CARTESIAN_POINT('Ctrl Pts',(17.426245132709,-14.9621954549827,12.));
#184276=CARTESIAN_POINT('Ctrl Pts',(17.4177329382828,-14.9515036315143,
12.));
#184277=CARTESIAN_POINT('Ctrl Pts',(17.4092914926071,-14.940969484645,12.));
#184278=CARTESIAN_POINT('Ctrl Pts',(17.4009228040749,-14.9305941128757,
12.));
#184279=CARTESIAN_POINT('Ctrl Pts',(17.3926289303986,-14.9203786389342,
12.));
#184280=CARTESIAN_POINT('Ctrl Pts',(17.3844119809824,-14.9103242110057,
12.));
#184281=CARTESIAN_POINT('Ctrl Pts',(17.3762741193076,-14.900432003961,12.));
#184282=CARTESIAN_POINT('Ctrl Pts',(17.3682175653235,-14.8907032205788,
12.));
#184283=CARTESIAN_POINT('Ctrl Pts',(17.3602445978161,-14.8811390927423,
12.));
#184284=CARTESIAN_POINT('Ctrl Pts',(17.3523575568645,-14.8717408826956,
12.));
#184285=CARTESIAN_POINT('Ctrl Pts',(17.3445588463474,-14.8625098843417,
12.));
#184286=CARTESIAN_POINT('Ctrl Pts',(17.336850936485,-14.8534474245434,12.));
#184287=CARTESIAN_POINT('Ctrl Pts',(17.3292363662605,-14.8445548643508,
12.));
#184288=CARTESIAN_POINT('Ctrl Pts',(17.3217177462101,-14.8358336004197,
12.));
#184289=CARTESIAN_POINT('Ctrl Pts',(17.3142977632659,-14.8272850675379,
12.));
#184290=CARTESIAN_POINT('Ctrl Pts',(17.3069791853706,-14.8189107410162,
12.));
#184291=CARTESIAN_POINT('Ctrl Pts',(17.299764866148,-14.8107121391035,12.));
#184292=CARTESIAN_POINT('Ctrl Pts',(17.2926577496513,-14.8026908254276,
12.));
#184293=CARTESIAN_POINT('Ctrl Pts',(17.2856608733196,-14.7948484105249,
12.));
#184294=CARTESIAN_POINT('Ctrl Pts',(17.2787773704849,-14.787186553128,12.));
#184295=CARTESIAN_POINT('Ctrl Pts',(17.2720104735194,-14.7797069617804,
12.));
#184296=CARTESIAN_POINT('Ctrl Pts',(17.2653635155319,-14.7724113956731,
12.));
#184297=CARTESIAN_POINT('Ctrl Pts',(17.2588399401465,-14.7653016697591,
12.));
#184298=CARTESIAN_POINT('Ctrl Pts',(17.2524433146837,-14.7583796616617,
12.));
#184299=CARTESIAN_POINT('Ctrl Pts',(17.2461773413288,-14.7516473175124,
12.));
#184300=CARTESIAN_POINT('Ctrl Pts',(17.2400458713565,-14.7451066593792,
12.));
#184301=CARTESIAN_POINT('Ctrl Pts',(17.2340529062076,-14.7387597858117,
12.));
#184302=CARTESIAN_POINT('Ctrl Pts',(17.2282025904314,-14.7326088681163,
12.));
#184303=CARTESIAN_POINT('Ctrl Pts',(17.2224992099667,-14.7266561494282,
12.));
#184304=CARTESIAN_POINT('Ctrl Pts',(17.2169471814256,-14.7209039390327,
12.));
#184305=CARTESIAN_POINT('Ctrl Pts',(17.2115510835989,-14.7153546289339,
12.));
#184306=CARTESIAN_POINT('Ctrl Pts',(17.2063157097315,-14.7100107213586,
12.));
#184307=CARTESIAN_POINT('Ctrl Pts',(17.2012461084268,-14.7048748502663,
12.));
#184308=CARTESIAN_POINT('Ctrl Pts',(17.1963476411694,-14.699949811582,12.));
#184309=CARTESIAN_POINT('Ctrl Pts',(17.1916259308415,-14.6952385361706,
12.));
#184310=CARTESIAN_POINT('Ctrl Pts',(17.1870867909918,-14.6907440526958,
12.));
#184311=CARTESIAN_POINT('Ctrl Pts',(17.182736158472,-14.686469452232,12.));
#184312=CARTESIAN_POINT('Ctrl Pts',(17.1785800350826,-14.6824178576167,
12.));
#184313=CARTESIAN_POINT('Ctrl Pts',(17.1746247499057,-14.6785925615677,
12.));
#184314=CARTESIAN_POINT('Ctrl Pts',(17.1708771619129,-14.6749971333867,
12.));
#184315=CARTESIAN_POINT('Ctrl Pts',(17.167344972302,-14.671635583332,12.));
#184316=CARTESIAN_POINT('Ctrl Pts',(17.1640366762305,-14.6685123374423,
12.));
#184317=CARTESIAN_POINT('Ctrl Pts',(17.1609609517369,-14.6656319165057,
12.));
#184318=CARTESIAN_POINT('Ctrl Pts',(17.1581262646789,-14.6629987285992,
12.));
#184319=CARTESIAN_POINT('Ctrl Pts',(17.1555401986401,-14.6606167169642,
12.));
#184320=CARTESIAN_POINT('Ctrl Pts',(17.1532107762718,-14.6584900555302,
12.));
#184321=CARTESIAN_POINT('Ctrl Pts',(17.1511476869496,-14.6566237952435,
12.));
#184322=CARTESIAN_POINT('Ctrl Pts',(17.1493641837558,-14.655024862281,12.));
#184323=CARTESIAN_POINT('Ctrl Pts',(17.147876394491,-14.6537016966184,12.));
#184324=CARTESIAN_POINT('Ctrl Pts',(17.1466998098673,-14.6526624064978,
12.));
#184325=CARTESIAN_POINT('Ctrl Pts',(17.1458462295271,-14.6519131634508,
12.));
#184326=CARTESIAN_POINT('Ctrl Pts',(17.1454262858043,-14.6515481598068,
12.));
#184327=CARTESIAN_POINT('Ctrl Pts',(17.1452600887037,-14.6514066997196,
12.));
#184328=CARTESIAN_POINT('Ctrl Pts',(17.1452153999142,-14.6513711852843,
12.));
#184329=CARTESIAN_POINT('Ctrl Pts',(17.1452095830632,-14.6513681262571,
12.));
#184330=CARTESIAN_POINT('',(16.7207683102834,-14.2886635873976,12.));
#184331=CARTESIAN_POINT('',(8.17248635976757,-6.98376450772884,12.));
#184332=CARTESIAN_POINT('',(16.6581946899465,-13.5924445804218,12.));
#184333=CARTESIAN_POINT('Origin',(17.0455945664569,-13.9085479427572,12.));
#184334=CARTESIAN_POINT('',(17.4407513054162,-12.572596943457,12.));
#184335=CARTESIAN_POINT('Origin',(6.00167842331873E-13,-4.9889687874677E-13,
12.));
#184336=CARTESIAN_POINT('',(18.1294424696716,-12.4528436808172,12.));
#184337=CARTESIAN_POINT('Origin',(17.846350172984,-12.8649829188862,12.));
#184338=CARTESIAN_POINT('',(18.5896416359912,-12.7689476255363,12.));
#184339=CARTESIAN_POINT('',(9.29482081799561,-6.38447381276812,12.));
#184340=CARTESIAN_POINT('',(22.1787195904339,-13.5685075571671,12.));
#184341=CARTESIAN_POINT('Ctrl Pts',(18.5896416359912,-12.7689476255363,
12.));
#184342=CARTESIAN_POINT('Ctrl Pts',(18.5896460962961,-12.7689524524484,
12.));
#184343=CARTESIAN_POINT('Ctrl Pts',(18.5896919669158,-12.7689864266924,
12.));
#184344=CARTESIAN_POINT('Ctrl Pts',(18.589871621842,-12.7691103481996,12.));
#184345=CARTESIAN_POINT('Ctrl Pts',(18.590332877722,-12.7694215127923,12.));
#184346=CARTESIAN_POINT('Ctrl Pts',(18.5912775137806,-12.7700520897174,
12.));
#184347=CARTESIAN_POINT('Ctrl Pts',(18.5925859134582,-12.7709195951153,
12.));
#184348=CARTESIAN_POINT('Ctrl Pts',(18.5942490615409,-12.7720142287169,
12.));
#184349=CARTESIAN_POINT('Ctrl Pts',(18.5962551167772,-12.7733231262107,
12.));
#184350=CARTESIAN_POINT('Ctrl Pts',(18.5985917525949,-12.7748328937639,
12.));
#184351=CARTESIAN_POINT('Ctrl Pts',(18.6012488486708,-12.7765325225082,
12.));
#184352=CARTESIAN_POINT('Ctrl Pts',(18.6042190183703,-12.7784139605067,
12.));
#184353=CARTESIAN_POINT('Ctrl Pts',(18.6074961535723,-12.7804705387658,
12.));
#184354=CARTESIAN_POINT('Ctrl Pts',(18.611074482622,-12.7826959526924,12.));
#184355=CARTESIAN_POINT('Ctrl Pts',(18.6149475565189,-12.78508316579,12.));
#184356=CARTESIAN_POINT('Ctrl Pts',(18.6191087624752,-12.7876249657834,
12.));
#184357=CARTESIAN_POINT('Ctrl Pts',(18.6235516265575,-12.7903142925234,
12.));
#184358=CARTESIAN_POINT('Ctrl Pts',(18.6282702819371,-12.7931447451556,
12.));
#184359=CARTESIAN_POINT('Ctrl Pts',(18.6332595057005,-12.7961106222251,
12.));
#184360=CARTESIAN_POINT('Ctrl Pts',(18.63851447924,-12.7992066625264,12.));
#184361=CARTESIAN_POINT('Ctrl Pts',(18.6440306327457,-12.8024278770153,
12.));
#184362=CARTESIAN_POINT('Ctrl Pts',(18.6498034438986,-12.805769331162,12.));
#184363=CARTESIAN_POINT('Ctrl Pts',(18.6558284825772,-12.8092261933858,
12.));
#184364=CARTESIAN_POINT('Ctrl Pts',(18.6621014624746,-12.8127937909632,
12.));
#184365=CARTESIAN_POINT('Ctrl Pts',(18.6686182952798,-12.8164676687361,
12.));
#184366=CARTESIAN_POINT('Ctrl Pts',(18.6753751301091,-12.8202436318473,
12.));
#184367=CARTESIAN_POINT('Ctrl Pts',(18.6823683094139,-12.8241176980016,
12.));
#184368=CARTESIAN_POINT('Ctrl Pts',(18.6895943376172,-12.8280860635231,
12.));
#184369=CARTESIAN_POINT('Ctrl Pts',(18.6970498410173,-12.832145059979,12.));
#184370=CARTESIAN_POINT('Ctrl Pts',(18.7047315436296,-12.8362911280362,
12.));
#184371=CARTESIAN_POINT('Ctrl Pts',(18.7126362754446,-12.8405208263432,
12.));
#184372=CARTESIAN_POINT('Ctrl Pts',(18.7207609737701,-12.8448308329494,
12.));
#184373=CARTESIAN_POINT('Ctrl Pts',(18.7291026886552,-12.849217951159,12.));
#184374=CARTESIAN_POINT('Ctrl Pts',(18.7376585820851,-12.8536791086315,
12.));
#184375=CARTESIAN_POINT('Ctrl Pts',(18.7464259171248,-12.8582113455644,
12.));
#184376=CARTESIAN_POINT('Ctrl Pts',(18.7554020493888,-12.8628118054172,
12.));
#184377=CARTESIAN_POINT('Ctrl Pts',(18.7645844169568,-12.8674777239656,
12.));
#184378=CARTESIAN_POINT('Ctrl Pts',(18.7739705329028,-12.8722064211814,
12.));
#184379=CARTESIAN_POINT('Ctrl Pts',(18.7835579840481,-12.8769952998097,
12.));
#184380=CARTESIAN_POINT('Ctrl Pts',(18.7933444285867,-12.8818418427474,
12.));
#184381=CARTESIAN_POINT('Ctrl Pts',(18.8033275941939,-12.8867436109543,
12.));
#184382=CARTESIAN_POINT('Ctrl Pts',(18.8135052757815,-12.8916982409931,
12.));
#184383=CARTESIAN_POINT('Ctrl Pts',(18.8238753319124,-12.8967034410752,
12.));
#184384=CARTESIAN_POINT('Ctrl Pts',(18.834435681259,-12.9017569871738,12.));
#184385=CARTESIAN_POINT('Ctrl Pts',(18.8451842990986,-12.9068567191856,
12.));
#184386=CARTESIAN_POINT('Ctrl Pts',(18.8561192136201,-12.9120005369066,
12.));
#184387=CARTESIAN_POINT('Ctrl Pts',(18.8672385038328,-12.9171863977047,
12.));
#184388=CARTESIAN_POINT('Ctrl Pts',(18.8785402977528,-12.9224123144982,
12.));
#184389=CARTESIAN_POINT('Ctrl Pts',(18.8900227704888,-12.9276763536372,
12.));
#184390=CARTESIAN_POINT('Ctrl Pts',(18.9016841423402,-12.9329766328184,
12.));
#184391=CARTESIAN_POINT('Ctrl Pts',(18.9135226769466,-12.9383113190375,
12.));
#184392=CARTESIAN_POINT('Ctrl Pts',(18.9255366795196,-12.9436786266106,
12.));
#184393=CARTESIAN_POINT('Ctrl Pts',(18.9377244950435,-12.9490768151821,
12.));
#184394=CARTESIAN_POINT('Ctrl Pts',(18.9500845064714,-12.9545041877377,
12.));
#184395=CARTESIAN_POINT('Ctrl Pts',(18.9626151329226,-12.9599590886318,
12.));
#184396=CARTESIAN_POINT('Ctrl Pts',(18.9753148284473,-12.9654399021868,
12.));
#184397=CARTESIAN_POINT('Ctrl Pts',(18.9881820807585,-12.9709450512747,
12.));
#184398=CARTESIAN_POINT('Ctrl Pts',(19.0012154099792,-12.9764729959206,
12.));
#184399=CARTESIAN_POINT('Ctrl Pts',(19.014413367335,-12.9820222318716,12.));
#184400=CARTESIAN_POINT('Ctrl Pts',(19.0277745339908,-12.9875912893003,
12.));
#184401=CARTESIAN_POINT('Ctrl Pts',(19.0412975200398,-12.9931787316514,
12.));
#184402=CARTESIAN_POINT('Ctrl Pts',(19.0549809634354,-12.9987831544502,
12.));
#184403=CARTESIAN_POINT('Ctrl Pts',(19.0688235289437,-13.0044031841382,
12.));
#184404=CARTESIAN_POINT('Ctrl Pts',(19.0828239070484,-13.0100374768788,
12.));
#184405=CARTESIAN_POINT('Ctrl Pts',(19.0969808131228,-13.0156847176097,
12.));
#184406=CARTESIAN_POINT('Ctrl Pts',(19.111292986631,-13.0213436191328,12.));
#184407=CARTESIAN_POINT('Ctrl Pts',(19.1257591903099,-13.0270129211976,
12.));
#184408=CARTESIAN_POINT('Ctrl Pts',(19.1403782093386,-13.0326913895838,
12.));
#184409=CARTESIAN_POINT('Ctrl Pts',(19.155148850523,-13.0383778152068,12.));
#184410=CARTESIAN_POINT('Ctrl Pts',(19.1700699416622,-13.0440710133772,
12.));
#184411=CARTESIAN_POINT('Ctrl Pts',(19.1851403308825,-13.0497698230441,
12.));
#184412=CARTESIAN_POINT('Ctrl Pts',(19.2003588859772,-13.0554731060538,
12.));
#184413=CARTESIAN_POINT('Ctrl Pts',(19.2157244937142,-13.0611797463915,
12.));
#184414=CARTESIAN_POINT('Ctrl Pts',(19.2312360592033,-13.0668886494795,
12.));
#184415=CARTESIAN_POINT('Ctrl Pts',(19.2468925053989,-13.0725987415859,
12.));
#184416=CARTESIAN_POINT('Ctrl Pts',(19.2626927725596,-13.0783089692118,
12.));
#184417=CARTESIAN_POINT('Ctrl Pts',(19.2786358177198,-13.0840182984949,
12.));
#184418=CARTESIAN_POINT('Ctrl Pts',(19.2947206141247,-13.0897257145969,
12.));
#184419=CARTESIAN_POINT('Ctrl Pts',(19.310946150736,-13.0954302211479,12.));
#184420=CARTESIAN_POINT('Ctrl Pts',(19.3273114318269,-13.1011308397591,
12.));
#184421=CARTESIAN_POINT('Ctrl Pts',(19.3438154765395,-13.1068266095186,
12.));
#184422=CARTESIAN_POINT('Ctrl Pts',(19.3604573184515,-13.1125165865022,
12.));
#184423=CARTESIAN_POINT('Ctrl Pts',(19.3772360051091,-13.118199843271,12.));
#184424=CARTESIAN_POINT('Ctrl Pts',(19.3941505976263,-13.1238754684177,
12.));
#184425=CARTESIAN_POINT('Ctrl Pts',(19.4112001703557,-13.1295425661634,
12.));
#184426=CARTESIAN_POINT('Ctrl Pts',(19.4283838105262,-13.1352002559438,
12.));
#184427=CARTESIAN_POINT('Ctrl Pts',(19.4457006178876,-13.1408476720061,
12.));
#184428=CARTESIAN_POINT('Ctrl Pts',(19.4631497043258,-13.1464839629971,
12.));
#184429=CARTESIAN_POINT('Ctrl Pts',(19.4807301935268,-13.1521082915853,
12.));
#184430=CARTESIAN_POINT('Ctrl Pts',(19.4984412207082,-13.1577198341245,
12.));
#184431=CARTESIAN_POINT('Ctrl Pts',(19.5162819323213,-13.1633177803101,
12.));
#184432=CARTESIAN_POINT('Ctrl Pts',(19.5342514857562,-13.168901332843,12.));
#184433=CARTESIAN_POINT('Ctrl Pts',(19.5523490490244,-13.1744697070911,
12.));
#184434=CARTESIAN_POINT('Ctrl Pts',(19.5705738004667,-13.1800221307673,
12.));
#184435=CARTESIAN_POINT('Ctrl Pts',(19.5889249285338,-13.1855578436471,
12.));
#184436=CARTESIAN_POINT('Ctrl Pts',(19.6074016315414,-13.1910760972814,
12.));
#184437=CARTESIAN_POINT('Ctrl Pts',(19.6260031174244,-13.1965761547151,
12.));
#184438=CARTESIAN_POINT('Ctrl Pts',(19.6447286034772,-13.2020572902065,
12.));
#184439=CARTESIAN_POINT('Ctrl Pts',(19.6635773160936,-13.2075187889529,
12.));
#184440=CARTESIAN_POINT('Ctrl Pts',(19.6825484905823,-13.2129599468485,
12.));
#184441=CARTESIAN_POINT('Ctrl Pts',(19.7016413709685,-13.2183800702436,
12.));
#184442=CARTESIAN_POINT('Ctrl Pts',(19.7208552097868,-13.2237784757065,
12.));
#184443=CARTESIAN_POINT('Ctrl Pts',(19.7401892678697,-13.2291544897899,
12.));
#184444=CARTESIAN_POINT('Ctrl Pts',(19.7596428141168,-13.2345074487963,
12.));
#184445=CARTESIAN_POINT('Ctrl Pts',(19.7792151253289,-13.2398366985675,
12.));
#184446=CARTESIAN_POINT('Ctrl Pts',(19.7989054860495,-13.2451415942805,
12.));
#184447=CARTESIAN_POINT('Ctrl Pts',(19.8187131883917,-13.2504215002457,
12.));
#184448=CARTESIAN_POINT('Ctrl Pts',(19.8386375318634,-13.2556757897086,
12.));
#184449=CARTESIAN_POINT('Ctrl Pts',(19.8586778231715,-13.2609038446529,
12.));
#184450=CARTESIAN_POINT('Ctrl Pts',(19.8788333760577,-13.2661050556132,
12.));
#184451=CARTESIAN_POINT('Ctrl Pts',(19.8991035111745,-13.271278821502,12.));
#184452=CARTESIAN_POINT('Ctrl Pts',(19.9194875559422,-13.2764245494357,
12.));
#184453=CARTESIAN_POINT('Ctrl Pts',(19.9399848444019,-13.2815416545663,
12.));
#184454=CARTESIAN_POINT('Ctrl Pts',(19.9605947170586,-13.286629559915,12.));
#184455=CARTESIAN_POINT('Ctrl Pts',(19.981316520717,-13.2916876962094,12.));
#184456=CARTESIAN_POINT('Ctrl Pts',(20.0021496083738,-13.2967155017306,
12.));
#184457=CARTESIAN_POINT('Ctrl Pts',(20.0230933391038,-13.3017124221637,
12.));
#184458=CARTESIAN_POINT('Ctrl Pts',(20.0441470779345,-13.3066779104515,
12.));
#184459=CARTESIAN_POINT('Ctrl Pts',(20.0653101957188,-13.3116114266515,
12.));
#184460=CARTESIAN_POINT('Ctrl Pts',(20.0865820689882,-13.3165124377963,
12.));
#184461=CARTESIAN_POINT('Ctrl Pts',(20.1079620798375,-13.3213804177587,
12.));
#184462=CARTESIAN_POINT('Ctrl Pts',(20.1294496158402,-13.3262148471226,
12.));
#184463=CARTESIAN_POINT('Ctrl Pts',(20.1510440699474,-13.3310152130564,
12.));
#184464=CARTESIAN_POINT('Ctrl Pts',(20.1727448403817,-13.3357810091903,
12.));
#184465=CARTESIAN_POINT('Ctrl Pts',(20.1945513305235,-13.3405117354971,
12.));
#184466=CARTESIAN_POINT('Ctrl Pts',(20.216462948786,-13.3452068981766,12.));
#184467=CARTESIAN_POINT('Ctrl Pts',(20.2384791085359,-13.3498660095386,
12.));
#184468=CARTESIAN_POINT('Ctrl Pts',(20.2605992280122,-13.3544885878889,
12.));
#184469=CARTESIAN_POINT('Ctrl Pts',(20.2828227302339,-13.3590741574195,
12.));
#184470=CARTESIAN_POINT('Ctrl Pts',(20.3051490429048,-13.3636222481016,
12.));
#184471=CARTESIAN_POINT('Ctrl Pts',(20.3275775983029,-13.3681323955826,
12.));
#184472=CARTESIAN_POINT('Ctrl Pts',(20.3501078331814,-13.3726041410867,
12.));
#184473=CARTESIAN_POINT('Ctrl Pts',(20.3727391887184,-13.3770370313188,
12.));
#184474=CARTESIAN_POINT('Ctrl Pts',(20.3954711104502,-13.3814306183719,
12.));
#184475=CARTESIAN_POINT('Ctrl Pts',(20.4183030482002,-13.3857844596387,
12.));
#184476=CARTESIAN_POINT('Ctrl Pts',(20.4412344560008,-13.3900981177255,
12.));
#184477=CARTESIAN_POINT('Ctrl Pts',(20.4642647920038,-13.3943711603739,
12.));
#184478=CARTESIAN_POINT('Ctrl Pts',(20.487393518404,-13.3986031603716,12.));
#184479=CARTESIAN_POINT('Ctrl Pts',(20.5106201013753,-13.4027936954529,
12.));
#184480=CARTESIAN_POINT('Ctrl Pts',(20.5339440109956,-13.4069423482076,
12.));
#184481=CARTESIAN_POINT('Ctrl Pts',(20.5573647211639,-13.4110487059912,
12.));
#184482=CARTESIAN_POINT('Ctrl Pts',(20.5808817095155,-13.4151123608411,
12.));
#184483=CARTESIAN_POINT('Ctrl Pts',(20.6044944573153,-13.4191329093933,
12.));
#184484=CARTESIAN_POINT('Ctrl Pts',(20.6282024494237,-13.4231099528179,
12.));
#184485=CARTESIAN_POINT('Ctrl Pts',(20.6520051742869,-13.4270430967651,
12.));
#184486=CARTESIAN_POINT('Ctrl Pts',(20.6759021239103,-13.4309319513119,
12.));
#184487=CARTESIAN_POINT('Ctrl Pts',(20.6998927938288,-13.4347761309154,
12.));
#184488=CARTESIAN_POINT('Ctrl Pts',(20.7239766830675,-13.4385752543663,
12.));
#184489=CARTESIAN_POINT('Ctrl Pts',(20.7481532941013,-13.4423289447561,
12.));
#184490=CARTESIAN_POINT('Ctrl Pts',(20.7724221327608,-13.4460368293688,
12.));
#184491=CARTESIAN_POINT('Ctrl Pts',(20.7967827081227,-13.4496985395637,
12.));
#184492=CARTESIAN_POINT('Ctrl Pts',(20.821234532398,-13.4533137106667,12.));
#184493=CARTESIAN_POINT('Ctrl Pts',(20.8457771208082,-13.4568819818631,
12.));
#184494=CARTESIAN_POINT('Ctrl Pts',(20.8704099914641,-13.4604029960983,
12.));
#184495=CARTESIAN_POINT('Ctrl Pts',(20.8951326652158,-13.4638763999725,
12.));
#184496=CARTESIAN_POINT('Ctrl Pts',(20.9199446657584,-13.4673018437718,
12.));
#184497=CARTESIAN_POINT('Ctrl Pts',(20.9448455197557,-13.4706789815166,
12.));
#184498=CARTESIAN_POINT('Ctrl Pts',(20.9698347569476,-13.4740074710087,
12.));
#184499=CARTESIAN_POINT('Ctrl Pts',(20.9949119102592,-13.4772869738879,
12.));
#184500=CARTESIAN_POINT('Ctrl Pts',(21.0200765158885,-13.4805171556822,
12.));
#184501=CARTESIAN_POINT('Ctrl Pts',(21.0453281134247,-13.4836976858912,
12.));
#184502=CARTESIAN_POINT('Ctrl Pts',(21.0706662455202,-13.4868282377192,
12.));
#184503=CARTESIAN_POINT('Ctrl Pts',(21.0960904575048,-13.4899084877718,
12.));
#184504=CARTESIAN_POINT('Ctrl Pts',(21.1216002970209,-13.4929381157778,
12.));
#184505=CARTESIAN_POINT('Ctrl Pts',(21.1471953136209,-13.4959168042934,
12.));
#184506=CARTESIAN_POINT('Ctrl Pts',(21.1728750584173,-13.4988442384491,
12.));
#184507=CARTESIAN_POINT('Ctrl Pts',(21.1986390835825,-13.5017201056088,
12.));
#184508=CARTESIAN_POINT('Ctrl Pts',(21.224486942933,-13.5045440957404,12.));
#184509=CARTESIAN_POINT('Ctrl Pts',(21.2504181927429,-13.5073159019454,
12.));
#184510=CARTESIAN_POINT('Ctrl Pts',(21.2764323924442,-13.5100352209207,
12.));
#184511=CARTESIAN_POINT('Ctrl Pts',(21.3025291054236,-13.5127017534972,
12.));
#184512=CARTESIAN_POINT('Ctrl Pts',(21.328707899634,-13.5153152050554,12.));
#184513=CARTESIAN_POINT('Ctrl Pts',(21.3549683486219,-13.5178752862461,
12.));
#184514=CARTESIAN_POINT('Ctrl Pts',(21.3813100304967,-13.5203817122497,
12.));
#184515=CARTESIAN_POINT('Ctrl Pts',(21.4077325259318,-13.5228342013508,
12.));
#184516=CARTESIAN_POINT('Ctrl Pts',(21.4342354165254,-13.5252324737795,
12.));
#184517=CARTESIAN_POINT('Ctrl Pts',(21.4608182828695,-13.5275762503553,
12.));
#184518=CARTESIAN_POINT('Ctrl Pts',(21.487480703047,-13.5298652514357,12.));
#184519=CARTESIAN_POINT('Ctrl Pts',(21.5142222501671,-13.5320991952145,
12.));
#184520=CARTESIAN_POINT('Ctrl Pts',(21.5410424932511,-13.5342777983225,
12.));
#184521=CARTESIAN_POINT('Ctrl Pts',(21.5679410019011,-13.5364007790292,
12.));
#184522=CARTESIAN_POINT('Ctrl Pts',(21.5949173499022,-13.5384678597206,
12.));
#184523=CARTESIAN_POINT('Ctrl Pts',(21.6219711193951,-13.5404787697798,
12.));
#184524=CARTESIAN_POINT('Ctrl Pts',(21.6491019044647,-13.5424332480698,
12.));
#184525=CARTESIAN_POINT('Ctrl Pts',(21.676309315769,-13.5443310461516,12.));
#184526=CARTESIAN_POINT('Ctrl Pts',(21.7035929822939,-13.546171929503,12.));
#184527=CARTESIAN_POINT('Ctrl Pts',(21.730952541226,-13.5479556704457,12.));
#184528=CARTESIAN_POINT('Ctrl Pts',(21.7583876294532,-13.5496820422186,
12.));
#184529=CARTESIAN_POINT('Ctrl Pts',(21.7858978745848,-13.5513508127232,
12.));
#184530=CARTESIAN_POINT('Ctrl Pts',(21.8134828857963,-13.5529617381569,
12.));
#184531=CARTESIAN_POINT('Ctrl Pts',(21.841142245609,-13.5545145573048,12.));
#184532=CARTESIAN_POINT('Ctrl Pts',(21.8688754989401,-13.5560089839426,
12.));
#184533=CARTESIAN_POINT('Ctrl Pts',(21.8966821688876,-13.5574447178485,
12.));
#184534=CARTESIAN_POINT('Ctrl Pts',(21.9245617765827,-13.5588214586672,
12.));
#184535=CARTESIAN_POINT('Ctrl Pts',(21.9525138592862,-13.5601389185315,
12.));
#184536=CARTESIAN_POINT('Ctrl Pts',(21.9805379899192,-13.5613968357589,
12.));
#184537=CARTESIAN_POINT('Ctrl Pts',(22.0086337943431,-13.5625949868313,
12.));
#184538=CARTESIAN_POINT('Ctrl Pts',(22.0368009736227,-13.5637332022393,
12.));
#184539=CARTESIAN_POINT('Ctrl Pts',(22.0650393089492,-13.5648113688895,
12.));
#184540=CARTESIAN_POINT('Ctrl Pts',(22.0933486464442,-13.5658294169106,
12.));
#184541=CARTESIAN_POINT('Ctrl Pts',(22.1217288871823,-13.5667873105179,
12.));
#184542=CARTESIAN_POINT('Ctrl Pts',(22.1444897575076,-13.5675054918922,
12.));
#184543=CARTESIAN_POINT('Ctrl Pts',(22.1615922804939,-13.5680170531724,
12.));
#184544=CARTESIAN_POINT('Ctrl Pts',(22.1730081264583,-13.5683460612913,
12.));
#184545=CARTESIAN_POINT('Ctrl Pts',(22.1787195904339,-13.5685075571671,
12.));
#184546=CARTESIAN_POINT('',(22.8400320311648,-12.4230808101438,12.));
#184547=CARTESIAN_POINT('Origin',(0.,0.,12.));
#184548=CARTESIAN_POINT('',(20.353053841303,-9.71462809124917,12.));
#184549=CARTESIAN_POINT('Ctrl Pts',(22.8400320311648,-12.4230808101438,
12.));
#184550=CARTESIAN_POINT('Ctrl Pts',(22.8370364396497,-12.4182152851867,
12.));
#184551=CARTESIAN_POINT('Ctrl Pts',(22.8310435872852,-12.4084933766366,
12.));
#184552=CARTESIAN_POINT('Ctrl Pts',(22.8220493007353,-12.393937937903,12.));
#184553=CARTESIAN_POINT('Ctrl Pts',(22.8100469022632,-12.3745855366772,
12.));
#184554=CARTESIAN_POINT('Ctrl Pts',(22.7950272216959,-12.3504864740361,
12.));
#184555=CARTESIAN_POINT('Ctrl Pts',(22.7799908974947,-12.3264788926108,
12.));
#184556=CARTESIAN_POINT('Ctrl Pts',(22.7649380101154,-12.3025628601812,
12.));
#184557=CARTESIAN_POINT('Ctrl Pts',(22.7498686970096,-12.2787384750747,
12.));
#184558=CARTESIAN_POINT('Ctrl Pts',(22.7347831655251,-12.2550058702389,
12.));
#184559=CARTESIAN_POINT('Ctrl Pts',(22.7196817119299,-12.2313652198047,
12.));
#184560=CARTESIAN_POINT('Ctrl Pts',(22.7045647168659,-12.2078167360267,
12.));
#184561=CARTESIAN_POINT('Ctrl Pts',(22.6894326204959,-12.1843606579246,
12.));
#184562=CARTESIAN_POINT('Ctrl Pts',(22.6742859034891,-12.1609972423089,
12.));
#184563=CARTESIAN_POINT('Ctrl Pts',(22.6591250653942,-12.1377267537141,
12.));
#184564=CARTESIAN_POINT('Ctrl Pts',(22.6439506046611,-12.1145494550384,
12.));
#184565=CARTESIAN_POINT('Ctrl Pts',(22.628762996708,-12.0914655972828,12.));
#184566=CARTESIAN_POINT('Ctrl Pts',(22.613562676493,-12.0684754113869,12.));
#184567=CARTESIAN_POINT('Ctrl Pts',(22.5983500505675,-12.0455791139135,
12.));
#184568=CARTESIAN_POINT('Ctrl Pts',(22.5831255061306,-12.0227769113132,
12.));
#184569=CARTESIAN_POINT('Ctrl Pts',(22.5678894211194,-12.0000690046697,
12.));
#184570=CARTESIAN_POINT('Ctrl Pts',(22.5526421741159,-11.9774555943496,
12.));
#184571=CARTESIAN_POINT('Ctrl Pts',(22.5373841537299,-11.9549368843996,
12.));
#184572=CARTESIAN_POINT('Ctrl Pts',(22.5221157697869,-11.9325130877801,
12.));
#184573=CARTESIAN_POINT('Ctrl Pts',(22.5068374513958,-11.9101844254555,
12.));
#184574=CARTESIAN_POINT('Ctrl Pts',(22.4915496418472,-11.8879511239941,
12.));
#184575=CARTESIAN_POINT('Ctrl Pts',(22.4762527946694,-11.8658134137018,
12.));
#184576=CARTESIAN_POINT('Ctrl Pts',(22.4609473690469,-11.8437715264487,
12.));
#184577=CARTESIAN_POINT('Ctrl Pts',(22.4456338258738,-11.8218256937889,
12.));
#184578=CARTESIAN_POINT('Ctrl Pts',(22.4303126226468,-11.7999761445175,
12.));
#184579=CARTESIAN_POINT('Ctrl Pts',(22.4149842125018,-11.7782231042041,
12.));
#184580=CARTESIAN_POINT('Ctrl Pts',(22.39964904692,-11.7565667964765,12.));
#184581=CARTESIAN_POINT('Ctrl Pts',(22.3843075773905,-11.7350074437961,
12.));
#184582=CARTESIAN_POINT('Ctrl Pts',(22.3689602575492,-11.7135452684532,
12.));
#184583=CARTESIAN_POINT('Ctrl Pts',(22.3536075450028,-11.6921804934056,
12.));
#184584=CARTESIAN_POINT('Ctrl Pts',(22.3382499035618,-11.6709133432986,
12.));
#184585=CARTESIAN_POINT('Ctrl Pts',(22.3228878043976,-11.6497440449858,
12.));
#184586=CARTESIAN_POINT('Ctrl Pts',(22.3075217249049,-11.6286728270011,
12.));
#184587=CARTESIAN_POINT('Ctrl Pts',(22.2921521480357,-11.6076999192359,
12.));
#184588=CARTESIAN_POINT('Ctrl Pts',(22.2767795614349,-11.5868255525189,
12.));
#184589=CARTESIAN_POINT('Ctrl Pts',(22.2614044566898,-11.5660499582403,
12.));
#184590=CARTESIAN_POINT('Ctrl Pts',(22.2460273284653,-11.545373367912,12.));
#184591=CARTESIAN_POINT('Ctrl Pts',(22.2306486738899,-11.5247960128476,
12.));
#184592=CARTESIAN_POINT('Ctrl Pts',(22.215268993102,-11.504318124424,12.));
#184593=CARTESIAN_POINT('Ctrl Pts',(22.1998887896435,-11.4839399342589,
12.));
#184594=CARTESIAN_POINT('Ctrl Pts',(22.1845085709169,-11.463661674411,12.));
#184595=CARTESIAN_POINT('Ctrl Pts',(22.1691288486096,-11.443483577557,12.));
#184596=CARTESIAN_POINT('Ctrl Pts',(22.1537501391486,-11.4234058771742,
12.));
#184597=CARTESIAN_POINT('Ctrl Pts',(22.1383729640963,-11.4034288076909,
12.));
#184598=CARTESIAN_POINT('Ctrl Pts',(22.1229978500185,-11.3835526044256,
12.));
#184599=CARTESIAN_POINT('Ctrl Pts',(22.1076253283978,-11.3637775035367,
12.));
#184600=CARTESIAN_POINT('Ctrl Pts',(22.0922559355293,-11.3441037419553,
12.));
#184601=CARTESIAN_POINT('Ctrl Pts',(22.0768902124267,-11.3245315573168,
12.));
#184602=CARTESIAN_POINT('Ctrl Pts',(22.0615287047179,-11.3050611878771,
12.));
#184603=CARTESIAN_POINT('Ctrl Pts',(22.046171962566,-11.2856928724374,12.));
#184604=CARTESIAN_POINT('Ctrl Pts',(22.0308205408351,-11.2664268504207,
12.));
#184605=CARTESIAN_POINT('Ctrl Pts',(22.0154749992364,-11.2472633619276,
12.));
#184606=CARTESIAN_POINT('Ctrl Pts',(22.0001359024839,-11.2282026477897,
12.));
#184607=CARTESIAN_POINT('Ctrl Pts',(21.9848038204439,-11.2092449496125,
12.));
#184608=CARTESIAN_POINT('Ctrl Pts',(21.9694793282913,-11.190390509811,12.));
#184609=CARTESIAN_POINT('Ctrl Pts',(21.9541630066504,-11.1716395716375,
12.));
#184610=CARTESIAN_POINT('Ctrl Pts',(21.9388554416437,-11.1529923792002,
12.));
#184611=CARTESIAN_POINT('Ctrl Pts',(21.9235572249518,-11.134449177474,12.));
#184612=CARTESIAN_POINT('Ctrl Pts',(21.9082689538687,-11.1160102123024,
12.));
#184613=CARTESIAN_POINT('Ctrl Pts',(21.8929912313608,-11.0976757303944,
12.));
#184614=CARTESIAN_POINT('Ctrl Pts',(21.8777246661191,-11.0794459793058,
12.));
#184615=CARTESIAN_POINT('Ctrl Pts',(21.8624698726319,-11.0613212074364,
12.));
#184616=CARTESIAN_POINT('Ctrl Pts',(21.8472274713103,-11.0433016640808,
12.));
#184617=CARTESIAN_POINT('Ctrl Pts',(21.8319980886033,-11.0253875994598,
12.));
#184618=CARTESIAN_POINT('Ctrl Pts',(21.8167823571168,-11.0075792647477,
12.));
#184619=CARTESIAN_POINT('Ctrl Pts',(21.8015809157302,-10.9898769120913,
12.));
#184620=CARTESIAN_POINT('Ctrl Pts',(21.7863944097143,-10.9722807946157,
12.));
#184621=CARTESIAN_POINT('Ctrl Pts',(21.7712234908468,-10.9547911664457,
12.));
#184622=CARTESIAN_POINT('Ctrl Pts',(21.7560688175252,-10.9374082827446,
12.));
#184623=CARTESIAN_POINT('Ctrl Pts',(21.74093105488,-10.9201323997386,12.));
#184624=CARTESIAN_POINT('Ctrl Pts',(21.7258108748874,-10.9029637747341,
12.));
#184625=CARTESIAN_POINT('Ctrl Pts',(21.7107089564822,-10.8859026661292,
12.));
#184626=CARTESIAN_POINT('Ctrl Pts',(21.6956259856667,-10.8689493334093,
12.));
#184627=CARTESIAN_POINT('Ctrl Pts',(21.6805626556461,-10.8521040371832,
12.));
#184628=CARTESIAN_POINT('Ctrl Pts',(21.6655196669727,-10.835367039227,12.));
#184629=CARTESIAN_POINT('Ctrl Pts',(21.6504977276864,-10.8187386025135,
12.));
#184630=CARTESIAN_POINT('Ctrl Pts',(21.6354975534557,-10.802218991237,12.));
#184631=CARTESIAN_POINT('Ctrl Pts',(21.6205198677176,-10.7858084708262,
12.));
#184632=CARTESIAN_POINT('Ctrl Pts',(21.6055654018179,-10.7695073079554,
12.));
#184633=CARTESIAN_POINT('Ctrl Pts',(21.5906348951745,-10.7533157705943,
12.));
#184634=CARTESIAN_POINT('Ctrl Pts',(21.5757290954372,-10.7372341280468,
12.));
#184635=CARTESIAN_POINT('Ctrl Pts',(21.5608487586467,-10.7212626509816,
12.));
#184636=CARTESIAN_POINT('Ctrl Pts',(21.5459946493955,-10.7054016114571,
12.));
#184637=CARTESIAN_POINT('Ctrl Pts',(21.531167540981,-10.689651282929,12.));
#184638=CARTESIAN_POINT('Ctrl Pts',(21.5163682155805,-10.6740119402835,
12.));
#184639=CARTESIAN_POINT('Ctrl Pts',(21.5015974644454,-10.6584838598941,
12.));
#184640=CARTESIAN_POINT('Ctrl Pts',(21.4868560880893,-10.6430673196609,
12.));
#184641=CARTESIAN_POINT('Ctrl Pts',(21.4721448964766,-10.6277625990457,
12.));
#184642=CARTESIAN_POINT('Ctrl Pts',(21.4574647092093,-10.612569979096,12.));
#184643=CARTESIAN_POINT('Ctrl Pts',(21.4428163557137,-10.597489742462,12.));
#184644=CARTESIAN_POINT('Ctrl Pts',(21.4282006754624,-10.582522173457,12.));
#184645=CARTESIAN_POINT('Ctrl Pts',(21.4136185181974,-10.5676675581106,
12.));
#184646=CARTESIAN_POINT('Ctrl Pts',(21.3990707441495,-10.5529261842107,
12.));
#184647=CARTESIAN_POINT('Ctrl Pts',(21.3845582242604,-10.5382983413422,
12.));
#184648=CARTESIAN_POINT('Ctrl Pts',(21.3700818403942,-10.523784320906,12.));
#184649=CARTESIAN_POINT('Ctrl Pts',(21.3556424855822,-10.509384416169,12.));
#184650=CARTESIAN_POINT('Ctrl Pts',(21.3412410642912,-10.4950989223341,
12.));
#184651=CARTESIAN_POINT('Ctrl Pts',(21.3268784926823,-10.4809281365933,
12.));
#184652=CARTESIAN_POINT('Ctrl Pts',(21.312555698873,-10.4668723581768,12.));
#184653=CARTESIAN_POINT('Ctrl Pts',(21.2982736231924,-10.452931888387,12.));
#184654=CARTESIAN_POINT('Ctrl Pts',(21.2840332184471,-10.4391070306385,
12.));
#184655=CARTESIAN_POINT('Ctrl Pts',(21.2698354502391,-10.4253980905394,
12.));
#184656=CARTESIAN_POINT('Ctrl Pts',(21.2556812972741,-10.4118053759584,
12.));
#184657=CARTESIAN_POINT('Ctrl Pts',(21.2415717516713,-10.3983291970846,
12.));
#184658=CARTESIAN_POINT('Ctrl Pts',(21.2275078192708,-10.384969866479,12.));
#184659=CARTESIAN_POINT('Ctrl Pts',(21.2134905199359,-10.3717276991137,
12.));
#184660=CARTESIAN_POINT('Ctrl Pts',(21.1995208879205,-10.3586030124595,
12.));
#184661=CARTESIAN_POINT('Ctrl Pts',(21.1855999722427,-10.3455961265706,
12.));
#184662=CARTESIAN_POINT('Ctrl Pts',(21.1717288370512,-10.3327073641574,
12.));
#184663=CARTESIAN_POINT('Ctrl Pts',(21.1579085619959,-10.3199370506541,
12.));
#184664=CARTESIAN_POINT('Ctrl Pts',(21.1441402425831,-10.307285514268,12.));
#184665=CARTESIAN_POINT('Ctrl Pts',(21.130424990599,-10.2947530860714,12.));
#184666=CARTESIAN_POINT('Ctrl Pts',(21.1167639345623,-10.2823401001067,
12.));
#184667=CARTESIAN_POINT('Ctrl Pts',(21.1031582201625,-10.2700468934743,
12.));
#184668=CARTESIAN_POINT('Ctrl Pts',(21.0896090107066,-10.2578738064183,
12.));
#184669=CARTESIAN_POINT('Ctrl Pts',(21.0761174875448,-10.2458211823915,
12.));
#184670=CARTESIAN_POINT('Ctrl Pts',(21.0626848505665,-10.233889368157,12.));
#184671=CARTESIAN_POINT('Ctrl Pts',(21.0493123187483,-10.2220787139157,
12.));
#184672=CARTESIAN_POINT('Ctrl Pts',(21.0360011306814,-10.2103895734124,
12.));
#184673=CARTESIAN_POINT('Ctrl Pts',(21.0227525451107,-10.1988223040425,
12.));
#184674=CARTESIAN_POINT('Ctrl Pts',(21.0095678414486,-10.1873772669358,
12.));
#184675=CARTESIAN_POINT('Ctrl Pts',(20.9964483203685,-10.1760548270765,
12.));
#184676=CARTESIAN_POINT('Ctrl Pts',(20.9833953044736,-10.1648553534567,
12.));
#184677=CARTESIAN_POINT('Ctrl Pts',(20.970410138937,-10.1537792192065,12.));
#184678=CARTESIAN_POINT('Ctrl Pts',(20.9574941921591,-10.1428268017257,
12.));
#184679=CARTESIAN_POINT('Ctrl Pts',(20.944648856393,-10.1319984827909,12.));
#184680=CARTESIAN_POINT('Ctrl Pts',(20.931875548473,-10.1212946487057,12.));
#184681=CARTESIAN_POINT('Ctrl Pts',(20.9191757106266,-10.1107156904836,
12.));
#184682=CARTESIAN_POINT('Ctrl Pts',(20.9065508112556,-10.1002620040076,
12.));
#184683=CARTESIAN_POINT('Ctrl Pts',(20.8940023457371,-10.0899339901916,
12.));
#184684=CARTESIAN_POINT('Ctrl Pts',(20.8815318371844,-10.0797320551154,
12.));
#184685=CARTESIAN_POINT('Ctrl Pts',(20.8691408373705,-10.0696566102219,
12.));
#184686=CARTESIAN_POINT('Ctrl Pts',(20.856830927732,-10.0597080725375,12.));
#184687=CARTESIAN_POINT('Ctrl Pts',(20.8446037203402,-10.0498868648733,
12.));
#184688=CARTESIAN_POINT('Ctrl Pts',(20.8324608588906,-10.0401934160234,
12.));
#184689=CARTESIAN_POINT('Ctrl Pts',(20.8204040196599,-10.0306281609435,
12.));
#184690=CARTESIAN_POINT('Ctrl Pts',(20.8084349126885,-10.0211915410095,
12.));
#184691=CARTESIAN_POINT('Ctrl Pts',(20.7965552829907,-10.0118840042786,
12.));
#184692=CARTESIAN_POINT('Ctrl Pts',(20.7847669117568,-10.0027060057389,
12.));
#184693=CARTESIAN_POINT('Ctrl Pts',(20.7730716175417,-9.99365800754638,
12.));
#184694=CARTESIAN_POINT('Ctrl Pts',(20.7614712574989,-9.98474047926846,
12.));
#184695=CARTESIAN_POINT('Ctrl Pts',(20.7499677289625,-9.97595389823461,
12.));
#184696=CARTESIAN_POINT('Ctrl Pts',(20.7385629709795,-9.96729874986199,
12.));
#184697=CARTESIAN_POINT('Ctrl Pts',(20.7272589658752,-9.95877552798403,
12.));
#184698=CARTESIAN_POINT('Ctrl Pts',(20.716057740758,-9.95038473514962,12.));
#184699=CARTESIAN_POINT('Ctrl Pts',(20.7049613692237,-9.94212688298251,
12.));
#184700=CARTESIAN_POINT('Ctrl Pts',(20.6939719732485,-9.93400249259737,
12.));
#184701=CARTESIAN_POINT('Ctrl Pts',(20.6830917250255,-9.92601209498751,
12.));
#184702=CARTESIAN_POINT('Ctrl Pts',(20.6723228488261,-9.91815623141285,
12.));
#184703=CARTESIAN_POINT('Ctrl Pts',(20.6616676228315,-9.91043545377005,
12.));
#184704=CARTESIAN_POINT('Ctrl Pts',(20.6511283817415,-9.90285032516696,
12.));
#184705=CARTESIAN_POINT('Ctrl Pts',(20.6407075193977,-9.89540142049124,
12.));
#184706=CARTESIAN_POINT('Ctrl Pts',(20.6304074914086,-9.88808932697305,
12.));
#184707=CARTESIAN_POINT('Ctrl Pts',(20.6202308177472,-9.88091464472669,
12.));
#184708=CARTESIAN_POINT('Ctrl Pts',(20.6101800854491,-9.87387798732944,
12.));
#184709=CARTESIAN_POINT('Ctrl Pts',(20.6002579513696,-9.86697998242612,
12.));
#184710=CARTESIAN_POINT('Ctrl Pts',(20.5904671449754,-9.8602212723275,12.));
#184711=CARTESIAN_POINT('Ctrl Pts',(20.580810471002,-9.85360251457004,12.));
#184712=CARTESIAN_POINT('Ctrl Pts',(20.5712908125145,-9.84712438256308,
12.));
#184713=CARTESIAN_POINT('Ctrl Pts',(20.5619111362406,-9.84078756677589,
12.));
#184714=CARTESIAN_POINT('Ctrl Pts',(20.5526744976461,-9.83459277585321,
12.));
#184715=CARTESIAN_POINT('Ctrl Pts',(20.5435840460717,-9.82854073773858,
12.));
#184716=CARTESIAN_POINT('Ctrl Pts',(20.534643029951,-9.82263220080328,12.));
#184717=CARTESIAN_POINT('Ctrl Pts',(20.5258548000625,-9.81686793455918,
12.));
#184718=CARTESIAN_POINT('Ctrl Pts',(20.5172228122839,-9.81124873025278,
12.));
#184719=CARTESIAN_POINT('Ctrl Pts',(20.5087506310507,-9.80577540161103,
12.));
#184720=CARTESIAN_POINT('Ctrl Pts',(20.500441931211,-9.80044878520968,12.));
#184721=CARTESIAN_POINT('Ctrl Pts',(20.4923005087945,-9.79526974288344,
12.));
#184722=CARTESIAN_POINT('Ctrl Pts',(20.4843302955329,-9.7902391649866,12.));
#184723=CARTESIAN_POINT('Ctrl Pts',(20.4765353711585,-9.78535797314162,
12.));
#184724=CARTESIAN_POINT('Ctrl Pts',(20.4689199790668,-9.78062712373313,
12.));
#184725=CARTESIAN_POINT('Ctrl Pts',(20.4614885274973,-9.77604760815523,
12.));
#184726=CARTESIAN_POINT('Ctrl Pts',(20.4542455817527,-9.7716204510407,12.));
#184727=CARTESIAN_POINT('Ctrl Pts',(20.447195862298,-9.76734670980897,12.));
#184728=CARTESIAN_POINT('Ctrl Pts',(20.4403442329401,-9.76322747195502,
12.));
#184729=CARTESIAN_POINT('Ctrl Pts',(20.4336957355474,-9.7592638628993,12.));
#184730=CARTESIAN_POINT('Ctrl Pts',(20.4272556476629,-9.75545705902416,
12.));
#184731=CARTESIAN_POINT('Ctrl Pts',(20.4210295275818,-9.75180829786433,
12.));
#184732=CARTESIAN_POINT('Ctrl Pts',(20.4150232777393,-9.74831889242175,
12.));
#184733=CARTESIAN_POINT('Ctrl Pts',(20.4092430879861,-9.74499021838537,
12.));
#184734=CARTESIAN_POINT('Ctrl Pts',(20.4036953576549,-9.74182369656273,
12.));
#184735=CARTESIAN_POINT('Ctrl Pts',(20.3983866213331,-9.73882077613206,
12.));
#184736=CARTESIAN_POINT('Ctrl Pts',(20.3933234845646,-9.7359829201425,12.));
#184737=CARTESIAN_POINT('Ctrl Pts',(20.3885129129912,-9.73331167102812,
12.));
#184738=CARTESIAN_POINT('Ctrl Pts',(20.3839624556742,-9.73080870123726,
12.));
#184739=CARTESIAN_POINT('Ctrl Pts',(20.3796805893304,-9.72847589116533,
12.));
#184740=CARTESIAN_POINT('Ctrl Pts',(20.3756766651952,-9.72631531732871,
12.));
#184741=CARTESIAN_POINT('Ctrl Pts',(20.371960235676,-9.72432910043193,12.));
#184742=CARTESIAN_POINT('Ctrl Pts',(20.3685406190576,-9.72251930722504,
12.));
#184743=CARTESIAN_POINT('Ctrl Pts',(20.3654261611055,-9.72088778381102,
12.));
#184744=CARTESIAN_POINT('Ctrl Pts',(20.362625691398,-9.71943648548115,12.));
#184745=CARTESIAN_POINT('Ctrl Pts',(20.3601498764344,-9.71816778327999,
12.));
#184746=CARTESIAN_POINT('Ctrl Pts',(20.3580133103357,-9.71708493723062,
12.));
#184747=CARTESIAN_POINT('Ctrl Pts',(20.3562337557875,-9.71619192554147,
12.));
#184748=CARTESIAN_POINT('Ctrl Pts',(20.3548282742361,-9.71549257088175,
12.));
#184749=CARTESIAN_POINT('Ctrl Pts',(20.3538098605706,-9.71498978052101,
12.));
#184750=CARTESIAN_POINT('Ctrl Pts',(20.3533097561886,-9.71474590350792,
12.));
#184751=CARTESIAN_POINT('Ctrl Pts',(20.3531126095522,-9.71465227853122,
12.));
#184752=CARTESIAN_POINT('Ctrl Pts',(20.353060251684,-9.71462954053074,12.));
#184753=CARTESIAN_POINT('Ctrl Pts',(20.353053841303,-9.71462809124917,12.));
#184754=CARTESIAN_POINT('',(19.84920021178,-9.47413589477549,12.));
#184755=CARTESIAN_POINT('',(9.70154690100589,-4.63060338698782,12.));
#184756=CARTESIAN_POINT('',(19.6085639972844,-8.81783521984851,12.));
#184757=CARTESIAN_POINT('Origin',(20.0645771135003,-9.02290115519382,12.));
#184758=CARTESIAN_POINT('',(20.1004996511507,-7.63019749246979,12.));
#184759=CARTESIAN_POINT('Origin',(7.08841632778409E-13,-3.26562511982935E-13,
12.));
#184760=CARTESIAN_POINT('',(20.7347298079577,-7.33627833380047,12.));
#184761=CARTESIAN_POINT('Origin',(20.56795313141,-7.80764394578304,12.));
#184762=CARTESIAN_POINT('',(21.2610617890679,-7.52250298901266,12.));
#184763=CARTESIAN_POINT('',(10.6305308945339,-3.76125149450632,12.));
#184764=CARTESIAN_POINT('',(24.9347862158358,-7.36589684767345,12.));
#184765=CARTESIAN_POINT('Ctrl Pts',(21.2610617890679,-7.52250298901266,
12.));
#184766=CARTESIAN_POINT('Ctrl Pts',(21.2610673466883,-7.52250649703992,
12.));
#184767=CARTESIAN_POINT('Ctrl Pts',(21.261120447486,-7.52252744144958,12.));
#184768=CARTESIAN_POINT('Ctrl Pts',(21.2613260540651,-7.52260064231736,
12.));
#184769=CARTESIAN_POINT('Ctrl Pts',(21.261852128355,-7.52278182242728,12.));
#184770=CARTESIAN_POINT('Ctrl Pts',(21.262927782038,-7.52314642316203,12.));
#184771=CARTESIAN_POINT('Ctrl Pts',(21.2644161259965,-7.52364573027521,
12.));
#184772=CARTESIAN_POINT('Ctrl Pts',(21.266305915706,-7.52427261074264,12.));
#184773=CARTESIAN_POINT('Ctrl Pts',(21.2685823838672,-7.52501770333522,
12.));
#184774=CARTESIAN_POINT('Ctrl Pts',(21.2712301573465,-7.52587126095544,
12.));
#184775=CARTESIAN_POINT('Ctrl Pts',(21.2742366113578,-7.52682526918561,
12.));
#184776=CARTESIAN_POINT('Ctrl Pts',(21.2775925269651,-7.52787386225344,
12.));
#184777=CARTESIAN_POINT('Ctrl Pts',(21.2812902781143,-7.52901217930407,
12.));
#184778=CARTESIAN_POINT('Ctrl Pts',(21.2853226580658,-7.53023562438221,
12.));
#184779=CARTESIAN_POINT('Ctrl Pts',(21.2896816163843,-7.53153906987847,
12.));
#184780=CARTESIAN_POINT('Ctrl Pts',(21.2943588989331,-7.53291726078527,
12.));
#184781=CARTESIAN_POINT('Ctrl Pts',(21.2993464250717,-7.53436505309949,
12.));
#184782=CARTESIAN_POINT('Ctrl Pts',(21.3046368712156,-7.53587778251743,
12.));
#184783=CARTESIAN_POINT('Ctrl Pts',(21.3102237167729,-7.5374512936462,12.));
#184784=CARTESIAN_POINT('Ctrl Pts',(21.3161009456256,-7.53908175169899,
12.));
#184785=CARTESIAN_POINT('Ctrl Pts',(21.3222628524165,-7.5407655203828,12.));
#184786=CARTESIAN_POINT('Ctrl Pts',(21.328703791771,-7.54249900377032,12.));
#184787=CARTESIAN_POINT('Ctrl Pts',(21.3354182340149,-7.54427868151269,
12.));
#184788=CARTESIAN_POINT('Ctrl Pts',(21.3424008295038,-7.54610114948351,
12.));
#184789=CARTESIAN_POINT('Ctrl Pts',(21.349646476153,-7.54796316246327,12.));
#184790=CARTESIAN_POINT('Ctrl Pts',(21.3571503685853,-7.54986166521307,
12.));
#184791=CARTESIAN_POINT('Ctrl Pts',(21.3649079431864,-7.55179375777442,
12.));
#184792=CARTESIAN_POINT('Ctrl Pts',(21.3729148390244,-7.55375667080032,
12.));
#184793=CARTESIAN_POINT('Ctrl Pts',(21.3811668478933,-7.55574773403508,
12.));
#184794=CARTESIAN_POINT('Ctrl Pts',(21.3896598842119,-7.55776435731422,
12.));
#184795=CARTESIAN_POINT('Ctrl Pts',(21.3983899952988,-7.55980403700615,
12.));
#184796=CARTESIAN_POINT('Ctrl Pts',(21.4073533630364,-7.56186435703622,
12.));
#184797=CARTESIAN_POINT('Ctrl Pts',(21.4165463106252,-7.56394299313683,
12.));
#184798=CARTESIAN_POINT('Ctrl Pts',(21.4259653015732,-7.56603771218706,
12.));
#184799=CARTESIAN_POINT('Ctrl Pts',(21.435606926151,-7.56814636360842,12.));
#184800=CARTESIAN_POINT('Ctrl Pts',(21.445467890751,-7.5702668726117,12.));
#184801=CARTESIAN_POINT('Ctrl Pts',(21.4555450053147,-7.57239723223521,
12.));
#184802=CARTESIAN_POINT('Ctrl Pts',(21.4658351740135,-7.57453549743435,
12.));
#184803=CARTESIAN_POINT('Ctrl Pts',(21.4763353936766,-7.57667978403003,
12.));
#184804=CARTESIAN_POINT('Ctrl Pts',(21.4870427508193,-7.57882826679131,
12.));
#184805=CARTESIAN_POINT('Ctrl Pts',(21.4979544192739,-7.5809791779073,12.));
#184806=CARTESIAN_POINT('Ctrl Pts',(21.5090676573866,-7.58313080519159,
12.));
#184807=CARTESIAN_POINT('Ctrl Pts',(21.5203798035294,-7.58528148919114,
12.));
#184808=CARTESIAN_POINT('Ctrl Pts',(21.5318882716735,-7.58742962034834,
12.));
#184809=CARTESIAN_POINT('Ctrl Pts',(21.5435905470113,-7.58957363620026,
12.));
#184810=CARTESIAN_POINT('Ctrl Pts',(21.5554841813465,-7.59171201844793,
12.));
#184811=CARTESIAN_POINT('Ctrl Pts',(21.5675667904728,-7.5938432912493,12.));
#184812=CARTESIAN_POINT('Ctrl Pts',(21.5798360518978,-7.59596601973589,
12.));
#184813=CARTESIAN_POINT('Ctrl Pts',(21.5922897024466,-7.59807880846193,
12.));
#184814=CARTESIAN_POINT('Ctrl Pts',(21.6049255358842,-7.60018029988238,
12.));
#184815=CARTESIAN_POINT('Ctrl Pts',(21.6177414005991,-7.60226917285432,
12.));
#184816=CARTESIAN_POINT('Ctrl Pts',(21.6307351973823,-7.604344141183,12.));
#184817=CARTESIAN_POINT('Ctrl Pts',(21.6439048771743,-7.60640395216359,
12.));
#184818=CARTESIAN_POINT('Ctrl Pts',(21.6572484388079,-7.60844738512872,
12.));
#184819=CARTESIAN_POINT('Ctrl Pts',(21.6707639267573,-7.6104732500095,12.));
#184820=CARTESIAN_POINT('Ctrl Pts',(21.6844494295813,-7.61248038630265,
12.));
#184821=CARTESIAN_POINT('Ctrl Pts',(21.6983030783321,-7.61446766202787,
12.));
#184822=CARTESIAN_POINT('Ctrl Pts',(21.7123230449835,-7.61643397270425,
12.));
#184823=CARTESIAN_POINT('Ctrl Pts',(21.7265075407977,-7.61837824030542,
12.));
#184824=CARTESIAN_POINT('Ctrl Pts',(21.7408548148657,-7.62029941230855,
12.));
#184825=CARTESIAN_POINT('Ctrl Pts',(21.7553631528329,-7.62219646084226,
12.));
#184826=CARTESIAN_POINT('Ctrl Pts',(21.7700308755583,-7.62406838181164,
12.));
#184827=CARTESIAN_POINT('Ctrl Pts',(21.7848563378022,-7.62591419404521,
12.));
#184828=CARTESIAN_POINT('Ctrl Pts',(21.7998379268583,-7.62773293842409,
12.));
#184829=CARTESIAN_POINT('Ctrl Pts',(21.8149740615093,-7.62952367718151,
12.));
#184830=CARTESIAN_POINT('Ctrl Pts',(21.8302631910197,-7.6312854932304,12.));
#184831=CARTESIAN_POINT('Ctrl Pts',(21.8457037941084,-7.63301748948936,
12.));
#184832=CARTESIAN_POINT('Ctrl Pts',(21.8612943779086,-7.63471878821204,
12.));
#184833=CARTESIAN_POINT('Ctrl Pts',(21.8770334769492,-7.63638853033368,
12.));
#184834=CARTESIAN_POINT('Ctrl Pts',(21.8929196523511,-7.63802587492008,
12.));
#184835=CARTESIAN_POINT('Ctrl Pts',(21.9089514909873,-7.63962999860917,
12.));
#184836=CARTESIAN_POINT('Ctrl Pts',(21.9251276046546,-7.6412000950654,12.));
#184837=CARTESIAN_POINT('Ctrl Pts',(21.9414466292074,-7.64273537442707,
12.));
#184838=CARTESIAN_POINT('Ctrl Pts',(21.9579072237653,-7.64423506279154,
12.));
#184839=CARTESIAN_POINT('Ctrl Pts',(21.97450807008,-7.64569840177359,12.));
#184840=CARTESIAN_POINT('Ctrl Pts',(21.9912478718542,-7.64712464805258,
12.));
#184841=CARTESIAN_POINT('Ctrl Pts',(22.0081253540773,-7.64851307293346,
12.));
#184842=CARTESIAN_POINT('Ctrl Pts',(22.0251392623209,-7.64986296190157,
12.));
#184843=CARTESIAN_POINT('Ctrl Pts',(22.0422883621176,-7.65117361421347,
12.));
#184844=CARTESIAN_POINT('Ctrl Pts',(22.0595714384432,-7.65244434253104,
12.));
#184845=CARTESIAN_POINT('Ctrl Pts',(22.0769872951596,-7.65367447254945,
12.));
#184846=CARTESIAN_POINT('Ctrl Pts',(22.094534754469,-7.65486334263651,12.));
#184847=CARTESIAN_POINT('Ctrl Pts',(22.1122126563327,-7.65601030346819,
12.));
#184848=CARTESIAN_POINT('Ctrl Pts',(22.1300198579671,-7.65711471769407,
12.));
#184849=CARTESIAN_POINT('Ctrl Pts',(22.1479552334206,-7.65817595963351,
12.));
#184850=CARTESIAN_POINT('Ctrl Pts',(22.1660176731174,-7.65919341496926,
12.));
#184851=CARTESIAN_POINT('Ctrl Pts',(22.1842060834092,-7.66016648045008,
12.));
#184852=CARTESIAN_POINT('Ctrl Pts',(22.2025193860972,-7.66109456359292,
12.));
#184853=CARTESIAN_POINT('Ctrl Pts',(22.2209565180098,-7.66197708240436,
12.));
#184854=CARTESIAN_POINT('Ctrl Pts',(22.239516430656,-7.66281346512546,12.));
#184855=CARTESIAN_POINT('Ctrl Pts',(22.2581980898487,-7.66360314997662,
12.));
#184856=CARTESIAN_POINT('Ctrl Pts',(22.2770004753332,-7.66434558490973,
12.));
#184857=CARTESIAN_POINT('Ctrl Pts',(22.2959225803925,-7.66504022736263,
12.));
#184858=CARTESIAN_POINT('Ctrl Pts',(22.3149634114823,-7.66568654402442,
12.));
#184859=CARTESIAN_POINT('Ctrl Pts',(22.3341219879454,-7.66628401061906,
12.));
#184860=CARTESIAN_POINT('Ctrl Pts',(22.3533973417013,-7.66683211169134,
12.));
#184861=CARTESIAN_POINT('Ctrl Pts',(22.3727885169361,-7.66733034039887,
12.));
#184862=CARTESIAN_POINT('Ctrl Pts',(22.3922945697782,-7.6677781983082,12.));
#184863=CARTESIAN_POINT('Ctrl Pts',(22.411914567977,-7.66817519519682,12.));
#184864=CARTESIAN_POINT('Ctrl Pts',(22.4316475906616,-7.66852084886746,
12.));
#184865=CARTESIAN_POINT('Ctrl Pts',(22.4514927280862,-7.6688146849666,12.));
#184866=CARTESIAN_POINT('Ctrl Pts',(22.47144908137,-7.66905623680836,12.));
#184867=CARTESIAN_POINT('Ctrl Pts',(22.4915157622308,-7.66924504520302,
12.));
#184868=CARTESIAN_POINT('Ctrl Pts',(22.5116918927023,-7.66938065829083,
12.));
#184869=CARTESIAN_POINT('Ctrl Pts',(22.5319766049191,-7.66946263138116,
12.));
#184870=CARTESIAN_POINT('Ctrl Pts',(22.5523690409109,-7.66949052679672,
12.));
#184871=CARTESIAN_POINT('Ctrl Pts',(22.5728683523828,-7.66946391372299,
12.));
#184872=CARTESIAN_POINT('Ctrl Pts',(22.5934737004955,-7.66938236806241,
12.));
#184873=CARTESIAN_POINT('Ctrl Pts',(22.6141842556248,-7.66924547229435,
12.));
#184874=CARTESIAN_POINT('Ctrl Pts',(22.6349991971547,-7.66905281533745,
12.));
#184875=CARTESIAN_POINT('Ctrl Pts',(22.6559177133133,-7.66880399241354,
12.));
#184876=CARTESIAN_POINT('Ctrl Pts',(22.6769390009889,-7.66849860491763,
12.));
#184877=CARTESIAN_POINT('Ctrl Pts',(22.6980622655446,-7.66813626029277,
12.));
#184878=CARTESIAN_POINT('Ctrl Pts',(22.7192867206242,-7.6677165719101,12.));
#184879=CARTESIAN_POINT('Ctrl Pts',(22.7406115879508,-7.66723915895413,
12.));
#184880=CARTESIAN_POINT('Ctrl Pts',(22.7620360971839,-7.66670364630273,
12.));
#184881=CARTESIAN_POINT('Ctrl Pts',(22.7835594857697,-7.66610966441259,
12.));
#184882=CARTESIAN_POINT('Ctrl Pts',(22.8051809987833,-7.66545684920988,
12.));
#184883=CARTESIAN_POINT('Ctrl Pts',(22.8268998887678,-7.66474484198553,
12.));
#184884=CARTESIAN_POINT('Ctrl Pts',(22.8487154155569,-7.66397328929805,
12.));
#184885=CARTESIAN_POINT('Ctrl Pts',(22.870626846128,-7.66314184287334,12.));
#184886=CARTESIAN_POINT('Ctrl Pts',(22.8926334544879,-7.66225015950148,
12.));
#184887=CARTESIAN_POINT('Ctrl Pts',(22.9147345215418,-7.661297900941,12.));
#184888=CARTESIAN_POINT('Ctrl Pts',(22.9369293349592,-7.66028473382777,
12.));
#184889=CARTESIAN_POINT('Ctrl Pts',(22.9592171890332,-7.65921032958912,
12.));
#184890=CARTESIAN_POINT('Ctrl Pts',(22.9815973845301,-7.65807436436453,
12.));
#184891=CARTESIAN_POINT('Ctrl Pts',(23.004069228582,-7.6568765189133,12.));
#184892=CARTESIAN_POINT('Ctrl Pts',(23.0266320345792,-7.65561647852555,
12.));
#184893=CARTESIAN_POINT('Ctrl Pts',(23.049285122053,-7.65429393293955,12.));
#184894=CARTESIAN_POINT('Ctrl Pts',(23.072027816555,-7.65290857626357,12.));
#184895=CARTESIAN_POINT('Ctrl Pts',(23.0948594495246,-7.65146010690465,
12.));
#184896=CARTESIAN_POINT('Ctrl Pts',(23.1177793581674,-7.64994822749845,
12.));
#184897=CARTESIAN_POINT('Ctrl Pts',(23.1407868853815,-7.64837264482929,
12.));
#184898=CARTESIAN_POINT('Ctrl Pts',(23.1638813796691,-7.64673306975797,
12.));
#184899=CARTESIAN_POINT('Ctrl Pts',(23.1870621950452,-7.64502921715483,
12.));
#184900=CARTESIAN_POINT('Ctrl Pts',(23.2103286909399,-7.64326080583684,
12.));
#184901=CARTESIAN_POINT('Ctrl Pts',(23.2336802320912,-7.64142755851508,
12.));
#184902=CARTESIAN_POINT('Ctrl Pts',(23.2571161884487,-7.63952920172837,
12.));
#184903=CARTESIAN_POINT('Ctrl Pts',(23.2806359350853,-7.63756546576375,
12.));
#184904=CARTESIAN_POINT('Ctrl Pts',(23.3042388521021,-7.63553608458784,
12.));
#184905=CARTESIAN_POINT('Ctrl Pts',(23.3279243245241,-7.63344079578163,
12.));
#184906=CARTESIAN_POINT('Ctrl Pts',(23.3516917421973,-7.63127934048139,
12.));
#184907=CARTESIAN_POINT('Ctrl Pts',(23.3755404996638,-7.62905146332598,
12.));
#184908=CARTESIAN_POINT('Ctrl Pts',(23.3994699961122,-7.62675691240335,
12.));
#184909=CARTESIAN_POINT('Ctrl Pts',(23.4234796353544,-7.62439543920055,
12.));
#184910=CARTESIAN_POINT('Ctrl Pts',(23.4475688257854,-7.62196679855957,
12.));
#184911=CARTESIAN_POINT('Ctrl Pts',(23.4717369803438,-7.61947074863978,
12.));
#184912=CARTESIAN_POINT('Ctrl Pts',(23.4959835164608,-7.61690705088319,
12.));
#184913=CARTESIAN_POINT('Ctrl Pts',(23.5203078560128,-7.61427546999299,
12.));
#184914=CARTESIAN_POINT('Ctrl Pts',(23.5447094252028,-7.61157577385372,
12.));
#184915=CARTESIAN_POINT('Ctrl Pts',(23.5691876544243,-7.608807733446,12.));
#184916=CARTESIAN_POINT('Ctrl Pts',(23.5937419781244,-7.60597112277094,
12.));
#184917=CARTESIAN_POINT('Ctrl Pts',(23.6183718346576,-7.60306571877806,
12.));
#184918=CARTESIAN_POINT('Ctrl Pts',(23.6430766661419,-7.6000913013013,12.));
#184919=CARTESIAN_POINT('Ctrl Pts',(23.6678559182876,-7.59704765299572,
12.));
#184920=CARTESIAN_POINT('Ctrl Pts',(23.6927090405067,-7.59393455934042,
12.));
#184921=CARTESIAN_POINT('Ctrl Pts',(23.7176354860457,-7.59075180865327,
12.));
#184922=CARTESIAN_POINT('Ctrl Pts',(23.7426347121006,-7.58749919210832,
12.));
#184923=CARTESIAN_POINT('Ctrl Pts',(23.7677061799376,-7.58417650376272,
12.));
#184924=CARTESIAN_POINT('Ctrl Pts',(23.7928493549908,-7.58078354058212,
12.));
#184925=CARTESIAN_POINT('Ctrl Pts',(23.8180637069977,-7.57732010249066,
12.));
#184926=CARTESIAN_POINT('Ctrl Pts',(23.8433487096134,-7.57378599219817,
12.));
#184927=CARTESIAN_POINT('Ctrl Pts',(23.8687038399597,-7.57018101500711,
12.));
#184928=CARTESIAN_POINT('Ctrl Pts',(23.8941285782003,-7.56650497863792,
12.));
#184929=CARTESIAN_POINT('Ctrl Pts',(23.9196224070759,-7.56275769304773,
12.));
#184930=CARTESIAN_POINT('Ctrl Pts',(23.9451848115,-7.55893897027683,12.));
#184931=CARTESIAN_POINT('Ctrl Pts',(23.9708152779884,-7.55504862424812,
12.));
#184932=CARTESIAN_POINT('Ctrl Pts',(23.9965132953185,-7.55108647097441,
12.));
#184933=CARTESIAN_POINT('Ctrl Pts',(24.022278355453,-7.5470523288591,12.));
#184934=CARTESIAN_POINT('Ctrl Pts',(24.0481099543353,-7.54294601896145,
12.));
#184935=CARTESIAN_POINT('Ctrl Pts',(24.0740075927985,-7.53876736531014,
12.));
#184936=CARTESIAN_POINT('Ctrl Pts',(24.0999707772642,-7.53451619514649,
12.));
#184937=CARTESIAN_POINT('Ctrl Pts',(24.1259990209207,-7.53019233935502,
12.));
#184938=CARTESIAN_POINT('Ctrl Pts',(24.1520918425364,-7.52579563201424,
12.));
#184939=CARTESIAN_POINT('Ctrl Pts',(24.1782487641594,-7.52132590953802,
12.));
#184940=CARTESIAN_POINT('Ctrl Pts',(24.2044693092349,-7.51678300997949,
12.));
#184941=CARTESIAN_POINT('Ctrl Pts',(24.2307530003887,-7.51216677222181,
12.));
#184942=CARTESIAN_POINT('Ctrl Pts',(24.2570993577034,-7.50747703535134,
12.));
#184943=CARTESIAN_POINT('Ctrl Pts',(24.2835078958973,-7.50271363765152,
12.));
#184944=CARTESIAN_POINT('Ctrl Pts',(24.3099781253355,-7.49787641695439,
12.));
#184945=CARTESIAN_POINT('Ctrl Pts',(24.3365095573685,-7.49296521252421,
12.));
#184946=CARTESIAN_POINT('Ctrl Pts',(24.3631017084524,-7.48797986651909,
12.));
#184947=CARTESIAN_POINT('Ctrl Pts',(24.3897541049254,-7.48292022569301,
12.));
#184948=CARTESIAN_POINT('Ctrl Pts',(24.4164662871163,-7.47778614286565,
12.));
#184949=CARTESIAN_POINT('Ctrl Pts',(24.443237814649,-7.47257747883246,12.));
#184950=CARTESIAN_POINT('Ctrl Pts',(24.4700682684524,-7.46729410308787,
12.));
#184951=CARTESIAN_POINT('Ctrl Pts',(24.4969572391483,-7.46193588961464,
12.));
#184952=CARTESIAN_POINT('Ctrl Pts',(24.5239043173072,-7.45650271335862,
12.));
#184953=CARTESIAN_POINT('Ctrl Pts',(24.5509090831559,-7.4509944465116,12.));
#184954=CARTESIAN_POINT('Ctrl Pts',(24.577971096086,-7.44541095473135,12.));
#184955=CARTESIAN_POINT('Ctrl Pts',(24.6050898852368,-7.43975209375504,
12.));
#184956=CARTESIAN_POINT('Ctrl Pts',(24.6322649369517,-7.43401770489524,
12.));
#184957=CARTESIAN_POINT('Ctrl Pts',(24.6594957128756,-7.42820762159126,
12.));
#184958=CARTESIAN_POINT('Ctrl Pts',(24.6867816727192,-7.42232167766266,
12.));
#184959=CARTESIAN_POINT('Ctrl Pts',(24.7141222950051,-7.41635971481674,
12.));
#184960=CARTESIAN_POINT('Ctrl Pts',(24.7415170994784,-7.41032159082382,
12.));
#184961=CARTESIAN_POINT('Ctrl Pts',(24.7689656668983,-7.40420718661603,
12.));
#184962=CARTESIAN_POINT('Ctrl Pts',(24.7964676646431,-7.39801641583013,
12.));
#184963=CARTESIAN_POINT('Ctrl Pts',(24.8240228520893,-7.39174922585809,
12.));
#184964=CARTESIAN_POINT('Ctrl Pts',(24.8516310625176,-7.38540558903621,
12.));
#184965=CARTESIAN_POINT('Ctrl Pts',(24.8792921911115,-7.3789854964027,12.));
#184966=CARTESIAN_POINT('Ctrl Pts',(24.901463382605,-7.37378825961676,12.));
#184967=CARTESIAN_POINT('Ctrl Pts',(24.9181155530543,-7.36985593120091,
12.));
#184968=CARTESIAN_POINT('Ctrl Pts',(24.9292275670674,-7.36721909028843,
12.));
#184969=CARTESIAN_POINT('Ctrl Pts',(24.9347862158358,-7.36589684767345,
12.));
#184970=CARTESIAN_POINT('',(25.2771067246846,-6.088339316177,12.));
#184971=CARTESIAN_POINT('Origin',(0.,0.,12.));
#184972=CARTESIAN_POINT('',(22.1738711152697,-4.11585220600463,12.));
#184973=CARTESIAN_POINT('Ctrl Pts',(25.2771067246846,-6.088339316177,12.));
#184974=CARTESIAN_POINT('Ctrl Pts',(25.2729539149517,-6.08441489609794,
12.));
#184975=CARTESIAN_POINT('Ctrl Pts',(25.2646490489922,-6.07657531787491,
12.));
#184976=CARTESIAN_POINT('Ctrl Pts',(25.2521940105705,-6.06484373634547,
12.));
#184977=CARTESIAN_POINT('Ctrl Pts',(25.2355918139032,-6.04925720151219,
12.));
#184978=CARTESIAN_POINT('Ctrl Pts',(25.21484662016,-6.02986667389998,12.));
#184979=CARTESIAN_POINT('Ctrl Pts',(25.1941090269819,-6.01056881804614,
12.));
#184980=CARTESIAN_POINT('Ctrl Pts',(25.1733791296259,-5.99136367859755,
12.));
#184981=CARTESIAN_POINT('Ctrl Pts',(25.1526570863092,-5.97225131495618,
12.));
#184982=CARTESIAN_POINT('Ctrl Pts',(25.1319431317237,-5.95323180187379,
12.));
#184983=CARTESIAN_POINT('Ctrl Pts',(25.1112375971106,-5.93430523086836,
12.));
#184984=CARTESIAN_POINT('Ctrl Pts',(25.0905409050773,-5.91547170844448,
12.));
#184985=CARTESIAN_POINT('Ctrl Pts',(25.0698535426514,-5.89673135155515,
12.));
#184986=CARTESIAN_POINT('Ctrl Pts',(25.049176040591,-5.87808428385367,12.));
#184987=CARTESIAN_POINT('Ctrl Pts',(25.0285089498899,-5.85953063156827,
12.));
#184988=CARTESIAN_POINT('Ctrl Pts',(25.0078528200564,-5.84107051963072,
12.));
#184989=CARTESIAN_POINT('Ctrl Pts',(24.9872081752734,-5.822704067442,12.));
#184990=CARTESIAN_POINT('Ctrl Pts',(24.9665754954496,-5.80443138549727,
12.));
#184991=CARTESIAN_POINT('Ctrl Pts',(24.945955229334,-5.78625257775682,12.));
#184992=CARTESIAN_POINT('Ctrl Pts',(24.9253478043656,-5.76816774342221,
12.));
#184993=CARTESIAN_POINT('Ctrl Pts',(24.904753637648,-5.75017697890805,12.));
#184994=CARTESIAN_POINT('Ctrl Pts',(24.884173146722,-5.73228037976928,12.));
#184995=CARTESIAN_POINT('Ctrl Pts',(24.8636067597669,-5.71447804252028,
12.));
#184996=CARTESIAN_POINT('Ctrl Pts',(24.8430549277621,-5.69677006679445,
12.));
#184997=CARTESIAN_POINT('Ctrl Pts',(24.8225181223845,-5.67915655496543,
12.));
#184998=CARTESIAN_POINT('Ctrl Pts',(24.8019968304605,-5.66163761114922,
12.));
#184999=CARTESIAN_POINT('Ctrl Pts',(24.781491549672,-5.64421334042262,12.));
#185000=CARTESIAN_POINT('Ctrl Pts',(24.7610027835697,-5.62688384790924,
12.));
#185001=CARTESIAN_POINT('Ctrl Pts',(24.7405310372739,-5.60964923798492,
12.));
#185002=CARTESIAN_POINT('Ctrl Pts',(24.7200768119088,-5.59250961323988,
12.));
#185003=CARTESIAN_POINT('Ctrl Pts',(24.6996406035517,-5.57546507427756,
12.));
#185004=CARTESIAN_POINT('Ctrl Pts',(24.6792229061794,-5.55851572025377,
12.));
#185005=CARTESIAN_POINT('Ctrl Pts',(24.6588242134738,-5.54166164919584,
12.));
#185006=CARTESIAN_POINT('Ctrl Pts',(24.6384450211467,-5.52490295840993,
12.));
#185007=CARTESIAN_POINT('Ctrl Pts',(24.6180858289179,-5.50823974481963,
12.));
#185008=CARTESIAN_POINT('Ctrl Pts',(24.5977471429364,-5.49167210537248,
12.));
#185009=CARTESIAN_POINT('Ctrl Pts',(24.5774294770329,-5.4752001372442,12.));
#185010=CARTESIAN_POINT('Ctrl Pts',(24.5571333514842,-5.45882393762263,
12.));
#185011=CARTESIAN_POINT('Ctrl Pts',(24.5368592922863,-5.44254360356881,
12.));
#185012=CARTESIAN_POINT('Ctrl Pts',(24.5166078302108,-5.4263592318342,12.));
#185013=CARTESIAN_POINT('Ctrl Pts',(24.496379499983,-5.41027091869242,12.));
#185014=CARTESIAN_POINT('Ctrl Pts',(24.4761748393321,-5.39427875973825,
12.));
#185015=CARTESIAN_POINT('Ctrl Pts',(24.4559943883157,-5.37838284973696,
12.));
#185016=CARTESIAN_POINT('Ctrl Pts',(24.435838689915,-5.36258328273628,12.));
#185017=CARTESIAN_POINT('Ctrl Pts',(24.4157082904614,-5.34688015213538,
12.));
#185018=CARTESIAN_POINT('Ctrl Pts',(24.3956037401293,-5.33127355076035,
12.));
#185019=CARTESIAN_POINT('Ctrl Pts',(24.3755255933917,-5.31576357092527,
12.));
#185020=CARTESIAN_POINT('Ctrl Pts',(24.3554744095075,-5.30035030449065,
12.));
#185021=CARTESIAN_POINT('Ctrl Pts',(24.3354507529414,-5.28503384290649,
12.));
#185022=CARTESIAN_POINT('Ctrl Pts',(24.3154551932221,-5.269814277188,12.));
#185023=CARTESIAN_POINT('Ctrl Pts',(24.2954883048447,-5.25469169788858,
12.));
#185024=CARTESIAN_POINT('Ctrl Pts',(24.2755506671525,-5.2396661950629,12.));
#185025=CARTESIAN_POINT('Ctrl Pts',(24.2556428642294,-5.22473785822443,
12.));
#185026=CARTESIAN_POINT('Ctrl Pts',(24.2357654847766,-5.20990677629177,
12.));
#185027=CARTESIAN_POINT('Ctrl Pts',(24.2159191220171,-5.19517303753648,
12.));
#185028=CARTESIAN_POINT('Ctrl Pts',(24.1961043738755,-5.180536729614,12.));
#185029=CARTESIAN_POINT('Ctrl Pts',(24.1763218431344,-5.16599793957987,
12.));
#185030=CARTESIAN_POINT('Ctrl Pts',(24.1565721375971,-5.1515567539008,12.));
#185031=CARTESIAN_POINT('Ctrl Pts',(24.1368558702443,-5.13721325845746,
12.));
#185032=CARTESIAN_POINT('Ctrl Pts',(24.117173659394,-5.12296753853858,12.));
#185033=CARTESIAN_POINT('Ctrl Pts',(24.0975261288444,-5.10881967883126,
12.));
#185034=CARTESIAN_POINT('Ctrl Pts',(24.0779139079264,-5.09476976342618,
12.));
#185035=CARTESIAN_POINT('Ctrl Pts',(24.0583376315636,-5.08081787581271,
12.));
#185036=CARTESIAN_POINT('Ctrl Pts',(24.0387979403268,-5.0669640988664,12.));
#185037=CARTESIAN_POINT('Ctrl Pts',(24.0192954804896,-5.05320851483069,
12.));
#185038=CARTESIAN_POINT('Ctrl Pts',(23.9998309040747,-5.03955120528528,
12.));
#185039=CARTESIAN_POINT('Ctrl Pts',(23.9804048689228,-5.02599225112462,
12.));
#185040=CARTESIAN_POINT('Ctrl Pts',(23.9610180388271,-5.01253173257459,
12.));
#185041=CARTESIAN_POINT('Ctrl Pts',(23.9416710836528,-4.9991697291931,12.));
#185042=CARTESIAN_POINT('Ctrl Pts',(23.9223646794591,-4.98590631986534,
12.));
#185043=CARTESIAN_POINT('Ctrl Pts',(23.9030995086164,-4.9727415827923,12.));
#185044=CARTESIAN_POINT('Ctrl Pts',(23.883876259922,-4.95967559546566,12.));
#185045=CARTESIAN_POINT('Ctrl Pts',(23.8646956287172,-4.94670843465869,
12.));
#185046=CARTESIAN_POINT('Ctrl Pts',(23.8455583170062,-4.93384017643443,
12.));
#185047=CARTESIAN_POINT('Ctrl Pts',(23.8264650335721,-4.92107089613978,
12.));
#185048=CARTESIAN_POINT('Ctrl Pts',(23.8074164940897,-4.90840066839348,
12.));
#185049=CARTESIAN_POINT('Ctrl Pts',(23.7884134212381,-4.89582956706772,
12.));
#185050=CARTESIAN_POINT('Ctrl Pts',(23.7694565448044,-4.88335766525566,
12.));
#185051=CARTESIAN_POINT('Ctrl Pts',(23.7505466018239,-4.87098503527144,
12.));
#185052=CARTESIAN_POINT('Ctrl Pts',(23.7316843367308,-4.85871174865493,
12.));
#185053=CARTESIAN_POINT('Ctrl Pts',(23.7128705015014,-4.84653787616424,
12.));
#185054=CARTESIAN_POINT('Ctrl Pts',(23.6941058557971,-4.83446348776268,
12.));
#185055=CARTESIAN_POINT('Ctrl Pts',(23.6753911671023,-4.82248865259571,
12.));
#185056=CARTESIAN_POINT('Ctrl Pts',(23.6567272108631,-4.81061343896443,
12.));
#185057=CARTESIAN_POINT('Ctrl Pts',(23.6381147706581,-4.79883791433231,
12.));
#185058=CARTESIAN_POINT('Ctrl Pts',(23.6195546383625,-4.78716214532105,
12.));
#185059=CARTESIAN_POINT('Ctrl Pts',(23.6010476143099,-4.77558619769876,
12.));
#185060=CARTESIAN_POINT('Ctrl Pts',(23.5825945074535,-4.76411013636252,
12.));
#185061=CARTESIAN_POINT('Ctrl Pts',(23.564196135517,-4.75273402530616,12.));
#185062=CARTESIAN_POINT('Ctrl Pts',(23.5458533251715,-4.74145792760699,
12.));
#185063=CARTESIAN_POINT('Ctrl Pts',(23.5275669122378,-4.73028190543032,
12.));
#185064=CARTESIAN_POINT('Ctrl Pts',(23.5093377418784,-4.71920602001905,
12.));
#185065=CARTESIAN_POINT('Ctrl Pts',(23.491166668789,-4.70823033167821,12.));
#185066=CARTESIAN_POINT('Ctrl Pts',(23.4730545573849,-4.69735489975024,
12.));
#185067=CARTESIAN_POINT('Ctrl Pts',(23.4550022819852,-4.68657978258298,
12.));
#185068=CARTESIAN_POINT('Ctrl Pts',(23.4370107270444,-4.67590503753051,
12.));
#185069=CARTESIAN_POINT('Ctrl Pts',(23.4190807873798,-4.66533072094664,
12.));
#185070=CARTESIAN_POINT('Ctrl Pts',(23.4012133683957,-4.65485688816923,
12.));
#185071=CARTESIAN_POINT('Ctrl Pts',(23.383409386307,-4.64448359349936,12.));
#185072=CARTESIAN_POINT('Ctrl Pts',(23.3656697683496,-4.63421089016556,
12.));
#185073=CARTESIAN_POINT('Ctrl Pts',(23.3479954530281,-4.62403883030825,
12.));
#185074=CARTESIAN_POINT('Ctrl Pts',(23.3303873903947,-4.6139674649785,12.));
#185075=CARTESIAN_POINT('Ctrl Pts',(23.3128465423119,-4.60399684412176,
12.));
#185076=CARTESIAN_POINT('Ctrl Pts',(23.295373882719,-4.59412701655751,12.));
#185077=CARTESIAN_POINT('Ctrl Pts',(23.2779703978868,-4.58435802994675,
12.));
#185078=CARTESIAN_POINT('Ctrl Pts',(23.2606370866853,-4.57468993076071,
12.));
#185079=CARTESIAN_POINT('Ctrl Pts',(23.2433749609117,-4.56512276427812,
12.));
#185080=CARTESIAN_POINT('Ctrl Pts',(23.2261850456054,-4.55565657456957,
12.));
#185081=CARTESIAN_POINT('Ctrl Pts',(23.2090683793627,-4.54629140447543,
12.));
#185082=CARTESIAN_POINT('Ctrl Pts',(23.1920260146474,-4.53702729557586,
12.));
#185083=CARTESIAN_POINT('Ctrl Pts',(23.1750590180923,-4.52786428815049,
12.));
#185084=CARTESIAN_POINT('Ctrl Pts',(23.1581684708778,-4.51880242116786,
12.));
#185085=CARTESIAN_POINT('Ctrl Pts',(23.1413554691136,-4.50984173227088,
12.));
#185086=CARTESIAN_POINT('Ctrl Pts',(23.1246211242117,-4.5009822577518,12.));
#185087=CARTESIAN_POINT('Ctrl Pts',(23.1079665632629,-4.49222403252202,
12.));
#185088=CARTESIAN_POINT('Ctrl Pts',(23.0913929293909,-4.48356709006757,
12.));
#185089=CARTESIAN_POINT('Ctrl Pts',(23.0749013821867,-4.47501146242822,
12.));
#185090=CARTESIAN_POINT('Ctrl Pts',(23.0584930981723,-4.46655718018206,
12.));
#185091=CARTESIAN_POINT('Ctrl Pts',(23.0421692712466,-4.45820427241678,
12.));
#185092=CARTESIAN_POINT('Ctrl Pts',(23.0259311131395,-4.44995276669699,
12.));
#185093=CARTESIAN_POINT('Ctrl Pts',(23.0097798538399,-4.44180268901667,
12.));
#185094=CARTESIAN_POINT('Ctrl Pts',(22.9937167421009,-4.43375406376906,
12.));
#185095=CARTESIAN_POINT('Ctrl Pts',(22.9777430460021,-4.42580691372772,
12.));
#185096=CARTESIAN_POINT('Ctrl Pts',(22.9618600534866,-4.41796126001311,
12.));
#185097=CARTESIAN_POINT('Ctrl Pts',(22.9460690729092,-4.41021712205549,
12.));
#185098=CARTESIAN_POINT('Ctrl Pts',(22.9303714335549,-4.40257451754309,
12.));
#185099=CARTESIAN_POINT('Ctrl Pts',(22.9147684862425,-4.39503346238455,
12.));
#185100=CARTESIAN_POINT('Ctrl Pts',(22.8992616040108,-4.38759397068393,
12.));
#185101=CARTESIAN_POINT('Ctrl Pts',(22.8838521827702,-4.38025605470091,
12.));
#185102=CARTESIAN_POINT('Ctrl Pts',(22.8685416419725,-4.37301972480753,
12.));
#185103=CARTESIAN_POINT('Ctrl Pts',(22.8533314252419,-4.36588498943011,
12.));
#185104=CARTESIAN_POINT('Ctrl Pts',(22.838223001118,-4.3588518550056,12.));
#185105=CARTESIAN_POINT('Ctrl Pts',(22.8232178638873,-4.35192032594802,
12.));
#185106=CARTESIAN_POINT('Ctrl Pts',(22.808317534379,-4.34509040460066,12.));
#185107=CARTESIAN_POINT('Ctrl Pts',(22.7935235607807,-4.33836209118444,
12.));
#185108=CARTESIAN_POINT('Ctrl Pts',(22.7788375194081,-4.33173538373183,
12.));
#185109=CARTESIAN_POINT('Ctrl Pts',(22.764261015648,-4.32521027803748,12.));
#185110=CARTESIAN_POINT('Ctrl Pts',(22.7497956849852,-4.31878676761231,
12.));
#185111=CARTESIAN_POINT('Ctrl Pts',(22.7354431939926,-4.31246484362551,
12.));
#185112=CARTESIAN_POINT('Ctrl Pts',(22.7212052413384,-4.30624449484075,
12.));
#185113=CARTESIAN_POINT('Ctrl Pts',(22.707083558756,-4.30012570754067,12.));
#185114=CARTESIAN_POINT('Ctrl Pts',(22.6930799122545,-4.29410846547062,
12.));
#185115=CARTESIAN_POINT('Ctrl Pts',(22.6791961033536,-4.28819274977767,
12.));
#185116=CARTESIAN_POINT('Ctrl Pts',(22.665433970311,-4.2823785389406,12.));
#185117=CARTESIAN_POINT('Ctrl Pts',(22.6517953893303,-4.27666580869118,
12.));
#185118=CARTESIAN_POINT('Ctrl Pts',(22.6382822758171,-4.27105453193,12.));
#185119=CARTESIAN_POINT('Ctrl Pts',(22.6248965859975,-4.26554467865572,
12.));
#185120=CARTESIAN_POINT('Ctrl Pts',(22.611640318482,-4.26013621588304,12.));
#185121=CARTESIAN_POINT('Ctrl Pts',(22.5985155158637,-4.25482910755486,
12.));
#185122=CARTESIAN_POINT('Ctrl Pts',(22.5855242662479,-4.24962331444186,
12.));
#185123=CARTESIAN_POINT('Ctrl Pts',(22.5726687049922,-4.2445187940486,12.));
#185124=CARTESIAN_POINT('Ctrl Pts',(22.559951016643,-4.23951550052527,12.));
#185125=CARTESIAN_POINT('Ctrl Pts',(22.5473734368086,-4.23461338456714,
12.));
#185126=CARTESIAN_POINT('Ctrl Pts',(22.5349382540587,-4.22981239330733,
12.));
#185127=CARTESIAN_POINT('Ctrl Pts',(22.5226478117885,-4.22511247020041,
12.));
#185128=CARTESIAN_POINT('Ctrl Pts',(22.5105045108882,-4.22051355490198,
12.));
#185129=CARTESIAN_POINT('Ctrl Pts',(22.4985108124229,-4.21601558313909,
12.));
#185130=CARTESIAN_POINT('Ctrl Pts',(22.4866692403147,-4.21161848657429,
12.));
#185131=CARTESIAN_POINT('Ctrl Pts',(22.4749823839915,-4.20732219265649,
12.));
#185132=CARTESIAN_POINT('Ctrl Pts',(22.4634529011433,-4.20312662448172,
12.));
#185133=CARTESIAN_POINT('Ctrl Pts',(22.4520835205419,-4.19903170066356,
12.));
#185134=CARTESIAN_POINT('Ctrl Pts',(22.4408770448917,-4.19503733518862,
12.));
#185135=CARTESIAN_POINT('Ctrl Pts',(22.4298363535421,-4.19114343726943,
12.));
#185136=CARTESIAN_POINT('Ctrl Pts',(22.4189644056115,-4.18734991117722,
12.));
#185137=CARTESIAN_POINT('Ctrl Pts',(22.4082642454453,-4.18365665600852,
12.));
#185138=CARTESIAN_POINT('Ctrl Pts',(22.3977390078075,-4.18006356544883,
12.));
#185139=CARTESIAN_POINT('Ctrl Pts',(22.3873919231334,-4.17657052752826,
12.));
#185140=CARTESIAN_POINT('Ctrl Pts',(22.3772263228617,-4.17317742436146,
12.));
#185141=CARTESIAN_POINT('Ctrl Pts',(22.3672456427599,-4.16988413199458,
12.));
#185142=CARTESIAN_POINT('Ctrl Pts',(22.3574534257396,-4.16669052026601,
12.));
#185143=CARTESIAN_POINT('Ctrl Pts',(22.3478533253889,-4.16359645263189,
12.));
#185144=CARTESIAN_POINT('Ctrl Pts',(22.3384491078602,-4.16060178604165,
12.));
#185145=CARTESIAN_POINT('Ctrl Pts',(22.3292446628959,-4.15770637047891,
12.));
#185146=CARTESIAN_POINT('Ctrl Pts',(22.3202440186979,-4.15491004835282,
12.));
#185147=CARTESIAN_POINT('Ctrl Pts',(22.3114513545185,-4.15221265396991,
12.));
#185148=CARTESIAN_POINT('Ctrl Pts',(22.3028710166933,-4.14961401285523,
12.));
#185149=CARTESIAN_POINT('Ctrl Pts',(22.2945075198467,-4.14711394168557,
12.));
#185150=CARTESIAN_POINT('Ctrl Pts',(22.2863655389166,-4.14471224859297,
12.));
#185151=CARTESIAN_POINT('Ctrl Pts',(22.2784499072027,-4.14240873321985,
12.));
#185152=CARTESIAN_POINT('Ctrl Pts',(22.2707656042457,-4.14020318715992,
12.));
#185153=CARTESIAN_POINT('Ctrl Pts',(22.2633177913972,-4.13809539255423,
12.));
#185154=CARTESIAN_POINT('Ctrl Pts',(22.2561118708421,-4.13608511977227,
12.));
#185155=CARTESIAN_POINT('Ctrl Pts',(22.249153531779,-4.13417212558811,12.));
#185156=CARTESIAN_POINT('Ctrl Pts',(22.2424488153523,-4.13235615060161,
12.));
#185157=CARTESIAN_POINT('Ctrl Pts',(22.2360040565533,-4.13063692157499,
12.));
#185158=CARTESIAN_POINT('Ctrl Pts',(22.2298258043947,-4.1290141546338,12.));
#185159=CARTESIAN_POINT('Ctrl Pts',(22.2239207458781,-4.12748755830105,
12.));
#185160=CARTESIAN_POINT('Ctrl Pts',(22.2182956401341,-4.12605683613308,
12.));
#185161=CARTESIAN_POINT('Ctrl Pts',(22.2129576146671,-4.12472167516608,
12.));
#185162=CARTESIAN_POINT('Ctrl Pts',(22.2079143941719,-4.12348173702024,
12.));
#185163=CARTESIAN_POINT('Ctrl Pts',(22.2031746532106,-4.12233664408228,
12.));
#185164=CARTESIAN_POINT('Ctrl Pts',(22.1987479618246,-4.12128598183523,
12.));
#185165=CARTESIAN_POINT('Ctrl Pts',(22.1946440958098,-4.12032932637738,
12.));
#185166=CARTESIAN_POINT('Ctrl Pts',(22.1908725908525,-4.11946626228637,
12.));
#185167=CARTESIAN_POINT('Ctrl Pts',(22.1874419861496,-4.11869641271775,
12.));
#185168=CARTESIAN_POINT('Ctrl Pts',(22.1843613164855,-4.11801938107481,
12.));
#185169=CARTESIAN_POINT('Ctrl Pts',(22.1816414985788,-4.11743469691757,
12.));
#185170=CARTESIAN_POINT('Ctrl Pts',(22.179297473024,-4.11694173195005,12.));
#185171=CARTESIAN_POINT('Ctrl Pts',(22.177347426894,-4.11653973150519,12.));
#185172=CARTESIAN_POINT('Ctrl Pts',(22.1758088296598,-4.1162279721707,12.));
#185173=CARTESIAN_POINT('Ctrl Pts',(22.1746949858775,-4.11600589882846,
12.));
#185174=CARTESIAN_POINT('Ctrl Pts',(22.1741488021234,-4.11589976826168,
12.));
#185175=CARTESIAN_POINT('Ctrl Pts',(22.1739341411687,-4.11586035878288,
12.));
#185176=CARTESIAN_POINT('Ctrl Pts',(22.173877682324,-4.11585194677443,12.));
#185177=CARTESIAN_POINT('Ctrl Pts',(22.1738711152697,-4.11585220600463,
12.));
#185178=CARTESIAN_POINT('',(21.624941921198,-4.0139614976743,12.));
#185179=CARTESIAN_POINT('',(10.5694630535049,-1.96187429785751,12.));
#185180=CARTESIAN_POINT('',(21.2226420728916,-3.4423049612042,12.));
#185181=CARTESIAN_POINT('Origin',(21.7161918885402,-3.52235856495314,12.));
#185182=CARTESIAN_POINT('',(21.3904321633055,-2.1678126918683,12.));
#185183=CARTESIAN_POINT('Origin',(7.6920903736728E-13,-1.31973449697531E-13,
12.));
#185184=CARTESIAN_POINT('',(21.9269795755927,-1.71975774210843,12.));
#185185=CARTESIAN_POINT('Origin',(21.88788407408,-2.2182269405164,12.));
#185186=CARTESIAN_POINT('',(11.2417878583927,-0.881706102655892,12.));
#185187=CARTESIAN_POINT('Origin',(21.88788407408,-2.2182269405164,0.));
#185188=CARTESIAN_POINT('',(21.3904321633055,-2.1678126918683,0.));
#185189=CARTESIAN_POINT('',(21.9269795755927,-1.71975774210843,0.));
#185190=CARTESIAN_POINT('Origin',(21.88788407408,-2.2182269405164,0.));
#185191=CARTESIAN_POINT('',(21.9269795755927,-1.71975774210843,0.));
#185192=CARTESIAN_POINT('',(21.3904321633055,-2.1678126918683,0.));
#185193=CARTESIAN_POINT('Origin',(22.4835757167854,-1.76341220531181,0.));
#185194=CARTESIAN_POINT('',(22.4835757167854,-1.76341220531181,0.));
#185195=CARTESIAN_POINT('',(11.2417878583927,-0.881706102655892,0.));
#185196=CARTESIAN_POINT('',(22.4835757167854,-1.76341220531181,0.));
#185197=CARTESIAN_POINT('Origin',(21.7161918885402,-3.52235856495314,0.));
#185198=CARTESIAN_POINT('',(21.624941921198,-4.0139614976743,0.));
#185199=CARTESIAN_POINT('',(21.2226420728916,-3.4423049612042,0.));
#185200=CARTESIAN_POINT('Origin',(21.7161918885402,-3.52235856495314,0.));
#185201=CARTESIAN_POINT('',(21.2226420728916,-3.4423049612042,0.));
#185202=CARTESIAN_POINT('',(21.624941921198,-4.0139614976743,0.));
#185203=CARTESIAN_POINT('Origin',(7.6920903736728E-13,-1.31973449697531E-13,
0.));
#185204=CARTESIAN_POINT('Origin',(7.6920903736728E-13,-1.31973449697531E-13,
0.));
#185205=CARTESIAN_POINT('Origin',(20.56795313141,-7.80764394578304,0.));
#185206=CARTESIAN_POINT('',(20.1004996511507,-7.63019749246979,0.));
#185207=CARTESIAN_POINT('',(20.7347298079577,-7.33627833380047,0.));
#185208=CARTESIAN_POINT('Origin',(20.56795313141,-7.80764394578304,0.));
#185209=CARTESIAN_POINT('',(20.7347298079577,-7.33627833380047,0.));
#185210=CARTESIAN_POINT('',(20.1004996511507,-7.63019749246979,0.));
#185211=CARTESIAN_POINT('Origin',(21.2610617890679,-7.52250298901266,0.));
#185212=CARTESIAN_POINT('',(21.2610617890679,-7.52250298901266,0.));
#185213=CARTESIAN_POINT('',(10.6305308945339,-3.76125149450632,0.));
#185214=CARTESIAN_POINT('',(21.2610617890679,-7.52250298901266,0.));
#185215=CARTESIAN_POINT('Origin',(20.0645771135003,-9.02290115519382,0.));
#185216=CARTESIAN_POINT('',(19.84920021178,-9.47413589477549,0.));
#185217=CARTESIAN_POINT('',(19.6085639972844,-8.81783521984851,0.));
#185218=CARTESIAN_POINT('Origin',(20.0645771135003,-9.02290115519382,0.));
#185219=CARTESIAN_POINT('',(19.6085639972844,-8.81783521984851,0.));
#185220=CARTESIAN_POINT('',(19.84920021178,-9.47413589477549,0.));
#185221=CARTESIAN_POINT('Origin',(7.08841632778409E-13,-3.26562511982935E-13,
0.));
#185222=CARTESIAN_POINT('Origin',(7.08841632778409E-13,-3.26562511982935E-13,
0.));
#185223=CARTESIAN_POINT('Origin',(17.846350172984,-12.8649829188862,0.));
#185224=CARTESIAN_POINT('',(17.4407513054162,-12.572596943457,0.));
#185225=CARTESIAN_POINT('',(18.1294424696716,-12.4528436808172,0.));
#185226=CARTESIAN_POINT('Origin',(17.846350172984,-12.8649829188862,0.));
#185227=CARTESIAN_POINT('',(18.1294424696716,-12.4528436808172,0.));
#185228=CARTESIAN_POINT('',(17.4407513054162,-12.572596943457,0.));
#185229=CARTESIAN_POINT('Origin',(18.5896416359912,-12.7689476255363,0.));
#185230=CARTESIAN_POINT('',(18.5896416359912,-12.7689476255363,0.));
#185231=CARTESIAN_POINT('',(9.29482081799561,-6.38447381276812,0.));
#185232=CARTESIAN_POINT('',(18.5896416359912,-12.7689476255363,0.));
#185233=CARTESIAN_POINT('Origin',(17.0455945664569,-13.9085479427572,0.));
#185234=CARTESIAN_POINT('',(16.7207683102834,-14.2886635873976,0.));
#185235=CARTESIAN_POINT('',(16.6581946899465,-13.5924445804218,0.));
#185236=CARTESIAN_POINT('Origin',(17.0455945664569,-13.9085479427572,0.));
#185237=CARTESIAN_POINT('',(16.6581946899465,-13.5924445804218,0.));
#185238=CARTESIAN_POINT('',(16.7207683102834,-14.2886635873976,0.));
#185239=CARTESIAN_POINT('Origin',(6.00167842331873E-13,-4.9889687874677E-13,
0.));
#185240=CARTESIAN_POINT('Origin',(6.00167842331873E-13,-4.9889687874677E-13,
0.));
#185241=CARTESIAN_POINT('Origin',(13.9085479427572,-17.0455945664569,0.));
#185242=CARTESIAN_POINT('',(13.5924445804218,-16.6581946899465,0.));
#185243=CARTESIAN_POINT('',(14.2886635873976,-16.7207683102834,0.));
#185244=CARTESIAN_POINT('Origin',(13.9085479427572,-17.0455945664569,0.));
#185245=CARTESIAN_POINT('',(14.2886635873976,-16.7207683102834,0.));
#185246=CARTESIAN_POINT('',(13.5924445804218,-16.6581946899465,0.));
#185247=CARTESIAN_POINT('Origin',(14.6513681262571,-17.1452095830633,0.));
#185248=CARTESIAN_POINT('',(14.6513681262571,-17.1452095830633,0.));
#185249=CARTESIAN_POINT('',(7.32568406312854,-8.57260479153162,0.));
#185250=CARTESIAN_POINT('',(14.6513681262571,-17.1452095830633,0.));
#185251=CARTESIAN_POINT('Origin',(12.8649829188862,-17.846350172984,0.));
#185252=CARTESIAN_POINT('',(12.4528436808172,-18.1294424696716,0.));
#185253=CARTESIAN_POINT('',(12.572596943457,-17.4407513054162,0.));
#185254=CARTESIAN_POINT('Origin',(12.8649829188862,-17.846350172984,0.));
#185255=CARTESIAN_POINT('',(12.572596943457,-17.4407513054162,0.));
#185256=CARTESIAN_POINT('',(12.4528436808172,-18.1294424696716,0.));
#185257=CARTESIAN_POINT('Origin',(4.50593605254674E-13,-6.37232247690087E-13,
0.));
#185258=CARTESIAN_POINT('Origin',(4.50593605254674E-13,-6.37232247690087E-13,
0.));
#185259=CARTESIAN_POINT('Origin',(9.02290115519381,-20.0645771135004,0.));
#185260=CARTESIAN_POINT('',(8.81783521984849,-19.6085639972844,0.));
#185261=CARTESIAN_POINT('',(9.47413589477548,-19.84920021178,0.));
#185262=CARTESIAN_POINT('Origin',(9.02290115519381,-20.0645771135004,0.));
#185263=CARTESIAN_POINT('',(9.47413589477547,-19.84920021178,0.));
#185264=CARTESIAN_POINT('',(8.81783521984849,-19.6085639972844,0.));
#185265=CARTESIAN_POINT('Origin',(9.71462809124915,-20.353053841303,0.));
#185266=CARTESIAN_POINT('',(9.71462809124915,-20.353053841303,0.));
#185267=CARTESIAN_POINT('',(4.85731404562459,-10.1765269206515,0.));
#185268=CARTESIAN_POINT('',(9.71462809124915,-20.353053841303,0.));
#185269=CARTESIAN_POINT('Origin',(7.80764394578302,-20.56795313141,0.));
#185270=CARTESIAN_POINT('',(7.33627833380045,-20.7347298079577,0.));
#185271=CARTESIAN_POINT('',(7.63019749246977,-20.1004996511507,0.));
#185272=CARTESIAN_POINT('Origin',(7.80764394578302,-20.56795313141,0.));
#185273=CARTESIAN_POINT('',(7.63019749246977,-20.1004996511507,0.));
#185274=CARTESIAN_POINT('',(7.33627833380045,-20.7347298079577,0.));
#185275=CARTESIAN_POINT('Origin',(2.70312158620511E-13,-7.32141292029404E-13,
0.));
#185276=CARTESIAN_POINT('Origin',(2.70312158620511E-13,-7.32141292029404E-13,
0.));
#185277=CARTESIAN_POINT('Origin',(3.52235856495312,-21.7161918885403,0.));
#185278=CARTESIAN_POINT('',(3.44230496120418,-21.2226420728916,0.));
#185279=CARTESIAN_POINT('',(4.01396149767428,-21.624941921198,0.));
#185280=CARTESIAN_POINT('Origin',(3.52235856495312,-21.7161918885403,0.));
#185281=CARTESIAN_POINT('',(4.01396149767428,-21.624941921198,0.));
#185282=CARTESIAN_POINT('',(3.44230496120418,-21.2226420728916,0.));
#185283=CARTESIAN_POINT('Origin',(4.11585220600461,-22.1738711152697,0.));
#185284=CARTESIAN_POINT('',(4.11585220600461,-22.1738711152697,0.));
#185285=CARTESIAN_POINT('',(2.05792610300232,-11.0869355576349,0.));
#185286=CARTESIAN_POINT('',(4.11585220600461,-22.1738711152697,0.));
#185287=CARTESIAN_POINT('Origin',(2.21822694051637,-21.8878840740801,0.));
#185288=CARTESIAN_POINT('',(1.71975774210841,-21.9269795755927,0.));
#185289=CARTESIAN_POINT('',(2.16781269186827,-21.3904321633055,0.));
#185290=CARTESIAN_POINT('Origin',(2.21822694051637,-21.8878840740801,0.));
#185291=CARTESIAN_POINT('',(2.16781269186827,-21.3904321633055,0.));
#185292=CARTESIAN_POINT('',(1.71975774210841,-21.9269795755927,0.));
#185293=CARTESIAN_POINT('Origin',(7.16093850883225E-14,-7.7715611723761E-13,
0.));
#185294=CARTESIAN_POINT('Origin',(7.16093850883225E-14,-7.7715611723761E-13,
0.));
#185295=CARTESIAN_POINT('Origin',(-2.21822694051639,-21.88788407408,0.));
#185296=CARTESIAN_POINT('',(-2.16781269186829,-21.3904321633055,0.));
#185297=CARTESIAN_POINT('',(-1.71975774210843,-21.9269795755927,0.));
#185298=CARTESIAN_POINT('Origin',(-2.21822694051639,-21.88788407408,0.));
#185299=CARTESIAN_POINT('',(-1.71975774210843,-21.9269795755927,0.));
#185300=CARTESIAN_POINT('',(-2.16781269186829,-21.3904321633055,0.));
#185301=CARTESIAN_POINT('Origin',(-1.76341220531181,-22.4835757167854,0.));
#185302=CARTESIAN_POINT('',(-1.76341220531181,-22.4835757167854,0.));
#185303=CARTESIAN_POINT('',(-0.881706102655891,-11.2417878583927,0.));
#185304=CARTESIAN_POINT('',(-1.76341220531181,-22.4835757167854,0.));
#185305=CARTESIAN_POINT('Origin',(-3.52235856495314,-21.7161918885402,0.));
#185306=CARTESIAN_POINT('',(-4.0139614976743,-21.624941921198,0.));
#185307=CARTESIAN_POINT('',(-3.4423049612042,-21.2226420728916,0.));
#185308=CARTESIAN_POINT('Origin',(-3.52235856495314,-21.7161918885402,0.));
#185309=CARTESIAN_POINT('',(-3.4423049612042,-21.2226420728916,0.));
#185310=CARTESIAN_POINT('',(-4.0139614976743,-21.624941921198,0.));
#185311=CARTESIAN_POINT('Origin',(-1.31973449697531E-13,-7.6920903736728E-13,
0.));
#185312=CARTESIAN_POINT('Origin',(-1.31973449697531E-13,-7.6920903736728E-13,
0.));
#185313=CARTESIAN_POINT('Origin',(-7.80764394578304,-20.56795313141,0.));
#185314=CARTESIAN_POINT('',(-7.63019749246979,-20.1004996511507,0.));
#185315=CARTESIAN_POINT('',(-7.33627833380047,-20.7347298079577,0.));
#185316=CARTESIAN_POINT('Origin',(-7.80764394578304,-20.56795313141,0.));
#185317=CARTESIAN_POINT('',(-7.33627833380047,-20.7347298079577,0.));
#185318=CARTESIAN_POINT('',(-7.63019749246979,-20.1004996511507,0.));
#185319=CARTESIAN_POINT('Origin',(-7.52250298901266,-21.2610617890679,0.));
#185320=CARTESIAN_POINT('',(-7.52250298901266,-21.2610617890679,0.));
#185321=CARTESIAN_POINT('',(-3.76125149450632,-10.6305308945339,0.));
#185322=CARTESIAN_POINT('',(-7.52250298901266,-21.2610617890679,0.));
#185323=CARTESIAN_POINT('Origin',(-9.02290115519382,-20.0645771135003,0.));
#185324=CARTESIAN_POINT('',(-9.47413589477549,-19.84920021178,0.));
#185325=CARTESIAN_POINT('',(-8.81783521984851,-19.6085639972844,0.));
#185326=CARTESIAN_POINT('Origin',(-9.02290115519382,-20.0645771135003,0.));
#185327=CARTESIAN_POINT('',(-8.81783521984851,-19.6085639972844,0.));
#185328=CARTESIAN_POINT('',(-9.47413589477549,-19.84920021178,0.));
#185329=CARTESIAN_POINT('Origin',(-3.26562511982935E-13,-7.08841632778409E-13,
0.));
#185330=CARTESIAN_POINT('Origin',(-3.26562511982935E-13,-7.08841632778409E-13,
0.));
#185331=CARTESIAN_POINT('Origin',(-12.8649829188863,-17.846350172984,0.));
#185332=CARTESIAN_POINT('',(-12.572596943457,-17.4407513054161,0.));
#185333=CARTESIAN_POINT('',(-12.4528436808172,-18.1294424696716,0.));
#185334=CARTESIAN_POINT('Origin',(-12.8649829188863,-17.846350172984,0.));
#185335=CARTESIAN_POINT('',(-12.4528436808172,-18.1294424696716,0.));
#185336=CARTESIAN_POINT('',(-12.572596943457,-17.4407513054161,0.));
#185337=CARTESIAN_POINT('Origin',(-12.7689476255363,-18.5896416359912,0.));
#185338=CARTESIAN_POINT('',(-12.7689476255363,-18.5896416359912,0.));
#185339=CARTESIAN_POINT('',(-6.38447381276812,-9.29482081799561,0.));
#185340=CARTESIAN_POINT('',(-12.7689476255363,-18.5896416359912,0.));
#185341=CARTESIAN_POINT('Origin',(-13.9085479427572,-17.0455945664569,0.));
#185342=CARTESIAN_POINT('',(-14.2886635873976,-16.7207683102834,0.));
#185343=CARTESIAN_POINT('',(-13.5924445804218,-16.6581946899465,0.));
#185344=CARTESIAN_POINT('Origin',(-13.9085479427572,-17.0455945664569,0.));
#185345=CARTESIAN_POINT('',(-13.5924445804218,-16.6581946899465,0.));
#185346=CARTESIAN_POINT('',(-14.2886635873976,-16.7207683102834,0.));
#185347=CARTESIAN_POINT('Origin',(-4.9889687874677E-13,-6.00167842331873E-13,
0.));
#185348=CARTESIAN_POINT('Origin',(-4.9889687874677E-13,-6.00167842331873E-13,
0.));
#185349=CARTESIAN_POINT('Origin',(-17.0455945664569,-13.9085479427572,0.));
#185350=CARTESIAN_POINT('',(-16.6581946899465,-13.5924445804218,0.));
#185351=CARTESIAN_POINT('',(-16.7207683102834,-14.2886635873976,0.));
#185352=CARTESIAN_POINT('Origin',(-17.0455945664569,-13.9085479427572,0.));
#185353=CARTESIAN_POINT('',(-16.7207683102834,-14.2886635873976,0.));
#185354=CARTESIAN_POINT('',(-16.6581946899465,-13.5924445804218,0.));
#185355=CARTESIAN_POINT('Origin',(-17.1452095830633,-14.6513681262571,0.));
#185356=CARTESIAN_POINT('',(-17.1452095830633,-14.6513681262571,0.));
#185357=CARTESIAN_POINT('',(-8.57260479153162,-7.32568406312855,0.));
#185358=CARTESIAN_POINT('',(-17.1452095830633,-14.6513681262571,0.));
#185359=CARTESIAN_POINT('Origin',(-17.846350172984,-12.8649829188862,0.));
#185360=CARTESIAN_POINT('',(-18.1294424696716,-12.4528436808172,0.));
#185361=CARTESIAN_POINT('',(-17.4407513054162,-12.572596943457,0.));
#185362=CARTESIAN_POINT('Origin',(-17.846350172984,-12.8649829188862,0.));
#185363=CARTESIAN_POINT('',(-17.4407513054162,-12.572596943457,0.));
#185364=CARTESIAN_POINT('',(-18.1294424696716,-12.4528436808172,0.));
#185365=CARTESIAN_POINT('Origin',(-6.37232247690086E-13,-4.50593605254675E-13,
0.));
#185366=CARTESIAN_POINT('Origin',(-6.37232247690086E-13,-4.50593605254675E-13,
0.));
#185367=CARTESIAN_POINT('Origin',(-20.0645771135004,-9.0229011551938,0.));
#185368=CARTESIAN_POINT('',(-19.6085639972844,-8.81783521984849,0.));
#185369=CARTESIAN_POINT('',(-19.84920021178,-9.47413589477548,0.));
#185370=CARTESIAN_POINT('Origin',(-20.0645771135004,-9.0229011551938,0.));
#185371=CARTESIAN_POINT('',(-19.84920021178,-9.47413589477547,0.));
#185372=CARTESIAN_POINT('',(-19.6085639972844,-8.81783521984849,0.));
#185373=CARTESIAN_POINT('Origin',(-20.353053841303,-9.71462809124915,0.));
#185374=CARTESIAN_POINT('',(-20.353053841303,-9.71462809124915,0.));
#185375=CARTESIAN_POINT('',(-10.1765269206515,-4.85731404562459,0.));
#185376=CARTESIAN_POINT('',(-20.353053841303,-9.71462809124915,0.));
#185377=CARTESIAN_POINT('Origin',(-20.56795313141,-7.80764394578302,0.));
#185378=CARTESIAN_POINT('',(-20.7347298079577,-7.33627833380045,0.));
#185379=CARTESIAN_POINT('',(-20.1004996511507,-7.63019749246977,0.));
#185380=CARTESIAN_POINT('Origin',(-20.56795313141,-7.80764394578302,0.));
#185381=CARTESIAN_POINT('',(-20.1004996511507,-7.63019749246977,0.));
#185382=CARTESIAN_POINT('',(-20.7347298079577,-7.33627833380045,0.));
#185383=CARTESIAN_POINT('Origin',(-7.32141292029404E-13,-2.70312158620511E-13,
0.));
#185384=CARTESIAN_POINT('Origin',(-7.32141292029404E-13,-2.70312158620511E-13,
0.));
#185385=CARTESIAN_POINT('Origin',(-21.7161918885403,-3.52235856495312,0.));
#185386=CARTESIAN_POINT('',(-21.2226420728916,-3.44230496120418,0.));
#185387=CARTESIAN_POINT('',(-21.624941921198,-4.01396149767428,0.));
#185388=CARTESIAN_POINT('Origin',(-21.7161918885403,-3.52235856495312,0.));
#185389=CARTESIAN_POINT('',(-21.624941921198,-4.01396149767428,0.));
#185390=CARTESIAN_POINT('',(-21.2226420728916,-3.44230496120418,0.));
#185391=CARTESIAN_POINT('Origin',(-22.1738711152697,-4.11585220600461,0.));
#185392=CARTESIAN_POINT('',(-22.1738711152697,-4.11585220600461,0.));
#185393=CARTESIAN_POINT('',(-11.0869355576349,-2.05792610300232,0.));
#185394=CARTESIAN_POINT('',(-22.1738711152697,-4.11585220600461,0.));
#185395=CARTESIAN_POINT('Origin',(-21.8878840740801,-2.21822694051637,0.));
#185396=CARTESIAN_POINT('',(-21.9269795755927,-1.71975774210841,0.));
#185397=CARTESIAN_POINT('',(-21.3904321633055,-2.16781269186828,0.));
#185398=CARTESIAN_POINT('Origin',(-21.8878840740801,-2.21822694051637,0.));
#185399=CARTESIAN_POINT('',(-21.3904321633055,-2.16781269186827,0.));
#185400=CARTESIAN_POINT('',(-21.9269795755927,-1.71975774210841,0.));
#185401=CARTESIAN_POINT('Origin',(-7.7715611723761E-13,-7.16093850883225E-14,
0.));
#185402=CARTESIAN_POINT('Origin',(-7.7715611723761E-13,-7.16093850883225E-14,
0.));
#185403=CARTESIAN_POINT('Origin',(-21.8878840740801,2.21822694051638,0.));
#185404=CARTESIAN_POINT('',(-21.3904321633055,2.16781269186828,0.));
#185405=CARTESIAN_POINT('',(-21.9269795755927,1.71975774210842,0.));
#185406=CARTESIAN_POINT('Origin',(-21.8878840740801,2.21822694051638,0.));
#185407=CARTESIAN_POINT('',(-21.9269795755927,1.71975774210842,0.));
#185408=CARTESIAN_POINT('',(-21.3904321633055,2.16781269186828,0.));
#185409=CARTESIAN_POINT('Origin',(-22.4835757167854,1.7634122053118,0.));
#185410=CARTESIAN_POINT('',(-22.4835757167854,1.7634122053118,0.));
#185411=CARTESIAN_POINT('',(-11.2417878583927,0.881706102655883,0.));
#185412=CARTESIAN_POINT('',(-22.4835757167854,1.7634122053118,0.));
#185413=CARTESIAN_POINT('Origin',(-21.7161918885402,3.52235856495312,0.));
#185414=CARTESIAN_POINT('',(-21.624941921198,4.01396149767429,0.));
#185415=CARTESIAN_POINT('',(-21.2226420728916,3.44230496120419,0.));
#185416=CARTESIAN_POINT('Origin',(-21.7161918885402,3.52235856495312,0.));
#185417=CARTESIAN_POINT('',(-21.2226420728916,3.44230496120419,0.));
#185418=CARTESIAN_POINT('',(-21.624941921198,4.01396149767429,0.));
#185419=CARTESIAN_POINT('Origin',(-7.6920903736728E-13,1.31973449697531E-13,
0.));
#185420=CARTESIAN_POINT('Origin',(-7.6920903736728E-13,1.31973449697531E-13,
0.));
#185421=CARTESIAN_POINT('Origin',(-20.56795313141,7.80764394578303,0.));
#185422=CARTESIAN_POINT('',(-20.1004996511507,7.63019749246978,0.));
#185423=CARTESIAN_POINT('',(-20.7347298079577,7.33627833380047,0.));
#185424=CARTESIAN_POINT('Origin',(-20.56795313141,7.80764394578303,0.));
#185425=CARTESIAN_POINT('',(-20.7347298079577,7.33627833380047,0.));
#185426=CARTESIAN_POINT('',(-20.1004996511507,7.63019749246978,0.));
#185427=CARTESIAN_POINT('Origin',(-21.2610617890679,7.52250298901265,0.));
#185428=CARTESIAN_POINT('',(-21.2610617890679,7.52250298901265,0.));
#185429=CARTESIAN_POINT('',(-10.6305308945339,3.76125149450631,0.));
#185430=CARTESIAN_POINT('',(-21.2610617890679,7.52250298901265,0.));
#185431=CARTESIAN_POINT('Origin',(-20.0645771135003,9.02290115519382,0.));
#185432=CARTESIAN_POINT('',(-19.84920021178,9.47413589477549,0.));
#185433=CARTESIAN_POINT('',(-19.6085639972844,8.81783521984851,0.));
#185434=CARTESIAN_POINT('Origin',(-20.0645771135003,9.02290115519382,0.));
#185435=CARTESIAN_POINT('',(-19.6085639972844,8.81783521984851,0.));
#185436=CARTESIAN_POINT('',(-19.84920021178,9.47413589477549,0.));
#185437=CARTESIAN_POINT('Origin',(-7.08841632778408E-13,3.26562511982935E-13,
0.));
#185438=CARTESIAN_POINT('Origin',(-7.08841632778408E-13,3.26562511982935E-13,
0.));
#185439=CARTESIAN_POINT('Origin',(-17.846350172984,12.8649829188862,0.));
#185440=CARTESIAN_POINT('',(-17.4407513054162,12.572596943457,0.));
#185441=CARTESIAN_POINT('',(-18.1294424696716,12.4528436808172,0.));
#185442=CARTESIAN_POINT('Origin',(-17.846350172984,12.8649829188862,0.));
#185443=CARTESIAN_POINT('',(-18.1294424696716,12.4528436808172,0.));
#185444=CARTESIAN_POINT('',(-17.4407513054162,12.572596943457,0.));
#185445=CARTESIAN_POINT('Origin',(-18.5896416359912,12.7689476255363,0.));
#185446=CARTESIAN_POINT('',(-18.5896416359912,12.7689476255363,0.));
#185447=CARTESIAN_POINT('',(-9.29482081799561,6.38447381276812,0.));
#185448=CARTESIAN_POINT('',(-18.5896416359912,12.7689476255363,0.));
#185449=CARTESIAN_POINT('Origin',(-17.0455945664569,13.9085479427572,0.));
#185450=CARTESIAN_POINT('',(-16.7207683102834,14.2886635873976,0.));
#185451=CARTESIAN_POINT('',(-16.6581946899465,13.5924445804218,0.));
#185452=CARTESIAN_POINT('Origin',(-17.0455945664569,13.9085479427572,0.));
#185453=CARTESIAN_POINT('',(-16.6581946899465,13.5924445804218,0.));
#185454=CARTESIAN_POINT('',(-16.7207683102834,14.2886635873976,0.));
#185455=CARTESIAN_POINT('Origin',(-6.00167842331873E-13,4.9889687874677E-13,
0.));
#185456=CARTESIAN_POINT('Origin',(-6.00167842331873E-13,4.9889687874677E-13,
0.));
#185457=CARTESIAN_POINT('Origin',(-13.9085479427572,17.0455945664569,0.));
#185458=CARTESIAN_POINT('',(-13.5924445804218,16.6581946899465,0.));
#185459=CARTESIAN_POINT('',(-14.2886635873976,16.7207683102834,0.));
#185460=CARTESIAN_POINT('Origin',(-13.9085479427572,17.0455945664569,0.));
#185461=CARTESIAN_POINT('',(-14.2886635873976,16.7207683102834,0.));
#185462=CARTESIAN_POINT('',(-13.5924445804218,16.6581946899465,0.));
#185463=CARTESIAN_POINT('Origin',(-14.6513681262571,17.1452095830633,0.));
#185464=CARTESIAN_POINT('',(-14.6513681262571,17.1452095830633,0.));
#185465=CARTESIAN_POINT('',(-7.32568406312854,8.57260479153162,0.));
#185466=CARTESIAN_POINT('',(-14.6513681262571,17.1452095830633,0.));
#185467=CARTESIAN_POINT('Origin',(-12.8649829188862,17.846350172984,0.));
#185468=CARTESIAN_POINT('',(-12.4528436808172,18.1294424696716,0.));
#185469=CARTESIAN_POINT('',(-12.572596943457,17.4407513054162,0.));
#185470=CARTESIAN_POINT('Origin',(-12.8649829188862,17.846350172984,0.));
#185471=CARTESIAN_POINT('',(-12.572596943457,17.4407513054162,0.));
#185472=CARTESIAN_POINT('',(-12.4528436808172,18.1294424696716,0.));
#185473=CARTESIAN_POINT('Origin',(-4.50593605254675E-13,6.37232247690086E-13,
0.));
#185474=CARTESIAN_POINT('Origin',(-4.50593605254675E-13,6.37232247690086E-13,
0.));
#185475=CARTESIAN_POINT('Origin',(-9.02290115519381,20.0645771135003,0.));
#185476=CARTESIAN_POINT('',(-8.8178352198485,19.6085639972844,0.));
#185477=CARTESIAN_POINT('',(-9.47413589477548,19.84920021178,0.));
#185478=CARTESIAN_POINT('Origin',(-9.02290115519381,20.0645771135003,0.));
#185479=CARTESIAN_POINT('',(-9.47413589477548,19.84920021178,0.));
#185480=CARTESIAN_POINT('',(-8.8178352198485,19.6085639972844,0.));
#185481=CARTESIAN_POINT('Origin',(-9.71462809124916,20.353053841303,0.));
#185482=CARTESIAN_POINT('',(-9.71462809124916,20.353053841303,0.));
#185483=CARTESIAN_POINT('',(-4.85731404562459,10.1765269206515,0.));
#185484=CARTESIAN_POINT('',(-9.71462809124916,20.353053841303,0.));
#185485=CARTESIAN_POINT('Origin',(-7.80764394578302,20.56795313141,0.));
#185486=CARTESIAN_POINT('',(-7.33627833380046,20.7347298079577,0.));
#185487=CARTESIAN_POINT('',(-7.63019749246977,20.1004996511507,0.));
#185488=CARTESIAN_POINT('Origin',(-7.80764394578302,20.56795313141,0.));
#185489=CARTESIAN_POINT('',(-7.63019749246977,20.1004996511507,0.));
#185490=CARTESIAN_POINT('',(-7.33627833380046,20.7347298079577,0.));
#185491=CARTESIAN_POINT('Origin',(-2.70312158620511E-13,7.32141292029404E-13,
0.));
#185492=CARTESIAN_POINT('Origin',(-2.70312158620511E-13,7.32141292029404E-13,
0.));
#185493=CARTESIAN_POINT('Origin',(-3.52235856495312,21.7161918885402,0.));
#185494=CARTESIAN_POINT('',(-3.44230496120418,21.2226420728916,0.));
#185495=CARTESIAN_POINT('',(-4.01396149767428,21.624941921198,0.));
#185496=CARTESIAN_POINT('Origin',(-3.52235856495312,21.7161918885402,0.));
#185497=CARTESIAN_POINT('',(-4.01396149767428,21.624941921198,0.));
#185498=CARTESIAN_POINT('',(-3.44230496120418,21.2226420728916,0.));
#185499=CARTESIAN_POINT('Origin',(-4.11585220600461,22.1738711152697,0.));
#185500=CARTESIAN_POINT('',(-4.11585220600461,22.1738711152697,0.));
#185501=CARTESIAN_POINT('',(-2.05792610300232,11.0869355576349,0.));
#185502=CARTESIAN_POINT('',(-4.11585220600461,22.1738711152697,0.));
#185503=CARTESIAN_POINT('Origin',(-2.21822694051637,21.8878840740801,0.));
#185504=CARTESIAN_POINT('',(-1.71975774210841,21.9269795755927,0.));
#185505=CARTESIAN_POINT('',(-2.16781269186828,21.3904321633055,0.));
#185506=CARTESIAN_POINT('Origin',(-2.21822694051637,21.8878840740801,0.));
#185507=CARTESIAN_POINT('',(-2.16781269186828,21.3904321633055,0.));
#185508=CARTESIAN_POINT('',(-1.71975774210841,21.9269795755927,0.));
#185509=CARTESIAN_POINT('Origin',(-7.16093850883226E-14,7.7715611723761E-13,
0.));
#185510=CARTESIAN_POINT('Origin',(-7.16093850883226E-14,7.7715611723761E-13,
0.));
#185511=CARTESIAN_POINT('Origin',(2.21822694051638,21.8878840740801,0.));
#185512=CARTESIAN_POINT('',(2.16781269186828,21.3904321633055,0.));
#185513=CARTESIAN_POINT('',(1.71975774210842,21.9269795755927,0.));
#185514=CARTESIAN_POINT('Origin',(2.21822694051638,21.8878840740801,0.));
#185515=CARTESIAN_POINT('',(1.71975774210842,21.9269795755927,0.));
#185516=CARTESIAN_POINT('',(2.16781269186828,21.3904321633055,0.));
#185517=CARTESIAN_POINT('Origin',(1.7634122053118,22.4835757167854,0.));
#185518=CARTESIAN_POINT('',(1.7634122053118,22.4835757167854,0.));
#185519=CARTESIAN_POINT('',(0.881706102655883,11.2417878583927,0.));
#185520=CARTESIAN_POINT('',(1.7634122053118,22.4835757167854,0.));
#185521=CARTESIAN_POINT('Origin',(3.52235856495312,21.7161918885402,0.));
#185522=CARTESIAN_POINT('',(4.01396149767429,21.624941921198,0.));
#185523=CARTESIAN_POINT('',(3.44230496120419,21.2226420728916,0.));
#185524=CARTESIAN_POINT('Origin',(3.52235856495312,21.7161918885402,0.));
#185525=CARTESIAN_POINT('',(3.44230496120419,21.2226420728916,0.));
#185526=CARTESIAN_POINT('',(4.01396149767429,21.624941921198,0.));
#185527=CARTESIAN_POINT('Origin',(1.31973449697531E-13,7.6920903736728E-13,
0.));
#185528=CARTESIAN_POINT('Origin',(1.31973449697531E-13,7.6920903736728E-13,
0.));
#185529=CARTESIAN_POINT('Origin',(7.80764394578303,20.56795313141,0.));
#185530=CARTESIAN_POINT('',(7.63019749246978,20.1004996511507,0.));
#185531=CARTESIAN_POINT('',(7.33627833380047,20.7347298079577,0.));
#185532=CARTESIAN_POINT('Origin',(7.80764394578303,20.56795313141,0.));
#185533=CARTESIAN_POINT('',(7.33627833380046,20.7347298079577,0.));
#185534=CARTESIAN_POINT('',(7.63019749246978,20.1004996511507,0.));
#185535=CARTESIAN_POINT('Origin',(7.52250298901265,21.2610617890679,0.));
#185536=CARTESIAN_POINT('',(7.52250298901265,21.2610617890679,0.));
#185537=CARTESIAN_POINT('',(3.76125149450631,10.6305308945339,0.));
#185538=CARTESIAN_POINT('',(7.52250298901265,21.2610617890679,0.));
#185539=CARTESIAN_POINT('Origin',(9.02290115519382,20.0645771135003,0.));
#185540=CARTESIAN_POINT('',(9.47413589477549,19.84920021178,0.));
#185541=CARTESIAN_POINT('',(8.8178352198485,19.6085639972844,0.));
#185542=CARTESIAN_POINT('Origin',(9.02290115519382,20.0645771135003,0.));
#185543=CARTESIAN_POINT('',(8.8178352198485,19.6085639972844,0.));
#185544=CARTESIAN_POINT('',(9.47413589477549,19.84920021178,0.));
#185545=CARTESIAN_POINT('Origin',(3.26562511982935E-13,7.08841632778409E-13,
0.));
#185546=CARTESIAN_POINT('Origin',(3.26562511982935E-13,7.08841632778409E-13,
0.));
#185547=CARTESIAN_POINT('Origin',(12.8649829188862,17.846350172984,0.));
#185548=CARTESIAN_POINT('',(12.572596943457,17.4407513054162,0.));
#185549=CARTESIAN_POINT('',(12.4528436808172,18.1294424696716,0.));
#185550=CARTESIAN_POINT('Origin',(12.8649829188862,17.846350172984,0.));
#185551=CARTESIAN_POINT('',(12.4528436808172,18.1294424696716,0.));
#185552=CARTESIAN_POINT('',(12.572596943457,17.4407513054162,0.));
#185553=CARTESIAN_POINT('Origin',(12.7689476255363,18.5896416359912,0.));
#185554=CARTESIAN_POINT('',(12.7689476255363,18.5896416359912,0.));
#185555=CARTESIAN_POINT('',(6.38447381276812,9.29482081799561,0.));
#185556=CARTESIAN_POINT('',(12.7689476255363,18.5896416359912,0.));
#185557=CARTESIAN_POINT('Origin',(13.9085479427572,17.0455945664569,0.));
#185558=CARTESIAN_POINT('',(14.2886635873976,16.7207683102834,0.));
#185559=CARTESIAN_POINT('',(13.5924445804218,16.6581946899465,0.));
#185560=CARTESIAN_POINT('Origin',(13.9085479427572,17.0455945664569,0.));
#185561=CARTESIAN_POINT('',(13.5924445804218,16.6581946899465,0.));
#185562=CARTESIAN_POINT('',(14.2886635873976,16.7207683102834,0.));
#185563=CARTESIAN_POINT('Origin',(4.9889687874677E-13,6.00167842331873E-13,
0.));
#185564=CARTESIAN_POINT('Origin',(4.9889687874677E-13,6.00167842331873E-13,
0.));
#185565=CARTESIAN_POINT('Origin',(17.0455945664569,13.9085479427572,0.));
#185566=CARTESIAN_POINT('',(16.6581946899465,13.5924445804218,0.));
#185567=CARTESIAN_POINT('',(16.7207683102834,14.2886635873976,0.));
#185568=CARTESIAN_POINT('Origin',(17.0455945664569,13.9085479427572,0.));
#185569=CARTESIAN_POINT('',(16.7207683102834,14.2886635873976,0.));
#185570=CARTESIAN_POINT('',(16.6581946899465,13.5924445804218,0.));
#185571=CARTESIAN_POINT('Origin',(17.1452095830633,14.6513681262571,0.));
#185572=CARTESIAN_POINT('',(17.1452095830633,14.6513681262571,0.));
#185573=CARTESIAN_POINT('',(8.57260479153162,7.32568406312855,0.));
#185574=CARTESIAN_POINT('',(17.1452095830633,14.6513681262571,0.));
#185575=CARTESIAN_POINT('Origin',(17.846350172984,12.8649829188862,0.));
#185576=CARTESIAN_POINT('',(18.1294424696716,12.4528436808172,0.));
#185577=CARTESIAN_POINT('',(17.4407513054162,12.572596943457,0.));
#185578=CARTESIAN_POINT('Origin',(17.846350172984,12.8649829188862,0.));
#185579=CARTESIAN_POINT('',(17.4407513054162,12.572596943457,0.));
#185580=CARTESIAN_POINT('',(18.1294424696716,12.4528436808172,0.));
#185581=CARTESIAN_POINT('Origin',(6.37232247690086E-13,4.50593605254675E-13,
0.));
#185582=CARTESIAN_POINT('Origin',(6.37232247690086E-13,4.50593605254675E-13,
0.));
#185583=CARTESIAN_POINT('Origin',(20.0645771135003,9.02290115519381,0.));
#185584=CARTESIAN_POINT('',(19.6085639972844,8.8178352198485,0.));
#185585=CARTESIAN_POINT('',(19.84920021178,9.47413589477548,0.));
#185586=CARTESIAN_POINT('Origin',(20.0645771135003,9.02290115519381,0.));
#185587=CARTESIAN_POINT('',(19.84920021178,9.47413589477548,0.));
#185588=CARTESIAN_POINT('',(19.6085639972844,8.8178352198485,0.));
#185589=CARTESIAN_POINT('Origin',(20.353053841303,9.71462809124916,0.));
#185590=CARTESIAN_POINT('',(20.353053841303,9.71462809124916,0.));
#185591=CARTESIAN_POINT('',(10.1765269206515,4.85731404562459,0.));
#185592=CARTESIAN_POINT('',(20.353053841303,9.71462809124916,0.));
#185593=CARTESIAN_POINT('Origin',(20.56795313141,7.80764394578302,0.));
#185594=CARTESIAN_POINT('',(20.7347298079577,7.33627833380046,0.));
#185595=CARTESIAN_POINT('',(20.1004996511507,7.63019749246977,0.));
#185596=CARTESIAN_POINT('Origin',(20.56795313141,7.80764394578302,0.));
#185597=CARTESIAN_POINT('',(20.1004996511507,7.63019749246977,0.));
#185598=CARTESIAN_POINT('',(20.7347298079577,7.33627833380046,0.));
#185599=CARTESIAN_POINT('Origin',(7.32141292029404E-13,2.70312158620511E-13,
0.));
#185600=CARTESIAN_POINT('Origin',(7.32141292029404E-13,2.70312158620511E-13,
0.));
#185601=CARTESIAN_POINT('Origin',(21.1389261070099,-3.92374859571502,0.));
#185602=CARTESIAN_POINT('',(22.1738711152697,-4.11585220600463,0.));
#185603=CARTESIAN_POINT('',(22.1738711152697,-4.11585220600463,0.));
#185604=CARTESIAN_POINT('',(10.5694630535049,-1.96187429785751,0.));
#185605=CARTESIAN_POINT('Ctrl Pts',(25.991588367311,-0.661312440730916,
0.));
#185606=CARTESIAN_POINT('Ctrl Pts',(25.991588367311,-0.661312440730916,
12.));
#185607=CARTESIAN_POINT('Ctrl Pts',(25.9865613464773,-0.66402831318764,
0.));
#185608=CARTESIAN_POINT('Ctrl Pts',(25.9865613464773,-0.66402831318764,
12.));
#185609=CARTESIAN_POINT('Ctrl Pts',(25.9765104298071,-0.669451306780839,
0.));
#185610=CARTESIAN_POINT('Ctrl Pts',(25.9765104298071,-0.669451306780839,
12.));
#185611=CARTESIAN_POINT('Ctrl Pts',(25.9614434297919,-0.67755954320974,
0.));
#185612=CARTESIAN_POINT('Ctrl Pts',(25.9614434297919,-0.67755954320974,
12.));
#185613=CARTESIAN_POINT('Ctrl Pts',(25.9413728471909,-0.688318015057744,
0.));
#185614=CARTESIAN_POINT('Ctrl Pts',(25.9413728471909,-0.688318015057744,
12.));
#185615=CARTESIAN_POINT('Ctrl Pts',(25.9163158909426,-0.701678575228769,
0.));
#185616=CARTESIAN_POINT('Ctrl Pts',(25.9163158909426,-0.701678575228769,
12.));
#185617=CARTESIAN_POINT('Ctrl Pts',(25.8912902614969,-0.714951588527653,
0.));
#185618=CARTESIAN_POINT('Ctrl Pts',(25.8912902614969,-0.714951588527653,
12.));
#185619=CARTESIAN_POINT('Ctrl Pts',(25.8662960624185,-0.728137036482349,
0.));
#185620=CARTESIAN_POINT('Ctrl Pts',(25.8662960624185,-0.728137036482349,
12.));
#185621=CARTESIAN_POINT('Ctrl Pts',(25.8413334619054,-0.74123490266382,
0.));
#185622=CARTESIAN_POINT('Ctrl Pts',(25.8413334619054,-0.74123490266382,
12.));
#185623=CARTESIAN_POINT('Ctrl Pts',(25.8164027059984,-0.754245175609537,
0.));
#185624=CARTESIAN_POINT('Ctrl Pts',(25.8164027059984,-0.754245175609537,
12.));
#185625=CARTESIAN_POINT('Ctrl Pts',(25.7915041383376,-0.767167852651183,
0.));
#185626=CARTESIAN_POINT('Ctrl Pts',(25.7915041383376,-0.767167852651183,
12.));
#185627=CARTESIAN_POINT('Ctrl Pts',(25.7666381946955,-0.780002940291977,
0.));
#185628=CARTESIAN_POINT('Ctrl Pts',(25.7666381946955,-0.780002940291977,
12.));
#185629=CARTESIAN_POINT('Ctrl Pts',(25.7418053757746,-0.79275045161614,
0.));
#185630=CARTESIAN_POINT('Ctrl Pts',(25.7418053757746,-0.79275045161614,
12.));
#185631=CARTESIAN_POINT('Ctrl Pts',(25.7170062262525,-0.805410404554366,
0.));
#185632=CARTESIAN_POINT('Ctrl Pts',(25.7170062262525,-0.805410404554366,
12.));
#185633=CARTESIAN_POINT('Ctrl Pts',(25.6922413110194,-0.817982819787478,
0.));
#185634=CARTESIAN_POINT('Ctrl Pts',(25.6922413110194,-0.817982819787478,
12.));
#185635=CARTESIAN_POINT('Ctrl Pts',(25.6675111931952,-0.830467718864221,
0.));
#185636=CARTESIAN_POINT('Ctrl Pts',(25.6675111931952,-0.830467718864221,
12.));
#185637=CARTESIAN_POINT('Ctrl Pts',(25.6428164100055,-0.842865122120773,
0.));
#185638=CARTESIAN_POINT('Ctrl Pts',(25.6428164100055,-0.842865122120773,
12.));
#185639=CARTESIAN_POINT('Ctrl Pts',(25.6181574536049,-0.855175047036563,
0.));
#185640=CARTESIAN_POINT('Ctrl Pts',(25.6181574536049,-0.855175047036563,
12.));
#185641=CARTESIAN_POINT('Ctrl Pts',(25.5935347843585,-0.867397509338443,
0.));
#185642=CARTESIAN_POINT('Ctrl Pts',(25.5935347843585,-0.867397509338443,
12.));
#185643=CARTESIAN_POINT('Ctrl Pts',(25.5689488408156,-0.879532523834308,
0.));
#185644=CARTESIAN_POINT('Ctrl Pts',(25.5689488408156,-0.879532523834308,
12.));
#185645=CARTESIAN_POINT('Ctrl Pts',(25.5444000508211,-0.891580105349052,
0.));
#185646=CARTESIAN_POINT('Ctrl Pts',(25.5444000508211,-0.891580105349052,
12.));
#185647=CARTESIAN_POINT('Ctrl Pts',(25.5198888424194,-0.903540269651121,
0.));
#185648=CARTESIAN_POINT('Ctrl Pts',(25.5198888424194,-0.903540269651121,
12.));
#185649=CARTESIAN_POINT('Ctrl Pts',(25.4954156541795,-0.915413034335626,
0.));
#185650=CARTESIAN_POINT('Ctrl Pts',(25.4954156541795,-0.915413034335626,
12.));
#185651=CARTESIAN_POINT('Ctrl Pts',(25.4709809475009,-0.927198419886108,
0.));
#185652=CARTESIAN_POINT('Ctrl Pts',(25.4709809475009,-0.927198419886108,
12.));
#185653=CARTESIAN_POINT('Ctrl Pts',(25.4465852044849,-0.938896449496205,
0.));
#185654=CARTESIAN_POINT('Ctrl Pts',(25.4465852044849,-0.938896449496205,
12.));
#185655=CARTESIAN_POINT('Ctrl Pts',(25.4222289223167,-0.950507148597483,
0.));
#185656=CARTESIAN_POINT('Ctrl Pts',(25.4222289223167,-0.950507148597483,
12.));
#185657=CARTESIAN_POINT('Ctrl Pts',(25.3979126089163,-0.962030544503156,
0.));
#185658=CARTESIAN_POINT('Ctrl Pts',(25.3979126089163,-0.962030544503156,
12.));
#185659=CARTESIAN_POINT('Ctrl Pts',(25.3736367778845,-0.973466666000178,
0.));
#185660=CARTESIAN_POINT('Ctrl Pts',(25.3736367778845,-0.973466666000178,
12.));
#185661=CARTESIAN_POINT('Ctrl Pts',(25.3494019441441,-0.984815543003986,
0.));
#185662=CARTESIAN_POINT('Ctrl Pts',(25.3494019441441,-0.984815543003986,
12.));
#185663=CARTESIAN_POINT('Ctrl Pts',(25.3252086182968,-0.996077206120637,
0.));
#185664=CARTESIAN_POINT('Ctrl Pts',(25.3252086182968,-0.996077206120637,
12.));
#185665=CARTESIAN_POINT('Ctrl Pts',(25.3010573055547,-1.00725168656897,
0.));
#185666=CARTESIAN_POINT('Ctrl Pts',(25.3010573055547,-1.00725168656897,
12.));
#185667=CARTESIAN_POINT('Ctrl Pts',(25.276948508726,-1.01833901642238,0.));
#185668=CARTESIAN_POINT('Ctrl Pts',(25.276948508726,-1.01833901642238,12.));
#185669=CARTESIAN_POINT('Ctrl Pts',(25.2528827300422,-1.02933922876807,
0.));
#185670=CARTESIAN_POINT('Ctrl Pts',(25.2528827300422,-1.02933922876807,
12.));
#185671=CARTESIAN_POINT('Ctrl Pts',(25.2288604735086,-1.04025235791508,
0.));
#185672=CARTESIAN_POINT('Ctrl Pts',(25.2288604735086,-1.04025235791508,
12.));
#185673=CARTESIAN_POINT('Ctrl Pts',(25.2048822469028,-1.05107843957933,
0.));
#185674=CARTESIAN_POINT('Ctrl Pts',(25.2048822469028,-1.05107843957933,
12.));
#185675=CARTESIAN_POINT('Ctrl Pts',(25.1809485642192,-1.06181751111769,
0.));
#185676=CARTESIAN_POINT('Ctrl Pts',(25.1809485642192,-1.06181751111769,
12.));
#185677=CARTESIAN_POINT('Ctrl Pts',(25.157059946931,-1.07246961165477,0.));
#185678=CARTESIAN_POINT('Ctrl Pts',(25.157059946931,-1.07246961165477,12.));
#185679=CARTESIAN_POINT('Ctrl Pts',(25.1332169227413,-1.08303478197189,
0.));
#185680=CARTESIAN_POINT('Ctrl Pts',(25.1332169227413,-1.08303478197189,
12.));
#185681=CARTESIAN_POINT('Ctrl Pts',(25.1094200248446,-1.09351306445309,
0.));
#185682=CARTESIAN_POINT('Ctrl Pts',(25.1094200248446,-1.09351306445309,
12.));
#185683=CARTESIAN_POINT('Ctrl Pts',(25.0856697909679,-1.10390450301747,
0.));
#185684=CARTESIAN_POINT('Ctrl Pts',(25.0856697909679,-1.10390450301747,
12.));
#185685=CARTESIAN_POINT('Ctrl Pts',(25.0619667625336,-1.11420914306891,
0.));
#185686=CARTESIAN_POINT('Ctrl Pts',(25.0619667625336,-1.11420914306891,
12.));
#185687=CARTESIAN_POINT('Ctrl Pts',(25.0383114836899,-1.12442703144453,
0.));
#185688=CARTESIAN_POINT('Ctrl Pts',(25.0383114836899,-1.12442703144453,
12.));
#185689=CARTESIAN_POINT('Ctrl Pts',(25.0147045006195,-1.13455821638531,
0.));
#185690=CARTESIAN_POINT('Ctrl Pts',(25.0147045006195,-1.13455821638531,
12.));
#185691=CARTESIAN_POINT('Ctrl Pts',(24.9911463621433,-1.14460274758202,
0.));
#185692=CARTESIAN_POINT('Ctrl Pts',(24.9911463621433,-1.14460274758202,
12.));
#185693=CARTESIAN_POINT('Ctrl Pts',(24.9676376201502,-1.15456067621891,
0.));
#185694=CARTESIAN_POINT('Ctrl Pts',(24.9676376201502,-1.15456067621891,
12.));
#185695=CARTESIAN_POINT('Ctrl Pts',(24.9441788300932,-1.16443205502851,
0.));
#185696=CARTESIAN_POINT('Ctrl Pts',(24.9441788300932,-1.16443205502851,
12.));
#185697=CARTESIAN_POINT('Ctrl Pts',(24.9207705514448,-1.17421693835042,
0.));
#185698=CARTESIAN_POINT('Ctrl Pts',(24.9207705514448,-1.17421693835042,
12.));
#185699=CARTESIAN_POINT('Ctrl Pts',(24.8974133481829,-1.18391538220104,
0.));
#185700=CARTESIAN_POINT('Ctrl Pts',(24.8974133481829,-1.18391538220104,
12.));
#185701=CARTESIAN_POINT('Ctrl Pts',(24.8741077892075,-1.19352744434066,
0.));
#185702=CARTESIAN_POINT('Ctrl Pts',(24.8741077892075,-1.19352744434066,
12.));
#185703=CARTESIAN_POINT('Ctrl Pts',(24.8508544481974,-1.20305318426021,
0.));
#185704=CARTESIAN_POINT('Ctrl Pts',(24.8508544481974,-1.20305318426021,
12.));
#185705=CARTESIAN_POINT('Ctrl Pts',(24.8276539035092,-1.21249266318209,
0.));
#185706=CARTESIAN_POINT('Ctrl Pts',(24.8276539035092,-1.21249266318209,
12.));
#185707=CARTESIAN_POINT('Ctrl Pts',(24.8045067380536,-1.22184594406529,
0.));
#185708=CARTESIAN_POINT('Ctrl Pts',(24.8045067380536,-1.22184594406529,
12.));
#185709=CARTESIAN_POINT('Ctrl Pts',(24.7814135391799,-1.23111309161845,
0.));
#185710=CARTESIAN_POINT('Ctrl Pts',(24.7814135391799,-1.23111309161845,
12.));
#185711=CARTESIAN_POINT('Ctrl Pts',(24.7583748985438,-1.2402941723199,0.));
#185712=CARTESIAN_POINT('Ctrl Pts',(24.7583748985438,-1.2402941723199,12.));
#185713=CARTESIAN_POINT('Ctrl Pts',(24.7353914120011,-1.24938925444327,
0.));
#185714=CARTESIAN_POINT('Ctrl Pts',(24.7353914120011,-1.24938925444327,
12.));
#185715=CARTESIAN_POINT('Ctrl Pts',(24.7124636797894,-1.25839840807419,
0.));
#185716=CARTESIAN_POINT('Ctrl Pts',(24.7124636797894,-1.25839840807419,
12.));
#185717=CARTESIAN_POINT('Ctrl Pts',(24.6895923066836,-1.26732170513501,
0.));
#185718=CARTESIAN_POINT('Ctrl Pts',(24.6895923066836,-1.26732170513501,
12.));
#185719=CARTESIAN_POINT('Ctrl Pts',(24.6667779021559,-1.27615921941643,
0.));
#185720=CARTESIAN_POINT('Ctrl Pts',(24.6667779021559,-1.27615921941643,
12.));
#185721=CARTESIAN_POINT('Ctrl Pts',(24.6440210805278,-1.28491102661515,
0.));
#185722=CARTESIAN_POINT('Ctrl Pts',(24.6440210805278,-1.28491102661515,
12.));
#185723=CARTESIAN_POINT('Ctrl Pts',(24.6213224611229,-1.29357720438108,
0.));
#185724=CARTESIAN_POINT('Ctrl Pts',(24.6213224611229,-1.29357720438108,
12.));
#185725=CARTESIAN_POINT('Ctrl Pts',(24.5986826684027,-1.30215783236363,
0.));
#185726=CARTESIAN_POINT('Ctrl Pts',(24.5986826684027,-1.30215783236363,
12.));
#185727=CARTESIAN_POINT('Ctrl Pts',(24.5761023320183,-1.31065299222023,
0.));
#185728=CARTESIAN_POINT('Ctrl Pts',(24.5761023320183,-1.31065299222023,
12.));
#185729=CARTESIAN_POINT('Ctrl Pts',(24.5535820868674,-1.31906276763669,
0.));
#185730=CARTESIAN_POINT('Ctrl Pts',(24.5535820868674,-1.31906276763669,
12.));
#185731=CARTESIAN_POINT('Ctrl Pts',(24.5311225731435,-1.32738724435327,
0.));
#185732=CARTESIAN_POINT('Ctrl Pts',(24.5311225731435,-1.32738724435327,
12.));
#185733=CARTESIAN_POINT('Ctrl Pts',(24.5087244363856,-1.33562651019687,
0.));
#185734=CARTESIAN_POINT('Ctrl Pts',(24.5087244363856,-1.33562651019687,
12.));
#185735=CARTESIAN_POINT('Ctrl Pts',(24.4863883275134,-1.34378065512339,
0.));
#185736=CARTESIAN_POINT('Ctrl Pts',(24.4863883275134,-1.34378065512339,
12.));
#185737=CARTESIAN_POINT('Ctrl Pts',(24.4641149028892,-1.35184977125649,
0.));
#185738=CARTESIAN_POINT('Ctrl Pts',(24.4641149028892,-1.35184977125649,
12.));
#185739=CARTESIAN_POINT('Ctrl Pts',(24.4419048244523,-1.35983395290629,
0.));
#185740=CARTESIAN_POINT('Ctrl Pts',(24.4419048244523,-1.35983395290629,
12.));
#185741=CARTESIAN_POINT('Ctrl Pts',(24.4197587598337,-1.36773329659958,
0.));
#185742=CARTESIAN_POINT('Ctrl Pts',(24.4197587598337,-1.36773329659958,
12.));
#185743=CARTESIAN_POINT('Ctrl Pts',(24.3976773824732,-1.37554790111611,
0.));
#185744=CARTESIAN_POINT('Ctrl Pts',(24.3976773824732,-1.37554790111611,
12.));
#185745=CARTESIAN_POINT('Ctrl Pts',(24.3756613717299,-1.38327786753,0.));
#185746=CARTESIAN_POINT('Ctrl Pts',(24.3756613717299,-1.38327786753,12.));
#185747=CARTESIAN_POINT('Ctrl Pts',(24.3537114129875,-1.3909232992639,0.));
#185748=CARTESIAN_POINT('Ctrl Pts',(24.3537114129875,-1.3909232992639,12.));
#185749=CARTESIAN_POINT('Ctrl Pts',(24.3318281977643,-1.39848430212808,
0.));
#185750=CARTESIAN_POINT('Ctrl Pts',(24.3318281977643,-1.39848430212808,
12.));
#185751=CARTESIAN_POINT('Ctrl Pts',(24.3100124238311,-1.40596098434339,
0.));
#185752=CARTESIAN_POINT('Ctrl Pts',(24.3100124238311,-1.40596098434339,
12.));
#185753=CARTESIAN_POINT('Ctrl Pts',(24.288264795321,-1.41335345657684,0.));
#185754=CARTESIAN_POINT('Ctrl Pts',(24.288264795321,-1.41335345657684,12.));
#185755=CARTESIAN_POINT('Ctrl Pts',(24.2665860228356,-1.42066183198254,
0.));
#185756=CARTESIAN_POINT('Ctrl Pts',(24.2665860228356,-1.42066183198254,
12.));
#185757=CARTESIAN_POINT('Ctrl Pts',(24.2449768235488,-1.42788622624855,
0.));
#185758=CARTESIAN_POINT('Ctrl Pts',(24.2449768235488,-1.42788622624855,
12.));
#185759=CARTESIAN_POINT('Ctrl Pts',(24.2234379212984,-1.4350267576551,0.));
#185760=CARTESIAN_POINT('Ctrl Pts',(24.2234379212984,-1.4350267576551,12.));
#185761=CARTESIAN_POINT('Ctrl Pts',(24.201970046722,-1.44208354711083,0.));
#185762=CARTESIAN_POINT('Ctrl Pts',(24.201970046722,-1.44208354711083,12.));
#185763=CARTESIAN_POINT('Ctrl Pts',(24.1805739374038,-1.44905671818729,
0.));
#185764=CARTESIAN_POINT('Ctrl Pts',(24.1805739374038,-1.44905671818729,
12.));
#185765=CARTESIAN_POINT('Ctrl Pts',(24.1592503380107,-1.45594639716319,
0.));
#185766=CARTESIAN_POINT('Ctrl Pts',(24.1592503380107,-1.45594639716319,
12.));
#185767=CARTESIAN_POINT('Ctrl Pts',(24.1380000004272,-1.46275271307399,
0.));
#185768=CARTESIAN_POINT('Ctrl Pts',(24.1380000004272,-1.46275271307399,
12.));
#185769=CARTESIAN_POINT('Ctrl Pts',(24.1168236838824,-1.46947579776993,
0.));
#185770=CARTESIAN_POINT('Ctrl Pts',(24.1168236838824,-1.46947579776993,
12.));
#185771=CARTESIAN_POINT('Ctrl Pts',(24.0957221550778,-1.47611578597743,
0.));
#185772=CARTESIAN_POINT('Ctrl Pts',(24.0957221550778,-1.47611578597743,
12.));
#185773=CARTESIAN_POINT('Ctrl Pts',(24.0746961883528,-1.48267281533684,
0.));
#185774=CARTESIAN_POINT('Ctrl Pts',(24.0746961883528,-1.48267281533684,
12.));
#185775=CARTESIAN_POINT('Ctrl Pts',(24.0537465658429,-1.48914702644889,
0.));
#185776=CARTESIAN_POINT('Ctrl Pts',(24.0537465658429,-1.48914702644889,
12.));
#185777=CARTESIAN_POINT('Ctrl Pts',(24.0328740776331,-1.49553856292802,
0.));
#185778=CARTESIAN_POINT('Ctrl Pts',(24.0328740776331,-1.49553856292802,
12.));
#185779=CARTESIAN_POINT('Ctrl Pts',(24.0120795219086,-1.501847571461,0.));
#185780=CARTESIAN_POINT('Ctrl Pts',(24.0120795219086,-1.501847571461,12.));
#185781=CARTESIAN_POINT('Ctrl Pts',(23.9913637050927,-1.50807420187695,
0.));
#185782=CARTESIAN_POINT('Ctrl Pts',(23.9913637050927,-1.50807420187695,
12.));
#185783=CARTESIAN_POINT('Ctrl Pts',(23.970727442014,-1.51421860720616,0.));
#185784=CARTESIAN_POINT('Ctrl Pts',(23.970727442014,-1.51421860720616,12.));
#185785=CARTESIAN_POINT('Ctrl Pts',(23.9501715561033,-1.52028094372793,
0.));
#185786=CARTESIAN_POINT('Ctrl Pts',(23.9501715561033,-1.52028094372793,
12.));
#185787=CARTESIAN_POINT('Ctrl Pts',(23.9296968795757,-1.52626137103033,
0.));
#185788=CARTESIAN_POINT('Ctrl Pts',(23.9296968795757,-1.52626137103033,
12.));
#185789=CARTESIAN_POINT('Ctrl Pts',(23.9093042536119,-1.53216005207464,
0.));
#185790=CARTESIAN_POINT('Ctrl Pts',(23.9093042536119,-1.53216005207464,
12.));
#185791=CARTESIAN_POINT('Ctrl Pts',(23.8889945285318,-1.53797715326759,
0.));
#185792=CARTESIAN_POINT('Ctrl Pts',(23.8889945285318,-1.53797715326759,
12.));
#185793=CARTESIAN_POINT('Ctrl Pts',(23.8687685639642,-1.54371284453992,
0.));
#185794=CARTESIAN_POINT('Ctrl Pts',(23.8687685639642,-1.54371284453992,
12.));
#185795=CARTESIAN_POINT('Ctrl Pts',(23.8486272290705,-1.54936729940542,
0.));
#185796=CARTESIAN_POINT('Ctrl Pts',(23.8486272290705,-1.54936729940542,
12.));
#185797=CARTESIAN_POINT('Ctrl Pts',(23.8285714027636,-1.55494069502636,
0.));
#185798=CARTESIAN_POINT('Ctrl Pts',(23.8285714027636,-1.55494069502636,
12.));
#185799=CARTESIAN_POINT('Ctrl Pts',(23.8086019739194,-1.56043321228635,
0.));
#185800=CARTESIAN_POINT('Ctrl Pts',(23.8086019739194,-1.56043321228635,
12.));
#185801=CARTESIAN_POINT('Ctrl Pts',(23.7887198415878,-1.56584503586844,
0.));
#185802=CARTESIAN_POINT('Ctrl Pts',(23.7887198415878,-1.56584503586844,
12.));
#185803=CARTESIAN_POINT('Ctrl Pts',(23.7689259151862,-1.57117635434409,
0.));
#185804=CARTESIAN_POINT('Ctrl Pts',(23.7689259151862,-1.57117635434409,
12.));
#185805=CARTESIAN_POINT('Ctrl Pts',(23.749221114736,-1.57642736025247,0.));
#185806=CARTESIAN_POINT('Ctrl Pts',(23.749221114736,-1.57642736025247,12.));
#185807=CARTESIAN_POINT('Ctrl Pts',(23.72960637113,-1.58159825017359,0.));
#185808=CARTESIAN_POINT('Ctrl Pts',(23.72960637113,-1.58159825017359,12.));
#185809=CARTESIAN_POINT('Ctrl Pts',(23.710082626383,-1.58668922481222,0.));
#185810=CARTESIAN_POINT('Ctrl Pts',(23.710082626383,-1.58668922481222,12.));
#185811=CARTESIAN_POINT('Ctrl Pts',(23.6906508338833,-1.59170048908634,
0.));
#185812=CARTESIAN_POINT('Ctrl Pts',(23.6906508338833,-1.59170048908634,
12.));
#185813=CARTESIAN_POINT('Ctrl Pts',(23.671311958631,-1.59663225222464,0.));
#185814=CARTESIAN_POINT('Ctrl Pts',(23.671311958631,-1.59663225222464,12.));
#185815=CARTESIAN_POINT('Ctrl Pts',(23.6520669774876,-1.60148472786596,
0.));
#185816=CARTESIAN_POINT('Ctrl Pts',(23.6520669774876,-1.60148472786596,
12.));
#185817=CARTESIAN_POINT('Ctrl Pts',(23.6329168794929,-1.60625813414674,
0.));
#185818=CARTESIAN_POINT('Ctrl Pts',(23.6329168794929,-1.60625813414674,
12.));
#185819=CARTESIAN_POINT('Ctrl Pts',(23.6138626661653,-1.61095269379779,
0.));
#185820=CARTESIAN_POINT('Ctrl Pts',(23.6138626661653,-1.61095269379779,
12.));
#185821=CARTESIAN_POINT('Ctrl Pts',(23.5949053517997,-1.61556863424699,
0.));
#185822=CARTESIAN_POINT('Ctrl Pts',(23.5949053517997,-1.61556863424699,
12.));
#185823=CARTESIAN_POINT('Ctrl Pts',(23.57604596376,-1.62010618772867,0.));
#185824=CARTESIAN_POINT('Ctrl Pts',(23.57604596376,-1.62010618772867,12.));
#185825=CARTESIAN_POINT('Ctrl Pts',(23.5572855427601,-1.62456559140066,
0.));
#185826=CARTESIAN_POINT('Ctrl Pts',(23.5572855427601,-1.62456559140066,
12.));
#185827=CARTESIAN_POINT('Ctrl Pts',(23.538625143226,-1.62894708745224,0.));
#185828=CARTESIAN_POINT('Ctrl Pts',(23.538625143226,-1.62894708745224,12.));
#185829=CARTESIAN_POINT('Ctrl Pts',(23.5200658336612,-1.63325092321727,
0.));
#185830=CARTESIAN_POINT('Ctrl Pts',(23.5200658336612,-1.63325092321727,
12.));
#185831=CARTESIAN_POINT('Ctrl Pts',(23.5016086970003,-1.63747735129475,
0.));
#185832=CARTESIAN_POINT('Ctrl Pts',(23.5016086970003,-1.63747735129475,
12.));
#185833=CARTESIAN_POINT('Ctrl Pts',(23.4832548309645,-1.64162662967529,
0.));
#185834=CARTESIAN_POINT('Ctrl Pts',(23.4832548309645,-1.64162662967529,
12.));
#185835=CARTESIAN_POINT('Ctrl Pts',(23.4650053483932,-1.64569902187612,
0.));
#185836=CARTESIAN_POINT('Ctrl Pts',(23.4650053483932,-1.64569902187612,
12.));
#185837=CARTESIAN_POINT('Ctrl Pts',(23.4468613776574,-1.64969479707341,
0.));
#185838=CARTESIAN_POINT('Ctrl Pts',(23.4468613776574,-1.64969479707341,
12.));
#185839=CARTESIAN_POINT('Ctrl Pts',(23.4288240631043,-1.6536142302373,0.));
#185840=CARTESIAN_POINT('Ctrl Pts',(23.4288240631043,-1.6536142302373,12.));
#185841=CARTESIAN_POINT('Ctrl Pts',(23.4108945654805,-1.65745760227506,
0.));
#185842=CARTESIAN_POINT('Ctrl Pts',(23.4108945654805,-1.65745760227506,
12.));
#185843=CARTESIAN_POINT('Ctrl Pts',(23.3930740623619,-1.66122520018012,
0.));
#185844=CARTESIAN_POINT('Ctrl Pts',(23.3930740623619,-1.66122520018012,
12.));
#185845=CARTESIAN_POINT('Ctrl Pts',(23.3753637485545,-1.66491731718878,
0.));
#185846=CARTESIAN_POINT('Ctrl Pts',(23.3753637485545,-1.66491731718878,
12.));
#185847=CARTESIAN_POINT('Ctrl Pts',(23.3577648365744,-1.66853425293997,
0.));
#185848=CARTESIAN_POINT('Ctrl Pts',(23.3577648365744,-1.66853425293997,
12.));
#185849=CARTESIAN_POINT('Ctrl Pts',(23.3402785571865,-1.67207631363923,
0.));
#185850=CARTESIAN_POINT('Ctrl Pts',(23.3402785571865,-1.67207631363923,
12.));
#185851=CARTESIAN_POINT('Ctrl Pts',(23.3229061599144,-1.67554381222995,
0.));
#185852=CARTESIAN_POINT('Ctrl Pts',(23.3229061599144,-1.67554381222995,
12.));
#185853=CARTESIAN_POINT('Ctrl Pts',(23.3056489135611,-1.67893706857118,
0.));
#185854=CARTESIAN_POINT('Ctrl Pts',(23.3056489135611,-1.67893706857118,
12.));
#185855=CARTESIAN_POINT('Ctrl Pts',(23.2885081066951,-1.68225640962169,
0.));
#185856=CARTESIAN_POINT('Ctrl Pts',(23.2885081066951,-1.68225640962169,
12.));
#185857=CARTESIAN_POINT('Ctrl Pts',(23.2714850482246,-1.68550216963259,
0.));
#185858=CARTESIAN_POINT('Ctrl Pts',(23.2714850482246,-1.68550216963259,
12.));
#185859=CARTESIAN_POINT('Ctrl Pts',(23.2545810680537,-1.68867469034897,
0.));
#185860=CARTESIAN_POINT('Ctrl Pts',(23.2545810680537,-1.68867469034897,
12.));
#185861=CARTESIAN_POINT('Ctrl Pts',(23.2377975177013,-1.69177432121712,
0.));
#185862=CARTESIAN_POINT('Ctrl Pts',(23.2377975177013,-1.69177432121712,
12.));
#185863=CARTESIAN_POINT('Ctrl Pts',(23.2211357709374,-1.69480141959954,
0.));
#185864=CARTESIAN_POINT('Ctrl Pts',(23.2211357709374,-1.69480141959954,
12.));
#185865=CARTESIAN_POINT('Ctrl Pts',(23.2045972243767,-1.69775635099444,
0.));
#185866=CARTESIAN_POINT('Ctrl Pts',(23.2045972243767,-1.69775635099444,
12.));
#185867=CARTESIAN_POINT('Ctrl Pts',(23.1881832981851,-1.70063948927011,
0.));
#185868=CARTESIAN_POINT('Ctrl Pts',(23.1881832981851,-1.70063948927011,
12.));
#185869=CARTESIAN_POINT('Ctrl Pts',(23.1718954368751,-1.70345121691278,
0.));
#185870=CARTESIAN_POINT('Ctrl Pts',(23.1718954368751,-1.70345121691278,
12.));
#185871=CARTESIAN_POINT('Ctrl Pts',(23.1557351100614,-1.70619192527853,
0.));
#185872=CARTESIAN_POINT('Ctrl Pts',(23.1557351100614,-1.70619192527853,
12.));
#185873=CARTESIAN_POINT('Ctrl Pts',(23.1397038132356,-1.70886201485453,
0.));
#185874=CARTESIAN_POINT('Ctrl Pts',(23.1397038132356,-1.70886201485453,
12.));
#185875=CARTESIAN_POINT('Ctrl Pts',(23.1238030684925,-1.71146189552175,
0.));
#185876=CARTESIAN_POINT('Ctrl Pts',(23.1238030684925,-1.71146189552175,
12.));
#185877=CARTESIAN_POINT('Ctrl Pts',(23.1080344254286,-1.71399198684705,
0.));
#185878=CARTESIAN_POINT('Ctrl Pts',(23.1080344254286,-1.71399198684705,
12.));
#185879=CARTESIAN_POINT('Ctrl Pts',(23.0923994621213,-1.71645271839298,
0.));
#185880=CARTESIAN_POINT('Ctrl Pts',(23.0923994621213,-1.71645271839298,
12.));
#185881=CARTESIAN_POINT('Ctrl Pts',(23.0768997860708,-1.71884453003028,
0.));
#185882=CARTESIAN_POINT('Ctrl Pts',(23.0768997860708,-1.71884453003028,
12.));
#185883=CARTESIAN_POINT('Ctrl Pts',(23.0615370351562,-1.72116787225993,
0.));
#185884=CARTESIAN_POINT('Ctrl Pts',(23.0615370351562,-1.72116787225993,
12.));
#185885=CARTESIAN_POINT('Ctrl Pts',(23.0463128785531,-1.72342320653748,
0.));
#185886=CARTESIAN_POINT('Ctrl Pts',(23.0463128785531,-1.72342320653748,
12.));
#185887=CARTESIAN_POINT('Ctrl Pts',(23.0312290178883,-1.72561100564047,
0.));
#185888=CARTESIAN_POINT('Ctrl Pts',(23.0312290178883,-1.72561100564047,
12.));
#185889=CARTESIAN_POINT('Ctrl Pts',(23.0162871884168,-1.7277317540471,0.));
#185890=CARTESIAN_POINT('Ctrl Pts',(23.0162871884168,-1.7277317540471,12.));
#185891=CARTESIAN_POINT('Ctrl Pts',(23.001489160189,-1.72978594832137,0.));
#185892=CARTESIAN_POINT('Ctrl Pts',(23.001489160189,-1.72978594832137,12.));
#185893=CARTESIAN_POINT('Ctrl Pts',(22.9868367391978,-1.73177409750192,
0.));
#185894=CARTESIAN_POINT('Ctrl Pts',(22.9868367391978,-1.73177409750192,
12.));
#185895=CARTESIAN_POINT('Ctrl Pts',(22.9723317685688,-1.73369672350816,
0.));
#185896=CARTESIAN_POINT('Ctrl Pts',(22.9723317685688,-1.73369672350816,
12.));
#185897=CARTESIAN_POINT('Ctrl Pts',(22.9579761301063,-1.73555436162771,
0.));
#185898=CARTESIAN_POINT('Ctrl Pts',(22.9579761301063,-1.73555436162771,
12.));
#185899=CARTESIAN_POINT('Ctrl Pts',(22.9437717457826,-1.7373475610004,0.));
#185900=CARTESIAN_POINT('Ctrl Pts',(22.9437717457826,-1.7373475610004,12.));
#185901=CARTESIAN_POINT('Ctrl Pts',(22.9297205792586,-1.73907688511667,
0.));
#185902=CARTESIAN_POINT('Ctrl Pts',(22.9297205792586,-1.73907688511667,
12.));
#185903=CARTESIAN_POINT('Ctrl Pts',(22.9158246373363,-1.7407429123106,0.));
#185904=CARTESIAN_POINT('Ctrl Pts',(22.9158246373363,-1.7407429123106,12.));
#185905=CARTESIAN_POINT('Ctrl Pts',(22.9020859716141,-1.74234623630081,
0.));
#185906=CARTESIAN_POINT('Ctrl Pts',(22.9020859716141,-1.74234623630081,
12.));
#185907=CARTESIAN_POINT('Ctrl Pts',(22.888506680335,-1.74388746677704,0.));
#185908=CARTESIAN_POINT('Ctrl Pts',(22.888506680335,-1.74388746677704,12.));
#185909=CARTESIAN_POINT('Ctrl Pts',(22.8750889101696,-1.74536722998202,
0.));
#185910=CARTESIAN_POINT('Ctrl Pts',(22.8750889101696,-1.74536722998202,
12.));
#185911=CARTESIAN_POINT('Ctrl Pts',(22.8618348580235,-1.74678616930666,
0.));
#185912=CARTESIAN_POINT('Ctrl Pts',(22.8618348580235,-1.74678616930666,
12.));
#185913=CARTESIAN_POINT('Ctrl Pts',(22.8487467728076,-1.74814494588494,
0.));
#185914=CARTESIAN_POINT('Ctrl Pts',(22.8487467728076,-1.74814494588494,
12.));
#185915=CARTESIAN_POINT('Ctrl Pts',(22.8358269579853,-1.74944423940117,
0.));
#185916=CARTESIAN_POINT('Ctrl Pts',(22.8358269579853,-1.74944423940117,
12.));
#185917=CARTESIAN_POINT('Ctrl Pts',(22.8230777741284,-1.75068474890884,
0.));
#185918=CARTESIAN_POINT('Ctrl Pts',(22.8230777741284,-1.75068474890884,
12.));
#185919=CARTESIAN_POINT('Ctrl Pts',(22.8105016414713,-1.75186719365593,
0.));
#185920=CARTESIAN_POINT('Ctrl Pts',(22.8105016414713,-1.75186719365593,
12.));
#185921=CARTESIAN_POINT('Ctrl Pts',(22.7981010424314,-1.75299231391468,
0.));
#185922=CARTESIAN_POINT('Ctrl Pts',(22.7981010424314,-1.75299231391468,
12.));
#185923=CARTESIAN_POINT('Ctrl Pts',(22.7858785242361,-1.75406087182937,
0.));
#185924=CARTESIAN_POINT('Ctrl Pts',(22.7858785242361,-1.75406087182937,
12.));
#185925=CARTESIAN_POINT('Ctrl Pts',(22.7738367016118,-1.75507365227133,
0.));
#185926=CARTESIAN_POINT('Ctrl Pts',(22.7738367016118,-1.75507365227133,
12.));
#185927=CARTESIAN_POINT('Ctrl Pts',(22.7619782595013,-1.75603146371642,
0.));
#185928=CARTESIAN_POINT('Ctrl Pts',(22.7619782595013,-1.75603146371642,
12.));
#185929=CARTESIAN_POINT('Ctrl Pts',(22.750305955645,-1.75693513908908,0.));
#185930=CARTESIAN_POINT('Ctrl Pts',(22.750305955645,-1.75693513908908,12.));
#185931=CARTESIAN_POINT('Ctrl Pts',(22.7388226235559,-1.75778553673245,
0.));
#185932=CARTESIAN_POINT('Ctrl Pts',(22.7388226235559,-1.75778553673245,
12.));
#185933=CARTESIAN_POINT('Ctrl Pts',(22.72753117773,-1.75858354204634,0.));
#185934=CARTESIAN_POINT('Ctrl Pts',(22.72753117773,-1.75858354204634,12.));
#185935=CARTESIAN_POINT('Ctrl Pts',(22.7164346186006,-1.75933006905926,
0.));
#185936=CARTESIAN_POINT('Ctrl Pts',(22.7164346186006,-1.75933006905926,
12.));
#185937=CARTESIAN_POINT('Ctrl Pts',(22.7055360375485,-1.76002606202402,
0.));
#185938=CARTESIAN_POINT('Ctrl Pts',(22.7055360375485,-1.76002606202402,
12.));
#185939=CARTESIAN_POINT('Ctrl Pts',(22.6948386219851,-1.76067249704888,
0.));
#185940=CARTESIAN_POINT('Ctrl Pts',(22.6948386219851,-1.76067249704888,
12.));
#185941=CARTESIAN_POINT('Ctrl Pts',(22.684345658525,-1.76127038310615,0.));
#185942=CARTESIAN_POINT('Ctrl Pts',(22.684345658525,-1.76127038310615,12.));
#185943=CARTESIAN_POINT('Ctrl Pts',(22.67406053567,-1.76182076289527,0.));
#185944=CARTESIAN_POINT('Ctrl Pts',(22.67406053567,-1.76182076289527,12.));
#185945=CARTESIAN_POINT('Ctrl Pts',(22.6639867471753,-1.7623247139257,0.));
#185946=CARTESIAN_POINT('Ctrl Pts',(22.6639867471753,-1.7623247139257,12.));
#185947=CARTESIAN_POINT('Ctrl Pts',(22.6541278938409,-1.76278334912562,
0.));
#185948=CARTESIAN_POINT('Ctrl Pts',(22.6541278938409,-1.76278334912562,
12.));
#185949=CARTESIAN_POINT('Ctrl Pts',(22.6444876940423,-1.76319782013917,
0.));
#185950=CARTESIAN_POINT('Ctrl Pts',(22.6444876940423,-1.76319782013917,
12.));
#185951=CARTESIAN_POINT('Ctrl Pts',(22.6350699979359,-1.76356932176274,
0.));
#185952=CARTESIAN_POINT('Ctrl Pts',(22.6350699979359,-1.76356932176274,
12.));
#185953=CARTESIAN_POINT('Ctrl Pts',(22.6258787994848,-1.76389909571404,
0.));
#185954=CARTESIAN_POINT('Ctrl Pts',(22.6258787994848,-1.76389909571404,
12.));
#185955=CARTESIAN_POINT('Ctrl Pts',(22.6169182517694,-1.76418843543741,
0.));
#185956=CARTESIAN_POINT('Ctrl Pts',(22.6169182517694,-1.76418843543741,
12.));
#185957=CARTESIAN_POINT('Ctrl Pts',(22.6081926681343,-1.76443868648017,
0.));
#185958=CARTESIAN_POINT('Ctrl Pts',(22.6081926681343,-1.76443868648017,
12.));
#185959=CARTESIAN_POINT('Ctrl Pts',(22.5997065145638,-1.76465124413558,
0.));
#185960=CARTESIAN_POINT('Ctrl Pts',(22.5997065145638,-1.76465124413558,
12.));
#185961=CARTESIAN_POINT('Ctrl Pts',(22.5914644078105,-1.76482755288412,
0.));
#185962=CARTESIAN_POINT('Ctrl Pts',(22.5914644078105,-1.76482755288412,
12.));
#185963=CARTESIAN_POINT('Ctrl Pts',(22.5834711038022,-1.76496910283089,
0.));
#185964=CARTESIAN_POINT('Ctrl Pts',(22.5834711038022,-1.76496910283089,
12.));
#185965=CARTESIAN_POINT('Ctrl Pts',(22.5757315316353,-1.76507744026747,
0.));
#185966=CARTESIAN_POINT('Ctrl Pts',(22.5757315316353,-1.76507744026747,
12.));
#185967=CARTESIAN_POINT('Ctrl Pts',(22.5682508499873,-1.76515418518832,
0.));
#185968=CARTESIAN_POINT('Ctrl Pts',(22.5682508499873,-1.76515418518832,
12.));
#185969=CARTESIAN_POINT('Ctrl Pts',(22.5610344912501,-1.76520104500451,
0.));
#185970=CARTESIAN_POINT('Ctrl Pts',(22.5610344912501,-1.76520104500451,
12.));
#185971=CARTESIAN_POINT('Ctrl Pts',(22.5540882235837,-1.76521983384064,
0.));
#185972=CARTESIAN_POINT('Ctrl Pts',(22.5540882235837,-1.76521983384064,
12.));
#185973=CARTESIAN_POINT('Ctrl Pts',(22.5474180954006,-1.76521245524048,
0.));
#185974=CARTESIAN_POINT('Ctrl Pts',(22.5474180954006,-1.76521245524048,
12.));
#185975=CARTESIAN_POINT('Ctrl Pts',(22.5410303590892,-1.76518087841494,
0.));
#185976=CARTESIAN_POINT('Ctrl Pts',(22.5410303590892,-1.76518087841494,
12.));
#185977=CARTESIAN_POINT('Ctrl Pts',(22.5349313983571,-1.76512711563255,
0.));
#185978=CARTESIAN_POINT('Ctrl Pts',(22.5349313983571,-1.76512711563255,
12.));
#185979=CARTESIAN_POINT('Ctrl Pts',(22.529127665298,-1.7650532026276,0.));
#185980=CARTESIAN_POINT('Ctrl Pts',(22.529127665298,-1.7650532026276,12.));
#185981=CARTESIAN_POINT('Ctrl Pts',(22.5236259635515,-1.76496128643376,
0.));
#185982=CARTESIAN_POINT('Ctrl Pts',(22.5236259635515,-1.76496128643376,
12.));
#185983=CARTESIAN_POINT('Ctrl Pts',(22.5184336670207,-1.76485369319896,
0.));
#185984=CARTESIAN_POINT('Ctrl Pts',(22.5184336670207,-1.76485369319896,
12.));
#185985=CARTESIAN_POINT('Ctrl Pts',(22.5135590569554,-1.7647330328115,0.));
#185986=CARTESIAN_POINT('Ctrl Pts',(22.5135590569554,-1.7647330328115,12.));
#185987=CARTESIAN_POINT('Ctrl Pts',(22.5090112700212,-1.76460218257314,
0.));
#185988=CARTESIAN_POINT('Ctrl Pts',(22.5090112700212,-1.76460218257314,
12.));
#185989=CARTESIAN_POINT('Ctrl Pts',(22.5047996391978,-1.76446408210366,
0.));
#185990=CARTESIAN_POINT('Ctrl Pts',(22.5047996391978,-1.76446408210366,
12.));
#185991=CARTESIAN_POINT('Ctrl Pts',(22.5009332677316,-1.76432160068739,
0.));
#185992=CARTESIAN_POINT('Ctrl Pts',(22.5009332677316,-1.76432160068739,
12.));
#185993=CARTESIAN_POINT('Ctrl Pts',(22.4974203063191,-1.76417731243484,
0.));
#185994=CARTESIAN_POINT('Ctrl Pts',(22.4974203063191,-1.76417731243484,
12.));
#185995=CARTESIAN_POINT('Ctrl Pts',(22.4942693792449,-1.76403393880317,
0.));
#185996=CARTESIAN_POINT('Ctrl Pts',(22.4942693792449,-1.76403393880317,
12.));
#185997=CARTESIAN_POINT('Ctrl Pts',(22.4914909094908,-1.76389475965715,
0.));
#185998=CARTESIAN_POINT('Ctrl Pts',(22.4914909094908,-1.76389475965715,
12.));
#185999=CARTESIAN_POINT('Ctrl Pts',(22.4890991659479,-1.76376424879469,
0.));
#186000=CARTESIAN_POINT('Ctrl Pts',(22.4890991659479,-1.76376424879469,
12.));
#186001=CARTESIAN_POINT('Ctrl Pts',(22.4871115206572,-1.76364784232927,
0.));
#186002=CARTESIAN_POINT('Ctrl Pts',(22.4871115206572,-1.76364784232927,
12.));
#186003=CARTESIAN_POINT('Ctrl Pts',(22.4855446605991,-1.7635507604555,0.));
#186004=CARTESIAN_POINT('Ctrl Pts',(22.4855446605991,-1.7635507604555,12.));
#186005=CARTESIAN_POINT('Ctrl Pts',(22.4844112933125,-1.76347698284863,
0.));
#186006=CARTESIAN_POINT('Ctrl Pts',(22.4844112933125,-1.76347698284863,
12.));
#186007=CARTESIAN_POINT('Ctrl Pts',(22.4838562517064,-1.7634381343466,0.));
#186008=CARTESIAN_POINT('Ctrl Pts',(22.4838562517064,-1.7634381343466,12.));
#186009=CARTESIAN_POINT('Ctrl Pts',(22.4836387052228,-1.76342064263638,
0.));
#186010=CARTESIAN_POINT('Ctrl Pts',(22.4836387052228,-1.76342064263638,
12.));
#186011=CARTESIAN_POINT('Ctrl Pts',(22.4835819929788,-1.76341415538792,
0.));
#186012=CARTESIAN_POINT('Ctrl Pts',(22.4835819929788,-1.76341415538792,
12.));
#186013=CARTESIAN_POINT('Ctrl Pts',(22.4835757167854,-1.76341220531181,
0.));
#186014=CARTESIAN_POINT('Ctrl Pts',(22.4835757167854,-1.76341220531181,
12.));
#186015=CARTESIAN_POINT('',(25.991588367311,-0.661312440730916,0.));
#186016=CARTESIAN_POINT('Ctrl Pts',(25.991588367311,-0.661312440730916,
0.));
#186017=CARTESIAN_POINT('Ctrl Pts',(25.9865613464773,-0.66402831318764,
0.));
#186018=CARTESIAN_POINT('Ctrl Pts',(25.9765104298071,-0.669451306780839,
0.));
#186019=CARTESIAN_POINT('Ctrl Pts',(25.9614434297919,-0.67755954320974,
0.));
#186020=CARTESIAN_POINT('Ctrl Pts',(25.9413728471909,-0.688318015057744,
0.));
#186021=CARTESIAN_POINT('Ctrl Pts',(25.9163158909426,-0.701678575228769,
0.));
#186022=CARTESIAN_POINT('Ctrl Pts',(25.8912902614969,-0.714951588527653,
0.));
#186023=CARTESIAN_POINT('Ctrl Pts',(25.8662960624185,-0.728137036482349,
0.));
#186024=CARTESIAN_POINT('Ctrl Pts',(25.8413334619054,-0.74123490266382,
0.));
#186025=CARTESIAN_POINT('Ctrl Pts',(25.8164027059984,-0.754245175609537,
0.));
#186026=CARTESIAN_POINT('Ctrl Pts',(25.7915041383376,-0.767167852651183,
0.));
#186027=CARTESIAN_POINT('Ctrl Pts',(25.7666381946955,-0.780002940291977,
0.));
#186028=CARTESIAN_POINT('Ctrl Pts',(25.7418053757746,-0.79275045161614,
0.));
#186029=CARTESIAN_POINT('Ctrl Pts',(25.7170062262525,-0.805410404554366,
0.));
#186030=CARTESIAN_POINT('Ctrl Pts',(25.6922413110194,-0.817982819787478,
0.));
#186031=CARTESIAN_POINT('Ctrl Pts',(25.6675111931952,-0.830467718864221,
0.));
#186032=CARTESIAN_POINT('Ctrl Pts',(25.6428164100055,-0.842865122120773,
0.));
#186033=CARTESIAN_POINT('Ctrl Pts',(25.6181574536049,-0.855175047036563,
0.));
#186034=CARTESIAN_POINT('Ctrl Pts',(25.5935347843585,-0.867397509338443,
0.));
#186035=CARTESIAN_POINT('Ctrl Pts',(25.5689488408156,-0.879532523834308,
0.));
#186036=CARTESIAN_POINT('Ctrl Pts',(25.5444000508211,-0.891580105349052,
0.));
#186037=CARTESIAN_POINT('Ctrl Pts',(25.5198888424194,-0.903540269651121,
0.));
#186038=CARTESIAN_POINT('Ctrl Pts',(25.4954156541795,-0.915413034335626,
0.));
#186039=CARTESIAN_POINT('Ctrl Pts',(25.4709809475009,-0.927198419886108,
0.));
#186040=CARTESIAN_POINT('Ctrl Pts',(25.4465852044849,-0.938896449496205,
0.));
#186041=CARTESIAN_POINT('Ctrl Pts',(25.4222289223167,-0.950507148597483,
0.));
#186042=CARTESIAN_POINT('Ctrl Pts',(25.3979126089163,-0.962030544503156,
0.));
#186043=CARTESIAN_POINT('Ctrl Pts',(25.3736367778845,-0.973466666000178,
0.));
#186044=CARTESIAN_POINT('Ctrl Pts',(25.3494019441441,-0.984815543003986,
0.));
#186045=CARTESIAN_POINT('Ctrl Pts',(25.3252086182968,-0.996077206120637,
0.));
#186046=CARTESIAN_POINT('Ctrl Pts',(25.3010573055547,-1.00725168656897,
0.));
#186047=CARTESIAN_POINT('Ctrl Pts',(25.276948508726,-1.01833901642238,0.));
#186048=CARTESIAN_POINT('Ctrl Pts',(25.2528827300422,-1.02933922876807,
0.));
#186049=CARTESIAN_POINT('Ctrl Pts',(25.2288604735086,-1.04025235791508,
0.));
#186050=CARTESIAN_POINT('Ctrl Pts',(25.2048822469028,-1.05107843957933,
0.));
#186051=CARTESIAN_POINT('Ctrl Pts',(25.1809485642192,-1.06181751111769,
0.));
#186052=CARTESIAN_POINT('Ctrl Pts',(25.157059946931,-1.07246961165477,0.));
#186053=CARTESIAN_POINT('Ctrl Pts',(25.1332169227413,-1.08303478197189,
0.));
#186054=CARTESIAN_POINT('Ctrl Pts',(25.1094200248446,-1.09351306445309,
0.));
#186055=CARTESIAN_POINT('Ctrl Pts',(25.0856697909679,-1.10390450301747,
0.));
#186056=CARTESIAN_POINT('Ctrl Pts',(25.0619667625336,-1.11420914306891,
0.));
#186057=CARTESIAN_POINT('Ctrl Pts',(25.0383114836899,-1.12442703144453,
0.));
#186058=CARTESIAN_POINT('Ctrl Pts',(25.0147045006195,-1.13455821638531,
0.));
#186059=CARTESIAN_POINT('Ctrl Pts',(24.9911463621433,-1.14460274758202,
0.));
#186060=CARTESIAN_POINT('Ctrl Pts',(24.9676376201502,-1.15456067621891,
0.));
#186061=CARTESIAN_POINT('Ctrl Pts',(24.9441788300932,-1.16443205502851,
0.));
#186062=CARTESIAN_POINT('Ctrl Pts',(24.9207705514448,-1.17421693835042,
0.));
#186063=CARTESIAN_POINT('Ctrl Pts',(24.8974133481829,-1.18391538220104,
0.));
#186064=CARTESIAN_POINT('Ctrl Pts',(24.8741077892075,-1.19352744434066,
0.));
#186065=CARTESIAN_POINT('Ctrl Pts',(24.8508544481974,-1.20305318426021,
0.));
#186066=CARTESIAN_POINT('Ctrl Pts',(24.8276539035092,-1.21249266318209,
0.));
#186067=CARTESIAN_POINT('Ctrl Pts',(24.8045067380536,-1.22184594406529,
0.));
#186068=CARTESIAN_POINT('Ctrl Pts',(24.7814135391799,-1.23111309161845,
0.));
#186069=CARTESIAN_POINT('Ctrl Pts',(24.7583748985438,-1.2402941723199,0.));
#186070=CARTESIAN_POINT('Ctrl Pts',(24.7353914120011,-1.24938925444327,
0.));
#186071=CARTESIAN_POINT('Ctrl Pts',(24.7124636797894,-1.25839840807419,
0.));
#186072=CARTESIAN_POINT('Ctrl Pts',(24.6895923066836,-1.26732170513501,
0.));
#186073=CARTESIAN_POINT('Ctrl Pts',(24.6667779021559,-1.27615921941643,
0.));
#186074=CARTESIAN_POINT('Ctrl Pts',(24.6440210805278,-1.28491102661515,
0.));
#186075=CARTESIAN_POINT('Ctrl Pts',(24.6213224611229,-1.29357720438108,
0.));
#186076=CARTESIAN_POINT('Ctrl Pts',(24.5986826684027,-1.30215783236363,
0.));
#186077=CARTESIAN_POINT('Ctrl Pts',(24.5761023320183,-1.31065299222023,
0.));
#186078=CARTESIAN_POINT('Ctrl Pts',(24.5535820868674,-1.31906276763669,
0.));
#186079=CARTESIAN_POINT('Ctrl Pts',(24.5311225731435,-1.32738724435327,
0.));
#186080=CARTESIAN_POINT('Ctrl Pts',(24.5087244363856,-1.33562651019687,
0.));
#186081=CARTESIAN_POINT('Ctrl Pts',(24.4863883275134,-1.34378065512339,
0.));
#186082=CARTESIAN_POINT('Ctrl Pts',(24.4641149028892,-1.35184977125649,
0.));
#186083=CARTESIAN_POINT('Ctrl Pts',(24.4419048244523,-1.35983395290629,
0.));
#186084=CARTESIAN_POINT('Ctrl Pts',(24.4197587598337,-1.36773329659958,
0.));
#186085=CARTESIAN_POINT('Ctrl Pts',(24.3976773824732,-1.37554790111611,
0.));
#186086=CARTESIAN_POINT('Ctrl Pts',(24.3756613717299,-1.38327786753,0.));
#186087=CARTESIAN_POINT('Ctrl Pts',(24.3537114129875,-1.3909232992639,0.));
#186088=CARTESIAN_POINT('Ctrl Pts',(24.3318281977643,-1.39848430212808,
0.));
#186089=CARTESIAN_POINT('Ctrl Pts',(24.3100124238311,-1.40596098434339,
0.));
#186090=CARTESIAN_POINT('Ctrl Pts',(24.288264795321,-1.41335345657684,0.));
#186091=CARTESIAN_POINT('Ctrl Pts',(24.2665860228356,-1.42066183198254,
0.));
#186092=CARTESIAN_POINT('Ctrl Pts',(24.2449768235488,-1.42788622624855,
0.));
#186093=CARTESIAN_POINT('Ctrl Pts',(24.2234379212984,-1.4350267576551,0.));
#186094=CARTESIAN_POINT('Ctrl Pts',(24.201970046722,-1.44208354711083,0.));
#186095=CARTESIAN_POINT('Ctrl Pts',(24.1805739374038,-1.44905671818729,
0.));
#186096=CARTESIAN_POINT('Ctrl Pts',(24.1592503380107,-1.45594639716319,
0.));
#186097=CARTESIAN_POINT('Ctrl Pts',(24.1380000004272,-1.46275271307399,
0.));
#186098=CARTESIAN_POINT('Ctrl Pts',(24.1168236838824,-1.46947579776993,
0.));
#186099=CARTESIAN_POINT('Ctrl Pts',(24.0957221550778,-1.47611578597743,
0.));
#186100=CARTESIAN_POINT('Ctrl Pts',(24.0746961883528,-1.48267281533684,
0.));
#186101=CARTESIAN_POINT('Ctrl Pts',(24.0537465658429,-1.48914702644889,
0.));
#186102=CARTESIAN_POINT('Ctrl Pts',(24.0328740776331,-1.49553856292802,
0.));
#186103=CARTESIAN_POINT('Ctrl Pts',(24.0120795219086,-1.501847571461,0.));
#186104=CARTESIAN_POINT('Ctrl Pts',(23.9913637050927,-1.50807420187695,
0.));
#186105=CARTESIAN_POINT('Ctrl Pts',(23.970727442014,-1.51421860720616,0.));
#186106=CARTESIAN_POINT('Ctrl Pts',(23.9501715561033,-1.52028094372793,
0.));
#186107=CARTESIAN_POINT('Ctrl Pts',(23.9296968795757,-1.52626137103033,
0.));
#186108=CARTESIAN_POINT('Ctrl Pts',(23.9093042536119,-1.53216005207464,
0.));
#186109=CARTESIAN_POINT('Ctrl Pts',(23.8889945285318,-1.53797715326759,
0.));
#186110=CARTESIAN_POINT('Ctrl Pts',(23.8687685639642,-1.54371284453992,
0.));
#186111=CARTESIAN_POINT('Ctrl Pts',(23.8486272290705,-1.54936729940542,
0.));
#186112=CARTESIAN_POINT('Ctrl Pts',(23.8285714027636,-1.55494069502636,
0.));
#186113=CARTESIAN_POINT('Ctrl Pts',(23.8086019739194,-1.56043321228635,
0.));
#186114=CARTESIAN_POINT('Ctrl Pts',(23.7887198415878,-1.56584503586844,
0.));
#186115=CARTESIAN_POINT('Ctrl Pts',(23.7689259151862,-1.57117635434409,
0.));
#186116=CARTESIAN_POINT('Ctrl Pts',(23.749221114736,-1.57642736025247,0.));
#186117=CARTESIAN_POINT('Ctrl Pts',(23.72960637113,-1.58159825017359,0.));
#186118=CARTESIAN_POINT('Ctrl Pts',(23.710082626383,-1.58668922481222,0.));
#186119=CARTESIAN_POINT('Ctrl Pts',(23.6906508338833,-1.59170048908634,
0.));
#186120=CARTESIAN_POINT('Ctrl Pts',(23.671311958631,-1.59663225222464,0.));
#186121=CARTESIAN_POINT('Ctrl Pts',(23.6520669774876,-1.60148472786596,
0.));
#186122=CARTESIAN_POINT('Ctrl Pts',(23.6329168794929,-1.60625813414674,
0.));
#186123=CARTESIAN_POINT('Ctrl Pts',(23.6138626661653,-1.61095269379779,
0.));
#186124=CARTESIAN_POINT('Ctrl Pts',(23.5949053517997,-1.61556863424699,
0.));
#186125=CARTESIAN_POINT('Ctrl Pts',(23.57604596376,-1.62010618772867,0.));
#186126=CARTESIAN_POINT('Ctrl Pts',(23.5572855427601,-1.62456559140066,
0.));
#186127=CARTESIAN_POINT('Ctrl Pts',(23.538625143226,-1.62894708745224,0.));
#186128=CARTESIAN_POINT('Ctrl Pts',(23.5200658336612,-1.63325092321727,
0.));
#186129=CARTESIAN_POINT('Ctrl Pts',(23.5016086970003,-1.63747735129475,
0.));
#186130=CARTESIAN_POINT('Ctrl Pts',(23.4832548309645,-1.64162662967529,
0.));
#186131=CARTESIAN_POINT('Ctrl Pts',(23.4650053483932,-1.64569902187612,
0.));
#186132=CARTESIAN_POINT('Ctrl Pts',(23.4468613776574,-1.64969479707341,
0.));
#186133=CARTESIAN_POINT('Ctrl Pts',(23.4288240631043,-1.6536142302373,0.));
#186134=CARTESIAN_POINT('Ctrl Pts',(23.4108945654805,-1.65745760227506,
0.));
#186135=CARTESIAN_POINT('Ctrl Pts',(23.3930740623619,-1.66122520018012,
0.));
#186136=CARTESIAN_POINT('Ctrl Pts',(23.3753637485545,-1.66491731718878,
0.));
#186137=CARTESIAN_POINT('Ctrl Pts',(23.3577648365744,-1.66853425293997,
0.));
#186138=CARTESIAN_POINT('Ctrl Pts',(23.3402785571865,-1.67207631363923,
0.));
#186139=CARTESIAN_POINT('Ctrl Pts',(23.3229061599144,-1.67554381222995,
0.));
#186140=CARTESIAN_POINT('Ctrl Pts',(23.3056489135611,-1.67893706857118,
0.));
#186141=CARTESIAN_POINT('Ctrl Pts',(23.2885081066951,-1.68225640962169,
0.));
#186142=CARTESIAN_POINT('Ctrl Pts',(23.2714850482246,-1.68550216963259,
0.));
#186143=CARTESIAN_POINT('Ctrl Pts',(23.2545810680537,-1.68867469034897,
0.));
#186144=CARTESIAN_POINT('Ctrl Pts',(23.2377975177013,-1.69177432121712,
0.));
#186145=CARTESIAN_POINT('Ctrl Pts',(23.2211357709374,-1.69480141959954,
0.));
#186146=CARTESIAN_POINT('Ctrl Pts',(23.2045972243767,-1.69775635099444,
0.));
#186147=CARTESIAN_POINT('Ctrl Pts',(23.1881832981851,-1.70063948927011,
0.));
#186148=CARTESIAN_POINT('Ctrl Pts',(23.1718954368751,-1.70345121691278,
0.));
#186149=CARTESIAN_POINT('Ctrl Pts',(23.1557351100614,-1.70619192527853,
0.));
#186150=CARTESIAN_POINT('Ctrl Pts',(23.1397038132356,-1.70886201485453,
0.));
#186151=CARTESIAN_POINT('Ctrl Pts',(23.1238030684925,-1.71146189552175,
0.));
#186152=CARTESIAN_POINT('Ctrl Pts',(23.1080344254286,-1.71399198684705,
0.));
#186153=CARTESIAN_POINT('Ctrl Pts',(23.0923994621213,-1.71645271839298,
0.));
#186154=CARTESIAN_POINT('Ctrl Pts',(23.0768997860708,-1.71884453003028,
0.));
#186155=CARTESIAN_POINT('Ctrl Pts',(23.0615370351562,-1.72116787225993,
0.));
#186156=CARTESIAN_POINT('Ctrl Pts',(23.0463128785531,-1.72342320653748,
0.));
#186157=CARTESIAN_POINT('Ctrl Pts',(23.0312290178883,-1.72561100564047,
0.));
#186158=CARTESIAN_POINT('Ctrl Pts',(23.0162871884168,-1.7277317540471,0.));
#186159=CARTESIAN_POINT('Ctrl Pts',(23.001489160189,-1.72978594832137,0.));
#186160=CARTESIAN_POINT('Ctrl Pts',(22.9868367391978,-1.73177409750192,
0.));
#186161=CARTESIAN_POINT('Ctrl Pts',(22.9723317685688,-1.73369672350816,
0.));
#186162=CARTESIAN_POINT('Ctrl Pts',(22.9579761301063,-1.73555436162771,
0.));
#186163=CARTESIAN_POINT('Ctrl Pts',(22.9437717457826,-1.7373475610004,0.));
#186164=CARTESIAN_POINT('Ctrl Pts',(22.9297205792586,-1.73907688511667,
0.));
#186165=CARTESIAN_POINT('Ctrl Pts',(22.9158246373363,-1.7407429123106,0.));
#186166=CARTESIAN_POINT('Ctrl Pts',(22.9020859716141,-1.74234623630081,
0.));
#186167=CARTESIAN_POINT('Ctrl Pts',(22.888506680335,-1.74388746677704,0.));
#186168=CARTESIAN_POINT('Ctrl Pts',(22.8750889101696,-1.74536722998202,
0.));
#186169=CARTESIAN_POINT('Ctrl Pts',(22.8618348580235,-1.74678616930666,
0.));
#186170=CARTESIAN_POINT('Ctrl Pts',(22.8487467728076,-1.74814494588494,
0.));
#186171=CARTESIAN_POINT('Ctrl Pts',(22.8358269579853,-1.74944423940117,
0.));
#186172=CARTESIAN_POINT('Ctrl Pts',(22.8230777741284,-1.75068474890884,
0.));
#186173=CARTESIAN_POINT('Ctrl Pts',(22.8105016414713,-1.75186719365593,
0.));
#186174=CARTESIAN_POINT('Ctrl Pts',(22.7981010424314,-1.75299231391468,
0.));
#186175=CARTESIAN_POINT('Ctrl Pts',(22.7858785242361,-1.75406087182937,
0.));
#186176=CARTESIAN_POINT('Ctrl Pts',(22.7738367016118,-1.75507365227133,
0.));
#186177=CARTESIAN_POINT('Ctrl Pts',(22.7619782595013,-1.75603146371642,
0.));
#186178=CARTESIAN_POINT('Ctrl Pts',(22.750305955645,-1.75693513908908,0.));
#186179=CARTESIAN_POINT('Ctrl Pts',(22.7388226235559,-1.75778553673245,
0.));
#186180=CARTESIAN_POINT('Ctrl Pts',(22.72753117773,-1.75858354204634,0.));
#186181=CARTESIAN_POINT('Ctrl Pts',(22.7164346186006,-1.75933006905926,
0.));
#186182=CARTESIAN_POINT('Ctrl Pts',(22.7055360375485,-1.76002606202402,
0.));
#186183=CARTESIAN_POINT('Ctrl Pts',(22.6948386219851,-1.76067249704888,
0.));
#186184=CARTESIAN_POINT('Ctrl Pts',(22.684345658525,-1.76127038310615,0.));
#186185=CARTESIAN_POINT('Ctrl Pts',(22.67406053567,-1.76182076289527,0.));
#186186=CARTESIAN_POINT('Ctrl Pts',(22.6639867471753,-1.7623247139257,0.));
#186187=CARTESIAN_POINT('Ctrl Pts',(22.6541278938409,-1.76278334912562,
0.));
#186188=CARTESIAN_POINT('Ctrl Pts',(22.6444876940423,-1.76319782013917,
0.));
#186189=CARTESIAN_POINT('Ctrl Pts',(22.6350699979359,-1.76356932176274,
0.));
#186190=CARTESIAN_POINT('Ctrl Pts',(22.6258787994848,-1.76389909571404,
0.));
#186191=CARTESIAN_POINT('Ctrl Pts',(22.6169182517694,-1.76418843543741,
0.));
#186192=CARTESIAN_POINT('Ctrl Pts',(22.6081926681343,-1.76443868648017,
0.));
#186193=CARTESIAN_POINT('Ctrl Pts',(22.5997065145638,-1.76465124413558,
0.));
#186194=CARTESIAN_POINT('Ctrl Pts',(22.5914644078105,-1.76482755288412,
0.));
#186195=CARTESIAN_POINT('Ctrl Pts',(22.5834711038022,-1.76496910283089,
0.));
#186196=CARTESIAN_POINT('Ctrl Pts',(22.5757315316353,-1.76507744026747,
0.));
#186197=CARTESIAN_POINT('Ctrl Pts',(22.5682508499873,-1.76515418518832,
0.));
#186198=CARTESIAN_POINT('Ctrl Pts',(22.5610344912501,-1.76520104500451,
0.));
#186199=CARTESIAN_POINT('Ctrl Pts',(22.5540882235837,-1.76521983384064,
0.));
#186200=CARTESIAN_POINT('Ctrl Pts',(22.5474180954006,-1.76521245524048,
0.));
#186201=CARTESIAN_POINT('Ctrl Pts',(22.5410303590892,-1.76518087841494,
0.));
#186202=CARTESIAN_POINT('Ctrl Pts',(22.5349313983571,-1.76512711563255,
0.));
#186203=CARTESIAN_POINT('Ctrl Pts',(22.529127665298,-1.7650532026276,0.));
#186204=CARTESIAN_POINT('Ctrl Pts',(22.5236259635515,-1.76496128643376,
0.));
#186205=CARTESIAN_POINT('Ctrl Pts',(22.5184336670207,-1.76485369319896,
0.));
#186206=CARTESIAN_POINT('Ctrl Pts',(22.5135590569554,-1.7647330328115,0.));
#186207=CARTESIAN_POINT('Ctrl Pts',(22.5090112700212,-1.76460218257314,
0.));
#186208=CARTESIAN_POINT('Ctrl Pts',(22.5047996391978,-1.76446408210366,
0.));
#186209=CARTESIAN_POINT('Ctrl Pts',(22.5009332677316,-1.76432160068739,
0.));
#186210=CARTESIAN_POINT('Ctrl Pts',(22.4974203063191,-1.76417731243484,
0.));
#186211=CARTESIAN_POINT('Ctrl Pts',(22.4942693792449,-1.76403393880317,
0.));
#186212=CARTESIAN_POINT('Ctrl Pts',(22.4914909094908,-1.76389475965715,
0.));
#186213=CARTESIAN_POINT('Ctrl Pts',(22.4890991659479,-1.76376424879469,
0.));
#186214=CARTESIAN_POINT('Ctrl Pts',(22.4871115206572,-1.76364784232927,
0.));
#186215=CARTESIAN_POINT('Ctrl Pts',(22.4855446605991,-1.7635507604555,0.));
#186216=CARTESIAN_POINT('Ctrl Pts',(22.4844112933125,-1.76347698284863,
0.));
#186217=CARTESIAN_POINT('Ctrl Pts',(22.4838562517064,-1.7634381343466,0.));
#186218=CARTESIAN_POINT('Ctrl Pts',(22.4836387052228,-1.76342064263638,
0.));
#186219=CARTESIAN_POINT('Ctrl Pts',(22.4835819929788,-1.76341415538792,
0.));
#186220=CARTESIAN_POINT('Ctrl Pts',(22.4835757167854,-1.76341220531181,
0.));
#186221=CARTESIAN_POINT('',(25.991588367311,-0.661312440730916,0.));
#186222=CARTESIAN_POINT('Ctrl Pts',(22.1738711152697,-4.11585220600463,
0.));
#186223=CARTESIAN_POINT('Ctrl Pts',(22.1738711152697,-4.11585220600463,
12.));
#186224=CARTESIAN_POINT('Ctrl Pts',(22.173877682324,-4.11585194677443,0.));
#186225=CARTESIAN_POINT('Ctrl Pts',(22.173877682324,-4.11585194677443,12.));
#186226=CARTESIAN_POINT('Ctrl Pts',(22.1739341411687,-4.11586035878288,
0.));
#186227=CARTESIAN_POINT('Ctrl Pts',(22.1739341411687,-4.11586035878288,
12.));
#186228=CARTESIAN_POINT('Ctrl Pts',(22.1741488021234,-4.11589976826168,
0.));
#186229=CARTESIAN_POINT('Ctrl Pts',(22.1741488021234,-4.11589976826168,
12.));
#186230=CARTESIAN_POINT('Ctrl Pts',(22.1746949858775,-4.11600589882846,
0.));
#186231=CARTESIAN_POINT('Ctrl Pts',(22.1746949858775,-4.11600589882846,
12.));
#186232=CARTESIAN_POINT('Ctrl Pts',(22.1758088296598,-4.1162279721707,0.));
#186233=CARTESIAN_POINT('Ctrl Pts',(22.1758088296598,-4.1162279721707,12.));
#186234=CARTESIAN_POINT('Ctrl Pts',(22.177347426894,-4.11653973150519,0.));
#186235=CARTESIAN_POINT('Ctrl Pts',(22.177347426894,-4.11653973150519,12.));
#186236=CARTESIAN_POINT('Ctrl Pts',(22.179297473024,-4.11694173195005,0.));
#186237=CARTESIAN_POINT('Ctrl Pts',(22.179297473024,-4.11694173195005,12.));
#186238=CARTESIAN_POINT('Ctrl Pts',(22.1816414985788,-4.11743469691757,
0.));
#186239=CARTESIAN_POINT('Ctrl Pts',(22.1816414985788,-4.11743469691757,
12.));
#186240=CARTESIAN_POINT('Ctrl Pts',(22.1843613164855,-4.11801938107481,
0.));
#186241=CARTESIAN_POINT('Ctrl Pts',(22.1843613164855,-4.11801938107481,
12.));
#186242=CARTESIAN_POINT('Ctrl Pts',(22.1874419861496,-4.11869641271775,
0.));
#186243=CARTESIAN_POINT('Ctrl Pts',(22.1874419861496,-4.11869641271775,
12.));
#186244=CARTESIAN_POINT('Ctrl Pts',(22.1908725908525,-4.11946626228637,
0.));
#186245=CARTESIAN_POINT('Ctrl Pts',(22.1908725908525,-4.11946626228637,
12.));
#186246=CARTESIAN_POINT('Ctrl Pts',(22.1946440958098,-4.12032932637738,
0.));
#186247=CARTESIAN_POINT('Ctrl Pts',(22.1946440958098,-4.12032932637738,
12.));
#186248=CARTESIAN_POINT('Ctrl Pts',(22.1987479618246,-4.12128598183523,
0.));
#186249=CARTESIAN_POINT('Ctrl Pts',(22.1987479618246,-4.12128598183523,
12.));
#186250=CARTESIAN_POINT('Ctrl Pts',(22.2031746532106,-4.12233664408228,
0.));
#186251=CARTESIAN_POINT('Ctrl Pts',(22.2031746532106,-4.12233664408228,
12.));
#186252=CARTESIAN_POINT('Ctrl Pts',(22.2079143941719,-4.12348173702024,
0.));
#186253=CARTESIAN_POINT('Ctrl Pts',(22.2079143941719,-4.12348173702024,
12.));
#186254=CARTESIAN_POINT('Ctrl Pts',(22.2129576146671,-4.12472167516608,
0.));
#186255=CARTESIAN_POINT('Ctrl Pts',(22.2129576146671,-4.12472167516608,
12.));
#186256=CARTESIAN_POINT('Ctrl Pts',(22.2182956401341,-4.12605683613308,
0.));
#186257=CARTESIAN_POINT('Ctrl Pts',(22.2182956401341,-4.12605683613308,
12.));
#186258=CARTESIAN_POINT('Ctrl Pts',(22.2239207458781,-4.12748755830105,
0.));
#186259=CARTESIAN_POINT('Ctrl Pts',(22.2239207458781,-4.12748755830105,
12.));
#186260=CARTESIAN_POINT('Ctrl Pts',(22.2298258043947,-4.1290141546338,0.));
#186261=CARTESIAN_POINT('Ctrl Pts',(22.2298258043947,-4.1290141546338,12.));
#186262=CARTESIAN_POINT('Ctrl Pts',(22.2360040565533,-4.13063692157499,
0.));
#186263=CARTESIAN_POINT('Ctrl Pts',(22.2360040565533,-4.13063692157499,
12.));
#186264=CARTESIAN_POINT('Ctrl Pts',(22.2424488153523,-4.13235615060161,
0.));
#186265=CARTESIAN_POINT('Ctrl Pts',(22.2424488153523,-4.13235615060161,
12.));
#186266=CARTESIAN_POINT('Ctrl Pts',(22.249153531779,-4.13417212558811,0.));
#186267=CARTESIAN_POINT('Ctrl Pts',(22.249153531779,-4.13417212558811,12.));
#186268=CARTESIAN_POINT('Ctrl Pts',(22.2561118708421,-4.13608511977227,
0.));
#186269=CARTESIAN_POINT('Ctrl Pts',(22.2561118708421,-4.13608511977227,
12.));
#186270=CARTESIAN_POINT('Ctrl Pts',(22.2633177913972,-4.13809539255423,
0.));
#186271=CARTESIAN_POINT('Ctrl Pts',(22.2633177913972,-4.13809539255423,
12.));
#186272=CARTESIAN_POINT('Ctrl Pts',(22.2707656042457,-4.14020318715992,
0.));
#186273=CARTESIAN_POINT('Ctrl Pts',(22.2707656042457,-4.14020318715992,
12.));
#186274=CARTESIAN_POINT('Ctrl Pts',(22.2784499072027,-4.14240873321985,
0.));
#186275=CARTESIAN_POINT('Ctrl Pts',(22.2784499072027,-4.14240873321985,
12.));
#186276=CARTESIAN_POINT('Ctrl Pts',(22.2863655389166,-4.14471224859297,
0.));
#186277=CARTESIAN_POINT('Ctrl Pts',(22.2863655389166,-4.14471224859297,
12.));
#186278=CARTESIAN_POINT('Ctrl Pts',(22.2945075198467,-4.14711394168557,
0.));
#186279=CARTESIAN_POINT('Ctrl Pts',(22.2945075198467,-4.14711394168557,
12.));
#186280=CARTESIAN_POINT('Ctrl Pts',(22.3028710166933,-4.14961401285523,
0.));
#186281=CARTESIAN_POINT('Ctrl Pts',(22.3028710166933,-4.14961401285523,
12.));
#186282=CARTESIAN_POINT('Ctrl Pts',(22.3114513545185,-4.15221265396991,
0.));
#186283=CARTESIAN_POINT('Ctrl Pts',(22.3114513545185,-4.15221265396991,
12.));
#186284=CARTESIAN_POINT('Ctrl Pts',(22.3202440186979,-4.15491004835282,
0.));
#186285=CARTESIAN_POINT('Ctrl Pts',(22.3202440186979,-4.15491004835282,
12.));
#186286=CARTESIAN_POINT('Ctrl Pts',(22.3292446628959,-4.15770637047891,
0.));
#186287=CARTESIAN_POINT('Ctrl Pts',(22.3292446628959,-4.15770637047891,
12.));
#186288=CARTESIAN_POINT('Ctrl Pts',(22.3384491078602,-4.16060178604165,
0.));
#186289=CARTESIAN_POINT('Ctrl Pts',(22.3384491078602,-4.16060178604165,
12.));
#186290=CARTESIAN_POINT('Ctrl Pts',(22.3478533253889,-4.16359645263189,
0.));
#186291=CARTESIAN_POINT('Ctrl Pts',(22.3478533253889,-4.16359645263189,
12.));
#186292=CARTESIAN_POINT('Ctrl Pts',(22.3574534257396,-4.16669052026601,
0.));
#186293=CARTESIAN_POINT('Ctrl Pts',(22.3574534257396,-4.16669052026601,
12.));
#186294=CARTESIAN_POINT('Ctrl Pts',(22.3672456427599,-4.16988413199458,
0.));
#186295=CARTESIAN_POINT('Ctrl Pts',(22.3672456427599,-4.16988413199458,
12.));
#186296=CARTESIAN_POINT('Ctrl Pts',(22.3772263228617,-4.17317742436146,
0.));
#186297=CARTESIAN_POINT('Ctrl Pts',(22.3772263228617,-4.17317742436146,
12.));
#186298=CARTESIAN_POINT('Ctrl Pts',(22.3873919231334,-4.17657052752826,
0.));
#186299=CARTESIAN_POINT('Ctrl Pts',(22.3873919231334,-4.17657052752826,
12.));
#186300=CARTESIAN_POINT('Ctrl Pts',(22.3977390078075,-4.18006356544883,
0.));
#186301=CARTESIAN_POINT('Ctrl Pts',(22.3977390078075,-4.18006356544883,
12.));
#186302=CARTESIAN_POINT('Ctrl Pts',(22.4082642454453,-4.18365665600852,
0.));
#186303=CARTESIAN_POINT('Ctrl Pts',(22.4082642454453,-4.18365665600852,
12.));
#186304=CARTESIAN_POINT('Ctrl Pts',(22.4189644056115,-4.18734991117722,
0.));
#186305=CARTESIAN_POINT('Ctrl Pts',(22.4189644056115,-4.18734991117722,
12.));
#186306=CARTESIAN_POINT('Ctrl Pts',(22.4298363535421,-4.19114343726943,
0.));
#186307=CARTESIAN_POINT('Ctrl Pts',(22.4298363535421,-4.19114343726943,
12.));
#186308=CARTESIAN_POINT('Ctrl Pts',(22.4408770448917,-4.19503733518862,
0.));
#186309=CARTESIAN_POINT('Ctrl Pts',(22.4408770448917,-4.19503733518862,
12.));
#186310=CARTESIAN_POINT('Ctrl Pts',(22.4520835205419,-4.19903170066356,
0.));
#186311=CARTESIAN_POINT('Ctrl Pts',(22.4520835205419,-4.19903170066356,
12.));
#186312=CARTESIAN_POINT('Ctrl Pts',(22.4634529011433,-4.20312662448172,
0.));
#186313=CARTESIAN_POINT('Ctrl Pts',(22.4634529011433,-4.20312662448172,
12.));
#186314=CARTESIAN_POINT('Ctrl Pts',(22.4749823839915,-4.20732219265649,
0.));
#186315=CARTESIAN_POINT('Ctrl Pts',(22.4749823839915,-4.20732219265649,
12.));
#186316=CARTESIAN_POINT('Ctrl Pts',(22.4866692403147,-4.21161848657429,
0.));
#186317=CARTESIAN_POINT('Ctrl Pts',(22.4866692403147,-4.21161848657429,
12.));
#186318=CARTESIAN_POINT('Ctrl Pts',(22.4985108124229,-4.21601558313909,
0.));
#186319=CARTESIAN_POINT('Ctrl Pts',(22.4985108124229,-4.21601558313909,
12.));
#186320=CARTESIAN_POINT('Ctrl Pts',(22.5105045108882,-4.22051355490198,
0.));
#186321=CARTESIAN_POINT('Ctrl Pts',(22.5105045108882,-4.22051355490198,
12.));
#186322=CARTESIAN_POINT('Ctrl Pts',(22.5226478117885,-4.22511247020041,
0.));
#186323=CARTESIAN_POINT('Ctrl Pts',(22.5226478117885,-4.22511247020041,
12.));
#186324=CARTESIAN_POINT('Ctrl Pts',(22.5349382540587,-4.22981239330733,
0.));
#186325=CARTESIAN_POINT('Ctrl Pts',(22.5349382540587,-4.22981239330733,
12.));
#186326=CARTESIAN_POINT('Ctrl Pts',(22.5473734368086,-4.23461338456714,
0.));
#186327=CARTESIAN_POINT('Ctrl Pts',(22.5473734368086,-4.23461338456714,
12.));
#186328=CARTESIAN_POINT('Ctrl Pts',(22.559951016643,-4.23951550052527,0.));
#186329=CARTESIAN_POINT('Ctrl Pts',(22.559951016643,-4.23951550052527,12.));
#186330=CARTESIAN_POINT('Ctrl Pts',(22.5726687049922,-4.2445187940486,0.));
#186331=CARTESIAN_POINT('Ctrl Pts',(22.5726687049922,-4.2445187940486,12.));
#186332=CARTESIAN_POINT('Ctrl Pts',(22.5855242662479,-4.24962331444186,
0.));
#186333=CARTESIAN_POINT('Ctrl Pts',(22.5855242662479,-4.24962331444186,
12.));
#186334=CARTESIAN_POINT('Ctrl Pts',(22.5985155158637,-4.25482910755486,
0.));
#186335=CARTESIAN_POINT('Ctrl Pts',(22.5985155158637,-4.25482910755486,
12.));
#186336=CARTESIAN_POINT('Ctrl Pts',(22.611640318482,-4.26013621588304,0.));
#186337=CARTESIAN_POINT('Ctrl Pts',(22.611640318482,-4.26013621588304,12.));
#186338=CARTESIAN_POINT('Ctrl Pts',(22.6248965859975,-4.26554467865572,
0.));
#186339=CARTESIAN_POINT('Ctrl Pts',(22.6248965859975,-4.26554467865572,
12.));
#186340=CARTESIAN_POINT('Ctrl Pts',(22.6382822758171,-4.27105453193,0.));
#186341=CARTESIAN_POINT('Ctrl Pts',(22.6382822758171,-4.27105453193,12.));
#186342=CARTESIAN_POINT('Ctrl Pts',(22.6517953893303,-4.27666580869118,
0.));
#186343=CARTESIAN_POINT('Ctrl Pts',(22.6517953893303,-4.27666580869118,
12.));
#186344=CARTESIAN_POINT('Ctrl Pts',(22.665433970311,-4.2823785389406,0.));
#186345=CARTESIAN_POINT('Ctrl Pts',(22.665433970311,-4.2823785389406,12.));
#186346=CARTESIAN_POINT('Ctrl Pts',(22.6791961033536,-4.28819274977767,
0.));
#186347=CARTESIAN_POINT('Ctrl Pts',(22.6791961033536,-4.28819274977767,
12.));
#186348=CARTESIAN_POINT('Ctrl Pts',(22.6930799122545,-4.29410846547062,
0.));
#186349=CARTESIAN_POINT('Ctrl Pts',(22.6930799122545,-4.29410846547062,
12.));
#186350=CARTESIAN_POINT('Ctrl Pts',(22.707083558756,-4.30012570754067,0.));
#186351=CARTESIAN_POINT('Ctrl Pts',(22.707083558756,-4.30012570754067,12.));
#186352=CARTESIAN_POINT('Ctrl Pts',(22.7212052413384,-4.30624449484075,
0.));
#186353=CARTESIAN_POINT('Ctrl Pts',(22.7212052413384,-4.30624449484075,
12.));
#186354=CARTESIAN_POINT('Ctrl Pts',(22.7354431939926,-4.31246484362551,
0.));
#186355=CARTESIAN_POINT('Ctrl Pts',(22.7354431939926,-4.31246484362551,
12.));
#186356=CARTESIAN_POINT('Ctrl Pts',(22.7497956849852,-4.31878676761231,
0.));
#186357=CARTESIAN_POINT('Ctrl Pts',(22.7497956849852,-4.31878676761231,
12.));
#186358=CARTESIAN_POINT('Ctrl Pts',(22.764261015648,-4.32521027803748,0.));
#186359=CARTESIAN_POINT('Ctrl Pts',(22.764261015648,-4.32521027803748,12.));
#186360=CARTESIAN_POINT('Ctrl Pts',(22.7788375194081,-4.33173538373183,
0.));
#186361=CARTESIAN_POINT('Ctrl Pts',(22.7788375194081,-4.33173538373183,
12.));
#186362=CARTESIAN_POINT('Ctrl Pts',(22.7935235607807,-4.33836209118444,
0.));
#186363=CARTESIAN_POINT('Ctrl Pts',(22.7935235607807,-4.33836209118444,
12.));
#186364=CARTESIAN_POINT('Ctrl Pts',(22.808317534379,-4.34509040460066,0.));
#186365=CARTESIAN_POINT('Ctrl Pts',(22.808317534379,-4.34509040460066,12.));
#186366=CARTESIAN_POINT('Ctrl Pts',(22.8232178638873,-4.35192032594802,
0.));
#186367=CARTESIAN_POINT('Ctrl Pts',(22.8232178638873,-4.35192032594802,
12.));
#186368=CARTESIAN_POINT('Ctrl Pts',(22.838223001118,-4.3588518550056,0.));
#186369=CARTESIAN_POINT('Ctrl Pts',(22.838223001118,-4.3588518550056,12.));
#186370=CARTESIAN_POINT('Ctrl Pts',(22.8533314252419,-4.36588498943011,
0.));
#186371=CARTESIAN_POINT('Ctrl Pts',(22.8533314252419,-4.36588498943011,
12.));
#186372=CARTESIAN_POINT('Ctrl Pts',(22.8685416419725,-4.37301972480753,
0.));
#186373=CARTESIAN_POINT('Ctrl Pts',(22.8685416419725,-4.37301972480753,
12.));
#186374=CARTESIAN_POINT('Ctrl Pts',(22.8838521827702,-4.38025605470091,
0.));
#186375=CARTESIAN_POINT('Ctrl Pts',(22.8838521827702,-4.38025605470091,
12.));
#186376=CARTESIAN_POINT('Ctrl Pts',(22.8992616040108,-4.38759397068393,
0.));
#186377=CARTESIAN_POINT('Ctrl Pts',(22.8992616040108,-4.38759397068393,
12.));
#186378=CARTESIAN_POINT('Ctrl Pts',(22.9147684862425,-4.39503346238455,
0.));
#186379=CARTESIAN_POINT('Ctrl Pts',(22.9147684862425,-4.39503346238455,
12.));
#186380=CARTESIAN_POINT('Ctrl Pts',(22.9303714335549,-4.40257451754309,
0.));
#186381=CARTESIAN_POINT('Ctrl Pts',(22.9303714335549,-4.40257451754309,
12.));
#186382=CARTESIAN_POINT('Ctrl Pts',(22.9460690729092,-4.41021712205549,
0.));
#186383=CARTESIAN_POINT('Ctrl Pts',(22.9460690729092,-4.41021712205549,
12.));
#186384=CARTESIAN_POINT('Ctrl Pts',(22.9618600534866,-4.41796126001311,
0.));
#186385=CARTESIAN_POINT('Ctrl Pts',(22.9618600534866,-4.41796126001311,
12.));
#186386=CARTESIAN_POINT('Ctrl Pts',(22.9777430460021,-4.42580691372772,
0.));
#186387=CARTESIAN_POINT('Ctrl Pts',(22.9777430460021,-4.42580691372772,
12.));
#186388=CARTESIAN_POINT('Ctrl Pts',(22.9937167421009,-4.43375406376906,
0.));
#186389=CARTESIAN_POINT('Ctrl Pts',(22.9937167421009,-4.43375406376906,
12.));
#186390=CARTESIAN_POINT('Ctrl Pts',(23.0097798538399,-4.44180268901667,
0.));
#186391=CARTESIAN_POINT('Ctrl Pts',(23.0097798538399,-4.44180268901667,
12.));
#186392=CARTESIAN_POINT('Ctrl Pts',(23.0259311131395,-4.44995276669699,
0.));
#186393=CARTESIAN_POINT('Ctrl Pts',(23.0259311131395,-4.44995276669699,
12.));
#186394=CARTESIAN_POINT('Ctrl Pts',(23.0421692712466,-4.45820427241678,
0.));
#186395=CARTESIAN_POINT('Ctrl Pts',(23.0421692712466,-4.45820427241678,
12.));
#186396=CARTESIAN_POINT('Ctrl Pts',(23.0584930981723,-4.46655718018206,
0.));
#186397=CARTESIAN_POINT('Ctrl Pts',(23.0584930981723,-4.46655718018206,
12.));
#186398=CARTESIAN_POINT('Ctrl Pts',(23.0749013821867,-4.47501146242822,
0.));
#186399=CARTESIAN_POINT('Ctrl Pts',(23.0749013821867,-4.47501146242822,
12.));
#186400=CARTESIAN_POINT('Ctrl Pts',(23.0913929293909,-4.48356709006757,
0.));
#186401=CARTESIAN_POINT('Ctrl Pts',(23.0913929293909,-4.48356709006757,
12.));
#186402=CARTESIAN_POINT('Ctrl Pts',(23.1079665632629,-4.49222403252202,
0.));
#186403=CARTESIAN_POINT('Ctrl Pts',(23.1079665632629,-4.49222403252202,
12.));
#186404=CARTESIAN_POINT('Ctrl Pts',(23.1246211242117,-4.5009822577518,0.));
#186405=CARTESIAN_POINT('Ctrl Pts',(23.1246211242117,-4.5009822577518,12.));
#186406=CARTESIAN_POINT('Ctrl Pts',(23.1413554691136,-4.50984173227088,
0.));
#186407=CARTESIAN_POINT('Ctrl Pts',(23.1413554691136,-4.50984173227088,
12.));
#186408=CARTESIAN_POINT('Ctrl Pts',(23.1581684708778,-4.51880242116786,
0.));
#186409=CARTESIAN_POINT('Ctrl Pts',(23.1581684708778,-4.51880242116786,
12.));
#186410=CARTESIAN_POINT('Ctrl Pts',(23.1750590180923,-4.52786428815049,
0.));
#186411=CARTESIAN_POINT('Ctrl Pts',(23.1750590180923,-4.52786428815049,
12.));
#186412=CARTESIAN_POINT('Ctrl Pts',(23.1920260146474,-4.53702729557586,
0.));
#186413=CARTESIAN_POINT('Ctrl Pts',(23.1920260146474,-4.53702729557586,
12.));
#186414=CARTESIAN_POINT('Ctrl Pts',(23.2090683793627,-4.54629140447543,
0.));
#186415=CARTESIAN_POINT('Ctrl Pts',(23.2090683793627,-4.54629140447543,
12.));
#186416=CARTESIAN_POINT('Ctrl Pts',(23.2261850456054,-4.55565657456957,
0.));
#186417=CARTESIAN_POINT('Ctrl Pts',(23.2261850456054,-4.55565657456957,
12.));
#186418=CARTESIAN_POINT('Ctrl Pts',(23.2433749609117,-4.56512276427812,
0.));
#186419=CARTESIAN_POINT('Ctrl Pts',(23.2433749609117,-4.56512276427812,
12.));
#186420=CARTESIAN_POINT('Ctrl Pts',(23.2606370866853,-4.57468993076071,
0.));
#186421=CARTESIAN_POINT('Ctrl Pts',(23.2606370866853,-4.57468993076071,
12.));
#186422=CARTESIAN_POINT('Ctrl Pts',(23.2779703978868,-4.58435802994675,
0.));
#186423=CARTESIAN_POINT('Ctrl Pts',(23.2779703978868,-4.58435802994675,
12.));
#186424=CARTESIAN_POINT('Ctrl Pts',(23.295373882719,-4.59412701655751,0.));
#186425=CARTESIAN_POINT('Ctrl Pts',(23.295373882719,-4.59412701655751,12.));
#186426=CARTESIAN_POINT('Ctrl Pts',(23.3128465423119,-4.60399684412176,
0.));
#186427=CARTESIAN_POINT('Ctrl Pts',(23.3128465423119,-4.60399684412176,
12.));
#186428=CARTESIAN_POINT('Ctrl Pts',(23.3303873903947,-4.6139674649785,0.));
#186429=CARTESIAN_POINT('Ctrl Pts',(23.3303873903947,-4.6139674649785,12.));
#186430=CARTESIAN_POINT('Ctrl Pts',(23.3479954530281,-4.62403883030825,
0.));
#186431=CARTESIAN_POINT('Ctrl Pts',(23.3479954530281,-4.62403883030825,
12.));
#186432=CARTESIAN_POINT('Ctrl Pts',(23.3656697683496,-4.63421089016556,
0.));
#186433=CARTESIAN_POINT('Ctrl Pts',(23.3656697683496,-4.63421089016556,
12.));
#186434=CARTESIAN_POINT('Ctrl Pts',(23.383409386307,-4.64448359349936,0.));
#186435=CARTESIAN_POINT('Ctrl Pts',(23.383409386307,-4.64448359349936,12.));
#186436=CARTESIAN_POINT('Ctrl Pts',(23.4012133683957,-4.65485688816923,
0.));
#186437=CARTESIAN_POINT('Ctrl Pts',(23.4012133683957,-4.65485688816923,
12.));
#186438=CARTESIAN_POINT('Ctrl Pts',(23.4190807873798,-4.66533072094664,
0.));
#186439=CARTESIAN_POINT('Ctrl Pts',(23.4190807873798,-4.66533072094664,
12.));
#186440=CARTESIAN_POINT('Ctrl Pts',(23.4370107270444,-4.67590503753051,
0.));
#186441=CARTESIAN_POINT('Ctrl Pts',(23.4370107270444,-4.67590503753051,
12.));
#186442=CARTESIAN_POINT('Ctrl Pts',(23.4550022819852,-4.68657978258298,
0.));
#186443=CARTESIAN_POINT('Ctrl Pts',(23.4550022819852,-4.68657978258298,
12.));
#186444=CARTESIAN_POINT('Ctrl Pts',(23.4730545573849,-4.69735489975024,
0.));
#186445=CARTESIAN_POINT('Ctrl Pts',(23.4730545573849,-4.69735489975024,
12.));
#186446=CARTESIAN_POINT('Ctrl Pts',(23.491166668789,-4.70823033167821,0.));
#186447=CARTESIAN_POINT('Ctrl Pts',(23.491166668789,-4.70823033167821,12.));
#186448=CARTESIAN_POINT('Ctrl Pts',(23.5093377418784,-4.71920602001905,
0.));
#186449=CARTESIAN_POINT('Ctrl Pts',(23.5093377418784,-4.71920602001905,
12.));
#186450=CARTESIAN_POINT('Ctrl Pts',(23.5275669122378,-4.73028190543032,
0.));
#186451=CARTESIAN_POINT('Ctrl Pts',(23.5275669122378,-4.73028190543032,
12.));
#186452=CARTESIAN_POINT('Ctrl Pts',(23.5458533251715,-4.74145792760699,
0.));
#186453=CARTESIAN_POINT('Ctrl Pts',(23.5458533251715,-4.74145792760699,
12.));
#186454=CARTESIAN_POINT('Ctrl Pts',(23.564196135517,-4.75273402530616,0.));
#186455=CARTESIAN_POINT('Ctrl Pts',(23.564196135517,-4.75273402530616,12.));
#186456=CARTESIAN_POINT('Ctrl Pts',(23.5825945074535,-4.76411013636252,
0.));
#186457=CARTESIAN_POINT('Ctrl Pts',(23.5825945074535,-4.76411013636252,
12.));
#186458=CARTESIAN_POINT('Ctrl Pts',(23.6010476143099,-4.77558619769876,
0.));
#186459=CARTESIAN_POINT('Ctrl Pts',(23.6010476143099,-4.77558619769876,
12.));
#186460=CARTESIAN_POINT('Ctrl Pts',(23.6195546383625,-4.78716214532105,
0.));
#186461=CARTESIAN_POINT('Ctrl Pts',(23.6195546383625,-4.78716214532105,
12.));
#186462=CARTESIAN_POINT('Ctrl Pts',(23.6381147706581,-4.79883791433231,
0.));
#186463=CARTESIAN_POINT('Ctrl Pts',(23.6381147706581,-4.79883791433231,
12.));
#186464=CARTESIAN_POINT('Ctrl Pts',(23.6567272108631,-4.81061343896443,
0.));
#186465=CARTESIAN_POINT('Ctrl Pts',(23.6567272108631,-4.81061343896443,
12.));
#186466=CARTESIAN_POINT('Ctrl Pts',(23.6753911671023,-4.82248865259571,
0.));
#186467=CARTESIAN_POINT('Ctrl Pts',(23.6753911671023,-4.82248865259571,
12.));
#186468=CARTESIAN_POINT('Ctrl Pts',(23.6941058557971,-4.83446348776268,
0.));
#186469=CARTESIAN_POINT('Ctrl Pts',(23.6941058557971,-4.83446348776268,
12.));
#186470=CARTESIAN_POINT('Ctrl Pts',(23.7128705015014,-4.84653787616424,
0.));
#186471=CARTESIAN_POINT('Ctrl Pts',(23.7128705015014,-4.84653787616424,
12.));
#186472=CARTESIAN_POINT('Ctrl Pts',(23.7316843367308,-4.85871174865493,
0.));
#186473=CARTESIAN_POINT('Ctrl Pts',(23.7316843367308,-4.85871174865493,
12.));
#186474=CARTESIAN_POINT('Ctrl Pts',(23.7505466018239,-4.87098503527144,
0.));
#186475=CARTESIAN_POINT('Ctrl Pts',(23.7505466018239,-4.87098503527144,
12.));
#186476=CARTESIAN_POINT('Ctrl Pts',(23.7694565448044,-4.88335766525566,
0.));
#186477=CARTESIAN_POINT('Ctrl Pts',(23.7694565448044,-4.88335766525566,
12.));
#186478=CARTESIAN_POINT('Ctrl Pts',(23.7884134212381,-4.89582956706772,
0.));
#186479=CARTESIAN_POINT('Ctrl Pts',(23.7884134212381,-4.89582956706772,
12.));
#186480=CARTESIAN_POINT('Ctrl Pts',(23.8074164940897,-4.90840066839348,
0.));
#186481=CARTESIAN_POINT('Ctrl Pts',(23.8074164940897,-4.90840066839348,
12.));
#186482=CARTESIAN_POINT('Ctrl Pts',(23.8264650335721,-4.92107089613978,
0.));
#186483=CARTESIAN_POINT('Ctrl Pts',(23.8264650335721,-4.92107089613978,
12.));
#186484=CARTESIAN_POINT('Ctrl Pts',(23.8455583170062,-4.93384017643443,
0.));
#186485=CARTESIAN_POINT('Ctrl Pts',(23.8455583170062,-4.93384017643443,
12.));
#186486=CARTESIAN_POINT('Ctrl Pts',(23.8646956287172,-4.94670843465869,
0.));
#186487=CARTESIAN_POINT('Ctrl Pts',(23.8646956287172,-4.94670843465869,
12.));
#186488=CARTESIAN_POINT('Ctrl Pts',(23.883876259922,-4.95967559546566,0.));
#186489=CARTESIAN_POINT('Ctrl Pts',(23.883876259922,-4.95967559546566,12.));
#186490=CARTESIAN_POINT('Ctrl Pts',(23.9030995086164,-4.9727415827923,0.));
#186491=CARTESIAN_POINT('Ctrl Pts',(23.9030995086164,-4.9727415827923,12.));
#186492=CARTESIAN_POINT('Ctrl Pts',(23.9223646794591,-4.98590631986534,
0.));
#186493=CARTESIAN_POINT('Ctrl Pts',(23.9223646794591,-4.98590631986534,
12.));
#186494=CARTESIAN_POINT('Ctrl Pts',(23.9416710836528,-4.9991697291931,0.));
#186495=CARTESIAN_POINT('Ctrl Pts',(23.9416710836528,-4.9991697291931,12.));
#186496=CARTESIAN_POINT('Ctrl Pts',(23.9610180388271,-5.01253173257459,
0.));
#186497=CARTESIAN_POINT('Ctrl Pts',(23.9610180388271,-5.01253173257459,
12.));
#186498=CARTESIAN_POINT('Ctrl Pts',(23.9804048689228,-5.02599225112462,
0.));
#186499=CARTESIAN_POINT('Ctrl Pts',(23.9804048689228,-5.02599225112462,
12.));
#186500=CARTESIAN_POINT('Ctrl Pts',(23.9998309040747,-5.03955120528528,
0.));
#186501=CARTESIAN_POINT('Ctrl Pts',(23.9998309040747,-5.03955120528528,
12.));
#186502=CARTESIAN_POINT('Ctrl Pts',(24.0192954804896,-5.05320851483069,
0.));
#186503=CARTESIAN_POINT('Ctrl Pts',(24.0192954804896,-5.05320851483069,
12.));
#186504=CARTESIAN_POINT('Ctrl Pts',(24.0387979403268,-5.0669640988664,0.));
#186505=CARTESIAN_POINT('Ctrl Pts',(24.0387979403268,-5.0669640988664,12.));
#186506=CARTESIAN_POINT('Ctrl Pts',(24.0583376315636,-5.08081787581271,
0.));
#186507=CARTESIAN_POINT('Ctrl Pts',(24.0583376315636,-5.08081787581271,
12.));
#186508=CARTESIAN_POINT('Ctrl Pts',(24.0779139079264,-5.09476976342618,
0.));
#186509=CARTESIAN_POINT('Ctrl Pts',(24.0779139079264,-5.09476976342618,
12.));
#186510=CARTESIAN_POINT('Ctrl Pts',(24.0975261288444,-5.10881967883126,
0.));
#186511=CARTESIAN_POINT('Ctrl Pts',(24.0975261288444,-5.10881967883126,
12.));
#186512=CARTESIAN_POINT('Ctrl Pts',(24.117173659394,-5.12296753853858,0.));
#186513=CARTESIAN_POINT('Ctrl Pts',(24.117173659394,-5.12296753853858,12.));
#186514=CARTESIAN_POINT('Ctrl Pts',(24.1368558702443,-5.13721325845746,
0.));
#186515=CARTESIAN_POINT('Ctrl Pts',(24.1368558702443,-5.13721325845746,
12.));
#186516=CARTESIAN_POINT('Ctrl Pts',(24.1565721375971,-5.1515567539008,0.));
#186517=CARTESIAN_POINT('Ctrl Pts',(24.1565721375971,-5.1515567539008,12.));
#186518=CARTESIAN_POINT('Ctrl Pts',(24.1763218431344,-5.16599793957987,
0.));
#186519=CARTESIAN_POINT('Ctrl Pts',(24.1763218431344,-5.16599793957987,
12.));
#186520=CARTESIAN_POINT('Ctrl Pts',(24.1961043738755,-5.180536729614,0.));
#186521=CARTESIAN_POINT('Ctrl Pts',(24.1961043738755,-5.180536729614,12.));
#186522=CARTESIAN_POINT('Ctrl Pts',(24.2159191220171,-5.19517303753648,
0.));
#186523=CARTESIAN_POINT('Ctrl Pts',(24.2159191220171,-5.19517303753648,
12.));
#186524=CARTESIAN_POINT('Ctrl Pts',(24.2357654847766,-5.20990677629177,
0.));
#186525=CARTESIAN_POINT('Ctrl Pts',(24.2357654847766,-5.20990677629177,
12.));
#186526=CARTESIAN_POINT('Ctrl Pts',(24.2556428642294,-5.22473785822443,
0.));
#186527=CARTESIAN_POINT('Ctrl Pts',(24.2556428642294,-5.22473785822443,
12.));
#186528=CARTESIAN_POINT('Ctrl Pts',(24.2755506671525,-5.2396661950629,0.));
#186529=CARTESIAN_POINT('Ctrl Pts',(24.2755506671525,-5.2396661950629,12.));
#186530=CARTESIAN_POINT('Ctrl Pts',(24.2954883048447,-5.25469169788858,
0.));
#186531=CARTESIAN_POINT('Ctrl Pts',(24.2954883048447,-5.25469169788858,
12.));
#186532=CARTESIAN_POINT('Ctrl Pts',(24.3154551932221,-5.269814277188,0.));
#186533=CARTESIAN_POINT('Ctrl Pts',(24.3154551932221,-5.269814277188,12.));
#186534=CARTESIAN_POINT('Ctrl Pts',(24.3354507529414,-5.28503384290649,
0.));
#186535=CARTESIAN_POINT('Ctrl Pts',(24.3354507529414,-5.28503384290649,
12.));
#186536=CARTESIAN_POINT('Ctrl Pts',(24.3554744095075,-5.30035030449065,
0.));
#186537=CARTESIAN_POINT('Ctrl Pts',(24.3554744095075,-5.30035030449065,
12.));
#186538=CARTESIAN_POINT('Ctrl Pts',(24.3755255933917,-5.31576357092527,
0.));
#186539=CARTESIAN_POINT('Ctrl Pts',(24.3755255933917,-5.31576357092527,
12.));
#186540=CARTESIAN_POINT('Ctrl Pts',(24.3956037401293,-5.33127355076035,
0.));
#186541=CARTESIAN_POINT('Ctrl Pts',(24.3956037401293,-5.33127355076035,
12.));
#186542=CARTESIAN_POINT('Ctrl Pts',(24.4157082904614,-5.34688015213538,
0.));
#186543=CARTESIAN_POINT('Ctrl Pts',(24.4157082904614,-5.34688015213538,
12.));
#186544=CARTESIAN_POINT('Ctrl Pts',(24.435838689915,-5.36258328273628,0.));
#186545=CARTESIAN_POINT('Ctrl Pts',(24.435838689915,-5.36258328273628,12.));
#186546=CARTESIAN_POINT('Ctrl Pts',(24.4559943883157,-5.37838284973696,
0.));
#186547=CARTESIAN_POINT('Ctrl Pts',(24.4559943883157,-5.37838284973696,
12.));
#186548=CARTESIAN_POINT('Ctrl Pts',(24.4761748393321,-5.39427875973825,
0.));
#186549=CARTESIAN_POINT('Ctrl Pts',(24.4761748393321,-5.39427875973825,
12.));
#186550=CARTESIAN_POINT('Ctrl Pts',(24.496379499983,-5.41027091869242,0.));
#186551=CARTESIAN_POINT('Ctrl Pts',(24.496379499983,-5.41027091869242,12.));
#186552=CARTESIAN_POINT('Ctrl Pts',(24.5166078302108,-5.4263592318342,0.));
#186553=CARTESIAN_POINT('Ctrl Pts',(24.5166078302108,-5.4263592318342,12.));
#186554=CARTESIAN_POINT('Ctrl Pts',(24.5368592922863,-5.44254360356881,
0.));
#186555=CARTESIAN_POINT('Ctrl Pts',(24.5368592922863,-5.44254360356881,
12.));
#186556=CARTESIAN_POINT('Ctrl Pts',(24.5571333514842,-5.45882393762263,
0.));
#186557=CARTESIAN_POINT('Ctrl Pts',(24.5571333514842,-5.45882393762263,
12.));
#186558=CARTESIAN_POINT('Ctrl Pts',(24.5774294770329,-5.4752001372442,0.));
#186559=CARTESIAN_POINT('Ctrl Pts',(24.5774294770329,-5.4752001372442,12.));
#186560=CARTESIAN_POINT('Ctrl Pts',(24.5977471429364,-5.49167210537248,
0.));
#186561=CARTESIAN_POINT('Ctrl Pts',(24.5977471429364,-5.49167210537248,
12.));
#186562=CARTESIAN_POINT('Ctrl Pts',(24.6180858289179,-5.50823974481963,
0.));
#186563=CARTESIAN_POINT('Ctrl Pts',(24.6180858289179,-5.50823974481963,
12.));
#186564=CARTESIAN_POINT('Ctrl Pts',(24.6384450211467,-5.52490295840993,
0.));
#186565=CARTESIAN_POINT('Ctrl Pts',(24.6384450211467,-5.52490295840993,
12.));
#186566=CARTESIAN_POINT('Ctrl Pts',(24.6588242134738,-5.54166164919584,
0.));
#186567=CARTESIAN_POINT('Ctrl Pts',(24.6588242134738,-5.54166164919584,
12.));
#186568=CARTESIAN_POINT('Ctrl Pts',(24.6792229061794,-5.55851572025377,
0.));
#186569=CARTESIAN_POINT('Ctrl Pts',(24.6792229061794,-5.55851572025377,
12.));
#186570=CARTESIAN_POINT('Ctrl Pts',(24.6996406035517,-5.57546507427756,
0.));
#186571=CARTESIAN_POINT('Ctrl Pts',(24.6996406035517,-5.57546507427756,
12.));
#186572=CARTESIAN_POINT('Ctrl Pts',(24.7200768119088,-5.59250961323988,
0.));
#186573=CARTESIAN_POINT('Ctrl Pts',(24.7200768119088,-5.59250961323988,
12.));
#186574=CARTESIAN_POINT('Ctrl Pts',(24.7405310372739,-5.60964923798492,
0.));
#186575=CARTESIAN_POINT('Ctrl Pts',(24.7405310372739,-5.60964923798492,
12.));
#186576=CARTESIAN_POINT('Ctrl Pts',(24.7610027835697,-5.62688384790924,
0.));
#186577=CARTESIAN_POINT('Ctrl Pts',(24.7610027835697,-5.62688384790924,
12.));
#186578=CARTESIAN_POINT('Ctrl Pts',(24.781491549672,-5.64421334042262,0.));
#186579=CARTESIAN_POINT('Ctrl Pts',(24.781491549672,-5.64421334042262,12.));
#186580=CARTESIAN_POINT('Ctrl Pts',(24.8019968304605,-5.66163761114922,
0.));
#186581=CARTESIAN_POINT('Ctrl Pts',(24.8019968304605,-5.66163761114922,
12.));
#186582=CARTESIAN_POINT('Ctrl Pts',(24.8225181223845,-5.67915655496543,
0.));
#186583=CARTESIAN_POINT('Ctrl Pts',(24.8225181223845,-5.67915655496543,
12.));
#186584=CARTESIAN_POINT('Ctrl Pts',(24.8430549277621,-5.69677006679445,
0.));
#186585=CARTESIAN_POINT('Ctrl Pts',(24.8430549277621,-5.69677006679445,
12.));
#186586=CARTESIAN_POINT('Ctrl Pts',(24.8636067597669,-5.71447804252028,
0.));
#186587=CARTESIAN_POINT('Ctrl Pts',(24.8636067597669,-5.71447804252028,
12.));
#186588=CARTESIAN_POINT('Ctrl Pts',(24.884173146722,-5.73228037976928,0.));
#186589=CARTESIAN_POINT('Ctrl Pts',(24.884173146722,-5.73228037976928,12.));
#186590=CARTESIAN_POINT('Ctrl Pts',(24.904753637648,-5.75017697890805,0.));
#186591=CARTESIAN_POINT('Ctrl Pts',(24.904753637648,-5.75017697890805,12.));
#186592=CARTESIAN_POINT('Ctrl Pts',(24.9253478043656,-5.76816774342221,
0.));
#186593=CARTESIAN_POINT('Ctrl Pts',(24.9253478043656,-5.76816774342221,
12.));
#186594=CARTESIAN_POINT('Ctrl Pts',(24.945955229334,-5.78625257775682,0.));
#186595=CARTESIAN_POINT('Ctrl Pts',(24.945955229334,-5.78625257775682,12.));
#186596=CARTESIAN_POINT('Ctrl Pts',(24.9665754954496,-5.80443138549727,
0.));
#186597=CARTESIAN_POINT('Ctrl Pts',(24.9665754954496,-5.80443138549727,
12.));
#186598=CARTESIAN_POINT('Ctrl Pts',(24.9872081752734,-5.822704067442,0.));
#186599=CARTESIAN_POINT('Ctrl Pts',(24.9872081752734,-5.822704067442,12.));
#186600=CARTESIAN_POINT('Ctrl Pts',(25.0078528200564,-5.84107051963072,
0.));
#186601=CARTESIAN_POINT('Ctrl Pts',(25.0078528200564,-5.84107051963072,
12.));
#186602=CARTESIAN_POINT('Ctrl Pts',(25.0285089498899,-5.85953063156827,
0.));
#186603=CARTESIAN_POINT('Ctrl Pts',(25.0285089498899,-5.85953063156827,
12.));
#186604=CARTESIAN_POINT('Ctrl Pts',(25.049176040591,-5.87808428385367,0.));
#186605=CARTESIAN_POINT('Ctrl Pts',(25.049176040591,-5.87808428385367,12.));
#186606=CARTESIAN_POINT('Ctrl Pts',(25.0698535426514,-5.89673135155515,
0.));
#186607=CARTESIAN_POINT('Ctrl Pts',(25.0698535426514,-5.89673135155515,
12.));
#186608=CARTESIAN_POINT('Ctrl Pts',(25.0905409050773,-5.91547170844448,
0.));
#186609=CARTESIAN_POINT('Ctrl Pts',(25.0905409050773,-5.91547170844448,
12.));
#186610=CARTESIAN_POINT('Ctrl Pts',(25.1112375971106,-5.93430523086836,
0.));
#186611=CARTESIAN_POINT('Ctrl Pts',(25.1112375971106,-5.93430523086836,
12.));
#186612=CARTESIAN_POINT('Ctrl Pts',(25.1319431317237,-5.95323180187379,
0.));
#186613=CARTESIAN_POINT('Ctrl Pts',(25.1319431317237,-5.95323180187379,
12.));
#186614=CARTESIAN_POINT('Ctrl Pts',(25.1526570863092,-5.97225131495618,
0.));
#186615=CARTESIAN_POINT('Ctrl Pts',(25.1526570863092,-5.97225131495618,
12.));
#186616=CARTESIAN_POINT('Ctrl Pts',(25.1733791296259,-5.99136367859755,
0.));
#186617=CARTESIAN_POINT('Ctrl Pts',(25.1733791296259,-5.99136367859755,
12.));
#186618=CARTESIAN_POINT('Ctrl Pts',(25.1941090269819,-6.01056881804614,
0.));
#186619=CARTESIAN_POINT('Ctrl Pts',(25.1941090269819,-6.01056881804614,
12.));
#186620=CARTESIAN_POINT('Ctrl Pts',(25.21484662016,-6.02986667389998,0.));
#186621=CARTESIAN_POINT('Ctrl Pts',(25.21484662016,-6.02986667389998,12.));
#186622=CARTESIAN_POINT('Ctrl Pts',(25.2355918139032,-6.04925720151219,
0.));
#186623=CARTESIAN_POINT('Ctrl Pts',(25.2355918139032,-6.04925720151219,
12.));
#186624=CARTESIAN_POINT('Ctrl Pts',(25.2521940105705,-6.06484373634547,
0.));
#186625=CARTESIAN_POINT('Ctrl Pts',(25.2521940105705,-6.06484373634547,
12.));
#186626=CARTESIAN_POINT('Ctrl Pts',(25.2646490489922,-6.07657531787491,
0.));
#186627=CARTESIAN_POINT('Ctrl Pts',(25.2646490489922,-6.07657531787491,
12.));
#186628=CARTESIAN_POINT('Ctrl Pts',(25.2729539149517,-6.08441489609794,
0.));
#186629=CARTESIAN_POINT('Ctrl Pts',(25.2729539149517,-6.08441489609794,
12.));
#186630=CARTESIAN_POINT('Ctrl Pts',(25.2771067246846,-6.088339316177,0.));
#186631=CARTESIAN_POINT('Ctrl Pts',(25.2771067246846,-6.088339316177,12.));
#186632=CARTESIAN_POINT('',(25.2771067246846,-6.088339316177,0.));
#186633=CARTESIAN_POINT('Ctrl Pts',(22.1738711152697,-4.11585220600463,
0.));
#186634=CARTESIAN_POINT('Ctrl Pts',(22.173877682324,-4.11585194677443,0.));
#186635=CARTESIAN_POINT('Ctrl Pts',(22.1739341411687,-4.11586035878288,
0.));
#186636=CARTESIAN_POINT('Ctrl Pts',(22.1741488021234,-4.11589976826168,
0.));
#186637=CARTESIAN_POINT('Ctrl Pts',(22.1746949858775,-4.11600589882846,
0.));
#186638=CARTESIAN_POINT('Ctrl Pts',(22.1758088296598,-4.1162279721707,0.));
#186639=CARTESIAN_POINT('Ctrl Pts',(22.177347426894,-4.11653973150519,0.));
#186640=CARTESIAN_POINT('Ctrl Pts',(22.179297473024,-4.11694173195005,0.));
#186641=CARTESIAN_POINT('Ctrl Pts',(22.1816414985788,-4.11743469691757,
0.));
#186642=CARTESIAN_POINT('Ctrl Pts',(22.1843613164855,-4.11801938107481,
0.));
#186643=CARTESIAN_POINT('Ctrl Pts',(22.1874419861496,-4.11869641271775,
0.));
#186644=CARTESIAN_POINT('Ctrl Pts',(22.1908725908525,-4.11946626228637,
0.));
#186645=CARTESIAN_POINT('Ctrl Pts',(22.1946440958098,-4.12032932637738,
0.));
#186646=CARTESIAN_POINT('Ctrl Pts',(22.1987479618246,-4.12128598183523,
0.));
#186647=CARTESIAN_POINT('Ctrl Pts',(22.2031746532106,-4.12233664408228,
0.));
#186648=CARTESIAN_POINT('Ctrl Pts',(22.2079143941719,-4.12348173702024,
0.));
#186649=CARTESIAN_POINT('Ctrl Pts',(22.2129576146671,-4.12472167516608,
0.));
#186650=CARTESIAN_POINT('Ctrl Pts',(22.2182956401341,-4.12605683613308,
0.));
#186651=CARTESIAN_POINT('Ctrl Pts',(22.2239207458781,-4.12748755830105,
0.));
#186652=CARTESIAN_POINT('Ctrl Pts',(22.2298258043947,-4.1290141546338,0.));
#186653=CARTESIAN_POINT('Ctrl Pts',(22.2360040565533,-4.13063692157499,
0.));
#186654=CARTESIAN_POINT('Ctrl Pts',(22.2424488153523,-4.13235615060161,
0.));
#186655=CARTESIAN_POINT('Ctrl Pts',(22.249153531779,-4.13417212558811,0.));
#186656=CARTESIAN_POINT('Ctrl Pts',(22.2561118708421,-4.13608511977227,
0.));
#186657=CARTESIAN_POINT('Ctrl Pts',(22.2633177913972,-4.13809539255423,
0.));
#186658=CARTESIAN_POINT('Ctrl Pts',(22.2707656042457,-4.14020318715992,
0.));
#186659=CARTESIAN_POINT('Ctrl Pts',(22.2784499072027,-4.14240873321985,
0.));
#186660=CARTESIAN_POINT('Ctrl Pts',(22.2863655389166,-4.14471224859297,
0.));
#186661=CARTESIAN_POINT('Ctrl Pts',(22.2945075198467,-4.14711394168557,
0.));
#186662=CARTESIAN_POINT('Ctrl Pts',(22.3028710166933,-4.14961401285523,
0.));
#186663=CARTESIAN_POINT('Ctrl Pts',(22.3114513545185,-4.15221265396991,
0.));
#186664=CARTESIAN_POINT('Ctrl Pts',(22.3202440186979,-4.15491004835282,
0.));
#186665=CARTESIAN_POINT('Ctrl Pts',(22.3292446628959,-4.15770637047891,
0.));
#186666=CARTESIAN_POINT('Ctrl Pts',(22.3384491078602,-4.16060178604165,
0.));
#186667=CARTESIAN_POINT('Ctrl Pts',(22.3478533253889,-4.16359645263189,
0.));
#186668=CARTESIAN_POINT('Ctrl Pts',(22.3574534257396,-4.16669052026601,
0.));
#186669=CARTESIAN_POINT('Ctrl Pts',(22.3672456427599,-4.16988413199458,
0.));
#186670=CARTESIAN_POINT('Ctrl Pts',(22.3772263228617,-4.17317742436146,
0.));
#186671=CARTESIAN_POINT('Ctrl Pts',(22.3873919231334,-4.17657052752826,
0.));
#186672=CARTESIAN_POINT('Ctrl Pts',(22.3977390078075,-4.18006356544883,
0.));
#186673=CARTESIAN_POINT('Ctrl Pts',(22.4082642454453,-4.18365665600852,
0.));
#186674=CARTESIAN_POINT('Ctrl Pts',(22.4189644056115,-4.18734991117722,
0.));
#186675=CARTESIAN_POINT('Ctrl Pts',(22.4298363535421,-4.19114343726943,
0.));
#186676=CARTESIAN_POINT('Ctrl Pts',(22.4408770448917,-4.19503733518862,
0.));
#186677=CARTESIAN_POINT('Ctrl Pts',(22.4520835205419,-4.19903170066356,
0.));
#186678=CARTESIAN_POINT('Ctrl Pts',(22.4634529011433,-4.20312662448172,
0.));
#186679=CARTESIAN_POINT('Ctrl Pts',(22.4749823839915,-4.20732219265649,
0.));
#186680=CARTESIAN_POINT('Ctrl Pts',(22.4866692403147,-4.21161848657429,
0.));
#186681=CARTESIAN_POINT('Ctrl Pts',(22.4985108124229,-4.21601558313909,
0.));
#186682=CARTESIAN_POINT('Ctrl Pts',(22.5105045108882,-4.22051355490198,
0.));
#186683=CARTESIAN_POINT('Ctrl Pts',(22.5226478117885,-4.22511247020041,
0.));
#186684=CARTESIAN_POINT('Ctrl Pts',(22.5349382540587,-4.22981239330733,
0.));
#186685=CARTESIAN_POINT('Ctrl Pts',(22.5473734368086,-4.23461338456714,
0.));
#186686=CARTESIAN_POINT('Ctrl Pts',(22.559951016643,-4.23951550052527,0.));
#186687=CARTESIAN_POINT('Ctrl Pts',(22.5726687049922,-4.2445187940486,0.));
#186688=CARTESIAN_POINT('Ctrl Pts',(22.5855242662479,-4.24962331444186,
0.));
#186689=CARTESIAN_POINT('Ctrl Pts',(22.5985155158637,-4.25482910755486,
0.));
#186690=CARTESIAN_POINT('Ctrl Pts',(22.611640318482,-4.26013621588304,0.));
#186691=CARTESIAN_POINT('Ctrl Pts',(22.6248965859975,-4.26554467865572,
0.));
#186692=CARTESIAN_POINT('Ctrl Pts',(22.6382822758171,-4.27105453193,0.));
#186693=CARTESIAN_POINT('Ctrl Pts',(22.6517953893303,-4.27666580869118,
0.));
#186694=CARTESIAN_POINT('Ctrl Pts',(22.665433970311,-4.2823785389406,0.));
#186695=CARTESIAN_POINT('Ctrl Pts',(22.6791961033536,-4.28819274977767,
0.));
#186696=CARTESIAN_POINT('Ctrl Pts',(22.6930799122545,-4.29410846547062,
0.));
#186697=CARTESIAN_POINT('Ctrl Pts',(22.707083558756,-4.30012570754067,0.));
#186698=CARTESIAN_POINT('Ctrl Pts',(22.7212052413384,-4.30624449484075,
0.));
#186699=CARTESIAN_POINT('Ctrl Pts',(22.7354431939926,-4.31246484362551,
0.));
#186700=CARTESIAN_POINT('Ctrl Pts',(22.7497956849852,-4.31878676761231,
0.));
#186701=CARTESIAN_POINT('Ctrl Pts',(22.764261015648,-4.32521027803748,0.));
#186702=CARTESIAN_POINT('Ctrl Pts',(22.7788375194081,-4.33173538373183,
0.));
#186703=CARTESIAN_POINT('Ctrl Pts',(22.7935235607807,-4.33836209118444,
0.));
#186704=CARTESIAN_POINT('Ctrl Pts',(22.808317534379,-4.34509040460066,0.));
#186705=CARTESIAN_POINT('Ctrl Pts',(22.8232178638873,-4.35192032594802,
0.));
#186706=CARTESIAN_POINT('Ctrl Pts',(22.838223001118,-4.3588518550056,0.));
#186707=CARTESIAN_POINT('Ctrl Pts',(22.8533314252419,-4.36588498943011,
0.));
#186708=CARTESIAN_POINT('Ctrl Pts',(22.8685416419725,-4.37301972480753,
0.));
#186709=CARTESIAN_POINT('Ctrl Pts',(22.8838521827702,-4.38025605470091,
0.));
#186710=CARTESIAN_POINT('Ctrl Pts',(22.8992616040108,-4.38759397068393,
0.));
#186711=CARTESIAN_POINT('Ctrl Pts',(22.9147684862425,-4.39503346238455,
0.));
#186712=CARTESIAN_POINT('Ctrl Pts',(22.9303714335549,-4.40257451754309,
0.));
#186713=CARTESIAN_POINT('Ctrl Pts',(22.9460690729092,-4.41021712205549,
0.));
#186714=CARTESIAN_POINT('Ctrl Pts',(22.9618600534866,-4.41796126001311,
0.));
#186715=CARTESIAN_POINT('Ctrl Pts',(22.9777430460021,-4.42580691372772,
0.));
#186716=CARTESIAN_POINT('Ctrl Pts',(22.9937167421009,-4.43375406376906,
0.));
#186717=CARTESIAN_POINT('Ctrl Pts',(23.0097798538399,-4.44180268901667,
0.));
#186718=CARTESIAN_POINT('Ctrl Pts',(23.0259311131395,-4.44995276669699,
0.));
#186719=CARTESIAN_POINT('Ctrl Pts',(23.0421692712466,-4.45820427241678,
0.));
#186720=CARTESIAN_POINT('Ctrl Pts',(23.0584930981723,-4.46655718018206,
0.));
#186721=CARTESIAN_POINT('Ctrl Pts',(23.0749013821867,-4.47501146242822,
0.));
#186722=CARTESIAN_POINT('Ctrl Pts',(23.0913929293909,-4.48356709006757,
0.));
#186723=CARTESIAN_POINT('Ctrl Pts',(23.1079665632629,-4.49222403252202,
0.));
#186724=CARTESIAN_POINT('Ctrl Pts',(23.1246211242117,-4.5009822577518,0.));
#186725=CARTESIAN_POINT('Ctrl Pts',(23.1413554691136,-4.50984173227088,
0.));
#186726=CARTESIAN_POINT('Ctrl Pts',(23.1581684708778,-4.51880242116786,
0.));
#186727=CARTESIAN_POINT('Ctrl Pts',(23.1750590180923,-4.52786428815049,
0.));
#186728=CARTESIAN_POINT('Ctrl Pts',(23.1920260146474,-4.53702729557586,
0.));
#186729=CARTESIAN_POINT('Ctrl Pts',(23.2090683793627,-4.54629140447543,
0.));
#186730=CARTESIAN_POINT('Ctrl Pts',(23.2261850456054,-4.55565657456957,
0.));
#186731=CARTESIAN_POINT('Ctrl Pts',(23.2433749609117,-4.56512276427812,
0.));
#186732=CARTESIAN_POINT('Ctrl Pts',(23.2606370866853,-4.57468993076071,
0.));
#186733=CARTESIAN_POINT('Ctrl Pts',(23.2779703978868,-4.58435802994675,
0.));
#186734=CARTESIAN_POINT('Ctrl Pts',(23.295373882719,-4.59412701655751,0.));
#186735=CARTESIAN_POINT('Ctrl Pts',(23.3128465423119,-4.60399684412176,
0.));
#186736=CARTESIAN_POINT('Ctrl Pts',(23.3303873903947,-4.6139674649785,0.));
#186737=CARTESIAN_POINT('Ctrl Pts',(23.3479954530281,-4.62403883030825,
0.));
#186738=CARTESIAN_POINT('Ctrl Pts',(23.3656697683496,-4.63421089016556,
0.));
#186739=CARTESIAN_POINT('Ctrl Pts',(23.383409386307,-4.64448359349936,0.));
#186740=CARTESIAN_POINT('Ctrl Pts',(23.4012133683957,-4.65485688816923,
0.));
#186741=CARTESIAN_POINT('Ctrl Pts',(23.4190807873798,-4.66533072094664,
0.));
#186742=CARTESIAN_POINT('Ctrl Pts',(23.4370107270444,-4.67590503753051,
0.));
#186743=CARTESIAN_POINT('Ctrl Pts',(23.4550022819852,-4.68657978258298,
0.));
#186744=CARTESIAN_POINT('Ctrl Pts',(23.4730545573849,-4.69735489975024,
0.));
#186745=CARTESIAN_POINT('Ctrl Pts',(23.491166668789,-4.70823033167821,0.));
#186746=CARTESIAN_POINT('Ctrl Pts',(23.5093377418784,-4.71920602001905,
0.));
#186747=CARTESIAN_POINT('Ctrl Pts',(23.5275669122378,-4.73028190543032,
0.));
#186748=CARTESIAN_POINT('Ctrl Pts',(23.5458533251715,-4.74145792760699,
0.));
#186749=CARTESIAN_POINT('Ctrl Pts',(23.564196135517,-4.75273402530616,0.));
#186750=CARTESIAN_POINT('Ctrl Pts',(23.5825945074535,-4.76411013636252,
0.));
#186751=CARTESIAN_POINT('Ctrl Pts',(23.6010476143099,-4.77558619769876,
0.));
#186752=CARTESIAN_POINT('Ctrl Pts',(23.6195546383625,-4.78716214532105,
0.));
#186753=CARTESIAN_POINT('Ctrl Pts',(23.6381147706581,-4.79883791433231,
0.));
#186754=CARTESIAN_POINT('Ctrl Pts',(23.6567272108631,-4.81061343896443,
0.));
#186755=CARTESIAN_POINT('Ctrl Pts',(23.6753911671023,-4.82248865259571,
0.));
#186756=CARTESIAN_POINT('Ctrl Pts',(23.6941058557971,-4.83446348776268,
0.));
#186757=CARTESIAN_POINT('Ctrl Pts',(23.7128705015014,-4.84653787616424,
0.));
#186758=CARTESIAN_POINT('Ctrl Pts',(23.7316843367308,-4.85871174865493,
0.));
#186759=CARTESIAN_POINT('Ctrl Pts',(23.7505466018239,-4.87098503527144,
0.));
#186760=CARTESIAN_POINT('Ctrl Pts',(23.7694565448044,-4.88335766525566,
0.));
#186761=CARTESIAN_POINT('Ctrl Pts',(23.7884134212381,-4.89582956706772,
0.));
#186762=CARTESIAN_POINT('Ctrl Pts',(23.8074164940897,-4.90840066839348,
0.));
#186763=CARTESIAN_POINT('Ctrl Pts',(23.8264650335721,-4.92107089613978,
0.));
#186764=CARTESIAN_POINT('Ctrl Pts',(23.8455583170062,-4.93384017643443,
0.));
#186765=CARTESIAN_POINT('Ctrl Pts',(23.8646956287172,-4.94670843465869,
0.));
#186766=CARTESIAN_POINT('Ctrl Pts',(23.883876259922,-4.95967559546566,0.));
#186767=CARTESIAN_POINT('Ctrl Pts',(23.9030995086164,-4.9727415827923,0.));
#186768=CARTESIAN_POINT('Ctrl Pts',(23.9223646794591,-4.98590631986534,
0.));
#186769=CARTESIAN_POINT('Ctrl Pts',(23.9416710836528,-4.9991697291931,0.));
#186770=CARTESIAN_POINT('Ctrl Pts',(23.9610180388271,-5.01253173257459,
0.));
#186771=CARTESIAN_POINT('Ctrl Pts',(23.9804048689228,-5.02599225112462,
0.));
#186772=CARTESIAN_POINT('Ctrl Pts',(23.9998309040747,-5.03955120528528,
0.));
#186773=CARTESIAN_POINT('Ctrl Pts',(24.0192954804896,-5.05320851483069,
0.));
#186774=CARTESIAN_POINT('Ctrl Pts',(24.0387979403268,-5.0669640988664,0.));
#186775=CARTESIAN_POINT('Ctrl Pts',(24.0583376315636,-5.08081787581271,
0.));
#186776=CARTESIAN_POINT('Ctrl Pts',(24.0779139079264,-5.09476976342618,
0.));
#186777=CARTESIAN_POINT('Ctrl Pts',(24.0975261288444,-5.10881967883126,
0.));
#186778=CARTESIAN_POINT('Ctrl Pts',(24.117173659394,-5.12296753853858,0.));
#186779=CARTESIAN_POINT('Ctrl Pts',(24.1368558702443,-5.13721325845746,
0.));
#186780=CARTESIAN_POINT('Ctrl Pts',(24.1565721375971,-5.1515567539008,0.));
#186781=CARTESIAN_POINT('Ctrl Pts',(24.1763218431344,-5.16599793957987,
0.));
#186782=CARTESIAN_POINT('Ctrl Pts',(24.1961043738755,-5.180536729614,0.));
#186783=CARTESIAN_POINT('Ctrl Pts',(24.2159191220171,-5.19517303753648,
0.));
#186784=CARTESIAN_POINT('Ctrl Pts',(24.2357654847766,-5.20990677629177,
0.));
#186785=CARTESIAN_POINT('Ctrl Pts',(24.2556428642294,-5.22473785822443,
0.));
#186786=CARTESIAN_POINT('Ctrl Pts',(24.2755506671525,-5.2396661950629,0.));
#186787=CARTESIAN_POINT('Ctrl Pts',(24.2954883048447,-5.25469169788858,
0.));
#186788=CARTESIAN_POINT('Ctrl Pts',(24.3154551932221,-5.269814277188,0.));
#186789=CARTESIAN_POINT('Ctrl Pts',(24.3354507529414,-5.28503384290649,
0.));
#186790=CARTESIAN_POINT('Ctrl Pts',(24.3554744095075,-5.30035030449065,
0.));
#186791=CARTESIAN_POINT('Ctrl Pts',(24.3755255933917,-5.31576357092527,
0.));
#186792=CARTESIAN_POINT('Ctrl Pts',(24.3956037401293,-5.33127355076035,
0.));
#186793=CARTESIAN_POINT('Ctrl Pts',(24.4157082904614,-5.34688015213538,
0.));
#186794=CARTESIAN_POINT('Ctrl Pts',(24.435838689915,-5.36258328273628,0.));
#186795=CARTESIAN_POINT('Ctrl Pts',(24.4559943883157,-5.37838284973696,
0.));
#186796=CARTESIAN_POINT('Ctrl Pts',(24.4761748393321,-5.39427875973825,
0.));
#186797=CARTESIAN_POINT('Ctrl Pts',(24.496379499983,-5.41027091869242,0.));
#186798=CARTESIAN_POINT('Ctrl Pts',(24.5166078302108,-5.4263592318342,0.));
#186799=CARTESIAN_POINT('Ctrl Pts',(24.5368592922863,-5.44254360356881,
0.));
#186800=CARTESIAN_POINT('Ctrl Pts',(24.5571333514842,-5.45882393762263,
0.));
#186801=CARTESIAN_POINT('Ctrl Pts',(24.5774294770329,-5.4752001372442,0.));
#186802=CARTESIAN_POINT('Ctrl Pts',(24.5977471429364,-5.49167210537248,
0.));
#186803=CARTESIAN_POINT('Ctrl Pts',(24.6180858289179,-5.50823974481963,
0.));
#186804=CARTESIAN_POINT('Ctrl Pts',(24.6384450211467,-5.52490295840993,
0.));
#186805=CARTESIAN_POINT('Ctrl Pts',(24.6588242134738,-5.54166164919584,
0.));
#186806=CARTESIAN_POINT('Ctrl Pts',(24.6792229061794,-5.55851572025377,
0.));
#186807=CARTESIAN_POINT('Ctrl Pts',(24.6996406035517,-5.57546507427756,
0.));
#186808=CARTESIAN_POINT('Ctrl Pts',(24.7200768119088,-5.59250961323988,
0.));
#186809=CARTESIAN_POINT('Ctrl Pts',(24.7405310372739,-5.60964923798492,
0.));
#186810=CARTESIAN_POINT('Ctrl Pts',(24.7610027835697,-5.62688384790924,
0.));
#186811=CARTESIAN_POINT('Ctrl Pts',(24.781491549672,-5.64421334042262,0.));
#186812=CARTESIAN_POINT('Ctrl Pts',(24.8019968304605,-5.66163761114922,
0.));
#186813=CARTESIAN_POINT('Ctrl Pts',(24.8225181223845,-5.67915655496543,
0.));
#186814=CARTESIAN_POINT('Ctrl Pts',(24.8430549277621,-5.69677006679445,
0.));
#186815=CARTESIAN_POINT('Ctrl Pts',(24.8636067597669,-5.71447804252028,
0.));
#186816=CARTESIAN_POINT('Ctrl Pts',(24.884173146722,-5.73228037976928,0.));
#186817=CARTESIAN_POINT('Ctrl Pts',(24.904753637648,-5.75017697890805,0.));
#186818=CARTESIAN_POINT('Ctrl Pts',(24.9253478043656,-5.76816774342221,
0.));
#186819=CARTESIAN_POINT('Ctrl Pts',(24.945955229334,-5.78625257775682,0.));
#186820=CARTESIAN_POINT('Ctrl Pts',(24.9665754954496,-5.80443138549727,
0.));
#186821=CARTESIAN_POINT('Ctrl Pts',(24.9872081752734,-5.822704067442,0.));
#186822=CARTESIAN_POINT('Ctrl Pts',(25.0078528200564,-5.84107051963072,
0.));
#186823=CARTESIAN_POINT('Ctrl Pts',(25.0285089498899,-5.85953063156827,
0.));
#186824=CARTESIAN_POINT('Ctrl Pts',(25.049176040591,-5.87808428385367,0.));
#186825=CARTESIAN_POINT('Ctrl Pts',(25.0698535426514,-5.89673135155515,
0.));
#186826=CARTESIAN_POINT('Ctrl Pts',(25.0905409050773,-5.91547170844448,
0.));
#186827=CARTESIAN_POINT('Ctrl Pts',(25.1112375971106,-5.93430523086836,
0.));
#186828=CARTESIAN_POINT('Ctrl Pts',(25.1319431317237,-5.95323180187379,
0.));
#186829=CARTESIAN_POINT('Ctrl Pts',(25.1526570863092,-5.97225131495618,
0.));
#186830=CARTESIAN_POINT('Ctrl Pts',(25.1733791296259,-5.99136367859755,
0.));
#186831=CARTESIAN_POINT('Ctrl Pts',(25.1941090269819,-6.01056881804614,
0.));
#186832=CARTESIAN_POINT('Ctrl Pts',(25.21484662016,-6.02986667389998,0.));
#186833=CARTESIAN_POINT('Ctrl Pts',(25.2355918139032,-6.04925720151219,
0.));
#186834=CARTESIAN_POINT('Ctrl Pts',(25.2521940105705,-6.06484373634547,
0.));
#186835=CARTESIAN_POINT('Ctrl Pts',(25.2646490489922,-6.07657531787491,
0.));
#186836=CARTESIAN_POINT('Ctrl Pts',(25.2729539149517,-6.08441489609794,
0.));
#186837=CARTESIAN_POINT('Ctrl Pts',(25.2771067246846,-6.088339316177,0.));
#186838=CARTESIAN_POINT('',(25.2771067246846,-6.088339316177,0.));
#186839=CARTESIAN_POINT('Origin',(19.4030938020118,-9.26120677397565,0.));
#186840=CARTESIAN_POINT('',(20.353053841303,-9.71462809124917,0.));
#186841=CARTESIAN_POINT('',(20.353053841303,-9.71462809124917,0.));
#186842=CARTESIAN_POINT('',(9.70154690100589,-4.63060338698782,0.));
#186843=CARTESIAN_POINT('Ctrl Pts',(24.9347862158358,-7.36589684767345,
0.));
#186844=CARTESIAN_POINT('Ctrl Pts',(24.9347862158358,-7.36589684767345,
12.));
#186845=CARTESIAN_POINT('Ctrl Pts',(24.9292275670674,-7.36721909028843,
0.));
#186846=CARTESIAN_POINT('Ctrl Pts',(24.9292275670674,-7.36721909028843,
12.));
#186847=CARTESIAN_POINT('Ctrl Pts',(24.9181155530543,-7.36985593120091,
0.));
#186848=CARTESIAN_POINT('Ctrl Pts',(24.9181155530543,-7.36985593120091,
12.));
#186849=CARTESIAN_POINT('Ctrl Pts',(24.901463382605,-7.37378825961676,0.));
#186850=CARTESIAN_POINT('Ctrl Pts',(24.901463382605,-7.37378825961676,12.));
#186851=CARTESIAN_POINT('Ctrl Pts',(24.8792921911115,-7.3789854964027,0.));
#186852=CARTESIAN_POINT('Ctrl Pts',(24.8792921911115,-7.3789854964027,12.));
#186853=CARTESIAN_POINT('Ctrl Pts',(24.8516310625176,-7.38540558903621,
0.));
#186854=CARTESIAN_POINT('Ctrl Pts',(24.8516310625176,-7.38540558903621,
12.));
#186855=CARTESIAN_POINT('Ctrl Pts',(24.8240228520893,-7.39174922585809,
0.));
#186856=CARTESIAN_POINT('Ctrl Pts',(24.8240228520893,-7.39174922585809,
12.));
#186857=CARTESIAN_POINT('Ctrl Pts',(24.7964676646431,-7.39801641583013,
0.));
#186858=CARTESIAN_POINT('Ctrl Pts',(24.7964676646431,-7.39801641583013,
12.));
#186859=CARTESIAN_POINT('Ctrl Pts',(24.7689656668983,-7.40420718661603,
0.));
#186860=CARTESIAN_POINT('Ctrl Pts',(24.7689656668983,-7.40420718661603,
12.));
#186861=CARTESIAN_POINT('Ctrl Pts',(24.7415170994784,-7.41032159082382,
0.));
#186862=CARTESIAN_POINT('Ctrl Pts',(24.7415170994784,-7.41032159082382,
12.));
#186863=CARTESIAN_POINT('Ctrl Pts',(24.7141222950051,-7.41635971481674,
0.));
#186864=CARTESIAN_POINT('Ctrl Pts',(24.7141222950051,-7.41635971481674,
12.));
#186865=CARTESIAN_POINT('Ctrl Pts',(24.6867816727192,-7.42232167766266,
0.));
#186866=CARTESIAN_POINT('Ctrl Pts',(24.6867816727192,-7.42232167766266,
12.));
#186867=CARTESIAN_POINT('Ctrl Pts',(24.6594957128756,-7.42820762159126,
0.));
#186868=CARTESIAN_POINT('Ctrl Pts',(24.6594957128756,-7.42820762159126,
12.));
#186869=CARTESIAN_POINT('Ctrl Pts',(24.6322649369517,-7.43401770489524,
0.));
#186870=CARTESIAN_POINT('Ctrl Pts',(24.6322649369517,-7.43401770489524,
12.));
#186871=CARTESIAN_POINT('Ctrl Pts',(24.6050898852368,-7.43975209375504,
0.));
#186872=CARTESIAN_POINT('Ctrl Pts',(24.6050898852368,-7.43975209375504,
12.));
#186873=CARTESIAN_POINT('Ctrl Pts',(24.577971096086,-7.44541095473135,0.));
#186874=CARTESIAN_POINT('Ctrl Pts',(24.577971096086,-7.44541095473135,12.));
#186875=CARTESIAN_POINT('Ctrl Pts',(24.5509090831559,-7.4509944465116,0.));
#186876=CARTESIAN_POINT('Ctrl Pts',(24.5509090831559,-7.4509944465116,12.));
#186877=CARTESIAN_POINT('Ctrl Pts',(24.5239043173072,-7.45650271335862,
0.));
#186878=CARTESIAN_POINT('Ctrl Pts',(24.5239043173072,-7.45650271335862,
12.));
#186879=CARTESIAN_POINT('Ctrl Pts',(24.4969572391483,-7.46193588961464,
0.));
#186880=CARTESIAN_POINT('Ctrl Pts',(24.4969572391483,-7.46193588961464,
12.));
#186881=CARTESIAN_POINT('Ctrl Pts',(24.4700682684524,-7.46729410308787,
0.));
#186882=CARTESIAN_POINT('Ctrl Pts',(24.4700682684524,-7.46729410308787,
12.));
#186883=CARTESIAN_POINT('Ctrl Pts',(24.443237814649,-7.47257747883246,0.));
#186884=CARTESIAN_POINT('Ctrl Pts',(24.443237814649,-7.47257747883246,12.));
#186885=CARTESIAN_POINT('Ctrl Pts',(24.4164662871163,-7.47778614286565,
0.));
#186886=CARTESIAN_POINT('Ctrl Pts',(24.4164662871163,-7.47778614286565,
12.));
#186887=CARTESIAN_POINT('Ctrl Pts',(24.3897541049254,-7.48292022569301,
0.));
#186888=CARTESIAN_POINT('Ctrl Pts',(24.3897541049254,-7.48292022569301,
12.));
#186889=CARTESIAN_POINT('Ctrl Pts',(24.3631017084524,-7.48797986651909,
0.));
#186890=CARTESIAN_POINT('Ctrl Pts',(24.3631017084524,-7.48797986651909,
12.));
#186891=CARTESIAN_POINT('Ctrl Pts',(24.3365095573685,-7.49296521252421,
0.));
#186892=CARTESIAN_POINT('Ctrl Pts',(24.3365095573685,-7.49296521252421,
12.));
#186893=CARTESIAN_POINT('Ctrl Pts',(24.3099781253355,-7.49787641695439,
0.));
#186894=CARTESIAN_POINT('Ctrl Pts',(24.3099781253355,-7.49787641695439,
12.));
#186895=CARTESIAN_POINT('Ctrl Pts',(24.2835078958973,-7.50271363765152,
0.));
#186896=CARTESIAN_POINT('Ctrl Pts',(24.2835078958973,-7.50271363765152,
12.));
#186897=CARTESIAN_POINT('Ctrl Pts',(24.2570993577034,-7.50747703535134,
0.));
#186898=CARTESIAN_POINT('Ctrl Pts',(24.2570993577034,-7.50747703535134,
12.));
#186899=CARTESIAN_POINT('Ctrl Pts',(24.2307530003887,-7.51216677222181,
0.));
#186900=CARTESIAN_POINT('Ctrl Pts',(24.2307530003887,-7.51216677222181,
12.));
#186901=CARTESIAN_POINT('Ctrl Pts',(24.2044693092349,-7.51678300997949,
0.));
#186902=CARTESIAN_POINT('Ctrl Pts',(24.2044693092349,-7.51678300997949,
12.));
#186903=CARTESIAN_POINT('Ctrl Pts',(24.1782487641594,-7.52132590953802,
0.));
#186904=CARTESIAN_POINT('Ctrl Pts',(24.1782487641594,-7.52132590953802,
12.));
#186905=CARTESIAN_POINT('Ctrl Pts',(24.1520918425364,-7.52579563201424,
0.));
#186906=CARTESIAN_POINT('Ctrl Pts',(24.1520918425364,-7.52579563201424,
12.));
#186907=CARTESIAN_POINT('Ctrl Pts',(24.1259990209207,-7.53019233935502,
0.));
#186908=CARTESIAN_POINT('Ctrl Pts',(24.1259990209207,-7.53019233935502,
12.));
#186909=CARTESIAN_POINT('Ctrl Pts',(24.0999707772642,-7.53451619514649,
0.));
#186910=CARTESIAN_POINT('Ctrl Pts',(24.0999707772642,-7.53451619514649,
12.));
#186911=CARTESIAN_POINT('Ctrl Pts',(24.0740075927985,-7.53876736531014,
0.));
#186912=CARTESIAN_POINT('Ctrl Pts',(24.0740075927985,-7.53876736531014,
12.));
#186913=CARTESIAN_POINT('Ctrl Pts',(24.0481099543353,-7.54294601896145,
0.));
#186914=CARTESIAN_POINT('Ctrl Pts',(24.0481099543353,-7.54294601896145,
12.));
#186915=CARTESIAN_POINT('Ctrl Pts',(24.022278355453,-7.5470523288591,0.));
#186916=CARTESIAN_POINT('Ctrl Pts',(24.022278355453,-7.5470523288591,12.));
#186917=CARTESIAN_POINT('Ctrl Pts',(23.9965132953185,-7.55108647097441,
0.));
#186918=CARTESIAN_POINT('Ctrl Pts',(23.9965132953185,-7.55108647097441,
12.));
#186919=CARTESIAN_POINT('Ctrl Pts',(23.9708152779884,-7.55504862424812,
0.));
#186920=CARTESIAN_POINT('Ctrl Pts',(23.9708152779884,-7.55504862424812,
12.));
#186921=CARTESIAN_POINT('Ctrl Pts',(23.9451848115,-7.55893897027683,0.));
#186922=CARTESIAN_POINT('Ctrl Pts',(23.9451848115,-7.55893897027683,12.));
#186923=CARTESIAN_POINT('Ctrl Pts',(23.9196224070759,-7.56275769304773,
0.));
#186924=CARTESIAN_POINT('Ctrl Pts',(23.9196224070759,-7.56275769304773,
12.));
#186925=CARTESIAN_POINT('Ctrl Pts',(23.8941285782003,-7.56650497863792,
0.));
#186926=CARTESIAN_POINT('Ctrl Pts',(23.8941285782003,-7.56650497863792,
12.));
#186927=CARTESIAN_POINT('Ctrl Pts',(23.8687038399597,-7.57018101500711,
0.));
#186928=CARTESIAN_POINT('Ctrl Pts',(23.8687038399597,-7.57018101500711,
12.));
#186929=CARTESIAN_POINT('Ctrl Pts',(23.8433487096134,-7.57378599219817,
0.));
#186930=CARTESIAN_POINT('Ctrl Pts',(23.8433487096134,-7.57378599219817,
12.));
#186931=CARTESIAN_POINT('Ctrl Pts',(23.8180637069977,-7.57732010249066,
0.));
#186932=CARTESIAN_POINT('Ctrl Pts',(23.8180637069977,-7.57732010249066,
12.));
#186933=CARTESIAN_POINT('Ctrl Pts',(23.7928493549908,-7.58078354058212,
0.));
#186934=CARTESIAN_POINT('Ctrl Pts',(23.7928493549908,-7.58078354058212,
12.));
#186935=CARTESIAN_POINT('Ctrl Pts',(23.7677061799376,-7.58417650376272,
0.));
#186936=CARTESIAN_POINT('Ctrl Pts',(23.7677061799376,-7.58417650376272,
12.));
#186937=CARTESIAN_POINT('Ctrl Pts',(23.7426347121006,-7.58749919210832,
0.));
#186938=CARTESIAN_POINT('Ctrl Pts',(23.7426347121006,-7.58749919210832,
12.));
#186939=CARTESIAN_POINT('Ctrl Pts',(23.7176354860457,-7.59075180865327,
0.));
#186940=CARTESIAN_POINT('Ctrl Pts',(23.7176354860457,-7.59075180865327,
12.));
#186941=CARTESIAN_POINT('Ctrl Pts',(23.6927090405067,-7.59393455934042,
0.));
#186942=CARTESIAN_POINT('Ctrl Pts',(23.6927090405067,-7.59393455934042,
12.));
#186943=CARTESIAN_POINT('Ctrl Pts',(23.6678559182876,-7.59704765299572,
0.));
#186944=CARTESIAN_POINT('Ctrl Pts',(23.6678559182876,-7.59704765299572,
12.));
#186945=CARTESIAN_POINT('Ctrl Pts',(23.6430766661419,-7.6000913013013,0.));
#186946=CARTESIAN_POINT('Ctrl Pts',(23.6430766661419,-7.6000913013013,12.));
#186947=CARTESIAN_POINT('Ctrl Pts',(23.6183718346576,-7.60306571877806,
0.));
#186948=CARTESIAN_POINT('Ctrl Pts',(23.6183718346576,-7.60306571877806,
12.));
#186949=CARTESIAN_POINT('Ctrl Pts',(23.5937419781244,-7.60597112277094,
0.));
#186950=CARTESIAN_POINT('Ctrl Pts',(23.5937419781244,-7.60597112277094,
12.));
#186951=CARTESIAN_POINT('Ctrl Pts',(23.5691876544243,-7.608807733446,0.));
#186952=CARTESIAN_POINT('Ctrl Pts',(23.5691876544243,-7.608807733446,12.));
#186953=CARTESIAN_POINT('Ctrl Pts',(23.5447094252028,-7.61157577385372,
0.));
#186954=CARTESIAN_POINT('Ctrl Pts',(23.5447094252028,-7.61157577385372,
12.));
#186955=CARTESIAN_POINT('Ctrl Pts',(23.5203078560128,-7.61427546999299,
0.));
#186956=CARTESIAN_POINT('Ctrl Pts',(23.5203078560128,-7.61427546999299,
12.));
#186957=CARTESIAN_POINT('Ctrl Pts',(23.4959835164608,-7.61690705088319,
0.));
#186958=CARTESIAN_POINT('Ctrl Pts',(23.4959835164608,-7.61690705088319,
12.));
#186959=CARTESIAN_POINT('Ctrl Pts',(23.4717369803438,-7.61947074863978,
0.));
#186960=CARTESIAN_POINT('Ctrl Pts',(23.4717369803438,-7.61947074863978,
12.));
#186961=CARTESIAN_POINT('Ctrl Pts',(23.4475688257854,-7.62196679855957,
0.));
#186962=CARTESIAN_POINT('Ctrl Pts',(23.4475688257854,-7.62196679855957,
12.));
#186963=CARTESIAN_POINT('Ctrl Pts',(23.4234796353544,-7.62439543920055,
0.));
#186964=CARTESIAN_POINT('Ctrl Pts',(23.4234796353544,-7.62439543920055,
12.));
#186965=CARTESIAN_POINT('Ctrl Pts',(23.3994699961122,-7.62675691240335,
0.));
#186966=CARTESIAN_POINT('Ctrl Pts',(23.3994699961122,-7.62675691240335,
12.));
#186967=CARTESIAN_POINT('Ctrl Pts',(23.3755404996638,-7.62905146332598,
0.));
#186968=CARTESIAN_POINT('Ctrl Pts',(23.3755404996638,-7.62905146332598,
12.));
#186969=CARTESIAN_POINT('Ctrl Pts',(23.3516917421973,-7.63127934048139,
0.));
#186970=CARTESIAN_POINT('Ctrl Pts',(23.3516917421973,-7.63127934048139,
12.));
#186971=CARTESIAN_POINT('Ctrl Pts',(23.3279243245241,-7.63344079578163,
0.));
#186972=CARTESIAN_POINT('Ctrl Pts',(23.3279243245241,-7.63344079578163,
12.));
#186973=CARTESIAN_POINT('Ctrl Pts',(23.3042388521021,-7.63553608458784,
0.));
#186974=CARTESIAN_POINT('Ctrl Pts',(23.3042388521021,-7.63553608458784,
12.));
#186975=CARTESIAN_POINT('Ctrl Pts',(23.2806359350853,-7.63756546576375,
0.));
#186976=CARTESIAN_POINT('Ctrl Pts',(23.2806359350853,-7.63756546576375,
12.));
#186977=CARTESIAN_POINT('Ctrl Pts',(23.2571161884487,-7.63952920172837,
0.));
#186978=CARTESIAN_POINT('Ctrl Pts',(23.2571161884487,-7.63952920172837,
12.));
#186979=CARTESIAN_POINT('Ctrl Pts',(23.2336802320912,-7.64142755851508,
0.));
#186980=CARTESIAN_POINT('Ctrl Pts',(23.2336802320912,-7.64142755851508,
12.));
#186981=CARTESIAN_POINT('Ctrl Pts',(23.2103286909399,-7.64326080583684,
0.));
#186982=CARTESIAN_POINT('Ctrl Pts',(23.2103286909399,-7.64326080583684,
12.));
#186983=CARTESIAN_POINT('Ctrl Pts',(23.1870621950452,-7.64502921715483,
0.));
#186984=CARTESIAN_POINT('Ctrl Pts',(23.1870621950452,-7.64502921715483,
12.));
#186985=CARTESIAN_POINT('Ctrl Pts',(23.1638813796691,-7.64673306975797,
0.));
#186986=CARTESIAN_POINT('Ctrl Pts',(23.1638813796691,-7.64673306975797,
12.));
#186987=CARTESIAN_POINT('Ctrl Pts',(23.1407868853815,-7.64837264482929,
0.));
#186988=CARTESIAN_POINT('Ctrl Pts',(23.1407868853815,-7.64837264482929,
12.));
#186989=CARTESIAN_POINT('Ctrl Pts',(23.1177793581674,-7.64994822749845,
0.));
#186990=CARTESIAN_POINT('Ctrl Pts',(23.1177793581674,-7.64994822749845,
12.));
#186991=CARTESIAN_POINT('Ctrl Pts',(23.0948594495246,-7.65146010690465,
0.));
#186992=CARTESIAN_POINT('Ctrl Pts',(23.0948594495246,-7.65146010690465,
12.));
#186993=CARTESIAN_POINT('Ctrl Pts',(23.072027816555,-7.65290857626357,0.));
#186994=CARTESIAN_POINT('Ctrl Pts',(23.072027816555,-7.65290857626357,12.));
#186995=CARTESIAN_POINT('Ctrl Pts',(23.049285122053,-7.65429393293955,0.));
#186996=CARTESIAN_POINT('Ctrl Pts',(23.049285122053,-7.65429393293955,12.));
#186997=CARTESIAN_POINT('Ctrl Pts',(23.0266320345792,-7.65561647852555,
0.));
#186998=CARTESIAN_POINT('Ctrl Pts',(23.0266320345792,-7.65561647852555,
12.));
#186999=CARTESIAN_POINT('Ctrl Pts',(23.004069228582,-7.6568765189133,0.));
#187000=CARTESIAN_POINT('Ctrl Pts',(23.004069228582,-7.6568765189133,12.));
#187001=CARTESIAN_POINT('Ctrl Pts',(22.9815973845301,-7.65807436436453,
0.));
#187002=CARTESIAN_POINT('Ctrl Pts',(22.9815973845301,-7.65807436436453,
12.));
#187003=CARTESIAN_POINT('Ctrl Pts',(22.9592171890332,-7.65921032958912,
0.));
#187004=CARTESIAN_POINT('Ctrl Pts',(22.9592171890332,-7.65921032958912,
12.));
#187005=CARTESIAN_POINT('Ctrl Pts',(22.9369293349592,-7.66028473382777,
0.));
#187006=CARTESIAN_POINT('Ctrl Pts',(22.9369293349592,-7.66028473382777,
12.));
#187007=CARTESIAN_POINT('Ctrl Pts',(22.9147345215418,-7.661297900941,0.));
#187008=CARTESIAN_POINT('Ctrl Pts',(22.9147345215418,-7.661297900941,12.));
#187009=CARTESIAN_POINT('Ctrl Pts',(22.8926334544879,-7.66225015950148,
0.));
#187010=CARTESIAN_POINT('Ctrl Pts',(22.8926334544879,-7.66225015950148,
12.));
#187011=CARTESIAN_POINT('Ctrl Pts',(22.870626846128,-7.66314184287334,0.));
#187012=CARTESIAN_POINT('Ctrl Pts',(22.870626846128,-7.66314184287334,12.));
#187013=CARTESIAN_POINT('Ctrl Pts',(22.8487154155569,-7.66397328929805,
0.));
#187014=CARTESIAN_POINT('Ctrl Pts',(22.8487154155569,-7.66397328929805,
12.));
#187015=CARTESIAN_POINT('Ctrl Pts',(22.8268998887678,-7.66474484198553,
0.));
#187016=CARTESIAN_POINT('Ctrl Pts',(22.8268998887678,-7.66474484198553,
12.));
#187017=CARTESIAN_POINT('Ctrl Pts',(22.8051809987833,-7.66545684920988,
0.));
#187018=CARTESIAN_POINT('Ctrl Pts',(22.8051809987833,-7.66545684920988,
12.));
#187019=CARTESIAN_POINT('Ctrl Pts',(22.7835594857697,-7.66610966441259,
0.));
#187020=CARTESIAN_POINT('Ctrl Pts',(22.7835594857697,-7.66610966441259,
12.));
#187021=CARTESIAN_POINT('Ctrl Pts',(22.7620360971839,-7.66670364630273,
0.));
#187022=CARTESIAN_POINT('Ctrl Pts',(22.7620360971839,-7.66670364630273,
12.));
#187023=CARTESIAN_POINT('Ctrl Pts',(22.7406115879508,-7.66723915895413,
0.));
#187024=CARTESIAN_POINT('Ctrl Pts',(22.7406115879508,-7.66723915895413,
12.));
#187025=CARTESIAN_POINT('Ctrl Pts',(22.7192867206242,-7.6677165719101,0.));
#187026=CARTESIAN_POINT('Ctrl Pts',(22.7192867206242,-7.6677165719101,12.));
#187027=CARTESIAN_POINT('Ctrl Pts',(22.6980622655446,-7.66813626029277,
0.));
#187028=CARTESIAN_POINT('Ctrl Pts',(22.6980622655446,-7.66813626029277,
12.));
#187029=CARTESIAN_POINT('Ctrl Pts',(22.6769390009889,-7.66849860491763,
0.));
#187030=CARTESIAN_POINT('Ctrl Pts',(22.6769390009889,-7.66849860491763,
12.));
#187031=CARTESIAN_POINT('Ctrl Pts',(22.6559177133133,-7.66880399241354,
0.));
#187032=CARTESIAN_POINT('Ctrl Pts',(22.6559177133133,-7.66880399241354,
12.));
#187033=CARTESIAN_POINT('Ctrl Pts',(22.6349991971547,-7.66905281533745,
0.));
#187034=CARTESIAN_POINT('Ctrl Pts',(22.6349991971547,-7.66905281533745,
12.));
#187035=CARTESIAN_POINT('Ctrl Pts',(22.6141842556248,-7.66924547229435,
0.));
#187036=CARTESIAN_POINT('Ctrl Pts',(22.6141842556248,-7.66924547229435,
12.));
#187037=CARTESIAN_POINT('Ctrl Pts',(22.5934737004955,-7.66938236806241,
0.));
#187038=CARTESIAN_POINT('Ctrl Pts',(22.5934737004955,-7.66938236806241,
12.));
#187039=CARTESIAN_POINT('Ctrl Pts',(22.5728683523828,-7.66946391372299,
0.));
#187040=CARTESIAN_POINT('Ctrl Pts',(22.5728683523828,-7.66946391372299,
12.));
#187041=CARTESIAN_POINT('Ctrl Pts',(22.5523690409109,-7.66949052679672,
0.));
#187042=CARTESIAN_POINT('Ctrl Pts',(22.5523690409109,-7.66949052679672,
12.));
#187043=CARTESIAN_POINT('Ctrl Pts',(22.5319766049191,-7.66946263138116,
0.));
#187044=CARTESIAN_POINT('Ctrl Pts',(22.5319766049191,-7.66946263138116,
12.));
#187045=CARTESIAN_POINT('Ctrl Pts',(22.5116918927023,-7.66938065829083,
0.));
#187046=CARTESIAN_POINT('Ctrl Pts',(22.5116918927023,-7.66938065829083,
12.));
#187047=CARTESIAN_POINT('Ctrl Pts',(22.4915157622308,-7.66924504520302,
0.));
#187048=CARTESIAN_POINT('Ctrl Pts',(22.4915157622308,-7.66924504520302,
12.));
#187049=CARTESIAN_POINT('Ctrl Pts',(22.47144908137,-7.66905623680836,0.));
#187050=CARTESIAN_POINT('Ctrl Pts',(22.47144908137,-7.66905623680836,12.));
#187051=CARTESIAN_POINT('Ctrl Pts',(22.4514927280862,-7.6688146849666,0.));
#187052=CARTESIAN_POINT('Ctrl Pts',(22.4514927280862,-7.6688146849666,12.));
#187053=CARTESIAN_POINT('Ctrl Pts',(22.4316475906616,-7.66852084886746,
0.));
#187054=CARTESIAN_POINT('Ctrl Pts',(22.4316475906616,-7.66852084886746,
12.));
#187055=CARTESIAN_POINT('Ctrl Pts',(22.411914567977,-7.66817519519682,0.));
#187056=CARTESIAN_POINT('Ctrl Pts',(22.411914567977,-7.66817519519682,12.));
#187057=CARTESIAN_POINT('Ctrl Pts',(22.3922945697782,-7.6677781983082,0.));
#187058=CARTESIAN_POINT('Ctrl Pts',(22.3922945697782,-7.6677781983082,12.));
#187059=CARTESIAN_POINT('Ctrl Pts',(22.3727885169361,-7.66733034039887,
0.));
#187060=CARTESIAN_POINT('Ctrl Pts',(22.3727885169361,-7.66733034039887,
12.));
#187061=CARTESIAN_POINT('Ctrl Pts',(22.3533973417013,-7.66683211169134,
0.));
#187062=CARTESIAN_POINT('Ctrl Pts',(22.3533973417013,-7.66683211169134,
12.));
#187063=CARTESIAN_POINT('Ctrl Pts',(22.3341219879454,-7.66628401061906,
0.));
#187064=CARTESIAN_POINT('Ctrl Pts',(22.3341219879454,-7.66628401061906,
12.));
#187065=CARTESIAN_POINT('Ctrl Pts',(22.3149634114823,-7.66568654402442,
0.));
#187066=CARTESIAN_POINT('Ctrl Pts',(22.3149634114823,-7.66568654402442,
12.));
#187067=CARTESIAN_POINT('Ctrl Pts',(22.2959225803925,-7.66504022736263,
0.));
#187068=CARTESIAN_POINT('Ctrl Pts',(22.2959225803925,-7.66504022736263,
12.));
#187069=CARTESIAN_POINT('Ctrl Pts',(22.2770004753332,-7.66434558490973,
0.));
#187070=CARTESIAN_POINT('Ctrl Pts',(22.2770004753332,-7.66434558490973,
12.));
#187071=CARTESIAN_POINT('Ctrl Pts',(22.2581980898487,-7.66360314997662,
0.));
#187072=CARTESIAN_POINT('Ctrl Pts',(22.2581980898487,-7.66360314997662,
12.));
#187073=CARTESIAN_POINT('Ctrl Pts',(22.239516430656,-7.66281346512546,0.));
#187074=CARTESIAN_POINT('Ctrl Pts',(22.239516430656,-7.66281346512546,12.));
#187075=CARTESIAN_POINT('Ctrl Pts',(22.2209565180098,-7.66197708240436,
0.));
#187076=CARTESIAN_POINT('Ctrl Pts',(22.2209565180098,-7.66197708240436,
12.));
#187077=CARTESIAN_POINT('Ctrl Pts',(22.2025193860972,-7.66109456359292,
0.));
#187078=CARTESIAN_POINT('Ctrl Pts',(22.2025193860972,-7.66109456359292,
12.));
#187079=CARTESIAN_POINT('Ctrl Pts',(22.1842060834092,-7.66016648045008,
0.));
#187080=CARTESIAN_POINT('Ctrl Pts',(22.1842060834092,-7.66016648045008,
12.));
#187081=CARTESIAN_POINT('Ctrl Pts',(22.1660176731174,-7.65919341496926,
0.));
#187082=CARTESIAN_POINT('Ctrl Pts',(22.1660176731174,-7.65919341496926,
12.));
#187083=CARTESIAN_POINT('Ctrl Pts',(22.1479552334206,-7.65817595963351,
0.));
#187084=CARTESIAN_POINT('Ctrl Pts',(22.1479552334206,-7.65817595963351,
12.));
#187085=CARTESIAN_POINT('Ctrl Pts',(22.1300198579671,-7.65711471769407,
0.));
#187086=CARTESIAN_POINT('Ctrl Pts',(22.1300198579671,-7.65711471769407,
12.));
#187087=CARTESIAN_POINT('Ctrl Pts',(22.1122126563327,-7.65601030346819,
0.));
#187088=CARTESIAN_POINT('Ctrl Pts',(22.1122126563327,-7.65601030346819,
12.));
#187089=CARTESIAN_POINT('Ctrl Pts',(22.094534754469,-7.65486334263651,0.));
#187090=CARTESIAN_POINT('Ctrl Pts',(22.094534754469,-7.65486334263651,12.));
#187091=CARTESIAN_POINT('Ctrl Pts',(22.0769872951596,-7.65367447254945,
0.));
#187092=CARTESIAN_POINT('Ctrl Pts',(22.0769872951596,-7.65367447254945,
12.));
#187093=CARTESIAN_POINT('Ctrl Pts',(22.0595714384432,-7.65244434253104,
0.));
#187094=CARTESIAN_POINT('Ctrl Pts',(22.0595714384432,-7.65244434253104,
12.));
#187095=CARTESIAN_POINT('Ctrl Pts',(22.0422883621176,-7.65117361421347,
0.));
#187096=CARTESIAN_POINT('Ctrl Pts',(22.0422883621176,-7.65117361421347,
12.));
#187097=CARTESIAN_POINT('Ctrl Pts',(22.0251392623209,-7.64986296190157,
0.));
#187098=CARTESIAN_POINT('Ctrl Pts',(22.0251392623209,-7.64986296190157,
12.));
#187099=CARTESIAN_POINT('Ctrl Pts',(22.0081253540773,-7.64851307293346,
0.));
#187100=CARTESIAN_POINT('Ctrl Pts',(22.0081253540773,-7.64851307293346,
12.));
#187101=CARTESIAN_POINT('Ctrl Pts',(21.9912478718542,-7.64712464805258,
0.));
#187102=CARTESIAN_POINT('Ctrl Pts',(21.9912478718542,-7.64712464805258,
12.));
#187103=CARTESIAN_POINT('Ctrl Pts',(21.97450807008,-7.64569840177359,0.));
#187104=CARTESIAN_POINT('Ctrl Pts',(21.97450807008,-7.64569840177359,12.));
#187105=CARTESIAN_POINT('Ctrl Pts',(21.9579072237653,-7.64423506279154,
0.));
#187106=CARTESIAN_POINT('Ctrl Pts',(21.9579072237653,-7.64423506279154,
12.));
#187107=CARTESIAN_POINT('Ctrl Pts',(21.9414466292074,-7.64273537442707,
0.));
#187108=CARTESIAN_POINT('Ctrl Pts',(21.9414466292074,-7.64273537442707,
12.));
#187109=CARTESIAN_POINT('Ctrl Pts',(21.9251276046546,-7.6412000950654,0.));
#187110=CARTESIAN_POINT('Ctrl Pts',(21.9251276046546,-7.6412000950654,12.));
#187111=CARTESIAN_POINT('Ctrl Pts',(21.9089514909873,-7.63962999860917,
0.));
#187112=CARTESIAN_POINT('Ctrl Pts',(21.9089514909873,-7.63962999860917,
12.));
#187113=CARTESIAN_POINT('Ctrl Pts',(21.8929196523511,-7.63802587492008,
0.));
#187114=CARTESIAN_POINT('Ctrl Pts',(21.8929196523511,-7.63802587492008,
12.));
#187115=CARTESIAN_POINT('Ctrl Pts',(21.8770334769492,-7.63638853033368,
0.));
#187116=CARTESIAN_POINT('Ctrl Pts',(21.8770334769492,-7.63638853033368,
12.));
#187117=CARTESIAN_POINT('Ctrl Pts',(21.8612943779086,-7.63471878821204,
0.));
#187118=CARTESIAN_POINT('Ctrl Pts',(21.8612943779086,-7.63471878821204,
12.));
#187119=CARTESIAN_POINT('Ctrl Pts',(21.8457037941084,-7.63301748948936,
0.));
#187120=CARTESIAN_POINT('Ctrl Pts',(21.8457037941084,-7.63301748948936,
12.));
#187121=CARTESIAN_POINT('Ctrl Pts',(21.8302631910197,-7.6312854932304,0.));
#187122=CARTESIAN_POINT('Ctrl Pts',(21.8302631910197,-7.6312854932304,12.));
#187123=CARTESIAN_POINT('Ctrl Pts',(21.8149740615093,-7.62952367718151,
0.));
#187124=CARTESIAN_POINT('Ctrl Pts',(21.8149740615093,-7.62952367718151,
12.));
#187125=CARTESIAN_POINT('Ctrl Pts',(21.7998379268583,-7.62773293842409,
0.));
#187126=CARTESIAN_POINT('Ctrl Pts',(21.7998379268583,-7.62773293842409,
12.));
#187127=CARTESIAN_POINT('Ctrl Pts',(21.7848563378022,-7.62591419404521,
0.));
#187128=CARTESIAN_POINT('Ctrl Pts',(21.7848563378022,-7.62591419404521,
12.));
#187129=CARTESIAN_POINT('Ctrl Pts',(21.7700308755583,-7.62406838181164,
0.));
#187130=CARTESIAN_POINT('Ctrl Pts',(21.7700308755583,-7.62406838181164,
12.));
#187131=CARTESIAN_POINT('Ctrl Pts',(21.7553631528329,-7.62219646084226,
0.));
#187132=CARTESIAN_POINT('Ctrl Pts',(21.7553631528329,-7.62219646084226,
12.));
#187133=CARTESIAN_POINT('Ctrl Pts',(21.7408548148657,-7.62029941230855,
0.));
#187134=CARTESIAN_POINT('Ctrl Pts',(21.7408548148657,-7.62029941230855,
12.));
#187135=CARTESIAN_POINT('Ctrl Pts',(21.7265075407977,-7.61837824030542,
0.));
#187136=CARTESIAN_POINT('Ctrl Pts',(21.7265075407977,-7.61837824030542,
12.));
#187137=CARTESIAN_POINT('Ctrl Pts',(21.7123230449835,-7.61643397270425,
0.));
#187138=CARTESIAN_POINT('Ctrl Pts',(21.7123230449835,-7.61643397270425,
12.));
#187139=CARTESIAN_POINT('Ctrl Pts',(21.6983030783321,-7.61446766202787,
0.));
#187140=CARTESIAN_POINT('Ctrl Pts',(21.6983030783321,-7.61446766202787,
12.));
#187141=CARTESIAN_POINT('Ctrl Pts',(21.6844494295813,-7.61248038630265,
0.));
#187142=CARTESIAN_POINT('Ctrl Pts',(21.6844494295813,-7.61248038630265,
12.));
#187143=CARTESIAN_POINT('Ctrl Pts',(21.6707639267573,-7.6104732500095,0.));
#187144=CARTESIAN_POINT('Ctrl Pts',(21.6707639267573,-7.6104732500095,12.));
#187145=CARTESIAN_POINT('Ctrl Pts',(21.6572484388079,-7.60844738512872,
0.));
#187146=CARTESIAN_POINT('Ctrl Pts',(21.6572484388079,-7.60844738512872,
12.));
#187147=CARTESIAN_POINT('Ctrl Pts',(21.6439048771743,-7.60640395216359,
0.));
#187148=CARTESIAN_POINT('Ctrl Pts',(21.6439048771743,-7.60640395216359,
12.));
#187149=CARTESIAN_POINT('Ctrl Pts',(21.6307351973823,-7.604344141183,0.));
#187150=CARTESIAN_POINT('Ctrl Pts',(21.6307351973823,-7.604344141183,12.));
#187151=CARTESIAN_POINT('Ctrl Pts',(21.6177414005991,-7.60226917285432,
0.));
#187152=CARTESIAN_POINT('Ctrl Pts',(21.6177414005991,-7.60226917285432,
12.));
#187153=CARTESIAN_POINT('Ctrl Pts',(21.6049255358842,-7.60018029988238,
0.));
#187154=CARTESIAN_POINT('Ctrl Pts',(21.6049255358842,-7.60018029988238,
12.));
#187155=CARTESIAN_POINT('Ctrl Pts',(21.5922897024466,-7.59807880846193,
0.));
#187156=CARTESIAN_POINT('Ctrl Pts',(21.5922897024466,-7.59807880846193,
12.));
#187157=CARTESIAN_POINT('Ctrl Pts',(21.5798360518978,-7.59596601973589,
0.));
#187158=CARTESIAN_POINT('Ctrl Pts',(21.5798360518978,-7.59596601973589,
12.));
#187159=CARTESIAN_POINT('Ctrl Pts',(21.5675667904728,-7.5938432912493,0.));
#187160=CARTESIAN_POINT('Ctrl Pts',(21.5675667904728,-7.5938432912493,12.));
#187161=CARTESIAN_POINT('Ctrl Pts',(21.5554841813465,-7.59171201844793,
0.));
#187162=CARTESIAN_POINT('Ctrl Pts',(21.5554841813465,-7.59171201844793,
12.));
#187163=CARTESIAN_POINT('Ctrl Pts',(21.5435905470113,-7.58957363620026,
0.));
#187164=CARTESIAN_POINT('Ctrl Pts',(21.5435905470113,-7.58957363620026,
12.));
#187165=CARTESIAN_POINT('Ctrl Pts',(21.5318882716735,-7.58742962034834,
0.));
#187166=CARTESIAN_POINT('Ctrl Pts',(21.5318882716735,-7.58742962034834,
12.));
#187167=CARTESIAN_POINT('Ctrl Pts',(21.5203798035294,-7.58528148919114,
0.));
#187168=CARTESIAN_POINT('Ctrl Pts',(21.5203798035294,-7.58528148919114,
12.));
#187169=CARTESIAN_POINT('Ctrl Pts',(21.5090676573866,-7.58313080519159,
0.));
#187170=CARTESIAN_POINT('Ctrl Pts',(21.5090676573866,-7.58313080519159,
12.));
#187171=CARTESIAN_POINT('Ctrl Pts',(21.4979544192739,-7.5809791779073,0.));
#187172=CARTESIAN_POINT('Ctrl Pts',(21.4979544192739,-7.5809791779073,12.));
#187173=CARTESIAN_POINT('Ctrl Pts',(21.4870427508193,-7.57882826679131,
0.));
#187174=CARTESIAN_POINT('Ctrl Pts',(21.4870427508193,-7.57882826679131,
12.));
#187175=CARTESIAN_POINT('Ctrl Pts',(21.4763353936766,-7.57667978403003,
0.));
#187176=CARTESIAN_POINT('Ctrl Pts',(21.4763353936766,-7.57667978403003,
12.));
#187177=CARTESIAN_POINT('Ctrl Pts',(21.4658351740135,-7.57453549743435,
0.));
#187178=CARTESIAN_POINT('Ctrl Pts',(21.4658351740135,-7.57453549743435,
12.));
#187179=CARTESIAN_POINT('Ctrl Pts',(21.4555450053147,-7.57239723223521,
0.));
#187180=CARTESIAN_POINT('Ctrl Pts',(21.4555450053147,-7.57239723223521,
12.));
#187181=CARTESIAN_POINT('Ctrl Pts',(21.445467890751,-7.5702668726117,0.));
#187182=CARTESIAN_POINT('Ctrl Pts',(21.445467890751,-7.5702668726117,12.));
#187183=CARTESIAN_POINT('Ctrl Pts',(21.435606926151,-7.56814636360842,0.));
#187184=CARTESIAN_POINT('Ctrl Pts',(21.435606926151,-7.56814636360842,12.));
#187185=CARTESIAN_POINT('Ctrl Pts',(21.4259653015732,-7.56603771218706,
0.));
#187186=CARTESIAN_POINT('Ctrl Pts',(21.4259653015732,-7.56603771218706,
12.));
#187187=CARTESIAN_POINT('Ctrl Pts',(21.4165463106252,-7.56394299313683,
0.));
#187188=CARTESIAN_POINT('Ctrl Pts',(21.4165463106252,-7.56394299313683,
12.));
#187189=CARTESIAN_POINT('Ctrl Pts',(21.4073533630364,-7.56186435703622,
0.));
#187190=CARTESIAN_POINT('Ctrl Pts',(21.4073533630364,-7.56186435703622,
12.));
#187191=CARTESIAN_POINT('Ctrl Pts',(21.3983899952988,-7.55980403700615,
0.));
#187192=CARTESIAN_POINT('Ctrl Pts',(21.3983899952988,-7.55980403700615,
12.));
#187193=CARTESIAN_POINT('Ctrl Pts',(21.3896598842119,-7.55776435731422,
0.));
#187194=CARTESIAN_POINT('Ctrl Pts',(21.3896598842119,-7.55776435731422,
12.));
#187195=CARTESIAN_POINT('Ctrl Pts',(21.3811668478933,-7.55574773403508,
0.));
#187196=CARTESIAN_POINT('Ctrl Pts',(21.3811668478933,-7.55574773403508,
12.));
#187197=CARTESIAN_POINT('Ctrl Pts',(21.3729148390244,-7.55375667080032,
0.));
#187198=CARTESIAN_POINT('Ctrl Pts',(21.3729148390244,-7.55375667080032,
12.));
#187199=CARTESIAN_POINT('Ctrl Pts',(21.3649079431864,-7.55179375777442,
0.));
#187200=CARTESIAN_POINT('Ctrl Pts',(21.3649079431864,-7.55179375777442,
12.));
#187201=CARTESIAN_POINT('Ctrl Pts',(21.3571503685853,-7.54986166521307,
0.));
#187202=CARTESIAN_POINT('Ctrl Pts',(21.3571503685853,-7.54986166521307,
12.));
#187203=CARTESIAN_POINT('Ctrl Pts',(21.349646476153,-7.54796316246327,0.));
#187204=CARTESIAN_POINT('Ctrl Pts',(21.349646476153,-7.54796316246327,12.));
#187205=CARTESIAN_POINT('Ctrl Pts',(21.3424008295038,-7.54610114948351,
0.));
#187206=CARTESIAN_POINT('Ctrl Pts',(21.3424008295038,-7.54610114948351,
12.));
#187207=CARTESIAN_POINT('Ctrl Pts',(21.3354182340149,-7.54427868151269,
0.));
#187208=CARTESIAN_POINT('Ctrl Pts',(21.3354182340149,-7.54427868151269,
12.));
#187209=CARTESIAN_POINT('Ctrl Pts',(21.328703791771,-7.54249900377032,0.));
#187210=CARTESIAN_POINT('Ctrl Pts',(21.328703791771,-7.54249900377032,12.));
#187211=CARTESIAN_POINT('Ctrl Pts',(21.3222628524165,-7.5407655203828,0.));
#187212=CARTESIAN_POINT('Ctrl Pts',(21.3222628524165,-7.5407655203828,12.));
#187213=CARTESIAN_POINT('Ctrl Pts',(21.3161009456256,-7.53908175169899,
0.));
#187214=CARTESIAN_POINT('Ctrl Pts',(21.3161009456256,-7.53908175169899,
12.));
#187215=CARTESIAN_POINT('Ctrl Pts',(21.3102237167729,-7.5374512936462,0.));
#187216=CARTESIAN_POINT('Ctrl Pts',(21.3102237167729,-7.5374512936462,12.));
#187217=CARTESIAN_POINT('Ctrl Pts',(21.3046368712156,-7.53587778251743,
0.));
#187218=CARTESIAN_POINT('Ctrl Pts',(21.3046368712156,-7.53587778251743,
12.));
#187219=CARTESIAN_POINT('Ctrl Pts',(21.2993464250717,-7.53436505309949,
0.));
#187220=CARTESIAN_POINT('Ctrl Pts',(21.2993464250717,-7.53436505309949,
12.));
#187221=CARTESIAN_POINT('Ctrl Pts',(21.2943588989331,-7.53291726078527,
0.));
#187222=CARTESIAN_POINT('Ctrl Pts',(21.2943588989331,-7.53291726078527,
12.));
#187223=CARTESIAN_POINT('Ctrl Pts',(21.2896816163843,-7.53153906987847,
0.));
#187224=CARTESIAN_POINT('Ctrl Pts',(21.2896816163843,-7.53153906987847,
12.));
#187225=CARTESIAN_POINT('Ctrl Pts',(21.2853226580658,-7.53023562438221,
0.));
#187226=CARTESIAN_POINT('Ctrl Pts',(21.2853226580658,-7.53023562438221,
12.));
#187227=CARTESIAN_POINT('Ctrl Pts',(21.2812902781143,-7.52901217930407,
0.));
#187228=CARTESIAN_POINT('Ctrl Pts',(21.2812902781143,-7.52901217930407,
12.));
#187229=CARTESIAN_POINT('Ctrl Pts',(21.2775925269651,-7.52787386225344,
0.));
#187230=CARTESIAN_POINT('Ctrl Pts',(21.2775925269651,-7.52787386225344,
12.));
#187231=CARTESIAN_POINT('Ctrl Pts',(21.2742366113578,-7.52682526918561,
0.));
#187232=CARTESIAN_POINT('Ctrl Pts',(21.2742366113578,-7.52682526918561,
12.));
#187233=CARTESIAN_POINT('Ctrl Pts',(21.2712301573465,-7.52587126095544,
0.));
#187234=CARTESIAN_POINT('Ctrl Pts',(21.2712301573465,-7.52587126095544,
12.));
#187235=CARTESIAN_POINT('Ctrl Pts',(21.2685823838672,-7.52501770333522,
0.));
#187236=CARTESIAN_POINT('Ctrl Pts',(21.2685823838672,-7.52501770333522,
12.));
#187237=CARTESIAN_POINT('Ctrl Pts',(21.266305915706,-7.52427261074264,0.));
#187238=CARTESIAN_POINT('Ctrl Pts',(21.266305915706,-7.52427261074264,12.));
#187239=CARTESIAN_POINT('Ctrl Pts',(21.2644161259965,-7.52364573027521,
0.));
#187240=CARTESIAN_POINT('Ctrl Pts',(21.2644161259965,-7.52364573027521,
12.));
#187241=CARTESIAN_POINT('Ctrl Pts',(21.262927782038,-7.52314642316203,0.));
#187242=CARTESIAN_POINT('Ctrl Pts',(21.262927782038,-7.52314642316203,12.));
#187243=CARTESIAN_POINT('Ctrl Pts',(21.261852128355,-7.52278182242728,0.));
#187244=CARTESIAN_POINT('Ctrl Pts',(21.261852128355,-7.52278182242728,12.));
#187245=CARTESIAN_POINT('Ctrl Pts',(21.2613260540651,-7.52260064231736,
0.));
#187246=CARTESIAN_POINT('Ctrl Pts',(21.2613260540651,-7.52260064231736,
12.));
#187247=CARTESIAN_POINT('Ctrl Pts',(21.261120447486,-7.52252744144958,0.));
#187248=CARTESIAN_POINT('Ctrl Pts',(21.261120447486,-7.52252744144958,12.));
#187249=CARTESIAN_POINT('Ctrl Pts',(21.2610673466883,-7.52250649703992,
0.));
#187250=CARTESIAN_POINT('Ctrl Pts',(21.2610673466883,-7.52250649703992,
12.));
#187251=CARTESIAN_POINT('Ctrl Pts',(21.2610617890679,-7.52250298901266,
0.));
#187252=CARTESIAN_POINT('Ctrl Pts',(21.2610617890679,-7.52250298901266,
12.));
#187253=CARTESIAN_POINT('',(24.9347862158358,-7.36589684767345,0.));
#187254=CARTESIAN_POINT('Ctrl Pts',(24.9347862158358,-7.36589684767345,
0.));
#187255=CARTESIAN_POINT('Ctrl Pts',(24.9292275670674,-7.36721909028843,
0.));
#187256=CARTESIAN_POINT('Ctrl Pts',(24.9181155530543,-7.36985593120091,
0.));
#187257=CARTESIAN_POINT('Ctrl Pts',(24.901463382605,-7.37378825961676,0.));
#187258=CARTESIAN_POINT('Ctrl Pts',(24.8792921911115,-7.3789854964027,0.));
#187259=CARTESIAN_POINT('Ctrl Pts',(24.8516310625176,-7.38540558903621,
0.));
#187260=CARTESIAN_POINT('Ctrl Pts',(24.8240228520893,-7.39174922585809,
0.));
#187261=CARTESIAN_POINT('Ctrl Pts',(24.7964676646431,-7.39801641583013,
0.));
#187262=CARTESIAN_POINT('Ctrl Pts',(24.7689656668983,-7.40420718661603,
0.));
#187263=CARTESIAN_POINT('Ctrl Pts',(24.7415170994784,-7.41032159082382,
0.));
#187264=CARTESIAN_POINT('Ctrl Pts',(24.7141222950051,-7.41635971481674,
0.));
#187265=CARTESIAN_POINT('Ctrl Pts',(24.6867816727192,-7.42232167766266,
0.));
#187266=CARTESIAN_POINT('Ctrl Pts',(24.6594957128756,-7.42820762159126,
0.));
#187267=CARTESIAN_POINT('Ctrl Pts',(24.6322649369517,-7.43401770489524,
0.));
#187268=CARTESIAN_POINT('Ctrl Pts',(24.6050898852368,-7.43975209375504,
0.));
#187269=CARTESIAN_POINT('Ctrl Pts',(24.577971096086,-7.44541095473135,0.));
#187270=CARTESIAN_POINT('Ctrl Pts',(24.5509090831559,-7.4509944465116,0.));
#187271=CARTESIAN_POINT('Ctrl Pts',(24.5239043173072,-7.45650271335862,
0.));
#187272=CARTESIAN_POINT('Ctrl Pts',(24.4969572391483,-7.46193588961464,
0.));
#187273=CARTESIAN_POINT('Ctrl Pts',(24.4700682684524,-7.46729410308787,
0.));
#187274=CARTESIAN_POINT('Ctrl Pts',(24.443237814649,-7.47257747883246,0.));
#187275=CARTESIAN_POINT('Ctrl Pts',(24.4164662871163,-7.47778614286565,
0.));
#187276=CARTESIAN_POINT('Ctrl Pts',(24.3897541049254,-7.48292022569301,
0.));
#187277=CARTESIAN_POINT('Ctrl Pts',(24.3631017084524,-7.48797986651909,
0.));
#187278=CARTESIAN_POINT('Ctrl Pts',(24.3365095573685,-7.49296521252421,
0.));
#187279=CARTESIAN_POINT('Ctrl Pts',(24.3099781253355,-7.49787641695439,
0.));
#187280=CARTESIAN_POINT('Ctrl Pts',(24.2835078958973,-7.50271363765152,
0.));
#187281=CARTESIAN_POINT('Ctrl Pts',(24.2570993577034,-7.50747703535134,
0.));
#187282=CARTESIAN_POINT('Ctrl Pts',(24.2307530003887,-7.51216677222181,
0.));
#187283=CARTESIAN_POINT('Ctrl Pts',(24.2044693092349,-7.51678300997949,
0.));
#187284=CARTESIAN_POINT('Ctrl Pts',(24.1782487641594,-7.52132590953802,
0.));
#187285=CARTESIAN_POINT('Ctrl Pts',(24.1520918425364,-7.52579563201424,
0.));
#187286=CARTESIAN_POINT('Ctrl Pts',(24.1259990209207,-7.53019233935502,
0.));
#187287=CARTESIAN_POINT('Ctrl Pts',(24.0999707772642,-7.53451619514649,
0.));
#187288=CARTESIAN_POINT('Ctrl Pts',(24.0740075927985,-7.53876736531014,
0.));
#187289=CARTESIAN_POINT('Ctrl Pts',(24.0481099543353,-7.54294601896145,
0.));
#187290=CARTESIAN_POINT('Ctrl Pts',(24.022278355453,-7.5470523288591,0.));
#187291=CARTESIAN_POINT('Ctrl Pts',(23.9965132953185,-7.55108647097441,
0.));
#187292=CARTESIAN_POINT('Ctrl Pts',(23.9708152779884,-7.55504862424812,
0.));
#187293=CARTESIAN_POINT('Ctrl Pts',(23.9451848115,-7.55893897027683,0.));
#187294=CARTESIAN_POINT('Ctrl Pts',(23.9196224070759,-7.56275769304773,
0.));
#187295=CARTESIAN_POINT('Ctrl Pts',(23.8941285782003,-7.56650497863792,
0.));
#187296=CARTESIAN_POINT('Ctrl Pts',(23.8687038399597,-7.57018101500711,
0.));
#187297=CARTESIAN_POINT('Ctrl Pts',(23.8433487096134,-7.57378599219817,
0.));
#187298=CARTESIAN_POINT('Ctrl Pts',(23.8180637069977,-7.57732010249066,
0.));
#187299=CARTESIAN_POINT('Ctrl Pts',(23.7928493549908,-7.58078354058212,
0.));
#187300=CARTESIAN_POINT('Ctrl Pts',(23.7677061799376,-7.58417650376272,
0.));
#187301=CARTESIAN_POINT('Ctrl Pts',(23.7426347121006,-7.58749919210832,
0.));
#187302=CARTESIAN_POINT('Ctrl Pts',(23.7176354860457,-7.59075180865327,
0.));
#187303=CARTESIAN_POINT('Ctrl Pts',(23.6927090405067,-7.59393455934042,
0.));
#187304=CARTESIAN_POINT('Ctrl Pts',(23.6678559182876,-7.59704765299572,
0.));
#187305=CARTESIAN_POINT('Ctrl Pts',(23.6430766661419,-7.6000913013013,0.));
#187306=CARTESIAN_POINT('Ctrl Pts',(23.6183718346576,-7.60306571877806,
0.));
#187307=CARTESIAN_POINT('Ctrl Pts',(23.5937419781244,-7.60597112277094,
0.));
#187308=CARTESIAN_POINT('Ctrl Pts',(23.5691876544243,-7.608807733446,0.));
#187309=CARTESIAN_POINT('Ctrl Pts',(23.5447094252028,-7.61157577385372,
0.));
#187310=CARTESIAN_POINT('Ctrl Pts',(23.5203078560128,-7.61427546999299,
0.));
#187311=CARTESIAN_POINT('Ctrl Pts',(23.4959835164608,-7.61690705088319,
0.));
#187312=CARTESIAN_POINT('Ctrl Pts',(23.4717369803438,-7.61947074863978,
0.));
#187313=CARTESIAN_POINT('Ctrl Pts',(23.4475688257854,-7.62196679855957,
0.));
#187314=CARTESIAN_POINT('Ctrl Pts',(23.4234796353544,-7.62439543920055,
0.));
#187315=CARTESIAN_POINT('Ctrl Pts',(23.3994699961122,-7.62675691240335,
0.));
#187316=CARTESIAN_POINT('Ctrl Pts',(23.3755404996638,-7.62905146332598,
0.));
#187317=CARTESIAN_POINT('Ctrl Pts',(23.3516917421973,-7.63127934048139,
0.));
#187318=CARTESIAN_POINT('Ctrl Pts',(23.3279243245241,-7.63344079578163,
0.));
#187319=CARTESIAN_POINT('Ctrl Pts',(23.3042388521021,-7.63553608458784,
0.));
#187320=CARTESIAN_POINT('Ctrl Pts',(23.2806359350853,-7.63756546576375,
0.));
#187321=CARTESIAN_POINT('Ctrl Pts',(23.2571161884487,-7.63952920172837,
0.));
#187322=CARTESIAN_POINT('Ctrl Pts',(23.2336802320912,-7.64142755851508,
0.));
#187323=CARTESIAN_POINT('Ctrl Pts',(23.2103286909399,-7.64326080583684,
0.));
#187324=CARTESIAN_POINT('Ctrl Pts',(23.1870621950452,-7.64502921715483,
0.));
#187325=CARTESIAN_POINT('Ctrl Pts',(23.1638813796691,-7.64673306975797,
0.));
#187326=CARTESIAN_POINT('Ctrl Pts',(23.1407868853815,-7.64837264482929,
0.));
#187327=CARTESIAN_POINT('Ctrl Pts',(23.1177793581674,-7.64994822749845,
0.));
#187328=CARTESIAN_POINT('Ctrl Pts',(23.0948594495246,-7.65146010690465,
0.));
#187329=CARTESIAN_POINT('Ctrl Pts',(23.072027816555,-7.65290857626357,0.));
#187330=CARTESIAN_POINT('Ctrl Pts',(23.049285122053,-7.65429393293955,0.));
#187331=CARTESIAN_POINT('Ctrl Pts',(23.0266320345792,-7.65561647852555,
0.));
#187332=CARTESIAN_POINT('Ctrl Pts',(23.004069228582,-7.6568765189133,0.));
#187333=CARTESIAN_POINT('Ctrl Pts',(22.9815973845301,-7.65807436436453,
0.));
#187334=CARTESIAN_POINT('Ctrl Pts',(22.9592171890332,-7.65921032958912,
0.));
#187335=CARTESIAN_POINT('Ctrl Pts',(22.9369293349592,-7.66028473382777,
0.));
#187336=CARTESIAN_POINT('Ctrl Pts',(22.9147345215418,-7.661297900941,0.));
#187337=CARTESIAN_POINT('Ctrl Pts',(22.8926334544879,-7.66225015950148,
0.));
#187338=CARTESIAN_POINT('Ctrl Pts',(22.870626846128,-7.66314184287334,0.));
#187339=CARTESIAN_POINT('Ctrl Pts',(22.8487154155569,-7.66397328929805,
0.));
#187340=CARTESIAN_POINT('Ctrl Pts',(22.8268998887678,-7.66474484198553,
0.));
#187341=CARTESIAN_POINT('Ctrl Pts',(22.8051809987833,-7.66545684920988,
0.));
#187342=CARTESIAN_POINT('Ctrl Pts',(22.7835594857697,-7.66610966441259,
0.));
#187343=CARTESIAN_POINT('Ctrl Pts',(22.7620360971839,-7.66670364630273,
0.));
#187344=CARTESIAN_POINT('Ctrl Pts',(22.7406115879508,-7.66723915895413,
0.));
#187345=CARTESIAN_POINT('Ctrl Pts',(22.7192867206242,-7.6677165719101,0.));
#187346=CARTESIAN_POINT('Ctrl Pts',(22.6980622655446,-7.66813626029277,
0.));
#187347=CARTESIAN_POINT('Ctrl Pts',(22.6769390009889,-7.66849860491763,
0.));
#187348=CARTESIAN_POINT('Ctrl Pts',(22.6559177133133,-7.66880399241354,
0.));
#187349=CARTESIAN_POINT('Ctrl Pts',(22.6349991971547,-7.66905281533745,
0.));
#187350=CARTESIAN_POINT('Ctrl Pts',(22.6141842556248,-7.66924547229435,
0.));
#187351=CARTESIAN_POINT('Ctrl Pts',(22.5934737004955,-7.66938236806241,
0.));
#187352=CARTESIAN_POINT('Ctrl Pts',(22.5728683523828,-7.66946391372299,
0.));
#187353=CARTESIAN_POINT('Ctrl Pts',(22.5523690409109,-7.66949052679672,
0.));
#187354=CARTESIAN_POINT('Ctrl Pts',(22.5319766049191,-7.66946263138116,
0.));
#187355=CARTESIAN_POINT('Ctrl Pts',(22.5116918927023,-7.66938065829083,
0.));
#187356=CARTESIAN_POINT('Ctrl Pts',(22.4915157622308,-7.66924504520302,
0.));
#187357=CARTESIAN_POINT('Ctrl Pts',(22.47144908137,-7.66905623680836,0.));
#187358=CARTESIAN_POINT('Ctrl Pts',(22.4514927280862,-7.6688146849666,0.));
#187359=CARTESIAN_POINT('Ctrl Pts',(22.4316475906616,-7.66852084886746,
0.));
#187360=CARTESIAN_POINT('Ctrl Pts',(22.411914567977,-7.66817519519682,0.));
#187361=CARTESIAN_POINT('Ctrl Pts',(22.3922945697782,-7.6677781983082,0.));
#187362=CARTESIAN_POINT('Ctrl Pts',(22.3727885169361,-7.66733034039887,
0.));
#187363=CARTESIAN_POINT('Ctrl Pts',(22.3533973417013,-7.66683211169134,
0.));
#187364=CARTESIAN_POINT('Ctrl Pts',(22.3341219879454,-7.66628401061906,
0.));
#187365=CARTESIAN_POINT('Ctrl Pts',(22.3149634114823,-7.66568654402442,
0.));
#187366=CARTESIAN_POINT('Ctrl Pts',(22.2959225803925,-7.66504022736263,
0.));
#187367=CARTESIAN_POINT('Ctrl Pts',(22.2770004753332,-7.66434558490973,
0.));
#187368=CARTESIAN_POINT('Ctrl Pts',(22.2581980898487,-7.66360314997662,
0.));
#187369=CARTESIAN_POINT('Ctrl Pts',(22.239516430656,-7.66281346512546,0.));
#187370=CARTESIAN_POINT('Ctrl Pts',(22.2209565180098,-7.66197708240436,
0.));
#187371=CARTESIAN_POINT('Ctrl Pts',(22.2025193860972,-7.66109456359292,
0.));
#187372=CARTESIAN_POINT('Ctrl Pts',(22.1842060834092,-7.66016648045008,
0.));
#187373=CARTESIAN_POINT('Ctrl Pts',(22.1660176731174,-7.65919341496926,
0.));
#187374=CARTESIAN_POINT('Ctrl Pts',(22.1479552334206,-7.65817595963351,
0.));
#187375=CARTESIAN_POINT('Ctrl Pts',(22.1300198579671,-7.65711471769407,
0.));
#187376=CARTESIAN_POINT('Ctrl Pts',(22.1122126563327,-7.65601030346819,
0.));
#187377=CARTESIAN_POINT('Ctrl Pts',(22.094534754469,-7.65486334263651,0.));
#187378=CARTESIAN_POINT('Ctrl Pts',(22.0769872951596,-7.65367447254945,
0.));
#187379=CARTESIAN_POINT('Ctrl Pts',(22.0595714384432,-7.65244434253104,
0.));
#187380=CARTESIAN_POINT('Ctrl Pts',(22.0422883621176,-7.65117361421347,
0.));
#187381=CARTESIAN_POINT('Ctrl Pts',(22.0251392623209,-7.64986296190157,
0.));
#187382=CARTESIAN_POINT('Ctrl Pts',(22.0081253540773,-7.64851307293346,
0.));
#187383=CARTESIAN_POINT('Ctrl Pts',(21.9912478718542,-7.64712464805258,
0.));
#187384=CARTESIAN_POINT('Ctrl Pts',(21.97450807008,-7.64569840177359,0.));
#187385=CARTESIAN_POINT('Ctrl Pts',(21.9579072237653,-7.64423506279154,
0.));
#187386=CARTESIAN_POINT('Ctrl Pts',(21.9414466292074,-7.64273537442707,
0.));
#187387=CARTESIAN_POINT('Ctrl Pts',(21.9251276046546,-7.6412000950654,0.));
#187388=CARTESIAN_POINT('Ctrl Pts',(21.9089514909873,-7.63962999860917,
0.));
#187389=CARTESIAN_POINT('Ctrl Pts',(21.8929196523511,-7.63802587492008,
0.));
#187390=CARTESIAN_POINT('Ctrl Pts',(21.8770334769492,-7.63638853033368,
0.));
#187391=CARTESIAN_POINT('Ctrl Pts',(21.8612943779086,-7.63471878821204,
0.));
#187392=CARTESIAN_POINT('Ctrl Pts',(21.8457037941084,-7.63301748948936,
0.));
#187393=CARTESIAN_POINT('Ctrl Pts',(21.8302631910197,-7.6312854932304,0.));
#187394=CARTESIAN_POINT('Ctrl Pts',(21.8149740615093,-7.62952367718151,
0.));
#187395=CARTESIAN_POINT('Ctrl Pts',(21.7998379268583,-7.62773293842409,
0.));
#187396=CARTESIAN_POINT('Ctrl Pts',(21.7848563378022,-7.62591419404521,
0.));
#187397=CARTESIAN_POINT('Ctrl Pts',(21.7700308755583,-7.62406838181164,
0.));
#187398=CARTESIAN_POINT('Ctrl Pts',(21.7553631528329,-7.62219646084226,
0.));
#187399=CARTESIAN_POINT('Ctrl Pts',(21.7408548148657,-7.62029941230855,
0.));
#187400=CARTESIAN_POINT('Ctrl Pts',(21.7265075407977,-7.61837824030542,
0.));
#187401=CARTESIAN_POINT('Ctrl Pts',(21.7123230449835,-7.61643397270425,
0.));
#187402=CARTESIAN_POINT('Ctrl Pts',(21.6983030783321,-7.61446766202787,
0.));
#187403=CARTESIAN_POINT('Ctrl Pts',(21.6844494295813,-7.61248038630265,
0.));
#187404=CARTESIAN_POINT('Ctrl Pts',(21.6707639267573,-7.6104732500095,0.));
#187405=CARTESIAN_POINT('Ctrl Pts',(21.6572484388079,-7.60844738512872,
0.));
#187406=CARTESIAN_POINT('Ctrl Pts',(21.6439048771743,-7.60640395216359,
0.));
#187407=CARTESIAN_POINT('Ctrl Pts',(21.6307351973823,-7.604344141183,0.));
#187408=CARTESIAN_POINT('Ctrl Pts',(21.6177414005991,-7.60226917285432,
0.));
#187409=CARTESIAN_POINT('Ctrl Pts',(21.6049255358842,-7.60018029988238,
0.));
#187410=CARTESIAN_POINT('Ctrl Pts',(21.5922897024466,-7.59807880846193,
0.));
#187411=CARTESIAN_POINT('Ctrl Pts',(21.5798360518978,-7.59596601973589,
0.));
#187412=CARTESIAN_POINT('Ctrl Pts',(21.5675667904728,-7.5938432912493,0.));
#187413=CARTESIAN_POINT('Ctrl Pts',(21.5554841813465,-7.59171201844793,
0.));
#187414=CARTESIAN_POINT('Ctrl Pts',(21.5435905470113,-7.58957363620026,
0.));
#187415=CARTESIAN_POINT('Ctrl Pts',(21.5318882716735,-7.58742962034834,
0.));
#187416=CARTESIAN_POINT('Ctrl Pts',(21.5203798035294,-7.58528148919114,
0.));
#187417=CARTESIAN_POINT('Ctrl Pts',(21.5090676573866,-7.58313080519159,
0.));
#187418=CARTESIAN_POINT('Ctrl Pts',(21.4979544192739,-7.5809791779073,0.));
#187419=CARTESIAN_POINT('Ctrl Pts',(21.4870427508193,-7.57882826679131,
0.));
#187420=CARTESIAN_POINT('Ctrl Pts',(21.4763353936766,-7.57667978403003,
0.));
#187421=CARTESIAN_POINT('Ctrl Pts',(21.4658351740135,-7.57453549743435,
0.));
#187422=CARTESIAN_POINT('Ctrl Pts',(21.4555450053147,-7.57239723223521,
0.));
#187423=CARTESIAN_POINT('Ctrl Pts',(21.445467890751,-7.5702668726117,0.));
#187424=CARTESIAN_POINT('Ctrl Pts',(21.435606926151,-7.56814636360842,0.));
#187425=CARTESIAN_POINT('Ctrl Pts',(21.4259653015732,-7.56603771218706,
0.));
#187426=CARTESIAN_POINT('Ctrl Pts',(21.4165463106252,-7.56394299313683,
0.));
#187427=CARTESIAN_POINT('Ctrl Pts',(21.4073533630364,-7.56186435703622,
0.));
#187428=CARTESIAN_POINT('Ctrl Pts',(21.3983899952988,-7.55980403700615,
0.));
#187429=CARTESIAN_POINT('Ctrl Pts',(21.3896598842119,-7.55776435731422,
0.));
#187430=CARTESIAN_POINT('Ctrl Pts',(21.3811668478933,-7.55574773403508,
0.));
#187431=CARTESIAN_POINT('Ctrl Pts',(21.3729148390244,-7.55375667080032,
0.));
#187432=CARTESIAN_POINT('Ctrl Pts',(21.3649079431864,-7.55179375777442,
0.));
#187433=CARTESIAN_POINT('Ctrl Pts',(21.3571503685853,-7.54986166521307,
0.));
#187434=CARTESIAN_POINT('Ctrl Pts',(21.349646476153,-7.54796316246327,0.));
#187435=CARTESIAN_POINT('Ctrl Pts',(21.3424008295038,-7.54610114948351,
0.));
#187436=CARTESIAN_POINT('Ctrl Pts',(21.3354182340149,-7.54427868151269,
0.));
#187437=CARTESIAN_POINT('Ctrl Pts',(21.328703791771,-7.54249900377032,0.));
#187438=CARTESIAN_POINT('Ctrl Pts',(21.3222628524165,-7.5407655203828,0.));
#187439=CARTESIAN_POINT('Ctrl Pts',(21.3161009456256,-7.53908175169899,
0.));
#187440=CARTESIAN_POINT('Ctrl Pts',(21.3102237167729,-7.5374512936462,0.));
#187441=CARTESIAN_POINT('Ctrl Pts',(21.3046368712156,-7.53587778251743,
0.));
#187442=CARTESIAN_POINT('Ctrl Pts',(21.2993464250717,-7.53436505309949,
0.));
#187443=CARTESIAN_POINT('Ctrl Pts',(21.2943588989331,-7.53291726078527,
0.));
#187444=CARTESIAN_POINT('Ctrl Pts',(21.2896816163843,-7.53153906987847,
0.));
#187445=CARTESIAN_POINT('Ctrl Pts',(21.2853226580658,-7.53023562438221,
0.));
#187446=CARTESIAN_POINT('Ctrl Pts',(21.2812902781143,-7.52901217930407,
0.));
#187447=CARTESIAN_POINT('Ctrl Pts',(21.2775925269651,-7.52787386225344,
0.));
#187448=CARTESIAN_POINT('Ctrl Pts',(21.2742366113578,-7.52682526918561,
0.));
#187449=CARTESIAN_POINT('Ctrl Pts',(21.2712301573465,-7.52587126095544,
0.));
#187450=CARTESIAN_POINT('Ctrl Pts',(21.2685823838672,-7.52501770333522,
0.));
#187451=CARTESIAN_POINT('Ctrl Pts',(21.266305915706,-7.52427261074264,0.));
#187452=CARTESIAN_POINT('Ctrl Pts',(21.2644161259965,-7.52364573027521,
0.));
#187453=CARTESIAN_POINT('Ctrl Pts',(21.262927782038,-7.52314642316203,0.));
#187454=CARTESIAN_POINT('Ctrl Pts',(21.261852128355,-7.52278182242728,0.));
#187455=CARTESIAN_POINT('Ctrl Pts',(21.2613260540651,-7.52260064231736,
0.));
#187456=CARTESIAN_POINT('Ctrl Pts',(21.261120447486,-7.52252744144958,0.));
#187457=CARTESIAN_POINT('Ctrl Pts',(21.2610673466883,-7.52250649703992,
0.));
#187458=CARTESIAN_POINT('Ctrl Pts',(21.2610617890679,-7.52250298901266,
0.));
#187459=CARTESIAN_POINT('',(24.9347862158358,-7.36589684767345,0.));
#187460=CARTESIAN_POINT('Ctrl Pts',(20.353053841303,-9.71462809124917,0.));
#187461=CARTESIAN_POINT('Ctrl Pts',(20.353053841303,-9.71462809124917,12.));
#187462=CARTESIAN_POINT('Ctrl Pts',(20.353060251684,-9.71462954053074,0.));
#187463=CARTESIAN_POINT('Ctrl Pts',(20.353060251684,-9.71462954053074,12.));
#187464=CARTESIAN_POINT('Ctrl Pts',(20.3531126095522,-9.71465227853122,
0.));
#187465=CARTESIAN_POINT('Ctrl Pts',(20.3531126095522,-9.71465227853122,
12.));
#187466=CARTESIAN_POINT('Ctrl Pts',(20.3533097561886,-9.71474590350792,
0.));
#187467=CARTESIAN_POINT('Ctrl Pts',(20.3533097561886,-9.71474590350792,
12.));
#187468=CARTESIAN_POINT('Ctrl Pts',(20.3538098605706,-9.71498978052101,
0.));
#187469=CARTESIAN_POINT('Ctrl Pts',(20.3538098605706,-9.71498978052101,
12.));
#187470=CARTESIAN_POINT('Ctrl Pts',(20.3548282742361,-9.71549257088175,
0.));
#187471=CARTESIAN_POINT('Ctrl Pts',(20.3548282742361,-9.71549257088175,
12.));
#187472=CARTESIAN_POINT('Ctrl Pts',(20.3562337557875,-9.71619192554147,
0.));
#187473=CARTESIAN_POINT('Ctrl Pts',(20.3562337557875,-9.71619192554147,
12.));
#187474=CARTESIAN_POINT('Ctrl Pts',(20.3580133103357,-9.71708493723062,
0.));
#187475=CARTESIAN_POINT('Ctrl Pts',(20.3580133103357,-9.71708493723062,
12.));
#187476=CARTESIAN_POINT('Ctrl Pts',(20.3601498764344,-9.71816778327999,
0.));
#187477=CARTESIAN_POINT('Ctrl Pts',(20.3601498764344,-9.71816778327999,
12.));
#187478=CARTESIAN_POINT('Ctrl Pts',(20.362625691398,-9.71943648548115,0.));
#187479=CARTESIAN_POINT('Ctrl Pts',(20.362625691398,-9.71943648548115,12.));
#187480=CARTESIAN_POINT('Ctrl Pts',(20.3654261611055,-9.72088778381102,
0.));
#187481=CARTESIAN_POINT('Ctrl Pts',(20.3654261611055,-9.72088778381102,
12.));
#187482=CARTESIAN_POINT('Ctrl Pts',(20.3685406190576,-9.72251930722504,
0.));
#187483=CARTESIAN_POINT('Ctrl Pts',(20.3685406190576,-9.72251930722504,
12.));
#187484=CARTESIAN_POINT('Ctrl Pts',(20.371960235676,-9.72432910043193,0.));
#187485=CARTESIAN_POINT('Ctrl Pts',(20.371960235676,-9.72432910043193,12.));
#187486=CARTESIAN_POINT('Ctrl Pts',(20.3756766651952,-9.72631531732871,
0.));
#187487=CARTESIAN_POINT('Ctrl Pts',(20.3756766651952,-9.72631531732871,
12.));
#187488=CARTESIAN_POINT('Ctrl Pts',(20.3796805893304,-9.72847589116533,
0.));
#187489=CARTESIAN_POINT('Ctrl Pts',(20.3796805893304,-9.72847589116533,
12.));
#187490=CARTESIAN_POINT('Ctrl Pts',(20.3839624556742,-9.73080870123726,
0.));
#187491=CARTESIAN_POINT('Ctrl Pts',(20.3839624556742,-9.73080870123726,
12.));
#187492=CARTESIAN_POINT('Ctrl Pts',(20.3885129129912,-9.73331167102812,
0.));
#187493=CARTESIAN_POINT('Ctrl Pts',(20.3885129129912,-9.73331167102812,
12.));
#187494=CARTESIAN_POINT('Ctrl Pts',(20.3933234845646,-9.7359829201425,0.));
#187495=CARTESIAN_POINT('Ctrl Pts',(20.3933234845646,-9.7359829201425,12.));
#187496=CARTESIAN_POINT('Ctrl Pts',(20.3983866213331,-9.73882077613206,
0.));
#187497=CARTESIAN_POINT('Ctrl Pts',(20.3983866213331,-9.73882077613206,
12.));
#187498=CARTESIAN_POINT('Ctrl Pts',(20.4036953576549,-9.74182369656273,
0.));
#187499=CARTESIAN_POINT('Ctrl Pts',(20.4036953576549,-9.74182369656273,
12.));
#187500=CARTESIAN_POINT('Ctrl Pts',(20.4092430879861,-9.74499021838537,
0.));
#187501=CARTESIAN_POINT('Ctrl Pts',(20.4092430879861,-9.74499021838537,
12.));
#187502=CARTESIAN_POINT('Ctrl Pts',(20.4150232777393,-9.74831889242175,
0.));
#187503=CARTESIAN_POINT('Ctrl Pts',(20.4150232777393,-9.74831889242175,
12.));
#187504=CARTESIAN_POINT('Ctrl Pts',(20.4210295275818,-9.75180829786433,
0.));
#187505=CARTESIAN_POINT('Ctrl Pts',(20.4210295275818,-9.75180829786433,
12.));
#187506=CARTESIAN_POINT('Ctrl Pts',(20.4272556476629,-9.75545705902416,
0.));
#187507=CARTESIAN_POINT('Ctrl Pts',(20.4272556476629,-9.75545705902416,
12.));
#187508=CARTESIAN_POINT('Ctrl Pts',(20.4336957355474,-9.7592638628993,0.));
#187509=CARTESIAN_POINT('Ctrl Pts',(20.4336957355474,-9.7592638628993,12.));
#187510=CARTESIAN_POINT('Ctrl Pts',(20.4403442329401,-9.76322747195502,
0.));
#187511=CARTESIAN_POINT('Ctrl Pts',(20.4403442329401,-9.76322747195502,
12.));
#187512=CARTESIAN_POINT('Ctrl Pts',(20.447195862298,-9.76734670980897,0.));
#187513=CARTESIAN_POINT('Ctrl Pts',(20.447195862298,-9.76734670980897,12.));
#187514=CARTESIAN_POINT('Ctrl Pts',(20.4542455817527,-9.7716204510407,0.));
#187515=CARTESIAN_POINT('Ctrl Pts',(20.4542455817527,-9.7716204510407,12.));
#187516=CARTESIAN_POINT('Ctrl Pts',(20.4614885274973,-9.77604760815523,
0.));
#187517=CARTESIAN_POINT('Ctrl Pts',(20.4614885274973,-9.77604760815523,
12.));
#187518=CARTESIAN_POINT('Ctrl Pts',(20.4689199790668,-9.78062712373313,
0.));
#187519=CARTESIAN_POINT('Ctrl Pts',(20.4689199790668,-9.78062712373313,
12.));
#187520=CARTESIAN_POINT('Ctrl Pts',(20.4765353711585,-9.78535797314162,
0.));
#187521=CARTESIAN_POINT('Ctrl Pts',(20.4765353711585,-9.78535797314162,
12.));
#187522=CARTESIAN_POINT('Ctrl Pts',(20.4843302955329,-9.7902391649866,0.));
#187523=CARTESIAN_POINT('Ctrl Pts',(20.4843302955329,-9.7902391649866,12.));
#187524=CARTESIAN_POINT('Ctrl Pts',(20.4923005087945,-9.79526974288344,
0.));
#187525=CARTESIAN_POINT('Ctrl Pts',(20.4923005087945,-9.79526974288344,
12.));
#187526=CARTESIAN_POINT('Ctrl Pts',(20.500441931211,-9.80044878520968,0.));
#187527=CARTESIAN_POINT('Ctrl Pts',(20.500441931211,-9.80044878520968,12.));
#187528=CARTESIAN_POINT('Ctrl Pts',(20.5087506310507,-9.80577540161103,
0.));
#187529=CARTESIAN_POINT('Ctrl Pts',(20.5087506310507,-9.80577540161103,
12.));
#187530=CARTESIAN_POINT('Ctrl Pts',(20.5172228122839,-9.81124873025278,
0.));
#187531=CARTESIAN_POINT('Ctrl Pts',(20.5172228122839,-9.81124873025278,
12.));
#187532=CARTESIAN_POINT('Ctrl Pts',(20.5258548000625,-9.81686793455918,
0.));
#187533=CARTESIAN_POINT('Ctrl Pts',(20.5258548000625,-9.81686793455918,
12.));
#187534=CARTESIAN_POINT('Ctrl Pts',(20.534643029951,-9.82263220080328,0.));
#187535=CARTESIAN_POINT('Ctrl Pts',(20.534643029951,-9.82263220080328,12.));
#187536=CARTESIAN_POINT('Ctrl Pts',(20.5435840460717,-9.82854073773858,
0.));
#187537=CARTESIAN_POINT('Ctrl Pts',(20.5435840460717,-9.82854073773858,
12.));
#187538=CARTESIAN_POINT('Ctrl Pts',(20.5526744976461,-9.83459277585321,
0.));
#187539=CARTESIAN_POINT('Ctrl Pts',(20.5526744976461,-9.83459277585321,
12.));
#187540=CARTESIAN_POINT('Ctrl Pts',(20.5619111362406,-9.84078756677589,
0.));
#187541=CARTESIAN_POINT('Ctrl Pts',(20.5619111362406,-9.84078756677589,
12.));
#187542=CARTESIAN_POINT('Ctrl Pts',(20.5712908125145,-9.84712438256308,
0.));
#187543=CARTESIAN_POINT('Ctrl Pts',(20.5712908125145,-9.84712438256308,
12.));
#187544=CARTESIAN_POINT('Ctrl Pts',(20.580810471002,-9.85360251457004,0.));
#187545=CARTESIAN_POINT('Ctrl Pts',(20.580810471002,-9.85360251457004,12.));
#187546=CARTESIAN_POINT('Ctrl Pts',(20.5904671449754,-9.8602212723275,0.));
#187547=CARTESIAN_POINT('Ctrl Pts',(20.5904671449754,-9.8602212723275,12.));
#187548=CARTESIAN_POINT('Ctrl Pts',(20.6002579513696,-9.86697998242612,
0.));
#187549=CARTESIAN_POINT('Ctrl Pts',(20.6002579513696,-9.86697998242612,
12.));
#187550=CARTESIAN_POINT('Ctrl Pts',(20.6101800854491,-9.87387798732944,
0.));
#187551=CARTESIAN_POINT('Ctrl Pts',(20.6101800854491,-9.87387798732944,
12.));
#187552=CARTESIAN_POINT('Ctrl Pts',(20.6202308177472,-9.88091464472669,
0.));
#187553=CARTESIAN_POINT('Ctrl Pts',(20.6202308177472,-9.88091464472669,
12.));
#187554=CARTESIAN_POINT('Ctrl Pts',(20.6304074914086,-9.88808932697305,
0.));
#187555=CARTESIAN_POINT('Ctrl Pts',(20.6304074914086,-9.88808932697305,
12.));
#187556=CARTESIAN_POINT('Ctrl Pts',(20.6407075193977,-9.89540142049124,
0.));
#187557=CARTESIAN_POINT('Ctrl Pts',(20.6407075193977,-9.89540142049124,
12.));
#187558=CARTESIAN_POINT('Ctrl Pts',(20.6511283817415,-9.90285032516696,
0.));
#187559=CARTESIAN_POINT('Ctrl Pts',(20.6511283817415,-9.90285032516696,
12.));
#187560=CARTESIAN_POINT('Ctrl Pts',(20.6616676228315,-9.91043545377005,
0.));
#187561=CARTESIAN_POINT('Ctrl Pts',(20.6616676228315,-9.91043545377005,
12.));
#187562=CARTESIAN_POINT('Ctrl Pts',(20.6723228488261,-9.91815623141285,
0.));
#187563=CARTESIAN_POINT('Ctrl Pts',(20.6723228488261,-9.91815623141285,
12.));
#187564=CARTESIAN_POINT('Ctrl Pts',(20.6830917250255,-9.92601209498751,
0.));
#187565=CARTESIAN_POINT('Ctrl Pts',(20.6830917250255,-9.92601209498751,
12.));
#187566=CARTESIAN_POINT('Ctrl Pts',(20.6939719732485,-9.93400249259737,
0.));
#187567=CARTESIAN_POINT('Ctrl Pts',(20.6939719732485,-9.93400249259737,
12.));
#187568=CARTESIAN_POINT('Ctrl Pts',(20.7049613692237,-9.94212688298251,
0.));
#187569=CARTESIAN_POINT('Ctrl Pts',(20.7049613692237,-9.94212688298251,
12.));
#187570=CARTESIAN_POINT('Ctrl Pts',(20.716057740758,-9.95038473514962,0.));
#187571=CARTESIAN_POINT('Ctrl Pts',(20.716057740758,-9.95038473514962,12.));
#187572=CARTESIAN_POINT('Ctrl Pts',(20.7272589658752,-9.95877552798403,
0.));
#187573=CARTESIAN_POINT('Ctrl Pts',(20.7272589658752,-9.95877552798403,
12.));
#187574=CARTESIAN_POINT('Ctrl Pts',(20.7385629709795,-9.96729874986199,
0.));
#187575=CARTESIAN_POINT('Ctrl Pts',(20.7385629709795,-9.96729874986199,
12.));
#187576=CARTESIAN_POINT('Ctrl Pts',(20.7499677289625,-9.97595389823461,
0.));
#187577=CARTESIAN_POINT('Ctrl Pts',(20.7499677289625,-9.97595389823461,
12.));
#187578=CARTESIAN_POINT('Ctrl Pts',(20.7614712574989,-9.98474047926846,
0.));
#187579=CARTESIAN_POINT('Ctrl Pts',(20.7614712574989,-9.98474047926846,
12.));
#187580=CARTESIAN_POINT('Ctrl Pts',(20.7730716175417,-9.99365800754638,
0.));
#187581=CARTESIAN_POINT('Ctrl Pts',(20.7730716175417,-9.99365800754638,
12.));
#187582=CARTESIAN_POINT('Ctrl Pts',(20.7847669117568,-10.0027060057389,
0.));
#187583=CARTESIAN_POINT('Ctrl Pts',(20.7847669117568,-10.0027060057389,
12.));
#187584=CARTESIAN_POINT('Ctrl Pts',(20.7965552829907,-10.0118840042786,
0.));
#187585=CARTESIAN_POINT('Ctrl Pts',(20.7965552829907,-10.0118840042786,
12.));
#187586=CARTESIAN_POINT('Ctrl Pts',(20.8084349126885,-10.0211915410095,
0.));
#187587=CARTESIAN_POINT('Ctrl Pts',(20.8084349126885,-10.0211915410095,
12.));
#187588=CARTESIAN_POINT('Ctrl Pts',(20.8204040196599,-10.0306281609435,
0.));
#187589=CARTESIAN_POINT('Ctrl Pts',(20.8204040196599,-10.0306281609435,
12.));
#187590=CARTESIAN_POINT('Ctrl Pts',(20.8324608588906,-10.0401934160234,
0.));
#187591=CARTESIAN_POINT('Ctrl Pts',(20.8324608588906,-10.0401934160234,
12.));
#187592=CARTESIAN_POINT('Ctrl Pts',(20.8446037203402,-10.0498868648733,
0.));
#187593=CARTESIAN_POINT('Ctrl Pts',(20.8446037203402,-10.0498868648733,
12.));
#187594=CARTESIAN_POINT('Ctrl Pts',(20.856830927732,-10.0597080725375,0.));
#187595=CARTESIAN_POINT('Ctrl Pts',(20.856830927732,-10.0597080725375,12.));
#187596=CARTESIAN_POINT('Ctrl Pts',(20.8691408373705,-10.0696566102219,
0.));
#187597=CARTESIAN_POINT('Ctrl Pts',(20.8691408373705,-10.0696566102219,
12.));
#187598=CARTESIAN_POINT('Ctrl Pts',(20.8815318371844,-10.0797320551154,
0.));
#187599=CARTESIAN_POINT('Ctrl Pts',(20.8815318371844,-10.0797320551154,
12.));
#187600=CARTESIAN_POINT('Ctrl Pts',(20.8940023457371,-10.0899339901916,
0.));
#187601=CARTESIAN_POINT('Ctrl Pts',(20.8940023457371,-10.0899339901916,
12.));
#187602=CARTESIAN_POINT('Ctrl Pts',(20.9065508112556,-10.1002620040076,
0.));
#187603=CARTESIAN_POINT('Ctrl Pts',(20.9065508112556,-10.1002620040076,
12.));
#187604=CARTESIAN_POINT('Ctrl Pts',(20.9191757106266,-10.1107156904836,
0.));
#187605=CARTESIAN_POINT('Ctrl Pts',(20.9191757106266,-10.1107156904836,
12.));
#187606=CARTESIAN_POINT('Ctrl Pts',(20.931875548473,-10.1212946487057,0.));
#187607=CARTESIAN_POINT('Ctrl Pts',(20.931875548473,-10.1212946487057,12.));
#187608=CARTESIAN_POINT('Ctrl Pts',(20.944648856393,-10.1319984827909,0.));
#187609=CARTESIAN_POINT('Ctrl Pts',(20.944648856393,-10.1319984827909,12.));
#187610=CARTESIAN_POINT('Ctrl Pts',(20.9574941921591,-10.1428268017257,
0.));
#187611=CARTESIAN_POINT('Ctrl Pts',(20.9574941921591,-10.1428268017257,
12.));
#187612=CARTESIAN_POINT('Ctrl Pts',(20.970410138937,-10.1537792192065,0.));
#187613=CARTESIAN_POINT('Ctrl Pts',(20.970410138937,-10.1537792192065,12.));
#187614=CARTESIAN_POINT('Ctrl Pts',(20.9833953044736,-10.1648553534567,
0.));
#187615=CARTESIAN_POINT('Ctrl Pts',(20.9833953044736,-10.1648553534567,
12.));
#187616=CARTESIAN_POINT('Ctrl Pts',(20.9964483203685,-10.1760548270765,
0.));
#187617=CARTESIAN_POINT('Ctrl Pts',(20.9964483203685,-10.1760548270765,
12.));
#187618=CARTESIAN_POINT('Ctrl Pts',(21.0095678414486,-10.1873772669358,
0.));
#187619=CARTESIAN_POINT('Ctrl Pts',(21.0095678414486,-10.1873772669358,
12.));
#187620=CARTESIAN_POINT('Ctrl Pts',(21.0227525451107,-10.1988223040425,
0.));
#187621=CARTESIAN_POINT('Ctrl Pts',(21.0227525451107,-10.1988223040425,
12.));
#187622=CARTESIAN_POINT('Ctrl Pts',(21.0360011306814,-10.2103895734124,
0.));
#187623=CARTESIAN_POINT('Ctrl Pts',(21.0360011306814,-10.2103895734124,
12.));
#187624=CARTESIAN_POINT('Ctrl Pts',(21.0493123187483,-10.2220787139157,
0.));
#187625=CARTESIAN_POINT('Ctrl Pts',(21.0493123187483,-10.2220787139157,
12.));
#187626=CARTESIAN_POINT('Ctrl Pts',(21.0626848505665,-10.233889368157,0.));
#187627=CARTESIAN_POINT('Ctrl Pts',(21.0626848505665,-10.233889368157,12.));
#187628=CARTESIAN_POINT('Ctrl Pts',(21.0761174875448,-10.2458211823915,
0.));
#187629=CARTESIAN_POINT('Ctrl Pts',(21.0761174875448,-10.2458211823915,
12.));
#187630=CARTESIAN_POINT('Ctrl Pts',(21.0896090107066,-10.2578738064183,
0.));
#187631=CARTESIAN_POINT('Ctrl Pts',(21.0896090107066,-10.2578738064183,
12.));
#187632=CARTESIAN_POINT('Ctrl Pts',(21.1031582201625,-10.2700468934743,
0.));
#187633=CARTESIAN_POINT('Ctrl Pts',(21.1031582201625,-10.2700468934743,
12.));
#187634=CARTESIAN_POINT('Ctrl Pts',(21.1167639345623,-10.2823401001067,
0.));
#187635=CARTESIAN_POINT('Ctrl Pts',(21.1167639345623,-10.2823401001067,
12.));
#187636=CARTESIAN_POINT('Ctrl Pts',(21.130424990599,-10.2947530860714,0.));
#187637=CARTESIAN_POINT('Ctrl Pts',(21.130424990599,-10.2947530860714,12.));
#187638=CARTESIAN_POINT('Ctrl Pts',(21.1441402425831,-10.307285514268,0.));
#187639=CARTESIAN_POINT('Ctrl Pts',(21.1441402425831,-10.307285514268,12.));
#187640=CARTESIAN_POINT('Ctrl Pts',(21.1579085619959,-10.3199370506541,
0.));
#187641=CARTESIAN_POINT('Ctrl Pts',(21.1579085619959,-10.3199370506541,
12.));
#187642=CARTESIAN_POINT('Ctrl Pts',(21.1717288370512,-10.3327073641574,
0.));
#187643=CARTESIAN_POINT('Ctrl Pts',(21.1717288370512,-10.3327073641574,
12.));
#187644=CARTESIAN_POINT('Ctrl Pts',(21.1855999722427,-10.3455961265706,
0.));
#187645=CARTESIAN_POINT('Ctrl Pts',(21.1855999722427,-10.3455961265706,
12.));
#187646=CARTESIAN_POINT('Ctrl Pts',(21.1995208879205,-10.3586030124595,
0.));
#187647=CARTESIAN_POINT('Ctrl Pts',(21.1995208879205,-10.3586030124595,
12.));
#187648=CARTESIAN_POINT('Ctrl Pts',(21.2134905199359,-10.3717276991137,
0.));
#187649=CARTESIAN_POINT('Ctrl Pts',(21.2134905199359,-10.3717276991137,
12.));
#187650=CARTESIAN_POINT('Ctrl Pts',(21.2275078192708,-10.384969866479,0.));
#187651=CARTESIAN_POINT('Ctrl Pts',(21.2275078192708,-10.384969866479,12.));
#187652=CARTESIAN_POINT('Ctrl Pts',(21.2415717516713,-10.3983291970846,
0.));
#187653=CARTESIAN_POINT('Ctrl Pts',(21.2415717516713,-10.3983291970846,
12.));
#187654=CARTESIAN_POINT('Ctrl Pts',(21.2556812972741,-10.4118053759584,
0.));
#187655=CARTESIAN_POINT('Ctrl Pts',(21.2556812972741,-10.4118053759584,
12.));
#187656=CARTESIAN_POINT('Ctrl Pts',(21.2698354502391,-10.4253980905394,
0.));
#187657=CARTESIAN_POINT('Ctrl Pts',(21.2698354502391,-10.4253980905394,
12.));
#187658=CARTESIAN_POINT('Ctrl Pts',(21.2840332184471,-10.4391070306385,
0.));
#187659=CARTESIAN_POINT('Ctrl Pts',(21.2840332184471,-10.4391070306385,
12.));
#187660=CARTESIAN_POINT('Ctrl Pts',(21.2982736231924,-10.452931888387,0.));
#187661=CARTESIAN_POINT('Ctrl Pts',(21.2982736231924,-10.452931888387,12.));
#187662=CARTESIAN_POINT('Ctrl Pts',(21.312555698873,-10.4668723581768,0.));
#187663=CARTESIAN_POINT('Ctrl Pts',(21.312555698873,-10.4668723581768,12.));
#187664=CARTESIAN_POINT('Ctrl Pts',(21.3268784926823,-10.4809281365933,
0.));
#187665=CARTESIAN_POINT('Ctrl Pts',(21.3268784926823,-10.4809281365933,
12.));
#187666=CARTESIAN_POINT('Ctrl Pts',(21.3412410642912,-10.4950989223341,
0.));
#187667=CARTESIAN_POINT('Ctrl Pts',(21.3412410642912,-10.4950989223341,
12.));
#187668=CARTESIAN_POINT('Ctrl Pts',(21.3556424855822,-10.509384416169,0.));
#187669=CARTESIAN_POINT('Ctrl Pts',(21.3556424855822,-10.509384416169,12.));
#187670=CARTESIAN_POINT('Ctrl Pts',(21.3700818403942,-10.523784320906,0.));
#187671=CARTESIAN_POINT('Ctrl Pts',(21.3700818403942,-10.523784320906,12.));
#187672=CARTESIAN_POINT('Ctrl Pts',(21.3845582242604,-10.5382983413422,
0.));
#187673=CARTESIAN_POINT('Ctrl Pts',(21.3845582242604,-10.5382983413422,
12.));
#187674=CARTESIAN_POINT('Ctrl Pts',(21.3990707441495,-10.5529261842107,
0.));
#187675=CARTESIAN_POINT('Ctrl Pts',(21.3990707441495,-10.5529261842107,
12.));
#187676=CARTESIAN_POINT('Ctrl Pts',(21.4136185181974,-10.5676675581106,
0.));
#187677=CARTESIAN_POINT('Ctrl Pts',(21.4136185181974,-10.5676675581106,
12.));
#187678=CARTESIAN_POINT('Ctrl Pts',(21.4282006754624,-10.582522173457,0.));
#187679=CARTESIAN_POINT('Ctrl Pts',(21.4282006754624,-10.582522173457,12.));
#187680=CARTESIAN_POINT('Ctrl Pts',(21.4428163557137,-10.597489742462,0.));
#187681=CARTESIAN_POINT('Ctrl Pts',(21.4428163557137,-10.597489742462,12.));
#187682=CARTESIAN_POINT('Ctrl Pts',(21.4574647092093,-10.612569979096,0.));
#187683=CARTESIAN_POINT('Ctrl Pts',(21.4574647092093,-10.612569979096,12.));
#187684=CARTESIAN_POINT('Ctrl Pts',(21.4721448964766,-10.6277625990457,
0.));
#187685=CARTESIAN_POINT('Ctrl Pts',(21.4721448964766,-10.6277625990457,
12.));
#187686=CARTESIAN_POINT('Ctrl Pts',(21.4868560880893,-10.6430673196609,
0.));
#187687=CARTESIAN_POINT('Ctrl Pts',(21.4868560880893,-10.6430673196609,
12.));
#187688=CARTESIAN_POINT('Ctrl Pts',(21.5015974644454,-10.6584838598941,
0.));
#187689=CARTESIAN_POINT('Ctrl Pts',(21.5015974644454,-10.6584838598941,
12.));
#187690=CARTESIAN_POINT('Ctrl Pts',(21.5163682155805,-10.6740119402835,
0.));
#187691=CARTESIAN_POINT('Ctrl Pts',(21.5163682155805,-10.6740119402835,
12.));
#187692=CARTESIAN_POINT('Ctrl Pts',(21.531167540981,-10.689651282929,0.));
#187693=CARTESIAN_POINT('Ctrl Pts',(21.531167540981,-10.689651282929,12.));
#187694=CARTESIAN_POINT('Ctrl Pts',(21.5459946493955,-10.7054016114571,
0.));
#187695=CARTESIAN_POINT('Ctrl Pts',(21.5459946493955,-10.7054016114571,
12.));
#187696=CARTESIAN_POINT('Ctrl Pts',(21.5608487586467,-10.7212626509816,
0.));
#187697=CARTESIAN_POINT('Ctrl Pts',(21.5608487586467,-10.7212626509816,
12.));
#187698=CARTESIAN_POINT('Ctrl Pts',(21.5757290954372,-10.7372341280468,
0.));
#187699=CARTESIAN_POINT('Ctrl Pts',(21.5757290954372,-10.7372341280468,
12.));
#187700=CARTESIAN_POINT('Ctrl Pts',(21.5906348951745,-10.7533157705943,
0.));
#187701=CARTESIAN_POINT('Ctrl Pts',(21.5906348951745,-10.7533157705943,
12.));
#187702=CARTESIAN_POINT('Ctrl Pts',(21.6055654018179,-10.7695073079554,
0.));
#187703=CARTESIAN_POINT('Ctrl Pts',(21.6055654018179,-10.7695073079554,
12.));
#187704=CARTESIAN_POINT('Ctrl Pts',(21.6205198677176,-10.7858084708262,
0.));
#187705=CARTESIAN_POINT('Ctrl Pts',(21.6205198677176,-10.7858084708262,
12.));
#187706=CARTESIAN_POINT('Ctrl Pts',(21.6354975534557,-10.802218991237,0.));
#187707=CARTESIAN_POINT('Ctrl Pts',(21.6354975534557,-10.802218991237,12.));
#187708=CARTESIAN_POINT('Ctrl Pts',(21.6504977276864,-10.8187386025135,
0.));
#187709=CARTESIAN_POINT('Ctrl Pts',(21.6504977276864,-10.8187386025135,
12.));
#187710=CARTESIAN_POINT('Ctrl Pts',(21.6655196669727,-10.835367039227,0.));
#187711=CARTESIAN_POINT('Ctrl Pts',(21.6655196669727,-10.835367039227,12.));
#187712=CARTESIAN_POINT('Ctrl Pts',(21.6805626556461,-10.8521040371832,
0.));
#187713=CARTESIAN_POINT('Ctrl Pts',(21.6805626556461,-10.8521040371832,
12.));
#187714=CARTESIAN_POINT('Ctrl Pts',(21.6956259856667,-10.8689493334093,
0.));
#187715=CARTESIAN_POINT('Ctrl Pts',(21.6956259856667,-10.8689493334093,
12.));
#187716=CARTESIAN_POINT('Ctrl Pts',(21.7107089564822,-10.8859026661292,
0.));
#187717=CARTESIAN_POINT('Ctrl Pts',(21.7107089564822,-10.8859026661292,
12.));
#187718=CARTESIAN_POINT('Ctrl Pts',(21.7258108748874,-10.9029637747341,
0.));
#187719=CARTESIAN_POINT('Ctrl Pts',(21.7258108748874,-10.9029637747341,
12.));
#187720=CARTESIAN_POINT('Ctrl Pts',(21.74093105488,-10.9201323997386,0.));
#187721=CARTESIAN_POINT('Ctrl Pts',(21.74093105488,-10.9201323997386,12.));
#187722=CARTESIAN_POINT('Ctrl Pts',(21.7560688175252,-10.9374082827446,
0.));
#187723=CARTESIAN_POINT('Ctrl Pts',(21.7560688175252,-10.9374082827446,
12.));
#187724=CARTESIAN_POINT('Ctrl Pts',(21.7712234908468,-10.9547911664457,
0.));
#187725=CARTESIAN_POINT('Ctrl Pts',(21.7712234908468,-10.9547911664457,
12.));
#187726=CARTESIAN_POINT('Ctrl Pts',(21.7863944097143,-10.9722807946157,
0.));
#187727=CARTESIAN_POINT('Ctrl Pts',(21.7863944097143,-10.9722807946157,
12.));
#187728=CARTESIAN_POINT('Ctrl Pts',(21.8015809157302,-10.9898769120913,
0.));
#187729=CARTESIAN_POINT('Ctrl Pts',(21.8015809157302,-10.9898769120913,
12.));
#187730=CARTESIAN_POINT('Ctrl Pts',(21.8167823571168,-11.0075792647477,
0.));
#187731=CARTESIAN_POINT('Ctrl Pts',(21.8167823571168,-11.0075792647477,
12.));
#187732=CARTESIAN_POINT('Ctrl Pts',(21.8319980886033,-11.0253875994598,
0.));
#187733=CARTESIAN_POINT('Ctrl Pts',(21.8319980886033,-11.0253875994598,
12.));
#187734=CARTESIAN_POINT('Ctrl Pts',(21.8472274713103,-11.0433016640808,
0.));
#187735=CARTESIAN_POINT('Ctrl Pts',(21.8472274713103,-11.0433016640808,
12.));
#187736=CARTESIAN_POINT('Ctrl Pts',(21.8624698726319,-11.0613212074364,
0.));
#187737=CARTESIAN_POINT('Ctrl Pts',(21.8624698726319,-11.0613212074364,
12.));
#187738=CARTESIAN_POINT('Ctrl Pts',(21.8777246661191,-11.0794459793058,
0.));
#187739=CARTESIAN_POINT('Ctrl Pts',(21.8777246661191,-11.0794459793058,
12.));
#187740=CARTESIAN_POINT('Ctrl Pts',(21.8929912313608,-11.0976757303944,
0.));
#187741=CARTESIAN_POINT('Ctrl Pts',(21.8929912313608,-11.0976757303944,
12.));
#187742=CARTESIAN_POINT('Ctrl Pts',(21.9082689538687,-11.1160102123024,
0.));
#187743=CARTESIAN_POINT('Ctrl Pts',(21.9082689538687,-11.1160102123024,
12.));
#187744=CARTESIAN_POINT('Ctrl Pts',(21.9235572249518,-11.134449177474,0.));
#187745=CARTESIAN_POINT('Ctrl Pts',(21.9235572249518,-11.134449177474,12.));
#187746=CARTESIAN_POINT('Ctrl Pts',(21.9388554416437,-11.1529923792002,
0.));
#187747=CARTESIAN_POINT('Ctrl Pts',(21.9388554416437,-11.1529923792002,
12.));
#187748=CARTESIAN_POINT('Ctrl Pts',(21.9541630066504,-11.1716395716375,
0.));
#187749=CARTESIAN_POINT('Ctrl Pts',(21.9541630066504,-11.1716395716375,
12.));
#187750=CARTESIAN_POINT('Ctrl Pts',(21.9694793282913,-11.190390509811,0.));
#187751=CARTESIAN_POINT('Ctrl Pts',(21.9694793282913,-11.190390509811,12.));
#187752=CARTESIAN_POINT('Ctrl Pts',(21.9848038204439,-11.2092449496125,
0.));
#187753=CARTESIAN_POINT('Ctrl Pts',(21.9848038204439,-11.2092449496125,
12.));
#187754=CARTESIAN_POINT('Ctrl Pts',(22.0001359024839,-11.2282026477897,
0.));
#187755=CARTESIAN_POINT('Ctrl Pts',(22.0001359024839,-11.2282026477897,
12.));
#187756=CARTESIAN_POINT('Ctrl Pts',(22.0154749992364,-11.2472633619276,
0.));
#187757=CARTESIAN_POINT('Ctrl Pts',(22.0154749992364,-11.2472633619276,
12.));
#187758=CARTESIAN_POINT('Ctrl Pts',(22.0308205408351,-11.2664268504207,
0.));
#187759=CARTESIAN_POINT('Ctrl Pts',(22.0308205408351,-11.2664268504207,
12.));
#187760=CARTESIAN_POINT('Ctrl Pts',(22.046171962566,-11.2856928724374,0.));
#187761=CARTESIAN_POINT('Ctrl Pts',(22.046171962566,-11.2856928724374,12.));
#187762=CARTESIAN_POINT('Ctrl Pts',(22.0615287047179,-11.3050611878771,
0.));
#187763=CARTESIAN_POINT('Ctrl Pts',(22.0615287047179,-11.3050611878771,
12.));
#187764=CARTESIAN_POINT('Ctrl Pts',(22.0768902124267,-11.3245315573168,
0.));
#187765=CARTESIAN_POINT('Ctrl Pts',(22.0768902124267,-11.3245315573168,
12.));
#187766=CARTESIAN_POINT('Ctrl Pts',(22.0922559355293,-11.3441037419553,
0.));
#187767=CARTESIAN_POINT('Ctrl Pts',(22.0922559355293,-11.3441037419553,
12.));
#187768=CARTESIAN_POINT('Ctrl Pts',(22.1076253283978,-11.3637775035367,
0.));
#187769=CARTESIAN_POINT('Ctrl Pts',(22.1076253283978,-11.3637775035367,
12.));
#187770=CARTESIAN_POINT('Ctrl Pts',(22.1229978500185,-11.3835526044256,
0.));
#187771=CARTESIAN_POINT('Ctrl Pts',(22.1229978500185,-11.3835526044256,
12.));
#187772=CARTESIAN_POINT('Ctrl Pts',(22.1383729640963,-11.4034288076909,
0.));
#187773=CARTESIAN_POINT('Ctrl Pts',(22.1383729640963,-11.4034288076909,
12.));
#187774=CARTESIAN_POINT('Ctrl Pts',(22.1537501391486,-11.4234058771742,
0.));
#187775=CARTESIAN_POINT('Ctrl Pts',(22.1537501391486,-11.4234058771742,
12.));
#187776=CARTESIAN_POINT('Ctrl Pts',(22.1691288486096,-11.443483577557,0.));
#187777=CARTESIAN_POINT('Ctrl Pts',(22.1691288486096,-11.443483577557,12.));
#187778=CARTESIAN_POINT('Ctrl Pts',(22.1845085709169,-11.463661674411,0.));
#187779=CARTESIAN_POINT('Ctrl Pts',(22.1845085709169,-11.463661674411,12.));
#187780=CARTESIAN_POINT('Ctrl Pts',(22.1998887896435,-11.4839399342589,
0.));
#187781=CARTESIAN_POINT('Ctrl Pts',(22.1998887896435,-11.4839399342589,
12.));
#187782=CARTESIAN_POINT('Ctrl Pts',(22.215268993102,-11.504318124424,0.));
#187783=CARTESIAN_POINT('Ctrl Pts',(22.215268993102,-11.504318124424,12.));
#187784=CARTESIAN_POINT('Ctrl Pts',(22.2306486738899,-11.5247960128476,
0.));
#187785=CARTESIAN_POINT('Ctrl Pts',(22.2306486738899,-11.5247960128476,
12.));
#187786=CARTESIAN_POINT('Ctrl Pts',(22.2460273284653,-11.545373367912,0.));
#187787=CARTESIAN_POINT('Ctrl Pts',(22.2460273284653,-11.545373367912,12.));
#187788=CARTESIAN_POINT('Ctrl Pts',(22.2614044566898,-11.5660499582403,
0.));
#187789=CARTESIAN_POINT('Ctrl Pts',(22.2614044566898,-11.5660499582403,
12.));
#187790=CARTESIAN_POINT('Ctrl Pts',(22.2767795614349,-11.5868255525189,
0.));
#187791=CARTESIAN_POINT('Ctrl Pts',(22.2767795614349,-11.5868255525189,
12.));
#187792=CARTESIAN_POINT('Ctrl Pts',(22.2921521480357,-11.6076999192359,
0.));
#187793=CARTESIAN_POINT('Ctrl Pts',(22.2921521480357,-11.6076999192359,
12.));
#187794=CARTESIAN_POINT('Ctrl Pts',(22.3075217249049,-11.6286728270011,
0.));
#187795=CARTESIAN_POINT('Ctrl Pts',(22.3075217249049,-11.6286728270011,
12.));
#187796=CARTESIAN_POINT('Ctrl Pts',(22.3228878043976,-11.6497440449858,
0.));
#187797=CARTESIAN_POINT('Ctrl Pts',(22.3228878043976,-11.6497440449858,
12.));
#187798=CARTESIAN_POINT('Ctrl Pts',(22.3382499035618,-11.6709133432986,
0.));
#187799=CARTESIAN_POINT('Ctrl Pts',(22.3382499035618,-11.6709133432986,
12.));
#187800=CARTESIAN_POINT('Ctrl Pts',(22.3536075450028,-11.6921804934056,
0.));
#187801=CARTESIAN_POINT('Ctrl Pts',(22.3536075450028,-11.6921804934056,
12.));
#187802=CARTESIAN_POINT('Ctrl Pts',(22.3689602575492,-11.7135452684532,
0.));
#187803=CARTESIAN_POINT('Ctrl Pts',(22.3689602575492,-11.7135452684532,
12.));
#187804=CARTESIAN_POINT('Ctrl Pts',(22.3843075773905,-11.7350074437961,
0.));
#187805=CARTESIAN_POINT('Ctrl Pts',(22.3843075773905,-11.7350074437961,
12.));
#187806=CARTESIAN_POINT('Ctrl Pts',(22.39964904692,-11.7565667964765,0.));
#187807=CARTESIAN_POINT('Ctrl Pts',(22.39964904692,-11.7565667964765,12.));
#187808=CARTESIAN_POINT('Ctrl Pts',(22.4149842125018,-11.7782231042041,
0.));
#187809=CARTESIAN_POINT('Ctrl Pts',(22.4149842125018,-11.7782231042041,
12.));
#187810=CARTESIAN_POINT('Ctrl Pts',(22.4303126226468,-11.7999761445175,
0.));
#187811=CARTESIAN_POINT('Ctrl Pts',(22.4303126226468,-11.7999761445175,
12.));
#187812=CARTESIAN_POINT('Ctrl Pts',(22.4456338258738,-11.8218256937889,
0.));
#187813=CARTESIAN_POINT('Ctrl Pts',(22.4456338258738,-11.8218256937889,
12.));
#187814=CARTESIAN_POINT('Ctrl Pts',(22.4609473690469,-11.8437715264487,
0.));
#187815=CARTESIAN_POINT('Ctrl Pts',(22.4609473690469,-11.8437715264487,
12.));
#187816=CARTESIAN_POINT('Ctrl Pts',(22.4762527946694,-11.8658134137018,
0.));
#187817=CARTESIAN_POINT('Ctrl Pts',(22.4762527946694,-11.8658134137018,
12.));
#187818=CARTESIAN_POINT('Ctrl Pts',(22.4915496418472,-11.8879511239941,
0.));
#187819=CARTESIAN_POINT('Ctrl Pts',(22.4915496418472,-11.8879511239941,
12.));
#187820=CARTESIAN_POINT('Ctrl Pts',(22.5068374513958,-11.9101844254555,
0.));
#187821=CARTESIAN_POINT('Ctrl Pts',(22.5068374513958,-11.9101844254555,
12.));
#187822=CARTESIAN_POINT('Ctrl Pts',(22.5221157697869,-11.9325130877801,
0.));
#187823=CARTESIAN_POINT('Ctrl Pts',(22.5221157697869,-11.9325130877801,
12.));
#187824=CARTESIAN_POINT('Ctrl Pts',(22.5373841537299,-11.9549368843996,
0.));
#187825=CARTESIAN_POINT('Ctrl Pts',(22.5373841537299,-11.9549368843996,
12.));
#187826=CARTESIAN_POINT('Ctrl Pts',(22.5526421741159,-11.9774555943496,
0.));
#187827=CARTESIAN_POINT('Ctrl Pts',(22.5526421741159,-11.9774555943496,
12.));
#187828=CARTESIAN_POINT('Ctrl Pts',(22.5678894211194,-12.0000690046697,
0.));
#187829=CARTESIAN_POINT('Ctrl Pts',(22.5678894211194,-12.0000690046697,
12.));
#187830=CARTESIAN_POINT('Ctrl Pts',(22.5831255061306,-12.0227769113132,
0.));
#187831=CARTESIAN_POINT('Ctrl Pts',(22.5831255061306,-12.0227769113132,
12.));
#187832=CARTESIAN_POINT('Ctrl Pts',(22.5983500505675,-12.0455791139135,
0.));
#187833=CARTESIAN_POINT('Ctrl Pts',(22.5983500505675,-12.0455791139135,
12.));
#187834=CARTESIAN_POINT('Ctrl Pts',(22.613562676493,-12.0684754113869,0.));
#187835=CARTESIAN_POINT('Ctrl Pts',(22.613562676493,-12.0684754113869,12.));
#187836=CARTESIAN_POINT('Ctrl Pts',(22.628762996708,-12.0914655972828,0.));
#187837=CARTESIAN_POINT('Ctrl Pts',(22.628762996708,-12.0914655972828,12.));
#187838=CARTESIAN_POINT('Ctrl Pts',(22.6439506046611,-12.1145494550384,
0.));
#187839=CARTESIAN_POINT('Ctrl Pts',(22.6439506046611,-12.1145494550384,
12.));
#187840=CARTESIAN_POINT('Ctrl Pts',(22.6591250653942,-12.1377267537141,
0.));
#187841=CARTESIAN_POINT('Ctrl Pts',(22.6591250653942,-12.1377267537141,
12.));
#187842=CARTESIAN_POINT('Ctrl Pts',(22.6742859034891,-12.1609972423089,
0.));
#187843=CARTESIAN_POINT('Ctrl Pts',(22.6742859034891,-12.1609972423089,
12.));
#187844=CARTESIAN_POINT('Ctrl Pts',(22.6894326204959,-12.1843606579246,
0.));
#187845=CARTESIAN_POINT('Ctrl Pts',(22.6894326204959,-12.1843606579246,
12.));
#187846=CARTESIAN_POINT('Ctrl Pts',(22.7045647168659,-12.2078167360267,
0.));
#187847=CARTESIAN_POINT('Ctrl Pts',(22.7045647168659,-12.2078167360267,
12.));
#187848=CARTESIAN_POINT('Ctrl Pts',(22.7196817119299,-12.2313652198047,
0.));
#187849=CARTESIAN_POINT('Ctrl Pts',(22.7196817119299,-12.2313652198047,
12.));
#187850=CARTESIAN_POINT('Ctrl Pts',(22.7347831655251,-12.2550058702389,
0.));
#187851=CARTESIAN_POINT('Ctrl Pts',(22.7347831655251,-12.2550058702389,
12.));
#187852=CARTESIAN_POINT('Ctrl Pts',(22.7498686970096,-12.2787384750747,
0.));
#187853=CARTESIAN_POINT('Ctrl Pts',(22.7498686970096,-12.2787384750747,
12.));
#187854=CARTESIAN_POINT('Ctrl Pts',(22.7649380101154,-12.3025628601812,
0.));
#187855=CARTESIAN_POINT('Ctrl Pts',(22.7649380101154,-12.3025628601812,
12.));
#187856=CARTESIAN_POINT('Ctrl Pts',(22.7799908974947,-12.3264788926108,
0.));
#187857=CARTESIAN_POINT('Ctrl Pts',(22.7799908974947,-12.3264788926108,
12.));
#187858=CARTESIAN_POINT('Ctrl Pts',(22.7950272216959,-12.3504864740361,
0.));
#187859=CARTESIAN_POINT('Ctrl Pts',(22.7950272216959,-12.3504864740361,
12.));
#187860=CARTESIAN_POINT('Ctrl Pts',(22.8100469022632,-12.3745855366772,
0.));
#187861=CARTESIAN_POINT('Ctrl Pts',(22.8100469022632,-12.3745855366772,
12.));
#187862=CARTESIAN_POINT('Ctrl Pts',(22.8220493007353,-12.393937937903,0.));
#187863=CARTESIAN_POINT('Ctrl Pts',(22.8220493007353,-12.393937937903,12.));
#187864=CARTESIAN_POINT('Ctrl Pts',(22.8310435872852,-12.4084933766366,
0.));
#187865=CARTESIAN_POINT('Ctrl Pts',(22.8310435872852,-12.4084933766366,
12.));
#187866=CARTESIAN_POINT('Ctrl Pts',(22.8370364396497,-12.4182152851867,
0.));
#187867=CARTESIAN_POINT('Ctrl Pts',(22.8370364396497,-12.4182152851867,
12.));
#187868=CARTESIAN_POINT('Ctrl Pts',(22.8400320311648,-12.4230808101438,
0.));
#187869=CARTESIAN_POINT('Ctrl Pts',(22.8400320311648,-12.4230808101438,
12.));
#187870=CARTESIAN_POINT('',(22.8400320311648,-12.4230808101438,0.));
#187871=CARTESIAN_POINT('Ctrl Pts',(20.353053841303,-9.71462809124917,0.));
#187872=CARTESIAN_POINT('Ctrl Pts',(20.353060251684,-9.71462954053074,0.));
#187873=CARTESIAN_POINT('Ctrl Pts',(20.3531126095522,-9.71465227853122,
0.));
#187874=CARTESIAN_POINT('Ctrl Pts',(20.3533097561886,-9.71474590350792,
0.));
#187875=CARTESIAN_POINT('Ctrl Pts',(20.3538098605706,-9.71498978052101,
0.));
#187876=CARTESIAN_POINT('Ctrl Pts',(20.3548282742361,-9.71549257088175,
0.));
#187877=CARTESIAN_POINT('Ctrl Pts',(20.3562337557875,-9.71619192554147,
0.));
#187878=CARTESIAN_POINT('Ctrl Pts',(20.3580133103357,-9.71708493723062,
0.));
#187879=CARTESIAN_POINT('Ctrl Pts',(20.3601498764344,-9.71816778327999,
0.));
#187880=CARTESIAN_POINT('Ctrl Pts',(20.362625691398,-9.71943648548115,0.));
#187881=CARTESIAN_POINT('Ctrl Pts',(20.3654261611055,-9.72088778381102,
0.));
#187882=CARTESIAN_POINT('Ctrl Pts',(20.3685406190576,-9.72251930722504,
0.));
#187883=CARTESIAN_POINT('Ctrl Pts',(20.371960235676,-9.72432910043193,0.));
#187884=CARTESIAN_POINT('Ctrl Pts',(20.3756766651952,-9.72631531732871,
0.));
#187885=CARTESIAN_POINT('Ctrl Pts',(20.3796805893304,-9.72847589116533,
0.));
#187886=CARTESIAN_POINT('Ctrl Pts',(20.3839624556742,-9.73080870123726,
0.));
#187887=CARTESIAN_POINT('Ctrl Pts',(20.3885129129912,-9.73331167102812,
0.));
#187888=CARTESIAN_POINT('Ctrl Pts',(20.3933234845646,-9.7359829201425,0.));
#187889=CARTESIAN_POINT('Ctrl Pts',(20.3983866213331,-9.73882077613206,
0.));
#187890=CARTESIAN_POINT('Ctrl Pts',(20.4036953576549,-9.74182369656273,
0.));
#187891=CARTESIAN_POINT('Ctrl Pts',(20.4092430879861,-9.74499021838537,
0.));
#187892=CARTESIAN_POINT('Ctrl Pts',(20.4150232777393,-9.74831889242175,
0.));
#187893=CARTESIAN_POINT('Ctrl Pts',(20.4210295275818,-9.75180829786433,
0.));
#187894=CARTESIAN_POINT('Ctrl Pts',(20.4272556476629,-9.75545705902416,
0.));
#187895=CARTESIAN_POINT('Ctrl Pts',(20.4336957355474,-9.7592638628993,0.));
#187896=CARTESIAN_POINT('Ctrl Pts',(20.4403442329401,-9.76322747195502,
0.));
#187897=CARTESIAN_POINT('Ctrl Pts',(20.447195862298,-9.76734670980897,0.));
#187898=CARTESIAN_POINT('Ctrl Pts',(20.4542455817527,-9.7716204510407,0.));
#187899=CARTESIAN_POINT('Ctrl Pts',(20.4614885274973,-9.77604760815523,
0.));
#187900=CARTESIAN_POINT('Ctrl Pts',(20.4689199790668,-9.78062712373313,
0.));
#187901=CARTESIAN_POINT('Ctrl Pts',(20.4765353711585,-9.78535797314162,
0.));
#187902=CARTESIAN_POINT('Ctrl Pts',(20.4843302955329,-9.7902391649866,0.));
#187903=CARTESIAN_POINT('Ctrl Pts',(20.4923005087945,-9.79526974288344,
0.));
#187904=CARTESIAN_POINT('Ctrl Pts',(20.500441931211,-9.80044878520968,0.));
#187905=CARTESIAN_POINT('Ctrl Pts',(20.5087506310507,-9.80577540161103,
0.));
#187906=CARTESIAN_POINT('Ctrl Pts',(20.5172228122839,-9.81124873025278,
0.));
#187907=CARTESIAN_POINT('Ctrl Pts',(20.5258548000625,-9.81686793455918,
0.));
#187908=CARTESIAN_POINT('Ctrl Pts',(20.534643029951,-9.82263220080328,0.));
#187909=CARTESIAN_POINT('Ctrl Pts',(20.5435840460717,-9.82854073773858,
0.));
#187910=CARTESIAN_POINT('Ctrl Pts',(20.5526744976461,-9.83459277585321,
0.));
#187911=CARTESIAN_POINT('Ctrl Pts',(20.5619111362406,-9.84078756677589,
0.));
#187912=CARTESIAN_POINT('Ctrl Pts',(20.5712908125145,-9.84712438256308,
0.));
#187913=CARTESIAN_POINT('Ctrl Pts',(20.580810471002,-9.85360251457004,0.));
#187914=CARTESIAN_POINT('Ctrl Pts',(20.5904671449754,-9.8602212723275,0.));
#187915=CARTESIAN_POINT('Ctrl Pts',(20.6002579513696,-9.86697998242612,
0.));
#187916=CARTESIAN_POINT('Ctrl Pts',(20.6101800854491,-9.87387798732944,
0.));
#187917=CARTESIAN_POINT('Ctrl Pts',(20.6202308177472,-9.88091464472669,
0.));
#187918=CARTESIAN_POINT('Ctrl Pts',(20.6304074914086,-9.88808932697305,
0.));
#187919=CARTESIAN_POINT('Ctrl Pts',(20.6407075193977,-9.89540142049124,
0.));
#187920=CARTESIAN_POINT('Ctrl Pts',(20.6511283817415,-9.90285032516696,
0.));
#187921=CARTESIAN_POINT('Ctrl Pts',(20.6616676228315,-9.91043545377005,
0.));
#187922=CARTESIAN_POINT('Ctrl Pts',(20.6723228488261,-9.91815623141285,
0.));
#187923=CARTESIAN_POINT('Ctrl Pts',(20.6830917250255,-9.92601209498751,
0.));
#187924=CARTESIAN_POINT('Ctrl Pts',(20.6939719732485,-9.93400249259737,
0.));
#187925=CARTESIAN_POINT('Ctrl Pts',(20.7049613692237,-9.94212688298251,
0.));
#187926=CARTESIAN_POINT('Ctrl Pts',(20.716057740758,-9.95038473514962,0.));
#187927=CARTESIAN_POINT('Ctrl Pts',(20.7272589658752,-9.95877552798403,
0.));
#187928=CARTESIAN_POINT('Ctrl Pts',(20.7385629709795,-9.96729874986199,
0.));
#187929=CARTESIAN_POINT('Ctrl Pts',(20.7499677289625,-9.97595389823461,
0.));
#187930=CARTESIAN_POINT('Ctrl Pts',(20.7614712574989,-9.98474047926846,
0.));
#187931=CARTESIAN_POINT('Ctrl Pts',(20.7730716175417,-9.99365800754638,
0.));
#187932=CARTESIAN_POINT('Ctrl Pts',(20.7847669117568,-10.0027060057389,
0.));
#187933=CARTESIAN_POINT('Ctrl Pts',(20.7965552829907,-10.0118840042786,
0.));
#187934=CARTESIAN_POINT('Ctrl Pts',(20.8084349126885,-10.0211915410095,
0.));
#187935=CARTESIAN_POINT('Ctrl Pts',(20.8204040196599,-10.0306281609435,
0.));
#187936=CARTESIAN_POINT('Ctrl Pts',(20.8324608588906,-10.0401934160234,
0.));
#187937=CARTESIAN_POINT('Ctrl Pts',(20.8446037203402,-10.0498868648733,
0.));
#187938=CARTESIAN_POINT('Ctrl Pts',(20.856830927732,-10.0597080725375,0.));
#187939=CARTESIAN_POINT('Ctrl Pts',(20.8691408373705,-10.0696566102219,
0.));
#187940=CARTESIAN_POINT('Ctrl Pts',(20.8815318371844,-10.0797320551154,
0.));
#187941=CARTESIAN_POINT('Ctrl Pts',(20.8940023457371,-10.0899339901916,
0.));
#187942=CARTESIAN_POINT('Ctrl Pts',(20.9065508112556,-10.1002620040076,
0.));
#187943=CARTESIAN_POINT('Ctrl Pts',(20.9191757106266,-10.1107156904836,
0.));
#187944=CARTESIAN_POINT('Ctrl Pts',(20.931875548473,-10.1212946487057,0.));
#187945=CARTESIAN_POINT('Ctrl Pts',(20.944648856393,-10.1319984827909,0.));
#187946=CARTESIAN_POINT('Ctrl Pts',(20.9574941921591,-10.1428268017257,
0.));
#187947=CARTESIAN_POINT('Ctrl Pts',(20.970410138937,-10.1537792192065,0.));
#187948=CARTESIAN_POINT('Ctrl Pts',(20.9833953044736,-10.1648553534567,
0.));
#187949=CARTESIAN_POINT('Ctrl Pts',(20.9964483203685,-10.1760548270765,
0.));
#187950=CARTESIAN_POINT('Ctrl Pts',(21.0095678414486,-10.1873772669358,
0.));
#187951=CARTESIAN_POINT('Ctrl Pts',(21.0227525451107,-10.1988223040425,
0.));
#187952=CARTESIAN_POINT('Ctrl Pts',(21.0360011306814,-10.2103895734124,
0.));
#187953=CARTESIAN_POINT('Ctrl Pts',(21.0493123187483,-10.2220787139157,
0.));
#187954=CARTESIAN_POINT('Ctrl Pts',(21.0626848505665,-10.233889368157,0.));
#187955=CARTESIAN_POINT('Ctrl Pts',(21.0761174875448,-10.2458211823915,
0.));
#187956=CARTESIAN_POINT('Ctrl Pts',(21.0896090107066,-10.2578738064183,
0.));
#187957=CARTESIAN_POINT('Ctrl Pts',(21.1031582201625,-10.2700468934743,
0.));
#187958=CARTESIAN_POINT('Ctrl Pts',(21.1167639345623,-10.2823401001067,
0.));
#187959=CARTESIAN_POINT('Ctrl Pts',(21.130424990599,-10.2947530860714,0.));
#187960=CARTESIAN_POINT('Ctrl Pts',(21.1441402425831,-10.307285514268,0.));
#187961=CARTESIAN_POINT('Ctrl Pts',(21.1579085619959,-10.3199370506541,
0.));
#187962=CARTESIAN_POINT('Ctrl Pts',(21.1717288370512,-10.3327073641574,
0.));
#187963=CARTESIAN_POINT('Ctrl Pts',(21.1855999722427,-10.3455961265706,
0.));
#187964=CARTESIAN_POINT('Ctrl Pts',(21.1995208879205,-10.3586030124595,
0.));
#187965=CARTESIAN_POINT('Ctrl Pts',(21.2134905199359,-10.3717276991137,
0.));
#187966=CARTESIAN_POINT('Ctrl Pts',(21.2275078192708,-10.384969866479,0.));
#187967=CARTESIAN_POINT('Ctrl Pts',(21.2415717516713,-10.3983291970846,
0.));
#187968=CARTESIAN_POINT('Ctrl Pts',(21.2556812972741,-10.4118053759584,
0.));
#187969=CARTESIAN_POINT('Ctrl Pts',(21.2698354502391,-10.4253980905394,
0.));
#187970=CARTESIAN_POINT('Ctrl Pts',(21.2840332184471,-10.4391070306385,
0.));
#187971=CARTESIAN_POINT('Ctrl Pts',(21.2982736231924,-10.452931888387,0.));
#187972=CARTESIAN_POINT('Ctrl Pts',(21.312555698873,-10.4668723581768,0.));
#187973=CARTESIAN_POINT('Ctrl Pts',(21.3268784926823,-10.4809281365933,
0.));
#187974=CARTESIAN_POINT('Ctrl Pts',(21.3412410642912,-10.4950989223341,
0.));
#187975=CARTESIAN_POINT('Ctrl Pts',(21.3556424855822,-10.509384416169,0.));
#187976=CARTESIAN_POINT('Ctrl Pts',(21.3700818403942,-10.523784320906,0.));
#187977=CARTESIAN_POINT('Ctrl Pts',(21.3845582242604,-10.5382983413422,
0.));
#187978=CARTESIAN_POINT('Ctrl Pts',(21.3990707441495,-10.5529261842107,
0.));
#187979=CARTESIAN_POINT('Ctrl Pts',(21.4136185181974,-10.5676675581106,
0.));
#187980=CARTESIAN_POINT('Ctrl Pts',(21.4282006754624,-10.582522173457,0.));
#187981=CARTESIAN_POINT('Ctrl Pts',(21.4428163557137,-10.597489742462,0.));
#187982=CARTESIAN_POINT('Ctrl Pts',(21.4574647092093,-10.612569979096,0.));
#187983=CARTESIAN_POINT('Ctrl Pts',(21.4721448964766,-10.6277625990457,
0.));
#187984=CARTESIAN_POINT('Ctrl Pts',(21.4868560880893,-10.6430673196609,
0.));
#187985=CARTESIAN_POINT('Ctrl Pts',(21.5015974644454,-10.6584838598941,
0.));
#187986=CARTESIAN_POINT('Ctrl Pts',(21.5163682155805,-10.6740119402835,
0.));
#187987=CARTESIAN_POINT('Ctrl Pts',(21.531167540981,-10.689651282929,0.));
#187988=CARTESIAN_POINT('Ctrl Pts',(21.5459946493955,-10.7054016114571,
0.));
#187989=CARTESIAN_POINT('Ctrl Pts',(21.5608487586467,-10.7212626509816,
0.));
#187990=CARTESIAN_POINT('Ctrl Pts',(21.5757290954372,-10.7372341280468,
0.));
#187991=CARTESIAN_POINT('Ctrl Pts',(21.5906348951745,-10.7533157705943,
0.));
#187992=CARTESIAN_POINT('Ctrl Pts',(21.6055654018179,-10.7695073079554,
0.));
#187993=CARTESIAN_POINT('Ctrl Pts',(21.6205198677176,-10.7858084708262,
0.));
#187994=CARTESIAN_POINT('Ctrl Pts',(21.6354975534557,-10.802218991237,0.));
#187995=CARTESIAN_POINT('Ctrl Pts',(21.6504977276864,-10.8187386025135,
0.));
#187996=CARTESIAN_POINT('Ctrl Pts',(21.6655196669727,-10.835367039227,0.));
#187997=CARTESIAN_POINT('Ctrl Pts',(21.6805626556461,-10.8521040371832,
0.));
#187998=CARTESIAN_POINT('Ctrl Pts',(21.6956259856667,-10.8689493334093,
0.));
#187999=CARTESIAN_POINT('Ctrl Pts',(21.7107089564822,-10.8859026661292,
0.));
#188000=CARTESIAN_POINT('Ctrl Pts',(21.7258108748874,-10.9029637747341,
0.));
#188001=CARTESIAN_POINT('Ctrl Pts',(21.74093105488,-10.9201323997386,0.));
#188002=CARTESIAN_POINT('Ctrl Pts',(21.7560688175252,-10.9374082827446,
0.));
#188003=CARTESIAN_POINT('Ctrl Pts',(21.7712234908468,-10.9547911664457,
0.));
#188004=CARTESIAN_POINT('Ctrl Pts',(21.7863944097143,-10.9722807946157,
0.));
#188005=CARTESIAN_POINT('Ctrl Pts',(21.8015809157302,-10.9898769120913,
0.));
#188006=CARTESIAN_POINT('Ctrl Pts',(21.8167823571168,-11.0075792647477,
0.));
#188007=CARTESIAN_POINT('Ctrl Pts',(21.8319980886033,-11.0253875994598,
0.));
#188008=CARTESIAN_POINT('Ctrl Pts',(21.8472274713103,-11.0433016640808,
0.));
#188009=CARTESIAN_POINT('Ctrl Pts',(21.8624698726319,-11.0613212074364,
0.));
#188010=CARTESIAN_POINT('Ctrl Pts',(21.8777246661191,-11.0794459793058,
0.));
#188011=CARTESIAN_POINT('Ctrl Pts',(21.8929912313608,-11.0976757303944,
0.));
#188012=CARTESIAN_POINT('Ctrl Pts',(21.9082689538687,-11.1160102123024,
0.));
#188013=CARTESIAN_POINT('Ctrl Pts',(21.9235572249518,-11.134449177474,0.));
#188014=CARTESIAN_POINT('Ctrl Pts',(21.9388554416437,-11.1529923792002,
0.));
#188015=CARTESIAN_POINT('Ctrl Pts',(21.9541630066504,-11.1716395716375,
0.));
#188016=CARTESIAN_POINT('Ctrl Pts',(21.9694793282913,-11.190390509811,0.));
#188017=CARTESIAN_POINT('Ctrl Pts',(21.9848038204439,-11.2092449496125,
0.));
#188018=CARTESIAN_POINT('Ctrl Pts',(22.0001359024839,-11.2282026477897,
0.));
#188019=CARTESIAN_POINT('Ctrl Pts',(22.0154749992364,-11.2472633619276,
0.));
#188020=CARTESIAN_POINT('Ctrl Pts',(22.0308205408351,-11.2664268504207,
0.));
#188021=CARTESIAN_POINT('Ctrl Pts',(22.046171962566,-11.2856928724374,0.));
#188022=CARTESIAN_POINT('Ctrl Pts',(22.0615287047179,-11.3050611878771,
0.));
#188023=CARTESIAN_POINT('Ctrl Pts',(22.0768902124267,-11.3245315573168,
0.));
#188024=CARTESIAN_POINT('Ctrl Pts',(22.0922559355293,-11.3441037419553,
0.));
#188025=CARTESIAN_POINT('Ctrl Pts',(22.1076253283978,-11.3637775035367,
0.));
#188026=CARTESIAN_POINT('Ctrl Pts',(22.1229978500185,-11.3835526044256,
0.));
#188027=CARTESIAN_POINT('Ctrl Pts',(22.1383729640963,-11.4034288076909,
0.));
#188028=CARTESIAN_POINT('Ctrl Pts',(22.1537501391486,-11.4234058771742,
0.));
#188029=CARTESIAN_POINT('Ctrl Pts',(22.1691288486096,-11.443483577557,0.));
#188030=CARTESIAN_POINT('Ctrl Pts',(22.1845085709169,-11.463661674411,0.));
#188031=CARTESIAN_POINT('Ctrl Pts',(22.1998887896435,-11.4839399342589,
0.));
#188032=CARTESIAN_POINT('Ctrl Pts',(22.215268993102,-11.504318124424,0.));
#188033=CARTESIAN_POINT('Ctrl Pts',(22.2306486738899,-11.5247960128476,
0.));
#188034=CARTESIAN_POINT('Ctrl Pts',(22.2460273284653,-11.545373367912,0.));
#188035=CARTESIAN_POINT('Ctrl Pts',(22.2614044566898,-11.5660499582403,
0.));
#188036=CARTESIAN_POINT('Ctrl Pts',(22.2767795614349,-11.5868255525189,
0.));
#188037=CARTESIAN_POINT('Ctrl Pts',(22.2921521480357,-11.6076999192359,
0.));
#188038=CARTESIAN_POINT('Ctrl Pts',(22.3075217249049,-11.6286728270011,
0.));
#188039=CARTESIAN_POINT('Ctrl Pts',(22.3228878043976,-11.6497440449858,
0.));
#188040=CARTESIAN_POINT('Ctrl Pts',(22.3382499035618,-11.6709133432986,
0.));
#188041=CARTESIAN_POINT('Ctrl Pts',(22.3536075450028,-11.6921804934056,
0.));
#188042=CARTESIAN_POINT('Ctrl Pts',(22.3689602575492,-11.7135452684532,
0.));
#188043=CARTESIAN_POINT('Ctrl Pts',(22.3843075773905,-11.7350074437961,
0.));
#188044=CARTESIAN_POINT('Ctrl Pts',(22.39964904692,-11.7565667964765,0.));
#188045=CARTESIAN_POINT('Ctrl Pts',(22.4149842125018,-11.7782231042041,
0.));
#188046=CARTESIAN_POINT('Ctrl Pts',(22.4303126226468,-11.7999761445175,
0.));
#188047=CARTESIAN_POINT('Ctrl Pts',(22.4456338258738,-11.8218256937889,
0.));
#188048=CARTESIAN_POINT('Ctrl Pts',(22.4609473690469,-11.8437715264487,
0.));
#188049=CARTESIAN_POINT('Ctrl Pts',(22.4762527946694,-11.8658134137018,
0.));
#188050=CARTESIAN_POINT('Ctrl Pts',(22.4915496418472,-11.8879511239941,
0.));
#188051=CARTESIAN_POINT('Ctrl Pts',(22.5068374513958,-11.9101844254555,
0.));
#188052=CARTESIAN_POINT('Ctrl Pts',(22.5221157697869,-11.9325130877801,
0.));
#188053=CARTESIAN_POINT('Ctrl Pts',(22.5373841537299,-11.9549368843996,
0.));
#188054=CARTESIAN_POINT('Ctrl Pts',(22.5526421741159,-11.9774555943496,
0.));
#188055=CARTESIAN_POINT('Ctrl Pts',(22.5678894211194,-12.0000690046697,
0.));
#188056=CARTESIAN_POINT('Ctrl Pts',(22.5831255061306,-12.0227769113132,
0.));
#188057=CARTESIAN_POINT('Ctrl Pts',(22.5983500505675,-12.0455791139135,
0.));
#188058=CARTESIAN_POINT('Ctrl Pts',(22.613562676493,-12.0684754113869,0.));
#188059=CARTESIAN_POINT('Ctrl Pts',(22.628762996708,-12.0914655972828,0.));
#188060=CARTESIAN_POINT('Ctrl Pts',(22.6439506046611,-12.1145494550384,
0.));
#188061=CARTESIAN_POINT('Ctrl Pts',(22.6591250653942,-12.1377267537141,
0.));
#188062=CARTESIAN_POINT('Ctrl Pts',(22.6742859034891,-12.1609972423089,
0.));
#188063=CARTESIAN_POINT('Ctrl Pts',(22.6894326204959,-12.1843606579246,
0.));
#188064=CARTESIAN_POINT('Ctrl Pts',(22.7045647168659,-12.2078167360267,
0.));
#188065=CARTESIAN_POINT('Ctrl Pts',(22.7196817119299,-12.2313652198047,
0.));
#188066=CARTESIAN_POINT('Ctrl Pts',(22.7347831655251,-12.2550058702389,
0.));
#188067=CARTESIAN_POINT('Ctrl Pts',(22.7498686970096,-12.2787384750747,
0.));
#188068=CARTESIAN_POINT('Ctrl Pts',(22.7649380101154,-12.3025628601812,
0.));
#188069=CARTESIAN_POINT('Ctrl Pts',(22.7799908974947,-12.3264788926108,
0.));
#188070=CARTESIAN_POINT('Ctrl Pts',(22.7950272216959,-12.3504864740361,
0.));
#188071=CARTESIAN_POINT('Ctrl Pts',(22.8100469022632,-12.3745855366772,
0.));
#188072=CARTESIAN_POINT('Ctrl Pts',(22.8220493007353,-12.393937937903,0.));
#188073=CARTESIAN_POINT('Ctrl Pts',(22.8310435872852,-12.4084933766366,
0.));
#188074=CARTESIAN_POINT('Ctrl Pts',(22.8370364396497,-12.4182152851867,
0.));
#188075=CARTESIAN_POINT('Ctrl Pts',(22.8400320311648,-12.4230808101438,
0.));
#188076=CARTESIAN_POINT('',(22.8400320311648,-12.4230808101438,0.));
#188077=CARTESIAN_POINT('Origin',(16.3449727195351,-13.9675290154577,0.));
#188078=CARTESIAN_POINT('',(17.1452095830632,-14.6513681262571,0.));
#188079=CARTESIAN_POINT('',(17.1452095830632,-14.6513681262571,0.));
#188080=CARTESIAN_POINT('',(8.17248635976757,-6.98376450772884,0.));
#188081=CARTESIAN_POINT('Ctrl Pts',(22.1787195904339,-13.5685075571671,
0.));
#188082=CARTESIAN_POINT('Ctrl Pts',(22.1787195904339,-13.5685075571671,
12.));
#188083=CARTESIAN_POINT('Ctrl Pts',(22.1730081264583,-13.5683460612913,
0.));
#188084=CARTESIAN_POINT('Ctrl Pts',(22.1730081264583,-13.5683460612913,
12.));
#188085=CARTESIAN_POINT('Ctrl Pts',(22.1615922804939,-13.5680170531724,
0.));
#188086=CARTESIAN_POINT('Ctrl Pts',(22.1615922804939,-13.5680170531724,
12.));
#188087=CARTESIAN_POINT('Ctrl Pts',(22.1444897575076,-13.5675054918922,
0.));
#188088=CARTESIAN_POINT('Ctrl Pts',(22.1444897575076,-13.5675054918922,
12.));
#188089=CARTESIAN_POINT('Ctrl Pts',(22.1217288871823,-13.5667873105179,
0.));
#188090=CARTESIAN_POINT('Ctrl Pts',(22.1217288871823,-13.5667873105179,
12.));
#188091=CARTESIAN_POINT('Ctrl Pts',(22.0933486464442,-13.5658294169106,
0.));
#188092=CARTESIAN_POINT('Ctrl Pts',(22.0933486464442,-13.5658294169106,
12.));
#188093=CARTESIAN_POINT('Ctrl Pts',(22.0650393089492,-13.5648113688895,
0.));
#188094=CARTESIAN_POINT('Ctrl Pts',(22.0650393089492,-13.5648113688895,
12.));
#188095=CARTESIAN_POINT('Ctrl Pts',(22.0368009736227,-13.5637332022393,
0.));
#188096=CARTESIAN_POINT('Ctrl Pts',(22.0368009736227,-13.5637332022393,
12.));
#188097=CARTESIAN_POINT('Ctrl Pts',(22.0086337943431,-13.5625949868313,
0.));
#188098=CARTESIAN_POINT('Ctrl Pts',(22.0086337943431,-13.5625949868313,
12.));
#188099=CARTESIAN_POINT('Ctrl Pts',(21.9805379899192,-13.5613968357589,
0.));
#188100=CARTESIAN_POINT('Ctrl Pts',(21.9805379899192,-13.5613968357589,
12.));
#188101=CARTESIAN_POINT('Ctrl Pts',(21.9525138592862,-13.5601389185315,
0.));
#188102=CARTESIAN_POINT('Ctrl Pts',(21.9525138592862,-13.5601389185315,
12.));
#188103=CARTESIAN_POINT('Ctrl Pts',(21.9245617765827,-13.5588214586672,
0.));
#188104=CARTESIAN_POINT('Ctrl Pts',(21.9245617765827,-13.5588214586672,
12.));
#188105=CARTESIAN_POINT('Ctrl Pts',(21.8966821688876,-13.5574447178485,
0.));
#188106=CARTESIAN_POINT('Ctrl Pts',(21.8966821688876,-13.5574447178485,
12.));
#188107=CARTESIAN_POINT('Ctrl Pts',(21.8688754989401,-13.5560089839426,
0.));
#188108=CARTESIAN_POINT('Ctrl Pts',(21.8688754989401,-13.5560089839426,
12.));
#188109=CARTESIAN_POINT('Ctrl Pts',(21.841142245609,-13.5545145573048,0.));
#188110=CARTESIAN_POINT('Ctrl Pts',(21.841142245609,-13.5545145573048,12.));
#188111=CARTESIAN_POINT('Ctrl Pts',(21.8134828857963,-13.5529617381569,
0.));
#188112=CARTESIAN_POINT('Ctrl Pts',(21.8134828857963,-13.5529617381569,
12.));
#188113=CARTESIAN_POINT('Ctrl Pts',(21.7858978745848,-13.5513508127232,
0.));
#188114=CARTESIAN_POINT('Ctrl Pts',(21.7858978745848,-13.5513508127232,
12.));
#188115=CARTESIAN_POINT('Ctrl Pts',(21.7583876294532,-13.5496820422186,
0.));
#188116=CARTESIAN_POINT('Ctrl Pts',(21.7583876294532,-13.5496820422186,
12.));
#188117=CARTESIAN_POINT('Ctrl Pts',(21.730952541226,-13.5479556704457,0.));
#188118=CARTESIAN_POINT('Ctrl Pts',(21.730952541226,-13.5479556704457,12.));
#188119=CARTESIAN_POINT('Ctrl Pts',(21.7035929822939,-13.546171929503,0.));
#188120=CARTESIAN_POINT('Ctrl Pts',(21.7035929822939,-13.546171929503,12.));
#188121=CARTESIAN_POINT('Ctrl Pts',(21.676309315769,-13.5443310461516,0.));
#188122=CARTESIAN_POINT('Ctrl Pts',(21.676309315769,-13.5443310461516,12.));
#188123=CARTESIAN_POINT('Ctrl Pts',(21.6491019044647,-13.5424332480698,
0.));
#188124=CARTESIAN_POINT('Ctrl Pts',(21.6491019044647,-13.5424332480698,
12.));
#188125=CARTESIAN_POINT('Ctrl Pts',(21.6219711193951,-13.5404787697798,
0.));
#188126=CARTESIAN_POINT('Ctrl Pts',(21.6219711193951,-13.5404787697798,
12.));
#188127=CARTESIAN_POINT('Ctrl Pts',(21.5949173499022,-13.5384678597206,
0.));
#188128=CARTESIAN_POINT('Ctrl Pts',(21.5949173499022,-13.5384678597206,
12.));
#188129=CARTESIAN_POINT('Ctrl Pts',(21.5679410019011,-13.5364007790292,
0.));
#188130=CARTESIAN_POINT('Ctrl Pts',(21.5679410019011,-13.5364007790292,
12.));
#188131=CARTESIAN_POINT('Ctrl Pts',(21.5410424932511,-13.5342777983225,
0.));
#188132=CARTESIAN_POINT('Ctrl Pts',(21.5410424932511,-13.5342777983225,
12.));
#188133=CARTESIAN_POINT('Ctrl Pts',(21.5142222501671,-13.5320991952145,
0.));
#188134=CARTESIAN_POINT('Ctrl Pts',(21.5142222501671,-13.5320991952145,
12.));
#188135=CARTESIAN_POINT('Ctrl Pts',(21.487480703047,-13.5298652514357,0.));
#188136=CARTESIAN_POINT('Ctrl Pts',(21.487480703047,-13.5298652514357,12.));
#188137=CARTESIAN_POINT('Ctrl Pts',(21.4608182828695,-13.5275762503553,
0.));
#188138=CARTESIAN_POINT('Ctrl Pts',(21.4608182828695,-13.5275762503553,
12.));
#188139=CARTESIAN_POINT('Ctrl Pts',(21.4342354165254,-13.5252324737795,
0.));
#188140=CARTESIAN_POINT('Ctrl Pts',(21.4342354165254,-13.5252324737795,
12.));
#188141=CARTESIAN_POINT('Ctrl Pts',(21.4077325259318,-13.5228342013508,
0.));
#188142=CARTESIAN_POINT('Ctrl Pts',(21.4077325259318,-13.5228342013508,
12.));
#188143=CARTESIAN_POINT('Ctrl Pts',(21.3813100304967,-13.5203817122497,
0.));
#188144=CARTESIAN_POINT('Ctrl Pts',(21.3813100304967,-13.5203817122497,
12.));
#188145=CARTESIAN_POINT('Ctrl Pts',(21.3549683486219,-13.5178752862461,
0.));
#188146=CARTESIAN_POINT('Ctrl Pts',(21.3549683486219,-13.5178752862461,
12.));
#188147=CARTESIAN_POINT('Ctrl Pts',(21.328707899634,-13.5153152050554,0.));
#188148=CARTESIAN_POINT('Ctrl Pts',(21.328707899634,-13.5153152050554,12.));
#188149=CARTESIAN_POINT('Ctrl Pts',(21.3025291054236,-13.5127017534972,
0.));
#188150=CARTESIAN_POINT('Ctrl Pts',(21.3025291054236,-13.5127017534972,
12.));
#188151=CARTESIAN_POINT('Ctrl Pts',(21.2764323924442,-13.5100352209207,
0.));
#188152=CARTESIAN_POINT('Ctrl Pts',(21.2764323924442,-13.5100352209207,
12.));
#188153=CARTESIAN_POINT('Ctrl Pts',(21.2504181927429,-13.5073159019454,
0.));
#188154=CARTESIAN_POINT('Ctrl Pts',(21.2504181927429,-13.5073159019454,
12.));
#188155=CARTESIAN_POINT('Ctrl Pts',(21.224486942933,-13.5045440957404,0.));
#188156=CARTESIAN_POINT('Ctrl Pts',(21.224486942933,-13.5045440957404,12.));
#188157=CARTESIAN_POINT('Ctrl Pts',(21.1986390835825,-13.5017201056088,
0.));
#188158=CARTESIAN_POINT('Ctrl Pts',(21.1986390835825,-13.5017201056088,
12.));
#188159=CARTESIAN_POINT('Ctrl Pts',(21.1728750584173,-13.4988442384491,
0.));
#188160=CARTESIAN_POINT('Ctrl Pts',(21.1728750584173,-13.4988442384491,
12.));
#188161=CARTESIAN_POINT('Ctrl Pts',(21.1471953136209,-13.4959168042934,
0.));
#188162=CARTESIAN_POINT('Ctrl Pts',(21.1471953136209,-13.4959168042934,
12.));
#188163=CARTESIAN_POINT('Ctrl Pts',(21.1216002970209,-13.4929381157778,
0.));
#188164=CARTESIAN_POINT('Ctrl Pts',(21.1216002970209,-13.4929381157778,
12.));
#188165=CARTESIAN_POINT('Ctrl Pts',(21.0960904575048,-13.4899084877718,
0.));
#188166=CARTESIAN_POINT('Ctrl Pts',(21.0960904575048,-13.4899084877718,
12.));
#188167=CARTESIAN_POINT('Ctrl Pts',(21.0706662455202,-13.4868282377192,
0.));
#188168=CARTESIAN_POINT('Ctrl Pts',(21.0706662455202,-13.4868282377192,
12.));
#188169=CARTESIAN_POINT('Ctrl Pts',(21.0453281134247,-13.4836976858912,
0.));
#188170=CARTESIAN_POINT('Ctrl Pts',(21.0453281134247,-13.4836976858912,
12.));
#188171=CARTESIAN_POINT('Ctrl Pts',(21.0200765158885,-13.4805171556822,
0.));
#188172=CARTESIAN_POINT('Ctrl Pts',(21.0200765158885,-13.4805171556822,
12.));
#188173=CARTESIAN_POINT('Ctrl Pts',(20.9949119102592,-13.4772869738879,
0.));
#188174=CARTESIAN_POINT('Ctrl Pts',(20.9949119102592,-13.4772869738879,
12.));
#188175=CARTESIAN_POINT('Ctrl Pts',(20.9698347569476,-13.4740074710087,
0.));
#188176=CARTESIAN_POINT('Ctrl Pts',(20.9698347569476,-13.4740074710087,
12.));
#188177=CARTESIAN_POINT('Ctrl Pts',(20.9448455197557,-13.4706789815166,
0.));
#188178=CARTESIAN_POINT('Ctrl Pts',(20.9448455197557,-13.4706789815166,
12.));
#188179=CARTESIAN_POINT('Ctrl Pts',(20.9199446657584,-13.4673018437718,
0.));
#188180=CARTESIAN_POINT('Ctrl Pts',(20.9199446657584,-13.4673018437718,
12.));
#188181=CARTESIAN_POINT('Ctrl Pts',(20.8951326652158,-13.4638763999725,
0.));
#188182=CARTESIAN_POINT('Ctrl Pts',(20.8951326652158,-13.4638763999725,
12.));
#188183=CARTESIAN_POINT('Ctrl Pts',(20.8704099914641,-13.4604029960983,
0.));
#188184=CARTESIAN_POINT('Ctrl Pts',(20.8704099914641,-13.4604029960983,
12.));
#188185=CARTESIAN_POINT('Ctrl Pts',(20.8457771208082,-13.4568819818631,
0.));
#188186=CARTESIAN_POINT('Ctrl Pts',(20.8457771208082,-13.4568819818631,
12.));
#188187=CARTESIAN_POINT('Ctrl Pts',(20.821234532398,-13.4533137106667,0.));
#188188=CARTESIAN_POINT('Ctrl Pts',(20.821234532398,-13.4533137106667,12.));
#188189=CARTESIAN_POINT('Ctrl Pts',(20.7967827081227,-13.4496985395637,
0.));
#188190=CARTESIAN_POINT('Ctrl Pts',(20.7967827081227,-13.4496985395637,
12.));
#188191=CARTESIAN_POINT('Ctrl Pts',(20.7724221327608,-13.4460368293688,
0.));
#188192=CARTESIAN_POINT('Ctrl Pts',(20.7724221327608,-13.4460368293688,
12.));
#188193=CARTESIAN_POINT('Ctrl Pts',(20.7481532941013,-13.4423289447561,
0.));
#188194=CARTESIAN_POINT('Ctrl Pts',(20.7481532941013,-13.4423289447561,
12.));
#188195=CARTESIAN_POINT('Ctrl Pts',(20.7239766830675,-13.4385752543663,
0.));
#188196=CARTESIAN_POINT('Ctrl Pts',(20.7239766830675,-13.4385752543663,
12.));
#188197=CARTESIAN_POINT('Ctrl Pts',(20.6998927938288,-13.4347761309154,
0.));
#188198=CARTESIAN_POINT('Ctrl Pts',(20.6998927938288,-13.4347761309154,
12.));
#188199=CARTESIAN_POINT('Ctrl Pts',(20.6759021239103,-13.4309319513119,
0.));
#188200=CARTESIAN_POINT('Ctrl Pts',(20.6759021239103,-13.4309319513119,
12.));
#188201=CARTESIAN_POINT('Ctrl Pts',(20.6520051742869,-13.4270430967651,
0.));
#188202=CARTESIAN_POINT('Ctrl Pts',(20.6520051742869,-13.4270430967651,
12.));
#188203=CARTESIAN_POINT('Ctrl Pts',(20.6282024494237,-13.4231099528179,
0.));
#188204=CARTESIAN_POINT('Ctrl Pts',(20.6282024494237,-13.4231099528179,
12.));
#188205=CARTESIAN_POINT('Ctrl Pts',(20.6044944573153,-13.4191329093933,
0.));
#188206=CARTESIAN_POINT('Ctrl Pts',(20.6044944573153,-13.4191329093933,
12.));
#188207=CARTESIAN_POINT('Ctrl Pts',(20.5808817095155,-13.4151123608411,
0.));
#188208=CARTESIAN_POINT('Ctrl Pts',(20.5808817095155,-13.4151123608411,
12.));
#188209=CARTESIAN_POINT('Ctrl Pts',(20.5573647211639,-13.4110487059912,
0.));
#188210=CARTESIAN_POINT('Ctrl Pts',(20.5573647211639,-13.4110487059912,
12.));
#188211=CARTESIAN_POINT('Ctrl Pts',(20.5339440109956,-13.4069423482076,
0.));
#188212=CARTESIAN_POINT('Ctrl Pts',(20.5339440109956,-13.4069423482076,
12.));
#188213=CARTESIAN_POINT('Ctrl Pts',(20.5106201013753,-13.4027936954529,
0.));
#188214=CARTESIAN_POINT('Ctrl Pts',(20.5106201013753,-13.4027936954529,
12.));
#188215=CARTESIAN_POINT('Ctrl Pts',(20.487393518404,-13.3986031603716,0.));
#188216=CARTESIAN_POINT('Ctrl Pts',(20.487393518404,-13.3986031603716,12.));
#188217=CARTESIAN_POINT('Ctrl Pts',(20.4642647920038,-13.3943711603739,
0.));
#188218=CARTESIAN_POINT('Ctrl Pts',(20.4642647920038,-13.3943711603739,
12.));
#188219=CARTESIAN_POINT('Ctrl Pts',(20.4412344560008,-13.3900981177255,
0.));
#188220=CARTESIAN_POINT('Ctrl Pts',(20.4412344560008,-13.3900981177255,
12.));
#188221=CARTESIAN_POINT('Ctrl Pts',(20.4183030482002,-13.3857844596387,
0.));
#188222=CARTESIAN_POINT('Ctrl Pts',(20.4183030482002,-13.3857844596387,
12.));
#188223=CARTESIAN_POINT('Ctrl Pts',(20.3954711104502,-13.3814306183719,
0.));
#188224=CARTESIAN_POINT('Ctrl Pts',(20.3954711104502,-13.3814306183719,
12.));
#188225=CARTESIAN_POINT('Ctrl Pts',(20.3727391887184,-13.3770370313188,
0.));
#188226=CARTESIAN_POINT('Ctrl Pts',(20.3727391887184,-13.3770370313188,
12.));
#188227=CARTESIAN_POINT('Ctrl Pts',(20.3501078331814,-13.3726041410867,
0.));
#188228=CARTESIAN_POINT('Ctrl Pts',(20.3501078331814,-13.3726041410867,
12.));
#188229=CARTESIAN_POINT('Ctrl Pts',(20.3275775983029,-13.3681323955826,
0.));
#188230=CARTESIAN_POINT('Ctrl Pts',(20.3275775983029,-13.3681323955826,
12.));
#188231=CARTESIAN_POINT('Ctrl Pts',(20.3051490429048,-13.3636222481016,
0.));
#188232=CARTESIAN_POINT('Ctrl Pts',(20.3051490429048,-13.3636222481016,
12.));
#188233=CARTESIAN_POINT('Ctrl Pts',(20.2828227302339,-13.3590741574195,
0.));
#188234=CARTESIAN_POINT('Ctrl Pts',(20.2828227302339,-13.3590741574195,
12.));
#188235=CARTESIAN_POINT('Ctrl Pts',(20.2605992280122,-13.3544885878889,
0.));
#188236=CARTESIAN_POINT('Ctrl Pts',(20.2605992280122,-13.3544885878889,
12.));
#188237=CARTESIAN_POINT('Ctrl Pts',(20.2384791085359,-13.3498660095386,
0.));
#188238=CARTESIAN_POINT('Ctrl Pts',(20.2384791085359,-13.3498660095386,
12.));
#188239=CARTESIAN_POINT('Ctrl Pts',(20.216462948786,-13.3452068981766,0.));
#188240=CARTESIAN_POINT('Ctrl Pts',(20.216462948786,-13.3452068981766,12.));
#188241=CARTESIAN_POINT('Ctrl Pts',(20.1945513305235,-13.3405117354971,
0.));
#188242=CARTESIAN_POINT('Ctrl Pts',(20.1945513305235,-13.3405117354971,
12.));
#188243=CARTESIAN_POINT('Ctrl Pts',(20.1727448403817,-13.3357810091903,
0.));
#188244=CARTESIAN_POINT('Ctrl Pts',(20.1727448403817,-13.3357810091903,
12.));
#188245=CARTESIAN_POINT('Ctrl Pts',(20.1510440699474,-13.3310152130564,
0.));
#188246=CARTESIAN_POINT('Ctrl Pts',(20.1510440699474,-13.3310152130564,
12.));
#188247=CARTESIAN_POINT('Ctrl Pts',(20.1294496158402,-13.3262148471226,
0.));
#188248=CARTESIAN_POINT('Ctrl Pts',(20.1294496158402,-13.3262148471226,
12.));
#188249=CARTESIAN_POINT('Ctrl Pts',(20.1079620798375,-13.3213804177587,
0.));
#188250=CARTESIAN_POINT('Ctrl Pts',(20.1079620798375,-13.3213804177587,
12.));
#188251=CARTESIAN_POINT('Ctrl Pts',(20.0865820689882,-13.3165124377963,
0.));
#188252=CARTESIAN_POINT('Ctrl Pts',(20.0865820689882,-13.3165124377963,
12.));
#188253=CARTESIAN_POINT('Ctrl Pts',(20.0653101957188,-13.3116114266515,
0.));
#188254=CARTESIAN_POINT('Ctrl Pts',(20.0653101957188,-13.3116114266515,
12.));
#188255=CARTESIAN_POINT('Ctrl Pts',(20.0441470779345,-13.3066779104515,
0.));
#188256=CARTESIAN_POINT('Ctrl Pts',(20.0441470779345,-13.3066779104515,
12.));
#188257=CARTESIAN_POINT('Ctrl Pts',(20.0230933391038,-13.3017124221637,
0.));
#188258=CARTESIAN_POINT('Ctrl Pts',(20.0230933391038,-13.3017124221637,
12.));
#188259=CARTESIAN_POINT('Ctrl Pts',(20.0021496083738,-13.2967155017306,
0.));
#188260=CARTESIAN_POINT('Ctrl Pts',(20.0021496083738,-13.2967155017306,
12.));
#188261=CARTESIAN_POINT('Ctrl Pts',(19.981316520717,-13.2916876962094,0.));
#188262=CARTESIAN_POINT('Ctrl Pts',(19.981316520717,-13.2916876962094,12.));
#188263=CARTESIAN_POINT('Ctrl Pts',(19.9605947170586,-13.286629559915,0.));
#188264=CARTESIAN_POINT('Ctrl Pts',(19.9605947170586,-13.286629559915,12.));
#188265=CARTESIAN_POINT('Ctrl Pts',(19.9399848444019,-13.2815416545663,
0.));
#188266=CARTESIAN_POINT('Ctrl Pts',(19.9399848444019,-13.2815416545663,
12.));
#188267=CARTESIAN_POINT('Ctrl Pts',(19.9194875559422,-13.2764245494357,
0.));
#188268=CARTESIAN_POINT('Ctrl Pts',(19.9194875559422,-13.2764245494357,
12.));
#188269=CARTESIAN_POINT('Ctrl Pts',(19.8991035111745,-13.271278821502,0.));
#188270=CARTESIAN_POINT('Ctrl Pts',(19.8991035111745,-13.271278821502,12.));
#188271=CARTESIAN_POINT('Ctrl Pts',(19.8788333760577,-13.2661050556132,
0.));
#188272=CARTESIAN_POINT('Ctrl Pts',(19.8788333760577,-13.2661050556132,
12.));
#188273=CARTESIAN_POINT('Ctrl Pts',(19.8586778231715,-13.2609038446529,
0.));
#188274=CARTESIAN_POINT('Ctrl Pts',(19.8586778231715,-13.2609038446529,
12.));
#188275=CARTESIAN_POINT('Ctrl Pts',(19.8386375318634,-13.2556757897086,
0.));
#188276=CARTESIAN_POINT('Ctrl Pts',(19.8386375318634,-13.2556757897086,
12.));
#188277=CARTESIAN_POINT('Ctrl Pts',(19.8187131883917,-13.2504215002457,
0.));
#188278=CARTESIAN_POINT('Ctrl Pts',(19.8187131883917,-13.2504215002457,
12.));
#188279=CARTESIAN_POINT('Ctrl Pts',(19.7989054860495,-13.2451415942805,
0.));
#188280=CARTESIAN_POINT('Ctrl Pts',(19.7989054860495,-13.2451415942805,
12.));
#188281=CARTESIAN_POINT('Ctrl Pts',(19.7792151253289,-13.2398366985675,
0.));
#188282=CARTESIAN_POINT('Ctrl Pts',(19.7792151253289,-13.2398366985675,
12.));
#188283=CARTESIAN_POINT('Ctrl Pts',(19.7596428141168,-13.2345074487963,
0.));
#188284=CARTESIAN_POINT('Ctrl Pts',(19.7596428141168,-13.2345074487963,
12.));
#188285=CARTESIAN_POINT('Ctrl Pts',(19.7401892678697,-13.2291544897899,
0.));
#188286=CARTESIAN_POINT('Ctrl Pts',(19.7401892678697,-13.2291544897899,
12.));
#188287=CARTESIAN_POINT('Ctrl Pts',(19.7208552097868,-13.2237784757065,
0.));
#188288=CARTESIAN_POINT('Ctrl Pts',(19.7208552097868,-13.2237784757065,
12.));
#188289=CARTESIAN_POINT('Ctrl Pts',(19.7016413709685,-13.2183800702436,
0.));
#188290=CARTESIAN_POINT('Ctrl Pts',(19.7016413709685,-13.2183800702436,
12.));
#188291=CARTESIAN_POINT('Ctrl Pts',(19.6825484905823,-13.2129599468485,
0.));
#188292=CARTESIAN_POINT('Ctrl Pts',(19.6825484905823,-13.2129599468485,
12.));
#188293=CARTESIAN_POINT('Ctrl Pts',(19.6635773160936,-13.2075187889529,
0.));
#188294=CARTESIAN_POINT('Ctrl Pts',(19.6635773160936,-13.2075187889529,
12.));
#188295=CARTESIAN_POINT('Ctrl Pts',(19.6447286034772,-13.2020572902065,
0.));
#188296=CARTESIAN_POINT('Ctrl Pts',(19.6447286034772,-13.2020572902065,
12.));
#188297=CARTESIAN_POINT('Ctrl Pts',(19.6260031174244,-13.1965761547151,
0.));
#188298=CARTESIAN_POINT('Ctrl Pts',(19.6260031174244,-13.1965761547151,
12.));
#188299=CARTESIAN_POINT('Ctrl Pts',(19.6074016315414,-13.1910760972814,
0.));
#188300=CARTESIAN_POINT('Ctrl Pts',(19.6074016315414,-13.1910760972814,
12.));
#188301=CARTESIAN_POINT('Ctrl Pts',(19.5889249285338,-13.1855578436471,
0.));
#188302=CARTESIAN_POINT('Ctrl Pts',(19.5889249285338,-13.1855578436471,
12.));
#188303=CARTESIAN_POINT('Ctrl Pts',(19.5705738004667,-13.1800221307673,
0.));
#188304=CARTESIAN_POINT('Ctrl Pts',(19.5705738004667,-13.1800221307673,
12.));
#188305=CARTESIAN_POINT('Ctrl Pts',(19.5523490490244,-13.1744697070911,
0.));
#188306=CARTESIAN_POINT('Ctrl Pts',(19.5523490490244,-13.1744697070911,
12.));
#188307=CARTESIAN_POINT('Ctrl Pts',(19.5342514857562,-13.168901332843,0.));
#188308=CARTESIAN_POINT('Ctrl Pts',(19.5342514857562,-13.168901332843,12.));
#188309=CARTESIAN_POINT('Ctrl Pts',(19.5162819323213,-13.1633177803101,
0.));
#188310=CARTESIAN_POINT('Ctrl Pts',(19.5162819323213,-13.1633177803101,
12.));
#188311=CARTESIAN_POINT('Ctrl Pts',(19.4984412207082,-13.1577198341245,
0.));
#188312=CARTESIAN_POINT('Ctrl Pts',(19.4984412207082,-13.1577198341245,
12.));
#188313=CARTESIAN_POINT('Ctrl Pts',(19.4807301935268,-13.1521082915853,
0.));
#188314=CARTESIAN_POINT('Ctrl Pts',(19.4807301935268,-13.1521082915853,
12.));
#188315=CARTESIAN_POINT('Ctrl Pts',(19.4631497043258,-13.1464839629971,
0.));
#188316=CARTESIAN_POINT('Ctrl Pts',(19.4631497043258,-13.1464839629971,
12.));
#188317=CARTESIAN_POINT('Ctrl Pts',(19.4457006178876,-13.1408476720061,
0.));
#188318=CARTESIAN_POINT('Ctrl Pts',(19.4457006178876,-13.1408476720061,
12.));
#188319=CARTESIAN_POINT('Ctrl Pts',(19.4283838105262,-13.1352002559438,
0.));
#188320=CARTESIAN_POINT('Ctrl Pts',(19.4283838105262,-13.1352002559438,
12.));
#188321=CARTESIAN_POINT('Ctrl Pts',(19.4112001703557,-13.1295425661634,
0.));
#188322=CARTESIAN_POINT('Ctrl Pts',(19.4112001703557,-13.1295425661634,
12.));
#188323=CARTESIAN_POINT('Ctrl Pts',(19.3941505976263,-13.1238754684177,
0.));
#188324=CARTESIAN_POINT('Ctrl Pts',(19.3941505976263,-13.1238754684177,
12.));
#188325=CARTESIAN_POINT('Ctrl Pts',(19.3772360051091,-13.118199843271,0.));
#188326=CARTESIAN_POINT('Ctrl Pts',(19.3772360051091,-13.118199843271,12.));
#188327=CARTESIAN_POINT('Ctrl Pts',(19.3604573184515,-13.1125165865022,
0.));
#188328=CARTESIAN_POINT('Ctrl Pts',(19.3604573184515,-13.1125165865022,
12.));
#188329=CARTESIAN_POINT('Ctrl Pts',(19.3438154765395,-13.1068266095186,
0.));
#188330=CARTESIAN_POINT('Ctrl Pts',(19.3438154765395,-13.1068266095186,
12.));
#188331=CARTESIAN_POINT('Ctrl Pts',(19.3273114318269,-13.1011308397591,
0.));
#188332=CARTESIAN_POINT('Ctrl Pts',(19.3273114318269,-13.1011308397591,
12.));
#188333=CARTESIAN_POINT('Ctrl Pts',(19.310946150736,-13.0954302211479,0.));
#188334=CARTESIAN_POINT('Ctrl Pts',(19.310946150736,-13.0954302211479,12.));
#188335=CARTESIAN_POINT('Ctrl Pts',(19.2947206141247,-13.0897257145969,
0.));
#188336=CARTESIAN_POINT('Ctrl Pts',(19.2947206141247,-13.0897257145969,
12.));
#188337=CARTESIAN_POINT('Ctrl Pts',(19.2786358177198,-13.0840182984949,
0.));
#188338=CARTESIAN_POINT('Ctrl Pts',(19.2786358177198,-13.0840182984949,
12.));
#188339=CARTESIAN_POINT('Ctrl Pts',(19.2626927725596,-13.0783089692118,
0.));
#188340=CARTESIAN_POINT('Ctrl Pts',(19.2626927725596,-13.0783089692118,
12.));
#188341=CARTESIAN_POINT('Ctrl Pts',(19.2468925053989,-13.0725987415859,
0.));
#188342=CARTESIAN_POINT('Ctrl Pts',(19.2468925053989,-13.0725987415859,
12.));
#188343=CARTESIAN_POINT('Ctrl Pts',(19.2312360592033,-13.0668886494795,
0.));
#188344=CARTESIAN_POINT('Ctrl Pts',(19.2312360592033,-13.0668886494795,
12.));
#188345=CARTESIAN_POINT('Ctrl Pts',(19.2157244937142,-13.0611797463915,
0.));
#188346=CARTESIAN_POINT('Ctrl Pts',(19.2157244937142,-13.0611797463915,
12.));
#188347=CARTESIAN_POINT('Ctrl Pts',(19.2003588859772,-13.0554731060538,
0.));
#188348=CARTESIAN_POINT('Ctrl Pts',(19.2003588859772,-13.0554731060538,
12.));
#188349=CARTESIAN_POINT('Ctrl Pts',(19.1851403308825,-13.0497698230441,
0.));
#188350=CARTESIAN_POINT('Ctrl Pts',(19.1851403308825,-13.0497698230441,
12.));
#188351=CARTESIAN_POINT('Ctrl Pts',(19.1700699416622,-13.0440710133772,
0.));
#188352=CARTESIAN_POINT('Ctrl Pts',(19.1700699416622,-13.0440710133772,
12.));
#188353=CARTESIAN_POINT('Ctrl Pts',(19.155148850523,-13.0383778152068,0.));
#188354=CARTESIAN_POINT('Ctrl Pts',(19.155148850523,-13.0383778152068,12.));
#188355=CARTESIAN_POINT('Ctrl Pts',(19.1403782093386,-13.0326913895838,
0.));
#188356=CARTESIAN_POINT('Ctrl Pts',(19.1403782093386,-13.0326913895838,
12.));
#188357=CARTESIAN_POINT('Ctrl Pts',(19.1257591903099,-13.0270129211976,
0.));
#188358=CARTESIAN_POINT('Ctrl Pts',(19.1257591903099,-13.0270129211976,
12.));
#188359=CARTESIAN_POINT('Ctrl Pts',(19.111292986631,-13.0213436191328,0.));
#188360=CARTESIAN_POINT('Ctrl Pts',(19.111292986631,-13.0213436191328,12.));
#188361=CARTESIAN_POINT('Ctrl Pts',(19.0969808131228,-13.0156847176097,
0.));
#188362=CARTESIAN_POINT('Ctrl Pts',(19.0969808131228,-13.0156847176097,
12.));
#188363=CARTESIAN_POINT('Ctrl Pts',(19.0828239070484,-13.0100374768788,
0.));
#188364=CARTESIAN_POINT('Ctrl Pts',(19.0828239070484,-13.0100374768788,
12.));
#188365=CARTESIAN_POINT('Ctrl Pts',(19.0688235289437,-13.0044031841382,
0.));
#188366=CARTESIAN_POINT('Ctrl Pts',(19.0688235289437,-13.0044031841382,
12.));
#188367=CARTESIAN_POINT('Ctrl Pts',(19.0549809634354,-12.9987831544502,
0.));
#188368=CARTESIAN_POINT('Ctrl Pts',(19.0549809634354,-12.9987831544502,
12.));
#188369=CARTESIAN_POINT('Ctrl Pts',(19.0412975200398,-12.9931787316514,
0.));
#188370=CARTESIAN_POINT('Ctrl Pts',(19.0412975200398,-12.9931787316514,
12.));
#188371=CARTESIAN_POINT('Ctrl Pts',(19.0277745339908,-12.9875912893003,
0.));
#188372=CARTESIAN_POINT('Ctrl Pts',(19.0277745339908,-12.9875912893003,
12.));
#188373=CARTESIAN_POINT('Ctrl Pts',(19.014413367335,-12.9820222318716,0.));
#188374=CARTESIAN_POINT('Ctrl Pts',(19.014413367335,-12.9820222318716,12.));
#188375=CARTESIAN_POINT('Ctrl Pts',(19.0012154099792,-12.9764729959206,
0.));
#188376=CARTESIAN_POINT('Ctrl Pts',(19.0012154099792,-12.9764729959206,
12.));
#188377=CARTESIAN_POINT('Ctrl Pts',(18.9881820807585,-12.9709450512747,
0.));
#188378=CARTESIAN_POINT('Ctrl Pts',(18.9881820807585,-12.9709450512747,
12.));
#188379=CARTESIAN_POINT('Ctrl Pts',(18.9753148284473,-12.9654399021868,
0.));
#188380=CARTESIAN_POINT('Ctrl Pts',(18.9753148284473,-12.9654399021868,
12.));
#188381=CARTESIAN_POINT('Ctrl Pts',(18.9626151329226,-12.9599590886318,
0.));
#188382=CARTESIAN_POINT('Ctrl Pts',(18.9626151329226,-12.9599590886318,
12.));
#188383=CARTESIAN_POINT('Ctrl Pts',(18.9500845064714,-12.9545041877377,
0.));
#188384=CARTESIAN_POINT('Ctrl Pts',(18.9500845064714,-12.9545041877377,
12.));
#188385=CARTESIAN_POINT('Ctrl Pts',(18.9377244950435,-12.9490768151821,
0.));
#188386=CARTESIAN_POINT('Ctrl Pts',(18.9377244950435,-12.9490768151821,
12.));
#188387=CARTESIAN_POINT('Ctrl Pts',(18.9255366795196,-12.9436786266106,
0.));
#188388=CARTESIAN_POINT('Ctrl Pts',(18.9255366795196,-12.9436786266106,
12.));
#188389=CARTESIAN_POINT('Ctrl Pts',(18.9135226769466,-12.9383113190375,
0.));
#188390=CARTESIAN_POINT('Ctrl Pts',(18.9135226769466,-12.9383113190375,
12.));
#188391=CARTESIAN_POINT('Ctrl Pts',(18.9016841423402,-12.9329766328184,
0.));
#188392=CARTESIAN_POINT('Ctrl Pts',(18.9016841423402,-12.9329766328184,
12.));
#188393=CARTESIAN_POINT('Ctrl Pts',(18.8900227704888,-12.9276763536372,
0.));
#188394=CARTESIAN_POINT('Ctrl Pts',(18.8900227704888,-12.9276763536372,
12.));
#188395=CARTESIAN_POINT('Ctrl Pts',(18.8785402977528,-12.9224123144982,
0.));
#188396=CARTESIAN_POINT('Ctrl Pts',(18.8785402977528,-12.9224123144982,
12.));
#188397=CARTESIAN_POINT('Ctrl Pts',(18.8672385038328,-12.9171863977047,
0.));
#188398=CARTESIAN_POINT('Ctrl Pts',(18.8672385038328,-12.9171863977047,
12.));
#188399=CARTESIAN_POINT('Ctrl Pts',(18.8561192136201,-12.9120005369066,
0.));
#188400=CARTESIAN_POINT('Ctrl Pts',(18.8561192136201,-12.9120005369066,
12.));
#188401=CARTESIAN_POINT('Ctrl Pts',(18.8451842990986,-12.9068567191856,
0.));
#188402=CARTESIAN_POINT('Ctrl Pts',(18.8451842990986,-12.9068567191856,
12.));
#188403=CARTESIAN_POINT('Ctrl Pts',(18.834435681259,-12.9017569871738,0.));
#188404=CARTESIAN_POINT('Ctrl Pts',(18.834435681259,-12.9017569871738,12.));
#188405=CARTESIAN_POINT('Ctrl Pts',(18.8238753319124,-12.8967034410752,
0.));
#188406=CARTESIAN_POINT('Ctrl Pts',(18.8238753319124,-12.8967034410752,
12.));
#188407=CARTESIAN_POINT('Ctrl Pts',(18.8135052757815,-12.8916982409931,
0.));
#188408=CARTESIAN_POINT('Ctrl Pts',(18.8135052757815,-12.8916982409931,
12.));
#188409=CARTESIAN_POINT('Ctrl Pts',(18.8033275941939,-12.8867436109543,
0.));
#188410=CARTESIAN_POINT('Ctrl Pts',(18.8033275941939,-12.8867436109543,
12.));
#188411=CARTESIAN_POINT('Ctrl Pts',(18.7933444285867,-12.8818418427474,
0.));
#188412=CARTESIAN_POINT('Ctrl Pts',(18.7933444285867,-12.8818418427474,
12.));
#188413=CARTESIAN_POINT('Ctrl Pts',(18.7835579840481,-12.8769952998097,
0.));
#188414=CARTESIAN_POINT('Ctrl Pts',(18.7835579840481,-12.8769952998097,
12.));
#188415=CARTESIAN_POINT('Ctrl Pts',(18.7739705329028,-12.8722064211814,
0.));
#188416=CARTESIAN_POINT('Ctrl Pts',(18.7739705329028,-12.8722064211814,
12.));
#188417=CARTESIAN_POINT('Ctrl Pts',(18.7645844169568,-12.8674777239656,
0.));
#188418=CARTESIAN_POINT('Ctrl Pts',(18.7645844169568,-12.8674777239656,
12.));
#188419=CARTESIAN_POINT('Ctrl Pts',(18.7554020493888,-12.8628118054172,
0.));
#188420=CARTESIAN_POINT('Ctrl Pts',(18.7554020493888,-12.8628118054172,
12.));
#188421=CARTESIAN_POINT('Ctrl Pts',(18.7464259171248,-12.8582113455644,
0.));
#188422=CARTESIAN_POINT('Ctrl Pts',(18.7464259171248,-12.8582113455644,
12.));
#188423=CARTESIAN_POINT('Ctrl Pts',(18.7376585820851,-12.8536791086315,
0.));
#188424=CARTESIAN_POINT('Ctrl Pts',(18.7376585820851,-12.8536791086315,
12.));
#188425=CARTESIAN_POINT('Ctrl Pts',(18.7291026886552,-12.849217951159,0.));
#188426=CARTESIAN_POINT('Ctrl Pts',(18.7291026886552,-12.849217951159,12.));
#188427=CARTESIAN_POINT('Ctrl Pts',(18.7207609737701,-12.8448308329494,
0.));
#188428=CARTESIAN_POINT('Ctrl Pts',(18.7207609737701,-12.8448308329494,
12.));
#188429=CARTESIAN_POINT('Ctrl Pts',(18.7126362754446,-12.8405208263432,
0.));
#188430=CARTESIAN_POINT('Ctrl Pts',(18.7126362754446,-12.8405208263432,
12.));
#188431=CARTESIAN_POINT('Ctrl Pts',(18.7047315436296,-12.8362911280362,
0.));
#188432=CARTESIAN_POINT('Ctrl Pts',(18.7047315436296,-12.8362911280362,
12.));
#188433=CARTESIAN_POINT('Ctrl Pts',(18.6970498410173,-12.832145059979,0.));
#188434=CARTESIAN_POINT('Ctrl Pts',(18.6970498410173,-12.832145059979,12.));
#188435=CARTESIAN_POINT('Ctrl Pts',(18.6895943376172,-12.8280860635231,
0.));
#188436=CARTESIAN_POINT('Ctrl Pts',(18.6895943376172,-12.8280860635231,
12.));
#188437=CARTESIAN_POINT('Ctrl Pts',(18.6823683094139,-12.8241176980016,
0.));
#188438=CARTESIAN_POINT('Ctrl Pts',(18.6823683094139,-12.8241176980016,
12.));
#188439=CARTESIAN_POINT('Ctrl Pts',(18.6753751301091,-12.8202436318473,
0.));
#188440=CARTESIAN_POINT('Ctrl Pts',(18.6753751301091,-12.8202436318473,
12.));
#188441=CARTESIAN_POINT('Ctrl Pts',(18.6686182952798,-12.8164676687361,
0.));
#188442=CARTESIAN_POINT('Ctrl Pts',(18.6686182952798,-12.8164676687361,
12.));
#188443=CARTESIAN_POINT('Ctrl Pts',(18.6621014624746,-12.8127937909632,
0.));
#188444=CARTESIAN_POINT('Ctrl Pts',(18.6621014624746,-12.8127937909632,
12.));
#188445=CARTESIAN_POINT('Ctrl Pts',(18.6558284825772,-12.8092261933858,
0.));
#188446=CARTESIAN_POINT('Ctrl Pts',(18.6558284825772,-12.8092261933858,
12.));
#188447=CARTESIAN_POINT('Ctrl Pts',(18.6498034438986,-12.805769331162,0.));
#188448=CARTESIAN_POINT('Ctrl Pts',(18.6498034438986,-12.805769331162,12.));
#188449=CARTESIAN_POINT('Ctrl Pts',(18.6440306327457,-12.8024278770153,
0.));
#188450=CARTESIAN_POINT('Ctrl Pts',(18.6440306327457,-12.8024278770153,
12.));
#188451=CARTESIAN_POINT('Ctrl Pts',(18.63851447924,-12.7992066625264,0.));
#188452=CARTESIAN_POINT('Ctrl Pts',(18.63851447924,-12.7992066625264,12.));
#188453=CARTESIAN_POINT('Ctrl Pts',(18.6332595057005,-12.7961106222251,
0.));
#188454=CARTESIAN_POINT('Ctrl Pts',(18.6332595057005,-12.7961106222251,
12.));
#188455=CARTESIAN_POINT('Ctrl Pts',(18.6282702819371,-12.7931447451556,
0.));
#188456=CARTESIAN_POINT('Ctrl Pts',(18.6282702819371,-12.7931447451556,
12.));
#188457=CARTESIAN_POINT('Ctrl Pts',(18.6235516265575,-12.7903142925234,
0.));
#188458=CARTESIAN_POINT('Ctrl Pts',(18.6235516265575,-12.7903142925234,
12.));
#188459=CARTESIAN_POINT('Ctrl Pts',(18.6191087624752,-12.7876249657834,
0.));
#188460=CARTESIAN_POINT('Ctrl Pts',(18.6191087624752,-12.7876249657834,
12.));
#188461=CARTESIAN_POINT('Ctrl Pts',(18.6149475565189,-12.78508316579,0.));
#188462=CARTESIAN_POINT('Ctrl Pts',(18.6149475565189,-12.78508316579,12.));
#188463=CARTESIAN_POINT('Ctrl Pts',(18.611074482622,-12.7826959526924,0.));
#188464=CARTESIAN_POINT('Ctrl Pts',(18.611074482622,-12.7826959526924,12.));
#188465=CARTESIAN_POINT('Ctrl Pts',(18.6074961535723,-12.7804705387658,
0.));
#188466=CARTESIAN_POINT('Ctrl Pts',(18.6074961535723,-12.7804705387658,
12.));
#188467=CARTESIAN_POINT('Ctrl Pts',(18.6042190183703,-12.7784139605067,
0.));
#188468=CARTESIAN_POINT('Ctrl Pts',(18.6042190183703,-12.7784139605067,
12.));
#188469=CARTESIAN_POINT('Ctrl Pts',(18.6012488486708,-12.7765325225082,
0.));
#188470=CARTESIAN_POINT('Ctrl Pts',(18.6012488486708,-12.7765325225082,
12.));
#188471=CARTESIAN_POINT('Ctrl Pts',(18.5985917525949,-12.7748328937639,
0.));
#188472=CARTESIAN_POINT('Ctrl Pts',(18.5985917525949,-12.7748328937639,
12.));
#188473=CARTESIAN_POINT('Ctrl Pts',(18.5962551167772,-12.7733231262107,
0.));
#188474=CARTESIAN_POINT('Ctrl Pts',(18.5962551167772,-12.7733231262107,
12.));
#188475=CARTESIAN_POINT('Ctrl Pts',(18.5942490615409,-12.7720142287169,
0.));
#188476=CARTESIAN_POINT('Ctrl Pts',(18.5942490615409,-12.7720142287169,
12.));
#188477=CARTESIAN_POINT('Ctrl Pts',(18.5925859134582,-12.7709195951153,
0.));
#188478=CARTESIAN_POINT('Ctrl Pts',(18.5925859134582,-12.7709195951153,
12.));
#188479=CARTESIAN_POINT('Ctrl Pts',(18.5912775137806,-12.7700520897174,
0.));
#188480=CARTESIAN_POINT('Ctrl Pts',(18.5912775137806,-12.7700520897174,
12.));
#188481=CARTESIAN_POINT('Ctrl Pts',(18.590332877722,-12.7694215127923,0.));
#188482=CARTESIAN_POINT('Ctrl Pts',(18.590332877722,-12.7694215127923,12.));
#188483=CARTESIAN_POINT('Ctrl Pts',(18.589871621842,-12.7691103481996,0.));
#188484=CARTESIAN_POINT('Ctrl Pts',(18.589871621842,-12.7691103481996,12.));
#188485=CARTESIAN_POINT('Ctrl Pts',(18.5896919669158,-12.7689864266924,
0.));
#188486=CARTESIAN_POINT('Ctrl Pts',(18.5896919669158,-12.7689864266924,
12.));
#188487=CARTESIAN_POINT('Ctrl Pts',(18.5896460962961,-12.7689524524484,
0.));
#188488=CARTESIAN_POINT('Ctrl Pts',(18.5896460962961,-12.7689524524484,
12.));
#188489=CARTESIAN_POINT('Ctrl Pts',(18.5896416359912,-12.7689476255363,
0.));
#188490=CARTESIAN_POINT('Ctrl Pts',(18.5896416359912,-12.7689476255363,
12.));
#188491=CARTESIAN_POINT('',(22.1787195904339,-13.5685075571671,0.));
#188492=CARTESIAN_POINT('Ctrl Pts',(22.1787195904339,-13.5685075571671,
0.));
#188493=CARTESIAN_POINT('Ctrl Pts',(22.1730081264583,-13.5683460612913,
0.));
#188494=CARTESIAN_POINT('Ctrl Pts',(22.1615922804939,-13.5680170531724,
0.));
#188495=CARTESIAN_POINT('Ctrl Pts',(22.1444897575076,-13.5675054918922,
0.));
#188496=CARTESIAN_POINT('Ctrl Pts',(22.1217288871823,-13.5667873105179,
0.));
#188497=CARTESIAN_POINT('Ctrl Pts',(22.0933486464442,-13.5658294169106,
0.));
#188498=CARTESIAN_POINT('Ctrl Pts',(22.0650393089492,-13.5648113688895,
0.));
#188499=CARTESIAN_POINT('Ctrl Pts',(22.0368009736227,-13.5637332022393,
0.));
#188500=CARTESIAN_POINT('Ctrl Pts',(22.0086337943431,-13.5625949868313,
0.));
#188501=CARTESIAN_POINT('Ctrl Pts',(21.9805379899192,-13.5613968357589,
0.));
#188502=CARTESIAN_POINT('Ctrl Pts',(21.9525138592862,-13.5601389185315,
0.));
#188503=CARTESIAN_POINT('Ctrl Pts',(21.9245617765827,-13.5588214586672,
0.));
#188504=CARTESIAN_POINT('Ctrl Pts',(21.8966821688876,-13.5574447178485,
0.));
#188505=CARTESIAN_POINT('Ctrl Pts',(21.8688754989401,-13.5560089839426,
0.));
#188506=CARTESIAN_POINT('Ctrl Pts',(21.841142245609,-13.5545145573048,0.));
#188507=CARTESIAN_POINT('Ctrl Pts',(21.8134828857963,-13.5529617381569,
0.));
#188508=CARTESIAN_POINT('Ctrl Pts',(21.7858978745848,-13.5513508127232,
0.));
#188509=CARTESIAN_POINT('Ctrl Pts',(21.7583876294532,-13.5496820422186,
0.));
#188510=CARTESIAN_POINT('Ctrl Pts',(21.730952541226,-13.5479556704457,0.));
#188511=CARTESIAN_POINT('Ctrl Pts',(21.7035929822939,-13.546171929503,0.));
#188512=CARTESIAN_POINT('Ctrl Pts',(21.676309315769,-13.5443310461516,0.));
#188513=CARTESIAN_POINT('Ctrl Pts',(21.6491019044647,-13.5424332480698,
0.));
#188514=CARTESIAN_POINT('Ctrl Pts',(21.6219711193951,-13.5404787697798,
0.));
#188515=CARTESIAN_POINT('Ctrl Pts',(21.5949173499022,-13.5384678597206,
0.));
#188516=CARTESIAN_POINT('Ctrl Pts',(21.5679410019011,-13.5364007790292,
0.));
#188517=CARTESIAN_POINT('Ctrl Pts',(21.5410424932511,-13.5342777983225,
0.));
#188518=CARTESIAN_POINT('Ctrl Pts',(21.5142222501671,-13.5320991952145,
0.));
#188519=CARTESIAN_POINT('Ctrl Pts',(21.487480703047,-13.5298652514357,0.));
#188520=CARTESIAN_POINT('Ctrl Pts',(21.4608182828695,-13.5275762503553,
0.));
#188521=CARTESIAN_POINT('Ctrl Pts',(21.4342354165254,-13.5252324737795,
0.));
#188522=CARTESIAN_POINT('Ctrl Pts',(21.4077325259318,-13.5228342013508,
0.));
#188523=CARTESIAN_POINT('Ctrl Pts',(21.3813100304967,-13.5203817122497,
0.));
#188524=CARTESIAN_POINT('Ctrl Pts',(21.3549683486219,-13.5178752862461,
0.));
#188525=CARTESIAN_POINT('Ctrl Pts',(21.328707899634,-13.5153152050554,0.));
#188526=CARTESIAN_POINT('Ctrl Pts',(21.3025291054236,-13.5127017534972,
0.));
#188527=CARTESIAN_POINT('Ctrl Pts',(21.2764323924442,-13.5100352209207,
0.));
#188528=CARTESIAN_POINT('Ctrl Pts',(21.2504181927429,-13.5073159019454,
0.));
#188529=CARTESIAN_POINT('Ctrl Pts',(21.224486942933,-13.5045440957404,0.));
#188530=CARTESIAN_POINT('Ctrl Pts',(21.1986390835825,-13.5017201056088,
0.));
#188531=CARTESIAN_POINT('Ctrl Pts',(21.1728750584173,-13.4988442384491,
0.));
#188532=CARTESIAN_POINT('Ctrl Pts',(21.1471953136209,-13.4959168042934,
0.));
#188533=CARTESIAN_POINT('Ctrl Pts',(21.1216002970209,-13.4929381157778,
0.));
#188534=CARTESIAN_POINT('Ctrl Pts',(21.0960904575048,-13.4899084877718,
0.));
#188535=CARTESIAN_POINT('Ctrl Pts',(21.0706662455202,-13.4868282377192,
0.));
#188536=CARTESIAN_POINT('Ctrl Pts',(21.0453281134247,-13.4836976858912,
0.));
#188537=CARTESIAN_POINT('Ctrl Pts',(21.0200765158885,-13.4805171556822,
0.));
#188538=CARTESIAN_POINT('Ctrl Pts',(20.9949119102592,-13.4772869738879,
0.));
#188539=CARTESIAN_POINT('Ctrl Pts',(20.9698347569476,-13.4740074710087,
0.));
#188540=CARTESIAN_POINT('Ctrl Pts',(20.9448455197557,-13.4706789815166,
0.));
#188541=CARTESIAN_POINT('Ctrl Pts',(20.9199446657584,-13.4673018437718,
0.));
#188542=CARTESIAN_POINT('Ctrl Pts',(20.8951326652158,-13.4638763999725,
0.));
#188543=CARTESIAN_POINT('Ctrl Pts',(20.8704099914641,-13.4604029960983,
0.));
#188544=CARTESIAN_POINT('Ctrl Pts',(20.8457771208082,-13.4568819818631,
0.));
#188545=CARTESIAN_POINT('Ctrl Pts',(20.821234532398,-13.4533137106667,0.));
#188546=CARTESIAN_POINT('Ctrl Pts',(20.7967827081227,-13.4496985395637,
0.));
#188547=CARTESIAN_POINT('Ctrl Pts',(20.7724221327608,-13.4460368293688,
0.));
#188548=CARTESIAN_POINT('Ctrl Pts',(20.7481532941013,-13.4423289447561,
0.));
#188549=CARTESIAN_POINT('Ctrl Pts',(20.7239766830675,-13.4385752543663,
0.));
#188550=CARTESIAN_POINT('Ctrl Pts',(20.6998927938288,-13.4347761309154,
0.));
#188551=CARTESIAN_POINT('Ctrl Pts',(20.6759021239103,-13.4309319513119,
0.));
#188552=CARTESIAN_POINT('Ctrl Pts',(20.6520051742869,-13.4270430967651,
0.));
#188553=CARTESIAN_POINT('Ctrl Pts',(20.6282024494237,-13.4231099528179,
0.));
#188554=CARTESIAN_POINT('Ctrl Pts',(20.6044944573153,-13.4191329093933,
0.));
#188555=CARTESIAN_POINT('Ctrl Pts',(20.5808817095155,-13.4151123608411,
0.));
#188556=CARTESIAN_POINT('Ctrl Pts',(20.5573647211639,-13.4110487059912,
0.));
#188557=CARTESIAN_POINT('Ctrl Pts',(20.5339440109956,-13.4069423482076,
0.));
#188558=CARTESIAN_POINT('Ctrl Pts',(20.5106201013753,-13.4027936954529,
0.));
#188559=CARTESIAN_POINT('Ctrl Pts',(20.487393518404,-13.3986031603716,0.));
#188560=CARTESIAN_POINT('Ctrl Pts',(20.4642647920038,-13.3943711603739,
0.));
#188561=CARTESIAN_POINT('Ctrl Pts',(20.4412344560008,-13.3900981177255,
0.));
#188562=CARTESIAN_POINT('Ctrl Pts',(20.4183030482002,-13.3857844596387,
0.));
#188563=CARTESIAN_POINT('Ctrl Pts',(20.3954711104502,-13.3814306183719,
0.));
#188564=CARTESIAN_POINT('Ctrl Pts',(20.3727391887184,-13.3770370313188,
0.));
#188565=CARTESIAN_POINT('Ctrl Pts',(20.3501078331814,-13.3726041410867,
0.));
#188566=CARTESIAN_POINT('Ctrl Pts',(20.3275775983029,-13.3681323955826,
0.));
#188567=CARTESIAN_POINT('Ctrl Pts',(20.3051490429048,-13.3636222481016,
0.));
#188568=CARTESIAN_POINT('Ctrl Pts',(20.2828227302339,-13.3590741574195,
0.));
#188569=CARTESIAN_POINT('Ctrl Pts',(20.2605992280122,-13.3544885878889,
0.));
#188570=CARTESIAN_POINT('Ctrl Pts',(20.2384791085359,-13.3498660095386,
0.));
#188571=CARTESIAN_POINT('Ctrl Pts',(20.216462948786,-13.3452068981766,0.));
#188572=CARTESIAN_POINT('Ctrl Pts',(20.1945513305235,-13.3405117354971,
0.));
#188573=CARTESIAN_POINT('Ctrl Pts',(20.1727448403817,-13.3357810091903,
0.));
#188574=CARTESIAN_POINT('Ctrl Pts',(20.1510440699474,-13.3310152130564,
0.));
#188575=CARTESIAN_POINT('Ctrl Pts',(20.1294496158402,-13.3262148471226,
0.));
#188576=CARTESIAN_POINT('Ctrl Pts',(20.1079620798375,-13.3213804177587,
0.));
#188577=CARTESIAN_POINT('Ctrl Pts',(20.0865820689882,-13.3165124377963,
0.));
#188578=CARTESIAN_POINT('Ctrl Pts',(20.0653101957188,-13.3116114266515,
0.));
#188579=CARTESIAN_POINT('Ctrl Pts',(20.0441470779345,-13.3066779104515,
0.));
#188580=CARTESIAN_POINT('Ctrl Pts',(20.0230933391038,-13.3017124221637,
0.));
#188581=CARTESIAN_POINT('Ctrl Pts',(20.0021496083738,-13.2967155017306,
0.));
#188582=CARTESIAN_POINT('Ctrl Pts',(19.981316520717,-13.2916876962094,0.));
#188583=CARTESIAN_POINT('Ctrl Pts',(19.9605947170586,-13.286629559915,0.));
#188584=CARTESIAN_POINT('Ctrl Pts',(19.9399848444019,-13.2815416545663,
0.));
#188585=CARTESIAN_POINT('Ctrl Pts',(19.9194875559422,-13.2764245494357,
0.));
#188586=CARTESIAN_POINT('Ctrl Pts',(19.8991035111745,-13.271278821502,0.));
#188587=CARTESIAN_POINT('Ctrl Pts',(19.8788333760577,-13.2661050556132,
0.));
#188588=CARTESIAN_POINT('Ctrl Pts',(19.8586778231715,-13.2609038446529,
0.));
#188589=CARTESIAN_POINT('Ctrl Pts',(19.8386375318634,-13.2556757897086,
0.));
#188590=CARTESIAN_POINT('Ctrl Pts',(19.8187131883917,-13.2504215002457,
0.));
#188591=CARTESIAN_POINT('Ctrl Pts',(19.7989054860495,-13.2451415942805,
0.));
#188592=CARTESIAN_POINT('Ctrl Pts',(19.7792151253289,-13.2398366985675,
0.));
#188593=CARTESIAN_POINT('Ctrl Pts',(19.7596428141168,-13.2345074487963,
0.));
#188594=CARTESIAN_POINT('Ctrl Pts',(19.7401892678697,-13.2291544897899,
0.));
#188595=CARTESIAN_POINT('Ctrl Pts',(19.7208552097868,-13.2237784757065,
0.));
#188596=CARTESIAN_POINT('Ctrl Pts',(19.7016413709685,-13.2183800702436,
0.));
#188597=CARTESIAN_POINT('Ctrl Pts',(19.6825484905823,-13.2129599468485,
0.));
#188598=CARTESIAN_POINT('Ctrl Pts',(19.6635773160936,-13.2075187889529,
0.));
#188599=CARTESIAN_POINT('Ctrl Pts',(19.6447286034772,-13.2020572902065,
0.));
#188600=CARTESIAN_POINT('Ctrl Pts',(19.6260031174244,-13.1965761547151,
0.));
#188601=CARTESIAN_POINT('Ctrl Pts',(19.6074016315414,-13.1910760972814,
0.));
#188602=CARTESIAN_POINT('Ctrl Pts',(19.5889249285338,-13.1855578436471,
0.));
#188603=CARTESIAN_POINT('Ctrl Pts',(19.5705738004667,-13.1800221307673,
0.));
#188604=CARTESIAN_POINT('Ctrl Pts',(19.5523490490244,-13.1744697070911,
0.));
#188605=CARTESIAN_POINT('Ctrl Pts',(19.5342514857562,-13.168901332843,0.));
#188606=CARTESIAN_POINT('Ctrl Pts',(19.5162819323213,-13.1633177803101,
0.));
#188607=CARTESIAN_POINT('Ctrl Pts',(19.4984412207082,-13.1577198341245,
0.));
#188608=CARTESIAN_POINT('Ctrl Pts',(19.4807301935268,-13.1521082915853,
0.));
#188609=CARTESIAN_POINT('Ctrl Pts',(19.4631497043258,-13.1464839629971,
0.));
#188610=CARTESIAN_POINT('Ctrl Pts',(19.4457006178876,-13.1408476720061,
0.));
#188611=CARTESIAN_POINT('Ctrl Pts',(19.4283838105262,-13.1352002559438,
0.));
#188612=CARTESIAN_POINT('Ctrl Pts',(19.4112001703557,-13.1295425661634,
0.));
#188613=CARTESIAN_POINT('Ctrl Pts',(19.3941505976263,-13.1238754684177,
0.));
#188614=CARTESIAN_POINT('Ctrl Pts',(19.3772360051091,-13.118199843271,0.));
#188615=CARTESIAN_POINT('Ctrl Pts',(19.3604573184515,-13.1125165865022,
0.));
#188616=CARTESIAN_POINT('Ctrl Pts',(19.3438154765395,-13.1068266095186,
0.));
#188617=CARTESIAN_POINT('Ctrl Pts',(19.3273114318269,-13.1011308397591,
0.));
#188618=CARTESIAN_POINT('Ctrl Pts',(19.310946150736,-13.0954302211479,0.));
#188619=CARTESIAN_POINT('Ctrl Pts',(19.2947206141247,-13.0897257145969,
0.));
#188620=CARTESIAN_POINT('Ctrl Pts',(19.2786358177198,-13.0840182984949,
0.));
#188621=CARTESIAN_POINT('Ctrl Pts',(19.2626927725596,-13.0783089692118,
0.));
#188622=CARTESIAN_POINT('Ctrl Pts',(19.2468925053989,-13.0725987415859,
0.));
#188623=CARTESIAN_POINT('Ctrl Pts',(19.2312360592033,-13.0668886494795,
0.));
#188624=CARTESIAN_POINT('Ctrl Pts',(19.2157244937142,-13.0611797463915,
0.));
#188625=CARTESIAN_POINT('Ctrl Pts',(19.2003588859772,-13.0554731060538,
0.));
#188626=CARTESIAN_POINT('Ctrl Pts',(19.1851403308825,-13.0497698230441,
0.));
#188627=CARTESIAN_POINT('Ctrl Pts',(19.1700699416622,-13.0440710133772,
0.));
#188628=CARTESIAN_POINT('Ctrl Pts',(19.155148850523,-13.0383778152068,0.));
#188629=CARTESIAN_POINT('Ctrl Pts',(19.1403782093386,-13.0326913895838,
0.));
#188630=CARTESIAN_POINT('Ctrl Pts',(19.1257591903099,-13.0270129211976,
0.));
#188631=CARTESIAN_POINT('Ctrl Pts',(19.111292986631,-13.0213436191328,0.));
#188632=CARTESIAN_POINT('Ctrl Pts',(19.0969808131228,-13.0156847176097,
0.));
#188633=CARTESIAN_POINT('Ctrl Pts',(19.0828239070484,-13.0100374768788,
0.));
#188634=CARTESIAN_POINT('Ctrl Pts',(19.0688235289437,-13.0044031841382,
0.));
#188635=CARTESIAN_POINT('Ctrl Pts',(19.0549809634354,-12.9987831544502,
0.));
#188636=CARTESIAN_POINT('Ctrl Pts',(19.0412975200398,-12.9931787316514,
0.));
#188637=CARTESIAN_POINT('Ctrl Pts',(19.0277745339908,-12.9875912893003,
0.));
#188638=CARTESIAN_POINT('Ctrl Pts',(19.014413367335,-12.9820222318716,0.));
#188639=CARTESIAN_POINT('Ctrl Pts',(19.0012154099792,-12.9764729959206,
0.));
#188640=CARTESIAN_POINT('Ctrl Pts',(18.9881820807585,-12.9709450512747,
0.));
#188641=CARTESIAN_POINT('Ctrl Pts',(18.9753148284473,-12.9654399021868,
0.));
#188642=CARTESIAN_POINT('Ctrl Pts',(18.9626151329226,-12.9599590886318,
0.));
#188643=CARTESIAN_POINT('Ctrl Pts',(18.9500845064714,-12.9545041877377,
0.));
#188644=CARTESIAN_POINT('Ctrl Pts',(18.9377244950435,-12.9490768151821,
0.));
#188645=CARTESIAN_POINT('Ctrl Pts',(18.9255366795196,-12.9436786266106,
0.));
#188646=CARTESIAN_POINT('Ctrl Pts',(18.9135226769466,-12.9383113190375,
0.));
#188647=CARTESIAN_POINT('Ctrl Pts',(18.9016841423402,-12.9329766328184,
0.));
#188648=CARTESIAN_POINT('Ctrl Pts',(18.8900227704888,-12.9276763536372,
0.));
#188649=CARTESIAN_POINT('Ctrl Pts',(18.8785402977528,-12.9224123144982,
0.));
#188650=CARTESIAN_POINT('Ctrl Pts',(18.8672385038328,-12.9171863977047,
0.));
#188651=CARTESIAN_POINT('Ctrl Pts',(18.8561192136201,-12.9120005369066,
0.));
#188652=CARTESIAN_POINT('Ctrl Pts',(18.8451842990986,-12.9068567191856,
0.));
#188653=CARTESIAN_POINT('Ctrl Pts',(18.834435681259,-12.9017569871738,0.));
#188654=CARTESIAN_POINT('Ctrl Pts',(18.8238753319124,-12.8967034410752,
0.));
#188655=CARTESIAN_POINT('Ctrl Pts',(18.8135052757815,-12.8916982409931,
0.));
#188656=CARTESIAN_POINT('Ctrl Pts',(18.8033275941939,-12.8867436109543,
0.));
#188657=CARTESIAN_POINT('Ctrl Pts',(18.7933444285867,-12.8818418427474,
0.));
#188658=CARTESIAN_POINT('Ctrl Pts',(18.7835579840481,-12.8769952998097,
0.));
#188659=CARTESIAN_POINT('Ctrl Pts',(18.7739705329028,-12.8722064211814,
0.));
#188660=CARTESIAN_POINT('Ctrl Pts',(18.7645844169568,-12.8674777239656,
0.));
#188661=CARTESIAN_POINT('Ctrl Pts',(18.7554020493888,-12.8628118054172,
0.));
#188662=CARTESIAN_POINT('Ctrl Pts',(18.7464259171248,-12.8582113455644,
0.));
#188663=CARTESIAN_POINT('Ctrl Pts',(18.7376585820851,-12.8536791086315,
0.));
#188664=CARTESIAN_POINT('Ctrl Pts',(18.7291026886552,-12.849217951159,0.));
#188665=CARTESIAN_POINT('Ctrl Pts',(18.7207609737701,-12.8448308329494,
0.));
#188666=CARTESIAN_POINT('Ctrl Pts',(18.7126362754446,-12.8405208263432,
0.));
#188667=CARTESIAN_POINT('Ctrl Pts',(18.7047315436296,-12.8362911280362,
0.));
#188668=CARTESIAN_POINT('Ctrl Pts',(18.6970498410173,-12.832145059979,0.));
#188669=CARTESIAN_POINT('Ctrl Pts',(18.6895943376172,-12.8280860635231,
0.));
#188670=CARTESIAN_POINT('Ctrl Pts',(18.6823683094139,-12.8241176980016,
0.));
#188671=CARTESIAN_POINT('Ctrl Pts',(18.6753751301091,-12.8202436318473,
0.));
#188672=CARTESIAN_POINT('Ctrl Pts',(18.6686182952798,-12.8164676687361,
0.));
#188673=CARTESIAN_POINT('Ctrl Pts',(18.6621014624746,-12.8127937909632,
0.));
#188674=CARTESIAN_POINT('Ctrl Pts',(18.6558284825772,-12.8092261933858,
0.));
#188675=CARTESIAN_POINT('Ctrl Pts',(18.6498034438986,-12.805769331162,0.));
#188676=CARTESIAN_POINT('Ctrl Pts',(18.6440306327457,-12.8024278770153,
0.));
#188677=CARTESIAN_POINT('Ctrl Pts',(18.63851447924,-12.7992066625264,0.));
#188678=CARTESIAN_POINT('Ctrl Pts',(18.6332595057005,-12.7961106222251,
0.));
#188679=CARTESIAN_POINT('Ctrl Pts',(18.6282702819371,-12.7931447451556,
0.));
#188680=CARTESIAN_POINT('Ctrl Pts',(18.6235516265575,-12.7903142925234,
0.));
#188681=CARTESIAN_POINT('Ctrl Pts',(18.6191087624752,-12.7876249657834,
0.));
#188682=CARTESIAN_POINT('Ctrl Pts',(18.6149475565189,-12.78508316579,0.));
#188683=CARTESIAN_POINT('Ctrl Pts',(18.611074482622,-12.7826959526924,0.));
#188684=CARTESIAN_POINT('Ctrl Pts',(18.6074961535723,-12.7804705387658,
0.));
#188685=CARTESIAN_POINT('Ctrl Pts',(18.6042190183703,-12.7784139605067,
0.));
#188686=CARTESIAN_POINT('Ctrl Pts',(18.6012488486708,-12.7765325225082,
0.));
#188687=CARTESIAN_POINT('Ctrl Pts',(18.5985917525949,-12.7748328937639,
0.));
#188688=CARTESIAN_POINT('Ctrl Pts',(18.5962551167772,-12.7733231262107,
0.));
#188689=CARTESIAN_POINT('Ctrl Pts',(18.5942490615409,-12.7720142287169,
0.));
#188690=CARTESIAN_POINT('Ctrl Pts',(18.5925859134582,-12.7709195951153,
0.));
#188691=CARTESIAN_POINT('Ctrl Pts',(18.5912775137806,-12.7700520897174,
0.));
#188692=CARTESIAN_POINT('Ctrl Pts',(18.590332877722,-12.7694215127923,0.));
#188693=CARTESIAN_POINT('Ctrl Pts',(18.589871621842,-12.7691103481996,0.));
#188694=CARTESIAN_POINT('Ctrl Pts',(18.5896919669158,-12.7689864266924,
0.));
#188695=CARTESIAN_POINT('Ctrl Pts',(18.5896460962961,-12.7689524524484,
0.));
#188696=CARTESIAN_POINT('Ctrl Pts',(18.5896416359912,-12.7689476255363,
0.));
#188697=CARTESIAN_POINT('',(22.1787195904339,-13.5685075571671,0.));
#188698=CARTESIAN_POINT('Ctrl Pts',(17.1452095830632,-14.6513681262571,
0.));
#188699=CARTESIAN_POINT('Ctrl Pts',(17.1452095830632,-14.6513681262571,
12.));
#188700=CARTESIAN_POINT('Ctrl Pts',(17.1452153999142,-14.6513711852843,
0.));
#188701=CARTESIAN_POINT('Ctrl Pts',(17.1452153999142,-14.6513711852843,
12.));
#188702=CARTESIAN_POINT('Ctrl Pts',(17.1452600887037,-14.6514066997196,
0.));
#188703=CARTESIAN_POINT('Ctrl Pts',(17.1452600887037,-14.6514066997196,
12.));
#188704=CARTESIAN_POINT('Ctrl Pts',(17.1454262858043,-14.6515481598068,
0.));
#188705=CARTESIAN_POINT('Ctrl Pts',(17.1454262858043,-14.6515481598068,
12.));
#188706=CARTESIAN_POINT('Ctrl Pts',(17.1458462295271,-14.6519131634508,
0.));
#188707=CARTESIAN_POINT('Ctrl Pts',(17.1458462295271,-14.6519131634508,
12.));
#188708=CARTESIAN_POINT('Ctrl Pts',(17.1466998098673,-14.6526624064978,
0.));
#188709=CARTESIAN_POINT('Ctrl Pts',(17.1466998098673,-14.6526624064978,
12.));
#188710=CARTESIAN_POINT('Ctrl Pts',(17.147876394491,-14.6537016966184,0.));
#188711=CARTESIAN_POINT('Ctrl Pts',(17.147876394491,-14.6537016966184,12.));
#188712=CARTESIAN_POINT('Ctrl Pts',(17.1493641837558,-14.655024862281,0.));
#188713=CARTESIAN_POINT('Ctrl Pts',(17.1493641837558,-14.655024862281,12.));
#188714=CARTESIAN_POINT('Ctrl Pts',(17.1511476869496,-14.6566237952435,
0.));
#188715=CARTESIAN_POINT('Ctrl Pts',(17.1511476869496,-14.6566237952435,
12.));
#188716=CARTESIAN_POINT('Ctrl Pts',(17.1532107762718,-14.6584900555302,
0.));
#188717=CARTESIAN_POINT('Ctrl Pts',(17.1532107762718,-14.6584900555302,
12.));
#188718=CARTESIAN_POINT('Ctrl Pts',(17.1555401986401,-14.6606167169642,
0.));
#188719=CARTESIAN_POINT('Ctrl Pts',(17.1555401986401,-14.6606167169642,
12.));
#188720=CARTESIAN_POINT('Ctrl Pts',(17.1581262646789,-14.6629987285992,
0.));
#188721=CARTESIAN_POINT('Ctrl Pts',(17.1581262646789,-14.6629987285992,
12.));
#188722=CARTESIAN_POINT('Ctrl Pts',(17.1609609517369,-14.6656319165057,
0.));
#188723=CARTESIAN_POINT('Ctrl Pts',(17.1609609517369,-14.6656319165057,
12.));
#188724=CARTESIAN_POINT('Ctrl Pts',(17.1640366762305,-14.6685123374423,
0.));
#188725=CARTESIAN_POINT('Ctrl Pts',(17.1640366762305,-14.6685123374423,
12.));
#188726=CARTESIAN_POINT('Ctrl Pts',(17.167344972302,-14.671635583332,0.));
#188727=CARTESIAN_POINT('Ctrl Pts',(17.167344972302,-14.671635583332,12.));
#188728=CARTESIAN_POINT('Ctrl Pts',(17.1708771619129,-14.6749971333867,
0.));
#188729=CARTESIAN_POINT('Ctrl Pts',(17.1708771619129,-14.6749971333867,
12.));
#188730=CARTESIAN_POINT('Ctrl Pts',(17.1746247499057,-14.6785925615677,
0.));
#188731=CARTESIAN_POINT('Ctrl Pts',(17.1746247499057,-14.6785925615677,
12.));
#188732=CARTESIAN_POINT('Ctrl Pts',(17.1785800350826,-14.6824178576167,
0.));
#188733=CARTESIAN_POINT('Ctrl Pts',(17.1785800350826,-14.6824178576167,
12.));
#188734=CARTESIAN_POINT('Ctrl Pts',(17.182736158472,-14.686469452232,0.));
#188735=CARTESIAN_POINT('Ctrl Pts',(17.182736158472,-14.686469452232,12.));
#188736=CARTESIAN_POINT('Ctrl Pts',(17.1870867909918,-14.6907440526958,
0.));
#188737=CARTESIAN_POINT('Ctrl Pts',(17.1870867909918,-14.6907440526958,
12.));
#188738=CARTESIAN_POINT('Ctrl Pts',(17.1916259308415,-14.6952385361706,
0.));
#188739=CARTESIAN_POINT('Ctrl Pts',(17.1916259308415,-14.6952385361706,
12.));
#188740=CARTESIAN_POINT('Ctrl Pts',(17.1963476411694,-14.699949811582,0.));
#188741=CARTESIAN_POINT('Ctrl Pts',(17.1963476411694,-14.699949811582,12.));
#188742=CARTESIAN_POINT('Ctrl Pts',(17.2012461084268,-14.7048748502663,
0.));
#188743=CARTESIAN_POINT('Ctrl Pts',(17.2012461084268,-14.7048748502663,
12.));
#188744=CARTESIAN_POINT('Ctrl Pts',(17.2063157097315,-14.7100107213586,
0.));
#188745=CARTESIAN_POINT('Ctrl Pts',(17.2063157097315,-14.7100107213586,
12.));
#188746=CARTESIAN_POINT('Ctrl Pts',(17.2115510835989,-14.7153546289339,
0.));
#188747=CARTESIAN_POINT('Ctrl Pts',(17.2115510835989,-14.7153546289339,
12.));
#188748=CARTESIAN_POINT('Ctrl Pts',(17.2169471814256,-14.7209039390327,
0.));
#188749=CARTESIAN_POINT('Ctrl Pts',(17.2169471814256,-14.7209039390327,
12.));
#188750=CARTESIAN_POINT('Ctrl Pts',(17.2224992099667,-14.7266561494282,
0.));
#188751=CARTESIAN_POINT('Ctrl Pts',(17.2224992099667,-14.7266561494282,
12.));
#188752=CARTESIAN_POINT('Ctrl Pts',(17.2282025904314,-14.7326088681163,
0.));
#188753=CARTESIAN_POINT('Ctrl Pts',(17.2282025904314,-14.7326088681163,
12.));
#188754=CARTESIAN_POINT('Ctrl Pts',(17.2340529062076,-14.7387597858117,
0.));
#188755=CARTESIAN_POINT('Ctrl Pts',(17.2340529062076,-14.7387597858117,
12.));
#188756=CARTESIAN_POINT('Ctrl Pts',(17.2400458713565,-14.7451066593792,
0.));
#188757=CARTESIAN_POINT('Ctrl Pts',(17.2400458713565,-14.7451066593792,
12.));
#188758=CARTESIAN_POINT('Ctrl Pts',(17.2461773413288,-14.7516473175124,
0.));
#188759=CARTESIAN_POINT('Ctrl Pts',(17.2461773413288,-14.7516473175124,
12.));
#188760=CARTESIAN_POINT('Ctrl Pts',(17.2524433146837,-14.7583796616617,
0.));
#188761=CARTESIAN_POINT('Ctrl Pts',(17.2524433146837,-14.7583796616617,
12.));
#188762=CARTESIAN_POINT('Ctrl Pts',(17.2588399401465,-14.7653016697591,
0.));
#188763=CARTESIAN_POINT('Ctrl Pts',(17.2588399401465,-14.7653016697591,
12.));
#188764=CARTESIAN_POINT('Ctrl Pts',(17.2653635155319,-14.7724113956731,
0.));
#188765=CARTESIAN_POINT('Ctrl Pts',(17.2653635155319,-14.7724113956731,
12.));
#188766=CARTESIAN_POINT('Ctrl Pts',(17.2720104735194,-14.7797069617804,
0.));
#188767=CARTESIAN_POINT('Ctrl Pts',(17.2720104735194,-14.7797069617804,
12.));
#188768=CARTESIAN_POINT('Ctrl Pts',(17.2787773704849,-14.787186553128,0.));
#188769=CARTESIAN_POINT('Ctrl Pts',(17.2787773704849,-14.787186553128,12.));
#188770=CARTESIAN_POINT('Ctrl Pts',(17.2856608733196,-14.7948484105249,
0.));
#188771=CARTESIAN_POINT('Ctrl Pts',(17.2856608733196,-14.7948484105249,
12.));
#188772=CARTESIAN_POINT('Ctrl Pts',(17.2926577496513,-14.8026908254276,
0.));
#188773=CARTESIAN_POINT('Ctrl Pts',(17.2926577496513,-14.8026908254276,
12.));
#188774=CARTESIAN_POINT('Ctrl Pts',(17.299764866148,-14.8107121391035,0.));
#188775=CARTESIAN_POINT('Ctrl Pts',(17.299764866148,-14.8107121391035,12.));
#188776=CARTESIAN_POINT('Ctrl Pts',(17.3069791853706,-14.8189107410162,
0.));
#188777=CARTESIAN_POINT('Ctrl Pts',(17.3069791853706,-14.8189107410162,
12.));
#188778=CARTESIAN_POINT('Ctrl Pts',(17.3142977632659,-14.8272850675379,
0.));
#188779=CARTESIAN_POINT('Ctrl Pts',(17.3142977632659,-14.8272850675379,
12.));
#188780=CARTESIAN_POINT('Ctrl Pts',(17.3217177462101,-14.8358336004197,
0.));
#188781=CARTESIAN_POINT('Ctrl Pts',(17.3217177462101,-14.8358336004197,
12.));
#188782=CARTESIAN_POINT('Ctrl Pts',(17.3292363662605,-14.8445548643508,
0.));
#188783=CARTESIAN_POINT('Ctrl Pts',(17.3292363662605,-14.8445548643508,
12.));
#188784=CARTESIAN_POINT('Ctrl Pts',(17.336850936485,-14.8534474245434,0.));
#188785=CARTESIAN_POINT('Ctrl Pts',(17.336850936485,-14.8534474245434,12.));
#188786=CARTESIAN_POINT('Ctrl Pts',(17.3445588463474,-14.8625098843417,
0.));
#188787=CARTESIAN_POINT('Ctrl Pts',(17.3445588463474,-14.8625098843417,
12.));
#188788=CARTESIAN_POINT('Ctrl Pts',(17.3523575568645,-14.8717408826956,
0.));
#188789=CARTESIAN_POINT('Ctrl Pts',(17.3523575568645,-14.8717408826956,
12.));
#188790=CARTESIAN_POINT('Ctrl Pts',(17.3602445978161,-14.8811390927423,
0.));
#188791=CARTESIAN_POINT('Ctrl Pts',(17.3602445978161,-14.8811390927423,
12.));
#188792=CARTESIAN_POINT('Ctrl Pts',(17.3682175653235,-14.8907032205788,
0.));
#188793=CARTESIAN_POINT('Ctrl Pts',(17.3682175653235,-14.8907032205788,
12.));
#188794=CARTESIAN_POINT('Ctrl Pts',(17.3762741193076,-14.900432003961,0.));
#188795=CARTESIAN_POINT('Ctrl Pts',(17.3762741193076,-14.900432003961,12.));
#188796=CARTESIAN_POINT('Ctrl Pts',(17.3844119809824,-14.9103242110057,
0.));
#188797=CARTESIAN_POINT('Ctrl Pts',(17.3844119809824,-14.9103242110057,
12.));
#188798=CARTESIAN_POINT('Ctrl Pts',(17.3926289303986,-14.9203786389342,
0.));
#188799=CARTESIAN_POINT('Ctrl Pts',(17.3926289303986,-14.9203786389342,
12.));
#188800=CARTESIAN_POINT('Ctrl Pts',(17.4009228040749,-14.9305941128757,
0.));
#188801=CARTESIAN_POINT('Ctrl Pts',(17.4009228040749,-14.9305941128757,
12.));
#188802=CARTESIAN_POINT('Ctrl Pts',(17.4092914926071,-14.940969484645,0.));
#188803=CARTESIAN_POINT('Ctrl Pts',(17.4092914926071,-14.940969484645,12.));
#188804=CARTESIAN_POINT('Ctrl Pts',(17.4177329382828,-14.9515036315143,
0.));
#188805=CARTESIAN_POINT('Ctrl Pts',(17.4177329382828,-14.9515036315143,
12.));
#188806=CARTESIAN_POINT('Ctrl Pts',(17.426245132709,-14.9621954549827,0.));
#188807=CARTESIAN_POINT('Ctrl Pts',(17.426245132709,-14.9621954549827,12.));
#188808=CARTESIAN_POINT('Ctrl Pts',(17.4348261151396,-14.9730438799452,
0.));
#188809=CARTESIAN_POINT('Ctrl Pts',(17.4348261151396,-14.9730438799452,
12.));
#188810=CARTESIAN_POINT('Ctrl Pts',(17.4434739707773,-14.9840478538358,
0.));
#188811=CARTESIAN_POINT('Ctrl Pts',(17.4434739707773,-14.9840478538358,
12.));
#188812=CARTESIAN_POINT('Ctrl Pts',(17.4521868291004,-14.9952063457778,
0.));
#188813=CARTESIAN_POINT('Ctrl Pts',(17.4521868291004,-14.9952063457778,
12.));
#188814=CARTESIAN_POINT('Ctrl Pts',(17.4609628621418,-15.0065183456921,
0.));
#188815=CARTESIAN_POINT('Ctrl Pts',(17.4609628621418,-15.0065183456921,
12.));
#188816=CARTESIAN_POINT('Ctrl Pts',(17.4698002829357,-15.0179828635086,
0.));
#188817=CARTESIAN_POINT('Ctrl Pts',(17.4698002829357,-15.0179828635086,
12.));
#188818=CARTESIAN_POINT('Ctrl Pts',(17.4786973441417,-15.029598928488,0.));
#188819=CARTESIAN_POINT('Ctrl Pts',(17.4786973441417,-15.029598928488,12.));
#188820=CARTESIAN_POINT('Ctrl Pts',(17.4876523366178,-15.0413655884993,
0.));
#188821=CARTESIAN_POINT('Ctrl Pts',(17.4876523366178,-15.0413655884993,
12.));
#188822=CARTESIAN_POINT('Ctrl Pts',(17.4966635880245,-15.0532819093085,
0.));
#188823=CARTESIAN_POINT('Ctrl Pts',(17.4966635880245,-15.0532819093085,
12.));
#188824=CARTESIAN_POINT('Ctrl Pts',(17.5057294613874,-15.0653469738306,
0.));
#188825=CARTESIAN_POINT('Ctrl Pts',(17.5057294613874,-15.0653469738306,
12.));
#188826=CARTESIAN_POINT('Ctrl Pts',(17.5148483539683,-15.0775598815748,
0.));
#188827=CARTESIAN_POINT('Ctrl Pts',(17.5148483539683,-15.0775598815748,
12.));
#188828=CARTESIAN_POINT('Ctrl Pts',(17.5240186961788,-15.0899197481082,
0.));
#188829=CARTESIAN_POINT('Ctrl Pts',(17.5240186961788,-15.0899197481082,
12.));
#188830=CARTESIAN_POINT('Ctrl Pts',(17.5332389504829,-15.1024257045033,
0.));
#188831=CARTESIAN_POINT('Ctrl Pts',(17.5332389504829,-15.1024257045033,
12.));
#188832=CARTESIAN_POINT('Ctrl Pts',(17.5425076102966,-15.1150768967729,
0.));
#188833=CARTESIAN_POINT('Ctrl Pts',(17.5425076102966,-15.1150768967729,
12.));
#188834=CARTESIAN_POINT('Ctrl Pts',(17.5518231989122,-15.127872485314,0.));
#188835=CARTESIAN_POINT('Ctrl Pts',(17.5518231989122,-15.127872485314,12.));
#188836=CARTESIAN_POINT('Ctrl Pts',(17.5611842686196,-15.1408116444877,
0.));
#188837=CARTESIAN_POINT('Ctrl Pts',(17.5611842686196,-15.1408116444877,
12.));
#188838=CARTESIAN_POINT('Ctrl Pts',(17.570589399803,-15.1538935621715,0.));
#188839=CARTESIAN_POINT('Ctrl Pts',(17.570589399803,-15.1538935621715,12.));
#188840=CARTESIAN_POINT('Ctrl Pts',(17.5800372000539,-15.1671174393136,
0.));
#188841=CARTESIAN_POINT('Ctrl Pts',(17.5800372000539,-15.1671174393136,
12.));
#188842=CARTESIAN_POINT('Ctrl Pts',(17.5895263032592,-15.1804824894605,
0.));
#188843=CARTESIAN_POINT('Ctrl Pts',(17.5895263032592,-15.1804824894605,
12.));
#188844=CARTESIAN_POINT('Ctrl Pts',(17.5990553687595,-15.1939879383268,
0.));
#188845=CARTESIAN_POINT('Ctrl Pts',(17.5990553687595,-15.1939879383268,
12.));
#188846=CARTESIAN_POINT('Ctrl Pts',(17.6086230806497,-15.2076330234686,
0.));
#188847=CARTESIAN_POINT('Ctrl Pts',(17.6086230806497,-15.2076330234686,
12.));
#188848=CARTESIAN_POINT('Ctrl Pts',(17.6182281470467,-15.22141699392,0.));
#188849=CARTESIAN_POINT('Ctrl Pts',(17.6182281470467,-15.22141699392,12.));
#188850=CARTESIAN_POINT('Ctrl Pts',(17.6278692993765,-15.2353391098367,
0.));
#188851=CARTESIAN_POINT('Ctrl Pts',(17.6278692993765,-15.2353391098367,
12.));
#188852=CARTESIAN_POINT('Ctrl Pts',(17.637545291637,-15.2493986421091,0.));
#188853=CARTESIAN_POINT('Ctrl Pts',(17.637545291637,-15.2493986421091,12.));
#188854=CARTESIAN_POINT('Ctrl Pts',(17.6472548997329,-15.263594872029,0.));
#188855=CARTESIAN_POINT('Ctrl Pts',(17.6472548997329,-15.263594872029,12.));
#188856=CARTESIAN_POINT('Ctrl Pts',(17.6569969209,-15.2779270910238,0.));
#188857=CARTESIAN_POINT('Ctrl Pts',(17.6569969209,-15.2779270910238,12.));
#188858=CARTESIAN_POINT('Ctrl Pts',(17.6667701731041,-15.2923946003598,
0.));
#188859=CARTESIAN_POINT('Ctrl Pts',(17.6667701731041,-15.2923946003598,
12.));
#188860=CARTESIAN_POINT('Ctrl Pts',(17.6765734944559,-15.3069967108501,
0.));
#188861=CARTESIAN_POINT('Ctrl Pts',(17.6765734944559,-15.3069967108501,
12.));
#188862=CARTESIAN_POINT('Ctrl Pts',(17.6864057426052,-15.3217327425341,
0.));
#188863=CARTESIAN_POINT('Ctrl Pts',(17.6864057426052,-15.3217327425341,
12.));
#188864=CARTESIAN_POINT('Ctrl Pts',(17.6962657941984,-15.3366020244069,
0.));
#188865=CARTESIAN_POINT('Ctrl Pts',(17.6962657941984,-15.3366020244069,
12.));
#188866=CARTESIAN_POINT('Ctrl Pts',(17.7061525444044,-15.3516038942064,
0.));
#188867=CARTESIAN_POINT('Ctrl Pts',(17.7061525444044,-15.3516038942064,
12.));
#188868=CARTESIAN_POINT('Ctrl Pts',(17.7160649064208,-15.3667376981702,
0.));
#188869=CARTESIAN_POINT('Ctrl Pts',(17.7160649064208,-15.3667376981702,
12.));
#188870=CARTESIAN_POINT('Ctrl Pts',(17.7260018109923,-15.3820027907965,
0.));
#188871=CARTESIAN_POINT('Ctrl Pts',(17.7260018109923,-15.3820027907965,
12.));
#188872=CARTESIAN_POINT('Ctrl Pts',(17.7359622059143,-15.3973985345796,
0.));
#188873=CARTESIAN_POINT('Ctrl Pts',(17.7359622059143,-15.3973985345796,
12.));
#188874=CARTESIAN_POINT('Ctrl Pts',(17.7459450555803,-15.4129242997828,
0.));
#188875=CARTESIAN_POINT('Ctrl Pts',(17.7459450555803,-15.4129242997828,
12.));
#188876=CARTESIAN_POINT('Ctrl Pts',(17.7559493405871,-15.4285794642658,
0.));
#188877=CARTESIAN_POINT('Ctrl Pts',(17.7559493405871,-15.4285794642658,
12.));
#188878=CARTESIAN_POINT('Ctrl Pts',(17.765974057326,-15.4443634132865,0.));
#188879=CARTESIAN_POINT('Ctrl Pts',(17.765974057326,-15.4443634132865,12.));
#188880=CARTESIAN_POINT('Ctrl Pts',(17.7760182175817,-15.4602755393019,
0.));
#188881=CARTESIAN_POINT('Ctrl Pts',(17.7760182175817,-15.4602755393019,
12.));
#188882=CARTESIAN_POINT('Ctrl Pts',(17.7860808481229,-15.4763152417506,
0.));
#188883=CARTESIAN_POINT('Ctrl Pts',(17.7860808481229,-15.4763152417506,
12.));
#188884=CARTESIAN_POINT('Ctrl Pts',(17.7961609903161,-15.4924819268529,
0.));
#188885=CARTESIAN_POINT('Ctrl Pts',(17.7961609903161,-15.4924819268529,
12.));
#188886=CARTESIAN_POINT('Ctrl Pts',(17.8062576997964,-15.5087750074728,
0.));
#188887=CARTESIAN_POINT('Ctrl Pts',(17.8062576997964,-15.5087750074728,
12.));
#188888=CARTESIAN_POINT('Ctrl Pts',(17.8163700461263,-15.5251939029558,
0.));
#188889=CARTESIAN_POINT('Ctrl Pts',(17.8163700461263,-15.5251939029558,
12.));
#188890=CARTESIAN_POINT('Ctrl Pts',(17.8264971124606,-15.5417380389639,
0.));
#188891=CARTESIAN_POINT('Ctrl Pts',(17.8264971124606,-15.5417380389639,
12.));
#188892=CARTESIAN_POINT('Ctrl Pts',(17.8366379952078,-15.5584068472976,
0.));
#188893=CARTESIAN_POINT('Ctrl Pts',(17.8366379952078,-15.5584068472976,
12.));
#188894=CARTESIAN_POINT('Ctrl Pts',(17.8467918036976,-15.5751997657153,
0.));
#188895=CARTESIAN_POINT('Ctrl Pts',(17.8467918036976,-15.5751997657153,
12.));
#188896=CARTESIAN_POINT('Ctrl Pts',(17.8569576598996,-15.5921162378183,
0.));
#188897=CARTESIAN_POINT('Ctrl Pts',(17.8569576598996,-15.5921162378183,
12.));
#188898=CARTESIAN_POINT('Ctrl Pts',(17.8671346981388,-15.6091557129205,
0.));
#188899=CARTESIAN_POINT('Ctrl Pts',(17.8671346981388,-15.6091557129205,
12.));
#188900=CARTESIAN_POINT('Ctrl Pts',(17.8773220648125,-15.6263176459107,
0.));
#188901=CARTESIAN_POINT('Ctrl Pts',(17.8773220648125,-15.6263176459107,
12.));
#188902=CARTESIAN_POINT('Ctrl Pts',(17.8875189181095,-15.6436014971088,
0.));
#188903=CARTESIAN_POINT('Ctrl Pts',(17.8875189181095,-15.6436014971088,
12.));
#188904=CARTESIAN_POINT('Ctrl Pts',(17.8977244277247,-15.6610067321036,
0.));
#188905=CARTESIAN_POINT('Ctrl Pts',(17.8977244277247,-15.6610067321036,
12.));
#188906=CARTESIAN_POINT('Ctrl Pts',(17.9079377746118,-15.6785328216467,
0.));
#188907=CARTESIAN_POINT('Ctrl Pts',(17.9079377746118,-15.6785328216467,
12.));
#188908=CARTESIAN_POINT('Ctrl Pts',(17.918158150746,-15.6961792415526,0.));
#188909=CARTESIAN_POINT('Ctrl Pts',(17.918158150746,-15.6961792415526,12.));
#188910=CARTESIAN_POINT('Ctrl Pts',(17.9283847588837,-15.713945472584,0.));
#188911=CARTESIAN_POINT('Ctrl Pts',(17.9283847588837,-15.713945472584,12.));
#188912=CARTESIAN_POINT('Ctrl Pts',(17.9386168123261,-15.7318310003334,
0.));
#188913=CARTESIAN_POINT('Ctrl Pts',(17.9386168123261,-15.7318310003334,
12.));
#188914=CARTESIAN_POINT('Ctrl Pts',(17.9488535346776,-15.7498353150856,
0.));
#188915=CARTESIAN_POINT('Ctrl Pts',(17.9488535346776,-15.7498353150856,
12.));
#188916=CARTESIAN_POINT('Ctrl Pts',(17.9590941596236,-15.7679579117072,
0.));
#188917=CARTESIAN_POINT('Ctrl Pts',(17.9590941596236,-15.7679579117072,
12.));
#188918=CARTESIAN_POINT('Ctrl Pts',(17.9693379307297,-15.786198289572,0.));
#188919=CARTESIAN_POINT('Ctrl Pts',(17.9693379307297,-15.786198289572,12.));
#188920=CARTESIAN_POINT('Ctrl Pts',(17.9795841012383,-15.8045559524674,
0.));
#188921=CARTESIAN_POINT('Ctrl Pts',(17.9795841012383,-15.8045559524674,
12.));
#188922=CARTESIAN_POINT('Ctrl Pts',(17.9898319338664,-15.8230304084963,
0.));
#188923=CARTESIAN_POINT('Ctrl Pts',(17.9898319338664,-15.8230304084963,
12.));
#188924=CARTESIAN_POINT('Ctrl Pts',(18.0000807006055,-15.8416211699682,
0.));
#188925=CARTESIAN_POINT('Ctrl Pts',(18.0000807006055,-15.8416211699682,
12.));
#188926=CARTESIAN_POINT('Ctrl Pts',(18.010329682521,-15.8603277532834,0.));
#188927=CARTESIAN_POINT('Ctrl Pts',(18.010329682521,-15.8603277532834,12.));
#188928=CARTESIAN_POINT('Ctrl Pts',(18.0205781695773,-15.8791496788685,
0.));
#188929=CARTESIAN_POINT('Ctrl Pts',(18.0205781695773,-15.8791496788685,
12.));
#188930=CARTESIAN_POINT('Ctrl Pts',(18.0308254604638,-15.8980864711043,
0.));
#188931=CARTESIAN_POINT('Ctrl Pts',(18.0308254604638,-15.8980864711043,
12.));
#188932=CARTESIAN_POINT('Ctrl Pts',(18.0410708624208,-15.9171376582436,
0.));
#188933=CARTESIAN_POINT('Ctrl Pts',(18.0410708624208,-15.9171376582436,
12.));
#188934=CARTESIAN_POINT('Ctrl Pts',(18.0513136910691,-15.9363027723244,
0.));
#188935=CARTESIAN_POINT('Ctrl Pts',(18.0513136910691,-15.9363027723244,
12.));
#188936=CARTESIAN_POINT('Ctrl Pts',(18.061553270236,-15.9555813490645,0.));
#188937=CARTESIAN_POINT('Ctrl Pts',(18.061553270236,-15.9555813490645,12.));
#188938=CARTESIAN_POINT('Ctrl Pts',(18.071788931796,-15.9749729277848,0.));
#188939=CARTESIAN_POINT('Ctrl Pts',(18.071788931796,-15.9749729277848,12.));
#188940=CARTESIAN_POINT('Ctrl Pts',(18.0820200155239,-15.9944770513616,
0.));
#188941=CARTESIAN_POINT('Ctrl Pts',(18.0820200155239,-15.9944770513616,
12.));
#188942=CARTESIAN_POINT('Ctrl Pts',(18.0922458689464,-16.0140932661612,
0.));
#188943=CARTESIAN_POINT('Ctrl Pts',(18.0922458689464,-16.0140932661612,
12.));
#188944=CARTESIAN_POINT('Ctrl Pts',(18.1024658471966,-16.0338211219694,
0.));
#188945=CARTESIAN_POINT('Ctrl Pts',(18.1024658471966,-16.0338211219694,
12.));
#188946=CARTESIAN_POINT('Ctrl Pts',(18.1126793128688,-16.0536601719124,
0.));
#188947=CARTESIAN_POINT('Ctrl Pts',(18.1126793128688,-16.0536601719124,
12.));
#188948=CARTESIAN_POINT('Ctrl Pts',(18.1228856358746,-16.0736099723664,
0.));
#188949=CARTESIAN_POINT('Ctrl Pts',(18.1228856358746,-16.0736099723664,
12.));
#188950=CARTESIAN_POINT('Ctrl Pts',(18.1330841933099,-16.0936700829108,
0.));
#188951=CARTESIAN_POINT('Ctrl Pts',(18.1330841933099,-16.0936700829108,
12.));
#188952=CARTESIAN_POINT('Ctrl Pts',(18.1432743693231,-16.113840066279,0.));
#188953=CARTESIAN_POINT('Ctrl Pts',(18.1432743693231,-16.113840066279,12.));
#188954=CARTESIAN_POINT('Ctrl Pts',(18.153455554985,-16.1341194882987,0.));
#188955=CARTESIAN_POINT('Ctrl Pts',(18.153455554985,-16.1341194882987,12.));
#188956=CARTESIAN_POINT('Ctrl Pts',(18.1636271481616,-16.1545079178261,
0.));
#188957=CARTESIAN_POINT('Ctrl Pts',(18.1636271481616,-16.1545079178261,
12.));
#188958=CARTESIAN_POINT('Ctrl Pts',(18.1737885533852,-16.1750049266673,
0.));
#188959=CARTESIAN_POINT('Ctrl Pts',(18.1737885533852,-16.1750049266673,
12.));
#188960=CARTESIAN_POINT('Ctrl Pts',(18.1839391817335,-16.1956100895076,
0.));
#188961=CARTESIAN_POINT('Ctrl Pts',(18.1839391817335,-16.1956100895076,
12.));
#188962=CARTESIAN_POINT('Ctrl Pts',(18.1940784507232,-16.2163229838878,
0.));
#188963=CARTESIAN_POINT('Ctrl Pts',(18.1940784507232,-16.2163229838878,
12.));
#188964=CARTESIAN_POINT('Ctrl Pts',(18.2042057842037,-16.237143190164,0.));
#188965=CARTESIAN_POINT('Ctrl Pts',(18.2042057842037,-16.237143190164,12.));
#188966=CARTESIAN_POINT('Ctrl Pts',(18.214320612253,-16.2580702914615,0.));
#188967=CARTESIAN_POINT('Ctrl Pts',(18.214320612253,-16.2580702914615,12.));
#188968=CARTESIAN_POINT('Ctrl Pts',(18.2244223710745,-16.2791038736223,
0.));
#188969=CARTESIAN_POINT('Ctrl Pts',(18.2244223710745,-16.2791038736223,
12.));
#188970=CARTESIAN_POINT('Ctrl Pts',(18.2345105028981,-16.3002435251378,
0.));
#188971=CARTESIAN_POINT('Ctrl Pts',(18.2345105028981,-16.3002435251378,
12.));
#188972=CARTESIAN_POINT('Ctrl Pts',(18.2445844558742,-16.3214888370988,
0.));
#188973=CARTESIAN_POINT('Ctrl Pts',(18.2445844558742,-16.3214888370988,
12.));
#188974=CARTESIAN_POINT('Ctrl Pts',(18.2546436839609,-16.342839403159,0.));
#188975=CARTESIAN_POINT('Ctrl Pts',(18.2546436839609,-16.342839403159,12.));
#188976=CARTESIAN_POINT('Ctrl Pts',(18.2646876468169,-16.3642948194869,
0.));
#188977=CARTESIAN_POINT('Ctrl Pts',(18.2646876468169,-16.3642948194869,
12.));
#188978=CARTESIAN_POINT('Ctrl Pts',(18.2747158096934,-16.385854684708,0.));
#188979=CARTESIAN_POINT('Ctrl Pts',(18.2747158096934,-16.385854684708,12.));
#188980=CARTESIAN_POINT('Ctrl Pts',(18.2847276433308,-16.4075185998454,
0.));
#188981=CARTESIAN_POINT('Ctrl Pts',(18.2847276433308,-16.4075185998454,
12.));
#188982=CARTESIAN_POINT('Ctrl Pts',(18.2947226238509,-16.4292861682377,
0.));
#188983=CARTESIAN_POINT('Ctrl Pts',(18.2947226238509,-16.4292861682377,
12.));
#188984=CARTESIAN_POINT('Ctrl Pts',(18.3047002326858,-16.4511569955231,
0.));
#188985=CARTESIAN_POINT('Ctrl Pts',(18.3047002326858,-16.4511569955231,
12.));
#188986=CARTESIAN_POINT('Ctrl Pts',(18.3146599565229,-16.4731306896439,
0.));
#188987=CARTESIAN_POINT('Ctrl Pts',(18.3146599565229,-16.4731306896439,
12.));
#188988=CARTESIAN_POINT('Ctrl Pts',(18.3246012872468,-16.4952068608344,
0.));
#188989=CARTESIAN_POINT('Ctrl Pts',(18.3246012872468,-16.4952068608344,
12.));
#188990=CARTESIAN_POINT('Ctrl Pts',(18.3345237218864,-16.5173851216045,
0.));
#188991=CARTESIAN_POINT('Ctrl Pts',(18.3345237218864,-16.5173851216045,
12.));
#188992=CARTESIAN_POINT('Ctrl Pts',(18.3444267625601,-16.5396650867139,
0.));
#188993=CARTESIAN_POINT('Ctrl Pts',(18.3444267625601,-16.5396650867139,
12.));
#188994=CARTESIAN_POINT('Ctrl Pts',(18.3543099164331,-16.5620463731414,
0.));
#188995=CARTESIAN_POINT('Ctrl Pts',(18.3543099164331,-16.5620463731414,
12.));
#188996=CARTESIAN_POINT('Ctrl Pts',(18.364172695589,-16.5845286000218,0.));
#188997=CARTESIAN_POINT('Ctrl Pts',(18.364172695589,-16.5845286000218,12.));
#188998=CARTESIAN_POINT('Ctrl Pts',(18.3740146168879,-16.6071113885711,
0.));
#188999=CARTESIAN_POINT('Ctrl Pts',(18.3740146168879,-16.6071113885711,
12.));
#189000=CARTESIAN_POINT('Ctrl Pts',(18.3838352018327,-16.6297943620056,
0.));
#189001=CARTESIAN_POINT('Ctrl Pts',(18.3838352018327,-16.6297943620056,
12.));
#189002=CARTESIAN_POINT('Ctrl Pts',(18.3936339764332,-16.6525771454513,
0.));
#189003=CARTESIAN_POINT('Ctrl Pts',(18.3936339764332,-16.6525771454513,
12.));
#189004=CARTESIAN_POINT('Ctrl Pts',(18.4034104710789,-16.6754593658513,
0.));
#189005=CARTESIAN_POINT('Ctrl Pts',(18.4034104710789,-16.6754593658513,
12.));
#189006=CARTESIAN_POINT('Ctrl Pts',(18.4131642203989,-16.698440651849,0.));
#189007=CARTESIAN_POINT('Ctrl Pts',(18.4131642203989,-16.698440651849,12.));
#189008=CARTESIAN_POINT('Ctrl Pts',(18.4228947633186,-16.7215206338818,
0.));
#189009=CARTESIAN_POINT('Ctrl Pts',(18.4228947633186,-16.7215206338818,
12.));
#189010=CARTESIAN_POINT('Ctrl Pts',(18.4326016431392,-16.7446989442882,
0.));
#189011=CARTESIAN_POINT('Ctrl Pts',(18.4326016431392,-16.7446989442882,
12.));
#189012=CARTESIAN_POINT('Ctrl Pts',(18.4422844076099,-16.7679752173992,
0.));
#189013=CARTESIAN_POINT('Ctrl Pts',(18.4422844076099,-16.7679752173992,
12.));
#189014=CARTESIAN_POINT('Ctrl Pts',(18.4519426090124,-16.791349089629,0.));
#189015=CARTESIAN_POINT('Ctrl Pts',(18.4519426090124,-16.791349089629,12.));
#189016=CARTESIAN_POINT('Ctrl Pts',(18.4615758042305,-16.8148201995472,
0.));
#189017=CARTESIAN_POINT('Ctrl Pts',(18.4615758042305,-16.8148201995472,
12.));
#189018=CARTESIAN_POINT('Ctrl Pts',(18.4711835548622,-16.8383881879707,
0.));
#189019=CARTESIAN_POINT('Ctrl Pts',(18.4711835548622,-16.8383881879707,
12.));
#189020=CARTESIAN_POINT('Ctrl Pts',(18.4807654268769,-16.8620526977169,
0.));
#189021=CARTESIAN_POINT('Ctrl Pts',(18.4807654268769,-16.8620526977169,
12.));
#189022=CARTESIAN_POINT('Ctrl Pts',(18.4903209902226,-16.8858133733086,
0.));
#189023=CARTESIAN_POINT('Ctrl Pts',(18.4903209902226,-16.8858133733086,
12.));
#189024=CARTESIAN_POINT('Ctrl Pts',(18.4998498184619,-16.9096698606942,
0.));
#189025=CARTESIAN_POINT('Ctrl Pts',(18.4998498184619,-16.9096698606942,
12.));
#189026=CARTESIAN_POINT('Ctrl Pts',(18.5093514883835,-16.9336218069353,
0.));
#189027=CARTESIAN_POINT('Ctrl Pts',(18.5093514883835,-16.9336218069353,
12.));
#189028=CARTESIAN_POINT('Ctrl Pts',(18.518825579666,-16.957668859934,0.));
#189029=CARTESIAN_POINT('Ctrl Pts',(18.518825579666,-16.957668859934,12.));
#189030=CARTESIAN_POINT('Ctrl Pts',(18.5282716744198,-16.9818106680382,
0.));
#189031=CARTESIAN_POINT('Ctrl Pts',(18.5282716744198,-16.9818106680382,
12.));
#189032=CARTESIAN_POINT('Ctrl Pts',(18.5376893576961,-17.0060468805099,
0.));
#189033=CARTESIAN_POINT('Ctrl Pts',(18.5376893576961,-17.0060468805099,
12.));
#189034=CARTESIAN_POINT('Ctrl Pts',(18.5470782182089,-17.030377148174,0.));
#189035=CARTESIAN_POINT('Ctrl Pts',(18.5470782182089,-17.030377148174,12.));
#189036=CARTESIAN_POINT('Ctrl Pts',(18.5564378489628,-17.0548011239751,
0.));
#189037=CARTESIAN_POINT('Ctrl Pts',(18.5564378489628,-17.0548011239751,
12.));
#189038=CARTESIAN_POINT('Ctrl Pts',(18.5657678479788,-17.0793184636079,
0.));
#189039=CARTESIAN_POINT('Ctrl Pts',(18.5657678479788,-17.0793184636079,
12.));
#189040=CARTESIAN_POINT('Ctrl Pts',(18.5750678188543,-17.1039288260002,
0.));
#189041=CARTESIAN_POINT('Ctrl Pts',(18.5750678188543,-17.1039288260002,
12.));
#189042=CARTESIAN_POINT('Ctrl Pts',(18.5843373717253,-17.1286318741185,
0.));
#189043=CARTESIAN_POINT('Ctrl Pts',(18.5843373717253,-17.1286318741185,
12.));
#189044=CARTESIAN_POINT('Ctrl Pts',(18.5935761222833,-17.1534272741646,
0.));
#189045=CARTESIAN_POINT('Ctrl Pts',(18.5935761222833,-17.1534272741646,
12.));
#189046=CARTESIAN_POINT('Ctrl Pts',(18.6027836898826,-17.1783146940131,
0.));
#189047=CARTESIAN_POINT('Ctrl Pts',(18.6027836898826,-17.1783146940131,
12.));
#189048=CARTESIAN_POINT('Ctrl Pts',(18.6119596959957,-17.2032938019288,
0.));
#189049=CARTESIAN_POINT('Ctrl Pts',(18.6119596959957,-17.2032938019288,
12.));
#189050=CARTESIAN_POINT('Ctrl Pts',(18.6211037624041,-17.2283642650519,
0.));
#189051=CARTESIAN_POINT('Ctrl Pts',(18.6211037624041,-17.2283642650519,
12.));
#189052=CARTESIAN_POINT('Ctrl Pts',(18.630215509794,-17.2535257482186,0.));
#189053=CARTESIAN_POINT('Ctrl Pts',(18.630215509794,-17.2535257482186,12.));
#189054=CARTESIAN_POINT('Ctrl Pts',(18.639294555474,-17.278777912021,0.));
#189055=CARTESIAN_POINT('Ctrl Pts',(18.639294555474,-17.278777912021,12.));
#189056=CARTESIAN_POINT('Ctrl Pts',(18.6483405141853,-17.3041204135069,
0.));
#189057=CARTESIAN_POINT('Ctrl Pts',(18.6483405141853,-17.3041204135069,
12.));
#189058=CARTESIAN_POINT('Ctrl Pts',(18.6573530024019,-17.3295529098612,
0.));
#189059=CARTESIAN_POINT('Ctrl Pts',(18.6573530024019,-17.3295529098612,
12.));
#189060=CARTESIAN_POINT('Ctrl Pts',(18.6663316416569,-17.3550750612438,
0.));
#189061=CARTESIAN_POINT('Ctrl Pts',(18.6663316416569,-17.3550750612438,
12.));
#189062=CARTESIAN_POINT('Ctrl Pts',(18.6752760624045,-17.3806865340744,
0.));
#189063=CARTESIAN_POINT('Ctrl Pts',(18.6752760624045,-17.3806865340744,
12.));
#189064=CARTESIAN_POINT('Ctrl Pts',(18.6841859073472,-17.4063870038563,
0.));
#189065=CARTESIAN_POINT('Ctrl Pts',(18.6841859073472,-17.4063870038563,
12.));
#189066=CARTESIAN_POINT('Ctrl Pts',(18.6930608357421,-17.4321761588148,
0.));
#189067=CARTESIAN_POINT('Ctrl Pts',(18.6930608357421,-17.4321761588148,
12.));
#189068=CARTESIAN_POINT('Ctrl Pts',(18.7019005250322,-17.4580537012764,
0.));
#189069=CARTESIAN_POINT('Ctrl Pts',(18.7019005250322,-17.4580537012764,
12.));
#189070=CARTESIAN_POINT('Ctrl Pts',(18.7107046613941,-17.4840193397176,
0.));
#189071=CARTESIAN_POINT('Ctrl Pts',(18.7107046613941,-17.4840193397176,
12.));
#189072=CARTESIAN_POINT('Ctrl Pts',(18.7194729318127,-17.5100727820891,
0.));
#189073=CARTESIAN_POINT('Ctrl Pts',(18.7194729318127,-17.5100727820891,
12.));
#189074=CARTESIAN_POINT('Ctrl Pts',(18.728205015716,-17.5362137287604,0.));
#189075=CARTESIAN_POINT('Ctrl Pts',(18.728205015716,-17.5362137287604,12.));
#189076=CARTESIAN_POINT('Ctrl Pts',(18.7369005764558,-17.5624418653248,
0.));
#189077=CARTESIAN_POINT('Ctrl Pts',(18.7369005764558,-17.5624418653248,
12.));
#189078=CARTESIAN_POINT('Ctrl Pts',(18.7455592536667,-17.5887568561361,
0.));
#189079=CARTESIAN_POINT('Ctrl Pts',(18.7455592536667,-17.5887568561361,
12.));
#189080=CARTESIAN_POINT('Ctrl Pts',(18.7541806530935,-17.6151583356989,
0.));
#189081=CARTESIAN_POINT('Ctrl Pts',(18.7541806530935,-17.6151583356989,
12.));
#189082=CARTESIAN_POINT('Ctrl Pts',(18.7627643613139,-17.6416459210646,
0.));
#189083=CARTESIAN_POINT('Ctrl Pts',(18.7627643613139,-17.6416459210646,
12.));
#189084=CARTESIAN_POINT('Ctrl Pts',(18.7713099642673,-17.6682192274197,
0.));
#189085=CARTESIAN_POINT('Ctrl Pts',(18.7713099642673,-17.6682192274197,
12.));
#189086=CARTESIAN_POINT('Ctrl Pts',(18.7798170641305,-17.6948778822982,
0.));
#189087=CARTESIAN_POINT('Ctrl Pts',(18.7798170641305,-17.6948778822982,
12.));
#189088=CARTESIAN_POINT('Ctrl Pts',(18.7882852976016,-17.7216215409019,
0.));
#189089=CARTESIAN_POINT('Ctrl Pts',(18.7882852976016,-17.7216215409019,
12.));
#189090=CARTESIAN_POINT('Ctrl Pts',(18.7967143519444,-17.7484498996916,
0.));
#189091=CARTESIAN_POINT('Ctrl Pts',(18.7967143519444,-17.7484498996916,
12.));
#189092=CARTESIAN_POINT('Ctrl Pts',(18.8051039860543,-17.7753627137898,
0.));
#189093=CARTESIAN_POINT('Ctrl Pts',(18.8051039860543,-17.7753627137898,
12.));
#189094=CARTESIAN_POINT('Ctrl Pts',(18.8134540340581,-17.8023598011135,
0.));
#189095=CARTESIAN_POINT('Ctrl Pts',(18.8134540340581,-17.8023598011135,
12.));
#189096=CARTESIAN_POINT('Ctrl Pts',(18.8217643886368,-17.8294410311105,
0.));
#189097=CARTESIAN_POINT('Ctrl Pts',(18.8217643886368,-17.8294410311105,
12.));
#189098=CARTESIAN_POINT('Ctrl Pts',(18.8300349896187,-17.8566063174871,
0.));
#189099=CARTESIAN_POINT('Ctrl Pts',(18.8300349896187,-17.8566063174871,
12.));
#189100=CARTESIAN_POINT('Ctrl Pts',(18.8366196462746,-17.8784057509434,
0.));
#189101=CARTESIAN_POINT('Ctrl Pts',(18.8366196462746,-17.8784057509434,
12.));
#189102=CARTESIAN_POINT('Ctrl Pts',(18.8415402351882,-17.8947931177853,
0.));
#189103=CARTESIAN_POINT('Ctrl Pts',(18.8415402351882,-17.8947931177853,
12.));
#189104=CARTESIAN_POINT('Ctrl Pts',(18.8448126709726,-17.9057348246611,
0.));
#189105=CARTESIAN_POINT('Ctrl Pts',(18.8448126709726,-17.9057348246611,
12.));
#189106=CARTESIAN_POINT('Ctrl Pts',(18.8464468996588,-17.9112098770111,
0.));
#189107=CARTESIAN_POINT('Ctrl Pts',(18.8464468996588,-17.9112098770111,
12.));
#189108=CARTESIAN_POINT('',(18.8464468996588,-17.9112098770111,0.));
#189109=CARTESIAN_POINT('Ctrl Pts',(17.1452095830632,-14.6513681262571,
0.));
#189110=CARTESIAN_POINT('Ctrl Pts',(17.1452153999142,-14.6513711852843,
0.));
#189111=CARTESIAN_POINT('Ctrl Pts',(17.1452600887037,-14.6514066997196,
0.));
#189112=CARTESIAN_POINT('Ctrl Pts',(17.1454262858043,-14.6515481598068,
0.));
#189113=CARTESIAN_POINT('Ctrl Pts',(17.1458462295271,-14.6519131634508,
0.));
#189114=CARTESIAN_POINT('Ctrl Pts',(17.1466998098673,-14.6526624064978,
0.));
#189115=CARTESIAN_POINT('Ctrl Pts',(17.147876394491,-14.6537016966184,0.));
#189116=CARTESIAN_POINT('Ctrl Pts',(17.1493641837558,-14.655024862281,0.));
#189117=CARTESIAN_POINT('Ctrl Pts',(17.1511476869496,-14.6566237952435,
0.));
#189118=CARTESIAN_POINT('Ctrl Pts',(17.1532107762718,-14.6584900555302,
0.));
#189119=CARTESIAN_POINT('Ctrl Pts',(17.1555401986401,-14.6606167169642,
0.));
#189120=CARTESIAN_POINT('Ctrl Pts',(17.1581262646789,-14.6629987285992,
0.));
#189121=CARTESIAN_POINT('Ctrl Pts',(17.1609609517369,-14.6656319165057,
0.));
#189122=CARTESIAN_POINT('Ctrl Pts',(17.1640366762305,-14.6685123374423,
0.));
#189123=CARTESIAN_POINT('Ctrl Pts',(17.167344972302,-14.671635583332,0.));
#189124=CARTESIAN_POINT('Ctrl Pts',(17.1708771619129,-14.6749971333867,
0.));
#189125=CARTESIAN_POINT('Ctrl Pts',(17.1746247499057,-14.6785925615677,
0.));
#189126=CARTESIAN_POINT('Ctrl Pts',(17.1785800350826,-14.6824178576167,
0.));
#189127=CARTESIAN_POINT('Ctrl Pts',(17.182736158472,-14.686469452232,0.));
#189128=CARTESIAN_POINT('Ctrl Pts',(17.1870867909918,-14.6907440526958,
0.));
#189129=CARTESIAN_POINT('Ctrl Pts',(17.1916259308415,-14.6952385361706,
0.));
#189130=CARTESIAN_POINT('Ctrl Pts',(17.1963476411694,-14.699949811582,0.));
#189131=CARTESIAN_POINT('Ctrl Pts',(17.2012461084268,-14.7048748502663,
0.));
#189132=CARTESIAN_POINT('Ctrl Pts',(17.2063157097315,-14.7100107213586,
0.));
#189133=CARTESIAN_POINT('Ctrl Pts',(17.2115510835989,-14.7153546289339,
0.));
#189134=CARTESIAN_POINT('Ctrl Pts',(17.2169471814256,-14.7209039390327,
0.));
#189135=CARTESIAN_POINT('Ctrl Pts',(17.2224992099667,-14.7266561494282,
0.));
#189136=CARTESIAN_POINT('Ctrl Pts',(17.2282025904314,-14.7326088681163,
0.));
#189137=CARTESIAN_POINT('Ctrl Pts',(17.2340529062076,-14.7387597858117,
0.));
#189138=CARTESIAN_POINT('Ctrl Pts',(17.2400458713565,-14.7451066593792,
0.));
#189139=CARTESIAN_POINT('Ctrl Pts',(17.2461773413288,-14.7516473175124,
0.));
#189140=CARTESIAN_POINT('Ctrl Pts',(17.2524433146837,-14.7583796616617,
0.));
#189141=CARTESIAN_POINT('Ctrl Pts',(17.2588399401465,-14.7653016697591,
0.));
#189142=CARTESIAN_POINT('Ctrl Pts',(17.2653635155319,-14.7724113956731,
0.));
#189143=CARTESIAN_POINT('Ctrl Pts',(17.2720104735194,-14.7797069617804,
0.));
#189144=CARTESIAN_POINT('Ctrl Pts',(17.2787773704849,-14.787186553128,0.));
#189145=CARTESIAN_POINT('Ctrl Pts',(17.2856608733196,-14.7948484105249,
0.));
#189146=CARTESIAN_POINT('Ctrl Pts',(17.2926577496513,-14.8026908254276,
0.));
#189147=CARTESIAN_POINT('Ctrl Pts',(17.299764866148,-14.8107121391035,0.));
#189148=CARTESIAN_POINT('Ctrl Pts',(17.3069791853706,-14.8189107410162,
0.));
#189149=CARTESIAN_POINT('Ctrl Pts',(17.3142977632659,-14.8272850675379,
0.));
#189150=CARTESIAN_POINT('Ctrl Pts',(17.3217177462101,-14.8358336004197,
0.));
#189151=CARTESIAN_POINT('Ctrl Pts',(17.3292363662605,-14.8445548643508,
0.));
#189152=CARTESIAN_POINT('Ctrl Pts',(17.336850936485,-14.8534474245434,0.));
#189153=CARTESIAN_POINT('Ctrl Pts',(17.3445588463474,-14.8625098843417,
0.));
#189154=CARTESIAN_POINT('Ctrl Pts',(17.3523575568645,-14.8717408826956,
0.));
#189155=CARTESIAN_POINT('Ctrl Pts',(17.3602445978161,-14.8811390927423,
0.));
#189156=CARTESIAN_POINT('Ctrl Pts',(17.3682175653235,-14.8907032205788,
0.));
#189157=CARTESIAN_POINT('Ctrl Pts',(17.3762741193076,-14.900432003961,0.));
#189158=CARTESIAN_POINT('Ctrl Pts',(17.3844119809824,-14.9103242110057,
0.));
#189159=CARTESIAN_POINT('Ctrl Pts',(17.3926289303986,-14.9203786389342,
0.));
#189160=CARTESIAN_POINT('Ctrl Pts',(17.4009228040749,-14.9305941128757,
0.));
#189161=CARTESIAN_POINT('Ctrl Pts',(17.4092914926071,-14.940969484645,0.));
#189162=CARTESIAN_POINT('Ctrl Pts',(17.4177329382828,-14.9515036315143,
0.));
#189163=CARTESIAN_POINT('Ctrl Pts',(17.426245132709,-14.9621954549827,0.));
#189164=CARTESIAN_POINT('Ctrl Pts',(17.4348261151396,-14.9730438799452,
0.));
#189165=CARTESIAN_POINT('Ctrl Pts',(17.4434739707773,-14.9840478538358,
0.));
#189166=CARTESIAN_POINT('Ctrl Pts',(17.4521868291004,-14.9952063457778,
0.));
#189167=CARTESIAN_POINT('Ctrl Pts',(17.4609628621418,-15.0065183456921,
0.));
#189168=CARTESIAN_POINT('Ctrl Pts',(17.4698002829357,-15.0179828635086,
0.));
#189169=CARTESIAN_POINT('Ctrl Pts',(17.4786973441417,-15.029598928488,0.));
#189170=CARTESIAN_POINT('Ctrl Pts',(17.4876523366178,-15.0413655884993,
0.));
#189171=CARTESIAN_POINT('Ctrl Pts',(17.4966635880245,-15.0532819093085,
0.));
#189172=CARTESIAN_POINT('Ctrl Pts',(17.5057294613874,-15.0653469738306,
0.));
#189173=CARTESIAN_POINT('Ctrl Pts',(17.5148483539683,-15.0775598815748,
0.));
#189174=CARTESIAN_POINT('Ctrl Pts',(17.5240186961788,-15.0899197481082,
0.));
#189175=CARTESIAN_POINT('Ctrl Pts',(17.5332389504829,-15.1024257045033,
0.));
#189176=CARTESIAN_POINT('Ctrl Pts',(17.5425076102966,-15.1150768967729,
0.));
#189177=CARTESIAN_POINT('Ctrl Pts',(17.5518231989122,-15.127872485314,0.));
#189178=CARTESIAN_POINT('Ctrl Pts',(17.5611842686196,-15.1408116444877,
0.));
#189179=CARTESIAN_POINT('Ctrl Pts',(17.570589399803,-15.1538935621715,0.));
#189180=CARTESIAN_POINT('Ctrl Pts',(17.5800372000539,-15.1671174393136,
0.));
#189181=CARTESIAN_POINT('Ctrl Pts',(17.5895263032592,-15.1804824894605,
0.));
#189182=CARTESIAN_POINT('Ctrl Pts',(17.5990553687595,-15.1939879383268,
0.));
#189183=CARTESIAN_POINT('Ctrl Pts',(17.6086230806497,-15.2076330234686,
0.));
#189184=CARTESIAN_POINT('Ctrl Pts',(17.6182281470467,-15.22141699392,0.));
#189185=CARTESIAN_POINT('Ctrl Pts',(17.6278692993765,-15.2353391098367,
0.));
#189186=CARTESIAN_POINT('Ctrl Pts',(17.637545291637,-15.2493986421091,0.));
#189187=CARTESIAN_POINT('Ctrl Pts',(17.6472548997329,-15.263594872029,0.));
#189188=CARTESIAN_POINT('Ctrl Pts',(17.6569969209,-15.2779270910238,0.));
#189189=CARTESIAN_POINT('Ctrl Pts',(17.6667701731041,-15.2923946003598,
0.));
#189190=CARTESIAN_POINT('Ctrl Pts',(17.6765734944559,-15.3069967108501,
0.));
#189191=CARTESIAN_POINT('Ctrl Pts',(17.6864057426052,-15.3217327425341,
0.));
#189192=CARTESIAN_POINT('Ctrl Pts',(17.6962657941984,-15.3366020244069,
0.));
#189193=CARTESIAN_POINT('Ctrl Pts',(17.7061525444044,-15.3516038942064,
0.));
#189194=CARTESIAN_POINT('Ctrl Pts',(17.7160649064208,-15.3667376981702,
0.));
#189195=CARTESIAN_POINT('Ctrl Pts',(17.7260018109923,-15.3820027907965,
0.));
#189196=CARTESIAN_POINT('Ctrl Pts',(17.7359622059143,-15.3973985345796,
0.));
#189197=CARTESIAN_POINT('Ctrl Pts',(17.7459450555803,-15.4129242997828,
0.));
#189198=CARTESIAN_POINT('Ctrl Pts',(17.7559493405871,-15.4285794642658,
0.));
#189199=CARTESIAN_POINT('Ctrl Pts',(17.765974057326,-15.4443634132865,0.));
#189200=CARTESIAN_POINT('Ctrl Pts',(17.7760182175817,-15.4602755393019,
0.));
#189201=CARTESIAN_POINT('Ctrl Pts',(17.7860808481229,-15.4763152417506,
0.));
#189202=CARTESIAN_POINT('Ctrl Pts',(17.7961609903161,-15.4924819268529,
0.));
#189203=CARTESIAN_POINT('Ctrl Pts',(17.8062576997964,-15.5087750074728,
0.));
#189204=CARTESIAN_POINT('Ctrl Pts',(17.8163700461263,-15.5251939029558,
0.));
#189205=CARTESIAN_POINT('Ctrl Pts',(17.8264971124606,-15.5417380389639,
0.));
#189206=CARTESIAN_POINT('Ctrl Pts',(17.8366379952078,-15.5584068472976,
0.));
#189207=CARTESIAN_POINT('Ctrl Pts',(17.8467918036976,-15.5751997657153,
0.));
#189208=CARTESIAN_POINT('Ctrl Pts',(17.8569576598996,-15.5921162378183,
0.));
#189209=CARTESIAN_POINT('Ctrl Pts',(17.8671346981388,-15.6091557129205,
0.));
#189210=CARTESIAN_POINT('Ctrl Pts',(17.8773220648125,-15.6263176459107,
0.));
#189211=CARTESIAN_POINT('Ctrl Pts',(17.8875189181095,-15.6436014971088,
0.));
#189212=CARTESIAN_POINT('Ctrl Pts',(17.8977244277247,-15.6610067321036,
0.));
#189213=CARTESIAN_POINT('Ctrl Pts',(17.9079377746118,-15.6785328216467,
0.));
#189214=CARTESIAN_POINT('Ctrl Pts',(17.918158150746,-15.6961792415526,0.));
#189215=CARTESIAN_POINT('Ctrl Pts',(17.9283847588837,-15.713945472584,0.));
#189216=CARTESIAN_POINT('Ctrl Pts',(17.9386168123261,-15.7318310003334,
0.));
#189217=CARTESIAN_POINT('Ctrl Pts',(17.9488535346776,-15.7498353150856,
0.));
#189218=CARTESIAN_POINT('Ctrl Pts',(17.9590941596236,-15.7679579117072,
0.));
#189219=CARTESIAN_POINT('Ctrl Pts',(17.9693379307297,-15.786198289572,0.));
#189220=CARTESIAN_POINT('Ctrl Pts',(17.9795841012383,-15.8045559524674,
0.));
#189221=CARTESIAN_POINT('Ctrl Pts',(17.9898319338664,-15.8230304084963,
0.));
#189222=CARTESIAN_POINT('Ctrl Pts',(18.0000807006055,-15.8416211699682,
0.));
#189223=CARTESIAN_POINT('Ctrl Pts',(18.010329682521,-15.8603277532834,0.));
#189224=CARTESIAN_POINT('Ctrl Pts',(18.0205781695773,-15.8791496788685,
0.));
#189225=CARTESIAN_POINT('Ctrl Pts',(18.0308254604638,-15.8980864711043,
0.));
#189226=CARTESIAN_POINT('Ctrl Pts',(18.0410708624208,-15.9171376582436,
0.));
#189227=CARTESIAN_POINT('Ctrl Pts',(18.0513136910691,-15.9363027723244,
0.));
#189228=CARTESIAN_POINT('Ctrl Pts',(18.061553270236,-15.9555813490645,0.));
#189229=CARTESIAN_POINT('Ctrl Pts',(18.071788931796,-15.9749729277848,0.));
#189230=CARTESIAN_POINT('Ctrl Pts',(18.0820200155239,-15.9944770513616,
0.));
#189231=CARTESIAN_POINT('Ctrl Pts',(18.0922458689464,-16.0140932661612,
0.));
#189232=CARTESIAN_POINT('Ctrl Pts',(18.1024658471966,-16.0338211219694,
0.));
#189233=CARTESIAN_POINT('Ctrl Pts',(18.1126793128688,-16.0536601719124,
0.));
#189234=CARTESIAN_POINT('Ctrl Pts',(18.1228856358746,-16.0736099723664,
0.));
#189235=CARTESIAN_POINT('Ctrl Pts',(18.1330841933099,-16.0936700829108,
0.));
#189236=CARTESIAN_POINT('Ctrl Pts',(18.1432743693231,-16.113840066279,0.));
#189237=CARTESIAN_POINT('Ctrl Pts',(18.153455554985,-16.1341194882987,0.));
#189238=CARTESIAN_POINT('Ctrl Pts',(18.1636271481616,-16.1545079178261,
0.));
#189239=CARTESIAN_POINT('Ctrl Pts',(18.1737885533852,-16.1750049266673,
0.));
#189240=CARTESIAN_POINT('Ctrl Pts',(18.1839391817335,-16.1956100895076,
0.));
#189241=CARTESIAN_POINT('Ctrl Pts',(18.1940784507232,-16.2163229838878,
0.));
#189242=CARTESIAN_POINT('Ctrl Pts',(18.2042057842037,-16.237143190164,0.));
#189243=CARTESIAN_POINT('Ctrl Pts',(18.214320612253,-16.2580702914615,0.));
#189244=CARTESIAN_POINT('Ctrl Pts',(18.2244223710745,-16.2791038736223,
0.));
#189245=CARTESIAN_POINT('Ctrl Pts',(18.2345105028981,-16.3002435251378,
0.));
#189246=CARTESIAN_POINT('Ctrl Pts',(18.2445844558742,-16.3214888370988,
0.));
#189247=CARTESIAN_POINT('Ctrl Pts',(18.2546436839609,-16.342839403159,0.));
#189248=CARTESIAN_POINT('Ctrl Pts',(18.2646876468169,-16.3642948194869,
0.));
#189249=CARTESIAN_POINT('Ctrl Pts',(18.2747158096934,-16.385854684708,0.));
#189250=CARTESIAN_POINT('Ctrl Pts',(18.2847276433308,-16.4075185998454,
0.));
#189251=CARTESIAN_POINT('Ctrl Pts',(18.2947226238509,-16.4292861682377,
0.));
#189252=CARTESIAN_POINT('Ctrl Pts',(18.3047002326858,-16.4511569955231,
0.));
#189253=CARTESIAN_POINT('Ctrl Pts',(18.3146599565229,-16.4731306896439,
0.));
#189254=CARTESIAN_POINT('Ctrl Pts',(18.3246012872468,-16.4952068608344,
0.));
#189255=CARTESIAN_POINT('Ctrl Pts',(18.3345237218864,-16.5173851216045,
0.));
#189256=CARTESIAN_POINT('Ctrl Pts',(18.3444267625601,-16.5396650867139,
0.));
#189257=CARTESIAN_POINT('Ctrl Pts',(18.3543099164331,-16.5620463731414,
0.));
#189258=CARTESIAN_POINT('Ctrl Pts',(18.364172695589,-16.5845286000218,0.));
#189259=CARTESIAN_POINT('Ctrl Pts',(18.3740146168879,-16.6071113885711,
0.));
#189260=CARTESIAN_POINT('Ctrl Pts',(18.3838352018327,-16.6297943620056,
0.));
#189261=CARTESIAN_POINT('Ctrl Pts',(18.3936339764332,-16.6525771454513,
0.));
#189262=CARTESIAN_POINT('Ctrl Pts',(18.4034104710789,-16.6754593658513,
0.));
#189263=CARTESIAN_POINT('Ctrl Pts',(18.4131642203989,-16.698440651849,0.));
#189264=CARTESIAN_POINT('Ctrl Pts',(18.4228947633186,-16.7215206338818,
0.));
#189265=CARTESIAN_POINT('Ctrl Pts',(18.4326016431392,-16.7446989442882,
0.));
#189266=CARTESIAN_POINT('Ctrl Pts',(18.4422844076099,-16.7679752173992,
0.));
#189267=CARTESIAN_POINT('Ctrl Pts',(18.4519426090124,-16.791349089629,0.));
#189268=CARTESIAN_POINT('Ctrl Pts',(18.4615758042305,-16.8148201995472,
0.));
#189269=CARTESIAN_POINT('Ctrl Pts',(18.4711835548622,-16.8383881879707,
0.));
#189270=CARTESIAN_POINT('Ctrl Pts',(18.4807654268769,-16.8620526977169,
0.));
#189271=CARTESIAN_POINT('Ctrl Pts',(18.4903209902226,-16.8858133733086,
0.));
#189272=CARTESIAN_POINT('Ctrl Pts',(18.4998498184619,-16.9096698606942,
0.));
#189273=CARTESIAN_POINT('Ctrl Pts',(18.5093514883835,-16.9336218069353,
0.));
#189274=CARTESIAN_POINT('Ctrl Pts',(18.518825579666,-16.957668859934,0.));
#189275=CARTESIAN_POINT('Ctrl Pts',(18.5282716744198,-16.9818106680382,
0.));
#189276=CARTESIAN_POINT('Ctrl Pts',(18.5376893576961,-17.0060468805099,
0.));
#189277=CARTESIAN_POINT('Ctrl Pts',(18.5470782182089,-17.030377148174,0.));
#189278=CARTESIAN_POINT('Ctrl Pts',(18.5564378489628,-17.0548011239751,
0.));
#189279=CARTESIAN_POINT('Ctrl Pts',(18.5657678479788,-17.0793184636079,
0.));
#189280=CARTESIAN_POINT('Ctrl Pts',(18.5750678188543,-17.1039288260002,
0.));
#189281=CARTESIAN_POINT('Ctrl Pts',(18.5843373717253,-17.1286318741185,
0.));
#189282=CARTESIAN_POINT('Ctrl Pts',(18.5935761222833,-17.1534272741646,
0.));
#189283=CARTESIAN_POINT('Ctrl Pts',(18.6027836898826,-17.1783146940131,
0.));
#189284=CARTESIAN_POINT('Ctrl Pts',(18.6119596959957,-17.2032938019288,
0.));
#189285=CARTESIAN_POINT('Ctrl Pts',(18.6211037624041,-17.2283642650519,
0.));
#189286=CARTESIAN_POINT('Ctrl Pts',(18.630215509794,-17.2535257482186,0.));
#189287=CARTESIAN_POINT('Ctrl Pts',(18.639294555474,-17.278777912021,0.));
#189288=CARTESIAN_POINT('Ctrl Pts',(18.6483405141853,-17.3041204135069,
0.));
#189289=CARTESIAN_POINT('Ctrl Pts',(18.6573530024019,-17.3295529098612,
0.));
#189290=CARTESIAN_POINT('Ctrl Pts',(18.6663316416569,-17.3550750612438,
0.));
#189291=CARTESIAN_POINT('Ctrl Pts',(18.6752760624045,-17.3806865340744,
0.));
#189292=CARTESIAN_POINT('Ctrl Pts',(18.6841859073472,-17.4063870038563,
0.));
#189293=CARTESIAN_POINT('Ctrl Pts',(18.6930608357421,-17.4321761588148,
0.));
#189294=CARTESIAN_POINT('Ctrl Pts',(18.7019005250322,-17.4580537012764,
0.));
#189295=CARTESIAN_POINT('Ctrl Pts',(18.7107046613941,-17.4840193397176,
0.));
#189296=CARTESIAN_POINT('Ctrl Pts',(18.7194729318127,-17.5100727820891,
0.));
#189297=CARTESIAN_POINT('Ctrl Pts',(18.728205015716,-17.5362137287604,0.));
#189298=CARTESIAN_POINT('Ctrl Pts',(18.7369005764558,-17.5624418653248,
0.));
#189299=CARTESIAN_POINT('Ctrl Pts',(18.7455592536667,-17.5887568561361,
0.));
#189300=CARTESIAN_POINT('Ctrl Pts',(18.7541806530935,-17.6151583356989,
0.));
#189301=CARTESIAN_POINT('Ctrl Pts',(18.7627643613139,-17.6416459210646,
0.));
#189302=CARTESIAN_POINT('Ctrl Pts',(18.7713099642673,-17.6682192274197,
0.));
#189303=CARTESIAN_POINT('Ctrl Pts',(18.7798170641305,-17.6948778822982,
0.));
#189304=CARTESIAN_POINT('Ctrl Pts',(18.7882852976016,-17.7216215409019,
0.));
#189305=CARTESIAN_POINT('Ctrl Pts',(18.7967143519444,-17.7484498996916,
0.));
#189306=CARTESIAN_POINT('Ctrl Pts',(18.8051039860543,-17.7753627137898,
0.));
#189307=CARTESIAN_POINT('Ctrl Pts',(18.8134540340581,-17.8023598011135,
0.));
#189308=CARTESIAN_POINT('Ctrl Pts',(18.8217643886368,-17.8294410311105,
0.));
#189309=CARTESIAN_POINT('Ctrl Pts',(18.8300349896187,-17.8566063174871,
0.));
#189310=CARTESIAN_POINT('Ctrl Pts',(18.8366196462746,-17.8784057509434,
0.));
#189311=CARTESIAN_POINT('Ctrl Pts',(18.8415402351882,-17.8947931177853,
0.));
#189312=CARTESIAN_POINT('Ctrl Pts',(18.8448126709726,-17.9057348246611,
0.));
#189313=CARTESIAN_POINT('Ctrl Pts',(18.8464468996588,-17.9112098770111,
0.));
#189314=CARTESIAN_POINT('',(18.8464468996588,-17.9112098770111,0.));
#189315=CARTESIAN_POINT('Origin',(12.1729687575668,-17.7219872369693,0.));
#189316=CARTESIAN_POINT('',(12.7689476255362,-18.5896416359912,0.));
#189317=CARTESIAN_POINT('',(12.7689476255362,-18.5896416359912,0.));
#189318=CARTESIAN_POINT('',(6.08648437878337,-8.86099361848466,0.));
#189319=CARTESIAN_POINT('Ctrl Pts',(17.9112098770111,-18.8464468996588,
0.));
#189320=CARTESIAN_POINT('Ctrl Pts',(17.9112098770111,-18.8464468996588,
12.));
#189321=CARTESIAN_POINT('Ctrl Pts',(17.9057348246595,-18.8448126709692,
0.));
#189322=CARTESIAN_POINT('Ctrl Pts',(17.9057348246595,-18.8448126709692,
12.));
#189323=CARTESIAN_POINT('Ctrl Pts',(17.8947931177807,-18.8415402351786,
0.));
#189324=CARTESIAN_POINT('Ctrl Pts',(17.8947931177807,-18.8415402351786,
12.));
#189325=CARTESIAN_POINT('Ctrl Pts',(17.8784057509355,-18.8366196462581,
0.));
#189326=CARTESIAN_POINT('Ctrl Pts',(17.8784057509355,-18.8366196462581,
12.));
#189327=CARTESIAN_POINT('Ctrl Pts',(17.856606317477,-18.8300349895974,0.));
#189328=CARTESIAN_POINT('Ctrl Pts',(17.856606317477,-18.8300349895974,12.));
#189329=CARTESIAN_POINT('Ctrl Pts',(17.8294410311006,-18.8217643886157,
0.));
#189330=CARTESIAN_POINT('Ctrl Pts',(17.8294410311006,-18.8217643886157,
12.));
#189331=CARTESIAN_POINT('Ctrl Pts',(17.8023598011057,-18.8134540340417,
0.));
#189332=CARTESIAN_POINT('Ctrl Pts',(17.8023598011057,-18.8134540340417,
12.));
#189333=CARTESIAN_POINT('Ctrl Pts',(17.7753627137853,-18.8051039860448,
0.));
#189334=CARTESIAN_POINT('Ctrl Pts',(17.7753627137853,-18.8051039860448,
12.));
#189335=CARTESIAN_POINT('Ctrl Pts',(17.7484498996905,-18.7967143519419,
0.));
#189336=CARTESIAN_POINT('Ctrl Pts',(17.7484498996905,-18.7967143519419,
12.));
#189337=CARTESIAN_POINT('Ctrl Pts',(17.7216215409035,-18.788285297605,0.));
#189338=CARTESIAN_POINT('Ctrl Pts',(17.7216215409035,-18.788285297605,12.));
#189339=CARTESIAN_POINT('Ctrl Pts',(17.6948778823014,-18.7798170641374,
0.));
#189340=CARTESIAN_POINT('Ctrl Pts',(17.6948778823014,-18.7798170641374,
12.));
#189341=CARTESIAN_POINT('Ctrl Pts',(17.6682192274236,-18.7713099642754,
0.));
#189342=CARTESIAN_POINT('Ctrl Pts',(17.6682192274236,-18.7713099642754,
12.));
#189343=CARTESIAN_POINT('Ctrl Pts',(17.6416459210681,-18.762764361321,0.));
#189344=CARTESIAN_POINT('Ctrl Pts',(17.6416459210681,-18.762764361321,12.));
#189345=CARTESIAN_POINT('Ctrl Pts',(17.6151583357012,-18.7541806530984,
0.));
#189346=CARTESIAN_POINT('Ctrl Pts',(17.6151583357012,-18.7541806530984,
12.));
#189347=CARTESIAN_POINT('Ctrl Pts',(17.5887568561371,-18.7455592536688,
0.));
#189348=CARTESIAN_POINT('Ctrl Pts',(17.5887568561371,-18.7455592536688,
12.));
#189349=CARTESIAN_POINT('Ctrl Pts',(17.5624418653245,-18.7369005764553,
0.));
#189350=CARTESIAN_POINT('Ctrl Pts',(17.5624418653245,-18.7369005764553,
12.));
#189351=CARTESIAN_POINT('Ctrl Pts',(17.5362137287593,-18.7282050157138,
0.));
#189352=CARTESIAN_POINT('Ctrl Pts',(17.5362137287593,-18.7282050157138,
12.));
#189353=CARTESIAN_POINT('Ctrl Pts',(17.5100727820876,-18.7194729318098,
0.));
#189354=CARTESIAN_POINT('Ctrl Pts',(17.5100727820876,-18.7194729318098,
12.));
#189355=CARTESIAN_POINT('Ctrl Pts',(17.4840193397162,-18.7107046613912,
0.));
#189356=CARTESIAN_POINT('Ctrl Pts',(17.4840193397162,-18.7107046613912,
12.));
#189357=CARTESIAN_POINT('Ctrl Pts',(17.4580537012753,-18.70190052503,0.));
#189358=CARTESIAN_POINT('Ctrl Pts',(17.4580537012753,-18.70190052503,12.));
#189359=CARTESIAN_POINT('Ctrl Pts',(17.4321761588142,-18.6930608357409,
0.));
#189360=CARTESIAN_POINT('Ctrl Pts',(17.4321761588142,-18.6930608357409,
12.));
#189361=CARTESIAN_POINT('Ctrl Pts',(17.4063870038562,-18.6841859073471,
0.));
#189362=CARTESIAN_POINT('Ctrl Pts',(17.4063870038562,-18.6841859073471,
12.));
#189363=CARTESIAN_POINT('Ctrl Pts',(17.3806865340747,-18.6752760624052,
0.));
#189364=CARTESIAN_POINT('Ctrl Pts',(17.3806865340747,-18.6752760624052,
12.));
#189365=CARTESIAN_POINT('Ctrl Pts',(17.3550750612443,-18.6663316416582,
0.));
#189366=CARTESIAN_POINT('Ctrl Pts',(17.3550750612443,-18.6663316416582,
12.));
#189367=CARTESIAN_POINT('Ctrl Pts',(17.3295529098618,-18.6573530024033,
0.));
#189368=CARTESIAN_POINT('Ctrl Pts',(17.3295529098618,-18.6573530024033,
12.));
#189369=CARTESIAN_POINT('Ctrl Pts',(17.3041204135074,-18.6483405141865,
0.));
#189370=CARTESIAN_POINT('Ctrl Pts',(17.3041204135074,-18.6483405141865,
12.));
#189371=CARTESIAN_POINT('Ctrl Pts',(17.2787779120213,-18.6392945554748,
0.));
#189372=CARTESIAN_POINT('Ctrl Pts',(17.2787779120213,-18.6392945554748,
12.));
#189373=CARTESIAN_POINT('Ctrl Pts',(17.2535257482187,-18.6302155097943,
0.));
#189374=CARTESIAN_POINT('Ctrl Pts',(17.2535257482187,-18.6302155097943,
12.));
#189375=CARTESIAN_POINT('Ctrl Pts',(17.2283642650517,-18.6211037624038,
0.));
#189376=CARTESIAN_POINT('Ctrl Pts',(17.2283642650517,-18.6211037624038,
12.));
#189377=CARTESIAN_POINT('Ctrl Pts',(17.2032938019284,-18.6119596959949,
0.));
#189378=CARTESIAN_POINT('Ctrl Pts',(17.2032938019284,-18.6119596959949,
12.));
#189379=CARTESIAN_POINT('Ctrl Pts',(17.1783146940127,-18.6027836898817,
0.));
#189380=CARTESIAN_POINT('Ctrl Pts',(17.1783146940127,-18.6027836898817,
12.));
#189381=CARTESIAN_POINT('Ctrl Pts',(17.1534272741643,-18.5935761222825,
0.));
#189382=CARTESIAN_POINT('Ctrl Pts',(17.1534272741643,-18.5935761222825,
12.));
#189383=CARTESIAN_POINT('Ctrl Pts',(17.1286318741183,-18.5843373717247,
0.));
#189384=CARTESIAN_POINT('Ctrl Pts',(17.1286318741183,-18.5843373717247,
12.));
#189385=CARTESIAN_POINT('Ctrl Pts',(17.1039288260001,-18.5750678188542,
0.));
#189386=CARTESIAN_POINT('Ctrl Pts',(17.1039288260001,-18.5750678188542,
12.));
#189387=CARTESIAN_POINT('Ctrl Pts',(17.0793184636079,-18.5657678479789,
0.));
#189388=CARTESIAN_POINT('Ctrl Pts',(17.0793184636079,-18.5657678479789,
12.));
#189389=CARTESIAN_POINT('Ctrl Pts',(17.0548011239751,-18.556437848963,0.));
#189390=CARTESIAN_POINT('Ctrl Pts',(17.0548011239751,-18.556437848963,12.));
#189391=CARTESIAN_POINT('Ctrl Pts',(17.0303771481738,-18.547078218209,0.));
#189392=CARTESIAN_POINT('Ctrl Pts',(17.0303771481738,-18.547078218209,12.));
#189393=CARTESIAN_POINT('Ctrl Pts',(17.0060468805097,-18.5376893576961,
0.));
#189394=CARTESIAN_POINT('Ctrl Pts',(17.0060468805097,-18.5376893576961,
12.));
#189395=CARTESIAN_POINT('Ctrl Pts',(16.981810668038,-18.5282716744197,0.));
#189396=CARTESIAN_POINT('Ctrl Pts',(16.981810668038,-18.5282716744197,12.));
#189397=CARTESIAN_POINT('Ctrl Pts',(16.9576688599339,-18.5188255796659,
0.));
#189398=CARTESIAN_POINT('Ctrl Pts',(16.9576688599339,-18.5188255796659,
12.));
#189399=CARTESIAN_POINT('Ctrl Pts',(16.9336218069353,-18.5093514883835,
0.));
#189400=CARTESIAN_POINT('Ctrl Pts',(16.9336218069353,-18.5093514883835,
12.));
#189401=CARTESIAN_POINT('Ctrl Pts',(16.9096698606943,-18.499849818462,0.));
#189402=CARTESIAN_POINT('Ctrl Pts',(16.9096698606943,-18.499849818462,12.));
#189403=CARTESIAN_POINT('Ctrl Pts',(16.8858133733088,-18.4903209902227,
0.));
#189404=CARTESIAN_POINT('Ctrl Pts',(16.8858133733088,-18.4903209902227,
12.));
#189405=CARTESIAN_POINT('Ctrl Pts',(16.8620526977171,-18.4807654268771,
0.));
#189406=CARTESIAN_POINT('Ctrl Pts',(16.8620526977171,-18.4807654268771,
12.));
#189407=CARTESIAN_POINT('Ctrl Pts',(16.8383881879709,-18.4711835548623,
0.));
#189408=CARTESIAN_POINT('Ctrl Pts',(16.8383881879709,-18.4711835548623,
12.));
#189409=CARTESIAN_POINT('Ctrl Pts',(16.8148201995472,-18.4615758042305,
0.));
#189410=CARTESIAN_POINT('Ctrl Pts',(16.8148201995472,-18.4615758042305,
12.));
#189411=CARTESIAN_POINT('Ctrl Pts',(16.791349089629,-18.4519426090124,0.));
#189412=CARTESIAN_POINT('Ctrl Pts',(16.791349089629,-18.4519426090124,12.));
#189413=CARTESIAN_POINT('Ctrl Pts',(16.7679752173992,-18.44228440761,0.));
#189414=CARTESIAN_POINT('Ctrl Pts',(16.7679752173992,-18.44228440761,12.));
#189415=CARTESIAN_POINT('Ctrl Pts',(16.7446989442882,-18.4326016431392,
0.));
#189416=CARTESIAN_POINT('Ctrl Pts',(16.7446989442882,-18.4326016431392,
12.));
#189417=CARTESIAN_POINT('Ctrl Pts',(16.7215206338818,-18.4228947633187,
0.));
#189418=CARTESIAN_POINT('Ctrl Pts',(16.7215206338818,-18.4228947633187,
12.));
#189419=CARTESIAN_POINT('Ctrl Pts',(16.698440651849,-18.413164220399,0.));
#189420=CARTESIAN_POINT('Ctrl Pts',(16.698440651849,-18.413164220399,12.));
#189421=CARTESIAN_POINT('Ctrl Pts',(16.6754593658513,-18.403410471079,0.));
#189422=CARTESIAN_POINT('Ctrl Pts',(16.6754593658513,-18.403410471079,12.));
#189423=CARTESIAN_POINT('Ctrl Pts',(16.6525771454513,-18.3936339764332,
0.));
#189424=CARTESIAN_POINT('Ctrl Pts',(16.6525771454513,-18.3936339764332,
12.));
#189425=CARTESIAN_POINT('Ctrl Pts',(16.6297943620056,-18.3838352018327,
0.));
#189426=CARTESIAN_POINT('Ctrl Pts',(16.6297943620056,-18.3838352018327,
12.));
#189427=CARTESIAN_POINT('Ctrl Pts',(16.607111388571,-18.3740146168879,0.));
#189428=CARTESIAN_POINT('Ctrl Pts',(16.607111388571,-18.3740146168879,12.));
#189429=CARTESIAN_POINT('Ctrl Pts',(16.5845286000217,-18.3641726955889,
0.));
#189430=CARTESIAN_POINT('Ctrl Pts',(16.5845286000217,-18.3641726955889,
12.));
#189431=CARTESIAN_POINT('Ctrl Pts',(16.5620463731413,-18.354309916433,0.));
#189432=CARTESIAN_POINT('Ctrl Pts',(16.5620463731413,-18.354309916433,12.));
#189433=CARTESIAN_POINT('Ctrl Pts',(16.5396650867139,-18.34442676256,0.));
#189434=CARTESIAN_POINT('Ctrl Pts',(16.5396650867139,-18.34442676256,12.));
#189435=CARTESIAN_POINT('Ctrl Pts',(16.5173851216045,-18.3345237218864,
0.));
#189436=CARTESIAN_POINT('Ctrl Pts',(16.5173851216045,-18.3345237218864,
12.));
#189437=CARTESIAN_POINT('Ctrl Pts',(16.4952068608345,-18.3246012872469,
0.));
#189438=CARTESIAN_POINT('Ctrl Pts',(16.4952068608345,-18.3246012872469,
12.));
#189439=CARTESIAN_POINT('Ctrl Pts',(16.4731306896441,-18.3146599565231,
0.));
#189440=CARTESIAN_POINT('Ctrl Pts',(16.4731306896441,-18.3146599565231,
12.));
#189441=CARTESIAN_POINT('Ctrl Pts',(16.4511569955233,-18.304700232686,0.));
#189442=CARTESIAN_POINT('Ctrl Pts',(16.4511569955233,-18.304700232686,12.));
#189443=CARTESIAN_POINT('Ctrl Pts',(16.4292861682378,-18.294722623851,0.));
#189444=CARTESIAN_POINT('Ctrl Pts',(16.4292861682378,-18.294722623851,12.));
#189445=CARTESIAN_POINT('Ctrl Pts',(16.4075185998454,-18.2847276433309,
0.));
#189446=CARTESIAN_POINT('Ctrl Pts',(16.4075185998454,-18.2847276433309,
12.));
#189447=CARTESIAN_POINT('Ctrl Pts',(16.385854684708,-18.2747158096934,0.));
#189448=CARTESIAN_POINT('Ctrl Pts',(16.385854684708,-18.2747158096934,12.));
#189449=CARTESIAN_POINT('Ctrl Pts',(16.3642948194868,-18.2646876468169,
0.));
#189450=CARTESIAN_POINT('Ctrl Pts',(16.3642948194868,-18.2646876468169,
12.));
#189451=CARTESIAN_POINT('Ctrl Pts',(16.3428394031589,-18.2546436839608,
0.));
#189452=CARTESIAN_POINT('Ctrl Pts',(16.3428394031589,-18.2546436839608,
12.));
#189453=CARTESIAN_POINT('Ctrl Pts',(16.3214888370987,-18.2445844558742,
0.));
#189454=CARTESIAN_POINT('Ctrl Pts',(16.3214888370987,-18.2445844558742,
12.));
#189455=CARTESIAN_POINT('Ctrl Pts',(16.3002435251378,-18.2345105028982,
0.));
#189456=CARTESIAN_POINT('Ctrl Pts',(16.3002435251378,-18.2345105028982,
12.));
#189457=CARTESIAN_POINT('Ctrl Pts',(16.2791038736223,-18.2244223710746,
0.));
#189458=CARTESIAN_POINT('Ctrl Pts',(16.2791038736223,-18.2244223710746,
12.));
#189459=CARTESIAN_POINT('Ctrl Pts',(16.2580702914615,-18.2143206122529,
0.));
#189460=CARTESIAN_POINT('Ctrl Pts',(16.2580702914615,-18.2143206122529,
12.));
#189461=CARTESIAN_POINT('Ctrl Pts',(16.2371431901638,-18.2042057842035,
0.));
#189462=CARTESIAN_POINT('Ctrl Pts',(16.2371431901638,-18.2042057842035,
12.));
#189463=CARTESIAN_POINT('Ctrl Pts',(16.2163229838875,-18.1940784507229,
0.));
#189464=CARTESIAN_POINT('Ctrl Pts',(16.2163229838875,-18.1940784507229,
12.));
#189465=CARTESIAN_POINT('Ctrl Pts',(16.1956100895073,-18.1839391817331,
0.));
#189466=CARTESIAN_POINT('Ctrl Pts',(16.1956100895073,-18.1839391817331,
12.));
#189467=CARTESIAN_POINT('Ctrl Pts',(16.1750049266671,-18.1737885533849,
0.));
#189468=CARTESIAN_POINT('Ctrl Pts',(16.1750049266671,-18.1737885533849,
12.));
#189469=CARTESIAN_POINT('Ctrl Pts',(16.154507917826,-18.1636271481615,0.));
#189470=CARTESIAN_POINT('Ctrl Pts',(16.154507917826,-18.1636271481615,12.));
#189471=CARTESIAN_POINT('Ctrl Pts',(16.1341194882988,-18.1534555549853,
0.));
#189472=CARTESIAN_POINT('Ctrl Pts',(16.1341194882988,-18.1534555549853,
12.));
#189473=CARTESIAN_POINT('Ctrl Pts',(16.1138400662794,-18.1432743693235,
0.));
#189474=CARTESIAN_POINT('Ctrl Pts',(16.1138400662794,-18.1432743693235,
12.));
#189475=CARTESIAN_POINT('Ctrl Pts',(16.0936700829112,-18.1330841933105,
0.));
#189476=CARTESIAN_POINT('Ctrl Pts',(16.0936700829112,-18.1330841933105,
12.));
#189477=CARTESIAN_POINT('Ctrl Pts',(16.0736099723668,-18.1228856358751,
0.));
#189478=CARTESIAN_POINT('Ctrl Pts',(16.0736099723668,-18.1228856358751,
12.));
#189479=CARTESIAN_POINT('Ctrl Pts',(16.0536601719125,-18.112679312869,0.));
#189480=CARTESIAN_POINT('Ctrl Pts',(16.0536601719125,-18.112679312869,12.));
#189481=CARTESIAN_POINT('Ctrl Pts',(16.0338211219693,-18.1024658471966,
0.));
#189482=CARTESIAN_POINT('Ctrl Pts',(16.0338211219693,-18.1024658471966,
12.));
#189483=CARTESIAN_POINT('Ctrl Pts',(16.014093266161,-18.0922458689462,0.));
#189484=CARTESIAN_POINT('Ctrl Pts',(16.014093266161,-18.0922458689462,12.));
#189485=CARTESIAN_POINT('Ctrl Pts',(15.9944770513613,-18.0820200155236,
0.));
#189486=CARTESIAN_POINT('Ctrl Pts',(15.9944770513613,-18.0820200155236,
12.));
#189487=CARTESIAN_POINT('Ctrl Pts',(15.9749729277846,-18.0717889317958,
0.));
#189488=CARTESIAN_POINT('Ctrl Pts',(15.9749729277846,-18.0717889317958,
12.));
#189489=CARTESIAN_POINT('Ctrl Pts',(15.9555813490644,-18.061553270236,0.));
#189490=CARTESIAN_POINT('Ctrl Pts',(15.9555813490644,-18.061553270236,12.));
#189491=CARTESIAN_POINT('Ctrl Pts',(15.9363027723244,-18.0513136910691,
0.));
#189492=CARTESIAN_POINT('Ctrl Pts',(15.9363027723244,-18.0513136910691,
12.));
#189493=CARTESIAN_POINT('Ctrl Pts',(15.9171376582436,-18.0410708624209,
0.));
#189494=CARTESIAN_POINT('Ctrl Pts',(15.9171376582436,-18.0410708624209,
12.));
#189495=CARTESIAN_POINT('Ctrl Pts',(15.8980864711042,-18.0308254604636,
0.));
#189496=CARTESIAN_POINT('Ctrl Pts',(15.8980864711042,-18.0308254604636,
12.));
#189497=CARTESIAN_POINT('Ctrl Pts',(15.8791496788682,-18.0205781695769,
0.));
#189498=CARTESIAN_POINT('Ctrl Pts',(15.8791496788682,-18.0205781695769,
12.));
#189499=CARTESIAN_POINT('Ctrl Pts',(15.8603277532831,-18.0103296825205,
0.));
#189500=CARTESIAN_POINT('Ctrl Pts',(15.8603277532831,-18.0103296825205,
12.));
#189501=CARTESIAN_POINT('Ctrl Pts',(15.8416211699679,-18.0000807006052,
0.));
#189502=CARTESIAN_POINT('Ctrl Pts',(15.8416211699679,-18.0000807006052,
12.));
#189503=CARTESIAN_POINT('Ctrl Pts',(15.8230304084962,-17.9898319338665,
0.));
#189504=CARTESIAN_POINT('Ctrl Pts',(15.8230304084962,-17.9898319338665,
12.));
#189505=CARTESIAN_POINT('Ctrl Pts',(15.8045559524676,-17.9795841012386,
0.));
#189506=CARTESIAN_POINT('Ctrl Pts',(15.8045559524676,-17.9795841012386,
12.));
#189507=CARTESIAN_POINT('Ctrl Pts',(15.7861982895724,-17.9693379307303,
0.));
#189508=CARTESIAN_POINT('Ctrl Pts',(15.7861982895724,-17.9693379307303,
12.));
#189509=CARTESIAN_POINT('Ctrl Pts',(15.7679579117077,-17.9590941596242,
0.));
#189510=CARTESIAN_POINT('Ctrl Pts',(15.7679579117077,-17.9590941596242,
12.));
#189511=CARTESIAN_POINT('Ctrl Pts',(15.749835315086,-17.9488535346781,0.));
#189512=CARTESIAN_POINT('Ctrl Pts',(15.749835315086,-17.9488535346781,12.));
#189513=CARTESIAN_POINT('Ctrl Pts',(15.7318310003335,-17.9386168123262,
0.));
#189514=CARTESIAN_POINT('Ctrl Pts',(15.7318310003335,-17.9386168123262,
12.));
#189515=CARTESIAN_POINT('Ctrl Pts',(15.7139454725838,-17.9283847588836,
0.));
#189516=CARTESIAN_POINT('Ctrl Pts',(15.7139454725838,-17.9283847588836,
12.));
#189517=CARTESIAN_POINT('Ctrl Pts',(15.6961792415522,-17.9181581507455,
0.));
#189518=CARTESIAN_POINT('Ctrl Pts',(15.6961792415522,-17.9181581507455,
12.));
#189519=CARTESIAN_POINT('Ctrl Pts',(15.678532821646,-17.9079377746111,0.));
#189520=CARTESIAN_POINT('Ctrl Pts',(15.678532821646,-17.9079377746111,12.));
#189521=CARTESIAN_POINT('Ctrl Pts',(15.661006732103,-17.897724427724,0.));
#189522=CARTESIAN_POINT('Ctrl Pts',(15.661006732103,-17.897724427724,12.));
#189523=CARTESIAN_POINT('Ctrl Pts',(15.6436014971084,-17.8875189181091,
0.));
#189524=CARTESIAN_POINT('Ctrl Pts',(15.6436014971084,-17.8875189181091,
12.));
#189525=CARTESIAN_POINT('Ctrl Pts',(15.6263176459108,-17.8773220648125,
0.));
#189526=CARTESIAN_POINT('Ctrl Pts',(15.6263176459108,-17.8773220648125,
12.));
#189527=CARTESIAN_POINT('Ctrl Pts',(15.609155712921,-17.8671346981394,0.));
#189528=CARTESIAN_POINT('Ctrl Pts',(15.609155712921,-17.8671346981394,12.));
#189529=CARTESIAN_POINT('Ctrl Pts',(15.5921162378192,-17.8569576599006,
0.));
#189530=CARTESIAN_POINT('Ctrl Pts',(15.5921162378192,-17.8569576599006,
12.));
#189531=CARTESIAN_POINT('Ctrl Pts',(15.5751997657162,-17.8467918036987,
0.));
#189532=CARTESIAN_POINT('Ctrl Pts',(15.5751997657162,-17.8467918036987,
12.));
#189533=CARTESIAN_POINT('Ctrl Pts',(15.5584068472982,-17.8366379952085,
0.));
#189534=CARTESIAN_POINT('Ctrl Pts',(15.5584068472982,-17.8366379952085,
12.));
#189535=CARTESIAN_POINT('Ctrl Pts',(15.541738038964,-17.8264971124607,0.));
#189536=CARTESIAN_POINT('Ctrl Pts',(15.541738038964,-17.8264971124607,12.));
#189537=CARTESIAN_POINT('Ctrl Pts',(15.5251939029552,-17.8163700461256,
0.));
#189538=CARTESIAN_POINT('Ctrl Pts',(15.5251939029552,-17.8163700461256,
12.));
#189539=CARTESIAN_POINT('Ctrl Pts',(15.5087750074718,-17.8062576997952,
0.));
#189540=CARTESIAN_POINT('Ctrl Pts',(15.5087750074718,-17.8062576997952,
12.));
#189541=CARTESIAN_POINT('Ctrl Pts',(15.4924819268517,-17.7961609903148,
0.));
#189542=CARTESIAN_POINT('Ctrl Pts',(15.4924819268517,-17.7961609903148,
12.));
#189543=CARTESIAN_POINT('Ctrl Pts',(15.4763152417497,-17.786080848122,0.));
#189544=CARTESIAN_POINT('Ctrl Pts',(15.4763152417497,-17.786080848122,12.));
#189545=CARTESIAN_POINT('Ctrl Pts',(15.4602755393017,-17.7760182175815,
0.));
#189546=CARTESIAN_POINT('Ctrl Pts',(15.4602755393017,-17.7760182175815,
12.));
#189547=CARTESIAN_POINT('Ctrl Pts',(15.4443634132869,-17.7659740573265,
0.));
#189548=CARTESIAN_POINT('Ctrl Pts',(15.4443634132869,-17.7659740573265,
12.));
#189549=CARTESIAN_POINT('Ctrl Pts',(15.4285794642667,-17.7559493405881,
0.));
#189550=CARTESIAN_POINT('Ctrl Pts',(15.4285794642667,-17.7559493405881,
12.));
#189551=CARTESIAN_POINT('Ctrl Pts',(15.4129242997837,-17.7459450555813,
0.));
#189552=CARTESIAN_POINT('Ctrl Pts',(15.4129242997837,-17.7459450555813,
12.));
#189553=CARTESIAN_POINT('Ctrl Pts',(15.3973985345802,-17.735962205915,0.));
#189554=CARTESIAN_POINT('Ctrl Pts',(15.3973985345802,-17.735962205915,12.));
#189555=CARTESIAN_POINT('Ctrl Pts',(15.3820027907966,-17.7260018109924,
0.));
#189556=CARTESIAN_POINT('Ctrl Pts',(15.3820027907966,-17.7260018109924,
12.));
#189557=CARTESIAN_POINT('Ctrl Pts',(15.3667376981699,-17.7160649064206,
0.));
#189558=CARTESIAN_POINT('Ctrl Pts',(15.3667376981699,-17.7160649064206,
12.));
#189559=CARTESIAN_POINT('Ctrl Pts',(15.351603894206,-17.7061525444042,0.));
#189560=CARTESIAN_POINT('Ctrl Pts',(15.351603894206,-17.7061525444042,12.));
#189561=CARTESIAN_POINT('Ctrl Pts',(15.3366020244066,-17.6962657941983,
0.));
#189562=CARTESIAN_POINT('Ctrl Pts',(15.3366020244066,-17.6962657941983,
12.));
#189563=CARTESIAN_POINT('Ctrl Pts',(15.3217327425338,-17.6864057426052,
0.));
#189564=CARTESIAN_POINT('Ctrl Pts',(15.3217327425338,-17.6864057426052,
12.));
#189565=CARTESIAN_POINT('Ctrl Pts',(15.30699671085,-17.676573494456,0.));
#189566=CARTESIAN_POINT('Ctrl Pts',(15.30699671085,-17.676573494456,12.));
#189567=CARTESIAN_POINT('Ctrl Pts',(15.2923946003598,-17.6667701731041,
0.));
#189568=CARTESIAN_POINT('Ctrl Pts',(15.2923946003598,-17.6667701731041,
12.));
#189569=CARTESIAN_POINT('Ctrl Pts',(15.2779270910239,-17.6569969209,0.));
#189570=CARTESIAN_POINT('Ctrl Pts',(15.2779270910239,-17.6569969209,12.));
#189571=CARTESIAN_POINT('Ctrl Pts',(15.2635948720292,-17.6472548997328,
0.));
#189572=CARTESIAN_POINT('Ctrl Pts',(15.2635948720292,-17.6472548997328,
12.));
#189573=CARTESIAN_POINT('Ctrl Pts',(15.2493986421092,-17.6375452916369,
0.));
#189574=CARTESIAN_POINT('Ctrl Pts',(15.2493986421092,-17.6375452916369,
12.));
#189575=CARTESIAN_POINT('Ctrl Pts',(15.2353391098366,-17.6278692993764,
0.));
#189576=CARTESIAN_POINT('Ctrl Pts',(15.2353391098366,-17.6278692993764,
12.));
#189577=CARTESIAN_POINT('Ctrl Pts',(15.2214169939199,-17.6182281470468,
0.));
#189578=CARTESIAN_POINT('Ctrl Pts',(15.2214169939199,-17.6182281470468,
12.));
#189579=CARTESIAN_POINT('Ctrl Pts',(15.2076330234686,-17.60862308065,0.));
#189580=CARTESIAN_POINT('Ctrl Pts',(15.2076330234686,-17.60862308065,12.));
#189581=CARTESIAN_POINT('Ctrl Pts',(15.1939879383268,-17.5990553687599,
0.));
#189582=CARTESIAN_POINT('Ctrl Pts',(15.1939879383268,-17.5990553687599,
12.));
#189583=CARTESIAN_POINT('Ctrl Pts',(15.1804824894605,-17.5895263032595,
0.));
#189584=CARTESIAN_POINT('Ctrl Pts',(15.1804824894605,-17.5895263032595,
12.));
#189585=CARTESIAN_POINT('Ctrl Pts',(15.1671174393137,-17.580037200054,0.));
#189586=CARTESIAN_POINT('Ctrl Pts',(15.1671174393137,-17.580037200054,12.));
#189587=CARTESIAN_POINT('Ctrl Pts',(15.1538935621714,-17.5705893998029,
0.));
#189588=CARTESIAN_POINT('Ctrl Pts',(15.1538935621714,-17.5705893998029,
12.));
#189589=CARTESIAN_POINT('Ctrl Pts',(15.1408116444876,-17.5611842686192,
0.));
#189590=CARTESIAN_POINT('Ctrl Pts',(15.1408116444876,-17.5611842686192,
12.));
#189591=CARTESIAN_POINT('Ctrl Pts',(15.1278724853138,-17.5518231989117,
0.));
#189592=CARTESIAN_POINT('Ctrl Pts',(15.1278724853138,-17.5518231989117,
12.));
#189593=CARTESIAN_POINT('Ctrl Pts',(15.1150768967728,-17.5425076102963,
0.));
#189594=CARTESIAN_POINT('Ctrl Pts',(15.1150768967728,-17.5425076102963,
12.));
#189595=CARTESIAN_POINT('Ctrl Pts',(15.1024257045033,-17.5332389504829,
0.));
#189596=CARTESIAN_POINT('Ctrl Pts',(15.1024257045033,-17.5332389504829,
12.));
#189597=CARTESIAN_POINT('Ctrl Pts',(15.0899197481082,-17.5240186961791,
0.));
#189598=CARTESIAN_POINT('Ctrl Pts',(15.0899197481082,-17.5240186961791,
12.));
#189599=CARTESIAN_POINT('Ctrl Pts',(15.0775598815749,-17.5148483539687,
0.));
#189600=CARTESIAN_POINT('Ctrl Pts',(15.0775598815749,-17.5148483539687,
12.));
#189601=CARTESIAN_POINT('Ctrl Pts',(15.0653469738307,-17.5057294613877,
0.));
#189602=CARTESIAN_POINT('Ctrl Pts',(15.0653469738307,-17.5057294613877,
12.));
#189603=CARTESIAN_POINT('Ctrl Pts',(15.0532819093085,-17.4966635880246,
0.));
#189604=CARTESIAN_POINT('Ctrl Pts',(15.0532819093085,-17.4966635880246,
12.));
#189605=CARTESIAN_POINT('Ctrl Pts',(15.0413655884993,-17.4876523366178,
0.));
#189606=CARTESIAN_POINT('Ctrl Pts',(15.0413655884993,-17.4876523366178,
12.));
#189607=CARTESIAN_POINT('Ctrl Pts',(15.029598928488,-17.4786973441417,0.));
#189608=CARTESIAN_POINT('Ctrl Pts',(15.029598928488,-17.4786973441417,12.));
#189609=CARTESIAN_POINT('Ctrl Pts',(15.0179828635087,-17.4698002829357,
0.));
#189610=CARTESIAN_POINT('Ctrl Pts',(15.0179828635087,-17.4698002829357,
12.));
#189611=CARTESIAN_POINT('Ctrl Pts',(15.0065183456922,-17.4609628621419,
0.));
#189612=CARTESIAN_POINT('Ctrl Pts',(15.0065183456922,-17.4609628621419,
12.));
#189613=CARTESIAN_POINT('Ctrl Pts',(14.9952063457779,-17.4521868291005,
0.));
#189614=CARTESIAN_POINT('Ctrl Pts',(14.9952063457779,-17.4521868291005,
12.));
#189615=CARTESIAN_POINT('Ctrl Pts',(14.9840478538357,-17.4434739707773,
0.));
#189616=CARTESIAN_POINT('Ctrl Pts',(14.9840478538357,-17.4434739707773,
12.));
#189617=CARTESIAN_POINT('Ctrl Pts',(14.973043879945,-17.4348261151395,0.));
#189618=CARTESIAN_POINT('Ctrl Pts',(14.973043879945,-17.4348261151395,12.));
#189619=CARTESIAN_POINT('Ctrl Pts',(14.9621954549825,-17.4262451327088,
0.));
#189620=CARTESIAN_POINT('Ctrl Pts',(14.9621954549825,-17.4262451327088,
12.));
#189621=CARTESIAN_POINT('Ctrl Pts',(14.9515036315142,-17.4177329382827,
0.));
#189622=CARTESIAN_POINT('Ctrl Pts',(14.9515036315142,-17.4177329382827,
12.));
#189623=CARTESIAN_POINT('Ctrl Pts',(14.940969484645,-17.4092914926072,0.));
#189624=CARTESIAN_POINT('Ctrl Pts',(14.940969484645,-17.4092914926072,12.));
#189625=CARTESIAN_POINT('Ctrl Pts',(14.9305941128758,-17.400922804075,0.));
#189626=CARTESIAN_POINT('Ctrl Pts',(14.9305941128758,-17.400922804075,12.));
#189627=CARTESIAN_POINT('Ctrl Pts',(14.9203786389343,-17.3926289303987,
0.));
#189628=CARTESIAN_POINT('Ctrl Pts',(14.9203786389343,-17.3926289303987,
12.));
#189629=CARTESIAN_POINT('Ctrl Pts',(14.9103242110057,-17.3844119809823,
0.));
#189630=CARTESIAN_POINT('Ctrl Pts',(14.9103242110057,-17.3844119809823,
12.));
#189631=CARTESIAN_POINT('Ctrl Pts',(14.9004320039609,-17.3762741193075,
0.));
#189632=CARTESIAN_POINT('Ctrl Pts',(14.9004320039609,-17.3762741193075,
12.));
#189633=CARTESIAN_POINT('Ctrl Pts',(14.8907032205789,-17.3682175653236,
0.));
#189634=CARTESIAN_POINT('Ctrl Pts',(14.8907032205789,-17.3682175653236,
12.));
#189635=CARTESIAN_POINT('Ctrl Pts',(14.8811390927424,-17.3602445978163,
0.));
#189636=CARTESIAN_POINT('Ctrl Pts',(14.8811390927424,-17.3602445978163,
12.));
#189637=CARTESIAN_POINT('Ctrl Pts',(14.8717408826957,-17.3523575568648,
0.));
#189638=CARTESIAN_POINT('Ctrl Pts',(14.8717408826957,-17.3523575568648,
12.));
#189639=CARTESIAN_POINT('Ctrl Pts',(14.8625098843419,-17.3445588463477,
0.));
#189640=CARTESIAN_POINT('Ctrl Pts',(14.8625098843419,-17.3445588463477,
12.));
#189641=CARTESIAN_POINT('Ctrl Pts',(14.8534474245433,-17.336850936485,0.));
#189642=CARTESIAN_POINT('Ctrl Pts',(14.8534474245433,-17.336850936485,12.));
#189643=CARTESIAN_POINT('Ctrl Pts',(14.8445548643504,-17.3292363662601,
0.));
#189644=CARTESIAN_POINT('Ctrl Pts',(14.8445548643504,-17.3292363662601,
12.));
#189645=CARTESIAN_POINT('Ctrl Pts',(14.8358336004193,-17.3217177462096,
0.));
#189646=CARTESIAN_POINT('Ctrl Pts',(14.8358336004193,-17.3217177462096,
12.));
#189647=CARTESIAN_POINT('Ctrl Pts',(14.8272850675375,-17.3142977632656,
0.));
#189648=CARTESIAN_POINT('Ctrl Pts',(14.8272850675375,-17.3142977632656,
12.));
#189649=CARTESIAN_POINT('Ctrl Pts',(14.8189107410161,-17.3069791853705,
0.));
#189650=CARTESIAN_POINT('Ctrl Pts',(14.8189107410161,-17.3069791853705,
12.));
#189651=CARTESIAN_POINT('Ctrl Pts',(14.8107121391038,-17.2997648661483,
0.));
#189652=CARTESIAN_POINT('Ctrl Pts',(14.8107121391038,-17.2997648661483,
12.));
#189653=CARTESIAN_POINT('Ctrl Pts',(14.8026908254281,-17.2926577496519,
0.));
#189654=CARTESIAN_POINT('Ctrl Pts',(14.8026908254281,-17.2926577496519,
12.));
#189655=CARTESIAN_POINT('Ctrl Pts',(14.7948484105252,-17.28566087332,0.));
#189656=CARTESIAN_POINT('Ctrl Pts',(14.7948484105252,-17.28566087332,12.));
#189657=CARTESIAN_POINT('Ctrl Pts',(14.787186553128,-17.278777370485,0.));
#189658=CARTESIAN_POINT('Ctrl Pts',(14.787186553128,-17.278777370485,12.));
#189659=CARTESIAN_POINT('Ctrl Pts',(14.7797069617802,-17.2720104735192,
0.));
#189660=CARTESIAN_POINT('Ctrl Pts',(14.7797069617802,-17.2720104735192,
12.));
#189661=CARTESIAN_POINT('Ctrl Pts',(14.7724113956728,-17.2653635155317,
0.));
#189662=CARTESIAN_POINT('Ctrl Pts',(14.7724113956728,-17.2653635155317,
12.));
#189663=CARTESIAN_POINT('Ctrl Pts',(14.7653016697589,-17.2588399401464,
0.));
#189664=CARTESIAN_POINT('Ctrl Pts',(14.7653016697589,-17.2588399401464,
12.));
#189665=CARTESIAN_POINT('Ctrl Pts',(14.7583796616617,-17.2524433146837,
0.));
#189666=CARTESIAN_POINT('Ctrl Pts',(14.7583796616617,-17.2524433146837,
12.));
#189667=CARTESIAN_POINT('Ctrl Pts',(14.7516473175124,-17.2461773413289,
0.));
#189668=CARTESIAN_POINT('Ctrl Pts',(14.7516473175124,-17.2461773413289,
12.));
#189669=CARTESIAN_POINT('Ctrl Pts',(14.7451066593793,-17.2400458713566,
0.));
#189670=CARTESIAN_POINT('Ctrl Pts',(14.7451066593793,-17.2400458713566,
12.));
#189671=CARTESIAN_POINT('Ctrl Pts',(14.7387597858117,-17.2340529062078,
0.));
#189672=CARTESIAN_POINT('Ctrl Pts',(14.7387597858117,-17.2340529062078,
12.));
#189673=CARTESIAN_POINT('Ctrl Pts',(14.7326088681163,-17.2282025904314,
0.));
#189674=CARTESIAN_POINT('Ctrl Pts',(14.7326088681163,-17.2282025904314,
12.));
#189675=CARTESIAN_POINT('Ctrl Pts',(14.7266561494282,-17.2224992099666,
0.));
#189676=CARTESIAN_POINT('Ctrl Pts',(14.7266561494282,-17.2224992099666,
12.));
#189677=CARTESIAN_POINT('Ctrl Pts',(14.7209039390325,-17.2169471814255,
0.));
#189678=CARTESIAN_POINT('Ctrl Pts',(14.7209039390325,-17.2169471814255,
12.));
#189679=CARTESIAN_POINT('Ctrl Pts',(14.7153546289338,-17.2115510835988,
0.));
#189680=CARTESIAN_POINT('Ctrl Pts',(14.7153546289338,-17.2115510835988,
12.));
#189681=CARTESIAN_POINT('Ctrl Pts',(14.7100107213586,-17.2063157097316,
0.));
#189682=CARTESIAN_POINT('Ctrl Pts',(14.7100107213586,-17.2063157097316,
12.));
#189683=CARTESIAN_POINT('Ctrl Pts',(14.7048748502662,-17.2012461084268,
0.));
#189684=CARTESIAN_POINT('Ctrl Pts',(14.7048748502662,-17.2012461084268,
12.));
#189685=CARTESIAN_POINT('Ctrl Pts',(14.699949811582,-17.1963476411694,0.));
#189686=CARTESIAN_POINT('Ctrl Pts',(14.699949811582,-17.1963476411694,12.));
#189687=CARTESIAN_POINT('Ctrl Pts',(14.6952385361706,-17.1916259308416,
0.));
#189688=CARTESIAN_POINT('Ctrl Pts',(14.6952385361706,-17.1916259308416,
12.));
#189689=CARTESIAN_POINT('Ctrl Pts',(14.6907440526957,-17.1870867909918,
0.));
#189690=CARTESIAN_POINT('Ctrl Pts',(14.6907440526957,-17.1870867909918,
12.));
#189691=CARTESIAN_POINT('Ctrl Pts',(14.6864694522319,-17.182736158472,0.));
#189692=CARTESIAN_POINT('Ctrl Pts',(14.6864694522319,-17.182736158472,12.));
#189693=CARTESIAN_POINT('Ctrl Pts',(14.6824178576166,-17.1785800350827,
0.));
#189694=CARTESIAN_POINT('Ctrl Pts',(14.6824178576166,-17.1785800350827,
12.));
#189695=CARTESIAN_POINT('Ctrl Pts',(14.6785925615676,-17.1746247499057,
0.));
#189696=CARTESIAN_POINT('Ctrl Pts',(14.6785925615676,-17.1746247499057,
12.));
#189697=CARTESIAN_POINT('Ctrl Pts',(14.6749971333867,-17.1708771619129,
0.));
#189698=CARTESIAN_POINT('Ctrl Pts',(14.6749971333867,-17.1708771619129,
12.));
#189699=CARTESIAN_POINT('Ctrl Pts',(14.6716355833321,-17.1673449723019,
0.));
#189700=CARTESIAN_POINT('Ctrl Pts',(14.6716355833321,-17.1673449723019,
12.));
#189701=CARTESIAN_POINT('Ctrl Pts',(14.6685123374424,-17.1640366762304,
0.));
#189702=CARTESIAN_POINT('Ctrl Pts',(14.6685123374424,-17.1640366762304,
12.));
#189703=CARTESIAN_POINT('Ctrl Pts',(14.6656319165057,-17.1609609517369,
0.));
#189704=CARTESIAN_POINT('Ctrl Pts',(14.6656319165057,-17.1609609517369,
12.));
#189705=CARTESIAN_POINT('Ctrl Pts',(14.662998728599,-17.1581262646789,0.));
#189706=CARTESIAN_POINT('Ctrl Pts',(14.662998728599,-17.1581262646789,12.));
#189707=CARTESIAN_POINT('Ctrl Pts',(14.660616716964,-17.1555401986403,0.));
#189708=CARTESIAN_POINT('Ctrl Pts',(14.660616716964,-17.1555401986403,12.));
#189709=CARTESIAN_POINT('Ctrl Pts',(14.65849005553,-17.1532107762719,0.));
#189710=CARTESIAN_POINT('Ctrl Pts',(14.65849005553,-17.1532107762719,12.));
#189711=CARTESIAN_POINT('Ctrl Pts',(14.6566237952435,-17.1511476869495,
0.));
#189712=CARTESIAN_POINT('Ctrl Pts',(14.6566237952435,-17.1511476869495,
12.));
#189713=CARTESIAN_POINT('Ctrl Pts',(14.6550248622813,-17.1493641837556,
0.));
#189714=CARTESIAN_POINT('Ctrl Pts',(14.6550248622813,-17.1493641837556,
12.));
#189715=CARTESIAN_POINT('Ctrl Pts',(14.6537016966188,-17.1478763944909,
0.));
#189716=CARTESIAN_POINT('Ctrl Pts',(14.6537016966188,-17.1478763944909,
12.));
#189717=CARTESIAN_POINT('Ctrl Pts',(14.6526624064978,-17.1466998098673,
0.));
#189718=CARTESIAN_POINT('Ctrl Pts',(14.6526624064978,-17.1466998098673,
12.));
#189719=CARTESIAN_POINT('Ctrl Pts',(14.65191316345,-17.1458462295273,0.));
#189720=CARTESIAN_POINT('Ctrl Pts',(14.65191316345,-17.1458462295273,12.));
#189721=CARTESIAN_POINT('Ctrl Pts',(14.6515481598057,-17.1454262858045,
0.));
#189722=CARTESIAN_POINT('Ctrl Pts',(14.6515481598057,-17.1454262858045,
12.));
#189723=CARTESIAN_POINT('Ctrl Pts',(14.6514066997188,-17.1452600887039,
0.));
#189724=CARTESIAN_POINT('Ctrl Pts',(14.6514066997188,-17.1452600887039,
12.));
#189725=CARTESIAN_POINT('Ctrl Pts',(14.6513711852839,-17.1452153999142,
0.));
#189726=CARTESIAN_POINT('Ctrl Pts',(14.6513711852839,-17.1452153999142,
12.));
#189727=CARTESIAN_POINT('Ctrl Pts',(14.6513681262571,-17.1452095830633,
0.));
#189728=CARTESIAN_POINT('Ctrl Pts',(14.6513681262571,-17.1452095830633,
12.));
#189729=CARTESIAN_POINT('',(17.9112098770111,-18.8464468996588,0.));
#189730=CARTESIAN_POINT('Ctrl Pts',(17.9112098770111,-18.8464468996588,
0.));
#189731=CARTESIAN_POINT('Ctrl Pts',(17.9057348246595,-18.8448126709692,
0.));
#189732=CARTESIAN_POINT('Ctrl Pts',(17.8947931177807,-18.8415402351786,
0.));
#189733=CARTESIAN_POINT('Ctrl Pts',(17.8784057509355,-18.8366196462581,
0.));
#189734=CARTESIAN_POINT('Ctrl Pts',(17.856606317477,-18.8300349895974,0.));
#189735=CARTESIAN_POINT('Ctrl Pts',(17.8294410311006,-18.8217643886157,
0.));
#189736=CARTESIAN_POINT('Ctrl Pts',(17.8023598011057,-18.8134540340417,
0.));
#189737=CARTESIAN_POINT('Ctrl Pts',(17.7753627137853,-18.8051039860448,
0.));
#189738=CARTESIAN_POINT('Ctrl Pts',(17.7484498996905,-18.7967143519419,
0.));
#189739=CARTESIAN_POINT('Ctrl Pts',(17.7216215409035,-18.788285297605,0.));
#189740=CARTESIAN_POINT('Ctrl Pts',(17.6948778823014,-18.7798170641374,
0.));
#189741=CARTESIAN_POINT('Ctrl Pts',(17.6682192274236,-18.7713099642754,
0.));
#189742=CARTESIAN_POINT('Ctrl Pts',(17.6416459210681,-18.762764361321,0.));
#189743=CARTESIAN_POINT('Ctrl Pts',(17.6151583357012,-18.7541806530984,
0.));
#189744=CARTESIAN_POINT('Ctrl Pts',(17.5887568561371,-18.7455592536688,
0.));
#189745=CARTESIAN_POINT('Ctrl Pts',(17.5624418653245,-18.7369005764553,
0.));
#189746=CARTESIAN_POINT('Ctrl Pts',(17.5362137287593,-18.7282050157138,
0.));
#189747=CARTESIAN_POINT('Ctrl Pts',(17.5100727820876,-18.7194729318098,
0.));
#189748=CARTESIAN_POINT('Ctrl Pts',(17.4840193397162,-18.7107046613912,
0.));
#189749=CARTESIAN_POINT('Ctrl Pts',(17.4580537012753,-18.70190052503,0.));
#189750=CARTESIAN_POINT('Ctrl Pts',(17.4321761588142,-18.6930608357409,
0.));
#189751=CARTESIAN_POINT('Ctrl Pts',(17.4063870038562,-18.6841859073471,
0.));
#189752=CARTESIAN_POINT('Ctrl Pts',(17.3806865340747,-18.6752760624052,
0.));
#189753=CARTESIAN_POINT('Ctrl Pts',(17.3550750612443,-18.6663316416582,
0.));
#189754=CARTESIAN_POINT('Ctrl Pts',(17.3295529098618,-18.6573530024033,
0.));
#189755=CARTESIAN_POINT('Ctrl Pts',(17.3041204135074,-18.6483405141865,
0.));
#189756=CARTESIAN_POINT('Ctrl Pts',(17.2787779120213,-18.6392945554748,
0.));
#189757=CARTESIAN_POINT('Ctrl Pts',(17.2535257482187,-18.6302155097943,
0.));
#189758=CARTESIAN_POINT('Ctrl Pts',(17.2283642650517,-18.6211037624038,
0.));
#189759=CARTESIAN_POINT('Ctrl Pts',(17.2032938019284,-18.6119596959949,
0.));
#189760=CARTESIAN_POINT('Ctrl Pts',(17.1783146940127,-18.6027836898817,
0.));
#189761=CARTESIAN_POINT('Ctrl Pts',(17.1534272741643,-18.5935761222825,
0.));
#189762=CARTESIAN_POINT('Ctrl Pts',(17.1286318741183,-18.5843373717247,
0.));
#189763=CARTESIAN_POINT('Ctrl Pts',(17.1039288260001,-18.5750678188542,
0.));
#189764=CARTESIAN_POINT('Ctrl Pts',(17.0793184636079,-18.5657678479789,
0.));
#189765=CARTESIAN_POINT('Ctrl Pts',(17.0548011239751,-18.556437848963,0.));
#189766=CARTESIAN_POINT('Ctrl Pts',(17.0303771481738,-18.547078218209,0.));
#189767=CARTESIAN_POINT('Ctrl Pts',(17.0060468805097,-18.5376893576961,
0.));
#189768=CARTESIAN_POINT('Ctrl Pts',(16.981810668038,-18.5282716744197,0.));
#189769=CARTESIAN_POINT('Ctrl Pts',(16.9576688599339,-18.5188255796659,
0.));
#189770=CARTESIAN_POINT('Ctrl Pts',(16.9336218069353,-18.5093514883835,
0.));
#189771=CARTESIAN_POINT('Ctrl Pts',(16.9096698606943,-18.499849818462,0.));
#189772=CARTESIAN_POINT('Ctrl Pts',(16.8858133733088,-18.4903209902227,
0.));
#189773=CARTESIAN_POINT('Ctrl Pts',(16.8620526977171,-18.4807654268771,
0.));
#189774=CARTESIAN_POINT('Ctrl Pts',(16.8383881879709,-18.4711835548623,
0.));
#189775=CARTESIAN_POINT('Ctrl Pts',(16.8148201995472,-18.4615758042305,
0.));
#189776=CARTESIAN_POINT('Ctrl Pts',(16.791349089629,-18.4519426090124,0.));
#189777=CARTESIAN_POINT('Ctrl Pts',(16.7679752173992,-18.44228440761,0.));
#189778=CARTESIAN_POINT('Ctrl Pts',(16.7446989442882,-18.4326016431392,
0.));
#189779=CARTESIAN_POINT('Ctrl Pts',(16.7215206338818,-18.4228947633187,
0.));
#189780=CARTESIAN_POINT('Ctrl Pts',(16.698440651849,-18.413164220399,0.));
#189781=CARTESIAN_POINT('Ctrl Pts',(16.6754593658513,-18.403410471079,0.));
#189782=CARTESIAN_POINT('Ctrl Pts',(16.6525771454513,-18.3936339764332,
0.));
#189783=CARTESIAN_POINT('Ctrl Pts',(16.6297943620056,-18.3838352018327,
0.));
#189784=CARTESIAN_POINT('Ctrl Pts',(16.607111388571,-18.3740146168879,0.));
#189785=CARTESIAN_POINT('Ctrl Pts',(16.5845286000217,-18.3641726955889,
0.));
#189786=CARTESIAN_POINT('Ctrl Pts',(16.5620463731413,-18.354309916433,0.));
#189787=CARTESIAN_POINT('Ctrl Pts',(16.5396650867139,-18.34442676256,0.));
#189788=CARTESIAN_POINT('Ctrl Pts',(16.5173851216045,-18.3345237218864,
0.));
#189789=CARTESIAN_POINT('Ctrl Pts',(16.4952068608345,-18.3246012872469,
0.));
#189790=CARTESIAN_POINT('Ctrl Pts',(16.4731306896441,-18.3146599565231,
0.));
#189791=CARTESIAN_POINT('Ctrl Pts',(16.4511569955233,-18.304700232686,0.));
#189792=CARTESIAN_POINT('Ctrl Pts',(16.4292861682378,-18.294722623851,0.));
#189793=CARTESIAN_POINT('Ctrl Pts',(16.4075185998454,-18.2847276433309,
0.));
#189794=CARTESIAN_POINT('Ctrl Pts',(16.385854684708,-18.2747158096934,0.));
#189795=CARTESIAN_POINT('Ctrl Pts',(16.3642948194868,-18.2646876468169,
0.));
#189796=CARTESIAN_POINT('Ctrl Pts',(16.3428394031589,-18.2546436839608,
0.));
#189797=CARTESIAN_POINT('Ctrl Pts',(16.3214888370987,-18.2445844558742,
0.));
#189798=CARTESIAN_POINT('Ctrl Pts',(16.3002435251378,-18.2345105028982,
0.));
#189799=CARTESIAN_POINT('Ctrl Pts',(16.2791038736223,-18.2244223710746,
0.));
#189800=CARTESIAN_POINT('Ctrl Pts',(16.2580702914615,-18.2143206122529,
0.));
#189801=CARTESIAN_POINT('Ctrl Pts',(16.2371431901638,-18.2042057842035,
0.));
#189802=CARTESIAN_POINT('Ctrl Pts',(16.2163229838875,-18.1940784507229,
0.));
#189803=CARTESIAN_POINT('Ctrl Pts',(16.1956100895073,-18.1839391817331,
0.));
#189804=CARTESIAN_POINT('Ctrl Pts',(16.1750049266671,-18.1737885533849,
0.));
#189805=CARTESIAN_POINT('Ctrl Pts',(16.154507917826,-18.1636271481615,0.));
#189806=CARTESIAN_POINT('Ctrl Pts',(16.1341194882988,-18.1534555549853,
0.));
#189807=CARTESIAN_POINT('Ctrl Pts',(16.1138400662794,-18.1432743693235,
0.));
#189808=CARTESIAN_POINT('Ctrl Pts',(16.0936700829112,-18.1330841933105,
0.));
#189809=CARTESIAN_POINT('Ctrl Pts',(16.0736099723668,-18.1228856358751,
0.));
#189810=CARTESIAN_POINT('Ctrl Pts',(16.0536601719125,-18.112679312869,0.));
#189811=CARTESIAN_POINT('Ctrl Pts',(16.0338211219693,-18.1024658471966,
0.));
#189812=CARTESIAN_POINT('Ctrl Pts',(16.014093266161,-18.0922458689462,0.));
#189813=CARTESIAN_POINT('Ctrl Pts',(15.9944770513613,-18.0820200155236,
0.));
#189814=CARTESIAN_POINT('Ctrl Pts',(15.9749729277846,-18.0717889317958,
0.));
#189815=CARTESIAN_POINT('Ctrl Pts',(15.9555813490644,-18.061553270236,0.));
#189816=CARTESIAN_POINT('Ctrl Pts',(15.9363027723244,-18.0513136910691,
0.));
#189817=CARTESIAN_POINT('Ctrl Pts',(15.9171376582436,-18.0410708624209,
0.));
#189818=CARTESIAN_POINT('Ctrl Pts',(15.8980864711042,-18.0308254604636,
0.));
#189819=CARTESIAN_POINT('Ctrl Pts',(15.8791496788682,-18.0205781695769,
0.));
#189820=CARTESIAN_POINT('Ctrl Pts',(15.8603277532831,-18.0103296825205,
0.));
#189821=CARTESIAN_POINT('Ctrl Pts',(15.8416211699679,-18.0000807006052,
0.));
#189822=CARTESIAN_POINT('Ctrl Pts',(15.8230304084962,-17.9898319338665,
0.));
#189823=CARTESIAN_POINT('Ctrl Pts',(15.8045559524676,-17.9795841012386,
0.));
#189824=CARTESIAN_POINT('Ctrl Pts',(15.7861982895724,-17.9693379307303,
0.));
#189825=CARTESIAN_POINT('Ctrl Pts',(15.7679579117077,-17.9590941596242,
0.));
#189826=CARTESIAN_POINT('Ctrl Pts',(15.749835315086,-17.9488535346781,0.));
#189827=CARTESIAN_POINT('Ctrl Pts',(15.7318310003335,-17.9386168123262,
0.));
#189828=CARTESIAN_POINT('Ctrl Pts',(15.7139454725838,-17.9283847588836,
0.));
#189829=CARTESIAN_POINT('Ctrl Pts',(15.6961792415522,-17.9181581507455,
0.));
#189830=CARTESIAN_POINT('Ctrl Pts',(15.678532821646,-17.9079377746111,0.));
#189831=CARTESIAN_POINT('Ctrl Pts',(15.661006732103,-17.897724427724,0.));
#189832=CARTESIAN_POINT('Ctrl Pts',(15.6436014971084,-17.8875189181091,
0.));
#189833=CARTESIAN_POINT('Ctrl Pts',(15.6263176459108,-17.8773220648125,
0.));
#189834=CARTESIAN_POINT('Ctrl Pts',(15.609155712921,-17.8671346981394,0.));
#189835=CARTESIAN_POINT('Ctrl Pts',(15.5921162378192,-17.8569576599006,
0.));
#189836=CARTESIAN_POINT('Ctrl Pts',(15.5751997657162,-17.8467918036987,
0.));
#189837=CARTESIAN_POINT('Ctrl Pts',(15.5584068472982,-17.8366379952085,
0.));
#189838=CARTESIAN_POINT('Ctrl Pts',(15.541738038964,-17.8264971124607,0.));
#189839=CARTESIAN_POINT('Ctrl Pts',(15.5251939029552,-17.8163700461256,
0.));
#189840=CARTESIAN_POINT('Ctrl Pts',(15.5087750074718,-17.8062576997952,
0.));
#189841=CARTESIAN_POINT('Ctrl Pts',(15.4924819268517,-17.7961609903148,
0.));
#189842=CARTESIAN_POINT('Ctrl Pts',(15.4763152417497,-17.786080848122,0.));
#189843=CARTESIAN_POINT('Ctrl Pts',(15.4602755393017,-17.7760182175815,
0.));
#189844=CARTESIAN_POINT('Ctrl Pts',(15.4443634132869,-17.7659740573265,
0.));
#189845=CARTESIAN_POINT('Ctrl Pts',(15.4285794642667,-17.7559493405881,
0.));
#189846=CARTESIAN_POINT('Ctrl Pts',(15.4129242997837,-17.7459450555813,
0.));
#189847=CARTESIAN_POINT('Ctrl Pts',(15.3973985345802,-17.735962205915,0.));
#189848=CARTESIAN_POINT('Ctrl Pts',(15.3820027907966,-17.7260018109924,
0.));
#189849=CARTESIAN_POINT('Ctrl Pts',(15.3667376981699,-17.7160649064206,
0.));
#189850=CARTESIAN_POINT('Ctrl Pts',(15.351603894206,-17.7061525444042,0.));
#189851=CARTESIAN_POINT('Ctrl Pts',(15.3366020244066,-17.6962657941983,
0.));
#189852=CARTESIAN_POINT('Ctrl Pts',(15.3217327425338,-17.6864057426052,
0.));
#189853=CARTESIAN_POINT('Ctrl Pts',(15.30699671085,-17.676573494456,0.));
#189854=CARTESIAN_POINT('Ctrl Pts',(15.2923946003598,-17.6667701731041,
0.));
#189855=CARTESIAN_POINT('Ctrl Pts',(15.2779270910239,-17.6569969209,0.));
#189856=CARTESIAN_POINT('Ctrl Pts',(15.2635948720292,-17.6472548997328,
0.));
#189857=CARTESIAN_POINT('Ctrl Pts',(15.2493986421092,-17.6375452916369,
0.));
#189858=CARTESIAN_POINT('Ctrl Pts',(15.2353391098366,-17.6278692993764,
0.));
#189859=CARTESIAN_POINT('Ctrl Pts',(15.2214169939199,-17.6182281470468,
0.));
#189860=CARTESIAN_POINT('Ctrl Pts',(15.2076330234686,-17.60862308065,0.));
#189861=CARTESIAN_POINT('Ctrl Pts',(15.1939879383268,-17.5990553687599,
0.));
#189862=CARTESIAN_POINT('Ctrl Pts',(15.1804824894605,-17.5895263032595,
0.));
#189863=CARTESIAN_POINT('Ctrl Pts',(15.1671174393137,-17.580037200054,0.));
#189864=CARTESIAN_POINT('Ctrl Pts',(15.1538935621714,-17.5705893998029,
0.));
#189865=CARTESIAN_POINT('Ctrl Pts',(15.1408116444876,-17.5611842686192,
0.));
#189866=CARTESIAN_POINT('Ctrl Pts',(15.1278724853138,-17.5518231989117,
0.));
#189867=CARTESIAN_POINT('Ctrl Pts',(15.1150768967728,-17.5425076102963,
0.));
#189868=CARTESIAN_POINT('Ctrl Pts',(15.1024257045033,-17.5332389504829,
0.));
#189869=CARTESIAN_POINT('Ctrl Pts',(15.0899197481082,-17.5240186961791,
0.));
#189870=CARTESIAN_POINT('Ctrl Pts',(15.0775598815749,-17.5148483539687,
0.));
#189871=CARTESIAN_POINT('Ctrl Pts',(15.0653469738307,-17.5057294613877,
0.));
#189872=CARTESIAN_POINT('Ctrl Pts',(15.0532819093085,-17.4966635880246,
0.));
#189873=CARTESIAN_POINT('Ctrl Pts',(15.0413655884993,-17.4876523366178,
0.));
#189874=CARTESIAN_POINT('Ctrl Pts',(15.029598928488,-17.4786973441417,0.));
#189875=CARTESIAN_POINT('Ctrl Pts',(15.0179828635087,-17.4698002829357,
0.));
#189876=CARTESIAN_POINT('Ctrl Pts',(15.0065183456922,-17.4609628621419,
0.));
#189877=CARTESIAN_POINT('Ctrl Pts',(14.9952063457779,-17.4521868291005,
0.));
#189878=CARTESIAN_POINT('Ctrl Pts',(14.9840478538357,-17.4434739707773,
0.));
#189879=CARTESIAN_POINT('Ctrl Pts',(14.973043879945,-17.4348261151395,0.));
#189880=CARTESIAN_POINT('Ctrl Pts',(14.9621954549825,-17.4262451327088,
0.));
#189881=CARTESIAN_POINT('Ctrl Pts',(14.9515036315142,-17.4177329382827,
0.));
#189882=CARTESIAN_POINT('Ctrl Pts',(14.940969484645,-17.4092914926072,0.));
#189883=CARTESIAN_POINT('Ctrl Pts',(14.9305941128758,-17.400922804075,0.));
#189884=CARTESIAN_POINT('Ctrl Pts',(14.9203786389343,-17.3926289303987,
0.));
#189885=CARTESIAN_POINT('Ctrl Pts',(14.9103242110057,-17.3844119809823,
0.));
#189886=CARTESIAN_POINT('Ctrl Pts',(14.9004320039609,-17.3762741193075,
0.));
#189887=CARTESIAN_POINT('Ctrl Pts',(14.8907032205789,-17.3682175653236,
0.));
#189888=CARTESIAN_POINT('Ctrl Pts',(14.8811390927424,-17.3602445978163,
0.));
#189889=CARTESIAN_POINT('Ctrl Pts',(14.8717408826957,-17.3523575568648,
0.));
#189890=CARTESIAN_POINT('Ctrl Pts',(14.8625098843419,-17.3445588463477,
0.));
#189891=CARTESIAN_POINT('Ctrl Pts',(14.8534474245433,-17.336850936485,0.));
#189892=CARTESIAN_POINT('Ctrl Pts',(14.8445548643504,-17.3292363662601,
0.));
#189893=CARTESIAN_POINT('Ctrl Pts',(14.8358336004193,-17.3217177462096,
0.));
#189894=CARTESIAN_POINT('Ctrl Pts',(14.8272850675375,-17.3142977632656,
0.));
#189895=CARTESIAN_POINT('Ctrl Pts',(14.8189107410161,-17.3069791853705,
0.));
#189896=CARTESIAN_POINT('Ctrl Pts',(14.8107121391038,-17.2997648661483,
0.));
#189897=CARTESIAN_POINT('Ctrl Pts',(14.8026908254281,-17.2926577496519,
0.));
#189898=CARTESIAN_POINT('Ctrl Pts',(14.7948484105252,-17.28566087332,0.));
#189899=CARTESIAN_POINT('Ctrl Pts',(14.787186553128,-17.278777370485,0.));
#189900=CARTESIAN_POINT('Ctrl Pts',(14.7797069617802,-17.2720104735192,
0.));
#189901=CARTESIAN_POINT('Ctrl Pts',(14.7724113956728,-17.2653635155317,
0.));
#189902=CARTESIAN_POINT('Ctrl Pts',(14.7653016697589,-17.2588399401464,
0.));
#189903=CARTESIAN_POINT('Ctrl Pts',(14.7583796616617,-17.2524433146837,
0.));
#189904=CARTESIAN_POINT('Ctrl Pts',(14.7516473175124,-17.2461773413289,
0.));
#189905=CARTESIAN_POINT('Ctrl Pts',(14.7451066593793,-17.2400458713566,
0.));
#189906=CARTESIAN_POINT('Ctrl Pts',(14.7387597858117,-17.2340529062078,
0.));
#189907=CARTESIAN_POINT('Ctrl Pts',(14.7326088681163,-17.2282025904314,
0.));
#189908=CARTESIAN_POINT('Ctrl Pts',(14.7266561494282,-17.2224992099666,
0.));
#189909=CARTESIAN_POINT('Ctrl Pts',(14.7209039390325,-17.2169471814255,
0.));
#189910=CARTESIAN_POINT('Ctrl Pts',(14.7153546289338,-17.2115510835988,
0.));
#189911=CARTESIAN_POINT('Ctrl Pts',(14.7100107213586,-17.2063157097316,
0.));
#189912=CARTESIAN_POINT('Ctrl Pts',(14.7048748502662,-17.2012461084268,
0.));
#189913=CARTESIAN_POINT('Ctrl Pts',(14.699949811582,-17.1963476411694,0.));
#189914=CARTESIAN_POINT('Ctrl Pts',(14.6952385361706,-17.1916259308416,
0.));
#189915=CARTESIAN_POINT('Ctrl Pts',(14.6907440526957,-17.1870867909918,
0.));
#189916=CARTESIAN_POINT('Ctrl Pts',(14.6864694522319,-17.182736158472,0.));
#189917=CARTESIAN_POINT('Ctrl Pts',(14.6824178576166,-17.1785800350827,
0.));
#189918=CARTESIAN_POINT('Ctrl Pts',(14.6785925615676,-17.1746247499057,
0.));
#189919=CARTESIAN_POINT('Ctrl Pts',(14.6749971333867,-17.1708771619129,
0.));
#189920=CARTESIAN_POINT('Ctrl Pts',(14.6716355833321,-17.1673449723019,
0.));
#189921=CARTESIAN_POINT('Ctrl Pts',(14.6685123374424,-17.1640366762304,
0.));
#189922=CARTESIAN_POINT('Ctrl Pts',(14.6656319165057,-17.1609609517369,
0.));
#189923=CARTESIAN_POINT('Ctrl Pts',(14.662998728599,-17.1581262646789,0.));
#189924=CARTESIAN_POINT('Ctrl Pts',(14.660616716964,-17.1555401986403,0.));
#189925=CARTESIAN_POINT('Ctrl Pts',(14.65849005553,-17.1532107762719,0.));
#189926=CARTESIAN_POINT('Ctrl Pts',(14.6566237952435,-17.1511476869495,
0.));
#189927=CARTESIAN_POINT('Ctrl Pts',(14.6550248622813,-17.1493641837556,
0.));
#189928=CARTESIAN_POINT('Ctrl Pts',(14.6537016966188,-17.1478763944909,
0.));
#189929=CARTESIAN_POINT('Ctrl Pts',(14.6526624064978,-17.1466998098673,
0.));
#189930=CARTESIAN_POINT('Ctrl Pts',(14.65191316345,-17.1458462295273,0.));
#189931=CARTESIAN_POINT('Ctrl Pts',(14.6515481598057,-17.1454262858045,
0.));
#189932=CARTESIAN_POINT('Ctrl Pts',(14.6514066997188,-17.1452600887039,
0.));
#189933=CARTESIAN_POINT('Ctrl Pts',(14.6513711852839,-17.1452153999142,
0.));
#189934=CARTESIAN_POINT('Ctrl Pts',(14.6513681262571,-17.1452095830633,
0.));
#189935=CARTESIAN_POINT('',(17.9112098770111,-18.8464468996588,0.));
#189936=CARTESIAN_POINT('Ctrl Pts',(12.7689476255362,-18.5896416359912,
0.));
#189937=CARTESIAN_POINT('Ctrl Pts',(12.7689476255362,-18.5896416359912,
12.));
#189938=CARTESIAN_POINT('Ctrl Pts',(12.7689524524483,-18.5896460962964,
0.));
#189939=CARTESIAN_POINT('Ctrl Pts',(12.7689524524483,-18.5896460962964,
12.));
#189940=CARTESIAN_POINT('Ctrl Pts',(12.768986426692,-18.5896919669165,0.));
#189941=CARTESIAN_POINT('Ctrl Pts',(12.768986426692,-18.5896919669165,12.));
#189942=CARTESIAN_POINT('Ctrl Pts',(12.769110348199,-18.589871621843,0.));
#189943=CARTESIAN_POINT('Ctrl Pts',(12.769110348199,-18.589871621843,12.));
#189944=CARTESIAN_POINT('Ctrl Pts',(12.7694215127918,-18.5903328777227,
0.));
#189945=CARTESIAN_POINT('Ctrl Pts',(12.7694215127918,-18.5903328777227,
12.));
#189946=CARTESIAN_POINT('Ctrl Pts',(12.7700520897173,-18.5912775137806,
0.));
#189947=CARTESIAN_POINT('Ctrl Pts',(12.7700520897173,-18.5912775137806,
12.));
#189948=CARTESIAN_POINT('Ctrl Pts',(12.7709195951156,-18.5925859134579,
0.));
#189949=CARTESIAN_POINT('Ctrl Pts',(12.7709195951156,-18.5925859134579,
12.));
#189950=CARTESIAN_POINT('Ctrl Pts',(12.7720142287172,-18.5942490615407,
0.));
#189951=CARTESIAN_POINT('Ctrl Pts',(12.7720142287172,-18.5942490615407,
12.));
#189952=CARTESIAN_POINT('Ctrl Pts',(12.7733231262108,-18.5962551167772,
0.));
#189953=CARTESIAN_POINT('Ctrl Pts',(12.7733231262108,-18.5962551167772,
12.));
#189954=CARTESIAN_POINT('Ctrl Pts',(12.7748328937638,-18.598591752595,0.));
#189955=CARTESIAN_POINT('Ctrl Pts',(12.7748328937638,-18.598591752595,12.));
#189956=CARTESIAN_POINT('Ctrl Pts',(12.7765325225081,-18.6012488486709,
0.));
#189957=CARTESIAN_POINT('Ctrl Pts',(12.7765325225081,-18.6012488486709,
12.));
#189958=CARTESIAN_POINT('Ctrl Pts',(12.7784139605066,-18.6042190183704,
0.));
#189959=CARTESIAN_POINT('Ctrl Pts',(12.7784139605066,-18.6042190183704,
12.));
#189960=CARTESIAN_POINT('Ctrl Pts',(12.7804705387658,-18.6074961535723,
0.));
#189961=CARTESIAN_POINT('Ctrl Pts',(12.7804705387658,-18.6074961535723,
12.));
#189962=CARTESIAN_POINT('Ctrl Pts',(12.7826959526924,-18.611074482622,0.));
#189963=CARTESIAN_POINT('Ctrl Pts',(12.7826959526924,-18.611074482622,12.));
#189964=CARTESIAN_POINT('Ctrl Pts',(12.7850831657901,-18.6149475565188,
0.));
#189965=CARTESIAN_POINT('Ctrl Pts',(12.7850831657901,-18.6149475565188,
12.));
#189966=CARTESIAN_POINT('Ctrl Pts',(12.7876249657834,-18.6191087624752,
0.));
#189967=CARTESIAN_POINT('Ctrl Pts',(12.7876249657834,-18.6191087624752,
12.));
#189968=CARTESIAN_POINT('Ctrl Pts',(12.7903142925234,-18.6235516265575,
0.));
#189969=CARTESIAN_POINT('Ctrl Pts',(12.7903142925234,-18.6235516265575,
12.));
#189970=CARTESIAN_POINT('Ctrl Pts',(12.7931447451555,-18.6282702819371,
0.));
#189971=CARTESIAN_POINT('Ctrl Pts',(12.7931447451555,-18.6282702819371,
12.));
#189972=CARTESIAN_POINT('Ctrl Pts',(12.796110622225,-18.6332595057006,0.));
#189973=CARTESIAN_POINT('Ctrl Pts',(12.796110622225,-18.6332595057006,12.));
#189974=CARTESIAN_POINT('Ctrl Pts',(12.7992066625264,-18.63851447924,0.));
#189975=CARTESIAN_POINT('Ctrl Pts',(12.7992066625264,-18.63851447924,12.));
#189976=CARTESIAN_POINT('Ctrl Pts',(12.8024278770152,-18.6440306327456,
0.));
#189977=CARTESIAN_POINT('Ctrl Pts',(12.8024278770152,-18.6440306327456,
12.));
#189978=CARTESIAN_POINT('Ctrl Pts',(12.805769331162,-18.6498034438987,0.));
#189979=CARTESIAN_POINT('Ctrl Pts',(12.805769331162,-18.6498034438987,12.));
#189980=CARTESIAN_POINT('Ctrl Pts',(12.8092261933858,-18.6558284825773,
0.));
#189981=CARTESIAN_POINT('Ctrl Pts',(12.8092261933858,-18.6558284825773,
12.));
#189982=CARTESIAN_POINT('Ctrl Pts',(12.8127937909631,-18.6621014624746,
0.));
#189983=CARTESIAN_POINT('Ctrl Pts',(12.8127937909631,-18.6621014624746,
12.));
#189984=CARTESIAN_POINT('Ctrl Pts',(12.8164676687362,-18.66861829528,0.));
#189985=CARTESIAN_POINT('Ctrl Pts',(12.8164676687362,-18.66861829528,12.));
#189986=CARTESIAN_POINT('Ctrl Pts',(12.8202436318474,-18.6753751301092,
0.));
#189987=CARTESIAN_POINT('Ctrl Pts',(12.8202436318474,-18.6753751301092,
12.));
#189988=CARTESIAN_POINT('Ctrl Pts',(12.8241176980017,-18.6823683094139,
0.));
#189989=CARTESIAN_POINT('Ctrl Pts',(12.8241176980017,-18.6823683094139,
12.));
#189990=CARTESIAN_POINT('Ctrl Pts',(12.8280860635231,-18.6895943376172,
0.));
#189991=CARTESIAN_POINT('Ctrl Pts',(12.8280860635231,-18.6895943376172,
12.));
#189992=CARTESIAN_POINT('Ctrl Pts',(12.8321450599789,-18.6970498410172,
0.));
#189993=CARTESIAN_POINT('Ctrl Pts',(12.8321450599789,-18.6970498410172,
12.));
#189994=CARTESIAN_POINT('Ctrl Pts',(12.8362911280361,-18.7047315436294,
0.));
#189995=CARTESIAN_POINT('Ctrl Pts',(12.8362911280361,-18.7047315436294,
12.));
#189996=CARTESIAN_POINT('Ctrl Pts',(12.8405208263431,-18.7126362754445,
0.));
#189997=CARTESIAN_POINT('Ctrl Pts',(12.8405208263431,-18.7126362754445,
12.));
#189998=CARTESIAN_POINT('Ctrl Pts',(12.8448308329494,-18.7207609737702,
0.));
#189999=CARTESIAN_POINT('Ctrl Pts',(12.8448308329494,-18.7207609737702,
12.));
#190000=CARTESIAN_POINT('Ctrl Pts',(12.8492179511591,-18.7291026886554,
0.));
#190001=CARTESIAN_POINT('Ctrl Pts',(12.8492179511591,-18.7291026886554,
12.));
#190002=CARTESIAN_POINT('Ctrl Pts',(12.8536791086316,-18.7376585820854,
0.));
#190003=CARTESIAN_POINT('Ctrl Pts',(12.8536791086316,-18.7376585820854,
12.));
#190004=CARTESIAN_POINT('Ctrl Pts',(12.8582113455646,-18.7464259171251,
0.));
#190005=CARTESIAN_POINT('Ctrl Pts',(12.8582113455646,-18.7464259171251,
12.));
#190006=CARTESIAN_POINT('Ctrl Pts',(12.8628118054171,-18.7554020493887,
0.));
#190007=CARTESIAN_POINT('Ctrl Pts',(12.8628118054171,-18.7554020493887,
12.));
#190008=CARTESIAN_POINT('Ctrl Pts',(12.8674777239653,-18.7645844169564,
0.));
#190009=CARTESIAN_POINT('Ctrl Pts',(12.8674777239653,-18.7645844169564,
12.));
#190010=CARTESIAN_POINT('Ctrl Pts',(12.872206421181,-18.7739705329022,0.));
#190011=CARTESIAN_POINT('Ctrl Pts',(12.872206421181,-18.7739705329022,12.));
#190012=CARTESIAN_POINT('Ctrl Pts',(12.8769952998095,-18.7835579840477,
0.));
#190013=CARTESIAN_POINT('Ctrl Pts',(12.8769952998095,-18.7835579840477,
12.));
#190014=CARTESIAN_POINT('Ctrl Pts',(12.8818418427475,-18.7933444285868,
0.));
#190015=CARTESIAN_POINT('Ctrl Pts',(12.8818418427475,-18.7933444285868,
12.));
#190016=CARTESIAN_POINT('Ctrl Pts',(12.8867436109546,-18.8033275941943,
0.));
#190017=CARTESIAN_POINT('Ctrl Pts',(12.8867436109546,-18.8033275941943,
12.));
#190018=CARTESIAN_POINT('Ctrl Pts',(12.8916982409935,-18.813505275782,0.));
#190019=CARTESIAN_POINT('Ctrl Pts',(12.8916982409935,-18.813505275782,12.));
#190020=CARTESIAN_POINT('Ctrl Pts',(12.8967034410754,-18.8238753319129,
0.));
#190021=CARTESIAN_POINT('Ctrl Pts',(12.8967034410754,-18.8238753319129,
12.));
#190022=CARTESIAN_POINT('Ctrl Pts',(12.9017569871738,-18.8344356812591,
0.));
#190023=CARTESIAN_POINT('Ctrl Pts',(12.9017569871738,-18.8344356812591,
12.));
#190024=CARTESIAN_POINT('Ctrl Pts',(12.9068567191854,-18.8451842990984,
0.));
#190025=CARTESIAN_POINT('Ctrl Pts',(12.9068567191854,-18.8451842990984,
12.));
#190026=CARTESIAN_POINT('Ctrl Pts',(12.9120005369063,-18.8561192136198,
0.));
#190027=CARTESIAN_POINT('Ctrl Pts',(12.9120005369063,-18.8561192136198,
12.));
#190028=CARTESIAN_POINT('Ctrl Pts',(12.9171863977045,-18.8672385038326,
0.));
#190029=CARTESIAN_POINT('Ctrl Pts',(12.9171863977045,-18.8672385038326,
12.));
#190030=CARTESIAN_POINT('Ctrl Pts',(12.9224123144981,-18.8785402977528,
0.));
#190031=CARTESIAN_POINT('Ctrl Pts',(12.9224123144981,-18.8785402977528,
12.));
#190032=CARTESIAN_POINT('Ctrl Pts',(12.9276763536373,-18.8900227704889,
0.));
#190033=CARTESIAN_POINT('Ctrl Pts',(12.9276763536373,-18.8900227704889,
12.));
#190034=CARTESIAN_POINT('Ctrl Pts',(12.9329766328184,-18.9016841423403,
0.));
#190035=CARTESIAN_POINT('Ctrl Pts',(12.9329766328184,-18.9016841423403,
12.));
#190036=CARTESIAN_POINT('Ctrl Pts',(12.9383113190374,-18.9135226769466,
0.));
#190037=CARTESIAN_POINT('Ctrl Pts',(12.9383113190374,-18.9135226769466,
12.));
#190038=CARTESIAN_POINT('Ctrl Pts',(12.9436786266105,-18.9255366795195,
0.));
#190039=CARTESIAN_POINT('Ctrl Pts',(12.9436786266105,-18.9255366795195,
12.));
#190040=CARTESIAN_POINT('Ctrl Pts',(12.9490768151821,-18.9377244950435,
0.));
#190041=CARTESIAN_POINT('Ctrl Pts',(12.9490768151821,-18.9377244950435,
12.));
#190042=CARTESIAN_POINT('Ctrl Pts',(12.9545041877377,-18.9500845064715,
0.));
#190043=CARTESIAN_POINT('Ctrl Pts',(12.9545041877377,-18.9500845064715,
12.));
#190044=CARTESIAN_POINT('Ctrl Pts',(12.9599590886319,-18.9626151329229,
0.));
#190045=CARTESIAN_POINT('Ctrl Pts',(12.9599590886319,-18.9626151329229,
12.));
#190046=CARTESIAN_POINT('Ctrl Pts',(12.9654399021869,-18.9753148284475,
0.));
#190047=CARTESIAN_POINT('Ctrl Pts',(12.9654399021869,-18.9753148284475,
12.));
#190048=CARTESIAN_POINT('Ctrl Pts',(12.9709450512747,-18.9881820807586,
0.));
#190049=CARTESIAN_POINT('Ctrl Pts',(12.9709450512747,-18.9881820807586,
12.));
#190050=CARTESIAN_POINT('Ctrl Pts',(12.9764729959205,-19.0012154099791,
0.));
#190051=CARTESIAN_POINT('Ctrl Pts',(12.9764729959205,-19.0012154099791,
12.));
#190052=CARTESIAN_POINT('Ctrl Pts',(12.9820222318715,-19.0144133673348,
0.));
#190053=CARTESIAN_POINT('Ctrl Pts',(12.9820222318715,-19.0144133673348,
12.));
#190054=CARTESIAN_POINT('Ctrl Pts',(12.9875912893003,-19.0277745339908,
0.));
#190055=CARTESIAN_POINT('Ctrl Pts',(12.9875912893003,-19.0277745339908,
12.));
#190056=CARTESIAN_POINT('Ctrl Pts',(12.9931787316514,-19.0412975200398,
0.));
#190057=CARTESIAN_POINT('Ctrl Pts',(12.9931787316514,-19.0412975200398,
12.));
#190058=CARTESIAN_POINT('Ctrl Pts',(12.9987831544502,-19.0549809634355,
0.));
#190059=CARTESIAN_POINT('Ctrl Pts',(12.9987831544502,-19.0549809634355,
12.));
#190060=CARTESIAN_POINT('Ctrl Pts',(13.0044031841381,-19.0688235289437,
0.));
#190061=CARTESIAN_POINT('Ctrl Pts',(13.0044031841381,-19.0688235289437,
12.));
#190062=CARTESIAN_POINT('Ctrl Pts',(13.0100374768785,-19.0828239070482,
0.));
#190063=CARTESIAN_POINT('Ctrl Pts',(13.0100374768785,-19.0828239070482,
12.));
#190064=CARTESIAN_POINT('Ctrl Pts',(13.0156847176093,-19.0969808131226,
0.));
#190065=CARTESIAN_POINT('Ctrl Pts',(13.0156847176093,-19.0969808131226,
12.));
#190066=CARTESIAN_POINT('Ctrl Pts',(13.0213436191326,-19.1112929866308,
0.));
#190067=CARTESIAN_POINT('Ctrl Pts',(13.0213436191326,-19.1112929866308,
12.));
#190068=CARTESIAN_POINT('Ctrl Pts',(13.0270129211976,-19.1257591903099,
0.));
#190069=CARTESIAN_POINT('Ctrl Pts',(13.0270129211976,-19.1257591903099,
12.));
#190070=CARTESIAN_POINT('Ctrl Pts',(13.0326913895841,-19.1403782093389,
0.));
#190071=CARTESIAN_POINT('Ctrl Pts',(13.0326913895841,-19.1403782093389,
12.));
#190072=CARTESIAN_POINT('Ctrl Pts',(13.0383778152072,-19.1551488505233,
0.));
#190073=CARTESIAN_POINT('Ctrl Pts',(13.0383778152072,-19.1551488505233,
12.));
#190074=CARTESIAN_POINT('Ctrl Pts',(13.0440710133775,-19.1700699416625,
0.));
#190075=CARTESIAN_POINT('Ctrl Pts',(13.0440710133775,-19.1700699416625,
12.));
#190076=CARTESIAN_POINT('Ctrl Pts',(13.0497698230442,-19.1851403308826,
0.));
#190077=CARTESIAN_POINT('Ctrl Pts',(13.0497698230442,-19.1851403308826,
12.));
#190078=CARTESIAN_POINT('Ctrl Pts',(13.0554731060537,-19.2003588859771,
0.));
#190079=CARTESIAN_POINT('Ctrl Pts',(13.0554731060537,-19.2003588859771,
12.));
#190080=CARTESIAN_POINT('Ctrl Pts',(13.0611797463912,-19.2157244937141,
0.));
#190081=CARTESIAN_POINT('Ctrl Pts',(13.0611797463912,-19.2157244937141,
12.));
#190082=CARTESIAN_POINT('Ctrl Pts',(13.0668886494791,-19.2312360592031,
0.));
#190083=CARTESIAN_POINT('Ctrl Pts',(13.0668886494791,-19.2312360592031,
12.));
#190084=CARTESIAN_POINT('Ctrl Pts',(13.0725987415856,-19.2468925053988,
0.));
#190085=CARTESIAN_POINT('Ctrl Pts',(13.0725987415856,-19.2468925053988,
12.));
#190086=CARTESIAN_POINT('Ctrl Pts',(13.0783089692117,-19.2626927725596,
0.));
#190087=CARTESIAN_POINT('Ctrl Pts',(13.0783089692117,-19.2626927725596,
12.));
#190088=CARTESIAN_POINT('Ctrl Pts',(13.0840182984949,-19.2786358177198,
0.));
#190089=CARTESIAN_POINT('Ctrl Pts',(13.0840182984949,-19.2786358177198,
12.));
#190090=CARTESIAN_POINT('Ctrl Pts',(13.0897257145969,-19.2947206141246,
0.));
#190091=CARTESIAN_POINT('Ctrl Pts',(13.0897257145969,-19.2947206141246,
12.));
#190092=CARTESIAN_POINT('Ctrl Pts',(13.095430221148,-19.3109461507358,0.));
#190093=CARTESIAN_POINT('Ctrl Pts',(13.095430221148,-19.3109461507358,12.));
#190094=CARTESIAN_POINT('Ctrl Pts',(13.1011308397591,-19.3273114318268,
0.));
#190095=CARTESIAN_POINT('Ctrl Pts',(13.1011308397591,-19.3273114318268,
12.));
#190096=CARTESIAN_POINT('Ctrl Pts',(13.1068266095186,-19.3438154765395,
0.));
#190097=CARTESIAN_POINT('Ctrl Pts',(13.1068266095186,-19.3438154765395,
12.));
#190098=CARTESIAN_POINT('Ctrl Pts',(13.1125165865021,-19.3604573184516,
0.));
#190099=CARTESIAN_POINT('Ctrl Pts',(13.1125165865021,-19.3604573184516,
12.));
#190100=CARTESIAN_POINT('Ctrl Pts',(13.118199843271,-19.3772360051093,0.));
#190101=CARTESIAN_POINT('Ctrl Pts',(13.118199843271,-19.3772360051093,12.));
#190102=CARTESIAN_POINT('Ctrl Pts',(13.1238754684177,-19.3941505976267,
0.));
#190103=CARTESIAN_POINT('Ctrl Pts',(13.1238754684177,-19.3941505976267,
12.));
#190104=CARTESIAN_POINT('Ctrl Pts',(13.1295425661635,-19.4112001703561,
0.));
#190105=CARTESIAN_POINT('Ctrl Pts',(13.1295425661635,-19.4112001703561,
12.));
#190106=CARTESIAN_POINT('Ctrl Pts',(13.1352002559439,-19.4283838105265,
0.));
#190107=CARTESIAN_POINT('Ctrl Pts',(13.1352002559439,-19.4283838105265,
12.));
#190108=CARTESIAN_POINT('Ctrl Pts',(13.140847672006,-19.4457006178875,0.));
#190109=CARTESIAN_POINT('Ctrl Pts',(13.140847672006,-19.4457006178875,12.));
#190110=CARTESIAN_POINT('Ctrl Pts',(13.1464839629966,-19.463149704325,0.));
#190111=CARTESIAN_POINT('Ctrl Pts',(13.1464839629966,-19.463149704325,12.));
#190112=CARTESIAN_POINT('Ctrl Pts',(13.1521082915846,-19.4807301935256,
0.));
#190113=CARTESIAN_POINT('Ctrl Pts',(13.1521082915846,-19.4807301935256,
12.));
#190114=CARTESIAN_POINT('Ctrl Pts',(13.1577198341238,-19.498441220707,0.));
#190115=CARTESIAN_POINT('Ctrl Pts',(13.1577198341238,-19.498441220707,12.));
#190116=CARTESIAN_POINT('Ctrl Pts',(13.1633177803097,-19.5162819323207,
0.));
#190117=CARTESIAN_POINT('Ctrl Pts',(13.1633177803097,-19.5162819323207,
12.));
#190118=CARTESIAN_POINT('Ctrl Pts',(13.1689013328432,-19.5342514857564,
0.));
#190119=CARTESIAN_POINT('Ctrl Pts',(13.1689013328432,-19.5342514857564,
12.));
#190120=CARTESIAN_POINT('Ctrl Pts',(13.1744697070918,-19.5523490490254,
0.));
#190121=CARTESIAN_POINT('Ctrl Pts',(13.1744697070918,-19.5523490490254,
12.));
#190122=CARTESIAN_POINT('Ctrl Pts',(13.1800221307682,-19.5705738004682,
0.));
#190123=CARTESIAN_POINT('Ctrl Pts',(13.1800221307682,-19.5705738004682,
12.));
#190124=CARTESIAN_POINT('Ctrl Pts',(13.1855578436479,-19.5889249285352,
0.));
#190125=CARTESIAN_POINT('Ctrl Pts',(13.1855578436479,-19.5889249285352,
12.));
#190126=CARTESIAN_POINT('Ctrl Pts',(13.1910760972818,-19.6074016315421,
0.));
#190127=CARTESIAN_POINT('Ctrl Pts',(13.1910760972818,-19.6074016315421,
12.));
#190128=CARTESIAN_POINT('Ctrl Pts',(13.196576154715,-19.6260031174244,0.));
#190129=CARTESIAN_POINT('Ctrl Pts',(13.196576154715,-19.6260031174244,12.));
#190130=CARTESIAN_POINT('Ctrl Pts',(13.202057290206,-19.6447286034764,0.));
#190131=CARTESIAN_POINT('Ctrl Pts',(13.202057290206,-19.6447286034764,12.));
#190132=CARTESIAN_POINT('Ctrl Pts',(13.2075187889522,-19.6635773160924,
0.));
#190133=CARTESIAN_POINT('Ctrl Pts',(13.2075187889522,-19.6635773160924,
12.));
#190134=CARTESIAN_POINT('Ctrl Pts',(13.2129599468478,-19.6825484905812,
0.));
#190135=CARTESIAN_POINT('Ctrl Pts',(13.2129599468478,-19.6825484905812,
12.));
#190136=CARTESIAN_POINT('Ctrl Pts',(13.2183800702431,-19.7016413709678,
0.));
#190137=CARTESIAN_POINT('Ctrl Pts',(13.2183800702431,-19.7016413709678,
12.));
#190138=CARTESIAN_POINT('Ctrl Pts',(13.2237784757065,-19.7208552097867,
0.));
#190139=CARTESIAN_POINT('Ctrl Pts',(13.2237784757065,-19.7208552097867,
12.));
#190140=CARTESIAN_POINT('Ctrl Pts',(13.2291544897902,-19.7401892678701,
0.));
#190141=CARTESIAN_POINT('Ctrl Pts',(13.2291544897902,-19.7401892678701,
12.));
#190142=CARTESIAN_POINT('Ctrl Pts',(13.2345074487968,-19.7596428141176,
0.));
#190143=CARTESIAN_POINT('Ctrl Pts',(13.2345074487968,-19.7596428141176,
12.));
#190144=CARTESIAN_POINT('Ctrl Pts',(13.239836698568,-19.7792151253297,0.));
#190145=CARTESIAN_POINT('Ctrl Pts',(13.239836698568,-19.7792151253297,12.));
#190146=CARTESIAN_POINT('Ctrl Pts',(13.2451415942809,-19.7989054860501,
0.));
#190147=CARTESIAN_POINT('Ctrl Pts',(13.2451415942809,-19.7989054860501,
12.));
#190148=CARTESIAN_POINT('Ctrl Pts',(13.2504215002458,-19.8187131883919,
0.));
#190149=CARTESIAN_POINT('Ctrl Pts',(13.2504215002458,-19.8187131883919,
12.));
#190150=CARTESIAN_POINT('Ctrl Pts',(13.2556757897085,-19.8386375318632,
0.));
#190151=CARTESIAN_POINT('Ctrl Pts',(13.2556757897085,-19.8386375318632,
12.));
#190152=CARTESIAN_POINT('Ctrl Pts',(13.2609038446525,-19.8586778231711,
0.));
#190153=CARTESIAN_POINT('Ctrl Pts',(13.2609038446525,-19.8586778231711,
12.));
#190154=CARTESIAN_POINT('Ctrl Pts',(13.2661050556128,-19.8788333760571,
0.));
#190155=CARTESIAN_POINT('Ctrl Pts',(13.2661050556128,-19.8788333760571,
12.));
#190156=CARTESIAN_POINT('Ctrl Pts',(13.2712788215015,-19.8991035111739,
0.));
#190157=CARTESIAN_POINT('Ctrl Pts',(13.2712788215015,-19.8991035111739,
12.));
#190158=CARTESIAN_POINT('Ctrl Pts',(13.2764245494354,-19.9194875559419,
0.));
#190159=CARTESIAN_POINT('Ctrl Pts',(13.2764245494354,-19.9194875559419,
12.));
#190160=CARTESIAN_POINT('Ctrl Pts',(13.2815416545662,-19.939984844402,0.));
#190161=CARTESIAN_POINT('Ctrl Pts',(13.2815416545662,-19.939984844402,12.));
#190162=CARTESIAN_POINT('Ctrl Pts',(13.2866295599152,-19.9605947170589,
0.));
#190163=CARTESIAN_POINT('Ctrl Pts',(13.2866295599152,-19.9605947170589,
12.));
#190164=CARTESIAN_POINT('Ctrl Pts',(13.2916876962098,-19.9813165207174,
0.));
#190165=CARTESIAN_POINT('Ctrl Pts',(13.2916876962098,-19.9813165207174,
12.));
#190166=CARTESIAN_POINT('Ctrl Pts',(13.296715501731,-20.0021496083742,0.));
#190167=CARTESIAN_POINT('Ctrl Pts',(13.296715501731,-20.0021496083742,12.));
#190168=CARTESIAN_POINT('Ctrl Pts',(13.3017124221639,-20.023093339104,0.));
#190169=CARTESIAN_POINT('Ctrl Pts',(13.3017124221639,-20.023093339104,12.));
#190170=CARTESIAN_POINT('Ctrl Pts',(13.3066779104515,-20.0441470779345,
0.));
#190171=CARTESIAN_POINT('Ctrl Pts',(13.3066779104515,-20.0441470779345,
12.));
#190172=CARTESIAN_POINT('Ctrl Pts',(13.3116114266514,-20.0653101957188,
0.));
#190173=CARTESIAN_POINT('Ctrl Pts',(13.3116114266514,-20.0653101957188,
12.));
#190174=CARTESIAN_POINT('Ctrl Pts',(13.3165124377962,-20.0865820689884,
0.));
#190175=CARTESIAN_POINT('Ctrl Pts',(13.3165124377962,-20.0865820689884,
12.));
#190176=CARTESIAN_POINT('Ctrl Pts',(13.3213804177588,-20.1079620798377,
0.));
#190177=CARTESIAN_POINT('Ctrl Pts',(13.3213804177588,-20.1079620798377,
12.));
#190178=CARTESIAN_POINT('Ctrl Pts',(13.3262148471228,-20.1294496158405,
0.));
#190179=CARTESIAN_POINT('Ctrl Pts',(13.3262148471228,-20.1294496158405,
12.));
#190180=CARTESIAN_POINT('Ctrl Pts',(13.3310152130565,-20.1510440699477,
0.));
#190181=CARTESIAN_POINT('Ctrl Pts',(13.3310152130565,-20.1510440699477,
12.));
#190182=CARTESIAN_POINT('Ctrl Pts',(13.3357810091903,-20.1727448403818,
0.));
#190183=CARTESIAN_POINT('Ctrl Pts',(13.3357810091903,-20.1727448403818,
12.));
#190184=CARTESIAN_POINT('Ctrl Pts',(13.3405117354969,-20.1945513305233,
0.));
#190185=CARTESIAN_POINT('Ctrl Pts',(13.3405117354969,-20.1945513305233,
12.));
#190186=CARTESIAN_POINT('Ctrl Pts',(13.3452068981762,-20.2164629487855,
0.));
#190187=CARTESIAN_POINT('Ctrl Pts',(13.3452068981762,-20.2164629487855,
12.));
#190188=CARTESIAN_POINT('Ctrl Pts',(13.3498660095381,-20.2384791085354,
0.));
#190189=CARTESIAN_POINT('Ctrl Pts',(13.3498660095381,-20.2384791085354,
12.));
#190190=CARTESIAN_POINT('Ctrl Pts',(13.3544885878886,-20.2605992280117,
0.));
#190191=CARTESIAN_POINT('Ctrl Pts',(13.3544885878886,-20.2605992280117,
12.));
#190192=CARTESIAN_POINT('Ctrl Pts',(13.3590741574194,-20.2828227302337,
0.));
#190193=CARTESIAN_POINT('Ctrl Pts',(13.3590741574194,-20.2828227302337,
12.));
#190194=CARTESIAN_POINT('Ctrl Pts',(13.3636222481016,-20.3051490429049,
0.));
#190195=CARTESIAN_POINT('Ctrl Pts',(13.3636222481016,-20.3051490429049,
12.));
#190196=CARTESIAN_POINT('Ctrl Pts',(13.3681323955828,-20.3275775983032,
0.));
#190197=CARTESIAN_POINT('Ctrl Pts',(13.3681323955828,-20.3275775983032,
12.));
#190198=CARTESIAN_POINT('Ctrl Pts',(13.3726041410869,-20.3501078331818,
0.));
#190199=CARTESIAN_POINT('Ctrl Pts',(13.3726041410869,-20.3501078331818,
12.));
#190200=CARTESIAN_POINT('Ctrl Pts',(13.377037031319,-20.3727391887187,0.));
#190201=CARTESIAN_POINT('Ctrl Pts',(13.377037031319,-20.3727391887187,12.));
#190202=CARTESIAN_POINT('Ctrl Pts',(13.3814306183721,-20.3954711104505,
0.));
#190203=CARTESIAN_POINT('Ctrl Pts',(13.3814306183721,-20.3954711104505,
12.));
#190204=CARTESIAN_POINT('Ctrl Pts',(13.3857844596387,-20.4183030482002,
0.));
#190205=CARTESIAN_POINT('Ctrl Pts',(13.3857844596387,-20.4183030482002,
12.));
#190206=CARTESIAN_POINT('Ctrl Pts',(13.3900981177254,-20.4412344560007,
0.));
#190207=CARTESIAN_POINT('Ctrl Pts',(13.3900981177254,-20.4412344560007,
12.));
#190208=CARTESIAN_POINT('Ctrl Pts',(13.3943711603739,-20.4642647920038,
0.));
#190209=CARTESIAN_POINT('Ctrl Pts',(13.3943711603739,-20.4642647920038,
12.));
#190210=CARTESIAN_POINT('Ctrl Pts',(13.3986031603716,-20.4873935184041,
0.));
#190211=CARTESIAN_POINT('Ctrl Pts',(13.3986031603716,-20.4873935184041,
12.));
#190212=CARTESIAN_POINT('Ctrl Pts',(13.4027936954529,-20.5106201013755,
0.));
#190213=CARTESIAN_POINT('Ctrl Pts',(13.4027936954529,-20.5106201013755,
12.));
#190214=CARTESIAN_POINT('Ctrl Pts',(13.4069423482076,-20.5339440109958,
0.));
#190215=CARTESIAN_POINT('Ctrl Pts',(13.4069423482076,-20.5339440109958,
12.));
#190216=CARTESIAN_POINT('Ctrl Pts',(13.4110487059912,-20.557364721164,0.));
#190217=CARTESIAN_POINT('Ctrl Pts',(13.4110487059912,-20.557364721164,12.));
#190218=CARTESIAN_POINT('Ctrl Pts',(13.415112360841,-20.5808817095155,0.));
#190219=CARTESIAN_POINT('Ctrl Pts',(13.415112360841,-20.5808817095155,12.));
#190220=CARTESIAN_POINT('Ctrl Pts',(13.4191329093931,-20.6044944573151,
0.));
#190221=CARTESIAN_POINT('Ctrl Pts',(13.4191329093931,-20.6044944573151,
12.));
#190222=CARTESIAN_POINT('Ctrl Pts',(13.4231099528178,-20.6282024494234,
0.));
#190223=CARTESIAN_POINT('Ctrl Pts',(13.4231099528178,-20.6282024494234,
12.));
#190224=CARTESIAN_POINT('Ctrl Pts',(13.427043096765,-20.6520051742868,0.));
#190225=CARTESIAN_POINT('Ctrl Pts',(13.427043096765,-20.6520051742868,12.));
#190226=CARTESIAN_POINT('Ctrl Pts',(13.4309319513119,-20.6759021239102,
0.));
#190227=CARTESIAN_POINT('Ctrl Pts',(13.4309319513119,-20.6759021239102,
12.));
#190228=CARTESIAN_POINT('Ctrl Pts',(13.4347761309154,-20.6998927938288,
0.));
#190229=CARTESIAN_POINT('Ctrl Pts',(13.4347761309154,-20.6998927938288,
12.));
#190230=CARTESIAN_POINT('Ctrl Pts',(13.4385752543663,-20.7239766830676,
0.));
#190231=CARTESIAN_POINT('Ctrl Pts',(13.4385752543663,-20.7239766830676,
12.));
#190232=CARTESIAN_POINT('Ctrl Pts',(13.4423289447561,-20.7481532941014,
0.));
#190233=CARTESIAN_POINT('Ctrl Pts',(13.4423289447561,-20.7481532941014,
12.));
#190234=CARTESIAN_POINT('Ctrl Pts',(13.4460368293689,-20.7724221327609,
0.));
#190235=CARTESIAN_POINT('Ctrl Pts',(13.4460368293689,-20.7724221327609,
12.));
#190236=CARTESIAN_POINT('Ctrl Pts',(13.4496985395637,-20.7967827081228,
0.));
#190237=CARTESIAN_POINT('Ctrl Pts',(13.4496985395637,-20.7967827081228,
12.));
#190238=CARTESIAN_POINT('Ctrl Pts',(13.4533137106667,-20.821234532398,0.));
#190239=CARTESIAN_POINT('Ctrl Pts',(13.4533137106667,-20.821234532398,12.));
#190240=CARTESIAN_POINT('Ctrl Pts',(13.4568819818631,-20.8457771208083,
0.));
#190241=CARTESIAN_POINT('Ctrl Pts',(13.4568819818631,-20.8457771208083,
12.));
#190242=CARTESIAN_POINT('Ctrl Pts',(13.4604029960983,-20.8704099914641,
0.));
#190243=CARTESIAN_POINT('Ctrl Pts',(13.4604029960983,-20.8704099914641,
12.));
#190244=CARTESIAN_POINT('Ctrl Pts',(13.4638763999725,-20.8951326652158,
0.));
#190245=CARTESIAN_POINT('Ctrl Pts',(13.4638763999725,-20.8951326652158,
12.));
#190246=CARTESIAN_POINT('Ctrl Pts',(13.4673018437717,-20.9199446657583,
0.));
#190247=CARTESIAN_POINT('Ctrl Pts',(13.4673018437717,-20.9199446657583,
12.));
#190248=CARTESIAN_POINT('Ctrl Pts',(13.4706789815166,-20.9448455197557,
0.));
#190249=CARTESIAN_POINT('Ctrl Pts',(13.4706789815166,-20.9448455197557,
12.));
#190250=CARTESIAN_POINT('Ctrl Pts',(13.4740074710086,-20.9698347569477,
0.));
#190251=CARTESIAN_POINT('Ctrl Pts',(13.4740074710086,-20.9698347569477,
12.));
#190252=CARTESIAN_POINT('Ctrl Pts',(13.4772869738878,-20.9949119102592,
0.));
#190253=CARTESIAN_POINT('Ctrl Pts',(13.4772869738878,-20.9949119102592,
12.));
#190254=CARTESIAN_POINT('Ctrl Pts',(13.4805171556822,-21.0200765158884,
0.));
#190255=CARTESIAN_POINT('Ctrl Pts',(13.4805171556822,-21.0200765158884,
12.));
#190256=CARTESIAN_POINT('Ctrl Pts',(13.4836976858912,-21.0453281134245,
0.));
#190257=CARTESIAN_POINT('Ctrl Pts',(13.4836976858912,-21.0453281134245,
12.));
#190258=CARTESIAN_POINT('Ctrl Pts',(13.4868282377191,-21.0706662455199,
0.));
#190259=CARTESIAN_POINT('Ctrl Pts',(13.4868282377191,-21.0706662455199,
12.));
#190260=CARTESIAN_POINT('Ctrl Pts',(13.4899084877717,-21.0960904575046,
0.));
#190261=CARTESIAN_POINT('Ctrl Pts',(13.4899084877717,-21.0960904575046,
12.));
#190262=CARTESIAN_POINT('Ctrl Pts',(13.4929381157778,-21.1216002970207,
0.));
#190263=CARTESIAN_POINT('Ctrl Pts',(13.4929381157778,-21.1216002970207,
12.));
#190264=CARTESIAN_POINT('Ctrl Pts',(13.4959168042934,-21.1471953136209,
0.));
#190265=CARTESIAN_POINT('Ctrl Pts',(13.4959168042934,-21.1471953136209,
12.));
#190266=CARTESIAN_POINT('Ctrl Pts',(13.4988442384491,-21.1728750584175,
0.));
#190267=CARTESIAN_POINT('Ctrl Pts',(13.4988442384491,-21.1728750584175,
12.));
#190268=CARTESIAN_POINT('Ctrl Pts',(13.5017201056088,-21.1986390835828,
0.));
#190269=CARTESIAN_POINT('Ctrl Pts',(13.5017201056088,-21.1986390835828,
12.));
#190270=CARTESIAN_POINT('Ctrl Pts',(13.5045440957404,-21.2244869429332,
0.));
#190271=CARTESIAN_POINT('Ctrl Pts',(13.5045440957404,-21.2244869429332,
12.));
#190272=CARTESIAN_POINT('Ctrl Pts',(13.5073159019452,-21.250418192743,0.));
#190273=CARTESIAN_POINT('Ctrl Pts',(13.5073159019452,-21.250418192743,12.));
#190274=CARTESIAN_POINT('Ctrl Pts',(13.5100352209205,-21.2764323924442,
0.));
#190275=CARTESIAN_POINT('Ctrl Pts',(13.5100352209205,-21.2764323924442,
12.));
#190276=CARTESIAN_POINT('Ctrl Pts',(13.5127017534971,-21.3025291054235,
0.));
#190277=CARTESIAN_POINT('Ctrl Pts',(13.5127017534971,-21.3025291054235,
12.));
#190278=CARTESIAN_POINT('Ctrl Pts',(13.5153152050555,-21.3287078996341,
0.));
#190279=CARTESIAN_POINT('Ctrl Pts',(13.5153152050555,-21.3287078996341,
12.));
#190280=CARTESIAN_POINT('Ctrl Pts',(13.5178752862466,-21.3549683486222,
0.));
#190281=CARTESIAN_POINT('Ctrl Pts',(13.5178752862466,-21.3549683486222,
12.));
#190282=CARTESIAN_POINT('Ctrl Pts',(13.5203817122503,-21.3813100304973,
0.));
#190283=CARTESIAN_POINT('Ctrl Pts',(13.5203817122503,-21.3813100304973,
12.));
#190284=CARTESIAN_POINT('Ctrl Pts',(13.5228342013516,-21.4077325259324,
0.));
#190285=CARTESIAN_POINT('Ctrl Pts',(13.5228342013516,-21.4077325259324,
12.));
#190286=CARTESIAN_POINT('Ctrl Pts',(13.5252324737801,-21.4342354165259,
0.));
#190287=CARTESIAN_POINT('Ctrl Pts',(13.5252324737801,-21.4342354165259,
12.));
#190288=CARTESIAN_POINT('Ctrl Pts',(13.5275762503555,-21.4608182828697,
0.));
#190289=CARTESIAN_POINT('Ctrl Pts',(13.5275762503555,-21.4608182828697,
12.));
#190290=CARTESIAN_POINT('Ctrl Pts',(13.5298652514355,-21.4874807030468,
0.));
#190291=CARTESIAN_POINT('Ctrl Pts',(13.5298652514355,-21.4874807030468,
12.));
#190292=CARTESIAN_POINT('Ctrl Pts',(13.5320991952138,-21.5142222501666,
0.));
#190293=CARTESIAN_POINT('Ctrl Pts',(13.5320991952138,-21.5142222501666,
12.));
#190294=CARTESIAN_POINT('Ctrl Pts',(13.5342777983214,-21.5410424932503,
0.));
#190295=CARTESIAN_POINT('Ctrl Pts',(13.5342777983214,-21.5410424932503,
12.));
#190296=CARTESIAN_POINT('Ctrl Pts',(13.536400779028,-21.5679410019002,0.));
#190297=CARTESIAN_POINT('Ctrl Pts',(13.536400779028,-21.5679410019002,12.));
#190298=CARTESIAN_POINT('Ctrl Pts',(13.5384678597195,-21.5949173499013,
0.));
#190299=CARTESIAN_POINT('Ctrl Pts',(13.5384678597195,-21.5949173499013,
12.));
#190300=CARTESIAN_POINT('Ctrl Pts',(13.5404787697791,-21.6219711193946,
0.));
#190301=CARTESIAN_POINT('Ctrl Pts',(13.5404787697791,-21.6219711193946,
12.));
#190302=CARTESIAN_POINT('Ctrl Pts',(13.5424332480699,-21.6491019044648,
0.));
#190303=CARTESIAN_POINT('Ctrl Pts',(13.5424332480699,-21.6491019044648,
12.));
#190304=CARTESIAN_POINT('Ctrl Pts',(13.5443310461526,-21.6763093157699,
0.));
#190305=CARTESIAN_POINT('Ctrl Pts',(13.5443310461526,-21.6763093157699,
12.));
#190306=CARTESIAN_POINT('Ctrl Pts',(13.5461719295048,-21.7035929822955,
0.));
#190307=CARTESIAN_POINT('Ctrl Pts',(13.5461719295048,-21.7035929822955,
12.));
#190308=CARTESIAN_POINT('Ctrl Pts',(13.5479556704481,-21.7309525412281,
0.));
#190309=CARTESIAN_POINT('Ctrl Pts',(13.5479556704481,-21.7309525412281,
12.));
#190310=CARTESIAN_POINT('Ctrl Pts',(13.5496820422211,-21.7583876294554,
0.));
#190311=CARTESIAN_POINT('Ctrl Pts',(13.5496820422211,-21.7583876294554,
12.));
#190312=CARTESIAN_POINT('Ctrl Pts',(13.551350812725,-21.7858978745865,0.));
#190313=CARTESIAN_POINT('Ctrl Pts',(13.551350812725,-21.7858978745865,12.));
#190314=CARTESIAN_POINT('Ctrl Pts',(13.5529617381573,-21.8134828857967,
0.));
#190315=CARTESIAN_POINT('Ctrl Pts',(13.5529617381573,-21.8134828857967,
12.));
#190316=CARTESIAN_POINT('Ctrl Pts',(13.5545145573031,-21.8411422456075,
0.));
#190317=CARTESIAN_POINT('Ctrl Pts',(13.5545145573031,-21.8411422456075,
12.));
#190318=CARTESIAN_POINT('Ctrl Pts',(13.5560089839385,-21.8688754989365,
0.));
#190319=CARTESIAN_POINT('Ctrl Pts',(13.5560089839385,-21.8688754989365,
12.));
#190320=CARTESIAN_POINT('Ctrl Pts',(13.5574447178424,-21.8966821688824,
0.));
#190321=CARTESIAN_POINT('Ctrl Pts',(13.5574447178424,-21.8966821688824,
12.));
#190322=CARTESIAN_POINT('Ctrl Pts',(13.5588214586604,-21.9245617765769,
0.));
#190323=CARTESIAN_POINT('Ctrl Pts',(13.5588214586604,-21.9245617765769,
12.));
#190324=CARTESIAN_POINT('Ctrl Pts',(13.5601389185257,-21.9525138592813,
0.));
#190325=CARTESIAN_POINT('Ctrl Pts',(13.5601389185257,-21.9525138592813,
12.));
#190326=CARTESIAN_POINT('Ctrl Pts',(13.5613968357561,-21.9805379899168,
0.));
#190327=CARTESIAN_POINT('Ctrl Pts',(13.5613968357561,-21.9805379899168,
12.));
#190328=CARTESIAN_POINT('Ctrl Pts',(13.5625949868333,-22.0086337943449,
0.));
#190329=CARTESIAN_POINT('Ctrl Pts',(13.5625949868333,-22.0086337943449,
12.));
#190330=CARTESIAN_POINT('Ctrl Pts',(13.5637332022473,-22.0368009736295,
0.));
#190331=CARTESIAN_POINT('Ctrl Pts',(13.5637332022473,-22.0368009736295,
12.));
#190332=CARTESIAN_POINT('Ctrl Pts',(13.5648113689033,-22.065039308961,0.));
#190333=CARTESIAN_POINT('Ctrl Pts',(13.5648113689033,-22.065039308961,12.));
#190334=CARTESIAN_POINT('Ctrl Pts',(13.5658294169284,-22.0933486464593,
0.));
#190335=CARTESIAN_POINT('Ctrl Pts',(13.5658294169284,-22.0933486464593,
12.));
#190336=CARTESIAN_POINT('Ctrl Pts',(13.5667873105359,-22.1217288871975,
0.));
#190337=CARTESIAN_POINT('Ctrl Pts',(13.5667873105359,-22.1217288871975,
12.));
#190338=CARTESIAN_POINT('Ctrl Pts',(13.5675054919061,-22.1444897575194,
0.));
#190339=CARTESIAN_POINT('Ctrl Pts',(13.5675054919061,-22.1444897575194,
12.));
#190340=CARTESIAN_POINT('Ctrl Pts',(13.5680170531805,-22.1615922805008,
0.));
#190341=CARTESIAN_POINT('Ctrl Pts',(13.5680170531805,-22.1615922805008,
12.));
#190342=CARTESIAN_POINT('Ctrl Pts',(13.5683460612942,-22.1730081264608,
0.));
#190343=CARTESIAN_POINT('Ctrl Pts',(13.5683460612942,-22.1730081264608,
12.));
#190344=CARTESIAN_POINT('Ctrl Pts',(13.5685075571671,-22.178719590434,0.));
#190345=CARTESIAN_POINT('Ctrl Pts',(13.5685075571671,-22.178719590434,12.));
#190346=CARTESIAN_POINT('',(13.5685075571671,-22.178719590434,0.));
#190347=CARTESIAN_POINT('Ctrl Pts',(12.7689476255362,-18.5896416359912,
0.));
#190348=CARTESIAN_POINT('Ctrl Pts',(12.7689524524483,-18.5896460962964,
0.));
#190349=CARTESIAN_POINT('Ctrl Pts',(12.768986426692,-18.5896919669165,0.));
#190350=CARTESIAN_POINT('Ctrl Pts',(12.769110348199,-18.589871621843,0.));
#190351=CARTESIAN_POINT('Ctrl Pts',(12.7694215127918,-18.5903328777227,
0.));
#190352=CARTESIAN_POINT('Ctrl Pts',(12.7700520897173,-18.5912775137806,
0.));
#190353=CARTESIAN_POINT('Ctrl Pts',(12.7709195951156,-18.5925859134579,
0.));
#190354=CARTESIAN_POINT('Ctrl Pts',(12.7720142287172,-18.5942490615407,
0.));
#190355=CARTESIAN_POINT('Ctrl Pts',(12.7733231262108,-18.5962551167772,
0.));
#190356=CARTESIAN_POINT('Ctrl Pts',(12.7748328937638,-18.598591752595,0.));
#190357=CARTESIAN_POINT('Ctrl Pts',(12.7765325225081,-18.6012488486709,
0.));
#190358=CARTESIAN_POINT('Ctrl Pts',(12.7784139605066,-18.6042190183704,
0.));
#190359=CARTESIAN_POINT('Ctrl Pts',(12.7804705387658,-18.6074961535723,
0.));
#190360=CARTESIAN_POINT('Ctrl Pts',(12.7826959526924,-18.611074482622,0.));
#190361=CARTESIAN_POINT('Ctrl Pts',(12.7850831657901,-18.6149475565188,
0.));
#190362=CARTESIAN_POINT('Ctrl Pts',(12.7876249657834,-18.6191087624752,
0.));
#190363=CARTESIAN_POINT('Ctrl Pts',(12.7903142925234,-18.6235516265575,
0.));
#190364=CARTESIAN_POINT('Ctrl Pts',(12.7931447451555,-18.6282702819371,
0.));
#190365=CARTESIAN_POINT('Ctrl Pts',(12.796110622225,-18.6332595057006,0.));
#190366=CARTESIAN_POINT('Ctrl Pts',(12.7992066625264,-18.63851447924,0.));
#190367=CARTESIAN_POINT('Ctrl Pts',(12.8024278770152,-18.6440306327456,
0.));
#190368=CARTESIAN_POINT('Ctrl Pts',(12.805769331162,-18.6498034438987,0.));
#190369=CARTESIAN_POINT('Ctrl Pts',(12.8092261933858,-18.6558284825773,
0.));
#190370=CARTESIAN_POINT('Ctrl Pts',(12.8127937909631,-18.6621014624746,
0.));
#190371=CARTESIAN_POINT('Ctrl Pts',(12.8164676687362,-18.66861829528,0.));
#190372=CARTESIAN_POINT('Ctrl Pts',(12.8202436318474,-18.6753751301092,
0.));
#190373=CARTESIAN_POINT('Ctrl Pts',(12.8241176980017,-18.6823683094139,
0.));
#190374=CARTESIAN_POINT('Ctrl Pts',(12.8280860635231,-18.6895943376172,
0.));
#190375=CARTESIAN_POINT('Ctrl Pts',(12.8321450599789,-18.6970498410172,
0.));
#190376=CARTESIAN_POINT('Ctrl Pts',(12.8362911280361,-18.7047315436294,
0.));
#190377=CARTESIAN_POINT('Ctrl Pts',(12.8405208263431,-18.7126362754445,
0.));
#190378=CARTESIAN_POINT('Ctrl Pts',(12.8448308329494,-18.7207609737702,
0.));
#190379=CARTESIAN_POINT('Ctrl Pts',(12.8492179511591,-18.7291026886554,
0.));
#190380=CARTESIAN_POINT('Ctrl Pts',(12.8536791086316,-18.7376585820854,
0.));
#190381=CARTESIAN_POINT('Ctrl Pts',(12.8582113455646,-18.7464259171251,
0.));
#190382=CARTESIAN_POINT('Ctrl Pts',(12.8628118054171,-18.7554020493887,
0.));
#190383=CARTESIAN_POINT('Ctrl Pts',(12.8674777239653,-18.7645844169564,
0.));
#190384=CARTESIAN_POINT('Ctrl Pts',(12.872206421181,-18.7739705329022,0.));
#190385=CARTESIAN_POINT('Ctrl Pts',(12.8769952998095,-18.7835579840477,
0.));
#190386=CARTESIAN_POINT('Ctrl Pts',(12.8818418427475,-18.7933444285868,
0.));
#190387=CARTESIAN_POINT('Ctrl Pts',(12.8867436109546,-18.8033275941943,
0.));
#190388=CARTESIAN_POINT('Ctrl Pts',(12.8916982409935,-18.813505275782,0.));
#190389=CARTESIAN_POINT('Ctrl Pts',(12.8967034410754,-18.8238753319129,
0.));
#190390=CARTESIAN_POINT('Ctrl Pts',(12.9017569871738,-18.8344356812591,
0.));
#190391=CARTESIAN_POINT('Ctrl Pts',(12.9068567191854,-18.8451842990984,
0.));
#190392=CARTESIAN_POINT('Ctrl Pts',(12.9120005369063,-18.8561192136198,
0.));
#190393=CARTESIAN_POINT('Ctrl Pts',(12.9171863977045,-18.8672385038326,
0.));
#190394=CARTESIAN_POINT('Ctrl Pts',(12.9224123144981,-18.8785402977528,
0.));
#190395=CARTESIAN_POINT('Ctrl Pts',(12.9276763536373,-18.8900227704889,
0.));
#190396=CARTESIAN_POINT('Ctrl Pts',(12.9329766328184,-18.9016841423403,
0.));
#190397=CARTESIAN_POINT('Ctrl Pts',(12.9383113190374,-18.9135226769466,
0.));
#190398=CARTESIAN_POINT('Ctrl Pts',(12.9436786266105,-18.9255366795195,
0.));
#190399=CARTESIAN_POINT('Ctrl Pts',(12.9490768151821,-18.9377244950435,
0.));
#190400=CARTESIAN_POINT('Ctrl Pts',(12.9545041877377,-18.9500845064715,
0.));
#190401=CARTESIAN_POINT('Ctrl Pts',(12.9599590886319,-18.9626151329229,
0.));
#190402=CARTESIAN_POINT('Ctrl Pts',(12.9654399021869,-18.9753148284475,
0.));
#190403=CARTESIAN_POINT('Ctrl Pts',(12.9709450512747,-18.9881820807586,
0.));
#190404=CARTESIAN_POINT('Ctrl Pts',(12.9764729959205,-19.0012154099791,
0.));
#190405=CARTESIAN_POINT('Ctrl Pts',(12.9820222318715,-19.0144133673348,
0.));
#190406=CARTESIAN_POINT('Ctrl Pts',(12.9875912893003,-19.0277745339908,
0.));
#190407=CARTESIAN_POINT('Ctrl Pts',(12.9931787316514,-19.0412975200398,
0.));
#190408=CARTESIAN_POINT('Ctrl Pts',(12.9987831544502,-19.0549809634355,
0.));
#190409=CARTESIAN_POINT('Ctrl Pts',(13.0044031841381,-19.0688235289437,
0.));
#190410=CARTESIAN_POINT('Ctrl Pts',(13.0100374768785,-19.0828239070482,
0.));
#190411=CARTESIAN_POINT('Ctrl Pts',(13.0156847176093,-19.0969808131226,
0.));
#190412=CARTESIAN_POINT('Ctrl Pts',(13.0213436191326,-19.1112929866308,
0.));
#190413=CARTESIAN_POINT('Ctrl Pts',(13.0270129211976,-19.1257591903099,
0.));
#190414=CARTESIAN_POINT('Ctrl Pts',(13.0326913895841,-19.1403782093389,
0.));
#190415=CARTESIAN_POINT('Ctrl Pts',(13.0383778152072,-19.1551488505233,
0.));
#190416=CARTESIAN_POINT('Ctrl Pts',(13.0440710133775,-19.1700699416625,
0.));
#190417=CARTESIAN_POINT('Ctrl Pts',(13.0497698230442,-19.1851403308826,
0.));
#190418=CARTESIAN_POINT('Ctrl Pts',(13.0554731060537,-19.2003588859771,
0.));
#190419=CARTESIAN_POINT('Ctrl Pts',(13.0611797463912,-19.2157244937141,
0.));
#190420=CARTESIAN_POINT('Ctrl Pts',(13.0668886494791,-19.2312360592031,
0.));
#190421=CARTESIAN_POINT('Ctrl Pts',(13.0725987415856,-19.2468925053988,
0.));
#190422=CARTESIAN_POINT('Ctrl Pts',(13.0783089692117,-19.2626927725596,
0.));
#190423=CARTESIAN_POINT('Ctrl Pts',(13.0840182984949,-19.2786358177198,
0.));
#190424=CARTESIAN_POINT('Ctrl Pts',(13.0897257145969,-19.2947206141246,
0.));
#190425=CARTESIAN_POINT('Ctrl Pts',(13.095430221148,-19.3109461507358,0.));
#190426=CARTESIAN_POINT('Ctrl Pts',(13.1011308397591,-19.3273114318268,
0.));
#190427=CARTESIAN_POINT('Ctrl Pts',(13.1068266095186,-19.3438154765395,
0.));
#190428=CARTESIAN_POINT('Ctrl Pts',(13.1125165865021,-19.3604573184516,
0.));
#190429=CARTESIAN_POINT('Ctrl Pts',(13.118199843271,-19.3772360051093,0.));
#190430=CARTESIAN_POINT('Ctrl Pts',(13.1238754684177,-19.3941505976267,
0.));
#190431=CARTESIAN_POINT('Ctrl Pts',(13.1295425661635,-19.4112001703561,
0.));
#190432=CARTESIAN_POINT('Ctrl Pts',(13.1352002559439,-19.4283838105265,
0.));
#190433=CARTESIAN_POINT('Ctrl Pts',(13.140847672006,-19.4457006178875,0.));
#190434=CARTESIAN_POINT('Ctrl Pts',(13.1464839629966,-19.463149704325,0.));
#190435=CARTESIAN_POINT('Ctrl Pts',(13.1521082915846,-19.4807301935256,
0.));
#190436=CARTESIAN_POINT('Ctrl Pts',(13.1577198341238,-19.498441220707,0.));
#190437=CARTESIAN_POINT('Ctrl Pts',(13.1633177803097,-19.5162819323207,
0.));
#190438=CARTESIAN_POINT('Ctrl Pts',(13.1689013328432,-19.5342514857564,
0.));
#190439=CARTESIAN_POINT('Ctrl Pts',(13.1744697070918,-19.5523490490254,
0.));
#190440=CARTESIAN_POINT('Ctrl Pts',(13.1800221307682,-19.5705738004682,
0.));
#190441=CARTESIAN_POINT('Ctrl Pts',(13.1855578436479,-19.5889249285352,
0.));
#190442=CARTESIAN_POINT('Ctrl Pts',(13.1910760972818,-19.6074016315421,
0.));
#190443=CARTESIAN_POINT('Ctrl Pts',(13.196576154715,-19.6260031174244,0.));
#190444=CARTESIAN_POINT('Ctrl Pts',(13.202057290206,-19.6447286034764,0.));
#190445=CARTESIAN_POINT('Ctrl Pts',(13.2075187889522,-19.6635773160924,
0.));
#190446=CARTESIAN_POINT('Ctrl Pts',(13.2129599468478,-19.6825484905812,
0.));
#190447=CARTESIAN_POINT('Ctrl Pts',(13.2183800702431,-19.7016413709678,
0.));
#190448=CARTESIAN_POINT('Ctrl Pts',(13.2237784757065,-19.7208552097867,
0.));
#190449=CARTESIAN_POINT('Ctrl Pts',(13.2291544897902,-19.7401892678701,
0.));
#190450=CARTESIAN_POINT('Ctrl Pts',(13.2345074487968,-19.7596428141176,
0.));
#190451=CARTESIAN_POINT('Ctrl Pts',(13.239836698568,-19.7792151253297,0.));
#190452=CARTESIAN_POINT('Ctrl Pts',(13.2451415942809,-19.7989054860501,
0.));
#190453=CARTESIAN_POINT('Ctrl Pts',(13.2504215002458,-19.8187131883919,
0.));
#190454=CARTESIAN_POINT('Ctrl Pts',(13.2556757897085,-19.8386375318632,
0.));
#190455=CARTESIAN_POINT('Ctrl Pts',(13.2609038446525,-19.8586778231711,
0.));
#190456=CARTESIAN_POINT('Ctrl Pts',(13.2661050556128,-19.8788333760571,
0.));
#190457=CARTESIAN_POINT('Ctrl Pts',(13.2712788215015,-19.8991035111739,
0.));
#190458=CARTESIAN_POINT('Ctrl Pts',(13.2764245494354,-19.9194875559419,
0.));
#190459=CARTESIAN_POINT('Ctrl Pts',(13.2815416545662,-19.939984844402,0.));
#190460=CARTESIAN_POINT('Ctrl Pts',(13.2866295599152,-19.9605947170589,
0.));
#190461=CARTESIAN_POINT('Ctrl Pts',(13.2916876962098,-19.9813165207174,
0.));
#190462=CARTESIAN_POINT('Ctrl Pts',(13.296715501731,-20.0021496083742,0.));
#190463=CARTESIAN_POINT('Ctrl Pts',(13.3017124221639,-20.023093339104,0.));
#190464=CARTESIAN_POINT('Ctrl Pts',(13.3066779104515,-20.0441470779345,
0.));
#190465=CARTESIAN_POINT('Ctrl Pts',(13.3116114266514,-20.0653101957188,
0.));
#190466=CARTESIAN_POINT('Ctrl Pts',(13.3165124377962,-20.0865820689884,
0.));
#190467=CARTESIAN_POINT('Ctrl Pts',(13.3213804177588,-20.1079620798377,
0.));
#190468=CARTESIAN_POINT('Ctrl Pts',(13.3262148471228,-20.1294496158405,
0.));
#190469=CARTESIAN_POINT('Ctrl Pts',(13.3310152130565,-20.1510440699477,
0.));
#190470=CARTESIAN_POINT('Ctrl Pts',(13.3357810091903,-20.1727448403818,
0.));
#190471=CARTESIAN_POINT('Ctrl Pts',(13.3405117354969,-20.1945513305233,
0.));
#190472=CARTESIAN_POINT('Ctrl Pts',(13.3452068981762,-20.2164629487855,
0.));
#190473=CARTESIAN_POINT('Ctrl Pts',(13.3498660095381,-20.2384791085354,
0.));
#190474=CARTESIAN_POINT('Ctrl Pts',(13.3544885878886,-20.2605992280117,
0.));
#190475=CARTESIAN_POINT('Ctrl Pts',(13.3590741574194,-20.2828227302337,
0.));
#190476=CARTESIAN_POINT('Ctrl Pts',(13.3636222481016,-20.3051490429049,
0.));
#190477=CARTESIAN_POINT('Ctrl Pts',(13.3681323955828,-20.3275775983032,
0.));
#190478=CARTESIAN_POINT('Ctrl Pts',(13.3726041410869,-20.3501078331818,
0.));
#190479=CARTESIAN_POINT('Ctrl Pts',(13.377037031319,-20.3727391887187,0.));
#190480=CARTESIAN_POINT('Ctrl Pts',(13.3814306183721,-20.3954711104505,
0.));
#190481=CARTESIAN_POINT('Ctrl Pts',(13.3857844596387,-20.4183030482002,
0.));
#190482=CARTESIAN_POINT('Ctrl Pts',(13.3900981177254,-20.4412344560007,
0.));
#190483=CARTESIAN_POINT('Ctrl Pts',(13.3943711603739,-20.4642647920038,
0.));
#190484=CARTESIAN_POINT('Ctrl Pts',(13.3986031603716,-20.4873935184041,
0.));
#190485=CARTESIAN_POINT('Ctrl Pts',(13.4027936954529,-20.5106201013755,
0.));
#190486=CARTESIAN_POINT('Ctrl Pts',(13.4069423482076,-20.5339440109958,
0.));
#190487=CARTESIAN_POINT('Ctrl Pts',(13.4110487059912,-20.557364721164,0.));
#190488=CARTESIAN_POINT('Ctrl Pts',(13.415112360841,-20.5808817095155,0.));
#190489=CARTESIAN_POINT('Ctrl Pts',(13.4191329093931,-20.6044944573151,
0.));
#190490=CARTESIAN_POINT('Ctrl Pts',(13.4231099528178,-20.6282024494234,
0.));
#190491=CARTESIAN_POINT('Ctrl Pts',(13.427043096765,-20.6520051742868,0.));
#190492=CARTESIAN_POINT('Ctrl Pts',(13.4309319513119,-20.6759021239102,
0.));
#190493=CARTESIAN_POINT('Ctrl Pts',(13.4347761309154,-20.6998927938288,
0.));
#190494=CARTESIAN_POINT('Ctrl Pts',(13.4385752543663,-20.7239766830676,
0.));
#190495=CARTESIAN_POINT('Ctrl Pts',(13.4423289447561,-20.7481532941014,
0.));
#190496=CARTESIAN_POINT('Ctrl Pts',(13.4460368293689,-20.7724221327609,
0.));
#190497=CARTESIAN_POINT('Ctrl Pts',(13.4496985395637,-20.7967827081228,
0.));
#190498=CARTESIAN_POINT('Ctrl Pts',(13.4533137106667,-20.821234532398,0.));
#190499=CARTESIAN_POINT('Ctrl Pts',(13.4568819818631,-20.8457771208083,
0.));
#190500=CARTESIAN_POINT('Ctrl Pts',(13.4604029960983,-20.8704099914641,
0.));
#190501=CARTESIAN_POINT('Ctrl Pts',(13.4638763999725,-20.8951326652158,
0.));
#190502=CARTESIAN_POINT('Ctrl Pts',(13.4673018437717,-20.9199446657583,
0.));
#190503=CARTESIAN_POINT('Ctrl Pts',(13.4706789815166,-20.9448455197557,
0.));
#190504=CARTESIAN_POINT('Ctrl Pts',(13.4740074710086,-20.9698347569477,
0.));
#190505=CARTESIAN_POINT('Ctrl Pts',(13.4772869738878,-20.9949119102592,
0.));
#190506=CARTESIAN_POINT('Ctrl Pts',(13.4805171556822,-21.0200765158884,
0.));
#190507=CARTESIAN_POINT('Ctrl Pts',(13.4836976858912,-21.0453281134245,
0.));
#190508=CARTESIAN_POINT('Ctrl Pts',(13.4868282377191,-21.0706662455199,
0.));
#190509=CARTESIAN_POINT('Ctrl Pts',(13.4899084877717,-21.0960904575046,
0.));
#190510=CARTESIAN_POINT('Ctrl Pts',(13.4929381157778,-21.1216002970207,
0.));
#190511=CARTESIAN_POINT('Ctrl Pts',(13.4959168042934,-21.1471953136209,
0.));
#190512=CARTESIAN_POINT('Ctrl Pts',(13.4988442384491,-21.1728750584175,
0.));
#190513=CARTESIAN_POINT('Ctrl Pts',(13.5017201056088,-21.1986390835828,
0.));
#190514=CARTESIAN_POINT('Ctrl Pts',(13.5045440957404,-21.2244869429332,
0.));
#190515=CARTESIAN_POINT('Ctrl Pts',(13.5073159019452,-21.250418192743,0.));
#190516=CARTESIAN_POINT('Ctrl Pts',(13.5100352209205,-21.2764323924442,
0.));
#190517=CARTESIAN_POINT('Ctrl Pts',(13.5127017534971,-21.3025291054235,
0.));
#190518=CARTESIAN_POINT('Ctrl Pts',(13.5153152050555,-21.3287078996341,
0.));
#190519=CARTESIAN_POINT('Ctrl Pts',(13.5178752862466,-21.3549683486222,
0.));
#190520=CARTESIAN_POINT('Ctrl Pts',(13.5203817122503,-21.3813100304973,
0.));
#190521=CARTESIAN_POINT('Ctrl Pts',(13.5228342013516,-21.4077325259324,
0.));
#190522=CARTESIAN_POINT('Ctrl Pts',(13.5252324737801,-21.4342354165259,
0.));
#190523=CARTESIAN_POINT('Ctrl Pts',(13.5275762503555,-21.4608182828697,
0.));
#190524=CARTESIAN_POINT('Ctrl Pts',(13.5298652514355,-21.4874807030468,
0.));
#190525=CARTESIAN_POINT('Ctrl Pts',(13.5320991952138,-21.5142222501666,
0.));
#190526=CARTESIAN_POINT('Ctrl Pts',(13.5342777983214,-21.5410424932503,
0.));
#190527=CARTESIAN_POINT('Ctrl Pts',(13.536400779028,-21.5679410019002,0.));
#190528=CARTESIAN_POINT('Ctrl Pts',(13.5384678597195,-21.5949173499013,
0.));
#190529=CARTESIAN_POINT('Ctrl Pts',(13.5404787697791,-21.6219711193946,
0.));
#190530=CARTESIAN_POINT('Ctrl Pts',(13.5424332480699,-21.6491019044648,
0.));
#190531=CARTESIAN_POINT('Ctrl Pts',(13.5443310461526,-21.6763093157699,
0.));
#190532=CARTESIAN_POINT('Ctrl Pts',(13.5461719295048,-21.7035929822955,
0.));
#190533=CARTESIAN_POINT('Ctrl Pts',(13.5479556704481,-21.7309525412281,
0.));
#190534=CARTESIAN_POINT('Ctrl Pts',(13.5496820422211,-21.7583876294554,
0.));
#190535=CARTESIAN_POINT('Ctrl Pts',(13.551350812725,-21.7858978745865,0.));
#190536=CARTESIAN_POINT('Ctrl Pts',(13.5529617381573,-21.8134828857967,
0.));
#190537=CARTESIAN_POINT('Ctrl Pts',(13.5545145573031,-21.8411422456075,
0.));
#190538=CARTESIAN_POINT('Ctrl Pts',(13.5560089839385,-21.8688754989365,
0.));
#190539=CARTESIAN_POINT('Ctrl Pts',(13.5574447178424,-21.8966821688824,
0.));
#190540=CARTESIAN_POINT('Ctrl Pts',(13.5588214586604,-21.9245617765769,
0.));
#190541=CARTESIAN_POINT('Ctrl Pts',(13.5601389185257,-21.9525138592813,
0.));
#190542=CARTESIAN_POINT('Ctrl Pts',(13.5613968357561,-21.9805379899168,
0.));
#190543=CARTESIAN_POINT('Ctrl Pts',(13.5625949868333,-22.0086337943449,
0.));
#190544=CARTESIAN_POINT('Ctrl Pts',(13.5637332022473,-22.0368009736295,
0.));
#190545=CARTESIAN_POINT('Ctrl Pts',(13.5648113689033,-22.065039308961,0.));
#190546=CARTESIAN_POINT('Ctrl Pts',(13.5658294169284,-22.0933486464593,
0.));
#190547=CARTESIAN_POINT('Ctrl Pts',(13.5667873105359,-22.1217288871975,
0.));
#190548=CARTESIAN_POINT('Ctrl Pts',(13.5675054919061,-22.1444897575194,
0.));
#190549=CARTESIAN_POINT('Ctrl Pts',(13.5680170531805,-22.1615922805008,
0.));
#190550=CARTESIAN_POINT('Ctrl Pts',(13.5683460612942,-22.1730081264608,
0.));
#190551=CARTESIAN_POINT('Ctrl Pts',(13.5685075571671,-22.178719590434,0.));
#190552=CARTESIAN_POINT('',(13.5685075571671,-22.178719590434,0.));
#190553=CARTESIAN_POINT('Origin',(7.17139709155223,-20.2687213152502,0.));
#190554=CARTESIAN_POINT('',(7.52250298901263,-21.2610617890679,0.));
#190555=CARTESIAN_POINT('',(7.52250298901263,-21.2610617890679,0.));
#190556=CARTESIAN_POINT('',(3.58569854577611,-10.1343606576251,0.));
#190557=CARTESIAN_POINT('Ctrl Pts',(12.4230808101438,-22.8400320311649,
0.));
#190558=CARTESIAN_POINT('Ctrl Pts',(12.4230808101438,-22.8400320311649,
12.));
#190559=CARTESIAN_POINT('Ctrl Pts',(12.418215285186,-22.8370364396459,0.));
#190560=CARTESIAN_POINT('Ctrl Pts',(12.418215285186,-22.8370364396459,12.));
#190561=CARTESIAN_POINT('Ctrl Pts',(12.4084933766346,-22.8310435872748,
0.));
#190562=CARTESIAN_POINT('Ctrl Pts',(12.4084933766346,-22.8310435872748,
12.));
#190563=CARTESIAN_POINT('Ctrl Pts',(12.3939379378998,-22.8220493007173,
0.));
#190564=CARTESIAN_POINT('Ctrl Pts',(12.3939379378998,-22.8220493007173,
12.));
#190565=CARTESIAN_POINT('Ctrl Pts',(12.374585536673,-22.81004690224,0.));
#190566=CARTESIAN_POINT('Ctrl Pts',(12.374585536673,-22.81004690224,12.));
#190567=CARTESIAN_POINT('Ctrl Pts',(12.3504864740319,-22.795027221673,0.));
#190568=CARTESIAN_POINT('Ctrl Pts',(12.3504864740319,-22.795027221673,12.));
#190569=CARTESIAN_POINT('Ctrl Pts',(12.3264788926075,-22.7799908974768,
0.));
#190570=CARTESIAN_POINT('Ctrl Pts',(12.3264788926075,-22.7799908974768,
12.));
#190571=CARTESIAN_POINT('Ctrl Pts',(12.3025628601792,-22.764938010105,0.));
#190572=CARTESIAN_POINT('Ctrl Pts',(12.3025628601792,-22.764938010105,12.));
#190573=CARTESIAN_POINT('Ctrl Pts',(12.2787384750742,-22.7498686970069,
0.));
#190574=CARTESIAN_POINT('Ctrl Pts',(12.2787384750742,-22.7498686970069,
12.));
#190575=CARTESIAN_POINT('Ctrl Pts',(12.2550058702395,-22.7347831655287,
0.));
#190576=CARTESIAN_POINT('Ctrl Pts',(12.2550058702395,-22.7347831655287,
12.));
#190577=CARTESIAN_POINT('Ctrl Pts',(12.2313652198061,-22.7196817119374,
0.));
#190578=CARTESIAN_POINT('Ctrl Pts',(12.2313652198061,-22.7196817119374,
12.));
#190579=CARTESIAN_POINT('Ctrl Pts',(12.2078167360284,-22.7045647168747,
0.));
#190580=CARTESIAN_POINT('Ctrl Pts',(12.2078167360284,-22.7045647168747,
12.));
#190581=CARTESIAN_POINT('Ctrl Pts',(12.1843606579261,-22.6894326205037,
0.));
#190582=CARTESIAN_POINT('Ctrl Pts',(12.1843606579261,-22.6894326205037,
12.));
#190583=CARTESIAN_POINT('Ctrl Pts',(12.1609972423099,-22.6742859034944,
0.));
#190584=CARTESIAN_POINT('Ctrl Pts',(12.1609972423099,-22.6742859034944,
12.));
#190585=CARTESIAN_POINT('Ctrl Pts',(12.1377267537145,-22.6591250653965,
0.));
#190586=CARTESIAN_POINT('Ctrl Pts',(12.1377267537145,-22.6591250653965,
12.));
#190587=CARTESIAN_POINT('Ctrl Pts',(12.1145494550383,-22.6439506046605,
0.));
#190588=CARTESIAN_POINT('Ctrl Pts',(12.1145494550383,-22.6439506046605,
12.));
#190589=CARTESIAN_POINT('Ctrl Pts',(12.0914655972823,-22.6287629967056,
0.));
#190590=CARTESIAN_POINT('Ctrl Pts',(12.0914655972823,-22.6287629967056,
12.));
#190591=CARTESIAN_POINT('Ctrl Pts',(12.0684754113862,-22.6135626764898,
0.));
#190592=CARTESIAN_POINT('Ctrl Pts',(12.0684754113862,-22.6135626764898,
12.));
#190593=CARTESIAN_POINT('Ctrl Pts',(12.0455791139128,-22.5983500505644,
0.));
#190594=CARTESIAN_POINT('Ctrl Pts',(12.0455791139128,-22.5983500505644,
12.));
#190595=CARTESIAN_POINT('Ctrl Pts',(12.0227769113127,-22.5831255061282,
0.));
#190596=CARTESIAN_POINT('Ctrl Pts',(12.0227769113127,-22.5831255061282,
12.));
#190597=CARTESIAN_POINT('Ctrl Pts',(12.0000690046694,-22.5678894211181,
0.));
#190598=CARTESIAN_POINT('Ctrl Pts',(12.0000690046694,-22.5678894211181,
12.));
#190599=CARTESIAN_POINT('Ctrl Pts',(11.9774555943496,-22.5526421741158,
0.));
#190600=CARTESIAN_POINT('Ctrl Pts',(11.9774555943496,-22.5526421741158,
12.));
#190601=CARTESIAN_POINT('Ctrl Pts',(11.9549368843997,-22.5373841537307,
0.));
#190602=CARTESIAN_POINT('Ctrl Pts',(11.9549368843997,-22.5373841537307,
12.));
#190603=CARTESIAN_POINT('Ctrl Pts',(11.9325130877803,-22.5221157697883,
0.));
#190604=CARTESIAN_POINT('Ctrl Pts',(11.9325130877803,-22.5221157697883,
12.));
#190605=CARTESIAN_POINT('Ctrl Pts',(11.9101844254557,-22.5068374513973,
0.));
#190606=CARTESIAN_POINT('Ctrl Pts',(11.9101844254557,-22.5068374513973,
12.));
#190607=CARTESIAN_POINT('Ctrl Pts',(11.8879511239942,-22.4915496418485,
0.));
#190608=CARTESIAN_POINT('Ctrl Pts',(11.8879511239942,-22.4915496418485,
12.));
#190609=CARTESIAN_POINT('Ctrl Pts',(11.8658134137019,-22.4762527946702,
0.));
#190610=CARTESIAN_POINT('Ctrl Pts',(11.8658134137019,-22.4762527946702,
12.));
#190611=CARTESIAN_POINT('Ctrl Pts',(11.8437715264487,-22.4609473690472,
0.));
#190612=CARTESIAN_POINT('Ctrl Pts',(11.8437715264487,-22.4609473690472,
12.));
#190613=CARTESIAN_POINT('Ctrl Pts',(11.8218256937889,-22.4456338258735,
0.));
#190614=CARTESIAN_POINT('Ctrl Pts',(11.8218256937889,-22.4456338258735,
12.));
#190615=CARTESIAN_POINT('Ctrl Pts',(11.7999761445173,-22.430312622646,0.));
#190616=CARTESIAN_POINT('Ctrl Pts',(11.7999761445173,-22.430312622646,12.));
#190617=CARTESIAN_POINT('Ctrl Pts',(11.7782231042039,-22.4149842125008,
0.));
#190618=CARTESIAN_POINT('Ctrl Pts',(11.7782231042039,-22.4149842125008,
12.));
#190619=CARTESIAN_POINT('Ctrl Pts',(11.7565667964764,-22.3996490469191,
0.));
#190620=CARTESIAN_POINT('Ctrl Pts',(11.7565667964764,-22.3996490469191,
12.));
#190621=CARTESIAN_POINT('Ctrl Pts',(11.7350074437961,-22.3843075773899,
0.));
#190622=CARTESIAN_POINT('Ctrl Pts',(11.7350074437961,-22.3843075773899,
12.));
#190623=CARTESIAN_POINT('Ctrl Pts',(11.7135452684532,-22.3689602575491,
0.));
#190624=CARTESIAN_POINT('Ctrl Pts',(11.7135452684532,-22.3689602575491,
12.));
#190625=CARTESIAN_POINT('Ctrl Pts',(11.6921804934056,-22.3536075450029,
0.));
#190626=CARTESIAN_POINT('Ctrl Pts',(11.6921804934056,-22.3536075450029,
12.));
#190627=CARTESIAN_POINT('Ctrl Pts',(11.6709133432985,-22.3382499035619,
0.));
#190628=CARTESIAN_POINT('Ctrl Pts',(11.6709133432985,-22.3382499035619,
12.));
#190629=CARTESIAN_POINT('Ctrl Pts',(11.6497440449857,-22.3228878043976,
0.));
#190630=CARTESIAN_POINT('Ctrl Pts',(11.6497440449857,-22.3228878043976,
12.));
#190631=CARTESIAN_POINT('Ctrl Pts',(11.6286728270009,-22.3075217249049,
0.));
#190632=CARTESIAN_POINT('Ctrl Pts',(11.6286728270009,-22.3075217249049,
12.));
#190633=CARTESIAN_POINT('Ctrl Pts',(11.6076999192357,-22.2921521480356,
0.));
#190634=CARTESIAN_POINT('Ctrl Pts',(11.6076999192357,-22.2921521480356,
12.));
#190635=CARTESIAN_POINT('Ctrl Pts',(11.5868255525188,-22.2767795614348,
0.));
#190636=CARTESIAN_POINT('Ctrl Pts',(11.5868255525188,-22.2767795614348,
12.));
#190637=CARTESIAN_POINT('Ctrl Pts',(11.5660499582403,-22.2614044566898,
0.));
#190638=CARTESIAN_POINT('Ctrl Pts',(11.5660499582403,-22.2614044566898,
12.));
#190639=CARTESIAN_POINT('Ctrl Pts',(11.5453733679121,-22.2460273284654,
0.));
#190640=CARTESIAN_POINT('Ctrl Pts',(11.5453733679121,-22.2460273284654,
12.));
#190641=CARTESIAN_POINT('Ctrl Pts',(11.5247960128477,-22.2306486738901,
0.));
#190642=CARTESIAN_POINT('Ctrl Pts',(11.5247960128477,-22.2306486738901,
12.));
#190643=CARTESIAN_POINT('Ctrl Pts',(11.5043181244242,-22.2152689931022,
0.));
#190644=CARTESIAN_POINT('Ctrl Pts',(11.5043181244242,-22.2152689931022,
12.));
#190645=CARTESIAN_POINT('Ctrl Pts',(11.483939934259,-22.1998887896436,0.));
#190646=CARTESIAN_POINT('Ctrl Pts',(11.483939934259,-22.1998887896436,12.));
#190647=CARTESIAN_POINT('Ctrl Pts',(11.463661674411,-22.184508570917,0.));
#190648=CARTESIAN_POINT('Ctrl Pts',(11.463661674411,-22.184508570917,12.));
#190649=CARTESIAN_POINT('Ctrl Pts',(11.443483577557,-22.1691288486096,0.));
#190650=CARTESIAN_POINT('Ctrl Pts',(11.443483577557,-22.1691288486096,12.));
#190651=CARTESIAN_POINT('Ctrl Pts',(11.4234058771742,-22.1537501391487,
0.));
#190652=CARTESIAN_POINT('Ctrl Pts',(11.4234058771742,-22.1537501391487,
12.));
#190653=CARTESIAN_POINT('Ctrl Pts',(11.4034288076908,-22.1383729640964,
0.));
#190654=CARTESIAN_POINT('Ctrl Pts',(11.4034288076908,-22.1383729640964,
12.));
#190655=CARTESIAN_POINT('Ctrl Pts',(11.3835526044256,-22.1229978500186,
0.));
#190656=CARTESIAN_POINT('Ctrl Pts',(11.3835526044256,-22.1229978500186,
12.));
#190657=CARTESIAN_POINT('Ctrl Pts',(11.3637775035367,-22.1076253283979,
0.));
#190658=CARTESIAN_POINT('Ctrl Pts',(11.3637775035367,-22.1076253283979,
12.));
#190659=CARTESIAN_POINT('Ctrl Pts',(11.3441037419553,-22.0922559355294,
0.));
#190660=CARTESIAN_POINT('Ctrl Pts',(11.3441037419553,-22.0922559355294,
12.));
#190661=CARTESIAN_POINT('Ctrl Pts',(11.3245315573168,-22.0768902124267,
0.));
#190662=CARTESIAN_POINT('Ctrl Pts',(11.3245315573168,-22.0768902124267,
12.));
#190663=CARTESIAN_POINT('Ctrl Pts',(11.3050611878771,-22.0615287047179,
0.));
#190664=CARTESIAN_POINT('Ctrl Pts',(11.3050611878771,-22.0615287047179,
12.));
#190665=CARTESIAN_POINT('Ctrl Pts',(11.2856928724374,-22.046171962566,0.));
#190666=CARTESIAN_POINT('Ctrl Pts',(11.2856928724374,-22.046171962566,12.));
#190667=CARTESIAN_POINT('Ctrl Pts',(11.2664268504206,-22.030820540835,0.));
#190668=CARTESIAN_POINT('Ctrl Pts',(11.2664268504206,-22.030820540835,12.));
#190669=CARTESIAN_POINT('Ctrl Pts',(11.2472633619275,-22.0154749992363,
0.));
#190670=CARTESIAN_POINT('Ctrl Pts',(11.2472633619275,-22.0154749992363,
12.));
#190671=CARTESIAN_POINT('Ctrl Pts',(11.2282026477896,-22.0001359024839,
0.));
#190672=CARTESIAN_POINT('Ctrl Pts',(11.2282026477896,-22.0001359024839,
12.));
#190673=CARTESIAN_POINT('Ctrl Pts',(11.2092449496125,-21.9848038204439,
0.));
#190674=CARTESIAN_POINT('Ctrl Pts',(11.2092449496125,-21.9848038204439,
12.));
#190675=CARTESIAN_POINT('Ctrl Pts',(11.190390509811,-21.9694793282914,0.));
#190676=CARTESIAN_POINT('Ctrl Pts',(11.190390509811,-21.9694793282914,12.));
#190677=CARTESIAN_POINT('Ctrl Pts',(11.1716395716376,-21.9541630066506,
0.));
#190678=CARTESIAN_POINT('Ctrl Pts',(11.1716395716376,-21.9541630066506,
12.));
#190679=CARTESIAN_POINT('Ctrl Pts',(11.1529923792003,-21.9388554416439,
0.));
#190680=CARTESIAN_POINT('Ctrl Pts',(11.1529923792003,-21.9388554416439,
12.));
#190681=CARTESIAN_POINT('Ctrl Pts',(11.1344491774741,-21.923557224952,0.));
#190682=CARTESIAN_POINT('Ctrl Pts',(11.1344491774741,-21.923557224952,12.));
#190683=CARTESIAN_POINT('Ctrl Pts',(11.1160102123024,-21.9082689538688,
0.));
#190684=CARTESIAN_POINT('Ctrl Pts',(11.1160102123024,-21.9082689538688,
12.));
#190685=CARTESIAN_POINT('Ctrl Pts',(11.0976757303944,-21.8929912313608,
0.));
#190686=CARTESIAN_POINT('Ctrl Pts',(11.0976757303944,-21.8929912313608,
12.));
#190687=CARTESIAN_POINT('Ctrl Pts',(11.0794459793057,-21.877724666119,0.));
#190688=CARTESIAN_POINT('Ctrl Pts',(11.0794459793057,-21.877724666119,12.));
#190689=CARTESIAN_POINT('Ctrl Pts',(11.0613212074363,-21.8624698726318,
0.));
#190690=CARTESIAN_POINT('Ctrl Pts',(11.0613212074363,-21.8624698726318,
12.));
#190691=CARTESIAN_POINT('Ctrl Pts',(11.0433016640807,-21.8472274713103,
0.));
#190692=CARTESIAN_POINT('Ctrl Pts',(11.0433016640807,-21.8472274713103,
12.));
#190693=CARTESIAN_POINT('Ctrl Pts',(11.0253875994598,-21.8319980886033,
0.));
#190694=CARTESIAN_POINT('Ctrl Pts',(11.0253875994598,-21.8319980886033,
12.));
#190695=CARTESIAN_POINT('Ctrl Pts',(11.0075792647477,-21.8167823571168,
0.));
#190696=CARTESIAN_POINT('Ctrl Pts',(11.0075792647477,-21.8167823571168,
12.));
#190697=CARTESIAN_POINT('Ctrl Pts',(10.9898769120912,-21.8015809157301,
0.));
#190698=CARTESIAN_POINT('Ctrl Pts',(10.9898769120912,-21.8015809157301,
12.));
#190699=CARTESIAN_POINT('Ctrl Pts',(10.9722807946155,-21.7863944097141,
0.));
#190700=CARTESIAN_POINT('Ctrl Pts',(10.9722807946155,-21.7863944097141,
12.));
#190701=CARTESIAN_POINT('Ctrl Pts',(10.9547911664455,-21.7712234908464,
0.));
#190702=CARTESIAN_POINT('Ctrl Pts',(10.9547911664455,-21.7712234908464,
12.));
#190703=CARTESIAN_POINT('Ctrl Pts',(10.9374082827444,-21.7560688175247,
0.));
#190704=CARTESIAN_POINT('Ctrl Pts',(10.9374082827444,-21.7560688175247,
12.));
#190705=CARTESIAN_POINT('Ctrl Pts',(10.9201323997384,-21.7409310548797,
0.));
#190706=CARTESIAN_POINT('Ctrl Pts',(10.9201323997384,-21.7409310548797,
12.));
#190707=CARTESIAN_POINT('Ctrl Pts',(10.902963774734,-21.7258108748873,0.));
#190708=CARTESIAN_POINT('Ctrl Pts',(10.902963774734,-21.7258108748873,12.));
#190709=CARTESIAN_POINT('Ctrl Pts',(10.8859026661293,-21.7107089564825,
0.));
#190710=CARTESIAN_POINT('Ctrl Pts',(10.8859026661293,-21.7107089564825,
12.));
#190711=CARTESIAN_POINT('Ctrl Pts',(10.8689493334095,-21.6956259856672,
0.));
#190712=CARTESIAN_POINT('Ctrl Pts',(10.8689493334095,-21.6956259856672,
12.));
#190713=CARTESIAN_POINT('Ctrl Pts',(10.8521040371835,-21.6805626556467,
0.));
#190714=CARTESIAN_POINT('Ctrl Pts',(10.8521040371835,-21.6805626556467,
12.));
#190715=CARTESIAN_POINT('Ctrl Pts',(10.8353670392272,-21.6655196669732,
0.));
#190716=CARTESIAN_POINT('Ctrl Pts',(10.8353670392272,-21.6655196669732,
12.));
#190717=CARTESIAN_POINT('Ctrl Pts',(10.8187386025136,-21.6504977276866,
0.));
#190718=CARTESIAN_POINT('Ctrl Pts',(10.8187386025136,-21.6504977276866,
12.));
#190719=CARTESIAN_POINT('Ctrl Pts',(10.8022189912369,-21.6354975534557,
0.));
#190720=CARTESIAN_POINT('Ctrl Pts',(10.8022189912369,-21.6354975534557,
12.));
#190721=CARTESIAN_POINT('Ctrl Pts',(10.7858084708261,-21.6205198677173,
0.));
#190722=CARTESIAN_POINT('Ctrl Pts',(10.7858084708261,-21.6205198677173,
12.));
#190723=CARTESIAN_POINT('Ctrl Pts',(10.7695073079552,-21.6055654018176,
0.));
#190724=CARTESIAN_POINT('Ctrl Pts',(10.7695073079552,-21.6055654018176,
12.));
#190725=CARTESIAN_POINT('Ctrl Pts',(10.7533157705941,-21.5906348951743,
0.));
#190726=CARTESIAN_POINT('Ctrl Pts',(10.7533157705941,-21.5906348951743,
12.));
#190727=CARTESIAN_POINT('Ctrl Pts',(10.7372341280467,-21.5757290954371,
0.));
#190728=CARTESIAN_POINT('Ctrl Pts',(10.7372341280467,-21.5757290954371,
12.));
#190729=CARTESIAN_POINT('Ctrl Pts',(10.7212626509816,-21.5608487586468,
0.));
#190730=CARTESIAN_POINT('Ctrl Pts',(10.7212626509816,-21.5608487586468,
12.));
#190731=CARTESIAN_POINT('Ctrl Pts',(10.7054016114571,-21.5459946493955,
0.));
#190732=CARTESIAN_POINT('Ctrl Pts',(10.7054016114571,-21.5459946493955,
12.));
#190733=CARTESIAN_POINT('Ctrl Pts',(10.689651282929,-21.5311675409807,0.));
#190734=CARTESIAN_POINT('Ctrl Pts',(10.689651282929,-21.5311675409807,12.));
#190735=CARTESIAN_POINT('Ctrl Pts',(10.6740119402834,-21.51636821558,0.));
#190736=CARTESIAN_POINT('Ctrl Pts',(10.6740119402834,-21.51636821558,12.));
#190737=CARTESIAN_POINT('Ctrl Pts',(10.6584838598939,-21.5015974644449,
0.));
#190738=CARTESIAN_POINT('Ctrl Pts',(10.6584838598939,-21.5015974644449,
12.));
#190739=CARTESIAN_POINT('Ctrl Pts',(10.6430673196607,-21.4868560880889,
0.));
#190740=CARTESIAN_POINT('Ctrl Pts',(10.6430673196607,-21.4868560880889,
12.));
#190741=CARTESIAN_POINT('Ctrl Pts',(10.6277625990456,-21.4721448964766,
0.));
#190742=CARTESIAN_POINT('Ctrl Pts',(10.6277625990456,-21.4721448964766,
12.));
#190743=CARTESIAN_POINT('Ctrl Pts',(10.6125699790961,-21.4574647092097,
0.));
#190744=CARTESIAN_POINT('Ctrl Pts',(10.6125699790961,-21.4574647092097,
12.));
#190745=CARTESIAN_POINT('Ctrl Pts',(10.5974897424622,-21.4428163557144,
0.));
#190746=CARTESIAN_POINT('Ctrl Pts',(10.5974897424622,-21.4428163557144,
12.));
#190747=CARTESIAN_POINT('Ctrl Pts',(10.5825221734573,-21.4282006754631,
0.));
#190748=CARTESIAN_POINT('Ctrl Pts',(10.5825221734573,-21.4282006754631,
12.));
#190749=CARTESIAN_POINT('Ctrl Pts',(10.5676675581108,-21.4136185181979,
0.));
#190750=CARTESIAN_POINT('Ctrl Pts',(10.5676675581108,-21.4136185181979,
12.));
#190751=CARTESIAN_POINT('Ctrl Pts',(10.5529261842108,-21.3990707441497,
0.));
#190752=CARTESIAN_POINT('Ctrl Pts',(10.5529261842108,-21.3990707441497,
12.));
#190753=CARTESIAN_POINT('Ctrl Pts',(10.5382983413421,-21.3845582242602,
0.));
#190754=CARTESIAN_POINT('Ctrl Pts',(10.5382983413421,-21.3845582242602,
12.));
#190755=CARTESIAN_POINT('Ctrl Pts',(10.5237843209057,-21.3700818403936,
0.));
#190756=CARTESIAN_POINT('Ctrl Pts',(10.5237843209057,-21.3700818403936,
12.));
#190757=CARTESIAN_POINT('Ctrl Pts',(10.5093844161685,-21.3556424855814,
0.));
#190758=CARTESIAN_POINT('Ctrl Pts',(10.5093844161685,-21.3556424855814,
12.));
#190759=CARTESIAN_POINT('Ctrl Pts',(10.4950989223336,-21.3412410642904,
0.));
#190760=CARTESIAN_POINT('Ctrl Pts',(10.4950989223336,-21.3412410642904,
12.));
#190761=CARTESIAN_POINT('Ctrl Pts',(10.4809281365931,-21.3268784926819,
0.));
#190762=CARTESIAN_POINT('Ctrl Pts',(10.4809281365931,-21.3268784926819,
12.));
#190763=CARTESIAN_POINT('Ctrl Pts',(10.4668723581768,-21.3125556988731,
0.));
#190764=CARTESIAN_POINT('Ctrl Pts',(10.4668723581768,-21.3125556988731,
12.));
#190765=CARTESIAN_POINT('Ctrl Pts',(10.4529318883874,-21.2982736231931,
0.));
#190766=CARTESIAN_POINT('Ctrl Pts',(10.4529318883874,-21.2982736231931,
12.));
#190767=CARTESIAN_POINT('Ctrl Pts',(10.4391070306391,-21.2840332184483,
0.));
#190768=CARTESIAN_POINT('Ctrl Pts',(10.4391070306391,-21.2840332184483,
12.));
#190769=CARTESIAN_POINT('Ctrl Pts',(10.42539809054,-21.2698354502403,0.));
#190770=CARTESIAN_POINT('Ctrl Pts',(10.42539809054,-21.2698354502403,12.));
#190771=CARTESIAN_POINT('Ctrl Pts',(10.4118053759588,-21.255681297275,0.));
#190772=CARTESIAN_POINT('Ctrl Pts',(10.4118053759588,-21.255681297275,12.));
#190773=CARTESIAN_POINT('Ctrl Pts',(10.3983291970846,-21.2415717516714,
0.));
#190774=CARTESIAN_POINT('Ctrl Pts',(10.3983291970846,-21.2415717516714,
12.));
#190775=CARTESIAN_POINT('Ctrl Pts',(10.3849698664786,-21.22750781927,0.));
#190776=CARTESIAN_POINT('Ctrl Pts',(10.3849698664786,-21.22750781927,12.));
#190777=CARTESIAN_POINT('Ctrl Pts',(10.371727699113,-21.2134905199345,0.));
#190778=CARTESIAN_POINT('Ctrl Pts',(10.371727699113,-21.2134905199345,12.));
#190779=CARTESIAN_POINT('Ctrl Pts',(10.3586030124587,-21.199520887919,0.));
#190780=CARTESIAN_POINT('Ctrl Pts',(10.3586030124587,-21.199520887919,12.));
#190781=CARTESIAN_POINT('Ctrl Pts',(10.34559612657,-21.1855999722416,0.));
#190782=CARTESIAN_POINT('Ctrl Pts',(10.34559612657,-21.1855999722416,12.));
#190783=CARTESIAN_POINT('Ctrl Pts',(10.3327073641572,-21.1717288370509,
0.));
#190784=CARTESIAN_POINT('Ctrl Pts',(10.3327073641572,-21.1717288370509,
12.));
#190785=CARTESIAN_POINT('Ctrl Pts',(10.3199370506544,-21.1579085619965,
0.));
#190786=CARTESIAN_POINT('Ctrl Pts',(10.3199370506544,-21.1579085619965,
12.));
#190787=CARTESIAN_POINT('Ctrl Pts',(10.3072855142687,-21.1441402425843,
0.));
#190788=CARTESIAN_POINT('Ctrl Pts',(10.3072855142687,-21.1441402425843,
12.));
#190789=CARTESIAN_POINT('Ctrl Pts',(10.2947530860721,-21.1304249906002,
0.));
#190790=CARTESIAN_POINT('Ctrl Pts',(10.2947530860721,-21.1304249906002,
12.));
#190791=CARTESIAN_POINT('Ctrl Pts',(10.2823401001072,-21.1167639345631,
0.));
#190792=CARTESIAN_POINT('Ctrl Pts',(10.2823401001072,-21.1167639345631,
12.));
#190793=CARTESIAN_POINT('Ctrl Pts',(10.2700468934744,-21.1031582201627,
0.));
#190794=CARTESIAN_POINT('Ctrl Pts',(10.2700468934744,-21.1031582201627,
12.));
#190795=CARTESIAN_POINT('Ctrl Pts',(10.2578738064181,-21.0896090107063,
0.));
#190796=CARTESIAN_POINT('Ctrl Pts',(10.2578738064181,-21.0896090107063,
12.));
#190797=CARTESIAN_POINT('Ctrl Pts',(10.2458211823912,-21.0761174875445,
0.));
#190798=CARTESIAN_POINT('Ctrl Pts',(10.2458211823912,-21.0761174875445,
12.));
#190799=CARTESIAN_POINT('Ctrl Pts',(10.2338893681567,-21.0626848505663,
0.));
#190800=CARTESIAN_POINT('Ctrl Pts',(10.2338893681567,-21.0626848505663,
12.));
#190801=CARTESIAN_POINT('Ctrl Pts',(10.2220787139154,-21.0493123187483,
0.));
#190802=CARTESIAN_POINT('Ctrl Pts',(10.2220787139154,-21.0493123187483,
12.));
#190803=CARTESIAN_POINT('Ctrl Pts',(10.2103895734123,-21.0360011306815,
0.));
#190804=CARTESIAN_POINT('Ctrl Pts',(10.2103895734123,-21.0360011306815,
12.));
#190805=CARTESIAN_POINT('Ctrl Pts',(10.1988223040425,-21.0227525451107,
0.));
#190806=CARTESIAN_POINT('Ctrl Pts',(10.1988223040425,-21.0227525451107,
12.));
#190807=CARTESIAN_POINT('Ctrl Pts',(10.187377266936,-21.0095678414486,0.));
#190808=CARTESIAN_POINT('Ctrl Pts',(10.187377266936,-21.0095678414486,12.));
#190809=CARTESIAN_POINT('Ctrl Pts',(10.1760548270767,-20.9964483203686,
0.));
#190810=CARTESIAN_POINT('Ctrl Pts',(10.1760548270767,-20.9964483203686,
12.));
#190811=CARTESIAN_POINT('Ctrl Pts',(10.1648553534568,-20.9833953044736,
0.));
#190812=CARTESIAN_POINT('Ctrl Pts',(10.1648553534568,-20.9833953044736,
12.));
#190813=CARTESIAN_POINT('Ctrl Pts',(10.1537792192065,-20.9704101389369,
0.));
#190814=CARTESIAN_POINT('Ctrl Pts',(10.1537792192065,-20.9704101389369,
12.));
#190815=CARTESIAN_POINT('Ctrl Pts',(10.1428268017256,-20.9574941921591,
0.));
#190816=CARTESIAN_POINT('Ctrl Pts',(10.1428268017256,-20.9574941921591,
12.));
#190817=CARTESIAN_POINT('Ctrl Pts',(10.1319984827908,-20.9446488563933,
0.));
#190818=CARTESIAN_POINT('Ctrl Pts',(10.1319984827908,-20.9446488563933,
12.));
#190819=CARTESIAN_POINT('Ctrl Pts',(10.1212946487057,-20.9318755484734,
0.));
#190820=CARTESIAN_POINT('Ctrl Pts',(10.1212946487057,-20.9318755484734,
12.));
#190821=CARTESIAN_POINT('Ctrl Pts',(10.1107156904836,-20.919175710627,0.));
#190822=CARTESIAN_POINT('Ctrl Pts',(10.1107156904836,-20.919175710627,12.));
#190823=CARTESIAN_POINT('Ctrl Pts',(10.1002620040076,-20.9065508112557,
0.));
#190824=CARTESIAN_POINT('Ctrl Pts',(10.1002620040076,-20.9065508112557,
12.));
#190825=CARTESIAN_POINT('Ctrl Pts',(10.0899339901915,-20.894002345737,0.));
#190826=CARTESIAN_POINT('Ctrl Pts',(10.0899339901915,-20.894002345737,12.));
#190827=CARTESIAN_POINT('Ctrl Pts',(10.0797320551154,-20.881531837184,0.));
#190828=CARTESIAN_POINT('Ctrl Pts',(10.0797320551154,-20.881531837184,12.));
#190829=CARTESIAN_POINT('Ctrl Pts',(10.0696566102218,-20.86914083737,0.));
#190830=CARTESIAN_POINT('Ctrl Pts',(10.0696566102218,-20.86914083737,12.));
#190831=CARTESIAN_POINT('Ctrl Pts',(10.0597080725375,-20.8568309277316,
0.));
#190832=CARTESIAN_POINT('Ctrl Pts',(10.0597080725375,-20.8568309277316,
12.));
#190833=CARTESIAN_POINT('Ctrl Pts',(10.0498868648733,-20.8446037203402,
0.));
#190834=CARTESIAN_POINT('Ctrl Pts',(10.0498868648733,-20.8446037203402,
12.));
#190835=CARTESIAN_POINT('Ctrl Pts',(10.0401934160234,-20.8324608588909,
0.));
#190836=CARTESIAN_POINT('Ctrl Pts',(10.0401934160234,-20.8324608588909,
12.));
#190837=CARTESIAN_POINT('Ctrl Pts',(10.0306281609435,-20.8204040196602,
0.));
#190838=CARTESIAN_POINT('Ctrl Pts',(10.0306281609435,-20.8204040196602,
12.));
#190839=CARTESIAN_POINT('Ctrl Pts',(10.0211915410095,-20.8084349126888,
0.));
#190840=CARTESIAN_POINT('Ctrl Pts',(10.0211915410095,-20.8084349126888,
12.));
#190841=CARTESIAN_POINT('Ctrl Pts',(10.0118840042786,-20.7965552829908,
0.));
#190842=CARTESIAN_POINT('Ctrl Pts',(10.0118840042786,-20.7965552829908,
12.));
#190843=CARTESIAN_POINT('Ctrl Pts',(10.0027060057389,-20.7847669117568,
0.));
#190844=CARTESIAN_POINT('Ctrl Pts',(10.0027060057389,-20.7847669117568,
12.));
#190845=CARTESIAN_POINT('Ctrl Pts',(9.9936580075464,-20.7730716175417,0.));
#190846=CARTESIAN_POINT('Ctrl Pts',(9.9936580075464,-20.7730716175417,12.));
#190847=CARTESIAN_POINT('Ctrl Pts',(9.98474047926852,-20.761471257499,0.));
#190848=CARTESIAN_POINT('Ctrl Pts',(9.98474047926852,-20.761471257499,12.));
#190849=CARTESIAN_POINT('Ctrl Pts',(9.97595389823469,-20.7499677289627,
0.));
#190850=CARTESIAN_POINT('Ctrl Pts',(9.97595389823469,-20.7499677289627,
12.));
#190851=CARTESIAN_POINT('Ctrl Pts',(9.96729874986201,-20.7385629709795,
0.));
#190852=CARTESIAN_POINT('Ctrl Pts',(9.96729874986201,-20.7385629709795,
12.));
#190853=CARTESIAN_POINT('Ctrl Pts',(9.95877552798397,-20.7272589658751,
0.));
#190854=CARTESIAN_POINT('Ctrl Pts',(9.95877552798397,-20.7272589658751,
12.));
#190855=CARTESIAN_POINT('Ctrl Pts',(9.95038473514948,-20.7160577407579,
0.));
#190856=CARTESIAN_POINT('Ctrl Pts',(9.95038473514948,-20.7160577407579,
12.));
#190857=CARTESIAN_POINT('Ctrl Pts',(9.94212688298236,-20.7049613692234,
0.));
#190858=CARTESIAN_POINT('Ctrl Pts',(9.94212688298236,-20.7049613692234,
12.));
#190859=CARTESIAN_POINT('Ctrl Pts',(9.93400249259729,-20.6939719732484,
0.));
#190860=CARTESIAN_POINT('Ctrl Pts',(9.93400249259729,-20.6939719732484,
12.));
#190861=CARTESIAN_POINT('Ctrl Pts',(9.92601209498748,-20.6830917250255,
0.));
#190862=CARTESIAN_POINT('Ctrl Pts',(9.92601209498748,-20.6830917250255,
12.));
#190863=CARTESIAN_POINT('Ctrl Pts',(9.91815623141288,-20.6723228488263,
0.));
#190864=CARTESIAN_POINT('Ctrl Pts',(9.91815623141288,-20.6723228488263,
12.));
#190865=CARTESIAN_POINT('Ctrl Pts',(9.91043545377007,-20.6616676228315,
0.));
#190866=CARTESIAN_POINT('Ctrl Pts',(9.91043545377007,-20.6616676228315,
12.));
#190867=CARTESIAN_POINT('Ctrl Pts',(9.90285032516692,-20.6511283817414,
0.));
#190868=CARTESIAN_POINT('Ctrl Pts',(9.90285032516692,-20.6511283817414,
12.));
#190869=CARTESIAN_POINT('Ctrl Pts',(9.89540142049119,-20.6407075193976,
0.));
#190870=CARTESIAN_POINT('Ctrl Pts',(9.89540142049119,-20.6407075193976,
12.));
#190871=CARTESIAN_POINT('Ctrl Pts',(9.88808932697305,-20.6304074914087,
0.));
#190872=CARTESIAN_POINT('Ctrl Pts',(9.88808932697305,-20.6304074914087,
12.));
#190873=CARTESIAN_POINT('Ctrl Pts',(9.88091464472675,-20.6202308177475,
0.));
#190874=CARTESIAN_POINT('Ctrl Pts',(9.88091464472675,-20.6202308177475,
12.));
#190875=CARTESIAN_POINT('Ctrl Pts',(9.87387798732955,-20.6101800854494,
0.));
#190876=CARTESIAN_POINT('Ctrl Pts',(9.87387798732955,-20.6101800854494,
12.));
#190877=CARTESIAN_POINT('Ctrl Pts',(9.86697998242622,-20.6002579513699,
0.));
#190878=CARTESIAN_POINT('Ctrl Pts',(9.86697998242622,-20.6002579513699,
12.));
#190879=CARTESIAN_POINT('Ctrl Pts',(9.86022127232747,-20.5904671449754,
0.));
#190880=CARTESIAN_POINT('Ctrl Pts',(9.86022127232747,-20.5904671449754,
12.));
#190881=CARTESIAN_POINT('Ctrl Pts',(9.8536025145698,-20.5808104710015,0.));
#190882=CARTESIAN_POINT('Ctrl Pts',(9.8536025145698,-20.5808104710015,12.));
#190883=CARTESIAN_POINT('Ctrl Pts',(9.84712438256277,-20.5712908125139,
0.));
#190884=CARTESIAN_POINT('Ctrl Pts',(9.84712438256277,-20.5712908125139,
12.));
#190885=CARTESIAN_POINT('Ctrl Pts',(9.84078756677565,-20.5619111362402,
0.));
#190886=CARTESIAN_POINT('Ctrl Pts',(9.84078756677565,-20.5619111362402,
12.));
#190887=CARTESIAN_POINT('Ctrl Pts',(9.83459277585315,-20.552674497646,0.));
#190888=CARTESIAN_POINT('Ctrl Pts',(9.83459277585315,-20.552674497646,12.));
#190889=CARTESIAN_POINT('Ctrl Pts',(9.82854073773876,-20.5435840460721,
0.));
#190890=CARTESIAN_POINT('Ctrl Pts',(9.82854073773876,-20.5435840460721,
12.));
#190891=CARTESIAN_POINT('Ctrl Pts',(9.82263220080362,-20.5346430299517,
0.));
#190892=CARTESIAN_POINT('Ctrl Pts',(9.82263220080362,-20.5346430299517,
12.));
#190893=CARTESIAN_POINT('Ctrl Pts',(9.81686793455942,-20.5258548000629,
0.));
#190894=CARTESIAN_POINT('Ctrl Pts',(9.81686793455942,-20.5258548000629,
12.));
#190895=CARTESIAN_POINT('Ctrl Pts',(9.81124873025281,-20.517222812284,0.));
#190896=CARTESIAN_POINT('Ctrl Pts',(9.81124873025281,-20.517222812284,12.));
#190897=CARTESIAN_POINT('Ctrl Pts',(9.80577540161087,-20.5087506310505,
0.));
#190898=CARTESIAN_POINT('Ctrl Pts',(9.80577540161087,-20.5087506310505,
12.));
#190899=CARTESIAN_POINT('Ctrl Pts',(9.80044878520948,-20.5004419312107,
0.));
#190900=CARTESIAN_POINT('Ctrl Pts',(9.80044878520948,-20.5004419312107,
12.));
#190901=CARTESIAN_POINT('Ctrl Pts',(9.7952697428833,-20.4923005087943,0.));
#190902=CARTESIAN_POINT('Ctrl Pts',(9.7952697428833,-20.4923005087943,12.));
#190903=CARTESIAN_POINT('Ctrl Pts',(9.79023916498655,-20.4843302955329,
0.));
#190904=CARTESIAN_POINT('Ctrl Pts',(9.79023916498655,-20.4843302955329,
12.));
#190905=CARTESIAN_POINT('Ctrl Pts',(9.78535797314166,-20.4765353711586,
0.));
#190906=CARTESIAN_POINT('Ctrl Pts',(9.78535797314166,-20.4765353711586,
12.));
#190907=CARTESIAN_POINT('Ctrl Pts',(9.7806271237332,-20.4689199790669,0.));
#190908=CARTESIAN_POINT('Ctrl Pts',(9.7806271237332,-20.4689199790669,12.));
#190909=CARTESIAN_POINT('Ctrl Pts',(9.77604760815528,-20.4614885274975,
0.));
#190910=CARTESIAN_POINT('Ctrl Pts',(9.77604760815528,-20.4614885274975,
12.));
#190911=CARTESIAN_POINT('Ctrl Pts',(9.77162045104069,-20.4542455817527,
0.));
#190912=CARTESIAN_POINT('Ctrl Pts',(9.77162045104069,-20.4542455817527,
12.));
#190913=CARTESIAN_POINT('Ctrl Pts',(9.76734670980891,-20.447195862298,0.));
#190914=CARTESIAN_POINT('Ctrl Pts',(9.76734670980891,-20.447195862298,12.));
#190915=CARTESIAN_POINT('Ctrl Pts',(9.76322747195494,-20.44034423294,0.));
#190916=CARTESIAN_POINT('Ctrl Pts',(9.76322747195494,-20.44034423294,12.));
#190917=CARTESIAN_POINT('Ctrl Pts',(9.75926386289922,-20.4336957355473,
0.));
#190918=CARTESIAN_POINT('Ctrl Pts',(9.75926386289922,-20.4336957355473,
12.));
#190919=CARTESIAN_POINT('Ctrl Pts',(9.75545705902417,-20.4272556476629,
0.));
#190920=CARTESIAN_POINT('Ctrl Pts',(9.75545705902417,-20.4272556476629,
12.));
#190921=CARTESIAN_POINT('Ctrl Pts',(9.75180829786429,-20.4210295275817,
0.));
#190922=CARTESIAN_POINT('Ctrl Pts',(9.75180829786429,-20.4210295275817,
12.));
#190923=CARTESIAN_POINT('Ctrl Pts',(9.74831889242173,-20.4150232777393,
0.));
#190924=CARTESIAN_POINT('Ctrl Pts',(9.74831889242173,-20.4150232777393,
12.));
#190925=CARTESIAN_POINT('Ctrl Pts',(9.74499021838537,-20.4092430879861,
0.));
#190926=CARTESIAN_POINT('Ctrl Pts',(9.74499021838537,-20.4092430879861,
12.));
#190927=CARTESIAN_POINT('Ctrl Pts',(9.74182369656271,-20.4036953576549,
0.));
#190928=CARTESIAN_POINT('Ctrl Pts',(9.74182369656271,-20.4036953576549,
12.));
#190929=CARTESIAN_POINT('Ctrl Pts',(9.738820776132,-20.3983866213331,0.));
#190930=CARTESIAN_POINT('Ctrl Pts',(9.738820776132,-20.3983866213331,12.));
#190931=CARTESIAN_POINT('Ctrl Pts',(9.73598292014242,-20.3933234845647,
0.));
#190932=CARTESIAN_POINT('Ctrl Pts',(9.73598292014242,-20.3933234845647,
12.));
#190933=CARTESIAN_POINT('Ctrl Pts',(9.73331167102807,-20.3885129129912,
0.));
#190934=CARTESIAN_POINT('Ctrl Pts',(9.73331167102807,-20.3885129129912,
12.));
#190935=CARTESIAN_POINT('Ctrl Pts',(9.73080870123726,-20.3839624556742,
0.));
#190936=CARTESIAN_POINT('Ctrl Pts',(9.73080870123726,-20.3839624556742,
12.));
#190937=CARTESIAN_POINT('Ctrl Pts',(9.72847589116541,-20.3796805893304,
0.));
#190938=CARTESIAN_POINT('Ctrl Pts',(9.72847589116541,-20.3796805893304,
12.));
#190939=CARTESIAN_POINT('Ctrl Pts',(9.7263153173288,-20.3756766651951,0.));
#190940=CARTESIAN_POINT('Ctrl Pts',(9.7263153173288,-20.3756766651951,12.));
#190941=CARTESIAN_POINT('Ctrl Pts',(9.72432910043194,-20.371960235676,0.));
#190942=CARTESIAN_POINT('Ctrl Pts',(9.72432910043194,-20.371960235676,12.));
#190943=CARTESIAN_POINT('Ctrl Pts',(9.72251930722489,-20.3685406190576,
0.));
#190944=CARTESIAN_POINT('Ctrl Pts',(9.72251930722489,-20.3685406190576,
12.));
#190945=CARTESIAN_POINT('Ctrl Pts',(9.7208877838108,-20.3654261611056,0.));
#190946=CARTESIAN_POINT('Ctrl Pts',(9.7208877838108,-20.3654261611056,12.));
#190947=CARTESIAN_POINT('Ctrl Pts',(9.71943648548099,-20.3626256913981,
0.));
#190948=CARTESIAN_POINT('Ctrl Pts',(9.71943648548099,-20.3626256913981,
12.));
#190949=CARTESIAN_POINT('Ctrl Pts',(9.71816778328006,-20.3601498764344,
0.));
#190950=CARTESIAN_POINT('Ctrl Pts',(9.71816778328006,-20.3601498764344,
12.));
#190951=CARTESIAN_POINT('Ctrl Pts',(9.71708493723096,-20.3580133103356,
0.));
#190952=CARTESIAN_POINT('Ctrl Pts',(9.71708493723096,-20.3580133103356,
12.));
#190953=CARTESIAN_POINT('Ctrl Pts',(9.71619192554185,-20.3562337557875,
0.));
#190954=CARTESIAN_POINT('Ctrl Pts',(9.71619192554185,-20.3562337557875,
12.));
#190955=CARTESIAN_POINT('Ctrl Pts',(9.71549257088172,-20.3548282742361,
0.));
#190956=CARTESIAN_POINT('Ctrl Pts',(9.71549257088172,-20.3548282742361,
12.));
#190957=CARTESIAN_POINT('Ctrl Pts',(9.7149897805202,-20.3538098605706,0.));
#190958=CARTESIAN_POINT('Ctrl Pts',(9.7149897805202,-20.3538098605706,12.));
#190959=CARTESIAN_POINT('Ctrl Pts',(9.7147459035068,-20.3533097561886,0.));
#190960=CARTESIAN_POINT('Ctrl Pts',(9.7147459035068,-20.3533097561886,12.));
#190961=CARTESIAN_POINT('Ctrl Pts',(9.71465227853041,-20.3531126095522,
0.));
#190962=CARTESIAN_POINT('Ctrl Pts',(9.71465227853041,-20.3531126095522,
12.));
#190963=CARTESIAN_POINT('Ctrl Pts',(9.71462954053041,-20.353060251684,0.));
#190964=CARTESIAN_POINT('Ctrl Pts',(9.71462954053041,-20.353060251684,12.));
#190965=CARTESIAN_POINT('Ctrl Pts',(9.71462809124915,-20.353053841303,0.));
#190966=CARTESIAN_POINT('Ctrl Pts',(9.71462809124915,-20.353053841303,12.));
#190967=CARTESIAN_POINT('',(12.4230808101438,-22.8400320311649,0.));
#190968=CARTESIAN_POINT('Ctrl Pts',(12.4230808101438,-22.8400320311649,
0.));
#190969=CARTESIAN_POINT('Ctrl Pts',(12.418215285186,-22.8370364396459,0.));
#190970=CARTESIAN_POINT('Ctrl Pts',(12.4084933766346,-22.8310435872748,
0.));
#190971=CARTESIAN_POINT('Ctrl Pts',(12.3939379378998,-22.8220493007173,
0.));
#190972=CARTESIAN_POINT('Ctrl Pts',(12.374585536673,-22.81004690224,0.));
#190973=CARTESIAN_POINT('Ctrl Pts',(12.3504864740319,-22.795027221673,0.));
#190974=CARTESIAN_POINT('Ctrl Pts',(12.3264788926075,-22.7799908974768,
0.));
#190975=CARTESIAN_POINT('Ctrl Pts',(12.3025628601792,-22.764938010105,0.));
#190976=CARTESIAN_POINT('Ctrl Pts',(12.2787384750742,-22.7498686970069,
0.));
#190977=CARTESIAN_POINT('Ctrl Pts',(12.2550058702395,-22.7347831655287,
0.));
#190978=CARTESIAN_POINT('Ctrl Pts',(12.2313652198061,-22.7196817119374,
0.));
#190979=CARTESIAN_POINT('Ctrl Pts',(12.2078167360284,-22.7045647168747,
0.));
#190980=CARTESIAN_POINT('Ctrl Pts',(12.1843606579261,-22.6894326205037,
0.));
#190981=CARTESIAN_POINT('Ctrl Pts',(12.1609972423099,-22.6742859034944,
0.));
#190982=CARTESIAN_POINT('Ctrl Pts',(12.1377267537145,-22.6591250653965,
0.));
#190983=CARTESIAN_POINT('Ctrl Pts',(12.1145494550383,-22.6439506046605,
0.));
#190984=CARTESIAN_POINT('Ctrl Pts',(12.0914655972823,-22.6287629967056,
0.));
#190985=CARTESIAN_POINT('Ctrl Pts',(12.0684754113862,-22.6135626764898,
0.));
#190986=CARTESIAN_POINT('Ctrl Pts',(12.0455791139128,-22.5983500505644,
0.));
#190987=CARTESIAN_POINT('Ctrl Pts',(12.0227769113127,-22.5831255061282,
0.));
#190988=CARTESIAN_POINT('Ctrl Pts',(12.0000690046694,-22.5678894211181,
0.));
#190989=CARTESIAN_POINT('Ctrl Pts',(11.9774555943496,-22.5526421741158,
0.));
#190990=CARTESIAN_POINT('Ctrl Pts',(11.9549368843997,-22.5373841537307,
0.));
#190991=CARTESIAN_POINT('Ctrl Pts',(11.9325130877803,-22.5221157697883,
0.));
#190992=CARTESIAN_POINT('Ctrl Pts',(11.9101844254557,-22.5068374513973,
0.));
#190993=CARTESIAN_POINT('Ctrl Pts',(11.8879511239942,-22.4915496418485,
0.));
#190994=CARTESIAN_POINT('Ctrl Pts',(11.8658134137019,-22.4762527946702,
0.));
#190995=CARTESIAN_POINT('Ctrl Pts',(11.8437715264487,-22.4609473690472,
0.));
#190996=CARTESIAN_POINT('Ctrl Pts',(11.8218256937889,-22.4456338258735,
0.));
#190997=CARTESIAN_POINT('Ctrl Pts',(11.7999761445173,-22.430312622646,0.));
#190998=CARTESIAN_POINT('Ctrl Pts',(11.7782231042039,-22.4149842125008,
0.));
#190999=CARTESIAN_POINT('Ctrl Pts',(11.7565667964764,-22.3996490469191,
0.));
#191000=CARTESIAN_POINT('Ctrl Pts',(11.7350074437961,-22.3843075773899,
0.));
#191001=CARTESIAN_POINT('Ctrl Pts',(11.7135452684532,-22.3689602575491,
0.));
#191002=CARTESIAN_POINT('Ctrl Pts',(11.6921804934056,-22.3536075450029,
0.));
#191003=CARTESIAN_POINT('Ctrl Pts',(11.6709133432985,-22.3382499035619,
0.));
#191004=CARTESIAN_POINT('Ctrl Pts',(11.6497440449857,-22.3228878043976,
0.));
#191005=CARTESIAN_POINT('Ctrl Pts',(11.6286728270009,-22.3075217249049,
0.));
#191006=CARTESIAN_POINT('Ctrl Pts',(11.6076999192357,-22.2921521480356,
0.));
#191007=CARTESIAN_POINT('Ctrl Pts',(11.5868255525188,-22.2767795614348,
0.));
#191008=CARTESIAN_POINT('Ctrl Pts',(11.5660499582403,-22.2614044566898,
0.));
#191009=CARTESIAN_POINT('Ctrl Pts',(11.5453733679121,-22.2460273284654,
0.));
#191010=CARTESIAN_POINT('Ctrl Pts',(11.5247960128477,-22.2306486738901,
0.));
#191011=CARTESIAN_POINT('Ctrl Pts',(11.5043181244242,-22.2152689931022,
0.));
#191012=CARTESIAN_POINT('Ctrl Pts',(11.483939934259,-22.1998887896436,0.));
#191013=CARTESIAN_POINT('Ctrl Pts',(11.463661674411,-22.184508570917,0.));
#191014=CARTESIAN_POINT('Ctrl Pts',(11.443483577557,-22.1691288486096,0.));
#191015=CARTESIAN_POINT('Ctrl Pts',(11.4234058771742,-22.1537501391487,
0.));
#191016=CARTESIAN_POINT('Ctrl Pts',(11.4034288076908,-22.1383729640964,
0.));
#191017=CARTESIAN_POINT('Ctrl Pts',(11.3835526044256,-22.1229978500186,
0.));
#191018=CARTESIAN_POINT('Ctrl Pts',(11.3637775035367,-22.1076253283979,
0.));
#191019=CARTESIAN_POINT('Ctrl Pts',(11.3441037419553,-22.0922559355294,
0.));
#191020=CARTESIAN_POINT('Ctrl Pts',(11.3245315573168,-22.0768902124267,
0.));
#191021=CARTESIAN_POINT('Ctrl Pts',(11.3050611878771,-22.0615287047179,
0.));
#191022=CARTESIAN_POINT('Ctrl Pts',(11.2856928724374,-22.046171962566,0.));
#191023=CARTESIAN_POINT('Ctrl Pts',(11.2664268504206,-22.030820540835,0.));
#191024=CARTESIAN_POINT('Ctrl Pts',(11.2472633619275,-22.0154749992363,
0.));
#191025=CARTESIAN_POINT('Ctrl Pts',(11.2282026477896,-22.0001359024839,
0.));
#191026=CARTESIAN_POINT('Ctrl Pts',(11.2092449496125,-21.9848038204439,
0.));
#191027=CARTESIAN_POINT('Ctrl Pts',(11.190390509811,-21.9694793282914,0.));
#191028=CARTESIAN_POINT('Ctrl Pts',(11.1716395716376,-21.9541630066506,
0.));
#191029=CARTESIAN_POINT('Ctrl Pts',(11.1529923792003,-21.9388554416439,
0.));
#191030=CARTESIAN_POINT('Ctrl Pts',(11.1344491774741,-21.923557224952,0.));
#191031=CARTESIAN_POINT('Ctrl Pts',(11.1160102123024,-21.9082689538688,
0.));
#191032=CARTESIAN_POINT('Ctrl Pts',(11.0976757303944,-21.8929912313608,
0.));
#191033=CARTESIAN_POINT('Ctrl Pts',(11.0794459793057,-21.877724666119,0.));
#191034=CARTESIAN_POINT('Ctrl Pts',(11.0613212074363,-21.8624698726318,
0.));
#191035=CARTESIAN_POINT('Ctrl Pts',(11.0433016640807,-21.8472274713103,
0.));
#191036=CARTESIAN_POINT('Ctrl Pts',(11.0253875994598,-21.8319980886033,
0.));
#191037=CARTESIAN_POINT('Ctrl Pts',(11.0075792647477,-21.8167823571168,
0.));
#191038=CARTESIAN_POINT('Ctrl Pts',(10.9898769120912,-21.8015809157301,
0.));
#191039=CARTESIAN_POINT('Ctrl Pts',(10.9722807946155,-21.7863944097141,
0.));
#191040=CARTESIAN_POINT('Ctrl Pts',(10.9547911664455,-21.7712234908464,
0.));
#191041=CARTESIAN_POINT('Ctrl Pts',(10.9374082827444,-21.7560688175247,
0.));
#191042=CARTESIAN_POINT('Ctrl Pts',(10.9201323997384,-21.7409310548797,
0.));
#191043=CARTESIAN_POINT('Ctrl Pts',(10.902963774734,-21.7258108748873,0.));
#191044=CARTESIAN_POINT('Ctrl Pts',(10.8859026661293,-21.7107089564825,
0.));
#191045=CARTESIAN_POINT('Ctrl Pts',(10.8689493334095,-21.6956259856672,
0.));
#191046=CARTESIAN_POINT('Ctrl Pts',(10.8521040371835,-21.6805626556467,
0.));
#191047=CARTESIAN_POINT('Ctrl Pts',(10.8353670392272,-21.6655196669732,
0.));
#191048=CARTESIAN_POINT('Ctrl Pts',(10.8187386025136,-21.6504977276866,
0.));
#191049=CARTESIAN_POINT('Ctrl Pts',(10.8022189912369,-21.6354975534557,
0.));
#191050=CARTESIAN_POINT('Ctrl Pts',(10.7858084708261,-21.6205198677173,
0.));
#191051=CARTESIAN_POINT('Ctrl Pts',(10.7695073079552,-21.6055654018176,
0.));
#191052=CARTESIAN_POINT('Ctrl Pts',(10.7533157705941,-21.5906348951743,
0.));
#191053=CARTESIAN_POINT('Ctrl Pts',(10.7372341280467,-21.5757290954371,
0.));
#191054=CARTESIAN_POINT('Ctrl Pts',(10.7212626509816,-21.5608487586468,
0.));
#191055=CARTESIAN_POINT('Ctrl Pts',(10.7054016114571,-21.5459946493955,
0.));
#191056=CARTESIAN_POINT('Ctrl Pts',(10.689651282929,-21.5311675409807,0.));
#191057=CARTESIAN_POINT('Ctrl Pts',(10.6740119402834,-21.51636821558,0.));
#191058=CARTESIAN_POINT('Ctrl Pts',(10.6584838598939,-21.5015974644449,
0.));
#191059=CARTESIAN_POINT('Ctrl Pts',(10.6430673196607,-21.4868560880889,
0.));
#191060=CARTESIAN_POINT('Ctrl Pts',(10.6277625990456,-21.4721448964766,
0.));
#191061=CARTESIAN_POINT('Ctrl Pts',(10.6125699790961,-21.4574647092097,
0.));
#191062=CARTESIAN_POINT('Ctrl Pts',(10.5974897424622,-21.4428163557144,
0.));
#191063=CARTESIAN_POINT('Ctrl Pts',(10.5825221734573,-21.4282006754631,
0.));
#191064=CARTESIAN_POINT('Ctrl Pts',(10.5676675581108,-21.4136185181979,
0.));
#191065=CARTESIAN_POINT('Ctrl Pts',(10.5529261842108,-21.3990707441497,
0.));
#191066=CARTESIAN_POINT('Ctrl Pts',(10.5382983413421,-21.3845582242602,
0.));
#191067=CARTESIAN_POINT('Ctrl Pts',(10.5237843209057,-21.3700818403936,
0.));
#191068=CARTESIAN_POINT('Ctrl Pts',(10.5093844161685,-21.3556424855814,
0.));
#191069=CARTESIAN_POINT('Ctrl Pts',(10.4950989223336,-21.3412410642904,
0.));
#191070=CARTESIAN_POINT('Ctrl Pts',(10.4809281365931,-21.3268784926819,
0.));
#191071=CARTESIAN_POINT('Ctrl Pts',(10.4668723581768,-21.3125556988731,
0.));
#191072=CARTESIAN_POINT('Ctrl Pts',(10.4529318883874,-21.2982736231931,
0.));
#191073=CARTESIAN_POINT('Ctrl Pts',(10.4391070306391,-21.2840332184483,
0.));
#191074=CARTESIAN_POINT('Ctrl Pts',(10.42539809054,-21.2698354502403,0.));
#191075=CARTESIAN_POINT('Ctrl Pts',(10.4118053759588,-21.255681297275,0.));
#191076=CARTESIAN_POINT('Ctrl Pts',(10.3983291970846,-21.2415717516714,
0.));
#191077=CARTESIAN_POINT('Ctrl Pts',(10.3849698664786,-21.22750781927,0.));
#191078=CARTESIAN_POINT('Ctrl Pts',(10.371727699113,-21.2134905199345,0.));
#191079=CARTESIAN_POINT('Ctrl Pts',(10.3586030124587,-21.199520887919,0.));
#191080=CARTESIAN_POINT('Ctrl Pts',(10.34559612657,-21.1855999722416,0.));
#191081=CARTESIAN_POINT('Ctrl Pts',(10.3327073641572,-21.1717288370509,
0.));
#191082=CARTESIAN_POINT('Ctrl Pts',(10.3199370506544,-21.1579085619965,
0.));
#191083=CARTESIAN_POINT('Ctrl Pts',(10.3072855142687,-21.1441402425843,
0.));
#191084=CARTESIAN_POINT('Ctrl Pts',(10.2947530860721,-21.1304249906002,
0.));
#191085=CARTESIAN_POINT('Ctrl Pts',(10.2823401001072,-21.1167639345631,
0.));
#191086=CARTESIAN_POINT('Ctrl Pts',(10.2700468934744,-21.1031582201627,
0.));
#191087=CARTESIAN_POINT('Ctrl Pts',(10.2578738064181,-21.0896090107063,
0.));
#191088=CARTESIAN_POINT('Ctrl Pts',(10.2458211823912,-21.0761174875445,
0.));
#191089=CARTESIAN_POINT('Ctrl Pts',(10.2338893681567,-21.0626848505663,
0.));
#191090=CARTESIAN_POINT('Ctrl Pts',(10.2220787139154,-21.0493123187483,
0.));
#191091=CARTESIAN_POINT('Ctrl Pts',(10.2103895734123,-21.0360011306815,
0.));
#191092=CARTESIAN_POINT('Ctrl Pts',(10.1988223040425,-21.0227525451107,
0.));
#191093=CARTESIAN_POINT('Ctrl Pts',(10.187377266936,-21.0095678414486,0.));
#191094=CARTESIAN_POINT('Ctrl Pts',(10.1760548270767,-20.9964483203686,
0.));
#191095=CARTESIAN_POINT('Ctrl Pts',(10.1648553534568,-20.9833953044736,
0.));
#191096=CARTESIAN_POINT('Ctrl Pts',(10.1537792192065,-20.9704101389369,
0.));
#191097=CARTESIAN_POINT('Ctrl Pts',(10.1428268017256,-20.9574941921591,
0.));
#191098=CARTESIAN_POINT('Ctrl Pts',(10.1319984827908,-20.9446488563933,
0.));
#191099=CARTESIAN_POINT('Ctrl Pts',(10.1212946487057,-20.9318755484734,
0.));
#191100=CARTESIAN_POINT('Ctrl Pts',(10.1107156904836,-20.919175710627,0.));
#191101=CARTESIAN_POINT('Ctrl Pts',(10.1002620040076,-20.9065508112557,
0.));
#191102=CARTESIAN_POINT('Ctrl Pts',(10.0899339901915,-20.894002345737,0.));
#191103=CARTESIAN_POINT('Ctrl Pts',(10.0797320551154,-20.881531837184,0.));
#191104=CARTESIAN_POINT('Ctrl Pts',(10.0696566102218,-20.86914083737,0.));
#191105=CARTESIAN_POINT('Ctrl Pts',(10.0597080725375,-20.8568309277316,
0.));
#191106=CARTESIAN_POINT('Ctrl Pts',(10.0498868648733,-20.8446037203402,
0.));
#191107=CARTESIAN_POINT('Ctrl Pts',(10.0401934160234,-20.8324608588909,
0.));
#191108=CARTESIAN_POINT('Ctrl Pts',(10.0306281609435,-20.8204040196602,
0.));
#191109=CARTESIAN_POINT('Ctrl Pts',(10.0211915410095,-20.8084349126888,
0.));
#191110=CARTESIAN_POINT('Ctrl Pts',(10.0118840042786,-20.7965552829908,
0.));
#191111=CARTESIAN_POINT('Ctrl Pts',(10.0027060057389,-20.7847669117568,
0.));
#191112=CARTESIAN_POINT('Ctrl Pts',(9.9936580075464,-20.7730716175417,0.));
#191113=CARTESIAN_POINT('Ctrl Pts',(9.98474047926852,-20.761471257499,0.));
#191114=CARTESIAN_POINT('Ctrl Pts',(9.97595389823469,-20.7499677289627,
0.));
#191115=CARTESIAN_POINT('Ctrl Pts',(9.96729874986201,-20.7385629709795,
0.));
#191116=CARTESIAN_POINT('Ctrl Pts',(9.95877552798397,-20.7272589658751,
0.));
#191117=CARTESIAN_POINT('Ctrl Pts',(9.95038473514948,-20.7160577407579,
0.));
#191118=CARTESIAN_POINT('Ctrl Pts',(9.94212688298236,-20.7049613692234,
0.));
#191119=CARTESIAN_POINT('Ctrl Pts',(9.93400249259729,-20.6939719732484,
0.));
#191120=CARTESIAN_POINT('Ctrl Pts',(9.92601209498748,-20.6830917250255,
0.));
#191121=CARTESIAN_POINT('Ctrl Pts',(9.91815623141288,-20.6723228488263,
0.));
#191122=CARTESIAN_POINT('Ctrl Pts',(9.91043545377007,-20.6616676228315,
0.));
#191123=CARTESIAN_POINT('Ctrl Pts',(9.90285032516692,-20.6511283817414,
0.));
#191124=CARTESIAN_POINT('Ctrl Pts',(9.89540142049119,-20.6407075193976,
0.));
#191125=CARTESIAN_POINT('Ctrl Pts',(9.88808932697305,-20.6304074914087,
0.));
#191126=CARTESIAN_POINT('Ctrl Pts',(9.88091464472675,-20.6202308177475,
0.));
#191127=CARTESIAN_POINT('Ctrl Pts',(9.87387798732955,-20.6101800854494,
0.));
#191128=CARTESIAN_POINT('Ctrl Pts',(9.86697998242622,-20.6002579513699,
0.));
#191129=CARTESIAN_POINT('Ctrl Pts',(9.86022127232747,-20.5904671449754,
0.));
#191130=CARTESIAN_POINT('Ctrl Pts',(9.8536025145698,-20.5808104710015,0.));
#191131=CARTESIAN_POINT('Ctrl Pts',(9.84712438256277,-20.5712908125139,
0.));
#191132=CARTESIAN_POINT('Ctrl Pts',(9.84078756677565,-20.5619111362402,
0.));
#191133=CARTESIAN_POINT('Ctrl Pts',(9.83459277585315,-20.552674497646,0.));
#191134=CARTESIAN_POINT('Ctrl Pts',(9.82854073773876,-20.5435840460721,
0.));
#191135=CARTESIAN_POINT('Ctrl Pts',(9.82263220080362,-20.5346430299517,
0.));
#191136=CARTESIAN_POINT('Ctrl Pts',(9.81686793455942,-20.5258548000629,
0.));
#191137=CARTESIAN_POINT('Ctrl Pts',(9.81124873025281,-20.517222812284,0.));
#191138=CARTESIAN_POINT('Ctrl Pts',(9.80577540161087,-20.5087506310505,
0.));
#191139=CARTESIAN_POINT('Ctrl Pts',(9.80044878520948,-20.5004419312107,
0.));
#191140=CARTESIAN_POINT('Ctrl Pts',(9.7952697428833,-20.4923005087943,0.));
#191141=CARTESIAN_POINT('Ctrl Pts',(9.79023916498655,-20.4843302955329,
0.));
#191142=CARTESIAN_POINT('Ctrl Pts',(9.78535797314166,-20.4765353711586,
0.));
#191143=CARTESIAN_POINT('Ctrl Pts',(9.7806271237332,-20.4689199790669,0.));
#191144=CARTESIAN_POINT('Ctrl Pts',(9.77604760815528,-20.4614885274975,
0.));
#191145=CARTESIAN_POINT('Ctrl Pts',(9.77162045104069,-20.4542455817527,
0.));
#191146=CARTESIAN_POINT('Ctrl Pts',(9.76734670980891,-20.447195862298,0.));
#191147=CARTESIAN_POINT('Ctrl Pts',(9.76322747195494,-20.44034423294,0.));
#191148=CARTESIAN_POINT('Ctrl Pts',(9.75926386289922,-20.4336957355473,
0.));
#191149=CARTESIAN_POINT('Ctrl Pts',(9.75545705902417,-20.4272556476629,
0.));
#191150=CARTESIAN_POINT('Ctrl Pts',(9.75180829786429,-20.4210295275817,
0.));
#191151=CARTESIAN_POINT('Ctrl Pts',(9.74831889242173,-20.4150232777393,
0.));
#191152=CARTESIAN_POINT('Ctrl Pts',(9.74499021838537,-20.4092430879861,
0.));
#191153=CARTESIAN_POINT('Ctrl Pts',(9.74182369656271,-20.4036953576549,
0.));
#191154=CARTESIAN_POINT('Ctrl Pts',(9.738820776132,-20.3983866213331,0.));
#191155=CARTESIAN_POINT('Ctrl Pts',(9.73598292014242,-20.3933234845647,
0.));
#191156=CARTESIAN_POINT('Ctrl Pts',(9.73331167102807,-20.3885129129912,
0.));
#191157=CARTESIAN_POINT('Ctrl Pts',(9.73080870123726,-20.3839624556742,
0.));
#191158=CARTESIAN_POINT('Ctrl Pts',(9.72847589116541,-20.3796805893304,
0.));
#191159=CARTESIAN_POINT('Ctrl Pts',(9.7263153173288,-20.3756766651951,0.));
#191160=CARTESIAN_POINT('Ctrl Pts',(9.72432910043194,-20.371960235676,0.));
#191161=CARTESIAN_POINT('Ctrl Pts',(9.72251930722489,-20.3685406190576,
0.));
#191162=CARTESIAN_POINT('Ctrl Pts',(9.7208877838108,-20.3654261611056,0.));
#191163=CARTESIAN_POINT('Ctrl Pts',(9.71943648548099,-20.3626256913981,
0.));
#191164=CARTESIAN_POINT('Ctrl Pts',(9.71816778328006,-20.3601498764344,
0.));
#191165=CARTESIAN_POINT('Ctrl Pts',(9.71708493723096,-20.3580133103356,
0.));
#191166=CARTESIAN_POINT('Ctrl Pts',(9.71619192554185,-20.3562337557875,
0.));
#191167=CARTESIAN_POINT('Ctrl Pts',(9.71549257088172,-20.3548282742361,
0.));
#191168=CARTESIAN_POINT('Ctrl Pts',(9.7149897805202,-20.3538098605706,0.));
#191169=CARTESIAN_POINT('Ctrl Pts',(9.7147459035068,-20.3533097561886,0.));
#191170=CARTESIAN_POINT('Ctrl Pts',(9.71465227853041,-20.3531126095522,
0.));
#191171=CARTESIAN_POINT('Ctrl Pts',(9.71462954053041,-20.353060251684,0.));
#191172=CARTESIAN_POINT('Ctrl Pts',(9.71462809124915,-20.353053841303,0.));
#191173=CARTESIAN_POINT('',(12.4230808101438,-22.8400320311649,0.));
#191174=CARTESIAN_POINT('Ctrl Pts',(7.52250298901263,-21.2610617890679,
0.));
#191175=CARTESIAN_POINT('Ctrl Pts',(7.52250298901263,-21.2610617890679,
12.));
#191176=CARTESIAN_POINT('Ctrl Pts',(7.52250649703969,-21.2610673466886,
0.));
#191177=CARTESIAN_POINT('Ctrl Pts',(7.52250649703969,-21.2610673466886,
12.));
#191178=CARTESIAN_POINT('Ctrl Pts',(7.52252744144903,-21.2611204474866,
0.));
#191179=CARTESIAN_POINT('Ctrl Pts',(7.52252744144903,-21.2611204474866,
12.));
#191180=CARTESIAN_POINT('Ctrl Pts',(7.5226006423166,-21.261326054066,0.));
#191181=CARTESIAN_POINT('Ctrl Pts',(7.5226006423166,-21.261326054066,12.));
#191182=CARTESIAN_POINT('Ctrl Pts',(7.52278182242669,-21.2618521283555,
0.));
#191183=CARTESIAN_POINT('Ctrl Pts',(7.52278182242669,-21.2618521283555,
12.));
#191184=CARTESIAN_POINT('Ctrl Pts',(7.52314642316199,-21.262927782038,0.));
#191185=CARTESIAN_POINT('Ctrl Pts',(7.52314642316199,-21.262927782038,12.));
#191186=CARTESIAN_POINT('Ctrl Pts',(7.52364573027552,-21.2644161259962,
0.));
#191187=CARTESIAN_POINT('Ctrl Pts',(7.52364573027552,-21.2644161259962,
12.));
#191188=CARTESIAN_POINT('Ctrl Pts',(7.52427261074297,-21.2663059157058,
0.));
#191189=CARTESIAN_POINT('Ctrl Pts',(7.52427261074297,-21.2663059157058,
12.));
#191190=CARTESIAN_POINT('Ctrl Pts',(7.5250177033353,-21.2685823838671,0.));
#191191=CARTESIAN_POINT('Ctrl Pts',(7.5250177033353,-21.2685823838671,12.));
#191192=CARTESIAN_POINT('Ctrl Pts',(7.52587126095529,-21.2712301573466,
0.));
#191193=CARTESIAN_POINT('Ctrl Pts',(7.52587126095529,-21.2712301573466,
12.));
#191194=CARTESIAN_POINT('Ctrl Pts',(7.5268252691854,-21.2742366113579,0.));
#191195=CARTESIAN_POINT('Ctrl Pts',(7.5268252691854,-21.2742366113579,12.));
#191196=CARTESIAN_POINT('Ctrl Pts',(7.52787386225332,-21.2775925269652,
0.));
#191197=CARTESIAN_POINT('Ctrl Pts',(7.52787386225332,-21.2775925269652,
12.));
#191198=CARTESIAN_POINT('Ctrl Pts',(7.52901217930407,-21.2812902781143,
0.));
#191199=CARTESIAN_POINT('Ctrl Pts',(7.52901217930407,-21.2812902781143,
12.));
#191200=CARTESIAN_POINT('Ctrl Pts',(7.53023562438229,-21.2853226580657,
0.));
#191201=CARTESIAN_POINT('Ctrl Pts',(7.53023562438229,-21.2853226580657,
12.));
#191202=CARTESIAN_POINT('Ctrl Pts',(7.53153906987855,-21.2896816163842,
0.));
#191203=CARTESIAN_POINT('Ctrl Pts',(7.53153906987855,-21.2896816163842,
12.));
#191204=CARTESIAN_POINT('Ctrl Pts',(7.53291726078526,-21.2943588989331,
0.));
#191205=CARTESIAN_POINT('Ctrl Pts',(7.53291726078526,-21.2943588989331,
12.));
#191206=CARTESIAN_POINT('Ctrl Pts',(7.53436505309942,-21.2993464250717,
0.));
#191207=CARTESIAN_POINT('Ctrl Pts',(7.53436505309942,-21.2993464250717,
12.));
#191208=CARTESIAN_POINT('Ctrl Pts',(7.53587778251735,-21.3046368712157,
0.));
#191209=CARTESIAN_POINT('Ctrl Pts',(7.53587778251735,-21.3046368712157,
12.));
#191210=CARTESIAN_POINT('Ctrl Pts',(7.53745129364615,-21.310223716773,0.));
#191211=CARTESIAN_POINT('Ctrl Pts',(7.53745129364615,-21.310223716773,12.));
#191212=CARTESIAN_POINT('Ctrl Pts',(7.53908175169898,-21.3161009456256,
0.));
#191213=CARTESIAN_POINT('Ctrl Pts',(7.53908175169898,-21.3161009456256,
12.));
#191214=CARTESIAN_POINT('Ctrl Pts',(7.54076552038278,-21.3222628524165,
0.));
#191215=CARTESIAN_POINT('Ctrl Pts',(7.54076552038278,-21.3222628524165,
12.));
#191216=CARTESIAN_POINT('Ctrl Pts',(7.5424990037703,-21.328703791771,0.));
#191217=CARTESIAN_POINT('Ctrl Pts',(7.5424990037703,-21.328703791771,12.));
#191218=CARTESIAN_POINT('Ctrl Pts',(7.54427868151267,-21.3354182340149,
0.));
#191219=CARTESIAN_POINT('Ctrl Pts',(7.54427868151267,-21.3354182340149,
12.));
#191220=CARTESIAN_POINT('Ctrl Pts',(7.54610114948346,-21.3424008295038,
0.));
#191221=CARTESIAN_POINT('Ctrl Pts',(7.54610114948346,-21.3424008295038,
12.));
#191222=CARTESIAN_POINT('Ctrl Pts',(7.5479631624633,-21.3496464761531,0.));
#191223=CARTESIAN_POINT('Ctrl Pts',(7.5479631624633,-21.3496464761531,12.));
#191224=CARTESIAN_POINT('Ctrl Pts',(7.54986166521309,-21.3571503685855,
0.));
#191225=CARTESIAN_POINT('Ctrl Pts',(7.54986166521309,-21.3571503685855,
12.));
#191226=CARTESIAN_POINT('Ctrl Pts',(7.55179375777443,-21.3649079431865,
0.));
#191227=CARTESIAN_POINT('Ctrl Pts',(7.55179375777443,-21.3649079431865,
12.));
#191228=CARTESIAN_POINT('Ctrl Pts',(7.55375667080028,-21.3729148390243,
0.));
#191229=CARTESIAN_POINT('Ctrl Pts',(7.55375667080028,-21.3729148390243,
12.));
#191230=CARTESIAN_POINT('Ctrl Pts',(7.55574773403502,-21.3811668478932,
0.));
#191231=CARTESIAN_POINT('Ctrl Pts',(7.55574773403502,-21.3811668478932,
12.));
#191232=CARTESIAN_POINT('Ctrl Pts',(7.55776435731416,-21.3896598842117,
0.));
#191233=CARTESIAN_POINT('Ctrl Pts',(7.55776435731416,-21.3896598842117,
12.));
#191234=CARTESIAN_POINT('Ctrl Pts',(7.5598040370061,-21.3983899952987,0.));
#191235=CARTESIAN_POINT('Ctrl Pts',(7.5598040370061,-21.3983899952987,12.));
#191236=CARTESIAN_POINT('Ctrl Pts',(7.56186435703621,-21.4073533630365,
0.));
#191237=CARTESIAN_POINT('Ctrl Pts',(7.56186435703621,-21.4073533630365,
12.));
#191238=CARTESIAN_POINT('Ctrl Pts',(7.56394299313684,-21.4165463106254,
0.));
#191239=CARTESIAN_POINT('Ctrl Pts',(7.56394299313684,-21.4165463106254,
12.));
#191240=CARTESIAN_POINT('Ctrl Pts',(7.56603771218711,-21.4259653015736,
0.));
#191241=CARTESIAN_POINT('Ctrl Pts',(7.56603771218711,-21.4259653015736,
12.));
#191242=CARTESIAN_POINT('Ctrl Pts',(7.56814636360847,-21.4356069261513,
0.));
#191243=CARTESIAN_POINT('Ctrl Pts',(7.56814636360847,-21.4356069261513,
12.));
#191244=CARTESIAN_POINT('Ctrl Pts',(7.57026687261165,-21.4454678907509,
0.));
#191245=CARTESIAN_POINT('Ctrl Pts',(7.57026687261165,-21.4454678907509,
12.));
#191246=CARTESIAN_POINT('Ctrl Pts',(7.57239723223505,-21.4555450053142,
0.));
#191247=CARTESIAN_POINT('Ctrl Pts',(7.57239723223505,-21.4555450053142,
12.));
#191248=CARTESIAN_POINT('Ctrl Pts',(7.57453549743411,-21.4658351740128,
0.));
#191249=CARTESIAN_POINT('Ctrl Pts',(7.57453549743411,-21.4658351740128,
12.));
#191250=CARTESIAN_POINT('Ctrl Pts',(7.57667978402986,-21.4763353936762,
0.));
#191251=CARTESIAN_POINT('Ctrl Pts',(7.57667978402986,-21.4763353936762,
12.));
#191252=CARTESIAN_POINT('Ctrl Pts',(7.57882826679131,-21.4870427508194,
0.));
#191253=CARTESIAN_POINT('Ctrl Pts',(7.57882826679131,-21.4870427508194,
12.));
#191254=CARTESIAN_POINT('Ctrl Pts',(7.58097917790743,-21.4979544192744,
0.));
#191255=CARTESIAN_POINT('Ctrl Pts',(7.58097917790743,-21.4979544192744,
12.));
#191256=CARTESIAN_POINT('Ctrl Pts',(7.58313080519179,-21.5090676573873,
0.));
#191257=CARTESIAN_POINT('Ctrl Pts',(7.58313080519179,-21.5090676573873,
12.));
#191258=CARTESIAN_POINT('Ctrl Pts',(7.58528148919129,-21.5203798035299,
0.));
#191259=CARTESIAN_POINT('Ctrl Pts',(7.58528148919129,-21.5203798035299,
12.));
#191260=CARTESIAN_POINT('Ctrl Pts',(7.58742962034833,-21.5318882716736,
0.));
#191261=CARTESIAN_POINT('Ctrl Pts',(7.58742962034833,-21.5318882716736,
12.));
#191262=CARTESIAN_POINT('Ctrl Pts',(7.58957363620013,-21.543590547011,0.));
#191263=CARTESIAN_POINT('Ctrl Pts',(7.58957363620013,-21.543590547011,12.));
#191264=CARTESIAN_POINT('Ctrl Pts',(7.59171201844776,-21.5554841813462,
0.));
#191265=CARTESIAN_POINT('Ctrl Pts',(7.59171201844776,-21.5554841813462,
12.));
#191266=CARTESIAN_POINT('Ctrl Pts',(7.59384329124918,-21.5675667904726,
0.));
#191267=CARTESIAN_POINT('Ctrl Pts',(7.59384329124918,-21.5675667904726,
12.));
#191268=CARTESIAN_POINT('Ctrl Pts',(7.59596601973583,-21.5798360518978,
0.));
#191269=CARTESIAN_POINT('Ctrl Pts',(7.59596601973583,-21.5798360518978,
12.));
#191270=CARTESIAN_POINT('Ctrl Pts',(7.59807880846194,-21.5922897024466,
0.));
#191271=CARTESIAN_POINT('Ctrl Pts',(7.59807880846194,-21.5922897024466,
12.));
#191272=CARTESIAN_POINT('Ctrl Pts',(7.6001802998824,-21.6049255358843,0.));
#191273=CARTESIAN_POINT('Ctrl Pts',(7.6001802998824,-21.6049255358843,12.));
#191274=CARTESIAN_POINT('Ctrl Pts',(7.60226917285428,-21.617741400599,0.));
#191275=CARTESIAN_POINT('Ctrl Pts',(7.60226917285428,-21.617741400599,12.));
#191276=CARTESIAN_POINT('Ctrl Pts',(7.60434414118295,-21.6307351973822,
0.));
#191277=CARTESIAN_POINT('Ctrl Pts',(7.60434414118295,-21.6307351973822,
12.));
#191278=CARTESIAN_POINT('Ctrl Pts',(7.60640395216356,-21.6439048771743,
0.));
#191279=CARTESIAN_POINT('Ctrl Pts',(7.60640395216356,-21.6439048771743,
12.));
#191280=CARTESIAN_POINT('Ctrl Pts',(7.60844738512873,-21.6572484388081,
0.));
#191281=CARTESIAN_POINT('Ctrl Pts',(7.60844738512873,-21.6572484388081,
12.));
#191282=CARTESIAN_POINT('Ctrl Pts',(7.61047325000955,-21.6707639267576,
0.));
#191283=CARTESIAN_POINT('Ctrl Pts',(7.61047325000955,-21.6707639267576,
12.));
#191284=CARTESIAN_POINT('Ctrl Pts',(7.61248038630268,-21.6844494295815,
0.));
#191285=CARTESIAN_POINT('Ctrl Pts',(7.61248038630268,-21.6844494295815,
12.));
#191286=CARTESIAN_POINT('Ctrl Pts',(7.61446766202786,-21.6983030783322,
0.));
#191287=CARTESIAN_POINT('Ctrl Pts',(7.61446766202786,-21.6983030783322,
12.));
#191288=CARTESIAN_POINT('Ctrl Pts',(7.6164339727042,-21.7123230449834,0.));
#191289=CARTESIAN_POINT('Ctrl Pts',(7.6164339727042,-21.7123230449834,12.));
#191290=CARTESIAN_POINT('Ctrl Pts',(7.61837824030537,-21.7265075407975,
0.));
#191291=CARTESIAN_POINT('Ctrl Pts',(7.61837824030537,-21.7265075407975,
12.));
#191292=CARTESIAN_POINT('Ctrl Pts',(7.62029941230854,-21.7408548148656,
0.));
#191293=CARTESIAN_POINT('Ctrl Pts',(7.62029941230854,-21.7408548148656,
12.));
#191294=CARTESIAN_POINT('Ctrl Pts',(7.62219646084228,-21.7553631528328,
0.));
#191295=CARTESIAN_POINT('Ctrl Pts',(7.62219646084228,-21.7553631528328,
12.));
#191296=CARTESIAN_POINT('Ctrl Pts',(7.62406838181165,-21.7700308755584,
0.));
#191297=CARTESIAN_POINT('Ctrl Pts',(7.62406838181165,-21.7700308755584,
12.));
#191298=CARTESIAN_POINT('Ctrl Pts',(7.62591419404512,-21.7848563378021,
0.));
#191299=CARTESIAN_POINT('Ctrl Pts',(7.62591419404512,-21.7848563378021,
12.));
#191300=CARTESIAN_POINT('Ctrl Pts',(7.62773293842388,-21.799837926858,0.));
#191301=CARTESIAN_POINT('Ctrl Pts',(7.62773293842388,-21.799837926858,12.));
#191302=CARTESIAN_POINT('Ctrl Pts',(7.62952367718126,-21.814974061509,0.));
#191303=CARTESIAN_POINT('Ctrl Pts',(7.62952367718126,-21.814974061509,12.));
#191304=CARTESIAN_POINT('Ctrl Pts',(7.63128549323022,-21.8302631910195,
0.));
#191305=CARTESIAN_POINT('Ctrl Pts',(7.63128549323022,-21.8302631910195,
12.));
#191306=CARTESIAN_POINT('Ctrl Pts',(7.63301748948935,-21.8457037941084,
0.));
#191307=CARTESIAN_POINT('Ctrl Pts',(7.63301748948935,-21.8457037941084,
12.));
#191308=CARTESIAN_POINT('Ctrl Pts',(7.63471878821225,-21.8612943779089,
0.));
#191309=CARTESIAN_POINT('Ctrl Pts',(7.63471878821225,-21.8612943779089,
12.));
#191310=CARTESIAN_POINT('Ctrl Pts',(7.63638853033399,-21.8770334769496,
0.));
#191311=CARTESIAN_POINT('Ctrl Pts',(7.63638853033399,-21.8770334769496,
12.));
#191312=CARTESIAN_POINT('Ctrl Pts',(7.63802587492034,-21.8929196523514,
0.));
#191313=CARTESIAN_POINT('Ctrl Pts',(7.63802587492034,-21.8929196523514,
12.));
#191314=CARTESIAN_POINT('Ctrl Pts',(7.63962999860926,-21.9089514909874,
0.));
#191315=CARTESIAN_POINT('Ctrl Pts',(7.63962999860926,-21.9089514909874,
12.));
#191316=CARTESIAN_POINT('Ctrl Pts',(7.64120009506531,-21.9251276046546,
0.));
#191317=CARTESIAN_POINT('Ctrl Pts',(7.64120009506531,-21.9251276046546,
12.));
#191318=CARTESIAN_POINT('Ctrl Pts',(7.64273537442681,-21.9414466292072,
0.));
#191319=CARTESIAN_POINT('Ctrl Pts',(7.64273537442681,-21.9414466292072,
12.));
#191320=CARTESIAN_POINT('Ctrl Pts',(7.64423506279122,-21.9579072237651,
0.));
#191321=CARTESIAN_POINT('Ctrl Pts',(7.64423506279122,-21.9579072237651,
12.));
#191322=CARTESIAN_POINT('Ctrl Pts',(7.64569840177335,-21.9745080700798,
0.));
#191323=CARTESIAN_POINT('Ctrl Pts',(7.64569840177335,-21.9745080700798,
12.));
#191324=CARTESIAN_POINT('Ctrl Pts',(7.64712464805249,-21.9912478718542,
0.));
#191325=CARTESIAN_POINT('Ctrl Pts',(7.64712464805249,-21.9912478718542,
12.));
#191326=CARTESIAN_POINT('Ctrl Pts',(7.64851307293351,-22.0081253540774,
0.));
#191327=CARTESIAN_POINT('Ctrl Pts',(7.64851307293351,-22.0081253540774,
12.));
#191328=CARTESIAN_POINT('Ctrl Pts',(7.64986296190168,-22.0251392623209,
0.));
#191329=CARTESIAN_POINT('Ctrl Pts',(7.64986296190168,-22.0251392623209,
12.));
#191330=CARTESIAN_POINT('Ctrl Pts',(7.65117361421358,-22.0422883621174,
0.));
#191331=CARTESIAN_POINT('Ctrl Pts',(7.65117361421358,-22.0422883621174,
12.));
#191332=CARTESIAN_POINT('Ctrl Pts',(7.65244434253112,-22.0595714384431,
0.));
#191333=CARTESIAN_POINT('Ctrl Pts',(7.65244434253112,-22.0595714384431,
12.));
#191334=CARTESIAN_POINT('Ctrl Pts',(7.65367447254949,-22.0769872951596,
0.));
#191335=CARTESIAN_POINT('Ctrl Pts',(7.65367447254949,-22.0769872951596,
12.));
#191336=CARTESIAN_POINT('Ctrl Pts',(7.65486334263643,-22.094534754469,0.));
#191337=CARTESIAN_POINT('Ctrl Pts',(7.65486334263643,-22.094534754469,12.));
#191338=CARTESIAN_POINT('Ctrl Pts',(7.65601030346806,-22.1122126563329,
0.));
#191339=CARTESIAN_POINT('Ctrl Pts',(7.65601030346806,-22.1122126563329,
12.));
#191340=CARTESIAN_POINT('Ctrl Pts',(7.65711471769396,-22.1300198579675,
0.));
#191341=CARTESIAN_POINT('Ctrl Pts',(7.65711471769396,-22.1300198579675,
12.));
#191342=CARTESIAN_POINT('Ctrl Pts',(7.65817595963348,-22.1479552334211,
0.));
#191343=CARTESIAN_POINT('Ctrl Pts',(7.65817595963348,-22.1479552334211,
12.));
#191344=CARTESIAN_POINT('Ctrl Pts',(7.6591934149693,-22.1660176731178,0.));
#191345=CARTESIAN_POINT('Ctrl Pts',(7.6591934149693,-22.1660176731178,12.));
#191346=CARTESIAN_POINT('Ctrl Pts',(7.66016648045004,-22.1842060834091,
0.));
#191347=CARTESIAN_POINT('Ctrl Pts',(7.66016648045004,-22.1842060834091,
12.));
#191348=CARTESIAN_POINT('Ctrl Pts',(7.6610945635927,-22.2025193860964,0.));
#191349=CARTESIAN_POINT('Ctrl Pts',(7.6610945635927,-22.2025193860964,12.));
#191350=CARTESIAN_POINT('Ctrl Pts',(7.66197708240399,-22.2209565180085,
0.));
#191351=CARTESIAN_POINT('Ctrl Pts',(7.66197708240399,-22.2209565180085,
12.));
#191352=CARTESIAN_POINT('Ctrl Pts',(7.66281346512508,-22.2395164306547,
0.));
#191353=CARTESIAN_POINT('Ctrl Pts',(7.66281346512508,-22.2395164306547,
12.));
#191354=CARTESIAN_POINT('Ctrl Pts',(7.6636031499764,-22.258198089848,0.));
#191355=CARTESIAN_POINT('Ctrl Pts',(7.6636031499764,-22.258198089848,12.));
#191356=CARTESIAN_POINT('Ctrl Pts',(7.66434558490978,-22.2770004753335,
0.));
#191357=CARTESIAN_POINT('Ctrl Pts',(7.66434558490978,-22.2770004753335,
12.));
#191358=CARTESIAN_POINT('Ctrl Pts',(7.66504022736298,-22.2959225803937,
0.));
#191359=CARTESIAN_POINT('Ctrl Pts',(7.66504022736298,-22.2959225803937,
12.));
#191360=CARTESIAN_POINT('Ctrl Pts',(7.66568654402493,-22.314963411484,0.));
#191361=CARTESIAN_POINT('Ctrl Pts',(7.66568654402493,-22.314963411484,12.));
#191362=CARTESIAN_POINT('Ctrl Pts',(7.66628401061951,-22.3341219879469,
0.));
#191363=CARTESIAN_POINT('Ctrl Pts',(7.66628401061951,-22.3341219879469,
12.));
#191364=CARTESIAN_POINT('Ctrl Pts',(7.66683211169157,-22.3533973417021,
0.));
#191365=CARTESIAN_POINT('Ctrl Pts',(7.66683211169157,-22.3533973417021,
12.));
#191366=CARTESIAN_POINT('Ctrl Pts',(7.66733034039882,-22.372788516936,0.));
#191367=CARTESIAN_POINT('Ctrl Pts',(7.66733034039882,-22.372788516936,12.));
#191368=CARTESIAN_POINT('Ctrl Pts',(7.66777819830789,-22.3922945697773,
0.));
#191369=CARTESIAN_POINT('Ctrl Pts',(7.66777819830789,-22.3922945697773,
12.));
#191370=CARTESIAN_POINT('Ctrl Pts',(7.66817519519639,-22.4119145679758,
0.));
#191371=CARTESIAN_POINT('Ctrl Pts',(7.66817519519639,-22.4119145679758,
12.));
#191372=CARTESIAN_POINT('Ctrl Pts',(7.66852084886703,-22.4316475906603,
0.));
#191373=CARTESIAN_POINT('Ctrl Pts',(7.66852084886703,-22.4316475906603,
12.));
#191374=CARTESIAN_POINT('Ctrl Pts',(7.66881468496634,-22.4514927280855,
0.));
#191375=CARTESIAN_POINT('Ctrl Pts',(7.66881468496634,-22.4514927280855,
12.));
#191376=CARTESIAN_POINT('Ctrl Pts',(7.6690562368083,-22.47144908137,0.));
#191377=CARTESIAN_POINT('Ctrl Pts',(7.6690562368083,-22.47144908137,12.));
#191378=CARTESIAN_POINT('Ctrl Pts',(7.66924504520314,-22.4915157622312,
0.));
#191379=CARTESIAN_POINT('Ctrl Pts',(7.66924504520314,-22.4915157622312,
12.));
#191380=CARTESIAN_POINT('Ctrl Pts',(7.66938065829107,-22.5116918927032,
0.));
#191381=CARTESIAN_POINT('Ctrl Pts',(7.66938065829107,-22.5116918927032,
12.));
#191382=CARTESIAN_POINT('Ctrl Pts',(7.66946263138143,-22.53197660492,0.));
#191383=CARTESIAN_POINT('Ctrl Pts',(7.66946263138143,-22.53197660492,12.));
#191384=CARTESIAN_POINT('Ctrl Pts',(7.66949052679692,-22.5523690409116,
0.));
#191385=CARTESIAN_POINT('Ctrl Pts',(7.66949052679692,-22.5523690409116,
12.));
#191386=CARTESIAN_POINT('Ctrl Pts',(7.66946391372305,-22.5728683523831,
0.));
#191387=CARTESIAN_POINT('Ctrl Pts',(7.66946391372305,-22.5728683523831,
12.));
#191388=CARTESIAN_POINT('Ctrl Pts',(7.66938236806232,-22.5934737004953,
0.));
#191389=CARTESIAN_POINT('Ctrl Pts',(7.66938236806232,-22.5934737004953,
12.));
#191390=CARTESIAN_POINT('Ctrl Pts',(7.66924547229413,-22.6141842556243,
0.));
#191391=CARTESIAN_POINT('Ctrl Pts',(7.66924547229413,-22.6141842556243,
12.));
#191392=CARTESIAN_POINT('Ctrl Pts',(7.66905281533714,-22.6349991971541,
0.));
#191393=CARTESIAN_POINT('Ctrl Pts',(7.66905281533714,-22.6349991971541,
12.));
#191394=CARTESIAN_POINT('Ctrl Pts',(7.66880399241322,-22.6559177133127,
0.));
#191395=CARTESIAN_POINT('Ctrl Pts',(7.66880399241322,-22.6559177133127,
12.));
#191396=CARTESIAN_POINT('Ctrl Pts',(7.66849860491742,-22.6769390009885,
0.));
#191397=CARTESIAN_POINT('Ctrl Pts',(7.66849860491742,-22.6769390009885,
12.));
#191398=CARTESIAN_POINT('Ctrl Pts',(7.66813626029274,-22.6980622655446,
0.));
#191399=CARTESIAN_POINT('Ctrl Pts',(7.66813626029274,-22.6980622655446,
12.));
#191400=CARTESIAN_POINT('Ctrl Pts',(7.66771657191027,-22.7192867206245,
0.));
#191401=CARTESIAN_POINT('Ctrl Pts',(7.66771657191027,-22.7192867206245,
12.));
#191402=CARTESIAN_POINT('Ctrl Pts',(7.66723915895439,-22.7406115879513,
0.));
#191403=CARTESIAN_POINT('Ctrl Pts',(7.66723915895439,-22.7406115879513,
12.));
#191404=CARTESIAN_POINT('Ctrl Pts',(7.66670364630298,-22.7620360971843,
0.));
#191405=CARTESIAN_POINT('Ctrl Pts',(7.66670364630298,-22.7620360971843,
12.));
#191406=CARTESIAN_POINT('Ctrl Pts',(7.66610966441272,-22.7835594857699,
0.));
#191407=CARTESIAN_POINT('Ctrl Pts',(7.66610966441272,-22.7835594857699,
12.));
#191408=CARTESIAN_POINT('Ctrl Pts',(7.66545684920986,-22.8051809987833,
0.));
#191409=CARTESIAN_POINT('Ctrl Pts',(7.66545684920986,-22.8051809987833,
12.));
#191410=CARTESIAN_POINT('Ctrl Pts',(7.66474484198548,-22.8268998887678,
0.));
#191411=CARTESIAN_POINT('Ctrl Pts',(7.66474484198548,-22.8268998887678,
12.));
#191412=CARTESIAN_POINT('Ctrl Pts',(7.66397328929802,-22.848715415557,0.));
#191413=CARTESIAN_POINT('Ctrl Pts',(7.66397328929802,-22.848715415557,12.));
#191414=CARTESIAN_POINT('Ctrl Pts',(7.66314184287336,-22.8706268461283,
0.));
#191415=CARTESIAN_POINT('Ctrl Pts',(7.66314184287336,-22.8706268461283,
12.));
#191416=CARTESIAN_POINT('Ctrl Pts',(7.66225015950155,-22.8926334544883,
0.));
#191417=CARTESIAN_POINT('Ctrl Pts',(7.66225015950155,-22.8926334544883,
12.));
#191418=CARTESIAN_POINT('Ctrl Pts',(7.66129790094107,-22.9147345215421,
0.));
#191419=CARTESIAN_POINT('Ctrl Pts',(7.66129790094107,-22.9147345215421,
12.));
#191420=CARTESIAN_POINT('Ctrl Pts',(7.66028473382777,-22.9369293349593,
0.));
#191421=CARTESIAN_POINT('Ctrl Pts',(7.66028473382777,-22.9369293349593,
12.));
#191422=CARTESIAN_POINT('Ctrl Pts',(7.65921032958901,-22.959217189033,0.));
#191423=CARTESIAN_POINT('Ctrl Pts',(7.65921032958901,-22.959217189033,12.));
#191424=CARTESIAN_POINT('Ctrl Pts',(7.65807436436431,-22.9815973845296,
0.));
#191425=CARTESIAN_POINT('Ctrl Pts',(7.65807436436431,-22.9815973845296,
12.));
#191426=CARTESIAN_POINT('Ctrl Pts',(7.65687651891303,-23.0040692285814,
0.));
#191427=CARTESIAN_POINT('Ctrl Pts',(7.65687651891303,-23.0040692285814,
12.));
#191428=CARTESIAN_POINT('Ctrl Pts',(7.65561647852533,-23.0266320345787,
0.));
#191429=CARTESIAN_POINT('Ctrl Pts',(7.65561647852533,-23.0266320345787,
12.));
#191430=CARTESIAN_POINT('Ctrl Pts',(7.65429393293945,-23.0492851220528,
0.));
#191431=CARTESIAN_POINT('Ctrl Pts',(7.65429393293945,-23.0492851220528,
12.));
#191432=CARTESIAN_POINT('Ctrl Pts',(7.65290857626357,-23.072027816555,0.));
#191433=CARTESIAN_POINT('Ctrl Pts',(7.65290857626357,-23.072027816555,12.));
#191434=CARTESIAN_POINT('Ctrl Pts',(7.65146010690475,-23.094859449525,0.));
#191435=CARTESIAN_POINT('Ctrl Pts',(7.65146010690475,-23.094859449525,12.));
#191436=CARTESIAN_POINT('Ctrl Pts',(7.64994822749859,-23.1177793581679,
0.));
#191437=CARTESIAN_POINT('Ctrl Pts',(7.64994822749859,-23.1177793581679,
12.));
#191438=CARTESIAN_POINT('Ctrl Pts',(7.64837264482942,-23.1407868853819,
0.));
#191439=CARTESIAN_POINT('Ctrl Pts',(7.64837264482942,-23.1407868853819,
12.));
#191440=CARTESIAN_POINT('Ctrl Pts',(7.64673306975804,-23.1638813796694,
0.));
#191441=CARTESIAN_POINT('Ctrl Pts',(7.64673306975804,-23.1638813796694,
12.));
#191442=CARTESIAN_POINT('Ctrl Pts',(7.64502921715482,-23.1870621950452,
0.));
#191443=CARTESIAN_POINT('Ctrl Pts',(7.64502921715482,-23.1870621950452,
12.));
#191444=CARTESIAN_POINT('Ctrl Pts',(7.64326080583679,-23.2103286909398,
0.));
#191445=CARTESIAN_POINT('Ctrl Pts',(7.64326080583679,-23.2103286909398,
12.));
#191446=CARTESIAN_POINT('Ctrl Pts',(7.64142755851504,-23.2336802320912,
0.));
#191447=CARTESIAN_POINT('Ctrl Pts',(7.64142755851504,-23.2336802320912,
12.));
#191448=CARTESIAN_POINT('Ctrl Pts',(7.63952920172834,-23.2571161884488,
0.));
#191449=CARTESIAN_POINT('Ctrl Pts',(7.63952920172834,-23.2571161884488,
12.));
#191450=CARTESIAN_POINT('Ctrl Pts',(7.63756546576373,-23.2806359350855,
0.));
#191451=CARTESIAN_POINT('Ctrl Pts',(7.63756546576373,-23.2806359350855,
12.));
#191452=CARTESIAN_POINT('Ctrl Pts',(7.63553608458782,-23.3042388521022,
0.));
#191453=CARTESIAN_POINT('Ctrl Pts',(7.63553608458782,-23.3042388521022,
12.));
#191454=CARTESIAN_POINT('Ctrl Pts',(7.63344079578161,-23.3279243245241,
0.));
#191455=CARTESIAN_POINT('Ctrl Pts',(7.63344079578161,-23.3279243245241,
12.));
#191456=CARTESIAN_POINT('Ctrl Pts',(7.63127934048136,-23.3516917421972,
0.));
#191457=CARTESIAN_POINT('Ctrl Pts',(7.63127934048136,-23.3516917421972,
12.));
#191458=CARTESIAN_POINT('Ctrl Pts',(7.62905146332592,-23.3755404996636,
0.));
#191459=CARTESIAN_POINT('Ctrl Pts',(7.62905146332592,-23.3755404996636,
12.));
#191460=CARTESIAN_POINT('Ctrl Pts',(7.62675691240328,-23.399469996112,0.));
#191461=CARTESIAN_POINT('Ctrl Pts',(7.62675691240328,-23.399469996112,12.));
#191462=CARTESIAN_POINT('Ctrl Pts',(7.62439543920049,-23.4234796353542,
0.));
#191463=CARTESIAN_POINT('Ctrl Pts',(7.62439543920049,-23.4234796353542,
12.));
#191464=CARTESIAN_POINT('Ctrl Pts',(7.62196679855954,-23.4475688257854,
0.));
#191465=CARTESIAN_POINT('Ctrl Pts',(7.62196679855954,-23.4475688257854,
12.));
#191466=CARTESIAN_POINT('Ctrl Pts',(7.61947074863976,-23.4717369803438,
0.));
#191467=CARTESIAN_POINT('Ctrl Pts',(7.61947074863976,-23.4717369803438,
12.));
#191468=CARTESIAN_POINT('Ctrl Pts',(7.61690705088318,-23.4959835164609,
0.));
#191469=CARTESIAN_POINT('Ctrl Pts',(7.61690705088318,-23.4959835164609,
12.));
#191470=CARTESIAN_POINT('Ctrl Pts',(7.61427546999297,-23.5203078560129,
0.));
#191471=CARTESIAN_POINT('Ctrl Pts',(7.61427546999297,-23.5203078560129,
12.));
#191472=CARTESIAN_POINT('Ctrl Pts',(7.61157577385371,-23.544709425203,0.));
#191473=CARTESIAN_POINT('Ctrl Pts',(7.61157577385371,-23.544709425203,12.));
#191474=CARTESIAN_POINT('Ctrl Pts',(7.60880773344599,-23.5691876544244,
0.));
#191475=CARTESIAN_POINT('Ctrl Pts',(7.60880773344599,-23.5691876544244,
12.));
#191476=CARTESIAN_POINT('Ctrl Pts',(7.60597112277093,-23.5937419781245,
0.));
#191477=CARTESIAN_POINT('Ctrl Pts',(7.60597112277093,-23.5937419781245,
12.));
#191478=CARTESIAN_POINT('Ctrl Pts',(7.60306571877805,-23.6183718346576,
0.));
#191479=CARTESIAN_POINT('Ctrl Pts',(7.60306571877805,-23.6183718346576,
12.));
#191480=CARTESIAN_POINT('Ctrl Pts',(7.60009130130125,-23.6430766661418,
0.));
#191481=CARTESIAN_POINT('Ctrl Pts',(7.60009130130125,-23.6430766661418,
12.));
#191482=CARTESIAN_POINT('Ctrl Pts',(7.59704765299566,-23.6678559182875,
0.));
#191483=CARTESIAN_POINT('Ctrl Pts',(7.59704765299566,-23.6678559182875,
12.));
#191484=CARTESIAN_POINT('Ctrl Pts',(7.59393455934034,-23.6927090405066,
0.));
#191485=CARTESIAN_POINT('Ctrl Pts',(7.59393455934034,-23.6927090405066,
12.));
#191486=CARTESIAN_POINT('Ctrl Pts',(7.5907518086532,-23.7176354860457,0.));
#191487=CARTESIAN_POINT('Ctrl Pts',(7.5907518086532,-23.7176354860457,12.));
#191488=CARTESIAN_POINT('Ctrl Pts',(7.58749919210825,-23.7426347121006,
0.));
#191489=CARTESIAN_POINT('Ctrl Pts',(7.58749919210825,-23.7426347121006,
12.));
#191490=CARTESIAN_POINT('Ctrl Pts',(7.5841765037627,-23.7677061799376,0.));
#191491=CARTESIAN_POINT('Ctrl Pts',(7.5841765037627,-23.7677061799376,12.));
#191492=CARTESIAN_POINT('Ctrl Pts',(7.58078354058212,-23.7928493549908,
0.));
#191493=CARTESIAN_POINT('Ctrl Pts',(7.58078354058212,-23.7928493549908,
12.));
#191494=CARTESIAN_POINT('Ctrl Pts',(7.57732010249065,-23.8180637069976,
0.));
#191495=CARTESIAN_POINT('Ctrl Pts',(7.57732010249065,-23.8180637069976,
12.));
#191496=CARTESIAN_POINT('Ctrl Pts',(7.57378599219813,-23.8433487096132,
0.));
#191497=CARTESIAN_POINT('Ctrl Pts',(7.57378599219813,-23.8433487096132,
12.));
#191498=CARTESIAN_POINT('Ctrl Pts',(7.57018101500708,-23.8687038399595,
0.));
#191499=CARTESIAN_POINT('Ctrl Pts',(7.57018101500708,-23.8687038399595,
12.));
#191500=CARTESIAN_POINT('Ctrl Pts',(7.5665049786379,-23.8941285782002,0.));
#191501=CARTESIAN_POINT('Ctrl Pts',(7.5665049786379,-23.8941285782002,12.));
#191502=CARTESIAN_POINT('Ctrl Pts',(7.56275769304772,-23.9196224070759,
0.));
#191503=CARTESIAN_POINT('Ctrl Pts',(7.56275769304772,-23.9196224070759,
12.));
#191504=CARTESIAN_POINT('Ctrl Pts',(7.55893897027679,-23.9451848115002,
0.));
#191505=CARTESIAN_POINT('Ctrl Pts',(7.55893897027679,-23.9451848115002,
12.));
#191506=CARTESIAN_POINT('Ctrl Pts',(7.55504862424807,-23.9708152779886,
0.));
#191507=CARTESIAN_POINT('Ctrl Pts',(7.55504862424807,-23.9708152779886,
12.));
#191508=CARTESIAN_POINT('Ctrl Pts',(7.55108647097431,-23.9965132953187,
0.));
#191509=CARTESIAN_POINT('Ctrl Pts',(7.55108647097431,-23.9965132953187,
12.));
#191510=CARTESIAN_POINT('Ctrl Pts',(7.54705232885894,-24.0222783554531,
0.));
#191511=CARTESIAN_POINT('Ctrl Pts',(7.54705232885894,-24.0222783554531,
12.));
#191512=CARTESIAN_POINT('Ctrl Pts',(7.54294601896127,-24.0481099543353,
0.));
#191513=CARTESIAN_POINT('Ctrl Pts',(7.54294601896127,-24.0481099543353,
12.));
#191514=CARTESIAN_POINT('Ctrl Pts',(7.53876736531004,-24.0740075927984,
0.));
#191515=CARTESIAN_POINT('Ctrl Pts',(7.53876736531004,-24.0740075927984,
12.));
#191516=CARTESIAN_POINT('Ctrl Pts',(7.53451619514658,-24.0999707772643,
0.));
#191517=CARTESIAN_POINT('Ctrl Pts',(7.53451619514658,-24.0999707772643,
12.));
#191518=CARTESIAN_POINT('Ctrl Pts',(7.53019233935536,-24.1259990209211,
0.));
#191519=CARTESIAN_POINT('Ctrl Pts',(7.53019233935536,-24.1259990209211,
12.));
#191520=CARTESIAN_POINT('Ctrl Pts',(7.52579563201478,-24.152091842537,0.));
#191521=CARTESIAN_POINT('Ctrl Pts',(7.52579563201478,-24.152091842537,12.));
#191522=CARTESIAN_POINT('Ctrl Pts',(7.52132590953862,-24.1782487641602,
0.));
#191523=CARTESIAN_POINT('Ctrl Pts',(7.52132590953862,-24.1782487641602,
12.));
#191524=CARTESIAN_POINT('Ctrl Pts',(7.51678300997997,-24.2044693092356,
0.));
#191525=CARTESIAN_POINT('Ctrl Pts',(7.51678300997997,-24.2044693092356,
12.));
#191526=CARTESIAN_POINT('Ctrl Pts',(7.51216677222198,-24.230753000389,0.));
#191527=CARTESIAN_POINT('Ctrl Pts',(7.51216677222198,-24.230753000389,12.));
#191528=CARTESIAN_POINT('Ctrl Pts',(7.50747703535114,-24.2570993577032,
0.));
#191529=CARTESIAN_POINT('Ctrl Pts',(7.50747703535114,-24.2570993577032,
12.));
#191530=CARTESIAN_POINT('Ctrl Pts',(7.50271363765098,-24.2835078958966,
0.));
#191531=CARTESIAN_POINT('Ctrl Pts',(7.50271363765098,-24.2835078958966,
12.));
#191532=CARTESIAN_POINT('Ctrl Pts',(7.49787641695358,-24.3099781253345,
0.));
#191533=CARTESIAN_POINT('Ctrl Pts',(7.49787641695358,-24.3099781253345,
12.));
#191534=CARTESIAN_POINT('Ctrl Pts',(7.49296521252329,-24.3365095573673,
0.));
#191535=CARTESIAN_POINT('Ctrl Pts',(7.49296521252329,-24.3365095573673,
12.));
#191536=CARTESIAN_POINT('Ctrl Pts',(7.48797986651827,-24.3631017084513,
0.));
#191537=CARTESIAN_POINT('Ctrl Pts',(7.48797986651827,-24.3631017084513,
12.));
#191538=CARTESIAN_POINT('Ctrl Pts',(7.48292022569253,-24.3897541049248,
0.));
#191539=CARTESIAN_POINT('Ctrl Pts',(7.48292022569253,-24.3897541049248,
12.));
#191540=CARTESIAN_POINT('Ctrl Pts',(7.47778614286572,-24.4164662871165,
0.));
#191541=CARTESIAN_POINT('Ctrl Pts',(7.47778614286572,-24.4164662871165,
12.));
#191542=CARTESIAN_POINT('Ctrl Pts',(7.47257747883318,-24.4432378146501,
0.));
#191543=CARTESIAN_POINT('Ctrl Pts',(7.47257747883318,-24.4432378146501,
12.));
#191544=CARTESIAN_POINT('Ctrl Pts',(7.46729410308922,-24.4700682684544,
0.));
#191545=CARTESIAN_POINT('Ctrl Pts',(7.46729410308922,-24.4700682684544,
12.));
#191546=CARTESIAN_POINT('Ctrl Pts',(7.46193588961641,-24.4969572391509,
0.));
#191547=CARTESIAN_POINT('Ctrl Pts',(7.46193588961641,-24.4969572391509,
12.));
#191548=CARTESIAN_POINT('Ctrl Pts',(7.45650271336044,-24.52390431731,0.));
#191549=CARTESIAN_POINT('Ctrl Pts',(7.45650271336044,-24.52390431731,12.));
#191550=CARTESIAN_POINT('Ctrl Pts',(7.45099444651295,-24.550909083158,0.));
#191551=CARTESIAN_POINT('Ctrl Pts',(7.45099444651295,-24.550909083158,12.));
#191552=CARTESIAN_POINT('Ctrl Pts',(7.44541095473162,-24.5779710960865,
0.));
#191553=CARTESIAN_POINT('Ctrl Pts',(7.44541095473162,-24.5779710960865,
12.));
#191554=CARTESIAN_POINT('Ctrl Pts',(7.43975209375374,-24.6050898852349,
0.));
#191555=CARTESIAN_POINT('Ctrl Pts',(7.43975209375374,-24.6050898852349,
12.));
#191556=CARTESIAN_POINT('Ctrl Pts',(7.4340177048922,-24.6322649369472,0.));
#191557=CARTESIAN_POINT('Ctrl Pts',(7.4340177048922,-24.6322649369472,12.));
#191558=CARTESIAN_POINT('Ctrl Pts',(7.4282076215868,-24.659495712869,0.));
#191559=CARTESIAN_POINT('Ctrl Pts',(7.4282076215868,-24.659495712869,12.));
#191560=CARTESIAN_POINT('Ctrl Pts',(7.42232167765762,-24.6867816727118,
0.));
#191561=CARTESIAN_POINT('Ctrl Pts',(7.42232167765762,-24.6867816727118,
12.));
#191562=CARTESIAN_POINT('Ctrl Pts',(7.41635971481242,-24.7141222949988,
0.));
#191563=CARTESIAN_POINT('Ctrl Pts',(7.41635971481242,-24.7141222949988,
12.));
#191564=CARTESIAN_POINT('Ctrl Pts',(7.41032159082172,-24.7415170994754,
0.));
#191565=CARTESIAN_POINT('Ctrl Pts',(7.41032159082172,-24.7415170994754,
12.));
#191566=CARTESIAN_POINT('Ctrl Pts',(7.40420718661754,-24.7689656669005,
0.));
#191567=CARTESIAN_POINT('Ctrl Pts',(7.40420718661754,-24.7689656669005,
12.));
#191568=CARTESIAN_POINT('Ctrl Pts',(7.39801641583612,-24.7964676646518,
0.));
#191569=CARTESIAN_POINT('Ctrl Pts',(7.39801641583612,-24.7964676646518,
12.));
#191570=CARTESIAN_POINT('Ctrl Pts',(7.3917492258684,-24.8240228521042,0.));
#191571=CARTESIAN_POINT('Ctrl Pts',(7.3917492258684,-24.8240228521042,12.));
#191572=CARTESIAN_POINT('Ctrl Pts',(7.38540558904945,-24.8516310625367,
0.));
#191573=CARTESIAN_POINT('Ctrl Pts',(7.38540558904945,-24.8516310625367,
12.));
#191574=CARTESIAN_POINT('Ctrl Pts',(7.37898549641609,-24.8792921911309,
0.));
#191575=CARTESIAN_POINT('Ctrl Pts',(7.37898549641609,-24.8792921911309,
12.));
#191576=CARTESIAN_POINT('Ctrl Pts',(7.37378825962717,-24.9014633826201,
0.));
#191577=CARTESIAN_POINT('Ctrl Pts',(7.37378825962717,-24.9014633826201,
12.));
#191578=CARTESIAN_POINT('Ctrl Pts',(7.36985593120695,-24.9181155530631,
0.));
#191579=CARTESIAN_POINT('Ctrl Pts',(7.36985593120695,-24.9181155530631,
12.));
#191580=CARTESIAN_POINT('Ctrl Pts',(7.36721909029059,-24.9292275670705,
0.));
#191581=CARTESIAN_POINT('Ctrl Pts',(7.36721909029059,-24.9292275670705,
12.));
#191582=CARTESIAN_POINT('Ctrl Pts',(7.36589684767343,-24.9347862158358,
0.));
#191583=CARTESIAN_POINT('Ctrl Pts',(7.36589684767343,-24.9347862158358,
12.));
#191584=CARTESIAN_POINT('',(7.36589684767343,-24.9347862158358,0.));
#191585=CARTESIAN_POINT('Ctrl Pts',(7.52250298901263,-21.2610617890679,
0.));
#191586=CARTESIAN_POINT('Ctrl Pts',(7.52250649703969,-21.2610673466886,
0.));
#191587=CARTESIAN_POINT('Ctrl Pts',(7.52252744144903,-21.2611204474866,
0.));
#191588=CARTESIAN_POINT('Ctrl Pts',(7.5226006423166,-21.261326054066,0.));
#191589=CARTESIAN_POINT('Ctrl Pts',(7.52278182242669,-21.2618521283555,
0.));
#191590=CARTESIAN_POINT('Ctrl Pts',(7.52314642316199,-21.262927782038,0.));
#191591=CARTESIAN_POINT('Ctrl Pts',(7.52364573027552,-21.2644161259962,
0.));
#191592=CARTESIAN_POINT('Ctrl Pts',(7.52427261074297,-21.2663059157058,
0.));
#191593=CARTESIAN_POINT('Ctrl Pts',(7.5250177033353,-21.2685823838671,0.));
#191594=CARTESIAN_POINT('Ctrl Pts',(7.52587126095529,-21.2712301573466,
0.));
#191595=CARTESIAN_POINT('Ctrl Pts',(7.5268252691854,-21.2742366113579,0.));
#191596=CARTESIAN_POINT('Ctrl Pts',(7.52787386225332,-21.2775925269652,
0.));
#191597=CARTESIAN_POINT('Ctrl Pts',(7.52901217930407,-21.2812902781143,
0.));
#191598=CARTESIAN_POINT('Ctrl Pts',(7.53023562438229,-21.2853226580657,
0.));
#191599=CARTESIAN_POINT('Ctrl Pts',(7.53153906987855,-21.2896816163842,
0.));
#191600=CARTESIAN_POINT('Ctrl Pts',(7.53291726078526,-21.2943588989331,
0.));
#191601=CARTESIAN_POINT('Ctrl Pts',(7.53436505309942,-21.2993464250717,
0.));
#191602=CARTESIAN_POINT('Ctrl Pts',(7.53587778251735,-21.3046368712157,
0.));
#191603=CARTESIAN_POINT('Ctrl Pts',(7.53745129364615,-21.310223716773,0.));
#191604=CARTESIAN_POINT('Ctrl Pts',(7.53908175169898,-21.3161009456256,
0.));
#191605=CARTESIAN_POINT('Ctrl Pts',(7.54076552038278,-21.3222628524165,
0.));
#191606=CARTESIAN_POINT('Ctrl Pts',(7.5424990037703,-21.328703791771,0.));
#191607=CARTESIAN_POINT('Ctrl Pts',(7.54427868151267,-21.3354182340149,
0.));
#191608=CARTESIAN_POINT('Ctrl Pts',(7.54610114948346,-21.3424008295038,
0.));
#191609=CARTESIAN_POINT('Ctrl Pts',(7.5479631624633,-21.3496464761531,0.));
#191610=CARTESIAN_POINT('Ctrl Pts',(7.54986166521309,-21.3571503685855,
0.));
#191611=CARTESIAN_POINT('Ctrl Pts',(7.55179375777443,-21.3649079431865,
0.));
#191612=CARTESIAN_POINT('Ctrl Pts',(7.55375667080028,-21.3729148390243,
0.));
#191613=CARTESIAN_POINT('Ctrl Pts',(7.55574773403502,-21.3811668478932,
0.));
#191614=CARTESIAN_POINT('Ctrl Pts',(7.55776435731416,-21.3896598842117,
0.));
#191615=CARTESIAN_POINT('Ctrl Pts',(7.5598040370061,-21.3983899952987,0.));
#191616=CARTESIAN_POINT('Ctrl Pts',(7.56186435703621,-21.4073533630365,
0.));
#191617=CARTESIAN_POINT('Ctrl Pts',(7.56394299313684,-21.4165463106254,
0.));
#191618=CARTESIAN_POINT('Ctrl Pts',(7.56603771218711,-21.4259653015736,
0.));
#191619=CARTESIAN_POINT('Ctrl Pts',(7.56814636360847,-21.4356069261513,
0.));
#191620=CARTESIAN_POINT('Ctrl Pts',(7.57026687261165,-21.4454678907509,
0.));
#191621=CARTESIAN_POINT('Ctrl Pts',(7.57239723223505,-21.4555450053142,
0.));
#191622=CARTESIAN_POINT('Ctrl Pts',(7.57453549743411,-21.4658351740128,
0.));
#191623=CARTESIAN_POINT('Ctrl Pts',(7.57667978402986,-21.4763353936762,
0.));
#191624=CARTESIAN_POINT('Ctrl Pts',(7.57882826679131,-21.4870427508194,
0.));
#191625=CARTESIAN_POINT('Ctrl Pts',(7.58097917790743,-21.4979544192744,
0.));
#191626=CARTESIAN_POINT('Ctrl Pts',(7.58313080519179,-21.5090676573873,
0.));
#191627=CARTESIAN_POINT('Ctrl Pts',(7.58528148919129,-21.5203798035299,
0.));
#191628=CARTESIAN_POINT('Ctrl Pts',(7.58742962034833,-21.5318882716736,
0.));
#191629=CARTESIAN_POINT('Ctrl Pts',(7.58957363620013,-21.543590547011,0.));
#191630=CARTESIAN_POINT('Ctrl Pts',(7.59171201844776,-21.5554841813462,
0.));
#191631=CARTESIAN_POINT('Ctrl Pts',(7.59384329124918,-21.5675667904726,
0.));
#191632=CARTESIAN_POINT('Ctrl Pts',(7.59596601973583,-21.5798360518978,
0.));
#191633=CARTESIAN_POINT('Ctrl Pts',(7.59807880846194,-21.5922897024466,
0.));
#191634=CARTESIAN_POINT('Ctrl Pts',(7.6001802998824,-21.6049255358843,0.));
#191635=CARTESIAN_POINT('Ctrl Pts',(7.60226917285428,-21.617741400599,0.));
#191636=CARTESIAN_POINT('Ctrl Pts',(7.60434414118295,-21.6307351973822,
0.));
#191637=CARTESIAN_POINT('Ctrl Pts',(7.60640395216356,-21.6439048771743,
0.));
#191638=CARTESIAN_POINT('Ctrl Pts',(7.60844738512873,-21.6572484388081,
0.));
#191639=CARTESIAN_POINT('Ctrl Pts',(7.61047325000955,-21.6707639267576,
0.));
#191640=CARTESIAN_POINT('Ctrl Pts',(7.61248038630268,-21.6844494295815,
0.));
#191641=CARTESIAN_POINT('Ctrl Pts',(7.61446766202786,-21.6983030783322,
0.));
#191642=CARTESIAN_POINT('Ctrl Pts',(7.6164339727042,-21.7123230449834,0.));
#191643=CARTESIAN_POINT('Ctrl Pts',(7.61837824030537,-21.7265075407975,
0.));
#191644=CARTESIAN_POINT('Ctrl Pts',(7.62029941230854,-21.7408548148656,
0.));
#191645=CARTESIAN_POINT('Ctrl Pts',(7.62219646084228,-21.7553631528328,
0.));
#191646=CARTESIAN_POINT('Ctrl Pts',(7.62406838181165,-21.7700308755584,
0.));
#191647=CARTESIAN_POINT('Ctrl Pts',(7.62591419404512,-21.7848563378021,
0.));
#191648=CARTESIAN_POINT('Ctrl Pts',(7.62773293842388,-21.799837926858,0.));
#191649=CARTESIAN_POINT('Ctrl Pts',(7.62952367718126,-21.814974061509,0.));
#191650=CARTESIAN_POINT('Ctrl Pts',(7.63128549323022,-21.8302631910195,
0.));
#191651=CARTESIAN_POINT('Ctrl Pts',(7.63301748948935,-21.8457037941084,
0.));
#191652=CARTESIAN_POINT('Ctrl Pts',(7.63471878821225,-21.8612943779089,
0.));
#191653=CARTESIAN_POINT('Ctrl Pts',(7.63638853033399,-21.8770334769496,
0.));
#191654=CARTESIAN_POINT('Ctrl Pts',(7.63802587492034,-21.8929196523514,
0.));
#191655=CARTESIAN_POINT('Ctrl Pts',(7.63962999860926,-21.9089514909874,
0.));
#191656=CARTESIAN_POINT('Ctrl Pts',(7.64120009506531,-21.9251276046546,
0.));
#191657=CARTESIAN_POINT('Ctrl Pts',(7.64273537442681,-21.9414466292072,
0.));
#191658=CARTESIAN_POINT('Ctrl Pts',(7.64423506279122,-21.9579072237651,
0.));
#191659=CARTESIAN_POINT('Ctrl Pts',(7.64569840177335,-21.9745080700798,
0.));
#191660=CARTESIAN_POINT('Ctrl Pts',(7.64712464805249,-21.9912478718542,
0.));
#191661=CARTESIAN_POINT('Ctrl Pts',(7.64851307293351,-22.0081253540774,
0.));
#191662=CARTESIAN_POINT('Ctrl Pts',(7.64986296190168,-22.0251392623209,
0.));
#191663=CARTESIAN_POINT('Ctrl Pts',(7.65117361421358,-22.0422883621174,
0.));
#191664=CARTESIAN_POINT('Ctrl Pts',(7.65244434253112,-22.0595714384431,
0.));
#191665=CARTESIAN_POINT('Ctrl Pts',(7.65367447254949,-22.0769872951596,
0.));
#191666=CARTESIAN_POINT('Ctrl Pts',(7.65486334263643,-22.094534754469,0.));
#191667=CARTESIAN_POINT('Ctrl Pts',(7.65601030346806,-22.1122126563329,
0.));
#191668=CARTESIAN_POINT('Ctrl Pts',(7.65711471769396,-22.1300198579675,
0.));
#191669=CARTESIAN_POINT('Ctrl Pts',(7.65817595963348,-22.1479552334211,
0.));
#191670=CARTESIAN_POINT('Ctrl Pts',(7.6591934149693,-22.1660176731178,0.));
#191671=CARTESIAN_POINT('Ctrl Pts',(7.66016648045004,-22.1842060834091,
0.));
#191672=CARTESIAN_POINT('Ctrl Pts',(7.6610945635927,-22.2025193860964,0.));
#191673=CARTESIAN_POINT('Ctrl Pts',(7.66197708240399,-22.2209565180085,
0.));
#191674=CARTESIAN_POINT('Ctrl Pts',(7.66281346512508,-22.2395164306547,
0.));
#191675=CARTESIAN_POINT('Ctrl Pts',(7.6636031499764,-22.258198089848,0.));
#191676=CARTESIAN_POINT('Ctrl Pts',(7.66434558490978,-22.2770004753335,
0.));
#191677=CARTESIAN_POINT('Ctrl Pts',(7.66504022736298,-22.2959225803937,
0.));
#191678=CARTESIAN_POINT('Ctrl Pts',(7.66568654402493,-22.314963411484,0.));
#191679=CARTESIAN_POINT('Ctrl Pts',(7.66628401061951,-22.3341219879469,
0.));
#191680=CARTESIAN_POINT('Ctrl Pts',(7.66683211169157,-22.3533973417021,
0.));
#191681=CARTESIAN_POINT('Ctrl Pts',(7.66733034039882,-22.372788516936,0.));
#191682=CARTESIAN_POINT('Ctrl Pts',(7.66777819830789,-22.3922945697773,
0.));
#191683=CARTESIAN_POINT('Ctrl Pts',(7.66817519519639,-22.4119145679758,
0.));
#191684=CARTESIAN_POINT('Ctrl Pts',(7.66852084886703,-22.4316475906603,
0.));
#191685=CARTESIAN_POINT('Ctrl Pts',(7.66881468496634,-22.4514927280855,
0.));
#191686=CARTESIAN_POINT('Ctrl Pts',(7.6690562368083,-22.47144908137,0.));
#191687=CARTESIAN_POINT('Ctrl Pts',(7.66924504520314,-22.4915157622312,
0.));
#191688=CARTESIAN_POINT('Ctrl Pts',(7.66938065829107,-22.5116918927032,
0.));
#191689=CARTESIAN_POINT('Ctrl Pts',(7.66946263138143,-22.53197660492,0.));
#191690=CARTESIAN_POINT('Ctrl Pts',(7.66949052679692,-22.5523690409116,
0.));
#191691=CARTESIAN_POINT('Ctrl Pts',(7.66946391372305,-22.5728683523831,
0.));
#191692=CARTESIAN_POINT('Ctrl Pts',(7.66938236806232,-22.5934737004953,
0.));
#191693=CARTESIAN_POINT('Ctrl Pts',(7.66924547229413,-22.6141842556243,
0.));
#191694=CARTESIAN_POINT('Ctrl Pts',(7.66905281533714,-22.6349991971541,
0.));
#191695=CARTESIAN_POINT('Ctrl Pts',(7.66880399241322,-22.6559177133127,
0.));
#191696=CARTESIAN_POINT('Ctrl Pts',(7.66849860491742,-22.6769390009885,
0.));
#191697=CARTESIAN_POINT('Ctrl Pts',(7.66813626029274,-22.6980622655446,
0.));
#191698=CARTESIAN_POINT('Ctrl Pts',(7.66771657191027,-22.7192867206245,
0.));
#191699=CARTESIAN_POINT('Ctrl Pts',(7.66723915895439,-22.7406115879513,
0.));
#191700=CARTESIAN_POINT('Ctrl Pts',(7.66670364630298,-22.7620360971843,
0.));
#191701=CARTESIAN_POINT('Ctrl Pts',(7.66610966441272,-22.7835594857699,
0.));
#191702=CARTESIAN_POINT('Ctrl Pts',(7.66545684920986,-22.8051809987833,
0.));
#191703=CARTESIAN_POINT('Ctrl Pts',(7.66474484198548,-22.8268998887678,
0.));
#191704=CARTESIAN_POINT('Ctrl Pts',(7.66397328929802,-22.848715415557,0.));
#191705=CARTESIAN_POINT('Ctrl Pts',(7.66314184287336,-22.8706268461283,
0.));
#191706=CARTESIAN_POINT('Ctrl Pts',(7.66225015950155,-22.8926334544883,
0.));
#191707=CARTESIAN_POINT('Ctrl Pts',(7.66129790094107,-22.9147345215421,
0.));
#191708=CARTESIAN_POINT('Ctrl Pts',(7.66028473382777,-22.9369293349593,
0.));
#191709=CARTESIAN_POINT('Ctrl Pts',(7.65921032958901,-22.959217189033,0.));
#191710=CARTESIAN_POINT('Ctrl Pts',(7.65807436436431,-22.9815973845296,
0.));
#191711=CARTESIAN_POINT('Ctrl Pts',(7.65687651891303,-23.0040692285814,
0.));
#191712=CARTESIAN_POINT('Ctrl Pts',(7.65561647852533,-23.0266320345787,
0.));
#191713=CARTESIAN_POINT('Ctrl Pts',(7.65429393293945,-23.0492851220528,
0.));
#191714=CARTESIAN_POINT('Ctrl Pts',(7.65290857626357,-23.072027816555,0.));
#191715=CARTESIAN_POINT('Ctrl Pts',(7.65146010690475,-23.094859449525,0.));
#191716=CARTESIAN_POINT('Ctrl Pts',(7.64994822749859,-23.1177793581679,
0.));
#191717=CARTESIAN_POINT('Ctrl Pts',(7.64837264482942,-23.1407868853819,
0.));
#191718=CARTESIAN_POINT('Ctrl Pts',(7.64673306975804,-23.1638813796694,
0.));
#191719=CARTESIAN_POINT('Ctrl Pts',(7.64502921715482,-23.1870621950452,
0.));
#191720=CARTESIAN_POINT('Ctrl Pts',(7.64326080583679,-23.2103286909398,
0.));
#191721=CARTESIAN_POINT('Ctrl Pts',(7.64142755851504,-23.2336802320912,
0.));
#191722=CARTESIAN_POINT('Ctrl Pts',(7.63952920172834,-23.2571161884488,
0.));
#191723=CARTESIAN_POINT('Ctrl Pts',(7.63756546576373,-23.2806359350855,
0.));
#191724=CARTESIAN_POINT('Ctrl Pts',(7.63553608458782,-23.3042388521022,
0.));
#191725=CARTESIAN_POINT('Ctrl Pts',(7.63344079578161,-23.3279243245241,
0.));
#191726=CARTESIAN_POINT('Ctrl Pts',(7.63127934048136,-23.3516917421972,
0.));
#191727=CARTESIAN_POINT('Ctrl Pts',(7.62905146332592,-23.3755404996636,
0.));
#191728=CARTESIAN_POINT('Ctrl Pts',(7.62675691240328,-23.399469996112,0.));
#191729=CARTESIAN_POINT('Ctrl Pts',(7.62439543920049,-23.4234796353542,
0.));
#191730=CARTESIAN_POINT('Ctrl Pts',(7.62196679855954,-23.4475688257854,
0.));
#191731=CARTESIAN_POINT('Ctrl Pts',(7.61947074863976,-23.4717369803438,
0.));
#191732=CARTESIAN_POINT('Ctrl Pts',(7.61690705088318,-23.4959835164609,
0.));
#191733=CARTESIAN_POINT('Ctrl Pts',(7.61427546999297,-23.5203078560129,
0.));
#191734=CARTESIAN_POINT('Ctrl Pts',(7.61157577385371,-23.544709425203,0.));
#191735=CARTESIAN_POINT('Ctrl Pts',(7.60880773344599,-23.5691876544244,
0.));
#191736=CARTESIAN_POINT('Ctrl Pts',(7.60597112277093,-23.5937419781245,
0.));
#191737=CARTESIAN_POINT('Ctrl Pts',(7.60306571877805,-23.6183718346576,
0.));
#191738=CARTESIAN_POINT('Ctrl Pts',(7.60009130130125,-23.6430766661418,
0.));
#191739=CARTESIAN_POINT('Ctrl Pts',(7.59704765299566,-23.6678559182875,
0.));
#191740=CARTESIAN_POINT('Ctrl Pts',(7.59393455934034,-23.6927090405066,
0.));
#191741=CARTESIAN_POINT('Ctrl Pts',(7.5907518086532,-23.7176354860457,0.));
#191742=CARTESIAN_POINT('Ctrl Pts',(7.58749919210825,-23.7426347121006,
0.));
#191743=CARTESIAN_POINT('Ctrl Pts',(7.5841765037627,-23.7677061799376,0.));
#191744=CARTESIAN_POINT('Ctrl Pts',(7.58078354058212,-23.7928493549908,
0.));
#191745=CARTESIAN_POINT('Ctrl Pts',(7.57732010249065,-23.8180637069976,
0.));
#191746=CARTESIAN_POINT('Ctrl Pts',(7.57378599219813,-23.8433487096132,
0.));
#191747=CARTESIAN_POINT('Ctrl Pts',(7.57018101500708,-23.8687038399595,
0.));
#191748=CARTESIAN_POINT('Ctrl Pts',(7.5665049786379,-23.8941285782002,0.));
#191749=CARTESIAN_POINT('Ctrl Pts',(7.56275769304772,-23.9196224070759,
0.));
#191750=CARTESIAN_POINT('Ctrl Pts',(7.55893897027679,-23.9451848115002,
0.));
#191751=CARTESIAN_POINT('Ctrl Pts',(7.55504862424807,-23.9708152779886,
0.));
#191752=CARTESIAN_POINT('Ctrl Pts',(7.55108647097431,-23.9965132953187,
0.));
#191753=CARTESIAN_POINT('Ctrl Pts',(7.54705232885894,-24.0222783554531,
0.));
#191754=CARTESIAN_POINT('Ctrl Pts',(7.54294601896127,-24.0481099543353,
0.));
#191755=CARTESIAN_POINT('Ctrl Pts',(7.53876736531004,-24.0740075927984,
0.));
#191756=CARTESIAN_POINT('Ctrl Pts',(7.53451619514658,-24.0999707772643,
0.));
#191757=CARTESIAN_POINT('Ctrl Pts',(7.53019233935536,-24.1259990209211,
0.));
#191758=CARTESIAN_POINT('Ctrl Pts',(7.52579563201478,-24.152091842537,0.));
#191759=CARTESIAN_POINT('Ctrl Pts',(7.52132590953862,-24.1782487641602,
0.));
#191760=CARTESIAN_POINT('Ctrl Pts',(7.51678300997997,-24.2044693092356,
0.));
#191761=CARTESIAN_POINT('Ctrl Pts',(7.51216677222198,-24.230753000389,0.));
#191762=CARTESIAN_POINT('Ctrl Pts',(7.50747703535114,-24.2570993577032,
0.));
#191763=CARTESIAN_POINT('Ctrl Pts',(7.50271363765098,-24.2835078958966,
0.));
#191764=CARTESIAN_POINT('Ctrl Pts',(7.49787641695358,-24.3099781253345,
0.));
#191765=CARTESIAN_POINT('Ctrl Pts',(7.49296521252329,-24.3365095573673,
0.));
#191766=CARTESIAN_POINT('Ctrl Pts',(7.48797986651827,-24.3631017084513,
0.));
#191767=CARTESIAN_POINT('Ctrl Pts',(7.48292022569253,-24.3897541049248,
0.));
#191768=CARTESIAN_POINT('Ctrl Pts',(7.47778614286572,-24.4164662871165,
0.));
#191769=CARTESIAN_POINT('Ctrl Pts',(7.47257747883318,-24.4432378146501,
0.));
#191770=CARTESIAN_POINT('Ctrl Pts',(7.46729410308922,-24.4700682684544,
0.));
#191771=CARTESIAN_POINT('Ctrl Pts',(7.46193588961641,-24.4969572391509,
0.));
#191772=CARTESIAN_POINT('Ctrl Pts',(7.45650271336044,-24.52390431731,0.));
#191773=CARTESIAN_POINT('Ctrl Pts',(7.45099444651295,-24.550909083158,0.));
#191774=CARTESIAN_POINT('Ctrl Pts',(7.44541095473162,-24.5779710960865,
0.));
#191775=CARTESIAN_POINT('Ctrl Pts',(7.43975209375374,-24.6050898852349,
0.));
#191776=CARTESIAN_POINT('Ctrl Pts',(7.4340177048922,-24.6322649369472,0.));
#191777=CARTESIAN_POINT('Ctrl Pts',(7.4282076215868,-24.659495712869,0.));
#191778=CARTESIAN_POINT('Ctrl Pts',(7.42232167765762,-24.6867816727118,
0.));
#191779=CARTESIAN_POINT('Ctrl Pts',(7.41635971481242,-24.7141222949988,
0.));
#191780=CARTESIAN_POINT('Ctrl Pts',(7.41032159082172,-24.7415170994754,
0.));
#191781=CARTESIAN_POINT('Ctrl Pts',(7.40420718661754,-24.7689656669005,
0.));
#191782=CARTESIAN_POINT('Ctrl Pts',(7.39801641583612,-24.7964676646518,
0.));
#191783=CARTESIAN_POINT('Ctrl Pts',(7.3917492258684,-24.8240228521042,0.));
#191784=CARTESIAN_POINT('Ctrl Pts',(7.38540558904945,-24.8516310625367,
0.));
#191785=CARTESIAN_POINT('Ctrl Pts',(7.37898549641609,-24.8792921911309,
0.));
#191786=CARTESIAN_POINT('Ctrl Pts',(7.37378825962717,-24.9014633826201,
0.));
#191787=CARTESIAN_POINT('Ctrl Pts',(7.36985593120695,-24.9181155530631,
0.));
#191788=CARTESIAN_POINT('Ctrl Pts',(7.36721909029059,-24.9292275670705,
0.));
#191789=CARTESIAN_POINT('Ctrl Pts',(7.36589684767343,-24.9347862158358,
0.));
#191790=CARTESIAN_POINT('',(7.36589684767343,-24.9347862158358,0.));
#191791=CARTESIAN_POINT('Origin',(1.68110656504246,-21.4341755315424,0.));
#191792=CARTESIAN_POINT('',(1.76341220531179,-22.4835757167854,0.));
#191793=CARTESIAN_POINT('',(1.76341220531179,-22.4835757167854,0.));
#191794=CARTESIAN_POINT('',(0.840553282521226,-10.7170877657712,0.));
#191795=CARTESIAN_POINT('Ctrl Pts',(6.08833931617698,-25.2771067246846,
0.));
#191796=CARTESIAN_POINT('Ctrl Pts',(6.08833931617698,-25.2771067246846,
12.));
#191797=CARTESIAN_POINT('Ctrl Pts',(6.08441489609824,-25.2729539149479,
0.));
#191798=CARTESIAN_POINT('Ctrl Pts',(6.08441489609824,-25.2729539149479,
12.));
#191799=CARTESIAN_POINT('Ctrl Pts',(6.07657531787577,-25.2646490489816,
0.));
#191800=CARTESIAN_POINT('Ctrl Pts',(6.07657531787577,-25.2646490489816,
12.));
#191801=CARTESIAN_POINT('Ctrl Pts',(6.06484373634696,-25.2521940105523,
0.));
#191802=CARTESIAN_POINT('Ctrl Pts',(6.06484373634696,-25.2521940105523,
12.));
#191803=CARTESIAN_POINT('Ctrl Pts',(6.04925720151412,-25.2355918138798,
0.));
#191804=CARTESIAN_POINT('Ctrl Pts',(6.04925720151412,-25.2355918138798,
12.));
#191805=CARTESIAN_POINT('Ctrl Pts',(6.02986667390187,-25.2148466201368,
0.));
#191806=CARTESIAN_POINT('Ctrl Pts',(6.02986667390187,-25.2148466201368,
12.));
#191807=CARTESIAN_POINT('Ctrl Pts',(6.0105688180476,-25.1941090269638,0.));
#191808=CARTESIAN_POINT('Ctrl Pts',(6.0105688180476,-25.1941090269638,12.));
#191809=CARTESIAN_POINT('Ctrl Pts',(5.99136367859838,-25.1733791296154,
0.));
#191810=CARTESIAN_POINT('Ctrl Pts',(5.99136367859838,-25.1733791296154,
12.));
#191811=CARTESIAN_POINT('Ctrl Pts',(5.97225131495636,-25.1526570863065,
0.));
#191812=CARTESIAN_POINT('Ctrl Pts',(5.97225131495636,-25.1526570863065,
12.));
#191813=CARTESIAN_POINT('Ctrl Pts',(5.95323180187347,-25.1319431317273,
0.));
#191814=CARTESIAN_POINT('Ctrl Pts',(5.95323180187347,-25.1319431317273,
12.));
#191815=CARTESIAN_POINT('Ctrl Pts',(5.93430523086776,-25.1112375971182,
0.));
#191816=CARTESIAN_POINT('Ctrl Pts',(5.93430523086776,-25.1112375971182,
12.));
#191817=CARTESIAN_POINT('Ctrl Pts',(5.91547170844382,-25.0905409050863,
0.));
#191818=CARTESIAN_POINT('Ctrl Pts',(5.91547170844382,-25.0905409050863,
12.));
#191819=CARTESIAN_POINT('Ctrl Pts',(5.89673135155458,-25.0698535426593,
0.));
#191820=CARTESIAN_POINT('Ctrl Pts',(5.89673135155458,-25.0698535426593,
12.));
#191821=CARTESIAN_POINT('Ctrl Pts',(5.87808428385329,-25.0491760405965,
0.));
#191822=CARTESIAN_POINT('Ctrl Pts',(5.87808428385329,-25.0491760405965,
12.));
#191823=CARTESIAN_POINT('Ctrl Pts',(5.8595306315681,-25.0285089498922,0.));
#191824=CARTESIAN_POINT('Ctrl Pts',(5.8595306315681,-25.0285089498922,12.));
#191825=CARTESIAN_POINT('Ctrl Pts',(5.84107051963073,-25.0078528200558,
0.));
#191826=CARTESIAN_POINT('Ctrl Pts',(5.84107051963073,-25.0078528200558,
12.));
#191827=CARTESIAN_POINT('Ctrl Pts',(5.82270406744213,-24.9872081752709,
0.));
#191828=CARTESIAN_POINT('Ctrl Pts',(5.82270406744213,-24.9872081752709,
12.));
#191829=CARTESIAN_POINT('Ctrl Pts',(5.80443138549747,-24.9665754954463,
0.));
#191830=CARTESIAN_POINT('Ctrl Pts',(5.80443138549747,-24.9665754954463,
12.));
#191831=CARTESIAN_POINT('Ctrl Pts',(5.78625257775702,-24.9459552293308,
0.));
#191832=CARTESIAN_POINT('Ctrl Pts',(5.78625257775702,-24.9459552293308,
12.));
#191833=CARTESIAN_POINT('Ctrl Pts',(5.76816774342236,-24.9253478043632,
0.));
#191834=CARTESIAN_POINT('Ctrl Pts',(5.76816774342236,-24.9253478043632,
12.));
#191835=CARTESIAN_POINT('Ctrl Pts',(5.75017697890812,-24.9047536376467,
0.));
#191836=CARTESIAN_POINT('Ctrl Pts',(5.75017697890812,-24.9047536376467,
12.));
#191837=CARTESIAN_POINT('Ctrl Pts',(5.73228037976926,-24.8841731467219,
0.));
#191838=CARTESIAN_POINT('Ctrl Pts',(5.73228037976926,-24.8841731467219,
12.));
#191839=CARTESIAN_POINT('Ctrl Pts',(5.71447804252019,-24.8636067597677,
0.));
#191840=CARTESIAN_POINT('Ctrl Pts',(5.71447804252019,-24.8636067597677,
12.));
#191841=CARTESIAN_POINT('Ctrl Pts',(5.69677006679429,-24.8430549277634,
0.));
#191842=CARTESIAN_POINT('Ctrl Pts',(5.69677006679429,-24.8430549277634,
12.));
#191843=CARTESIAN_POINT('Ctrl Pts',(5.67915655496524,-24.822518122386,0.));
#191844=CARTESIAN_POINT('Ctrl Pts',(5.67915655496524,-24.822518122386,12.));
#191845=CARTESIAN_POINT('Ctrl Pts',(5.66163761114903,-24.8019968304618,
0.));
#191846=CARTESIAN_POINT('Ctrl Pts',(5.66163761114903,-24.8019968304618,
12.));
#191847=CARTESIAN_POINT('Ctrl Pts',(5.64421334042247,-24.7814915496728,
0.));
#191848=CARTESIAN_POINT('Ctrl Pts',(5.64421334042247,-24.7814915496728,
12.));
#191849=CARTESIAN_POINT('Ctrl Pts',(5.62688384790918,-24.76100278357,0.));
#191850=CARTESIAN_POINT('Ctrl Pts',(5.62688384790918,-24.76100278357,12.));
#191851=CARTESIAN_POINT('Ctrl Pts',(5.60964923798494,-24.7405310372736,
0.));
#191852=CARTESIAN_POINT('Ctrl Pts',(5.60964923798494,-24.7405310372736,
12.));
#191853=CARTESIAN_POINT('Ctrl Pts',(5.59250961323995,-24.7200768119079,
0.));
#191854=CARTESIAN_POINT('Ctrl Pts',(5.59250961323995,-24.7200768119079,
12.));
#191855=CARTESIAN_POINT('Ctrl Pts',(5.57546507427766,-24.6996406035507,
0.));
#191856=CARTESIAN_POINT('Ctrl Pts',(5.57546507427766,-24.6996406035507,
12.));
#191857=CARTESIAN_POINT('Ctrl Pts',(5.55851572025389,-24.6792229061785,
0.));
#191858=CARTESIAN_POINT('Ctrl Pts',(5.55851572025389,-24.6792229061785,
12.));
#191859=CARTESIAN_POINT('Ctrl Pts',(5.54166164919592,-24.6588242134733,
0.));
#191860=CARTESIAN_POINT('Ctrl Pts',(5.54166164919592,-24.6588242134733,
12.));
#191861=CARTESIAN_POINT('Ctrl Pts',(5.52490295840996,-24.6384450211466,
0.));
#191862=CARTESIAN_POINT('Ctrl Pts',(5.52490295840996,-24.6384450211466,
12.));
#191863=CARTESIAN_POINT('Ctrl Pts',(5.50823974481959,-24.618085828918,0.));
#191864=CARTESIAN_POINT('Ctrl Pts',(5.50823974481959,-24.618085828918,12.));
#191865=CARTESIAN_POINT('Ctrl Pts',(5.49167210537235,-24.5977471429365,
0.));
#191866=CARTESIAN_POINT('Ctrl Pts',(5.49167210537235,-24.5977471429365,
12.));
#191867=CARTESIAN_POINT('Ctrl Pts',(5.47520013724403,-24.5774294770329,
0.));
#191868=CARTESIAN_POINT('Ctrl Pts',(5.47520013724403,-24.5774294770329,
12.));
#191869=CARTESIAN_POINT('Ctrl Pts',(5.45882393762244,-24.5571333514841,
0.));
#191870=CARTESIAN_POINT('Ctrl Pts',(5.45882393762244,-24.5571333514841,
12.));
#191871=CARTESIAN_POINT('Ctrl Pts',(5.44254360356865,-24.5368592922861,
0.));
#191872=CARTESIAN_POINT('Ctrl Pts',(5.44254360356865,-24.5368592922861,
12.));
#191873=CARTESIAN_POINT('Ctrl Pts',(5.42635923183411,-24.5166078302107,
0.));
#191874=CARTESIAN_POINT('Ctrl Pts',(5.42635923183411,-24.5166078302107,
12.));
#191875=CARTESIAN_POINT('Ctrl Pts',(5.41027091869242,-24.4963794999831,
0.));
#191876=CARTESIAN_POINT('Ctrl Pts',(5.41027091869242,-24.4963794999831,
12.));
#191877=CARTESIAN_POINT('Ctrl Pts',(5.3942787597383,-24.4761748393322,0.));
#191878=CARTESIAN_POINT('Ctrl Pts',(5.3942787597383,-24.4761748393322,12.));
#191879=CARTESIAN_POINT('Ctrl Pts',(5.37838284973706,-24.4559943883159,
0.));
#191880=CARTESIAN_POINT('Ctrl Pts',(5.37838284973706,-24.4559943883159,
12.));
#191881=CARTESIAN_POINT('Ctrl Pts',(5.36258328273639,-24.4358386899152,
0.));
#191882=CARTESIAN_POINT('Ctrl Pts',(5.36258328273639,-24.4358386899152,
12.));
#191883=CARTESIAN_POINT('Ctrl Pts',(5.34688015213546,-24.4157082904615,
0.));
#191884=CARTESIAN_POINT('Ctrl Pts',(5.34688015213546,-24.4157082904615,
12.));
#191885=CARTESIAN_POINT('Ctrl Pts',(5.33127355076036,-24.3956037401293,
0.));
#191886=CARTESIAN_POINT('Ctrl Pts',(5.33127355076036,-24.3956037401293,
12.));
#191887=CARTESIAN_POINT('Ctrl Pts',(5.31576357092524,-24.3755255933917,
0.));
#191888=CARTESIAN_POINT('Ctrl Pts',(5.31576357092524,-24.3755255933917,
12.));
#191889=CARTESIAN_POINT('Ctrl Pts',(5.30035030449058,-24.3554744095075,
0.));
#191890=CARTESIAN_POINT('Ctrl Pts',(5.30035030449058,-24.3554744095075,
12.));
#191891=CARTESIAN_POINT('Ctrl Pts',(5.28503384290644,-24.3354507529415,
0.));
#191892=CARTESIAN_POINT('Ctrl Pts',(5.28503384290644,-24.3354507529415,
12.));
#191893=CARTESIAN_POINT('Ctrl Pts',(5.26981427718796,-24.3154551932222,
0.));
#191894=CARTESIAN_POINT('Ctrl Pts',(5.26981427718796,-24.3154551932222,
12.));
#191895=CARTESIAN_POINT('Ctrl Pts',(5.25469169788855,-24.2954883048448,
0.));
#191896=CARTESIAN_POINT('Ctrl Pts',(5.25469169788855,-24.2954883048448,
12.));
#191897=CARTESIAN_POINT('Ctrl Pts',(5.23966619506289,-24.2755506671526,
0.));
#191898=CARTESIAN_POINT('Ctrl Pts',(5.23966619506289,-24.2755506671526,
12.));
#191899=CARTESIAN_POINT('Ctrl Pts',(5.22473785822441,-24.2556428642294,
0.));
#191900=CARTESIAN_POINT('Ctrl Pts',(5.22473785822441,-24.2556428642294,
12.));
#191901=CARTESIAN_POINT('Ctrl Pts',(5.20990677629173,-24.2357654847765,
0.));
#191902=CARTESIAN_POINT('Ctrl Pts',(5.20990677629173,-24.2357654847765,
12.));
#191903=CARTESIAN_POINT('Ctrl Pts',(5.19517303753642,-24.215919122017,0.));
#191904=CARTESIAN_POINT('Ctrl Pts',(5.19517303753642,-24.215919122017,12.));
#191905=CARTESIAN_POINT('Ctrl Pts',(5.18053672961392,-24.1961043738754,
0.));
#191906=CARTESIAN_POINT('Ctrl Pts',(5.18053672961392,-24.1961043738754,
12.));
#191907=CARTESIAN_POINT('Ctrl Pts',(5.16599793957979,-24.1763218431343,
0.));
#191908=CARTESIAN_POINT('Ctrl Pts',(5.16599793957979,-24.1763218431343,
12.));
#191909=CARTESIAN_POINT('Ctrl Pts',(5.15155675390075,-24.1565721375971,
0.));
#191910=CARTESIAN_POINT('Ctrl Pts',(5.15155675390075,-24.1565721375971,
12.));
#191911=CARTESIAN_POINT('Ctrl Pts',(5.13721325845744,-24.1368558702443,
0.));
#191912=CARTESIAN_POINT('Ctrl Pts',(5.13721325845744,-24.1368558702443,
12.));
#191913=CARTESIAN_POINT('Ctrl Pts',(5.12296753853859,-24.117173659394,0.));
#191914=CARTESIAN_POINT('Ctrl Pts',(5.12296753853859,-24.117173659394,12.));
#191915=CARTESIAN_POINT('Ctrl Pts',(5.10881967883132,-24.0975261288446,
0.));
#191916=CARTESIAN_POINT('Ctrl Pts',(5.10881967883132,-24.0975261288446,
12.));
#191917=CARTESIAN_POINT('Ctrl Pts',(5.09476976342625,-24.0779139079266,
0.));
#191918=CARTESIAN_POINT('Ctrl Pts',(5.09476976342625,-24.0779139079266,
12.));
#191919=CARTESIAN_POINT('Ctrl Pts',(5.08081787581276,-24.0583376315638,
0.));
#191920=CARTESIAN_POINT('Ctrl Pts',(5.08081787581276,-24.0583376315638,
12.));
#191921=CARTESIAN_POINT('Ctrl Pts',(5.06696409886641,-24.0387979403268,
0.));
#191922=CARTESIAN_POINT('Ctrl Pts',(5.06696409886641,-24.0387979403268,
12.));
#191923=CARTESIAN_POINT('Ctrl Pts',(5.05320851483065,-24.0192954804896,
0.));
#191924=CARTESIAN_POINT('Ctrl Pts',(5.05320851483065,-24.0192954804896,
12.));
#191925=CARTESIAN_POINT('Ctrl Pts',(5.03955120528521,-23.9998309040746,
0.));
#191926=CARTESIAN_POINT('Ctrl Pts',(5.03955120528521,-23.9998309040746,
12.));
#191927=CARTESIAN_POINT('Ctrl Pts',(5.02599225112454,-23.9804048689227,
0.));
#191928=CARTESIAN_POINT('Ctrl Pts',(5.02599225112454,-23.9804048689227,
12.));
#191929=CARTESIAN_POINT('Ctrl Pts',(5.01253173257452,-23.9610180388271,
0.));
#191930=CARTESIAN_POINT('Ctrl Pts',(5.01253173257452,-23.9610180388271,
12.));
#191931=CARTESIAN_POINT('Ctrl Pts',(4.99916972919306,-23.9416710836529,
0.));
#191932=CARTESIAN_POINT('Ctrl Pts',(4.99916972919306,-23.9416710836529,
12.));
#191933=CARTESIAN_POINT('Ctrl Pts',(4.98590631986532,-23.9223646794592,
0.));
#191934=CARTESIAN_POINT('Ctrl Pts',(4.98590631986532,-23.9223646794592,
12.));
#191935=CARTESIAN_POINT('Ctrl Pts',(4.97274158279226,-23.9030995086163,
0.));
#191936=CARTESIAN_POINT('Ctrl Pts',(4.97274158279226,-23.9030995086163,
12.));
#191937=CARTESIAN_POINT('Ctrl Pts',(4.9596755954656,-23.8838762599218,0.));
#191938=CARTESIAN_POINT('Ctrl Pts',(4.9596755954656,-23.8838762599218,12.));
#191939=CARTESIAN_POINT('Ctrl Pts',(4.9467084346586,-23.8646956287168,0.));
#191940=CARTESIAN_POINT('Ctrl Pts',(4.9467084346586,-23.8646956287168,12.));
#191941=CARTESIAN_POINT('Ctrl Pts',(4.93384017643432,-23.8455583170057,
0.));
#191942=CARTESIAN_POINT('Ctrl Pts',(4.93384017643432,-23.8455583170057,
12.));
#191943=CARTESIAN_POINT('Ctrl Pts',(4.92107089613968,-23.8264650335717,
0.));
#191944=CARTESIAN_POINT('Ctrl Pts',(4.92107089613968,-23.8264650335717,
12.));
#191945=CARTESIAN_POINT('Ctrl Pts',(4.90840066839344,-23.8074164940896,
0.));
#191946=CARTESIAN_POINT('Ctrl Pts',(4.90840066839344,-23.8074164940896,
12.));
#191947=CARTESIAN_POINT('Ctrl Pts',(4.89582956706775,-23.7884134212384,
0.));
#191948=CARTESIAN_POINT('Ctrl Pts',(4.89582956706775,-23.7884134212384,
12.));
#191949=CARTESIAN_POINT('Ctrl Pts',(4.88335766525573,-23.7694565448049,
0.));
#191950=CARTESIAN_POINT('Ctrl Pts',(4.88335766525573,-23.7694565448049,
12.));
#191951=CARTESIAN_POINT('Ctrl Pts',(4.87098503527152,-23.7505466018245,
0.));
#191952=CARTESIAN_POINT('Ctrl Pts',(4.87098503527152,-23.7505466018245,
12.));
#191953=CARTESIAN_POINT('Ctrl Pts',(4.85871174865499,-23.7316843367313,
0.));
#191954=CARTESIAN_POINT('Ctrl Pts',(4.85871174865499,-23.7316843367313,
12.));
#191955=CARTESIAN_POINT('Ctrl Pts',(4.84653787616425,-23.7128705015017,
0.));
#191956=CARTESIAN_POINT('Ctrl Pts',(4.84653787616425,-23.7128705015017,
12.));
#191957=CARTESIAN_POINT('Ctrl Pts',(4.83446348776265,-23.6941058557971,
0.));
#191958=CARTESIAN_POINT('Ctrl Pts',(4.83446348776265,-23.6941058557971,
12.));
#191959=CARTESIAN_POINT('Ctrl Pts',(4.82248865259562,-23.675391167102,0.));
#191960=CARTESIAN_POINT('Ctrl Pts',(4.82248865259562,-23.675391167102,12.));
#191961=CARTESIAN_POINT('Ctrl Pts',(4.81061343896432,-23.6567272108628,
0.));
#191962=CARTESIAN_POINT('Ctrl Pts',(4.81061343896432,-23.6567272108628,
12.));
#191963=CARTESIAN_POINT('Ctrl Pts',(4.7988379143322,-23.6381147706579,0.));
#191964=CARTESIAN_POINT('Ctrl Pts',(4.7988379143322,-23.6381147706579,12.));
#191965=CARTESIAN_POINT('Ctrl Pts',(4.78716214532097,-23.6195546383624,
0.));
#191966=CARTESIAN_POINT('Ctrl Pts',(4.78716214532097,-23.6195546383624,
12.));
#191967=CARTESIAN_POINT('Ctrl Pts',(4.77558619769872,-23.6010476143099,
0.));
#191968=CARTESIAN_POINT('Ctrl Pts',(4.77558619769872,-23.6010476143099,
12.));
#191969=CARTESIAN_POINT('Ctrl Pts',(4.76411013636251,-23.5825945074535,
0.));
#191970=CARTESIAN_POINT('Ctrl Pts',(4.76411013636251,-23.5825945074535,
12.));
#191971=CARTESIAN_POINT('Ctrl Pts',(4.75273402530617,-23.5641961355168,
0.));
#191972=CARTESIAN_POINT('Ctrl Pts',(4.75273402530617,-23.5641961355168,
12.));
#191973=CARTESIAN_POINT('Ctrl Pts',(4.74145792760698,-23.545853325171,0.));
#191974=CARTESIAN_POINT('Ctrl Pts',(4.74145792760698,-23.545853325171,12.));
#191975=CARTESIAN_POINT('Ctrl Pts',(4.73028190543029,-23.5275669122372,
0.));
#191976=CARTESIAN_POINT('Ctrl Pts',(4.73028190543029,-23.5275669122372,
12.));
#191977=CARTESIAN_POINT('Ctrl Pts',(4.71920602001901,-23.509337741878,0.));
#191978=CARTESIAN_POINT('Ctrl Pts',(4.71920602001901,-23.509337741878,12.));
#191979=CARTESIAN_POINT('Ctrl Pts',(4.70823033167818,-23.491166668789,0.));
#191980=CARTESIAN_POINT('Ctrl Pts',(4.70823033167818,-23.491166668789,12.));
#191981=CARTESIAN_POINT('Ctrl Pts',(4.69735489975024,-23.4730545573853,
0.));
#191982=CARTESIAN_POINT('Ctrl Pts',(4.69735489975024,-23.4730545573853,
12.));
#191983=CARTESIAN_POINT('Ctrl Pts',(4.68657978258303,-23.455002281986,0.));
#191984=CARTESIAN_POINT('Ctrl Pts',(4.68657978258303,-23.455002281986,12.));
#191985=CARTESIAN_POINT('Ctrl Pts',(4.67590503753058,-23.4370107270451,
0.));
#191986=CARTESIAN_POINT('Ctrl Pts',(4.67590503753058,-23.4370107270451,
12.));
#191987=CARTESIAN_POINT('Ctrl Pts',(4.6653307209467,-23.4190807873803,0.));
#191988=CARTESIAN_POINT('Ctrl Pts',(4.6653307209467,-23.4190807873803,12.));
#191989=CARTESIAN_POINT('Ctrl Pts',(4.65485688816924,-23.4012133683959,
0.));
#191990=CARTESIAN_POINT('Ctrl Pts',(4.65485688816924,-23.4012133683959,
12.));
#191991=CARTESIAN_POINT('Ctrl Pts',(4.6444835934993,-23.3834093863068,0.));
#191992=CARTESIAN_POINT('Ctrl Pts',(4.6444835934993,-23.3834093863068,12.));
#191993=CARTESIAN_POINT('Ctrl Pts',(4.63421089016541,-23.3656697683489,
0.));
#191994=CARTESIAN_POINT('Ctrl Pts',(4.63421089016541,-23.3656697683489,
12.));
#191995=CARTESIAN_POINT('Ctrl Pts',(4.62403883030805,-23.3479954530272,
0.));
#191996=CARTESIAN_POINT('Ctrl Pts',(4.62403883030805,-23.3479954530272,
12.));
#191997=CARTESIAN_POINT('Ctrl Pts',(4.6139674649783,-23.3303873903938,0.));
#191998=CARTESIAN_POINT('Ctrl Pts',(4.6139674649783,-23.3303873903938,12.));
#191999=CARTESIAN_POINT('Ctrl Pts',(4.60399684412163,-23.3128465423115,
0.));
#192000=CARTESIAN_POINT('Ctrl Pts',(4.60399684412163,-23.3128465423115,
12.));
#192001=CARTESIAN_POINT('Ctrl Pts',(4.5941270165575,-23.2953738827191,0.));
#192002=CARTESIAN_POINT('Ctrl Pts',(4.5941270165575,-23.2953738827191,12.));
#192003=CARTESIAN_POINT('Ctrl Pts',(4.5843580299469,-23.2779703978876,0.));
#192004=CARTESIAN_POINT('Ctrl Pts',(4.5843580299469,-23.2779703978876,12.));
#192005=CARTESIAN_POINT('Ctrl Pts',(4.57468993076097,-23.2606370866866,
0.));
#192006=CARTESIAN_POINT('Ctrl Pts',(4.57468993076097,-23.2606370866866,
12.));
#192007=CARTESIAN_POINT('Ctrl Pts',(4.56512276427839,-23.2433749609131,
0.));
#192008=CARTESIAN_POINT('Ctrl Pts',(4.56512276427839,-23.2433749609131,
12.));
#192009=CARTESIAN_POINT('Ctrl Pts',(4.55565657456975,-23.2261850456064,
0.));
#192010=CARTESIAN_POINT('Ctrl Pts',(4.55565657456975,-23.2261850456064,
12.));
#192011=CARTESIAN_POINT('Ctrl Pts',(4.54629140447544,-23.2090683793629,
0.));
#192012=CARTESIAN_POINT('Ctrl Pts',(4.54629140447544,-23.2090683793629,
12.));
#192013=CARTESIAN_POINT('Ctrl Pts',(4.53702729557566,-23.1920260146465,
0.));
#192014=CARTESIAN_POINT('Ctrl Pts',(4.53702729557566,-23.1920260146465,
12.));
#192015=CARTESIAN_POINT('Ctrl Pts',(4.52786428815014,-23.1750590180908,
0.));
#192016=CARTESIAN_POINT('Ctrl Pts',(4.52786428815014,-23.1750590180908,
12.));
#192017=CARTESIAN_POINT('Ctrl Pts',(4.51880242116748,-23.1581684708761,
0.));
#192018=CARTESIAN_POINT('Ctrl Pts',(4.51880242116748,-23.1581684708761,
12.));
#192019=CARTESIAN_POINT('Ctrl Pts',(4.5098417322706,-23.1413554691123,0.));
#192020=CARTESIAN_POINT('Ctrl Pts',(4.5098417322706,-23.1413554691123,12.));
#192021=CARTESIAN_POINT('Ctrl Pts',(4.50098225775171,-23.1246211242115,
0.));
#192022=CARTESIAN_POINT('Ctrl Pts',(4.50098225775171,-23.1246211242115,
12.));
#192023=CARTESIAN_POINT('Ctrl Pts',(4.49222403252216,-23.1079665632636,
0.));
#192024=CARTESIAN_POINT('Ctrl Pts',(4.49222403252216,-23.1079665632636,
12.));
#192025=CARTESIAN_POINT('Ctrl Pts',(4.48356709006788,-23.0913929293922,
0.));
#192026=CARTESIAN_POINT('Ctrl Pts',(4.48356709006788,-23.0913929293922,
12.));
#192027=CARTESIAN_POINT('Ctrl Pts',(4.47501146242856,-23.0749013821881,
0.));
#192028=CARTESIAN_POINT('Ctrl Pts',(4.47501146242856,-23.0749013821881,
12.));
#192029=CARTESIAN_POINT('Ctrl Pts',(4.4665571801823,-23.0584930981732,0.));
#192030=CARTESIAN_POINT('Ctrl Pts',(4.4665571801823,-23.0584930981732,12.));
#192031=CARTESIAN_POINT('Ctrl Pts',(4.45820427241683,-23.0421692712467,
0.));
#192032=CARTESIAN_POINT('Ctrl Pts',(4.45820427241683,-23.0421692712467,
12.));
#192033=CARTESIAN_POINT('Ctrl Pts',(4.44995276669686,-23.0259311131392,
0.));
#192034=CARTESIAN_POINT('Ctrl Pts',(4.44995276669686,-23.0259311131392,
12.));
#192035=CARTESIAN_POINT('Ctrl Pts',(4.44180268901643,-23.0097798538395,
0.));
#192036=CARTESIAN_POINT('Ctrl Pts',(4.44180268901643,-23.0097798538395,
12.));
#192037=CARTESIAN_POINT('Ctrl Pts',(4.43375406376879,-22.9937167421006,
0.));
#192038=CARTESIAN_POINT('Ctrl Pts',(4.43375406376879,-22.9937167421006,
12.));
#192039=CARTESIAN_POINT('Ctrl Pts',(4.42580691372751,-22.977743046002,0.));
#192040=CARTESIAN_POINT('Ctrl Pts',(4.42580691372751,-22.977743046002,12.));
#192041=CARTESIAN_POINT('Ctrl Pts',(4.41796126001302,-22.9618600534866,
0.));
#192042=CARTESIAN_POINT('Ctrl Pts',(4.41796126001302,-22.9618600534866,
12.));
#192043=CARTESIAN_POINT('Ctrl Pts',(4.41021712205553,-22.9460690729093,
0.));
#192044=CARTESIAN_POINT('Ctrl Pts',(4.41021712205553,-22.9460690729093,
12.));
#192045=CARTESIAN_POINT('Ctrl Pts',(4.40257451754323,-22.930371433555,0.));
#192046=CARTESIAN_POINT('Ctrl Pts',(4.40257451754323,-22.930371433555,12.));
#192047=CARTESIAN_POINT('Ctrl Pts',(4.39503346238473,-22.9147684862426,
0.));
#192048=CARTESIAN_POINT('Ctrl Pts',(4.39503346238473,-22.9147684862426,
12.));
#192049=CARTESIAN_POINT('Ctrl Pts',(4.38759397068405,-22.8992616040108,
0.));
#192050=CARTESIAN_POINT('Ctrl Pts',(4.38759397068405,-22.8992616040108,
12.));
#192051=CARTESIAN_POINT('Ctrl Pts',(4.38025605470092,-22.8838521827701,
0.));
#192052=CARTESIAN_POINT('Ctrl Pts',(4.38025605470092,-22.8838521827701,
12.));
#192053=CARTESIAN_POINT('Ctrl Pts',(4.37301972480745,-22.8685416419725,
0.));
#192054=CARTESIAN_POINT('Ctrl Pts',(4.37301972480745,-22.8685416419725,
12.));
#192055=CARTESIAN_POINT('Ctrl Pts',(4.36588498942997,-22.8533314252422,
0.));
#192056=CARTESIAN_POINT('Ctrl Pts',(4.36588498942997,-22.8533314252422,
12.));
#192057=CARTESIAN_POINT('Ctrl Pts',(4.35885185500546,-22.8382230011184,
0.));
#192058=CARTESIAN_POINT('Ctrl Pts',(4.35885185500546,-22.8382230011184,
12.));
#192059=CARTESIAN_POINT('Ctrl Pts',(4.3519203259479,-22.8232178638876,0.));
#192060=CARTESIAN_POINT('Ctrl Pts',(4.3519203259479,-22.8232178638876,12.));
#192061=CARTESIAN_POINT('Ctrl Pts',(4.34509040460062,-22.8083175343791,
0.));
#192062=CARTESIAN_POINT('Ctrl Pts',(4.34509040460062,-22.8083175343791,
12.));
#192063=CARTESIAN_POINT('Ctrl Pts',(4.33836209118446,-22.7935235607806,
0.));
#192064=CARTESIAN_POINT('Ctrl Pts',(4.33836209118446,-22.7935235607806,
12.));
#192065=CARTESIAN_POINT('Ctrl Pts',(4.33173538373189,-22.7788375194076,
0.));
#192066=CARTESIAN_POINT('Ctrl Pts',(4.33173538373189,-22.7788375194076,
12.));
#192067=CARTESIAN_POINT('Ctrl Pts',(4.32521027803754,-22.7642610156475,
0.));
#192068=CARTESIAN_POINT('Ctrl Pts',(4.32521027803754,-22.7642610156475,
12.));
#192069=CARTESIAN_POINT('Ctrl Pts',(4.31878676761235,-22.7497956849848,
0.));
#192070=CARTESIAN_POINT('Ctrl Pts',(4.31878676761235,-22.7497956849848,
12.));
#192071=CARTESIAN_POINT('Ctrl Pts',(4.31246484362549,-22.7354431939926,
0.));
#192072=CARTESIAN_POINT('Ctrl Pts',(4.31246484362549,-22.7354431939926,
12.));
#192073=CARTESIAN_POINT('Ctrl Pts',(4.30624449484069,-22.7212052413386,
0.));
#192074=CARTESIAN_POINT('Ctrl Pts',(4.30624449484069,-22.7212052413386,
12.));
#192075=CARTESIAN_POINT('Ctrl Pts',(4.3001257075406,-22.7070835587564,0.));
#192076=CARTESIAN_POINT('Ctrl Pts',(4.3001257075406,-22.7070835587564,12.));
#192077=CARTESIAN_POINT('Ctrl Pts',(4.29410846547056,-22.6930799122548,
0.));
#192078=CARTESIAN_POINT('Ctrl Pts',(4.29410846547056,-22.6930799122548,
12.));
#192079=CARTESIAN_POINT('Ctrl Pts',(4.28819274977763,-22.6791961033538,
0.));
#192080=CARTESIAN_POINT('Ctrl Pts',(4.28819274977763,-22.6791961033538,
12.));
#192081=CARTESIAN_POINT('Ctrl Pts',(4.28237853894058,-22.6654339703109,
0.));
#192082=CARTESIAN_POINT('Ctrl Pts',(4.28237853894058,-22.6654339703109,
12.));
#192083=CARTESIAN_POINT('Ctrl Pts',(4.2766658086912,-22.6517953893303,0.));
#192084=CARTESIAN_POINT('Ctrl Pts',(4.2766658086912,-22.6517953893303,12.));
#192085=CARTESIAN_POINT('Ctrl Pts',(4.27105453193004,-22.6382822758172,
0.));
#192086=CARTESIAN_POINT('Ctrl Pts',(4.27105453193004,-22.6382822758172,
12.));
#192087=CARTESIAN_POINT('Ctrl Pts',(4.26554467865576,-22.6248965859977,
0.));
#192088=CARTESIAN_POINT('Ctrl Pts',(4.26554467865576,-22.6248965859977,
12.));
#192089=CARTESIAN_POINT('Ctrl Pts',(4.26013621588305,-22.6116403184821,
0.));
#192090=CARTESIAN_POINT('Ctrl Pts',(4.26013621588305,-22.6116403184821,
12.));
#192091=CARTESIAN_POINT('Ctrl Pts',(4.25482910755481,-22.5985155158636,
0.));
#192092=CARTESIAN_POINT('Ctrl Pts',(4.25482910755481,-22.5985155158636,
12.));
#192093=CARTESIAN_POINT('Ctrl Pts',(4.24962331444177,-22.5855242662477,
0.));
#192094=CARTESIAN_POINT('Ctrl Pts',(4.24962331444177,-22.5855242662477,
12.));
#192095=CARTESIAN_POINT('Ctrl Pts',(4.24451879404851,-22.572668704992,0.));
#192096=CARTESIAN_POINT('Ctrl Pts',(4.24451879404851,-22.572668704992,12.));
#192097=CARTESIAN_POINT('Ctrl Pts',(4.23951550052522,-22.5599510166429,
0.));
#192098=CARTESIAN_POINT('Ctrl Pts',(4.23951550052522,-22.5599510166429,
12.));
#192099=CARTESIAN_POINT('Ctrl Pts',(4.23461338456712,-22.5473734368086,
0.));
#192100=CARTESIAN_POINT('Ctrl Pts',(4.23461338456712,-22.5473734368086,
12.));
#192101=CARTESIAN_POINT('Ctrl Pts',(4.22981239330733,-22.5349382540588,
0.));
#192102=CARTESIAN_POINT('Ctrl Pts',(4.22981239330733,-22.5349382540588,
12.));
#192103=CARTESIAN_POINT('Ctrl Pts',(4.22511247020041,-22.5226478117886,
0.));
#192104=CARTESIAN_POINT('Ctrl Pts',(4.22511247020041,-22.5226478117886,
12.));
#192105=CARTESIAN_POINT('Ctrl Pts',(4.22051355490196,-22.5105045108881,
0.));
#192106=CARTESIAN_POINT('Ctrl Pts',(4.22051355490196,-22.5105045108881,
12.));
#192107=CARTESIAN_POINT('Ctrl Pts',(4.21601558313906,-22.4985108124228,
0.));
#192108=CARTESIAN_POINT('Ctrl Pts',(4.21601558313906,-22.4985108124228,
12.));
#192109=CARTESIAN_POINT('Ctrl Pts',(4.21161848657428,-22.4866692403147,
0.));
#192110=CARTESIAN_POINT('Ctrl Pts',(4.21161848657428,-22.4866692403147,
12.));
#192111=CARTESIAN_POINT('Ctrl Pts',(4.20732219265648,-22.4749823839917,
0.));
#192112=CARTESIAN_POINT('Ctrl Pts',(4.20732219265648,-22.4749823839917,
12.));
#192113=CARTESIAN_POINT('Ctrl Pts',(4.20312662448174,-22.4634529011437,
0.));
#192114=CARTESIAN_POINT('Ctrl Pts',(4.20312662448174,-22.4634529011437,
12.));
#192115=CARTESIAN_POINT('Ctrl Pts',(4.19903170066358,-22.4520835205422,
0.));
#192116=CARTESIAN_POINT('Ctrl Pts',(4.19903170066358,-22.4520835205422,
12.));
#192117=CARTESIAN_POINT('Ctrl Pts',(4.1950373351886,-22.4408770448917,0.));
#192118=CARTESIAN_POINT('Ctrl Pts',(4.1950373351886,-22.4408770448917,12.));
#192119=CARTESIAN_POINT('Ctrl Pts',(4.19114343726932,-22.4298363535416,
0.));
#192120=CARTESIAN_POINT('Ctrl Pts',(4.19114343726932,-22.4298363535416,
12.));
#192121=CARTESIAN_POINT('Ctrl Pts',(4.18734991117707,-22.4189644056109,
0.));
#192122=CARTESIAN_POINT('Ctrl Pts',(4.18734991117707,-22.4189644056109,
12.));
#192123=CARTESIAN_POINT('Ctrl Pts',(4.18365665600839,-22.4082642454448,
0.));
#192124=CARTESIAN_POINT('Ctrl Pts',(4.18365665600839,-22.4082642454448,
12.));
#192125=CARTESIAN_POINT('Ctrl Pts',(4.18006356544879,-22.3977390078074,
0.));
#192126=CARTESIAN_POINT('Ctrl Pts',(4.18006356544879,-22.3977390078074,
12.));
#192127=CARTESIAN_POINT('Ctrl Pts',(4.17657052752834,-22.3873919231339,
0.));
#192128=CARTESIAN_POINT('Ctrl Pts',(4.17657052752834,-22.3873919231339,
12.));
#192129=CARTESIAN_POINT('Ctrl Pts',(4.17317742436162,-22.3772263228624,
0.));
#192130=CARTESIAN_POINT('Ctrl Pts',(4.17317742436162,-22.3772263228624,
12.));
#192131=CARTESIAN_POINT('Ctrl Pts',(4.16988413199469,-22.3672456427605,
0.));
#192132=CARTESIAN_POINT('Ctrl Pts',(4.16988413199469,-22.3672456427605,
12.));
#192133=CARTESIAN_POINT('Ctrl Pts',(4.16669052026602,-22.3574534257397,
0.));
#192134=CARTESIAN_POINT('Ctrl Pts',(4.16669052026602,-22.3574534257397,
12.));
#192135=CARTESIAN_POINT('Ctrl Pts',(4.1635964526318,-22.3478533253886,0.));
#192136=CARTESIAN_POINT('Ctrl Pts',(4.1635964526318,-22.3478533253886,12.));
#192137=CARTESIAN_POINT('Ctrl Pts',(4.16060178604153,-22.3384491078599,
0.));
#192138=CARTESIAN_POINT('Ctrl Pts',(4.16060178604153,-22.3384491078599,
12.));
#192139=CARTESIAN_POINT('Ctrl Pts',(4.15770637047882,-22.3292446628957,
0.));
#192140=CARTESIAN_POINT('Ctrl Pts',(4.15770637047882,-22.3292446628957,
12.));
#192141=CARTESIAN_POINT('Ctrl Pts',(4.15491004835278,-22.3202440186979,
0.));
#192142=CARTESIAN_POINT('Ctrl Pts',(4.15491004835278,-22.3202440186979,
12.));
#192143=CARTESIAN_POINT('Ctrl Pts',(4.15221265396992,-22.3114513545186,
0.));
#192144=CARTESIAN_POINT('Ctrl Pts',(4.15221265396992,-22.3114513545186,
12.));
#192145=CARTESIAN_POINT('Ctrl Pts',(4.14961401285525,-22.3028710166935,
0.));
#192146=CARTESIAN_POINT('Ctrl Pts',(4.14961401285525,-22.3028710166935,
12.));
#192147=CARTESIAN_POINT('Ctrl Pts',(4.14711394168559,-22.2945075198468,
0.));
#192148=CARTESIAN_POINT('Ctrl Pts',(4.14711394168559,-22.2945075198468,
12.));
#192149=CARTESIAN_POINT('Ctrl Pts',(4.14471224859295,-22.2863655389167,
0.));
#192150=CARTESIAN_POINT('Ctrl Pts',(4.14471224859295,-22.2863655389167,
12.));
#192151=CARTESIAN_POINT('Ctrl Pts',(4.14240873321982,-22.2784499072026,
0.));
#192152=CARTESIAN_POINT('Ctrl Pts',(4.14240873321982,-22.2784499072026,
12.));
#192153=CARTESIAN_POINT('Ctrl Pts',(4.14020318715987,-22.2707656042456,
0.));
#192154=CARTESIAN_POINT('Ctrl Pts',(4.14020318715987,-22.2707656042456,
12.));
#192155=CARTESIAN_POINT('Ctrl Pts',(4.13809539255418,-22.263317791397,0.));
#192156=CARTESIAN_POINT('Ctrl Pts',(4.13809539255418,-22.263317791397,12.));
#192157=CARTESIAN_POINT('Ctrl Pts',(4.13608511977226,-22.2561118708422,
0.));
#192158=CARTESIAN_POINT('Ctrl Pts',(4.13608511977226,-22.2561118708422,
12.));
#192159=CARTESIAN_POINT('Ctrl Pts',(4.13417212558808,-22.2491535317789,
0.));
#192160=CARTESIAN_POINT('Ctrl Pts',(4.13417212558808,-22.2491535317789,
12.));
#192161=CARTESIAN_POINT('Ctrl Pts',(4.1323561506016,-22.2424488153523,0.));
#192162=CARTESIAN_POINT('Ctrl Pts',(4.1323561506016,-22.2424488153523,12.));
#192163=CARTESIAN_POINT('Ctrl Pts',(4.13063692157499,-22.2360040565534,
0.));
#192164=CARTESIAN_POINT('Ctrl Pts',(4.13063692157499,-22.2360040565534,
12.));
#192165=CARTESIAN_POINT('Ctrl Pts',(4.12901415463378,-22.2298258043947,
0.));
#192166=CARTESIAN_POINT('Ctrl Pts',(4.12901415463378,-22.2298258043947,
12.));
#192167=CARTESIAN_POINT('Ctrl Pts',(4.12748755830099,-22.2239207458781,
0.));
#192168=CARTESIAN_POINT('Ctrl Pts',(4.12748755830099,-22.2239207458781,
12.));
#192169=CARTESIAN_POINT('Ctrl Pts',(4.12605683613299,-22.2182956401341,
0.));
#192170=CARTESIAN_POINT('Ctrl Pts',(4.12605683613299,-22.2182956401341,
12.));
#192171=CARTESIAN_POINT('Ctrl Pts',(4.12472167516602,-22.2129576146671,
0.));
#192172=CARTESIAN_POINT('Ctrl Pts',(4.12472167516602,-22.2129576146671,
12.));
#192173=CARTESIAN_POINT('Ctrl Pts',(4.12348173702024,-22.2079143941719,
0.));
#192174=CARTESIAN_POINT('Ctrl Pts',(4.12348173702024,-22.2079143941719,
12.));
#192175=CARTESIAN_POINT('Ctrl Pts',(4.12233664408237,-22.2031746532106,
0.));
#192176=CARTESIAN_POINT('Ctrl Pts',(4.12233664408237,-22.2031746532106,
12.));
#192177=CARTESIAN_POINT('Ctrl Pts',(4.12128598183533,-22.1987479618246,
0.));
#192178=CARTESIAN_POINT('Ctrl Pts',(4.12128598183533,-22.1987479618246,
12.));
#192179=CARTESIAN_POINT('Ctrl Pts',(4.12032932637738,-22.1946440958098,
0.));
#192180=CARTESIAN_POINT('Ctrl Pts',(4.12032932637738,-22.1946440958098,
12.));
#192181=CARTESIAN_POINT('Ctrl Pts',(4.11946626228623,-22.1908725908525,
0.));
#192182=CARTESIAN_POINT('Ctrl Pts',(4.11946626228623,-22.1908725908525,
12.));
#192183=CARTESIAN_POINT('Ctrl Pts',(4.11869641271752,-22.1874419861496,
0.));
#192184=CARTESIAN_POINT('Ctrl Pts',(4.11869641271752,-22.1874419861496,
12.));
#192185=CARTESIAN_POINT('Ctrl Pts',(4.11801938107464,-22.1843613164855,
0.));
#192186=CARTESIAN_POINT('Ctrl Pts',(4.11801938107464,-22.1843613164855,
12.));
#192187=CARTESIAN_POINT('Ctrl Pts',(4.11743469691765,-22.1816414985788,
0.));
#192188=CARTESIAN_POINT('Ctrl Pts',(4.11743469691765,-22.1816414985788,
12.));
#192189=CARTESIAN_POINT('Ctrl Pts',(4.11694173195041,-22.179297473024,0.));
#192190=CARTESIAN_POINT('Ctrl Pts',(4.11694173195041,-22.179297473024,12.));
#192191=CARTESIAN_POINT('Ctrl Pts',(4.11653973150558,-22.177347426894,0.));
#192192=CARTESIAN_POINT('Ctrl Pts',(4.11653973150558,-22.177347426894,12.));
#192193=CARTESIAN_POINT('Ctrl Pts',(4.11622797217066,-22.1758088296598,
0.));
#192194=CARTESIAN_POINT('Ctrl Pts',(4.11622797217066,-22.1758088296598,
12.));
#192195=CARTESIAN_POINT('Ctrl Pts',(4.11600589882767,-22.1746949858773,
0.));
#192196=CARTESIAN_POINT('Ctrl Pts',(4.11600589882767,-22.1746949858773,
12.));
#192197=CARTESIAN_POINT('Ctrl Pts',(4.11589976826061,-22.174148802123,0.));
#192198=CARTESIAN_POINT('Ctrl Pts',(4.11589976826061,-22.174148802123,12.));
#192199=CARTESIAN_POINT('Ctrl Pts',(4.1158603587821,-22.1739341411684,0.));
#192200=CARTESIAN_POINT('Ctrl Pts',(4.1158603587821,-22.1739341411684,12.));
#192201=CARTESIAN_POINT('Ctrl Pts',(4.11585194677412,-22.1738776823239,
0.));
#192202=CARTESIAN_POINT('Ctrl Pts',(4.11585194677412,-22.1738776823239,
12.));
#192203=CARTESIAN_POINT('Ctrl Pts',(4.11585220600461,-22.1738711152697,
0.));
#192204=CARTESIAN_POINT('Ctrl Pts',(4.11585220600461,-22.1738711152697,
12.));
#192205=CARTESIAN_POINT('',(6.08833931617698,-25.2771067246846,0.));
#192206=CARTESIAN_POINT('Ctrl Pts',(6.08833931617698,-25.2771067246846,
0.));
#192207=CARTESIAN_POINT('Ctrl Pts',(6.08441489609824,-25.2729539149479,
0.));
#192208=CARTESIAN_POINT('Ctrl Pts',(6.07657531787577,-25.2646490489816,
0.));
#192209=CARTESIAN_POINT('Ctrl Pts',(6.06484373634696,-25.2521940105523,
0.));
#192210=CARTESIAN_POINT('Ctrl Pts',(6.04925720151412,-25.2355918138798,
0.));
#192211=CARTESIAN_POINT('Ctrl Pts',(6.02986667390187,-25.2148466201368,
0.));
#192212=CARTESIAN_POINT('Ctrl Pts',(6.0105688180476,-25.1941090269638,0.));
#192213=CARTESIAN_POINT('Ctrl Pts',(5.99136367859838,-25.1733791296154,
0.));
#192214=CARTESIAN_POINT('Ctrl Pts',(5.97225131495636,-25.1526570863065,
0.));
#192215=CARTESIAN_POINT('Ctrl Pts',(5.95323180187347,-25.1319431317273,
0.));
#192216=CARTESIAN_POINT('Ctrl Pts',(5.93430523086776,-25.1112375971182,
0.));
#192217=CARTESIAN_POINT('Ctrl Pts',(5.91547170844382,-25.0905409050863,
0.));
#192218=CARTESIAN_POINT('Ctrl Pts',(5.89673135155458,-25.0698535426593,
0.));
#192219=CARTESIAN_POINT('Ctrl Pts',(5.87808428385329,-25.0491760405965,
0.));
#192220=CARTESIAN_POINT('Ctrl Pts',(5.8595306315681,-25.0285089498922,0.));
#192221=CARTESIAN_POINT('Ctrl Pts',(5.84107051963073,-25.0078528200558,
0.));
#192222=CARTESIAN_POINT('Ctrl Pts',(5.82270406744213,-24.9872081752709,
0.));
#192223=CARTESIAN_POINT('Ctrl Pts',(5.80443138549747,-24.9665754954463,
0.));
#192224=CARTESIAN_POINT('Ctrl Pts',(5.78625257775702,-24.9459552293308,
0.));
#192225=CARTESIAN_POINT('Ctrl Pts',(5.76816774342236,-24.9253478043632,
0.));
#192226=CARTESIAN_POINT('Ctrl Pts',(5.75017697890812,-24.9047536376467,
0.));
#192227=CARTESIAN_POINT('Ctrl Pts',(5.73228037976926,-24.8841731467219,
0.));
#192228=CARTESIAN_POINT('Ctrl Pts',(5.71447804252019,-24.8636067597677,
0.));
#192229=CARTESIAN_POINT('Ctrl Pts',(5.69677006679429,-24.8430549277634,
0.));
#192230=CARTESIAN_POINT('Ctrl Pts',(5.67915655496524,-24.822518122386,0.));
#192231=CARTESIAN_POINT('Ctrl Pts',(5.66163761114903,-24.8019968304618,
0.));
#192232=CARTESIAN_POINT('Ctrl Pts',(5.64421334042247,-24.7814915496728,
0.));
#192233=CARTESIAN_POINT('Ctrl Pts',(5.62688384790918,-24.76100278357,0.));
#192234=CARTESIAN_POINT('Ctrl Pts',(5.60964923798494,-24.7405310372736,
0.));
#192235=CARTESIAN_POINT('Ctrl Pts',(5.59250961323995,-24.7200768119079,
0.));
#192236=CARTESIAN_POINT('Ctrl Pts',(5.57546507427766,-24.6996406035507,
0.));
#192237=CARTESIAN_POINT('Ctrl Pts',(5.55851572025389,-24.6792229061785,
0.));
#192238=CARTESIAN_POINT('Ctrl Pts',(5.54166164919592,-24.6588242134733,
0.));
#192239=CARTESIAN_POINT('Ctrl Pts',(5.52490295840996,-24.6384450211466,
0.));
#192240=CARTESIAN_POINT('Ctrl Pts',(5.50823974481959,-24.618085828918,0.));
#192241=CARTESIAN_POINT('Ctrl Pts',(5.49167210537235,-24.5977471429365,
0.));
#192242=CARTESIAN_POINT('Ctrl Pts',(5.47520013724403,-24.5774294770329,
0.));
#192243=CARTESIAN_POINT('Ctrl Pts',(5.45882393762244,-24.5571333514841,
0.));
#192244=CARTESIAN_POINT('Ctrl Pts',(5.44254360356865,-24.5368592922861,
0.));
#192245=CARTESIAN_POINT('Ctrl Pts',(5.42635923183411,-24.5166078302107,
0.));
#192246=CARTESIAN_POINT('Ctrl Pts',(5.41027091869242,-24.4963794999831,
0.));
#192247=CARTESIAN_POINT('Ctrl Pts',(5.3942787597383,-24.4761748393322,0.));
#192248=CARTESIAN_POINT('Ctrl Pts',(5.37838284973706,-24.4559943883159,
0.));
#192249=CARTESIAN_POINT('Ctrl Pts',(5.36258328273639,-24.4358386899152,
0.));
#192250=CARTESIAN_POINT('Ctrl Pts',(5.34688015213546,-24.4157082904615,
0.));
#192251=CARTESIAN_POINT('Ctrl Pts',(5.33127355076036,-24.3956037401293,
0.));
#192252=CARTESIAN_POINT('Ctrl Pts',(5.31576357092524,-24.3755255933917,
0.));
#192253=CARTESIAN_POINT('Ctrl Pts',(5.30035030449058,-24.3554744095075,
0.));
#192254=CARTESIAN_POINT('Ctrl Pts',(5.28503384290644,-24.3354507529415,
0.));
#192255=CARTESIAN_POINT('Ctrl Pts',(5.26981427718796,-24.3154551932222,
0.));
#192256=CARTESIAN_POINT('Ctrl Pts',(5.25469169788855,-24.2954883048448,
0.));
#192257=CARTESIAN_POINT('Ctrl Pts',(5.23966619506289,-24.2755506671526,
0.));
#192258=CARTESIAN_POINT('Ctrl Pts',(5.22473785822441,-24.2556428642294,
0.));
#192259=CARTESIAN_POINT('Ctrl Pts',(5.20990677629173,-24.2357654847765,
0.));
#192260=CARTESIAN_POINT('Ctrl Pts',(5.19517303753642,-24.215919122017,0.));
#192261=CARTESIAN_POINT('Ctrl Pts',(5.18053672961392,-24.1961043738754,
0.));
#192262=CARTESIAN_POINT('Ctrl Pts',(5.16599793957979,-24.1763218431343,
0.));
#192263=CARTESIAN_POINT('Ctrl Pts',(5.15155675390075,-24.1565721375971,
0.));
#192264=CARTESIAN_POINT('Ctrl Pts',(5.13721325845744,-24.1368558702443,
0.));
#192265=CARTESIAN_POINT('Ctrl Pts',(5.12296753853859,-24.117173659394,0.));
#192266=CARTESIAN_POINT('Ctrl Pts',(5.10881967883132,-24.0975261288446,
0.));
#192267=CARTESIAN_POINT('Ctrl Pts',(5.09476976342625,-24.0779139079266,
0.));
#192268=CARTESIAN_POINT('Ctrl Pts',(5.08081787581276,-24.0583376315638,
0.));
#192269=CARTESIAN_POINT('Ctrl Pts',(5.06696409886641,-24.0387979403268,
0.));
#192270=CARTESIAN_POINT('Ctrl Pts',(5.05320851483065,-24.0192954804896,
0.));
#192271=CARTESIAN_POINT('Ctrl Pts',(5.03955120528521,-23.9998309040746,
0.));
#192272=CARTESIAN_POINT('Ctrl Pts',(5.02599225112454,-23.9804048689227,
0.));
#192273=CARTESIAN_POINT('Ctrl Pts',(5.01253173257452,-23.9610180388271,
0.));
#192274=CARTESIAN_POINT('Ctrl Pts',(4.99916972919306,-23.9416710836529,
0.));
#192275=CARTESIAN_POINT('Ctrl Pts',(4.98590631986532,-23.9223646794592,
0.));
#192276=CARTESIAN_POINT('Ctrl Pts',(4.97274158279226,-23.9030995086163,
0.));
#192277=CARTESIAN_POINT('Ctrl Pts',(4.9596755954656,-23.8838762599218,0.));
#192278=CARTESIAN_POINT('Ctrl Pts',(4.9467084346586,-23.8646956287168,0.));
#192279=CARTESIAN_POINT('Ctrl Pts',(4.93384017643432,-23.8455583170057,
0.));
#192280=CARTESIAN_POINT('Ctrl Pts',(4.92107089613968,-23.8264650335717,
0.));
#192281=CARTESIAN_POINT('Ctrl Pts',(4.90840066839344,-23.8074164940896,
0.));
#192282=CARTESIAN_POINT('Ctrl Pts',(4.89582956706775,-23.7884134212384,
0.));
#192283=CARTESIAN_POINT('Ctrl Pts',(4.88335766525573,-23.7694565448049,
0.));
#192284=CARTESIAN_POINT('Ctrl Pts',(4.87098503527152,-23.7505466018245,
0.));
#192285=CARTESIAN_POINT('Ctrl Pts',(4.85871174865499,-23.7316843367313,
0.));
#192286=CARTESIAN_POINT('Ctrl Pts',(4.84653787616425,-23.7128705015017,
0.));
#192287=CARTESIAN_POINT('Ctrl Pts',(4.83446348776265,-23.6941058557971,
0.));
#192288=CARTESIAN_POINT('Ctrl Pts',(4.82248865259562,-23.675391167102,0.));
#192289=CARTESIAN_POINT('Ctrl Pts',(4.81061343896432,-23.6567272108628,
0.));
#192290=CARTESIAN_POINT('Ctrl Pts',(4.7988379143322,-23.6381147706579,0.));
#192291=CARTESIAN_POINT('Ctrl Pts',(4.78716214532097,-23.6195546383624,
0.));
#192292=CARTESIAN_POINT('Ctrl Pts',(4.77558619769872,-23.6010476143099,
0.));
#192293=CARTESIAN_POINT('Ctrl Pts',(4.76411013636251,-23.5825945074535,
0.));
#192294=CARTESIAN_POINT('Ctrl Pts',(4.75273402530617,-23.5641961355168,
0.));
#192295=CARTESIAN_POINT('Ctrl Pts',(4.74145792760698,-23.545853325171,0.));
#192296=CARTESIAN_POINT('Ctrl Pts',(4.73028190543029,-23.5275669122372,
0.));
#192297=CARTESIAN_POINT('Ctrl Pts',(4.71920602001901,-23.509337741878,0.));
#192298=CARTESIAN_POINT('Ctrl Pts',(4.70823033167818,-23.491166668789,0.));
#192299=CARTESIAN_POINT('Ctrl Pts',(4.69735489975024,-23.4730545573853,
0.));
#192300=CARTESIAN_POINT('Ctrl Pts',(4.68657978258303,-23.455002281986,0.));
#192301=CARTESIAN_POINT('Ctrl Pts',(4.67590503753058,-23.4370107270451,
0.));
#192302=CARTESIAN_POINT('Ctrl Pts',(4.6653307209467,-23.4190807873803,0.));
#192303=CARTESIAN_POINT('Ctrl Pts',(4.65485688816924,-23.4012133683959,
0.));
#192304=CARTESIAN_POINT('Ctrl Pts',(4.6444835934993,-23.3834093863068,0.));
#192305=CARTESIAN_POINT('Ctrl Pts',(4.63421089016541,-23.3656697683489,
0.));
#192306=CARTESIAN_POINT('Ctrl Pts',(4.62403883030805,-23.3479954530272,
0.));
#192307=CARTESIAN_POINT('Ctrl Pts',(4.6139674649783,-23.3303873903938,0.));
#192308=CARTESIAN_POINT('Ctrl Pts',(4.60399684412163,-23.3128465423115,
0.));
#192309=CARTESIAN_POINT('Ctrl Pts',(4.5941270165575,-23.2953738827191,0.));
#192310=CARTESIAN_POINT('Ctrl Pts',(4.5843580299469,-23.2779703978876,0.));
#192311=CARTESIAN_POINT('Ctrl Pts',(4.57468993076097,-23.2606370866866,
0.));
#192312=CARTESIAN_POINT('Ctrl Pts',(4.56512276427839,-23.2433749609131,
0.));
#192313=CARTESIAN_POINT('Ctrl Pts',(4.55565657456975,-23.2261850456064,
0.));
#192314=CARTESIAN_POINT('Ctrl Pts',(4.54629140447544,-23.2090683793629,
0.));
#192315=CARTESIAN_POINT('Ctrl Pts',(4.53702729557566,-23.1920260146465,
0.));
#192316=CARTESIAN_POINT('Ctrl Pts',(4.52786428815014,-23.1750590180908,
0.));
#192317=CARTESIAN_POINT('Ctrl Pts',(4.51880242116748,-23.1581684708761,
0.));
#192318=CARTESIAN_POINT('Ctrl Pts',(4.5098417322706,-23.1413554691123,0.));
#192319=CARTESIAN_POINT('Ctrl Pts',(4.50098225775171,-23.1246211242115,
0.));
#192320=CARTESIAN_POINT('Ctrl Pts',(4.49222403252216,-23.1079665632636,
0.));
#192321=CARTESIAN_POINT('Ctrl Pts',(4.48356709006788,-23.0913929293922,
0.));
#192322=CARTESIAN_POINT('Ctrl Pts',(4.47501146242856,-23.0749013821881,
0.));
#192323=CARTESIAN_POINT('Ctrl Pts',(4.4665571801823,-23.0584930981732,0.));
#192324=CARTESIAN_POINT('Ctrl Pts',(4.45820427241683,-23.0421692712467,
0.));
#192325=CARTESIAN_POINT('Ctrl Pts',(4.44995276669686,-23.0259311131392,
0.));
#192326=CARTESIAN_POINT('Ctrl Pts',(4.44180268901643,-23.0097798538395,
0.));
#192327=CARTESIAN_POINT('Ctrl Pts',(4.43375406376879,-22.9937167421006,
0.));
#192328=CARTESIAN_POINT('Ctrl Pts',(4.42580691372751,-22.977743046002,0.));
#192329=CARTESIAN_POINT('Ctrl Pts',(4.41796126001302,-22.9618600534866,
0.));
#192330=CARTESIAN_POINT('Ctrl Pts',(4.41021712205553,-22.9460690729093,
0.));
#192331=CARTESIAN_POINT('Ctrl Pts',(4.40257451754323,-22.930371433555,0.));
#192332=CARTESIAN_POINT('Ctrl Pts',(4.39503346238473,-22.9147684862426,
0.));
#192333=CARTESIAN_POINT('Ctrl Pts',(4.38759397068405,-22.8992616040108,
0.));
#192334=CARTESIAN_POINT('Ctrl Pts',(4.38025605470092,-22.8838521827701,
0.));
#192335=CARTESIAN_POINT('Ctrl Pts',(4.37301972480745,-22.8685416419725,
0.));
#192336=CARTESIAN_POINT('Ctrl Pts',(4.36588498942997,-22.8533314252422,
0.));
#192337=CARTESIAN_POINT('Ctrl Pts',(4.35885185500546,-22.8382230011184,
0.));
#192338=CARTESIAN_POINT('Ctrl Pts',(4.3519203259479,-22.8232178638876,0.));
#192339=CARTESIAN_POINT('Ctrl Pts',(4.34509040460062,-22.8083175343791,
0.));
#192340=CARTESIAN_POINT('Ctrl Pts',(4.33836209118446,-22.7935235607806,
0.));
#192341=CARTESIAN_POINT('Ctrl Pts',(4.33173538373189,-22.7788375194076,
0.));
#192342=CARTESIAN_POINT('Ctrl Pts',(4.32521027803754,-22.7642610156475,
0.));
#192343=CARTESIAN_POINT('Ctrl Pts',(4.31878676761235,-22.7497956849848,
0.));
#192344=CARTESIAN_POINT('Ctrl Pts',(4.31246484362549,-22.7354431939926,
0.));
#192345=CARTESIAN_POINT('Ctrl Pts',(4.30624449484069,-22.7212052413386,
0.));
#192346=CARTESIAN_POINT('Ctrl Pts',(4.3001257075406,-22.7070835587564,0.));
#192347=CARTESIAN_POINT('Ctrl Pts',(4.29410846547056,-22.6930799122548,
0.));
#192348=CARTESIAN_POINT('Ctrl Pts',(4.28819274977763,-22.6791961033538,
0.));
#192349=CARTESIAN_POINT('Ctrl Pts',(4.28237853894058,-22.6654339703109,
0.));
#192350=CARTESIAN_POINT('Ctrl Pts',(4.2766658086912,-22.6517953893303,0.));
#192351=CARTESIAN_POINT('Ctrl Pts',(4.27105453193004,-22.6382822758172,
0.));
#192352=CARTESIAN_POINT('Ctrl Pts',(4.26554467865576,-22.6248965859977,
0.));
#192353=CARTESIAN_POINT('Ctrl Pts',(4.26013621588305,-22.6116403184821,
0.));
#192354=CARTESIAN_POINT('Ctrl Pts',(4.25482910755481,-22.5985155158636,
0.));
#192355=CARTESIAN_POINT('Ctrl Pts',(4.24962331444177,-22.5855242662477,
0.));
#192356=CARTESIAN_POINT('Ctrl Pts',(4.24451879404851,-22.572668704992,0.));
#192357=CARTESIAN_POINT('Ctrl Pts',(4.23951550052522,-22.5599510166429,
0.));
#192358=CARTESIAN_POINT('Ctrl Pts',(4.23461338456712,-22.5473734368086,
0.));
#192359=CARTESIAN_POINT('Ctrl Pts',(4.22981239330733,-22.5349382540588,
0.));
#192360=CARTESIAN_POINT('Ctrl Pts',(4.22511247020041,-22.5226478117886,
0.));
#192361=CARTESIAN_POINT('Ctrl Pts',(4.22051355490196,-22.5105045108881,
0.));
#192362=CARTESIAN_POINT('Ctrl Pts',(4.21601558313906,-22.4985108124228,
0.));
#192363=CARTESIAN_POINT('Ctrl Pts',(4.21161848657428,-22.4866692403147,
0.));
#192364=CARTESIAN_POINT('Ctrl Pts',(4.20732219265648,-22.4749823839917,
0.));
#192365=CARTESIAN_POINT('Ctrl Pts',(4.20312662448174,-22.4634529011437,
0.));
#192366=CARTESIAN_POINT('Ctrl Pts',(4.19903170066358,-22.4520835205422,
0.));
#192367=CARTESIAN_POINT('Ctrl Pts',(4.1950373351886,-22.4408770448917,0.));
#192368=CARTESIAN_POINT('Ctrl Pts',(4.19114343726932,-22.4298363535416,
0.));
#192369=CARTESIAN_POINT('Ctrl Pts',(4.18734991117707,-22.4189644056109,
0.));
#192370=CARTESIAN_POINT('Ctrl Pts',(4.18365665600839,-22.4082642454448,
0.));
#192371=CARTESIAN_POINT('Ctrl Pts',(4.18006356544879,-22.3977390078074,
0.));
#192372=CARTESIAN_POINT('Ctrl Pts',(4.17657052752834,-22.3873919231339,
0.));
#192373=CARTESIAN_POINT('Ctrl Pts',(4.17317742436162,-22.3772263228624,
0.));
#192374=CARTESIAN_POINT('Ctrl Pts',(4.16988413199469,-22.3672456427605,
0.));
#192375=CARTESIAN_POINT('Ctrl Pts',(4.16669052026602,-22.3574534257397,
0.));
#192376=CARTESIAN_POINT('Ctrl Pts',(4.1635964526318,-22.3478533253886,0.));
#192377=CARTESIAN_POINT('Ctrl Pts',(4.16060178604153,-22.3384491078599,
0.));
#192378=CARTESIAN_POINT('Ctrl Pts',(4.15770637047882,-22.3292446628957,
0.));
#192379=CARTESIAN_POINT('Ctrl Pts',(4.15491004835278,-22.3202440186979,
0.));
#192380=CARTESIAN_POINT('Ctrl Pts',(4.15221265396992,-22.3114513545186,
0.));
#192381=CARTESIAN_POINT('Ctrl Pts',(4.14961401285525,-22.3028710166935,
0.));
#192382=CARTESIAN_POINT('Ctrl Pts',(4.14711394168559,-22.2945075198468,
0.));
#192383=CARTESIAN_POINT('Ctrl Pts',(4.14471224859295,-22.2863655389167,
0.));
#192384=CARTESIAN_POINT('Ctrl Pts',(4.14240873321982,-22.2784499072026,
0.));
#192385=CARTESIAN_POINT('Ctrl Pts',(4.14020318715987,-22.2707656042456,
0.));
#192386=CARTESIAN_POINT('Ctrl Pts',(4.13809539255418,-22.263317791397,0.));
#192387=CARTESIAN_POINT('Ctrl Pts',(4.13608511977226,-22.2561118708422,
0.));
#192388=CARTESIAN_POINT('Ctrl Pts',(4.13417212558808,-22.2491535317789,
0.));
#192389=CARTESIAN_POINT('Ctrl Pts',(4.1323561506016,-22.2424488153523,0.));
#192390=CARTESIAN_POINT('Ctrl Pts',(4.13063692157499,-22.2360040565534,
0.));
#192391=CARTESIAN_POINT('Ctrl Pts',(4.12901415463378,-22.2298258043947,
0.));
#192392=CARTESIAN_POINT('Ctrl Pts',(4.12748755830099,-22.2239207458781,
0.));
#192393=CARTESIAN_POINT('Ctrl Pts',(4.12605683613299,-22.2182956401341,
0.));
#192394=CARTESIAN_POINT('Ctrl Pts',(4.12472167516602,-22.2129576146671,
0.));
#192395=CARTESIAN_POINT('Ctrl Pts',(4.12348173702024,-22.2079143941719,
0.));
#192396=CARTESIAN_POINT('Ctrl Pts',(4.12233664408237,-22.2031746532106,
0.));
#192397=CARTESIAN_POINT('Ctrl Pts',(4.12128598183533,-22.1987479618246,
0.));
#192398=CARTESIAN_POINT('Ctrl Pts',(4.12032932637738,-22.1946440958098,
0.));
#192399=CARTESIAN_POINT('Ctrl Pts',(4.11946626228623,-22.1908725908525,
0.));
#192400=CARTESIAN_POINT('Ctrl Pts',(4.11869641271752,-22.1874419861496,
0.));
#192401=CARTESIAN_POINT('Ctrl Pts',(4.11801938107464,-22.1843613164855,
0.));
#192402=CARTESIAN_POINT('Ctrl Pts',(4.11743469691765,-22.1816414985788,
0.));
#192403=CARTESIAN_POINT('Ctrl Pts',(4.11694173195041,-22.179297473024,0.));
#192404=CARTESIAN_POINT('Ctrl Pts',(4.11653973150558,-22.177347426894,0.));
#192405=CARTESIAN_POINT('Ctrl Pts',(4.11622797217066,-22.1758088296598,
0.));
#192406=CARTESIAN_POINT('Ctrl Pts',(4.11600589882767,-22.1746949858773,
0.));
#192407=CARTESIAN_POINT('Ctrl Pts',(4.11589976826061,-22.174148802123,0.));
#192408=CARTESIAN_POINT('Ctrl Pts',(4.1158603587821,-22.1739341411684,0.));
#192409=CARTESIAN_POINT('Ctrl Pts',(4.11585194677412,-22.1738776823239,
0.));
#192410=CARTESIAN_POINT('Ctrl Pts',(4.11585220600461,-22.1738711152697,
0.));
#192411=CARTESIAN_POINT('',(6.08833931617698,-25.2771067246846,0.));
#192412=CARTESIAN_POINT('Ctrl Pts',(1.76341220531179,-22.4835757167854,
0.));
#192413=CARTESIAN_POINT('Ctrl Pts',(1.76341220531179,-22.4835757167854,
12.));
#192414=CARTESIAN_POINT('Ctrl Pts',(1.76341415538764,-22.483581992979,0.));
#192415=CARTESIAN_POINT('Ctrl Pts',(1.76341415538764,-22.483581992979,12.));
#192416=CARTESIAN_POINT('Ctrl Pts',(1.7634206426357,-22.4836387052232,0.));
#192417=CARTESIAN_POINT('Ctrl Pts',(1.7634206426357,-22.4836387052232,12.));
#192418=CARTESIAN_POINT('Ctrl Pts',(1.76343813434565,-22.483856251707,0.));
#192419=CARTESIAN_POINT('Ctrl Pts',(1.76343813434565,-22.483856251707,12.));
#192420=CARTESIAN_POINT('Ctrl Pts',(1.76347698284791,-22.4844112933129,
0.));
#192421=CARTESIAN_POINT('Ctrl Pts',(1.76347698284791,-22.4844112933129,
12.));
#192422=CARTESIAN_POINT('Ctrl Pts',(1.76355076045546,-22.4855446605991,
0.));
#192423=CARTESIAN_POINT('Ctrl Pts',(1.76355076045546,-22.4855446605991,
12.));
#192424=CARTESIAN_POINT('Ctrl Pts',(1.76364784232963,-22.4871115206571,
0.));
#192425=CARTESIAN_POINT('Ctrl Pts',(1.76364784232963,-22.4871115206571,
12.));
#192426=CARTESIAN_POINT('Ctrl Pts',(1.76376424879504,-22.4890991659478,
0.));
#192427=CARTESIAN_POINT('Ctrl Pts',(1.76376424879504,-22.4890991659478,
12.));
#192428=CARTESIAN_POINT('Ctrl Pts',(1.76389475965723,-22.4914909094908,
0.));
#192429=CARTESIAN_POINT('Ctrl Pts',(1.76389475965723,-22.4914909094908,
12.));
#192430=CARTESIAN_POINT('Ctrl Pts',(1.764033938803,-22.4942693792449,0.));
#192431=CARTESIAN_POINT('Ctrl Pts',(1.764033938803,-22.4942693792449,12.));
#192432=CARTESIAN_POINT('Ctrl Pts',(1.76417731243462,-22.4974203063191,
0.));
#192433=CARTESIAN_POINT('Ctrl Pts',(1.76417731243462,-22.4974203063191,
12.));
#192434=CARTESIAN_POINT('Ctrl Pts',(1.76432160068725,-22.5009332677316,
0.));
#192435=CARTESIAN_POINT('Ctrl Pts',(1.76432160068725,-22.5009332677316,
12.));
#192436=CARTESIAN_POINT('Ctrl Pts',(1.76446408210366,-22.5047996391978,
0.));
#192437=CARTESIAN_POINT('Ctrl Pts',(1.76446408210366,-22.5047996391978,
12.));
#192438=CARTESIAN_POINT('Ctrl Pts',(1.76460218257323,-22.5090112700212,
0.));
#192439=CARTESIAN_POINT('Ctrl Pts',(1.76460218257323,-22.5090112700212,
12.));
#192440=CARTESIAN_POINT('Ctrl Pts',(1.76473303281158,-22.5135590569554,
0.));
#192441=CARTESIAN_POINT('Ctrl Pts',(1.76473303281158,-22.5135590569554,
12.));
#192442=CARTESIAN_POINT('Ctrl Pts',(1.76485369319896,-22.5184336670207,
0.));
#192443=CARTESIAN_POINT('Ctrl Pts',(1.76485369319896,-22.5184336670207,
12.));
#192444=CARTESIAN_POINT('Ctrl Pts',(1.76496128643369,-22.5236259635515,
0.));
#192445=CARTESIAN_POINT('Ctrl Pts',(1.76496128643369,-22.5236259635515,
12.));
#192446=CARTESIAN_POINT('Ctrl Pts',(1.76505320262751,-22.529127665298,0.));
#192447=CARTESIAN_POINT('Ctrl Pts',(1.76505320262751,-22.529127665298,12.));
#192448=CARTESIAN_POINT('Ctrl Pts',(1.7651271156325,-22.5349313983571,0.));
#192449=CARTESIAN_POINT('Ctrl Pts',(1.7651271156325,-22.5349313983571,12.));
#192450=CARTESIAN_POINT('Ctrl Pts',(1.76518087841492,-22.5410303590891,
0.));
#192451=CARTESIAN_POINT('Ctrl Pts',(1.76518087841492,-22.5410303590891,
12.));
#192452=CARTESIAN_POINT('Ctrl Pts',(1.76521245524047,-22.5474180954006,
0.));
#192453=CARTESIAN_POINT('Ctrl Pts',(1.76521245524047,-22.5474180954006,
12.));
#192454=CARTESIAN_POINT('Ctrl Pts',(1.76521983384062,-22.5540882235837,
0.));
#192455=CARTESIAN_POINT('Ctrl Pts',(1.76521983384062,-22.5540882235837,
12.));
#192456=CARTESIAN_POINT('Ctrl Pts',(1.76520104500449,-22.5610344912501,
0.));
#192457=CARTESIAN_POINT('Ctrl Pts',(1.76520104500449,-22.5610344912501,
12.));
#192458=CARTESIAN_POINT('Ctrl Pts',(1.76515418518829,-22.5682508499873,
0.));
#192459=CARTESIAN_POINT('Ctrl Pts',(1.76515418518829,-22.5682508499873,
12.));
#192460=CARTESIAN_POINT('Ctrl Pts',(1.76507744026747,-22.5757315316355,
0.));
#192461=CARTESIAN_POINT('Ctrl Pts',(1.76507744026747,-22.5757315316355,
12.));
#192462=CARTESIAN_POINT('Ctrl Pts',(1.76496910283088,-22.5834711038024,
0.));
#192463=CARTESIAN_POINT('Ctrl Pts',(1.76496910283088,-22.5834711038024,
12.));
#192464=CARTESIAN_POINT('Ctrl Pts',(1.76482755288411,-22.5914644078106,
0.));
#192465=CARTESIAN_POINT('Ctrl Pts',(1.76482755288411,-22.5914644078106,
12.));
#192466=CARTESIAN_POINT('Ctrl Pts',(1.76465124413556,-22.5997065145638,
0.));
#192467=CARTESIAN_POINT('Ctrl Pts',(1.76465124413556,-22.5997065145638,
12.));
#192468=CARTESIAN_POINT('Ctrl Pts',(1.76443868648015,-22.6081926681342,
0.));
#192469=CARTESIAN_POINT('Ctrl Pts',(1.76443868648015,-22.6081926681342,
12.));
#192470=CARTESIAN_POINT('Ctrl Pts',(1.76418843543739,-22.6169182517693,
0.));
#192471=CARTESIAN_POINT('Ctrl Pts',(1.76418843543739,-22.6169182517693,
12.));
#192472=CARTESIAN_POINT('Ctrl Pts',(1.76389909571402,-22.6258787994847,
0.));
#192473=CARTESIAN_POINT('Ctrl Pts',(1.76389909571402,-22.6258787994847,
12.));
#192474=CARTESIAN_POINT('Ctrl Pts',(1.76356932176272,-22.635069997936,0.));
#192475=CARTESIAN_POINT('Ctrl Pts',(1.76356932176272,-22.635069997936,12.));
#192476=CARTESIAN_POINT('Ctrl Pts',(1.76319782013913,-22.6444876940425,
0.));
#192477=CARTESIAN_POINT('Ctrl Pts',(1.76319782013913,-22.6444876940425,
12.));
#192478=CARTESIAN_POINT('Ctrl Pts',(1.76278334912559,-22.6541278938413,
0.));
#192479=CARTESIAN_POINT('Ctrl Pts',(1.76278334912559,-22.6541278938413,
12.));
#192480=CARTESIAN_POINT('Ctrl Pts',(1.76232471392567,-22.6639867471756,
0.));
#192481=CARTESIAN_POINT('Ctrl Pts',(1.76232471392567,-22.6639867471756,
12.));
#192482=CARTESIAN_POINT('Ctrl Pts',(1.76182076289525,-22.6740605356699,
0.));
#192483=CARTESIAN_POINT('Ctrl Pts',(1.76182076289525,-22.6740605356699,
12.));
#192484=CARTESIAN_POINT('Ctrl Pts',(1.76127038310612,-22.6843456585245,
0.));
#192485=CARTESIAN_POINT('Ctrl Pts',(1.76127038310612,-22.6843456585245,
12.));
#192486=CARTESIAN_POINT('Ctrl Pts',(1.76067249704884,-22.6948386219843,
0.));
#192487=CARTESIAN_POINT('Ctrl Pts',(1.76067249704884,-22.6948386219843,
12.));
#192488=CARTESIAN_POINT('Ctrl Pts',(1.76002606202398,-22.7055360375481,
0.));
#192489=CARTESIAN_POINT('Ctrl Pts',(1.76002606202398,-22.7055360375481,
12.));
#192490=CARTESIAN_POINT('Ctrl Pts',(1.75933006905924,-22.7164346186007,
0.));
#192491=CARTESIAN_POINT('Ctrl Pts',(1.75933006905924,-22.7164346186007,
12.));
#192492=CARTESIAN_POINT('Ctrl Pts',(1.75858354204634,-22.7275311777305,
0.));
#192493=CARTESIAN_POINT('Ctrl Pts',(1.75858354204634,-22.7275311777305,
12.));
#192494=CARTESIAN_POINT('Ctrl Pts',(1.75778553673249,-22.7388226235565,
0.));
#192495=CARTESIAN_POINT('Ctrl Pts',(1.75778553673249,-22.7388226235565,
12.));
#192496=CARTESIAN_POINT('Ctrl Pts',(1.75693513908911,-22.7503059556455,
0.));
#192497=CARTESIAN_POINT('Ctrl Pts',(1.75693513908911,-22.7503059556455,
12.));
#192498=CARTESIAN_POINT('Ctrl Pts',(1.7560314637164,-22.7619782595013,0.));
#192499=CARTESIAN_POINT('Ctrl Pts',(1.7560314637164,-22.7619782595013,12.));
#192500=CARTESIAN_POINT('Ctrl Pts',(1.75507365227127,-22.7738367016115,
0.));
#192501=CARTESIAN_POINT('Ctrl Pts',(1.75507365227127,-22.7738367016115,
12.));
#192502=CARTESIAN_POINT('Ctrl Pts',(1.75406087182929,-22.7858785242358,
0.));
#192503=CARTESIAN_POINT('Ctrl Pts',(1.75406087182929,-22.7858785242358,
12.));
#192504=CARTESIAN_POINT('Ctrl Pts',(1.75299231391461,-22.7981010424312,
0.));
#192505=CARTESIAN_POINT('Ctrl Pts',(1.75299231391461,-22.7981010424312,
12.));
#192506=CARTESIAN_POINT('Ctrl Pts',(1.75186719365589,-22.8105016414712,
0.));
#192507=CARTESIAN_POINT('Ctrl Pts',(1.75186719365589,-22.8105016414712,
12.));
#192508=CARTESIAN_POINT('Ctrl Pts',(1.75068474890883,-22.8230777741285,
0.));
#192509=CARTESIAN_POINT('Ctrl Pts',(1.75068474890883,-22.8230777741285,
12.));
#192510=CARTESIAN_POINT('Ctrl Pts',(1.74944423940117,-22.8358269579854,
0.));
#192511=CARTESIAN_POINT('Ctrl Pts',(1.74944423940117,-22.8358269579854,
12.));
#192512=CARTESIAN_POINT('Ctrl Pts',(1.74814494588491,-22.8487467728075,
0.));
#192513=CARTESIAN_POINT('Ctrl Pts',(1.74814494588491,-22.8487467728075,
12.));
#192514=CARTESIAN_POINT('Ctrl Pts',(1.74678616930663,-22.8618348580234,
0.));
#192515=CARTESIAN_POINT('Ctrl Pts',(1.74678616930663,-22.8618348580234,
12.));
#192516=CARTESIAN_POINT('Ctrl Pts',(1.74536722998199,-22.8750889101696,
0.));
#192517=CARTESIAN_POINT('Ctrl Pts',(1.74536722998199,-22.8750889101696,
12.));
#192518=CARTESIAN_POINT('Ctrl Pts',(1.74388746677702,-22.8885066803351,
0.));
#192519=CARTESIAN_POINT('Ctrl Pts',(1.74388746677702,-22.8885066803351,
12.));
#192520=CARTESIAN_POINT('Ctrl Pts',(1.74234623630079,-22.9020859716144,
0.));
#192521=CARTESIAN_POINT('Ctrl Pts',(1.74234623630079,-22.9020859716144,
12.));
#192522=CARTESIAN_POINT('Ctrl Pts',(1.74074291231056,-22.9158246373365,
0.));
#192523=CARTESIAN_POINT('Ctrl Pts',(1.74074291231056,-22.9158246373365,
12.));
#192524=CARTESIAN_POINT('Ctrl Pts',(1.73907688511664,-22.9297205792587,
0.));
#192525=CARTESIAN_POINT('Ctrl Pts',(1.73907688511664,-22.9297205792587,
12.));
#192526=CARTESIAN_POINT('Ctrl Pts',(1.73734756100038,-22.9437717457825,
0.));
#192527=CARTESIAN_POINT('Ctrl Pts',(1.73734756100038,-22.9437717457825,
12.));
#192528=CARTESIAN_POINT('Ctrl Pts',(1.73555436162771,-22.9579761301062,
0.));
#192529=CARTESIAN_POINT('Ctrl Pts',(1.73555436162771,-22.9579761301062,
12.));
#192530=CARTESIAN_POINT('Ctrl Pts',(1.73369672350817,-22.9723317685688,
0.));
#192531=CARTESIAN_POINT('Ctrl Pts',(1.73369672350817,-22.9723317685688,
12.));
#192532=CARTESIAN_POINT('Ctrl Pts',(1.73177409750193,-22.9868367391978,
0.));
#192533=CARTESIAN_POINT('Ctrl Pts',(1.73177409750193,-22.9868367391978,
12.));
#192534=CARTESIAN_POINT('Ctrl Pts',(1.72978594832137,-23.0014891601891,
0.));
#192535=CARTESIAN_POINT('Ctrl Pts',(1.72978594832137,-23.0014891601891,
12.));
#192536=CARTESIAN_POINT('Ctrl Pts',(1.72773175404702,-23.0162871884167,
0.));
#192537=CARTESIAN_POINT('Ctrl Pts',(1.72773175404702,-23.0162871884167,
12.));
#192538=CARTESIAN_POINT('Ctrl Pts',(1.72561100564033,-23.031229017888,0.));
#192539=CARTESIAN_POINT('Ctrl Pts',(1.72561100564033,-23.031229017888,12.));
#192540=CARTESIAN_POINT('Ctrl Pts',(1.72342320653731,-23.0463128785528,
0.));
#192541=CARTESIAN_POINT('Ctrl Pts',(1.72342320653731,-23.0463128785528,
12.));
#192542=CARTESIAN_POINT('Ctrl Pts',(1.7211678722598,-23.061537035156,0.));
#192543=CARTESIAN_POINT('Ctrl Pts',(1.7211678722598,-23.061537035156,12.));
#192544=CARTESIAN_POINT('Ctrl Pts',(1.71884453003027,-23.0768997860709,
0.));
#192545=CARTESIAN_POINT('Ctrl Pts',(1.71884453003027,-23.0768997860709,
12.));
#192546=CARTESIAN_POINT('Ctrl Pts',(1.71645271839311,-23.0923994621216,
0.));
#192547=CARTESIAN_POINT('Ctrl Pts',(1.71645271839311,-23.0923994621216,
12.));
#192548=CARTESIAN_POINT('Ctrl Pts',(1.71399198684724,-23.1080344254291,
0.));
#192549=CARTESIAN_POINT('Ctrl Pts',(1.71399198684724,-23.1080344254291,
12.));
#192550=CARTESIAN_POINT('Ctrl Pts',(1.71146189552192,-23.1238030684929,
0.));
#192551=CARTESIAN_POINT('Ctrl Pts',(1.71146189552192,-23.1238030684929,
12.));
#192552=CARTESIAN_POINT('Ctrl Pts',(1.70886201485459,-23.1397038132358,
0.));
#192553=CARTESIAN_POINT('Ctrl Pts',(1.70886201485459,-23.1397038132358,
12.));
#192554=CARTESIAN_POINT('Ctrl Pts',(1.70619192527846,-23.1557351100613,
0.));
#192555=CARTESIAN_POINT('Ctrl Pts',(1.70619192527846,-23.1557351100613,
12.));
#192556=CARTESIAN_POINT('Ctrl Pts',(1.70345121691259,-23.1718954368749,
0.));
#192557=CARTESIAN_POINT('Ctrl Pts',(1.70345121691259,-23.1718954368749,
12.));
#192558=CARTESIAN_POINT('Ctrl Pts',(1.70063948926987,-23.1881832981848,
0.));
#192559=CARTESIAN_POINT('Ctrl Pts',(1.70063948926987,-23.1881832981848,
12.));
#192560=CARTESIAN_POINT('Ctrl Pts',(1.69775635099425,-23.2045972243765,
0.));
#192561=CARTESIAN_POINT('Ctrl Pts',(1.69775635099425,-23.2045972243765,
12.));
#192562=CARTESIAN_POINT('Ctrl Pts',(1.69480141959945,-23.2211357709374,
0.));
#192563=CARTESIAN_POINT('Ctrl Pts',(1.69480141959945,-23.2211357709374,
12.));
#192564=CARTESIAN_POINT('Ctrl Pts',(1.69177432121716,-23.2377975177014,
0.));
#192565=CARTESIAN_POINT('Ctrl Pts',(1.69177432121716,-23.2377975177014,
12.));
#192566=CARTESIAN_POINT('Ctrl Pts',(1.6886746903491,-23.2545810680536,0.));
#192567=CARTESIAN_POINT('Ctrl Pts',(1.6886746903491,-23.2545810680536,12.));
#192568=CARTESIAN_POINT('Ctrl Pts',(1.68550216963274,-23.2714850482245,
0.));
#192569=CARTESIAN_POINT('Ctrl Pts',(1.68550216963274,-23.2714850482245,
12.));
#192570=CARTESIAN_POINT('Ctrl Pts',(1.68225640962181,-23.2885081066949,
0.));
#192571=CARTESIAN_POINT('Ctrl Pts',(1.68225640962181,-23.2885081066949,
12.));
#192572=CARTESIAN_POINT('Ctrl Pts',(1.67893706857123,-23.3056489135611,
0.));
#192573=CARTESIAN_POINT('Ctrl Pts',(1.67893706857123,-23.3056489135611,
12.));
#192574=CARTESIAN_POINT('Ctrl Pts',(1.67554381222987,-23.3229061599145,
0.));
#192575=CARTESIAN_POINT('Ctrl Pts',(1.67554381222987,-23.3229061599145,
12.));
#192576=CARTESIAN_POINT('Ctrl Pts',(1.67207631363905,-23.3402785571866,
0.));
#192577=CARTESIAN_POINT('Ctrl Pts',(1.67207631363905,-23.3402785571866,
12.));
#192578=CARTESIAN_POINT('Ctrl Pts',(1.66853425293977,-23.3577648365747,
0.));
#192579=CARTESIAN_POINT('Ctrl Pts',(1.66853425293977,-23.3577648365747,
12.));
#192580=CARTESIAN_POINT('Ctrl Pts',(1.66491731718864,-23.375363748555,0.));
#192581=CARTESIAN_POINT('Ctrl Pts',(1.66491731718864,-23.375363748555,12.));
#192582=CARTESIAN_POINT('Ctrl Pts',(1.66122520018008,-23.3930740623622,
0.));
#192583=CARTESIAN_POINT('Ctrl Pts',(1.66122520018008,-23.3930740623622,
12.));
#192584=CARTESIAN_POINT('Ctrl Pts',(1.65745760227507,-23.4108945654803,
0.));
#192585=CARTESIAN_POINT('Ctrl Pts',(1.65745760227507,-23.4108945654803,
12.));
#192586=CARTESIAN_POINT('Ctrl Pts',(1.6536142302373,-23.4288240631034,0.));
#192587=CARTESIAN_POINT('Ctrl Pts',(1.6536142302373,-23.4288240631034,12.));
#192588=CARTESIAN_POINT('Ctrl Pts',(1.64969479707339,-23.446861377656,0.));
#192589=CARTESIAN_POINT('Ctrl Pts',(1.64969479707339,-23.446861377656,12.));
#192590=CARTESIAN_POINT('Ctrl Pts',(1.64569902187608,-23.4650053483919,
0.));
#192591=CARTESIAN_POINT('Ctrl Pts',(1.64569902187608,-23.4650053483919,
12.));
#192592=CARTESIAN_POINT('Ctrl Pts',(1.64162662967524,-23.4832548309638,
0.));
#192593=CARTESIAN_POINT('Ctrl Pts',(1.64162662967524,-23.4832548309638,
12.));
#192594=CARTESIAN_POINT('Ctrl Pts',(1.63747735129474,-23.5016086970006,
0.));
#192595=CARTESIAN_POINT('Ctrl Pts',(1.63747735129474,-23.5016086970006,
12.));
#192596=CARTESIAN_POINT('Ctrl Pts',(1.63325092321731,-23.5200658336624,
0.));
#192597=CARTESIAN_POINT('Ctrl Pts',(1.63325092321731,-23.5200658336624,
12.));
#192598=CARTESIAN_POINT('Ctrl Pts',(1.62894708745231,-23.5386251432278,
0.));
#192599=CARTESIAN_POINT('Ctrl Pts',(1.62894708745231,-23.5386251432278,
12.));
#192600=CARTESIAN_POINT('Ctrl Pts',(1.62456559140071,-23.5572855427617,
0.));
#192601=CARTESIAN_POINT('Ctrl Pts',(1.62456559140071,-23.5572855427617,
12.));
#192602=CARTESIAN_POINT('Ctrl Pts',(1.62010618772869,-23.5760459637608,
0.));
#192603=CARTESIAN_POINT('Ctrl Pts',(1.62010618772869,-23.5760459637608,
12.));
#192604=CARTESIAN_POINT('Ctrl Pts',(1.61556863424697,-23.5949053517996,
0.));
#192605=CARTESIAN_POINT('Ctrl Pts',(1.61556863424697,-23.5949053517996,
12.));
#192606=CARTESIAN_POINT('Ctrl Pts',(1.61095269379773,-23.6138626661644,
0.));
#192607=CARTESIAN_POINT('Ctrl Pts',(1.61095269379773,-23.6138626661644,
12.));
#192608=CARTESIAN_POINT('Ctrl Pts',(1.60625813414666,-23.6329168794916,
0.));
#192609=CARTESIAN_POINT('Ctrl Pts',(1.60625813414666,-23.6329168794916,
12.));
#192610=CARTESIAN_POINT('Ctrl Pts',(1.60148472786588,-23.6520669774863,
0.));
#192611=CARTESIAN_POINT('Ctrl Pts',(1.60148472786588,-23.6520669774863,
12.));
#192612=CARTESIAN_POINT('Ctrl Pts',(1.59663225222458,-23.6713119586302,
0.));
#192613=CARTESIAN_POINT('Ctrl Pts',(1.59663225222458,-23.6713119586302,
12.));
#192614=CARTESIAN_POINT('Ctrl Pts',(1.59170048908631,-23.6906508338833,
0.));
#192615=CARTESIAN_POINT('Ctrl Pts',(1.59170048908631,-23.6906508338833,
12.));
#192616=CARTESIAN_POINT('Ctrl Pts',(1.58668922481222,-23.7100826263835,
0.));
#192617=CARTESIAN_POINT('Ctrl Pts',(1.58668922481222,-23.7100826263835,
12.));
#192618=CARTESIAN_POINT('Ctrl Pts',(1.58159825017362,-23.7296063711308,
0.));
#192619=CARTESIAN_POINT('Ctrl Pts',(1.58159825017362,-23.7296063711308,
12.));
#192620=CARTESIAN_POINT('Ctrl Pts',(1.57642736025251,-23.7492211147369,
0.));
#192621=CARTESIAN_POINT('Ctrl Pts',(1.57642736025251,-23.7492211147369,
12.));
#192622=CARTESIAN_POINT('Ctrl Pts',(1.57117635434412,-23.7689259151869,
0.));
#192623=CARTESIAN_POINT('Ctrl Pts',(1.57117635434412,-23.7689259151869,
12.));
#192624=CARTESIAN_POINT('Ctrl Pts',(1.56584503586844,-23.788719841588,0.));
#192625=CARTESIAN_POINT('Ctrl Pts',(1.56584503586844,-23.788719841588,12.));
#192626=CARTESIAN_POINT('Ctrl Pts',(1.56043321228631,-23.8086019739192,
0.));
#192627=CARTESIAN_POINT('Ctrl Pts',(1.56043321228631,-23.8086019739192,
12.));
#192628=CARTESIAN_POINT('Ctrl Pts',(1.55494069502627,-23.8285714027631,
0.));
#192629=CARTESIAN_POINT('Ctrl Pts',(1.55494069502627,-23.8285714027631,
12.));
#192630=CARTESIAN_POINT('Ctrl Pts',(1.5493672994053,-23.8486272290698,0.));
#192631=CARTESIAN_POINT('Ctrl Pts',(1.5493672994053,-23.8486272290698,12.));
#192632=CARTESIAN_POINT('Ctrl Pts',(1.54371284453977,-23.8687685639635,
0.));
#192633=CARTESIAN_POINT('Ctrl Pts',(1.54371284453977,-23.8687685639635,
12.));
#192634=CARTESIAN_POINT('Ctrl Pts',(1.53797715326748,-23.8889945285313,
0.));
#192635=CARTESIAN_POINT('Ctrl Pts',(1.53797715326748,-23.8889945285313,
12.));
#192636=CARTESIAN_POINT('Ctrl Pts',(1.53216005207462,-23.9093042536119,
0.));
#192637=CARTESIAN_POINT('Ctrl Pts',(1.53216005207462,-23.9093042536119,
12.));
#192638=CARTESIAN_POINT('Ctrl Pts',(1.52626137103039,-23.9296968795761,
0.));
#192639=CARTESIAN_POINT('Ctrl Pts',(1.52626137103039,-23.9296968795761,
12.));
#192640=CARTESIAN_POINT('Ctrl Pts',(1.52028094372806,-23.9501715561038,
0.));
#192641=CARTESIAN_POINT('Ctrl Pts',(1.52028094372806,-23.9501715561038,
12.));
#192642=CARTESIAN_POINT('Ctrl Pts',(1.51421860720628,-23.9707274420145,
0.));
#192643=CARTESIAN_POINT('Ctrl Pts',(1.51421860720628,-23.9707274420145,
12.));
#192644=CARTESIAN_POINT('Ctrl Pts',(1.50807420187702,-23.991363705093,0.));
#192645=CARTESIAN_POINT('Ctrl Pts',(1.50807420187702,-23.991363705093,12.));
#192646=CARTESIAN_POINT('Ctrl Pts',(1.50184757146099,-24.0120795219086,
0.));
#192647=CARTESIAN_POINT('Ctrl Pts',(1.50184757146099,-24.0120795219086,
12.));
#192648=CARTESIAN_POINT('Ctrl Pts',(1.49553856292798,-24.0328740776331,
0.));
#192649=CARTESIAN_POINT('Ctrl Pts',(1.49553856292798,-24.0328740776331,
12.));
#192650=CARTESIAN_POINT('Ctrl Pts',(1.48914702644883,-24.053746565843,0.));
#192651=CARTESIAN_POINT('Ctrl Pts',(1.48914702644883,-24.053746565843,12.));
#192652=CARTESIAN_POINT('Ctrl Pts',(1.4826728153368,-24.074696188353,0.));
#192653=CARTESIAN_POINT('Ctrl Pts',(1.4826728153368,-24.074696188353,12.));
#192654=CARTESIAN_POINT('Ctrl Pts',(1.47611578597741,-24.0957221550782,
0.));
#192655=CARTESIAN_POINT('Ctrl Pts',(1.47611578597741,-24.0957221550782,
12.));
#192656=CARTESIAN_POINT('Ctrl Pts',(1.46947579776991,-24.1168236838827,
0.));
#192657=CARTESIAN_POINT('Ctrl Pts',(1.46947579776991,-24.1168236838827,
12.));
#192658=CARTESIAN_POINT('Ctrl Pts',(1.46275271307398,-24.1380000004272,
0.));
#192659=CARTESIAN_POINT('Ctrl Pts',(1.46275271307398,-24.1380000004272,
12.));
#192660=CARTESIAN_POINT('Ctrl Pts',(1.45594639716314,-24.1592503380105,
0.));
#192661=CARTESIAN_POINT('Ctrl Pts',(1.45594639716314,-24.1592503380105,
12.));
#192662=CARTESIAN_POINT('Ctrl Pts',(1.4490567181872,-24.1805739374033,0.));
#192663=CARTESIAN_POINT('Ctrl Pts',(1.4490567181872,-24.1805739374033,12.));
#192664=CARTESIAN_POINT('Ctrl Pts',(1.44208354711074,-24.2019700467214,
0.));
#192665=CARTESIAN_POINT('Ctrl Pts',(1.44208354711074,-24.2019700467214,
12.));
#192666=CARTESIAN_POINT('Ctrl Pts',(1.43502675765502,-24.2234379212978,
0.));
#192667=CARTESIAN_POINT('Ctrl Pts',(1.43502675765502,-24.2234379212978,
12.));
#192668=CARTESIAN_POINT('Ctrl Pts',(1.42788622624851,-24.2449768235485,
0.));
#192669=CARTESIAN_POINT('Ctrl Pts',(1.42788622624851,-24.2449768235485,
12.));
#192670=CARTESIAN_POINT('Ctrl Pts',(1.42066183198252,-24.2665860228357,
0.));
#192671=CARTESIAN_POINT('Ctrl Pts',(1.42066183198252,-24.2665860228357,
12.));
#192672=CARTESIAN_POINT('Ctrl Pts',(1.41335345657684,-24.2882647953214,
0.));
#192673=CARTESIAN_POINT('Ctrl Pts',(1.41335345657684,-24.2882647953214,
12.));
#192674=CARTESIAN_POINT('Ctrl Pts',(1.4059609843434,-24.3100124238316,0.));
#192675=CARTESIAN_POINT('Ctrl Pts',(1.4059609843434,-24.3100124238316,12.));
#192676=CARTESIAN_POINT('Ctrl Pts',(1.3984843021281,-24.3318281977647,0.));
#192677=CARTESIAN_POINT('Ctrl Pts',(1.3984843021281,-24.3318281977647,12.));
#192678=CARTESIAN_POINT('Ctrl Pts',(1.3909232992639,-24.3537114129877,0.));
#192679=CARTESIAN_POINT('Ctrl Pts',(1.3909232992639,-24.3537114129877,12.));
#192680=CARTESIAN_POINT('Ctrl Pts',(1.38327786752998,-24.37566137173,0.));
#192681=CARTESIAN_POINT('Ctrl Pts',(1.38327786752998,-24.37566137173,12.));
#192682=CARTESIAN_POINT('Ctrl Pts',(1.37554790111607,-24.3976773824731,
0.));
#192683=CARTESIAN_POINT('Ctrl Pts',(1.37554790111607,-24.3976773824731,
12.));
#192684=CARTESIAN_POINT('Ctrl Pts',(1.36773329659954,-24.4197587598337,
0.));
#192685=CARTESIAN_POINT('Ctrl Pts',(1.36773329659954,-24.4197587598337,
12.));
#192686=CARTESIAN_POINT('Ctrl Pts',(1.35983395290624,-24.4419048244524,
0.));
#192687=CARTESIAN_POINT('Ctrl Pts',(1.35983395290624,-24.4419048244524,
12.));
#192688=CARTESIAN_POINT('Ctrl Pts',(1.35184977125644,-24.4641149028894,
0.));
#192689=CARTESIAN_POINT('Ctrl Pts',(1.35184977125644,-24.4641149028894,
12.));
#192690=CARTESIAN_POINT('Ctrl Pts',(1.34378065512335,-24.4863883275135,
0.));
#192691=CARTESIAN_POINT('Ctrl Pts',(1.34378065512335,-24.4863883275135,
12.));
#192692=CARTESIAN_POINT('Ctrl Pts',(1.33562651019684,-24.5087244363856,
0.));
#192693=CARTESIAN_POINT('Ctrl Pts',(1.33562651019684,-24.5087244363856,
12.));
#192694=CARTESIAN_POINT('Ctrl Pts',(1.32738724435326,-24.5311225731434,
0.));
#192695=CARTESIAN_POINT('Ctrl Pts',(1.32738724435326,-24.5311225731434,
12.));
#192696=CARTESIAN_POINT('Ctrl Pts',(1.31906276763669,-24.5535820868671,
0.));
#192697=CARTESIAN_POINT('Ctrl Pts',(1.31906276763669,-24.5535820868671,
12.));
#192698=CARTESIAN_POINT('Ctrl Pts',(1.31065299222023,-24.576102332018,0.));
#192699=CARTESIAN_POINT('Ctrl Pts',(1.31065299222023,-24.576102332018,12.));
#192700=CARTESIAN_POINT('Ctrl Pts',(1.30215783236363,-24.5986826684025,
0.));
#192701=CARTESIAN_POINT('Ctrl Pts',(1.30215783236363,-24.5986826684025,
12.));
#192702=CARTESIAN_POINT('Ctrl Pts',(1.29357720438107,-24.6213224611228,
0.));
#192703=CARTESIAN_POINT('Ctrl Pts',(1.29357720438107,-24.6213224611228,
12.));
#192704=CARTESIAN_POINT('Ctrl Pts',(1.28491102661513,-24.6440210805278,
0.));
#192705=CARTESIAN_POINT('Ctrl Pts',(1.28491102661513,-24.6440210805278,
12.));
#192706=CARTESIAN_POINT('Ctrl Pts',(1.2761592194164,-24.666777902156,0.));
#192707=CARTESIAN_POINT('Ctrl Pts',(1.2761592194164,-24.666777902156,12.));
#192708=CARTESIAN_POINT('Ctrl Pts',(1.26732170513497,-24.6895923066837,
0.));
#192709=CARTESIAN_POINT('Ctrl Pts',(1.26732170513497,-24.6895923066837,
12.));
#192710=CARTESIAN_POINT('Ctrl Pts',(1.25839840807414,-24.7124636797895,
0.));
#192711=CARTESIAN_POINT('Ctrl Pts',(1.25839840807414,-24.7124636797895,
12.));
#192712=CARTESIAN_POINT('Ctrl Pts',(1.24938925444323,-24.7353914120012,
0.));
#192713=CARTESIAN_POINT('Ctrl Pts',(1.24938925444323,-24.7353914120012,
12.));
#192714=CARTESIAN_POINT('Ctrl Pts',(1.24029417231987,-24.7583748985439,
0.));
#192715=CARTESIAN_POINT('Ctrl Pts',(1.24029417231987,-24.7583748985439,
12.));
#192716=CARTESIAN_POINT('Ctrl Pts',(1.23111309161843,-24.78141353918,0.));
#192717=CARTESIAN_POINT('Ctrl Pts',(1.23111309161843,-24.78141353918,12.));
#192718=CARTESIAN_POINT('Ctrl Pts',(1.22184594406526,-24.8045067380536,
0.));
#192719=CARTESIAN_POINT('Ctrl Pts',(1.22184594406526,-24.8045067380536,
12.));
#192720=CARTESIAN_POINT('Ctrl Pts',(1.21249266318205,-24.8276539035092,
0.));
#192721=CARTESIAN_POINT('Ctrl Pts',(1.21249266318205,-24.8276539035092,
12.));
#192722=CARTESIAN_POINT('Ctrl Pts',(1.20305318426015,-24.8508544481973,
0.));
#192723=CARTESIAN_POINT('Ctrl Pts',(1.20305318426015,-24.8508544481973,
12.));
#192724=CARTESIAN_POINT('Ctrl Pts',(1.19352744434059,-24.8741077892074,
0.));
#192725=CARTESIAN_POINT('Ctrl Pts',(1.19352744434059,-24.8741077892074,
12.));
#192726=CARTESIAN_POINT('Ctrl Pts',(1.18391538220098,-24.8974133481829,
0.));
#192727=CARTESIAN_POINT('Ctrl Pts',(1.18391538220098,-24.8974133481829,
12.));
#192728=CARTESIAN_POINT('Ctrl Pts',(1.17421693835039,-24.9207705514449,
0.));
#192729=CARTESIAN_POINT('Ctrl Pts',(1.17421693835039,-24.9207705514449,
12.));
#192730=CARTESIAN_POINT('Ctrl Pts',(1.16443205502852,-24.9441788300932,
0.));
#192731=CARTESIAN_POINT('Ctrl Pts',(1.16443205502852,-24.9441788300932,
12.));
#192732=CARTESIAN_POINT('Ctrl Pts',(1.15456067621894,-24.9676376201501,
0.));
#192733=CARTESIAN_POINT('Ctrl Pts',(1.15456067621894,-24.9676376201501,
12.));
#192734=CARTESIAN_POINT('Ctrl Pts',(1.14460274758206,-24.9911463621431,
0.));
#192735=CARTESIAN_POINT('Ctrl Pts',(1.14460274758206,-24.9911463621431,
12.));
#192736=CARTESIAN_POINT('Ctrl Pts',(1.13455821638535,-25.0147045006193,
0.));
#192737=CARTESIAN_POINT('Ctrl Pts',(1.13455821638535,-25.0147045006193,
12.));
#192738=CARTESIAN_POINT('Ctrl Pts',(1.12442703144455,-25.0383114836898,
0.));
#192739=CARTESIAN_POINT('Ctrl Pts',(1.12442703144455,-25.0383114836898,
12.));
#192740=CARTESIAN_POINT('Ctrl Pts',(1.1142091430689,-25.0619667625336,0.));
#192741=CARTESIAN_POINT('Ctrl Pts',(1.1142091430689,-25.0619667625336,12.));
#192742=CARTESIAN_POINT('Ctrl Pts',(1.1039045030174,-25.085669790968,0.));
#192743=CARTESIAN_POINT('Ctrl Pts',(1.1039045030174,-25.085669790968,12.));
#192744=CARTESIAN_POINT('Ctrl Pts',(1.09351306445299,-25.1094200248448,
0.));
#192745=CARTESIAN_POINT('Ctrl Pts',(1.09351306445299,-25.1094200248448,
12.));
#192746=CARTESIAN_POINT('Ctrl Pts',(1.08303478197174,-25.1332169227415,
0.));
#192747=CARTESIAN_POINT('Ctrl Pts',(1.08303478197174,-25.1332169227415,
12.));
#192748=CARTESIAN_POINT('Ctrl Pts',(1.07246961165459,-25.1570599469311,
0.));
#192749=CARTESIAN_POINT('Ctrl Pts',(1.07246961165459,-25.1570599469311,
12.));
#192750=CARTESIAN_POINT('Ctrl Pts',(1.06181751111754,-25.1809485642191,
0.));
#192751=CARTESIAN_POINT('Ctrl Pts',(1.06181751111754,-25.1809485642191,
12.));
#192752=CARTESIAN_POINT('Ctrl Pts',(1.05107843957925,-25.2048822469027,
0.));
#192753=CARTESIAN_POINT('Ctrl Pts',(1.05107843957925,-25.2048822469027,
12.));
#192754=CARTESIAN_POINT('Ctrl Pts',(1.04025235791514,-25.2288604735087,
0.));
#192755=CARTESIAN_POINT('Ctrl Pts',(1.04025235791514,-25.2288604735087,
12.));
#192756=CARTESIAN_POINT('Ctrl Pts',(1.0293392287683,-25.2528827300427,0.));
#192757=CARTESIAN_POINT('Ctrl Pts',(1.0293392287683,-25.2528827300427,12.));
#192758=CARTESIAN_POINT('Ctrl Pts',(1.01833901642272,-25.2769485087268,
0.));
#192759=CARTESIAN_POINT('Ctrl Pts',(1.01833901642272,-25.2769485087268,
12.));
#192760=CARTESIAN_POINT('Ctrl Pts',(1.00725168656933,-25.3010573055557,
0.));
#192761=CARTESIAN_POINT('Ctrl Pts',(1.00725168656933,-25.3010573055557,
12.));
#192762=CARTESIAN_POINT('Ctrl Pts',(0.996077206120918,-25.3252086182976,
0.));
#192763=CARTESIAN_POINT('Ctrl Pts',(0.996077206120918,-25.3252086182976,
12.));
#192764=CARTESIAN_POINT('Ctrl Pts',(0.984815543004088,-25.3494019441444,
0.));
#192765=CARTESIAN_POINT('Ctrl Pts',(0.984815543004088,-25.3494019441444,
12.));
#192766=CARTESIAN_POINT('Ctrl Pts',(0.973466666000047,-25.3736367778842,
0.));
#192767=CARTESIAN_POINT('Ctrl Pts',(0.973466666000047,-25.3736367778842,
12.));
#192768=CARTESIAN_POINT('Ctrl Pts',(0.962030544502801,-25.3979126089155,
0.));
#192769=CARTESIAN_POINT('Ctrl Pts',(0.962030544502801,-25.3979126089155,
12.));
#192770=CARTESIAN_POINT('Ctrl Pts',(0.950507148596967,-25.4222289223155,
0.));
#192771=CARTESIAN_POINT('Ctrl Pts',(0.950507148596967,-25.4222289223155,
12.));
#192772=CARTESIAN_POINT('Ctrl Pts',(0.938896449495631,-25.4465852044835,
0.));
#192773=CARTESIAN_POINT('Ctrl Pts',(0.938896449495631,-25.4465852044835,
12.));
#192774=CARTESIAN_POINT('Ctrl Pts',(0.927198419885603,-25.4709809474996,
0.));
#192775=CARTESIAN_POINT('Ctrl Pts',(0.927198419885603,-25.4709809474996,
12.));
#192776=CARTESIAN_POINT('Ctrl Pts',(0.915413034335331,-25.4954156541787,
0.));
#192777=CARTESIAN_POINT('Ctrl Pts',(0.915413034335331,-25.4954156541787,
12.));
#192778=CARTESIAN_POINT('Ctrl Pts',(0.903540269651152,-25.5198888424195,
0.));
#192779=CARTESIAN_POINT('Ctrl Pts',(0.903540269651152,-25.5198888424195,
12.));
#192780=CARTESIAN_POINT('Ctrl Pts',(0.891580105349464,-25.5444000508223,
0.));
#192781=CARTESIAN_POINT('Ctrl Pts',(0.891580105349464,-25.5444000508223,
12.));
#192782=CARTESIAN_POINT('Ctrl Pts',(0.879532523835088,-25.568948840818,
0.));
#192783=CARTESIAN_POINT('Ctrl Pts',(0.879532523835088,-25.568948840818,
12.));
#192784=CARTESIAN_POINT('Ctrl Pts',(0.867397509339468,-25.5935347843616,
0.));
#192785=CARTESIAN_POINT('Ctrl Pts',(0.867397509339468,-25.5935347843616,
12.));
#192786=CARTESIAN_POINT('Ctrl Pts',(0.855175047037614,-25.618157453608,
0.));
#192787=CARTESIAN_POINT('Ctrl Pts',(0.855175047037614,-25.618157453608,
12.));
#192788=CARTESIAN_POINT('Ctrl Pts',(0.842865122121542,-25.6428164100078,
0.));
#192789=CARTESIAN_POINT('Ctrl Pts',(0.842865122121542,-25.6428164100078,
12.));
#192790=CARTESIAN_POINT('Ctrl Pts',(0.830467718864366,-25.6675111931957,
0.));
#192791=CARTESIAN_POINT('Ctrl Pts',(0.830467718864366,-25.6675111931957,
12.));
#192792=CARTESIAN_POINT('Ctrl Pts',(0.817982819786718,-25.6922413110172,
0.));
#192793=CARTESIAN_POINT('Ctrl Pts',(0.817982819786718,-25.6922413110172,
12.));
#192794=CARTESIAN_POINT('Ctrl Pts',(0.805410404552592,-25.7170062262474,
0.));
#192795=CARTESIAN_POINT('Ctrl Pts',(0.805410404552592,-25.7170062262474,
12.));
#192796=CARTESIAN_POINT('Ctrl Pts',(0.792750451613533,-25.7418053757671,
0.));
#192797=CARTESIAN_POINT('Ctrl Pts',(0.792750451613533,-25.7418053757671,
12.));
#192798=CARTESIAN_POINT('Ctrl Pts',(0.780002940289024,-25.7666381946871,
0.));
#192799=CARTESIAN_POINT('Ctrl Pts',(0.780002940289024,-25.7666381946871,
12.));
#192800=CARTESIAN_POINT('Ctrl Pts',(0.767167852648638,-25.7915041383304,
0.));
#192801=CARTESIAN_POINT('Ctrl Pts',(0.767167852648638,-25.7915041383304,
12.));
#192802=CARTESIAN_POINT('Ctrl Pts',(0.754245175608287,-25.816402705995,
0.));
#192803=CARTESIAN_POINT('Ctrl Pts',(0.754245175608287,-25.816402705995,
12.));
#192804=CARTESIAN_POINT('Ctrl Pts',(0.741234902664695,-25.841333461908,
0.));
#192805=CARTESIAN_POINT('Ctrl Pts',(0.741234902664695,-25.841333461908,
12.));
#192806=CARTESIAN_POINT('Ctrl Pts',(0.728137036485876,-25.8662960624285,
0.));
#192807=CARTESIAN_POINT('Ctrl Pts',(0.728137036485876,-25.8662960624285,
12.));
#192808=CARTESIAN_POINT('Ctrl Pts',(0.714951588533752,-25.8912902615141,
0.));
#192809=CARTESIAN_POINT('Ctrl Pts',(0.714951588533752,-25.8912902615141,
12.));
#192810=CARTESIAN_POINT('Ctrl Pts',(0.701678575236601,-25.9163158909645,
0.));
#192811=CARTESIAN_POINT('Ctrl Pts',(0.701678575236601,-25.9163158909645,
12.));
#192812=CARTESIAN_POINT('Ctrl Pts',(0.688318015065675,-25.941372847213,
0.));
#192813=CARTESIAN_POINT('Ctrl Pts',(0.688318015065675,-25.941372847213,
12.));
#192814=CARTESIAN_POINT('Ctrl Pts',(0.677559543215902,-25.9614434298092,
0.));
#192815=CARTESIAN_POINT('Ctrl Pts',(0.677559543215902,-25.9614434298092,
12.));
#192816=CARTESIAN_POINT('Ctrl Pts',(0.669451306784414,-25.9765104298171,
0.));
#192817=CARTESIAN_POINT('Ctrl Pts',(0.669451306784414,-25.9765104298171,
12.));
#192818=CARTESIAN_POINT('Ctrl Pts',(0.664028313188911,-25.9865613464809,
0.));
#192819=CARTESIAN_POINT('Ctrl Pts',(0.664028313188911,-25.9865613464809,
12.));
#192820=CARTESIAN_POINT('Ctrl Pts',(0.66131244073089,-25.991588367311,0.));
#192821=CARTESIAN_POINT('Ctrl Pts',(0.66131244073089,-25.991588367311,12.));
#192822=CARTESIAN_POINT('',(0.66131244073089,-25.991588367311,0.));
#192823=CARTESIAN_POINT('Ctrl Pts',(1.76341220531179,-22.4835757167854,
0.));
#192824=CARTESIAN_POINT('Ctrl Pts',(1.76341415538764,-22.483581992979,0.));
#192825=CARTESIAN_POINT('Ctrl Pts',(1.7634206426357,-22.4836387052232,0.));
#192826=CARTESIAN_POINT('Ctrl Pts',(1.76343813434565,-22.483856251707,0.));
#192827=CARTESIAN_POINT('Ctrl Pts',(1.76347698284791,-22.4844112933129,
0.));
#192828=CARTESIAN_POINT('Ctrl Pts',(1.76355076045546,-22.4855446605991,
0.));
#192829=CARTESIAN_POINT('Ctrl Pts',(1.76364784232963,-22.4871115206571,
0.));
#192830=CARTESIAN_POINT('Ctrl Pts',(1.76376424879504,-22.4890991659478,
0.));
#192831=CARTESIAN_POINT('Ctrl Pts',(1.76389475965723,-22.4914909094908,
0.));
#192832=CARTESIAN_POINT('Ctrl Pts',(1.764033938803,-22.4942693792449,0.));
#192833=CARTESIAN_POINT('Ctrl Pts',(1.76417731243462,-22.4974203063191,
0.));
#192834=CARTESIAN_POINT('Ctrl Pts',(1.76432160068725,-22.5009332677316,
0.));
#192835=CARTESIAN_POINT('Ctrl Pts',(1.76446408210366,-22.5047996391978,
0.));
#192836=CARTESIAN_POINT('Ctrl Pts',(1.76460218257323,-22.5090112700212,
0.));
#192837=CARTESIAN_POINT('Ctrl Pts',(1.76473303281158,-22.5135590569554,
0.));
#192838=CARTESIAN_POINT('Ctrl Pts',(1.76485369319896,-22.5184336670207,
0.));
#192839=CARTESIAN_POINT('Ctrl Pts',(1.76496128643369,-22.5236259635515,
0.));
#192840=CARTESIAN_POINT('Ctrl Pts',(1.76505320262751,-22.529127665298,0.));
#192841=CARTESIAN_POINT('Ctrl Pts',(1.7651271156325,-22.5349313983571,0.));
#192842=CARTESIAN_POINT('Ctrl Pts',(1.76518087841492,-22.5410303590891,
0.));
#192843=CARTESIAN_POINT('Ctrl Pts',(1.76521245524047,-22.5474180954006,
0.));
#192844=CARTESIAN_POINT('Ctrl Pts',(1.76521983384062,-22.5540882235837,
0.));
#192845=CARTESIAN_POINT('Ctrl Pts',(1.76520104500449,-22.5610344912501,
0.));
#192846=CARTESIAN_POINT('Ctrl Pts',(1.76515418518829,-22.5682508499873,
0.));
#192847=CARTESIAN_POINT('Ctrl Pts',(1.76507744026747,-22.5757315316355,
0.));
#192848=CARTESIAN_POINT('Ctrl Pts',(1.76496910283088,-22.5834711038024,
0.));
#192849=CARTESIAN_POINT('Ctrl Pts',(1.76482755288411,-22.5914644078106,
0.));
#192850=CARTESIAN_POINT('Ctrl Pts',(1.76465124413556,-22.5997065145638,
0.));
#192851=CARTESIAN_POINT('Ctrl Pts',(1.76443868648015,-22.6081926681342,
0.));
#192852=CARTESIAN_POINT('Ctrl Pts',(1.76418843543739,-22.6169182517693,
0.));
#192853=CARTESIAN_POINT('Ctrl Pts',(1.76389909571402,-22.6258787994847,
0.));
#192854=CARTESIAN_POINT('Ctrl Pts',(1.76356932176272,-22.635069997936,0.));
#192855=CARTESIAN_POINT('Ctrl Pts',(1.76319782013913,-22.6444876940425,
0.));
#192856=CARTESIAN_POINT('Ctrl Pts',(1.76278334912559,-22.6541278938413,
0.));
#192857=CARTESIAN_POINT('Ctrl Pts',(1.76232471392567,-22.6639867471756,
0.));
#192858=CARTESIAN_POINT('Ctrl Pts',(1.76182076289525,-22.6740605356699,
0.));
#192859=CARTESIAN_POINT('Ctrl Pts',(1.76127038310612,-22.6843456585245,
0.));
#192860=CARTESIAN_POINT('Ctrl Pts',(1.76067249704884,-22.6948386219843,
0.));
#192861=CARTESIAN_POINT('Ctrl Pts',(1.76002606202398,-22.7055360375481,
0.));
#192862=CARTESIAN_POINT('Ctrl Pts',(1.75933006905924,-22.7164346186007,
0.));
#192863=CARTESIAN_POINT('Ctrl Pts',(1.75858354204634,-22.7275311777305,
0.));
#192864=CARTESIAN_POINT('Ctrl Pts',(1.75778553673249,-22.7388226235565,
0.));
#192865=CARTESIAN_POINT('Ctrl Pts',(1.75693513908911,-22.7503059556455,
0.));
#192866=CARTESIAN_POINT('Ctrl Pts',(1.7560314637164,-22.7619782595013,0.));
#192867=CARTESIAN_POINT('Ctrl Pts',(1.75507365227127,-22.7738367016115,
0.));
#192868=CARTESIAN_POINT('Ctrl Pts',(1.75406087182929,-22.7858785242358,
0.));
#192869=CARTESIAN_POINT('Ctrl Pts',(1.75299231391461,-22.7981010424312,
0.));
#192870=CARTESIAN_POINT('Ctrl Pts',(1.75186719365589,-22.8105016414712,
0.));
#192871=CARTESIAN_POINT('Ctrl Pts',(1.75068474890883,-22.8230777741285,
0.));
#192872=CARTESIAN_POINT('Ctrl Pts',(1.74944423940117,-22.8358269579854,
0.));
#192873=CARTESIAN_POINT('Ctrl Pts',(1.74814494588491,-22.8487467728075,
0.));
#192874=CARTESIAN_POINT('Ctrl Pts',(1.74678616930663,-22.8618348580234,
0.));
#192875=CARTESIAN_POINT('Ctrl Pts',(1.74536722998199,-22.8750889101696,
0.));
#192876=CARTESIAN_POINT('Ctrl Pts',(1.74388746677702,-22.8885066803351,
0.));
#192877=CARTESIAN_POINT('Ctrl Pts',(1.74234623630079,-22.9020859716144,
0.));
#192878=CARTESIAN_POINT('Ctrl Pts',(1.74074291231056,-22.9158246373365,
0.));
#192879=CARTESIAN_POINT('Ctrl Pts',(1.73907688511664,-22.9297205792587,
0.));
#192880=CARTESIAN_POINT('Ctrl Pts',(1.73734756100038,-22.9437717457825,
0.));
#192881=CARTESIAN_POINT('Ctrl Pts',(1.73555436162771,-22.9579761301062,
0.));
#192882=CARTESIAN_POINT('Ctrl Pts',(1.73369672350817,-22.9723317685688,
0.));
#192883=CARTESIAN_POINT('Ctrl Pts',(1.73177409750193,-22.9868367391978,
0.));
#192884=CARTESIAN_POINT('Ctrl Pts',(1.72978594832137,-23.0014891601891,
0.));
#192885=CARTESIAN_POINT('Ctrl Pts',(1.72773175404702,-23.0162871884167,
0.));
#192886=CARTESIAN_POINT('Ctrl Pts',(1.72561100564033,-23.031229017888,0.));
#192887=CARTESIAN_POINT('Ctrl Pts',(1.72342320653731,-23.0463128785528,
0.));
#192888=CARTESIAN_POINT('Ctrl Pts',(1.7211678722598,-23.061537035156,0.));
#192889=CARTESIAN_POINT('Ctrl Pts',(1.71884453003027,-23.0768997860709,
0.));
#192890=CARTESIAN_POINT('Ctrl Pts',(1.71645271839311,-23.0923994621216,
0.));
#192891=CARTESIAN_POINT('Ctrl Pts',(1.71399198684724,-23.1080344254291,
0.));
#192892=CARTESIAN_POINT('Ctrl Pts',(1.71146189552192,-23.1238030684929,
0.));
#192893=CARTESIAN_POINT('Ctrl Pts',(1.70886201485459,-23.1397038132358,
0.));
#192894=CARTESIAN_POINT('Ctrl Pts',(1.70619192527846,-23.1557351100613,
0.));
#192895=CARTESIAN_POINT('Ctrl Pts',(1.70345121691259,-23.1718954368749,
0.));
#192896=CARTESIAN_POINT('Ctrl Pts',(1.70063948926987,-23.1881832981848,
0.));
#192897=CARTESIAN_POINT('Ctrl Pts',(1.69775635099425,-23.2045972243765,
0.));
#192898=CARTESIAN_POINT('Ctrl Pts',(1.69480141959945,-23.2211357709374,
0.));
#192899=CARTESIAN_POINT('Ctrl Pts',(1.69177432121716,-23.2377975177014,
0.));
#192900=CARTESIAN_POINT('Ctrl Pts',(1.6886746903491,-23.2545810680536,0.));
#192901=CARTESIAN_POINT('Ctrl Pts',(1.68550216963274,-23.2714850482245,
0.));
#192902=CARTESIAN_POINT('Ctrl Pts',(1.68225640962181,-23.2885081066949,
0.));
#192903=CARTESIAN_POINT('Ctrl Pts',(1.67893706857123,-23.3056489135611,
0.));
#192904=CARTESIAN_POINT('Ctrl Pts',(1.67554381222987,-23.3229061599145,
0.));
#192905=CARTESIAN_POINT('Ctrl Pts',(1.67207631363905,-23.3402785571866,
0.));
#192906=CARTESIAN_POINT('Ctrl Pts',(1.66853425293977,-23.3577648365747,
0.));
#192907=CARTESIAN_POINT('Ctrl Pts',(1.66491731718864,-23.375363748555,0.));
#192908=CARTESIAN_POINT('Ctrl Pts',(1.66122520018008,-23.3930740623622,
0.));
#192909=CARTESIAN_POINT('Ctrl Pts',(1.65745760227507,-23.4108945654803,
0.));
#192910=CARTESIAN_POINT('Ctrl Pts',(1.6536142302373,-23.4288240631034,0.));
#192911=CARTESIAN_POINT('Ctrl Pts',(1.64969479707339,-23.446861377656,0.));
#192912=CARTESIAN_POINT('Ctrl Pts',(1.64569902187608,-23.4650053483919,
0.));
#192913=CARTESIAN_POINT('Ctrl Pts',(1.64162662967524,-23.4832548309638,
0.));
#192914=CARTESIAN_POINT('Ctrl Pts',(1.63747735129474,-23.5016086970006,
0.));
#192915=CARTESIAN_POINT('Ctrl Pts',(1.63325092321731,-23.5200658336624,
0.));
#192916=CARTESIAN_POINT('Ctrl Pts',(1.62894708745231,-23.5386251432278,
0.));
#192917=CARTESIAN_POINT('Ctrl Pts',(1.62456559140071,-23.5572855427617,
0.));
#192918=CARTESIAN_POINT('Ctrl Pts',(1.62010618772869,-23.5760459637608,
0.));
#192919=CARTESIAN_POINT('Ctrl Pts',(1.61556863424697,-23.5949053517996,
0.));
#192920=CARTESIAN_POINT('Ctrl Pts',(1.61095269379773,-23.6138626661644,
0.));
#192921=CARTESIAN_POINT('Ctrl Pts',(1.60625813414666,-23.6329168794916,
0.));
#192922=CARTESIAN_POINT('Ctrl Pts',(1.60148472786588,-23.6520669774863,
0.));
#192923=CARTESIAN_POINT('Ctrl Pts',(1.59663225222458,-23.6713119586302,
0.));
#192924=CARTESIAN_POINT('Ctrl Pts',(1.59170048908631,-23.6906508338833,
0.));
#192925=CARTESIAN_POINT('Ctrl Pts',(1.58668922481222,-23.7100826263835,
0.));
#192926=CARTESIAN_POINT('Ctrl Pts',(1.58159825017362,-23.7296063711308,
0.));
#192927=CARTESIAN_POINT('Ctrl Pts',(1.57642736025251,-23.7492211147369,
0.));
#192928=CARTESIAN_POINT('Ctrl Pts',(1.57117635434412,-23.7689259151869,
0.));
#192929=CARTESIAN_POINT('Ctrl Pts',(1.56584503586844,-23.788719841588,0.));
#192930=CARTESIAN_POINT('Ctrl Pts',(1.56043321228631,-23.8086019739192,
0.));
#192931=CARTESIAN_POINT('Ctrl Pts',(1.55494069502627,-23.8285714027631,
0.));
#192932=CARTESIAN_POINT('Ctrl Pts',(1.5493672994053,-23.8486272290698,0.));
#192933=CARTESIAN_POINT('Ctrl Pts',(1.54371284453977,-23.8687685639635,
0.));
#192934=CARTESIAN_POINT('Ctrl Pts',(1.53797715326748,-23.8889945285313,
0.));
#192935=CARTESIAN_POINT('Ctrl Pts',(1.53216005207462,-23.9093042536119,
0.));
#192936=CARTESIAN_POINT('Ctrl Pts',(1.52626137103039,-23.9296968795761,
0.));
#192937=CARTESIAN_POINT('Ctrl Pts',(1.52028094372806,-23.9501715561038,
0.));
#192938=CARTESIAN_POINT('Ctrl Pts',(1.51421860720628,-23.9707274420145,
0.));
#192939=CARTESIAN_POINT('Ctrl Pts',(1.50807420187702,-23.991363705093,0.));
#192940=CARTESIAN_POINT('Ctrl Pts',(1.50184757146099,-24.0120795219086,
0.));
#192941=CARTESIAN_POINT('Ctrl Pts',(1.49553856292798,-24.0328740776331,
0.));
#192942=CARTESIAN_POINT('Ctrl Pts',(1.48914702644883,-24.053746565843,0.));
#192943=CARTESIAN_POINT('Ctrl Pts',(1.4826728153368,-24.074696188353,0.));
#192944=CARTESIAN_POINT('Ctrl Pts',(1.47611578597741,-24.0957221550782,
0.));
#192945=CARTESIAN_POINT('Ctrl Pts',(1.46947579776991,-24.1168236838827,
0.));
#192946=CARTESIAN_POINT('Ctrl Pts',(1.46275271307398,-24.1380000004272,
0.));
#192947=CARTESIAN_POINT('Ctrl Pts',(1.45594639716314,-24.1592503380105,
0.));
#192948=CARTESIAN_POINT('Ctrl Pts',(1.4490567181872,-24.1805739374033,0.));
#192949=CARTESIAN_POINT('Ctrl Pts',(1.44208354711074,-24.2019700467214,
0.));
#192950=CARTESIAN_POINT('Ctrl Pts',(1.43502675765502,-24.2234379212978,
0.));
#192951=CARTESIAN_POINT('Ctrl Pts',(1.42788622624851,-24.2449768235485,
0.));
#192952=CARTESIAN_POINT('Ctrl Pts',(1.42066183198252,-24.2665860228357,
0.));
#192953=CARTESIAN_POINT('Ctrl Pts',(1.41335345657684,-24.2882647953214,
0.));
#192954=CARTESIAN_POINT('Ctrl Pts',(1.4059609843434,-24.3100124238316,0.));
#192955=CARTESIAN_POINT('Ctrl Pts',(1.3984843021281,-24.3318281977647,0.));
#192956=CARTESIAN_POINT('Ctrl Pts',(1.3909232992639,-24.3537114129877,0.));
#192957=CARTESIAN_POINT('Ctrl Pts',(1.38327786752998,-24.37566137173,0.));
#192958=CARTESIAN_POINT('Ctrl Pts',(1.37554790111607,-24.3976773824731,
0.));
#192959=CARTESIAN_POINT('Ctrl Pts',(1.36773329659954,-24.4197587598337,
0.));
#192960=CARTESIAN_POINT('Ctrl Pts',(1.35983395290624,-24.4419048244524,
0.));
#192961=CARTESIAN_POINT('Ctrl Pts',(1.35184977125644,-24.4641149028894,
0.));
#192962=CARTESIAN_POINT('Ctrl Pts',(1.34378065512335,-24.4863883275135,
0.));
#192963=CARTESIAN_POINT('Ctrl Pts',(1.33562651019684,-24.5087244363856,
0.));
#192964=CARTESIAN_POINT('Ctrl Pts',(1.32738724435326,-24.5311225731434,
0.));
#192965=CARTESIAN_POINT('Ctrl Pts',(1.31906276763669,-24.5535820868671,
0.));
#192966=CARTESIAN_POINT('Ctrl Pts',(1.31065299222023,-24.576102332018,0.));
#192967=CARTESIAN_POINT('Ctrl Pts',(1.30215783236363,-24.5986826684025,
0.));
#192968=CARTESIAN_POINT('Ctrl Pts',(1.29357720438107,-24.6213224611228,
0.));
#192969=CARTESIAN_POINT('Ctrl Pts',(1.28491102661513,-24.6440210805278,
0.));
#192970=CARTESIAN_POINT('Ctrl Pts',(1.2761592194164,-24.666777902156,0.));
#192971=CARTESIAN_POINT('Ctrl Pts',(1.26732170513497,-24.6895923066837,
0.));
#192972=CARTESIAN_POINT('Ctrl Pts',(1.25839840807414,-24.7124636797895,
0.));
#192973=CARTESIAN_POINT('Ctrl Pts',(1.24938925444323,-24.7353914120012,
0.));
#192974=CARTESIAN_POINT('Ctrl Pts',(1.24029417231987,-24.7583748985439,
0.));
#192975=CARTESIAN_POINT('Ctrl Pts',(1.23111309161843,-24.78141353918,0.));
#192976=CARTESIAN_POINT('Ctrl Pts',(1.22184594406526,-24.8045067380536,
0.));
#192977=CARTESIAN_POINT('Ctrl Pts',(1.21249266318205,-24.8276539035092,
0.));
#192978=CARTESIAN_POINT('Ctrl Pts',(1.20305318426015,-24.8508544481973,
0.));
#192979=CARTESIAN_POINT('Ctrl Pts',(1.19352744434059,-24.8741077892074,
0.));
#192980=CARTESIAN_POINT('Ctrl Pts',(1.18391538220098,-24.8974133481829,
0.));
#192981=CARTESIAN_POINT('Ctrl Pts',(1.17421693835039,-24.9207705514449,
0.));
#192982=CARTESIAN_POINT('Ctrl Pts',(1.16443205502852,-24.9441788300932,
0.));
#192983=CARTESIAN_POINT('Ctrl Pts',(1.15456067621894,-24.9676376201501,
0.));
#192984=CARTESIAN_POINT('Ctrl Pts',(1.14460274758206,-24.9911463621431,
0.));
#192985=CARTESIAN_POINT('Ctrl Pts',(1.13455821638535,-25.0147045006193,
0.));
#192986=CARTESIAN_POINT('Ctrl Pts',(1.12442703144455,-25.0383114836898,
0.));
#192987=CARTESIAN_POINT('Ctrl Pts',(1.1142091430689,-25.0619667625336,0.));
#192988=CARTESIAN_POINT('Ctrl Pts',(1.1039045030174,-25.085669790968,0.));
#192989=CARTESIAN_POINT('Ctrl Pts',(1.09351306445299,-25.1094200248448,
0.));
#192990=CARTESIAN_POINT('Ctrl Pts',(1.08303478197174,-25.1332169227415,
0.));
#192991=CARTESIAN_POINT('Ctrl Pts',(1.07246961165459,-25.1570599469311,
0.));
#192992=CARTESIAN_POINT('Ctrl Pts',(1.06181751111754,-25.1809485642191,
0.));
#192993=CARTESIAN_POINT('Ctrl Pts',(1.05107843957925,-25.2048822469027,
0.));
#192994=CARTESIAN_POINT('Ctrl Pts',(1.04025235791514,-25.2288604735087,
0.));
#192995=CARTESIAN_POINT('Ctrl Pts',(1.0293392287683,-25.2528827300427,0.));
#192996=CARTESIAN_POINT('Ctrl Pts',(1.01833901642272,-25.2769485087268,
0.));
#192997=CARTESIAN_POINT('Ctrl Pts',(1.00725168656933,-25.3010573055557,
0.));
#192998=CARTESIAN_POINT('Ctrl Pts',(0.996077206120918,-25.3252086182976,
0.));
#192999=CARTESIAN_POINT('Ctrl Pts',(0.984815543004088,-25.3494019441444,
0.));
#193000=CARTESIAN_POINT('Ctrl Pts',(0.973466666000047,-25.3736367778842,
0.));
#193001=CARTESIAN_POINT('Ctrl Pts',(0.962030544502801,-25.3979126089155,
0.));
#193002=CARTESIAN_POINT('Ctrl Pts',(0.950507148596967,-25.4222289223155,
0.));
#193003=CARTESIAN_POINT('Ctrl Pts',(0.938896449495631,-25.4465852044835,
0.));
#193004=CARTESIAN_POINT('Ctrl Pts',(0.927198419885603,-25.4709809474996,
0.));
#193005=CARTESIAN_POINT('Ctrl Pts',(0.915413034335331,-25.4954156541787,
0.));
#193006=CARTESIAN_POINT('Ctrl Pts',(0.903540269651152,-25.5198888424195,
0.));
#193007=CARTESIAN_POINT('Ctrl Pts',(0.891580105349464,-25.5444000508223,
0.));
#193008=CARTESIAN_POINT('Ctrl Pts',(0.879532523835088,-25.568948840818,
0.));
#193009=CARTESIAN_POINT('Ctrl Pts',(0.867397509339468,-25.5935347843616,
0.));
#193010=CARTESIAN_POINT('Ctrl Pts',(0.855175047037614,-25.618157453608,
0.));
#193011=CARTESIAN_POINT('Ctrl Pts',(0.842865122121542,-25.6428164100078,
0.));
#193012=CARTESIAN_POINT('Ctrl Pts',(0.830467718864366,-25.6675111931957,
0.));
#193013=CARTESIAN_POINT('Ctrl Pts',(0.817982819786718,-25.6922413110172,
0.));
#193014=CARTESIAN_POINT('Ctrl Pts',(0.805410404552592,-25.7170062262474,
0.));
#193015=CARTESIAN_POINT('Ctrl Pts',(0.792750451613533,-25.7418053757671,
0.));
#193016=CARTESIAN_POINT('Ctrl Pts',(0.780002940289024,-25.7666381946871,
0.));
#193017=CARTESIAN_POINT('Ctrl Pts',(0.767167852648638,-25.7915041383304,
0.));
#193018=CARTESIAN_POINT('Ctrl Pts',(0.754245175608287,-25.816402705995,
0.));
#193019=CARTESIAN_POINT('Ctrl Pts',(0.741234902664695,-25.841333461908,
0.));
#193020=CARTESIAN_POINT('Ctrl Pts',(0.728137036485876,-25.8662960624285,
0.));
#193021=CARTESIAN_POINT('Ctrl Pts',(0.714951588533752,-25.8912902615141,
0.));
#193022=CARTESIAN_POINT('Ctrl Pts',(0.701678575236601,-25.9163158909645,
0.));
#193023=CARTESIAN_POINT('Ctrl Pts',(0.688318015065675,-25.941372847213,
0.));
#193024=CARTESIAN_POINT('Ctrl Pts',(0.677559543215902,-25.9614434298092,
0.));
#193025=CARTESIAN_POINT('Ctrl Pts',(0.669451306784414,-25.9765104298171,
0.));
#193026=CARTESIAN_POINT('Ctrl Pts',(0.664028313188911,-25.9865613464809,
0.));
#193027=CARTESIAN_POINT('Ctrl Pts',(0.66131244073089,-25.991588367311,0.));
#193028=CARTESIAN_POINT('',(0.66131244073089,-25.991588367311,0.));
#193029=CARTESIAN_POINT('Origin',(-3.92374859571502,-21.1389261070099,0.));
#193030=CARTESIAN_POINT('',(-4.11585220600463,-22.1738711152697,0.));
#193031=CARTESIAN_POINT('',(-4.11585220600463,-22.1738711152697,0.));
#193032=CARTESIAN_POINT('',(-1.96187429785751,-10.5694630535049,0.));
#193033=CARTESIAN_POINT('Ctrl Pts',(-0.661312440730913,-25.991588367311,
0.));
#193034=CARTESIAN_POINT('Ctrl Pts',(-0.661312440730913,-25.991588367311,
12.));
#193035=CARTESIAN_POINT('Ctrl Pts',(-0.664028313187638,-25.9865613464773,
0.));
#193036=CARTESIAN_POINT('Ctrl Pts',(-0.664028313187638,-25.9865613464773,
12.));
#193037=CARTESIAN_POINT('Ctrl Pts',(-0.669451306780837,-25.9765104298071,
0.));
#193038=CARTESIAN_POINT('Ctrl Pts',(-0.669451306780837,-25.9765104298071,
12.));
#193039=CARTESIAN_POINT('Ctrl Pts',(-0.677559543209739,-25.9614434297919,
0.));
#193040=CARTESIAN_POINT('Ctrl Pts',(-0.677559543209739,-25.9614434297919,
12.));
#193041=CARTESIAN_POINT('Ctrl Pts',(-0.688318015057743,-25.9413728471909,
0.));
#193042=CARTESIAN_POINT('Ctrl Pts',(-0.688318015057743,-25.9413728471909,
12.));
#193043=CARTESIAN_POINT('Ctrl Pts',(-0.701678575228768,-25.9163158909426,
0.));
#193044=CARTESIAN_POINT('Ctrl Pts',(-0.701678575228768,-25.9163158909426,
12.));
#193045=CARTESIAN_POINT('Ctrl Pts',(-0.714951588527651,-25.891290261497,
0.));
#193046=CARTESIAN_POINT('Ctrl Pts',(-0.714951588527651,-25.891290261497,
12.));
#193047=CARTESIAN_POINT('Ctrl Pts',(-0.728137036482348,-25.8662960624185,
0.));
#193048=CARTESIAN_POINT('Ctrl Pts',(-0.728137036482348,-25.8662960624185,
12.));
#193049=CARTESIAN_POINT('Ctrl Pts',(-0.741234902663818,-25.8413334619055,
0.));
#193050=CARTESIAN_POINT('Ctrl Pts',(-0.741234902663818,-25.8413334619055,
12.));
#193051=CARTESIAN_POINT('Ctrl Pts',(-0.754245175609535,-25.8164027059984,
0.));
#193052=CARTESIAN_POINT('Ctrl Pts',(-0.754245175609535,-25.8164027059984,
12.));
#193053=CARTESIAN_POINT('Ctrl Pts',(-0.76716785265118,-25.7915041383376,
0.));
#193054=CARTESIAN_POINT('Ctrl Pts',(-0.76716785265118,-25.7915041383376,
12.));
#193055=CARTESIAN_POINT('Ctrl Pts',(-0.780002940291976,-25.7666381946955,
0.));
#193056=CARTESIAN_POINT('Ctrl Pts',(-0.780002940291976,-25.7666381946955,
12.));
#193057=CARTESIAN_POINT('Ctrl Pts',(-0.792750451616139,-25.7418053757746,
0.));
#193058=CARTESIAN_POINT('Ctrl Pts',(-0.792750451616139,-25.7418053757746,
12.));
#193059=CARTESIAN_POINT('Ctrl Pts',(-0.805410404554365,-25.7170062262525,
0.));
#193060=CARTESIAN_POINT('Ctrl Pts',(-0.805410404554365,-25.7170062262525,
12.));
#193061=CARTESIAN_POINT('Ctrl Pts',(-0.817982819787476,-25.6922413110194,
0.));
#193062=CARTESIAN_POINT('Ctrl Pts',(-0.817982819787476,-25.6922413110194,
12.));
#193063=CARTESIAN_POINT('Ctrl Pts',(-0.830467718864218,-25.6675111931952,
0.));
#193064=CARTESIAN_POINT('Ctrl Pts',(-0.830467718864218,-25.6675111931952,
12.));
#193065=CARTESIAN_POINT('Ctrl Pts',(-0.842865122120771,-25.6428164100055,
0.));
#193066=CARTESIAN_POINT('Ctrl Pts',(-0.842865122120771,-25.6428164100055,
12.));
#193067=CARTESIAN_POINT('Ctrl Pts',(-0.85517504703656,-25.6181574536049,
0.));
#193068=CARTESIAN_POINT('Ctrl Pts',(-0.85517504703656,-25.6181574536049,
12.));
#193069=CARTESIAN_POINT('Ctrl Pts',(-0.867397509338443,-25.5935347843585,
0.));
#193070=CARTESIAN_POINT('Ctrl Pts',(-0.867397509338443,-25.5935347843585,
12.));
#193071=CARTESIAN_POINT('Ctrl Pts',(-0.879532523834307,-25.5689488408156,
0.));
#193072=CARTESIAN_POINT('Ctrl Pts',(-0.879532523834307,-25.5689488408156,
12.));
#193073=CARTESIAN_POINT('Ctrl Pts',(-0.891580105349052,-25.5444000508211,
0.));
#193074=CARTESIAN_POINT('Ctrl Pts',(-0.891580105349052,-25.5444000508211,
12.));
#193075=CARTESIAN_POINT('Ctrl Pts',(-0.903540269651119,-25.5198888424194,
0.));
#193076=CARTESIAN_POINT('Ctrl Pts',(-0.903540269651119,-25.5198888424194,
12.));
#193077=CARTESIAN_POINT('Ctrl Pts',(-0.915413034335626,-25.4954156541795,
0.));
#193078=CARTESIAN_POINT('Ctrl Pts',(-0.915413034335626,-25.4954156541795,
12.));
#193079=CARTESIAN_POINT('Ctrl Pts',(-0.927198419886107,-25.4709809475009,
0.));
#193080=CARTESIAN_POINT('Ctrl Pts',(-0.927198419886107,-25.4709809475009,
12.));
#193081=CARTESIAN_POINT('Ctrl Pts',(-0.938896449496205,-25.4465852044849,
0.));
#193082=CARTESIAN_POINT('Ctrl Pts',(-0.938896449496205,-25.4465852044849,
12.));
#193083=CARTESIAN_POINT('Ctrl Pts',(-0.950507148597481,-25.4222289223167,
0.));
#193084=CARTESIAN_POINT('Ctrl Pts',(-0.950507148597481,-25.4222289223167,
12.));
#193085=CARTESIAN_POINT('Ctrl Pts',(-0.962030544503155,-25.3979126089163,
0.));
#193086=CARTESIAN_POINT('Ctrl Pts',(-0.962030544503155,-25.3979126089163,
12.));
#193087=CARTESIAN_POINT('Ctrl Pts',(-0.973466666000176,-25.3736367778845,
0.));
#193088=CARTESIAN_POINT('Ctrl Pts',(-0.973466666000176,-25.3736367778845,
12.));
#193089=CARTESIAN_POINT('Ctrl Pts',(-0.984815543003984,-25.3494019441441,
0.));
#193090=CARTESIAN_POINT('Ctrl Pts',(-0.984815543003984,-25.3494019441441,
12.));
#193091=CARTESIAN_POINT('Ctrl Pts',(-0.996077206120636,-25.3252086182968,
0.));
#193092=CARTESIAN_POINT('Ctrl Pts',(-0.996077206120636,-25.3252086182968,
12.));
#193093=CARTESIAN_POINT('Ctrl Pts',(-1.00725168656897,-25.3010573055548,
0.));
#193094=CARTESIAN_POINT('Ctrl Pts',(-1.00725168656897,-25.3010573055548,
12.));
#193095=CARTESIAN_POINT('Ctrl Pts',(-1.01833901642238,-25.276948508726,
0.));
#193096=CARTESIAN_POINT('Ctrl Pts',(-1.01833901642238,-25.276948508726,
12.));
#193097=CARTESIAN_POINT('Ctrl Pts',(-1.02933922876807,-25.2528827300422,
0.));
#193098=CARTESIAN_POINT('Ctrl Pts',(-1.02933922876807,-25.2528827300422,
12.));
#193099=CARTESIAN_POINT('Ctrl Pts',(-1.04025235791508,-25.2288604735086,
0.));
#193100=CARTESIAN_POINT('Ctrl Pts',(-1.04025235791508,-25.2288604735086,
12.));
#193101=CARTESIAN_POINT('Ctrl Pts',(-1.05107843957933,-25.2048822469028,
0.));
#193102=CARTESIAN_POINT('Ctrl Pts',(-1.05107843957933,-25.2048822469028,
12.));
#193103=CARTESIAN_POINT('Ctrl Pts',(-1.06181751111769,-25.1809485642192,
0.));
#193104=CARTESIAN_POINT('Ctrl Pts',(-1.06181751111769,-25.1809485642192,
12.));
#193105=CARTESIAN_POINT('Ctrl Pts',(-1.07246961165477,-25.157059946931,
0.));
#193106=CARTESIAN_POINT('Ctrl Pts',(-1.07246961165477,-25.157059946931,
12.));
#193107=CARTESIAN_POINT('Ctrl Pts',(-1.08303478197189,-25.1332169227413,
0.));
#193108=CARTESIAN_POINT('Ctrl Pts',(-1.08303478197189,-25.1332169227413,
12.));
#193109=CARTESIAN_POINT('Ctrl Pts',(-1.09351306445309,-25.1094200248446,
0.));
#193110=CARTESIAN_POINT('Ctrl Pts',(-1.09351306445309,-25.1094200248446,
12.));
#193111=CARTESIAN_POINT('Ctrl Pts',(-1.10390450301746,-25.0856697909679,
0.));
#193112=CARTESIAN_POINT('Ctrl Pts',(-1.10390450301746,-25.0856697909679,
12.));
#193113=CARTESIAN_POINT('Ctrl Pts',(-1.1142091430689,-25.0619667625336,
0.));
#193114=CARTESIAN_POINT('Ctrl Pts',(-1.1142091430689,-25.0619667625336,
12.));
#193115=CARTESIAN_POINT('Ctrl Pts',(-1.12442703144453,-25.0383114836899,
0.));
#193116=CARTESIAN_POINT('Ctrl Pts',(-1.12442703144453,-25.0383114836899,
12.));
#193117=CARTESIAN_POINT('Ctrl Pts',(-1.13455821638531,-25.0147045006196,
0.));
#193118=CARTESIAN_POINT('Ctrl Pts',(-1.13455821638531,-25.0147045006196,
12.));
#193119=CARTESIAN_POINT('Ctrl Pts',(-1.14460274758202,-24.9911463621433,
0.));
#193120=CARTESIAN_POINT('Ctrl Pts',(-1.14460274758202,-24.9911463621433,
12.));
#193121=CARTESIAN_POINT('Ctrl Pts',(-1.1545606762189,-24.9676376201502,
0.));
#193122=CARTESIAN_POINT('Ctrl Pts',(-1.1545606762189,-24.9676376201502,
12.));
#193123=CARTESIAN_POINT('Ctrl Pts',(-1.16443205502851,-24.9441788300932,
0.));
#193124=CARTESIAN_POINT('Ctrl Pts',(-1.16443205502851,-24.9441788300932,
12.));
#193125=CARTESIAN_POINT('Ctrl Pts',(-1.17421693835042,-24.9207705514448,
0.));
#193126=CARTESIAN_POINT('Ctrl Pts',(-1.17421693835042,-24.9207705514448,
12.));
#193127=CARTESIAN_POINT('Ctrl Pts',(-1.18391538220104,-24.8974133481829,
0.));
#193128=CARTESIAN_POINT('Ctrl Pts',(-1.18391538220104,-24.8974133481829,
12.));
#193129=CARTESIAN_POINT('Ctrl Pts',(-1.19352744434065,-24.8741077892075,
0.));
#193130=CARTESIAN_POINT('Ctrl Pts',(-1.19352744434065,-24.8741077892075,
12.));
#193131=CARTESIAN_POINT('Ctrl Pts',(-1.20305318426021,-24.8508544481974,
0.));
#193132=CARTESIAN_POINT('Ctrl Pts',(-1.20305318426021,-24.8508544481974,
12.));
#193133=CARTESIAN_POINT('Ctrl Pts',(-1.21249266318209,-24.8276539035092,
0.));
#193134=CARTESIAN_POINT('Ctrl Pts',(-1.21249266318209,-24.8276539035092,
12.));
#193135=CARTESIAN_POINT('Ctrl Pts',(-1.22184594406529,-24.8045067380536,
0.));
#193136=CARTESIAN_POINT('Ctrl Pts',(-1.22184594406529,-24.8045067380536,
12.));
#193137=CARTESIAN_POINT('Ctrl Pts',(-1.23111309161845,-24.7814135391799,
0.));
#193138=CARTESIAN_POINT('Ctrl Pts',(-1.23111309161845,-24.7814135391799,
12.));
#193139=CARTESIAN_POINT('Ctrl Pts',(-1.2402941723199,-24.7583748985438,
0.));
#193140=CARTESIAN_POINT('Ctrl Pts',(-1.2402941723199,-24.7583748985438,
12.));
#193141=CARTESIAN_POINT('Ctrl Pts',(-1.24938925444327,-24.7353914120011,
0.));
#193142=CARTESIAN_POINT('Ctrl Pts',(-1.24938925444327,-24.7353914120011,
12.));
#193143=CARTESIAN_POINT('Ctrl Pts',(-1.25839840807419,-24.7124636797894,
0.));
#193144=CARTESIAN_POINT('Ctrl Pts',(-1.25839840807419,-24.7124636797894,
12.));
#193145=CARTESIAN_POINT('Ctrl Pts',(-1.26732170513501,-24.6895923066836,
0.));
#193146=CARTESIAN_POINT('Ctrl Pts',(-1.26732170513501,-24.6895923066836,
12.));
#193147=CARTESIAN_POINT('Ctrl Pts',(-1.27615921941643,-24.6667779021559,
0.));
#193148=CARTESIAN_POINT('Ctrl Pts',(-1.27615921941643,-24.6667779021559,
12.));
#193149=CARTESIAN_POINT('Ctrl Pts',(-1.28491102661515,-24.6440210805278,
0.));
#193150=CARTESIAN_POINT('Ctrl Pts',(-1.28491102661515,-24.6440210805278,
12.));
#193151=CARTESIAN_POINT('Ctrl Pts',(-1.29357720438108,-24.6213224611229,
0.));
#193152=CARTESIAN_POINT('Ctrl Pts',(-1.29357720438108,-24.6213224611229,
12.));
#193153=CARTESIAN_POINT('Ctrl Pts',(-1.30215783236363,-24.5986826684027,
0.));
#193154=CARTESIAN_POINT('Ctrl Pts',(-1.30215783236363,-24.5986826684027,
12.));
#193155=CARTESIAN_POINT('Ctrl Pts',(-1.31065299222023,-24.5761023320183,
0.));
#193156=CARTESIAN_POINT('Ctrl Pts',(-1.31065299222023,-24.5761023320183,
12.));
#193157=CARTESIAN_POINT('Ctrl Pts',(-1.31906276763669,-24.5535820868674,
0.));
#193158=CARTESIAN_POINT('Ctrl Pts',(-1.31906276763669,-24.5535820868674,
12.));
#193159=CARTESIAN_POINT('Ctrl Pts',(-1.32738724435327,-24.5311225731435,
0.));
#193160=CARTESIAN_POINT('Ctrl Pts',(-1.32738724435327,-24.5311225731435,
12.));
#193161=CARTESIAN_POINT('Ctrl Pts',(-1.33562651019687,-24.5087244363856,
0.));
#193162=CARTESIAN_POINT('Ctrl Pts',(-1.33562651019687,-24.5087244363856,
12.));
#193163=CARTESIAN_POINT('Ctrl Pts',(-1.34378065512339,-24.4863883275134,
0.));
#193164=CARTESIAN_POINT('Ctrl Pts',(-1.34378065512339,-24.4863883275134,
12.));
#193165=CARTESIAN_POINT('Ctrl Pts',(-1.35184977125649,-24.4641149028892,
0.));
#193166=CARTESIAN_POINT('Ctrl Pts',(-1.35184977125649,-24.4641149028892,
12.));
#193167=CARTESIAN_POINT('Ctrl Pts',(-1.35983395290628,-24.4419048244523,
0.));
#193168=CARTESIAN_POINT('Ctrl Pts',(-1.35983395290628,-24.4419048244523,
12.));
#193169=CARTESIAN_POINT('Ctrl Pts',(-1.36773329659957,-24.4197587598337,
0.));
#193170=CARTESIAN_POINT('Ctrl Pts',(-1.36773329659957,-24.4197587598337,
12.));
#193171=CARTESIAN_POINT('Ctrl Pts',(-1.3755479011161,-24.3976773824732,
0.));
#193172=CARTESIAN_POINT('Ctrl Pts',(-1.3755479011161,-24.3976773824732,
12.));
#193173=CARTESIAN_POINT('Ctrl Pts',(-1.38327786753,-24.3756613717299,0.));
#193174=CARTESIAN_POINT('Ctrl Pts',(-1.38327786753,-24.3756613717299,12.));
#193175=CARTESIAN_POINT('Ctrl Pts',(-1.39092329926389,-24.3537114129875,
0.));
#193176=CARTESIAN_POINT('Ctrl Pts',(-1.39092329926389,-24.3537114129875,
12.));
#193177=CARTESIAN_POINT('Ctrl Pts',(-1.39848430212808,-24.3318281977643,
0.));
#193178=CARTESIAN_POINT('Ctrl Pts',(-1.39848430212808,-24.3318281977643,
12.));
#193179=CARTESIAN_POINT('Ctrl Pts',(-1.40596098434338,-24.3100124238311,
0.));
#193180=CARTESIAN_POINT('Ctrl Pts',(-1.40596098434338,-24.3100124238311,
12.));
#193181=CARTESIAN_POINT('Ctrl Pts',(-1.41335345657684,-24.288264795321,
0.));
#193182=CARTESIAN_POINT('Ctrl Pts',(-1.41335345657684,-24.288264795321,
12.));
#193183=CARTESIAN_POINT('Ctrl Pts',(-1.42066183198254,-24.2665860228356,
0.));
#193184=CARTESIAN_POINT('Ctrl Pts',(-1.42066183198254,-24.2665860228356,
12.));
#193185=CARTESIAN_POINT('Ctrl Pts',(-1.42788622624855,-24.2449768235488,
0.));
#193186=CARTESIAN_POINT('Ctrl Pts',(-1.42788622624855,-24.2449768235488,
12.));
#193187=CARTESIAN_POINT('Ctrl Pts',(-1.43502675765509,-24.2234379212984,
0.));
#193188=CARTESIAN_POINT('Ctrl Pts',(-1.43502675765509,-24.2234379212984,
12.));
#193189=CARTESIAN_POINT('Ctrl Pts',(-1.44208354711083,-24.201970046722,
0.));
#193190=CARTESIAN_POINT('Ctrl Pts',(-1.44208354711083,-24.201970046722,
12.));
#193191=CARTESIAN_POINT('Ctrl Pts',(-1.44905671818729,-24.1805739374038,
0.));
#193192=CARTESIAN_POINT('Ctrl Pts',(-1.44905671818729,-24.1805739374038,
12.));
#193193=CARTESIAN_POINT('Ctrl Pts',(-1.45594639716319,-24.1592503380107,
0.));
#193194=CARTESIAN_POINT('Ctrl Pts',(-1.45594639716319,-24.1592503380107,
12.));
#193195=CARTESIAN_POINT('Ctrl Pts',(-1.46275271307399,-24.1380000004272,
0.));
#193196=CARTESIAN_POINT('Ctrl Pts',(-1.46275271307399,-24.1380000004272,
12.));
#193197=CARTESIAN_POINT('Ctrl Pts',(-1.46947579776992,-24.1168236838824,
0.));
#193198=CARTESIAN_POINT('Ctrl Pts',(-1.46947579776992,-24.1168236838824,
12.));
#193199=CARTESIAN_POINT('Ctrl Pts',(-1.47611578597743,-24.0957221550778,
0.));
#193200=CARTESIAN_POINT('Ctrl Pts',(-1.47611578597743,-24.0957221550778,
12.));
#193201=CARTESIAN_POINT('Ctrl Pts',(-1.48267281533684,-24.0746961883528,
0.));
#193202=CARTESIAN_POINT('Ctrl Pts',(-1.48267281533684,-24.0746961883528,
12.));
#193203=CARTESIAN_POINT('Ctrl Pts',(-1.48914702644888,-24.0537465658429,
0.));
#193204=CARTESIAN_POINT('Ctrl Pts',(-1.48914702644888,-24.0537465658429,
12.));
#193205=CARTESIAN_POINT('Ctrl Pts',(-1.49553856292802,-24.0328740776331,
0.));
#193206=CARTESIAN_POINT('Ctrl Pts',(-1.49553856292802,-24.0328740776331,
12.));
#193207=CARTESIAN_POINT('Ctrl Pts',(-1.501847571461,-24.0120795219086,0.));
#193208=CARTESIAN_POINT('Ctrl Pts',(-1.501847571461,-24.0120795219086,12.));
#193209=CARTESIAN_POINT('Ctrl Pts',(-1.50807420187695,-23.9913637050927,
0.));
#193210=CARTESIAN_POINT('Ctrl Pts',(-1.50807420187695,-23.9913637050927,
12.));
#193211=CARTESIAN_POINT('Ctrl Pts',(-1.51421860720615,-23.970727442014,
0.));
#193212=CARTESIAN_POINT('Ctrl Pts',(-1.51421860720615,-23.970727442014,
12.));
#193213=CARTESIAN_POINT('Ctrl Pts',(-1.52028094372793,-23.9501715561033,
0.));
#193214=CARTESIAN_POINT('Ctrl Pts',(-1.52028094372793,-23.9501715561033,
12.));
#193215=CARTESIAN_POINT('Ctrl Pts',(-1.52626137103033,-23.9296968795757,
0.));
#193216=CARTESIAN_POINT('Ctrl Pts',(-1.52626137103033,-23.9296968795757,
12.));
#193217=CARTESIAN_POINT('Ctrl Pts',(-1.53216005207464,-23.9093042536119,
0.));
#193218=CARTESIAN_POINT('Ctrl Pts',(-1.53216005207464,-23.9093042536119,
12.));
#193219=CARTESIAN_POINT('Ctrl Pts',(-1.53797715326759,-23.8889945285318,
0.));
#193220=CARTESIAN_POINT('Ctrl Pts',(-1.53797715326759,-23.8889945285318,
12.));
#193221=CARTESIAN_POINT('Ctrl Pts',(-1.54371284453991,-23.8687685639642,
0.));
#193222=CARTESIAN_POINT('Ctrl Pts',(-1.54371284453991,-23.8687685639642,
12.));
#193223=CARTESIAN_POINT('Ctrl Pts',(-1.54936729940542,-23.8486272290705,
0.));
#193224=CARTESIAN_POINT('Ctrl Pts',(-1.54936729940542,-23.8486272290705,
12.));
#193225=CARTESIAN_POINT('Ctrl Pts',(-1.55494069502636,-23.8285714027636,
0.));
#193226=CARTESIAN_POINT('Ctrl Pts',(-1.55494069502636,-23.8285714027636,
12.));
#193227=CARTESIAN_POINT('Ctrl Pts',(-1.56043321228635,-23.8086019739194,
0.));
#193228=CARTESIAN_POINT('Ctrl Pts',(-1.56043321228635,-23.8086019739194,
12.));
#193229=CARTESIAN_POINT('Ctrl Pts',(-1.56584503586844,-23.7887198415878,
0.));
#193230=CARTESIAN_POINT('Ctrl Pts',(-1.56584503586844,-23.7887198415878,
12.));
#193231=CARTESIAN_POINT('Ctrl Pts',(-1.57117635434409,-23.7689259151862,
0.));
#193232=CARTESIAN_POINT('Ctrl Pts',(-1.57117635434409,-23.7689259151862,
12.));
#193233=CARTESIAN_POINT('Ctrl Pts',(-1.57642736025247,-23.749221114736,
0.));
#193234=CARTESIAN_POINT('Ctrl Pts',(-1.57642736025247,-23.749221114736,
12.));
#193235=CARTESIAN_POINT('Ctrl Pts',(-1.58159825017359,-23.72960637113,0.));
#193236=CARTESIAN_POINT('Ctrl Pts',(-1.58159825017359,-23.72960637113,12.));
#193237=CARTESIAN_POINT('Ctrl Pts',(-1.58668922481222,-23.710082626383,
0.));
#193238=CARTESIAN_POINT('Ctrl Pts',(-1.58668922481222,-23.710082626383,
12.));
#193239=CARTESIAN_POINT('Ctrl Pts',(-1.59170048908634,-23.6906508338833,
0.));
#193240=CARTESIAN_POINT('Ctrl Pts',(-1.59170048908634,-23.6906508338833,
12.));
#193241=CARTESIAN_POINT('Ctrl Pts',(-1.59663225222464,-23.671311958631,
0.));
#193242=CARTESIAN_POINT('Ctrl Pts',(-1.59663225222464,-23.671311958631,
12.));
#193243=CARTESIAN_POINT('Ctrl Pts',(-1.60148472786596,-23.6520669774876,
0.));
#193244=CARTESIAN_POINT('Ctrl Pts',(-1.60148472786596,-23.6520669774876,
12.));
#193245=CARTESIAN_POINT('Ctrl Pts',(-1.60625813414674,-23.6329168794929,
0.));
#193246=CARTESIAN_POINT('Ctrl Pts',(-1.60625813414674,-23.6329168794929,
12.));
#193247=CARTESIAN_POINT('Ctrl Pts',(-1.61095269379779,-23.6138626661653,
0.));
#193248=CARTESIAN_POINT('Ctrl Pts',(-1.61095269379779,-23.6138626661653,
12.));
#193249=CARTESIAN_POINT('Ctrl Pts',(-1.61556863424699,-23.5949053517997,
0.));
#193250=CARTESIAN_POINT('Ctrl Pts',(-1.61556863424699,-23.5949053517997,
12.));
#193251=CARTESIAN_POINT('Ctrl Pts',(-1.62010618772867,-23.57604596376,0.));
#193252=CARTESIAN_POINT('Ctrl Pts',(-1.62010618772867,-23.57604596376,12.));
#193253=CARTESIAN_POINT('Ctrl Pts',(-1.62456559140065,-23.5572855427601,
0.));
#193254=CARTESIAN_POINT('Ctrl Pts',(-1.62456559140065,-23.5572855427601,
12.));
#193255=CARTESIAN_POINT('Ctrl Pts',(-1.62894708745224,-23.538625143226,
0.));
#193256=CARTESIAN_POINT('Ctrl Pts',(-1.62894708745224,-23.538625143226,
12.));
#193257=CARTESIAN_POINT('Ctrl Pts',(-1.63325092321727,-23.5200658336612,
0.));
#193258=CARTESIAN_POINT('Ctrl Pts',(-1.63325092321727,-23.5200658336612,
12.));
#193259=CARTESIAN_POINT('Ctrl Pts',(-1.63747735129475,-23.5016086970003,
0.));
#193260=CARTESIAN_POINT('Ctrl Pts',(-1.63747735129475,-23.5016086970003,
12.));
#193261=CARTESIAN_POINT('Ctrl Pts',(-1.64162662967529,-23.4832548309645,
0.));
#193262=CARTESIAN_POINT('Ctrl Pts',(-1.64162662967529,-23.4832548309645,
12.));
#193263=CARTESIAN_POINT('Ctrl Pts',(-1.64569902187612,-23.4650053483932,
0.));
#193264=CARTESIAN_POINT('Ctrl Pts',(-1.64569902187612,-23.4650053483932,
12.));
#193265=CARTESIAN_POINT('Ctrl Pts',(-1.64969479707341,-23.4468613776574,
0.));
#193266=CARTESIAN_POINT('Ctrl Pts',(-1.64969479707341,-23.4468613776574,
12.));
#193267=CARTESIAN_POINT('Ctrl Pts',(-1.65361423023729,-23.4288240631043,
0.));
#193268=CARTESIAN_POINT('Ctrl Pts',(-1.65361423023729,-23.4288240631043,
12.));
#193269=CARTESIAN_POINT('Ctrl Pts',(-1.65745760227506,-23.4108945654805,
0.));
#193270=CARTESIAN_POINT('Ctrl Pts',(-1.65745760227506,-23.4108945654805,
12.));
#193271=CARTESIAN_POINT('Ctrl Pts',(-1.66122520018012,-23.3930740623619,
0.));
#193272=CARTESIAN_POINT('Ctrl Pts',(-1.66122520018012,-23.3930740623619,
12.));
#193273=CARTESIAN_POINT('Ctrl Pts',(-1.66491731718878,-23.3753637485545,
0.));
#193274=CARTESIAN_POINT('Ctrl Pts',(-1.66491731718878,-23.3753637485545,
12.));
#193275=CARTESIAN_POINT('Ctrl Pts',(-1.66853425293997,-23.3577648365744,
0.));
#193276=CARTESIAN_POINT('Ctrl Pts',(-1.66853425293997,-23.3577648365744,
12.));
#193277=CARTESIAN_POINT('Ctrl Pts',(-1.67207631363923,-23.3402785571865,
0.));
#193278=CARTESIAN_POINT('Ctrl Pts',(-1.67207631363923,-23.3402785571865,
12.));
#193279=CARTESIAN_POINT('Ctrl Pts',(-1.67554381222995,-23.3229061599145,
0.));
#193280=CARTESIAN_POINT('Ctrl Pts',(-1.67554381222995,-23.3229061599145,
12.));
#193281=CARTESIAN_POINT('Ctrl Pts',(-1.67893706857118,-23.3056489135611,
0.));
#193282=CARTESIAN_POINT('Ctrl Pts',(-1.67893706857118,-23.3056489135611,
12.));
#193283=CARTESIAN_POINT('Ctrl Pts',(-1.68225640962169,-23.2885081066951,
0.));
#193284=CARTESIAN_POINT('Ctrl Pts',(-1.68225640962169,-23.2885081066951,
12.));
#193285=CARTESIAN_POINT('Ctrl Pts',(-1.68550216963259,-23.2714850482246,
0.));
#193286=CARTESIAN_POINT('Ctrl Pts',(-1.68550216963259,-23.2714850482246,
12.));
#193287=CARTESIAN_POINT('Ctrl Pts',(-1.68867469034897,-23.2545810680537,
0.));
#193288=CARTESIAN_POINT('Ctrl Pts',(-1.68867469034897,-23.2545810680537,
12.));
#193289=CARTESIAN_POINT('Ctrl Pts',(-1.69177432121712,-23.2377975177013,
0.));
#193290=CARTESIAN_POINT('Ctrl Pts',(-1.69177432121712,-23.2377975177013,
12.));
#193291=CARTESIAN_POINT('Ctrl Pts',(-1.69480141959954,-23.2211357709374,
0.));
#193292=CARTESIAN_POINT('Ctrl Pts',(-1.69480141959954,-23.2211357709374,
12.));
#193293=CARTESIAN_POINT('Ctrl Pts',(-1.69775635099444,-23.2045972243767,
0.));
#193294=CARTESIAN_POINT('Ctrl Pts',(-1.69775635099444,-23.2045972243767,
12.));
#193295=CARTESIAN_POINT('Ctrl Pts',(-1.70063948927011,-23.1881832981851,
0.));
#193296=CARTESIAN_POINT('Ctrl Pts',(-1.70063948927011,-23.1881832981851,
12.));
#193297=CARTESIAN_POINT('Ctrl Pts',(-1.70345121691277,-23.1718954368751,
0.));
#193298=CARTESIAN_POINT('Ctrl Pts',(-1.70345121691277,-23.1718954368751,
12.));
#193299=CARTESIAN_POINT('Ctrl Pts',(-1.70619192527853,-23.1557351100614,
0.));
#193300=CARTESIAN_POINT('Ctrl Pts',(-1.70619192527853,-23.1557351100614,
12.));
#193301=CARTESIAN_POINT('Ctrl Pts',(-1.70886201485453,-23.1397038132356,
0.));
#193302=CARTESIAN_POINT('Ctrl Pts',(-1.70886201485453,-23.1397038132356,
12.));
#193303=CARTESIAN_POINT('Ctrl Pts',(-1.71146189552175,-23.1238030684925,
0.));
#193304=CARTESIAN_POINT('Ctrl Pts',(-1.71146189552175,-23.1238030684925,
12.));
#193305=CARTESIAN_POINT('Ctrl Pts',(-1.71399198684705,-23.1080344254286,
0.));
#193306=CARTESIAN_POINT('Ctrl Pts',(-1.71399198684705,-23.1080344254286,
12.));
#193307=CARTESIAN_POINT('Ctrl Pts',(-1.71645271839298,-23.0923994621213,
0.));
#193308=CARTESIAN_POINT('Ctrl Pts',(-1.71645271839298,-23.0923994621213,
12.));
#193309=CARTESIAN_POINT('Ctrl Pts',(-1.71884453003028,-23.0768997860709,
0.));
#193310=CARTESIAN_POINT('Ctrl Pts',(-1.71884453003028,-23.0768997860709,
12.));
#193311=CARTESIAN_POINT('Ctrl Pts',(-1.72116787225993,-23.0615370351562,
0.));
#193312=CARTESIAN_POINT('Ctrl Pts',(-1.72116787225993,-23.0615370351562,
12.));
#193313=CARTESIAN_POINT('Ctrl Pts',(-1.72342320653748,-23.0463128785531,
0.));
#193314=CARTESIAN_POINT('Ctrl Pts',(-1.72342320653748,-23.0463128785531,
12.));
#193315=CARTESIAN_POINT('Ctrl Pts',(-1.72561100564047,-23.0312290178883,
0.));
#193316=CARTESIAN_POINT('Ctrl Pts',(-1.72561100564047,-23.0312290178883,
12.));
#193317=CARTESIAN_POINT('Ctrl Pts',(-1.7277317540471,-23.0162871884168,
0.));
#193318=CARTESIAN_POINT('Ctrl Pts',(-1.7277317540471,-23.0162871884168,
12.));
#193319=CARTESIAN_POINT('Ctrl Pts',(-1.72978594832137,-23.001489160189,
0.));
#193320=CARTESIAN_POINT('Ctrl Pts',(-1.72978594832137,-23.001489160189,
12.));
#193321=CARTESIAN_POINT('Ctrl Pts',(-1.73177409750192,-22.9868367391978,
0.));
#193322=CARTESIAN_POINT('Ctrl Pts',(-1.73177409750192,-22.9868367391978,
12.));
#193323=CARTESIAN_POINT('Ctrl Pts',(-1.73369672350816,-22.9723317685688,
0.));
#193324=CARTESIAN_POINT('Ctrl Pts',(-1.73369672350816,-22.9723317685688,
12.));
#193325=CARTESIAN_POINT('Ctrl Pts',(-1.7355543616277,-22.9579761301063,
0.));
#193326=CARTESIAN_POINT('Ctrl Pts',(-1.7355543616277,-22.9579761301063,
12.));
#193327=CARTESIAN_POINT('Ctrl Pts',(-1.7373475610004,-22.9437717457826,
0.));
#193328=CARTESIAN_POINT('Ctrl Pts',(-1.7373475610004,-22.9437717457826,
12.));
#193329=CARTESIAN_POINT('Ctrl Pts',(-1.73907688511667,-22.9297205792586,
0.));
#193330=CARTESIAN_POINT('Ctrl Pts',(-1.73907688511667,-22.9297205792586,
12.));
#193331=CARTESIAN_POINT('Ctrl Pts',(-1.74074291231059,-22.9158246373363,
0.));
#193332=CARTESIAN_POINT('Ctrl Pts',(-1.74074291231059,-22.9158246373363,
12.));
#193333=CARTESIAN_POINT('Ctrl Pts',(-1.74234623630081,-22.9020859716141,
0.));
#193334=CARTESIAN_POINT('Ctrl Pts',(-1.74234623630081,-22.9020859716141,
12.));
#193335=CARTESIAN_POINT('Ctrl Pts',(-1.74388746677703,-22.888506680335,
0.));
#193336=CARTESIAN_POINT('Ctrl Pts',(-1.74388746677703,-22.888506680335,
12.));
#193337=CARTESIAN_POINT('Ctrl Pts',(-1.74536722998202,-22.8750889101696,
0.));
#193338=CARTESIAN_POINT('Ctrl Pts',(-1.74536722998202,-22.8750889101696,
12.));
#193339=CARTESIAN_POINT('Ctrl Pts',(-1.74678616930666,-22.8618348580235,
0.));
#193340=CARTESIAN_POINT('Ctrl Pts',(-1.74678616930666,-22.8618348580235,
12.));
#193341=CARTESIAN_POINT('Ctrl Pts',(-1.74814494588494,-22.8487467728076,
0.));
#193342=CARTESIAN_POINT('Ctrl Pts',(-1.74814494588494,-22.8487467728076,
12.));
#193343=CARTESIAN_POINT('Ctrl Pts',(-1.74944423940117,-22.8358269579853,
0.));
#193344=CARTESIAN_POINT('Ctrl Pts',(-1.74944423940117,-22.8358269579853,
12.));
#193345=CARTESIAN_POINT('Ctrl Pts',(-1.75068474890884,-22.8230777741284,
0.));
#193346=CARTESIAN_POINT('Ctrl Pts',(-1.75068474890884,-22.8230777741284,
12.));
#193347=CARTESIAN_POINT('Ctrl Pts',(-1.75186719365593,-22.8105016414713,
0.));
#193348=CARTESIAN_POINT('Ctrl Pts',(-1.75186719365593,-22.8105016414713,
12.));
#193349=CARTESIAN_POINT('Ctrl Pts',(-1.75299231391467,-22.7981010424314,
0.));
#193350=CARTESIAN_POINT('Ctrl Pts',(-1.75299231391467,-22.7981010424314,
12.));
#193351=CARTESIAN_POINT('Ctrl Pts',(-1.75406087182937,-22.7858785242361,
0.));
#193352=CARTESIAN_POINT('Ctrl Pts',(-1.75406087182937,-22.7858785242361,
12.));
#193353=CARTESIAN_POINT('Ctrl Pts',(-1.75507365227133,-22.7738367016118,
0.));
#193354=CARTESIAN_POINT('Ctrl Pts',(-1.75507365227133,-22.7738367016118,
12.));
#193355=CARTESIAN_POINT('Ctrl Pts',(-1.75603146371642,-22.7619782595013,
0.));
#193356=CARTESIAN_POINT('Ctrl Pts',(-1.75603146371642,-22.7619782595013,
12.));
#193357=CARTESIAN_POINT('Ctrl Pts',(-1.75693513908908,-22.750305955645,
0.));
#193358=CARTESIAN_POINT('Ctrl Pts',(-1.75693513908908,-22.750305955645,
12.));
#193359=CARTESIAN_POINT('Ctrl Pts',(-1.75778553673245,-22.7388226235559,
0.));
#193360=CARTESIAN_POINT('Ctrl Pts',(-1.75778553673245,-22.7388226235559,
12.));
#193361=CARTESIAN_POINT('Ctrl Pts',(-1.75858354204634,-22.72753117773,0.));
#193362=CARTESIAN_POINT('Ctrl Pts',(-1.75858354204634,-22.72753117773,12.));
#193363=CARTESIAN_POINT('Ctrl Pts',(-1.75933006905926,-22.7164346186006,
0.));
#193364=CARTESIAN_POINT('Ctrl Pts',(-1.75933006905926,-22.7164346186006,
12.));
#193365=CARTESIAN_POINT('Ctrl Pts',(-1.76002606202402,-22.7055360375485,
0.));
#193366=CARTESIAN_POINT('Ctrl Pts',(-1.76002606202402,-22.7055360375485,
12.));
#193367=CARTESIAN_POINT('Ctrl Pts',(-1.76067249704888,-22.6948386219851,
0.));
#193368=CARTESIAN_POINT('Ctrl Pts',(-1.76067249704888,-22.6948386219851,
12.));
#193369=CARTESIAN_POINT('Ctrl Pts',(-1.76127038310615,-22.684345658525,
0.));
#193370=CARTESIAN_POINT('Ctrl Pts',(-1.76127038310615,-22.684345658525,
12.));
#193371=CARTESIAN_POINT('Ctrl Pts',(-1.76182076289527,-22.67406053567,0.));
#193372=CARTESIAN_POINT('Ctrl Pts',(-1.76182076289527,-22.67406053567,12.));
#193373=CARTESIAN_POINT('Ctrl Pts',(-1.7623247139257,-22.6639867471753,
0.));
#193374=CARTESIAN_POINT('Ctrl Pts',(-1.7623247139257,-22.6639867471753,
12.));
#193375=CARTESIAN_POINT('Ctrl Pts',(-1.76278334912562,-22.654127893841,
0.));
#193376=CARTESIAN_POINT('Ctrl Pts',(-1.76278334912562,-22.654127893841,
12.));
#193377=CARTESIAN_POINT('Ctrl Pts',(-1.76319782013917,-22.6444876940423,
0.));
#193378=CARTESIAN_POINT('Ctrl Pts',(-1.76319782013917,-22.6444876940423,
12.));
#193379=CARTESIAN_POINT('Ctrl Pts',(-1.76356932176274,-22.6350699979359,
0.));
#193380=CARTESIAN_POINT('Ctrl Pts',(-1.76356932176274,-22.6350699979359,
12.));
#193381=CARTESIAN_POINT('Ctrl Pts',(-1.76389909571404,-22.6258787994848,
0.));
#193382=CARTESIAN_POINT('Ctrl Pts',(-1.76389909571404,-22.6258787994848,
12.));
#193383=CARTESIAN_POINT('Ctrl Pts',(-1.7641884354374,-22.6169182517694,
0.));
#193384=CARTESIAN_POINT('Ctrl Pts',(-1.7641884354374,-22.6169182517694,
12.));
#193385=CARTESIAN_POINT('Ctrl Pts',(-1.76443868648017,-22.6081926681343,
0.));
#193386=CARTESIAN_POINT('Ctrl Pts',(-1.76443868648017,-22.6081926681343,
12.));
#193387=CARTESIAN_POINT('Ctrl Pts',(-1.76465124413558,-22.5997065145638,
0.));
#193388=CARTESIAN_POINT('Ctrl Pts',(-1.76465124413558,-22.5997065145638,
12.));
#193389=CARTESIAN_POINT('Ctrl Pts',(-1.76482755288412,-22.5914644078106,
0.));
#193390=CARTESIAN_POINT('Ctrl Pts',(-1.76482755288412,-22.5914644078106,
12.));
#193391=CARTESIAN_POINT('Ctrl Pts',(-1.76496910283089,-22.5834711038022,
0.));
#193392=CARTESIAN_POINT('Ctrl Pts',(-1.76496910283089,-22.5834711038022,
12.));
#193393=CARTESIAN_POINT('Ctrl Pts',(-1.76507744026747,-22.5757315316353,
0.));
#193394=CARTESIAN_POINT('Ctrl Pts',(-1.76507744026747,-22.5757315316353,
12.));
#193395=CARTESIAN_POINT('Ctrl Pts',(-1.76515418518832,-22.5682508499874,
0.));
#193396=CARTESIAN_POINT('Ctrl Pts',(-1.76515418518832,-22.5682508499874,
12.));
#193397=CARTESIAN_POINT('Ctrl Pts',(-1.76520104500451,-22.5610344912501,
0.));
#193398=CARTESIAN_POINT('Ctrl Pts',(-1.76520104500451,-22.5610344912501,
12.));
#193399=CARTESIAN_POINT('Ctrl Pts',(-1.76521983384063,-22.5540882235837,
0.));
#193400=CARTESIAN_POINT('Ctrl Pts',(-1.76521983384063,-22.5540882235837,
12.));
#193401=CARTESIAN_POINT('Ctrl Pts',(-1.76521245524048,-22.5474180954006,
0.));
#193402=CARTESIAN_POINT('Ctrl Pts',(-1.76521245524048,-22.5474180954006,
12.));
#193403=CARTESIAN_POINT('Ctrl Pts',(-1.76518087841494,-22.5410303590892,
0.));
#193404=CARTESIAN_POINT('Ctrl Pts',(-1.76518087841494,-22.5410303590892,
12.));
#193405=CARTESIAN_POINT('Ctrl Pts',(-1.76512711563255,-22.5349313983571,
0.));
#193406=CARTESIAN_POINT('Ctrl Pts',(-1.76512711563255,-22.5349313983571,
12.));
#193407=CARTESIAN_POINT('Ctrl Pts',(-1.7650532026276,-22.529127665298,0.));
#193408=CARTESIAN_POINT('Ctrl Pts',(-1.7650532026276,-22.529127665298,12.));
#193409=CARTESIAN_POINT('Ctrl Pts',(-1.76496128643376,-22.5236259635515,
0.));
#193410=CARTESIAN_POINT('Ctrl Pts',(-1.76496128643376,-22.5236259635515,
12.));
#193411=CARTESIAN_POINT('Ctrl Pts',(-1.76485369319896,-22.5184336670207,
0.));
#193412=CARTESIAN_POINT('Ctrl Pts',(-1.76485369319896,-22.5184336670207,
12.));
#193413=CARTESIAN_POINT('Ctrl Pts',(-1.7647330328115,-22.5135590569554,
0.));
#193414=CARTESIAN_POINT('Ctrl Pts',(-1.7647330328115,-22.5135590569554,
12.));
#193415=CARTESIAN_POINT('Ctrl Pts',(-1.76460218257314,-22.5090112700212,
0.));
#193416=CARTESIAN_POINT('Ctrl Pts',(-1.76460218257314,-22.5090112700212,
12.));
#193417=CARTESIAN_POINT('Ctrl Pts',(-1.76446408210366,-22.5047996391978,
0.));
#193418=CARTESIAN_POINT('Ctrl Pts',(-1.76446408210366,-22.5047996391978,
12.));
#193419=CARTESIAN_POINT('Ctrl Pts',(-1.76432160068739,-22.5009332677316,
0.));
#193420=CARTESIAN_POINT('Ctrl Pts',(-1.76432160068739,-22.5009332677316,
12.));
#193421=CARTESIAN_POINT('Ctrl Pts',(-1.76417731243484,-22.4974203063191,
0.));
#193422=CARTESIAN_POINT('Ctrl Pts',(-1.76417731243484,-22.4974203063191,
12.));
#193423=CARTESIAN_POINT('Ctrl Pts',(-1.76403393880317,-22.4942693792449,
0.));
#193424=CARTESIAN_POINT('Ctrl Pts',(-1.76403393880317,-22.4942693792449,
12.));
#193425=CARTESIAN_POINT('Ctrl Pts',(-1.76389475965715,-22.4914909094908,
0.));
#193426=CARTESIAN_POINT('Ctrl Pts',(-1.76389475965715,-22.4914909094908,
12.));
#193427=CARTESIAN_POINT('Ctrl Pts',(-1.76376424879469,-22.4890991659479,
0.));
#193428=CARTESIAN_POINT('Ctrl Pts',(-1.76376424879469,-22.4890991659479,
12.));
#193429=CARTESIAN_POINT('Ctrl Pts',(-1.76364784232926,-22.4871115206572,
0.));
#193430=CARTESIAN_POINT('Ctrl Pts',(-1.76364784232926,-22.4871115206572,
12.));
#193431=CARTESIAN_POINT('Ctrl Pts',(-1.7635507604555,-22.4855446605991,
0.));
#193432=CARTESIAN_POINT('Ctrl Pts',(-1.7635507604555,-22.4855446605991,
12.));
#193433=CARTESIAN_POINT('Ctrl Pts',(-1.76347698284863,-22.4844112933125,
0.));
#193434=CARTESIAN_POINT('Ctrl Pts',(-1.76347698284863,-22.4844112933125,
12.));
#193435=CARTESIAN_POINT('Ctrl Pts',(-1.7634381343466,-22.4838562517064,
0.));
#193436=CARTESIAN_POINT('Ctrl Pts',(-1.7634381343466,-22.4838562517064,
12.));
#193437=CARTESIAN_POINT('Ctrl Pts',(-1.76342064263638,-22.4836387052228,
0.));
#193438=CARTESIAN_POINT('Ctrl Pts',(-1.76342064263638,-22.4836387052228,
12.));
#193439=CARTESIAN_POINT('Ctrl Pts',(-1.76341415538792,-22.4835819929788,
0.));
#193440=CARTESIAN_POINT('Ctrl Pts',(-1.76341415538792,-22.4835819929788,
12.));
#193441=CARTESIAN_POINT('Ctrl Pts',(-1.76341220531181,-22.4835757167854,
0.));
#193442=CARTESIAN_POINT('Ctrl Pts',(-1.76341220531181,-22.4835757167854,
12.));
#193443=CARTESIAN_POINT('',(-0.661312440730913,-25.991588367311,0.));
#193444=CARTESIAN_POINT('Ctrl Pts',(-0.661312440730913,-25.991588367311,
0.));
#193445=CARTESIAN_POINT('Ctrl Pts',(-0.664028313187638,-25.9865613464773,
0.));
#193446=CARTESIAN_POINT('Ctrl Pts',(-0.669451306780837,-25.9765104298071,
0.));
#193447=CARTESIAN_POINT('Ctrl Pts',(-0.677559543209739,-25.9614434297919,
0.));
#193448=CARTESIAN_POINT('Ctrl Pts',(-0.688318015057743,-25.9413728471909,
0.));
#193449=CARTESIAN_POINT('Ctrl Pts',(-0.701678575228768,-25.9163158909426,
0.));
#193450=CARTESIAN_POINT('Ctrl Pts',(-0.714951588527651,-25.891290261497,
0.));
#193451=CARTESIAN_POINT('Ctrl Pts',(-0.728137036482348,-25.8662960624185,
0.));
#193452=CARTESIAN_POINT('Ctrl Pts',(-0.741234902663818,-25.8413334619055,
0.));
#193453=CARTESIAN_POINT('Ctrl Pts',(-0.754245175609535,-25.8164027059984,
0.));
#193454=CARTESIAN_POINT('Ctrl Pts',(-0.76716785265118,-25.7915041383376,
0.));
#193455=CARTESIAN_POINT('Ctrl Pts',(-0.780002940291976,-25.7666381946955,
0.));
#193456=CARTESIAN_POINT('Ctrl Pts',(-0.792750451616139,-25.7418053757746,
0.));
#193457=CARTESIAN_POINT('Ctrl Pts',(-0.805410404554365,-25.7170062262525,
0.));
#193458=CARTESIAN_POINT('Ctrl Pts',(-0.817982819787476,-25.6922413110194,
0.));
#193459=CARTESIAN_POINT('Ctrl Pts',(-0.830467718864218,-25.6675111931952,
0.));
#193460=CARTESIAN_POINT('Ctrl Pts',(-0.842865122120771,-25.6428164100055,
0.));
#193461=CARTESIAN_POINT('Ctrl Pts',(-0.85517504703656,-25.6181574536049,
0.));
#193462=CARTESIAN_POINT('Ctrl Pts',(-0.867397509338443,-25.5935347843585,
0.));
#193463=CARTESIAN_POINT('Ctrl Pts',(-0.879532523834307,-25.5689488408156,
0.));
#193464=CARTESIAN_POINT('Ctrl Pts',(-0.891580105349052,-25.5444000508211,
0.));
#193465=CARTESIAN_POINT('Ctrl Pts',(-0.903540269651119,-25.5198888424194,
0.));
#193466=CARTESIAN_POINT('Ctrl Pts',(-0.915413034335626,-25.4954156541795,
0.));
#193467=CARTESIAN_POINT('Ctrl Pts',(-0.927198419886107,-25.4709809475009,
0.));
#193468=CARTESIAN_POINT('Ctrl Pts',(-0.938896449496205,-25.4465852044849,
0.));
#193469=CARTESIAN_POINT('Ctrl Pts',(-0.950507148597481,-25.4222289223167,
0.));
#193470=CARTESIAN_POINT('Ctrl Pts',(-0.962030544503155,-25.3979126089163,
0.));
#193471=CARTESIAN_POINT('Ctrl Pts',(-0.973466666000176,-25.3736367778845,
0.));
#193472=CARTESIAN_POINT('Ctrl Pts',(-0.984815543003984,-25.3494019441441,
0.));
#193473=CARTESIAN_POINT('Ctrl Pts',(-0.996077206120636,-25.3252086182968,
0.));
#193474=CARTESIAN_POINT('Ctrl Pts',(-1.00725168656897,-25.3010573055548,
0.));
#193475=CARTESIAN_POINT('Ctrl Pts',(-1.01833901642238,-25.276948508726,
0.));
#193476=CARTESIAN_POINT('Ctrl Pts',(-1.02933922876807,-25.2528827300422,
0.));
#193477=CARTESIAN_POINT('Ctrl Pts',(-1.04025235791508,-25.2288604735086,
0.));
#193478=CARTESIAN_POINT('Ctrl Pts',(-1.05107843957933,-25.2048822469028,
0.));
#193479=CARTESIAN_POINT('Ctrl Pts',(-1.06181751111769,-25.1809485642192,
0.));
#193480=CARTESIAN_POINT('Ctrl Pts',(-1.07246961165477,-25.157059946931,
0.));
#193481=CARTESIAN_POINT('Ctrl Pts',(-1.08303478197189,-25.1332169227413,
0.));
#193482=CARTESIAN_POINT('Ctrl Pts',(-1.09351306445309,-25.1094200248446,
0.));
#193483=CARTESIAN_POINT('Ctrl Pts',(-1.10390450301746,-25.0856697909679,
0.));
#193484=CARTESIAN_POINT('Ctrl Pts',(-1.1142091430689,-25.0619667625336,
0.));
#193485=CARTESIAN_POINT('Ctrl Pts',(-1.12442703144453,-25.0383114836899,
0.));
#193486=CARTESIAN_POINT('Ctrl Pts',(-1.13455821638531,-25.0147045006196,
0.));
#193487=CARTESIAN_POINT('Ctrl Pts',(-1.14460274758202,-24.9911463621433,
0.));
#193488=CARTESIAN_POINT('Ctrl Pts',(-1.1545606762189,-24.9676376201502,
0.));
#193489=CARTESIAN_POINT('Ctrl Pts',(-1.16443205502851,-24.9441788300932,
0.));
#193490=CARTESIAN_POINT('Ctrl Pts',(-1.17421693835042,-24.9207705514448,
0.));
#193491=CARTESIAN_POINT('Ctrl Pts',(-1.18391538220104,-24.8974133481829,
0.));
#193492=CARTESIAN_POINT('Ctrl Pts',(-1.19352744434065,-24.8741077892075,
0.));
#193493=CARTESIAN_POINT('Ctrl Pts',(-1.20305318426021,-24.8508544481974,
0.));
#193494=CARTESIAN_POINT('Ctrl Pts',(-1.21249266318209,-24.8276539035092,
0.));
#193495=CARTESIAN_POINT('Ctrl Pts',(-1.22184594406529,-24.8045067380536,
0.));
#193496=CARTESIAN_POINT('Ctrl Pts',(-1.23111309161845,-24.7814135391799,
0.));
#193497=CARTESIAN_POINT('Ctrl Pts',(-1.2402941723199,-24.7583748985438,
0.));
#193498=CARTESIAN_POINT('Ctrl Pts',(-1.24938925444327,-24.7353914120011,
0.));
#193499=CARTESIAN_POINT('Ctrl Pts',(-1.25839840807419,-24.7124636797894,
0.));
#193500=CARTESIAN_POINT('Ctrl Pts',(-1.26732170513501,-24.6895923066836,
0.));
#193501=CARTESIAN_POINT('Ctrl Pts',(-1.27615921941643,-24.6667779021559,
0.));
#193502=CARTESIAN_POINT('Ctrl Pts',(-1.28491102661515,-24.6440210805278,
0.));
#193503=CARTESIAN_POINT('Ctrl Pts',(-1.29357720438108,-24.6213224611229,
0.));
#193504=CARTESIAN_POINT('Ctrl Pts',(-1.30215783236363,-24.5986826684027,
0.));
#193505=CARTESIAN_POINT('Ctrl Pts',(-1.31065299222023,-24.5761023320183,
0.));
#193506=CARTESIAN_POINT('Ctrl Pts',(-1.31906276763669,-24.5535820868674,
0.));
#193507=CARTESIAN_POINT('Ctrl Pts',(-1.32738724435327,-24.5311225731435,
0.));
#193508=CARTESIAN_POINT('Ctrl Pts',(-1.33562651019687,-24.5087244363856,
0.));
#193509=CARTESIAN_POINT('Ctrl Pts',(-1.34378065512339,-24.4863883275134,
0.));
#193510=CARTESIAN_POINT('Ctrl Pts',(-1.35184977125649,-24.4641149028892,
0.));
#193511=CARTESIAN_POINT('Ctrl Pts',(-1.35983395290628,-24.4419048244523,
0.));
#193512=CARTESIAN_POINT('Ctrl Pts',(-1.36773329659957,-24.4197587598337,
0.));
#193513=CARTESIAN_POINT('Ctrl Pts',(-1.3755479011161,-24.3976773824732,
0.));
#193514=CARTESIAN_POINT('Ctrl Pts',(-1.38327786753,-24.3756613717299,0.));
#193515=CARTESIAN_POINT('Ctrl Pts',(-1.39092329926389,-24.3537114129875,
0.));
#193516=CARTESIAN_POINT('Ctrl Pts',(-1.39848430212808,-24.3318281977643,
0.));
#193517=CARTESIAN_POINT('Ctrl Pts',(-1.40596098434338,-24.3100124238311,
0.));
#193518=CARTESIAN_POINT('Ctrl Pts',(-1.41335345657684,-24.288264795321,
0.));
#193519=CARTESIAN_POINT('Ctrl Pts',(-1.42066183198254,-24.2665860228356,
0.));
#193520=CARTESIAN_POINT('Ctrl Pts',(-1.42788622624855,-24.2449768235488,
0.));
#193521=CARTESIAN_POINT('Ctrl Pts',(-1.43502675765509,-24.2234379212984,
0.));
#193522=CARTESIAN_POINT('Ctrl Pts',(-1.44208354711083,-24.201970046722,
0.));
#193523=CARTESIAN_POINT('Ctrl Pts',(-1.44905671818729,-24.1805739374038,
0.));
#193524=CARTESIAN_POINT('Ctrl Pts',(-1.45594639716319,-24.1592503380107,
0.));
#193525=CARTESIAN_POINT('Ctrl Pts',(-1.46275271307399,-24.1380000004272,
0.));
#193526=CARTESIAN_POINT('Ctrl Pts',(-1.46947579776992,-24.1168236838824,
0.));
#193527=CARTESIAN_POINT('Ctrl Pts',(-1.47611578597743,-24.0957221550778,
0.));
#193528=CARTESIAN_POINT('Ctrl Pts',(-1.48267281533684,-24.0746961883528,
0.));
#193529=CARTESIAN_POINT('Ctrl Pts',(-1.48914702644888,-24.0537465658429,
0.));
#193530=CARTESIAN_POINT('Ctrl Pts',(-1.49553856292802,-24.0328740776331,
0.));
#193531=CARTESIAN_POINT('Ctrl Pts',(-1.501847571461,-24.0120795219086,0.));
#193532=CARTESIAN_POINT('Ctrl Pts',(-1.50807420187695,-23.9913637050927,
0.));
#193533=CARTESIAN_POINT('Ctrl Pts',(-1.51421860720615,-23.970727442014,
0.));
#193534=CARTESIAN_POINT('Ctrl Pts',(-1.52028094372793,-23.9501715561033,
0.));
#193535=CARTESIAN_POINT('Ctrl Pts',(-1.52626137103033,-23.9296968795757,
0.));
#193536=CARTESIAN_POINT('Ctrl Pts',(-1.53216005207464,-23.9093042536119,
0.));
#193537=CARTESIAN_POINT('Ctrl Pts',(-1.53797715326759,-23.8889945285318,
0.));
#193538=CARTESIAN_POINT('Ctrl Pts',(-1.54371284453991,-23.8687685639642,
0.));
#193539=CARTESIAN_POINT('Ctrl Pts',(-1.54936729940542,-23.8486272290705,
0.));
#193540=CARTESIAN_POINT('Ctrl Pts',(-1.55494069502636,-23.8285714027636,
0.));
#193541=CARTESIAN_POINT('Ctrl Pts',(-1.56043321228635,-23.8086019739194,
0.));
#193542=CARTESIAN_POINT('Ctrl Pts',(-1.56584503586844,-23.7887198415878,
0.));
#193543=CARTESIAN_POINT('Ctrl Pts',(-1.57117635434409,-23.7689259151862,
0.));
#193544=CARTESIAN_POINT('Ctrl Pts',(-1.57642736025247,-23.749221114736,
0.));
#193545=CARTESIAN_POINT('Ctrl Pts',(-1.58159825017359,-23.72960637113,0.));
#193546=CARTESIAN_POINT('Ctrl Pts',(-1.58668922481222,-23.710082626383,
0.));
#193547=CARTESIAN_POINT('Ctrl Pts',(-1.59170048908634,-23.6906508338833,
0.));
#193548=CARTESIAN_POINT('Ctrl Pts',(-1.59663225222464,-23.671311958631,
0.));
#193549=CARTESIAN_POINT('Ctrl Pts',(-1.60148472786596,-23.6520669774876,
0.));
#193550=CARTESIAN_POINT('Ctrl Pts',(-1.60625813414674,-23.6329168794929,
0.));
#193551=CARTESIAN_POINT('Ctrl Pts',(-1.61095269379779,-23.6138626661653,
0.));
#193552=CARTESIAN_POINT('Ctrl Pts',(-1.61556863424699,-23.5949053517997,
0.));
#193553=CARTESIAN_POINT('Ctrl Pts',(-1.62010618772867,-23.57604596376,0.));
#193554=CARTESIAN_POINT('Ctrl Pts',(-1.62456559140065,-23.5572855427601,
0.));
#193555=CARTESIAN_POINT('Ctrl Pts',(-1.62894708745224,-23.538625143226,
0.));
#193556=CARTESIAN_POINT('Ctrl Pts',(-1.63325092321727,-23.5200658336612,
0.));
#193557=CARTESIAN_POINT('Ctrl Pts',(-1.63747735129475,-23.5016086970003,
0.));
#193558=CARTESIAN_POINT('Ctrl Pts',(-1.64162662967529,-23.4832548309645,
0.));
#193559=CARTESIAN_POINT('Ctrl Pts',(-1.64569902187612,-23.4650053483932,
0.));
#193560=CARTESIAN_POINT('Ctrl Pts',(-1.64969479707341,-23.4468613776574,
0.));
#193561=CARTESIAN_POINT('Ctrl Pts',(-1.65361423023729,-23.4288240631043,
0.));
#193562=CARTESIAN_POINT('Ctrl Pts',(-1.65745760227506,-23.4108945654805,
0.));
#193563=CARTESIAN_POINT('Ctrl Pts',(-1.66122520018012,-23.3930740623619,
0.));
#193564=CARTESIAN_POINT('Ctrl Pts',(-1.66491731718878,-23.3753637485545,
0.));
#193565=CARTESIAN_POINT('Ctrl Pts',(-1.66853425293997,-23.3577648365744,
0.));
#193566=CARTESIAN_POINT('Ctrl Pts',(-1.67207631363923,-23.3402785571865,
0.));
#193567=CARTESIAN_POINT('Ctrl Pts',(-1.67554381222995,-23.3229061599145,
0.));
#193568=CARTESIAN_POINT('Ctrl Pts',(-1.67893706857118,-23.3056489135611,
0.));
#193569=CARTESIAN_POINT('Ctrl Pts',(-1.68225640962169,-23.2885081066951,
0.));
#193570=CARTESIAN_POINT('Ctrl Pts',(-1.68550216963259,-23.2714850482246,
0.));
#193571=CARTESIAN_POINT('Ctrl Pts',(-1.68867469034897,-23.2545810680537,
0.));
#193572=CARTESIAN_POINT('Ctrl Pts',(-1.69177432121712,-23.2377975177013,
0.));
#193573=CARTESIAN_POINT('Ctrl Pts',(-1.69480141959954,-23.2211357709374,
0.));
#193574=CARTESIAN_POINT('Ctrl Pts',(-1.69775635099444,-23.2045972243767,
0.));
#193575=CARTESIAN_POINT('Ctrl Pts',(-1.70063948927011,-23.1881832981851,
0.));
#193576=CARTESIAN_POINT('Ctrl Pts',(-1.70345121691277,-23.1718954368751,
0.));
#193577=CARTESIAN_POINT('Ctrl Pts',(-1.70619192527853,-23.1557351100614,
0.));
#193578=CARTESIAN_POINT('Ctrl Pts',(-1.70886201485453,-23.1397038132356,
0.));
#193579=CARTESIAN_POINT('Ctrl Pts',(-1.71146189552175,-23.1238030684925,
0.));
#193580=CARTESIAN_POINT('Ctrl Pts',(-1.71399198684705,-23.1080344254286,
0.));
#193581=CARTESIAN_POINT('Ctrl Pts',(-1.71645271839298,-23.0923994621213,
0.));
#193582=CARTESIAN_POINT('Ctrl Pts',(-1.71884453003028,-23.0768997860709,
0.));
#193583=CARTESIAN_POINT('Ctrl Pts',(-1.72116787225993,-23.0615370351562,
0.));
#193584=CARTESIAN_POINT('Ctrl Pts',(-1.72342320653748,-23.0463128785531,
0.));
#193585=CARTESIAN_POINT('Ctrl Pts',(-1.72561100564047,-23.0312290178883,
0.));
#193586=CARTESIAN_POINT('Ctrl Pts',(-1.7277317540471,-23.0162871884168,
0.));
#193587=CARTESIAN_POINT('Ctrl Pts',(-1.72978594832137,-23.001489160189,
0.));
#193588=CARTESIAN_POINT('Ctrl Pts',(-1.73177409750192,-22.9868367391978,
0.));
#193589=CARTESIAN_POINT('Ctrl Pts',(-1.73369672350816,-22.9723317685688,
0.));
#193590=CARTESIAN_POINT('Ctrl Pts',(-1.7355543616277,-22.9579761301063,
0.));
#193591=CARTESIAN_POINT('Ctrl Pts',(-1.7373475610004,-22.9437717457826,
0.));
#193592=CARTESIAN_POINT('Ctrl Pts',(-1.73907688511667,-22.9297205792586,
0.));
#193593=CARTESIAN_POINT('Ctrl Pts',(-1.74074291231059,-22.9158246373363,
0.));
#193594=CARTESIAN_POINT('Ctrl Pts',(-1.74234623630081,-22.9020859716141,
0.));
#193595=CARTESIAN_POINT('Ctrl Pts',(-1.74388746677703,-22.888506680335,
0.));
#193596=CARTESIAN_POINT('Ctrl Pts',(-1.74536722998202,-22.8750889101696,
0.));
#193597=CARTESIAN_POINT('Ctrl Pts',(-1.74678616930666,-22.8618348580235,
0.));
#193598=CARTESIAN_POINT('Ctrl Pts',(-1.74814494588494,-22.8487467728076,
0.));
#193599=CARTESIAN_POINT('Ctrl Pts',(-1.74944423940117,-22.8358269579853,
0.));
#193600=CARTESIAN_POINT('Ctrl Pts',(-1.75068474890884,-22.8230777741284,
0.));
#193601=CARTESIAN_POINT('Ctrl Pts',(-1.75186719365593,-22.8105016414713,
0.));
#193602=CARTESIAN_POINT('Ctrl Pts',(-1.75299231391467,-22.7981010424314,
0.));
#193603=CARTESIAN_POINT('Ctrl Pts',(-1.75406087182937,-22.7858785242361,
0.));
#193604=CARTESIAN_POINT('Ctrl Pts',(-1.75507365227133,-22.7738367016118,
0.));
#193605=CARTESIAN_POINT('Ctrl Pts',(-1.75603146371642,-22.7619782595013,
0.));
#193606=CARTESIAN_POINT('Ctrl Pts',(-1.75693513908908,-22.750305955645,
0.));
#193607=CARTESIAN_POINT('Ctrl Pts',(-1.75778553673245,-22.7388226235559,
0.));
#193608=CARTESIAN_POINT('Ctrl Pts',(-1.75858354204634,-22.72753117773,0.));
#193609=CARTESIAN_POINT('Ctrl Pts',(-1.75933006905926,-22.7164346186006,
0.));
#193610=CARTESIAN_POINT('Ctrl Pts',(-1.76002606202402,-22.7055360375485,
0.));
#193611=CARTESIAN_POINT('Ctrl Pts',(-1.76067249704888,-22.6948386219851,
0.));
#193612=CARTESIAN_POINT('Ctrl Pts',(-1.76127038310615,-22.684345658525,
0.));
#193613=CARTESIAN_POINT('Ctrl Pts',(-1.76182076289527,-22.67406053567,0.));
#193614=CARTESIAN_POINT('Ctrl Pts',(-1.7623247139257,-22.6639867471753,
0.));
#193615=CARTESIAN_POINT('Ctrl Pts',(-1.76278334912562,-22.654127893841,
0.));
#193616=CARTESIAN_POINT('Ctrl Pts',(-1.76319782013917,-22.6444876940423,
0.));
#193617=CARTESIAN_POINT('Ctrl Pts',(-1.76356932176274,-22.6350699979359,
0.));
#193618=CARTESIAN_POINT('Ctrl Pts',(-1.76389909571404,-22.6258787994848,
0.));
#193619=CARTESIAN_POINT('Ctrl Pts',(-1.7641884354374,-22.6169182517694,
0.));
#193620=CARTESIAN_POINT('Ctrl Pts',(-1.76443868648017,-22.6081926681343,
0.));
#193621=CARTESIAN_POINT('Ctrl Pts',(-1.76465124413558,-22.5997065145638,
0.));
#193622=CARTESIAN_POINT('Ctrl Pts',(-1.76482755288412,-22.5914644078106,
0.));
#193623=CARTESIAN_POINT('Ctrl Pts',(-1.76496910283089,-22.5834711038022,
0.));
#193624=CARTESIAN_POINT('Ctrl Pts',(-1.76507744026747,-22.5757315316353,
0.));
#193625=CARTESIAN_POINT('Ctrl Pts',(-1.76515418518832,-22.5682508499874,
0.));
#193626=CARTESIAN_POINT('Ctrl Pts',(-1.76520104500451,-22.5610344912501,
0.));
#193627=CARTESIAN_POINT('Ctrl Pts',(-1.76521983384063,-22.5540882235837,
0.));
#193628=CARTESIAN_POINT('Ctrl Pts',(-1.76521245524048,-22.5474180954006,
0.));
#193629=CARTESIAN_POINT('Ctrl Pts',(-1.76518087841494,-22.5410303590892,
0.));
#193630=CARTESIAN_POINT('Ctrl Pts',(-1.76512711563255,-22.5349313983571,
0.));
#193631=CARTESIAN_POINT('Ctrl Pts',(-1.7650532026276,-22.529127665298,0.));
#193632=CARTESIAN_POINT('Ctrl Pts',(-1.76496128643376,-22.5236259635515,
0.));
#193633=CARTESIAN_POINT('Ctrl Pts',(-1.76485369319896,-22.5184336670207,
0.));
#193634=CARTESIAN_POINT('Ctrl Pts',(-1.7647330328115,-22.5135590569554,
0.));
#193635=CARTESIAN_POINT('Ctrl Pts',(-1.76460218257314,-22.5090112700212,
0.));
#193636=CARTESIAN_POINT('Ctrl Pts',(-1.76446408210366,-22.5047996391978,
0.));
#193637=CARTESIAN_POINT('Ctrl Pts',(-1.76432160068739,-22.5009332677316,
0.));
#193638=CARTESIAN_POINT('Ctrl Pts',(-1.76417731243484,-22.4974203063191,
0.));
#193639=CARTESIAN_POINT('Ctrl Pts',(-1.76403393880317,-22.4942693792449,
0.));
#193640=CARTESIAN_POINT('Ctrl Pts',(-1.76389475965715,-22.4914909094908,
0.));
#193641=CARTESIAN_POINT('Ctrl Pts',(-1.76376424879469,-22.4890991659479,
0.));
#193642=CARTESIAN_POINT('Ctrl Pts',(-1.76364784232926,-22.4871115206572,
0.));
#193643=CARTESIAN_POINT('Ctrl Pts',(-1.7635507604555,-22.4855446605991,
0.));
#193644=CARTESIAN_POINT('Ctrl Pts',(-1.76347698284863,-22.4844112933125,
0.));
#193645=CARTESIAN_POINT('Ctrl Pts',(-1.7634381343466,-22.4838562517064,
0.));
#193646=CARTESIAN_POINT('Ctrl Pts',(-1.76342064263638,-22.4836387052228,
0.));
#193647=CARTESIAN_POINT('Ctrl Pts',(-1.76341415538792,-22.4835819929788,
0.));
#193648=CARTESIAN_POINT('Ctrl Pts',(-1.76341220531181,-22.4835757167854,
0.));
#193649=CARTESIAN_POINT('',(-0.661312440730913,-25.991588367311,0.));
#193650=CARTESIAN_POINT('Ctrl Pts',(-4.11585220600463,-22.1738711152697,
0.));
#193651=CARTESIAN_POINT('Ctrl Pts',(-4.11585220600463,-22.1738711152697,
12.));
#193652=CARTESIAN_POINT('Ctrl Pts',(-4.11585194677443,-22.173877682324,
0.));
#193653=CARTESIAN_POINT('Ctrl Pts',(-4.11585194677443,-22.173877682324,
12.));
#193654=CARTESIAN_POINT('Ctrl Pts',(-4.11586035878288,-22.1739341411687,
0.));
#193655=CARTESIAN_POINT('Ctrl Pts',(-4.11586035878288,-22.1739341411687,
12.));
#193656=CARTESIAN_POINT('Ctrl Pts',(-4.11589976826167,-22.1741488021234,
0.));
#193657=CARTESIAN_POINT('Ctrl Pts',(-4.11589976826167,-22.1741488021234,
12.));
#193658=CARTESIAN_POINT('Ctrl Pts',(-4.11600589882846,-22.1746949858775,
0.));
#193659=CARTESIAN_POINT('Ctrl Pts',(-4.11600589882846,-22.1746949858775,
12.));
#193660=CARTESIAN_POINT('Ctrl Pts',(-4.11622797217069,-22.1758088296598,
0.));
#193661=CARTESIAN_POINT('Ctrl Pts',(-4.11622797217069,-22.1758088296598,
12.));
#193662=CARTESIAN_POINT('Ctrl Pts',(-4.11653973150519,-22.177347426894,
0.));
#193663=CARTESIAN_POINT('Ctrl Pts',(-4.11653973150519,-22.177347426894,
12.));
#193664=CARTESIAN_POINT('Ctrl Pts',(-4.11694173195005,-22.179297473024,
0.));
#193665=CARTESIAN_POINT('Ctrl Pts',(-4.11694173195005,-22.179297473024,
12.));
#193666=CARTESIAN_POINT('Ctrl Pts',(-4.11743469691757,-22.1816414985788,
0.));
#193667=CARTESIAN_POINT('Ctrl Pts',(-4.11743469691757,-22.1816414985788,
12.));
#193668=CARTESIAN_POINT('Ctrl Pts',(-4.11801938107481,-22.1843613164855,
0.));
#193669=CARTESIAN_POINT('Ctrl Pts',(-4.11801938107481,-22.1843613164855,
12.));
#193670=CARTESIAN_POINT('Ctrl Pts',(-4.11869641271774,-22.1874419861496,
0.));
#193671=CARTESIAN_POINT('Ctrl Pts',(-4.11869641271774,-22.1874419861496,
12.));
#193672=CARTESIAN_POINT('Ctrl Pts',(-4.11946626228637,-22.1908725908525,
0.));
#193673=CARTESIAN_POINT('Ctrl Pts',(-4.11946626228637,-22.1908725908525,
12.));
#193674=CARTESIAN_POINT('Ctrl Pts',(-4.12032932637737,-22.1946440958098,
0.));
#193675=CARTESIAN_POINT('Ctrl Pts',(-4.12032932637737,-22.1946440958098,
12.));
#193676=CARTESIAN_POINT('Ctrl Pts',(-4.12128598183523,-22.1987479618246,
0.));
#193677=CARTESIAN_POINT('Ctrl Pts',(-4.12128598183523,-22.1987479618246,
12.));
#193678=CARTESIAN_POINT('Ctrl Pts',(-4.12233664408228,-22.2031746532106,
0.));
#193679=CARTESIAN_POINT('Ctrl Pts',(-4.12233664408228,-22.2031746532106,
12.));
#193680=CARTESIAN_POINT('Ctrl Pts',(-4.12348173702024,-22.2079143941719,
0.));
#193681=CARTESIAN_POINT('Ctrl Pts',(-4.12348173702024,-22.2079143941719,
12.));
#193682=CARTESIAN_POINT('Ctrl Pts',(-4.12472167516608,-22.2129576146671,
0.));
#193683=CARTESIAN_POINT('Ctrl Pts',(-4.12472167516608,-22.2129576146671,
12.));
#193684=CARTESIAN_POINT('Ctrl Pts',(-4.12605683613308,-22.2182956401341,
0.));
#193685=CARTESIAN_POINT('Ctrl Pts',(-4.12605683613308,-22.2182956401341,
12.));
#193686=CARTESIAN_POINT('Ctrl Pts',(-4.12748755830105,-22.2239207458781,
0.));
#193687=CARTESIAN_POINT('Ctrl Pts',(-4.12748755830105,-22.2239207458781,
12.));
#193688=CARTESIAN_POINT('Ctrl Pts',(-4.1290141546338,-22.2298258043947,
0.));
#193689=CARTESIAN_POINT('Ctrl Pts',(-4.1290141546338,-22.2298258043947,
12.));
#193690=CARTESIAN_POINT('Ctrl Pts',(-4.13063692157499,-22.2360040565533,
0.));
#193691=CARTESIAN_POINT('Ctrl Pts',(-4.13063692157499,-22.2360040565533,
12.));
#193692=CARTESIAN_POINT('Ctrl Pts',(-4.13235615060161,-22.2424488153523,
0.));
#193693=CARTESIAN_POINT('Ctrl Pts',(-4.13235615060161,-22.2424488153523,
12.));
#193694=CARTESIAN_POINT('Ctrl Pts',(-4.13417212558811,-22.249153531779,
0.));
#193695=CARTESIAN_POINT('Ctrl Pts',(-4.13417212558811,-22.249153531779,
12.));
#193696=CARTESIAN_POINT('Ctrl Pts',(-4.13608511977226,-22.2561118708421,
0.));
#193697=CARTESIAN_POINT('Ctrl Pts',(-4.13608511977226,-22.2561118708421,
12.));
#193698=CARTESIAN_POINT('Ctrl Pts',(-4.13809539255423,-22.2633177913972,
0.));
#193699=CARTESIAN_POINT('Ctrl Pts',(-4.13809539255423,-22.2633177913972,
12.));
#193700=CARTESIAN_POINT('Ctrl Pts',(-4.14020318715992,-22.2707656042457,
0.));
#193701=CARTESIAN_POINT('Ctrl Pts',(-4.14020318715992,-22.2707656042457,
12.));
#193702=CARTESIAN_POINT('Ctrl Pts',(-4.14240873321985,-22.2784499072027,
0.));
#193703=CARTESIAN_POINT('Ctrl Pts',(-4.14240873321985,-22.2784499072027,
12.));
#193704=CARTESIAN_POINT('Ctrl Pts',(-4.14471224859296,-22.2863655389166,
0.));
#193705=CARTESIAN_POINT('Ctrl Pts',(-4.14471224859296,-22.2863655389166,
12.));
#193706=CARTESIAN_POINT('Ctrl Pts',(-4.14711394168557,-22.2945075198467,
0.));
#193707=CARTESIAN_POINT('Ctrl Pts',(-4.14711394168557,-22.2945075198467,
12.));
#193708=CARTESIAN_POINT('Ctrl Pts',(-4.14961401285523,-22.3028710166933,
0.));
#193709=CARTESIAN_POINT('Ctrl Pts',(-4.14961401285523,-22.3028710166933,
12.));
#193710=CARTESIAN_POINT('Ctrl Pts',(-4.15221265396991,-22.3114513545185,
0.));
#193711=CARTESIAN_POINT('Ctrl Pts',(-4.15221265396991,-22.3114513545185,
12.));
#193712=CARTESIAN_POINT('Ctrl Pts',(-4.15491004835282,-22.320244018698,
0.));
#193713=CARTESIAN_POINT('Ctrl Pts',(-4.15491004835282,-22.320244018698,
12.));
#193714=CARTESIAN_POINT('Ctrl Pts',(-4.15770637047891,-22.3292446628959,
0.));
#193715=CARTESIAN_POINT('Ctrl Pts',(-4.15770637047891,-22.3292446628959,
12.));
#193716=CARTESIAN_POINT('Ctrl Pts',(-4.16060178604165,-22.3384491078602,
0.));
#193717=CARTESIAN_POINT('Ctrl Pts',(-4.16060178604165,-22.3384491078602,
12.));
#193718=CARTESIAN_POINT('Ctrl Pts',(-4.16359645263189,-22.3478533253889,
0.));
#193719=CARTESIAN_POINT('Ctrl Pts',(-4.16359645263189,-22.3478533253889,
12.));
#193720=CARTESIAN_POINT('Ctrl Pts',(-4.16669052026601,-22.3574534257396,
0.));
#193721=CARTESIAN_POINT('Ctrl Pts',(-4.16669052026601,-22.3574534257396,
12.));
#193722=CARTESIAN_POINT('Ctrl Pts',(-4.16988413199458,-22.36724564276,0.));
#193723=CARTESIAN_POINT('Ctrl Pts',(-4.16988413199458,-22.36724564276,12.));
#193724=CARTESIAN_POINT('Ctrl Pts',(-4.17317742436146,-22.3772263228617,
0.));
#193725=CARTESIAN_POINT('Ctrl Pts',(-4.17317742436146,-22.3772263228617,
12.));
#193726=CARTESIAN_POINT('Ctrl Pts',(-4.17657052752826,-22.3873919231334,
0.));
#193727=CARTESIAN_POINT('Ctrl Pts',(-4.17657052752826,-22.3873919231334,
12.));
#193728=CARTESIAN_POINT('Ctrl Pts',(-4.18006356544883,-22.3977390078075,
0.));
#193729=CARTESIAN_POINT('Ctrl Pts',(-4.18006356544883,-22.3977390078075,
12.));
#193730=CARTESIAN_POINT('Ctrl Pts',(-4.18365665600851,-22.4082642454453,
0.));
#193731=CARTESIAN_POINT('Ctrl Pts',(-4.18365665600851,-22.4082642454453,
12.));
#193732=CARTESIAN_POINT('Ctrl Pts',(-4.18734991117722,-22.4189644056115,
0.));
#193733=CARTESIAN_POINT('Ctrl Pts',(-4.18734991117722,-22.4189644056115,
12.));
#193734=CARTESIAN_POINT('Ctrl Pts',(-4.19114343726943,-22.4298363535421,
0.));
#193735=CARTESIAN_POINT('Ctrl Pts',(-4.19114343726943,-22.4298363535421,
12.));
#193736=CARTESIAN_POINT('Ctrl Pts',(-4.19503733518862,-22.4408770448917,
0.));
#193737=CARTESIAN_POINT('Ctrl Pts',(-4.19503733518862,-22.4408770448917,
12.));
#193738=CARTESIAN_POINT('Ctrl Pts',(-4.19903170066356,-22.4520835205419,
0.));
#193739=CARTESIAN_POINT('Ctrl Pts',(-4.19903170066356,-22.4520835205419,
12.));
#193740=CARTESIAN_POINT('Ctrl Pts',(-4.20312662448172,-22.4634529011433,
0.));
#193741=CARTESIAN_POINT('Ctrl Pts',(-4.20312662448172,-22.4634529011433,
12.));
#193742=CARTESIAN_POINT('Ctrl Pts',(-4.20732219265649,-22.4749823839915,
0.));
#193743=CARTESIAN_POINT('Ctrl Pts',(-4.20732219265649,-22.4749823839915,
12.));
#193744=CARTESIAN_POINT('Ctrl Pts',(-4.21161848657429,-22.4866692403147,
0.));
#193745=CARTESIAN_POINT('Ctrl Pts',(-4.21161848657429,-22.4866692403147,
12.));
#193746=CARTESIAN_POINT('Ctrl Pts',(-4.21601558313909,-22.4985108124229,
0.));
#193747=CARTESIAN_POINT('Ctrl Pts',(-4.21601558313909,-22.4985108124229,
12.));
#193748=CARTESIAN_POINT('Ctrl Pts',(-4.22051355490198,-22.5105045108882,
0.));
#193749=CARTESIAN_POINT('Ctrl Pts',(-4.22051355490198,-22.5105045108882,
12.));
#193750=CARTESIAN_POINT('Ctrl Pts',(-4.22511247020041,-22.5226478117885,
0.));
#193751=CARTESIAN_POINT('Ctrl Pts',(-4.22511247020041,-22.5226478117885,
12.));
#193752=CARTESIAN_POINT('Ctrl Pts',(-4.22981239330732,-22.5349382540587,
0.));
#193753=CARTESIAN_POINT('Ctrl Pts',(-4.22981239330732,-22.5349382540587,
12.));
#193754=CARTESIAN_POINT('Ctrl Pts',(-4.23461338456714,-22.5473734368086,
0.));
#193755=CARTESIAN_POINT('Ctrl Pts',(-4.23461338456714,-22.5473734368086,
12.));
#193756=CARTESIAN_POINT('Ctrl Pts',(-4.23951550052527,-22.559951016643,
0.));
#193757=CARTESIAN_POINT('Ctrl Pts',(-4.23951550052527,-22.559951016643,
12.));
#193758=CARTESIAN_POINT('Ctrl Pts',(-4.2445187940486,-22.5726687049922,
0.));
#193759=CARTESIAN_POINT('Ctrl Pts',(-4.2445187940486,-22.5726687049922,
12.));
#193760=CARTESIAN_POINT('Ctrl Pts',(-4.24962331444186,-22.5855242662479,
0.));
#193761=CARTESIAN_POINT('Ctrl Pts',(-4.24962331444186,-22.5855242662479,
12.));
#193762=CARTESIAN_POINT('Ctrl Pts',(-4.25482910755486,-22.5985155158637,
0.));
#193763=CARTESIAN_POINT('Ctrl Pts',(-4.25482910755486,-22.5985155158637,
12.));
#193764=CARTESIAN_POINT('Ctrl Pts',(-4.26013621588304,-22.611640318482,
0.));
#193765=CARTESIAN_POINT('Ctrl Pts',(-4.26013621588304,-22.611640318482,
12.));
#193766=CARTESIAN_POINT('Ctrl Pts',(-4.26554467865572,-22.6248965859975,
0.));
#193767=CARTESIAN_POINT('Ctrl Pts',(-4.26554467865572,-22.6248965859975,
12.));
#193768=CARTESIAN_POINT('Ctrl Pts',(-4.27105453193,-22.6382822758171,0.));
#193769=CARTESIAN_POINT('Ctrl Pts',(-4.27105453193,-22.6382822758171,12.));
#193770=CARTESIAN_POINT('Ctrl Pts',(-4.27666580869118,-22.6517953893303,
0.));
#193771=CARTESIAN_POINT('Ctrl Pts',(-4.27666580869118,-22.6517953893303,
12.));
#193772=CARTESIAN_POINT('Ctrl Pts',(-4.2823785389406,-22.665433970311,0.));
#193773=CARTESIAN_POINT('Ctrl Pts',(-4.2823785389406,-22.665433970311,12.));
#193774=CARTESIAN_POINT('Ctrl Pts',(-4.28819274977767,-22.6791961033536,
0.));
#193775=CARTESIAN_POINT('Ctrl Pts',(-4.28819274977767,-22.6791961033536,
12.));
#193776=CARTESIAN_POINT('Ctrl Pts',(-4.29410846547062,-22.6930799122545,
0.));
#193777=CARTESIAN_POINT('Ctrl Pts',(-4.29410846547062,-22.6930799122545,
12.));
#193778=CARTESIAN_POINT('Ctrl Pts',(-4.30012570754067,-22.707083558756,
0.));
#193779=CARTESIAN_POINT('Ctrl Pts',(-4.30012570754067,-22.707083558756,
12.));
#193780=CARTESIAN_POINT('Ctrl Pts',(-4.30624449484075,-22.7212052413384,
0.));
#193781=CARTESIAN_POINT('Ctrl Pts',(-4.30624449484075,-22.7212052413384,
12.));
#193782=CARTESIAN_POINT('Ctrl Pts',(-4.31246484362551,-22.7354431939926,
0.));
#193783=CARTESIAN_POINT('Ctrl Pts',(-4.31246484362551,-22.7354431939926,
12.));
#193784=CARTESIAN_POINT('Ctrl Pts',(-4.31878676761231,-22.7497956849852,
0.));
#193785=CARTESIAN_POINT('Ctrl Pts',(-4.31878676761231,-22.7497956849852,
12.));
#193786=CARTESIAN_POINT('Ctrl Pts',(-4.32521027803748,-22.764261015648,
0.));
#193787=CARTESIAN_POINT('Ctrl Pts',(-4.32521027803748,-22.764261015648,
12.));
#193788=CARTESIAN_POINT('Ctrl Pts',(-4.33173538373183,-22.7788375194081,
0.));
#193789=CARTESIAN_POINT('Ctrl Pts',(-4.33173538373183,-22.7788375194081,
12.));
#193790=CARTESIAN_POINT('Ctrl Pts',(-4.33836209118444,-22.7935235607807,
0.));
#193791=CARTESIAN_POINT('Ctrl Pts',(-4.33836209118444,-22.7935235607807,
12.));
#193792=CARTESIAN_POINT('Ctrl Pts',(-4.34509040460066,-22.808317534379,
0.));
#193793=CARTESIAN_POINT('Ctrl Pts',(-4.34509040460066,-22.808317534379,
12.));
#193794=CARTESIAN_POINT('Ctrl Pts',(-4.35192032594802,-22.8232178638873,
0.));
#193795=CARTESIAN_POINT('Ctrl Pts',(-4.35192032594802,-22.8232178638873,
12.));
#193796=CARTESIAN_POINT('Ctrl Pts',(-4.3588518550056,-22.838223001118,0.));
#193797=CARTESIAN_POINT('Ctrl Pts',(-4.3588518550056,-22.838223001118,12.));
#193798=CARTESIAN_POINT('Ctrl Pts',(-4.36588498943011,-22.8533314252419,
0.));
#193799=CARTESIAN_POINT('Ctrl Pts',(-4.36588498943011,-22.8533314252419,
12.));
#193800=CARTESIAN_POINT('Ctrl Pts',(-4.37301972480753,-22.8685416419725,
0.));
#193801=CARTESIAN_POINT('Ctrl Pts',(-4.37301972480753,-22.8685416419725,
12.));
#193802=CARTESIAN_POINT('Ctrl Pts',(-4.38025605470091,-22.8838521827702,
0.));
#193803=CARTESIAN_POINT('Ctrl Pts',(-4.38025605470091,-22.8838521827702,
12.));
#193804=CARTESIAN_POINT('Ctrl Pts',(-4.38759397068393,-22.8992616040108,
0.));
#193805=CARTESIAN_POINT('Ctrl Pts',(-4.38759397068393,-22.8992616040108,
12.));
#193806=CARTESIAN_POINT('Ctrl Pts',(-4.39503346238455,-22.9147684862425,
0.));
#193807=CARTESIAN_POINT('Ctrl Pts',(-4.39503346238455,-22.9147684862425,
12.));
#193808=CARTESIAN_POINT('Ctrl Pts',(-4.40257451754308,-22.9303714335549,
0.));
#193809=CARTESIAN_POINT('Ctrl Pts',(-4.40257451754308,-22.9303714335549,
12.));
#193810=CARTESIAN_POINT('Ctrl Pts',(-4.41021712205549,-22.9460690729093,
0.));
#193811=CARTESIAN_POINT('Ctrl Pts',(-4.41021712205549,-22.9460690729093,
12.));
#193812=CARTESIAN_POINT('Ctrl Pts',(-4.41796126001311,-22.9618600534866,
0.));
#193813=CARTESIAN_POINT('Ctrl Pts',(-4.41796126001311,-22.9618600534866,
12.));
#193814=CARTESIAN_POINT('Ctrl Pts',(-4.42580691372772,-22.9777430460021,
0.));
#193815=CARTESIAN_POINT('Ctrl Pts',(-4.42580691372772,-22.9777430460021,
12.));
#193816=CARTESIAN_POINT('Ctrl Pts',(-4.43375406376906,-22.9937167421009,
0.));
#193817=CARTESIAN_POINT('Ctrl Pts',(-4.43375406376906,-22.9937167421009,
12.));
#193818=CARTESIAN_POINT('Ctrl Pts',(-4.44180268901667,-23.0097798538399,
0.));
#193819=CARTESIAN_POINT('Ctrl Pts',(-4.44180268901667,-23.0097798538399,
12.));
#193820=CARTESIAN_POINT('Ctrl Pts',(-4.44995276669699,-23.0259311131395,
0.));
#193821=CARTESIAN_POINT('Ctrl Pts',(-4.44995276669699,-23.0259311131395,
12.));
#193822=CARTESIAN_POINT('Ctrl Pts',(-4.45820427241677,-23.0421692712466,
0.));
#193823=CARTESIAN_POINT('Ctrl Pts',(-4.45820427241677,-23.0421692712466,
12.));
#193824=CARTESIAN_POINT('Ctrl Pts',(-4.46655718018206,-23.0584930981723,
0.));
#193825=CARTESIAN_POINT('Ctrl Pts',(-4.46655718018206,-23.0584930981723,
12.));
#193826=CARTESIAN_POINT('Ctrl Pts',(-4.47501146242822,-23.0749013821867,
0.));
#193827=CARTESIAN_POINT('Ctrl Pts',(-4.47501146242822,-23.0749013821867,
12.));
#193828=CARTESIAN_POINT('Ctrl Pts',(-4.48356709006757,-23.0913929293909,
0.));
#193829=CARTESIAN_POINT('Ctrl Pts',(-4.48356709006757,-23.0913929293909,
12.));
#193830=CARTESIAN_POINT('Ctrl Pts',(-4.49222403252202,-23.1079665632629,
0.));
#193831=CARTESIAN_POINT('Ctrl Pts',(-4.49222403252202,-23.1079665632629,
12.));
#193832=CARTESIAN_POINT('Ctrl Pts',(-4.50098225775179,-23.1246211242117,
0.));
#193833=CARTESIAN_POINT('Ctrl Pts',(-4.50098225775179,-23.1246211242117,
12.));
#193834=CARTESIAN_POINT('Ctrl Pts',(-4.50984173227088,-23.1413554691136,
0.));
#193835=CARTESIAN_POINT('Ctrl Pts',(-4.50984173227088,-23.1413554691136,
12.));
#193836=CARTESIAN_POINT('Ctrl Pts',(-4.51880242116786,-23.1581684708778,
0.));
#193837=CARTESIAN_POINT('Ctrl Pts',(-4.51880242116786,-23.1581684708778,
12.));
#193838=CARTESIAN_POINT('Ctrl Pts',(-4.52786428815049,-23.1750590180923,
0.));
#193839=CARTESIAN_POINT('Ctrl Pts',(-4.52786428815049,-23.1750590180923,
12.));
#193840=CARTESIAN_POINT('Ctrl Pts',(-4.53702729557586,-23.1920260146474,
0.));
#193841=CARTESIAN_POINT('Ctrl Pts',(-4.53702729557586,-23.1920260146474,
12.));
#193842=CARTESIAN_POINT('Ctrl Pts',(-4.54629140447543,-23.2090683793627,
0.));
#193843=CARTESIAN_POINT('Ctrl Pts',(-4.54629140447543,-23.2090683793627,
12.));
#193844=CARTESIAN_POINT('Ctrl Pts',(-4.55565657456957,-23.2261850456055,
0.));
#193845=CARTESIAN_POINT('Ctrl Pts',(-4.55565657456957,-23.2261850456055,
12.));
#193846=CARTESIAN_POINT('Ctrl Pts',(-4.56512276427812,-23.2433749609117,
0.));
#193847=CARTESIAN_POINT('Ctrl Pts',(-4.56512276427812,-23.2433749609117,
12.));
#193848=CARTESIAN_POINT('Ctrl Pts',(-4.57468993076071,-23.2606370866854,
0.));
#193849=CARTESIAN_POINT('Ctrl Pts',(-4.57468993076071,-23.2606370866854,
12.));
#193850=CARTESIAN_POINT('Ctrl Pts',(-4.58435802994675,-23.2779703978868,
0.));
#193851=CARTESIAN_POINT('Ctrl Pts',(-4.58435802994675,-23.2779703978868,
12.));
#193852=CARTESIAN_POINT('Ctrl Pts',(-4.5941270165575,-23.295373882719,0.));
#193853=CARTESIAN_POINT('Ctrl Pts',(-4.5941270165575,-23.295373882719,12.));
#193854=CARTESIAN_POINT('Ctrl Pts',(-4.60399684412176,-23.3128465423119,
0.));
#193855=CARTESIAN_POINT('Ctrl Pts',(-4.60399684412176,-23.3128465423119,
12.));
#193856=CARTESIAN_POINT('Ctrl Pts',(-4.61396746497849,-23.3303873903947,
0.));
#193857=CARTESIAN_POINT('Ctrl Pts',(-4.61396746497849,-23.3303873903947,
12.));
#193858=CARTESIAN_POINT('Ctrl Pts',(-4.62403883030825,-23.3479954530281,
0.));
#193859=CARTESIAN_POINT('Ctrl Pts',(-4.62403883030825,-23.3479954530281,
12.));
#193860=CARTESIAN_POINT('Ctrl Pts',(-4.63421089016555,-23.3656697683496,
0.));
#193861=CARTESIAN_POINT('Ctrl Pts',(-4.63421089016555,-23.3656697683496,
12.));
#193862=CARTESIAN_POINT('Ctrl Pts',(-4.64448359349936,-23.383409386307,
0.));
#193863=CARTESIAN_POINT('Ctrl Pts',(-4.64448359349936,-23.383409386307,
12.));
#193864=CARTESIAN_POINT('Ctrl Pts',(-4.65485688816923,-23.4012133683957,
0.));
#193865=CARTESIAN_POINT('Ctrl Pts',(-4.65485688816923,-23.4012133683957,
12.));
#193866=CARTESIAN_POINT('Ctrl Pts',(-4.66533072094664,-23.4190807873798,
0.));
#193867=CARTESIAN_POINT('Ctrl Pts',(-4.66533072094664,-23.4190807873798,
12.));
#193868=CARTESIAN_POINT('Ctrl Pts',(-4.67590503753051,-23.4370107270444,
0.));
#193869=CARTESIAN_POINT('Ctrl Pts',(-4.67590503753051,-23.4370107270444,
12.));
#193870=CARTESIAN_POINT('Ctrl Pts',(-4.68657978258298,-23.4550022819852,
0.));
#193871=CARTESIAN_POINT('Ctrl Pts',(-4.68657978258298,-23.4550022819852,
12.));
#193872=CARTESIAN_POINT('Ctrl Pts',(-4.69735489975024,-23.4730545573849,
0.));
#193873=CARTESIAN_POINT('Ctrl Pts',(-4.69735489975024,-23.4730545573849,
12.));
#193874=CARTESIAN_POINT('Ctrl Pts',(-4.70823033167821,-23.491166668789,
0.));
#193875=CARTESIAN_POINT('Ctrl Pts',(-4.70823033167821,-23.491166668789,
12.));
#193876=CARTESIAN_POINT('Ctrl Pts',(-4.71920602001905,-23.5093377418784,
0.));
#193877=CARTESIAN_POINT('Ctrl Pts',(-4.71920602001905,-23.5093377418784,
12.));
#193878=CARTESIAN_POINT('Ctrl Pts',(-4.73028190543032,-23.5275669122378,
0.));
#193879=CARTESIAN_POINT('Ctrl Pts',(-4.73028190543032,-23.5275669122378,
12.));
#193880=CARTESIAN_POINT('Ctrl Pts',(-4.74145792760699,-23.5458533251715,
0.));
#193881=CARTESIAN_POINT('Ctrl Pts',(-4.74145792760699,-23.5458533251715,
12.));
#193882=CARTESIAN_POINT('Ctrl Pts',(-4.75273402530616,-23.564196135517,
0.));
#193883=CARTESIAN_POINT('Ctrl Pts',(-4.75273402530616,-23.564196135517,
12.));
#193884=CARTESIAN_POINT('Ctrl Pts',(-4.76411013636252,-23.5825945074535,
0.));
#193885=CARTESIAN_POINT('Ctrl Pts',(-4.76411013636252,-23.5825945074535,
12.));
#193886=CARTESIAN_POINT('Ctrl Pts',(-4.77558619769876,-23.6010476143099,
0.));
#193887=CARTESIAN_POINT('Ctrl Pts',(-4.77558619769876,-23.6010476143099,
12.));
#193888=CARTESIAN_POINT('Ctrl Pts',(-4.78716214532105,-23.6195546383625,
0.));
#193889=CARTESIAN_POINT('Ctrl Pts',(-4.78716214532105,-23.6195546383625,
12.));
#193890=CARTESIAN_POINT('Ctrl Pts',(-4.79883791433231,-23.6381147706581,
0.));
#193891=CARTESIAN_POINT('Ctrl Pts',(-4.79883791433231,-23.6381147706581,
12.));
#193892=CARTESIAN_POINT('Ctrl Pts',(-4.81061343896443,-23.6567272108631,
0.));
#193893=CARTESIAN_POINT('Ctrl Pts',(-4.81061343896443,-23.6567272108631,
12.));
#193894=CARTESIAN_POINT('Ctrl Pts',(-4.82248865259571,-23.6753911671023,
0.));
#193895=CARTESIAN_POINT('Ctrl Pts',(-4.82248865259571,-23.6753911671023,
12.));
#193896=CARTESIAN_POINT('Ctrl Pts',(-4.83446348776268,-23.6941058557971,
0.));
#193897=CARTESIAN_POINT('Ctrl Pts',(-4.83446348776268,-23.6941058557971,
12.));
#193898=CARTESIAN_POINT('Ctrl Pts',(-4.84653787616424,-23.7128705015014,
0.));
#193899=CARTESIAN_POINT('Ctrl Pts',(-4.84653787616424,-23.7128705015014,
12.));
#193900=CARTESIAN_POINT('Ctrl Pts',(-4.85871174865492,-23.7316843367308,
0.));
#193901=CARTESIAN_POINT('Ctrl Pts',(-4.85871174865492,-23.7316843367308,
12.));
#193902=CARTESIAN_POINT('Ctrl Pts',(-4.87098503527144,-23.7505466018239,
0.));
#193903=CARTESIAN_POINT('Ctrl Pts',(-4.87098503527144,-23.7505466018239,
12.));
#193904=CARTESIAN_POINT('Ctrl Pts',(-4.88335766525566,-23.7694565448044,
0.));
#193905=CARTESIAN_POINT('Ctrl Pts',(-4.88335766525566,-23.7694565448044,
12.));
#193906=CARTESIAN_POINT('Ctrl Pts',(-4.89582956706772,-23.7884134212381,
0.));
#193907=CARTESIAN_POINT('Ctrl Pts',(-4.89582956706772,-23.7884134212381,
12.));
#193908=CARTESIAN_POINT('Ctrl Pts',(-4.90840066839348,-23.8074164940897,
0.));
#193909=CARTESIAN_POINT('Ctrl Pts',(-4.90840066839348,-23.8074164940897,
12.));
#193910=CARTESIAN_POINT('Ctrl Pts',(-4.92107089613977,-23.8264650335721,
0.));
#193911=CARTESIAN_POINT('Ctrl Pts',(-4.92107089613977,-23.8264650335721,
12.));
#193912=CARTESIAN_POINT('Ctrl Pts',(-4.93384017643442,-23.8455583170062,
0.));
#193913=CARTESIAN_POINT('Ctrl Pts',(-4.93384017643442,-23.8455583170062,
12.));
#193914=CARTESIAN_POINT('Ctrl Pts',(-4.94670843465869,-23.8646956287172,
0.));
#193915=CARTESIAN_POINT('Ctrl Pts',(-4.94670843465869,-23.8646956287172,
12.));
#193916=CARTESIAN_POINT('Ctrl Pts',(-4.95967559546566,-23.883876259922,
0.));
#193917=CARTESIAN_POINT('Ctrl Pts',(-4.95967559546566,-23.883876259922,
12.));
#193918=CARTESIAN_POINT('Ctrl Pts',(-4.9727415827923,-23.9030995086164,
0.));
#193919=CARTESIAN_POINT('Ctrl Pts',(-4.9727415827923,-23.9030995086164,
12.));
#193920=CARTESIAN_POINT('Ctrl Pts',(-4.98590631986534,-23.9223646794591,
0.));
#193921=CARTESIAN_POINT('Ctrl Pts',(-4.98590631986534,-23.9223646794591,
12.));
#193922=CARTESIAN_POINT('Ctrl Pts',(-4.9991697291931,-23.9416710836529,
0.));
#193923=CARTESIAN_POINT('Ctrl Pts',(-4.9991697291931,-23.9416710836529,
12.));
#193924=CARTESIAN_POINT('Ctrl Pts',(-5.01253173257459,-23.9610180388271,
0.));
#193925=CARTESIAN_POINT('Ctrl Pts',(-5.01253173257459,-23.9610180388271,
12.));
#193926=CARTESIAN_POINT('Ctrl Pts',(-5.02599225112462,-23.9804048689228,
0.));
#193927=CARTESIAN_POINT('Ctrl Pts',(-5.02599225112462,-23.9804048689228,
12.));
#193928=CARTESIAN_POINT('Ctrl Pts',(-5.03955120528528,-23.9998309040747,
0.));
#193929=CARTESIAN_POINT('Ctrl Pts',(-5.03955120528528,-23.9998309040747,
12.));
#193930=CARTESIAN_POINT('Ctrl Pts',(-5.05320851483069,-24.0192954804896,
0.));
#193931=CARTESIAN_POINT('Ctrl Pts',(-5.05320851483069,-24.0192954804896,
12.));
#193932=CARTESIAN_POINT('Ctrl Pts',(-5.0669640988664,-24.0387979403268,
0.));
#193933=CARTESIAN_POINT('Ctrl Pts',(-5.0669640988664,-24.0387979403268,
12.));
#193934=CARTESIAN_POINT('Ctrl Pts',(-5.08081787581271,-24.0583376315636,
0.));
#193935=CARTESIAN_POINT('Ctrl Pts',(-5.08081787581271,-24.0583376315636,
12.));
#193936=CARTESIAN_POINT('Ctrl Pts',(-5.09476976342618,-24.0779139079264,
0.));
#193937=CARTESIAN_POINT('Ctrl Pts',(-5.09476976342618,-24.0779139079264,
12.));
#193938=CARTESIAN_POINT('Ctrl Pts',(-5.10881967883126,-24.0975261288444,
0.));
#193939=CARTESIAN_POINT('Ctrl Pts',(-5.10881967883126,-24.0975261288444,
12.));
#193940=CARTESIAN_POINT('Ctrl Pts',(-5.12296753853858,-24.117173659394,
0.));
#193941=CARTESIAN_POINT('Ctrl Pts',(-5.12296753853858,-24.117173659394,
12.));
#193942=CARTESIAN_POINT('Ctrl Pts',(-5.13721325845746,-24.1368558702443,
0.));
#193943=CARTESIAN_POINT('Ctrl Pts',(-5.13721325845746,-24.1368558702443,
12.));
#193944=CARTESIAN_POINT('Ctrl Pts',(-5.1515567539008,-24.1565721375971,
0.));
#193945=CARTESIAN_POINT('Ctrl Pts',(-5.1515567539008,-24.1565721375971,
12.));
#193946=CARTESIAN_POINT('Ctrl Pts',(-5.16599793957987,-24.1763218431344,
0.));
#193947=CARTESIAN_POINT('Ctrl Pts',(-5.16599793957987,-24.1763218431344,
12.));
#193948=CARTESIAN_POINT('Ctrl Pts',(-5.180536729614,-24.1961043738756,0.));
#193949=CARTESIAN_POINT('Ctrl Pts',(-5.180536729614,-24.1961043738756,12.));
#193950=CARTESIAN_POINT('Ctrl Pts',(-5.19517303753648,-24.2159191220171,
0.));
#193951=CARTESIAN_POINT('Ctrl Pts',(-5.19517303753648,-24.2159191220171,
12.));
#193952=CARTESIAN_POINT('Ctrl Pts',(-5.20990677629177,-24.2357654847766,
0.));
#193953=CARTESIAN_POINT('Ctrl Pts',(-5.20990677629177,-24.2357654847766,
12.));
#193954=CARTESIAN_POINT('Ctrl Pts',(-5.22473785822443,-24.2556428642294,
0.));
#193955=CARTESIAN_POINT('Ctrl Pts',(-5.22473785822443,-24.2556428642294,
12.));
#193956=CARTESIAN_POINT('Ctrl Pts',(-5.2396661950629,-24.2755506671525,
0.));
#193957=CARTESIAN_POINT('Ctrl Pts',(-5.2396661950629,-24.2755506671525,
12.));
#193958=CARTESIAN_POINT('Ctrl Pts',(-5.25469169788857,-24.2954883048447,
0.));
#193959=CARTESIAN_POINT('Ctrl Pts',(-5.25469169788857,-24.2954883048447,
12.));
#193960=CARTESIAN_POINT('Ctrl Pts',(-5.269814277188,-24.3154551932221,0.));
#193961=CARTESIAN_POINT('Ctrl Pts',(-5.269814277188,-24.3154551932221,12.));
#193962=CARTESIAN_POINT('Ctrl Pts',(-5.28503384290649,-24.3354507529414,
0.));
#193963=CARTESIAN_POINT('Ctrl Pts',(-5.28503384290649,-24.3354507529414,
12.));
#193964=CARTESIAN_POINT('Ctrl Pts',(-5.30035030449064,-24.3554744095075,
0.));
#193965=CARTESIAN_POINT('Ctrl Pts',(-5.30035030449064,-24.3554744095075,
12.));
#193966=CARTESIAN_POINT('Ctrl Pts',(-5.31576357092527,-24.3755255933917,
0.));
#193967=CARTESIAN_POINT('Ctrl Pts',(-5.31576357092527,-24.3755255933917,
12.));
#193968=CARTESIAN_POINT('Ctrl Pts',(-5.33127355076035,-24.3956037401293,
0.));
#193969=CARTESIAN_POINT('Ctrl Pts',(-5.33127355076035,-24.3956037401293,
12.));
#193970=CARTESIAN_POINT('Ctrl Pts',(-5.34688015213538,-24.4157082904614,
0.));
#193971=CARTESIAN_POINT('Ctrl Pts',(-5.34688015213538,-24.4157082904614,
12.));
#193972=CARTESIAN_POINT('Ctrl Pts',(-5.36258328273628,-24.435838689915,
0.));
#193973=CARTESIAN_POINT('Ctrl Pts',(-5.36258328273628,-24.435838689915,
12.));
#193974=CARTESIAN_POINT('Ctrl Pts',(-5.37838284973696,-24.4559943883157,
0.));
#193975=CARTESIAN_POINT('Ctrl Pts',(-5.37838284973696,-24.4559943883157,
12.));
#193976=CARTESIAN_POINT('Ctrl Pts',(-5.39427875973825,-24.4761748393321,
0.));
#193977=CARTESIAN_POINT('Ctrl Pts',(-5.39427875973825,-24.4761748393321,
12.));
#193978=CARTESIAN_POINT('Ctrl Pts',(-5.41027091869242,-24.496379499983,
0.));
#193979=CARTESIAN_POINT('Ctrl Pts',(-5.41027091869242,-24.496379499983,
12.));
#193980=CARTESIAN_POINT('Ctrl Pts',(-5.4263592318342,-24.5166078302108,
0.));
#193981=CARTESIAN_POINT('Ctrl Pts',(-5.4263592318342,-24.5166078302108,
12.));
#193982=CARTESIAN_POINT('Ctrl Pts',(-5.44254360356881,-24.5368592922863,
0.));
#193983=CARTESIAN_POINT('Ctrl Pts',(-5.44254360356881,-24.5368592922863,
12.));
#193984=CARTESIAN_POINT('Ctrl Pts',(-5.45882393762262,-24.5571333514842,
0.));
#193985=CARTESIAN_POINT('Ctrl Pts',(-5.45882393762262,-24.5571333514842,
12.));
#193986=CARTESIAN_POINT('Ctrl Pts',(-5.4752001372442,-24.5774294770329,
0.));
#193987=CARTESIAN_POINT('Ctrl Pts',(-5.4752001372442,-24.5774294770329,
12.));
#193988=CARTESIAN_POINT('Ctrl Pts',(-5.49167210537248,-24.5977471429364,
0.));
#193989=CARTESIAN_POINT('Ctrl Pts',(-5.49167210537248,-24.5977471429364,
12.));
#193990=CARTESIAN_POINT('Ctrl Pts',(-5.50823974481963,-24.6180858289179,
0.));
#193991=CARTESIAN_POINT('Ctrl Pts',(-5.50823974481963,-24.6180858289179,
12.));
#193992=CARTESIAN_POINT('Ctrl Pts',(-5.52490295840993,-24.6384450211467,
0.));
#193993=CARTESIAN_POINT('Ctrl Pts',(-5.52490295840993,-24.6384450211467,
12.));
#193994=CARTESIAN_POINT('Ctrl Pts',(-5.54166164919584,-24.6588242134738,
0.));
#193995=CARTESIAN_POINT('Ctrl Pts',(-5.54166164919584,-24.6588242134738,
12.));
#193996=CARTESIAN_POINT('Ctrl Pts',(-5.55851572025377,-24.6792229061794,
0.));
#193997=CARTESIAN_POINT('Ctrl Pts',(-5.55851572025377,-24.6792229061794,
12.));
#193998=CARTESIAN_POINT('Ctrl Pts',(-5.57546507427756,-24.6996406035517,
0.));
#193999=CARTESIAN_POINT('Ctrl Pts',(-5.57546507427756,-24.6996406035517,
12.));
#194000=CARTESIAN_POINT('Ctrl Pts',(-5.59250961323988,-24.7200768119088,
0.));
#194001=CARTESIAN_POINT('Ctrl Pts',(-5.59250961323988,-24.7200768119088,
12.));
#194002=CARTESIAN_POINT('Ctrl Pts',(-5.60964923798492,-24.7405310372739,
0.));
#194003=CARTESIAN_POINT('Ctrl Pts',(-5.60964923798492,-24.7405310372739,
12.));
#194004=CARTESIAN_POINT('Ctrl Pts',(-5.62688384790924,-24.7610027835697,
0.));
#194005=CARTESIAN_POINT('Ctrl Pts',(-5.62688384790924,-24.7610027835697,
12.));
#194006=CARTESIAN_POINT('Ctrl Pts',(-5.64421334042262,-24.781491549672,
0.));
#194007=CARTESIAN_POINT('Ctrl Pts',(-5.64421334042262,-24.781491549672,
12.));
#194008=CARTESIAN_POINT('Ctrl Pts',(-5.66163761114922,-24.8019968304605,
0.));
#194009=CARTESIAN_POINT('Ctrl Pts',(-5.66163761114922,-24.8019968304605,
12.));
#194010=CARTESIAN_POINT('Ctrl Pts',(-5.67915655496543,-24.8225181223845,
0.));
#194011=CARTESIAN_POINT('Ctrl Pts',(-5.67915655496543,-24.8225181223845,
12.));
#194012=CARTESIAN_POINT('Ctrl Pts',(-5.69677006679445,-24.8430549277621,
0.));
#194013=CARTESIAN_POINT('Ctrl Pts',(-5.69677006679445,-24.8430549277621,
12.));
#194014=CARTESIAN_POINT('Ctrl Pts',(-5.71447804252028,-24.8636067597669,
0.));
#194015=CARTESIAN_POINT('Ctrl Pts',(-5.71447804252028,-24.8636067597669,
12.));
#194016=CARTESIAN_POINT('Ctrl Pts',(-5.73228037976928,-24.884173146722,
0.));
#194017=CARTESIAN_POINT('Ctrl Pts',(-5.73228037976928,-24.884173146722,
12.));
#194018=CARTESIAN_POINT('Ctrl Pts',(-5.75017697890805,-24.904753637648,
0.));
#194019=CARTESIAN_POINT('Ctrl Pts',(-5.75017697890805,-24.904753637648,
12.));
#194020=CARTESIAN_POINT('Ctrl Pts',(-5.76816774342221,-24.9253478043656,
0.));
#194021=CARTESIAN_POINT('Ctrl Pts',(-5.76816774342221,-24.9253478043656,
12.));
#194022=CARTESIAN_POINT('Ctrl Pts',(-5.78625257775682,-24.945955229334,
0.));
#194023=CARTESIAN_POINT('Ctrl Pts',(-5.78625257775682,-24.945955229334,
12.));
#194024=CARTESIAN_POINT('Ctrl Pts',(-5.80443138549727,-24.9665754954496,
0.));
#194025=CARTESIAN_POINT('Ctrl Pts',(-5.80443138549727,-24.9665754954496,
12.));
#194026=CARTESIAN_POINT('Ctrl Pts',(-5.822704067442,-24.9872081752734,0.));
#194027=CARTESIAN_POINT('Ctrl Pts',(-5.822704067442,-24.9872081752734,12.));
#194028=CARTESIAN_POINT('Ctrl Pts',(-5.84107051963072,-25.0078528200564,
0.));
#194029=CARTESIAN_POINT('Ctrl Pts',(-5.84107051963072,-25.0078528200564,
12.));
#194030=CARTESIAN_POINT('Ctrl Pts',(-5.85953063156827,-25.0285089498899,
0.));
#194031=CARTESIAN_POINT('Ctrl Pts',(-5.85953063156827,-25.0285089498899,
12.));
#194032=CARTESIAN_POINT('Ctrl Pts',(-5.87808428385367,-25.049176040591,
0.));
#194033=CARTESIAN_POINT('Ctrl Pts',(-5.87808428385367,-25.049176040591,
12.));
#194034=CARTESIAN_POINT('Ctrl Pts',(-5.89673135155515,-25.0698535426514,
0.));
#194035=CARTESIAN_POINT('Ctrl Pts',(-5.89673135155515,-25.0698535426514,
12.));
#194036=CARTESIAN_POINT('Ctrl Pts',(-5.91547170844448,-25.0905409050773,
0.));
#194037=CARTESIAN_POINT('Ctrl Pts',(-5.91547170844448,-25.0905409050773,
12.));
#194038=CARTESIAN_POINT('Ctrl Pts',(-5.93430523086836,-25.1112375971106,
0.));
#194039=CARTESIAN_POINT('Ctrl Pts',(-5.93430523086836,-25.1112375971106,
12.));
#194040=CARTESIAN_POINT('Ctrl Pts',(-5.95323180187379,-25.1319431317237,
0.));
#194041=CARTESIAN_POINT('Ctrl Pts',(-5.95323180187379,-25.1319431317237,
12.));
#194042=CARTESIAN_POINT('Ctrl Pts',(-5.97225131495618,-25.1526570863092,
0.));
#194043=CARTESIAN_POINT('Ctrl Pts',(-5.97225131495618,-25.1526570863092,
12.));
#194044=CARTESIAN_POINT('Ctrl Pts',(-5.99136367859755,-25.1733791296259,
0.));
#194045=CARTESIAN_POINT('Ctrl Pts',(-5.99136367859755,-25.1733791296259,
12.));
#194046=CARTESIAN_POINT('Ctrl Pts',(-6.01056881804614,-25.1941090269819,
0.));
#194047=CARTESIAN_POINT('Ctrl Pts',(-6.01056881804614,-25.1941090269819,
12.));
#194048=CARTESIAN_POINT('Ctrl Pts',(-6.02986667389998,-25.21484662016,0.));
#194049=CARTESIAN_POINT('Ctrl Pts',(-6.02986667389998,-25.21484662016,12.));
#194050=CARTESIAN_POINT('Ctrl Pts',(-6.04925720151219,-25.2355918139032,
0.));
#194051=CARTESIAN_POINT('Ctrl Pts',(-6.04925720151219,-25.2355918139032,
12.));
#194052=CARTESIAN_POINT('Ctrl Pts',(-6.06484373634547,-25.2521940105705,
0.));
#194053=CARTESIAN_POINT('Ctrl Pts',(-6.06484373634547,-25.2521940105705,
12.));
#194054=CARTESIAN_POINT('Ctrl Pts',(-6.07657531787491,-25.2646490489922,
0.));
#194055=CARTESIAN_POINT('Ctrl Pts',(-6.07657531787491,-25.2646490489922,
12.));
#194056=CARTESIAN_POINT('Ctrl Pts',(-6.08441489609794,-25.2729539149517,
0.));
#194057=CARTESIAN_POINT('Ctrl Pts',(-6.08441489609794,-25.2729539149517,
12.));
#194058=CARTESIAN_POINT('Ctrl Pts',(-6.088339316177,-25.2771067246846,0.));
#194059=CARTESIAN_POINT('Ctrl Pts',(-6.088339316177,-25.2771067246846,12.));
#194060=CARTESIAN_POINT('',(-6.088339316177,-25.2771067246846,0.));
#194061=CARTESIAN_POINT('Ctrl Pts',(-4.11585220600463,-22.1738711152697,
0.));
#194062=CARTESIAN_POINT('Ctrl Pts',(-4.11585194677443,-22.173877682324,
0.));
#194063=CARTESIAN_POINT('Ctrl Pts',(-4.11586035878288,-22.1739341411687,
0.));
#194064=CARTESIAN_POINT('Ctrl Pts',(-4.11589976826167,-22.1741488021234,
0.));
#194065=CARTESIAN_POINT('Ctrl Pts',(-4.11600589882846,-22.1746949858775,
0.));
#194066=CARTESIAN_POINT('Ctrl Pts',(-4.11622797217069,-22.1758088296598,
0.));
#194067=CARTESIAN_POINT('Ctrl Pts',(-4.11653973150519,-22.177347426894,
0.));
#194068=CARTESIAN_POINT('Ctrl Pts',(-4.11694173195005,-22.179297473024,
0.));
#194069=CARTESIAN_POINT('Ctrl Pts',(-4.11743469691757,-22.1816414985788,
0.));
#194070=CARTESIAN_POINT('Ctrl Pts',(-4.11801938107481,-22.1843613164855,
0.));
#194071=CARTESIAN_POINT('Ctrl Pts',(-4.11869641271774,-22.1874419861496,
0.));
#194072=CARTESIAN_POINT('Ctrl Pts',(-4.11946626228637,-22.1908725908525,
0.));
#194073=CARTESIAN_POINT('Ctrl Pts',(-4.12032932637737,-22.1946440958098,
0.));
#194074=CARTESIAN_POINT('Ctrl Pts',(-4.12128598183523,-22.1987479618246,
0.));
#194075=CARTESIAN_POINT('Ctrl Pts',(-4.12233664408228,-22.2031746532106,
0.));
#194076=CARTESIAN_POINT('Ctrl Pts',(-4.12348173702024,-22.2079143941719,
0.));
#194077=CARTESIAN_POINT('Ctrl Pts',(-4.12472167516608,-22.2129576146671,
0.));
#194078=CARTESIAN_POINT('Ctrl Pts',(-4.12605683613308,-22.2182956401341,
0.));
#194079=CARTESIAN_POINT('Ctrl Pts',(-4.12748755830105,-22.2239207458781,
0.));
#194080=CARTESIAN_POINT('Ctrl Pts',(-4.1290141546338,-22.2298258043947,
0.));
#194081=CARTESIAN_POINT('Ctrl Pts',(-4.13063692157499,-22.2360040565533,
0.));
#194082=CARTESIAN_POINT('Ctrl Pts',(-4.13235615060161,-22.2424488153523,
0.));
#194083=CARTESIAN_POINT('Ctrl Pts',(-4.13417212558811,-22.249153531779,
0.));
#194084=CARTESIAN_POINT('Ctrl Pts',(-4.13608511977226,-22.2561118708421,
0.));
#194085=CARTESIAN_POINT('Ctrl Pts',(-4.13809539255423,-22.2633177913972,
0.));
#194086=CARTESIAN_POINT('Ctrl Pts',(-4.14020318715992,-22.2707656042457,
0.));
#194087=CARTESIAN_POINT('Ctrl Pts',(-4.14240873321985,-22.2784499072027,
0.));
#194088=CARTESIAN_POINT('Ctrl Pts',(-4.14471224859296,-22.2863655389166,
0.));
#194089=CARTESIAN_POINT('Ctrl Pts',(-4.14711394168557,-22.2945075198467,
0.));
#194090=CARTESIAN_POINT('Ctrl Pts',(-4.14961401285523,-22.3028710166933,
0.));
#194091=CARTESIAN_POINT('Ctrl Pts',(-4.15221265396991,-22.3114513545185,
0.));
#194092=CARTESIAN_POINT('Ctrl Pts',(-4.15491004835282,-22.320244018698,
0.));
#194093=CARTESIAN_POINT('Ctrl Pts',(-4.15770637047891,-22.3292446628959,
0.));
#194094=CARTESIAN_POINT('Ctrl Pts',(-4.16060178604165,-22.3384491078602,
0.));
#194095=CARTESIAN_POINT('Ctrl Pts',(-4.16359645263189,-22.3478533253889,
0.));
#194096=CARTESIAN_POINT('Ctrl Pts',(-4.16669052026601,-22.3574534257396,
0.));
#194097=CARTESIAN_POINT('Ctrl Pts',(-4.16988413199458,-22.36724564276,0.));
#194098=CARTESIAN_POINT('Ctrl Pts',(-4.17317742436146,-22.3772263228617,
0.));
#194099=CARTESIAN_POINT('Ctrl Pts',(-4.17657052752826,-22.3873919231334,
0.));
#194100=CARTESIAN_POINT('Ctrl Pts',(-4.18006356544883,-22.3977390078075,
0.));
#194101=CARTESIAN_POINT('Ctrl Pts',(-4.18365665600851,-22.4082642454453,
0.));
#194102=CARTESIAN_POINT('Ctrl Pts',(-4.18734991117722,-22.4189644056115,
0.));
#194103=CARTESIAN_POINT('Ctrl Pts',(-4.19114343726943,-22.4298363535421,
0.));
#194104=CARTESIAN_POINT('Ctrl Pts',(-4.19503733518862,-22.4408770448917,
0.));
#194105=CARTESIAN_POINT('Ctrl Pts',(-4.19903170066356,-22.4520835205419,
0.));
#194106=CARTESIAN_POINT('Ctrl Pts',(-4.20312662448172,-22.4634529011433,
0.));
#194107=CARTESIAN_POINT('Ctrl Pts',(-4.20732219265649,-22.4749823839915,
0.));
#194108=CARTESIAN_POINT('Ctrl Pts',(-4.21161848657429,-22.4866692403147,
0.));
#194109=CARTESIAN_POINT('Ctrl Pts',(-4.21601558313909,-22.4985108124229,
0.));
#194110=CARTESIAN_POINT('Ctrl Pts',(-4.22051355490198,-22.5105045108882,
0.));
#194111=CARTESIAN_POINT('Ctrl Pts',(-4.22511247020041,-22.5226478117885,
0.));
#194112=CARTESIAN_POINT('Ctrl Pts',(-4.22981239330732,-22.5349382540587,
0.));
#194113=CARTESIAN_POINT('Ctrl Pts',(-4.23461338456714,-22.5473734368086,
0.));
#194114=CARTESIAN_POINT('Ctrl Pts',(-4.23951550052527,-22.559951016643,
0.));
#194115=CARTESIAN_POINT('Ctrl Pts',(-4.2445187940486,-22.5726687049922,
0.));
#194116=CARTESIAN_POINT('Ctrl Pts',(-4.24962331444186,-22.5855242662479,
0.));
#194117=CARTESIAN_POINT('Ctrl Pts',(-4.25482910755486,-22.5985155158637,
0.));
#194118=CARTESIAN_POINT('Ctrl Pts',(-4.26013621588304,-22.611640318482,
0.));
#194119=CARTESIAN_POINT('Ctrl Pts',(-4.26554467865572,-22.6248965859975,
0.));
#194120=CARTESIAN_POINT('Ctrl Pts',(-4.27105453193,-22.6382822758171,0.));
#194121=CARTESIAN_POINT('Ctrl Pts',(-4.27666580869118,-22.6517953893303,
0.));
#194122=CARTESIAN_POINT('Ctrl Pts',(-4.2823785389406,-22.665433970311,0.));
#194123=CARTESIAN_POINT('Ctrl Pts',(-4.28819274977767,-22.6791961033536,
0.));
#194124=CARTESIAN_POINT('Ctrl Pts',(-4.29410846547062,-22.6930799122545,
0.));
#194125=CARTESIAN_POINT('Ctrl Pts',(-4.30012570754067,-22.707083558756,
0.));
#194126=CARTESIAN_POINT('Ctrl Pts',(-4.30624449484075,-22.7212052413384,
0.));
#194127=CARTESIAN_POINT('Ctrl Pts',(-4.31246484362551,-22.7354431939926,
0.));
#194128=CARTESIAN_POINT('Ctrl Pts',(-4.31878676761231,-22.7497956849852,
0.));
#194129=CARTESIAN_POINT('Ctrl Pts',(-4.32521027803748,-22.764261015648,
0.));
#194130=CARTESIAN_POINT('Ctrl Pts',(-4.33173538373183,-22.7788375194081,
0.));
#194131=CARTESIAN_POINT('Ctrl Pts',(-4.33836209118444,-22.7935235607807,
0.));
#194132=CARTESIAN_POINT('Ctrl Pts',(-4.34509040460066,-22.808317534379,
0.));
#194133=CARTESIAN_POINT('Ctrl Pts',(-4.35192032594802,-22.8232178638873,
0.));
#194134=CARTESIAN_POINT('Ctrl Pts',(-4.3588518550056,-22.838223001118,0.));
#194135=CARTESIAN_POINT('Ctrl Pts',(-4.36588498943011,-22.8533314252419,
0.));
#194136=CARTESIAN_POINT('Ctrl Pts',(-4.37301972480753,-22.8685416419725,
0.));
#194137=CARTESIAN_POINT('Ctrl Pts',(-4.38025605470091,-22.8838521827702,
0.));
#194138=CARTESIAN_POINT('Ctrl Pts',(-4.38759397068393,-22.8992616040108,
0.));
#194139=CARTESIAN_POINT('Ctrl Pts',(-4.39503346238455,-22.9147684862425,
0.));
#194140=CARTESIAN_POINT('Ctrl Pts',(-4.40257451754308,-22.9303714335549,
0.));
#194141=CARTESIAN_POINT('Ctrl Pts',(-4.41021712205549,-22.9460690729093,
0.));
#194142=CARTESIAN_POINT('Ctrl Pts',(-4.41796126001311,-22.9618600534866,
0.));
#194143=CARTESIAN_POINT('Ctrl Pts',(-4.42580691372772,-22.9777430460021,
0.));
#194144=CARTESIAN_POINT('Ctrl Pts',(-4.43375406376906,-22.9937167421009,
0.));
#194145=CARTESIAN_POINT('Ctrl Pts',(-4.44180268901667,-23.0097798538399,
0.));
#194146=CARTESIAN_POINT('Ctrl Pts',(-4.44995276669699,-23.0259311131395,
0.));
#194147=CARTESIAN_POINT('Ctrl Pts',(-4.45820427241677,-23.0421692712466,
0.));
#194148=CARTESIAN_POINT('Ctrl Pts',(-4.46655718018206,-23.0584930981723,
0.));
#194149=CARTESIAN_POINT('Ctrl Pts',(-4.47501146242822,-23.0749013821867,
0.));
#194150=CARTESIAN_POINT('Ctrl Pts',(-4.48356709006757,-23.0913929293909,
0.));
#194151=CARTESIAN_POINT('Ctrl Pts',(-4.49222403252202,-23.1079665632629,
0.));
#194152=CARTESIAN_POINT('Ctrl Pts',(-4.50098225775179,-23.1246211242117,
0.));
#194153=CARTESIAN_POINT('Ctrl Pts',(-4.50984173227088,-23.1413554691136,
0.));
#194154=CARTESIAN_POINT('Ctrl Pts',(-4.51880242116786,-23.1581684708778,
0.));
#194155=CARTESIAN_POINT('Ctrl Pts',(-4.52786428815049,-23.1750590180923,
0.));
#194156=CARTESIAN_POINT('Ctrl Pts',(-4.53702729557586,-23.1920260146474,
0.));
#194157=CARTESIAN_POINT('Ctrl Pts',(-4.54629140447543,-23.2090683793627,
0.));
#194158=CARTESIAN_POINT('Ctrl Pts',(-4.55565657456957,-23.2261850456055,
0.));
#194159=CARTESIAN_POINT('Ctrl Pts',(-4.56512276427812,-23.2433749609117,
0.));
#194160=CARTESIAN_POINT('Ctrl Pts',(-4.57468993076071,-23.2606370866854,
0.));
#194161=CARTESIAN_POINT('Ctrl Pts',(-4.58435802994675,-23.2779703978868,
0.));
#194162=CARTESIAN_POINT('Ctrl Pts',(-4.5941270165575,-23.295373882719,0.));
#194163=CARTESIAN_POINT('Ctrl Pts',(-4.60399684412176,-23.3128465423119,
0.));
#194164=CARTESIAN_POINT('Ctrl Pts',(-4.61396746497849,-23.3303873903947,
0.));
#194165=CARTESIAN_POINT('Ctrl Pts',(-4.62403883030825,-23.3479954530281,
0.));
#194166=CARTESIAN_POINT('Ctrl Pts',(-4.63421089016555,-23.3656697683496,
0.));
#194167=CARTESIAN_POINT('Ctrl Pts',(-4.64448359349936,-23.383409386307,
0.));
#194168=CARTESIAN_POINT('Ctrl Pts',(-4.65485688816923,-23.4012133683957,
0.));
#194169=CARTESIAN_POINT('Ctrl Pts',(-4.66533072094664,-23.4190807873798,
0.));
#194170=CARTESIAN_POINT('Ctrl Pts',(-4.67590503753051,-23.4370107270444,
0.));
#194171=CARTESIAN_POINT('Ctrl Pts',(-4.68657978258298,-23.4550022819852,
0.));
#194172=CARTESIAN_POINT('Ctrl Pts',(-4.69735489975024,-23.4730545573849,
0.));
#194173=CARTESIAN_POINT('Ctrl Pts',(-4.70823033167821,-23.491166668789,
0.));
#194174=CARTESIAN_POINT('Ctrl Pts',(-4.71920602001905,-23.5093377418784,
0.));
#194175=CARTESIAN_POINT('Ctrl Pts',(-4.73028190543032,-23.5275669122378,
0.));
#194176=CARTESIAN_POINT('Ctrl Pts',(-4.74145792760699,-23.5458533251715,
0.));
#194177=CARTESIAN_POINT('Ctrl Pts',(-4.75273402530616,-23.564196135517,
0.));
#194178=CARTESIAN_POINT('Ctrl Pts',(-4.76411013636252,-23.5825945074535,
0.));
#194179=CARTESIAN_POINT('Ctrl Pts',(-4.77558619769876,-23.6010476143099,
0.));
#194180=CARTESIAN_POINT('Ctrl Pts',(-4.78716214532105,-23.6195546383625,
0.));
#194181=CARTESIAN_POINT('Ctrl Pts',(-4.79883791433231,-23.6381147706581,
0.));
#194182=CARTESIAN_POINT('Ctrl Pts',(-4.81061343896443,-23.6567272108631,
0.));
#194183=CARTESIAN_POINT('Ctrl Pts',(-4.82248865259571,-23.6753911671023,
0.));
#194184=CARTESIAN_POINT('Ctrl Pts',(-4.83446348776268,-23.6941058557971,
0.));
#194185=CARTESIAN_POINT('Ctrl Pts',(-4.84653787616424,-23.7128705015014,
0.));
#194186=CARTESIAN_POINT('Ctrl Pts',(-4.85871174865492,-23.7316843367308,
0.));
#194187=CARTESIAN_POINT('Ctrl Pts',(-4.87098503527144,-23.7505466018239,
0.));
#194188=CARTESIAN_POINT('Ctrl Pts',(-4.88335766525566,-23.7694565448044,
0.));
#194189=CARTESIAN_POINT('Ctrl Pts',(-4.89582956706772,-23.7884134212381,
0.));
#194190=CARTESIAN_POINT('Ctrl Pts',(-4.90840066839348,-23.8074164940897,
0.));
#194191=CARTESIAN_POINT('Ctrl Pts',(-4.92107089613977,-23.8264650335721,
0.));
#194192=CARTESIAN_POINT('Ctrl Pts',(-4.93384017643442,-23.8455583170062,
0.));
#194193=CARTESIAN_POINT('Ctrl Pts',(-4.94670843465869,-23.8646956287172,
0.));
#194194=CARTESIAN_POINT('Ctrl Pts',(-4.95967559546566,-23.883876259922,
0.));
#194195=CARTESIAN_POINT('Ctrl Pts',(-4.9727415827923,-23.9030995086164,
0.));
#194196=CARTESIAN_POINT('Ctrl Pts',(-4.98590631986534,-23.9223646794591,
0.));
#194197=CARTESIAN_POINT('Ctrl Pts',(-4.9991697291931,-23.9416710836529,
0.));
#194198=CARTESIAN_POINT('Ctrl Pts',(-5.01253173257459,-23.9610180388271,
0.));
#194199=CARTESIAN_POINT('Ctrl Pts',(-5.02599225112462,-23.9804048689228,
0.));
#194200=CARTESIAN_POINT('Ctrl Pts',(-5.03955120528528,-23.9998309040747,
0.));
#194201=CARTESIAN_POINT('Ctrl Pts',(-5.05320851483069,-24.0192954804896,
0.));
#194202=CARTESIAN_POINT('Ctrl Pts',(-5.0669640988664,-24.0387979403268,
0.));
#194203=CARTESIAN_POINT('Ctrl Pts',(-5.08081787581271,-24.0583376315636,
0.));
#194204=CARTESIAN_POINT('Ctrl Pts',(-5.09476976342618,-24.0779139079264,
0.));
#194205=CARTESIAN_POINT('Ctrl Pts',(-5.10881967883126,-24.0975261288444,
0.));
#194206=CARTESIAN_POINT('Ctrl Pts',(-5.12296753853858,-24.117173659394,
0.));
#194207=CARTESIAN_POINT('Ctrl Pts',(-5.13721325845746,-24.1368558702443,
0.));
#194208=CARTESIAN_POINT('Ctrl Pts',(-5.1515567539008,-24.1565721375971,
0.));
#194209=CARTESIAN_POINT('Ctrl Pts',(-5.16599793957987,-24.1763218431344,
0.));
#194210=CARTESIAN_POINT('Ctrl Pts',(-5.180536729614,-24.1961043738756,0.));
#194211=CARTESIAN_POINT('Ctrl Pts',(-5.19517303753648,-24.2159191220171,
0.));
#194212=CARTESIAN_POINT('Ctrl Pts',(-5.20990677629177,-24.2357654847766,
0.));
#194213=CARTESIAN_POINT('Ctrl Pts',(-5.22473785822443,-24.2556428642294,
0.));
#194214=CARTESIAN_POINT('Ctrl Pts',(-5.2396661950629,-24.2755506671525,
0.));
#194215=CARTESIAN_POINT('Ctrl Pts',(-5.25469169788857,-24.2954883048447,
0.));
#194216=CARTESIAN_POINT('Ctrl Pts',(-5.269814277188,-24.3154551932221,0.));
#194217=CARTESIAN_POINT('Ctrl Pts',(-5.28503384290649,-24.3354507529414,
0.));
#194218=CARTESIAN_POINT('Ctrl Pts',(-5.30035030449064,-24.3554744095075,
0.));
#194219=CARTESIAN_POINT('Ctrl Pts',(-5.31576357092527,-24.3755255933917,
0.));
#194220=CARTESIAN_POINT('Ctrl Pts',(-5.33127355076035,-24.3956037401293,
0.));
#194221=CARTESIAN_POINT('Ctrl Pts',(-5.34688015213538,-24.4157082904614,
0.));
#194222=CARTESIAN_POINT('Ctrl Pts',(-5.36258328273628,-24.435838689915,
0.));
#194223=CARTESIAN_POINT('Ctrl Pts',(-5.37838284973696,-24.4559943883157,
0.));
#194224=CARTESIAN_POINT('Ctrl Pts',(-5.39427875973825,-24.4761748393321,
0.));
#194225=CARTESIAN_POINT('Ctrl Pts',(-5.41027091869242,-24.496379499983,
0.));
#194226=CARTESIAN_POINT('Ctrl Pts',(-5.4263592318342,-24.5166078302108,
0.));
#194227=CARTESIAN_POINT('Ctrl Pts',(-5.44254360356881,-24.5368592922863,
0.));
#194228=CARTESIAN_POINT('Ctrl Pts',(-5.45882393762262,-24.5571333514842,
0.));
#194229=CARTESIAN_POINT('Ctrl Pts',(-5.4752001372442,-24.5774294770329,
0.));
#194230=CARTESIAN_POINT('Ctrl Pts',(-5.49167210537248,-24.5977471429364,
0.));
#194231=CARTESIAN_POINT('Ctrl Pts',(-5.50823974481963,-24.6180858289179,
0.));
#194232=CARTESIAN_POINT('Ctrl Pts',(-5.52490295840993,-24.6384450211467,
0.));
#194233=CARTESIAN_POINT('Ctrl Pts',(-5.54166164919584,-24.6588242134738,
0.));
#194234=CARTESIAN_POINT('Ctrl Pts',(-5.55851572025377,-24.6792229061794,
0.));
#194235=CARTESIAN_POINT('Ctrl Pts',(-5.57546507427756,-24.6996406035517,
0.));
#194236=CARTESIAN_POINT('Ctrl Pts',(-5.59250961323988,-24.7200768119088,
0.));
#194237=CARTESIAN_POINT('Ctrl Pts',(-5.60964923798492,-24.7405310372739,
0.));
#194238=CARTESIAN_POINT('Ctrl Pts',(-5.62688384790924,-24.7610027835697,
0.));
#194239=CARTESIAN_POINT('Ctrl Pts',(-5.64421334042262,-24.781491549672,
0.));
#194240=CARTESIAN_POINT('Ctrl Pts',(-5.66163761114922,-24.8019968304605,
0.));
#194241=CARTESIAN_POINT('Ctrl Pts',(-5.67915655496543,-24.8225181223845,
0.));
#194242=CARTESIAN_POINT('Ctrl Pts',(-5.69677006679445,-24.8430549277621,
0.));
#194243=CARTESIAN_POINT('Ctrl Pts',(-5.71447804252028,-24.8636067597669,
0.));
#194244=CARTESIAN_POINT('Ctrl Pts',(-5.73228037976928,-24.884173146722,
0.));
#194245=CARTESIAN_POINT('Ctrl Pts',(-5.75017697890805,-24.904753637648,
0.));
#194246=CARTESIAN_POINT('Ctrl Pts',(-5.76816774342221,-24.9253478043656,
0.));
#194247=CARTESIAN_POINT('Ctrl Pts',(-5.78625257775682,-24.945955229334,
0.));
#194248=CARTESIAN_POINT('Ctrl Pts',(-5.80443138549727,-24.9665754954496,
0.));
#194249=CARTESIAN_POINT('Ctrl Pts',(-5.822704067442,-24.9872081752734,0.));
#194250=CARTESIAN_POINT('Ctrl Pts',(-5.84107051963072,-25.0078528200564,
0.));
#194251=CARTESIAN_POINT('Ctrl Pts',(-5.85953063156827,-25.0285089498899,
0.));
#194252=CARTESIAN_POINT('Ctrl Pts',(-5.87808428385367,-25.049176040591,
0.));
#194253=CARTESIAN_POINT('Ctrl Pts',(-5.89673135155515,-25.0698535426514,
0.));
#194254=CARTESIAN_POINT('Ctrl Pts',(-5.91547170844448,-25.0905409050773,
0.));
#194255=CARTESIAN_POINT('Ctrl Pts',(-5.93430523086836,-25.1112375971106,
0.));
#194256=CARTESIAN_POINT('Ctrl Pts',(-5.95323180187379,-25.1319431317237,
0.));
#194257=CARTESIAN_POINT('Ctrl Pts',(-5.97225131495618,-25.1526570863092,
0.));
#194258=CARTESIAN_POINT('Ctrl Pts',(-5.99136367859755,-25.1733791296259,
0.));
#194259=CARTESIAN_POINT('Ctrl Pts',(-6.01056881804614,-25.1941090269819,
0.));
#194260=CARTESIAN_POINT('Ctrl Pts',(-6.02986667389998,-25.21484662016,0.));
#194261=CARTESIAN_POINT('Ctrl Pts',(-6.04925720151219,-25.2355918139032,
0.));
#194262=CARTESIAN_POINT('Ctrl Pts',(-6.06484373634547,-25.2521940105705,
0.));
#194263=CARTESIAN_POINT('Ctrl Pts',(-6.07657531787491,-25.2646490489922,
0.));
#194264=CARTESIAN_POINT('Ctrl Pts',(-6.08441489609794,-25.2729539149517,
0.));
#194265=CARTESIAN_POINT('Ctrl Pts',(-6.088339316177,-25.2771067246846,0.));
#194266=CARTESIAN_POINT('',(-6.088339316177,-25.2771067246846,0.));
#194267=CARTESIAN_POINT('Origin',(-9.26120677397565,-19.4030938020118,0.));
#194268=CARTESIAN_POINT('',(-9.71462809124917,-20.353053841303,0.));
#194269=CARTESIAN_POINT('',(-9.71462809124917,-20.353053841303,0.));
#194270=CARTESIAN_POINT('',(-4.63060338698782,-9.70154690100589,0.));
#194271=CARTESIAN_POINT('Ctrl Pts',(-7.36589684767345,-24.9347862158358,
0.));
#194272=CARTESIAN_POINT('Ctrl Pts',(-7.36589684767345,-24.9347862158358,
12.));
#194273=CARTESIAN_POINT('Ctrl Pts',(-7.36721909028843,-24.9292275670674,
0.));
#194274=CARTESIAN_POINT('Ctrl Pts',(-7.36721909028843,-24.9292275670674,
12.));
#194275=CARTESIAN_POINT('Ctrl Pts',(-7.36985593120091,-24.9181155530543,
0.));
#194276=CARTESIAN_POINT('Ctrl Pts',(-7.36985593120091,-24.9181155530543,
12.));
#194277=CARTESIAN_POINT('Ctrl Pts',(-7.37378825961676,-24.901463382605,
0.));
#194278=CARTESIAN_POINT('Ctrl Pts',(-7.37378825961676,-24.901463382605,
12.));
#194279=CARTESIAN_POINT('Ctrl Pts',(-7.3789854964027,-24.8792921911115,
0.));
#194280=CARTESIAN_POINT('Ctrl Pts',(-7.3789854964027,-24.8792921911115,
12.));
#194281=CARTESIAN_POINT('Ctrl Pts',(-7.38540558903621,-24.8516310625176,
0.));
#194282=CARTESIAN_POINT('Ctrl Pts',(-7.38540558903621,-24.8516310625176,
12.));
#194283=CARTESIAN_POINT('Ctrl Pts',(-7.39174922585809,-24.8240228520893,
0.));
#194284=CARTESIAN_POINT('Ctrl Pts',(-7.39174922585809,-24.8240228520893,
12.));
#194285=CARTESIAN_POINT('Ctrl Pts',(-7.39801641583013,-24.7964676646431,
0.));
#194286=CARTESIAN_POINT('Ctrl Pts',(-7.39801641583013,-24.7964676646431,
12.));
#194287=CARTESIAN_POINT('Ctrl Pts',(-7.40420718661603,-24.7689656668983,
0.));
#194288=CARTESIAN_POINT('Ctrl Pts',(-7.40420718661603,-24.7689656668983,
12.));
#194289=CARTESIAN_POINT('Ctrl Pts',(-7.41032159082382,-24.7415170994784,
0.));
#194290=CARTESIAN_POINT('Ctrl Pts',(-7.41032159082382,-24.7415170994784,
12.));
#194291=CARTESIAN_POINT('Ctrl Pts',(-7.41635971481674,-24.7141222950051,
0.));
#194292=CARTESIAN_POINT('Ctrl Pts',(-7.41635971481674,-24.7141222950051,
12.));
#194293=CARTESIAN_POINT('Ctrl Pts',(-7.42232167766266,-24.6867816727192,
0.));
#194294=CARTESIAN_POINT('Ctrl Pts',(-7.42232167766266,-24.6867816727192,
12.));
#194295=CARTESIAN_POINT('Ctrl Pts',(-7.42820762159126,-24.6594957128756,
0.));
#194296=CARTESIAN_POINT('Ctrl Pts',(-7.42820762159126,-24.6594957128756,
12.));
#194297=CARTESIAN_POINT('Ctrl Pts',(-7.43401770489524,-24.6322649369517,
0.));
#194298=CARTESIAN_POINT('Ctrl Pts',(-7.43401770489524,-24.6322649369517,
12.));
#194299=CARTESIAN_POINT('Ctrl Pts',(-7.43975209375504,-24.6050898852368,
0.));
#194300=CARTESIAN_POINT('Ctrl Pts',(-7.43975209375504,-24.6050898852368,
12.));
#194301=CARTESIAN_POINT('Ctrl Pts',(-7.44541095473135,-24.577971096086,
0.));
#194302=CARTESIAN_POINT('Ctrl Pts',(-7.44541095473135,-24.577971096086,
12.));
#194303=CARTESIAN_POINT('Ctrl Pts',(-7.4509944465116,-24.5509090831559,
0.));
#194304=CARTESIAN_POINT('Ctrl Pts',(-7.4509944465116,-24.5509090831559,
12.));
#194305=CARTESIAN_POINT('Ctrl Pts',(-7.45650271335862,-24.5239043173072,
0.));
#194306=CARTESIAN_POINT('Ctrl Pts',(-7.45650271335862,-24.5239043173072,
12.));
#194307=CARTESIAN_POINT('Ctrl Pts',(-7.46193588961464,-24.4969572391483,
0.));
#194308=CARTESIAN_POINT('Ctrl Pts',(-7.46193588961464,-24.4969572391483,
12.));
#194309=CARTESIAN_POINT('Ctrl Pts',(-7.46729410308787,-24.4700682684524,
0.));
#194310=CARTESIAN_POINT('Ctrl Pts',(-7.46729410308787,-24.4700682684524,
12.));
#194311=CARTESIAN_POINT('Ctrl Pts',(-7.47257747883246,-24.443237814649,
0.));
#194312=CARTESIAN_POINT('Ctrl Pts',(-7.47257747883246,-24.443237814649,
12.));
#194313=CARTESIAN_POINT('Ctrl Pts',(-7.47778614286565,-24.4164662871163,
0.));
#194314=CARTESIAN_POINT('Ctrl Pts',(-7.47778614286565,-24.4164662871163,
12.));
#194315=CARTESIAN_POINT('Ctrl Pts',(-7.48292022569301,-24.3897541049254,
0.));
#194316=CARTESIAN_POINT('Ctrl Pts',(-7.48292022569301,-24.3897541049254,
12.));
#194317=CARTESIAN_POINT('Ctrl Pts',(-7.48797986651909,-24.3631017084524,
0.));
#194318=CARTESIAN_POINT('Ctrl Pts',(-7.48797986651909,-24.3631017084524,
12.));
#194319=CARTESIAN_POINT('Ctrl Pts',(-7.49296521252421,-24.3365095573685,
0.));
#194320=CARTESIAN_POINT('Ctrl Pts',(-7.49296521252421,-24.3365095573685,
12.));
#194321=CARTESIAN_POINT('Ctrl Pts',(-7.49787641695439,-24.3099781253355,
0.));
#194322=CARTESIAN_POINT('Ctrl Pts',(-7.49787641695439,-24.3099781253355,
12.));
#194323=CARTESIAN_POINT('Ctrl Pts',(-7.50271363765152,-24.2835078958973,
0.));
#194324=CARTESIAN_POINT('Ctrl Pts',(-7.50271363765152,-24.2835078958973,
12.));
#194325=CARTESIAN_POINT('Ctrl Pts',(-7.50747703535134,-24.2570993577034,
0.));
#194326=CARTESIAN_POINT('Ctrl Pts',(-7.50747703535134,-24.2570993577034,
12.));
#194327=CARTESIAN_POINT('Ctrl Pts',(-7.51216677222181,-24.2307530003887,
0.));
#194328=CARTESIAN_POINT('Ctrl Pts',(-7.51216677222181,-24.2307530003887,
12.));
#194329=CARTESIAN_POINT('Ctrl Pts',(-7.51678300997949,-24.2044693092349,
0.));
#194330=CARTESIAN_POINT('Ctrl Pts',(-7.51678300997949,-24.2044693092349,
12.));
#194331=CARTESIAN_POINT('Ctrl Pts',(-7.52132590953802,-24.1782487641594,
0.));
#194332=CARTESIAN_POINT('Ctrl Pts',(-7.52132590953802,-24.1782487641594,
12.));
#194333=CARTESIAN_POINT('Ctrl Pts',(-7.52579563201424,-24.1520918425364,
0.));
#194334=CARTESIAN_POINT('Ctrl Pts',(-7.52579563201424,-24.1520918425364,
12.));
#194335=CARTESIAN_POINT('Ctrl Pts',(-7.53019233935502,-24.1259990209207,
0.));
#194336=CARTESIAN_POINT('Ctrl Pts',(-7.53019233935502,-24.1259990209207,
12.));
#194337=CARTESIAN_POINT('Ctrl Pts',(-7.53451619514649,-24.0999707772642,
0.));
#194338=CARTESIAN_POINT('Ctrl Pts',(-7.53451619514649,-24.0999707772642,
12.));
#194339=CARTESIAN_POINT('Ctrl Pts',(-7.53876736531014,-24.0740075927985,
0.));
#194340=CARTESIAN_POINT('Ctrl Pts',(-7.53876736531014,-24.0740075927985,
12.));
#194341=CARTESIAN_POINT('Ctrl Pts',(-7.54294601896145,-24.0481099543353,
0.));
#194342=CARTESIAN_POINT('Ctrl Pts',(-7.54294601896145,-24.0481099543353,
12.));
#194343=CARTESIAN_POINT('Ctrl Pts',(-7.5470523288591,-24.022278355453,0.));
#194344=CARTESIAN_POINT('Ctrl Pts',(-7.5470523288591,-24.022278355453,12.));
#194345=CARTESIAN_POINT('Ctrl Pts',(-7.55108647097441,-23.9965132953185,
0.));
#194346=CARTESIAN_POINT('Ctrl Pts',(-7.55108647097441,-23.9965132953185,
12.));
#194347=CARTESIAN_POINT('Ctrl Pts',(-7.55504862424812,-23.9708152779884,
0.));
#194348=CARTESIAN_POINT('Ctrl Pts',(-7.55504862424812,-23.9708152779884,
12.));
#194349=CARTESIAN_POINT('Ctrl Pts',(-7.55893897027683,-23.9451848115,0.));
#194350=CARTESIAN_POINT('Ctrl Pts',(-7.55893897027683,-23.9451848115,12.));
#194351=CARTESIAN_POINT('Ctrl Pts',(-7.56275769304773,-23.9196224070759,
0.));
#194352=CARTESIAN_POINT('Ctrl Pts',(-7.56275769304773,-23.9196224070759,
12.));
#194353=CARTESIAN_POINT('Ctrl Pts',(-7.56650497863792,-23.8941285782003,
0.));
#194354=CARTESIAN_POINT('Ctrl Pts',(-7.56650497863792,-23.8941285782003,
12.));
#194355=CARTESIAN_POINT('Ctrl Pts',(-7.57018101500711,-23.8687038399597,
0.));
#194356=CARTESIAN_POINT('Ctrl Pts',(-7.57018101500711,-23.8687038399597,
12.));
#194357=CARTESIAN_POINT('Ctrl Pts',(-7.57378599219817,-23.8433487096134,
0.));
#194358=CARTESIAN_POINT('Ctrl Pts',(-7.57378599219817,-23.8433487096134,
12.));
#194359=CARTESIAN_POINT('Ctrl Pts',(-7.57732010249066,-23.8180637069977,
0.));
#194360=CARTESIAN_POINT('Ctrl Pts',(-7.57732010249066,-23.8180637069977,
12.));
#194361=CARTESIAN_POINT('Ctrl Pts',(-7.58078354058212,-23.7928493549908,
0.));
#194362=CARTESIAN_POINT('Ctrl Pts',(-7.58078354058212,-23.7928493549908,
12.));
#194363=CARTESIAN_POINT('Ctrl Pts',(-7.58417650376272,-23.7677061799376,
0.));
#194364=CARTESIAN_POINT('Ctrl Pts',(-7.58417650376272,-23.7677061799376,
12.));
#194365=CARTESIAN_POINT('Ctrl Pts',(-7.58749919210832,-23.7426347121006,
0.));
#194366=CARTESIAN_POINT('Ctrl Pts',(-7.58749919210832,-23.7426347121006,
12.));
#194367=CARTESIAN_POINT('Ctrl Pts',(-7.59075180865327,-23.7176354860457,
0.));
#194368=CARTESIAN_POINT('Ctrl Pts',(-7.59075180865327,-23.7176354860457,
12.));
#194369=CARTESIAN_POINT('Ctrl Pts',(-7.59393455934042,-23.6927090405067,
0.));
#194370=CARTESIAN_POINT('Ctrl Pts',(-7.59393455934042,-23.6927090405067,
12.));
#194371=CARTESIAN_POINT('Ctrl Pts',(-7.59704765299572,-23.6678559182876,
0.));
#194372=CARTESIAN_POINT('Ctrl Pts',(-7.59704765299572,-23.6678559182876,
12.));
#194373=CARTESIAN_POINT('Ctrl Pts',(-7.6000913013013,-23.6430766661419,
0.));
#194374=CARTESIAN_POINT('Ctrl Pts',(-7.6000913013013,-23.6430766661419,
12.));
#194375=CARTESIAN_POINT('Ctrl Pts',(-7.60306571877806,-23.6183718346576,
0.));
#194376=CARTESIAN_POINT('Ctrl Pts',(-7.60306571877806,-23.6183718346576,
12.));
#194377=CARTESIAN_POINT('Ctrl Pts',(-7.60597112277094,-23.5937419781244,
0.));
#194378=CARTESIAN_POINT('Ctrl Pts',(-7.60597112277094,-23.5937419781244,
12.));
#194379=CARTESIAN_POINT('Ctrl Pts',(-7.608807733446,-23.5691876544243,0.));
#194380=CARTESIAN_POINT('Ctrl Pts',(-7.608807733446,-23.5691876544243,12.));
#194381=CARTESIAN_POINT('Ctrl Pts',(-7.61157577385372,-23.5447094252028,
0.));
#194382=CARTESIAN_POINT('Ctrl Pts',(-7.61157577385372,-23.5447094252028,
12.));
#194383=CARTESIAN_POINT('Ctrl Pts',(-7.61427546999299,-23.5203078560128,
0.));
#194384=CARTESIAN_POINT('Ctrl Pts',(-7.61427546999299,-23.5203078560128,
12.));
#194385=CARTESIAN_POINT('Ctrl Pts',(-7.61690705088319,-23.4959835164608,
0.));
#194386=CARTESIAN_POINT('Ctrl Pts',(-7.61690705088319,-23.4959835164608,
12.));
#194387=CARTESIAN_POINT('Ctrl Pts',(-7.61947074863978,-23.4717369803438,
0.));
#194388=CARTESIAN_POINT('Ctrl Pts',(-7.61947074863978,-23.4717369803438,
12.));
#194389=CARTESIAN_POINT('Ctrl Pts',(-7.62196679855957,-23.4475688257854,
0.));
#194390=CARTESIAN_POINT('Ctrl Pts',(-7.62196679855957,-23.4475688257854,
12.));
#194391=CARTESIAN_POINT('Ctrl Pts',(-7.62439543920055,-23.4234796353544,
0.));
#194392=CARTESIAN_POINT('Ctrl Pts',(-7.62439543920055,-23.4234796353544,
12.));
#194393=CARTESIAN_POINT('Ctrl Pts',(-7.62675691240335,-23.3994699961122,
0.));
#194394=CARTESIAN_POINT('Ctrl Pts',(-7.62675691240335,-23.3994699961122,
12.));
#194395=CARTESIAN_POINT('Ctrl Pts',(-7.62905146332598,-23.3755404996638,
0.));
#194396=CARTESIAN_POINT('Ctrl Pts',(-7.62905146332598,-23.3755404996638,
12.));
#194397=CARTESIAN_POINT('Ctrl Pts',(-7.63127934048139,-23.3516917421973,
0.));
#194398=CARTESIAN_POINT('Ctrl Pts',(-7.63127934048139,-23.3516917421973,
12.));
#194399=CARTESIAN_POINT('Ctrl Pts',(-7.63344079578163,-23.3279243245241,
0.));
#194400=CARTESIAN_POINT('Ctrl Pts',(-7.63344079578163,-23.3279243245241,
12.));
#194401=CARTESIAN_POINT('Ctrl Pts',(-7.63553608458784,-23.3042388521021,
0.));
#194402=CARTESIAN_POINT('Ctrl Pts',(-7.63553608458784,-23.3042388521021,
12.));
#194403=CARTESIAN_POINT('Ctrl Pts',(-7.63756546576375,-23.2806359350853,
0.));
#194404=CARTESIAN_POINT('Ctrl Pts',(-7.63756546576375,-23.2806359350853,
12.));
#194405=CARTESIAN_POINT('Ctrl Pts',(-7.63952920172837,-23.2571161884487,
0.));
#194406=CARTESIAN_POINT('Ctrl Pts',(-7.63952920172837,-23.2571161884487,
12.));
#194407=CARTESIAN_POINT('Ctrl Pts',(-7.64142755851508,-23.2336802320912,
0.));
#194408=CARTESIAN_POINT('Ctrl Pts',(-7.64142755851508,-23.2336802320912,
12.));
#194409=CARTESIAN_POINT('Ctrl Pts',(-7.64326080583684,-23.2103286909399,
0.));
#194410=CARTESIAN_POINT('Ctrl Pts',(-7.64326080583684,-23.2103286909399,
12.));
#194411=CARTESIAN_POINT('Ctrl Pts',(-7.64502921715483,-23.1870621950452,
0.));
#194412=CARTESIAN_POINT('Ctrl Pts',(-7.64502921715483,-23.1870621950452,
12.));
#194413=CARTESIAN_POINT('Ctrl Pts',(-7.64673306975797,-23.1638813796691,
0.));
#194414=CARTESIAN_POINT('Ctrl Pts',(-7.64673306975797,-23.1638813796691,
12.));
#194415=CARTESIAN_POINT('Ctrl Pts',(-7.64837264482929,-23.1407868853815,
0.));
#194416=CARTESIAN_POINT('Ctrl Pts',(-7.64837264482929,-23.1407868853815,
12.));
#194417=CARTESIAN_POINT('Ctrl Pts',(-7.64994822749845,-23.1177793581674,
0.));
#194418=CARTESIAN_POINT('Ctrl Pts',(-7.64994822749845,-23.1177793581674,
12.));
#194419=CARTESIAN_POINT('Ctrl Pts',(-7.65146010690465,-23.0948594495246,
0.));
#194420=CARTESIAN_POINT('Ctrl Pts',(-7.65146010690465,-23.0948594495246,
12.));
#194421=CARTESIAN_POINT('Ctrl Pts',(-7.65290857626357,-23.072027816555,
0.));
#194422=CARTESIAN_POINT('Ctrl Pts',(-7.65290857626357,-23.072027816555,
12.));
#194423=CARTESIAN_POINT('Ctrl Pts',(-7.65429393293955,-23.049285122053,
0.));
#194424=CARTESIAN_POINT('Ctrl Pts',(-7.65429393293955,-23.049285122053,
12.));
#194425=CARTESIAN_POINT('Ctrl Pts',(-7.65561647852555,-23.0266320345792,
0.));
#194426=CARTESIAN_POINT('Ctrl Pts',(-7.65561647852555,-23.0266320345792,
12.));
#194427=CARTESIAN_POINT('Ctrl Pts',(-7.6568765189133,-23.004069228582,0.));
#194428=CARTESIAN_POINT('Ctrl Pts',(-7.6568765189133,-23.004069228582,12.));
#194429=CARTESIAN_POINT('Ctrl Pts',(-7.65807436436453,-22.9815973845301,
0.));
#194430=CARTESIAN_POINT('Ctrl Pts',(-7.65807436436453,-22.9815973845301,
12.));
#194431=CARTESIAN_POINT('Ctrl Pts',(-7.65921032958912,-22.9592171890332,
0.));
#194432=CARTESIAN_POINT('Ctrl Pts',(-7.65921032958912,-22.9592171890332,
12.));
#194433=CARTESIAN_POINT('Ctrl Pts',(-7.66028473382777,-22.9369293349592,
0.));
#194434=CARTESIAN_POINT('Ctrl Pts',(-7.66028473382777,-22.9369293349592,
12.));
#194435=CARTESIAN_POINT('Ctrl Pts',(-7.661297900941,-22.9147345215418,0.));
#194436=CARTESIAN_POINT('Ctrl Pts',(-7.661297900941,-22.9147345215418,12.));
#194437=CARTESIAN_POINT('Ctrl Pts',(-7.66225015950148,-22.8926334544879,
0.));
#194438=CARTESIAN_POINT('Ctrl Pts',(-7.66225015950148,-22.8926334544879,
12.));
#194439=CARTESIAN_POINT('Ctrl Pts',(-7.66314184287334,-22.870626846128,
0.));
#194440=CARTESIAN_POINT('Ctrl Pts',(-7.66314184287334,-22.870626846128,
12.));
#194441=CARTESIAN_POINT('Ctrl Pts',(-7.66397328929805,-22.8487154155569,
0.));
#194442=CARTESIAN_POINT('Ctrl Pts',(-7.66397328929805,-22.8487154155569,
12.));
#194443=CARTESIAN_POINT('Ctrl Pts',(-7.66474484198553,-22.8268998887678,
0.));
#194444=CARTESIAN_POINT('Ctrl Pts',(-7.66474484198553,-22.8268998887678,
12.));
#194445=CARTESIAN_POINT('Ctrl Pts',(-7.66545684920988,-22.8051809987833,
0.));
#194446=CARTESIAN_POINT('Ctrl Pts',(-7.66545684920988,-22.8051809987833,
12.));
#194447=CARTESIAN_POINT('Ctrl Pts',(-7.66610966441259,-22.7835594857697,
0.));
#194448=CARTESIAN_POINT('Ctrl Pts',(-7.66610966441259,-22.7835594857697,
12.));
#194449=CARTESIAN_POINT('Ctrl Pts',(-7.66670364630273,-22.7620360971839,
0.));
#194450=CARTESIAN_POINT('Ctrl Pts',(-7.66670364630273,-22.7620360971839,
12.));
#194451=CARTESIAN_POINT('Ctrl Pts',(-7.66723915895413,-22.7406115879508,
0.));
#194452=CARTESIAN_POINT('Ctrl Pts',(-7.66723915895413,-22.7406115879508,
12.));
#194453=CARTESIAN_POINT('Ctrl Pts',(-7.6677165719101,-22.7192867206242,
0.));
#194454=CARTESIAN_POINT('Ctrl Pts',(-7.6677165719101,-22.7192867206242,
12.));
#194455=CARTESIAN_POINT('Ctrl Pts',(-7.66813626029277,-22.6980622655446,
0.));
#194456=CARTESIAN_POINT('Ctrl Pts',(-7.66813626029277,-22.6980622655446,
12.));
#194457=CARTESIAN_POINT('Ctrl Pts',(-7.66849860491763,-22.6769390009889,
0.));
#194458=CARTESIAN_POINT('Ctrl Pts',(-7.66849860491763,-22.6769390009889,
12.));
#194459=CARTESIAN_POINT('Ctrl Pts',(-7.66880399241354,-22.6559177133133,
0.));
#194460=CARTESIAN_POINT('Ctrl Pts',(-7.66880399241354,-22.6559177133133,
12.));
#194461=CARTESIAN_POINT('Ctrl Pts',(-7.66905281533745,-22.6349991971547,
0.));
#194462=CARTESIAN_POINT('Ctrl Pts',(-7.66905281533745,-22.6349991971547,
12.));
#194463=CARTESIAN_POINT('Ctrl Pts',(-7.66924547229435,-22.6141842556248,
0.));
#194464=CARTESIAN_POINT('Ctrl Pts',(-7.66924547229435,-22.6141842556248,
12.));
#194465=CARTESIAN_POINT('Ctrl Pts',(-7.66938236806241,-22.5934737004955,
0.));
#194466=CARTESIAN_POINT('Ctrl Pts',(-7.66938236806241,-22.5934737004955,
12.));
#194467=CARTESIAN_POINT('Ctrl Pts',(-7.66946391372299,-22.5728683523828,
0.));
#194468=CARTESIAN_POINT('Ctrl Pts',(-7.66946391372299,-22.5728683523828,
12.));
#194469=CARTESIAN_POINT('Ctrl Pts',(-7.66949052679672,-22.5523690409109,
0.));
#194470=CARTESIAN_POINT('Ctrl Pts',(-7.66949052679672,-22.5523690409109,
12.));
#194471=CARTESIAN_POINT('Ctrl Pts',(-7.66946263138116,-22.5319766049191,
0.));
#194472=CARTESIAN_POINT('Ctrl Pts',(-7.66946263138116,-22.5319766049191,
12.));
#194473=CARTESIAN_POINT('Ctrl Pts',(-7.66938065829083,-22.5116918927023,
0.));
#194474=CARTESIAN_POINT('Ctrl Pts',(-7.66938065829083,-22.5116918927023,
12.));
#194475=CARTESIAN_POINT('Ctrl Pts',(-7.66924504520302,-22.4915157622308,
0.));
#194476=CARTESIAN_POINT('Ctrl Pts',(-7.66924504520302,-22.4915157622308,
12.));
#194477=CARTESIAN_POINT('Ctrl Pts',(-7.66905623680836,-22.47144908137,0.));
#194478=CARTESIAN_POINT('Ctrl Pts',(-7.66905623680836,-22.47144908137,12.));
#194479=CARTESIAN_POINT('Ctrl Pts',(-7.6688146849666,-22.4514927280862,
0.));
#194480=CARTESIAN_POINT('Ctrl Pts',(-7.6688146849666,-22.4514927280862,
12.));
#194481=CARTESIAN_POINT('Ctrl Pts',(-7.66852084886746,-22.4316475906616,
0.));
#194482=CARTESIAN_POINT('Ctrl Pts',(-7.66852084886746,-22.4316475906616,
12.));
#194483=CARTESIAN_POINT('Ctrl Pts',(-7.66817519519682,-22.411914567977,
0.));
#194484=CARTESIAN_POINT('Ctrl Pts',(-7.66817519519682,-22.411914567977,
12.));
#194485=CARTESIAN_POINT('Ctrl Pts',(-7.6677781983082,-22.3922945697782,
0.));
#194486=CARTESIAN_POINT('Ctrl Pts',(-7.6677781983082,-22.3922945697782,
12.));
#194487=CARTESIAN_POINT('Ctrl Pts',(-7.66733034039887,-22.3727885169361,
0.));
#194488=CARTESIAN_POINT('Ctrl Pts',(-7.66733034039887,-22.3727885169361,
12.));
#194489=CARTESIAN_POINT('Ctrl Pts',(-7.66683211169134,-22.3533973417013,
0.));
#194490=CARTESIAN_POINT('Ctrl Pts',(-7.66683211169134,-22.3533973417013,
12.));
#194491=CARTESIAN_POINT('Ctrl Pts',(-7.66628401061906,-22.3341219879454,
0.));
#194492=CARTESIAN_POINT('Ctrl Pts',(-7.66628401061906,-22.3341219879454,
12.));
#194493=CARTESIAN_POINT('Ctrl Pts',(-7.66568654402442,-22.3149634114823,
0.));
#194494=CARTESIAN_POINT('Ctrl Pts',(-7.66568654402442,-22.3149634114823,
12.));
#194495=CARTESIAN_POINT('Ctrl Pts',(-7.66504022736263,-22.2959225803925,
0.));
#194496=CARTESIAN_POINT('Ctrl Pts',(-7.66504022736263,-22.2959225803925,
12.));
#194497=CARTESIAN_POINT('Ctrl Pts',(-7.66434558490973,-22.2770004753332,
0.));
#194498=CARTESIAN_POINT('Ctrl Pts',(-7.66434558490973,-22.2770004753332,
12.));
#194499=CARTESIAN_POINT('Ctrl Pts',(-7.66360314997662,-22.2581980898487,
0.));
#194500=CARTESIAN_POINT('Ctrl Pts',(-7.66360314997662,-22.2581980898487,
12.));
#194501=CARTESIAN_POINT('Ctrl Pts',(-7.66281346512546,-22.239516430656,
0.));
#194502=CARTESIAN_POINT('Ctrl Pts',(-7.66281346512546,-22.239516430656,
12.));
#194503=CARTESIAN_POINT('Ctrl Pts',(-7.66197708240436,-22.2209565180098,
0.));
#194504=CARTESIAN_POINT('Ctrl Pts',(-7.66197708240436,-22.2209565180098,
12.));
#194505=CARTESIAN_POINT('Ctrl Pts',(-7.66109456359292,-22.2025193860972,
0.));
#194506=CARTESIAN_POINT('Ctrl Pts',(-7.66109456359292,-22.2025193860972,
12.));
#194507=CARTESIAN_POINT('Ctrl Pts',(-7.66016648045008,-22.1842060834092,
0.));
#194508=CARTESIAN_POINT('Ctrl Pts',(-7.66016648045008,-22.1842060834092,
12.));
#194509=CARTESIAN_POINT('Ctrl Pts',(-7.65919341496926,-22.1660176731174,
0.));
#194510=CARTESIAN_POINT('Ctrl Pts',(-7.65919341496926,-22.1660176731174,
12.));
#194511=CARTESIAN_POINT('Ctrl Pts',(-7.65817595963351,-22.1479552334206,
0.));
#194512=CARTESIAN_POINT('Ctrl Pts',(-7.65817595963351,-22.1479552334206,
12.));
#194513=CARTESIAN_POINT('Ctrl Pts',(-7.65711471769407,-22.1300198579671,
0.));
#194514=CARTESIAN_POINT('Ctrl Pts',(-7.65711471769407,-22.1300198579671,
12.));
#194515=CARTESIAN_POINT('Ctrl Pts',(-7.65601030346819,-22.1122126563327,
0.));
#194516=CARTESIAN_POINT('Ctrl Pts',(-7.65601030346819,-22.1122126563327,
12.));
#194517=CARTESIAN_POINT('Ctrl Pts',(-7.65486334263651,-22.094534754469,
0.));
#194518=CARTESIAN_POINT('Ctrl Pts',(-7.65486334263651,-22.094534754469,
12.));
#194519=CARTESIAN_POINT('Ctrl Pts',(-7.65367447254945,-22.0769872951596,
0.));
#194520=CARTESIAN_POINT('Ctrl Pts',(-7.65367447254945,-22.0769872951596,
12.));
#194521=CARTESIAN_POINT('Ctrl Pts',(-7.65244434253104,-22.0595714384432,
0.));
#194522=CARTESIAN_POINT('Ctrl Pts',(-7.65244434253104,-22.0595714384432,
12.));
#194523=CARTESIAN_POINT('Ctrl Pts',(-7.65117361421347,-22.0422883621176,
0.));
#194524=CARTESIAN_POINT('Ctrl Pts',(-7.65117361421347,-22.0422883621176,
12.));
#194525=CARTESIAN_POINT('Ctrl Pts',(-7.64986296190157,-22.0251392623209,
0.));
#194526=CARTESIAN_POINT('Ctrl Pts',(-7.64986296190157,-22.0251392623209,
12.));
#194527=CARTESIAN_POINT('Ctrl Pts',(-7.64851307293346,-22.0081253540773,
0.));
#194528=CARTESIAN_POINT('Ctrl Pts',(-7.64851307293346,-22.0081253540773,
12.));
#194529=CARTESIAN_POINT('Ctrl Pts',(-7.64712464805258,-21.9912478718542,
0.));
#194530=CARTESIAN_POINT('Ctrl Pts',(-7.64712464805258,-21.9912478718542,
12.));
#194531=CARTESIAN_POINT('Ctrl Pts',(-7.64569840177359,-21.97450807008,0.));
#194532=CARTESIAN_POINT('Ctrl Pts',(-7.64569840177359,-21.97450807008,12.));
#194533=CARTESIAN_POINT('Ctrl Pts',(-7.64423506279154,-21.9579072237653,
0.));
#194534=CARTESIAN_POINT('Ctrl Pts',(-7.64423506279154,-21.9579072237653,
12.));
#194535=CARTESIAN_POINT('Ctrl Pts',(-7.64273537442707,-21.9414466292074,
0.));
#194536=CARTESIAN_POINT('Ctrl Pts',(-7.64273537442707,-21.9414466292074,
12.));
#194537=CARTESIAN_POINT('Ctrl Pts',(-7.6412000950654,-21.9251276046546,
0.));
#194538=CARTESIAN_POINT('Ctrl Pts',(-7.6412000950654,-21.9251276046546,
12.));
#194539=CARTESIAN_POINT('Ctrl Pts',(-7.63962999860917,-21.9089514909873,
0.));
#194540=CARTESIAN_POINT('Ctrl Pts',(-7.63962999860917,-21.9089514909873,
12.));
#194541=CARTESIAN_POINT('Ctrl Pts',(-7.63802587492008,-21.8929196523511,
0.));
#194542=CARTESIAN_POINT('Ctrl Pts',(-7.63802587492008,-21.8929196523511,
12.));
#194543=CARTESIAN_POINT('Ctrl Pts',(-7.63638853033368,-21.8770334769492,
0.));
#194544=CARTESIAN_POINT('Ctrl Pts',(-7.63638853033368,-21.8770334769492,
12.));
#194545=CARTESIAN_POINT('Ctrl Pts',(-7.63471878821204,-21.8612943779086,
0.));
#194546=CARTESIAN_POINT('Ctrl Pts',(-7.63471878821204,-21.8612943779086,
12.));
#194547=CARTESIAN_POINT('Ctrl Pts',(-7.63301748948936,-21.8457037941084,
0.));
#194548=CARTESIAN_POINT('Ctrl Pts',(-7.63301748948936,-21.8457037941084,
12.));
#194549=CARTESIAN_POINT('Ctrl Pts',(-7.6312854932304,-21.8302631910197,
0.));
#194550=CARTESIAN_POINT('Ctrl Pts',(-7.6312854932304,-21.8302631910197,
12.));
#194551=CARTESIAN_POINT('Ctrl Pts',(-7.62952367718151,-21.8149740615093,
0.));
#194552=CARTESIAN_POINT('Ctrl Pts',(-7.62952367718151,-21.8149740615093,
12.));
#194553=CARTESIAN_POINT('Ctrl Pts',(-7.62773293842409,-21.7998379268583,
0.));
#194554=CARTESIAN_POINT('Ctrl Pts',(-7.62773293842409,-21.7998379268583,
12.));
#194555=CARTESIAN_POINT('Ctrl Pts',(-7.62591419404521,-21.7848563378022,
0.));
#194556=CARTESIAN_POINT('Ctrl Pts',(-7.62591419404521,-21.7848563378022,
12.));
#194557=CARTESIAN_POINT('Ctrl Pts',(-7.62406838181164,-21.7700308755583,
0.));
#194558=CARTESIAN_POINT('Ctrl Pts',(-7.62406838181164,-21.7700308755583,
12.));
#194559=CARTESIAN_POINT('Ctrl Pts',(-7.62219646084226,-21.7553631528329,
0.));
#194560=CARTESIAN_POINT('Ctrl Pts',(-7.62219646084226,-21.7553631528329,
12.));
#194561=CARTESIAN_POINT('Ctrl Pts',(-7.62029941230855,-21.7408548148657,
0.));
#194562=CARTESIAN_POINT('Ctrl Pts',(-7.62029941230855,-21.7408548148657,
12.));
#194563=CARTESIAN_POINT('Ctrl Pts',(-7.61837824030542,-21.7265075407977,
0.));
#194564=CARTESIAN_POINT('Ctrl Pts',(-7.61837824030542,-21.7265075407977,
12.));
#194565=CARTESIAN_POINT('Ctrl Pts',(-7.61643397270425,-21.7123230449835,
0.));
#194566=CARTESIAN_POINT('Ctrl Pts',(-7.61643397270425,-21.7123230449835,
12.));
#194567=CARTESIAN_POINT('Ctrl Pts',(-7.61446766202787,-21.6983030783321,
0.));
#194568=CARTESIAN_POINT('Ctrl Pts',(-7.61446766202787,-21.6983030783321,
12.));
#194569=CARTESIAN_POINT('Ctrl Pts',(-7.61248038630265,-21.6844494295813,
0.));
#194570=CARTESIAN_POINT('Ctrl Pts',(-7.61248038630265,-21.6844494295813,
12.));
#194571=CARTESIAN_POINT('Ctrl Pts',(-7.6104732500095,-21.6707639267573,
0.));
#194572=CARTESIAN_POINT('Ctrl Pts',(-7.6104732500095,-21.6707639267573,
12.));
#194573=CARTESIAN_POINT('Ctrl Pts',(-7.60844738512872,-21.6572484388079,
0.));
#194574=CARTESIAN_POINT('Ctrl Pts',(-7.60844738512872,-21.6572484388079,
12.));
#194575=CARTESIAN_POINT('Ctrl Pts',(-7.60640395216359,-21.6439048771743,
0.));
#194576=CARTESIAN_POINT('Ctrl Pts',(-7.60640395216359,-21.6439048771743,
12.));
#194577=CARTESIAN_POINT('Ctrl Pts',(-7.604344141183,-21.6307351973823,0.));
#194578=CARTESIAN_POINT('Ctrl Pts',(-7.604344141183,-21.6307351973823,12.));
#194579=CARTESIAN_POINT('Ctrl Pts',(-7.60226917285432,-21.6177414005991,
0.));
#194580=CARTESIAN_POINT('Ctrl Pts',(-7.60226917285432,-21.6177414005991,
12.));
#194581=CARTESIAN_POINT('Ctrl Pts',(-7.60018029988238,-21.6049255358842,
0.));
#194582=CARTESIAN_POINT('Ctrl Pts',(-7.60018029988238,-21.6049255358842,
12.));
#194583=CARTESIAN_POINT('Ctrl Pts',(-7.59807880846193,-21.5922897024466,
0.));
#194584=CARTESIAN_POINT('Ctrl Pts',(-7.59807880846193,-21.5922897024466,
12.));
#194585=CARTESIAN_POINT('Ctrl Pts',(-7.59596601973589,-21.5798360518978,
0.));
#194586=CARTESIAN_POINT('Ctrl Pts',(-7.59596601973589,-21.5798360518978,
12.));
#194587=CARTESIAN_POINT('Ctrl Pts',(-7.5938432912493,-21.5675667904728,
0.));
#194588=CARTESIAN_POINT('Ctrl Pts',(-7.5938432912493,-21.5675667904728,
12.));
#194589=CARTESIAN_POINT('Ctrl Pts',(-7.59171201844793,-21.5554841813465,
0.));
#194590=CARTESIAN_POINT('Ctrl Pts',(-7.59171201844793,-21.5554841813465,
12.));
#194591=CARTESIAN_POINT('Ctrl Pts',(-7.58957363620026,-21.5435905470113,
0.));
#194592=CARTESIAN_POINT('Ctrl Pts',(-7.58957363620026,-21.5435905470113,
12.));
#194593=CARTESIAN_POINT('Ctrl Pts',(-7.58742962034834,-21.5318882716735,
0.));
#194594=CARTESIAN_POINT('Ctrl Pts',(-7.58742962034834,-21.5318882716735,
12.));
#194595=CARTESIAN_POINT('Ctrl Pts',(-7.58528148919114,-21.5203798035294,
0.));
#194596=CARTESIAN_POINT('Ctrl Pts',(-7.58528148919114,-21.5203798035294,
12.));
#194597=CARTESIAN_POINT('Ctrl Pts',(-7.58313080519159,-21.5090676573866,
0.));
#194598=CARTESIAN_POINT('Ctrl Pts',(-7.58313080519159,-21.5090676573866,
12.));
#194599=CARTESIAN_POINT('Ctrl Pts',(-7.5809791779073,-21.4979544192739,
0.));
#194600=CARTESIAN_POINT('Ctrl Pts',(-7.5809791779073,-21.4979544192739,
12.));
#194601=CARTESIAN_POINT('Ctrl Pts',(-7.57882826679131,-21.4870427508193,
0.));
#194602=CARTESIAN_POINT('Ctrl Pts',(-7.57882826679131,-21.4870427508193,
12.));
#194603=CARTESIAN_POINT('Ctrl Pts',(-7.57667978403003,-21.4763353936766,
0.));
#194604=CARTESIAN_POINT('Ctrl Pts',(-7.57667978403003,-21.4763353936766,
12.));
#194605=CARTESIAN_POINT('Ctrl Pts',(-7.57453549743435,-21.4658351740135,
0.));
#194606=CARTESIAN_POINT('Ctrl Pts',(-7.57453549743435,-21.4658351740135,
12.));
#194607=CARTESIAN_POINT('Ctrl Pts',(-7.57239723223521,-21.4555450053147,
0.));
#194608=CARTESIAN_POINT('Ctrl Pts',(-7.57239723223521,-21.4555450053147,
12.));
#194609=CARTESIAN_POINT('Ctrl Pts',(-7.5702668726117,-21.445467890751,0.));
#194610=CARTESIAN_POINT('Ctrl Pts',(-7.5702668726117,-21.445467890751,12.));
#194611=CARTESIAN_POINT('Ctrl Pts',(-7.56814636360842,-21.435606926151,
0.));
#194612=CARTESIAN_POINT('Ctrl Pts',(-7.56814636360842,-21.435606926151,
12.));
#194613=CARTESIAN_POINT('Ctrl Pts',(-7.56603771218706,-21.4259653015732,
0.));
#194614=CARTESIAN_POINT('Ctrl Pts',(-7.56603771218706,-21.4259653015732,
12.));
#194615=CARTESIAN_POINT('Ctrl Pts',(-7.56394299313683,-21.4165463106252,
0.));
#194616=CARTESIAN_POINT('Ctrl Pts',(-7.56394299313683,-21.4165463106252,
12.));
#194617=CARTESIAN_POINT('Ctrl Pts',(-7.56186435703622,-21.4073533630364,
0.));
#194618=CARTESIAN_POINT('Ctrl Pts',(-7.56186435703622,-21.4073533630364,
12.));
#194619=CARTESIAN_POINT('Ctrl Pts',(-7.55980403700615,-21.3983899952988,
0.));
#194620=CARTESIAN_POINT('Ctrl Pts',(-7.55980403700615,-21.3983899952988,
12.));
#194621=CARTESIAN_POINT('Ctrl Pts',(-7.55776435731422,-21.3896598842119,
0.));
#194622=CARTESIAN_POINT('Ctrl Pts',(-7.55776435731422,-21.3896598842119,
12.));
#194623=CARTESIAN_POINT('Ctrl Pts',(-7.55574773403508,-21.3811668478933,
0.));
#194624=CARTESIAN_POINT('Ctrl Pts',(-7.55574773403508,-21.3811668478933,
12.));
#194625=CARTESIAN_POINT('Ctrl Pts',(-7.55375667080032,-21.3729148390244,
0.));
#194626=CARTESIAN_POINT('Ctrl Pts',(-7.55375667080032,-21.3729148390244,
12.));
#194627=CARTESIAN_POINT('Ctrl Pts',(-7.55179375777442,-21.3649079431864,
0.));
#194628=CARTESIAN_POINT('Ctrl Pts',(-7.55179375777442,-21.3649079431864,
12.));
#194629=CARTESIAN_POINT('Ctrl Pts',(-7.54986166521307,-21.3571503685853,
0.));
#194630=CARTESIAN_POINT('Ctrl Pts',(-7.54986166521307,-21.3571503685853,
12.));
#194631=CARTESIAN_POINT('Ctrl Pts',(-7.54796316246327,-21.349646476153,
0.));
#194632=CARTESIAN_POINT('Ctrl Pts',(-7.54796316246327,-21.349646476153,
12.));
#194633=CARTESIAN_POINT('Ctrl Pts',(-7.54610114948351,-21.3424008295038,
0.));
#194634=CARTESIAN_POINT('Ctrl Pts',(-7.54610114948351,-21.3424008295038,
12.));
#194635=CARTESIAN_POINT('Ctrl Pts',(-7.54427868151269,-21.3354182340149,
0.));
#194636=CARTESIAN_POINT('Ctrl Pts',(-7.54427868151269,-21.3354182340149,
12.));
#194637=CARTESIAN_POINT('Ctrl Pts',(-7.54249900377032,-21.328703791771,
0.));
#194638=CARTESIAN_POINT('Ctrl Pts',(-7.54249900377032,-21.328703791771,
12.));
#194639=CARTESIAN_POINT('Ctrl Pts',(-7.5407655203828,-21.3222628524165,
0.));
#194640=CARTESIAN_POINT('Ctrl Pts',(-7.5407655203828,-21.3222628524165,
12.));
#194641=CARTESIAN_POINT('Ctrl Pts',(-7.53908175169899,-21.3161009456256,
0.));
#194642=CARTESIAN_POINT('Ctrl Pts',(-7.53908175169899,-21.3161009456256,
12.));
#194643=CARTESIAN_POINT('Ctrl Pts',(-7.5374512936462,-21.3102237167729,
0.));
#194644=CARTESIAN_POINT('Ctrl Pts',(-7.5374512936462,-21.3102237167729,
12.));
#194645=CARTESIAN_POINT('Ctrl Pts',(-7.53587778251743,-21.3046368712156,
0.));
#194646=CARTESIAN_POINT('Ctrl Pts',(-7.53587778251743,-21.3046368712156,
12.));
#194647=CARTESIAN_POINT('Ctrl Pts',(-7.53436505309949,-21.2993464250717,
0.));
#194648=CARTESIAN_POINT('Ctrl Pts',(-7.53436505309949,-21.2993464250717,
12.));
#194649=CARTESIAN_POINT('Ctrl Pts',(-7.53291726078527,-21.2943588989331,
0.));
#194650=CARTESIAN_POINT('Ctrl Pts',(-7.53291726078527,-21.2943588989331,
12.));
#194651=CARTESIAN_POINT('Ctrl Pts',(-7.53153906987847,-21.2896816163843,
0.));
#194652=CARTESIAN_POINT('Ctrl Pts',(-7.53153906987847,-21.2896816163843,
12.));
#194653=CARTESIAN_POINT('Ctrl Pts',(-7.53023562438221,-21.2853226580658,
0.));
#194654=CARTESIAN_POINT('Ctrl Pts',(-7.53023562438221,-21.2853226580658,
12.));
#194655=CARTESIAN_POINT('Ctrl Pts',(-7.52901217930407,-21.2812902781143,
0.));
#194656=CARTESIAN_POINT('Ctrl Pts',(-7.52901217930407,-21.2812902781143,
12.));
#194657=CARTESIAN_POINT('Ctrl Pts',(-7.52787386225344,-21.2775925269651,
0.));
#194658=CARTESIAN_POINT('Ctrl Pts',(-7.52787386225344,-21.2775925269651,
12.));
#194659=CARTESIAN_POINT('Ctrl Pts',(-7.52682526918561,-21.2742366113578,
0.));
#194660=CARTESIAN_POINT('Ctrl Pts',(-7.52682526918561,-21.2742366113578,
12.));
#194661=CARTESIAN_POINT('Ctrl Pts',(-7.52587126095544,-21.2712301573465,
0.));
#194662=CARTESIAN_POINT('Ctrl Pts',(-7.52587126095544,-21.2712301573465,
12.));
#194663=CARTESIAN_POINT('Ctrl Pts',(-7.52501770333522,-21.2685823838672,
0.));
#194664=CARTESIAN_POINT('Ctrl Pts',(-7.52501770333522,-21.2685823838672,
12.));
#194665=CARTESIAN_POINT('Ctrl Pts',(-7.52427261074264,-21.266305915706,
0.));
#194666=CARTESIAN_POINT('Ctrl Pts',(-7.52427261074264,-21.266305915706,
12.));
#194667=CARTESIAN_POINT('Ctrl Pts',(-7.52364573027521,-21.2644161259965,
0.));
#194668=CARTESIAN_POINT('Ctrl Pts',(-7.52364573027521,-21.2644161259965,
12.));
#194669=CARTESIAN_POINT('Ctrl Pts',(-7.52314642316203,-21.262927782038,
0.));
#194670=CARTESIAN_POINT('Ctrl Pts',(-7.52314642316203,-21.262927782038,
12.));
#194671=CARTESIAN_POINT('Ctrl Pts',(-7.52278182242728,-21.261852128355,
0.));
#194672=CARTESIAN_POINT('Ctrl Pts',(-7.52278182242728,-21.261852128355,
12.));
#194673=CARTESIAN_POINT('Ctrl Pts',(-7.52260064231736,-21.2613260540651,
0.));
#194674=CARTESIAN_POINT('Ctrl Pts',(-7.52260064231736,-21.2613260540651,
12.));
#194675=CARTESIAN_POINT('Ctrl Pts',(-7.52252744144958,-21.261120447486,
0.));
#194676=CARTESIAN_POINT('Ctrl Pts',(-7.52252744144958,-21.261120447486,
12.));
#194677=CARTESIAN_POINT('Ctrl Pts',(-7.52250649703992,-21.2610673466883,
0.));
#194678=CARTESIAN_POINT('Ctrl Pts',(-7.52250649703992,-21.2610673466883,
12.));
#194679=CARTESIAN_POINT('Ctrl Pts',(-7.52250298901266,-21.2610617890679,
0.));
#194680=CARTESIAN_POINT('Ctrl Pts',(-7.52250298901266,-21.2610617890679,
12.));
#194681=CARTESIAN_POINT('',(-7.36589684767345,-24.9347862158358,0.));
#194682=CARTESIAN_POINT('Ctrl Pts',(-7.36589684767345,-24.9347862158358,
0.));
#194683=CARTESIAN_POINT('Ctrl Pts',(-7.36721909028843,-24.9292275670674,
0.));
#194684=CARTESIAN_POINT('Ctrl Pts',(-7.36985593120091,-24.9181155530543,
0.));
#194685=CARTESIAN_POINT('Ctrl Pts',(-7.37378825961676,-24.901463382605,
0.));
#194686=CARTESIAN_POINT('Ctrl Pts',(-7.3789854964027,-24.8792921911115,
0.));
#194687=CARTESIAN_POINT('Ctrl Pts',(-7.38540558903621,-24.8516310625176,
0.));
#194688=CARTESIAN_POINT('Ctrl Pts',(-7.39174922585809,-24.8240228520893,
0.));
#194689=CARTESIAN_POINT('Ctrl Pts',(-7.39801641583013,-24.7964676646431,
0.));
#194690=CARTESIAN_POINT('Ctrl Pts',(-7.40420718661603,-24.7689656668983,
0.));
#194691=CARTESIAN_POINT('Ctrl Pts',(-7.41032159082382,-24.7415170994784,
0.));
#194692=CARTESIAN_POINT('Ctrl Pts',(-7.41635971481674,-24.7141222950051,
0.));
#194693=CARTESIAN_POINT('Ctrl Pts',(-7.42232167766266,-24.6867816727192,
0.));
#194694=CARTESIAN_POINT('Ctrl Pts',(-7.42820762159126,-24.6594957128756,
0.));
#194695=CARTESIAN_POINT('Ctrl Pts',(-7.43401770489524,-24.6322649369517,
0.));
#194696=CARTESIAN_POINT('Ctrl Pts',(-7.43975209375504,-24.6050898852368,
0.));
#194697=CARTESIAN_POINT('Ctrl Pts',(-7.44541095473135,-24.577971096086,
0.));
#194698=CARTESIAN_POINT('Ctrl Pts',(-7.4509944465116,-24.5509090831559,
0.));
#194699=CARTESIAN_POINT('Ctrl Pts',(-7.45650271335862,-24.5239043173072,
0.));
#194700=CARTESIAN_POINT('Ctrl Pts',(-7.46193588961464,-24.4969572391483,
0.));
#194701=CARTESIAN_POINT('Ctrl Pts',(-7.46729410308787,-24.4700682684524,
0.));
#194702=CARTESIAN_POINT('Ctrl Pts',(-7.47257747883246,-24.443237814649,
0.));
#194703=CARTESIAN_POINT('Ctrl Pts',(-7.47778614286565,-24.4164662871163,
0.));
#194704=CARTESIAN_POINT('Ctrl Pts',(-7.48292022569301,-24.3897541049254,
0.));
#194705=CARTESIAN_POINT('Ctrl Pts',(-7.48797986651909,-24.3631017084524,
0.));
#194706=CARTESIAN_POINT('Ctrl Pts',(-7.49296521252421,-24.3365095573685,
0.));
#194707=CARTESIAN_POINT('Ctrl Pts',(-7.49787641695439,-24.3099781253355,
0.));
#194708=CARTESIAN_POINT('Ctrl Pts',(-7.50271363765152,-24.2835078958973,
0.));
#194709=CARTESIAN_POINT('Ctrl Pts',(-7.50747703535134,-24.2570993577034,
0.));
#194710=CARTESIAN_POINT('Ctrl Pts',(-7.51216677222181,-24.2307530003887,
0.));
#194711=CARTESIAN_POINT('Ctrl Pts',(-7.51678300997949,-24.2044693092349,
0.));
#194712=CARTESIAN_POINT('Ctrl Pts',(-7.52132590953802,-24.1782487641594,
0.));
#194713=CARTESIAN_POINT('Ctrl Pts',(-7.52579563201424,-24.1520918425364,
0.));
#194714=CARTESIAN_POINT('Ctrl Pts',(-7.53019233935502,-24.1259990209207,
0.));
#194715=CARTESIAN_POINT('Ctrl Pts',(-7.53451619514649,-24.0999707772642,
0.));
#194716=CARTESIAN_POINT('Ctrl Pts',(-7.53876736531014,-24.0740075927985,
0.));
#194717=CARTESIAN_POINT('Ctrl Pts',(-7.54294601896145,-24.0481099543353,
0.));
#194718=CARTESIAN_POINT('Ctrl Pts',(-7.5470523288591,-24.022278355453,0.));
#194719=CARTESIAN_POINT('Ctrl Pts',(-7.55108647097441,-23.9965132953185,
0.));
#194720=CARTESIAN_POINT('Ctrl Pts',(-7.55504862424812,-23.9708152779884,
0.));
#194721=CARTESIAN_POINT('Ctrl Pts',(-7.55893897027683,-23.9451848115,0.));
#194722=CARTESIAN_POINT('Ctrl Pts',(-7.56275769304773,-23.9196224070759,
0.));
#194723=CARTESIAN_POINT('Ctrl Pts',(-7.56650497863792,-23.8941285782003,
0.));
#194724=CARTESIAN_POINT('Ctrl Pts',(-7.57018101500711,-23.8687038399597,
0.));
#194725=CARTESIAN_POINT('Ctrl Pts',(-7.57378599219817,-23.8433487096134,
0.));
#194726=CARTESIAN_POINT('Ctrl Pts',(-7.57732010249066,-23.8180637069977,
0.));
#194727=CARTESIAN_POINT('Ctrl Pts',(-7.58078354058212,-23.7928493549908,
0.));
#194728=CARTESIAN_POINT('Ctrl Pts',(-7.58417650376272,-23.7677061799376,
0.));
#194729=CARTESIAN_POINT('Ctrl Pts',(-7.58749919210832,-23.7426347121006,
0.));
#194730=CARTESIAN_POINT('Ctrl Pts',(-7.59075180865327,-23.7176354860457,
0.));
#194731=CARTESIAN_POINT('Ctrl Pts',(-7.59393455934042,-23.6927090405067,
0.));
#194732=CARTESIAN_POINT('Ctrl Pts',(-7.59704765299572,-23.6678559182876,
0.));
#194733=CARTESIAN_POINT('Ctrl Pts',(-7.6000913013013,-23.6430766661419,
0.));
#194734=CARTESIAN_POINT('Ctrl Pts',(-7.60306571877806,-23.6183718346576,
0.));
#194735=CARTESIAN_POINT('Ctrl Pts',(-7.60597112277094,-23.5937419781244,
0.));
#194736=CARTESIAN_POINT('Ctrl Pts',(-7.608807733446,-23.5691876544243,0.));
#194737=CARTESIAN_POINT('Ctrl Pts',(-7.61157577385372,-23.5447094252028,
0.));
#194738=CARTESIAN_POINT('Ctrl Pts',(-7.61427546999299,-23.5203078560128,
0.));
#194739=CARTESIAN_POINT('Ctrl Pts',(-7.61690705088319,-23.4959835164608,
0.));
#194740=CARTESIAN_POINT('Ctrl Pts',(-7.61947074863978,-23.4717369803438,
0.));
#194741=CARTESIAN_POINT('Ctrl Pts',(-7.62196679855957,-23.4475688257854,
0.));
#194742=CARTESIAN_POINT('Ctrl Pts',(-7.62439543920055,-23.4234796353544,
0.));
#194743=CARTESIAN_POINT('Ctrl Pts',(-7.62675691240335,-23.3994699961122,
0.));
#194744=CARTESIAN_POINT('Ctrl Pts',(-7.62905146332598,-23.3755404996638,
0.));
#194745=CARTESIAN_POINT('Ctrl Pts',(-7.63127934048139,-23.3516917421973,
0.));
#194746=CARTESIAN_POINT('Ctrl Pts',(-7.63344079578163,-23.3279243245241,
0.));
#194747=CARTESIAN_POINT('Ctrl Pts',(-7.63553608458784,-23.3042388521021,
0.));
#194748=CARTESIAN_POINT('Ctrl Pts',(-7.63756546576375,-23.2806359350853,
0.));
#194749=CARTESIAN_POINT('Ctrl Pts',(-7.63952920172837,-23.2571161884487,
0.));
#194750=CARTESIAN_POINT('Ctrl Pts',(-7.64142755851508,-23.2336802320912,
0.));
#194751=CARTESIAN_POINT('Ctrl Pts',(-7.64326080583684,-23.2103286909399,
0.));
#194752=CARTESIAN_POINT('Ctrl Pts',(-7.64502921715483,-23.1870621950452,
0.));
#194753=CARTESIAN_POINT('Ctrl Pts',(-7.64673306975797,-23.1638813796691,
0.));
#194754=CARTESIAN_POINT('Ctrl Pts',(-7.64837264482929,-23.1407868853815,
0.));
#194755=CARTESIAN_POINT('Ctrl Pts',(-7.64994822749845,-23.1177793581674,
0.));
#194756=CARTESIAN_POINT('Ctrl Pts',(-7.65146010690465,-23.0948594495246,
0.));
#194757=CARTESIAN_POINT('Ctrl Pts',(-7.65290857626357,-23.072027816555,
0.));
#194758=CARTESIAN_POINT('Ctrl Pts',(-7.65429393293955,-23.049285122053,
0.));
#194759=CARTESIAN_POINT('Ctrl Pts',(-7.65561647852555,-23.0266320345792,
0.));
#194760=CARTESIAN_POINT('Ctrl Pts',(-7.6568765189133,-23.004069228582,0.));
#194761=CARTESIAN_POINT('Ctrl Pts',(-7.65807436436453,-22.9815973845301,
0.));
#194762=CARTESIAN_POINT('Ctrl Pts',(-7.65921032958912,-22.9592171890332,
0.));
#194763=CARTESIAN_POINT('Ctrl Pts',(-7.66028473382777,-22.9369293349592,
0.));
#194764=CARTESIAN_POINT('Ctrl Pts',(-7.661297900941,-22.9147345215418,0.));
#194765=CARTESIAN_POINT('Ctrl Pts',(-7.66225015950148,-22.8926334544879,
0.));
#194766=CARTESIAN_POINT('Ctrl Pts',(-7.66314184287334,-22.870626846128,
0.));
#194767=CARTESIAN_POINT('Ctrl Pts',(-7.66397328929805,-22.8487154155569,
0.));
#194768=CARTESIAN_POINT('Ctrl Pts',(-7.66474484198553,-22.8268998887678,
0.));
#194769=CARTESIAN_POINT('Ctrl Pts',(-7.66545684920988,-22.8051809987833,
0.));
#194770=CARTESIAN_POINT('Ctrl Pts',(-7.66610966441259,-22.7835594857697,
0.));
#194771=CARTESIAN_POINT('Ctrl Pts',(-7.66670364630273,-22.7620360971839,
0.));
#194772=CARTESIAN_POINT('Ctrl Pts',(-7.66723915895413,-22.7406115879508,
0.));
#194773=CARTESIAN_POINT('Ctrl Pts',(-7.6677165719101,-22.7192867206242,
0.));
#194774=CARTESIAN_POINT('Ctrl Pts',(-7.66813626029277,-22.6980622655446,
0.));
#194775=CARTESIAN_POINT('Ctrl Pts',(-7.66849860491763,-22.6769390009889,
0.));
#194776=CARTESIAN_POINT('Ctrl Pts',(-7.66880399241354,-22.6559177133133,
0.));
#194777=CARTESIAN_POINT('Ctrl Pts',(-7.66905281533745,-22.6349991971547,
0.));
#194778=CARTESIAN_POINT('Ctrl Pts',(-7.66924547229435,-22.6141842556248,
0.));
#194779=CARTESIAN_POINT('Ctrl Pts',(-7.66938236806241,-22.5934737004955,
0.));
#194780=CARTESIAN_POINT('Ctrl Pts',(-7.66946391372299,-22.5728683523828,
0.));
#194781=CARTESIAN_POINT('Ctrl Pts',(-7.66949052679672,-22.5523690409109,
0.));
#194782=CARTESIAN_POINT('Ctrl Pts',(-7.66946263138116,-22.5319766049191,
0.));
#194783=CARTESIAN_POINT('Ctrl Pts',(-7.66938065829083,-22.5116918927023,
0.));
#194784=CARTESIAN_POINT('Ctrl Pts',(-7.66924504520302,-22.4915157622308,
0.));
#194785=CARTESIAN_POINT('Ctrl Pts',(-7.66905623680836,-22.47144908137,0.));
#194786=CARTESIAN_POINT('Ctrl Pts',(-7.6688146849666,-22.4514927280862,
0.));
#194787=CARTESIAN_POINT('Ctrl Pts',(-7.66852084886746,-22.4316475906616,
0.));
#194788=CARTESIAN_POINT('Ctrl Pts',(-7.66817519519682,-22.411914567977,
0.));
#194789=CARTESIAN_POINT('Ctrl Pts',(-7.6677781983082,-22.3922945697782,
0.));
#194790=CARTESIAN_POINT('Ctrl Pts',(-7.66733034039887,-22.3727885169361,
0.));
#194791=CARTESIAN_POINT('Ctrl Pts',(-7.66683211169134,-22.3533973417013,
0.));
#194792=CARTESIAN_POINT('Ctrl Pts',(-7.66628401061906,-22.3341219879454,
0.));
#194793=CARTESIAN_POINT('Ctrl Pts',(-7.66568654402442,-22.3149634114823,
0.));
#194794=CARTESIAN_POINT('Ctrl Pts',(-7.66504022736263,-22.2959225803925,
0.));
#194795=CARTESIAN_POINT('Ctrl Pts',(-7.66434558490973,-22.2770004753332,
0.));
#194796=CARTESIAN_POINT('Ctrl Pts',(-7.66360314997662,-22.2581980898487,
0.));
#194797=CARTESIAN_POINT('Ctrl Pts',(-7.66281346512546,-22.239516430656,
0.));
#194798=CARTESIAN_POINT('Ctrl Pts',(-7.66197708240436,-22.2209565180098,
0.));
#194799=CARTESIAN_POINT('Ctrl Pts',(-7.66109456359292,-22.2025193860972,
0.));
#194800=CARTESIAN_POINT('Ctrl Pts',(-7.66016648045008,-22.1842060834092,
0.));
#194801=CARTESIAN_POINT('Ctrl Pts',(-7.65919341496926,-22.1660176731174,
0.));
#194802=CARTESIAN_POINT('Ctrl Pts',(-7.65817595963351,-22.1479552334206,
0.));
#194803=CARTESIAN_POINT('Ctrl Pts',(-7.65711471769407,-22.1300198579671,
0.));
#194804=CARTESIAN_POINT('Ctrl Pts',(-7.65601030346819,-22.1122126563327,
0.));
#194805=CARTESIAN_POINT('Ctrl Pts',(-7.65486334263651,-22.094534754469,
0.));
#194806=CARTESIAN_POINT('Ctrl Pts',(-7.65367447254945,-22.0769872951596,
0.));
#194807=CARTESIAN_POINT('Ctrl Pts',(-7.65244434253104,-22.0595714384432,
0.));
#194808=CARTESIAN_POINT('Ctrl Pts',(-7.65117361421347,-22.0422883621176,
0.));
#194809=CARTESIAN_POINT('Ctrl Pts',(-7.64986296190157,-22.0251392623209,
0.));
#194810=CARTESIAN_POINT('Ctrl Pts',(-7.64851307293346,-22.0081253540773,
0.));
#194811=CARTESIAN_POINT('Ctrl Pts',(-7.64712464805258,-21.9912478718542,
0.));
#194812=CARTESIAN_POINT('Ctrl Pts',(-7.64569840177359,-21.97450807008,0.));
#194813=CARTESIAN_POINT('Ctrl Pts',(-7.64423506279154,-21.9579072237653,
0.));
#194814=CARTESIAN_POINT('Ctrl Pts',(-7.64273537442707,-21.9414466292074,
0.));
#194815=CARTESIAN_POINT('Ctrl Pts',(-7.6412000950654,-21.9251276046546,
0.));
#194816=CARTESIAN_POINT('Ctrl Pts',(-7.63962999860917,-21.9089514909873,
0.));
#194817=CARTESIAN_POINT('Ctrl Pts',(-7.63802587492008,-21.8929196523511,
0.));
#194818=CARTESIAN_POINT('Ctrl Pts',(-7.63638853033368,-21.8770334769492,
0.));
#194819=CARTESIAN_POINT('Ctrl Pts',(-7.63471878821204,-21.8612943779086,
0.));
#194820=CARTESIAN_POINT('Ctrl Pts',(-7.63301748948936,-21.8457037941084,
0.));
#194821=CARTESIAN_POINT('Ctrl Pts',(-7.6312854932304,-21.8302631910197,
0.));
#194822=CARTESIAN_POINT('Ctrl Pts',(-7.62952367718151,-21.8149740615093,
0.));
#194823=CARTESIAN_POINT('Ctrl Pts',(-7.62773293842409,-21.7998379268583,
0.));
#194824=CARTESIAN_POINT('Ctrl Pts',(-7.62591419404521,-21.7848563378022,
0.));
#194825=CARTESIAN_POINT('Ctrl Pts',(-7.62406838181164,-21.7700308755583,
0.));
#194826=CARTESIAN_POINT('Ctrl Pts',(-7.62219646084226,-21.7553631528329,
0.));
#194827=CARTESIAN_POINT('Ctrl Pts',(-7.62029941230855,-21.7408548148657,
0.));
#194828=CARTESIAN_POINT('Ctrl Pts',(-7.61837824030542,-21.7265075407977,
0.));
#194829=CARTESIAN_POINT('Ctrl Pts',(-7.61643397270425,-21.7123230449835,
0.));
#194830=CARTESIAN_POINT('Ctrl Pts',(-7.61446766202787,-21.6983030783321,
0.));
#194831=CARTESIAN_POINT('Ctrl Pts',(-7.61248038630265,-21.6844494295813,
0.));
#194832=CARTESIAN_POINT('Ctrl Pts',(-7.6104732500095,-21.6707639267573,
0.));
#194833=CARTESIAN_POINT('Ctrl Pts',(-7.60844738512872,-21.6572484388079,
0.));
#194834=CARTESIAN_POINT('Ctrl Pts',(-7.60640395216359,-21.6439048771743,
0.));
#194835=CARTESIAN_POINT('Ctrl Pts',(-7.604344141183,-21.6307351973823,0.));
#194836=CARTESIAN_POINT('Ctrl Pts',(-7.60226917285432,-21.6177414005991,
0.));
#194837=CARTESIAN_POINT('Ctrl Pts',(-7.60018029988238,-21.6049255358842,
0.));
#194838=CARTESIAN_POINT('Ctrl Pts',(-7.59807880846193,-21.5922897024466,
0.));
#194839=CARTESIAN_POINT('Ctrl Pts',(-7.59596601973589,-21.5798360518978,
0.));
#194840=CARTESIAN_POINT('Ctrl Pts',(-7.5938432912493,-21.5675667904728,
0.));
#194841=CARTESIAN_POINT('Ctrl Pts',(-7.59171201844793,-21.5554841813465,
0.));
#194842=CARTESIAN_POINT('Ctrl Pts',(-7.58957363620026,-21.5435905470113,
0.));
#194843=CARTESIAN_POINT('Ctrl Pts',(-7.58742962034834,-21.5318882716735,
0.));
#194844=CARTESIAN_POINT('Ctrl Pts',(-7.58528148919114,-21.5203798035294,
0.));
#194845=CARTESIAN_POINT('Ctrl Pts',(-7.58313080519159,-21.5090676573866,
0.));
#194846=CARTESIAN_POINT('Ctrl Pts',(-7.5809791779073,-21.4979544192739,
0.));
#194847=CARTESIAN_POINT('Ctrl Pts',(-7.57882826679131,-21.4870427508193,
0.));
#194848=CARTESIAN_POINT('Ctrl Pts',(-7.57667978403003,-21.4763353936766,
0.));
#194849=CARTESIAN_POINT('Ctrl Pts',(-7.57453549743435,-21.4658351740135,
0.));
#194850=CARTESIAN_POINT('Ctrl Pts',(-7.57239723223521,-21.4555450053147,
0.));
#194851=CARTESIAN_POINT('Ctrl Pts',(-7.5702668726117,-21.445467890751,0.));
#194852=CARTESIAN_POINT('Ctrl Pts',(-7.56814636360842,-21.435606926151,
0.));
#194853=CARTESIAN_POINT('Ctrl Pts',(-7.56603771218706,-21.4259653015732,
0.));
#194854=CARTESIAN_POINT('Ctrl Pts',(-7.56394299313683,-21.4165463106252,
0.));
#194855=CARTESIAN_POINT('Ctrl Pts',(-7.56186435703622,-21.4073533630364,
0.));
#194856=CARTESIAN_POINT('Ctrl Pts',(-7.55980403700615,-21.3983899952988,
0.));
#194857=CARTESIAN_POINT('Ctrl Pts',(-7.55776435731422,-21.3896598842119,
0.));
#194858=CARTESIAN_POINT('Ctrl Pts',(-7.55574773403508,-21.3811668478933,
0.));
#194859=CARTESIAN_POINT('Ctrl Pts',(-7.55375667080032,-21.3729148390244,
0.));
#194860=CARTESIAN_POINT('Ctrl Pts',(-7.55179375777442,-21.3649079431864,
0.));
#194861=CARTESIAN_POINT('Ctrl Pts',(-7.54986166521307,-21.3571503685853,
0.));
#194862=CARTESIAN_POINT('Ctrl Pts',(-7.54796316246327,-21.349646476153,
0.));
#194863=CARTESIAN_POINT('Ctrl Pts',(-7.54610114948351,-21.3424008295038,
0.));
#194864=CARTESIAN_POINT('Ctrl Pts',(-7.54427868151269,-21.3354182340149,
0.));
#194865=CARTESIAN_POINT('Ctrl Pts',(-7.54249900377032,-21.328703791771,
0.));
#194866=CARTESIAN_POINT('Ctrl Pts',(-7.5407655203828,-21.3222628524165,
0.));
#194867=CARTESIAN_POINT('Ctrl Pts',(-7.53908175169899,-21.3161009456256,
0.));
#194868=CARTESIAN_POINT('Ctrl Pts',(-7.5374512936462,-21.3102237167729,
0.));
#194869=CARTESIAN_POINT('Ctrl Pts',(-7.53587778251743,-21.3046368712156,
0.));
#194870=CARTESIAN_POINT('Ctrl Pts',(-7.53436505309949,-21.2993464250717,
0.));
#194871=CARTESIAN_POINT('Ctrl Pts',(-7.53291726078527,-21.2943588989331,
0.));
#194872=CARTESIAN_POINT('Ctrl Pts',(-7.53153906987847,-21.2896816163843,
0.));
#194873=CARTESIAN_POINT('Ctrl Pts',(-7.53023562438221,-21.2853226580658,
0.));
#194874=CARTESIAN_POINT('Ctrl Pts',(-7.52901217930407,-21.2812902781143,
0.));
#194875=CARTESIAN_POINT('Ctrl Pts',(-7.52787386225344,-21.2775925269651,
0.));
#194876=CARTESIAN_POINT('Ctrl Pts',(-7.52682526918561,-21.2742366113578,
0.));
#194877=CARTESIAN_POINT('Ctrl Pts',(-7.52587126095544,-21.2712301573465,
0.));
#194878=CARTESIAN_POINT('Ctrl Pts',(-7.52501770333522,-21.2685823838672,
0.));
#194879=CARTESIAN_POINT('Ctrl Pts',(-7.52427261074264,-21.266305915706,
0.));
#194880=CARTESIAN_POINT('Ctrl Pts',(-7.52364573027521,-21.2644161259965,
0.));
#194881=CARTESIAN_POINT('Ctrl Pts',(-7.52314642316203,-21.262927782038,
0.));
#194882=CARTESIAN_POINT('Ctrl Pts',(-7.52278182242728,-21.261852128355,
0.));
#194883=CARTESIAN_POINT('Ctrl Pts',(-7.52260064231736,-21.2613260540651,
0.));
#194884=CARTESIAN_POINT('Ctrl Pts',(-7.52252744144958,-21.261120447486,
0.));
#194885=CARTESIAN_POINT('Ctrl Pts',(-7.52250649703992,-21.2610673466883,
0.));
#194886=CARTESIAN_POINT('Ctrl Pts',(-7.52250298901266,-21.2610617890679,
0.));
#194887=CARTESIAN_POINT('',(-7.36589684767345,-24.9347862158358,0.));
#194888=CARTESIAN_POINT('Ctrl Pts',(-9.71462809124917,-20.353053841303,
0.));
#194889=CARTESIAN_POINT('Ctrl Pts',(-9.71462809124917,-20.353053841303,
12.));
#194890=CARTESIAN_POINT('Ctrl Pts',(-9.71462954053074,-20.353060251684,
0.));
#194891=CARTESIAN_POINT('Ctrl Pts',(-9.71462954053074,-20.353060251684,
12.));
#194892=CARTESIAN_POINT('Ctrl Pts',(-9.71465227853122,-20.3531126095522,
0.));
#194893=CARTESIAN_POINT('Ctrl Pts',(-9.71465227853122,-20.3531126095522,
12.));
#194894=CARTESIAN_POINT('Ctrl Pts',(-9.71474590350792,-20.3533097561886,
0.));
#194895=CARTESIAN_POINT('Ctrl Pts',(-9.71474590350792,-20.3533097561886,
12.));
#194896=CARTESIAN_POINT('Ctrl Pts',(-9.71498978052101,-20.3538098605706,
0.));
#194897=CARTESIAN_POINT('Ctrl Pts',(-9.71498978052101,-20.3538098605706,
12.));
#194898=CARTESIAN_POINT('Ctrl Pts',(-9.71549257088175,-20.3548282742361,
0.));
#194899=CARTESIAN_POINT('Ctrl Pts',(-9.71549257088175,-20.3548282742361,
12.));
#194900=CARTESIAN_POINT('Ctrl Pts',(-9.71619192554147,-20.3562337557875,
0.));
#194901=CARTESIAN_POINT('Ctrl Pts',(-9.71619192554147,-20.3562337557875,
12.));
#194902=CARTESIAN_POINT('Ctrl Pts',(-9.71708493723062,-20.3580133103357,
0.));
#194903=CARTESIAN_POINT('Ctrl Pts',(-9.71708493723062,-20.3580133103357,
12.));
#194904=CARTESIAN_POINT('Ctrl Pts',(-9.71816778327999,-20.3601498764344,
0.));
#194905=CARTESIAN_POINT('Ctrl Pts',(-9.71816778327999,-20.3601498764344,
12.));
#194906=CARTESIAN_POINT('Ctrl Pts',(-9.71943648548115,-20.362625691398,
0.));
#194907=CARTESIAN_POINT('Ctrl Pts',(-9.71943648548115,-20.362625691398,
12.));
#194908=CARTESIAN_POINT('Ctrl Pts',(-9.72088778381102,-20.3654261611055,
0.));
#194909=CARTESIAN_POINT('Ctrl Pts',(-9.72088778381102,-20.3654261611055,
12.));
#194910=CARTESIAN_POINT('Ctrl Pts',(-9.72251930722504,-20.3685406190576,
0.));
#194911=CARTESIAN_POINT('Ctrl Pts',(-9.72251930722504,-20.3685406190576,
12.));
#194912=CARTESIAN_POINT('Ctrl Pts',(-9.72432910043193,-20.371960235676,
0.));
#194913=CARTESIAN_POINT('Ctrl Pts',(-9.72432910043193,-20.371960235676,
12.));
#194914=CARTESIAN_POINT('Ctrl Pts',(-9.72631531732871,-20.3756766651952,
0.));
#194915=CARTESIAN_POINT('Ctrl Pts',(-9.72631531732871,-20.3756766651952,
12.));
#194916=CARTESIAN_POINT('Ctrl Pts',(-9.72847589116533,-20.3796805893304,
0.));
#194917=CARTESIAN_POINT('Ctrl Pts',(-9.72847589116533,-20.3796805893304,
12.));
#194918=CARTESIAN_POINT('Ctrl Pts',(-9.73080870123726,-20.3839624556742,
0.));
#194919=CARTESIAN_POINT('Ctrl Pts',(-9.73080870123726,-20.3839624556742,
12.));
#194920=CARTESIAN_POINT('Ctrl Pts',(-9.73331167102812,-20.3885129129912,
0.));
#194921=CARTESIAN_POINT('Ctrl Pts',(-9.73331167102812,-20.3885129129912,
12.));
#194922=CARTESIAN_POINT('Ctrl Pts',(-9.7359829201425,-20.3933234845646,
0.));
#194923=CARTESIAN_POINT('Ctrl Pts',(-9.7359829201425,-20.3933234845646,
12.));
#194924=CARTESIAN_POINT('Ctrl Pts',(-9.73882077613206,-20.3983866213331,
0.));
#194925=CARTESIAN_POINT('Ctrl Pts',(-9.73882077613206,-20.3983866213331,
12.));
#194926=CARTESIAN_POINT('Ctrl Pts',(-9.74182369656273,-20.4036953576549,
0.));
#194927=CARTESIAN_POINT('Ctrl Pts',(-9.74182369656273,-20.4036953576549,
12.));
#194928=CARTESIAN_POINT('Ctrl Pts',(-9.74499021838537,-20.4092430879861,
0.));
#194929=CARTESIAN_POINT('Ctrl Pts',(-9.74499021838537,-20.4092430879861,
12.));
#194930=CARTESIAN_POINT('Ctrl Pts',(-9.74831889242175,-20.4150232777393,
0.));
#194931=CARTESIAN_POINT('Ctrl Pts',(-9.74831889242175,-20.4150232777393,
12.));
#194932=CARTESIAN_POINT('Ctrl Pts',(-9.75180829786433,-20.4210295275818,
0.));
#194933=CARTESIAN_POINT('Ctrl Pts',(-9.75180829786433,-20.4210295275818,
12.));
#194934=CARTESIAN_POINT('Ctrl Pts',(-9.75545705902416,-20.4272556476629,
0.));
#194935=CARTESIAN_POINT('Ctrl Pts',(-9.75545705902416,-20.4272556476629,
12.));
#194936=CARTESIAN_POINT('Ctrl Pts',(-9.7592638628993,-20.4336957355474,
0.));
#194937=CARTESIAN_POINT('Ctrl Pts',(-9.7592638628993,-20.4336957355474,
12.));
#194938=CARTESIAN_POINT('Ctrl Pts',(-9.76322747195502,-20.4403442329401,
0.));
#194939=CARTESIAN_POINT('Ctrl Pts',(-9.76322747195502,-20.4403442329401,
12.));
#194940=CARTESIAN_POINT('Ctrl Pts',(-9.76734670980897,-20.447195862298,
0.));
#194941=CARTESIAN_POINT('Ctrl Pts',(-9.76734670980897,-20.447195862298,
12.));
#194942=CARTESIAN_POINT('Ctrl Pts',(-9.7716204510407,-20.4542455817527,
0.));
#194943=CARTESIAN_POINT('Ctrl Pts',(-9.7716204510407,-20.4542455817527,
12.));
#194944=CARTESIAN_POINT('Ctrl Pts',(-9.77604760815523,-20.4614885274973,
0.));
#194945=CARTESIAN_POINT('Ctrl Pts',(-9.77604760815523,-20.4614885274973,
12.));
#194946=CARTESIAN_POINT('Ctrl Pts',(-9.78062712373313,-20.4689199790668,
0.));
#194947=CARTESIAN_POINT('Ctrl Pts',(-9.78062712373313,-20.4689199790668,
12.));
#194948=CARTESIAN_POINT('Ctrl Pts',(-9.78535797314162,-20.4765353711585,
0.));
#194949=CARTESIAN_POINT('Ctrl Pts',(-9.78535797314162,-20.4765353711585,
12.));
#194950=CARTESIAN_POINT('Ctrl Pts',(-9.7902391649866,-20.4843302955329,
0.));
#194951=CARTESIAN_POINT('Ctrl Pts',(-9.7902391649866,-20.4843302955329,
12.));
#194952=CARTESIAN_POINT('Ctrl Pts',(-9.79526974288344,-20.4923005087945,
0.));
#194953=CARTESIAN_POINT('Ctrl Pts',(-9.79526974288344,-20.4923005087945,
12.));
#194954=CARTESIAN_POINT('Ctrl Pts',(-9.80044878520968,-20.500441931211,
0.));
#194955=CARTESIAN_POINT('Ctrl Pts',(-9.80044878520968,-20.500441931211,
12.));
#194956=CARTESIAN_POINT('Ctrl Pts',(-9.80577540161103,-20.5087506310507,
0.));
#194957=CARTESIAN_POINT('Ctrl Pts',(-9.80577540161103,-20.5087506310507,
12.));
#194958=CARTESIAN_POINT('Ctrl Pts',(-9.81124873025278,-20.5172228122839,
0.));
#194959=CARTESIAN_POINT('Ctrl Pts',(-9.81124873025278,-20.5172228122839,
12.));
#194960=CARTESIAN_POINT('Ctrl Pts',(-9.81686793455918,-20.5258548000625,
0.));
#194961=CARTESIAN_POINT('Ctrl Pts',(-9.81686793455918,-20.5258548000625,
12.));
#194962=CARTESIAN_POINT('Ctrl Pts',(-9.82263220080328,-20.534643029951,
0.));
#194963=CARTESIAN_POINT('Ctrl Pts',(-9.82263220080328,-20.534643029951,
12.));
#194964=CARTESIAN_POINT('Ctrl Pts',(-9.82854073773858,-20.5435840460717,
0.));
#194965=CARTESIAN_POINT('Ctrl Pts',(-9.82854073773858,-20.5435840460717,
12.));
#194966=CARTESIAN_POINT('Ctrl Pts',(-9.83459277585321,-20.5526744976461,
0.));
#194967=CARTESIAN_POINT('Ctrl Pts',(-9.83459277585321,-20.5526744976461,
12.));
#194968=CARTESIAN_POINT('Ctrl Pts',(-9.84078756677589,-20.5619111362406,
0.));
#194969=CARTESIAN_POINT('Ctrl Pts',(-9.84078756677589,-20.5619111362406,
12.));
#194970=CARTESIAN_POINT('Ctrl Pts',(-9.84712438256308,-20.5712908125145,
0.));
#194971=CARTESIAN_POINT('Ctrl Pts',(-9.84712438256308,-20.5712908125145,
12.));
#194972=CARTESIAN_POINT('Ctrl Pts',(-9.85360251457004,-20.580810471002,
0.));
#194973=CARTESIAN_POINT('Ctrl Pts',(-9.85360251457004,-20.580810471002,
12.));
#194974=CARTESIAN_POINT('Ctrl Pts',(-9.8602212723275,-20.5904671449754,
0.));
#194975=CARTESIAN_POINT('Ctrl Pts',(-9.8602212723275,-20.5904671449754,
12.));
#194976=CARTESIAN_POINT('Ctrl Pts',(-9.86697998242612,-20.6002579513696,
0.));
#194977=CARTESIAN_POINT('Ctrl Pts',(-9.86697998242612,-20.6002579513696,
12.));
#194978=CARTESIAN_POINT('Ctrl Pts',(-9.87387798732944,-20.6101800854491,
0.));
#194979=CARTESIAN_POINT('Ctrl Pts',(-9.87387798732944,-20.6101800854491,
12.));
#194980=CARTESIAN_POINT('Ctrl Pts',(-9.88091464472669,-20.6202308177472,
0.));
#194981=CARTESIAN_POINT('Ctrl Pts',(-9.88091464472669,-20.6202308177472,
12.));
#194982=CARTESIAN_POINT('Ctrl Pts',(-9.88808932697305,-20.6304074914086,
0.));
#194983=CARTESIAN_POINT('Ctrl Pts',(-9.88808932697305,-20.6304074914086,
12.));
#194984=CARTESIAN_POINT('Ctrl Pts',(-9.89540142049124,-20.6407075193977,
0.));
#194985=CARTESIAN_POINT('Ctrl Pts',(-9.89540142049124,-20.6407075193977,
12.));
#194986=CARTESIAN_POINT('Ctrl Pts',(-9.90285032516696,-20.6511283817415,
0.));
#194987=CARTESIAN_POINT('Ctrl Pts',(-9.90285032516696,-20.6511283817415,
12.));
#194988=CARTESIAN_POINT('Ctrl Pts',(-9.91043545377005,-20.6616676228315,
0.));
#194989=CARTESIAN_POINT('Ctrl Pts',(-9.91043545377005,-20.6616676228315,
12.));
#194990=CARTESIAN_POINT('Ctrl Pts',(-9.91815623141285,-20.6723228488261,
0.));
#194991=CARTESIAN_POINT('Ctrl Pts',(-9.91815623141285,-20.6723228488261,
12.));
#194992=CARTESIAN_POINT('Ctrl Pts',(-9.92601209498751,-20.6830917250255,
0.));
#194993=CARTESIAN_POINT('Ctrl Pts',(-9.92601209498751,-20.6830917250255,
12.));
#194994=CARTESIAN_POINT('Ctrl Pts',(-9.93400249259737,-20.6939719732485,
0.));
#194995=CARTESIAN_POINT('Ctrl Pts',(-9.93400249259737,-20.6939719732485,
12.));
#194996=CARTESIAN_POINT('Ctrl Pts',(-9.94212688298251,-20.7049613692237,
0.));
#194997=CARTESIAN_POINT('Ctrl Pts',(-9.94212688298251,-20.7049613692237,
12.));
#194998=CARTESIAN_POINT('Ctrl Pts',(-9.95038473514962,-20.716057740758,
0.));
#194999=CARTESIAN_POINT('Ctrl Pts',(-9.95038473514962,-20.716057740758,
12.));
#195000=CARTESIAN_POINT('Ctrl Pts',(-9.95877552798403,-20.7272589658752,
0.));
#195001=CARTESIAN_POINT('Ctrl Pts',(-9.95877552798403,-20.7272589658752,
12.));
#195002=CARTESIAN_POINT('Ctrl Pts',(-9.96729874986199,-20.7385629709795,
0.));
#195003=CARTESIAN_POINT('Ctrl Pts',(-9.96729874986199,-20.7385629709795,
12.));
#195004=CARTESIAN_POINT('Ctrl Pts',(-9.97595389823461,-20.7499677289625,
0.));
#195005=CARTESIAN_POINT('Ctrl Pts',(-9.97595389823461,-20.7499677289625,
12.));
#195006=CARTESIAN_POINT('Ctrl Pts',(-9.98474047926846,-20.7614712574989,
0.));
#195007=CARTESIAN_POINT('Ctrl Pts',(-9.98474047926846,-20.7614712574989,
12.));
#195008=CARTESIAN_POINT('Ctrl Pts',(-9.99365800754638,-20.7730716175417,
0.));
#195009=CARTESIAN_POINT('Ctrl Pts',(-9.99365800754638,-20.7730716175417,
12.));
#195010=CARTESIAN_POINT('Ctrl Pts',(-10.0027060057389,-20.7847669117568,
0.));
#195011=CARTESIAN_POINT('Ctrl Pts',(-10.0027060057389,-20.7847669117568,
12.));
#195012=CARTESIAN_POINT('Ctrl Pts',(-10.0118840042786,-20.7965552829907,
0.));
#195013=CARTESIAN_POINT('Ctrl Pts',(-10.0118840042786,-20.7965552829907,
12.));
#195014=CARTESIAN_POINT('Ctrl Pts',(-10.0211915410095,-20.8084349126885,
0.));
#195015=CARTESIAN_POINT('Ctrl Pts',(-10.0211915410095,-20.8084349126885,
12.));
#195016=CARTESIAN_POINT('Ctrl Pts',(-10.0306281609435,-20.8204040196599,
0.));
#195017=CARTESIAN_POINT('Ctrl Pts',(-10.0306281609435,-20.8204040196599,
12.));
#195018=CARTESIAN_POINT('Ctrl Pts',(-10.0401934160234,-20.8324608588906,
0.));
#195019=CARTESIAN_POINT('Ctrl Pts',(-10.0401934160234,-20.8324608588906,
12.));
#195020=CARTESIAN_POINT('Ctrl Pts',(-10.0498868648733,-20.8446037203402,
0.));
#195021=CARTESIAN_POINT('Ctrl Pts',(-10.0498868648733,-20.8446037203402,
12.));
#195022=CARTESIAN_POINT('Ctrl Pts',(-10.0597080725375,-20.856830927732,
0.));
#195023=CARTESIAN_POINT('Ctrl Pts',(-10.0597080725375,-20.856830927732,
12.));
#195024=CARTESIAN_POINT('Ctrl Pts',(-10.0696566102219,-20.8691408373705,
0.));
#195025=CARTESIAN_POINT('Ctrl Pts',(-10.0696566102219,-20.8691408373705,
12.));
#195026=CARTESIAN_POINT('Ctrl Pts',(-10.0797320551154,-20.8815318371844,
0.));
#195027=CARTESIAN_POINT('Ctrl Pts',(-10.0797320551154,-20.8815318371844,
12.));
#195028=CARTESIAN_POINT('Ctrl Pts',(-10.0899339901916,-20.8940023457371,
0.));
#195029=CARTESIAN_POINT('Ctrl Pts',(-10.0899339901916,-20.8940023457371,
12.));
#195030=CARTESIAN_POINT('Ctrl Pts',(-10.1002620040076,-20.9065508112556,
0.));
#195031=CARTESIAN_POINT('Ctrl Pts',(-10.1002620040076,-20.9065508112556,
12.));
#195032=CARTESIAN_POINT('Ctrl Pts',(-10.1107156904836,-20.9191757106266,
0.));
#195033=CARTESIAN_POINT('Ctrl Pts',(-10.1107156904836,-20.9191757106266,
12.));
#195034=CARTESIAN_POINT('Ctrl Pts',(-10.1212946487057,-20.931875548473,
0.));
#195035=CARTESIAN_POINT('Ctrl Pts',(-10.1212946487057,-20.931875548473,
12.));
#195036=CARTESIAN_POINT('Ctrl Pts',(-10.1319984827909,-20.944648856393,
0.));
#195037=CARTESIAN_POINT('Ctrl Pts',(-10.1319984827909,-20.944648856393,
12.));
#195038=CARTESIAN_POINT('Ctrl Pts',(-10.1428268017257,-20.9574941921591,
0.));
#195039=CARTESIAN_POINT('Ctrl Pts',(-10.1428268017257,-20.9574941921591,
12.));
#195040=CARTESIAN_POINT('Ctrl Pts',(-10.1537792192065,-20.970410138937,
0.));
#195041=CARTESIAN_POINT('Ctrl Pts',(-10.1537792192065,-20.970410138937,
12.));
#195042=CARTESIAN_POINT('Ctrl Pts',(-10.1648553534567,-20.9833953044736,
0.));
#195043=CARTESIAN_POINT('Ctrl Pts',(-10.1648553534567,-20.9833953044736,
12.));
#195044=CARTESIAN_POINT('Ctrl Pts',(-10.1760548270765,-20.9964483203685,
0.));
#195045=CARTESIAN_POINT('Ctrl Pts',(-10.1760548270765,-20.9964483203685,
12.));
#195046=CARTESIAN_POINT('Ctrl Pts',(-10.1873772669358,-21.0095678414486,
0.));
#195047=CARTESIAN_POINT('Ctrl Pts',(-10.1873772669358,-21.0095678414486,
12.));
#195048=CARTESIAN_POINT('Ctrl Pts',(-10.1988223040425,-21.0227525451107,
0.));
#195049=CARTESIAN_POINT('Ctrl Pts',(-10.1988223040425,-21.0227525451107,
12.));
#195050=CARTESIAN_POINT('Ctrl Pts',(-10.2103895734124,-21.0360011306814,
0.));
#195051=CARTESIAN_POINT('Ctrl Pts',(-10.2103895734124,-21.0360011306814,
12.));
#195052=CARTESIAN_POINT('Ctrl Pts',(-10.2220787139157,-21.0493123187483,
0.));
#195053=CARTESIAN_POINT('Ctrl Pts',(-10.2220787139157,-21.0493123187483,
12.));
#195054=CARTESIAN_POINT('Ctrl Pts',(-10.233889368157,-21.0626848505665,
0.));
#195055=CARTESIAN_POINT('Ctrl Pts',(-10.233889368157,-21.0626848505665,
12.));
#195056=CARTESIAN_POINT('Ctrl Pts',(-10.2458211823915,-21.0761174875448,
0.));
#195057=CARTESIAN_POINT('Ctrl Pts',(-10.2458211823915,-21.0761174875448,
12.));
#195058=CARTESIAN_POINT('Ctrl Pts',(-10.2578738064183,-21.0896090107066,
0.));
#195059=CARTESIAN_POINT('Ctrl Pts',(-10.2578738064183,-21.0896090107066,
12.));
#195060=CARTESIAN_POINT('Ctrl Pts',(-10.2700468934743,-21.1031582201625,
0.));
#195061=CARTESIAN_POINT('Ctrl Pts',(-10.2700468934743,-21.1031582201625,
12.));
#195062=CARTESIAN_POINT('Ctrl Pts',(-10.2823401001067,-21.1167639345623,
0.));
#195063=CARTESIAN_POINT('Ctrl Pts',(-10.2823401001067,-21.1167639345623,
12.));
#195064=CARTESIAN_POINT('Ctrl Pts',(-10.2947530860714,-21.130424990599,
0.));
#195065=CARTESIAN_POINT('Ctrl Pts',(-10.2947530860714,-21.130424990599,
12.));
#195066=CARTESIAN_POINT('Ctrl Pts',(-10.307285514268,-21.1441402425831,
0.));
#195067=CARTESIAN_POINT('Ctrl Pts',(-10.307285514268,-21.1441402425831,
12.));
#195068=CARTESIAN_POINT('Ctrl Pts',(-10.3199370506541,-21.1579085619959,
0.));
#195069=CARTESIAN_POINT('Ctrl Pts',(-10.3199370506541,-21.1579085619959,
12.));
#195070=CARTESIAN_POINT('Ctrl Pts',(-10.3327073641574,-21.1717288370512,
0.));
#195071=CARTESIAN_POINT('Ctrl Pts',(-10.3327073641574,-21.1717288370512,
12.));
#195072=CARTESIAN_POINT('Ctrl Pts',(-10.3455961265706,-21.1855999722427,
0.));
#195073=CARTESIAN_POINT('Ctrl Pts',(-10.3455961265706,-21.1855999722427,
12.));
#195074=CARTESIAN_POINT('Ctrl Pts',(-10.3586030124595,-21.1995208879205,
0.));
#195075=CARTESIAN_POINT('Ctrl Pts',(-10.3586030124595,-21.1995208879205,
12.));
#195076=CARTESIAN_POINT('Ctrl Pts',(-10.3717276991137,-21.2134905199359,
0.));
#195077=CARTESIAN_POINT('Ctrl Pts',(-10.3717276991137,-21.2134905199359,
12.));
#195078=CARTESIAN_POINT('Ctrl Pts',(-10.384969866479,-21.2275078192708,
0.));
#195079=CARTESIAN_POINT('Ctrl Pts',(-10.384969866479,-21.2275078192708,
12.));
#195080=CARTESIAN_POINT('Ctrl Pts',(-10.3983291970846,-21.2415717516713,
0.));
#195081=CARTESIAN_POINT('Ctrl Pts',(-10.3983291970846,-21.2415717516713,
12.));
#195082=CARTESIAN_POINT('Ctrl Pts',(-10.4118053759584,-21.2556812972741,
0.));
#195083=CARTESIAN_POINT('Ctrl Pts',(-10.4118053759584,-21.2556812972741,
12.));
#195084=CARTESIAN_POINT('Ctrl Pts',(-10.4253980905394,-21.2698354502391,
0.));
#195085=CARTESIAN_POINT('Ctrl Pts',(-10.4253980905394,-21.2698354502391,
12.));
#195086=CARTESIAN_POINT('Ctrl Pts',(-10.4391070306385,-21.2840332184471,
0.));
#195087=CARTESIAN_POINT('Ctrl Pts',(-10.4391070306385,-21.2840332184471,
12.));
#195088=CARTESIAN_POINT('Ctrl Pts',(-10.452931888387,-21.2982736231924,
0.));
#195089=CARTESIAN_POINT('Ctrl Pts',(-10.452931888387,-21.2982736231924,
12.));
#195090=CARTESIAN_POINT('Ctrl Pts',(-10.4668723581768,-21.312555698873,
0.));
#195091=CARTESIAN_POINT('Ctrl Pts',(-10.4668723581768,-21.312555698873,
12.));
#195092=CARTESIAN_POINT('Ctrl Pts',(-10.4809281365933,-21.3268784926823,
0.));
#195093=CARTESIAN_POINT('Ctrl Pts',(-10.4809281365933,-21.3268784926823,
12.));
#195094=CARTESIAN_POINT('Ctrl Pts',(-10.4950989223341,-21.3412410642912,
0.));
#195095=CARTESIAN_POINT('Ctrl Pts',(-10.4950989223341,-21.3412410642912,
12.));
#195096=CARTESIAN_POINT('Ctrl Pts',(-10.509384416169,-21.3556424855822,
0.));
#195097=CARTESIAN_POINT('Ctrl Pts',(-10.509384416169,-21.3556424855822,
12.));
#195098=CARTESIAN_POINT('Ctrl Pts',(-10.523784320906,-21.3700818403942,
0.));
#195099=CARTESIAN_POINT('Ctrl Pts',(-10.523784320906,-21.3700818403942,
12.));
#195100=CARTESIAN_POINT('Ctrl Pts',(-10.5382983413422,-21.3845582242604,
0.));
#195101=CARTESIAN_POINT('Ctrl Pts',(-10.5382983413422,-21.3845582242604,
12.));
#195102=CARTESIAN_POINT('Ctrl Pts',(-10.5529261842107,-21.3990707441495,
0.));
#195103=CARTESIAN_POINT('Ctrl Pts',(-10.5529261842107,-21.3990707441495,
12.));
#195104=CARTESIAN_POINT('Ctrl Pts',(-10.5676675581106,-21.4136185181974,
0.));
#195105=CARTESIAN_POINT('Ctrl Pts',(-10.5676675581106,-21.4136185181974,
12.));
#195106=CARTESIAN_POINT('Ctrl Pts',(-10.582522173457,-21.4282006754624,
0.));
#195107=CARTESIAN_POINT('Ctrl Pts',(-10.582522173457,-21.4282006754624,
12.));
#195108=CARTESIAN_POINT('Ctrl Pts',(-10.597489742462,-21.4428163557137,
0.));
#195109=CARTESIAN_POINT('Ctrl Pts',(-10.597489742462,-21.4428163557137,
12.));
#195110=CARTESIAN_POINT('Ctrl Pts',(-10.612569979096,-21.4574647092093,
0.));
#195111=CARTESIAN_POINT('Ctrl Pts',(-10.612569979096,-21.4574647092093,
12.));
#195112=CARTESIAN_POINT('Ctrl Pts',(-10.6277625990457,-21.4721448964766,
0.));
#195113=CARTESIAN_POINT('Ctrl Pts',(-10.6277625990457,-21.4721448964766,
12.));
#195114=CARTESIAN_POINT('Ctrl Pts',(-10.6430673196609,-21.4868560880893,
0.));
#195115=CARTESIAN_POINT('Ctrl Pts',(-10.6430673196609,-21.4868560880893,
12.));
#195116=CARTESIAN_POINT('Ctrl Pts',(-10.6584838598941,-21.5015974644454,
0.));
#195117=CARTESIAN_POINT('Ctrl Pts',(-10.6584838598941,-21.5015974644454,
12.));
#195118=CARTESIAN_POINT('Ctrl Pts',(-10.6740119402835,-21.5163682155805,
0.));
#195119=CARTESIAN_POINT('Ctrl Pts',(-10.6740119402835,-21.5163682155805,
12.));
#195120=CARTESIAN_POINT('Ctrl Pts',(-10.689651282929,-21.531167540981,0.));
#195121=CARTESIAN_POINT('Ctrl Pts',(-10.689651282929,-21.531167540981,12.));
#195122=CARTESIAN_POINT('Ctrl Pts',(-10.7054016114571,-21.5459946493955,
0.));
#195123=CARTESIAN_POINT('Ctrl Pts',(-10.7054016114571,-21.5459946493955,
12.));
#195124=CARTESIAN_POINT('Ctrl Pts',(-10.7212626509816,-21.5608487586467,
0.));
#195125=CARTESIAN_POINT('Ctrl Pts',(-10.7212626509816,-21.5608487586467,
12.));
#195126=CARTESIAN_POINT('Ctrl Pts',(-10.7372341280468,-21.5757290954372,
0.));
#195127=CARTESIAN_POINT('Ctrl Pts',(-10.7372341280468,-21.5757290954372,
12.));
#195128=CARTESIAN_POINT('Ctrl Pts',(-10.7533157705943,-21.5906348951745,
0.));
#195129=CARTESIAN_POINT('Ctrl Pts',(-10.7533157705943,-21.5906348951745,
12.));
#195130=CARTESIAN_POINT('Ctrl Pts',(-10.7695073079554,-21.6055654018179,
0.));
#195131=CARTESIAN_POINT('Ctrl Pts',(-10.7695073079554,-21.6055654018179,
12.));
#195132=CARTESIAN_POINT('Ctrl Pts',(-10.7858084708262,-21.6205198677176,
0.));
#195133=CARTESIAN_POINT('Ctrl Pts',(-10.7858084708262,-21.6205198677176,
12.));
#195134=CARTESIAN_POINT('Ctrl Pts',(-10.802218991237,-21.6354975534557,
0.));
#195135=CARTESIAN_POINT('Ctrl Pts',(-10.802218991237,-21.6354975534557,
12.));
#195136=CARTESIAN_POINT('Ctrl Pts',(-10.8187386025135,-21.6504977276864,
0.));
#195137=CARTESIAN_POINT('Ctrl Pts',(-10.8187386025135,-21.6504977276864,
12.));
#195138=CARTESIAN_POINT('Ctrl Pts',(-10.835367039227,-21.6655196669727,
0.));
#195139=CARTESIAN_POINT('Ctrl Pts',(-10.835367039227,-21.6655196669727,
12.));
#195140=CARTESIAN_POINT('Ctrl Pts',(-10.8521040371832,-21.6805626556461,
0.));
#195141=CARTESIAN_POINT('Ctrl Pts',(-10.8521040371832,-21.6805626556461,
12.));
#195142=CARTESIAN_POINT('Ctrl Pts',(-10.8689493334093,-21.6956259856667,
0.));
#195143=CARTESIAN_POINT('Ctrl Pts',(-10.8689493334093,-21.6956259856667,
12.));
#195144=CARTESIAN_POINT('Ctrl Pts',(-10.8859026661292,-21.7107089564822,
0.));
#195145=CARTESIAN_POINT('Ctrl Pts',(-10.8859026661292,-21.7107089564822,
12.));
#195146=CARTESIAN_POINT('Ctrl Pts',(-10.9029637747341,-21.7258108748874,
0.));
#195147=CARTESIAN_POINT('Ctrl Pts',(-10.9029637747341,-21.7258108748874,
12.));
#195148=CARTESIAN_POINT('Ctrl Pts',(-10.9201323997386,-21.74093105488,0.));
#195149=CARTESIAN_POINT('Ctrl Pts',(-10.9201323997386,-21.74093105488,12.));
#195150=CARTESIAN_POINT('Ctrl Pts',(-10.9374082827446,-21.7560688175252,
0.));
#195151=CARTESIAN_POINT('Ctrl Pts',(-10.9374082827446,-21.7560688175252,
12.));
#195152=CARTESIAN_POINT('Ctrl Pts',(-10.9547911664457,-21.7712234908468,
0.));
#195153=CARTESIAN_POINT('Ctrl Pts',(-10.9547911664457,-21.7712234908468,
12.));
#195154=CARTESIAN_POINT('Ctrl Pts',(-10.9722807946157,-21.7863944097143,
0.));
#195155=CARTESIAN_POINT('Ctrl Pts',(-10.9722807946157,-21.7863944097143,
12.));
#195156=CARTESIAN_POINT('Ctrl Pts',(-10.9898769120913,-21.8015809157302,
0.));
#195157=CARTESIAN_POINT('Ctrl Pts',(-10.9898769120913,-21.8015809157302,
12.));
#195158=CARTESIAN_POINT('Ctrl Pts',(-11.0075792647477,-21.8167823571168,
0.));
#195159=CARTESIAN_POINT('Ctrl Pts',(-11.0075792647477,-21.8167823571168,
12.));
#195160=CARTESIAN_POINT('Ctrl Pts',(-11.0253875994598,-21.8319980886033,
0.));
#195161=CARTESIAN_POINT('Ctrl Pts',(-11.0253875994598,-21.8319980886033,
12.));
#195162=CARTESIAN_POINT('Ctrl Pts',(-11.0433016640808,-21.8472274713103,
0.));
#195163=CARTESIAN_POINT('Ctrl Pts',(-11.0433016640808,-21.8472274713103,
12.));
#195164=CARTESIAN_POINT('Ctrl Pts',(-11.0613212074364,-21.8624698726319,
0.));
#195165=CARTESIAN_POINT('Ctrl Pts',(-11.0613212074364,-21.8624698726319,
12.));
#195166=CARTESIAN_POINT('Ctrl Pts',(-11.0794459793058,-21.8777246661191,
0.));
#195167=CARTESIAN_POINT('Ctrl Pts',(-11.0794459793058,-21.8777246661191,
12.));
#195168=CARTESIAN_POINT('Ctrl Pts',(-11.0976757303944,-21.8929912313608,
0.));
#195169=CARTESIAN_POINT('Ctrl Pts',(-11.0976757303944,-21.8929912313608,
12.));
#195170=CARTESIAN_POINT('Ctrl Pts',(-11.1160102123024,-21.9082689538687,
0.));
#195171=CARTESIAN_POINT('Ctrl Pts',(-11.1160102123024,-21.9082689538687,
12.));
#195172=CARTESIAN_POINT('Ctrl Pts',(-11.134449177474,-21.9235572249518,
0.));
#195173=CARTESIAN_POINT('Ctrl Pts',(-11.134449177474,-21.9235572249518,
12.));
#195174=CARTESIAN_POINT('Ctrl Pts',(-11.1529923792002,-21.9388554416437,
0.));
#195175=CARTESIAN_POINT('Ctrl Pts',(-11.1529923792002,-21.9388554416437,
12.));
#195176=CARTESIAN_POINT('Ctrl Pts',(-11.1716395716375,-21.9541630066504,
0.));
#195177=CARTESIAN_POINT('Ctrl Pts',(-11.1716395716375,-21.9541630066504,
12.));
#195178=CARTESIAN_POINT('Ctrl Pts',(-11.190390509811,-21.9694793282913,
0.));
#195179=CARTESIAN_POINT('Ctrl Pts',(-11.190390509811,-21.9694793282913,
12.));
#195180=CARTESIAN_POINT('Ctrl Pts',(-11.2092449496125,-21.9848038204439,
0.));
#195181=CARTESIAN_POINT('Ctrl Pts',(-11.2092449496125,-21.9848038204439,
12.));
#195182=CARTESIAN_POINT('Ctrl Pts',(-11.2282026477897,-22.0001359024839,
0.));
#195183=CARTESIAN_POINT('Ctrl Pts',(-11.2282026477897,-22.0001359024839,
12.));
#195184=CARTESIAN_POINT('Ctrl Pts',(-11.2472633619276,-22.0154749992364,
0.));
#195185=CARTESIAN_POINT('Ctrl Pts',(-11.2472633619276,-22.0154749992364,
12.));
#195186=CARTESIAN_POINT('Ctrl Pts',(-11.2664268504207,-22.0308205408351,
0.));
#195187=CARTESIAN_POINT('Ctrl Pts',(-11.2664268504207,-22.0308205408351,
12.));
#195188=CARTESIAN_POINT('Ctrl Pts',(-11.2856928724374,-22.046171962566,
0.));
#195189=CARTESIAN_POINT('Ctrl Pts',(-11.2856928724374,-22.046171962566,
12.));
#195190=CARTESIAN_POINT('Ctrl Pts',(-11.3050611878771,-22.0615287047179,
0.));
#195191=CARTESIAN_POINT('Ctrl Pts',(-11.3050611878771,-22.0615287047179,
12.));
#195192=CARTESIAN_POINT('Ctrl Pts',(-11.3245315573168,-22.0768902124267,
0.));
#195193=CARTESIAN_POINT('Ctrl Pts',(-11.3245315573168,-22.0768902124267,
12.));
#195194=CARTESIAN_POINT('Ctrl Pts',(-11.3441037419553,-22.0922559355293,
0.));
#195195=CARTESIAN_POINT('Ctrl Pts',(-11.3441037419553,-22.0922559355293,
12.));
#195196=CARTESIAN_POINT('Ctrl Pts',(-11.3637775035367,-22.1076253283978,
0.));
#195197=CARTESIAN_POINT('Ctrl Pts',(-11.3637775035367,-22.1076253283978,
12.));
#195198=CARTESIAN_POINT('Ctrl Pts',(-11.3835526044256,-22.1229978500185,
0.));
#195199=CARTESIAN_POINT('Ctrl Pts',(-11.3835526044256,-22.1229978500185,
12.));
#195200=CARTESIAN_POINT('Ctrl Pts',(-11.4034288076909,-22.1383729640963,
0.));
#195201=CARTESIAN_POINT('Ctrl Pts',(-11.4034288076909,-22.1383729640963,
12.));
#195202=CARTESIAN_POINT('Ctrl Pts',(-11.4234058771742,-22.1537501391486,
0.));
#195203=CARTESIAN_POINT('Ctrl Pts',(-11.4234058771742,-22.1537501391486,
12.));
#195204=CARTESIAN_POINT('Ctrl Pts',(-11.443483577557,-22.1691288486096,
0.));
#195205=CARTESIAN_POINT('Ctrl Pts',(-11.443483577557,-22.1691288486096,
12.));
#195206=CARTESIAN_POINT('Ctrl Pts',(-11.463661674411,-22.1845085709169,
0.));
#195207=CARTESIAN_POINT('Ctrl Pts',(-11.463661674411,-22.1845085709169,
12.));
#195208=CARTESIAN_POINT('Ctrl Pts',(-11.4839399342589,-22.1998887896435,
0.));
#195209=CARTESIAN_POINT('Ctrl Pts',(-11.4839399342589,-22.1998887896435,
12.));
#195210=CARTESIAN_POINT('Ctrl Pts',(-11.504318124424,-22.215268993102,0.));
#195211=CARTESIAN_POINT('Ctrl Pts',(-11.504318124424,-22.215268993102,12.));
#195212=CARTESIAN_POINT('Ctrl Pts',(-11.5247960128476,-22.2306486738899,
0.));
#195213=CARTESIAN_POINT('Ctrl Pts',(-11.5247960128476,-22.2306486738899,
12.));
#195214=CARTESIAN_POINT('Ctrl Pts',(-11.545373367912,-22.2460273284653,
0.));
#195215=CARTESIAN_POINT('Ctrl Pts',(-11.545373367912,-22.2460273284653,
12.));
#195216=CARTESIAN_POINT('Ctrl Pts',(-11.5660499582403,-22.2614044566898,
0.));
#195217=CARTESIAN_POINT('Ctrl Pts',(-11.5660499582403,-22.2614044566898,
12.));
#195218=CARTESIAN_POINT('Ctrl Pts',(-11.5868255525189,-22.2767795614349,
0.));
#195219=CARTESIAN_POINT('Ctrl Pts',(-11.5868255525189,-22.2767795614349,
12.));
#195220=CARTESIAN_POINT('Ctrl Pts',(-11.6076999192359,-22.2921521480357,
0.));
#195221=CARTESIAN_POINT('Ctrl Pts',(-11.6076999192359,-22.2921521480357,
12.));
#195222=CARTESIAN_POINT('Ctrl Pts',(-11.6286728270011,-22.3075217249049,
0.));
#195223=CARTESIAN_POINT('Ctrl Pts',(-11.6286728270011,-22.3075217249049,
12.));
#195224=CARTESIAN_POINT('Ctrl Pts',(-11.6497440449858,-22.3228878043976,
0.));
#195225=CARTESIAN_POINT('Ctrl Pts',(-11.6497440449858,-22.3228878043976,
12.));
#195226=CARTESIAN_POINT('Ctrl Pts',(-11.6709133432986,-22.3382499035618,
0.));
#195227=CARTESIAN_POINT('Ctrl Pts',(-11.6709133432986,-22.3382499035618,
12.));
#195228=CARTESIAN_POINT('Ctrl Pts',(-11.6921804934056,-22.3536075450028,
0.));
#195229=CARTESIAN_POINT('Ctrl Pts',(-11.6921804934056,-22.3536075450028,
12.));
#195230=CARTESIAN_POINT('Ctrl Pts',(-11.7135452684532,-22.3689602575492,
0.));
#195231=CARTESIAN_POINT('Ctrl Pts',(-11.7135452684532,-22.3689602575492,
12.));
#195232=CARTESIAN_POINT('Ctrl Pts',(-11.7350074437961,-22.3843075773905,
0.));
#195233=CARTESIAN_POINT('Ctrl Pts',(-11.7350074437961,-22.3843075773905,
12.));
#195234=CARTESIAN_POINT('Ctrl Pts',(-11.7565667964765,-22.39964904692,0.));
#195235=CARTESIAN_POINT('Ctrl Pts',(-11.7565667964765,-22.39964904692,12.));
#195236=CARTESIAN_POINT('Ctrl Pts',(-11.7782231042041,-22.4149842125018,
0.));
#195237=CARTESIAN_POINT('Ctrl Pts',(-11.7782231042041,-22.4149842125018,
12.));
#195238=CARTESIAN_POINT('Ctrl Pts',(-11.7999761445175,-22.4303126226468,
0.));
#195239=CARTESIAN_POINT('Ctrl Pts',(-11.7999761445175,-22.4303126226468,
12.));
#195240=CARTESIAN_POINT('Ctrl Pts',(-11.8218256937889,-22.4456338258738,
0.));
#195241=CARTESIAN_POINT('Ctrl Pts',(-11.8218256937889,-22.4456338258738,
12.));
#195242=CARTESIAN_POINT('Ctrl Pts',(-11.8437715264487,-22.4609473690469,
0.));
#195243=CARTESIAN_POINT('Ctrl Pts',(-11.8437715264487,-22.4609473690469,
12.));
#195244=CARTESIAN_POINT('Ctrl Pts',(-11.8658134137018,-22.4762527946694,
0.));
#195245=CARTESIAN_POINT('Ctrl Pts',(-11.8658134137018,-22.4762527946694,
12.));
#195246=CARTESIAN_POINT('Ctrl Pts',(-11.8879511239941,-22.4915496418472,
0.));
#195247=CARTESIAN_POINT('Ctrl Pts',(-11.8879511239941,-22.4915496418472,
12.));
#195248=CARTESIAN_POINT('Ctrl Pts',(-11.9101844254555,-22.5068374513958,
0.));
#195249=CARTESIAN_POINT('Ctrl Pts',(-11.9101844254555,-22.5068374513958,
12.));
#195250=CARTESIAN_POINT('Ctrl Pts',(-11.9325130877801,-22.5221157697869,
0.));
#195251=CARTESIAN_POINT('Ctrl Pts',(-11.9325130877801,-22.5221157697869,
12.));
#195252=CARTESIAN_POINT('Ctrl Pts',(-11.9549368843996,-22.5373841537299,
0.));
#195253=CARTESIAN_POINT('Ctrl Pts',(-11.9549368843996,-22.5373841537299,
12.));
#195254=CARTESIAN_POINT('Ctrl Pts',(-11.9774555943496,-22.5526421741159,
0.));
#195255=CARTESIAN_POINT('Ctrl Pts',(-11.9774555943496,-22.5526421741159,
12.));
#195256=CARTESIAN_POINT('Ctrl Pts',(-12.0000690046697,-22.5678894211194,
0.));
#195257=CARTESIAN_POINT('Ctrl Pts',(-12.0000690046697,-22.5678894211194,
12.));
#195258=CARTESIAN_POINT('Ctrl Pts',(-12.0227769113132,-22.5831255061306,
0.));
#195259=CARTESIAN_POINT('Ctrl Pts',(-12.0227769113132,-22.5831255061306,
12.));
#195260=CARTESIAN_POINT('Ctrl Pts',(-12.0455791139135,-22.5983500505675,
0.));
#195261=CARTESIAN_POINT('Ctrl Pts',(-12.0455791139135,-22.5983500505675,
12.));
#195262=CARTESIAN_POINT('Ctrl Pts',(-12.0684754113869,-22.613562676493,
0.));
#195263=CARTESIAN_POINT('Ctrl Pts',(-12.0684754113869,-22.613562676493,
12.));
#195264=CARTESIAN_POINT('Ctrl Pts',(-12.0914655972828,-22.628762996708,
0.));
#195265=CARTESIAN_POINT('Ctrl Pts',(-12.0914655972828,-22.628762996708,
12.));
#195266=CARTESIAN_POINT('Ctrl Pts',(-12.1145494550384,-22.6439506046611,
0.));
#195267=CARTESIAN_POINT('Ctrl Pts',(-12.1145494550384,-22.6439506046611,
12.));
#195268=CARTESIAN_POINT('Ctrl Pts',(-12.1377267537141,-22.6591250653942,
0.));
#195269=CARTESIAN_POINT('Ctrl Pts',(-12.1377267537141,-22.6591250653942,
12.));
#195270=CARTESIAN_POINT('Ctrl Pts',(-12.1609972423089,-22.6742859034891,
0.));
#195271=CARTESIAN_POINT('Ctrl Pts',(-12.1609972423089,-22.6742859034891,
12.));
#195272=CARTESIAN_POINT('Ctrl Pts',(-12.1843606579246,-22.6894326204959,
0.));
#195273=CARTESIAN_POINT('Ctrl Pts',(-12.1843606579246,-22.6894326204959,
12.));
#195274=CARTESIAN_POINT('Ctrl Pts',(-12.2078167360267,-22.7045647168659,
0.));
#195275=CARTESIAN_POINT('Ctrl Pts',(-12.2078167360267,-22.7045647168659,
12.));
#195276=CARTESIAN_POINT('Ctrl Pts',(-12.2313652198047,-22.7196817119299,
0.));
#195277=CARTESIAN_POINT('Ctrl Pts',(-12.2313652198047,-22.7196817119299,
12.));
#195278=CARTESIAN_POINT('Ctrl Pts',(-12.2550058702389,-22.7347831655251,
0.));
#195279=CARTESIAN_POINT('Ctrl Pts',(-12.2550058702389,-22.7347831655251,
12.));
#195280=CARTESIAN_POINT('Ctrl Pts',(-12.2787384750747,-22.7498686970096,
0.));
#195281=CARTESIAN_POINT('Ctrl Pts',(-12.2787384750747,-22.7498686970096,
12.));
#195282=CARTESIAN_POINT('Ctrl Pts',(-12.3025628601812,-22.7649380101154,
0.));
#195283=CARTESIAN_POINT('Ctrl Pts',(-12.3025628601812,-22.7649380101154,
12.));
#195284=CARTESIAN_POINT('Ctrl Pts',(-12.3264788926108,-22.7799908974947,
0.));
#195285=CARTESIAN_POINT('Ctrl Pts',(-12.3264788926108,-22.7799908974947,
12.));
#195286=CARTESIAN_POINT('Ctrl Pts',(-12.3504864740361,-22.7950272216959,
0.));
#195287=CARTESIAN_POINT('Ctrl Pts',(-12.3504864740361,-22.7950272216959,
12.));
#195288=CARTESIAN_POINT('Ctrl Pts',(-12.3745855366772,-22.8100469022632,
0.));
#195289=CARTESIAN_POINT('Ctrl Pts',(-12.3745855366772,-22.8100469022632,
12.));
#195290=CARTESIAN_POINT('Ctrl Pts',(-12.393937937903,-22.8220493007353,
0.));
#195291=CARTESIAN_POINT('Ctrl Pts',(-12.393937937903,-22.8220493007353,
12.));
#195292=CARTESIAN_POINT('Ctrl Pts',(-12.4084933766366,-22.8310435872852,
0.));
#195293=CARTESIAN_POINT('Ctrl Pts',(-12.4084933766366,-22.8310435872852,
12.));
#195294=CARTESIAN_POINT('Ctrl Pts',(-12.4182152851867,-22.8370364396497,
0.));
#195295=CARTESIAN_POINT('Ctrl Pts',(-12.4182152851867,-22.8370364396497,
12.));
#195296=CARTESIAN_POINT('Ctrl Pts',(-12.4230808101438,-22.8400320311648,
0.));
#195297=CARTESIAN_POINT('Ctrl Pts',(-12.4230808101438,-22.8400320311648,
12.));
#195298=CARTESIAN_POINT('',(-12.4230808101438,-22.8400320311648,0.));
#195299=CARTESIAN_POINT('Ctrl Pts',(-9.71462809124917,-20.353053841303,
0.));
#195300=CARTESIAN_POINT('Ctrl Pts',(-9.71462954053074,-20.353060251684,
0.));
#195301=CARTESIAN_POINT('Ctrl Pts',(-9.71465227853122,-20.3531126095522,
0.));
#195302=CARTESIAN_POINT('Ctrl Pts',(-9.71474590350792,-20.3533097561886,
0.));
#195303=CARTESIAN_POINT('Ctrl Pts',(-9.71498978052101,-20.3538098605706,
0.));
#195304=CARTESIAN_POINT('Ctrl Pts',(-9.71549257088175,-20.3548282742361,
0.));
#195305=CARTESIAN_POINT('Ctrl Pts',(-9.71619192554147,-20.3562337557875,
0.));
#195306=CARTESIAN_POINT('Ctrl Pts',(-9.71708493723062,-20.3580133103357,
0.));
#195307=CARTESIAN_POINT('Ctrl Pts',(-9.71816778327999,-20.3601498764344,
0.));
#195308=CARTESIAN_POINT('Ctrl Pts',(-9.71943648548115,-20.362625691398,
0.));
#195309=CARTESIAN_POINT('Ctrl Pts',(-9.72088778381102,-20.3654261611055,
0.));
#195310=CARTESIAN_POINT('Ctrl Pts',(-9.72251930722504,-20.3685406190576,
0.));
#195311=CARTESIAN_POINT('Ctrl Pts',(-9.72432910043193,-20.371960235676,
0.));
#195312=CARTESIAN_POINT('Ctrl Pts',(-9.72631531732871,-20.3756766651952,
0.));
#195313=CARTESIAN_POINT('Ctrl Pts',(-9.72847589116533,-20.3796805893304,
0.));
#195314=CARTESIAN_POINT('Ctrl Pts',(-9.73080870123726,-20.3839624556742,
0.));
#195315=CARTESIAN_POINT('Ctrl Pts',(-9.73331167102812,-20.3885129129912,
0.));
#195316=CARTESIAN_POINT('Ctrl Pts',(-9.7359829201425,-20.3933234845646,
0.));
#195317=CARTESIAN_POINT('Ctrl Pts',(-9.73882077613206,-20.3983866213331,
0.));
#195318=CARTESIAN_POINT('Ctrl Pts',(-9.74182369656273,-20.4036953576549,
0.));
#195319=CARTESIAN_POINT('Ctrl Pts',(-9.74499021838537,-20.4092430879861,
0.));
#195320=CARTESIAN_POINT('Ctrl Pts',(-9.74831889242175,-20.4150232777393,
0.));
#195321=CARTESIAN_POINT('Ctrl Pts',(-9.75180829786433,-20.4210295275818,
0.));
#195322=CARTESIAN_POINT('Ctrl Pts',(-9.75545705902416,-20.4272556476629,
0.));
#195323=CARTESIAN_POINT('Ctrl Pts',(-9.7592638628993,-20.4336957355474,
0.));
#195324=CARTESIAN_POINT('Ctrl Pts',(-9.76322747195502,-20.4403442329401,
0.));
#195325=CARTESIAN_POINT('Ctrl Pts',(-9.76734670980897,-20.447195862298,
0.));
#195326=CARTESIAN_POINT('Ctrl Pts',(-9.7716204510407,-20.4542455817527,
0.));
#195327=CARTESIAN_POINT('Ctrl Pts',(-9.77604760815523,-20.4614885274973,
0.));
#195328=CARTESIAN_POINT('Ctrl Pts',(-9.78062712373313,-20.4689199790668,
0.));
#195329=CARTESIAN_POINT('Ctrl Pts',(-9.78535797314162,-20.4765353711585,
0.));
#195330=CARTESIAN_POINT('Ctrl Pts',(-9.7902391649866,-20.4843302955329,
0.));
#195331=CARTESIAN_POINT('Ctrl Pts',(-9.79526974288344,-20.4923005087945,
0.));
#195332=CARTESIAN_POINT('Ctrl Pts',(-9.80044878520968,-20.500441931211,
0.));
#195333=CARTESIAN_POINT('Ctrl Pts',(-9.80577540161103,-20.5087506310507,
0.));
#195334=CARTESIAN_POINT('Ctrl Pts',(-9.81124873025278,-20.5172228122839,
0.));
#195335=CARTESIAN_POINT('Ctrl Pts',(-9.81686793455918,-20.5258548000625,
0.));
#195336=CARTESIAN_POINT('Ctrl Pts',(-9.82263220080328,-20.534643029951,
0.));
#195337=CARTESIAN_POINT('Ctrl Pts',(-9.82854073773858,-20.5435840460717,
0.));
#195338=CARTESIAN_POINT('Ctrl Pts',(-9.83459277585321,-20.5526744976461,
0.));
#195339=CARTESIAN_POINT('Ctrl Pts',(-9.84078756677589,-20.5619111362406,
0.));
#195340=CARTESIAN_POINT('Ctrl Pts',(-9.84712438256308,-20.5712908125145,
0.));
#195341=CARTESIAN_POINT('Ctrl Pts',(-9.85360251457004,-20.580810471002,
0.));
#195342=CARTESIAN_POINT('Ctrl Pts',(-9.8602212723275,-20.5904671449754,
0.));
#195343=CARTESIAN_POINT('Ctrl Pts',(-9.86697998242612,-20.6002579513696,
0.));
#195344=CARTESIAN_POINT('Ctrl Pts',(-9.87387798732944,-20.6101800854491,
0.));
#195345=CARTESIAN_POINT('Ctrl Pts',(-9.88091464472669,-20.6202308177472,
0.));
#195346=CARTESIAN_POINT('Ctrl Pts',(-9.88808932697305,-20.6304074914086,
0.));
#195347=CARTESIAN_POINT('Ctrl Pts',(-9.89540142049124,-20.6407075193977,
0.));
#195348=CARTESIAN_POINT('Ctrl Pts',(-9.90285032516696,-20.6511283817415,
0.));
#195349=CARTESIAN_POINT('Ctrl Pts',(-9.91043545377005,-20.6616676228315,
0.));
#195350=CARTESIAN_POINT('Ctrl Pts',(-9.91815623141285,-20.6723228488261,
0.));
#195351=CARTESIAN_POINT('Ctrl Pts',(-9.92601209498751,-20.6830917250255,
0.));
#195352=CARTESIAN_POINT('Ctrl Pts',(-9.93400249259737,-20.6939719732485,
0.));
#195353=CARTESIAN_POINT('Ctrl Pts',(-9.94212688298251,-20.7049613692237,
0.));
#195354=CARTESIAN_POINT('Ctrl Pts',(-9.95038473514962,-20.716057740758,
0.));
#195355=CARTESIAN_POINT('Ctrl Pts',(-9.95877552798403,-20.7272589658752,
0.));
#195356=CARTESIAN_POINT('Ctrl Pts',(-9.96729874986199,-20.7385629709795,
0.));
#195357=CARTESIAN_POINT('Ctrl Pts',(-9.97595389823461,-20.7499677289625,
0.));
#195358=CARTESIAN_POINT('Ctrl Pts',(-9.98474047926846,-20.7614712574989,
0.));
#195359=CARTESIAN_POINT('Ctrl Pts',(-9.99365800754638,-20.7730716175417,
0.));
#195360=CARTESIAN_POINT('Ctrl Pts',(-10.0027060057389,-20.7847669117568,
0.));
#195361=CARTESIAN_POINT('Ctrl Pts',(-10.0118840042786,-20.7965552829907,
0.));
#195362=CARTESIAN_POINT('Ctrl Pts',(-10.0211915410095,-20.8084349126885,
0.));
#195363=CARTESIAN_POINT('Ctrl Pts',(-10.0306281609435,-20.8204040196599,
0.));
#195364=CARTESIAN_POINT('Ctrl Pts',(-10.0401934160234,-20.8324608588906,
0.));
#195365=CARTESIAN_POINT('Ctrl Pts',(-10.0498868648733,-20.8446037203402,
0.));
#195366=CARTESIAN_POINT('Ctrl Pts',(-10.0597080725375,-20.856830927732,
0.));
#195367=CARTESIAN_POINT('Ctrl Pts',(-10.0696566102219,-20.8691408373705,
0.));
#195368=CARTESIAN_POINT('Ctrl Pts',(-10.0797320551154,-20.8815318371844,
0.));
#195369=CARTESIAN_POINT('Ctrl Pts',(-10.0899339901916,-20.8940023457371,
0.));
#195370=CARTESIAN_POINT('Ctrl Pts',(-10.1002620040076,-20.9065508112556,
0.));
#195371=CARTESIAN_POINT('Ctrl Pts',(-10.1107156904836,-20.9191757106266,
0.));
#195372=CARTESIAN_POINT('Ctrl Pts',(-10.1212946487057,-20.931875548473,
0.));
#195373=CARTESIAN_POINT('Ctrl Pts',(-10.1319984827909,-20.944648856393,
0.));
#195374=CARTESIAN_POINT('Ctrl Pts',(-10.1428268017257,-20.9574941921591,
0.));
#195375=CARTESIAN_POINT('Ctrl Pts',(-10.1537792192065,-20.970410138937,
0.));
#195376=CARTESIAN_POINT('Ctrl Pts',(-10.1648553534567,-20.9833953044736,
0.));
#195377=CARTESIAN_POINT('Ctrl Pts',(-10.1760548270765,-20.9964483203685,
0.));
#195378=CARTESIAN_POINT('Ctrl Pts',(-10.1873772669358,-21.0095678414486,
0.));
#195379=CARTESIAN_POINT('Ctrl Pts',(-10.1988223040425,-21.0227525451107,
0.));
#195380=CARTESIAN_POINT('Ctrl Pts',(-10.2103895734124,-21.0360011306814,
0.));
#195381=CARTESIAN_POINT('Ctrl Pts',(-10.2220787139157,-21.0493123187483,
0.));
#195382=CARTESIAN_POINT('Ctrl Pts',(-10.233889368157,-21.0626848505665,
0.));
#195383=CARTESIAN_POINT('Ctrl Pts',(-10.2458211823915,-21.0761174875448,
0.));
#195384=CARTESIAN_POINT('Ctrl Pts',(-10.2578738064183,-21.0896090107066,
0.));
#195385=CARTESIAN_POINT('Ctrl Pts',(-10.2700468934743,-21.1031582201625,
0.));
#195386=CARTESIAN_POINT('Ctrl Pts',(-10.2823401001067,-21.1167639345623,
0.));
#195387=CARTESIAN_POINT('Ctrl Pts',(-10.2947530860714,-21.130424990599,
0.));
#195388=CARTESIAN_POINT('Ctrl Pts',(-10.307285514268,-21.1441402425831,
0.));
#195389=CARTESIAN_POINT('Ctrl Pts',(-10.3199370506541,-21.1579085619959,
0.));
#195390=CARTESIAN_POINT('Ctrl Pts',(-10.3327073641574,-21.1717288370512,
0.));
#195391=CARTESIAN_POINT('Ctrl Pts',(-10.3455961265706,-21.1855999722427,
0.));
#195392=CARTESIAN_POINT('Ctrl Pts',(-10.3586030124595,-21.1995208879205,
0.));
#195393=CARTESIAN_POINT('Ctrl Pts',(-10.3717276991137,-21.2134905199359,
0.));
#195394=CARTESIAN_POINT('Ctrl Pts',(-10.384969866479,-21.2275078192708,
0.));
#195395=CARTESIAN_POINT('Ctrl Pts',(-10.3983291970846,-21.2415717516713,
0.));
#195396=CARTESIAN_POINT('Ctrl Pts',(-10.4118053759584,-21.2556812972741,
0.));
#195397=CARTESIAN_POINT('Ctrl Pts',(-10.4253980905394,-21.2698354502391,
0.));
#195398=CARTESIAN_POINT('Ctrl Pts',(-10.4391070306385,-21.2840332184471,
0.));
#195399=CARTESIAN_POINT('Ctrl Pts',(-10.452931888387,-21.2982736231924,
0.));
#195400=CARTESIAN_POINT('Ctrl Pts',(-10.4668723581768,-21.312555698873,
0.));
#195401=CARTESIAN_POINT('Ctrl Pts',(-10.4809281365933,-21.3268784926823,
0.));
#195402=CARTESIAN_POINT('Ctrl Pts',(-10.4950989223341,-21.3412410642912,
0.));
#195403=CARTESIAN_POINT('Ctrl Pts',(-10.509384416169,-21.3556424855822,
0.));
#195404=CARTESIAN_POINT('Ctrl Pts',(-10.523784320906,-21.3700818403942,
0.));
#195405=CARTESIAN_POINT('Ctrl Pts',(-10.5382983413422,-21.3845582242604,
0.));
#195406=CARTESIAN_POINT('Ctrl Pts',(-10.5529261842107,-21.3990707441495,
0.));
#195407=CARTESIAN_POINT('Ctrl Pts',(-10.5676675581106,-21.4136185181974,
0.));
#195408=CARTESIAN_POINT('Ctrl Pts',(-10.582522173457,-21.4282006754624,
0.));
#195409=CARTESIAN_POINT('Ctrl Pts',(-10.597489742462,-21.4428163557137,
0.));
#195410=CARTESIAN_POINT('Ctrl Pts',(-10.612569979096,-21.4574647092093,
0.));
#195411=CARTESIAN_POINT('Ctrl Pts',(-10.6277625990457,-21.4721448964766,
0.));
#195412=CARTESIAN_POINT('Ctrl Pts',(-10.6430673196609,-21.4868560880893,
0.));
#195413=CARTESIAN_POINT('Ctrl Pts',(-10.6584838598941,-21.5015974644454,
0.));
#195414=CARTESIAN_POINT('Ctrl Pts',(-10.6740119402835,-21.5163682155805,
0.));
#195415=CARTESIAN_POINT('Ctrl Pts',(-10.689651282929,-21.531167540981,0.));
#195416=CARTESIAN_POINT('Ctrl Pts',(-10.7054016114571,-21.5459946493955,
0.));
#195417=CARTESIAN_POINT('Ctrl Pts',(-10.7212626509816,-21.5608487586467,
0.));
#195418=CARTESIAN_POINT('Ctrl Pts',(-10.7372341280468,-21.5757290954372,
0.));
#195419=CARTESIAN_POINT('Ctrl Pts',(-10.7533157705943,-21.5906348951745,
0.));
#195420=CARTESIAN_POINT('Ctrl Pts',(-10.7695073079554,-21.6055654018179,
0.));
#195421=CARTESIAN_POINT('Ctrl Pts',(-10.7858084708262,-21.6205198677176,
0.));
#195422=CARTESIAN_POINT('Ctrl Pts',(-10.802218991237,-21.6354975534557,
0.));
#195423=CARTESIAN_POINT('Ctrl Pts',(-10.8187386025135,-21.6504977276864,
0.));
#195424=CARTESIAN_POINT('Ctrl Pts',(-10.835367039227,-21.6655196669727,
0.));
#195425=CARTESIAN_POINT('Ctrl Pts',(-10.8521040371832,-21.6805626556461,
0.));
#195426=CARTESIAN_POINT('Ctrl Pts',(-10.8689493334093,-21.6956259856667,
0.));
#195427=CARTESIAN_POINT('Ctrl Pts',(-10.8859026661292,-21.7107089564822,
0.));
#195428=CARTESIAN_POINT('Ctrl Pts',(-10.9029637747341,-21.7258108748874,
0.));
#195429=CARTESIAN_POINT('Ctrl Pts',(-10.9201323997386,-21.74093105488,0.));
#195430=CARTESIAN_POINT('Ctrl Pts',(-10.9374082827446,-21.7560688175252,
0.));
#195431=CARTESIAN_POINT('Ctrl Pts',(-10.9547911664457,-21.7712234908468,
0.));
#195432=CARTESIAN_POINT('Ctrl Pts',(-10.9722807946157,-21.7863944097143,
0.));
#195433=CARTESIAN_POINT('Ctrl Pts',(-10.9898769120913,-21.8015809157302,
0.));
#195434=CARTESIAN_POINT('Ctrl Pts',(-11.0075792647477,-21.8167823571168,
0.));
#195435=CARTESIAN_POINT('Ctrl Pts',(-11.0253875994598,-21.8319980886033,
0.));
#195436=CARTESIAN_POINT('Ctrl Pts',(-11.0433016640808,-21.8472274713103,
0.));
#195437=CARTESIAN_POINT('Ctrl Pts',(-11.0613212074364,-21.8624698726319,
0.));
#195438=CARTESIAN_POINT('Ctrl Pts',(-11.0794459793058,-21.8777246661191,
0.));
#195439=CARTESIAN_POINT('Ctrl Pts',(-11.0976757303944,-21.8929912313608,
0.));
#195440=CARTESIAN_POINT('Ctrl Pts',(-11.1160102123024,-21.9082689538687,
0.));
#195441=CARTESIAN_POINT('Ctrl Pts',(-11.134449177474,-21.9235572249518,
0.));
#195442=CARTESIAN_POINT('Ctrl Pts',(-11.1529923792002,-21.9388554416437,
0.));
#195443=CARTESIAN_POINT('Ctrl Pts',(-11.1716395716375,-21.9541630066504,
0.));
#195444=CARTESIAN_POINT('Ctrl Pts',(-11.190390509811,-21.9694793282913,
0.));
#195445=CARTESIAN_POINT('Ctrl Pts',(-11.2092449496125,-21.9848038204439,
0.));
#195446=CARTESIAN_POINT('Ctrl Pts',(-11.2282026477897,-22.0001359024839,
0.));
#195447=CARTESIAN_POINT('Ctrl Pts',(-11.2472633619276,-22.0154749992364,
0.));
#195448=CARTESIAN_POINT('Ctrl Pts',(-11.2664268504207,-22.0308205408351,
0.));
#195449=CARTESIAN_POINT('Ctrl Pts',(-11.2856928724374,-22.046171962566,
0.));
#195450=CARTESIAN_POINT('Ctrl Pts',(-11.3050611878771,-22.0615287047179,
0.));
#195451=CARTESIAN_POINT('Ctrl Pts',(-11.3245315573168,-22.0768902124267,
0.));
#195452=CARTESIAN_POINT('Ctrl Pts',(-11.3441037419553,-22.0922559355293,
0.));
#195453=CARTESIAN_POINT('Ctrl Pts',(-11.3637775035367,-22.1076253283978,
0.));
#195454=CARTESIAN_POINT('Ctrl Pts',(-11.3835526044256,-22.1229978500185,
0.));
#195455=CARTESIAN_POINT('Ctrl Pts',(-11.4034288076909,-22.1383729640963,
0.));
#195456=CARTESIAN_POINT('Ctrl Pts',(-11.4234058771742,-22.1537501391486,
0.));
#195457=CARTESIAN_POINT('Ctrl Pts',(-11.443483577557,-22.1691288486096,
0.));
#195458=CARTESIAN_POINT('Ctrl Pts',(-11.463661674411,-22.1845085709169,
0.));
#195459=CARTESIAN_POINT('Ctrl Pts',(-11.4839399342589,-22.1998887896435,
0.));
#195460=CARTESIAN_POINT('Ctrl Pts',(-11.504318124424,-22.215268993102,0.));
#195461=CARTESIAN_POINT('Ctrl Pts',(-11.5247960128476,-22.2306486738899,
0.));
#195462=CARTESIAN_POINT('Ctrl Pts',(-11.545373367912,-22.2460273284653,
0.));
#195463=CARTESIAN_POINT('Ctrl Pts',(-11.5660499582403,-22.2614044566898,
0.));
#195464=CARTESIAN_POINT('Ctrl Pts',(-11.5868255525189,-22.2767795614349,
0.));
#195465=CARTESIAN_POINT('Ctrl Pts',(-11.6076999192359,-22.2921521480357,
0.));
#195466=CARTESIAN_POINT('Ctrl Pts',(-11.6286728270011,-22.3075217249049,
0.));
#195467=CARTESIAN_POINT('Ctrl Pts',(-11.6497440449858,-22.3228878043976,
0.));
#195468=CARTESIAN_POINT('Ctrl Pts',(-11.6709133432986,-22.3382499035618,
0.));
#195469=CARTESIAN_POINT('Ctrl Pts',(-11.6921804934056,-22.3536075450028,
0.));
#195470=CARTESIAN_POINT('Ctrl Pts',(-11.7135452684532,-22.3689602575492,
0.));
#195471=CARTESIAN_POINT('Ctrl Pts',(-11.7350074437961,-22.3843075773905,
0.));
#195472=CARTESIAN_POINT('Ctrl Pts',(-11.7565667964765,-22.39964904692,0.));
#195473=CARTESIAN_POINT('Ctrl Pts',(-11.7782231042041,-22.4149842125018,
0.));
#195474=CARTESIAN_POINT('Ctrl Pts',(-11.7999761445175,-22.4303126226468,
0.));
#195475=CARTESIAN_POINT('Ctrl Pts',(-11.8218256937889,-22.4456338258738,
0.));
#195476=CARTESIAN_POINT('Ctrl Pts',(-11.8437715264487,-22.4609473690469,
0.));
#195477=CARTESIAN_POINT('Ctrl Pts',(-11.8658134137018,-22.4762527946694,
0.));
#195478=CARTESIAN_POINT('Ctrl Pts',(-11.8879511239941,-22.4915496418472,
0.));
#195479=CARTESIAN_POINT('Ctrl Pts',(-11.9101844254555,-22.5068374513958,
0.));
#195480=CARTESIAN_POINT('Ctrl Pts',(-11.9325130877801,-22.5221157697869,
0.));
#195481=CARTESIAN_POINT('Ctrl Pts',(-11.9549368843996,-22.5373841537299,
0.));
#195482=CARTESIAN_POINT('Ctrl Pts',(-11.9774555943496,-22.5526421741159,
0.));
#195483=CARTESIAN_POINT('Ctrl Pts',(-12.0000690046697,-22.5678894211194,
0.));
#195484=CARTESIAN_POINT('Ctrl Pts',(-12.0227769113132,-22.5831255061306,
0.));
#195485=CARTESIAN_POINT('Ctrl Pts',(-12.0455791139135,-22.5983500505675,
0.));
#195486=CARTESIAN_POINT('Ctrl Pts',(-12.0684754113869,-22.613562676493,
0.));
#195487=CARTESIAN_POINT('Ctrl Pts',(-12.0914655972828,-22.628762996708,
0.));
#195488=CARTESIAN_POINT('Ctrl Pts',(-12.1145494550384,-22.6439506046611,
0.));
#195489=CARTESIAN_POINT('Ctrl Pts',(-12.1377267537141,-22.6591250653942,
0.));
#195490=CARTESIAN_POINT('Ctrl Pts',(-12.1609972423089,-22.6742859034891,
0.));
#195491=CARTESIAN_POINT('Ctrl Pts',(-12.1843606579246,-22.6894326204959,
0.));
#195492=CARTESIAN_POINT('Ctrl Pts',(-12.2078167360267,-22.7045647168659,
0.));
#195493=CARTESIAN_POINT('Ctrl Pts',(-12.2313652198047,-22.7196817119299,
0.));
#195494=CARTESIAN_POINT('Ctrl Pts',(-12.2550058702389,-22.7347831655251,
0.));
#195495=CARTESIAN_POINT('Ctrl Pts',(-12.2787384750747,-22.7498686970096,
0.));
#195496=CARTESIAN_POINT('Ctrl Pts',(-12.3025628601812,-22.7649380101154,
0.));
#195497=CARTESIAN_POINT('Ctrl Pts',(-12.3264788926108,-22.7799908974947,
0.));
#195498=CARTESIAN_POINT('Ctrl Pts',(-12.3504864740361,-22.7950272216959,
0.));
#195499=CARTESIAN_POINT('Ctrl Pts',(-12.3745855366772,-22.8100469022632,
0.));
#195500=CARTESIAN_POINT('Ctrl Pts',(-12.393937937903,-22.8220493007353,
0.));
#195501=CARTESIAN_POINT('Ctrl Pts',(-12.4084933766366,-22.8310435872852,
0.));
#195502=CARTESIAN_POINT('Ctrl Pts',(-12.4182152851867,-22.8370364396497,
0.));
#195503=CARTESIAN_POINT('Ctrl Pts',(-12.4230808101438,-22.8400320311648,
0.));
#195504=CARTESIAN_POINT('',(-12.4230808101438,-22.8400320311648,0.));
#195505=CARTESIAN_POINT('Origin',(-13.9675290154577,-16.3449727195351,0.));
#195506=CARTESIAN_POINT('',(-14.6513681262571,-17.1452095830632,0.));
#195507=CARTESIAN_POINT('',(-14.6513681262571,-17.1452095830632,0.));
#195508=CARTESIAN_POINT('',(-6.98376450772884,-8.17248635976757,0.));
#195509=CARTESIAN_POINT('Ctrl Pts',(-13.5685075571671,-22.1787195904339,
0.));
#195510=CARTESIAN_POINT('Ctrl Pts',(-13.5685075571671,-22.1787195904339,
12.));
#195511=CARTESIAN_POINT('Ctrl Pts',(-13.5683460612913,-22.1730081264583,
0.));
#195512=CARTESIAN_POINT('Ctrl Pts',(-13.5683460612913,-22.1730081264583,
12.));
#195513=CARTESIAN_POINT('Ctrl Pts',(-13.5680170531724,-22.1615922804939,
0.));
#195514=CARTESIAN_POINT('Ctrl Pts',(-13.5680170531724,-22.1615922804939,
12.));
#195515=CARTESIAN_POINT('Ctrl Pts',(-13.5675054918922,-22.1444897575076,
0.));
#195516=CARTESIAN_POINT('Ctrl Pts',(-13.5675054918922,-22.1444897575076,
12.));
#195517=CARTESIAN_POINT('Ctrl Pts',(-13.5667873105179,-22.1217288871823,
0.));
#195518=CARTESIAN_POINT('Ctrl Pts',(-13.5667873105179,-22.1217288871823,
12.));
#195519=CARTESIAN_POINT('Ctrl Pts',(-13.5658294169107,-22.0933486464442,
0.));
#195520=CARTESIAN_POINT('Ctrl Pts',(-13.5658294169107,-22.0933486464442,
12.));
#195521=CARTESIAN_POINT('Ctrl Pts',(-13.5648113688895,-22.0650393089492,
0.));
#195522=CARTESIAN_POINT('Ctrl Pts',(-13.5648113688895,-22.0650393089492,
12.));
#195523=CARTESIAN_POINT('Ctrl Pts',(-13.5637332022393,-22.0368009736227,
0.));
#195524=CARTESIAN_POINT('Ctrl Pts',(-13.5637332022393,-22.0368009736227,
12.));
#195525=CARTESIAN_POINT('Ctrl Pts',(-13.5625949868313,-22.0086337943431,
0.));
#195526=CARTESIAN_POINT('Ctrl Pts',(-13.5625949868313,-22.0086337943431,
12.));
#195527=CARTESIAN_POINT('Ctrl Pts',(-13.5613968357589,-21.9805379899192,
0.));
#195528=CARTESIAN_POINT('Ctrl Pts',(-13.5613968357589,-21.9805379899192,
12.));
#195529=CARTESIAN_POINT('Ctrl Pts',(-13.5601389185315,-21.9525138592862,
0.));
#195530=CARTESIAN_POINT('Ctrl Pts',(-13.5601389185315,-21.9525138592862,
12.));
#195531=CARTESIAN_POINT('Ctrl Pts',(-13.5588214586672,-21.9245617765827,
0.));
#195532=CARTESIAN_POINT('Ctrl Pts',(-13.5588214586672,-21.9245617765827,
12.));
#195533=CARTESIAN_POINT('Ctrl Pts',(-13.5574447178485,-21.8966821688876,
0.));
#195534=CARTESIAN_POINT('Ctrl Pts',(-13.5574447178485,-21.8966821688876,
12.));
#195535=CARTESIAN_POINT('Ctrl Pts',(-13.5560089839426,-21.8688754989401,
0.));
#195536=CARTESIAN_POINT('Ctrl Pts',(-13.5560089839426,-21.8688754989401,
12.));
#195537=CARTESIAN_POINT('Ctrl Pts',(-13.5545145573049,-21.841142245609,
0.));
#195538=CARTESIAN_POINT('Ctrl Pts',(-13.5545145573049,-21.841142245609,
12.));
#195539=CARTESIAN_POINT('Ctrl Pts',(-13.5529617381569,-21.8134828857963,
0.));
#195540=CARTESIAN_POINT('Ctrl Pts',(-13.5529617381569,-21.8134828857963,
12.));
#195541=CARTESIAN_POINT('Ctrl Pts',(-13.5513508127232,-21.7858978745848,
0.));
#195542=CARTESIAN_POINT('Ctrl Pts',(-13.5513508127232,-21.7858978745848,
12.));
#195543=CARTESIAN_POINT('Ctrl Pts',(-13.5496820422187,-21.7583876294532,
0.));
#195544=CARTESIAN_POINT('Ctrl Pts',(-13.5496820422187,-21.7583876294532,
12.));
#195545=CARTESIAN_POINT('Ctrl Pts',(-13.5479556704457,-21.730952541226,
0.));
#195546=CARTESIAN_POINT('Ctrl Pts',(-13.5479556704457,-21.730952541226,
12.));
#195547=CARTESIAN_POINT('Ctrl Pts',(-13.546171929503,-21.7035929822939,
0.));
#195548=CARTESIAN_POINT('Ctrl Pts',(-13.546171929503,-21.7035929822939,
12.));
#195549=CARTESIAN_POINT('Ctrl Pts',(-13.5443310461516,-21.676309315769,
0.));
#195550=CARTESIAN_POINT('Ctrl Pts',(-13.5443310461516,-21.676309315769,
12.));
#195551=CARTESIAN_POINT('Ctrl Pts',(-13.5424332480698,-21.6491019044647,
0.));
#195552=CARTESIAN_POINT('Ctrl Pts',(-13.5424332480698,-21.6491019044647,
12.));
#195553=CARTESIAN_POINT('Ctrl Pts',(-13.5404787697798,-21.6219711193951,
0.));
#195554=CARTESIAN_POINT('Ctrl Pts',(-13.5404787697798,-21.6219711193951,
12.));
#195555=CARTESIAN_POINT('Ctrl Pts',(-13.5384678597206,-21.5949173499022,
0.));
#195556=CARTESIAN_POINT('Ctrl Pts',(-13.5384678597206,-21.5949173499022,
12.));
#195557=CARTESIAN_POINT('Ctrl Pts',(-13.5364007790292,-21.5679410019011,
0.));
#195558=CARTESIAN_POINT('Ctrl Pts',(-13.5364007790292,-21.5679410019011,
12.));
#195559=CARTESIAN_POINT('Ctrl Pts',(-13.5342777983225,-21.5410424932511,
0.));
#195560=CARTESIAN_POINT('Ctrl Pts',(-13.5342777983225,-21.5410424932511,
12.));
#195561=CARTESIAN_POINT('Ctrl Pts',(-13.5320991952145,-21.5142222501671,
0.));
#195562=CARTESIAN_POINT('Ctrl Pts',(-13.5320991952145,-21.5142222501671,
12.));
#195563=CARTESIAN_POINT('Ctrl Pts',(-13.5298652514357,-21.487480703047,
0.));
#195564=CARTESIAN_POINT('Ctrl Pts',(-13.5298652514357,-21.487480703047,
12.));
#195565=CARTESIAN_POINT('Ctrl Pts',(-13.5275762503553,-21.4608182828695,
0.));
#195566=CARTESIAN_POINT('Ctrl Pts',(-13.5275762503553,-21.4608182828695,
12.));
#195567=CARTESIAN_POINT('Ctrl Pts',(-13.5252324737795,-21.4342354165253,
0.));
#195568=CARTESIAN_POINT('Ctrl Pts',(-13.5252324737795,-21.4342354165253,
12.));
#195569=CARTESIAN_POINT('Ctrl Pts',(-13.5228342013508,-21.4077325259318,
0.));
#195570=CARTESIAN_POINT('Ctrl Pts',(-13.5228342013508,-21.4077325259318,
12.));
#195571=CARTESIAN_POINT('Ctrl Pts',(-13.5203817122497,-21.3813100304967,
0.));
#195572=CARTESIAN_POINT('Ctrl Pts',(-13.5203817122497,-21.3813100304967,
12.));
#195573=CARTESIAN_POINT('Ctrl Pts',(-13.5178752862461,-21.3549683486219,
0.));
#195574=CARTESIAN_POINT('Ctrl Pts',(-13.5178752862461,-21.3549683486219,
12.));
#195575=CARTESIAN_POINT('Ctrl Pts',(-13.5153152050554,-21.328707899634,
0.));
#195576=CARTESIAN_POINT('Ctrl Pts',(-13.5153152050554,-21.328707899634,
12.));
#195577=CARTESIAN_POINT('Ctrl Pts',(-13.5127017534972,-21.3025291054236,
0.));
#195578=CARTESIAN_POINT('Ctrl Pts',(-13.5127017534972,-21.3025291054236,
12.));
#195579=CARTESIAN_POINT('Ctrl Pts',(-13.5100352209207,-21.2764323924442,
0.));
#195580=CARTESIAN_POINT('Ctrl Pts',(-13.5100352209207,-21.2764323924442,
12.));
#195581=CARTESIAN_POINT('Ctrl Pts',(-13.5073159019454,-21.2504181927429,
0.));
#195582=CARTESIAN_POINT('Ctrl Pts',(-13.5073159019454,-21.2504181927429,
12.));
#195583=CARTESIAN_POINT('Ctrl Pts',(-13.5045440957404,-21.224486942933,
0.));
#195584=CARTESIAN_POINT('Ctrl Pts',(-13.5045440957404,-21.224486942933,
12.));
#195585=CARTESIAN_POINT('Ctrl Pts',(-13.5017201056088,-21.1986390835825,
0.));
#195586=CARTESIAN_POINT('Ctrl Pts',(-13.5017201056088,-21.1986390835825,
12.));
#195587=CARTESIAN_POINT('Ctrl Pts',(-13.4988442384491,-21.1728750584173,
0.));
#195588=CARTESIAN_POINT('Ctrl Pts',(-13.4988442384491,-21.1728750584173,
12.));
#195589=CARTESIAN_POINT('Ctrl Pts',(-13.4959168042934,-21.1471953136209,
0.));
#195590=CARTESIAN_POINT('Ctrl Pts',(-13.4959168042934,-21.1471953136209,
12.));
#195591=CARTESIAN_POINT('Ctrl Pts',(-13.4929381157778,-21.1216002970209,
0.));
#195592=CARTESIAN_POINT('Ctrl Pts',(-13.4929381157778,-21.1216002970209,
12.));
#195593=CARTESIAN_POINT('Ctrl Pts',(-13.4899084877718,-21.0960904575048,
0.));
#195594=CARTESIAN_POINT('Ctrl Pts',(-13.4899084877718,-21.0960904575048,
12.));
#195595=CARTESIAN_POINT('Ctrl Pts',(-13.4868282377192,-21.0706662455202,
0.));
#195596=CARTESIAN_POINT('Ctrl Pts',(-13.4868282377192,-21.0706662455202,
12.));
#195597=CARTESIAN_POINT('Ctrl Pts',(-13.4836976858912,-21.0453281134247,
0.));
#195598=CARTESIAN_POINT('Ctrl Pts',(-13.4836976858912,-21.0453281134247,
12.));
#195599=CARTESIAN_POINT('Ctrl Pts',(-13.4805171556822,-21.0200765158885,
0.));
#195600=CARTESIAN_POINT('Ctrl Pts',(-13.4805171556822,-21.0200765158885,
12.));
#195601=CARTESIAN_POINT('Ctrl Pts',(-13.4772869738879,-20.9949119102592,
0.));
#195602=CARTESIAN_POINT('Ctrl Pts',(-13.4772869738879,-20.9949119102592,
12.));
#195603=CARTESIAN_POINT('Ctrl Pts',(-13.4740074710087,-20.9698347569476,
0.));
#195604=CARTESIAN_POINT('Ctrl Pts',(-13.4740074710087,-20.9698347569476,
12.));
#195605=CARTESIAN_POINT('Ctrl Pts',(-13.4706789815167,-20.9448455197557,
0.));
#195606=CARTESIAN_POINT('Ctrl Pts',(-13.4706789815167,-20.9448455197557,
12.));
#195607=CARTESIAN_POINT('Ctrl Pts',(-13.4673018437718,-20.9199446657584,
0.));
#195608=CARTESIAN_POINT('Ctrl Pts',(-13.4673018437718,-20.9199446657584,
12.));
#195609=CARTESIAN_POINT('Ctrl Pts',(-13.4638763999726,-20.8951326652158,
0.));
#195610=CARTESIAN_POINT('Ctrl Pts',(-13.4638763999726,-20.8951326652158,
12.));
#195611=CARTESIAN_POINT('Ctrl Pts',(-13.4604029960983,-20.8704099914641,
0.));
#195612=CARTESIAN_POINT('Ctrl Pts',(-13.4604029960983,-20.8704099914641,
12.));
#195613=CARTESIAN_POINT('Ctrl Pts',(-13.4568819818631,-20.8457771208082,
0.));
#195614=CARTESIAN_POINT('Ctrl Pts',(-13.4568819818631,-20.8457771208082,
12.));
#195615=CARTESIAN_POINT('Ctrl Pts',(-13.4533137106667,-20.821234532398,
0.));
#195616=CARTESIAN_POINT('Ctrl Pts',(-13.4533137106667,-20.821234532398,
12.));
#195617=CARTESIAN_POINT('Ctrl Pts',(-13.4496985395637,-20.7967827081227,
0.));
#195618=CARTESIAN_POINT('Ctrl Pts',(-13.4496985395637,-20.7967827081227,
12.));
#195619=CARTESIAN_POINT('Ctrl Pts',(-13.4460368293688,-20.7724221327608,
0.));
#195620=CARTESIAN_POINT('Ctrl Pts',(-13.4460368293688,-20.7724221327608,
12.));
#195621=CARTESIAN_POINT('Ctrl Pts',(-13.4423289447561,-20.7481532941013,
0.));
#195622=CARTESIAN_POINT('Ctrl Pts',(-13.4423289447561,-20.7481532941013,
12.));
#195623=CARTESIAN_POINT('Ctrl Pts',(-13.4385752543663,-20.7239766830675,
0.));
#195624=CARTESIAN_POINT('Ctrl Pts',(-13.4385752543663,-20.7239766830675,
12.));
#195625=CARTESIAN_POINT('Ctrl Pts',(-13.4347761309154,-20.6998927938288,
0.));
#195626=CARTESIAN_POINT('Ctrl Pts',(-13.4347761309154,-20.6998927938288,
12.));
#195627=CARTESIAN_POINT('Ctrl Pts',(-13.4309319513119,-20.6759021239103,
0.));
#195628=CARTESIAN_POINT('Ctrl Pts',(-13.4309319513119,-20.6759021239103,
12.));
#195629=CARTESIAN_POINT('Ctrl Pts',(-13.4270430967652,-20.6520051742869,
0.));
#195630=CARTESIAN_POINT('Ctrl Pts',(-13.4270430967652,-20.6520051742869,
12.));
#195631=CARTESIAN_POINT('Ctrl Pts',(-13.4231099528179,-20.6282024494237,
0.));
#195632=CARTESIAN_POINT('Ctrl Pts',(-13.4231099528179,-20.6282024494237,
12.));
#195633=CARTESIAN_POINT('Ctrl Pts',(-13.4191329093933,-20.6044944573153,
0.));
#195634=CARTESIAN_POINT('Ctrl Pts',(-13.4191329093933,-20.6044944573153,
12.));
#195635=CARTESIAN_POINT('Ctrl Pts',(-13.4151123608411,-20.5808817095155,
0.));
#195636=CARTESIAN_POINT('Ctrl Pts',(-13.4151123608411,-20.5808817095155,
12.));
#195637=CARTESIAN_POINT('Ctrl Pts',(-13.4110487059912,-20.5573647211639,
0.));
#195638=CARTESIAN_POINT('Ctrl Pts',(-13.4110487059912,-20.5573647211639,
12.));
#195639=CARTESIAN_POINT('Ctrl Pts',(-13.4069423482076,-20.5339440109956,
0.));
#195640=CARTESIAN_POINT('Ctrl Pts',(-13.4069423482076,-20.5339440109956,
12.));
#195641=CARTESIAN_POINT('Ctrl Pts',(-13.4027936954529,-20.5106201013753,
0.));
#195642=CARTESIAN_POINT('Ctrl Pts',(-13.4027936954529,-20.5106201013753,
12.));
#195643=CARTESIAN_POINT('Ctrl Pts',(-13.3986031603716,-20.487393518404,
0.));
#195644=CARTESIAN_POINT('Ctrl Pts',(-13.3986031603716,-20.487393518404,
12.));
#195645=CARTESIAN_POINT('Ctrl Pts',(-13.3943711603739,-20.4642647920037,
0.));
#195646=CARTESIAN_POINT('Ctrl Pts',(-13.3943711603739,-20.4642647920037,
12.));
#195647=CARTESIAN_POINT('Ctrl Pts',(-13.3900981177255,-20.4412344560007,
0.));
#195648=CARTESIAN_POINT('Ctrl Pts',(-13.3900981177255,-20.4412344560007,
12.));
#195649=CARTESIAN_POINT('Ctrl Pts',(-13.3857844596387,-20.4183030482002,
0.));
#195650=CARTESIAN_POINT('Ctrl Pts',(-13.3857844596387,-20.4183030482002,
12.));
#195651=CARTESIAN_POINT('Ctrl Pts',(-13.3814306183719,-20.3954711104502,
0.));
#195652=CARTESIAN_POINT('Ctrl Pts',(-13.3814306183719,-20.3954711104502,
12.));
#195653=CARTESIAN_POINT('Ctrl Pts',(-13.3770370313188,-20.3727391887184,
0.));
#195654=CARTESIAN_POINT('Ctrl Pts',(-13.3770370313188,-20.3727391887184,
12.));
#195655=CARTESIAN_POINT('Ctrl Pts',(-13.3726041410867,-20.3501078331814,
0.));
#195656=CARTESIAN_POINT('Ctrl Pts',(-13.3726041410867,-20.3501078331814,
12.));
#195657=CARTESIAN_POINT('Ctrl Pts',(-13.3681323955826,-20.3275775983029,
0.));
#195658=CARTESIAN_POINT('Ctrl Pts',(-13.3681323955826,-20.3275775983029,
12.));
#195659=CARTESIAN_POINT('Ctrl Pts',(-13.3636222481016,-20.3051490429048,
0.));
#195660=CARTESIAN_POINT('Ctrl Pts',(-13.3636222481016,-20.3051490429048,
12.));
#195661=CARTESIAN_POINT('Ctrl Pts',(-13.3590741574195,-20.2828227302339,
0.));
#195662=CARTESIAN_POINT('Ctrl Pts',(-13.3590741574195,-20.2828227302339,
12.));
#195663=CARTESIAN_POINT('Ctrl Pts',(-13.3544885878889,-20.2605992280122,
0.));
#195664=CARTESIAN_POINT('Ctrl Pts',(-13.3544885878889,-20.2605992280122,
12.));
#195665=CARTESIAN_POINT('Ctrl Pts',(-13.3498660095386,-20.2384791085359,
0.));
#195666=CARTESIAN_POINT('Ctrl Pts',(-13.3498660095386,-20.2384791085359,
12.));
#195667=CARTESIAN_POINT('Ctrl Pts',(-13.3452068981766,-20.216462948786,
0.));
#195668=CARTESIAN_POINT('Ctrl Pts',(-13.3452068981766,-20.216462948786,
12.));
#195669=CARTESIAN_POINT('Ctrl Pts',(-13.3405117354971,-20.1945513305235,
0.));
#195670=CARTESIAN_POINT('Ctrl Pts',(-13.3405117354971,-20.1945513305235,
12.));
#195671=CARTESIAN_POINT('Ctrl Pts',(-13.3357810091903,-20.1727448403817,
0.));
#195672=CARTESIAN_POINT('Ctrl Pts',(-13.3357810091903,-20.1727448403817,
12.));
#195673=CARTESIAN_POINT('Ctrl Pts',(-13.3310152130564,-20.1510440699474,
0.));
#195674=CARTESIAN_POINT('Ctrl Pts',(-13.3310152130564,-20.1510440699474,
12.));
#195675=CARTESIAN_POINT('Ctrl Pts',(-13.3262148471226,-20.1294496158402,
0.));
#195676=CARTESIAN_POINT('Ctrl Pts',(-13.3262148471226,-20.1294496158402,
12.));
#195677=CARTESIAN_POINT('Ctrl Pts',(-13.3213804177587,-20.1079620798375,
0.));
#195678=CARTESIAN_POINT('Ctrl Pts',(-13.3213804177587,-20.1079620798375,
12.));
#195679=CARTESIAN_POINT('Ctrl Pts',(-13.3165124377963,-20.0865820689882,
0.));
#195680=CARTESIAN_POINT('Ctrl Pts',(-13.3165124377963,-20.0865820689882,
12.));
#195681=CARTESIAN_POINT('Ctrl Pts',(-13.3116114266515,-20.0653101957188,
0.));
#195682=CARTESIAN_POINT('Ctrl Pts',(-13.3116114266515,-20.0653101957188,
12.));
#195683=CARTESIAN_POINT('Ctrl Pts',(-13.3066779104515,-20.0441470779345,
0.));
#195684=CARTESIAN_POINT('Ctrl Pts',(-13.3066779104515,-20.0441470779345,
12.));
#195685=CARTESIAN_POINT('Ctrl Pts',(-13.3017124221637,-20.0230933391038,
0.));
#195686=CARTESIAN_POINT('Ctrl Pts',(-13.3017124221637,-20.0230933391038,
12.));
#195687=CARTESIAN_POINT('Ctrl Pts',(-13.2967155017306,-20.0021496083738,
0.));
#195688=CARTESIAN_POINT('Ctrl Pts',(-13.2967155017306,-20.0021496083738,
12.));
#195689=CARTESIAN_POINT('Ctrl Pts',(-13.2916876962094,-19.981316520717,
0.));
#195690=CARTESIAN_POINT('Ctrl Pts',(-13.2916876962094,-19.981316520717,
12.));
#195691=CARTESIAN_POINT('Ctrl Pts',(-13.286629559915,-19.9605947170586,
0.));
#195692=CARTESIAN_POINT('Ctrl Pts',(-13.286629559915,-19.9605947170586,
12.));
#195693=CARTESIAN_POINT('Ctrl Pts',(-13.2815416545663,-19.9399848444019,
0.));
#195694=CARTESIAN_POINT('Ctrl Pts',(-13.2815416545663,-19.9399848444019,
12.));
#195695=CARTESIAN_POINT('Ctrl Pts',(-13.2764245494357,-19.9194875559422,
0.));
#195696=CARTESIAN_POINT('Ctrl Pts',(-13.2764245494357,-19.9194875559422,
12.));
#195697=CARTESIAN_POINT('Ctrl Pts',(-13.271278821502,-19.8991035111745,
0.));
#195698=CARTESIAN_POINT('Ctrl Pts',(-13.271278821502,-19.8991035111745,
12.));
#195699=CARTESIAN_POINT('Ctrl Pts',(-13.2661050556132,-19.8788333760577,
0.));
#195700=CARTESIAN_POINT('Ctrl Pts',(-13.2661050556132,-19.8788333760577,
12.));
#195701=CARTESIAN_POINT('Ctrl Pts',(-13.2609038446529,-19.8586778231715,
0.));
#195702=CARTESIAN_POINT('Ctrl Pts',(-13.2609038446529,-19.8586778231715,
12.));
#195703=CARTESIAN_POINT('Ctrl Pts',(-13.2556757897086,-19.8386375318634,
0.));
#195704=CARTESIAN_POINT('Ctrl Pts',(-13.2556757897086,-19.8386375318634,
12.));
#195705=CARTESIAN_POINT('Ctrl Pts',(-13.2504215002457,-19.8187131883917,
0.));
#195706=CARTESIAN_POINT('Ctrl Pts',(-13.2504215002457,-19.8187131883917,
12.));
#195707=CARTESIAN_POINT('Ctrl Pts',(-13.2451415942805,-19.7989054860495,
0.));
#195708=CARTESIAN_POINT('Ctrl Pts',(-13.2451415942805,-19.7989054860495,
12.));
#195709=CARTESIAN_POINT('Ctrl Pts',(-13.2398366985675,-19.7792151253289,
0.));
#195710=CARTESIAN_POINT('Ctrl Pts',(-13.2398366985675,-19.7792151253289,
12.));
#195711=CARTESIAN_POINT('Ctrl Pts',(-13.2345074487963,-19.7596428141168,
0.));
#195712=CARTESIAN_POINT('Ctrl Pts',(-13.2345074487963,-19.7596428141168,
12.));
#195713=CARTESIAN_POINT('Ctrl Pts',(-13.2291544897899,-19.7401892678697,
0.));
#195714=CARTESIAN_POINT('Ctrl Pts',(-13.2291544897899,-19.7401892678697,
12.));
#195715=CARTESIAN_POINT('Ctrl Pts',(-13.2237784757066,-19.7208552097868,
0.));
#195716=CARTESIAN_POINT('Ctrl Pts',(-13.2237784757066,-19.7208552097868,
12.));
#195717=CARTESIAN_POINT('Ctrl Pts',(-13.2183800702436,-19.7016413709685,
0.));
#195718=CARTESIAN_POINT('Ctrl Pts',(-13.2183800702436,-19.7016413709685,
12.));
#195719=CARTESIAN_POINT('Ctrl Pts',(-13.2129599468485,-19.6825484905823,
0.));
#195720=CARTESIAN_POINT('Ctrl Pts',(-13.2129599468485,-19.6825484905823,
12.));
#195721=CARTESIAN_POINT('Ctrl Pts',(-13.2075187889529,-19.6635773160936,
0.));
#195722=CARTESIAN_POINT('Ctrl Pts',(-13.2075187889529,-19.6635773160936,
12.));
#195723=CARTESIAN_POINT('Ctrl Pts',(-13.2020572902065,-19.6447286034772,
0.));
#195724=CARTESIAN_POINT('Ctrl Pts',(-13.2020572902065,-19.6447286034772,
12.));
#195725=CARTESIAN_POINT('Ctrl Pts',(-13.1965761547151,-19.6260031174244,
0.));
#195726=CARTESIAN_POINT('Ctrl Pts',(-13.1965761547151,-19.6260031174244,
12.));
#195727=CARTESIAN_POINT('Ctrl Pts',(-13.1910760972814,-19.6074016315414,
0.));
#195728=CARTESIAN_POINT('Ctrl Pts',(-13.1910760972814,-19.6074016315414,
12.));
#195729=CARTESIAN_POINT('Ctrl Pts',(-13.1855578436471,-19.5889249285338,
0.));
#195730=CARTESIAN_POINT('Ctrl Pts',(-13.1855578436471,-19.5889249285338,
12.));
#195731=CARTESIAN_POINT('Ctrl Pts',(-13.1800221307673,-19.5705738004667,
0.));
#195732=CARTESIAN_POINT('Ctrl Pts',(-13.1800221307673,-19.5705738004667,
12.));
#195733=CARTESIAN_POINT('Ctrl Pts',(-13.1744697070911,-19.5523490490244,
0.));
#195734=CARTESIAN_POINT('Ctrl Pts',(-13.1744697070911,-19.5523490490244,
12.));
#195735=CARTESIAN_POINT('Ctrl Pts',(-13.1689013328431,-19.5342514857562,
0.));
#195736=CARTESIAN_POINT('Ctrl Pts',(-13.1689013328431,-19.5342514857562,
12.));
#195737=CARTESIAN_POINT('Ctrl Pts',(-13.1633177803101,-19.5162819323213,
0.));
#195738=CARTESIAN_POINT('Ctrl Pts',(-13.1633177803101,-19.5162819323213,
12.));
#195739=CARTESIAN_POINT('Ctrl Pts',(-13.1577198341245,-19.4984412207081,
0.));
#195740=CARTESIAN_POINT('Ctrl Pts',(-13.1577198341245,-19.4984412207081,
12.));
#195741=CARTESIAN_POINT('Ctrl Pts',(-13.1521082915853,-19.4807301935268,
0.));
#195742=CARTESIAN_POINT('Ctrl Pts',(-13.1521082915853,-19.4807301935268,
12.));
#195743=CARTESIAN_POINT('Ctrl Pts',(-13.1464839629971,-19.4631497043258,
0.));
#195744=CARTESIAN_POINT('Ctrl Pts',(-13.1464839629971,-19.4631497043258,
12.));
#195745=CARTESIAN_POINT('Ctrl Pts',(-13.1408476720061,-19.4457006178876,
0.));
#195746=CARTESIAN_POINT('Ctrl Pts',(-13.1408476720061,-19.4457006178876,
12.));
#195747=CARTESIAN_POINT('Ctrl Pts',(-13.1352002559438,-19.4283838105262,
0.));
#195748=CARTESIAN_POINT('Ctrl Pts',(-13.1352002559438,-19.4283838105262,
12.));
#195749=CARTESIAN_POINT('Ctrl Pts',(-13.1295425661634,-19.4112001703557,
0.));
#195750=CARTESIAN_POINT('Ctrl Pts',(-13.1295425661634,-19.4112001703557,
12.));
#195751=CARTESIAN_POINT('Ctrl Pts',(-13.1238754684177,-19.3941505976263,
0.));
#195752=CARTESIAN_POINT('Ctrl Pts',(-13.1238754684177,-19.3941505976263,
12.));
#195753=CARTESIAN_POINT('Ctrl Pts',(-13.118199843271,-19.3772360051091,
0.));
#195754=CARTESIAN_POINT('Ctrl Pts',(-13.118199843271,-19.3772360051091,
12.));
#195755=CARTESIAN_POINT('Ctrl Pts',(-13.1125165865022,-19.3604573184515,
0.));
#195756=CARTESIAN_POINT('Ctrl Pts',(-13.1125165865022,-19.3604573184515,
12.));
#195757=CARTESIAN_POINT('Ctrl Pts',(-13.1068266095186,-19.3438154765395,
0.));
#195758=CARTESIAN_POINT('Ctrl Pts',(-13.1068266095186,-19.3438154765395,
12.));
#195759=CARTESIAN_POINT('Ctrl Pts',(-13.1011308397591,-19.3273114318269,
0.));
#195760=CARTESIAN_POINT('Ctrl Pts',(-13.1011308397591,-19.3273114318269,
12.));
#195761=CARTESIAN_POINT('Ctrl Pts',(-13.0954302211479,-19.310946150736,
0.));
#195762=CARTESIAN_POINT('Ctrl Pts',(-13.0954302211479,-19.310946150736,
12.));
#195763=CARTESIAN_POINT('Ctrl Pts',(-13.0897257145969,-19.2947206141247,
0.));
#195764=CARTESIAN_POINT('Ctrl Pts',(-13.0897257145969,-19.2947206141247,
12.));
#195765=CARTESIAN_POINT('Ctrl Pts',(-13.0840182984949,-19.2786358177198,
0.));
#195766=CARTESIAN_POINT('Ctrl Pts',(-13.0840182984949,-19.2786358177198,
12.));
#195767=CARTESIAN_POINT('Ctrl Pts',(-13.0783089692118,-19.2626927725596,
0.));
#195768=CARTESIAN_POINT('Ctrl Pts',(-13.0783089692118,-19.2626927725596,
12.));
#195769=CARTESIAN_POINT('Ctrl Pts',(-13.0725987415859,-19.2468925053989,
0.));
#195770=CARTESIAN_POINT('Ctrl Pts',(-13.0725987415859,-19.2468925053989,
12.));
#195771=CARTESIAN_POINT('Ctrl Pts',(-13.0668886494795,-19.2312360592033,
0.));
#195772=CARTESIAN_POINT('Ctrl Pts',(-13.0668886494795,-19.2312360592033,
12.));
#195773=CARTESIAN_POINT('Ctrl Pts',(-13.0611797463915,-19.2157244937142,
0.));
#195774=CARTESIAN_POINT('Ctrl Pts',(-13.0611797463915,-19.2157244937142,
12.));
#195775=CARTESIAN_POINT('Ctrl Pts',(-13.0554731060538,-19.2003588859772,
0.));
#195776=CARTESIAN_POINT('Ctrl Pts',(-13.0554731060538,-19.2003588859772,
12.));
#195777=CARTESIAN_POINT('Ctrl Pts',(-13.0497698230441,-19.1851403308825,
0.));
#195778=CARTESIAN_POINT('Ctrl Pts',(-13.0497698230441,-19.1851403308825,
12.));
#195779=CARTESIAN_POINT('Ctrl Pts',(-13.0440710133772,-19.1700699416622,
0.));
#195780=CARTESIAN_POINT('Ctrl Pts',(-13.0440710133772,-19.1700699416622,
12.));
#195781=CARTESIAN_POINT('Ctrl Pts',(-13.0383778152068,-19.155148850523,
0.));
#195782=CARTESIAN_POINT('Ctrl Pts',(-13.0383778152068,-19.155148850523,
12.));
#195783=CARTESIAN_POINT('Ctrl Pts',(-13.0326913895838,-19.1403782093386,
0.));
#195784=CARTESIAN_POINT('Ctrl Pts',(-13.0326913895838,-19.1403782093386,
12.));
#195785=CARTESIAN_POINT('Ctrl Pts',(-13.0270129211976,-19.1257591903099,
0.));
#195786=CARTESIAN_POINT('Ctrl Pts',(-13.0270129211976,-19.1257591903099,
12.));
#195787=CARTESIAN_POINT('Ctrl Pts',(-13.0213436191328,-19.111292986631,
0.));
#195788=CARTESIAN_POINT('Ctrl Pts',(-13.0213436191328,-19.111292986631,
12.));
#195789=CARTESIAN_POINT('Ctrl Pts',(-13.0156847176097,-19.0969808131228,
0.));
#195790=CARTESIAN_POINT('Ctrl Pts',(-13.0156847176097,-19.0969808131228,
12.));
#195791=CARTESIAN_POINT('Ctrl Pts',(-13.0100374768788,-19.0828239070484,
0.));
#195792=CARTESIAN_POINT('Ctrl Pts',(-13.0100374768788,-19.0828239070484,
12.));
#195793=CARTESIAN_POINT('Ctrl Pts',(-13.0044031841382,-19.0688235289437,
0.));
#195794=CARTESIAN_POINT('Ctrl Pts',(-13.0044031841382,-19.0688235289437,
12.));
#195795=CARTESIAN_POINT('Ctrl Pts',(-12.9987831544502,-19.0549809634354,
0.));
#195796=CARTESIAN_POINT('Ctrl Pts',(-12.9987831544502,-19.0549809634354,
12.));
#195797=CARTESIAN_POINT('Ctrl Pts',(-12.9931787316514,-19.0412975200398,
0.));
#195798=CARTESIAN_POINT('Ctrl Pts',(-12.9931787316514,-19.0412975200398,
12.));
#195799=CARTESIAN_POINT('Ctrl Pts',(-12.9875912893003,-19.0277745339908,
0.));
#195800=CARTESIAN_POINT('Ctrl Pts',(-12.9875912893003,-19.0277745339908,
12.));
#195801=CARTESIAN_POINT('Ctrl Pts',(-12.9820222318716,-19.014413367335,
0.));
#195802=CARTESIAN_POINT('Ctrl Pts',(-12.9820222318716,-19.014413367335,
12.));
#195803=CARTESIAN_POINT('Ctrl Pts',(-12.9764729959206,-19.0012154099792,
0.));
#195804=CARTESIAN_POINT('Ctrl Pts',(-12.9764729959206,-19.0012154099792,
12.));
#195805=CARTESIAN_POINT('Ctrl Pts',(-12.9709450512747,-18.9881820807585,
0.));
#195806=CARTESIAN_POINT('Ctrl Pts',(-12.9709450512747,-18.9881820807585,
12.));
#195807=CARTESIAN_POINT('Ctrl Pts',(-12.9654399021868,-18.9753148284473,
0.));
#195808=CARTESIAN_POINT('Ctrl Pts',(-12.9654399021868,-18.9753148284473,
12.));
#195809=CARTESIAN_POINT('Ctrl Pts',(-12.9599590886318,-18.9626151329226,
0.));
#195810=CARTESIAN_POINT('Ctrl Pts',(-12.9599590886318,-18.9626151329226,
12.));
#195811=CARTESIAN_POINT('Ctrl Pts',(-12.9545041877377,-18.9500845064714,
0.));
#195812=CARTESIAN_POINT('Ctrl Pts',(-12.9545041877377,-18.9500845064714,
12.));
#195813=CARTESIAN_POINT('Ctrl Pts',(-12.9490768151821,-18.9377244950435,
0.));
#195814=CARTESIAN_POINT('Ctrl Pts',(-12.9490768151821,-18.9377244950435,
12.));
#195815=CARTESIAN_POINT('Ctrl Pts',(-12.9436786266106,-18.9255366795196,
0.));
#195816=CARTESIAN_POINT('Ctrl Pts',(-12.9436786266106,-18.9255366795196,
12.));
#195817=CARTESIAN_POINT('Ctrl Pts',(-12.9383113190375,-18.9135226769466,
0.));
#195818=CARTESIAN_POINT('Ctrl Pts',(-12.9383113190375,-18.9135226769466,
12.));
#195819=CARTESIAN_POINT('Ctrl Pts',(-12.9329766328184,-18.9016841423402,
0.));
#195820=CARTESIAN_POINT('Ctrl Pts',(-12.9329766328184,-18.9016841423402,
12.));
#195821=CARTESIAN_POINT('Ctrl Pts',(-12.9276763536373,-18.8900227704888,
0.));
#195822=CARTESIAN_POINT('Ctrl Pts',(-12.9276763536373,-18.8900227704888,
12.));
#195823=CARTESIAN_POINT('Ctrl Pts',(-12.9224123144982,-18.8785402977528,
0.));
#195824=CARTESIAN_POINT('Ctrl Pts',(-12.9224123144982,-18.8785402977528,
12.));
#195825=CARTESIAN_POINT('Ctrl Pts',(-12.9171863977047,-18.8672385038328,
0.));
#195826=CARTESIAN_POINT('Ctrl Pts',(-12.9171863977047,-18.8672385038328,
12.));
#195827=CARTESIAN_POINT('Ctrl Pts',(-12.9120005369066,-18.8561192136201,
0.));
#195828=CARTESIAN_POINT('Ctrl Pts',(-12.9120005369066,-18.8561192136201,
12.));
#195829=CARTESIAN_POINT('Ctrl Pts',(-12.9068567191856,-18.8451842990986,
0.));
#195830=CARTESIAN_POINT('Ctrl Pts',(-12.9068567191856,-18.8451842990986,
12.));
#195831=CARTESIAN_POINT('Ctrl Pts',(-12.9017569871738,-18.834435681259,
0.));
#195832=CARTESIAN_POINT('Ctrl Pts',(-12.9017569871738,-18.834435681259,
12.));
#195833=CARTESIAN_POINT('Ctrl Pts',(-12.8967034410752,-18.8238753319124,
0.));
#195834=CARTESIAN_POINT('Ctrl Pts',(-12.8967034410752,-18.8238753319124,
12.));
#195835=CARTESIAN_POINT('Ctrl Pts',(-12.8916982409931,-18.8135052757815,
0.));
#195836=CARTESIAN_POINT('Ctrl Pts',(-12.8916982409931,-18.8135052757815,
12.));
#195837=CARTESIAN_POINT('Ctrl Pts',(-12.8867436109543,-18.8033275941939,
0.));
#195838=CARTESIAN_POINT('Ctrl Pts',(-12.8867436109543,-18.8033275941939,
12.));
#195839=CARTESIAN_POINT('Ctrl Pts',(-12.8818418427474,-18.7933444285867,
0.));
#195840=CARTESIAN_POINT('Ctrl Pts',(-12.8818418427474,-18.7933444285867,
12.));
#195841=CARTESIAN_POINT('Ctrl Pts',(-12.8769952998097,-18.7835579840481,
0.));
#195842=CARTESIAN_POINT('Ctrl Pts',(-12.8769952998097,-18.7835579840481,
12.));
#195843=CARTESIAN_POINT('Ctrl Pts',(-12.8722064211814,-18.7739705329028,
0.));
#195844=CARTESIAN_POINT('Ctrl Pts',(-12.8722064211814,-18.7739705329028,
12.));
#195845=CARTESIAN_POINT('Ctrl Pts',(-12.8674777239656,-18.7645844169568,
0.));
#195846=CARTESIAN_POINT('Ctrl Pts',(-12.8674777239656,-18.7645844169568,
12.));
#195847=CARTESIAN_POINT('Ctrl Pts',(-12.8628118054172,-18.7554020493888,
0.));
#195848=CARTESIAN_POINT('Ctrl Pts',(-12.8628118054172,-18.7554020493888,
12.));
#195849=CARTESIAN_POINT('Ctrl Pts',(-12.8582113455645,-18.7464259171248,
0.));
#195850=CARTESIAN_POINT('Ctrl Pts',(-12.8582113455645,-18.7464259171248,
12.));
#195851=CARTESIAN_POINT('Ctrl Pts',(-12.8536791086315,-18.7376585820851,
0.));
#195852=CARTESIAN_POINT('Ctrl Pts',(-12.8536791086315,-18.7376585820851,
12.));
#195853=CARTESIAN_POINT('Ctrl Pts',(-12.849217951159,-18.7291026886552,
0.));
#195854=CARTESIAN_POINT('Ctrl Pts',(-12.849217951159,-18.7291026886552,
12.));
#195855=CARTESIAN_POINT('Ctrl Pts',(-12.8448308329494,-18.7207609737701,
0.));
#195856=CARTESIAN_POINT('Ctrl Pts',(-12.8448308329494,-18.7207609737701,
12.));
#195857=CARTESIAN_POINT('Ctrl Pts',(-12.8405208263432,-18.7126362754446,
0.));
#195858=CARTESIAN_POINT('Ctrl Pts',(-12.8405208263432,-18.7126362754446,
12.));
#195859=CARTESIAN_POINT('Ctrl Pts',(-12.8362911280362,-18.7047315436296,
0.));
#195860=CARTESIAN_POINT('Ctrl Pts',(-12.8362911280362,-18.7047315436296,
12.));
#195861=CARTESIAN_POINT('Ctrl Pts',(-12.832145059979,-18.6970498410173,
0.));
#195862=CARTESIAN_POINT('Ctrl Pts',(-12.832145059979,-18.6970498410173,
12.));
#195863=CARTESIAN_POINT('Ctrl Pts',(-12.8280860635231,-18.6895943376172,
0.));
#195864=CARTESIAN_POINT('Ctrl Pts',(-12.8280860635231,-18.6895943376172,
12.));
#195865=CARTESIAN_POINT('Ctrl Pts',(-12.8241176980016,-18.6823683094138,
0.));
#195866=CARTESIAN_POINT('Ctrl Pts',(-12.8241176980016,-18.6823683094138,
12.));
#195867=CARTESIAN_POINT('Ctrl Pts',(-12.8202436318473,-18.6753751301091,
0.));
#195868=CARTESIAN_POINT('Ctrl Pts',(-12.8202436318473,-18.6753751301091,
12.));
#195869=CARTESIAN_POINT('Ctrl Pts',(-12.8164676687361,-18.6686182952798,
0.));
#195870=CARTESIAN_POINT('Ctrl Pts',(-12.8164676687361,-18.6686182952798,
12.));
#195871=CARTESIAN_POINT('Ctrl Pts',(-12.8127937909632,-18.6621014624746,
0.));
#195872=CARTESIAN_POINT('Ctrl Pts',(-12.8127937909632,-18.6621014624746,
12.));
#195873=CARTESIAN_POINT('Ctrl Pts',(-12.8092261933858,-18.6558284825772,
0.));
#195874=CARTESIAN_POINT('Ctrl Pts',(-12.8092261933858,-18.6558284825772,
12.));
#195875=CARTESIAN_POINT('Ctrl Pts',(-12.805769331162,-18.6498034438986,
0.));
#195876=CARTESIAN_POINT('Ctrl Pts',(-12.805769331162,-18.6498034438986,
12.));
#195877=CARTESIAN_POINT('Ctrl Pts',(-12.8024278770153,-18.6440306327457,
0.));
#195878=CARTESIAN_POINT('Ctrl Pts',(-12.8024278770153,-18.6440306327457,
12.));
#195879=CARTESIAN_POINT('Ctrl Pts',(-12.7992066625264,-18.63851447924,0.));
#195880=CARTESIAN_POINT('Ctrl Pts',(-12.7992066625264,-18.63851447924,12.));
#195881=CARTESIAN_POINT('Ctrl Pts',(-12.7961106222251,-18.6332595057005,
0.));
#195882=CARTESIAN_POINT('Ctrl Pts',(-12.7961106222251,-18.6332595057005,
12.));
#195883=CARTESIAN_POINT('Ctrl Pts',(-12.7931447451556,-18.6282702819371,
0.));
#195884=CARTESIAN_POINT('Ctrl Pts',(-12.7931447451556,-18.6282702819371,
12.));
#195885=CARTESIAN_POINT('Ctrl Pts',(-12.7903142925235,-18.6235516265575,
0.));
#195886=CARTESIAN_POINT('Ctrl Pts',(-12.7903142925235,-18.6235516265575,
12.));
#195887=CARTESIAN_POINT('Ctrl Pts',(-12.7876249657834,-18.6191087624752,
0.));
#195888=CARTESIAN_POINT('Ctrl Pts',(-12.7876249657834,-18.6191087624752,
12.));
#195889=CARTESIAN_POINT('Ctrl Pts',(-12.78508316579,-18.6149475565189,0.));
#195890=CARTESIAN_POINT('Ctrl Pts',(-12.78508316579,-18.6149475565189,12.));
#195891=CARTESIAN_POINT('Ctrl Pts',(-12.7826959526924,-18.611074482622,
0.));
#195892=CARTESIAN_POINT('Ctrl Pts',(-12.7826959526924,-18.611074482622,
12.));
#195893=CARTESIAN_POINT('Ctrl Pts',(-12.7804705387658,-18.6074961535723,
0.));
#195894=CARTESIAN_POINT('Ctrl Pts',(-12.7804705387658,-18.6074961535723,
12.));
#195895=CARTESIAN_POINT('Ctrl Pts',(-12.7784139605067,-18.6042190183703,
0.));
#195896=CARTESIAN_POINT('Ctrl Pts',(-12.7784139605067,-18.6042190183703,
12.));
#195897=CARTESIAN_POINT('Ctrl Pts',(-12.7765325225083,-18.6012488486708,
0.));
#195898=CARTESIAN_POINT('Ctrl Pts',(-12.7765325225083,-18.6012488486708,
12.));
#195899=CARTESIAN_POINT('Ctrl Pts',(-12.7748328937639,-18.5985917525949,
0.));
#195900=CARTESIAN_POINT('Ctrl Pts',(-12.7748328937639,-18.5985917525949,
12.));
#195901=CARTESIAN_POINT('Ctrl Pts',(-12.7733231262107,-18.5962551167772,
0.));
#195902=CARTESIAN_POINT('Ctrl Pts',(-12.7733231262107,-18.5962551167772,
12.));
#195903=CARTESIAN_POINT('Ctrl Pts',(-12.7720142287169,-18.5942490615409,
0.));
#195904=CARTESIAN_POINT('Ctrl Pts',(-12.7720142287169,-18.5942490615409,
12.));
#195905=CARTESIAN_POINT('Ctrl Pts',(-12.7709195951154,-18.5925859134582,
0.));
#195906=CARTESIAN_POINT('Ctrl Pts',(-12.7709195951154,-18.5925859134582,
12.));
#195907=CARTESIAN_POINT('Ctrl Pts',(-12.7700520897174,-18.5912775137806,
0.));
#195908=CARTESIAN_POINT('Ctrl Pts',(-12.7700520897174,-18.5912775137806,
12.));
#195909=CARTESIAN_POINT('Ctrl Pts',(-12.7694215127923,-18.590332877722,
0.));
#195910=CARTESIAN_POINT('Ctrl Pts',(-12.7694215127923,-18.590332877722,
12.));
#195911=CARTESIAN_POINT('Ctrl Pts',(-12.7691103481996,-18.589871621842,
0.));
#195912=CARTESIAN_POINT('Ctrl Pts',(-12.7691103481996,-18.589871621842,
12.));
#195913=CARTESIAN_POINT('Ctrl Pts',(-12.7689864266924,-18.5896919669158,
0.));
#195914=CARTESIAN_POINT('Ctrl Pts',(-12.7689864266924,-18.5896919669158,
12.));
#195915=CARTESIAN_POINT('Ctrl Pts',(-12.7689524524484,-18.5896460962961,
0.));
#195916=CARTESIAN_POINT('Ctrl Pts',(-12.7689524524484,-18.5896460962961,
12.));
#195917=CARTESIAN_POINT('Ctrl Pts',(-12.7689476255363,-18.5896416359912,
0.));
#195918=CARTESIAN_POINT('Ctrl Pts',(-12.7689476255363,-18.5896416359912,
12.));
#195919=CARTESIAN_POINT('',(-13.5685075571671,-22.1787195904339,0.));
#195920=CARTESIAN_POINT('Ctrl Pts',(-13.5685075571671,-22.1787195904339,
0.));
#195921=CARTESIAN_POINT('Ctrl Pts',(-13.5683460612913,-22.1730081264583,
0.));
#195922=CARTESIAN_POINT('Ctrl Pts',(-13.5680170531724,-22.1615922804939,
0.));
#195923=CARTESIAN_POINT('Ctrl Pts',(-13.5675054918922,-22.1444897575076,
0.));
#195924=CARTESIAN_POINT('Ctrl Pts',(-13.5667873105179,-22.1217288871823,
0.));
#195925=CARTESIAN_POINT('Ctrl Pts',(-13.5658294169107,-22.0933486464442,
0.));
#195926=CARTESIAN_POINT('Ctrl Pts',(-13.5648113688895,-22.0650393089492,
0.));
#195927=CARTESIAN_POINT('Ctrl Pts',(-13.5637332022393,-22.0368009736227,
0.));
#195928=CARTESIAN_POINT('Ctrl Pts',(-13.5625949868313,-22.0086337943431,
0.));
#195929=CARTESIAN_POINT('Ctrl Pts',(-13.5613968357589,-21.9805379899192,
0.));
#195930=CARTESIAN_POINT('Ctrl Pts',(-13.5601389185315,-21.9525138592862,
0.));
#195931=CARTESIAN_POINT('Ctrl Pts',(-13.5588214586672,-21.9245617765827,
0.));
#195932=CARTESIAN_POINT('Ctrl Pts',(-13.5574447178485,-21.8966821688876,
0.));
#195933=CARTESIAN_POINT('Ctrl Pts',(-13.5560089839426,-21.8688754989401,
0.));
#195934=CARTESIAN_POINT('Ctrl Pts',(-13.5545145573049,-21.841142245609,
0.));
#195935=CARTESIAN_POINT('Ctrl Pts',(-13.5529617381569,-21.8134828857963,
0.));
#195936=CARTESIAN_POINT('Ctrl Pts',(-13.5513508127232,-21.7858978745848,
0.));
#195937=CARTESIAN_POINT('Ctrl Pts',(-13.5496820422187,-21.7583876294532,
0.));
#195938=CARTESIAN_POINT('Ctrl Pts',(-13.5479556704457,-21.730952541226,
0.));
#195939=CARTESIAN_POINT('Ctrl Pts',(-13.546171929503,-21.7035929822939,
0.));
#195940=CARTESIAN_POINT('Ctrl Pts',(-13.5443310461516,-21.676309315769,
0.));
#195941=CARTESIAN_POINT('Ctrl Pts',(-13.5424332480698,-21.6491019044647,
0.));
#195942=CARTESIAN_POINT('Ctrl Pts',(-13.5404787697798,-21.6219711193951,
0.));
#195943=CARTESIAN_POINT('Ctrl Pts',(-13.5384678597206,-21.5949173499022,
0.));
#195944=CARTESIAN_POINT('Ctrl Pts',(-13.5364007790292,-21.5679410019011,
0.));
#195945=CARTESIAN_POINT('Ctrl Pts',(-13.5342777983225,-21.5410424932511,
0.));
#195946=CARTESIAN_POINT('Ctrl Pts',(-13.5320991952145,-21.5142222501671,
0.));
#195947=CARTESIAN_POINT('Ctrl Pts',(-13.5298652514357,-21.487480703047,
0.));
#195948=CARTESIAN_POINT('Ctrl Pts',(-13.5275762503553,-21.4608182828695,
0.));
#195949=CARTESIAN_POINT('Ctrl Pts',(-13.5252324737795,-21.4342354165253,
0.));
#195950=CARTESIAN_POINT('Ctrl Pts',(-13.5228342013508,-21.4077325259318,
0.));
#195951=CARTESIAN_POINT('Ctrl Pts',(-13.5203817122497,-21.3813100304967,
0.));
#195952=CARTESIAN_POINT('Ctrl Pts',(-13.5178752862461,-21.3549683486219,
0.));
#195953=CARTESIAN_POINT('Ctrl Pts',(-13.5153152050554,-21.328707899634,
0.));
#195954=CARTESIAN_POINT('Ctrl Pts',(-13.5127017534972,-21.3025291054236,
0.));
#195955=CARTESIAN_POINT('Ctrl Pts',(-13.5100352209207,-21.2764323924442,
0.));
#195956=CARTESIAN_POINT('Ctrl Pts',(-13.5073159019454,-21.2504181927429,
0.));
#195957=CARTESIAN_POINT('Ctrl Pts',(-13.5045440957404,-21.224486942933,
0.));
#195958=CARTESIAN_POINT('Ctrl Pts',(-13.5017201056088,-21.1986390835825,
0.));
#195959=CARTESIAN_POINT('Ctrl Pts',(-13.4988442384491,-21.1728750584173,
0.));
#195960=CARTESIAN_POINT('Ctrl Pts',(-13.4959168042934,-21.1471953136209,
0.));
#195961=CARTESIAN_POINT('Ctrl Pts',(-13.4929381157778,-21.1216002970209,
0.));
#195962=CARTESIAN_POINT('Ctrl Pts',(-13.4899084877718,-21.0960904575048,
0.));
#195963=CARTESIAN_POINT('Ctrl Pts',(-13.4868282377192,-21.0706662455202,
0.));
#195964=CARTESIAN_POINT('Ctrl Pts',(-13.4836976858912,-21.0453281134247,
0.));
#195965=CARTESIAN_POINT('Ctrl Pts',(-13.4805171556822,-21.0200765158885,
0.));
#195966=CARTESIAN_POINT('Ctrl Pts',(-13.4772869738879,-20.9949119102592,
0.));
#195967=CARTESIAN_POINT('Ctrl Pts',(-13.4740074710087,-20.9698347569476,
0.));
#195968=CARTESIAN_POINT('Ctrl Pts',(-13.4706789815167,-20.9448455197557,
0.));
#195969=CARTESIAN_POINT('Ctrl Pts',(-13.4673018437718,-20.9199446657584,
0.));
#195970=CARTESIAN_POINT('Ctrl Pts',(-13.4638763999726,-20.8951326652158,
0.));
#195971=CARTESIAN_POINT('Ctrl Pts',(-13.4604029960983,-20.8704099914641,
0.));
#195972=CARTESIAN_POINT('Ctrl Pts',(-13.4568819818631,-20.8457771208082,
0.));
#195973=CARTESIAN_POINT('Ctrl Pts',(-13.4533137106667,-20.821234532398,
0.));
#195974=CARTESIAN_POINT('Ctrl Pts',(-13.4496985395637,-20.7967827081227,
0.));
#195975=CARTESIAN_POINT('Ctrl Pts',(-13.4460368293688,-20.7724221327608,
0.));
#195976=CARTESIAN_POINT('Ctrl Pts',(-13.4423289447561,-20.7481532941013,
0.));
#195977=CARTESIAN_POINT('Ctrl Pts',(-13.4385752543663,-20.7239766830675,
0.));
#195978=CARTESIAN_POINT('Ctrl Pts',(-13.4347761309154,-20.6998927938288,
0.));
#195979=CARTESIAN_POINT('Ctrl Pts',(-13.4309319513119,-20.6759021239103,
0.));
#195980=CARTESIAN_POINT('Ctrl Pts',(-13.4270430967652,-20.6520051742869,
0.));
#195981=CARTESIAN_POINT('Ctrl Pts',(-13.4231099528179,-20.6282024494237,
0.));
#195982=CARTESIAN_POINT('Ctrl Pts',(-13.4191329093933,-20.6044944573153,
0.));
#195983=CARTESIAN_POINT('Ctrl Pts',(-13.4151123608411,-20.5808817095155,
0.));
#195984=CARTESIAN_POINT('Ctrl Pts',(-13.4110487059912,-20.5573647211639,
0.));
#195985=CARTESIAN_POINT('Ctrl Pts',(-13.4069423482076,-20.5339440109956,
0.));
#195986=CARTESIAN_POINT('Ctrl Pts',(-13.4027936954529,-20.5106201013753,
0.));
#195987=CARTESIAN_POINT('Ctrl Pts',(-13.3986031603716,-20.487393518404,
0.));
#195988=CARTESIAN_POINT('Ctrl Pts',(-13.3943711603739,-20.4642647920037,
0.));
#195989=CARTESIAN_POINT('Ctrl Pts',(-13.3900981177255,-20.4412344560007,
0.));
#195990=CARTESIAN_POINT('Ctrl Pts',(-13.3857844596387,-20.4183030482002,
0.));
#195991=CARTESIAN_POINT('Ctrl Pts',(-13.3814306183719,-20.3954711104502,
0.));
#195992=CARTESIAN_POINT('Ctrl Pts',(-13.3770370313188,-20.3727391887184,
0.));
#195993=CARTESIAN_POINT('Ctrl Pts',(-13.3726041410867,-20.3501078331814,
0.));
#195994=CARTESIAN_POINT('Ctrl Pts',(-13.3681323955826,-20.3275775983029,
0.));
#195995=CARTESIAN_POINT('Ctrl Pts',(-13.3636222481016,-20.3051490429048,
0.));
#195996=CARTESIAN_POINT('Ctrl Pts',(-13.3590741574195,-20.2828227302339,
0.));
#195997=CARTESIAN_POINT('Ctrl Pts',(-13.3544885878889,-20.2605992280122,
0.));
#195998=CARTESIAN_POINT('Ctrl Pts',(-13.3498660095386,-20.2384791085359,
0.));
#195999=CARTESIAN_POINT('Ctrl Pts',(-13.3452068981766,-20.216462948786,
0.));
#196000=CARTESIAN_POINT('Ctrl Pts',(-13.3405117354971,-20.1945513305235,
0.));
#196001=CARTESIAN_POINT('Ctrl Pts',(-13.3357810091903,-20.1727448403817,
0.));
#196002=CARTESIAN_POINT('Ctrl Pts',(-13.3310152130564,-20.1510440699474,
0.));
#196003=CARTESIAN_POINT('Ctrl Pts',(-13.3262148471226,-20.1294496158402,
0.));
#196004=CARTESIAN_POINT('Ctrl Pts',(-13.3213804177587,-20.1079620798375,
0.));
#196005=CARTESIAN_POINT('Ctrl Pts',(-13.3165124377963,-20.0865820689882,
0.));
#196006=CARTESIAN_POINT('Ctrl Pts',(-13.3116114266515,-20.0653101957188,
0.));
#196007=CARTESIAN_POINT('Ctrl Pts',(-13.3066779104515,-20.0441470779345,
0.));
#196008=CARTESIAN_POINT('Ctrl Pts',(-13.3017124221637,-20.0230933391038,
0.));
#196009=CARTESIAN_POINT('Ctrl Pts',(-13.2967155017306,-20.0021496083738,
0.));
#196010=CARTESIAN_POINT('Ctrl Pts',(-13.2916876962094,-19.981316520717,
0.));
#196011=CARTESIAN_POINT('Ctrl Pts',(-13.286629559915,-19.9605947170586,
0.));
#196012=CARTESIAN_POINT('Ctrl Pts',(-13.2815416545663,-19.9399848444019,
0.));
#196013=CARTESIAN_POINT('Ctrl Pts',(-13.2764245494357,-19.9194875559422,
0.));
#196014=CARTESIAN_POINT('Ctrl Pts',(-13.271278821502,-19.8991035111745,
0.));
#196015=CARTESIAN_POINT('Ctrl Pts',(-13.2661050556132,-19.8788333760577,
0.));
#196016=CARTESIAN_POINT('Ctrl Pts',(-13.2609038446529,-19.8586778231715,
0.));
#196017=CARTESIAN_POINT('Ctrl Pts',(-13.2556757897086,-19.8386375318634,
0.));
#196018=CARTESIAN_POINT('Ctrl Pts',(-13.2504215002457,-19.8187131883917,
0.));
#196019=CARTESIAN_POINT('Ctrl Pts',(-13.2451415942805,-19.7989054860495,
0.));
#196020=CARTESIAN_POINT('Ctrl Pts',(-13.2398366985675,-19.7792151253289,
0.));
#196021=CARTESIAN_POINT('Ctrl Pts',(-13.2345074487963,-19.7596428141168,
0.));
#196022=CARTESIAN_POINT('Ctrl Pts',(-13.2291544897899,-19.7401892678697,
0.));
#196023=CARTESIAN_POINT('Ctrl Pts',(-13.2237784757066,-19.7208552097868,
0.));
#196024=CARTESIAN_POINT('Ctrl Pts',(-13.2183800702436,-19.7016413709685,
0.));
#196025=CARTESIAN_POINT('Ctrl Pts',(-13.2129599468485,-19.6825484905823,
0.));
#196026=CARTESIAN_POINT('Ctrl Pts',(-13.2075187889529,-19.6635773160936,
0.));
#196027=CARTESIAN_POINT('Ctrl Pts',(-13.2020572902065,-19.6447286034772,
0.));
#196028=CARTESIAN_POINT('Ctrl Pts',(-13.1965761547151,-19.6260031174244,
0.));
#196029=CARTESIAN_POINT('Ctrl Pts',(-13.1910760972814,-19.6074016315414,
0.));
#196030=CARTESIAN_POINT('Ctrl Pts',(-13.1855578436471,-19.5889249285338,
0.));
#196031=CARTESIAN_POINT('Ctrl Pts',(-13.1800221307673,-19.5705738004667,
0.));
#196032=CARTESIAN_POINT('Ctrl Pts',(-13.1744697070911,-19.5523490490244,
0.));
#196033=CARTESIAN_POINT('Ctrl Pts',(-13.1689013328431,-19.5342514857562,
0.));
#196034=CARTESIAN_POINT('Ctrl Pts',(-13.1633177803101,-19.5162819323213,
0.));
#196035=CARTESIAN_POINT('Ctrl Pts',(-13.1577198341245,-19.4984412207081,
0.));
#196036=CARTESIAN_POINT('Ctrl Pts',(-13.1521082915853,-19.4807301935268,
0.));
#196037=CARTESIAN_POINT('Ctrl Pts',(-13.1464839629971,-19.4631497043258,
0.));
#196038=CARTESIAN_POINT('Ctrl Pts',(-13.1408476720061,-19.4457006178876,
0.));
#196039=CARTESIAN_POINT('Ctrl Pts',(-13.1352002559438,-19.4283838105262,
0.));
#196040=CARTESIAN_POINT('Ctrl Pts',(-13.1295425661634,-19.4112001703557,
0.));
#196041=CARTESIAN_POINT('Ctrl Pts',(-13.1238754684177,-19.3941505976263,
0.));
#196042=CARTESIAN_POINT('Ctrl Pts',(-13.118199843271,-19.3772360051091,
0.));
#196043=CARTESIAN_POINT('Ctrl Pts',(-13.1125165865022,-19.3604573184515,
0.));
#196044=CARTESIAN_POINT('Ctrl Pts',(-13.1068266095186,-19.3438154765395,
0.));
#196045=CARTESIAN_POINT('Ctrl Pts',(-13.1011308397591,-19.3273114318269,
0.));
#196046=CARTESIAN_POINT('Ctrl Pts',(-13.0954302211479,-19.310946150736,
0.));
#196047=CARTESIAN_POINT('Ctrl Pts',(-13.0897257145969,-19.2947206141247,
0.));
#196048=CARTESIAN_POINT('Ctrl Pts',(-13.0840182984949,-19.2786358177198,
0.));
#196049=CARTESIAN_POINT('Ctrl Pts',(-13.0783089692118,-19.2626927725596,
0.));
#196050=CARTESIAN_POINT('Ctrl Pts',(-13.0725987415859,-19.2468925053989,
0.));
#196051=CARTESIAN_POINT('Ctrl Pts',(-13.0668886494795,-19.2312360592033,
0.));
#196052=CARTESIAN_POINT('Ctrl Pts',(-13.0611797463915,-19.2157244937142,
0.));
#196053=CARTESIAN_POINT('Ctrl Pts',(-13.0554731060538,-19.2003588859772,
0.));
#196054=CARTESIAN_POINT('Ctrl Pts',(-13.0497698230441,-19.1851403308825,
0.));
#196055=CARTESIAN_POINT('Ctrl Pts',(-13.0440710133772,-19.1700699416622,
0.));
#196056=CARTESIAN_POINT('Ctrl Pts',(-13.0383778152068,-19.155148850523,
0.));
#196057=CARTESIAN_POINT('Ctrl Pts',(-13.0326913895838,-19.1403782093386,
0.));
#196058=CARTESIAN_POINT('Ctrl Pts',(-13.0270129211976,-19.1257591903099,
0.));
#196059=CARTESIAN_POINT('Ctrl Pts',(-13.0213436191328,-19.111292986631,
0.));
#196060=CARTESIAN_POINT('Ctrl Pts',(-13.0156847176097,-19.0969808131228,
0.));
#196061=CARTESIAN_POINT('Ctrl Pts',(-13.0100374768788,-19.0828239070484,
0.));
#196062=CARTESIAN_POINT('Ctrl Pts',(-13.0044031841382,-19.0688235289437,
0.));
#196063=CARTESIAN_POINT('Ctrl Pts',(-12.9987831544502,-19.0549809634354,
0.));
#196064=CARTESIAN_POINT('Ctrl Pts',(-12.9931787316514,-19.0412975200398,
0.));
#196065=CARTESIAN_POINT('Ctrl Pts',(-12.9875912893003,-19.0277745339908,
0.));
#196066=CARTESIAN_POINT('Ctrl Pts',(-12.9820222318716,-19.014413367335,
0.));
#196067=CARTESIAN_POINT('Ctrl Pts',(-12.9764729959206,-19.0012154099792,
0.));
#196068=CARTESIAN_POINT('Ctrl Pts',(-12.9709450512747,-18.9881820807585,
0.));
#196069=CARTESIAN_POINT('Ctrl Pts',(-12.9654399021868,-18.9753148284473,
0.));
#196070=CARTESIAN_POINT('Ctrl Pts',(-12.9599590886318,-18.9626151329226,
0.));
#196071=CARTESIAN_POINT('Ctrl Pts',(-12.9545041877377,-18.9500845064714,
0.));
#196072=CARTESIAN_POINT('Ctrl Pts',(-12.9490768151821,-18.9377244950435,
0.));
#196073=CARTESIAN_POINT('Ctrl Pts',(-12.9436786266106,-18.9255366795196,
0.));
#196074=CARTESIAN_POINT('Ctrl Pts',(-12.9383113190375,-18.9135226769466,
0.));
#196075=CARTESIAN_POINT('Ctrl Pts',(-12.9329766328184,-18.9016841423402,
0.));
#196076=CARTESIAN_POINT('Ctrl Pts',(-12.9276763536373,-18.8900227704888,
0.));
#196077=CARTESIAN_POINT('Ctrl Pts',(-12.9224123144982,-18.8785402977528,
0.));
#196078=CARTESIAN_POINT('Ctrl Pts',(-12.9171863977047,-18.8672385038328,
0.));
#196079=CARTESIAN_POINT('Ctrl Pts',(-12.9120005369066,-18.8561192136201,
0.));
#196080=CARTESIAN_POINT('Ctrl Pts',(-12.9068567191856,-18.8451842990986,
0.));
#196081=CARTESIAN_POINT('Ctrl Pts',(-12.9017569871738,-18.834435681259,
0.));
#196082=CARTESIAN_POINT('Ctrl Pts',(-12.8967034410752,-18.8238753319124,
0.));
#196083=CARTESIAN_POINT('Ctrl Pts',(-12.8916982409931,-18.8135052757815,
0.));
#196084=CARTESIAN_POINT('Ctrl Pts',(-12.8867436109543,-18.8033275941939,
0.));
#196085=CARTESIAN_POINT('Ctrl Pts',(-12.8818418427474,-18.7933444285867,
0.));
#196086=CARTESIAN_POINT('Ctrl Pts',(-12.8769952998097,-18.7835579840481,
0.));
#196087=CARTESIAN_POINT('Ctrl Pts',(-12.8722064211814,-18.7739705329028,
0.));
#196088=CARTESIAN_POINT('Ctrl Pts',(-12.8674777239656,-18.7645844169568,
0.));
#196089=CARTESIAN_POINT('Ctrl Pts',(-12.8628118054172,-18.7554020493888,
0.));
#196090=CARTESIAN_POINT('Ctrl Pts',(-12.8582113455645,-18.7464259171248,
0.));
#196091=CARTESIAN_POINT('Ctrl Pts',(-12.8536791086315,-18.7376585820851,
0.));
#196092=CARTESIAN_POINT('Ctrl Pts',(-12.849217951159,-18.7291026886552,
0.));
#196093=CARTESIAN_POINT('Ctrl Pts',(-12.8448308329494,-18.7207609737701,
0.));
#196094=CARTESIAN_POINT('Ctrl Pts',(-12.8405208263432,-18.7126362754446,
0.));
#196095=CARTESIAN_POINT('Ctrl Pts',(-12.8362911280362,-18.7047315436296,
0.));
#196096=CARTESIAN_POINT('Ctrl Pts',(-12.832145059979,-18.6970498410173,
0.));
#196097=CARTESIAN_POINT('Ctrl Pts',(-12.8280860635231,-18.6895943376172,
0.));
#196098=CARTESIAN_POINT('Ctrl Pts',(-12.8241176980016,-18.6823683094138,
0.));
#196099=CARTESIAN_POINT('Ctrl Pts',(-12.8202436318473,-18.6753751301091,
0.));
#196100=CARTESIAN_POINT('Ctrl Pts',(-12.8164676687361,-18.6686182952798,
0.));
#196101=CARTESIAN_POINT('Ctrl Pts',(-12.8127937909632,-18.6621014624746,
0.));
#196102=CARTESIAN_POINT('Ctrl Pts',(-12.8092261933858,-18.6558284825772,
0.));
#196103=CARTESIAN_POINT('Ctrl Pts',(-12.805769331162,-18.6498034438986,
0.));
#196104=CARTESIAN_POINT('Ctrl Pts',(-12.8024278770153,-18.6440306327457,
0.));
#196105=CARTESIAN_POINT('Ctrl Pts',(-12.7992066625264,-18.63851447924,0.));
#196106=CARTESIAN_POINT('Ctrl Pts',(-12.7961106222251,-18.6332595057005,
0.));
#196107=CARTESIAN_POINT('Ctrl Pts',(-12.7931447451556,-18.6282702819371,
0.));
#196108=CARTESIAN_POINT('Ctrl Pts',(-12.7903142925235,-18.6235516265575,
0.));
#196109=CARTESIAN_POINT('Ctrl Pts',(-12.7876249657834,-18.6191087624752,
0.));
#196110=CARTESIAN_POINT('Ctrl Pts',(-12.78508316579,-18.6149475565189,0.));
#196111=CARTESIAN_POINT('Ctrl Pts',(-12.7826959526924,-18.611074482622,
0.));
#196112=CARTESIAN_POINT('Ctrl Pts',(-12.7804705387658,-18.6074961535723,
0.));
#196113=CARTESIAN_POINT('Ctrl Pts',(-12.7784139605067,-18.6042190183703,
0.));
#196114=CARTESIAN_POINT('Ctrl Pts',(-12.7765325225083,-18.6012488486708,
0.));
#196115=CARTESIAN_POINT('Ctrl Pts',(-12.7748328937639,-18.5985917525949,
0.));
#196116=CARTESIAN_POINT('Ctrl Pts',(-12.7733231262107,-18.5962551167772,
0.));
#196117=CARTESIAN_POINT('Ctrl Pts',(-12.7720142287169,-18.5942490615409,
0.));
#196118=CARTESIAN_POINT('Ctrl Pts',(-12.7709195951154,-18.5925859134582,
0.));
#196119=CARTESIAN_POINT('Ctrl Pts',(-12.7700520897174,-18.5912775137806,
0.));
#196120=CARTESIAN_POINT('Ctrl Pts',(-12.7694215127923,-18.590332877722,
0.));
#196121=CARTESIAN_POINT('Ctrl Pts',(-12.7691103481996,-18.589871621842,
0.));
#196122=CARTESIAN_POINT('Ctrl Pts',(-12.7689864266924,-18.5896919669158,
0.));
#196123=CARTESIAN_POINT('Ctrl Pts',(-12.7689524524484,-18.5896460962961,
0.));
#196124=CARTESIAN_POINT('Ctrl Pts',(-12.7689476255363,-18.5896416359912,
0.));
#196125=CARTESIAN_POINT('',(-13.5685075571671,-22.1787195904339,0.));
#196126=CARTESIAN_POINT('Ctrl Pts',(-14.6513681262571,-17.1452095830632,
0.));
#196127=CARTESIAN_POINT('Ctrl Pts',(-14.6513681262571,-17.1452095830632,
12.));
#196128=CARTESIAN_POINT('Ctrl Pts',(-14.6513711852843,-17.1452153999142,
0.));
#196129=CARTESIAN_POINT('Ctrl Pts',(-14.6513711852843,-17.1452153999142,
12.));
#196130=CARTESIAN_POINT('Ctrl Pts',(-14.6514066997196,-17.1452600887037,
0.));
#196131=CARTESIAN_POINT('Ctrl Pts',(-14.6514066997196,-17.1452600887037,
12.));
#196132=CARTESIAN_POINT('Ctrl Pts',(-14.6515481598068,-17.1454262858043,
0.));
#196133=CARTESIAN_POINT('Ctrl Pts',(-14.6515481598068,-17.1454262858043,
12.));
#196134=CARTESIAN_POINT('Ctrl Pts',(-14.6519131634508,-17.1458462295271,
0.));
#196135=CARTESIAN_POINT('Ctrl Pts',(-14.6519131634508,-17.1458462295271,
12.));
#196136=CARTESIAN_POINT('Ctrl Pts',(-14.6526624064978,-17.1466998098673,
0.));
#196137=CARTESIAN_POINT('Ctrl Pts',(-14.6526624064978,-17.1466998098673,
12.));
#196138=CARTESIAN_POINT('Ctrl Pts',(-14.6537016966184,-17.147876394491,
0.));
#196139=CARTESIAN_POINT('Ctrl Pts',(-14.6537016966184,-17.147876394491,
12.));
#196140=CARTESIAN_POINT('Ctrl Pts',(-14.655024862281,-17.1493641837558,
0.));
#196141=CARTESIAN_POINT('Ctrl Pts',(-14.655024862281,-17.1493641837558,
12.));
#196142=CARTESIAN_POINT('Ctrl Pts',(-14.6566237952435,-17.1511476869496,
0.));
#196143=CARTESIAN_POINT('Ctrl Pts',(-14.6566237952435,-17.1511476869496,
12.));
#196144=CARTESIAN_POINT('Ctrl Pts',(-14.6584900555302,-17.1532107762718,
0.));
#196145=CARTESIAN_POINT('Ctrl Pts',(-14.6584900555302,-17.1532107762718,
12.));
#196146=CARTESIAN_POINT('Ctrl Pts',(-14.6606167169642,-17.1555401986401,
0.));
#196147=CARTESIAN_POINT('Ctrl Pts',(-14.6606167169642,-17.1555401986401,
12.));
#196148=CARTESIAN_POINT('Ctrl Pts',(-14.6629987285992,-17.1581262646789,
0.));
#196149=CARTESIAN_POINT('Ctrl Pts',(-14.6629987285992,-17.1581262646789,
12.));
#196150=CARTESIAN_POINT('Ctrl Pts',(-14.6656319165057,-17.1609609517369,
0.));
#196151=CARTESIAN_POINT('Ctrl Pts',(-14.6656319165057,-17.1609609517369,
12.));
#196152=CARTESIAN_POINT('Ctrl Pts',(-14.6685123374423,-17.1640366762305,
0.));
#196153=CARTESIAN_POINT('Ctrl Pts',(-14.6685123374423,-17.1640366762305,
12.));
#196154=CARTESIAN_POINT('Ctrl Pts',(-14.671635583332,-17.167344972302,0.));
#196155=CARTESIAN_POINT('Ctrl Pts',(-14.671635583332,-17.167344972302,12.));
#196156=CARTESIAN_POINT('Ctrl Pts',(-14.6749971333867,-17.1708771619129,
0.));
#196157=CARTESIAN_POINT('Ctrl Pts',(-14.6749971333867,-17.1708771619129,
12.));
#196158=CARTESIAN_POINT('Ctrl Pts',(-14.6785925615677,-17.1746247499056,
0.));
#196159=CARTESIAN_POINT('Ctrl Pts',(-14.6785925615677,-17.1746247499056,
12.));
#196160=CARTESIAN_POINT('Ctrl Pts',(-14.6824178576167,-17.1785800350826,
0.));
#196161=CARTESIAN_POINT('Ctrl Pts',(-14.6824178576167,-17.1785800350826,
12.));
#196162=CARTESIAN_POINT('Ctrl Pts',(-14.686469452232,-17.1827361584719,
0.));
#196163=CARTESIAN_POINT('Ctrl Pts',(-14.686469452232,-17.1827361584719,
12.));
#196164=CARTESIAN_POINT('Ctrl Pts',(-14.6907440526958,-17.1870867909918,
0.));
#196165=CARTESIAN_POINT('Ctrl Pts',(-14.6907440526958,-17.1870867909918,
12.));
#196166=CARTESIAN_POINT('Ctrl Pts',(-14.6952385361706,-17.1916259308415,
0.));
#196167=CARTESIAN_POINT('Ctrl Pts',(-14.6952385361706,-17.1916259308415,
12.));
#196168=CARTESIAN_POINT('Ctrl Pts',(-14.699949811582,-17.1963476411694,
0.));
#196169=CARTESIAN_POINT('Ctrl Pts',(-14.699949811582,-17.1963476411694,
12.));
#196170=CARTESIAN_POINT('Ctrl Pts',(-14.7048748502663,-17.2012461084268,
0.));
#196171=CARTESIAN_POINT('Ctrl Pts',(-14.7048748502663,-17.2012461084268,
12.));
#196172=CARTESIAN_POINT('Ctrl Pts',(-14.7100107213586,-17.2063157097315,
0.));
#196173=CARTESIAN_POINT('Ctrl Pts',(-14.7100107213586,-17.2063157097315,
12.));
#196174=CARTESIAN_POINT('Ctrl Pts',(-14.7153546289339,-17.2115510835989,
0.));
#196175=CARTESIAN_POINT('Ctrl Pts',(-14.7153546289339,-17.2115510835989,
12.));
#196176=CARTESIAN_POINT('Ctrl Pts',(-14.7209039390327,-17.2169471814256,
0.));
#196177=CARTESIAN_POINT('Ctrl Pts',(-14.7209039390327,-17.2169471814256,
12.));
#196178=CARTESIAN_POINT('Ctrl Pts',(-14.7266561494282,-17.2224992099666,
0.));
#196179=CARTESIAN_POINT('Ctrl Pts',(-14.7266561494282,-17.2224992099666,
12.));
#196180=CARTESIAN_POINT('Ctrl Pts',(-14.7326088681163,-17.2282025904314,
0.));
#196181=CARTESIAN_POINT('Ctrl Pts',(-14.7326088681163,-17.2282025904314,
12.));
#196182=CARTESIAN_POINT('Ctrl Pts',(-14.7387597858117,-17.2340529062076,
0.));
#196183=CARTESIAN_POINT('Ctrl Pts',(-14.7387597858117,-17.2340529062076,
12.));
#196184=CARTESIAN_POINT('Ctrl Pts',(-14.7451066593792,-17.2400458713565,
0.));
#196185=CARTESIAN_POINT('Ctrl Pts',(-14.7451066593792,-17.2400458713565,
12.));
#196186=CARTESIAN_POINT('Ctrl Pts',(-14.7516473175124,-17.2461773413288,
0.));
#196187=CARTESIAN_POINT('Ctrl Pts',(-14.7516473175124,-17.2461773413288,
12.));
#196188=CARTESIAN_POINT('Ctrl Pts',(-14.7583796616617,-17.2524433146837,
0.));
#196189=CARTESIAN_POINT('Ctrl Pts',(-14.7583796616617,-17.2524433146837,
12.));
#196190=CARTESIAN_POINT('Ctrl Pts',(-14.7653016697591,-17.2588399401465,
0.));
#196191=CARTESIAN_POINT('Ctrl Pts',(-14.7653016697591,-17.2588399401465,
12.));
#196192=CARTESIAN_POINT('Ctrl Pts',(-14.7724113956731,-17.2653635155319,
0.));
#196193=CARTESIAN_POINT('Ctrl Pts',(-14.7724113956731,-17.2653635155319,
12.));
#196194=CARTESIAN_POINT('Ctrl Pts',(-14.7797069617804,-17.2720104735194,
0.));
#196195=CARTESIAN_POINT('Ctrl Pts',(-14.7797069617804,-17.2720104735194,
12.));
#196196=CARTESIAN_POINT('Ctrl Pts',(-14.787186553128,-17.2787773704849,
0.));
#196197=CARTESIAN_POINT('Ctrl Pts',(-14.787186553128,-17.2787773704849,
12.));
#196198=CARTESIAN_POINT('Ctrl Pts',(-14.7948484105249,-17.2856608733196,
0.));
#196199=CARTESIAN_POINT('Ctrl Pts',(-14.7948484105249,-17.2856608733196,
12.));
#196200=CARTESIAN_POINT('Ctrl Pts',(-14.8026908254276,-17.2926577496513,
0.));
#196201=CARTESIAN_POINT('Ctrl Pts',(-14.8026908254276,-17.2926577496513,
12.));
#196202=CARTESIAN_POINT('Ctrl Pts',(-14.8107121391036,-17.299764866148,
0.));
#196203=CARTESIAN_POINT('Ctrl Pts',(-14.8107121391036,-17.299764866148,
12.));
#196204=CARTESIAN_POINT('Ctrl Pts',(-14.8189107410162,-17.3069791853706,
0.));
#196205=CARTESIAN_POINT('Ctrl Pts',(-14.8189107410162,-17.3069791853706,
12.));
#196206=CARTESIAN_POINT('Ctrl Pts',(-14.8272850675379,-17.3142977632659,
0.));
#196207=CARTESIAN_POINT('Ctrl Pts',(-14.8272850675379,-17.3142977632659,
12.));
#196208=CARTESIAN_POINT('Ctrl Pts',(-14.8358336004197,-17.3217177462101,
0.));
#196209=CARTESIAN_POINT('Ctrl Pts',(-14.8358336004197,-17.3217177462101,
12.));
#196210=CARTESIAN_POINT('Ctrl Pts',(-14.8445548643508,-17.3292363662605,
0.));
#196211=CARTESIAN_POINT('Ctrl Pts',(-14.8445548643508,-17.3292363662605,
12.));
#196212=CARTESIAN_POINT('Ctrl Pts',(-14.8534474245434,-17.336850936485,
0.));
#196213=CARTESIAN_POINT('Ctrl Pts',(-14.8534474245434,-17.336850936485,
12.));
#196214=CARTESIAN_POINT('Ctrl Pts',(-14.8625098843417,-17.3445588463474,
0.));
#196215=CARTESIAN_POINT('Ctrl Pts',(-14.8625098843417,-17.3445588463474,
12.));
#196216=CARTESIAN_POINT('Ctrl Pts',(-14.8717408826956,-17.3523575568645,
0.));
#196217=CARTESIAN_POINT('Ctrl Pts',(-14.8717408826956,-17.3523575568645,
12.));
#196218=CARTESIAN_POINT('Ctrl Pts',(-14.8811390927423,-17.3602445978161,
0.));
#196219=CARTESIAN_POINT('Ctrl Pts',(-14.8811390927423,-17.3602445978161,
12.));
#196220=CARTESIAN_POINT('Ctrl Pts',(-14.8907032205788,-17.3682175653235,
0.));
#196221=CARTESIAN_POINT('Ctrl Pts',(-14.8907032205788,-17.3682175653235,
12.));
#196222=CARTESIAN_POINT('Ctrl Pts',(-14.900432003961,-17.3762741193076,
0.));
#196223=CARTESIAN_POINT('Ctrl Pts',(-14.900432003961,-17.3762741193076,
12.));
#196224=CARTESIAN_POINT('Ctrl Pts',(-14.9103242110058,-17.3844119809824,
0.));
#196225=CARTESIAN_POINT('Ctrl Pts',(-14.9103242110058,-17.3844119809824,
12.));
#196226=CARTESIAN_POINT('Ctrl Pts',(-14.9203786389342,-17.3926289303986,
0.));
#196227=CARTESIAN_POINT('Ctrl Pts',(-14.9203786389342,-17.3926289303986,
12.));
#196228=CARTESIAN_POINT('Ctrl Pts',(-14.9305941128757,-17.4009228040749,
0.));
#196229=CARTESIAN_POINT('Ctrl Pts',(-14.9305941128757,-17.4009228040749,
12.));
#196230=CARTESIAN_POINT('Ctrl Pts',(-14.940969484645,-17.4092914926071,
0.));
#196231=CARTESIAN_POINT('Ctrl Pts',(-14.940969484645,-17.4092914926071,
12.));
#196232=CARTESIAN_POINT('Ctrl Pts',(-14.9515036315143,-17.4177329382828,
0.));
#196233=CARTESIAN_POINT('Ctrl Pts',(-14.9515036315143,-17.4177329382828,
12.));
#196234=CARTESIAN_POINT('Ctrl Pts',(-14.9621954549827,-17.426245132709,
0.));
#196235=CARTESIAN_POINT('Ctrl Pts',(-14.9621954549827,-17.426245132709,
12.));
#196236=CARTESIAN_POINT('Ctrl Pts',(-14.9730438799452,-17.4348261151396,
0.));
#196237=CARTESIAN_POINT('Ctrl Pts',(-14.9730438799452,-17.4348261151396,
12.));
#196238=CARTESIAN_POINT('Ctrl Pts',(-14.9840478538358,-17.4434739707773,
0.));
#196239=CARTESIAN_POINT('Ctrl Pts',(-14.9840478538358,-17.4434739707773,
12.));
#196240=CARTESIAN_POINT('Ctrl Pts',(-14.9952063457778,-17.4521868291004,
0.));
#196241=CARTESIAN_POINT('Ctrl Pts',(-14.9952063457778,-17.4521868291004,
12.));
#196242=CARTESIAN_POINT('Ctrl Pts',(-15.0065183456921,-17.4609628621418,
0.));
#196243=CARTESIAN_POINT('Ctrl Pts',(-15.0065183456921,-17.4609628621418,
12.));
#196244=CARTESIAN_POINT('Ctrl Pts',(-15.0179828635086,-17.4698002829356,
0.));
#196245=CARTESIAN_POINT('Ctrl Pts',(-15.0179828635086,-17.4698002829356,
12.));
#196246=CARTESIAN_POINT('Ctrl Pts',(-15.029598928488,-17.4786973441417,
0.));
#196247=CARTESIAN_POINT('Ctrl Pts',(-15.029598928488,-17.4786973441417,
12.));
#196248=CARTESIAN_POINT('Ctrl Pts',(-15.0413655884993,-17.4876523366178,
0.));
#196249=CARTESIAN_POINT('Ctrl Pts',(-15.0413655884993,-17.4876523366178,
12.));
#196250=CARTESIAN_POINT('Ctrl Pts',(-15.0532819093085,-17.4966635880245,
0.));
#196251=CARTESIAN_POINT('Ctrl Pts',(-15.0532819093085,-17.4966635880245,
12.));
#196252=CARTESIAN_POINT('Ctrl Pts',(-15.0653469738306,-17.5057294613874,
0.));
#196253=CARTESIAN_POINT('Ctrl Pts',(-15.0653469738306,-17.5057294613874,
12.));
#196254=CARTESIAN_POINT('Ctrl Pts',(-15.0775598815748,-17.5148483539683,
0.));
#196255=CARTESIAN_POINT('Ctrl Pts',(-15.0775598815748,-17.5148483539683,
12.));
#196256=CARTESIAN_POINT('Ctrl Pts',(-15.0899197481082,-17.5240186961788,
0.));
#196257=CARTESIAN_POINT('Ctrl Pts',(-15.0899197481082,-17.5240186961788,
12.));
#196258=CARTESIAN_POINT('Ctrl Pts',(-15.1024257045033,-17.5332389504829,
0.));
#196259=CARTESIAN_POINT('Ctrl Pts',(-15.1024257045033,-17.5332389504829,
12.));
#196260=CARTESIAN_POINT('Ctrl Pts',(-15.1150768967729,-17.5425076102966,
0.));
#196261=CARTESIAN_POINT('Ctrl Pts',(-15.1150768967729,-17.5425076102966,
12.));
#196262=CARTESIAN_POINT('Ctrl Pts',(-15.127872485314,-17.5518231989122,
0.));
#196263=CARTESIAN_POINT('Ctrl Pts',(-15.127872485314,-17.5518231989122,
12.));
#196264=CARTESIAN_POINT('Ctrl Pts',(-15.1408116444877,-17.5611842686196,
0.));
#196265=CARTESIAN_POINT('Ctrl Pts',(-15.1408116444877,-17.5611842686196,
12.));
#196266=CARTESIAN_POINT('Ctrl Pts',(-15.1538935621715,-17.570589399803,
0.));
#196267=CARTESIAN_POINT('Ctrl Pts',(-15.1538935621715,-17.570589399803,
12.));
#196268=CARTESIAN_POINT('Ctrl Pts',(-15.1671174393137,-17.5800372000539,
0.));
#196269=CARTESIAN_POINT('Ctrl Pts',(-15.1671174393137,-17.5800372000539,
12.));
#196270=CARTESIAN_POINT('Ctrl Pts',(-15.1804824894605,-17.5895263032592,
0.));
#196271=CARTESIAN_POINT('Ctrl Pts',(-15.1804824894605,-17.5895263032592,
12.));
#196272=CARTESIAN_POINT('Ctrl Pts',(-15.1939879383268,-17.5990553687595,
0.));
#196273=CARTESIAN_POINT('Ctrl Pts',(-15.1939879383268,-17.5990553687595,
12.));
#196274=CARTESIAN_POINT('Ctrl Pts',(-15.2076330234686,-17.6086230806497,
0.));
#196275=CARTESIAN_POINT('Ctrl Pts',(-15.2076330234686,-17.6086230806497,
12.));
#196276=CARTESIAN_POINT('Ctrl Pts',(-15.22141699392,-17.6182281470467,0.));
#196277=CARTESIAN_POINT('Ctrl Pts',(-15.22141699392,-17.6182281470467,12.));
#196278=CARTESIAN_POINT('Ctrl Pts',(-15.2353391098367,-17.6278692993765,
0.));
#196279=CARTESIAN_POINT('Ctrl Pts',(-15.2353391098367,-17.6278692993765,
12.));
#196280=CARTESIAN_POINT('Ctrl Pts',(-15.2493986421091,-17.637545291637,
0.));
#196281=CARTESIAN_POINT('Ctrl Pts',(-15.2493986421091,-17.637545291637,
12.));
#196282=CARTESIAN_POINT('Ctrl Pts',(-15.263594872029,-17.6472548997329,
0.));
#196283=CARTESIAN_POINT('Ctrl Pts',(-15.263594872029,-17.6472548997329,
12.));
#196284=CARTESIAN_POINT('Ctrl Pts',(-15.2779270910238,-17.6569969209,0.));
#196285=CARTESIAN_POINT('Ctrl Pts',(-15.2779270910238,-17.6569969209,12.));
#196286=CARTESIAN_POINT('Ctrl Pts',(-15.2923946003598,-17.6667701731041,
0.));
#196287=CARTESIAN_POINT('Ctrl Pts',(-15.2923946003598,-17.6667701731041,
12.));
#196288=CARTESIAN_POINT('Ctrl Pts',(-15.3069967108501,-17.6765734944559,
0.));
#196289=CARTESIAN_POINT('Ctrl Pts',(-15.3069967108501,-17.6765734944559,
12.));
#196290=CARTESIAN_POINT('Ctrl Pts',(-15.3217327425341,-17.6864057426052,
0.));
#196291=CARTESIAN_POINT('Ctrl Pts',(-15.3217327425341,-17.6864057426052,
12.));
#196292=CARTESIAN_POINT('Ctrl Pts',(-15.3366020244069,-17.6962657941984,
0.));
#196293=CARTESIAN_POINT('Ctrl Pts',(-15.3366020244069,-17.6962657941984,
12.));
#196294=CARTESIAN_POINT('Ctrl Pts',(-15.3516038942064,-17.7061525444044,
0.));
#196295=CARTESIAN_POINT('Ctrl Pts',(-15.3516038942064,-17.7061525444044,
12.));
#196296=CARTESIAN_POINT('Ctrl Pts',(-15.3667376981702,-17.7160649064208,
0.));
#196297=CARTESIAN_POINT('Ctrl Pts',(-15.3667376981702,-17.7160649064208,
12.));
#196298=CARTESIAN_POINT('Ctrl Pts',(-15.3820027907965,-17.7260018109923,
0.));
#196299=CARTESIAN_POINT('Ctrl Pts',(-15.3820027907965,-17.7260018109923,
12.));
#196300=CARTESIAN_POINT('Ctrl Pts',(-15.3973985345796,-17.7359622059143,
0.));
#196301=CARTESIAN_POINT('Ctrl Pts',(-15.3973985345796,-17.7359622059143,
12.));
#196302=CARTESIAN_POINT('Ctrl Pts',(-15.4129242997828,-17.7459450555803,
0.));
#196303=CARTESIAN_POINT('Ctrl Pts',(-15.4129242997828,-17.7459450555803,
12.));
#196304=CARTESIAN_POINT('Ctrl Pts',(-15.4285794642658,-17.7559493405871,
0.));
#196305=CARTESIAN_POINT('Ctrl Pts',(-15.4285794642658,-17.7559493405871,
12.));
#196306=CARTESIAN_POINT('Ctrl Pts',(-15.4443634132865,-17.765974057326,
0.));
#196307=CARTESIAN_POINT('Ctrl Pts',(-15.4443634132865,-17.765974057326,
12.));
#196308=CARTESIAN_POINT('Ctrl Pts',(-15.460275539302,-17.7760182175817,
0.));
#196309=CARTESIAN_POINT('Ctrl Pts',(-15.460275539302,-17.7760182175817,
12.));
#196310=CARTESIAN_POINT('Ctrl Pts',(-15.4763152417506,-17.7860808481229,
0.));
#196311=CARTESIAN_POINT('Ctrl Pts',(-15.4763152417506,-17.7860808481229,
12.));
#196312=CARTESIAN_POINT('Ctrl Pts',(-15.4924819268529,-17.7961609903161,
0.));
#196313=CARTESIAN_POINT('Ctrl Pts',(-15.4924819268529,-17.7961609903161,
12.));
#196314=CARTESIAN_POINT('Ctrl Pts',(-15.5087750074728,-17.8062576997964,
0.));
#196315=CARTESIAN_POINT('Ctrl Pts',(-15.5087750074728,-17.8062576997964,
12.));
#196316=CARTESIAN_POINT('Ctrl Pts',(-15.5251939029558,-17.8163700461262,
0.));
#196317=CARTESIAN_POINT('Ctrl Pts',(-15.5251939029558,-17.8163700461262,
12.));
#196318=CARTESIAN_POINT('Ctrl Pts',(-15.5417380389639,-17.8264971124606,
0.));
#196319=CARTESIAN_POINT('Ctrl Pts',(-15.5417380389639,-17.8264971124606,
12.));
#196320=CARTESIAN_POINT('Ctrl Pts',(-15.5584068472976,-17.8366379952078,
0.));
#196321=CARTESIAN_POINT('Ctrl Pts',(-15.5584068472976,-17.8366379952078,
12.));
#196322=CARTESIAN_POINT('Ctrl Pts',(-15.5751997657154,-17.8467918036976,
0.));
#196323=CARTESIAN_POINT('Ctrl Pts',(-15.5751997657154,-17.8467918036976,
12.));
#196324=CARTESIAN_POINT('Ctrl Pts',(-15.5921162378183,-17.8569576598996,
0.));
#196325=CARTESIAN_POINT('Ctrl Pts',(-15.5921162378183,-17.8569576598996,
12.));
#196326=CARTESIAN_POINT('Ctrl Pts',(-15.6091557129205,-17.8671346981388,
0.));
#196327=CARTESIAN_POINT('Ctrl Pts',(-15.6091557129205,-17.8671346981388,
12.));
#196328=CARTESIAN_POINT('Ctrl Pts',(-15.6263176459107,-17.8773220648125,
0.));
#196329=CARTESIAN_POINT('Ctrl Pts',(-15.6263176459107,-17.8773220648125,
12.));
#196330=CARTESIAN_POINT('Ctrl Pts',(-15.6436014971088,-17.8875189181095,
0.));
#196331=CARTESIAN_POINT('Ctrl Pts',(-15.6436014971088,-17.8875189181095,
12.));
#196332=CARTESIAN_POINT('Ctrl Pts',(-15.6610067321036,-17.8977244277247,
0.));
#196333=CARTESIAN_POINT('Ctrl Pts',(-15.6610067321036,-17.8977244277247,
12.));
#196334=CARTESIAN_POINT('Ctrl Pts',(-15.6785328216467,-17.9079377746118,
0.));
#196335=CARTESIAN_POINT('Ctrl Pts',(-15.6785328216467,-17.9079377746118,
12.));
#196336=CARTESIAN_POINT('Ctrl Pts',(-15.6961792415526,-17.918158150746,
0.));
#196337=CARTESIAN_POINT('Ctrl Pts',(-15.6961792415526,-17.918158150746,
12.));
#196338=CARTESIAN_POINT('Ctrl Pts',(-15.713945472584,-17.9283847588837,
0.));
#196339=CARTESIAN_POINT('Ctrl Pts',(-15.713945472584,-17.9283847588837,
12.));
#196340=CARTESIAN_POINT('Ctrl Pts',(-15.7318310003334,-17.9386168123261,
0.));
#196341=CARTESIAN_POINT('Ctrl Pts',(-15.7318310003334,-17.9386168123261,
12.));
#196342=CARTESIAN_POINT('Ctrl Pts',(-15.7498353150856,-17.9488535346776,
0.));
#196343=CARTESIAN_POINT('Ctrl Pts',(-15.7498353150856,-17.9488535346776,
12.));
#196344=CARTESIAN_POINT('Ctrl Pts',(-15.7679579117072,-17.9590941596236,
0.));
#196345=CARTESIAN_POINT('Ctrl Pts',(-15.7679579117072,-17.9590941596236,
12.));
#196346=CARTESIAN_POINT('Ctrl Pts',(-15.786198289572,-17.9693379307297,
0.));
#196347=CARTESIAN_POINT('Ctrl Pts',(-15.786198289572,-17.9693379307297,
12.));
#196348=CARTESIAN_POINT('Ctrl Pts',(-15.8045559524674,-17.9795841012383,
0.));
#196349=CARTESIAN_POINT('Ctrl Pts',(-15.8045559524674,-17.9795841012383,
12.));
#196350=CARTESIAN_POINT('Ctrl Pts',(-15.8230304084963,-17.9898319338664,
0.));
#196351=CARTESIAN_POINT('Ctrl Pts',(-15.8230304084963,-17.9898319338664,
12.));
#196352=CARTESIAN_POINT('Ctrl Pts',(-15.8416211699682,-18.0000807006055,
0.));
#196353=CARTESIAN_POINT('Ctrl Pts',(-15.8416211699682,-18.0000807006055,
12.));
#196354=CARTESIAN_POINT('Ctrl Pts',(-15.8603277532834,-18.010329682521,
0.));
#196355=CARTESIAN_POINT('Ctrl Pts',(-15.8603277532834,-18.010329682521,
12.));
#196356=CARTESIAN_POINT('Ctrl Pts',(-15.8791496788685,-18.0205781695773,
0.));
#196357=CARTESIAN_POINT('Ctrl Pts',(-15.8791496788685,-18.0205781695773,
12.));
#196358=CARTESIAN_POINT('Ctrl Pts',(-15.8980864711043,-18.0308254604638,
0.));
#196359=CARTESIAN_POINT('Ctrl Pts',(-15.8980864711043,-18.0308254604638,
12.));
#196360=CARTESIAN_POINT('Ctrl Pts',(-15.9171376582436,-18.0410708624208,
0.));
#196361=CARTESIAN_POINT('Ctrl Pts',(-15.9171376582436,-18.0410708624208,
12.));
#196362=CARTESIAN_POINT('Ctrl Pts',(-15.9363027723244,-18.0513136910691,
0.));
#196363=CARTESIAN_POINT('Ctrl Pts',(-15.9363027723244,-18.0513136910691,
12.));
#196364=CARTESIAN_POINT('Ctrl Pts',(-15.9555813490645,-18.061553270236,
0.));
#196365=CARTESIAN_POINT('Ctrl Pts',(-15.9555813490645,-18.061553270236,
12.));
#196366=CARTESIAN_POINT('Ctrl Pts',(-15.9749729277848,-18.071788931796,
0.));
#196367=CARTESIAN_POINT('Ctrl Pts',(-15.9749729277848,-18.071788931796,
12.));
#196368=CARTESIAN_POINT('Ctrl Pts',(-15.9944770513616,-18.0820200155238,
0.));
#196369=CARTESIAN_POINT('Ctrl Pts',(-15.9944770513616,-18.0820200155238,
12.));
#196370=CARTESIAN_POINT('Ctrl Pts',(-16.0140932661612,-18.0922458689464,
0.));
#196371=CARTESIAN_POINT('Ctrl Pts',(-16.0140932661612,-18.0922458689464,
12.));
#196372=CARTESIAN_POINT('Ctrl Pts',(-16.0338211219694,-18.1024658471966,
0.));
#196373=CARTESIAN_POINT('Ctrl Pts',(-16.0338211219694,-18.1024658471966,
12.));
#196374=CARTESIAN_POINT('Ctrl Pts',(-16.0536601719124,-18.1126793128688,
0.));
#196375=CARTESIAN_POINT('Ctrl Pts',(-16.0536601719124,-18.1126793128688,
12.));
#196376=CARTESIAN_POINT('Ctrl Pts',(-16.0736099723665,-18.1228856358746,
0.));
#196377=CARTESIAN_POINT('Ctrl Pts',(-16.0736099723665,-18.1228856358746,
12.));
#196378=CARTESIAN_POINT('Ctrl Pts',(-16.0936700829108,-18.1330841933099,
0.));
#196379=CARTESIAN_POINT('Ctrl Pts',(-16.0936700829108,-18.1330841933099,
12.));
#196380=CARTESIAN_POINT('Ctrl Pts',(-16.1138400662791,-18.1432743693231,
0.));
#196381=CARTESIAN_POINT('Ctrl Pts',(-16.1138400662791,-18.1432743693231,
12.));
#196382=CARTESIAN_POINT('Ctrl Pts',(-16.1341194882987,-18.153455554985,
0.));
#196383=CARTESIAN_POINT('Ctrl Pts',(-16.1341194882987,-18.153455554985,
12.));
#196384=CARTESIAN_POINT('Ctrl Pts',(-16.1545079178261,-18.1636271481616,
0.));
#196385=CARTESIAN_POINT('Ctrl Pts',(-16.1545079178261,-18.1636271481616,
12.));
#196386=CARTESIAN_POINT('Ctrl Pts',(-16.1750049266673,-18.1737885533852,
0.));
#196387=CARTESIAN_POINT('Ctrl Pts',(-16.1750049266673,-18.1737885533852,
12.));
#196388=CARTESIAN_POINT('Ctrl Pts',(-16.1956100895076,-18.1839391817335,
0.));
#196389=CARTESIAN_POINT('Ctrl Pts',(-16.1956100895076,-18.1839391817335,
12.));
#196390=CARTESIAN_POINT('Ctrl Pts',(-16.2163229838878,-18.1940784507232,
0.));
#196391=CARTESIAN_POINT('Ctrl Pts',(-16.2163229838878,-18.1940784507232,
12.));
#196392=CARTESIAN_POINT('Ctrl Pts',(-16.237143190164,-18.2042057842037,
0.));
#196393=CARTESIAN_POINT('Ctrl Pts',(-16.237143190164,-18.2042057842037,
12.));
#196394=CARTESIAN_POINT('Ctrl Pts',(-16.2580702914615,-18.214320612253,
0.));
#196395=CARTESIAN_POINT('Ctrl Pts',(-16.2580702914615,-18.214320612253,
12.));
#196396=CARTESIAN_POINT('Ctrl Pts',(-16.2791038736223,-18.2244223710745,
0.));
#196397=CARTESIAN_POINT('Ctrl Pts',(-16.2791038736223,-18.2244223710745,
12.));
#196398=CARTESIAN_POINT('Ctrl Pts',(-16.3002435251378,-18.2345105028981,
0.));
#196399=CARTESIAN_POINT('Ctrl Pts',(-16.3002435251378,-18.2345105028981,
12.));
#196400=CARTESIAN_POINT('Ctrl Pts',(-16.3214888370988,-18.2445844558742,
0.));
#196401=CARTESIAN_POINT('Ctrl Pts',(-16.3214888370988,-18.2445844558742,
12.));
#196402=CARTESIAN_POINT('Ctrl Pts',(-16.342839403159,-18.2546436839609,
0.));
#196403=CARTESIAN_POINT('Ctrl Pts',(-16.342839403159,-18.2546436839609,
12.));
#196404=CARTESIAN_POINT('Ctrl Pts',(-16.3642948194869,-18.2646876468169,
0.));
#196405=CARTESIAN_POINT('Ctrl Pts',(-16.3642948194869,-18.2646876468169,
12.));
#196406=CARTESIAN_POINT('Ctrl Pts',(-16.385854684708,-18.2747158096934,
0.));
#196407=CARTESIAN_POINT('Ctrl Pts',(-16.385854684708,-18.2747158096934,
12.));
#196408=CARTESIAN_POINT('Ctrl Pts',(-16.4075185998454,-18.2847276433308,
0.));
#196409=CARTESIAN_POINT('Ctrl Pts',(-16.4075185998454,-18.2847276433308,
12.));
#196410=CARTESIAN_POINT('Ctrl Pts',(-16.4292861682377,-18.2947226238509,
0.));
#196411=CARTESIAN_POINT('Ctrl Pts',(-16.4292861682377,-18.2947226238509,
12.));
#196412=CARTESIAN_POINT('Ctrl Pts',(-16.4511569955231,-18.3047002326858,
0.));
#196413=CARTESIAN_POINT('Ctrl Pts',(-16.4511569955231,-18.3047002326858,
12.));
#196414=CARTESIAN_POINT('Ctrl Pts',(-16.4731306896439,-18.3146599565229,
0.));
#196415=CARTESIAN_POINT('Ctrl Pts',(-16.4731306896439,-18.3146599565229,
12.));
#196416=CARTESIAN_POINT('Ctrl Pts',(-16.4952068608344,-18.3246012872468,
0.));
#196417=CARTESIAN_POINT('Ctrl Pts',(-16.4952068608344,-18.3246012872468,
12.));
#196418=CARTESIAN_POINT('Ctrl Pts',(-16.5173851216045,-18.3345237218864,
0.));
#196419=CARTESIAN_POINT('Ctrl Pts',(-16.5173851216045,-18.3345237218864,
12.));
#196420=CARTESIAN_POINT('Ctrl Pts',(-16.539665086714,-18.3444267625601,
0.));
#196421=CARTESIAN_POINT('Ctrl Pts',(-16.539665086714,-18.3444267625601,
12.));
#196422=CARTESIAN_POINT('Ctrl Pts',(-16.5620463731414,-18.3543099164331,
0.));
#196423=CARTESIAN_POINT('Ctrl Pts',(-16.5620463731414,-18.3543099164331,
12.));
#196424=CARTESIAN_POINT('Ctrl Pts',(-16.5845286000219,-18.364172695589,
0.));
#196425=CARTESIAN_POINT('Ctrl Pts',(-16.5845286000219,-18.364172695589,
12.));
#196426=CARTESIAN_POINT('Ctrl Pts',(-16.6071113885711,-18.3740146168879,
0.));
#196427=CARTESIAN_POINT('Ctrl Pts',(-16.6071113885711,-18.3740146168879,
12.));
#196428=CARTESIAN_POINT('Ctrl Pts',(-16.6297943620056,-18.3838352018327,
0.));
#196429=CARTESIAN_POINT('Ctrl Pts',(-16.6297943620056,-18.3838352018327,
12.));
#196430=CARTESIAN_POINT('Ctrl Pts',(-16.6525771454513,-18.3936339764332,
0.));
#196431=CARTESIAN_POINT('Ctrl Pts',(-16.6525771454513,-18.3936339764332,
12.));
#196432=CARTESIAN_POINT('Ctrl Pts',(-16.6754593658513,-18.4034104710789,
0.));
#196433=CARTESIAN_POINT('Ctrl Pts',(-16.6754593658513,-18.4034104710789,
12.));
#196434=CARTESIAN_POINT('Ctrl Pts',(-16.698440651849,-18.4131642203989,
0.));
#196435=CARTESIAN_POINT('Ctrl Pts',(-16.698440651849,-18.4131642203989,
12.));
#196436=CARTESIAN_POINT('Ctrl Pts',(-16.7215206338818,-18.4228947633186,
0.));
#196437=CARTESIAN_POINT('Ctrl Pts',(-16.7215206338818,-18.4228947633186,
12.));
#196438=CARTESIAN_POINT('Ctrl Pts',(-16.7446989442882,-18.4326016431392,
0.));
#196439=CARTESIAN_POINT('Ctrl Pts',(-16.7446989442882,-18.4326016431392,
12.));
#196440=CARTESIAN_POINT('Ctrl Pts',(-16.7679752173992,-18.4422844076099,
0.));
#196441=CARTESIAN_POINT('Ctrl Pts',(-16.7679752173992,-18.4422844076099,
12.));
#196442=CARTESIAN_POINT('Ctrl Pts',(-16.791349089629,-18.4519426090124,
0.));
#196443=CARTESIAN_POINT('Ctrl Pts',(-16.791349089629,-18.4519426090124,
12.));
#196444=CARTESIAN_POINT('Ctrl Pts',(-16.8148201995472,-18.4615758042305,
0.));
#196445=CARTESIAN_POINT('Ctrl Pts',(-16.8148201995472,-18.4615758042305,
12.));
#196446=CARTESIAN_POINT('Ctrl Pts',(-16.8383881879707,-18.4711835548622,
0.));
#196447=CARTESIAN_POINT('Ctrl Pts',(-16.8383881879707,-18.4711835548622,
12.));
#196448=CARTESIAN_POINT('Ctrl Pts',(-16.8620526977169,-18.4807654268769,
0.));
#196449=CARTESIAN_POINT('Ctrl Pts',(-16.8620526977169,-18.4807654268769,
12.));
#196450=CARTESIAN_POINT('Ctrl Pts',(-16.8858133733086,-18.4903209902226,
0.));
#196451=CARTESIAN_POINT('Ctrl Pts',(-16.8858133733086,-18.4903209902226,
12.));
#196452=CARTESIAN_POINT('Ctrl Pts',(-16.9096698606942,-18.4998498184619,
0.));
#196453=CARTESIAN_POINT('Ctrl Pts',(-16.9096698606942,-18.4998498184619,
12.));
#196454=CARTESIAN_POINT('Ctrl Pts',(-16.9336218069353,-18.5093514883835,
0.));
#196455=CARTESIAN_POINT('Ctrl Pts',(-16.9336218069353,-18.5093514883835,
12.));
#196456=CARTESIAN_POINT('Ctrl Pts',(-16.957668859934,-18.518825579666,0.));
#196457=CARTESIAN_POINT('Ctrl Pts',(-16.957668859934,-18.518825579666,12.));
#196458=CARTESIAN_POINT('Ctrl Pts',(-16.9818106680382,-18.5282716744198,
0.));
#196459=CARTESIAN_POINT('Ctrl Pts',(-16.9818106680382,-18.5282716744198,
12.));
#196460=CARTESIAN_POINT('Ctrl Pts',(-17.0060468805099,-18.5376893576961,
0.));
#196461=CARTESIAN_POINT('Ctrl Pts',(-17.0060468805099,-18.5376893576961,
12.));
#196462=CARTESIAN_POINT('Ctrl Pts',(-17.030377148174,-18.5470782182089,
0.));
#196463=CARTESIAN_POINT('Ctrl Pts',(-17.030377148174,-18.5470782182089,
12.));
#196464=CARTESIAN_POINT('Ctrl Pts',(-17.0548011239751,-18.5564378489628,
0.));
#196465=CARTESIAN_POINT('Ctrl Pts',(-17.0548011239751,-18.5564378489628,
12.));
#196466=CARTESIAN_POINT('Ctrl Pts',(-17.0793184636079,-18.5657678479788,
0.));
#196467=CARTESIAN_POINT('Ctrl Pts',(-17.0793184636079,-18.5657678479788,
12.));
#196468=CARTESIAN_POINT('Ctrl Pts',(-17.1039288260002,-18.5750678188543,
0.));
#196469=CARTESIAN_POINT('Ctrl Pts',(-17.1039288260002,-18.5750678188543,
12.));
#196470=CARTESIAN_POINT('Ctrl Pts',(-17.1286318741185,-18.5843373717253,
0.));
#196471=CARTESIAN_POINT('Ctrl Pts',(-17.1286318741185,-18.5843373717253,
12.));
#196472=CARTESIAN_POINT('Ctrl Pts',(-17.1534272741646,-18.5935761222833,
0.));
#196473=CARTESIAN_POINT('Ctrl Pts',(-17.1534272741646,-18.5935761222833,
12.));
#196474=CARTESIAN_POINT('Ctrl Pts',(-17.1783146940131,-18.6027836898826,
0.));
#196475=CARTESIAN_POINT('Ctrl Pts',(-17.1783146940131,-18.6027836898826,
12.));
#196476=CARTESIAN_POINT('Ctrl Pts',(-17.2032938019288,-18.6119596959957,
0.));
#196477=CARTESIAN_POINT('Ctrl Pts',(-17.2032938019288,-18.6119596959957,
12.));
#196478=CARTESIAN_POINT('Ctrl Pts',(-17.2283642650519,-18.6211037624041,
0.));
#196479=CARTESIAN_POINT('Ctrl Pts',(-17.2283642650519,-18.6211037624041,
12.));
#196480=CARTESIAN_POINT('Ctrl Pts',(-17.2535257482186,-18.630215509794,
0.));
#196481=CARTESIAN_POINT('Ctrl Pts',(-17.2535257482186,-18.630215509794,
12.));
#196482=CARTESIAN_POINT('Ctrl Pts',(-17.278777912021,-18.639294555474,0.));
#196483=CARTESIAN_POINT('Ctrl Pts',(-17.278777912021,-18.639294555474,12.));
#196484=CARTESIAN_POINT('Ctrl Pts',(-17.3041204135069,-18.6483405141853,
0.));
#196485=CARTESIAN_POINT('Ctrl Pts',(-17.3041204135069,-18.6483405141853,
12.));
#196486=CARTESIAN_POINT('Ctrl Pts',(-17.3295529098612,-18.6573530024019,
0.));
#196487=CARTESIAN_POINT('Ctrl Pts',(-17.3295529098612,-18.6573530024019,
12.));
#196488=CARTESIAN_POINT('Ctrl Pts',(-17.3550750612438,-18.6663316416569,
0.));
#196489=CARTESIAN_POINT('Ctrl Pts',(-17.3550750612438,-18.6663316416569,
12.));
#196490=CARTESIAN_POINT('Ctrl Pts',(-17.3806865340744,-18.6752760624045,
0.));
#196491=CARTESIAN_POINT('Ctrl Pts',(-17.3806865340744,-18.6752760624045,
12.));
#196492=CARTESIAN_POINT('Ctrl Pts',(-17.4063870038563,-18.6841859073472,
0.));
#196493=CARTESIAN_POINT('Ctrl Pts',(-17.4063870038563,-18.6841859073472,
12.));
#196494=CARTESIAN_POINT('Ctrl Pts',(-17.4321761588148,-18.6930608357421,
0.));
#196495=CARTESIAN_POINT('Ctrl Pts',(-17.4321761588148,-18.6930608357421,
12.));
#196496=CARTESIAN_POINT('Ctrl Pts',(-17.4580537012764,-18.7019005250322,
0.));
#196497=CARTESIAN_POINT('Ctrl Pts',(-17.4580537012764,-18.7019005250322,
12.));
#196498=CARTESIAN_POINT('Ctrl Pts',(-17.4840193397176,-18.7107046613941,
0.));
#196499=CARTESIAN_POINT('Ctrl Pts',(-17.4840193397176,-18.7107046613941,
12.));
#196500=CARTESIAN_POINT('Ctrl Pts',(-17.5100727820891,-18.7194729318127,
0.));
#196501=CARTESIAN_POINT('Ctrl Pts',(-17.5100727820891,-18.7194729318127,
12.));
#196502=CARTESIAN_POINT('Ctrl Pts',(-17.5362137287604,-18.728205015716,
0.));
#196503=CARTESIAN_POINT('Ctrl Pts',(-17.5362137287604,-18.728205015716,
12.));
#196504=CARTESIAN_POINT('Ctrl Pts',(-17.5624418653248,-18.7369005764558,
0.));
#196505=CARTESIAN_POINT('Ctrl Pts',(-17.5624418653248,-18.7369005764558,
12.));
#196506=CARTESIAN_POINT('Ctrl Pts',(-17.5887568561361,-18.7455592536667,
0.));
#196507=CARTESIAN_POINT('Ctrl Pts',(-17.5887568561361,-18.7455592536667,
12.));
#196508=CARTESIAN_POINT('Ctrl Pts',(-17.6151583356989,-18.7541806530935,
0.));
#196509=CARTESIAN_POINT('Ctrl Pts',(-17.6151583356989,-18.7541806530935,
12.));
#196510=CARTESIAN_POINT('Ctrl Pts',(-17.6416459210646,-18.7627643613138,
0.));
#196511=CARTESIAN_POINT('Ctrl Pts',(-17.6416459210646,-18.7627643613138,
12.));
#196512=CARTESIAN_POINT('Ctrl Pts',(-17.6682192274197,-18.7713099642673,
0.));
#196513=CARTESIAN_POINT('Ctrl Pts',(-17.6682192274197,-18.7713099642673,
12.));
#196514=CARTESIAN_POINT('Ctrl Pts',(-17.6948778822982,-18.7798170641305,
0.));
#196515=CARTESIAN_POINT('Ctrl Pts',(-17.6948778822982,-18.7798170641305,
12.));
#196516=CARTESIAN_POINT('Ctrl Pts',(-17.7216215409019,-18.7882852976016,
0.));
#196517=CARTESIAN_POINT('Ctrl Pts',(-17.7216215409019,-18.7882852976016,
12.));
#196518=CARTESIAN_POINT('Ctrl Pts',(-17.7484498996917,-18.7967143519444,
0.));
#196519=CARTESIAN_POINT('Ctrl Pts',(-17.7484498996917,-18.7967143519444,
12.));
#196520=CARTESIAN_POINT('Ctrl Pts',(-17.7753627137898,-18.8051039860543,
0.));
#196521=CARTESIAN_POINT('Ctrl Pts',(-17.7753627137898,-18.8051039860543,
12.));
#196522=CARTESIAN_POINT('Ctrl Pts',(-17.8023598011135,-18.8134540340581,
0.));
#196523=CARTESIAN_POINT('Ctrl Pts',(-17.8023598011135,-18.8134540340581,
12.));
#196524=CARTESIAN_POINT('Ctrl Pts',(-17.8294410311105,-18.8217643886368,
0.));
#196525=CARTESIAN_POINT('Ctrl Pts',(-17.8294410311105,-18.8217643886368,
12.));
#196526=CARTESIAN_POINT('Ctrl Pts',(-17.8566063174871,-18.8300349896187,
0.));
#196527=CARTESIAN_POINT('Ctrl Pts',(-17.8566063174871,-18.8300349896187,
12.));
#196528=CARTESIAN_POINT('Ctrl Pts',(-17.8784057509434,-18.8366196462746,
0.));
#196529=CARTESIAN_POINT('Ctrl Pts',(-17.8784057509434,-18.8366196462746,
12.));
#196530=CARTESIAN_POINT('Ctrl Pts',(-17.8947931177853,-18.8415402351882,
0.));
#196531=CARTESIAN_POINT('Ctrl Pts',(-17.8947931177853,-18.8415402351882,
12.));
#196532=CARTESIAN_POINT('Ctrl Pts',(-17.9057348246611,-18.8448126709726,
0.));
#196533=CARTESIAN_POINT('Ctrl Pts',(-17.9057348246611,-18.8448126709726,
12.));
#196534=CARTESIAN_POINT('Ctrl Pts',(-17.9112098770111,-18.8464468996588,
0.));
#196535=CARTESIAN_POINT('Ctrl Pts',(-17.9112098770111,-18.8464468996588,
12.));
#196536=CARTESIAN_POINT('',(-17.9112098770111,-18.8464468996588,0.));
#196537=CARTESIAN_POINT('Ctrl Pts',(-14.6513681262571,-17.1452095830632,
0.));
#196538=CARTESIAN_POINT('Ctrl Pts',(-14.6513711852843,-17.1452153999142,
0.));
#196539=CARTESIAN_POINT('Ctrl Pts',(-14.6514066997196,-17.1452600887037,
0.));
#196540=CARTESIAN_POINT('Ctrl Pts',(-14.6515481598068,-17.1454262858043,
0.));
#196541=CARTESIAN_POINT('Ctrl Pts',(-14.6519131634508,-17.1458462295271,
0.));
#196542=CARTESIAN_POINT('Ctrl Pts',(-14.6526624064978,-17.1466998098673,
0.));
#196543=CARTESIAN_POINT('Ctrl Pts',(-14.6537016966184,-17.147876394491,
0.));
#196544=CARTESIAN_POINT('Ctrl Pts',(-14.655024862281,-17.1493641837558,
0.));
#196545=CARTESIAN_POINT('Ctrl Pts',(-14.6566237952435,-17.1511476869496,
0.));
#196546=CARTESIAN_POINT('Ctrl Pts',(-14.6584900555302,-17.1532107762718,
0.));
#196547=CARTESIAN_POINT('Ctrl Pts',(-14.6606167169642,-17.1555401986401,
0.));
#196548=CARTESIAN_POINT('Ctrl Pts',(-14.6629987285992,-17.1581262646789,
0.));
#196549=CARTESIAN_POINT('Ctrl Pts',(-14.6656319165057,-17.1609609517369,
0.));
#196550=CARTESIAN_POINT('Ctrl Pts',(-14.6685123374423,-17.1640366762305,
0.));
#196551=CARTESIAN_POINT('Ctrl Pts',(-14.671635583332,-17.167344972302,0.));
#196552=CARTESIAN_POINT('Ctrl Pts',(-14.6749971333867,-17.1708771619129,
0.));
#196553=CARTESIAN_POINT('Ctrl Pts',(-14.6785925615677,-17.1746247499056,
0.));
#196554=CARTESIAN_POINT('Ctrl Pts',(-14.6824178576167,-17.1785800350826,
0.));
#196555=CARTESIAN_POINT('Ctrl Pts',(-14.686469452232,-17.1827361584719,
0.));
#196556=CARTESIAN_POINT('Ctrl Pts',(-14.6907440526958,-17.1870867909918,
0.));
#196557=CARTESIAN_POINT('Ctrl Pts',(-14.6952385361706,-17.1916259308415,
0.));
#196558=CARTESIAN_POINT('Ctrl Pts',(-14.699949811582,-17.1963476411694,
0.));
#196559=CARTESIAN_POINT('Ctrl Pts',(-14.7048748502663,-17.2012461084268,
0.));
#196560=CARTESIAN_POINT('Ctrl Pts',(-14.7100107213586,-17.2063157097315,
0.));
#196561=CARTESIAN_POINT('Ctrl Pts',(-14.7153546289339,-17.2115510835989,
0.));
#196562=CARTESIAN_POINT('Ctrl Pts',(-14.7209039390327,-17.2169471814256,
0.));
#196563=CARTESIAN_POINT('Ctrl Pts',(-14.7266561494282,-17.2224992099666,
0.));
#196564=CARTESIAN_POINT('Ctrl Pts',(-14.7326088681163,-17.2282025904314,
0.));
#196565=CARTESIAN_POINT('Ctrl Pts',(-14.7387597858117,-17.2340529062076,
0.));
#196566=CARTESIAN_POINT('Ctrl Pts',(-14.7451066593792,-17.2400458713565,
0.));
#196567=CARTESIAN_POINT('Ctrl Pts',(-14.7516473175124,-17.2461773413288,
0.));
#196568=CARTESIAN_POINT('Ctrl Pts',(-14.7583796616617,-17.2524433146837,
0.));
#196569=CARTESIAN_POINT('Ctrl Pts',(-14.7653016697591,-17.2588399401465,
0.));
#196570=CARTESIAN_POINT('Ctrl Pts',(-14.7724113956731,-17.2653635155319,
0.));
#196571=CARTESIAN_POINT('Ctrl Pts',(-14.7797069617804,-17.2720104735194,
0.));
#196572=CARTESIAN_POINT('Ctrl Pts',(-14.787186553128,-17.2787773704849,
0.));
#196573=CARTESIAN_POINT('Ctrl Pts',(-14.7948484105249,-17.2856608733196,
0.));
#196574=CARTESIAN_POINT('Ctrl Pts',(-14.8026908254276,-17.2926577496513,
0.));
#196575=CARTESIAN_POINT('Ctrl Pts',(-14.8107121391036,-17.299764866148,
0.));
#196576=CARTESIAN_POINT('Ctrl Pts',(-14.8189107410162,-17.3069791853706,
0.));
#196577=CARTESIAN_POINT('Ctrl Pts',(-14.8272850675379,-17.3142977632659,
0.));
#196578=CARTESIAN_POINT('Ctrl Pts',(-14.8358336004197,-17.3217177462101,
0.));
#196579=CARTESIAN_POINT('Ctrl Pts',(-14.8445548643508,-17.3292363662605,
0.));
#196580=CARTESIAN_POINT('Ctrl Pts',(-14.8534474245434,-17.336850936485,
0.));
#196581=CARTESIAN_POINT('Ctrl Pts',(-14.8625098843417,-17.3445588463474,
0.));
#196582=CARTESIAN_POINT('Ctrl Pts',(-14.8717408826956,-17.3523575568645,
0.));
#196583=CARTESIAN_POINT('Ctrl Pts',(-14.8811390927423,-17.3602445978161,
0.));
#196584=CARTESIAN_POINT('Ctrl Pts',(-14.8907032205788,-17.3682175653235,
0.));
#196585=CARTESIAN_POINT('Ctrl Pts',(-14.900432003961,-17.3762741193076,
0.));
#196586=CARTESIAN_POINT('Ctrl Pts',(-14.9103242110058,-17.3844119809824,
0.));
#196587=CARTESIAN_POINT('Ctrl Pts',(-14.9203786389342,-17.3926289303986,
0.));
#196588=CARTESIAN_POINT('Ctrl Pts',(-14.9305941128757,-17.4009228040749,
0.));
#196589=CARTESIAN_POINT('Ctrl Pts',(-14.940969484645,-17.4092914926071,
0.));
#196590=CARTESIAN_POINT('Ctrl Pts',(-14.9515036315143,-17.4177329382828,
0.));
#196591=CARTESIAN_POINT('Ctrl Pts',(-14.9621954549827,-17.426245132709,
0.));
#196592=CARTESIAN_POINT('Ctrl Pts',(-14.9730438799452,-17.4348261151396,
0.));
#196593=CARTESIAN_POINT('Ctrl Pts',(-14.9840478538358,-17.4434739707773,
0.));
#196594=CARTESIAN_POINT('Ctrl Pts',(-14.9952063457778,-17.4521868291004,
0.));
#196595=CARTESIAN_POINT('Ctrl Pts',(-15.0065183456921,-17.4609628621418,
0.));
#196596=CARTESIAN_POINT('Ctrl Pts',(-15.0179828635086,-17.4698002829356,
0.));
#196597=CARTESIAN_POINT('Ctrl Pts',(-15.029598928488,-17.4786973441417,
0.));
#196598=CARTESIAN_POINT('Ctrl Pts',(-15.0413655884993,-17.4876523366178,
0.));
#196599=CARTESIAN_POINT('Ctrl Pts',(-15.0532819093085,-17.4966635880245,
0.));
#196600=CARTESIAN_POINT('Ctrl Pts',(-15.0653469738306,-17.5057294613874,
0.));
#196601=CARTESIAN_POINT('Ctrl Pts',(-15.0775598815748,-17.5148483539683,
0.));
#196602=CARTESIAN_POINT('Ctrl Pts',(-15.0899197481082,-17.5240186961788,
0.));
#196603=CARTESIAN_POINT('Ctrl Pts',(-15.1024257045033,-17.5332389504829,
0.));
#196604=CARTESIAN_POINT('Ctrl Pts',(-15.1150768967729,-17.5425076102966,
0.));
#196605=CARTESIAN_POINT('Ctrl Pts',(-15.127872485314,-17.5518231989122,
0.));
#196606=CARTESIAN_POINT('Ctrl Pts',(-15.1408116444877,-17.5611842686196,
0.));
#196607=CARTESIAN_POINT('Ctrl Pts',(-15.1538935621715,-17.570589399803,
0.));
#196608=CARTESIAN_POINT('Ctrl Pts',(-15.1671174393137,-17.5800372000539,
0.));
#196609=CARTESIAN_POINT('Ctrl Pts',(-15.1804824894605,-17.5895263032592,
0.));
#196610=CARTESIAN_POINT('Ctrl Pts',(-15.1939879383268,-17.5990553687595,
0.));
#196611=CARTESIAN_POINT('Ctrl Pts',(-15.2076330234686,-17.6086230806497,
0.));
#196612=CARTESIAN_POINT('Ctrl Pts',(-15.22141699392,-17.6182281470467,0.));
#196613=CARTESIAN_POINT('Ctrl Pts',(-15.2353391098367,-17.6278692993765,
0.));
#196614=CARTESIAN_POINT('Ctrl Pts',(-15.2493986421091,-17.637545291637,
0.));
#196615=CARTESIAN_POINT('Ctrl Pts',(-15.263594872029,-17.6472548997329,
0.));
#196616=CARTESIAN_POINT('Ctrl Pts',(-15.2779270910238,-17.6569969209,0.));
#196617=CARTESIAN_POINT('Ctrl Pts',(-15.2923946003598,-17.6667701731041,
0.));
#196618=CARTESIAN_POINT('Ctrl Pts',(-15.3069967108501,-17.6765734944559,
0.));
#196619=CARTESIAN_POINT('Ctrl Pts',(-15.3217327425341,-17.6864057426052,
0.));
#196620=CARTESIAN_POINT('Ctrl Pts',(-15.3366020244069,-17.6962657941984,
0.));
#196621=CARTESIAN_POINT('Ctrl Pts',(-15.3516038942064,-17.7061525444044,
0.));
#196622=CARTESIAN_POINT('Ctrl Pts',(-15.3667376981702,-17.7160649064208,
0.));
#196623=CARTESIAN_POINT('Ctrl Pts',(-15.3820027907965,-17.7260018109923,
0.));
#196624=CARTESIAN_POINT('Ctrl Pts',(-15.3973985345796,-17.7359622059143,
0.));
#196625=CARTESIAN_POINT('Ctrl Pts',(-15.4129242997828,-17.7459450555803,
0.));
#196626=CARTESIAN_POINT('Ctrl Pts',(-15.4285794642658,-17.7559493405871,
0.));
#196627=CARTESIAN_POINT('Ctrl Pts',(-15.4443634132865,-17.765974057326,
0.));
#196628=CARTESIAN_POINT('Ctrl Pts',(-15.460275539302,-17.7760182175817,
0.));
#196629=CARTESIAN_POINT('Ctrl Pts',(-15.4763152417506,-17.7860808481229,
0.));
#196630=CARTESIAN_POINT('Ctrl Pts',(-15.4924819268529,-17.7961609903161,
0.));
#196631=CARTESIAN_POINT('Ctrl Pts',(-15.5087750074728,-17.8062576997964,
0.));
#196632=CARTESIAN_POINT('Ctrl Pts',(-15.5251939029558,-17.8163700461262,
0.));
#196633=CARTESIAN_POINT('Ctrl Pts',(-15.5417380389639,-17.8264971124606,
0.));
#196634=CARTESIAN_POINT('Ctrl Pts',(-15.5584068472976,-17.8366379952078,
0.));
#196635=CARTESIAN_POINT('Ctrl Pts',(-15.5751997657154,-17.8467918036976,
0.));
#196636=CARTESIAN_POINT('Ctrl Pts',(-15.5921162378183,-17.8569576598996,
0.));
#196637=CARTESIAN_POINT('Ctrl Pts',(-15.6091557129205,-17.8671346981388,
0.));
#196638=CARTESIAN_POINT('Ctrl Pts',(-15.6263176459107,-17.8773220648125,
0.));
#196639=CARTESIAN_POINT('Ctrl Pts',(-15.6436014971088,-17.8875189181095,
0.));
#196640=CARTESIAN_POINT('Ctrl Pts',(-15.6610067321036,-17.8977244277247,
0.));
#196641=CARTESIAN_POINT('Ctrl Pts',(-15.6785328216467,-17.9079377746118,
0.));
#196642=CARTESIAN_POINT('Ctrl Pts',(-15.6961792415526,-17.918158150746,
0.));
#196643=CARTESIAN_POINT('Ctrl Pts',(-15.713945472584,-17.9283847588837,
0.));
#196644=CARTESIAN_POINT('Ctrl Pts',(-15.7318310003334,-17.9386168123261,
0.));
#196645=CARTESIAN_POINT('Ctrl Pts',(-15.7498353150856,-17.9488535346776,
0.));
#196646=CARTESIAN_POINT('Ctrl Pts',(-15.7679579117072,-17.9590941596236,
0.));
#196647=CARTESIAN_POINT('Ctrl Pts',(-15.786198289572,-17.9693379307297,
0.));
#196648=CARTESIAN_POINT('Ctrl Pts',(-15.8045559524674,-17.9795841012383,
0.));
#196649=CARTESIAN_POINT('Ctrl Pts',(-15.8230304084963,-17.9898319338664,
0.));
#196650=CARTESIAN_POINT('Ctrl Pts',(-15.8416211699682,-18.0000807006055,
0.));
#196651=CARTESIAN_POINT('Ctrl Pts',(-15.8603277532834,-18.010329682521,
0.));
#196652=CARTESIAN_POINT('Ctrl Pts',(-15.8791496788685,-18.0205781695773,
0.));
#196653=CARTESIAN_POINT('Ctrl Pts',(-15.8980864711043,-18.0308254604638,
0.));
#196654=CARTESIAN_POINT('Ctrl Pts',(-15.9171376582436,-18.0410708624208,
0.));
#196655=CARTESIAN_POINT('Ctrl Pts',(-15.9363027723244,-18.0513136910691,
0.));
#196656=CARTESIAN_POINT('Ctrl Pts',(-15.9555813490645,-18.061553270236,
0.));
#196657=CARTESIAN_POINT('Ctrl Pts',(-15.9749729277848,-18.071788931796,
0.));
#196658=CARTESIAN_POINT('Ctrl Pts',(-15.9944770513616,-18.0820200155238,
0.));
#196659=CARTESIAN_POINT('Ctrl Pts',(-16.0140932661612,-18.0922458689464,
0.));
#196660=CARTESIAN_POINT('Ctrl Pts',(-16.0338211219694,-18.1024658471966,
0.));
#196661=CARTESIAN_POINT('Ctrl Pts',(-16.0536601719124,-18.1126793128688,
0.));
#196662=CARTESIAN_POINT('Ctrl Pts',(-16.0736099723665,-18.1228856358746,
0.));
#196663=CARTESIAN_POINT('Ctrl Pts',(-16.0936700829108,-18.1330841933099,
0.));
#196664=CARTESIAN_POINT('Ctrl Pts',(-16.1138400662791,-18.1432743693231,
0.));
#196665=CARTESIAN_POINT('Ctrl Pts',(-16.1341194882987,-18.153455554985,
0.));
#196666=CARTESIAN_POINT('Ctrl Pts',(-16.1545079178261,-18.1636271481616,
0.));
#196667=CARTESIAN_POINT('Ctrl Pts',(-16.1750049266673,-18.1737885533852,
0.));
#196668=CARTESIAN_POINT('Ctrl Pts',(-16.1956100895076,-18.1839391817335,
0.));
#196669=CARTESIAN_POINT('Ctrl Pts',(-16.2163229838878,-18.1940784507232,
0.));
#196670=CARTESIAN_POINT('Ctrl Pts',(-16.237143190164,-18.2042057842037,
0.));
#196671=CARTESIAN_POINT('Ctrl Pts',(-16.2580702914615,-18.214320612253,
0.));
#196672=CARTESIAN_POINT('Ctrl Pts',(-16.2791038736223,-18.2244223710745,
0.));
#196673=CARTESIAN_POINT('Ctrl Pts',(-16.3002435251378,-18.2345105028981,
0.));
#196674=CARTESIAN_POINT('Ctrl Pts',(-16.3214888370988,-18.2445844558742,
0.));
#196675=CARTESIAN_POINT('Ctrl Pts',(-16.342839403159,-18.2546436839609,
0.));
#196676=CARTESIAN_POINT('Ctrl Pts',(-16.3642948194869,-18.2646876468169,
0.));
#196677=CARTESIAN_POINT('Ctrl Pts',(-16.385854684708,-18.2747158096934,
0.));
#196678=CARTESIAN_POINT('Ctrl Pts',(-16.4075185998454,-18.2847276433308,
0.));
#196679=CARTESIAN_POINT('Ctrl Pts',(-16.4292861682377,-18.2947226238509,
0.));
#196680=CARTESIAN_POINT('Ctrl Pts',(-16.4511569955231,-18.3047002326858,
0.));
#196681=CARTESIAN_POINT('Ctrl Pts',(-16.4731306896439,-18.3146599565229,
0.));
#196682=CARTESIAN_POINT('Ctrl Pts',(-16.4952068608344,-18.3246012872468,
0.));
#196683=CARTESIAN_POINT('Ctrl Pts',(-16.5173851216045,-18.3345237218864,
0.));
#196684=CARTESIAN_POINT('Ctrl Pts',(-16.539665086714,-18.3444267625601,
0.));
#196685=CARTESIAN_POINT('Ctrl Pts',(-16.5620463731414,-18.3543099164331,
0.));
#196686=CARTESIAN_POINT('Ctrl Pts',(-16.5845286000219,-18.364172695589,
0.));
#196687=CARTESIAN_POINT('Ctrl Pts',(-16.6071113885711,-18.3740146168879,
0.));
#196688=CARTESIAN_POINT('Ctrl Pts',(-16.6297943620056,-18.3838352018327,
0.));
#196689=CARTESIAN_POINT('Ctrl Pts',(-16.6525771454513,-18.3936339764332,
0.));
#196690=CARTESIAN_POINT('Ctrl Pts',(-16.6754593658513,-18.4034104710789,
0.));
#196691=CARTESIAN_POINT('Ctrl Pts',(-16.698440651849,-18.4131642203989,
0.));
#196692=CARTESIAN_POINT('Ctrl Pts',(-16.7215206338818,-18.4228947633186,
0.));
#196693=CARTESIAN_POINT('Ctrl Pts',(-16.7446989442882,-18.4326016431392,
0.));
#196694=CARTESIAN_POINT('Ctrl Pts',(-16.7679752173992,-18.4422844076099,
0.));
#196695=CARTESIAN_POINT('Ctrl Pts',(-16.791349089629,-18.4519426090124,
0.));
#196696=CARTESIAN_POINT('Ctrl Pts',(-16.8148201995472,-18.4615758042305,
0.));
#196697=CARTESIAN_POINT('Ctrl Pts',(-16.8383881879707,-18.4711835548622,
0.));
#196698=CARTESIAN_POINT('Ctrl Pts',(-16.8620526977169,-18.4807654268769,
0.));
#196699=CARTESIAN_POINT('Ctrl Pts',(-16.8858133733086,-18.4903209902226,
0.));
#196700=CARTESIAN_POINT('Ctrl Pts',(-16.9096698606942,-18.4998498184619,
0.));
#196701=CARTESIAN_POINT('Ctrl Pts',(-16.9336218069353,-18.5093514883835,
0.));
#196702=CARTESIAN_POINT('Ctrl Pts',(-16.957668859934,-18.518825579666,0.));
#196703=CARTESIAN_POINT('Ctrl Pts',(-16.9818106680382,-18.5282716744198,
0.));
#196704=CARTESIAN_POINT('Ctrl Pts',(-17.0060468805099,-18.5376893576961,
0.));
#196705=CARTESIAN_POINT('Ctrl Pts',(-17.030377148174,-18.5470782182089,
0.));
#196706=CARTESIAN_POINT('Ctrl Pts',(-17.0548011239751,-18.5564378489628,
0.));
#196707=CARTESIAN_POINT('Ctrl Pts',(-17.0793184636079,-18.5657678479788,
0.));
#196708=CARTESIAN_POINT('Ctrl Pts',(-17.1039288260002,-18.5750678188543,
0.));
#196709=CARTESIAN_POINT('Ctrl Pts',(-17.1286318741185,-18.5843373717253,
0.));
#196710=CARTESIAN_POINT('Ctrl Pts',(-17.1534272741646,-18.5935761222833,
0.));
#196711=CARTESIAN_POINT('Ctrl Pts',(-17.1783146940131,-18.6027836898826,
0.));
#196712=CARTESIAN_POINT('Ctrl Pts',(-17.2032938019288,-18.6119596959957,
0.));
#196713=CARTESIAN_POINT('Ctrl Pts',(-17.2283642650519,-18.6211037624041,
0.));
#196714=CARTESIAN_POINT('Ctrl Pts',(-17.2535257482186,-18.630215509794,
0.));
#196715=CARTESIAN_POINT('Ctrl Pts',(-17.278777912021,-18.639294555474,0.));
#196716=CARTESIAN_POINT('Ctrl Pts',(-17.3041204135069,-18.6483405141853,
0.));
#196717=CARTESIAN_POINT('Ctrl Pts',(-17.3295529098612,-18.6573530024019,
0.));
#196718=CARTESIAN_POINT('Ctrl Pts',(-17.3550750612438,-18.6663316416569,
0.));
#196719=CARTESIAN_POINT('Ctrl Pts',(-17.3806865340744,-18.6752760624045,
0.));
#196720=CARTESIAN_POINT('Ctrl Pts',(-17.4063870038563,-18.6841859073472,
0.));
#196721=CARTESIAN_POINT('Ctrl Pts',(-17.4321761588148,-18.6930608357421,
0.));
#196722=CARTESIAN_POINT('Ctrl Pts',(-17.4580537012764,-18.7019005250322,
0.));
#196723=CARTESIAN_POINT('Ctrl Pts',(-17.4840193397176,-18.7107046613941,
0.));
#196724=CARTESIAN_POINT('Ctrl Pts',(-17.5100727820891,-18.7194729318127,
0.));
#196725=CARTESIAN_POINT('Ctrl Pts',(-17.5362137287604,-18.728205015716,
0.));
#196726=CARTESIAN_POINT('Ctrl Pts',(-17.5624418653248,-18.7369005764558,
0.));
#196727=CARTESIAN_POINT('Ctrl Pts',(-17.5887568561361,-18.7455592536667,
0.));
#196728=CARTESIAN_POINT('Ctrl Pts',(-17.6151583356989,-18.7541806530935,
0.));
#196729=CARTESIAN_POINT('Ctrl Pts',(-17.6416459210646,-18.7627643613138,
0.));
#196730=CARTESIAN_POINT('Ctrl Pts',(-17.6682192274197,-18.7713099642673,
0.));
#196731=CARTESIAN_POINT('Ctrl Pts',(-17.6948778822982,-18.7798170641305,
0.));
#196732=CARTESIAN_POINT('Ctrl Pts',(-17.7216215409019,-18.7882852976016,
0.));
#196733=CARTESIAN_POINT('Ctrl Pts',(-17.7484498996917,-18.7967143519444,
0.));
#196734=CARTESIAN_POINT('Ctrl Pts',(-17.7753627137898,-18.8051039860543,
0.));
#196735=CARTESIAN_POINT('Ctrl Pts',(-17.8023598011135,-18.8134540340581,
0.));
#196736=CARTESIAN_POINT('Ctrl Pts',(-17.8294410311105,-18.8217643886368,
0.));
#196737=CARTESIAN_POINT('Ctrl Pts',(-17.8566063174871,-18.8300349896187,
0.));
#196738=CARTESIAN_POINT('Ctrl Pts',(-17.8784057509434,-18.8366196462746,
0.));
#196739=CARTESIAN_POINT('Ctrl Pts',(-17.8947931177853,-18.8415402351882,
0.));
#196740=CARTESIAN_POINT('Ctrl Pts',(-17.9057348246611,-18.8448126709726,
0.));
#196741=CARTESIAN_POINT('Ctrl Pts',(-17.9112098770111,-18.8464468996588,
0.));
#196742=CARTESIAN_POINT('',(-17.9112098770111,-18.8464468996588,0.));
#196743=CARTESIAN_POINT('Origin',(-17.7219872369693,-12.1729687575668,0.));
#196744=CARTESIAN_POINT('',(-18.5896416359912,-12.7689476255363,0.));
#196745=CARTESIAN_POINT('',(-18.5896416359912,-12.7689476255363,0.));
#196746=CARTESIAN_POINT('',(-8.86099361848466,-6.08648437878338,0.));
#196747=CARTESIAN_POINT('Ctrl Pts',(-18.8464468996588,-17.9112098770111,
0.));
#196748=CARTESIAN_POINT('Ctrl Pts',(-18.8464468996588,-17.9112098770111,
12.));
#196749=CARTESIAN_POINT('Ctrl Pts',(-18.8448126709692,-17.9057348246595,
0.));
#196750=CARTESIAN_POINT('Ctrl Pts',(-18.8448126709692,-17.9057348246595,
12.));
#196751=CARTESIAN_POINT('Ctrl Pts',(-18.8415402351786,-17.8947931177807,
0.));
#196752=CARTESIAN_POINT('Ctrl Pts',(-18.8415402351786,-17.8947931177807,
12.));
#196753=CARTESIAN_POINT('Ctrl Pts',(-18.8366196462581,-17.8784057509356,
0.));
#196754=CARTESIAN_POINT('Ctrl Pts',(-18.8366196462581,-17.8784057509356,
12.));
#196755=CARTESIAN_POINT('Ctrl Pts',(-18.8300349895974,-17.8566063174771,
0.));
#196756=CARTESIAN_POINT('Ctrl Pts',(-18.8300349895974,-17.8566063174771,
12.));
#196757=CARTESIAN_POINT('Ctrl Pts',(-18.8217643886157,-17.8294410311006,
0.));
#196758=CARTESIAN_POINT('Ctrl Pts',(-18.8217643886157,-17.8294410311006,
12.));
#196759=CARTESIAN_POINT('Ctrl Pts',(-18.8134540340417,-17.8023598011057,
0.));
#196760=CARTESIAN_POINT('Ctrl Pts',(-18.8134540340417,-17.8023598011057,
12.));
#196761=CARTESIAN_POINT('Ctrl Pts',(-18.8051039860448,-17.7753627137853,
0.));
#196762=CARTESIAN_POINT('Ctrl Pts',(-18.8051039860448,-17.7753627137853,
12.));
#196763=CARTESIAN_POINT('Ctrl Pts',(-18.7967143519419,-17.7484498996905,
0.));
#196764=CARTESIAN_POINT('Ctrl Pts',(-18.7967143519419,-17.7484498996905,
12.));
#196765=CARTESIAN_POINT('Ctrl Pts',(-18.788285297605,-17.7216215409035,
0.));
#196766=CARTESIAN_POINT('Ctrl Pts',(-18.788285297605,-17.7216215409035,
12.));
#196767=CARTESIAN_POINT('Ctrl Pts',(-18.7798170641374,-17.6948778823014,
0.));
#196768=CARTESIAN_POINT('Ctrl Pts',(-18.7798170641374,-17.6948778823014,
12.));
#196769=CARTESIAN_POINT('Ctrl Pts',(-18.7713099642754,-17.6682192274236,
0.));
#196770=CARTESIAN_POINT('Ctrl Pts',(-18.7713099642754,-17.6682192274236,
12.));
#196771=CARTESIAN_POINT('Ctrl Pts',(-18.762764361321,-17.6416459210681,
0.));
#196772=CARTESIAN_POINT('Ctrl Pts',(-18.762764361321,-17.6416459210681,
12.));
#196773=CARTESIAN_POINT('Ctrl Pts',(-18.7541806530984,-17.6151583357012,
0.));
#196774=CARTESIAN_POINT('Ctrl Pts',(-18.7541806530984,-17.6151583357012,
12.));
#196775=CARTESIAN_POINT('Ctrl Pts',(-18.7455592536687,-17.5887568561371,
0.));
#196776=CARTESIAN_POINT('Ctrl Pts',(-18.7455592536687,-17.5887568561371,
12.));
#196777=CARTESIAN_POINT('Ctrl Pts',(-18.7369005764553,-17.5624418653245,
0.));
#196778=CARTESIAN_POINT('Ctrl Pts',(-18.7369005764553,-17.5624418653245,
12.));
#196779=CARTESIAN_POINT('Ctrl Pts',(-18.7282050157138,-17.5362137287593,
0.));
#196780=CARTESIAN_POINT('Ctrl Pts',(-18.7282050157138,-17.5362137287593,
12.));
#196781=CARTESIAN_POINT('Ctrl Pts',(-18.7194729318098,-17.5100727820876,
0.));
#196782=CARTESIAN_POINT('Ctrl Pts',(-18.7194729318098,-17.5100727820876,
12.));
#196783=CARTESIAN_POINT('Ctrl Pts',(-18.7107046613912,-17.4840193397162,
0.));
#196784=CARTESIAN_POINT('Ctrl Pts',(-18.7107046613912,-17.4840193397162,
12.));
#196785=CARTESIAN_POINT('Ctrl Pts',(-18.70190052503,-17.4580537012753,0.));
#196786=CARTESIAN_POINT('Ctrl Pts',(-18.70190052503,-17.4580537012753,12.));
#196787=CARTESIAN_POINT('Ctrl Pts',(-18.6930608357409,-17.4321761588142,
0.));
#196788=CARTESIAN_POINT('Ctrl Pts',(-18.6930608357409,-17.4321761588142,
12.));
#196789=CARTESIAN_POINT('Ctrl Pts',(-18.6841859073471,-17.4063870038562,
0.));
#196790=CARTESIAN_POINT('Ctrl Pts',(-18.6841859073471,-17.4063870038562,
12.));
#196791=CARTESIAN_POINT('Ctrl Pts',(-18.6752760624052,-17.3806865340747,
0.));
#196792=CARTESIAN_POINT('Ctrl Pts',(-18.6752760624052,-17.3806865340747,
12.));
#196793=CARTESIAN_POINT('Ctrl Pts',(-18.6663316416582,-17.3550750612443,
0.));
#196794=CARTESIAN_POINT('Ctrl Pts',(-18.6663316416582,-17.3550750612443,
12.));
#196795=CARTESIAN_POINT('Ctrl Pts',(-18.6573530024033,-17.3295529098618,
0.));
#196796=CARTESIAN_POINT('Ctrl Pts',(-18.6573530024033,-17.3295529098618,
12.));
#196797=CARTESIAN_POINT('Ctrl Pts',(-18.6483405141865,-17.3041204135074,
0.));
#196798=CARTESIAN_POINT('Ctrl Pts',(-18.6483405141865,-17.3041204135074,
12.));
#196799=CARTESIAN_POINT('Ctrl Pts',(-18.6392945554748,-17.2787779120213,
0.));
#196800=CARTESIAN_POINT('Ctrl Pts',(-18.6392945554748,-17.2787779120213,
12.));
#196801=CARTESIAN_POINT('Ctrl Pts',(-18.6302155097943,-17.2535257482187,
0.));
#196802=CARTESIAN_POINT('Ctrl Pts',(-18.6302155097943,-17.2535257482187,
12.));
#196803=CARTESIAN_POINT('Ctrl Pts',(-18.6211037624038,-17.2283642650518,
0.));
#196804=CARTESIAN_POINT('Ctrl Pts',(-18.6211037624038,-17.2283642650518,
12.));
#196805=CARTESIAN_POINT('Ctrl Pts',(-18.6119596959949,-17.2032938019284,
0.));
#196806=CARTESIAN_POINT('Ctrl Pts',(-18.6119596959949,-17.2032938019284,
12.));
#196807=CARTESIAN_POINT('Ctrl Pts',(-18.6027836898817,-17.1783146940127,
0.));
#196808=CARTESIAN_POINT('Ctrl Pts',(-18.6027836898817,-17.1783146940127,
12.));
#196809=CARTESIAN_POINT('Ctrl Pts',(-18.5935761222825,-17.1534272741643,
0.));
#196810=CARTESIAN_POINT('Ctrl Pts',(-18.5935761222825,-17.1534272741643,
12.));
#196811=CARTESIAN_POINT('Ctrl Pts',(-18.5843373717247,-17.1286318741183,
0.));
#196812=CARTESIAN_POINT('Ctrl Pts',(-18.5843373717247,-17.1286318741183,
12.));
#196813=CARTESIAN_POINT('Ctrl Pts',(-18.5750678188542,-17.1039288260001,
0.));
#196814=CARTESIAN_POINT('Ctrl Pts',(-18.5750678188542,-17.1039288260001,
12.));
#196815=CARTESIAN_POINT('Ctrl Pts',(-18.5657678479789,-17.0793184636079,
0.));
#196816=CARTESIAN_POINT('Ctrl Pts',(-18.5657678479789,-17.0793184636079,
12.));
#196817=CARTESIAN_POINT('Ctrl Pts',(-18.556437848963,-17.0548011239751,
0.));
#196818=CARTESIAN_POINT('Ctrl Pts',(-18.556437848963,-17.0548011239751,
12.));
#196819=CARTESIAN_POINT('Ctrl Pts',(-18.547078218209,-17.0303771481738,
0.));
#196820=CARTESIAN_POINT('Ctrl Pts',(-18.547078218209,-17.0303771481738,
12.));
#196821=CARTESIAN_POINT('Ctrl Pts',(-18.5376893576961,-17.0060468805097,
0.));
#196822=CARTESIAN_POINT('Ctrl Pts',(-18.5376893576961,-17.0060468805097,
12.));
#196823=CARTESIAN_POINT('Ctrl Pts',(-18.5282716744197,-16.981810668038,
0.));
#196824=CARTESIAN_POINT('Ctrl Pts',(-18.5282716744197,-16.981810668038,
12.));
#196825=CARTESIAN_POINT('Ctrl Pts',(-18.5188255796659,-16.9576688599339,
0.));
#196826=CARTESIAN_POINT('Ctrl Pts',(-18.5188255796659,-16.9576688599339,
12.));
#196827=CARTESIAN_POINT('Ctrl Pts',(-18.5093514883835,-16.9336218069353,
0.));
#196828=CARTESIAN_POINT('Ctrl Pts',(-18.5093514883835,-16.9336218069353,
12.));
#196829=CARTESIAN_POINT('Ctrl Pts',(-18.499849818462,-16.9096698606943,
0.));
#196830=CARTESIAN_POINT('Ctrl Pts',(-18.499849818462,-16.9096698606943,
12.));
#196831=CARTESIAN_POINT('Ctrl Pts',(-18.4903209902227,-16.8858133733088,
0.));
#196832=CARTESIAN_POINT('Ctrl Pts',(-18.4903209902227,-16.8858133733088,
12.));
#196833=CARTESIAN_POINT('Ctrl Pts',(-18.4807654268771,-16.8620526977171,
0.));
#196834=CARTESIAN_POINT('Ctrl Pts',(-18.4807654268771,-16.8620526977171,
12.));
#196835=CARTESIAN_POINT('Ctrl Pts',(-18.4711835548623,-16.8383881879709,
0.));
#196836=CARTESIAN_POINT('Ctrl Pts',(-18.4711835548623,-16.8383881879709,
12.));
#196837=CARTESIAN_POINT('Ctrl Pts',(-18.4615758042305,-16.8148201995472,
0.));
#196838=CARTESIAN_POINT('Ctrl Pts',(-18.4615758042305,-16.8148201995472,
12.));
#196839=CARTESIAN_POINT('Ctrl Pts',(-18.4519426090124,-16.791349089629,
0.));
#196840=CARTESIAN_POINT('Ctrl Pts',(-18.4519426090124,-16.791349089629,
12.));
#196841=CARTESIAN_POINT('Ctrl Pts',(-18.44228440761,-16.7679752173992,0.));
#196842=CARTESIAN_POINT('Ctrl Pts',(-18.44228440761,-16.7679752173992,12.));
#196843=CARTESIAN_POINT('Ctrl Pts',(-18.4326016431392,-16.7446989442882,
0.));
#196844=CARTESIAN_POINT('Ctrl Pts',(-18.4326016431392,-16.7446989442882,
12.));
#196845=CARTESIAN_POINT('Ctrl Pts',(-18.4228947633187,-16.7215206338818,
0.));
#196846=CARTESIAN_POINT('Ctrl Pts',(-18.4228947633187,-16.7215206338818,
12.));
#196847=CARTESIAN_POINT('Ctrl Pts',(-18.413164220399,-16.6984406518491,
0.));
#196848=CARTESIAN_POINT('Ctrl Pts',(-18.413164220399,-16.6984406518491,
12.));
#196849=CARTESIAN_POINT('Ctrl Pts',(-18.403410471079,-16.6754593658513,
0.));
#196850=CARTESIAN_POINT('Ctrl Pts',(-18.403410471079,-16.6754593658513,
12.));
#196851=CARTESIAN_POINT('Ctrl Pts',(-18.3936339764332,-16.6525771454513,
0.));
#196852=CARTESIAN_POINT('Ctrl Pts',(-18.3936339764332,-16.6525771454513,
12.));
#196853=CARTESIAN_POINT('Ctrl Pts',(-18.3838352018327,-16.6297943620056,
0.));
#196854=CARTESIAN_POINT('Ctrl Pts',(-18.3838352018327,-16.6297943620056,
12.));
#196855=CARTESIAN_POINT('Ctrl Pts',(-18.3740146168879,-16.607111388571,
0.));
#196856=CARTESIAN_POINT('Ctrl Pts',(-18.3740146168879,-16.607111388571,
12.));
#196857=CARTESIAN_POINT('Ctrl Pts',(-18.3641726955889,-16.5845286000217,
0.));
#196858=CARTESIAN_POINT('Ctrl Pts',(-18.3641726955889,-16.5845286000217,
12.));
#196859=CARTESIAN_POINT('Ctrl Pts',(-18.354309916433,-16.5620463731413,
0.));
#196860=CARTESIAN_POINT('Ctrl Pts',(-18.354309916433,-16.5620463731413,
12.));
#196861=CARTESIAN_POINT('Ctrl Pts',(-18.34442676256,-16.5396650867139,0.));
#196862=CARTESIAN_POINT('Ctrl Pts',(-18.34442676256,-16.5396650867139,12.));
#196863=CARTESIAN_POINT('Ctrl Pts',(-18.3345237218864,-16.5173851216045,
0.));
#196864=CARTESIAN_POINT('Ctrl Pts',(-18.3345237218864,-16.5173851216045,
12.));
#196865=CARTESIAN_POINT('Ctrl Pts',(-18.3246012872469,-16.4952068608345,
0.));
#196866=CARTESIAN_POINT('Ctrl Pts',(-18.3246012872469,-16.4952068608345,
12.));
#196867=CARTESIAN_POINT('Ctrl Pts',(-18.3146599565231,-16.4731306896441,
0.));
#196868=CARTESIAN_POINT('Ctrl Pts',(-18.3146599565231,-16.4731306896441,
12.));
#196869=CARTESIAN_POINT('Ctrl Pts',(-18.304700232686,-16.4511569955233,
0.));
#196870=CARTESIAN_POINT('Ctrl Pts',(-18.304700232686,-16.4511569955233,
12.));
#196871=CARTESIAN_POINT('Ctrl Pts',(-18.294722623851,-16.4292861682379,
0.));
#196872=CARTESIAN_POINT('Ctrl Pts',(-18.294722623851,-16.4292861682379,
12.));
#196873=CARTESIAN_POINT('Ctrl Pts',(-18.2847276433309,-16.4075185998455,
0.));
#196874=CARTESIAN_POINT('Ctrl Pts',(-18.2847276433309,-16.4075185998455,
12.));
#196875=CARTESIAN_POINT('Ctrl Pts',(-18.2747158096934,-16.385854684708,
0.));
#196876=CARTESIAN_POINT('Ctrl Pts',(-18.2747158096934,-16.385854684708,
12.));
#196877=CARTESIAN_POINT('Ctrl Pts',(-18.2646876468169,-16.3642948194868,
0.));
#196878=CARTESIAN_POINT('Ctrl Pts',(-18.2646876468169,-16.3642948194868,
12.));
#196879=CARTESIAN_POINT('Ctrl Pts',(-18.2546436839608,-16.3428394031589,
0.));
#196880=CARTESIAN_POINT('Ctrl Pts',(-18.2546436839608,-16.3428394031589,
12.));
#196881=CARTESIAN_POINT('Ctrl Pts',(-18.2445844558742,-16.3214888370987,
0.));
#196882=CARTESIAN_POINT('Ctrl Pts',(-18.2445844558742,-16.3214888370987,
12.));
#196883=CARTESIAN_POINT('Ctrl Pts',(-18.2345105028982,-16.3002435251378,
0.));
#196884=CARTESIAN_POINT('Ctrl Pts',(-18.2345105028982,-16.3002435251378,
12.));
#196885=CARTESIAN_POINT('Ctrl Pts',(-18.2244223710746,-16.2791038736223,
0.));
#196886=CARTESIAN_POINT('Ctrl Pts',(-18.2244223710746,-16.2791038736223,
12.));
#196887=CARTESIAN_POINT('Ctrl Pts',(-18.2143206122529,-16.2580702914615,
0.));
#196888=CARTESIAN_POINT('Ctrl Pts',(-18.2143206122529,-16.2580702914615,
12.));
#196889=CARTESIAN_POINT('Ctrl Pts',(-18.2042057842035,-16.2371431901638,
0.));
#196890=CARTESIAN_POINT('Ctrl Pts',(-18.2042057842035,-16.2371431901638,
12.));
#196891=CARTESIAN_POINT('Ctrl Pts',(-18.1940784507229,-16.2163229838875,
0.));
#196892=CARTESIAN_POINT('Ctrl Pts',(-18.1940784507229,-16.2163229838875,
12.));
#196893=CARTESIAN_POINT('Ctrl Pts',(-18.1839391817331,-16.1956100895073,
0.));
#196894=CARTESIAN_POINT('Ctrl Pts',(-18.1839391817331,-16.1956100895073,
12.));
#196895=CARTESIAN_POINT('Ctrl Pts',(-18.1737885533849,-16.1750049266671,
0.));
#196896=CARTESIAN_POINT('Ctrl Pts',(-18.1737885533849,-16.1750049266671,
12.));
#196897=CARTESIAN_POINT('Ctrl Pts',(-18.1636271481615,-16.154507917826,
0.));
#196898=CARTESIAN_POINT('Ctrl Pts',(-18.1636271481615,-16.154507917826,
12.));
#196899=CARTESIAN_POINT('Ctrl Pts',(-18.1534555549852,-16.1341194882988,
0.));
#196900=CARTESIAN_POINT('Ctrl Pts',(-18.1534555549852,-16.1341194882988,
12.));
#196901=CARTESIAN_POINT('Ctrl Pts',(-18.1432743693235,-16.1138400662794,
0.));
#196902=CARTESIAN_POINT('Ctrl Pts',(-18.1432743693235,-16.1138400662794,
12.));
#196903=CARTESIAN_POINT('Ctrl Pts',(-18.1330841933105,-16.0936700829112,
0.));
#196904=CARTESIAN_POINT('Ctrl Pts',(-18.1330841933105,-16.0936700829112,
12.));
#196905=CARTESIAN_POINT('Ctrl Pts',(-18.1228856358751,-16.0736099723668,
0.));
#196906=CARTESIAN_POINT('Ctrl Pts',(-18.1228856358751,-16.0736099723668,
12.));
#196907=CARTESIAN_POINT('Ctrl Pts',(-18.112679312869,-16.0536601719126,
0.));
#196908=CARTESIAN_POINT('Ctrl Pts',(-18.112679312869,-16.0536601719126,
12.));
#196909=CARTESIAN_POINT('Ctrl Pts',(-18.1024658471966,-16.0338211219693,
0.));
#196910=CARTESIAN_POINT('Ctrl Pts',(-18.1024658471966,-16.0338211219693,
12.));
#196911=CARTESIAN_POINT('Ctrl Pts',(-18.0922458689462,-16.014093266161,
0.));
#196912=CARTESIAN_POINT('Ctrl Pts',(-18.0922458689462,-16.014093266161,
12.));
#196913=CARTESIAN_POINT('Ctrl Pts',(-18.0820200155236,-15.9944770513613,
0.));
#196914=CARTESIAN_POINT('Ctrl Pts',(-18.0820200155236,-15.9944770513613,
12.));
#196915=CARTESIAN_POINT('Ctrl Pts',(-18.0717889317958,-15.9749729277846,
0.));
#196916=CARTESIAN_POINT('Ctrl Pts',(-18.0717889317958,-15.9749729277846,
12.));
#196917=CARTESIAN_POINT('Ctrl Pts',(-18.061553270236,-15.9555813490644,
0.));
#196918=CARTESIAN_POINT('Ctrl Pts',(-18.061553270236,-15.9555813490644,
12.));
#196919=CARTESIAN_POINT('Ctrl Pts',(-18.0513136910691,-15.9363027723244,
0.));
#196920=CARTESIAN_POINT('Ctrl Pts',(-18.0513136910691,-15.9363027723244,
12.));
#196921=CARTESIAN_POINT('Ctrl Pts',(-18.0410708624208,-15.9171376582436,
0.));
#196922=CARTESIAN_POINT('Ctrl Pts',(-18.0410708624208,-15.9171376582436,
12.));
#196923=CARTESIAN_POINT('Ctrl Pts',(-18.0308254604636,-15.8980864711042,
0.));
#196924=CARTESIAN_POINT('Ctrl Pts',(-18.0308254604636,-15.8980864711042,
12.));
#196925=CARTESIAN_POINT('Ctrl Pts',(-18.0205781695769,-15.8791496788682,
0.));
#196926=CARTESIAN_POINT('Ctrl Pts',(-18.0205781695769,-15.8791496788682,
12.));
#196927=CARTESIAN_POINT('Ctrl Pts',(-18.0103296825205,-15.8603277532831,
0.));
#196928=CARTESIAN_POINT('Ctrl Pts',(-18.0103296825205,-15.8603277532831,
12.));
#196929=CARTESIAN_POINT('Ctrl Pts',(-18.0000807006052,-15.8416211699679,
0.));
#196930=CARTESIAN_POINT('Ctrl Pts',(-18.0000807006052,-15.8416211699679,
12.));
#196931=CARTESIAN_POINT('Ctrl Pts',(-17.9898319338664,-15.8230304084962,
0.));
#196932=CARTESIAN_POINT('Ctrl Pts',(-17.9898319338664,-15.8230304084962,
12.));
#196933=CARTESIAN_POINT('Ctrl Pts',(-17.9795841012386,-15.8045559524676,
0.));
#196934=CARTESIAN_POINT('Ctrl Pts',(-17.9795841012386,-15.8045559524676,
12.));
#196935=CARTESIAN_POINT('Ctrl Pts',(-17.9693379307303,-15.7861982895724,
0.));
#196936=CARTESIAN_POINT('Ctrl Pts',(-17.9693379307303,-15.7861982895724,
12.));
#196937=CARTESIAN_POINT('Ctrl Pts',(-17.9590941596242,-15.7679579117077,
0.));
#196938=CARTESIAN_POINT('Ctrl Pts',(-17.9590941596242,-15.7679579117077,
12.));
#196939=CARTESIAN_POINT('Ctrl Pts',(-17.9488535346781,-15.749835315086,
0.));
#196940=CARTESIAN_POINT('Ctrl Pts',(-17.9488535346781,-15.749835315086,
12.));
#196941=CARTESIAN_POINT('Ctrl Pts',(-17.9386168123262,-15.7318310003335,
0.));
#196942=CARTESIAN_POINT('Ctrl Pts',(-17.9386168123262,-15.7318310003335,
12.));
#196943=CARTESIAN_POINT('Ctrl Pts',(-17.9283847588836,-15.7139454725838,
0.));
#196944=CARTESIAN_POINT('Ctrl Pts',(-17.9283847588836,-15.7139454725838,
12.));
#196945=CARTESIAN_POINT('Ctrl Pts',(-17.9181581507455,-15.6961792415522,
0.));
#196946=CARTESIAN_POINT('Ctrl Pts',(-17.9181581507455,-15.6961792415522,
12.));
#196947=CARTESIAN_POINT('Ctrl Pts',(-17.9079377746111,-15.678532821646,
0.));
#196948=CARTESIAN_POINT('Ctrl Pts',(-17.9079377746111,-15.678532821646,
12.));
#196949=CARTESIAN_POINT('Ctrl Pts',(-17.897724427724,-15.661006732103,0.));
#196950=CARTESIAN_POINT('Ctrl Pts',(-17.897724427724,-15.661006732103,12.));
#196951=CARTESIAN_POINT('Ctrl Pts',(-17.8875189181091,-15.6436014971084,
0.));
#196952=CARTESIAN_POINT('Ctrl Pts',(-17.8875189181091,-15.6436014971084,
12.));
#196953=CARTESIAN_POINT('Ctrl Pts',(-17.8773220648125,-15.6263176459108,
0.));
#196954=CARTESIAN_POINT('Ctrl Pts',(-17.8773220648125,-15.6263176459108,
12.));
#196955=CARTESIAN_POINT('Ctrl Pts',(-17.8671346981394,-15.609155712921,
0.));
#196956=CARTESIAN_POINT('Ctrl Pts',(-17.8671346981394,-15.609155712921,
12.));
#196957=CARTESIAN_POINT('Ctrl Pts',(-17.8569576599006,-15.5921162378192,
0.));
#196958=CARTESIAN_POINT('Ctrl Pts',(-17.8569576599006,-15.5921162378192,
12.));
#196959=CARTESIAN_POINT('Ctrl Pts',(-17.8467918036987,-15.5751997657163,
0.));
#196960=CARTESIAN_POINT('Ctrl Pts',(-17.8467918036987,-15.5751997657163,
12.));
#196961=CARTESIAN_POINT('Ctrl Pts',(-17.8366379952085,-15.5584068472982,
0.));
#196962=CARTESIAN_POINT('Ctrl Pts',(-17.8366379952085,-15.5584068472982,
12.));
#196963=CARTESIAN_POINT('Ctrl Pts',(-17.8264971124607,-15.541738038964,
0.));
#196964=CARTESIAN_POINT('Ctrl Pts',(-17.8264971124607,-15.541738038964,
12.));
#196965=CARTESIAN_POINT('Ctrl Pts',(-17.8163700461256,-15.5251939029552,
0.));
#196966=CARTESIAN_POINT('Ctrl Pts',(-17.8163700461256,-15.5251939029552,
12.));
#196967=CARTESIAN_POINT('Ctrl Pts',(-17.8062576997952,-15.5087750074718,
0.));
#196968=CARTESIAN_POINT('Ctrl Pts',(-17.8062576997952,-15.5087750074718,
12.));
#196969=CARTESIAN_POINT('Ctrl Pts',(-17.7961609903148,-15.4924819268517,
0.));
#196970=CARTESIAN_POINT('Ctrl Pts',(-17.7961609903148,-15.4924819268517,
12.));
#196971=CARTESIAN_POINT('Ctrl Pts',(-17.786080848122,-15.4763152417497,
0.));
#196972=CARTESIAN_POINT('Ctrl Pts',(-17.786080848122,-15.4763152417497,
12.));
#196973=CARTESIAN_POINT('Ctrl Pts',(-17.7760182175815,-15.4602755393017,
0.));
#196974=CARTESIAN_POINT('Ctrl Pts',(-17.7760182175815,-15.4602755393017,
12.));
#196975=CARTESIAN_POINT('Ctrl Pts',(-17.7659740573265,-15.4443634132869,
0.));
#196976=CARTESIAN_POINT('Ctrl Pts',(-17.7659740573265,-15.4443634132869,
12.));
#196977=CARTESIAN_POINT('Ctrl Pts',(-17.7559493405881,-15.4285794642668,
0.));
#196978=CARTESIAN_POINT('Ctrl Pts',(-17.7559493405881,-15.4285794642668,
12.));
#196979=CARTESIAN_POINT('Ctrl Pts',(-17.7459450555812,-15.4129242997837,
0.));
#196980=CARTESIAN_POINT('Ctrl Pts',(-17.7459450555812,-15.4129242997837,
12.));
#196981=CARTESIAN_POINT('Ctrl Pts',(-17.735962205915,-15.3973985345802,
0.));
#196982=CARTESIAN_POINT('Ctrl Pts',(-17.735962205915,-15.3973985345802,
12.));
#196983=CARTESIAN_POINT('Ctrl Pts',(-17.7260018109924,-15.3820027907967,
0.));
#196984=CARTESIAN_POINT('Ctrl Pts',(-17.7260018109924,-15.3820027907967,
12.));
#196985=CARTESIAN_POINT('Ctrl Pts',(-17.7160649064206,-15.3667376981699,
0.));
#196986=CARTESIAN_POINT('Ctrl Pts',(-17.7160649064206,-15.3667376981699,
12.));
#196987=CARTESIAN_POINT('Ctrl Pts',(-17.7061525444042,-15.351603894206,
0.));
#196988=CARTESIAN_POINT('Ctrl Pts',(-17.7061525444042,-15.351603894206,
12.));
#196989=CARTESIAN_POINT('Ctrl Pts',(-17.6962657941983,-15.3366020244066,
0.));
#196990=CARTESIAN_POINT('Ctrl Pts',(-17.6962657941983,-15.3366020244066,
12.));
#196991=CARTESIAN_POINT('Ctrl Pts',(-17.6864057426052,-15.3217327425338,
0.));
#196992=CARTESIAN_POINT('Ctrl Pts',(-17.6864057426052,-15.3217327425338,
12.));
#196993=CARTESIAN_POINT('Ctrl Pts',(-17.676573494456,-15.3069967108501,
0.));
#196994=CARTESIAN_POINT('Ctrl Pts',(-17.676573494456,-15.3069967108501,
12.));
#196995=CARTESIAN_POINT('Ctrl Pts',(-17.6667701731041,-15.2923946003598,
0.));
#196996=CARTESIAN_POINT('Ctrl Pts',(-17.6667701731041,-15.2923946003598,
12.));
#196997=CARTESIAN_POINT('Ctrl Pts',(-17.6569969209,-15.2779270910239,0.));
#196998=CARTESIAN_POINT('Ctrl Pts',(-17.6569969209,-15.2779270910239,12.));
#196999=CARTESIAN_POINT('Ctrl Pts',(-17.6472548997328,-15.2635948720292,
0.));
#197000=CARTESIAN_POINT('Ctrl Pts',(-17.6472548997328,-15.2635948720292,
12.));
#197001=CARTESIAN_POINT('Ctrl Pts',(-17.6375452916369,-15.2493986421092,
0.));
#197002=CARTESIAN_POINT('Ctrl Pts',(-17.6375452916369,-15.2493986421092,
12.));
#197003=CARTESIAN_POINT('Ctrl Pts',(-17.6278692993764,-15.2353391098366,
0.));
#197004=CARTESIAN_POINT('Ctrl Pts',(-17.6278692993764,-15.2353391098366,
12.));
#197005=CARTESIAN_POINT('Ctrl Pts',(-17.6182281470468,-15.2214169939199,
0.));
#197006=CARTESIAN_POINT('Ctrl Pts',(-17.6182281470468,-15.2214169939199,
12.));
#197007=CARTESIAN_POINT('Ctrl Pts',(-17.60862308065,-15.2076330234686,0.));
#197008=CARTESIAN_POINT('Ctrl Pts',(-17.60862308065,-15.2076330234686,12.));
#197009=CARTESIAN_POINT('Ctrl Pts',(-17.5990553687599,-15.1939879383268,
0.));
#197010=CARTESIAN_POINT('Ctrl Pts',(-17.5990553687599,-15.1939879383268,
12.));
#197011=CARTESIAN_POINT('Ctrl Pts',(-17.5895263032595,-15.1804824894605,
0.));
#197012=CARTESIAN_POINT('Ctrl Pts',(-17.5895263032595,-15.1804824894605,
12.));
#197013=CARTESIAN_POINT('Ctrl Pts',(-17.580037200054,-15.1671174393137,
0.));
#197014=CARTESIAN_POINT('Ctrl Pts',(-17.580037200054,-15.1671174393137,
12.));
#197015=CARTESIAN_POINT('Ctrl Pts',(-17.5705893998029,-15.1538935621714,
0.));
#197016=CARTESIAN_POINT('Ctrl Pts',(-17.5705893998029,-15.1538935621714,
12.));
#197017=CARTESIAN_POINT('Ctrl Pts',(-17.5611842686192,-15.1408116444876,
0.));
#197018=CARTESIAN_POINT('Ctrl Pts',(-17.5611842686192,-15.1408116444876,
12.));
#197019=CARTESIAN_POINT('Ctrl Pts',(-17.5518231989117,-15.1278724853138,
0.));
#197020=CARTESIAN_POINT('Ctrl Pts',(-17.5518231989117,-15.1278724853138,
12.));
#197021=CARTESIAN_POINT('Ctrl Pts',(-17.5425076102963,-15.1150768967728,
0.));
#197022=CARTESIAN_POINT('Ctrl Pts',(-17.5425076102963,-15.1150768967728,
12.));
#197023=CARTESIAN_POINT('Ctrl Pts',(-17.5332389504829,-15.1024257045033,
0.));
#197024=CARTESIAN_POINT('Ctrl Pts',(-17.5332389504829,-15.1024257045033,
12.));
#197025=CARTESIAN_POINT('Ctrl Pts',(-17.5240186961791,-15.0899197481082,
0.));
#197026=CARTESIAN_POINT('Ctrl Pts',(-17.5240186961791,-15.0899197481082,
12.));
#197027=CARTESIAN_POINT('Ctrl Pts',(-17.5148483539687,-15.0775598815749,
0.));
#197028=CARTESIAN_POINT('Ctrl Pts',(-17.5148483539687,-15.0775598815749,
12.));
#197029=CARTESIAN_POINT('Ctrl Pts',(-17.5057294613877,-15.0653469738307,
0.));
#197030=CARTESIAN_POINT('Ctrl Pts',(-17.5057294613877,-15.0653469738307,
12.));
#197031=CARTESIAN_POINT('Ctrl Pts',(-17.4966635880246,-15.0532819093085,
0.));
#197032=CARTESIAN_POINT('Ctrl Pts',(-17.4966635880246,-15.0532819093085,
12.));
#197033=CARTESIAN_POINT('Ctrl Pts',(-17.4876523366178,-15.0413655884993,
0.));
#197034=CARTESIAN_POINT('Ctrl Pts',(-17.4876523366178,-15.0413655884993,
12.));
#197035=CARTESIAN_POINT('Ctrl Pts',(-17.4786973441417,-15.029598928488,
0.));
#197036=CARTESIAN_POINT('Ctrl Pts',(-17.4786973441417,-15.029598928488,
12.));
#197037=CARTESIAN_POINT('Ctrl Pts',(-17.4698002829357,-15.0179828635087,
0.));
#197038=CARTESIAN_POINT('Ctrl Pts',(-17.4698002829357,-15.0179828635087,
12.));
#197039=CARTESIAN_POINT('Ctrl Pts',(-17.4609628621419,-15.0065183456922,
0.));
#197040=CARTESIAN_POINT('Ctrl Pts',(-17.4609628621419,-15.0065183456922,
12.));
#197041=CARTESIAN_POINT('Ctrl Pts',(-17.4521868291005,-14.9952063457779,
0.));
#197042=CARTESIAN_POINT('Ctrl Pts',(-17.4521868291005,-14.9952063457779,
12.));
#197043=CARTESIAN_POINT('Ctrl Pts',(-17.4434739707773,-14.9840478538357,
0.));
#197044=CARTESIAN_POINT('Ctrl Pts',(-17.4434739707773,-14.9840478538357,
12.));
#197045=CARTESIAN_POINT('Ctrl Pts',(-17.4348261151395,-14.973043879945,
0.));
#197046=CARTESIAN_POINT('Ctrl Pts',(-17.4348261151395,-14.973043879945,
12.));
#197047=CARTESIAN_POINT('Ctrl Pts',(-17.4262451327088,-14.9621954549825,
0.));
#197048=CARTESIAN_POINT('Ctrl Pts',(-17.4262451327088,-14.9621954549825,
12.));
#197049=CARTESIAN_POINT('Ctrl Pts',(-17.4177329382827,-14.9515036315142,
0.));
#197050=CARTESIAN_POINT('Ctrl Pts',(-17.4177329382827,-14.9515036315142,
12.));
#197051=CARTESIAN_POINT('Ctrl Pts',(-17.4092914926071,-14.940969484645,
0.));
#197052=CARTESIAN_POINT('Ctrl Pts',(-17.4092914926071,-14.940969484645,
12.));
#197053=CARTESIAN_POINT('Ctrl Pts',(-17.400922804075,-14.9305941128758,
0.));
#197054=CARTESIAN_POINT('Ctrl Pts',(-17.400922804075,-14.9305941128758,
12.));
#197055=CARTESIAN_POINT('Ctrl Pts',(-17.3926289303987,-14.9203786389343,
0.));
#197056=CARTESIAN_POINT('Ctrl Pts',(-17.3926289303987,-14.9203786389343,
12.));
#197057=CARTESIAN_POINT('Ctrl Pts',(-17.3844119809823,-14.9103242110057,
0.));
#197058=CARTESIAN_POINT('Ctrl Pts',(-17.3844119809823,-14.9103242110057,
12.));
#197059=CARTESIAN_POINT('Ctrl Pts',(-17.3762741193075,-14.9004320039609,
0.));
#197060=CARTESIAN_POINT('Ctrl Pts',(-17.3762741193075,-14.9004320039609,
12.));
#197061=CARTESIAN_POINT('Ctrl Pts',(-17.3682175653236,-14.8907032205789,
0.));
#197062=CARTESIAN_POINT('Ctrl Pts',(-17.3682175653236,-14.8907032205789,
12.));
#197063=CARTESIAN_POINT('Ctrl Pts',(-17.3602445978163,-14.8811390927424,
0.));
#197064=CARTESIAN_POINT('Ctrl Pts',(-17.3602445978163,-14.8811390927424,
12.));
#197065=CARTESIAN_POINT('Ctrl Pts',(-17.3523575568648,-14.8717408826958,
0.));
#197066=CARTESIAN_POINT('Ctrl Pts',(-17.3523575568648,-14.8717408826958,
12.));
#197067=CARTESIAN_POINT('Ctrl Pts',(-17.3445588463477,-14.8625098843419,
0.));
#197068=CARTESIAN_POINT('Ctrl Pts',(-17.3445588463477,-14.8625098843419,
12.));
#197069=CARTESIAN_POINT('Ctrl Pts',(-17.336850936485,-14.8534474245433,
0.));
#197070=CARTESIAN_POINT('Ctrl Pts',(-17.336850936485,-14.8534474245433,
12.));
#197071=CARTESIAN_POINT('Ctrl Pts',(-17.3292363662601,-14.8445548643505,
0.));
#197072=CARTESIAN_POINT('Ctrl Pts',(-17.3292363662601,-14.8445548643505,
12.));
#197073=CARTESIAN_POINT('Ctrl Pts',(-17.3217177462096,-14.8358336004193,
0.));
#197074=CARTESIAN_POINT('Ctrl Pts',(-17.3217177462096,-14.8358336004193,
12.));
#197075=CARTESIAN_POINT('Ctrl Pts',(-17.3142977632656,-14.8272850675375,
0.));
#197076=CARTESIAN_POINT('Ctrl Pts',(-17.3142977632656,-14.8272850675375,
12.));
#197077=CARTESIAN_POINT('Ctrl Pts',(-17.3069791853705,-14.8189107410161,
0.));
#197078=CARTESIAN_POINT('Ctrl Pts',(-17.3069791853705,-14.8189107410161,
12.));
#197079=CARTESIAN_POINT('Ctrl Pts',(-17.2997648661483,-14.8107121391038,
0.));
#197080=CARTESIAN_POINT('Ctrl Pts',(-17.2997648661483,-14.8107121391038,
12.));
#197081=CARTESIAN_POINT('Ctrl Pts',(-17.2926577496519,-14.8026908254281,
0.));
#197082=CARTESIAN_POINT('Ctrl Pts',(-17.2926577496519,-14.8026908254281,
12.));
#197083=CARTESIAN_POINT('Ctrl Pts',(-17.28566087332,-14.7948484105253,0.));
#197084=CARTESIAN_POINT('Ctrl Pts',(-17.28566087332,-14.7948484105253,12.));
#197085=CARTESIAN_POINT('Ctrl Pts',(-17.278777370485,-14.787186553128,0.));
#197086=CARTESIAN_POINT('Ctrl Pts',(-17.278777370485,-14.787186553128,12.));
#197087=CARTESIAN_POINT('Ctrl Pts',(-17.2720104735192,-14.7797069617802,
0.));
#197088=CARTESIAN_POINT('Ctrl Pts',(-17.2720104735192,-14.7797069617802,
12.));
#197089=CARTESIAN_POINT('Ctrl Pts',(-17.2653635155317,-14.7724113956728,
0.));
#197090=CARTESIAN_POINT('Ctrl Pts',(-17.2653635155317,-14.7724113956728,
12.));
#197091=CARTESIAN_POINT('Ctrl Pts',(-17.2588399401464,-14.7653016697589,
0.));
#197092=CARTESIAN_POINT('Ctrl Pts',(-17.2588399401464,-14.7653016697589,
12.));
#197093=CARTESIAN_POINT('Ctrl Pts',(-17.2524433146837,-14.7583796616617,
0.));
#197094=CARTESIAN_POINT('Ctrl Pts',(-17.2524433146837,-14.7583796616617,
12.));
#197095=CARTESIAN_POINT('Ctrl Pts',(-17.2461773413289,-14.7516473175125,
0.));
#197096=CARTESIAN_POINT('Ctrl Pts',(-17.2461773413289,-14.7516473175125,
12.));
#197097=CARTESIAN_POINT('Ctrl Pts',(-17.2400458713566,-14.7451066593793,
0.));
#197098=CARTESIAN_POINT('Ctrl Pts',(-17.2400458713566,-14.7451066593793,
12.));
#197099=CARTESIAN_POINT('Ctrl Pts',(-17.2340529062077,-14.7387597858117,
0.));
#197100=CARTESIAN_POINT('Ctrl Pts',(-17.2340529062077,-14.7387597858117,
12.));
#197101=CARTESIAN_POINT('Ctrl Pts',(-17.2282025904314,-14.7326088681163,
0.));
#197102=CARTESIAN_POINT('Ctrl Pts',(-17.2282025904314,-14.7326088681163,
12.));
#197103=CARTESIAN_POINT('Ctrl Pts',(-17.2224992099666,-14.7266561494282,
0.));
#197104=CARTESIAN_POINT('Ctrl Pts',(-17.2224992099666,-14.7266561494282,
12.));
#197105=CARTESIAN_POINT('Ctrl Pts',(-17.2169471814255,-14.7209039390326,
0.));
#197106=CARTESIAN_POINT('Ctrl Pts',(-17.2169471814255,-14.7209039390326,
12.));
#197107=CARTESIAN_POINT('Ctrl Pts',(-17.2115510835988,-14.7153546289338,
0.));
#197108=CARTESIAN_POINT('Ctrl Pts',(-17.2115510835988,-14.7153546289338,
12.));
#197109=CARTESIAN_POINT('Ctrl Pts',(-17.2063157097316,-14.7100107213586,
0.));
#197110=CARTESIAN_POINT('Ctrl Pts',(-17.2063157097316,-14.7100107213586,
12.));
#197111=CARTESIAN_POINT('Ctrl Pts',(-17.2012461084268,-14.7048748502663,
0.));
#197112=CARTESIAN_POINT('Ctrl Pts',(-17.2012461084268,-14.7048748502663,
12.));
#197113=CARTESIAN_POINT('Ctrl Pts',(-17.1963476411694,-14.699949811582,
0.));
#197114=CARTESIAN_POINT('Ctrl Pts',(-17.1963476411694,-14.699949811582,
12.));
#197115=CARTESIAN_POINT('Ctrl Pts',(-17.1916259308416,-14.6952385361706,
0.));
#197116=CARTESIAN_POINT('Ctrl Pts',(-17.1916259308416,-14.6952385361706,
12.));
#197117=CARTESIAN_POINT('Ctrl Pts',(-17.1870867909918,-14.6907440526958,
0.));
#197118=CARTESIAN_POINT('Ctrl Pts',(-17.1870867909918,-14.6907440526958,
12.));
#197119=CARTESIAN_POINT('Ctrl Pts',(-17.182736158472,-14.6864694522319,
0.));
#197120=CARTESIAN_POINT('Ctrl Pts',(-17.182736158472,-14.6864694522319,
12.));
#197121=CARTESIAN_POINT('Ctrl Pts',(-17.1785800350827,-14.6824178576167,
0.));
#197122=CARTESIAN_POINT('Ctrl Pts',(-17.1785800350827,-14.6824178576167,
12.));
#197123=CARTESIAN_POINT('Ctrl Pts',(-17.1746247499057,-14.6785925615676,
0.));
#197124=CARTESIAN_POINT('Ctrl Pts',(-17.1746247499057,-14.6785925615676,
12.));
#197125=CARTESIAN_POINT('Ctrl Pts',(-17.1708771619129,-14.6749971333867,
0.));
#197126=CARTESIAN_POINT('Ctrl Pts',(-17.1708771619129,-14.6749971333867,
12.));
#197127=CARTESIAN_POINT('Ctrl Pts',(-17.1673449723019,-14.6716355833321,
0.));
#197128=CARTESIAN_POINT('Ctrl Pts',(-17.1673449723019,-14.6716355833321,
12.));
#197129=CARTESIAN_POINT('Ctrl Pts',(-17.1640366762304,-14.6685123374424,
0.));
#197130=CARTESIAN_POINT('Ctrl Pts',(-17.1640366762304,-14.6685123374424,
12.));
#197131=CARTESIAN_POINT('Ctrl Pts',(-17.1609609517369,-14.6656319165057,
0.));
#197132=CARTESIAN_POINT('Ctrl Pts',(-17.1609609517369,-14.6656319165057,
12.));
#197133=CARTESIAN_POINT('Ctrl Pts',(-17.1581262646789,-14.662998728599,
0.));
#197134=CARTESIAN_POINT('Ctrl Pts',(-17.1581262646789,-14.662998728599,
12.));
#197135=CARTESIAN_POINT('Ctrl Pts',(-17.1555401986403,-14.660616716964,
0.));
#197136=CARTESIAN_POINT('Ctrl Pts',(-17.1555401986403,-14.660616716964,
12.));
#197137=CARTESIAN_POINT('Ctrl Pts',(-17.1532107762719,-14.6584900555301,
0.));
#197138=CARTESIAN_POINT('Ctrl Pts',(-17.1532107762719,-14.6584900555301,
12.));
#197139=CARTESIAN_POINT('Ctrl Pts',(-17.1511476869495,-14.6566237952435,
0.));
#197140=CARTESIAN_POINT('Ctrl Pts',(-17.1511476869495,-14.6566237952435,
12.));
#197141=CARTESIAN_POINT('Ctrl Pts',(-17.1493641837556,-14.6550248622813,
0.));
#197142=CARTESIAN_POINT('Ctrl Pts',(-17.1493641837556,-14.6550248622813,
12.));
#197143=CARTESIAN_POINT('Ctrl Pts',(-17.1478763944909,-14.6537016966188,
0.));
#197144=CARTESIAN_POINT('Ctrl Pts',(-17.1478763944909,-14.6537016966188,
12.));
#197145=CARTESIAN_POINT('Ctrl Pts',(-17.1466998098673,-14.6526624064978,
0.));
#197146=CARTESIAN_POINT('Ctrl Pts',(-17.1466998098673,-14.6526624064978,
12.));
#197147=CARTESIAN_POINT('Ctrl Pts',(-17.1458462295273,-14.65191316345,0.));
#197148=CARTESIAN_POINT('Ctrl Pts',(-17.1458462295273,-14.65191316345,12.));
#197149=CARTESIAN_POINT('Ctrl Pts',(-17.1454262858045,-14.6515481598057,
0.));
#197150=CARTESIAN_POINT('Ctrl Pts',(-17.1454262858045,-14.6515481598057,
12.));
#197151=CARTESIAN_POINT('Ctrl Pts',(-17.1452600887039,-14.6514066997188,
0.));
#197152=CARTESIAN_POINT('Ctrl Pts',(-17.1452600887039,-14.6514066997188,
12.));
#197153=CARTESIAN_POINT('Ctrl Pts',(-17.1452153999142,-14.651371185284,
0.));
#197154=CARTESIAN_POINT('Ctrl Pts',(-17.1452153999142,-14.651371185284,
12.));
#197155=CARTESIAN_POINT('Ctrl Pts',(-17.1452095830633,-14.6513681262571,
0.));
#197156=CARTESIAN_POINT('Ctrl Pts',(-17.1452095830633,-14.6513681262571,
12.));
#197157=CARTESIAN_POINT('',(-18.8464468996588,-17.9112098770111,0.));
#197158=CARTESIAN_POINT('Ctrl Pts',(-18.8464468996588,-17.9112098770111,
0.));
#197159=CARTESIAN_POINT('Ctrl Pts',(-18.8448126709692,-17.9057348246595,
0.));
#197160=CARTESIAN_POINT('Ctrl Pts',(-18.8415402351786,-17.8947931177807,
0.));
#197161=CARTESIAN_POINT('Ctrl Pts',(-18.8366196462581,-17.8784057509356,
0.));
#197162=CARTESIAN_POINT('Ctrl Pts',(-18.8300349895974,-17.8566063174771,
0.));
#197163=CARTESIAN_POINT('Ctrl Pts',(-18.8217643886157,-17.8294410311006,
0.));
#197164=CARTESIAN_POINT('Ctrl Pts',(-18.8134540340417,-17.8023598011057,
0.));
#197165=CARTESIAN_POINT('Ctrl Pts',(-18.8051039860448,-17.7753627137853,
0.));
#197166=CARTESIAN_POINT('Ctrl Pts',(-18.7967143519419,-17.7484498996905,
0.));
#197167=CARTESIAN_POINT('Ctrl Pts',(-18.788285297605,-17.7216215409035,
0.));
#197168=CARTESIAN_POINT('Ctrl Pts',(-18.7798170641374,-17.6948778823014,
0.));
#197169=CARTESIAN_POINT('Ctrl Pts',(-18.7713099642754,-17.6682192274236,
0.));
#197170=CARTESIAN_POINT('Ctrl Pts',(-18.762764361321,-17.6416459210681,
0.));
#197171=CARTESIAN_POINT('Ctrl Pts',(-18.7541806530984,-17.6151583357012,
0.));
#197172=CARTESIAN_POINT('Ctrl Pts',(-18.7455592536687,-17.5887568561371,
0.));
#197173=CARTESIAN_POINT('Ctrl Pts',(-18.7369005764553,-17.5624418653245,
0.));
#197174=CARTESIAN_POINT('Ctrl Pts',(-18.7282050157138,-17.5362137287593,
0.));
#197175=CARTESIAN_POINT('Ctrl Pts',(-18.7194729318098,-17.5100727820876,
0.));
#197176=CARTESIAN_POINT('Ctrl Pts',(-18.7107046613912,-17.4840193397162,
0.));
#197177=CARTESIAN_POINT('Ctrl Pts',(-18.70190052503,-17.4580537012753,0.));
#197178=CARTESIAN_POINT('Ctrl Pts',(-18.6930608357409,-17.4321761588142,
0.));
#197179=CARTESIAN_POINT('Ctrl Pts',(-18.6841859073471,-17.4063870038562,
0.));
#197180=CARTESIAN_POINT('Ctrl Pts',(-18.6752760624052,-17.3806865340747,
0.));
#197181=CARTESIAN_POINT('Ctrl Pts',(-18.6663316416582,-17.3550750612443,
0.));
#197182=CARTESIAN_POINT('Ctrl Pts',(-18.6573530024033,-17.3295529098618,
0.));
#197183=CARTESIAN_POINT('Ctrl Pts',(-18.6483405141865,-17.3041204135074,
0.));
#197184=CARTESIAN_POINT('Ctrl Pts',(-18.6392945554748,-17.2787779120213,
0.));
#197185=CARTESIAN_POINT('Ctrl Pts',(-18.6302155097943,-17.2535257482187,
0.));
#197186=CARTESIAN_POINT('Ctrl Pts',(-18.6211037624038,-17.2283642650518,
0.));
#197187=CARTESIAN_POINT('Ctrl Pts',(-18.6119596959949,-17.2032938019284,
0.));
#197188=CARTESIAN_POINT('Ctrl Pts',(-18.6027836898817,-17.1783146940127,
0.));
#197189=CARTESIAN_POINT('Ctrl Pts',(-18.5935761222825,-17.1534272741643,
0.));
#197190=CARTESIAN_POINT('Ctrl Pts',(-18.5843373717247,-17.1286318741183,
0.));
#197191=CARTESIAN_POINT('Ctrl Pts',(-18.5750678188542,-17.1039288260001,
0.));
#197192=CARTESIAN_POINT('Ctrl Pts',(-18.5657678479789,-17.0793184636079,
0.));
#197193=CARTESIAN_POINT('Ctrl Pts',(-18.556437848963,-17.0548011239751,
0.));
#197194=CARTESIAN_POINT('Ctrl Pts',(-18.547078218209,-17.0303771481738,
0.));
#197195=CARTESIAN_POINT('Ctrl Pts',(-18.5376893576961,-17.0060468805097,
0.));
#197196=CARTESIAN_POINT('Ctrl Pts',(-18.5282716744197,-16.981810668038,
0.));
#197197=CARTESIAN_POINT('Ctrl Pts',(-18.5188255796659,-16.9576688599339,
0.));
#197198=CARTESIAN_POINT('Ctrl Pts',(-18.5093514883835,-16.9336218069353,
0.));
#197199=CARTESIAN_POINT('Ctrl Pts',(-18.499849818462,-16.9096698606943,
0.));
#197200=CARTESIAN_POINT('Ctrl Pts',(-18.4903209902227,-16.8858133733088,
0.));
#197201=CARTESIAN_POINT('Ctrl Pts',(-18.4807654268771,-16.8620526977171,
0.));
#197202=CARTESIAN_POINT('Ctrl Pts',(-18.4711835548623,-16.8383881879709,
0.));
#197203=CARTESIAN_POINT('Ctrl Pts',(-18.4615758042305,-16.8148201995472,
0.));
#197204=CARTESIAN_POINT('Ctrl Pts',(-18.4519426090124,-16.791349089629,
0.));
#197205=CARTESIAN_POINT('Ctrl Pts',(-18.44228440761,-16.7679752173992,0.));
#197206=CARTESIAN_POINT('Ctrl Pts',(-18.4326016431392,-16.7446989442882,
0.));
#197207=CARTESIAN_POINT('Ctrl Pts',(-18.4228947633187,-16.7215206338818,
0.));
#197208=CARTESIAN_POINT('Ctrl Pts',(-18.413164220399,-16.6984406518491,
0.));
#197209=CARTESIAN_POINT('Ctrl Pts',(-18.403410471079,-16.6754593658513,
0.));
#197210=CARTESIAN_POINT('Ctrl Pts',(-18.3936339764332,-16.6525771454513,
0.));
#197211=CARTESIAN_POINT('Ctrl Pts',(-18.3838352018327,-16.6297943620056,
0.));
#197212=CARTESIAN_POINT('Ctrl Pts',(-18.3740146168879,-16.607111388571,
0.));
#197213=CARTESIAN_POINT('Ctrl Pts',(-18.3641726955889,-16.5845286000217,
0.));
#197214=CARTESIAN_POINT('Ctrl Pts',(-18.354309916433,-16.5620463731413,
0.));
#197215=CARTESIAN_POINT('Ctrl Pts',(-18.34442676256,-16.5396650867139,0.));
#197216=CARTESIAN_POINT('Ctrl Pts',(-18.3345237218864,-16.5173851216045,
0.));
#197217=CARTESIAN_POINT('Ctrl Pts',(-18.3246012872469,-16.4952068608345,
0.));
#197218=CARTESIAN_POINT('Ctrl Pts',(-18.3146599565231,-16.4731306896441,
0.));
#197219=CARTESIAN_POINT('Ctrl Pts',(-18.304700232686,-16.4511569955233,
0.));
#197220=CARTESIAN_POINT('Ctrl Pts',(-18.294722623851,-16.4292861682379,
0.));
#197221=CARTESIAN_POINT('Ctrl Pts',(-18.2847276433309,-16.4075185998455,
0.));
#197222=CARTESIAN_POINT('Ctrl Pts',(-18.2747158096934,-16.385854684708,
0.));
#197223=CARTESIAN_POINT('Ctrl Pts',(-18.2646876468169,-16.3642948194868,
0.));
#197224=CARTESIAN_POINT('Ctrl Pts',(-18.2546436839608,-16.3428394031589,
0.));
#197225=CARTESIAN_POINT('Ctrl Pts',(-18.2445844558742,-16.3214888370987,
0.));
#197226=CARTESIAN_POINT('Ctrl Pts',(-18.2345105028982,-16.3002435251378,
0.));
#197227=CARTESIAN_POINT('Ctrl Pts',(-18.2244223710746,-16.2791038736223,
0.));
#197228=CARTESIAN_POINT('Ctrl Pts',(-18.2143206122529,-16.2580702914615,
0.));
#197229=CARTESIAN_POINT('Ctrl Pts',(-18.2042057842035,-16.2371431901638,
0.));
#197230=CARTESIAN_POINT('Ctrl Pts',(-18.1940784507229,-16.2163229838875,
0.));
#197231=CARTESIAN_POINT('Ctrl Pts',(-18.1839391817331,-16.1956100895073,
0.));
#197232=CARTESIAN_POINT('Ctrl Pts',(-18.1737885533849,-16.1750049266671,
0.));
#197233=CARTESIAN_POINT('Ctrl Pts',(-18.1636271481615,-16.154507917826,
0.));
#197234=CARTESIAN_POINT('Ctrl Pts',(-18.1534555549852,-16.1341194882988,
0.));
#197235=CARTESIAN_POINT('Ctrl Pts',(-18.1432743693235,-16.1138400662794,
0.));
#197236=CARTESIAN_POINT('Ctrl Pts',(-18.1330841933105,-16.0936700829112,
0.));
#197237=CARTESIAN_POINT('Ctrl Pts',(-18.1228856358751,-16.0736099723668,
0.));
#197238=CARTESIAN_POINT('Ctrl Pts',(-18.112679312869,-16.0536601719126,
0.));
#197239=CARTESIAN_POINT('Ctrl Pts',(-18.1024658471966,-16.0338211219693,
0.));
#197240=CARTESIAN_POINT('Ctrl Pts',(-18.0922458689462,-16.014093266161,
0.));
#197241=CARTESIAN_POINT('Ctrl Pts',(-18.0820200155236,-15.9944770513613,
0.));
#197242=CARTESIAN_POINT('Ctrl Pts',(-18.0717889317958,-15.9749729277846,
0.));
#197243=CARTESIAN_POINT('Ctrl Pts',(-18.061553270236,-15.9555813490644,
0.));
#197244=CARTESIAN_POINT('Ctrl Pts',(-18.0513136910691,-15.9363027723244,
0.));
#197245=CARTESIAN_POINT('Ctrl Pts',(-18.0410708624208,-15.9171376582436,
0.));
#197246=CARTESIAN_POINT('Ctrl Pts',(-18.0308254604636,-15.8980864711042,
0.));
#197247=CARTESIAN_POINT('Ctrl Pts',(-18.0205781695769,-15.8791496788682,
0.));
#197248=CARTESIAN_POINT('Ctrl Pts',(-18.0103296825205,-15.8603277532831,
0.));
#197249=CARTESIAN_POINT('Ctrl Pts',(-18.0000807006052,-15.8416211699679,
0.));
#197250=CARTESIAN_POINT('Ctrl Pts',(-17.9898319338664,-15.8230304084962,
0.));
#197251=CARTESIAN_POINT('Ctrl Pts',(-17.9795841012386,-15.8045559524676,
0.));
#197252=CARTESIAN_POINT('Ctrl Pts',(-17.9693379307303,-15.7861982895724,
0.));
#197253=CARTESIAN_POINT('Ctrl Pts',(-17.9590941596242,-15.7679579117077,
0.));
#197254=CARTESIAN_POINT('Ctrl Pts',(-17.9488535346781,-15.749835315086,
0.));
#197255=CARTESIAN_POINT('Ctrl Pts',(-17.9386168123262,-15.7318310003335,
0.));
#197256=CARTESIAN_POINT('Ctrl Pts',(-17.9283847588836,-15.7139454725838,
0.));
#197257=CARTESIAN_POINT('Ctrl Pts',(-17.9181581507455,-15.6961792415522,
0.));
#197258=CARTESIAN_POINT('Ctrl Pts',(-17.9079377746111,-15.678532821646,
0.));
#197259=CARTESIAN_POINT('Ctrl Pts',(-17.897724427724,-15.661006732103,0.));
#197260=CARTESIAN_POINT('Ctrl Pts',(-17.8875189181091,-15.6436014971084,
0.));
#197261=CARTESIAN_POINT('Ctrl Pts',(-17.8773220648125,-15.6263176459108,
0.));
#197262=CARTESIAN_POINT('Ctrl Pts',(-17.8671346981394,-15.609155712921,
0.));
#197263=CARTESIAN_POINT('Ctrl Pts',(-17.8569576599006,-15.5921162378192,
0.));
#197264=CARTESIAN_POINT('Ctrl Pts',(-17.8467918036987,-15.5751997657163,
0.));
#197265=CARTESIAN_POINT('Ctrl Pts',(-17.8366379952085,-15.5584068472982,
0.));
#197266=CARTESIAN_POINT('Ctrl Pts',(-17.8264971124607,-15.541738038964,
0.));
#197267=CARTESIAN_POINT('Ctrl Pts',(-17.8163700461256,-15.5251939029552,
0.));
#197268=CARTESIAN_POINT('Ctrl Pts',(-17.8062576997952,-15.5087750074718,
0.));
#197269=CARTESIAN_POINT('Ctrl Pts',(-17.7961609903148,-15.4924819268517,
0.));
#197270=CARTESIAN_POINT('Ctrl Pts',(-17.786080848122,-15.4763152417497,
0.));
#197271=CARTESIAN_POINT('Ctrl Pts',(-17.7760182175815,-15.4602755393017,
0.));
#197272=CARTESIAN_POINT('Ctrl Pts',(-17.7659740573265,-15.4443634132869,
0.));
#197273=CARTESIAN_POINT('Ctrl Pts',(-17.7559493405881,-15.4285794642668,
0.));
#197274=CARTESIAN_POINT('Ctrl Pts',(-17.7459450555812,-15.4129242997837,
0.));
#197275=CARTESIAN_POINT('Ctrl Pts',(-17.735962205915,-15.3973985345802,
0.));
#197276=CARTESIAN_POINT('Ctrl Pts',(-17.7260018109924,-15.3820027907967,
0.));
#197277=CARTESIAN_POINT('Ctrl Pts',(-17.7160649064206,-15.3667376981699,
0.));
#197278=CARTESIAN_POINT('Ctrl Pts',(-17.7061525444042,-15.351603894206,
0.));
#197279=CARTESIAN_POINT('Ctrl Pts',(-17.6962657941983,-15.3366020244066,
0.));
#197280=CARTESIAN_POINT('Ctrl Pts',(-17.6864057426052,-15.3217327425338,
0.));
#197281=CARTESIAN_POINT('Ctrl Pts',(-17.676573494456,-15.3069967108501,
0.));
#197282=CARTESIAN_POINT('Ctrl Pts',(-17.6667701731041,-15.2923946003598,
0.));
#197283=CARTESIAN_POINT('Ctrl Pts',(-17.6569969209,-15.2779270910239,0.));
#197284=CARTESIAN_POINT('Ctrl Pts',(-17.6472548997328,-15.2635948720292,
0.));
#197285=CARTESIAN_POINT('Ctrl Pts',(-17.6375452916369,-15.2493986421092,
0.));
#197286=CARTESIAN_POINT('Ctrl Pts',(-17.6278692993764,-15.2353391098366,
0.));
#197287=CARTESIAN_POINT('Ctrl Pts',(-17.6182281470468,-15.2214169939199,
0.));
#197288=CARTESIAN_POINT('Ctrl Pts',(-17.60862308065,-15.2076330234686,0.));
#197289=CARTESIAN_POINT('Ctrl Pts',(-17.5990553687599,-15.1939879383268,
0.));
#197290=CARTESIAN_POINT('Ctrl Pts',(-17.5895263032595,-15.1804824894605,
0.));
#197291=CARTESIAN_POINT('Ctrl Pts',(-17.580037200054,-15.1671174393137,
0.));
#197292=CARTESIAN_POINT('Ctrl Pts',(-17.5705893998029,-15.1538935621714,
0.));
#197293=CARTESIAN_POINT('Ctrl Pts',(-17.5611842686192,-15.1408116444876,
0.));
#197294=CARTESIAN_POINT('Ctrl Pts',(-17.5518231989117,-15.1278724853138,
0.));
#197295=CARTESIAN_POINT('Ctrl Pts',(-17.5425076102963,-15.1150768967728,
0.));
#197296=CARTESIAN_POINT('Ctrl Pts',(-17.5332389504829,-15.1024257045033,
0.));
#197297=CARTESIAN_POINT('Ctrl Pts',(-17.5240186961791,-15.0899197481082,
0.));
#197298=CARTESIAN_POINT('Ctrl Pts',(-17.5148483539687,-15.0775598815749,
0.));
#197299=CARTESIAN_POINT('Ctrl Pts',(-17.5057294613877,-15.0653469738307,
0.));
#197300=CARTESIAN_POINT('Ctrl Pts',(-17.4966635880246,-15.0532819093085,
0.));
#197301=CARTESIAN_POINT('Ctrl Pts',(-17.4876523366178,-15.0413655884993,
0.));
#197302=CARTESIAN_POINT('Ctrl Pts',(-17.4786973441417,-15.029598928488,
0.));
#197303=CARTESIAN_POINT('Ctrl Pts',(-17.4698002829357,-15.0179828635087,
0.));
#197304=CARTESIAN_POINT('Ctrl Pts',(-17.4609628621419,-15.0065183456922,
0.));
#197305=CARTESIAN_POINT('Ctrl Pts',(-17.4521868291005,-14.9952063457779,
0.));
#197306=CARTESIAN_POINT('Ctrl Pts',(-17.4434739707773,-14.9840478538357,
0.));
#197307=CARTESIAN_POINT('Ctrl Pts',(-17.4348261151395,-14.973043879945,
0.));
#197308=CARTESIAN_POINT('Ctrl Pts',(-17.4262451327088,-14.9621954549825,
0.));
#197309=CARTESIAN_POINT('Ctrl Pts',(-17.4177329382827,-14.9515036315142,
0.));
#197310=CARTESIAN_POINT('Ctrl Pts',(-17.4092914926071,-14.940969484645,
0.));
#197311=CARTESIAN_POINT('Ctrl Pts',(-17.400922804075,-14.9305941128758,
0.));
#197312=CARTESIAN_POINT('Ctrl Pts',(-17.3926289303987,-14.9203786389343,
0.));
#197313=CARTESIAN_POINT('Ctrl Pts',(-17.3844119809823,-14.9103242110057,
0.));
#197314=CARTESIAN_POINT('Ctrl Pts',(-17.3762741193075,-14.9004320039609,
0.));
#197315=CARTESIAN_POINT('Ctrl Pts',(-17.3682175653236,-14.8907032205789,
0.));
#197316=CARTESIAN_POINT('Ctrl Pts',(-17.3602445978163,-14.8811390927424,
0.));
#197317=CARTESIAN_POINT('Ctrl Pts',(-17.3523575568648,-14.8717408826958,
0.));
#197318=CARTESIAN_POINT('Ctrl Pts',(-17.3445588463477,-14.8625098843419,
0.));
#197319=CARTESIAN_POINT('Ctrl Pts',(-17.336850936485,-14.8534474245433,
0.));
#197320=CARTESIAN_POINT('Ctrl Pts',(-17.3292363662601,-14.8445548643505,
0.));
#197321=CARTESIAN_POINT('Ctrl Pts',(-17.3217177462096,-14.8358336004193,
0.));
#197322=CARTESIAN_POINT('Ctrl Pts',(-17.3142977632656,-14.8272850675375,
0.));
#197323=CARTESIAN_POINT('Ctrl Pts',(-17.3069791853705,-14.8189107410161,
0.));
#197324=CARTESIAN_POINT('Ctrl Pts',(-17.2997648661483,-14.8107121391038,
0.));
#197325=CARTESIAN_POINT('Ctrl Pts',(-17.2926577496519,-14.8026908254281,
0.));
#197326=CARTESIAN_POINT('Ctrl Pts',(-17.28566087332,-14.7948484105253,0.));
#197327=CARTESIAN_POINT('Ctrl Pts',(-17.278777370485,-14.787186553128,0.));
#197328=CARTESIAN_POINT('Ctrl Pts',(-17.2720104735192,-14.7797069617802,
0.));
#197329=CARTESIAN_POINT('Ctrl Pts',(-17.2653635155317,-14.7724113956728,
0.));
#197330=CARTESIAN_POINT('Ctrl Pts',(-17.2588399401464,-14.7653016697589,
0.));
#197331=CARTESIAN_POINT('Ctrl Pts',(-17.2524433146837,-14.7583796616617,
0.));
#197332=CARTESIAN_POINT('Ctrl Pts',(-17.2461773413289,-14.7516473175125,
0.));
#197333=CARTESIAN_POINT('Ctrl Pts',(-17.2400458713566,-14.7451066593793,
0.));
#197334=CARTESIAN_POINT('Ctrl Pts',(-17.2340529062077,-14.7387597858117,
0.));
#197335=CARTESIAN_POINT('Ctrl Pts',(-17.2282025904314,-14.7326088681163,
0.));
#197336=CARTESIAN_POINT('Ctrl Pts',(-17.2224992099666,-14.7266561494282,
0.));
#197337=CARTESIAN_POINT('Ctrl Pts',(-17.2169471814255,-14.7209039390326,
0.));
#197338=CARTESIAN_POINT('Ctrl Pts',(-17.2115510835988,-14.7153546289338,
0.));
#197339=CARTESIAN_POINT('Ctrl Pts',(-17.2063157097316,-14.7100107213586,
0.));
#197340=CARTESIAN_POINT('Ctrl Pts',(-17.2012461084268,-14.7048748502663,
0.));
#197341=CARTESIAN_POINT('Ctrl Pts',(-17.1963476411694,-14.699949811582,
0.));
#197342=CARTESIAN_POINT('Ctrl Pts',(-17.1916259308416,-14.6952385361706,
0.));
#197343=CARTESIAN_POINT('Ctrl Pts',(-17.1870867909918,-14.6907440526958,
0.));
#197344=CARTESIAN_POINT('Ctrl Pts',(-17.182736158472,-14.6864694522319,
0.));
#197345=CARTESIAN_POINT('Ctrl Pts',(-17.1785800350827,-14.6824178576167,
0.));
#197346=CARTESIAN_POINT('Ctrl Pts',(-17.1746247499057,-14.6785925615676,
0.));
#197347=CARTESIAN_POINT('Ctrl Pts',(-17.1708771619129,-14.6749971333867,
0.));
#197348=CARTESIAN_POINT('Ctrl Pts',(-17.1673449723019,-14.6716355833321,
0.));
#197349=CARTESIAN_POINT('Ctrl Pts',(-17.1640366762304,-14.6685123374424,
0.));
#197350=CARTESIAN_POINT('Ctrl Pts',(-17.1609609517369,-14.6656319165057,
0.));
#197351=CARTESIAN_POINT('Ctrl Pts',(-17.1581262646789,-14.662998728599,
0.));
#197352=CARTESIAN_POINT('Ctrl Pts',(-17.1555401986403,-14.660616716964,
0.));
#197353=CARTESIAN_POINT('Ctrl Pts',(-17.1532107762719,-14.6584900555301,
0.));
#197354=CARTESIAN_POINT('Ctrl Pts',(-17.1511476869495,-14.6566237952435,
0.));
#197355=CARTESIAN_POINT('Ctrl Pts',(-17.1493641837556,-14.6550248622813,
0.));
#197356=CARTESIAN_POINT('Ctrl Pts',(-17.1478763944909,-14.6537016966188,
0.));
#197357=CARTESIAN_POINT('Ctrl Pts',(-17.1466998098673,-14.6526624064978,
0.));
#197358=CARTESIAN_POINT('Ctrl Pts',(-17.1458462295273,-14.65191316345,0.));
#197359=CARTESIAN_POINT('Ctrl Pts',(-17.1454262858045,-14.6515481598057,
0.));
#197360=CARTESIAN_POINT('Ctrl Pts',(-17.1452600887039,-14.6514066997188,
0.));
#197361=CARTESIAN_POINT('Ctrl Pts',(-17.1452153999142,-14.651371185284,
0.));
#197362=CARTESIAN_POINT('Ctrl Pts',(-17.1452095830633,-14.6513681262571,
0.));
#197363=CARTESIAN_POINT('',(-18.8464468996588,-17.9112098770111,0.));
#197364=CARTESIAN_POINT('Ctrl Pts',(-18.5896416359912,-12.7689476255363,
0.));
#197365=CARTESIAN_POINT('Ctrl Pts',(-18.5896416359912,-12.7689476255363,
12.));
#197366=CARTESIAN_POINT('Ctrl Pts',(-18.5896460962964,-12.7689524524483,
0.));
#197367=CARTESIAN_POINT('Ctrl Pts',(-18.5896460962964,-12.7689524524483,
12.));
#197368=CARTESIAN_POINT('Ctrl Pts',(-18.5896919669165,-12.768986426692,
0.));
#197369=CARTESIAN_POINT('Ctrl Pts',(-18.5896919669165,-12.768986426692,
12.));
#197370=CARTESIAN_POINT('Ctrl Pts',(-18.589871621843,-12.769110348199,0.));
#197371=CARTESIAN_POINT('Ctrl Pts',(-18.589871621843,-12.769110348199,12.));
#197372=CARTESIAN_POINT('Ctrl Pts',(-18.5903328777227,-12.7694215127919,
0.));
#197373=CARTESIAN_POINT('Ctrl Pts',(-18.5903328777227,-12.7694215127919,
12.));
#197374=CARTESIAN_POINT('Ctrl Pts',(-18.5912775137806,-12.7700520897173,
0.));
#197375=CARTESIAN_POINT('Ctrl Pts',(-18.5912775137806,-12.7700520897173,
12.));
#197376=CARTESIAN_POINT('Ctrl Pts',(-18.5925859134579,-12.7709195951156,
0.));
#197377=CARTESIAN_POINT('Ctrl Pts',(-18.5925859134579,-12.7709195951156,
12.));
#197378=CARTESIAN_POINT('Ctrl Pts',(-18.5942490615407,-12.7720142287172,
0.));
#197379=CARTESIAN_POINT('Ctrl Pts',(-18.5942490615407,-12.7720142287172,
12.));
#197380=CARTESIAN_POINT('Ctrl Pts',(-18.5962551167772,-12.7733231262108,
0.));
#197381=CARTESIAN_POINT('Ctrl Pts',(-18.5962551167772,-12.7733231262108,
12.));
#197382=CARTESIAN_POINT('Ctrl Pts',(-18.598591752595,-12.7748328937638,
0.));
#197383=CARTESIAN_POINT('Ctrl Pts',(-18.598591752595,-12.7748328937638,
12.));
#197384=CARTESIAN_POINT('Ctrl Pts',(-18.6012488486709,-12.7765325225081,
0.));
#197385=CARTESIAN_POINT('Ctrl Pts',(-18.6012488486709,-12.7765325225081,
12.));
#197386=CARTESIAN_POINT('Ctrl Pts',(-18.6042190183704,-12.7784139605066,
0.));
#197387=CARTESIAN_POINT('Ctrl Pts',(-18.6042190183704,-12.7784139605066,
12.));
#197388=CARTESIAN_POINT('Ctrl Pts',(-18.6074961535723,-12.7804705387658,
0.));
#197389=CARTESIAN_POINT('Ctrl Pts',(-18.6074961535723,-12.7804705387658,
12.));
#197390=CARTESIAN_POINT('Ctrl Pts',(-18.6110744826219,-12.7826959526925,
0.));
#197391=CARTESIAN_POINT('Ctrl Pts',(-18.6110744826219,-12.7826959526925,
12.));
#197392=CARTESIAN_POINT('Ctrl Pts',(-18.6149475565188,-12.7850831657901,
0.));
#197393=CARTESIAN_POINT('Ctrl Pts',(-18.6149475565188,-12.7850831657901,
12.));
#197394=CARTESIAN_POINT('Ctrl Pts',(-18.6191087624752,-12.7876249657834,
0.));
#197395=CARTESIAN_POINT('Ctrl Pts',(-18.6191087624752,-12.7876249657834,
12.));
#197396=CARTESIAN_POINT('Ctrl Pts',(-18.6235516265575,-12.7903142925234,
0.));
#197397=CARTESIAN_POINT('Ctrl Pts',(-18.6235516265575,-12.7903142925234,
12.));
#197398=CARTESIAN_POINT('Ctrl Pts',(-18.6282702819371,-12.7931447451555,
0.));
#197399=CARTESIAN_POINT('Ctrl Pts',(-18.6282702819371,-12.7931447451555,
12.));
#197400=CARTESIAN_POINT('Ctrl Pts',(-18.6332595057006,-12.7961106222251,
0.));
#197401=CARTESIAN_POINT('Ctrl Pts',(-18.6332595057006,-12.7961106222251,
12.));
#197402=CARTESIAN_POINT('Ctrl Pts',(-18.63851447924,-12.7992066625264,0.));
#197403=CARTESIAN_POINT('Ctrl Pts',(-18.63851447924,-12.7992066625264,12.));
#197404=CARTESIAN_POINT('Ctrl Pts',(-18.6440306327456,-12.8024278770152,
0.));
#197405=CARTESIAN_POINT('Ctrl Pts',(-18.6440306327456,-12.8024278770152,
12.));
#197406=CARTESIAN_POINT('Ctrl Pts',(-18.6498034438987,-12.805769331162,
0.));
#197407=CARTESIAN_POINT('Ctrl Pts',(-18.6498034438987,-12.805769331162,
12.));
#197408=CARTESIAN_POINT('Ctrl Pts',(-18.6558284825773,-12.8092261933858,
0.));
#197409=CARTESIAN_POINT('Ctrl Pts',(-18.6558284825773,-12.8092261933858,
12.));
#197410=CARTESIAN_POINT('Ctrl Pts',(-18.6621014624746,-12.8127937909631,
0.));
#197411=CARTESIAN_POINT('Ctrl Pts',(-18.6621014624746,-12.8127937909631,
12.));
#197412=CARTESIAN_POINT('Ctrl Pts',(-18.6686182952799,-12.8164676687362,
0.));
#197413=CARTESIAN_POINT('Ctrl Pts',(-18.6686182952799,-12.8164676687362,
12.));
#197414=CARTESIAN_POINT('Ctrl Pts',(-18.6753751301092,-12.8202436318474,
0.));
#197415=CARTESIAN_POINT('Ctrl Pts',(-18.6753751301092,-12.8202436318474,
12.));
#197416=CARTESIAN_POINT('Ctrl Pts',(-18.6823683094139,-12.8241176980017,
0.));
#197417=CARTESIAN_POINT('Ctrl Pts',(-18.6823683094139,-12.8241176980017,
12.));
#197418=CARTESIAN_POINT('Ctrl Pts',(-18.6895943376171,-12.8280860635231,
0.));
#197419=CARTESIAN_POINT('Ctrl Pts',(-18.6895943376171,-12.8280860635231,
12.));
#197420=CARTESIAN_POINT('Ctrl Pts',(-18.6970498410172,-12.8321450599789,
0.));
#197421=CARTESIAN_POINT('Ctrl Pts',(-18.6970498410172,-12.8321450599789,
12.));
#197422=CARTESIAN_POINT('Ctrl Pts',(-18.7047315436294,-12.8362911280361,
0.));
#197423=CARTESIAN_POINT('Ctrl Pts',(-18.7047315436294,-12.8362911280361,
12.));
#197424=CARTESIAN_POINT('Ctrl Pts',(-18.7126362754445,-12.8405208263431,
0.));
#197425=CARTESIAN_POINT('Ctrl Pts',(-18.7126362754445,-12.8405208263431,
12.));
#197426=CARTESIAN_POINT('Ctrl Pts',(-18.7207609737702,-12.8448308329494,
0.));
#197427=CARTESIAN_POINT('Ctrl Pts',(-18.7207609737702,-12.8448308329494,
12.));
#197428=CARTESIAN_POINT('Ctrl Pts',(-18.7291026886554,-12.8492179511591,
0.));
#197429=CARTESIAN_POINT('Ctrl Pts',(-18.7291026886554,-12.8492179511591,
12.));
#197430=CARTESIAN_POINT('Ctrl Pts',(-18.7376585820854,-12.8536791086316,
0.));
#197431=CARTESIAN_POINT('Ctrl Pts',(-18.7376585820854,-12.8536791086316,
12.));
#197432=CARTESIAN_POINT('Ctrl Pts',(-18.7464259171251,-12.8582113455646,
0.));
#197433=CARTESIAN_POINT('Ctrl Pts',(-18.7464259171251,-12.8582113455646,
12.));
#197434=CARTESIAN_POINT('Ctrl Pts',(-18.7554020493887,-12.8628118054171,
0.));
#197435=CARTESIAN_POINT('Ctrl Pts',(-18.7554020493887,-12.8628118054171,
12.));
#197436=CARTESIAN_POINT('Ctrl Pts',(-18.7645844169564,-12.8674777239653,
0.));
#197437=CARTESIAN_POINT('Ctrl Pts',(-18.7645844169564,-12.8674777239653,
12.));
#197438=CARTESIAN_POINT('Ctrl Pts',(-18.7739705329022,-12.872206421181,
0.));
#197439=CARTESIAN_POINT('Ctrl Pts',(-18.7739705329022,-12.872206421181,
12.));
#197440=CARTESIAN_POINT('Ctrl Pts',(-18.7835579840477,-12.8769952998095,
0.));
#197441=CARTESIAN_POINT('Ctrl Pts',(-18.7835579840477,-12.8769952998095,
12.));
#197442=CARTESIAN_POINT('Ctrl Pts',(-18.7933444285868,-12.8818418427475,
0.));
#197443=CARTESIAN_POINT('Ctrl Pts',(-18.7933444285868,-12.8818418427475,
12.));
#197444=CARTESIAN_POINT('Ctrl Pts',(-18.8033275941943,-12.8867436109546,
0.));
#197445=CARTESIAN_POINT('Ctrl Pts',(-18.8033275941943,-12.8867436109546,
12.));
#197446=CARTESIAN_POINT('Ctrl Pts',(-18.813505275782,-12.8916982409935,
0.));
#197447=CARTESIAN_POINT('Ctrl Pts',(-18.813505275782,-12.8916982409935,
12.));
#197448=CARTESIAN_POINT('Ctrl Pts',(-18.8238753319129,-12.8967034410755,
0.));
#197449=CARTESIAN_POINT('Ctrl Pts',(-18.8238753319129,-12.8967034410755,
12.));
#197450=CARTESIAN_POINT('Ctrl Pts',(-18.834435681259,-12.9017569871738,
0.));
#197451=CARTESIAN_POINT('Ctrl Pts',(-18.834435681259,-12.9017569871738,
12.));
#197452=CARTESIAN_POINT('Ctrl Pts',(-18.8451842990984,-12.9068567191854,
0.));
#197453=CARTESIAN_POINT('Ctrl Pts',(-18.8451842990984,-12.9068567191854,
12.));
#197454=CARTESIAN_POINT('Ctrl Pts',(-18.8561192136198,-12.9120005369063,
0.));
#197455=CARTESIAN_POINT('Ctrl Pts',(-18.8561192136198,-12.9120005369063,
12.));
#197456=CARTESIAN_POINT('Ctrl Pts',(-18.8672385038326,-12.9171863977045,
0.));
#197457=CARTESIAN_POINT('Ctrl Pts',(-18.8672385038326,-12.9171863977045,
12.));
#197458=CARTESIAN_POINT('Ctrl Pts',(-18.8785402977527,-12.9224123144982,
0.));
#197459=CARTESIAN_POINT('Ctrl Pts',(-18.8785402977527,-12.9224123144982,
12.));
#197460=CARTESIAN_POINT('Ctrl Pts',(-18.8900227704889,-12.9276763536373,
0.));
#197461=CARTESIAN_POINT('Ctrl Pts',(-18.8900227704889,-12.9276763536373,
12.));
#197462=CARTESIAN_POINT('Ctrl Pts',(-18.9016841423403,-12.9329766328185,
0.));
#197463=CARTESIAN_POINT('Ctrl Pts',(-18.9016841423403,-12.9329766328185,
12.));
#197464=CARTESIAN_POINT('Ctrl Pts',(-18.9135226769465,-12.9383113190375,
0.));
#197465=CARTESIAN_POINT('Ctrl Pts',(-18.9135226769465,-12.9383113190375,
12.));
#197466=CARTESIAN_POINT('Ctrl Pts',(-18.9255366795195,-12.9436786266105,
0.));
#197467=CARTESIAN_POINT('Ctrl Pts',(-18.9255366795195,-12.9436786266105,
12.));
#197468=CARTESIAN_POINT('Ctrl Pts',(-18.9377244950435,-12.9490768151821,
0.));
#197469=CARTESIAN_POINT('Ctrl Pts',(-18.9377244950435,-12.9490768151821,
12.));
#197470=CARTESIAN_POINT('Ctrl Pts',(-18.9500845064715,-12.9545041877377,
0.));
#197471=CARTESIAN_POINT('Ctrl Pts',(-18.9500845064715,-12.9545041877377,
12.));
#197472=CARTESIAN_POINT('Ctrl Pts',(-18.9626151329229,-12.9599590886319,
0.));
#197473=CARTESIAN_POINT('Ctrl Pts',(-18.9626151329229,-12.9599590886319,
12.));
#197474=CARTESIAN_POINT('Ctrl Pts',(-18.9753148284475,-12.9654399021869,
0.));
#197475=CARTESIAN_POINT('Ctrl Pts',(-18.9753148284475,-12.9654399021869,
12.));
#197476=CARTESIAN_POINT('Ctrl Pts',(-18.9881820807586,-12.9709450512747,
0.));
#197477=CARTESIAN_POINT('Ctrl Pts',(-18.9881820807586,-12.9709450512747,
12.));
#197478=CARTESIAN_POINT('Ctrl Pts',(-19.0012154099791,-12.9764729959205,
0.));
#197479=CARTESIAN_POINT('Ctrl Pts',(-19.0012154099791,-12.9764729959205,
12.));
#197480=CARTESIAN_POINT('Ctrl Pts',(-19.0144133673348,-12.9820222318716,
0.));
#197481=CARTESIAN_POINT('Ctrl Pts',(-19.0144133673348,-12.9820222318716,
12.));
#197482=CARTESIAN_POINT('Ctrl Pts',(-19.0277745339908,-12.9875912893003,
0.));
#197483=CARTESIAN_POINT('Ctrl Pts',(-19.0277745339908,-12.9875912893003,
12.));
#197484=CARTESIAN_POINT('Ctrl Pts',(-19.0412975200398,-12.9931787316515,
0.));
#197485=CARTESIAN_POINT('Ctrl Pts',(-19.0412975200398,-12.9931787316515,
12.));
#197486=CARTESIAN_POINT('Ctrl Pts',(-19.0549809634355,-12.9987831544502,
0.));
#197487=CARTESIAN_POINT('Ctrl Pts',(-19.0549809634355,-12.9987831544502,
12.));
#197488=CARTESIAN_POINT('Ctrl Pts',(-19.0688235289437,-13.0044031841381,
0.));
#197489=CARTESIAN_POINT('Ctrl Pts',(-19.0688235289437,-13.0044031841381,
12.));
#197490=CARTESIAN_POINT('Ctrl Pts',(-19.0828239070482,-13.0100374768785,
0.));
#197491=CARTESIAN_POINT('Ctrl Pts',(-19.0828239070482,-13.0100374768785,
12.));
#197492=CARTESIAN_POINT('Ctrl Pts',(-19.0969808131226,-13.0156847176093,
0.));
#197493=CARTESIAN_POINT('Ctrl Pts',(-19.0969808131226,-13.0156847176093,
12.));
#197494=CARTESIAN_POINT('Ctrl Pts',(-19.1112929866308,-13.0213436191326,
0.));
#197495=CARTESIAN_POINT('Ctrl Pts',(-19.1112929866308,-13.0213436191326,
12.));
#197496=CARTESIAN_POINT('Ctrl Pts',(-19.1257591903099,-13.0270129211976,
0.));
#197497=CARTESIAN_POINT('Ctrl Pts',(-19.1257591903099,-13.0270129211976,
12.));
#197498=CARTESIAN_POINT('Ctrl Pts',(-19.1403782093389,-13.0326913895841,
0.));
#197499=CARTESIAN_POINT('Ctrl Pts',(-19.1403782093389,-13.0326913895841,
12.));
#197500=CARTESIAN_POINT('Ctrl Pts',(-19.1551488505233,-13.0383778152072,
0.));
#197501=CARTESIAN_POINT('Ctrl Pts',(-19.1551488505233,-13.0383778152072,
12.));
#197502=CARTESIAN_POINT('Ctrl Pts',(-19.1700699416625,-13.0440710133775,
0.));
#197503=CARTESIAN_POINT('Ctrl Pts',(-19.1700699416625,-13.0440710133775,
12.));
#197504=CARTESIAN_POINT('Ctrl Pts',(-19.1851403308825,-13.0497698230442,
0.));
#197505=CARTESIAN_POINT('Ctrl Pts',(-19.1851403308825,-13.0497698230442,
12.));
#197506=CARTESIAN_POINT('Ctrl Pts',(-19.2003588859771,-13.0554731060537,
0.));
#197507=CARTESIAN_POINT('Ctrl Pts',(-19.2003588859771,-13.0554731060537,
12.));
#197508=CARTESIAN_POINT('Ctrl Pts',(-19.2157244937141,-13.0611797463913,
0.));
#197509=CARTESIAN_POINT('Ctrl Pts',(-19.2157244937141,-13.0611797463913,
12.));
#197510=CARTESIAN_POINT('Ctrl Pts',(-19.2312360592031,-13.0668886494791,
0.));
#197511=CARTESIAN_POINT('Ctrl Pts',(-19.2312360592031,-13.0668886494791,
12.));
#197512=CARTESIAN_POINT('Ctrl Pts',(-19.2468925053988,-13.0725987415856,
0.));
#197513=CARTESIAN_POINT('Ctrl Pts',(-19.2468925053988,-13.0725987415856,
12.));
#197514=CARTESIAN_POINT('Ctrl Pts',(-19.2626927725596,-13.0783089692118,
0.));
#197515=CARTESIAN_POINT('Ctrl Pts',(-19.2626927725596,-13.0783089692118,
12.));
#197516=CARTESIAN_POINT('Ctrl Pts',(-19.2786358177198,-13.0840182984949,
0.));
#197517=CARTESIAN_POINT('Ctrl Pts',(-19.2786358177198,-13.0840182984949,
12.));
#197518=CARTESIAN_POINT('Ctrl Pts',(-19.2947206141246,-13.0897257145969,
0.));
#197519=CARTESIAN_POINT('Ctrl Pts',(-19.2947206141246,-13.0897257145969,
12.));
#197520=CARTESIAN_POINT('Ctrl Pts',(-19.3109461507358,-13.095430221148,
0.));
#197521=CARTESIAN_POINT('Ctrl Pts',(-19.3109461507358,-13.095430221148,
12.));
#197522=CARTESIAN_POINT('Ctrl Pts',(-19.3273114318268,-13.1011308397592,
0.));
#197523=CARTESIAN_POINT('Ctrl Pts',(-19.3273114318268,-13.1011308397592,
12.));
#197524=CARTESIAN_POINT('Ctrl Pts',(-19.3438154765395,-13.1068266095186,
0.));
#197525=CARTESIAN_POINT('Ctrl Pts',(-19.3438154765395,-13.1068266095186,
12.));
#197526=CARTESIAN_POINT('Ctrl Pts',(-19.3604573184516,-13.1125165865021,
0.));
#197527=CARTESIAN_POINT('Ctrl Pts',(-19.3604573184516,-13.1125165865021,
12.));
#197528=CARTESIAN_POINT('Ctrl Pts',(-19.3772360051093,-13.118199843271,
0.));
#197529=CARTESIAN_POINT('Ctrl Pts',(-19.3772360051093,-13.118199843271,
12.));
#197530=CARTESIAN_POINT('Ctrl Pts',(-19.3941505976267,-13.1238754684177,
0.));
#197531=CARTESIAN_POINT('Ctrl Pts',(-19.3941505976267,-13.1238754684177,
12.));
#197532=CARTESIAN_POINT('Ctrl Pts',(-19.4112001703561,-13.1295425661635,
0.));
#197533=CARTESIAN_POINT('Ctrl Pts',(-19.4112001703561,-13.1295425661635,
12.));
#197534=CARTESIAN_POINT('Ctrl Pts',(-19.4283838105265,-13.1352002559439,
0.));
#197535=CARTESIAN_POINT('Ctrl Pts',(-19.4283838105265,-13.1352002559439,
12.));
#197536=CARTESIAN_POINT('Ctrl Pts',(-19.4457006178875,-13.140847672006,
0.));
#197537=CARTESIAN_POINT('Ctrl Pts',(-19.4457006178875,-13.140847672006,
12.));
#197538=CARTESIAN_POINT('Ctrl Pts',(-19.463149704325,-13.1464839629966,
0.));
#197539=CARTESIAN_POINT('Ctrl Pts',(-19.463149704325,-13.1464839629966,
12.));
#197540=CARTESIAN_POINT('Ctrl Pts',(-19.4807301935256,-13.1521082915846,
0.));
#197541=CARTESIAN_POINT('Ctrl Pts',(-19.4807301935256,-13.1521082915846,
12.));
#197542=CARTESIAN_POINT('Ctrl Pts',(-19.498441220707,-13.1577198341238,
0.));
#197543=CARTESIAN_POINT('Ctrl Pts',(-19.498441220707,-13.1577198341238,
12.));
#197544=CARTESIAN_POINT('Ctrl Pts',(-19.5162819323207,-13.1633177803097,
0.));
#197545=CARTESIAN_POINT('Ctrl Pts',(-19.5162819323207,-13.1633177803097,
12.));
#197546=CARTESIAN_POINT('Ctrl Pts',(-19.5342514857564,-13.1689013328432,
0.));
#197547=CARTESIAN_POINT('Ctrl Pts',(-19.5342514857564,-13.1689013328432,
12.));
#197548=CARTESIAN_POINT('Ctrl Pts',(-19.5523490490254,-13.1744697070918,
0.));
#197549=CARTESIAN_POINT('Ctrl Pts',(-19.5523490490254,-13.1744697070918,
12.));
#197550=CARTESIAN_POINT('Ctrl Pts',(-19.5705738004682,-13.1800221307682,
0.));
#197551=CARTESIAN_POINT('Ctrl Pts',(-19.5705738004682,-13.1800221307682,
12.));
#197552=CARTESIAN_POINT('Ctrl Pts',(-19.5889249285352,-13.1855578436479,
0.));
#197553=CARTESIAN_POINT('Ctrl Pts',(-19.5889249285352,-13.1855578436479,
12.));
#197554=CARTESIAN_POINT('Ctrl Pts',(-19.6074016315421,-13.1910760972818,
0.));
#197555=CARTESIAN_POINT('Ctrl Pts',(-19.6074016315421,-13.1910760972818,
12.));
#197556=CARTESIAN_POINT('Ctrl Pts',(-19.6260031174244,-13.196576154715,
0.));
#197557=CARTESIAN_POINT('Ctrl Pts',(-19.6260031174244,-13.196576154715,
12.));
#197558=CARTESIAN_POINT('Ctrl Pts',(-19.6447286034764,-13.202057290206,
0.));
#197559=CARTESIAN_POINT('Ctrl Pts',(-19.6447286034764,-13.202057290206,
12.));
#197560=CARTESIAN_POINT('Ctrl Pts',(-19.6635773160924,-13.2075187889522,
0.));
#197561=CARTESIAN_POINT('Ctrl Pts',(-19.6635773160924,-13.2075187889522,
12.));
#197562=CARTESIAN_POINT('Ctrl Pts',(-19.6825484905812,-13.2129599468478,
0.));
#197563=CARTESIAN_POINT('Ctrl Pts',(-19.6825484905812,-13.2129599468478,
12.));
#197564=CARTESIAN_POINT('Ctrl Pts',(-19.7016413709678,-13.2183800702431,
0.));
#197565=CARTESIAN_POINT('Ctrl Pts',(-19.7016413709678,-13.2183800702431,
12.));
#197566=CARTESIAN_POINT('Ctrl Pts',(-19.7208552097867,-13.2237784757065,
0.));
#197567=CARTESIAN_POINT('Ctrl Pts',(-19.7208552097867,-13.2237784757065,
12.));
#197568=CARTESIAN_POINT('Ctrl Pts',(-19.7401892678701,-13.2291544897902,
0.));
#197569=CARTESIAN_POINT('Ctrl Pts',(-19.7401892678701,-13.2291544897902,
12.));
#197570=CARTESIAN_POINT('Ctrl Pts',(-19.7596428141176,-13.2345074487968,
0.));
#197571=CARTESIAN_POINT('Ctrl Pts',(-19.7596428141176,-13.2345074487968,
12.));
#197572=CARTESIAN_POINT('Ctrl Pts',(-19.7792151253297,-13.239836698568,
0.));
#197573=CARTESIAN_POINT('Ctrl Pts',(-19.7792151253297,-13.239836698568,
12.));
#197574=CARTESIAN_POINT('Ctrl Pts',(-19.7989054860501,-13.2451415942809,
0.));
#197575=CARTESIAN_POINT('Ctrl Pts',(-19.7989054860501,-13.2451415942809,
12.));
#197576=CARTESIAN_POINT('Ctrl Pts',(-19.8187131883919,-13.2504215002458,
0.));
#197577=CARTESIAN_POINT('Ctrl Pts',(-19.8187131883919,-13.2504215002458,
12.));
#197578=CARTESIAN_POINT('Ctrl Pts',(-19.8386375318632,-13.2556757897085,
0.));
#197579=CARTESIAN_POINT('Ctrl Pts',(-19.8386375318632,-13.2556757897085,
12.));
#197580=CARTESIAN_POINT('Ctrl Pts',(-19.8586778231711,-13.2609038446525,
0.));
#197581=CARTESIAN_POINT('Ctrl Pts',(-19.8586778231711,-13.2609038446525,
12.));
#197582=CARTESIAN_POINT('Ctrl Pts',(-19.8788333760571,-13.2661050556128,
0.));
#197583=CARTESIAN_POINT('Ctrl Pts',(-19.8788333760571,-13.2661050556128,
12.));
#197584=CARTESIAN_POINT('Ctrl Pts',(-19.8991035111739,-13.2712788215015,
0.));
#197585=CARTESIAN_POINT('Ctrl Pts',(-19.8991035111739,-13.2712788215015,
12.));
#197586=CARTESIAN_POINT('Ctrl Pts',(-19.9194875559419,-13.2764245494354,
0.));
#197587=CARTESIAN_POINT('Ctrl Pts',(-19.9194875559419,-13.2764245494354,
12.));
#197588=CARTESIAN_POINT('Ctrl Pts',(-19.9399848444019,-13.2815416545663,
0.));
#197589=CARTESIAN_POINT('Ctrl Pts',(-19.9399848444019,-13.2815416545663,
12.));
#197590=CARTESIAN_POINT('Ctrl Pts',(-19.9605947170589,-13.2866295599152,
0.));
#197591=CARTESIAN_POINT('Ctrl Pts',(-19.9605947170589,-13.2866295599152,
12.));
#197592=CARTESIAN_POINT('Ctrl Pts',(-19.9813165207174,-13.2916876962098,
0.));
#197593=CARTESIAN_POINT('Ctrl Pts',(-19.9813165207174,-13.2916876962098,
12.));
#197594=CARTESIAN_POINT('Ctrl Pts',(-20.0021496083742,-13.296715501731,
0.));
#197595=CARTESIAN_POINT('Ctrl Pts',(-20.0021496083742,-13.296715501731,
12.));
#197596=CARTESIAN_POINT('Ctrl Pts',(-20.023093339104,-13.3017124221639,
0.));
#197597=CARTESIAN_POINT('Ctrl Pts',(-20.023093339104,-13.3017124221639,
12.));
#197598=CARTESIAN_POINT('Ctrl Pts',(-20.0441470779345,-13.3066779104515,
0.));
#197599=CARTESIAN_POINT('Ctrl Pts',(-20.0441470779345,-13.3066779104515,
12.));
#197600=CARTESIAN_POINT('Ctrl Pts',(-20.0653101957188,-13.3116114266514,
0.));
#197601=CARTESIAN_POINT('Ctrl Pts',(-20.0653101957188,-13.3116114266514,
12.));
#197602=CARTESIAN_POINT('Ctrl Pts',(-20.0865820689883,-13.3165124377963,
0.));
#197603=CARTESIAN_POINT('Ctrl Pts',(-20.0865820689883,-13.3165124377963,
12.));
#197604=CARTESIAN_POINT('Ctrl Pts',(-20.1079620798377,-13.3213804177588,
0.));
#197605=CARTESIAN_POINT('Ctrl Pts',(-20.1079620798377,-13.3213804177588,
12.));
#197606=CARTESIAN_POINT('Ctrl Pts',(-20.1294496158405,-13.3262148471228,
0.));
#197607=CARTESIAN_POINT('Ctrl Pts',(-20.1294496158405,-13.3262148471228,
12.));
#197608=CARTESIAN_POINT('Ctrl Pts',(-20.1510440699477,-13.3310152130565,
0.));
#197609=CARTESIAN_POINT('Ctrl Pts',(-20.1510440699477,-13.3310152130565,
12.));
#197610=CARTESIAN_POINT('Ctrl Pts',(-20.1727448403818,-13.3357810091903,
0.));
#197611=CARTESIAN_POINT('Ctrl Pts',(-20.1727448403818,-13.3357810091903,
12.));
#197612=CARTESIAN_POINT('Ctrl Pts',(-20.1945513305233,-13.3405117354969,
0.));
#197613=CARTESIAN_POINT('Ctrl Pts',(-20.1945513305233,-13.3405117354969,
12.));
#197614=CARTESIAN_POINT('Ctrl Pts',(-20.2164629487855,-13.3452068981763,
0.));
#197615=CARTESIAN_POINT('Ctrl Pts',(-20.2164629487855,-13.3452068981763,
12.));
#197616=CARTESIAN_POINT('Ctrl Pts',(-20.2384791085354,-13.3498660095382,
0.));
#197617=CARTESIAN_POINT('Ctrl Pts',(-20.2384791085354,-13.3498660095382,
12.));
#197618=CARTESIAN_POINT('Ctrl Pts',(-20.2605992280117,-13.3544885878886,
0.));
#197619=CARTESIAN_POINT('Ctrl Pts',(-20.2605992280117,-13.3544885878886,
12.));
#197620=CARTESIAN_POINT('Ctrl Pts',(-20.2828227302337,-13.3590741574194,
0.));
#197621=CARTESIAN_POINT('Ctrl Pts',(-20.2828227302337,-13.3590741574194,
12.));
#197622=CARTESIAN_POINT('Ctrl Pts',(-20.3051490429049,-13.3636222481017,
0.));
#197623=CARTESIAN_POINT('Ctrl Pts',(-20.3051490429049,-13.3636222481017,
12.));
#197624=CARTESIAN_POINT('Ctrl Pts',(-20.3275775983032,-13.3681323955828,
0.));
#197625=CARTESIAN_POINT('Ctrl Pts',(-20.3275775983032,-13.3681323955828,
12.));
#197626=CARTESIAN_POINT('Ctrl Pts',(-20.3501078331818,-13.3726041410869,
0.));
#197627=CARTESIAN_POINT('Ctrl Pts',(-20.3501078331818,-13.3726041410869,
12.));
#197628=CARTESIAN_POINT('Ctrl Pts',(-20.3727391887187,-13.377037031319,
0.));
#197629=CARTESIAN_POINT('Ctrl Pts',(-20.3727391887187,-13.377037031319,
12.));
#197630=CARTESIAN_POINT('Ctrl Pts',(-20.3954711104505,-13.3814306183721,
0.));
#197631=CARTESIAN_POINT('Ctrl Pts',(-20.3954711104505,-13.3814306183721,
12.));
#197632=CARTESIAN_POINT('Ctrl Pts',(-20.4183030482002,-13.3857844596387,
0.));
#197633=CARTESIAN_POINT('Ctrl Pts',(-20.4183030482002,-13.3857844596387,
12.));
#197634=CARTESIAN_POINT('Ctrl Pts',(-20.4412344560007,-13.3900981177254,
0.));
#197635=CARTESIAN_POINT('Ctrl Pts',(-20.4412344560007,-13.3900981177254,
12.));
#197636=CARTESIAN_POINT('Ctrl Pts',(-20.4642647920038,-13.3943711603739,
0.));
#197637=CARTESIAN_POINT('Ctrl Pts',(-20.4642647920038,-13.3943711603739,
12.));
#197638=CARTESIAN_POINT('Ctrl Pts',(-20.4873935184041,-13.3986031603716,
0.));
#197639=CARTESIAN_POINT('Ctrl Pts',(-20.4873935184041,-13.3986031603716,
12.));
#197640=CARTESIAN_POINT('Ctrl Pts',(-20.5106201013755,-13.4027936954529,
0.));
#197641=CARTESIAN_POINT('Ctrl Pts',(-20.5106201013755,-13.4027936954529,
12.));
#197642=CARTESIAN_POINT('Ctrl Pts',(-20.5339440109958,-13.4069423482076,
0.));
#197643=CARTESIAN_POINT('Ctrl Pts',(-20.5339440109958,-13.4069423482076,
12.));
#197644=CARTESIAN_POINT('Ctrl Pts',(-20.557364721164,-13.4110487059912,
0.));
#197645=CARTESIAN_POINT('Ctrl Pts',(-20.557364721164,-13.4110487059912,
12.));
#197646=CARTESIAN_POINT('Ctrl Pts',(-20.5808817095155,-13.4151123608411,
0.));
#197647=CARTESIAN_POINT('Ctrl Pts',(-20.5808817095155,-13.4151123608411,
12.));
#197648=CARTESIAN_POINT('Ctrl Pts',(-20.6044944573151,-13.4191329093932,
0.));
#197649=CARTESIAN_POINT('Ctrl Pts',(-20.6044944573151,-13.4191329093932,
12.));
#197650=CARTESIAN_POINT('Ctrl Pts',(-20.6282024494234,-13.4231099528178,
0.));
#197651=CARTESIAN_POINT('Ctrl Pts',(-20.6282024494234,-13.4231099528178,
12.));
#197652=CARTESIAN_POINT('Ctrl Pts',(-20.6520051742868,-13.427043096765,
0.));
#197653=CARTESIAN_POINT('Ctrl Pts',(-20.6520051742868,-13.427043096765,
12.));
#197654=CARTESIAN_POINT('Ctrl Pts',(-20.6759021239102,-13.4309319513119,
0.));
#197655=CARTESIAN_POINT('Ctrl Pts',(-20.6759021239102,-13.4309319513119,
12.));
#197656=CARTESIAN_POINT('Ctrl Pts',(-20.6998927938288,-13.4347761309154,
0.));
#197657=CARTESIAN_POINT('Ctrl Pts',(-20.6998927938288,-13.4347761309154,
12.));
#197658=CARTESIAN_POINT('Ctrl Pts',(-20.7239766830675,-13.4385752543663,
0.));
#197659=CARTESIAN_POINT('Ctrl Pts',(-20.7239766830675,-13.4385752543663,
12.));
#197660=CARTESIAN_POINT('Ctrl Pts',(-20.7481532941014,-13.4423289447561,
0.));
#197661=CARTESIAN_POINT('Ctrl Pts',(-20.7481532941014,-13.4423289447561,
12.));
#197662=CARTESIAN_POINT('Ctrl Pts',(-20.7724221327609,-13.4460368293689,
0.));
#197663=CARTESIAN_POINT('Ctrl Pts',(-20.7724221327609,-13.4460368293689,
12.));
#197664=CARTESIAN_POINT('Ctrl Pts',(-20.7967827081228,-13.4496985395637,
0.));
#197665=CARTESIAN_POINT('Ctrl Pts',(-20.7967827081228,-13.4496985395637,
12.));
#197666=CARTESIAN_POINT('Ctrl Pts',(-20.821234532398,-13.4533137106667,
0.));
#197667=CARTESIAN_POINT('Ctrl Pts',(-20.821234532398,-13.4533137106667,
12.));
#197668=CARTESIAN_POINT('Ctrl Pts',(-20.8457771208083,-13.4568819818631,
0.));
#197669=CARTESIAN_POINT('Ctrl Pts',(-20.8457771208083,-13.4568819818631,
12.));
#197670=CARTESIAN_POINT('Ctrl Pts',(-20.8704099914641,-13.4604029960983,
0.));
#197671=CARTESIAN_POINT('Ctrl Pts',(-20.8704099914641,-13.4604029960983,
12.));
#197672=CARTESIAN_POINT('Ctrl Pts',(-20.8951326652158,-13.4638763999725,
0.));
#197673=CARTESIAN_POINT('Ctrl Pts',(-20.8951326652158,-13.4638763999725,
12.));
#197674=CARTESIAN_POINT('Ctrl Pts',(-20.9199446657583,-13.4673018437717,
0.));
#197675=CARTESIAN_POINT('Ctrl Pts',(-20.9199446657583,-13.4673018437717,
12.));
#197676=CARTESIAN_POINT('Ctrl Pts',(-20.9448455197557,-13.4706789815166,
0.));
#197677=CARTESIAN_POINT('Ctrl Pts',(-20.9448455197557,-13.4706789815166,
12.));
#197678=CARTESIAN_POINT('Ctrl Pts',(-20.9698347569477,-13.4740074710086,
0.));
#197679=CARTESIAN_POINT('Ctrl Pts',(-20.9698347569477,-13.4740074710086,
12.));
#197680=CARTESIAN_POINT('Ctrl Pts',(-20.9949119102592,-13.4772869738879,
0.));
#197681=CARTESIAN_POINT('Ctrl Pts',(-20.9949119102592,-13.4772869738879,
12.));
#197682=CARTESIAN_POINT('Ctrl Pts',(-21.0200765158884,-13.4805171556822,
0.));
#197683=CARTESIAN_POINT('Ctrl Pts',(-21.0200765158884,-13.4805171556822,
12.));
#197684=CARTESIAN_POINT('Ctrl Pts',(-21.0453281134245,-13.4836976858912,
0.));
#197685=CARTESIAN_POINT('Ctrl Pts',(-21.0453281134245,-13.4836976858912,
12.));
#197686=CARTESIAN_POINT('Ctrl Pts',(-21.0706662455199,-13.4868282377191,
0.));
#197687=CARTESIAN_POINT('Ctrl Pts',(-21.0706662455199,-13.4868282377191,
12.));
#197688=CARTESIAN_POINT('Ctrl Pts',(-21.0960904575046,-13.4899084877717,
0.));
#197689=CARTESIAN_POINT('Ctrl Pts',(-21.0960904575046,-13.4899084877717,
12.));
#197690=CARTESIAN_POINT('Ctrl Pts',(-21.1216002970207,-13.4929381157778,
0.));
#197691=CARTESIAN_POINT('Ctrl Pts',(-21.1216002970207,-13.4929381157778,
12.));
#197692=CARTESIAN_POINT('Ctrl Pts',(-21.1471953136209,-13.4959168042934,
0.));
#197693=CARTESIAN_POINT('Ctrl Pts',(-21.1471953136209,-13.4959168042934,
12.));
#197694=CARTESIAN_POINT('Ctrl Pts',(-21.1728750584175,-13.4988442384491,
0.));
#197695=CARTESIAN_POINT('Ctrl Pts',(-21.1728750584175,-13.4988442384491,
12.));
#197696=CARTESIAN_POINT('Ctrl Pts',(-21.1986390835828,-13.5017201056088,
0.));
#197697=CARTESIAN_POINT('Ctrl Pts',(-21.1986390835828,-13.5017201056088,
12.));
#197698=CARTESIAN_POINT('Ctrl Pts',(-21.2244869429332,-13.5045440957404,
0.));
#197699=CARTESIAN_POINT('Ctrl Pts',(-21.2244869429332,-13.5045440957404,
12.));
#197700=CARTESIAN_POINT('Ctrl Pts',(-21.250418192743,-13.5073159019452,
0.));
#197701=CARTESIAN_POINT('Ctrl Pts',(-21.250418192743,-13.5073159019452,
12.));
#197702=CARTESIAN_POINT('Ctrl Pts',(-21.2764323924442,-13.5100352209205,
0.));
#197703=CARTESIAN_POINT('Ctrl Pts',(-21.2764323924442,-13.5100352209205,
12.));
#197704=CARTESIAN_POINT('Ctrl Pts',(-21.3025291054235,-13.5127017534971,
0.));
#197705=CARTESIAN_POINT('Ctrl Pts',(-21.3025291054235,-13.5127017534971,
12.));
#197706=CARTESIAN_POINT('Ctrl Pts',(-21.3287078996341,-13.5153152050555,
0.));
#197707=CARTESIAN_POINT('Ctrl Pts',(-21.3287078996341,-13.5153152050555,
12.));
#197708=CARTESIAN_POINT('Ctrl Pts',(-21.3549683486222,-13.5178752862466,
0.));
#197709=CARTESIAN_POINT('Ctrl Pts',(-21.3549683486222,-13.5178752862466,
12.));
#197710=CARTESIAN_POINT('Ctrl Pts',(-21.3813100304973,-13.5203817122504,
0.));
#197711=CARTESIAN_POINT('Ctrl Pts',(-21.3813100304973,-13.5203817122504,
12.));
#197712=CARTESIAN_POINT('Ctrl Pts',(-21.4077325259324,-13.5228342013516,
0.));
#197713=CARTESIAN_POINT('Ctrl Pts',(-21.4077325259324,-13.5228342013516,
12.));
#197714=CARTESIAN_POINT('Ctrl Pts',(-21.4342354165259,-13.5252324737802,
0.));
#197715=CARTESIAN_POINT('Ctrl Pts',(-21.4342354165259,-13.5252324737802,
12.));
#197716=CARTESIAN_POINT('Ctrl Pts',(-21.4608182828697,-13.5275762503555,
0.));
#197717=CARTESIAN_POINT('Ctrl Pts',(-21.4608182828697,-13.5275762503555,
12.));
#197718=CARTESIAN_POINT('Ctrl Pts',(-21.4874807030468,-13.5298652514355,
0.));
#197719=CARTESIAN_POINT('Ctrl Pts',(-21.4874807030468,-13.5298652514355,
12.));
#197720=CARTESIAN_POINT('Ctrl Pts',(-21.5142222501666,-13.5320991952138,
0.));
#197721=CARTESIAN_POINT('Ctrl Pts',(-21.5142222501666,-13.5320991952138,
12.));
#197722=CARTESIAN_POINT('Ctrl Pts',(-21.5410424932503,-13.5342777983215,
0.));
#197723=CARTESIAN_POINT('Ctrl Pts',(-21.5410424932503,-13.5342777983215,
12.));
#197724=CARTESIAN_POINT('Ctrl Pts',(-21.5679410019001,-13.536400779028,
0.));
#197725=CARTESIAN_POINT('Ctrl Pts',(-21.5679410019001,-13.536400779028,
12.));
#197726=CARTESIAN_POINT('Ctrl Pts',(-21.5949173499013,-13.5384678597195,
0.));
#197727=CARTESIAN_POINT('Ctrl Pts',(-21.5949173499013,-13.5384678597195,
12.));
#197728=CARTESIAN_POINT('Ctrl Pts',(-21.6219711193946,-13.5404787697792,
0.));
#197729=CARTESIAN_POINT('Ctrl Pts',(-21.6219711193946,-13.5404787697792,
12.));
#197730=CARTESIAN_POINT('Ctrl Pts',(-21.6491019044648,-13.5424332480699,
0.));
#197731=CARTESIAN_POINT('Ctrl Pts',(-21.6491019044648,-13.5424332480699,
12.));
#197732=CARTESIAN_POINT('Ctrl Pts',(-21.6763093157699,-13.5443310461526,
0.));
#197733=CARTESIAN_POINT('Ctrl Pts',(-21.6763093157699,-13.5443310461526,
12.));
#197734=CARTESIAN_POINT('Ctrl Pts',(-21.7035929822955,-13.5461719295048,
0.));
#197735=CARTESIAN_POINT('Ctrl Pts',(-21.7035929822955,-13.5461719295048,
12.));
#197736=CARTESIAN_POINT('Ctrl Pts',(-21.7309525412281,-13.5479556704481,
0.));
#197737=CARTESIAN_POINT('Ctrl Pts',(-21.7309525412281,-13.5479556704481,
12.));
#197738=CARTESIAN_POINT('Ctrl Pts',(-21.7583876294554,-13.5496820422211,
0.));
#197739=CARTESIAN_POINT('Ctrl Pts',(-21.7583876294554,-13.5496820422211,
12.));
#197740=CARTESIAN_POINT('Ctrl Pts',(-21.7858978745865,-13.551350812725,
0.));
#197741=CARTESIAN_POINT('Ctrl Pts',(-21.7858978745865,-13.551350812725,
12.));
#197742=CARTESIAN_POINT('Ctrl Pts',(-21.8134828857967,-13.5529617381573,
0.));
#197743=CARTESIAN_POINT('Ctrl Pts',(-21.8134828857967,-13.5529617381573,
12.));
#197744=CARTESIAN_POINT('Ctrl Pts',(-21.8411422456075,-13.5545145573031,
0.));
#197745=CARTESIAN_POINT('Ctrl Pts',(-21.8411422456075,-13.5545145573031,
12.));
#197746=CARTESIAN_POINT('Ctrl Pts',(-21.8688754989365,-13.5560089839385,
0.));
#197747=CARTESIAN_POINT('Ctrl Pts',(-21.8688754989365,-13.5560089839385,
12.));
#197748=CARTESIAN_POINT('Ctrl Pts',(-21.8966821688824,-13.5574447178424,
0.));
#197749=CARTESIAN_POINT('Ctrl Pts',(-21.8966821688824,-13.5574447178424,
12.));
#197750=CARTESIAN_POINT('Ctrl Pts',(-21.9245617765769,-13.5588214586604,
0.));
#197751=CARTESIAN_POINT('Ctrl Pts',(-21.9245617765769,-13.5588214586604,
12.));
#197752=CARTESIAN_POINT('Ctrl Pts',(-21.9525138592813,-13.5601389185257,
0.));
#197753=CARTESIAN_POINT('Ctrl Pts',(-21.9525138592813,-13.5601389185257,
12.));
#197754=CARTESIAN_POINT('Ctrl Pts',(-21.9805379899168,-13.5613968357561,
0.));
#197755=CARTESIAN_POINT('Ctrl Pts',(-21.9805379899168,-13.5613968357561,
12.));
#197756=CARTESIAN_POINT('Ctrl Pts',(-22.0086337943449,-13.5625949868333,
0.));
#197757=CARTESIAN_POINT('Ctrl Pts',(-22.0086337943449,-13.5625949868333,
12.));
#197758=CARTESIAN_POINT('Ctrl Pts',(-22.0368009736295,-13.5637332022473,
0.));
#197759=CARTESIAN_POINT('Ctrl Pts',(-22.0368009736295,-13.5637332022473,
12.));
#197760=CARTESIAN_POINT('Ctrl Pts',(-22.0650393089609,-13.5648113689033,
0.));
#197761=CARTESIAN_POINT('Ctrl Pts',(-22.0650393089609,-13.5648113689033,
12.));
#197762=CARTESIAN_POINT('Ctrl Pts',(-22.0933486464593,-13.5658294169284,
0.));
#197763=CARTESIAN_POINT('Ctrl Pts',(-22.0933486464593,-13.5658294169284,
12.));
#197764=CARTESIAN_POINT('Ctrl Pts',(-22.1217288871975,-13.5667873105359,
0.));
#197765=CARTESIAN_POINT('Ctrl Pts',(-22.1217288871975,-13.5667873105359,
12.));
#197766=CARTESIAN_POINT('Ctrl Pts',(-22.1444897575194,-13.5675054919061,
0.));
#197767=CARTESIAN_POINT('Ctrl Pts',(-22.1444897575194,-13.5675054919061,
12.));
#197768=CARTESIAN_POINT('Ctrl Pts',(-22.1615922805008,-13.5680170531805,
0.));
#197769=CARTESIAN_POINT('Ctrl Pts',(-22.1615922805008,-13.5680170531805,
12.));
#197770=CARTESIAN_POINT('Ctrl Pts',(-22.1730081264608,-13.5683460612942,
0.));
#197771=CARTESIAN_POINT('Ctrl Pts',(-22.1730081264608,-13.5683460612942,
12.));
#197772=CARTESIAN_POINT('Ctrl Pts',(-22.1787195904339,-13.5685075571671,
0.));
#197773=CARTESIAN_POINT('Ctrl Pts',(-22.1787195904339,-13.5685075571671,
12.));
#197774=CARTESIAN_POINT('',(-22.1787195904339,-13.5685075571671,0.));
#197775=CARTESIAN_POINT('Ctrl Pts',(-18.5896416359912,-12.7689476255363,
0.));
#197776=CARTESIAN_POINT('Ctrl Pts',(-18.5896460962964,-12.7689524524483,
0.));
#197777=CARTESIAN_POINT('Ctrl Pts',(-18.5896919669165,-12.768986426692,
0.));
#197778=CARTESIAN_POINT('Ctrl Pts',(-18.589871621843,-12.769110348199,0.));
#197779=CARTESIAN_POINT('Ctrl Pts',(-18.5903328777227,-12.7694215127919,
0.));
#197780=CARTESIAN_POINT('Ctrl Pts',(-18.5912775137806,-12.7700520897173,
0.));
#197781=CARTESIAN_POINT('Ctrl Pts',(-18.5925859134579,-12.7709195951156,
0.));
#197782=CARTESIAN_POINT('Ctrl Pts',(-18.5942490615407,-12.7720142287172,
0.));
#197783=CARTESIAN_POINT('Ctrl Pts',(-18.5962551167772,-12.7733231262108,
0.));
#197784=CARTESIAN_POINT('Ctrl Pts',(-18.598591752595,-12.7748328937638,
0.));
#197785=CARTESIAN_POINT('Ctrl Pts',(-18.6012488486709,-12.7765325225081,
0.));
#197786=CARTESIAN_POINT('Ctrl Pts',(-18.6042190183704,-12.7784139605066,
0.));
#197787=CARTESIAN_POINT('Ctrl Pts',(-18.6074961535723,-12.7804705387658,
0.));
#197788=CARTESIAN_POINT('Ctrl Pts',(-18.6110744826219,-12.7826959526925,
0.));
#197789=CARTESIAN_POINT('Ctrl Pts',(-18.6149475565188,-12.7850831657901,
0.));
#197790=CARTESIAN_POINT('Ctrl Pts',(-18.6191087624752,-12.7876249657834,
0.));
#197791=CARTESIAN_POINT('Ctrl Pts',(-18.6235516265575,-12.7903142925234,
0.));
#197792=CARTESIAN_POINT('Ctrl Pts',(-18.6282702819371,-12.7931447451555,
0.));
#197793=CARTESIAN_POINT('Ctrl Pts',(-18.6332595057006,-12.7961106222251,
0.));
#197794=CARTESIAN_POINT('Ctrl Pts',(-18.63851447924,-12.7992066625264,0.));
#197795=CARTESIAN_POINT('Ctrl Pts',(-18.6440306327456,-12.8024278770152,
0.));
#197796=CARTESIAN_POINT('Ctrl Pts',(-18.6498034438987,-12.805769331162,
0.));
#197797=CARTESIAN_POINT('Ctrl Pts',(-18.6558284825773,-12.8092261933858,
0.));
#197798=CARTESIAN_POINT('Ctrl Pts',(-18.6621014624746,-12.8127937909631,
0.));
#197799=CARTESIAN_POINT('Ctrl Pts',(-18.6686182952799,-12.8164676687362,
0.));
#197800=CARTESIAN_POINT('Ctrl Pts',(-18.6753751301092,-12.8202436318474,
0.));
#197801=CARTESIAN_POINT('Ctrl Pts',(-18.6823683094139,-12.8241176980017,
0.));
#197802=CARTESIAN_POINT('Ctrl Pts',(-18.6895943376171,-12.8280860635231,
0.));
#197803=CARTESIAN_POINT('Ctrl Pts',(-18.6970498410172,-12.8321450599789,
0.));
#197804=CARTESIAN_POINT('Ctrl Pts',(-18.7047315436294,-12.8362911280361,
0.));
#197805=CARTESIAN_POINT('Ctrl Pts',(-18.7126362754445,-12.8405208263431,
0.));
#197806=CARTESIAN_POINT('Ctrl Pts',(-18.7207609737702,-12.8448308329494,
0.));
#197807=CARTESIAN_POINT('Ctrl Pts',(-18.7291026886554,-12.8492179511591,
0.));
#197808=CARTESIAN_POINT('Ctrl Pts',(-18.7376585820854,-12.8536791086316,
0.));
#197809=CARTESIAN_POINT('Ctrl Pts',(-18.7464259171251,-12.8582113455646,
0.));
#197810=CARTESIAN_POINT('Ctrl Pts',(-18.7554020493887,-12.8628118054171,
0.));
#197811=CARTESIAN_POINT('Ctrl Pts',(-18.7645844169564,-12.8674777239653,
0.));
#197812=CARTESIAN_POINT('Ctrl Pts',(-18.7739705329022,-12.872206421181,
0.));
#197813=CARTESIAN_POINT('Ctrl Pts',(-18.7835579840477,-12.8769952998095,
0.));
#197814=CARTESIAN_POINT('Ctrl Pts',(-18.7933444285868,-12.8818418427475,
0.));
#197815=CARTESIAN_POINT('Ctrl Pts',(-18.8033275941943,-12.8867436109546,
0.));
#197816=CARTESIAN_POINT('Ctrl Pts',(-18.813505275782,-12.8916982409935,
0.));
#197817=CARTESIAN_POINT('Ctrl Pts',(-18.8238753319129,-12.8967034410755,
0.));
#197818=CARTESIAN_POINT('Ctrl Pts',(-18.834435681259,-12.9017569871738,
0.));
#197819=CARTESIAN_POINT('Ctrl Pts',(-18.8451842990984,-12.9068567191854,
0.));
#197820=CARTESIAN_POINT('Ctrl Pts',(-18.8561192136198,-12.9120005369063,
0.));
#197821=CARTESIAN_POINT('Ctrl Pts',(-18.8672385038326,-12.9171863977045,
0.));
#197822=CARTESIAN_POINT('Ctrl Pts',(-18.8785402977527,-12.9224123144982,
0.));
#197823=CARTESIAN_POINT('Ctrl Pts',(-18.8900227704889,-12.9276763536373,
0.));
#197824=CARTESIAN_POINT('Ctrl Pts',(-18.9016841423403,-12.9329766328185,
0.));
#197825=CARTESIAN_POINT('Ctrl Pts',(-18.9135226769465,-12.9383113190375,
0.));
#197826=CARTESIAN_POINT('Ctrl Pts',(-18.9255366795195,-12.9436786266105,
0.));
#197827=CARTESIAN_POINT('Ctrl Pts',(-18.9377244950435,-12.9490768151821,
0.));
#197828=CARTESIAN_POINT('Ctrl Pts',(-18.9500845064715,-12.9545041877377,
0.));
#197829=CARTESIAN_POINT('Ctrl Pts',(-18.9626151329229,-12.9599590886319,
0.));
#197830=CARTESIAN_POINT('Ctrl Pts',(-18.9753148284475,-12.9654399021869,
0.));
#197831=CARTESIAN_POINT('Ctrl Pts',(-18.9881820807586,-12.9709450512747,
0.));
#197832=CARTESIAN_POINT('Ctrl Pts',(-19.0012154099791,-12.9764729959205,
0.));
#197833=CARTESIAN_POINT('Ctrl Pts',(-19.0144133673348,-12.9820222318716,
0.));
#197834=CARTESIAN_POINT('Ctrl Pts',(-19.0277745339908,-12.9875912893003,
0.));
#197835=CARTESIAN_POINT('Ctrl Pts',(-19.0412975200398,-12.9931787316515,
0.));
#197836=CARTESIAN_POINT('Ctrl Pts',(-19.0549809634355,-12.9987831544502,
0.));
#197837=CARTESIAN_POINT('Ctrl Pts',(-19.0688235289437,-13.0044031841381,
0.));
#197838=CARTESIAN_POINT('Ctrl Pts',(-19.0828239070482,-13.0100374768785,
0.));
#197839=CARTESIAN_POINT('Ctrl Pts',(-19.0969808131226,-13.0156847176093,
0.));
#197840=CARTESIAN_POINT('Ctrl Pts',(-19.1112929866308,-13.0213436191326,
0.));
#197841=CARTESIAN_POINT('Ctrl Pts',(-19.1257591903099,-13.0270129211976,
0.));
#197842=CARTESIAN_POINT('Ctrl Pts',(-19.1403782093389,-13.0326913895841,
0.));
#197843=CARTESIAN_POINT('Ctrl Pts',(-19.1551488505233,-13.0383778152072,
0.));
#197844=CARTESIAN_POINT('Ctrl Pts',(-19.1700699416625,-13.0440710133775,
0.));
#197845=CARTESIAN_POINT('Ctrl Pts',(-19.1851403308825,-13.0497698230442,
0.));
#197846=CARTESIAN_POINT('Ctrl Pts',(-19.2003588859771,-13.0554731060537,
0.));
#197847=CARTESIAN_POINT('Ctrl Pts',(-19.2157244937141,-13.0611797463913,
0.));
#197848=CARTESIAN_POINT('Ctrl Pts',(-19.2312360592031,-13.0668886494791,
0.));
#197849=CARTESIAN_POINT('Ctrl Pts',(-19.2468925053988,-13.0725987415856,
0.));
#197850=CARTESIAN_POINT('Ctrl Pts',(-19.2626927725596,-13.0783089692118,
0.));
#197851=CARTESIAN_POINT('Ctrl Pts',(-19.2786358177198,-13.0840182984949,
0.));
#197852=CARTESIAN_POINT('Ctrl Pts',(-19.2947206141246,-13.0897257145969,
0.));
#197853=CARTESIAN_POINT('Ctrl Pts',(-19.3109461507358,-13.095430221148,
0.));
#197854=CARTESIAN_POINT('Ctrl Pts',(-19.3273114318268,-13.1011308397592,
0.));
#197855=CARTESIAN_POINT('Ctrl Pts',(-19.3438154765395,-13.1068266095186,
0.));
#197856=CARTESIAN_POINT('Ctrl Pts',(-19.3604573184516,-13.1125165865021,
0.));
#197857=CARTESIAN_POINT('Ctrl Pts',(-19.3772360051093,-13.118199843271,
0.));
#197858=CARTESIAN_POINT('Ctrl Pts',(-19.3941505976267,-13.1238754684177,
0.));
#197859=CARTESIAN_POINT('Ctrl Pts',(-19.4112001703561,-13.1295425661635,
0.));
#197860=CARTESIAN_POINT('Ctrl Pts',(-19.4283838105265,-13.1352002559439,
0.));
#197861=CARTESIAN_POINT('Ctrl Pts',(-19.4457006178875,-13.140847672006,
0.));
#197862=CARTESIAN_POINT('Ctrl Pts',(-19.463149704325,-13.1464839629966,
0.));
#197863=CARTESIAN_POINT('Ctrl Pts',(-19.4807301935256,-13.1521082915846,
0.));
#197864=CARTESIAN_POINT('Ctrl Pts',(-19.498441220707,-13.1577198341238,
0.));
#197865=CARTESIAN_POINT('Ctrl Pts',(-19.5162819323207,-13.1633177803097,
0.));
#197866=CARTESIAN_POINT('Ctrl Pts',(-19.5342514857564,-13.1689013328432,
0.));
#197867=CARTESIAN_POINT('Ctrl Pts',(-19.5523490490254,-13.1744697070918,
0.));
#197868=CARTESIAN_POINT('Ctrl Pts',(-19.5705738004682,-13.1800221307682,
0.));
#197869=CARTESIAN_POINT('Ctrl Pts',(-19.5889249285352,-13.1855578436479,
0.));
#197870=CARTESIAN_POINT('Ctrl Pts',(-19.6074016315421,-13.1910760972818,
0.));
#197871=CARTESIAN_POINT('Ctrl Pts',(-19.6260031174244,-13.196576154715,
0.));
#197872=CARTESIAN_POINT('Ctrl Pts',(-19.6447286034764,-13.202057290206,
0.));
#197873=CARTESIAN_POINT('Ctrl Pts',(-19.6635773160924,-13.2075187889522,
0.));
#197874=CARTESIAN_POINT('Ctrl Pts',(-19.6825484905812,-13.2129599468478,
0.));
#197875=CARTESIAN_POINT('Ctrl Pts',(-19.7016413709678,-13.2183800702431,
0.));
#197876=CARTESIAN_POINT('Ctrl Pts',(-19.7208552097867,-13.2237784757065,
0.));
#197877=CARTESIAN_POINT('Ctrl Pts',(-19.7401892678701,-13.2291544897902,
0.));
#197878=CARTESIAN_POINT('Ctrl Pts',(-19.7596428141176,-13.2345074487968,
0.));
#197879=CARTESIAN_POINT('Ctrl Pts',(-19.7792151253297,-13.239836698568,
0.));
#197880=CARTESIAN_POINT('Ctrl Pts',(-19.7989054860501,-13.2451415942809,
0.));
#197881=CARTESIAN_POINT('Ctrl Pts',(-19.8187131883919,-13.2504215002458,
0.));
#197882=CARTESIAN_POINT('Ctrl Pts',(-19.8386375318632,-13.2556757897085,
0.));
#197883=CARTESIAN_POINT('Ctrl Pts',(-19.8586778231711,-13.2609038446525,
0.));
#197884=CARTESIAN_POINT('Ctrl Pts',(-19.8788333760571,-13.2661050556128,
0.));
#197885=CARTESIAN_POINT('Ctrl Pts',(-19.8991035111739,-13.2712788215015,
0.));
#197886=CARTESIAN_POINT('Ctrl Pts',(-19.9194875559419,-13.2764245494354,
0.));
#197887=CARTESIAN_POINT('Ctrl Pts',(-19.9399848444019,-13.2815416545663,
0.));
#197888=CARTESIAN_POINT('Ctrl Pts',(-19.9605947170589,-13.2866295599152,
0.));
#197889=CARTESIAN_POINT('Ctrl Pts',(-19.9813165207174,-13.2916876962098,
0.));
#197890=CARTESIAN_POINT('Ctrl Pts',(-20.0021496083742,-13.296715501731,
0.));
#197891=CARTESIAN_POINT('Ctrl Pts',(-20.023093339104,-13.3017124221639,
0.));
#197892=CARTESIAN_POINT('Ctrl Pts',(-20.0441470779345,-13.3066779104515,
0.));
#197893=CARTESIAN_POINT('Ctrl Pts',(-20.0653101957188,-13.3116114266514,
0.));
#197894=CARTESIAN_POINT('Ctrl Pts',(-20.0865820689883,-13.3165124377963,
0.));
#197895=CARTESIAN_POINT('Ctrl Pts',(-20.1079620798377,-13.3213804177588,
0.));
#197896=CARTESIAN_POINT('Ctrl Pts',(-20.1294496158405,-13.3262148471228,
0.));
#197897=CARTESIAN_POINT('Ctrl Pts',(-20.1510440699477,-13.3310152130565,
0.));
#197898=CARTESIAN_POINT('Ctrl Pts',(-20.1727448403818,-13.3357810091903,
0.));
#197899=CARTESIAN_POINT('Ctrl Pts',(-20.1945513305233,-13.3405117354969,
0.));
#197900=CARTESIAN_POINT('Ctrl Pts',(-20.2164629487855,-13.3452068981763,
0.));
#197901=CARTESIAN_POINT('Ctrl Pts',(-20.2384791085354,-13.3498660095382,
0.));
#197902=CARTESIAN_POINT('Ctrl Pts',(-20.2605992280117,-13.3544885878886,
0.));
#197903=CARTESIAN_POINT('Ctrl Pts',(-20.2828227302337,-13.3590741574194,
0.));
#197904=CARTESIAN_POINT('Ctrl Pts',(-20.3051490429049,-13.3636222481017,
0.));
#197905=CARTESIAN_POINT('Ctrl Pts',(-20.3275775983032,-13.3681323955828,
0.));
#197906=CARTESIAN_POINT('Ctrl Pts',(-20.3501078331818,-13.3726041410869,
0.));
#197907=CARTESIAN_POINT('Ctrl Pts',(-20.3727391887187,-13.377037031319,
0.));
#197908=CARTESIAN_POINT('Ctrl Pts',(-20.3954711104505,-13.3814306183721,
0.));
#197909=CARTESIAN_POINT('Ctrl Pts',(-20.4183030482002,-13.3857844596387,
0.));
#197910=CARTESIAN_POINT('Ctrl Pts',(-20.4412344560007,-13.3900981177254,
0.));
#197911=CARTESIAN_POINT('Ctrl Pts',(-20.4642647920038,-13.3943711603739,
0.));
#197912=CARTESIAN_POINT('Ctrl Pts',(-20.4873935184041,-13.3986031603716,
0.));
#197913=CARTESIAN_POINT('Ctrl Pts',(-20.5106201013755,-13.4027936954529,
0.));
#197914=CARTESIAN_POINT('Ctrl Pts',(-20.5339440109958,-13.4069423482076,
0.));
#197915=CARTESIAN_POINT('Ctrl Pts',(-20.557364721164,-13.4110487059912,
0.));
#197916=CARTESIAN_POINT('Ctrl Pts',(-20.5808817095155,-13.4151123608411,
0.));
#197917=CARTESIAN_POINT('Ctrl Pts',(-20.6044944573151,-13.4191329093932,
0.));
#197918=CARTESIAN_POINT('Ctrl Pts',(-20.6282024494234,-13.4231099528178,
0.));
#197919=CARTESIAN_POINT('Ctrl Pts',(-20.6520051742868,-13.427043096765,
0.));
#197920=CARTESIAN_POINT('Ctrl Pts',(-20.6759021239102,-13.4309319513119,
0.));
#197921=CARTESIAN_POINT('Ctrl Pts',(-20.6998927938288,-13.4347761309154,
0.));
#197922=CARTESIAN_POINT('Ctrl Pts',(-20.7239766830675,-13.4385752543663,
0.));
#197923=CARTESIAN_POINT('Ctrl Pts',(-20.7481532941014,-13.4423289447561,
0.));
#197924=CARTESIAN_POINT('Ctrl Pts',(-20.7724221327609,-13.4460368293689,
0.));
#197925=CARTESIAN_POINT('Ctrl Pts',(-20.7967827081228,-13.4496985395637,
0.));
#197926=CARTESIAN_POINT('Ctrl Pts',(-20.821234532398,-13.4533137106667,
0.));
#197927=CARTESIAN_POINT('Ctrl Pts',(-20.8457771208083,-13.4568819818631,
0.));
#197928=CARTESIAN_POINT('Ctrl Pts',(-20.8704099914641,-13.4604029960983,
0.));
#197929=CARTESIAN_POINT('Ctrl Pts',(-20.8951326652158,-13.4638763999725,
0.));
#197930=CARTESIAN_POINT('Ctrl Pts',(-20.9199446657583,-13.4673018437717,
0.));
#197931=CARTESIAN_POINT('Ctrl Pts',(-20.9448455197557,-13.4706789815166,
0.));
#197932=CARTESIAN_POINT('Ctrl Pts',(-20.9698347569477,-13.4740074710086,
0.));
#197933=CARTESIAN_POINT('Ctrl Pts',(-20.9949119102592,-13.4772869738879,
0.));
#197934=CARTESIAN_POINT('Ctrl Pts',(-21.0200765158884,-13.4805171556822,
0.));
#197935=CARTESIAN_POINT('Ctrl Pts',(-21.0453281134245,-13.4836976858912,
0.));
#197936=CARTESIAN_POINT('Ctrl Pts',(-21.0706662455199,-13.4868282377191,
0.));
#197937=CARTESIAN_POINT('Ctrl Pts',(-21.0960904575046,-13.4899084877717,
0.));
#197938=CARTESIAN_POINT('Ctrl Pts',(-21.1216002970207,-13.4929381157778,
0.));
#197939=CARTESIAN_POINT('Ctrl Pts',(-21.1471953136209,-13.4959168042934,
0.));
#197940=CARTESIAN_POINT('Ctrl Pts',(-21.1728750584175,-13.4988442384491,
0.));
#197941=CARTESIAN_POINT('Ctrl Pts',(-21.1986390835828,-13.5017201056088,
0.));
#197942=CARTESIAN_POINT('Ctrl Pts',(-21.2244869429332,-13.5045440957404,
0.));
#197943=CARTESIAN_POINT('Ctrl Pts',(-21.250418192743,-13.5073159019452,
0.));
#197944=CARTESIAN_POINT('Ctrl Pts',(-21.2764323924442,-13.5100352209205,
0.));
#197945=CARTESIAN_POINT('Ctrl Pts',(-21.3025291054235,-13.5127017534971,
0.));
#197946=CARTESIAN_POINT('Ctrl Pts',(-21.3287078996341,-13.5153152050555,
0.));
#197947=CARTESIAN_POINT('Ctrl Pts',(-21.3549683486222,-13.5178752862466,
0.));
#197948=CARTESIAN_POINT('Ctrl Pts',(-21.3813100304973,-13.5203817122504,
0.));
#197949=CARTESIAN_POINT('Ctrl Pts',(-21.4077325259324,-13.5228342013516,
0.));
#197950=CARTESIAN_POINT('Ctrl Pts',(-21.4342354165259,-13.5252324737802,
0.));
#197951=CARTESIAN_POINT('Ctrl Pts',(-21.4608182828697,-13.5275762503555,
0.));
#197952=CARTESIAN_POINT('Ctrl Pts',(-21.4874807030468,-13.5298652514355,
0.));
#197953=CARTESIAN_POINT('Ctrl Pts',(-21.5142222501666,-13.5320991952138,
0.));
#197954=CARTESIAN_POINT('Ctrl Pts',(-21.5410424932503,-13.5342777983215,
0.));
#197955=CARTESIAN_POINT('Ctrl Pts',(-21.5679410019001,-13.536400779028,
0.));
#197956=CARTESIAN_POINT('Ctrl Pts',(-21.5949173499013,-13.5384678597195,
0.));
#197957=CARTESIAN_POINT('Ctrl Pts',(-21.6219711193946,-13.5404787697792,
0.));
#197958=CARTESIAN_POINT('Ctrl Pts',(-21.6491019044648,-13.5424332480699,
0.));
#197959=CARTESIAN_POINT('Ctrl Pts',(-21.6763093157699,-13.5443310461526,
0.));
#197960=CARTESIAN_POINT('Ctrl Pts',(-21.7035929822955,-13.5461719295048,
0.));
#197961=CARTESIAN_POINT('Ctrl Pts',(-21.7309525412281,-13.5479556704481,
0.));
#197962=CARTESIAN_POINT('Ctrl Pts',(-21.7583876294554,-13.5496820422211,
0.));
#197963=CARTESIAN_POINT('Ctrl Pts',(-21.7858978745865,-13.551350812725,
0.));
#197964=CARTESIAN_POINT('Ctrl Pts',(-21.8134828857967,-13.5529617381573,
0.));
#197965=CARTESIAN_POINT('Ctrl Pts',(-21.8411422456075,-13.5545145573031,
0.));
#197966=CARTESIAN_POINT('Ctrl Pts',(-21.8688754989365,-13.5560089839385,
0.));
#197967=CARTESIAN_POINT('Ctrl Pts',(-21.8966821688824,-13.5574447178424,
0.));
#197968=CARTESIAN_POINT('Ctrl Pts',(-21.9245617765769,-13.5588214586604,
0.));
#197969=CARTESIAN_POINT('Ctrl Pts',(-21.9525138592813,-13.5601389185257,
0.));
#197970=CARTESIAN_POINT('Ctrl Pts',(-21.9805379899168,-13.5613968357561,
0.));
#197971=CARTESIAN_POINT('Ctrl Pts',(-22.0086337943449,-13.5625949868333,
0.));
#197972=CARTESIAN_POINT('Ctrl Pts',(-22.0368009736295,-13.5637332022473,
0.));
#197973=CARTESIAN_POINT('Ctrl Pts',(-22.0650393089609,-13.5648113689033,
0.));
#197974=CARTESIAN_POINT('Ctrl Pts',(-22.0933486464593,-13.5658294169284,
0.));
#197975=CARTESIAN_POINT('Ctrl Pts',(-22.1217288871975,-13.5667873105359,
0.));
#197976=CARTESIAN_POINT('Ctrl Pts',(-22.1444897575194,-13.5675054919061,
0.));
#197977=CARTESIAN_POINT('Ctrl Pts',(-22.1615922805008,-13.5680170531805,
0.));
#197978=CARTESIAN_POINT('Ctrl Pts',(-22.1730081264608,-13.5683460612942,
0.));
#197979=CARTESIAN_POINT('Ctrl Pts',(-22.1787195904339,-13.5685075571671,
0.));
#197980=CARTESIAN_POINT('',(-22.178719590434,-13.5685075571671,0.));
#197981=CARTESIAN_POINT('Origin',(-20.2687213152502,-7.17139709155223,0.));
#197982=CARTESIAN_POINT('',(-21.2610617890679,-7.52250298901264,0.));
#197983=CARTESIAN_POINT('',(-21.2610617890679,-7.52250298901264,0.));
#197984=CARTESIAN_POINT('',(-10.1343606576251,-3.58569854577611,0.));
#197985=CARTESIAN_POINT('Ctrl Pts',(-22.8400320311649,-12.4230808101438,
0.));
#197986=CARTESIAN_POINT('Ctrl Pts',(-22.8400320311649,-12.4230808101438,
12.));
#197987=CARTESIAN_POINT('Ctrl Pts',(-22.8370364396459,-12.418215285186,
0.));
#197988=CARTESIAN_POINT('Ctrl Pts',(-22.8370364396459,-12.418215285186,
12.));
#197989=CARTESIAN_POINT('Ctrl Pts',(-22.8310435872748,-12.4084933766346,
0.));
#197990=CARTESIAN_POINT('Ctrl Pts',(-22.8310435872748,-12.4084933766346,
12.));
#197991=CARTESIAN_POINT('Ctrl Pts',(-22.8220493007173,-12.3939379378998,
0.));
#197992=CARTESIAN_POINT('Ctrl Pts',(-22.8220493007173,-12.3939379378998,
12.));
#197993=CARTESIAN_POINT('Ctrl Pts',(-22.81004690224,-12.374585536673,0.));
#197994=CARTESIAN_POINT('Ctrl Pts',(-22.81004690224,-12.374585536673,12.));
#197995=CARTESIAN_POINT('Ctrl Pts',(-22.795027221673,-12.3504864740319,
0.));
#197996=CARTESIAN_POINT('Ctrl Pts',(-22.795027221673,-12.3504864740319,
12.));
#197997=CARTESIAN_POINT('Ctrl Pts',(-22.7799908974768,-12.3264788926075,
0.));
#197998=CARTESIAN_POINT('Ctrl Pts',(-22.7799908974768,-12.3264788926075,
12.));
#197999=CARTESIAN_POINT('Ctrl Pts',(-22.764938010105,-12.3025628601792,
0.));
#198000=CARTESIAN_POINT('Ctrl Pts',(-22.764938010105,-12.3025628601792,
12.));
#198001=CARTESIAN_POINT('Ctrl Pts',(-22.7498686970069,-12.2787384750742,
0.));
#198002=CARTESIAN_POINT('Ctrl Pts',(-22.7498686970069,-12.2787384750742,
12.));
#198003=CARTESIAN_POINT('Ctrl Pts',(-22.7347831655287,-12.2550058702395,
0.));
#198004=CARTESIAN_POINT('Ctrl Pts',(-22.7347831655287,-12.2550058702395,
12.));
#198005=CARTESIAN_POINT('Ctrl Pts',(-22.7196817119374,-12.2313652198061,
0.));
#198006=CARTESIAN_POINT('Ctrl Pts',(-22.7196817119374,-12.2313652198061,
12.));
#198007=CARTESIAN_POINT('Ctrl Pts',(-22.7045647168747,-12.2078167360284,
0.));
#198008=CARTESIAN_POINT('Ctrl Pts',(-22.7045647168747,-12.2078167360284,
12.));
#198009=CARTESIAN_POINT('Ctrl Pts',(-22.6894326205037,-12.1843606579261,
0.));
#198010=CARTESIAN_POINT('Ctrl Pts',(-22.6894326205037,-12.1843606579261,
12.));
#198011=CARTESIAN_POINT('Ctrl Pts',(-22.6742859034944,-12.1609972423099,
0.));
#198012=CARTESIAN_POINT('Ctrl Pts',(-22.6742859034944,-12.1609972423099,
12.));
#198013=CARTESIAN_POINT('Ctrl Pts',(-22.6591250653965,-12.1377267537145,
0.));
#198014=CARTESIAN_POINT('Ctrl Pts',(-22.6591250653965,-12.1377267537145,
12.));
#198015=CARTESIAN_POINT('Ctrl Pts',(-22.6439506046605,-12.1145494550383,
0.));
#198016=CARTESIAN_POINT('Ctrl Pts',(-22.6439506046605,-12.1145494550383,
12.));
#198017=CARTESIAN_POINT('Ctrl Pts',(-22.6287629967056,-12.0914655972823,
0.));
#198018=CARTESIAN_POINT('Ctrl Pts',(-22.6287629967056,-12.0914655972823,
12.));
#198019=CARTESIAN_POINT('Ctrl Pts',(-22.6135626764898,-12.0684754113862,
0.));
#198020=CARTESIAN_POINT('Ctrl Pts',(-22.6135626764898,-12.0684754113862,
12.));
#198021=CARTESIAN_POINT('Ctrl Pts',(-22.5983500505644,-12.0455791139128,
0.));
#198022=CARTESIAN_POINT('Ctrl Pts',(-22.5983500505644,-12.0455791139128,
12.));
#198023=CARTESIAN_POINT('Ctrl Pts',(-22.5831255061282,-12.0227769113127,
0.));
#198024=CARTESIAN_POINT('Ctrl Pts',(-22.5831255061282,-12.0227769113127,
12.));
#198025=CARTESIAN_POINT('Ctrl Pts',(-22.5678894211181,-12.0000690046695,
0.));
#198026=CARTESIAN_POINT('Ctrl Pts',(-22.5678894211181,-12.0000690046695,
12.));
#198027=CARTESIAN_POINT('Ctrl Pts',(-22.5526421741158,-11.9774555943496,
0.));
#198028=CARTESIAN_POINT('Ctrl Pts',(-22.5526421741158,-11.9774555943496,
12.));
#198029=CARTESIAN_POINT('Ctrl Pts',(-22.5373841537307,-11.9549368843997,
0.));
#198030=CARTESIAN_POINT('Ctrl Pts',(-22.5373841537307,-11.9549368843997,
12.));
#198031=CARTESIAN_POINT('Ctrl Pts',(-22.5221157697883,-11.9325130877803,
0.));
#198032=CARTESIAN_POINT('Ctrl Pts',(-22.5221157697883,-11.9325130877803,
12.));
#198033=CARTESIAN_POINT('Ctrl Pts',(-22.5068374513973,-11.9101844254557,
0.));
#198034=CARTESIAN_POINT('Ctrl Pts',(-22.5068374513973,-11.9101844254557,
12.));
#198035=CARTESIAN_POINT('Ctrl Pts',(-22.4915496418485,-11.8879511239942,
0.));
#198036=CARTESIAN_POINT('Ctrl Pts',(-22.4915496418485,-11.8879511239942,
12.));
#198037=CARTESIAN_POINT('Ctrl Pts',(-22.4762527946702,-11.8658134137019,
0.));
#198038=CARTESIAN_POINT('Ctrl Pts',(-22.4762527946702,-11.8658134137019,
12.));
#198039=CARTESIAN_POINT('Ctrl Pts',(-22.4609473690471,-11.8437715264487,
0.));
#198040=CARTESIAN_POINT('Ctrl Pts',(-22.4609473690471,-11.8437715264487,
12.));
#198041=CARTESIAN_POINT('Ctrl Pts',(-22.4456338258735,-11.8218256937889,
0.));
#198042=CARTESIAN_POINT('Ctrl Pts',(-22.4456338258735,-11.8218256937889,
12.));
#198043=CARTESIAN_POINT('Ctrl Pts',(-22.430312622646,-11.7999761445173,
0.));
#198044=CARTESIAN_POINT('Ctrl Pts',(-22.430312622646,-11.7999761445173,
12.));
#198045=CARTESIAN_POINT('Ctrl Pts',(-22.4149842125008,-11.7782231042039,
0.));
#198046=CARTESIAN_POINT('Ctrl Pts',(-22.4149842125008,-11.7782231042039,
12.));
#198047=CARTESIAN_POINT('Ctrl Pts',(-22.3996490469191,-11.7565667964764,
0.));
#198048=CARTESIAN_POINT('Ctrl Pts',(-22.3996490469191,-11.7565667964764,
12.));
#198049=CARTESIAN_POINT('Ctrl Pts',(-22.3843075773899,-11.7350074437961,
0.));
#198050=CARTESIAN_POINT('Ctrl Pts',(-22.3843075773899,-11.7350074437961,
12.));
#198051=CARTESIAN_POINT('Ctrl Pts',(-22.3689602575491,-11.7135452684532,
0.));
#198052=CARTESIAN_POINT('Ctrl Pts',(-22.3689602575491,-11.7135452684532,
12.));
#198053=CARTESIAN_POINT('Ctrl Pts',(-22.3536075450029,-11.6921804934056,
0.));
#198054=CARTESIAN_POINT('Ctrl Pts',(-22.3536075450029,-11.6921804934056,
12.));
#198055=CARTESIAN_POINT('Ctrl Pts',(-22.3382499035619,-11.6709133432985,
0.));
#198056=CARTESIAN_POINT('Ctrl Pts',(-22.3382499035619,-11.6709133432985,
12.));
#198057=CARTESIAN_POINT('Ctrl Pts',(-22.3228878043976,-11.6497440449857,
0.));
#198058=CARTESIAN_POINT('Ctrl Pts',(-22.3228878043976,-11.6497440449857,
12.));
#198059=CARTESIAN_POINT('Ctrl Pts',(-22.3075217249049,-11.6286728270009,
0.));
#198060=CARTESIAN_POINT('Ctrl Pts',(-22.3075217249049,-11.6286728270009,
12.));
#198061=CARTESIAN_POINT('Ctrl Pts',(-22.2921521480356,-11.6076999192357,
0.));
#198062=CARTESIAN_POINT('Ctrl Pts',(-22.2921521480356,-11.6076999192357,
12.));
#198063=CARTESIAN_POINT('Ctrl Pts',(-22.2767795614348,-11.5868255525188,
0.));
#198064=CARTESIAN_POINT('Ctrl Pts',(-22.2767795614348,-11.5868255525188,
12.));
#198065=CARTESIAN_POINT('Ctrl Pts',(-22.2614044566898,-11.5660499582403,
0.));
#198066=CARTESIAN_POINT('Ctrl Pts',(-22.2614044566898,-11.5660499582403,
12.));
#198067=CARTESIAN_POINT('Ctrl Pts',(-22.2460273284654,-11.5453733679121,
0.));
#198068=CARTESIAN_POINT('Ctrl Pts',(-22.2460273284654,-11.5453733679121,
12.));
#198069=CARTESIAN_POINT('Ctrl Pts',(-22.2306486738901,-11.5247960128477,
0.));
#198070=CARTESIAN_POINT('Ctrl Pts',(-22.2306486738901,-11.5247960128477,
12.));
#198071=CARTESIAN_POINT('Ctrl Pts',(-22.2152689931022,-11.5043181244242,
0.));
#198072=CARTESIAN_POINT('Ctrl Pts',(-22.2152689931022,-11.5043181244242,
12.));
#198073=CARTESIAN_POINT('Ctrl Pts',(-22.1998887896436,-11.483939934259,
0.));
#198074=CARTESIAN_POINT('Ctrl Pts',(-22.1998887896436,-11.483939934259,
12.));
#198075=CARTESIAN_POINT('Ctrl Pts',(-22.184508570917,-11.463661674411,0.));
#198076=CARTESIAN_POINT('Ctrl Pts',(-22.184508570917,-11.463661674411,12.));
#198077=CARTESIAN_POINT('Ctrl Pts',(-22.1691288486096,-11.443483577557,
0.));
#198078=CARTESIAN_POINT('Ctrl Pts',(-22.1691288486096,-11.443483577557,
12.));
#198079=CARTESIAN_POINT('Ctrl Pts',(-22.1537501391487,-11.4234058771742,
0.));
#198080=CARTESIAN_POINT('Ctrl Pts',(-22.1537501391487,-11.4234058771742,
12.));
#198081=CARTESIAN_POINT('Ctrl Pts',(-22.1383729640964,-11.4034288076908,
0.));
#198082=CARTESIAN_POINT('Ctrl Pts',(-22.1383729640964,-11.4034288076908,
12.));
#198083=CARTESIAN_POINT('Ctrl Pts',(-22.1229978500186,-11.3835526044256,
0.));
#198084=CARTESIAN_POINT('Ctrl Pts',(-22.1229978500186,-11.3835526044256,
12.));
#198085=CARTESIAN_POINT('Ctrl Pts',(-22.1076253283979,-11.3637775035367,
0.));
#198086=CARTESIAN_POINT('Ctrl Pts',(-22.1076253283979,-11.3637775035367,
12.));
#198087=CARTESIAN_POINT('Ctrl Pts',(-22.0922559355294,-11.3441037419553,
0.));
#198088=CARTESIAN_POINT('Ctrl Pts',(-22.0922559355294,-11.3441037419553,
12.));
#198089=CARTESIAN_POINT('Ctrl Pts',(-22.0768902124267,-11.3245315573168,
0.));
#198090=CARTESIAN_POINT('Ctrl Pts',(-22.0768902124267,-11.3245315573168,
12.));
#198091=CARTESIAN_POINT('Ctrl Pts',(-22.0615287047179,-11.3050611878771,
0.));
#198092=CARTESIAN_POINT('Ctrl Pts',(-22.0615287047179,-11.3050611878771,
12.));
#198093=CARTESIAN_POINT('Ctrl Pts',(-22.046171962566,-11.2856928724374,
0.));
#198094=CARTESIAN_POINT('Ctrl Pts',(-22.046171962566,-11.2856928724374,
12.));
#198095=CARTESIAN_POINT('Ctrl Pts',(-22.030820540835,-11.2664268504206,
0.));
#198096=CARTESIAN_POINT('Ctrl Pts',(-22.030820540835,-11.2664268504206,
12.));
#198097=CARTESIAN_POINT('Ctrl Pts',(-22.0154749992363,-11.2472633619275,
0.));
#198098=CARTESIAN_POINT('Ctrl Pts',(-22.0154749992363,-11.2472633619275,
12.));
#198099=CARTESIAN_POINT('Ctrl Pts',(-22.0001359024839,-11.2282026477896,
0.));
#198100=CARTESIAN_POINT('Ctrl Pts',(-22.0001359024839,-11.2282026477896,
12.));
#198101=CARTESIAN_POINT('Ctrl Pts',(-21.9848038204439,-11.2092449496125,
0.));
#198102=CARTESIAN_POINT('Ctrl Pts',(-21.9848038204439,-11.2092449496125,
12.));
#198103=CARTESIAN_POINT('Ctrl Pts',(-21.9694793282914,-11.190390509811,
0.));
#198104=CARTESIAN_POINT('Ctrl Pts',(-21.9694793282914,-11.190390509811,
12.));
#198105=CARTESIAN_POINT('Ctrl Pts',(-21.9541630066506,-11.1716395716376,
0.));
#198106=CARTESIAN_POINT('Ctrl Pts',(-21.9541630066506,-11.1716395716376,
12.));
#198107=CARTESIAN_POINT('Ctrl Pts',(-21.9388554416439,-11.1529923792003,
0.));
#198108=CARTESIAN_POINT('Ctrl Pts',(-21.9388554416439,-11.1529923792003,
12.));
#198109=CARTESIAN_POINT('Ctrl Pts',(-21.923557224952,-11.1344491774741,
0.));
#198110=CARTESIAN_POINT('Ctrl Pts',(-21.923557224952,-11.1344491774741,
12.));
#198111=CARTESIAN_POINT('Ctrl Pts',(-21.9082689538688,-11.1160102123024,
0.));
#198112=CARTESIAN_POINT('Ctrl Pts',(-21.9082689538688,-11.1160102123024,
12.));
#198113=CARTESIAN_POINT('Ctrl Pts',(-21.8929912313608,-11.0976757303944,
0.));
#198114=CARTESIAN_POINT('Ctrl Pts',(-21.8929912313608,-11.0976757303944,
12.));
#198115=CARTESIAN_POINT('Ctrl Pts',(-21.877724666119,-11.0794459793057,
0.));
#198116=CARTESIAN_POINT('Ctrl Pts',(-21.877724666119,-11.0794459793057,
12.));
#198117=CARTESIAN_POINT('Ctrl Pts',(-21.8624698726318,-11.0613212074363,
0.));
#198118=CARTESIAN_POINT('Ctrl Pts',(-21.8624698726318,-11.0613212074363,
12.));
#198119=CARTESIAN_POINT('Ctrl Pts',(-21.8472274713103,-11.0433016640807,
0.));
#198120=CARTESIAN_POINT('Ctrl Pts',(-21.8472274713103,-11.0433016640807,
12.));
#198121=CARTESIAN_POINT('Ctrl Pts',(-21.8319980886033,-11.0253875994598,
0.));
#198122=CARTESIAN_POINT('Ctrl Pts',(-21.8319980886033,-11.0253875994598,
12.));
#198123=CARTESIAN_POINT('Ctrl Pts',(-21.8167823571168,-11.0075792647477,
0.));
#198124=CARTESIAN_POINT('Ctrl Pts',(-21.8167823571168,-11.0075792647477,
12.));
#198125=CARTESIAN_POINT('Ctrl Pts',(-21.8015809157301,-10.9898769120912,
0.));
#198126=CARTESIAN_POINT('Ctrl Pts',(-21.8015809157301,-10.9898769120912,
12.));
#198127=CARTESIAN_POINT('Ctrl Pts',(-21.7863944097141,-10.9722807946155,
0.));
#198128=CARTESIAN_POINT('Ctrl Pts',(-21.7863944097141,-10.9722807946155,
12.));
#198129=CARTESIAN_POINT('Ctrl Pts',(-21.7712234908464,-10.9547911664455,
0.));
#198130=CARTESIAN_POINT('Ctrl Pts',(-21.7712234908464,-10.9547911664455,
12.));
#198131=CARTESIAN_POINT('Ctrl Pts',(-21.7560688175247,-10.9374082827444,
0.));
#198132=CARTESIAN_POINT('Ctrl Pts',(-21.7560688175247,-10.9374082827444,
12.));
#198133=CARTESIAN_POINT('Ctrl Pts',(-21.7409310548797,-10.9201323997384,
0.));
#198134=CARTESIAN_POINT('Ctrl Pts',(-21.7409310548797,-10.9201323997384,
12.));
#198135=CARTESIAN_POINT('Ctrl Pts',(-21.7258108748873,-10.902963774734,
0.));
#198136=CARTESIAN_POINT('Ctrl Pts',(-21.7258108748873,-10.902963774734,
12.));
#198137=CARTESIAN_POINT('Ctrl Pts',(-21.7107089564825,-10.8859026661293,
0.));
#198138=CARTESIAN_POINT('Ctrl Pts',(-21.7107089564825,-10.8859026661293,
12.));
#198139=CARTESIAN_POINT('Ctrl Pts',(-21.6956259856672,-10.8689493334095,
0.));
#198140=CARTESIAN_POINT('Ctrl Pts',(-21.6956259856672,-10.8689493334095,
12.));
#198141=CARTESIAN_POINT('Ctrl Pts',(-21.6805626556467,-10.8521040371835,
0.));
#198142=CARTESIAN_POINT('Ctrl Pts',(-21.6805626556467,-10.8521040371835,
12.));
#198143=CARTESIAN_POINT('Ctrl Pts',(-21.6655196669732,-10.8353670392272,
0.));
#198144=CARTESIAN_POINT('Ctrl Pts',(-21.6655196669732,-10.8353670392272,
12.));
#198145=CARTESIAN_POINT('Ctrl Pts',(-21.6504977276866,-10.8187386025136,
0.));
#198146=CARTESIAN_POINT('Ctrl Pts',(-21.6504977276866,-10.8187386025136,
12.));
#198147=CARTESIAN_POINT('Ctrl Pts',(-21.6354975534557,-10.8022189912369,
0.));
#198148=CARTESIAN_POINT('Ctrl Pts',(-21.6354975534557,-10.8022189912369,
12.));
#198149=CARTESIAN_POINT('Ctrl Pts',(-21.6205198677173,-10.7858084708261,
0.));
#198150=CARTESIAN_POINT('Ctrl Pts',(-21.6205198677173,-10.7858084708261,
12.));
#198151=CARTESIAN_POINT('Ctrl Pts',(-21.6055654018176,-10.7695073079552,
0.));
#198152=CARTESIAN_POINT('Ctrl Pts',(-21.6055654018176,-10.7695073079552,
12.));
#198153=CARTESIAN_POINT('Ctrl Pts',(-21.5906348951743,-10.7533157705941,
0.));
#198154=CARTESIAN_POINT('Ctrl Pts',(-21.5906348951743,-10.7533157705941,
12.));
#198155=CARTESIAN_POINT('Ctrl Pts',(-21.5757290954371,-10.7372341280467,
0.));
#198156=CARTESIAN_POINT('Ctrl Pts',(-21.5757290954371,-10.7372341280467,
12.));
#198157=CARTESIAN_POINT('Ctrl Pts',(-21.5608487586468,-10.7212626509816,
0.));
#198158=CARTESIAN_POINT('Ctrl Pts',(-21.5608487586468,-10.7212626509816,
12.));
#198159=CARTESIAN_POINT('Ctrl Pts',(-21.5459946493955,-10.7054016114571,
0.));
#198160=CARTESIAN_POINT('Ctrl Pts',(-21.5459946493955,-10.7054016114571,
12.));
#198161=CARTESIAN_POINT('Ctrl Pts',(-21.5311675409807,-10.689651282929,
0.));
#198162=CARTESIAN_POINT('Ctrl Pts',(-21.5311675409807,-10.689651282929,
12.));
#198163=CARTESIAN_POINT('Ctrl Pts',(-21.51636821558,-10.6740119402834,0.));
#198164=CARTESIAN_POINT('Ctrl Pts',(-21.51636821558,-10.6740119402834,12.));
#198165=CARTESIAN_POINT('Ctrl Pts',(-21.5015974644449,-10.6584838598939,
0.));
#198166=CARTESIAN_POINT('Ctrl Pts',(-21.5015974644449,-10.6584838598939,
12.));
#198167=CARTESIAN_POINT('Ctrl Pts',(-21.4868560880889,-10.6430673196607,
0.));
#198168=CARTESIAN_POINT('Ctrl Pts',(-21.4868560880889,-10.6430673196607,
12.));
#198169=CARTESIAN_POINT('Ctrl Pts',(-21.4721448964766,-10.6277625990456,
0.));
#198170=CARTESIAN_POINT('Ctrl Pts',(-21.4721448964766,-10.6277625990456,
12.));
#198171=CARTESIAN_POINT('Ctrl Pts',(-21.4574647092097,-10.6125699790961,
0.));
#198172=CARTESIAN_POINT('Ctrl Pts',(-21.4574647092097,-10.6125699790961,
12.));
#198173=CARTESIAN_POINT('Ctrl Pts',(-21.4428163557144,-10.5974897424622,
0.));
#198174=CARTESIAN_POINT('Ctrl Pts',(-21.4428163557144,-10.5974897424622,
12.));
#198175=CARTESIAN_POINT('Ctrl Pts',(-21.4282006754631,-10.5825221734573,
0.));
#198176=CARTESIAN_POINT('Ctrl Pts',(-21.4282006754631,-10.5825221734573,
12.));
#198177=CARTESIAN_POINT('Ctrl Pts',(-21.4136185181979,-10.5676675581108,
0.));
#198178=CARTESIAN_POINT('Ctrl Pts',(-21.4136185181979,-10.5676675581108,
12.));
#198179=CARTESIAN_POINT('Ctrl Pts',(-21.3990707441497,-10.5529261842108,
0.));
#198180=CARTESIAN_POINT('Ctrl Pts',(-21.3990707441497,-10.5529261842108,
12.));
#198181=CARTESIAN_POINT('Ctrl Pts',(-21.3845582242602,-10.5382983413421,
0.));
#198182=CARTESIAN_POINT('Ctrl Pts',(-21.3845582242602,-10.5382983413421,
12.));
#198183=CARTESIAN_POINT('Ctrl Pts',(-21.3700818403936,-10.5237843209057,
0.));
#198184=CARTESIAN_POINT('Ctrl Pts',(-21.3700818403936,-10.5237843209057,
12.));
#198185=CARTESIAN_POINT('Ctrl Pts',(-21.3556424855814,-10.5093844161685,
0.));
#198186=CARTESIAN_POINT('Ctrl Pts',(-21.3556424855814,-10.5093844161685,
12.));
#198187=CARTESIAN_POINT('Ctrl Pts',(-21.3412410642904,-10.4950989223337,
0.));
#198188=CARTESIAN_POINT('Ctrl Pts',(-21.3412410642904,-10.4950989223337,
12.));
#198189=CARTESIAN_POINT('Ctrl Pts',(-21.3268784926819,-10.4809281365931,
0.));
#198190=CARTESIAN_POINT('Ctrl Pts',(-21.3268784926819,-10.4809281365931,
12.));
#198191=CARTESIAN_POINT('Ctrl Pts',(-21.3125556988731,-10.4668723581768,
0.));
#198192=CARTESIAN_POINT('Ctrl Pts',(-21.3125556988731,-10.4668723581768,
12.));
#198193=CARTESIAN_POINT('Ctrl Pts',(-21.2982736231931,-10.4529318883874,
0.));
#198194=CARTESIAN_POINT('Ctrl Pts',(-21.2982736231931,-10.4529318883874,
12.));
#198195=CARTESIAN_POINT('Ctrl Pts',(-21.2840332184483,-10.4391070306391,
0.));
#198196=CARTESIAN_POINT('Ctrl Pts',(-21.2840332184483,-10.4391070306391,
12.));
#198197=CARTESIAN_POINT('Ctrl Pts',(-21.2698354502403,-10.42539809054,0.));
#198198=CARTESIAN_POINT('Ctrl Pts',(-21.2698354502403,-10.42539809054,12.));
#198199=CARTESIAN_POINT('Ctrl Pts',(-21.255681297275,-10.4118053759588,
0.));
#198200=CARTESIAN_POINT('Ctrl Pts',(-21.255681297275,-10.4118053759588,
12.));
#198201=CARTESIAN_POINT('Ctrl Pts',(-21.2415717516714,-10.3983291970846,
0.));
#198202=CARTESIAN_POINT('Ctrl Pts',(-21.2415717516714,-10.3983291970846,
12.));
#198203=CARTESIAN_POINT('Ctrl Pts',(-21.22750781927,-10.3849698664786,0.));
#198204=CARTESIAN_POINT('Ctrl Pts',(-21.22750781927,-10.3849698664786,12.));
#198205=CARTESIAN_POINT('Ctrl Pts',(-21.2134905199345,-10.371727699113,
0.));
#198206=CARTESIAN_POINT('Ctrl Pts',(-21.2134905199345,-10.371727699113,
12.));
#198207=CARTESIAN_POINT('Ctrl Pts',(-21.199520887919,-10.3586030124587,
0.));
#198208=CARTESIAN_POINT('Ctrl Pts',(-21.199520887919,-10.3586030124587,
12.));
#198209=CARTESIAN_POINT('Ctrl Pts',(-21.1855999722416,-10.34559612657,0.));
#198210=CARTESIAN_POINT('Ctrl Pts',(-21.1855999722416,-10.34559612657,12.));
#198211=CARTESIAN_POINT('Ctrl Pts',(-21.1717288370509,-10.3327073641572,
0.));
#198212=CARTESIAN_POINT('Ctrl Pts',(-21.1717288370509,-10.3327073641572,
12.));
#198213=CARTESIAN_POINT('Ctrl Pts',(-21.1579085619965,-10.3199370506544,
0.));
#198214=CARTESIAN_POINT('Ctrl Pts',(-21.1579085619965,-10.3199370506544,
12.));
#198215=CARTESIAN_POINT('Ctrl Pts',(-21.1441402425843,-10.3072855142687,
0.));
#198216=CARTESIAN_POINT('Ctrl Pts',(-21.1441402425843,-10.3072855142687,
12.));
#198217=CARTESIAN_POINT('Ctrl Pts',(-21.1304249906002,-10.2947530860721,
0.));
#198218=CARTESIAN_POINT('Ctrl Pts',(-21.1304249906002,-10.2947530860721,
12.));
#198219=CARTESIAN_POINT('Ctrl Pts',(-21.1167639345631,-10.2823401001072,
0.));
#198220=CARTESIAN_POINT('Ctrl Pts',(-21.1167639345631,-10.2823401001072,
12.));
#198221=CARTESIAN_POINT('Ctrl Pts',(-21.1031582201627,-10.2700468934744,
0.));
#198222=CARTESIAN_POINT('Ctrl Pts',(-21.1031582201627,-10.2700468934744,
12.));
#198223=CARTESIAN_POINT('Ctrl Pts',(-21.0896090107063,-10.2578738064181,
0.));
#198224=CARTESIAN_POINT('Ctrl Pts',(-21.0896090107063,-10.2578738064181,
12.));
#198225=CARTESIAN_POINT('Ctrl Pts',(-21.0761174875445,-10.2458211823912,
0.));
#198226=CARTESIAN_POINT('Ctrl Pts',(-21.0761174875445,-10.2458211823912,
12.));
#198227=CARTESIAN_POINT('Ctrl Pts',(-21.0626848505663,-10.2338893681567,
0.));
#198228=CARTESIAN_POINT('Ctrl Pts',(-21.0626848505663,-10.2338893681567,
12.));
#198229=CARTESIAN_POINT('Ctrl Pts',(-21.0493123187483,-10.2220787139154,
0.));
#198230=CARTESIAN_POINT('Ctrl Pts',(-21.0493123187483,-10.2220787139154,
12.));
#198231=CARTESIAN_POINT('Ctrl Pts',(-21.0360011306815,-10.2103895734123,
0.));
#198232=CARTESIAN_POINT('Ctrl Pts',(-21.0360011306815,-10.2103895734123,
12.));
#198233=CARTESIAN_POINT('Ctrl Pts',(-21.0227525451107,-10.1988223040425,
0.));
#198234=CARTESIAN_POINT('Ctrl Pts',(-21.0227525451107,-10.1988223040425,
12.));
#198235=CARTESIAN_POINT('Ctrl Pts',(-21.0095678414486,-10.187377266936,
0.));
#198236=CARTESIAN_POINT('Ctrl Pts',(-21.0095678414486,-10.187377266936,
12.));
#198237=CARTESIAN_POINT('Ctrl Pts',(-20.9964483203686,-10.1760548270767,
0.));
#198238=CARTESIAN_POINT('Ctrl Pts',(-20.9964483203686,-10.1760548270767,
12.));
#198239=CARTESIAN_POINT('Ctrl Pts',(-20.9833953044736,-10.1648553534568,
0.));
#198240=CARTESIAN_POINT('Ctrl Pts',(-20.9833953044736,-10.1648553534568,
12.));
#198241=CARTESIAN_POINT('Ctrl Pts',(-20.9704101389369,-10.1537792192065,
0.));
#198242=CARTESIAN_POINT('Ctrl Pts',(-20.9704101389369,-10.1537792192065,
12.));
#198243=CARTESIAN_POINT('Ctrl Pts',(-20.9574941921591,-10.1428268017256,
0.));
#198244=CARTESIAN_POINT('Ctrl Pts',(-20.9574941921591,-10.1428268017256,
12.));
#198245=CARTESIAN_POINT('Ctrl Pts',(-20.9446488563933,-10.1319984827908,
0.));
#198246=CARTESIAN_POINT('Ctrl Pts',(-20.9446488563933,-10.1319984827908,
12.));
#198247=CARTESIAN_POINT('Ctrl Pts',(-20.9318755484734,-10.1212946487057,
0.));
#198248=CARTESIAN_POINT('Ctrl Pts',(-20.9318755484734,-10.1212946487057,
12.));
#198249=CARTESIAN_POINT('Ctrl Pts',(-20.919175710627,-10.1107156904836,
0.));
#198250=CARTESIAN_POINT('Ctrl Pts',(-20.919175710627,-10.1107156904836,
12.));
#198251=CARTESIAN_POINT('Ctrl Pts',(-20.9065508112557,-10.1002620040076,
0.));
#198252=CARTESIAN_POINT('Ctrl Pts',(-20.9065508112557,-10.1002620040076,
12.));
#198253=CARTESIAN_POINT('Ctrl Pts',(-20.894002345737,-10.0899339901915,
0.));
#198254=CARTESIAN_POINT('Ctrl Pts',(-20.894002345737,-10.0899339901915,
12.));
#198255=CARTESIAN_POINT('Ctrl Pts',(-20.881531837184,-10.0797320551154,
0.));
#198256=CARTESIAN_POINT('Ctrl Pts',(-20.881531837184,-10.0797320551154,
12.));
#198257=CARTESIAN_POINT('Ctrl Pts',(-20.86914083737,-10.0696566102218,0.));
#198258=CARTESIAN_POINT('Ctrl Pts',(-20.86914083737,-10.0696566102218,12.));
#198259=CARTESIAN_POINT('Ctrl Pts',(-20.8568309277316,-10.0597080725375,
0.));
#198260=CARTESIAN_POINT('Ctrl Pts',(-20.8568309277316,-10.0597080725375,
12.));
#198261=CARTESIAN_POINT('Ctrl Pts',(-20.8446037203402,-10.0498868648733,
0.));
#198262=CARTESIAN_POINT('Ctrl Pts',(-20.8446037203402,-10.0498868648733,
12.));
#198263=CARTESIAN_POINT('Ctrl Pts',(-20.8324608588909,-10.0401934160234,
0.));
#198264=CARTESIAN_POINT('Ctrl Pts',(-20.8324608588909,-10.0401934160234,
12.));
#198265=CARTESIAN_POINT('Ctrl Pts',(-20.8204040196602,-10.0306281609435,
0.));
#198266=CARTESIAN_POINT('Ctrl Pts',(-20.8204040196602,-10.0306281609435,
12.));
#198267=CARTESIAN_POINT('Ctrl Pts',(-20.8084349126888,-10.0211915410095,
0.));
#198268=CARTESIAN_POINT('Ctrl Pts',(-20.8084349126888,-10.0211915410095,
12.));
#198269=CARTESIAN_POINT('Ctrl Pts',(-20.7965552829908,-10.0118840042786,
0.));
#198270=CARTESIAN_POINT('Ctrl Pts',(-20.7965552829908,-10.0118840042786,
12.));
#198271=CARTESIAN_POINT('Ctrl Pts',(-20.7847669117568,-10.0027060057389,
0.));
#198272=CARTESIAN_POINT('Ctrl Pts',(-20.7847669117568,-10.0027060057389,
12.));
#198273=CARTESIAN_POINT('Ctrl Pts',(-20.7730716175417,-9.9936580075464,
0.));
#198274=CARTESIAN_POINT('Ctrl Pts',(-20.7730716175417,-9.9936580075464,
12.));
#198275=CARTESIAN_POINT('Ctrl Pts',(-20.761471257499,-9.98474047926852,
0.));
#198276=CARTESIAN_POINT('Ctrl Pts',(-20.761471257499,-9.98474047926852,
12.));
#198277=CARTESIAN_POINT('Ctrl Pts',(-20.7499677289627,-9.9759538982347,
0.));
#198278=CARTESIAN_POINT('Ctrl Pts',(-20.7499677289627,-9.9759538982347,
12.));
#198279=CARTESIAN_POINT('Ctrl Pts',(-20.7385629709795,-9.96729874986201,
0.));
#198280=CARTESIAN_POINT('Ctrl Pts',(-20.7385629709795,-9.96729874986201,
12.));
#198281=CARTESIAN_POINT('Ctrl Pts',(-20.7272589658751,-9.95877552798397,
0.));
#198282=CARTESIAN_POINT('Ctrl Pts',(-20.7272589658751,-9.95877552798397,
12.));
#198283=CARTESIAN_POINT('Ctrl Pts',(-20.7160577407579,-9.95038473514948,
0.));
#198284=CARTESIAN_POINT('Ctrl Pts',(-20.7160577407579,-9.95038473514948,
12.));
#198285=CARTESIAN_POINT('Ctrl Pts',(-20.7049613692234,-9.94212688298236,
0.));
#198286=CARTESIAN_POINT('Ctrl Pts',(-20.7049613692234,-9.94212688298236,
12.));
#198287=CARTESIAN_POINT('Ctrl Pts',(-20.6939719732484,-9.93400249259729,
0.));
#198288=CARTESIAN_POINT('Ctrl Pts',(-20.6939719732484,-9.93400249259729,
12.));
#198289=CARTESIAN_POINT('Ctrl Pts',(-20.6830917250255,-9.92601209498748,
0.));
#198290=CARTESIAN_POINT('Ctrl Pts',(-20.6830917250255,-9.92601209498748,
12.));
#198291=CARTESIAN_POINT('Ctrl Pts',(-20.6723228488263,-9.91815623141288,
0.));
#198292=CARTESIAN_POINT('Ctrl Pts',(-20.6723228488263,-9.91815623141288,
12.));
#198293=CARTESIAN_POINT('Ctrl Pts',(-20.6616676228315,-9.91043545377007,
0.));
#198294=CARTESIAN_POINT('Ctrl Pts',(-20.6616676228315,-9.91043545377007,
12.));
#198295=CARTESIAN_POINT('Ctrl Pts',(-20.6511283817414,-9.90285032516692,
0.));
#198296=CARTESIAN_POINT('Ctrl Pts',(-20.6511283817414,-9.90285032516692,
12.));
#198297=CARTESIAN_POINT('Ctrl Pts',(-20.6407075193976,-9.89540142049119,
0.));
#198298=CARTESIAN_POINT('Ctrl Pts',(-20.6407075193976,-9.89540142049119,
12.));
#198299=CARTESIAN_POINT('Ctrl Pts',(-20.6304074914087,-9.88808932697306,
0.));
#198300=CARTESIAN_POINT('Ctrl Pts',(-20.6304074914087,-9.88808932697306,
12.));
#198301=CARTESIAN_POINT('Ctrl Pts',(-20.6202308177474,-9.88091464472675,
0.));
#198302=CARTESIAN_POINT('Ctrl Pts',(-20.6202308177474,-9.88091464472675,
12.));
#198303=CARTESIAN_POINT('Ctrl Pts',(-20.6101800854494,-9.87387798732956,
0.));
#198304=CARTESIAN_POINT('Ctrl Pts',(-20.6101800854494,-9.87387798732956,
12.));
#198305=CARTESIAN_POINT('Ctrl Pts',(-20.6002579513699,-9.86697998242622,
0.));
#198306=CARTESIAN_POINT('Ctrl Pts',(-20.6002579513699,-9.86697998242622,
12.));
#198307=CARTESIAN_POINT('Ctrl Pts',(-20.5904671449754,-9.86022127232747,
0.));
#198308=CARTESIAN_POINT('Ctrl Pts',(-20.5904671449754,-9.86022127232747,
12.));
#198309=CARTESIAN_POINT('Ctrl Pts',(-20.5808104710015,-9.8536025145698,
0.));
#198310=CARTESIAN_POINT('Ctrl Pts',(-20.5808104710015,-9.8536025145698,
12.));
#198311=CARTESIAN_POINT('Ctrl Pts',(-20.5712908125139,-9.84712438256277,
0.));
#198312=CARTESIAN_POINT('Ctrl Pts',(-20.5712908125139,-9.84712438256277,
12.));
#198313=CARTESIAN_POINT('Ctrl Pts',(-20.5619111362402,-9.84078756677565,
0.));
#198314=CARTESIAN_POINT('Ctrl Pts',(-20.5619111362402,-9.84078756677565,
12.));
#198315=CARTESIAN_POINT('Ctrl Pts',(-20.552674497646,-9.83459277585315,
0.));
#198316=CARTESIAN_POINT('Ctrl Pts',(-20.552674497646,-9.83459277585315,
12.));
#198317=CARTESIAN_POINT('Ctrl Pts',(-20.5435840460721,-9.82854073773877,
0.));
#198318=CARTESIAN_POINT('Ctrl Pts',(-20.5435840460721,-9.82854073773877,
12.));
#198319=CARTESIAN_POINT('Ctrl Pts',(-20.5346430299517,-9.82263220080362,
0.));
#198320=CARTESIAN_POINT('Ctrl Pts',(-20.5346430299517,-9.82263220080362,
12.));
#198321=CARTESIAN_POINT('Ctrl Pts',(-20.5258548000629,-9.81686793455942,
0.));
#198322=CARTESIAN_POINT('Ctrl Pts',(-20.5258548000629,-9.81686793455942,
12.));
#198323=CARTESIAN_POINT('Ctrl Pts',(-20.517222812284,-9.81124873025281,
0.));
#198324=CARTESIAN_POINT('Ctrl Pts',(-20.517222812284,-9.81124873025281,
12.));
#198325=CARTESIAN_POINT('Ctrl Pts',(-20.5087506310505,-9.80577540161087,
0.));
#198326=CARTESIAN_POINT('Ctrl Pts',(-20.5087506310505,-9.80577540161087,
12.));
#198327=CARTESIAN_POINT('Ctrl Pts',(-20.5004419312107,-9.80044878520948,
0.));
#198328=CARTESIAN_POINT('Ctrl Pts',(-20.5004419312107,-9.80044878520948,
12.));
#198329=CARTESIAN_POINT('Ctrl Pts',(-20.4923005087943,-9.7952697428833,
0.));
#198330=CARTESIAN_POINT('Ctrl Pts',(-20.4923005087943,-9.7952697428833,
12.));
#198331=CARTESIAN_POINT('Ctrl Pts',(-20.4843302955329,-9.79023916498655,
0.));
#198332=CARTESIAN_POINT('Ctrl Pts',(-20.4843302955329,-9.79023916498655,
12.));
#198333=CARTESIAN_POINT('Ctrl Pts',(-20.4765353711586,-9.78535797314166,
0.));
#198334=CARTESIAN_POINT('Ctrl Pts',(-20.4765353711586,-9.78535797314166,
12.));
#198335=CARTESIAN_POINT('Ctrl Pts',(-20.4689199790669,-9.7806271237332,
0.));
#198336=CARTESIAN_POINT('Ctrl Pts',(-20.4689199790669,-9.7806271237332,
12.));
#198337=CARTESIAN_POINT('Ctrl Pts',(-20.4614885274975,-9.77604760815528,
0.));
#198338=CARTESIAN_POINT('Ctrl Pts',(-20.4614885274975,-9.77604760815528,
12.));
#198339=CARTESIAN_POINT('Ctrl Pts',(-20.4542455817527,-9.77162045104069,
0.));
#198340=CARTESIAN_POINT('Ctrl Pts',(-20.4542455817527,-9.77162045104069,
12.));
#198341=CARTESIAN_POINT('Ctrl Pts',(-20.447195862298,-9.76734670980891,
0.));
#198342=CARTESIAN_POINT('Ctrl Pts',(-20.447195862298,-9.76734670980891,
12.));
#198343=CARTESIAN_POINT('Ctrl Pts',(-20.44034423294,-9.76322747195494,0.));
#198344=CARTESIAN_POINT('Ctrl Pts',(-20.44034423294,-9.76322747195494,12.));
#198345=CARTESIAN_POINT('Ctrl Pts',(-20.4336957355473,-9.75926386289922,
0.));
#198346=CARTESIAN_POINT('Ctrl Pts',(-20.4336957355473,-9.75926386289922,
12.));
#198347=CARTESIAN_POINT('Ctrl Pts',(-20.4272556476629,-9.75545705902417,
0.));
#198348=CARTESIAN_POINT('Ctrl Pts',(-20.4272556476629,-9.75545705902417,
12.));
#198349=CARTESIAN_POINT('Ctrl Pts',(-20.4210295275817,-9.7518082978643,
0.));
#198350=CARTESIAN_POINT('Ctrl Pts',(-20.4210295275817,-9.7518082978643,
12.));
#198351=CARTESIAN_POINT('Ctrl Pts',(-20.4150232777393,-9.74831889242174,
0.));
#198352=CARTESIAN_POINT('Ctrl Pts',(-20.4150232777393,-9.74831889242174,
12.));
#198353=CARTESIAN_POINT('Ctrl Pts',(-20.4092430879861,-9.74499021838537,
0.));
#198354=CARTESIAN_POINT('Ctrl Pts',(-20.4092430879861,-9.74499021838537,
12.));
#198355=CARTESIAN_POINT('Ctrl Pts',(-20.4036953576549,-9.74182369656271,
0.));
#198356=CARTESIAN_POINT('Ctrl Pts',(-20.4036953576549,-9.74182369656271,
12.));
#198357=CARTESIAN_POINT('Ctrl Pts',(-20.3983866213331,-9.738820776132,0.));
#198358=CARTESIAN_POINT('Ctrl Pts',(-20.3983866213331,-9.738820776132,12.));
#198359=CARTESIAN_POINT('Ctrl Pts',(-20.3933234845647,-9.73598292014242,
0.));
#198360=CARTESIAN_POINT('Ctrl Pts',(-20.3933234845647,-9.73598292014242,
12.));
#198361=CARTESIAN_POINT('Ctrl Pts',(-20.3885129129912,-9.73331167102807,
0.));
#198362=CARTESIAN_POINT('Ctrl Pts',(-20.3885129129912,-9.73331167102807,
12.));
#198363=CARTESIAN_POINT('Ctrl Pts',(-20.3839624556742,-9.73080870123727,
0.));
#198364=CARTESIAN_POINT('Ctrl Pts',(-20.3839624556742,-9.73080870123727,
12.));
#198365=CARTESIAN_POINT('Ctrl Pts',(-20.3796805893304,-9.72847589116541,
0.));
#198366=CARTESIAN_POINT('Ctrl Pts',(-20.3796805893304,-9.72847589116541,
12.));
#198367=CARTESIAN_POINT('Ctrl Pts',(-20.3756766651951,-9.7263153173288,
0.));
#198368=CARTESIAN_POINT('Ctrl Pts',(-20.3756766651951,-9.7263153173288,
12.));
#198369=CARTESIAN_POINT('Ctrl Pts',(-20.371960235676,-9.72432910043194,
0.));
#198370=CARTESIAN_POINT('Ctrl Pts',(-20.371960235676,-9.72432910043194,
12.));
#198371=CARTESIAN_POINT('Ctrl Pts',(-20.3685406190576,-9.72251930722489,
0.));
#198372=CARTESIAN_POINT('Ctrl Pts',(-20.3685406190576,-9.72251930722489,
12.));
#198373=CARTESIAN_POINT('Ctrl Pts',(-20.3654261611056,-9.7208877838108,
0.));
#198374=CARTESIAN_POINT('Ctrl Pts',(-20.3654261611056,-9.7208877838108,
12.));
#198375=CARTESIAN_POINT('Ctrl Pts',(-20.3626256913981,-9.71943648548099,
0.));
#198376=CARTESIAN_POINT('Ctrl Pts',(-20.3626256913981,-9.71943648548099,
12.));
#198377=CARTESIAN_POINT('Ctrl Pts',(-20.3601498764344,-9.71816778328006,
0.));
#198378=CARTESIAN_POINT('Ctrl Pts',(-20.3601498764344,-9.71816778328006,
12.));
#198379=CARTESIAN_POINT('Ctrl Pts',(-20.3580133103356,-9.71708493723096,
0.));
#198380=CARTESIAN_POINT('Ctrl Pts',(-20.3580133103356,-9.71708493723096,
12.));
#198381=CARTESIAN_POINT('Ctrl Pts',(-20.3562337557875,-9.71619192554185,
0.));
#198382=CARTESIAN_POINT('Ctrl Pts',(-20.3562337557875,-9.71619192554185,
12.));
#198383=CARTESIAN_POINT('Ctrl Pts',(-20.3548282742361,-9.71549257088172,
0.));
#198384=CARTESIAN_POINT('Ctrl Pts',(-20.3548282742361,-9.71549257088172,
12.));
#198385=CARTESIAN_POINT('Ctrl Pts',(-20.3538098605706,-9.7149897805202,
0.));
#198386=CARTESIAN_POINT('Ctrl Pts',(-20.3538098605706,-9.7149897805202,
12.));
#198387=CARTESIAN_POINT('Ctrl Pts',(-20.3533097561886,-9.7147459035068,
0.));
#198388=CARTESIAN_POINT('Ctrl Pts',(-20.3533097561886,-9.7147459035068,
12.));
#198389=CARTESIAN_POINT('Ctrl Pts',(-20.3531126095522,-9.71465227853041,
0.));
#198390=CARTESIAN_POINT('Ctrl Pts',(-20.3531126095522,-9.71465227853041,
12.));
#198391=CARTESIAN_POINT('Ctrl Pts',(-20.353060251684,-9.71462954053041,
0.));
#198392=CARTESIAN_POINT('Ctrl Pts',(-20.353060251684,-9.71462954053041,
12.));
#198393=CARTESIAN_POINT('Ctrl Pts',(-20.353053841303,-9.71462809124915,
0.));
#198394=CARTESIAN_POINT('Ctrl Pts',(-20.353053841303,-9.71462809124915,
12.));
#198395=CARTESIAN_POINT('',(-22.8400320311649,-12.4230808101438,0.));
#198396=CARTESIAN_POINT('Ctrl Pts',(-22.8400320311649,-12.4230808101438,
0.));
#198397=CARTESIAN_POINT('Ctrl Pts',(-22.8370364396459,-12.418215285186,
0.));
#198398=CARTESIAN_POINT('Ctrl Pts',(-22.8310435872748,-12.4084933766346,
0.));
#198399=CARTESIAN_POINT('Ctrl Pts',(-22.8220493007173,-12.3939379378998,
0.));
#198400=CARTESIAN_POINT('Ctrl Pts',(-22.81004690224,-12.374585536673,0.));
#198401=CARTESIAN_POINT('Ctrl Pts',(-22.795027221673,-12.3504864740319,
0.));
#198402=CARTESIAN_POINT('Ctrl Pts',(-22.7799908974768,-12.3264788926075,
0.));
#198403=CARTESIAN_POINT('Ctrl Pts',(-22.764938010105,-12.3025628601792,
0.));
#198404=CARTESIAN_POINT('Ctrl Pts',(-22.7498686970069,-12.2787384750742,
0.));
#198405=CARTESIAN_POINT('Ctrl Pts',(-22.7347831655287,-12.2550058702395,
0.));
#198406=CARTESIAN_POINT('Ctrl Pts',(-22.7196817119374,-12.2313652198061,
0.));
#198407=CARTESIAN_POINT('Ctrl Pts',(-22.7045647168747,-12.2078167360284,
0.));
#198408=CARTESIAN_POINT('Ctrl Pts',(-22.6894326205037,-12.1843606579261,
0.));
#198409=CARTESIAN_POINT('Ctrl Pts',(-22.6742859034944,-12.1609972423099,
0.));
#198410=CARTESIAN_POINT('Ctrl Pts',(-22.6591250653965,-12.1377267537145,
0.));
#198411=CARTESIAN_POINT('Ctrl Pts',(-22.6439506046605,-12.1145494550383,
0.));
#198412=CARTESIAN_POINT('Ctrl Pts',(-22.6287629967056,-12.0914655972823,
0.));
#198413=CARTESIAN_POINT('Ctrl Pts',(-22.6135626764898,-12.0684754113862,
0.));
#198414=CARTESIAN_POINT('Ctrl Pts',(-22.5983500505644,-12.0455791139128,
0.));
#198415=CARTESIAN_POINT('Ctrl Pts',(-22.5831255061282,-12.0227769113127,
0.));
#198416=CARTESIAN_POINT('Ctrl Pts',(-22.5678894211181,-12.0000690046695,
0.));
#198417=CARTESIAN_POINT('Ctrl Pts',(-22.5526421741158,-11.9774555943496,
0.));
#198418=CARTESIAN_POINT('Ctrl Pts',(-22.5373841537307,-11.9549368843997,
0.));
#198419=CARTESIAN_POINT('Ctrl Pts',(-22.5221157697883,-11.9325130877803,
0.));
#198420=CARTESIAN_POINT('Ctrl Pts',(-22.5068374513973,-11.9101844254557,
0.));
#198421=CARTESIAN_POINT('Ctrl Pts',(-22.4915496418485,-11.8879511239942,
0.));
#198422=CARTESIAN_POINT('Ctrl Pts',(-22.4762527946702,-11.8658134137019,
0.));
#198423=CARTESIAN_POINT('Ctrl Pts',(-22.4609473690471,-11.8437715264487,
0.));
#198424=CARTESIAN_POINT('Ctrl Pts',(-22.4456338258735,-11.8218256937889,
0.));
#198425=CARTESIAN_POINT('Ctrl Pts',(-22.430312622646,-11.7999761445173,
0.));
#198426=CARTESIAN_POINT('Ctrl Pts',(-22.4149842125008,-11.7782231042039,
0.));
#198427=CARTESIAN_POINT('Ctrl Pts',(-22.3996490469191,-11.7565667964764,
0.));
#198428=CARTESIAN_POINT('Ctrl Pts',(-22.3843075773899,-11.7350074437961,
0.));
#198429=CARTESIAN_POINT('Ctrl Pts',(-22.3689602575491,-11.7135452684532,
0.));
#198430=CARTESIAN_POINT('Ctrl Pts',(-22.3536075450029,-11.6921804934056,
0.));
#198431=CARTESIAN_POINT('Ctrl Pts',(-22.3382499035619,-11.6709133432985,
0.));
#198432=CARTESIAN_POINT('Ctrl Pts',(-22.3228878043976,-11.6497440449857,
0.));
#198433=CARTESIAN_POINT('Ctrl Pts',(-22.3075217249049,-11.6286728270009,
0.));
#198434=CARTESIAN_POINT('Ctrl Pts',(-22.2921521480356,-11.6076999192357,
0.));
#198435=CARTESIAN_POINT('Ctrl Pts',(-22.2767795614348,-11.5868255525188,
0.));
#198436=CARTESIAN_POINT('Ctrl Pts',(-22.2614044566898,-11.5660499582403,
0.));
#198437=CARTESIAN_POINT('Ctrl Pts',(-22.2460273284654,-11.5453733679121,
0.));
#198438=CARTESIAN_POINT('Ctrl Pts',(-22.2306486738901,-11.5247960128477,
0.));
#198439=CARTESIAN_POINT('Ctrl Pts',(-22.2152689931022,-11.5043181244242,
0.));
#198440=CARTESIAN_POINT('Ctrl Pts',(-22.1998887896436,-11.483939934259,
0.));
#198441=CARTESIAN_POINT('Ctrl Pts',(-22.184508570917,-11.463661674411,0.));
#198442=CARTESIAN_POINT('Ctrl Pts',(-22.1691288486096,-11.443483577557,
0.));
#198443=CARTESIAN_POINT('Ctrl Pts',(-22.1537501391487,-11.4234058771742,
0.));
#198444=CARTESIAN_POINT('Ctrl Pts',(-22.1383729640964,-11.4034288076908,
0.));
#198445=CARTESIAN_POINT('Ctrl Pts',(-22.1229978500186,-11.3835526044256,
0.));
#198446=CARTESIAN_POINT('Ctrl Pts',(-22.1076253283979,-11.3637775035367,
0.));
#198447=CARTESIAN_POINT('Ctrl Pts',(-22.0922559355294,-11.3441037419553,
0.));
#198448=CARTESIAN_POINT('Ctrl Pts',(-22.0768902124267,-11.3245315573168,
0.));
#198449=CARTESIAN_POINT('Ctrl Pts',(-22.0615287047179,-11.3050611878771,
0.));
#198450=CARTESIAN_POINT('Ctrl Pts',(-22.046171962566,-11.2856928724374,
0.));
#198451=CARTESIAN_POINT('Ctrl Pts',(-22.030820540835,-11.2664268504206,
0.));
#198452=CARTESIAN_POINT('Ctrl Pts',(-22.0154749992363,-11.2472633619275,
0.));
#198453=CARTESIAN_POINT('Ctrl Pts',(-22.0001359024839,-11.2282026477896,
0.));
#198454=CARTESIAN_POINT('Ctrl Pts',(-21.9848038204439,-11.2092449496125,
0.));
#198455=CARTESIAN_POINT('Ctrl Pts',(-21.9694793282914,-11.190390509811,
0.));
#198456=CARTESIAN_POINT('Ctrl Pts',(-21.9541630066506,-11.1716395716376,
0.));
#198457=CARTESIAN_POINT('Ctrl Pts',(-21.9388554416439,-11.1529923792003,
0.));
#198458=CARTESIAN_POINT('Ctrl Pts',(-21.923557224952,-11.1344491774741,
0.));
#198459=CARTESIAN_POINT('Ctrl Pts',(-21.9082689538688,-11.1160102123024,
0.));
#198460=CARTESIAN_POINT('Ctrl Pts',(-21.8929912313608,-11.0976757303944,
0.));
#198461=CARTESIAN_POINT('Ctrl Pts',(-21.877724666119,-11.0794459793057,
0.));
#198462=CARTESIAN_POINT('Ctrl Pts',(-21.8624698726318,-11.0613212074363,
0.));
#198463=CARTESIAN_POINT('Ctrl Pts',(-21.8472274713103,-11.0433016640807,
0.));
#198464=CARTESIAN_POINT('Ctrl Pts',(-21.8319980886033,-11.0253875994598,
0.));
#198465=CARTESIAN_POINT('Ctrl Pts',(-21.8167823571168,-11.0075792647477,
0.));
#198466=CARTESIAN_POINT('Ctrl Pts',(-21.8015809157301,-10.9898769120912,
0.));
#198467=CARTESIAN_POINT('Ctrl Pts',(-21.7863944097141,-10.9722807946155,
0.));
#198468=CARTESIAN_POINT('Ctrl Pts',(-21.7712234908464,-10.9547911664455,
0.));
#198469=CARTESIAN_POINT('Ctrl Pts',(-21.7560688175247,-10.9374082827444,
0.));
#198470=CARTESIAN_POINT('Ctrl Pts',(-21.7409310548797,-10.9201323997384,
0.));
#198471=CARTESIAN_POINT('Ctrl Pts',(-21.7258108748873,-10.902963774734,
0.));
#198472=CARTESIAN_POINT('Ctrl Pts',(-21.7107089564825,-10.8859026661293,
0.));
#198473=CARTESIAN_POINT('Ctrl Pts',(-21.6956259856672,-10.8689493334095,
0.));
#198474=CARTESIAN_POINT('Ctrl Pts',(-21.6805626556467,-10.8521040371835,
0.));
#198475=CARTESIAN_POINT('Ctrl Pts',(-21.6655196669732,-10.8353670392272,
0.));
#198476=CARTESIAN_POINT('Ctrl Pts',(-21.6504977276866,-10.8187386025136,
0.));
#198477=CARTESIAN_POINT('Ctrl Pts',(-21.6354975534557,-10.8022189912369,
0.));
#198478=CARTESIAN_POINT('Ctrl Pts',(-21.6205198677173,-10.7858084708261,
0.));
#198479=CARTESIAN_POINT('Ctrl Pts',(-21.6055654018176,-10.7695073079552,
0.));
#198480=CARTESIAN_POINT('Ctrl Pts',(-21.5906348951743,-10.7533157705941,
0.));
#198481=CARTESIAN_POINT('Ctrl Pts',(-21.5757290954371,-10.7372341280467,
0.));
#198482=CARTESIAN_POINT('Ctrl Pts',(-21.5608487586468,-10.7212626509816,
0.));
#198483=CARTESIAN_POINT('Ctrl Pts',(-21.5459946493955,-10.7054016114571,
0.));
#198484=CARTESIAN_POINT('Ctrl Pts',(-21.5311675409807,-10.689651282929,
0.));
#198485=CARTESIAN_POINT('Ctrl Pts',(-21.51636821558,-10.6740119402834,0.));
#198486=CARTESIAN_POINT('Ctrl Pts',(-21.5015974644449,-10.6584838598939,
0.));
#198487=CARTESIAN_POINT('Ctrl Pts',(-21.4868560880889,-10.6430673196607,
0.));
#198488=CARTESIAN_POINT('Ctrl Pts',(-21.4721448964766,-10.6277625990456,
0.));
#198489=CARTESIAN_POINT('Ctrl Pts',(-21.4574647092097,-10.6125699790961,
0.));
#198490=CARTESIAN_POINT('Ctrl Pts',(-21.4428163557144,-10.5974897424622,
0.));
#198491=CARTESIAN_POINT('Ctrl Pts',(-21.4282006754631,-10.5825221734573,
0.));
#198492=CARTESIAN_POINT('Ctrl Pts',(-21.4136185181979,-10.5676675581108,
0.));
#198493=CARTESIAN_POINT('Ctrl Pts',(-21.3990707441497,-10.5529261842108,
0.));
#198494=CARTESIAN_POINT('Ctrl Pts',(-21.3845582242602,-10.5382983413421,
0.));
#198495=CARTESIAN_POINT('Ctrl Pts',(-21.3700818403936,-10.5237843209057,
0.));
#198496=CARTESIAN_POINT('Ctrl Pts',(-21.3556424855814,-10.5093844161685,
0.));
#198497=CARTESIAN_POINT('Ctrl Pts',(-21.3412410642904,-10.4950989223337,
0.));
#198498=CARTESIAN_POINT('Ctrl Pts',(-21.3268784926819,-10.4809281365931,
0.));
#198499=CARTESIAN_POINT('Ctrl Pts',(-21.3125556988731,-10.4668723581768,
0.));
#198500=CARTESIAN_POINT('Ctrl Pts',(-21.2982736231931,-10.4529318883874,
0.));
#198501=CARTESIAN_POINT('Ctrl Pts',(-21.2840332184483,-10.4391070306391,
0.));
#198502=CARTESIAN_POINT('Ctrl Pts',(-21.2698354502403,-10.42539809054,0.));
#198503=CARTESIAN_POINT('Ctrl Pts',(-21.255681297275,-10.4118053759588,
0.));
#198504=CARTESIAN_POINT('Ctrl Pts',(-21.2415717516714,-10.3983291970846,
0.));
#198505=CARTESIAN_POINT('Ctrl Pts',(-21.22750781927,-10.3849698664786,0.));
#198506=CARTESIAN_POINT('Ctrl Pts',(-21.2134905199345,-10.371727699113,
0.));
#198507=CARTESIAN_POINT('Ctrl Pts',(-21.199520887919,-10.3586030124587,
0.));
#198508=CARTESIAN_POINT('Ctrl Pts',(-21.1855999722416,-10.34559612657,0.));
#198509=CARTESIAN_POINT('Ctrl Pts',(-21.1717288370509,-10.3327073641572,
0.));
#198510=CARTESIAN_POINT('Ctrl Pts',(-21.1579085619965,-10.3199370506544,
0.));
#198511=CARTESIAN_POINT('Ctrl Pts',(-21.1441402425843,-10.3072855142687,
0.));
#198512=CARTESIAN_POINT('Ctrl Pts',(-21.1304249906002,-10.2947530860721,
0.));
#198513=CARTESIAN_POINT('Ctrl Pts',(-21.1167639345631,-10.2823401001072,
0.));
#198514=CARTESIAN_POINT('Ctrl Pts',(-21.1031582201627,-10.2700468934744,
0.));
#198515=CARTESIAN_POINT('Ctrl Pts',(-21.0896090107063,-10.2578738064181,
0.));
#198516=CARTESIAN_POINT('Ctrl Pts',(-21.0761174875445,-10.2458211823912,
0.));
#198517=CARTESIAN_POINT('Ctrl Pts',(-21.0626848505663,-10.2338893681567,
0.));
#198518=CARTESIAN_POINT('Ctrl Pts',(-21.0493123187483,-10.2220787139154,
0.));
#198519=CARTESIAN_POINT('Ctrl Pts',(-21.0360011306815,-10.2103895734123,
0.));
#198520=CARTESIAN_POINT('Ctrl Pts',(-21.0227525451107,-10.1988223040425,
0.));
#198521=CARTESIAN_POINT('Ctrl Pts',(-21.0095678414486,-10.187377266936,
0.));
#198522=CARTESIAN_POINT('Ctrl Pts',(-20.9964483203686,-10.1760548270767,
0.));
#198523=CARTESIAN_POINT('Ctrl Pts',(-20.9833953044736,-10.1648553534568,
0.));
#198524=CARTESIAN_POINT('Ctrl Pts',(-20.9704101389369,-10.1537792192065,
0.));
#198525=CARTESIAN_POINT('Ctrl Pts',(-20.9574941921591,-10.1428268017256,
0.));
#198526=CARTESIAN_POINT('Ctrl Pts',(-20.9446488563933,-10.1319984827908,
0.));
#198527=CARTESIAN_POINT('Ctrl Pts',(-20.9318755484734,-10.1212946487057,
0.));
#198528=CARTESIAN_POINT('Ctrl Pts',(-20.919175710627,-10.1107156904836,
0.));
#198529=CARTESIAN_POINT('Ctrl Pts',(-20.9065508112557,-10.1002620040076,
0.));
#198530=CARTESIAN_POINT('Ctrl Pts',(-20.894002345737,-10.0899339901915,
0.));
#198531=CARTESIAN_POINT('Ctrl Pts',(-20.881531837184,-10.0797320551154,
0.));
#198532=CARTESIAN_POINT('Ctrl Pts',(-20.86914083737,-10.0696566102218,0.));
#198533=CARTESIAN_POINT('Ctrl Pts',(-20.8568309277316,-10.0597080725375,
0.));
#198534=CARTESIAN_POINT('Ctrl Pts',(-20.8446037203402,-10.0498868648733,
0.));
#198535=CARTESIAN_POINT('Ctrl Pts',(-20.8324608588909,-10.0401934160234,
0.));
#198536=CARTESIAN_POINT('Ctrl Pts',(-20.8204040196602,-10.0306281609435,
0.));
#198537=CARTESIAN_POINT('Ctrl Pts',(-20.8084349126888,-10.0211915410095,
0.));
#198538=CARTESIAN_POINT('Ctrl Pts',(-20.7965552829908,-10.0118840042786,
0.));
#198539=CARTESIAN_POINT('Ctrl Pts',(-20.7847669117568,-10.0027060057389,
0.));
#198540=CARTESIAN_POINT('Ctrl Pts',(-20.7730716175417,-9.9936580075464,
0.));
#198541=CARTESIAN_POINT('Ctrl Pts',(-20.761471257499,-9.98474047926852,
0.));
#198542=CARTESIAN_POINT('Ctrl Pts',(-20.7499677289627,-9.9759538982347,
0.));
#198543=CARTESIAN_POINT('Ctrl Pts',(-20.7385629709795,-9.96729874986201,
0.));
#198544=CARTESIAN_POINT('Ctrl Pts',(-20.7272589658751,-9.95877552798397,
0.));
#198545=CARTESIAN_POINT('Ctrl Pts',(-20.7160577407579,-9.95038473514948,
0.));
#198546=CARTESIAN_POINT('Ctrl Pts',(-20.7049613692234,-9.94212688298236,
0.));
#198547=CARTESIAN_POINT('Ctrl Pts',(-20.6939719732484,-9.93400249259729,
0.));
#198548=CARTESIAN_POINT('Ctrl Pts',(-20.6830917250255,-9.92601209498748,
0.));
#198549=CARTESIAN_POINT('Ctrl Pts',(-20.6723228488263,-9.91815623141288,
0.));
#198550=CARTESIAN_POINT('Ctrl Pts',(-20.6616676228315,-9.91043545377007,
0.));
#198551=CARTESIAN_POINT('Ctrl Pts',(-20.6511283817414,-9.90285032516692,
0.));
#198552=CARTESIAN_POINT('Ctrl Pts',(-20.6407075193976,-9.89540142049119,
0.));
#198553=CARTESIAN_POINT('Ctrl Pts',(-20.6304074914087,-9.88808932697306,
0.));
#198554=CARTESIAN_POINT('Ctrl Pts',(-20.6202308177474,-9.88091464472675,
0.));
#198555=CARTESIAN_POINT('Ctrl Pts',(-20.6101800854494,-9.87387798732956,
0.));
#198556=CARTESIAN_POINT('Ctrl Pts',(-20.6002579513699,-9.86697998242622,
0.));
#198557=CARTESIAN_POINT('Ctrl Pts',(-20.5904671449754,-9.86022127232747,
0.));
#198558=CARTESIAN_POINT('Ctrl Pts',(-20.5808104710015,-9.8536025145698,
0.));
#198559=CARTESIAN_POINT('Ctrl Pts',(-20.5712908125139,-9.84712438256277,
0.));
#198560=CARTESIAN_POINT('Ctrl Pts',(-20.5619111362402,-9.84078756677565,
0.));
#198561=CARTESIAN_POINT('Ctrl Pts',(-20.552674497646,-9.83459277585315,
0.));
#198562=CARTESIAN_POINT('Ctrl Pts',(-20.5435840460721,-9.82854073773877,
0.));
#198563=CARTESIAN_POINT('Ctrl Pts',(-20.5346430299517,-9.82263220080362,
0.));
#198564=CARTESIAN_POINT('Ctrl Pts',(-20.5258548000629,-9.81686793455942,
0.));
#198565=CARTESIAN_POINT('Ctrl Pts',(-20.517222812284,-9.81124873025281,
0.));
#198566=CARTESIAN_POINT('Ctrl Pts',(-20.5087506310505,-9.80577540161087,
0.));
#198567=CARTESIAN_POINT('Ctrl Pts',(-20.5004419312107,-9.80044878520948,
0.));
#198568=CARTESIAN_POINT('Ctrl Pts',(-20.4923005087943,-9.7952697428833,
0.));
#198569=CARTESIAN_POINT('Ctrl Pts',(-20.4843302955329,-9.79023916498655,
0.));
#198570=CARTESIAN_POINT('Ctrl Pts',(-20.4765353711586,-9.78535797314166,
0.));
#198571=CARTESIAN_POINT('Ctrl Pts',(-20.4689199790669,-9.7806271237332,
0.));
#198572=CARTESIAN_POINT('Ctrl Pts',(-20.4614885274975,-9.77604760815528,
0.));
#198573=CARTESIAN_POINT('Ctrl Pts',(-20.4542455817527,-9.77162045104069,
0.));
#198574=CARTESIAN_POINT('Ctrl Pts',(-20.447195862298,-9.76734670980891,
0.));
#198575=CARTESIAN_POINT('Ctrl Pts',(-20.44034423294,-9.76322747195494,0.));
#198576=CARTESIAN_POINT('Ctrl Pts',(-20.4336957355473,-9.75926386289922,
0.));
#198577=CARTESIAN_POINT('Ctrl Pts',(-20.4272556476629,-9.75545705902417,
0.));
#198578=CARTESIAN_POINT('Ctrl Pts',(-20.4210295275817,-9.7518082978643,
0.));
#198579=CARTESIAN_POINT('Ctrl Pts',(-20.4150232777393,-9.74831889242174,
0.));
#198580=CARTESIAN_POINT('Ctrl Pts',(-20.4092430879861,-9.74499021838537,
0.));
#198581=CARTESIAN_POINT('Ctrl Pts',(-20.4036953576549,-9.74182369656271,
0.));
#198582=CARTESIAN_POINT('Ctrl Pts',(-20.3983866213331,-9.738820776132,0.));
#198583=CARTESIAN_POINT('Ctrl Pts',(-20.3933234845647,-9.73598292014242,
0.));
#198584=CARTESIAN_POINT('Ctrl Pts',(-20.3885129129912,-9.73331167102807,
0.));
#198585=CARTESIAN_POINT('Ctrl Pts',(-20.3839624556742,-9.73080870123727,
0.));
#198586=CARTESIAN_POINT('Ctrl Pts',(-20.3796805893304,-9.72847589116541,
0.));
#198587=CARTESIAN_POINT('Ctrl Pts',(-20.3756766651951,-9.7263153173288,
0.));
#198588=CARTESIAN_POINT('Ctrl Pts',(-20.371960235676,-9.72432910043194,
0.));
#198589=CARTESIAN_POINT('Ctrl Pts',(-20.3685406190576,-9.72251930722489,
0.));
#198590=CARTESIAN_POINT('Ctrl Pts',(-20.3654261611056,-9.7208877838108,
0.));
#198591=CARTESIAN_POINT('Ctrl Pts',(-20.3626256913981,-9.71943648548099,
0.));
#198592=CARTESIAN_POINT('Ctrl Pts',(-20.3601498764344,-9.71816778328006,
0.));
#198593=CARTESIAN_POINT('Ctrl Pts',(-20.3580133103356,-9.71708493723096,
0.));
#198594=CARTESIAN_POINT('Ctrl Pts',(-20.3562337557875,-9.71619192554185,
0.));
#198595=CARTESIAN_POINT('Ctrl Pts',(-20.3548282742361,-9.71549257088172,
0.));
#198596=CARTESIAN_POINT('Ctrl Pts',(-20.3538098605706,-9.7149897805202,
0.));
#198597=CARTESIAN_POINT('Ctrl Pts',(-20.3533097561886,-9.7147459035068,
0.));
#198598=CARTESIAN_POINT('Ctrl Pts',(-20.3531126095522,-9.71465227853041,
0.));
#198599=CARTESIAN_POINT('Ctrl Pts',(-20.353060251684,-9.71462954053041,
0.));
#198600=CARTESIAN_POINT('Ctrl Pts',(-20.353053841303,-9.71462809124915,
0.));
#198601=CARTESIAN_POINT('',(-22.8400320311649,-12.4230808101438,0.));
#198602=CARTESIAN_POINT('Ctrl Pts',(-21.2610617890679,-7.52250298901264,
0.));
#198603=CARTESIAN_POINT('Ctrl Pts',(-21.2610617890679,-7.52250298901264,
12.));
#198604=CARTESIAN_POINT('Ctrl Pts',(-21.2610673466886,-7.5225064970397,
0.));
#198605=CARTESIAN_POINT('Ctrl Pts',(-21.2610673466886,-7.5225064970397,
12.));
#198606=CARTESIAN_POINT('Ctrl Pts',(-21.2611204474866,-7.52252744144903,
0.));
#198607=CARTESIAN_POINT('Ctrl Pts',(-21.2611204474866,-7.52252744144903,
12.));
#198608=CARTESIAN_POINT('Ctrl Pts',(-21.261326054066,-7.5226006423166,0.));
#198609=CARTESIAN_POINT('Ctrl Pts',(-21.261326054066,-7.5226006423166,12.));
#198610=CARTESIAN_POINT('Ctrl Pts',(-21.2618521283555,-7.52278182242669,
0.));
#198611=CARTESIAN_POINT('Ctrl Pts',(-21.2618521283555,-7.52278182242669,
12.));
#198612=CARTESIAN_POINT('Ctrl Pts',(-21.262927782038,-7.52314642316199,
0.));
#198613=CARTESIAN_POINT('Ctrl Pts',(-21.262927782038,-7.52314642316199,
12.));
#198614=CARTESIAN_POINT('Ctrl Pts',(-21.2644161259962,-7.52364573027552,
0.));
#198615=CARTESIAN_POINT('Ctrl Pts',(-21.2644161259962,-7.52364573027552,
12.));
#198616=CARTESIAN_POINT('Ctrl Pts',(-21.2663059157058,-7.52427261074297,
0.));
#198617=CARTESIAN_POINT('Ctrl Pts',(-21.2663059157058,-7.52427261074297,
12.));
#198618=CARTESIAN_POINT('Ctrl Pts',(-21.2685823838671,-7.5250177033353,
0.));
#198619=CARTESIAN_POINT('Ctrl Pts',(-21.2685823838671,-7.5250177033353,
12.));
#198620=CARTESIAN_POINT('Ctrl Pts',(-21.2712301573466,-7.52587126095529,
0.));
#198621=CARTESIAN_POINT('Ctrl Pts',(-21.2712301573466,-7.52587126095529,
12.));
#198622=CARTESIAN_POINT('Ctrl Pts',(-21.2742366113579,-7.5268252691854,
0.));
#198623=CARTESIAN_POINT('Ctrl Pts',(-21.2742366113579,-7.5268252691854,
12.));
#198624=CARTESIAN_POINT('Ctrl Pts',(-21.2775925269652,-7.52787386225332,
0.));
#198625=CARTESIAN_POINT('Ctrl Pts',(-21.2775925269652,-7.52787386225332,
12.));
#198626=CARTESIAN_POINT('Ctrl Pts',(-21.2812902781143,-7.52901217930407,
0.));
#198627=CARTESIAN_POINT('Ctrl Pts',(-21.2812902781143,-7.52901217930407,
12.));
#198628=CARTESIAN_POINT('Ctrl Pts',(-21.2853226580657,-7.53023562438229,
0.));
#198629=CARTESIAN_POINT('Ctrl Pts',(-21.2853226580657,-7.53023562438229,
12.));
#198630=CARTESIAN_POINT('Ctrl Pts',(-21.2896816163842,-7.53153906987855,
0.));
#198631=CARTESIAN_POINT('Ctrl Pts',(-21.2896816163842,-7.53153906987855,
12.));
#198632=CARTESIAN_POINT('Ctrl Pts',(-21.2943588989331,-7.53291726078526,
0.));
#198633=CARTESIAN_POINT('Ctrl Pts',(-21.2943588989331,-7.53291726078526,
12.));
#198634=CARTESIAN_POINT('Ctrl Pts',(-21.2993464250717,-7.53436505309942,
0.));
#198635=CARTESIAN_POINT('Ctrl Pts',(-21.2993464250717,-7.53436505309942,
12.));
#198636=CARTESIAN_POINT('Ctrl Pts',(-21.3046368712157,-7.53587778251735,
0.));
#198637=CARTESIAN_POINT('Ctrl Pts',(-21.3046368712157,-7.53587778251735,
12.));
#198638=CARTESIAN_POINT('Ctrl Pts',(-21.310223716773,-7.53745129364616,
0.));
#198639=CARTESIAN_POINT('Ctrl Pts',(-21.310223716773,-7.53745129364616,
12.));
#198640=CARTESIAN_POINT('Ctrl Pts',(-21.3161009456256,-7.53908175169898,
0.));
#198641=CARTESIAN_POINT('Ctrl Pts',(-21.3161009456256,-7.53908175169898,
12.));
#198642=CARTESIAN_POINT('Ctrl Pts',(-21.3222628524165,-7.54076552038278,
0.));
#198643=CARTESIAN_POINT('Ctrl Pts',(-21.3222628524165,-7.54076552038278,
12.));
#198644=CARTESIAN_POINT('Ctrl Pts',(-21.328703791771,-7.5424990037703,0.));
#198645=CARTESIAN_POINT('Ctrl Pts',(-21.328703791771,-7.5424990037703,12.));
#198646=CARTESIAN_POINT('Ctrl Pts',(-21.3354182340149,-7.54427868151267,
0.));
#198647=CARTESIAN_POINT('Ctrl Pts',(-21.3354182340149,-7.54427868151267,
12.));
#198648=CARTESIAN_POINT('Ctrl Pts',(-21.3424008295038,-7.54610114948346,
0.));
#198649=CARTESIAN_POINT('Ctrl Pts',(-21.3424008295038,-7.54610114948346,
12.));
#198650=CARTESIAN_POINT('Ctrl Pts',(-21.3496464761531,-7.5479631624633,
0.));
#198651=CARTESIAN_POINT('Ctrl Pts',(-21.3496464761531,-7.5479631624633,
12.));
#198652=CARTESIAN_POINT('Ctrl Pts',(-21.3571503685855,-7.54986166521309,
0.));
#198653=CARTESIAN_POINT('Ctrl Pts',(-21.3571503685855,-7.54986166521309,
12.));
#198654=CARTESIAN_POINT('Ctrl Pts',(-21.3649079431865,-7.55179375777443,
0.));
#198655=CARTESIAN_POINT('Ctrl Pts',(-21.3649079431865,-7.55179375777443,
12.));
#198656=CARTESIAN_POINT('Ctrl Pts',(-21.3729148390243,-7.55375667080028,
0.));
#198657=CARTESIAN_POINT('Ctrl Pts',(-21.3729148390243,-7.55375667080028,
12.));
#198658=CARTESIAN_POINT('Ctrl Pts',(-21.3811668478932,-7.55574773403502,
0.));
#198659=CARTESIAN_POINT('Ctrl Pts',(-21.3811668478932,-7.55574773403502,
12.));
#198660=CARTESIAN_POINT('Ctrl Pts',(-21.3896598842117,-7.55776435731416,
0.));
#198661=CARTESIAN_POINT('Ctrl Pts',(-21.3896598842117,-7.55776435731416,
12.));
#198662=CARTESIAN_POINT('Ctrl Pts',(-21.3983899952987,-7.5598040370061,
0.));
#198663=CARTESIAN_POINT('Ctrl Pts',(-21.3983899952987,-7.5598040370061,
12.));
#198664=CARTESIAN_POINT('Ctrl Pts',(-21.4073533630365,-7.56186435703621,
0.));
#198665=CARTESIAN_POINT('Ctrl Pts',(-21.4073533630365,-7.56186435703621,
12.));
#198666=CARTESIAN_POINT('Ctrl Pts',(-21.4165463106254,-7.56394299313684,
0.));
#198667=CARTESIAN_POINT('Ctrl Pts',(-21.4165463106254,-7.56394299313684,
12.));
#198668=CARTESIAN_POINT('Ctrl Pts',(-21.4259653015736,-7.56603771218712,
0.));
#198669=CARTESIAN_POINT('Ctrl Pts',(-21.4259653015736,-7.56603771218712,
12.));
#198670=CARTESIAN_POINT('Ctrl Pts',(-21.4356069261513,-7.56814636360847,
0.));
#198671=CARTESIAN_POINT('Ctrl Pts',(-21.4356069261513,-7.56814636360847,
12.));
#198672=CARTESIAN_POINT('Ctrl Pts',(-21.4454678907509,-7.57026687261165,
0.));
#198673=CARTESIAN_POINT('Ctrl Pts',(-21.4454678907509,-7.57026687261165,
12.));
#198674=CARTESIAN_POINT('Ctrl Pts',(-21.4555450053142,-7.57239723223505,
0.));
#198675=CARTESIAN_POINT('Ctrl Pts',(-21.4555450053142,-7.57239723223505,
12.));
#198676=CARTESIAN_POINT('Ctrl Pts',(-21.4658351740128,-7.57453549743411,
0.));
#198677=CARTESIAN_POINT('Ctrl Pts',(-21.4658351740128,-7.57453549743411,
12.));
#198678=CARTESIAN_POINT('Ctrl Pts',(-21.4763353936762,-7.57667978402987,
0.));
#198679=CARTESIAN_POINT('Ctrl Pts',(-21.4763353936762,-7.57667978402987,
12.));
#198680=CARTESIAN_POINT('Ctrl Pts',(-21.4870427508194,-7.57882826679131,
0.));
#198681=CARTESIAN_POINT('Ctrl Pts',(-21.4870427508194,-7.57882826679131,
12.));
#198682=CARTESIAN_POINT('Ctrl Pts',(-21.4979544192744,-7.58097917790744,
0.));
#198683=CARTESIAN_POINT('Ctrl Pts',(-21.4979544192744,-7.58097917790744,
12.));
#198684=CARTESIAN_POINT('Ctrl Pts',(-21.5090676573873,-7.58313080519179,
0.));
#198685=CARTESIAN_POINT('Ctrl Pts',(-21.5090676573873,-7.58313080519179,
12.));
#198686=CARTESIAN_POINT('Ctrl Pts',(-21.5203798035299,-7.58528148919129,
0.));
#198687=CARTESIAN_POINT('Ctrl Pts',(-21.5203798035299,-7.58528148919129,
12.));
#198688=CARTESIAN_POINT('Ctrl Pts',(-21.5318882716736,-7.58742962034833,
0.));
#198689=CARTESIAN_POINT('Ctrl Pts',(-21.5318882716736,-7.58742962034833,
12.));
#198690=CARTESIAN_POINT('Ctrl Pts',(-21.543590547011,-7.58957363620013,
0.));
#198691=CARTESIAN_POINT('Ctrl Pts',(-21.543590547011,-7.58957363620013,
12.));
#198692=CARTESIAN_POINT('Ctrl Pts',(-21.5554841813462,-7.59171201844776,
0.));
#198693=CARTESIAN_POINT('Ctrl Pts',(-21.5554841813462,-7.59171201844776,
12.));
#198694=CARTESIAN_POINT('Ctrl Pts',(-21.5675667904726,-7.59384329124918,
0.));
#198695=CARTESIAN_POINT('Ctrl Pts',(-21.5675667904726,-7.59384329124918,
12.));
#198696=CARTESIAN_POINT('Ctrl Pts',(-21.5798360518978,-7.59596601973583,
0.));
#198697=CARTESIAN_POINT('Ctrl Pts',(-21.5798360518978,-7.59596601973583,
12.));
#198698=CARTESIAN_POINT('Ctrl Pts',(-21.5922897024466,-7.59807880846194,
0.));
#198699=CARTESIAN_POINT('Ctrl Pts',(-21.5922897024466,-7.59807880846194,
12.));
#198700=CARTESIAN_POINT('Ctrl Pts',(-21.6049255358843,-7.6001802998824,
0.));
#198701=CARTESIAN_POINT('Ctrl Pts',(-21.6049255358843,-7.6001802998824,
12.));
#198702=CARTESIAN_POINT('Ctrl Pts',(-21.617741400599,-7.60226917285428,
0.));
#198703=CARTESIAN_POINT('Ctrl Pts',(-21.617741400599,-7.60226917285428,
12.));
#198704=CARTESIAN_POINT('Ctrl Pts',(-21.6307351973822,-7.60434414118295,
0.));
#198705=CARTESIAN_POINT('Ctrl Pts',(-21.6307351973822,-7.60434414118295,
12.));
#198706=CARTESIAN_POINT('Ctrl Pts',(-21.6439048771743,-7.60640395216356,
0.));
#198707=CARTESIAN_POINT('Ctrl Pts',(-21.6439048771743,-7.60640395216356,
12.));
#198708=CARTESIAN_POINT('Ctrl Pts',(-21.6572484388081,-7.60844738512873,
0.));
#198709=CARTESIAN_POINT('Ctrl Pts',(-21.6572484388081,-7.60844738512873,
12.));
#198710=CARTESIAN_POINT('Ctrl Pts',(-21.6707639267576,-7.61047325000955,
0.));
#198711=CARTESIAN_POINT('Ctrl Pts',(-21.6707639267576,-7.61047325000955,
12.));
#198712=CARTESIAN_POINT('Ctrl Pts',(-21.6844494295815,-7.61248038630268,
0.));
#198713=CARTESIAN_POINT('Ctrl Pts',(-21.6844494295815,-7.61248038630268,
12.));
#198714=CARTESIAN_POINT('Ctrl Pts',(-21.6983030783322,-7.61446766202786,
0.));
#198715=CARTESIAN_POINT('Ctrl Pts',(-21.6983030783322,-7.61446766202786,
12.));
#198716=CARTESIAN_POINT('Ctrl Pts',(-21.7123230449834,-7.6164339727042,
0.));
#198717=CARTESIAN_POINT('Ctrl Pts',(-21.7123230449834,-7.6164339727042,
12.));
#198718=CARTESIAN_POINT('Ctrl Pts',(-21.7265075407975,-7.61837824030537,
0.));
#198719=CARTESIAN_POINT('Ctrl Pts',(-21.7265075407975,-7.61837824030537,
12.));
#198720=CARTESIAN_POINT('Ctrl Pts',(-21.7408548148656,-7.62029941230854,
0.));
#198721=CARTESIAN_POINT('Ctrl Pts',(-21.7408548148656,-7.62029941230854,
12.));
#198722=CARTESIAN_POINT('Ctrl Pts',(-21.7553631528328,-7.62219646084228,
0.));
#198723=CARTESIAN_POINT('Ctrl Pts',(-21.7553631528328,-7.62219646084228,
12.));
#198724=CARTESIAN_POINT('Ctrl Pts',(-21.7700308755584,-7.62406838181166,
0.));
#198725=CARTESIAN_POINT('Ctrl Pts',(-21.7700308755584,-7.62406838181166,
12.));
#198726=CARTESIAN_POINT('Ctrl Pts',(-21.7848563378021,-7.62591419404512,
0.));
#198727=CARTESIAN_POINT('Ctrl Pts',(-21.7848563378021,-7.62591419404512,
12.));
#198728=CARTESIAN_POINT('Ctrl Pts',(-21.799837926858,-7.62773293842389,
0.));
#198729=CARTESIAN_POINT('Ctrl Pts',(-21.799837926858,-7.62773293842389,
12.));
#198730=CARTESIAN_POINT('Ctrl Pts',(-21.814974061509,-7.62952367718126,
0.));
#198731=CARTESIAN_POINT('Ctrl Pts',(-21.814974061509,-7.62952367718126,
12.));
#198732=CARTESIAN_POINT('Ctrl Pts',(-21.8302631910195,-7.63128549323022,
0.));
#198733=CARTESIAN_POINT('Ctrl Pts',(-21.8302631910195,-7.63128549323022,
12.));
#198734=CARTESIAN_POINT('Ctrl Pts',(-21.8457037941084,-7.63301748948935,
0.));
#198735=CARTESIAN_POINT('Ctrl Pts',(-21.8457037941084,-7.63301748948935,
12.));
#198736=CARTESIAN_POINT('Ctrl Pts',(-21.8612943779089,-7.63471878821225,
0.));
#198737=CARTESIAN_POINT('Ctrl Pts',(-21.8612943779089,-7.63471878821225,
12.));
#198738=CARTESIAN_POINT('Ctrl Pts',(-21.8770334769496,-7.63638853033399,
0.));
#198739=CARTESIAN_POINT('Ctrl Pts',(-21.8770334769496,-7.63638853033399,
12.));
#198740=CARTESIAN_POINT('Ctrl Pts',(-21.8929196523514,-7.63802587492034,
0.));
#198741=CARTESIAN_POINT('Ctrl Pts',(-21.8929196523514,-7.63802587492034,
12.));
#198742=CARTESIAN_POINT('Ctrl Pts',(-21.9089514909874,-7.63962999860927,
0.));
#198743=CARTESIAN_POINT('Ctrl Pts',(-21.9089514909874,-7.63962999860927,
12.));
#198744=CARTESIAN_POINT('Ctrl Pts',(-21.9251276046546,-7.64120009506531,
0.));
#198745=CARTESIAN_POINT('Ctrl Pts',(-21.9251276046546,-7.64120009506531,
12.));
#198746=CARTESIAN_POINT('Ctrl Pts',(-21.9414466292072,-7.64273537442682,
0.));
#198747=CARTESIAN_POINT('Ctrl Pts',(-21.9414466292072,-7.64273537442682,
12.));
#198748=CARTESIAN_POINT('Ctrl Pts',(-21.9579072237651,-7.64423506279122,
0.));
#198749=CARTESIAN_POINT('Ctrl Pts',(-21.9579072237651,-7.64423506279122,
12.));
#198750=CARTESIAN_POINT('Ctrl Pts',(-21.9745080700798,-7.64569840177335,
0.));
#198751=CARTESIAN_POINT('Ctrl Pts',(-21.9745080700798,-7.64569840177335,
12.));
#198752=CARTESIAN_POINT('Ctrl Pts',(-21.9912478718542,-7.64712464805249,
0.));
#198753=CARTESIAN_POINT('Ctrl Pts',(-21.9912478718542,-7.64712464805249,
12.));
#198754=CARTESIAN_POINT('Ctrl Pts',(-22.0081253540774,-7.64851307293351,
0.));
#198755=CARTESIAN_POINT('Ctrl Pts',(-22.0081253540774,-7.64851307293351,
12.));
#198756=CARTESIAN_POINT('Ctrl Pts',(-22.0251392623209,-7.64986296190168,
0.));
#198757=CARTESIAN_POINT('Ctrl Pts',(-22.0251392623209,-7.64986296190168,
12.));
#198758=CARTESIAN_POINT('Ctrl Pts',(-22.0422883621174,-7.65117361421358,
0.));
#198759=CARTESIAN_POINT('Ctrl Pts',(-22.0422883621174,-7.65117361421358,
12.));
#198760=CARTESIAN_POINT('Ctrl Pts',(-22.0595714384431,-7.65244434253112,
0.));
#198761=CARTESIAN_POINT('Ctrl Pts',(-22.0595714384431,-7.65244434253112,
12.));
#198762=CARTESIAN_POINT('Ctrl Pts',(-22.0769872951596,-7.65367447254949,
0.));
#198763=CARTESIAN_POINT('Ctrl Pts',(-22.0769872951596,-7.65367447254949,
12.));
#198764=CARTESIAN_POINT('Ctrl Pts',(-22.094534754469,-7.65486334263643,
0.));
#198765=CARTESIAN_POINT('Ctrl Pts',(-22.094534754469,-7.65486334263643,
12.));
#198766=CARTESIAN_POINT('Ctrl Pts',(-22.1122126563329,-7.65601030346806,
0.));
#198767=CARTESIAN_POINT('Ctrl Pts',(-22.1122126563329,-7.65601030346806,
12.));
#198768=CARTESIAN_POINT('Ctrl Pts',(-22.1300198579675,-7.65711471769396,
0.));
#198769=CARTESIAN_POINT('Ctrl Pts',(-22.1300198579675,-7.65711471769396,
12.));
#198770=CARTESIAN_POINT('Ctrl Pts',(-22.1479552334211,-7.65817595963349,
0.));
#198771=CARTESIAN_POINT('Ctrl Pts',(-22.1479552334211,-7.65817595963349,
12.));
#198772=CARTESIAN_POINT('Ctrl Pts',(-22.1660176731178,-7.6591934149693,
0.));
#198773=CARTESIAN_POINT('Ctrl Pts',(-22.1660176731178,-7.6591934149693,
12.));
#198774=CARTESIAN_POINT('Ctrl Pts',(-22.1842060834091,-7.66016648045004,
0.));
#198775=CARTESIAN_POINT('Ctrl Pts',(-22.1842060834091,-7.66016648045004,
12.));
#198776=CARTESIAN_POINT('Ctrl Pts',(-22.2025193860964,-7.6610945635927,
0.));
#198777=CARTESIAN_POINT('Ctrl Pts',(-22.2025193860964,-7.6610945635927,
12.));
#198778=CARTESIAN_POINT('Ctrl Pts',(-22.2209565180085,-7.66197708240399,
0.));
#198779=CARTESIAN_POINT('Ctrl Pts',(-22.2209565180085,-7.66197708240399,
12.));
#198780=CARTESIAN_POINT('Ctrl Pts',(-22.2395164306547,-7.66281346512508,
0.));
#198781=CARTESIAN_POINT('Ctrl Pts',(-22.2395164306547,-7.66281346512508,
12.));
#198782=CARTESIAN_POINT('Ctrl Pts',(-22.258198089848,-7.6636031499764,0.));
#198783=CARTESIAN_POINT('Ctrl Pts',(-22.258198089848,-7.6636031499764,12.));
#198784=CARTESIAN_POINT('Ctrl Pts',(-22.2770004753335,-7.66434558490978,
0.));
#198785=CARTESIAN_POINT('Ctrl Pts',(-22.2770004753335,-7.66434558490978,
12.));
#198786=CARTESIAN_POINT('Ctrl Pts',(-22.2959225803937,-7.66504022736298,
0.));
#198787=CARTESIAN_POINT('Ctrl Pts',(-22.2959225803937,-7.66504022736298,
12.));
#198788=CARTESIAN_POINT('Ctrl Pts',(-22.314963411484,-7.66568654402493,
0.));
#198789=CARTESIAN_POINT('Ctrl Pts',(-22.314963411484,-7.66568654402493,
12.));
#198790=CARTESIAN_POINT('Ctrl Pts',(-22.3341219879469,-7.66628401061952,
0.));
#198791=CARTESIAN_POINT('Ctrl Pts',(-22.3341219879469,-7.66628401061952,
12.));
#198792=CARTESIAN_POINT('Ctrl Pts',(-22.3533973417021,-7.66683211169158,
0.));
#198793=CARTESIAN_POINT('Ctrl Pts',(-22.3533973417021,-7.66683211169158,
12.));
#198794=CARTESIAN_POINT('Ctrl Pts',(-22.372788516936,-7.66733034039882,
0.));
#198795=CARTESIAN_POINT('Ctrl Pts',(-22.372788516936,-7.66733034039882,
12.));
#198796=CARTESIAN_POINT('Ctrl Pts',(-22.3922945697773,-7.66777819830789,
0.));
#198797=CARTESIAN_POINT('Ctrl Pts',(-22.3922945697773,-7.66777819830789,
12.));
#198798=CARTESIAN_POINT('Ctrl Pts',(-22.4119145679758,-7.66817519519639,
0.));
#198799=CARTESIAN_POINT('Ctrl Pts',(-22.4119145679758,-7.66817519519639,
12.));
#198800=CARTESIAN_POINT('Ctrl Pts',(-22.4316475906603,-7.66852084886704,
0.));
#198801=CARTESIAN_POINT('Ctrl Pts',(-22.4316475906603,-7.66852084886704,
12.));
#198802=CARTESIAN_POINT('Ctrl Pts',(-22.4514927280855,-7.66881468496634,
0.));
#198803=CARTESIAN_POINT('Ctrl Pts',(-22.4514927280855,-7.66881468496634,
12.));
#198804=CARTESIAN_POINT('Ctrl Pts',(-22.47144908137,-7.6690562368083,0.));
#198805=CARTESIAN_POINT('Ctrl Pts',(-22.47144908137,-7.6690562368083,12.));
#198806=CARTESIAN_POINT('Ctrl Pts',(-22.4915157622312,-7.66924504520314,
0.));
#198807=CARTESIAN_POINT('Ctrl Pts',(-22.4915157622312,-7.66924504520314,
12.));
#198808=CARTESIAN_POINT('Ctrl Pts',(-22.5116918927032,-7.66938065829107,
0.));
#198809=CARTESIAN_POINT('Ctrl Pts',(-22.5116918927032,-7.66938065829107,
12.));
#198810=CARTESIAN_POINT('Ctrl Pts',(-22.53197660492,-7.66946263138143,0.));
#198811=CARTESIAN_POINT('Ctrl Pts',(-22.53197660492,-7.66946263138143,12.));
#198812=CARTESIAN_POINT('Ctrl Pts',(-22.5523690409116,-7.66949052679692,
0.));
#198813=CARTESIAN_POINT('Ctrl Pts',(-22.5523690409116,-7.66949052679692,
12.));
#198814=CARTESIAN_POINT('Ctrl Pts',(-22.5728683523831,-7.66946391372305,
0.));
#198815=CARTESIAN_POINT('Ctrl Pts',(-22.5728683523831,-7.66946391372305,
12.));
#198816=CARTESIAN_POINT('Ctrl Pts',(-22.5934737004953,-7.66938236806232,
0.));
#198817=CARTESIAN_POINT('Ctrl Pts',(-22.5934737004953,-7.66938236806232,
12.));
#198818=CARTESIAN_POINT('Ctrl Pts',(-22.6141842556243,-7.66924547229413,
0.));
#198819=CARTESIAN_POINT('Ctrl Pts',(-22.6141842556243,-7.66924547229413,
12.));
#198820=CARTESIAN_POINT('Ctrl Pts',(-22.6349991971541,-7.66905281533714,
0.));
#198821=CARTESIAN_POINT('Ctrl Pts',(-22.6349991971541,-7.66905281533714,
12.));
#198822=CARTESIAN_POINT('Ctrl Pts',(-22.6559177133127,-7.66880399241322,
0.));
#198823=CARTESIAN_POINT('Ctrl Pts',(-22.6559177133127,-7.66880399241322,
12.));
#198824=CARTESIAN_POINT('Ctrl Pts',(-22.6769390009885,-7.66849860491742,
0.));
#198825=CARTESIAN_POINT('Ctrl Pts',(-22.6769390009885,-7.66849860491742,
12.));
#198826=CARTESIAN_POINT('Ctrl Pts',(-22.6980622655446,-7.66813626029274,
0.));
#198827=CARTESIAN_POINT('Ctrl Pts',(-22.6980622655446,-7.66813626029274,
12.));
#198828=CARTESIAN_POINT('Ctrl Pts',(-22.7192867206245,-7.66771657191027,
0.));
#198829=CARTESIAN_POINT('Ctrl Pts',(-22.7192867206245,-7.66771657191027,
12.));
#198830=CARTESIAN_POINT('Ctrl Pts',(-22.7406115879513,-7.66723915895439,
0.));
#198831=CARTESIAN_POINT('Ctrl Pts',(-22.7406115879513,-7.66723915895439,
12.));
#198832=CARTESIAN_POINT('Ctrl Pts',(-22.7620360971843,-7.66670364630298,
0.));
#198833=CARTESIAN_POINT('Ctrl Pts',(-22.7620360971843,-7.66670364630298,
12.));
#198834=CARTESIAN_POINT('Ctrl Pts',(-22.7835594857699,-7.66610966441272,
0.));
#198835=CARTESIAN_POINT('Ctrl Pts',(-22.7835594857699,-7.66610966441272,
12.));
#198836=CARTESIAN_POINT('Ctrl Pts',(-22.8051809987833,-7.66545684920987,
0.));
#198837=CARTESIAN_POINT('Ctrl Pts',(-22.8051809987833,-7.66545684920987,
12.));
#198838=CARTESIAN_POINT('Ctrl Pts',(-22.8268998887678,-7.66474484198548,
0.));
#198839=CARTESIAN_POINT('Ctrl Pts',(-22.8268998887678,-7.66474484198548,
12.));
#198840=CARTESIAN_POINT('Ctrl Pts',(-22.848715415557,-7.66397328929802,
0.));
#198841=CARTESIAN_POINT('Ctrl Pts',(-22.848715415557,-7.66397328929802,
12.));
#198842=CARTESIAN_POINT('Ctrl Pts',(-22.8706268461283,-7.66314184287336,
0.));
#198843=CARTESIAN_POINT('Ctrl Pts',(-22.8706268461283,-7.66314184287336,
12.));
#198844=CARTESIAN_POINT('Ctrl Pts',(-22.8926334544883,-7.66225015950155,
0.));
#198845=CARTESIAN_POINT('Ctrl Pts',(-22.8926334544883,-7.66225015950155,
12.));
#198846=CARTESIAN_POINT('Ctrl Pts',(-22.9147345215421,-7.66129790094107,
0.));
#198847=CARTESIAN_POINT('Ctrl Pts',(-22.9147345215421,-7.66129790094107,
12.));
#198848=CARTESIAN_POINT('Ctrl Pts',(-22.9369293349593,-7.66028473382777,
0.));
#198849=CARTESIAN_POINT('Ctrl Pts',(-22.9369293349593,-7.66028473382777,
12.));
#198850=CARTESIAN_POINT('Ctrl Pts',(-22.959217189033,-7.65921032958901,
0.));
#198851=CARTESIAN_POINT('Ctrl Pts',(-22.959217189033,-7.65921032958901,
12.));
#198852=CARTESIAN_POINT('Ctrl Pts',(-22.9815973845296,-7.65807436436431,
0.));
#198853=CARTESIAN_POINT('Ctrl Pts',(-22.9815973845296,-7.65807436436431,
12.));
#198854=CARTESIAN_POINT('Ctrl Pts',(-23.0040692285814,-7.65687651891304,
0.));
#198855=CARTESIAN_POINT('Ctrl Pts',(-23.0040692285814,-7.65687651891304,
12.));
#198856=CARTESIAN_POINT('Ctrl Pts',(-23.0266320345787,-7.65561647852533,
0.));
#198857=CARTESIAN_POINT('Ctrl Pts',(-23.0266320345787,-7.65561647852533,
12.));
#198858=CARTESIAN_POINT('Ctrl Pts',(-23.0492851220528,-7.65429393293945,
0.));
#198859=CARTESIAN_POINT('Ctrl Pts',(-23.0492851220528,-7.65429393293945,
12.));
#198860=CARTESIAN_POINT('Ctrl Pts',(-23.072027816555,-7.65290857626357,
0.));
#198861=CARTESIAN_POINT('Ctrl Pts',(-23.072027816555,-7.65290857626357,
12.));
#198862=CARTESIAN_POINT('Ctrl Pts',(-23.094859449525,-7.65146010690475,
0.));
#198863=CARTESIAN_POINT('Ctrl Pts',(-23.094859449525,-7.65146010690475,
12.));
#198864=CARTESIAN_POINT('Ctrl Pts',(-23.1177793581679,-7.64994822749859,
0.));
#198865=CARTESIAN_POINT('Ctrl Pts',(-23.1177793581679,-7.64994822749859,
12.));
#198866=CARTESIAN_POINT('Ctrl Pts',(-23.1407868853819,-7.64837264482942,
0.));
#198867=CARTESIAN_POINT('Ctrl Pts',(-23.1407868853819,-7.64837264482942,
12.));
#198868=CARTESIAN_POINT('Ctrl Pts',(-23.1638813796694,-7.64673306975804,
0.));
#198869=CARTESIAN_POINT('Ctrl Pts',(-23.1638813796694,-7.64673306975804,
12.));
#198870=CARTESIAN_POINT('Ctrl Pts',(-23.1870621950452,-7.64502921715482,
0.));
#198871=CARTESIAN_POINT('Ctrl Pts',(-23.1870621950452,-7.64502921715482,
12.));
#198872=CARTESIAN_POINT('Ctrl Pts',(-23.2103286909398,-7.64326080583679,
0.));
#198873=CARTESIAN_POINT('Ctrl Pts',(-23.2103286909398,-7.64326080583679,
12.));
#198874=CARTESIAN_POINT('Ctrl Pts',(-23.2336802320912,-7.64142755851504,
0.));
#198875=CARTESIAN_POINT('Ctrl Pts',(-23.2336802320912,-7.64142755851504,
12.));
#198876=CARTESIAN_POINT('Ctrl Pts',(-23.2571161884488,-7.63952920172835,
0.));
#198877=CARTESIAN_POINT('Ctrl Pts',(-23.2571161884488,-7.63952920172835,
12.));
#198878=CARTESIAN_POINT('Ctrl Pts',(-23.2806359350855,-7.63756546576374,
0.));
#198879=CARTESIAN_POINT('Ctrl Pts',(-23.2806359350855,-7.63756546576374,
12.));
#198880=CARTESIAN_POINT('Ctrl Pts',(-23.3042388521022,-7.63553608458782,
0.));
#198881=CARTESIAN_POINT('Ctrl Pts',(-23.3042388521022,-7.63553608458782,
12.));
#198882=CARTESIAN_POINT('Ctrl Pts',(-23.3279243245241,-7.63344079578161,
0.));
#198883=CARTESIAN_POINT('Ctrl Pts',(-23.3279243245241,-7.63344079578161,
12.));
#198884=CARTESIAN_POINT('Ctrl Pts',(-23.3516917421972,-7.63127934048136,
0.));
#198885=CARTESIAN_POINT('Ctrl Pts',(-23.3516917421972,-7.63127934048136,
12.));
#198886=CARTESIAN_POINT('Ctrl Pts',(-23.3755404996636,-7.62905146332592,
0.));
#198887=CARTESIAN_POINT('Ctrl Pts',(-23.3755404996636,-7.62905146332592,
12.));
#198888=CARTESIAN_POINT('Ctrl Pts',(-23.399469996112,-7.62675691240328,
0.));
#198889=CARTESIAN_POINT('Ctrl Pts',(-23.399469996112,-7.62675691240328,
12.));
#198890=CARTESIAN_POINT('Ctrl Pts',(-23.4234796353542,-7.62439543920049,
0.));
#198891=CARTESIAN_POINT('Ctrl Pts',(-23.4234796353542,-7.62439543920049,
12.));
#198892=CARTESIAN_POINT('Ctrl Pts',(-23.4475688257854,-7.62196679855954,
0.));
#198893=CARTESIAN_POINT('Ctrl Pts',(-23.4475688257854,-7.62196679855954,
12.));
#198894=CARTESIAN_POINT('Ctrl Pts',(-23.4717369803438,-7.61947074863976,
0.));
#198895=CARTESIAN_POINT('Ctrl Pts',(-23.4717369803438,-7.61947074863976,
12.));
#198896=CARTESIAN_POINT('Ctrl Pts',(-23.4959835164609,-7.61690705088318,
0.));
#198897=CARTESIAN_POINT('Ctrl Pts',(-23.4959835164609,-7.61690705088318,
12.));
#198898=CARTESIAN_POINT('Ctrl Pts',(-23.5203078560129,-7.61427546999297,
0.));
#198899=CARTESIAN_POINT('Ctrl Pts',(-23.5203078560129,-7.61427546999297,
12.));
#198900=CARTESIAN_POINT('Ctrl Pts',(-23.544709425203,-7.61157577385371,
0.));
#198901=CARTESIAN_POINT('Ctrl Pts',(-23.544709425203,-7.61157577385371,
12.));
#198902=CARTESIAN_POINT('Ctrl Pts',(-23.5691876544244,-7.60880773344599,
0.));
#198903=CARTESIAN_POINT('Ctrl Pts',(-23.5691876544244,-7.60880773344599,
12.));
#198904=CARTESIAN_POINT('Ctrl Pts',(-23.5937419781245,-7.60597112277093,
0.));
#198905=CARTESIAN_POINT('Ctrl Pts',(-23.5937419781245,-7.60597112277093,
12.));
#198906=CARTESIAN_POINT('Ctrl Pts',(-23.6183718346576,-7.60306571877805,
0.));
#198907=CARTESIAN_POINT('Ctrl Pts',(-23.6183718346576,-7.60306571877805,
12.));
#198908=CARTESIAN_POINT('Ctrl Pts',(-23.6430766661418,-7.60009130130125,
0.));
#198909=CARTESIAN_POINT('Ctrl Pts',(-23.6430766661418,-7.60009130130125,
12.));
#198910=CARTESIAN_POINT('Ctrl Pts',(-23.6678559182875,-7.59704765299566,
0.));
#198911=CARTESIAN_POINT('Ctrl Pts',(-23.6678559182875,-7.59704765299566,
12.));
#198912=CARTESIAN_POINT('Ctrl Pts',(-23.6927090405066,-7.59393455934034,
0.));
#198913=CARTESIAN_POINT('Ctrl Pts',(-23.6927090405066,-7.59393455934034,
12.));
#198914=CARTESIAN_POINT('Ctrl Pts',(-23.7176354860457,-7.5907518086532,
0.));
#198915=CARTESIAN_POINT('Ctrl Pts',(-23.7176354860457,-7.5907518086532,
12.));
#198916=CARTESIAN_POINT('Ctrl Pts',(-23.7426347121006,-7.58749919210825,
0.));
#198917=CARTESIAN_POINT('Ctrl Pts',(-23.7426347121006,-7.58749919210825,
12.));
#198918=CARTESIAN_POINT('Ctrl Pts',(-23.7677061799376,-7.5841765037627,
0.));
#198919=CARTESIAN_POINT('Ctrl Pts',(-23.7677061799376,-7.5841765037627,
12.));
#198920=CARTESIAN_POINT('Ctrl Pts',(-23.7928493549908,-7.58078354058212,
0.));
#198921=CARTESIAN_POINT('Ctrl Pts',(-23.7928493549908,-7.58078354058212,
12.));
#198922=CARTESIAN_POINT('Ctrl Pts',(-23.8180637069976,-7.57732010249065,
0.));
#198923=CARTESIAN_POINT('Ctrl Pts',(-23.8180637069976,-7.57732010249065,
12.));
#198924=CARTESIAN_POINT('Ctrl Pts',(-23.8433487096132,-7.57378599219814,
0.));
#198925=CARTESIAN_POINT('Ctrl Pts',(-23.8433487096132,-7.57378599219814,
12.));
#198926=CARTESIAN_POINT('Ctrl Pts',(-23.8687038399595,-7.57018101500709,
0.));
#198927=CARTESIAN_POINT('Ctrl Pts',(-23.8687038399595,-7.57018101500709,
12.));
#198928=CARTESIAN_POINT('Ctrl Pts',(-23.8941285782002,-7.5665049786379,
0.));
#198929=CARTESIAN_POINT('Ctrl Pts',(-23.8941285782002,-7.5665049786379,
12.));
#198930=CARTESIAN_POINT('Ctrl Pts',(-23.9196224070759,-7.56275769304772,
0.));
#198931=CARTESIAN_POINT('Ctrl Pts',(-23.9196224070759,-7.56275769304772,
12.));
#198932=CARTESIAN_POINT('Ctrl Pts',(-23.9451848115002,-7.55893897027679,
0.));
#198933=CARTESIAN_POINT('Ctrl Pts',(-23.9451848115002,-7.55893897027679,
12.));
#198934=CARTESIAN_POINT('Ctrl Pts',(-23.9708152779886,-7.55504862424807,
0.));
#198935=CARTESIAN_POINT('Ctrl Pts',(-23.9708152779886,-7.55504862424807,
12.));
#198936=CARTESIAN_POINT('Ctrl Pts',(-23.9965132953187,-7.55108647097431,
0.));
#198937=CARTESIAN_POINT('Ctrl Pts',(-23.9965132953187,-7.55108647097431,
12.));
#198938=CARTESIAN_POINT('Ctrl Pts',(-24.0222783554531,-7.54705232885894,
0.));
#198939=CARTESIAN_POINT('Ctrl Pts',(-24.0222783554531,-7.54705232885894,
12.));
#198940=CARTESIAN_POINT('Ctrl Pts',(-24.0481099543353,-7.54294601896127,
0.));
#198941=CARTESIAN_POINT('Ctrl Pts',(-24.0481099543353,-7.54294601896127,
12.));
#198942=CARTESIAN_POINT('Ctrl Pts',(-24.0740075927984,-7.53876736531004,
0.));
#198943=CARTESIAN_POINT('Ctrl Pts',(-24.0740075927984,-7.53876736531004,
12.));
#198944=CARTESIAN_POINT('Ctrl Pts',(-24.0999707772643,-7.53451619514658,
0.));
#198945=CARTESIAN_POINT('Ctrl Pts',(-24.0999707772643,-7.53451619514658,
12.));
#198946=CARTESIAN_POINT('Ctrl Pts',(-24.1259990209211,-7.53019233935536,
0.));
#198947=CARTESIAN_POINT('Ctrl Pts',(-24.1259990209211,-7.53019233935536,
12.));
#198948=CARTESIAN_POINT('Ctrl Pts',(-24.152091842537,-7.52579563201478,
0.));
#198949=CARTESIAN_POINT('Ctrl Pts',(-24.152091842537,-7.52579563201478,
12.));
#198950=CARTESIAN_POINT('Ctrl Pts',(-24.1782487641602,-7.52132590953862,
0.));
#198951=CARTESIAN_POINT('Ctrl Pts',(-24.1782487641602,-7.52132590953862,
12.));
#198952=CARTESIAN_POINT('Ctrl Pts',(-24.2044693092356,-7.51678300997997,
0.));
#198953=CARTESIAN_POINT('Ctrl Pts',(-24.2044693092356,-7.51678300997997,
12.));
#198954=CARTESIAN_POINT('Ctrl Pts',(-24.230753000389,-7.51216677222198,
0.));
#198955=CARTESIAN_POINT('Ctrl Pts',(-24.230753000389,-7.51216677222198,
12.));
#198956=CARTESIAN_POINT('Ctrl Pts',(-24.2570993577032,-7.50747703535114,
0.));
#198957=CARTESIAN_POINT('Ctrl Pts',(-24.2570993577032,-7.50747703535114,
12.));
#198958=CARTESIAN_POINT('Ctrl Pts',(-24.2835078958966,-7.50271363765098,
0.));
#198959=CARTESIAN_POINT('Ctrl Pts',(-24.2835078958966,-7.50271363765098,
12.));
#198960=CARTESIAN_POINT('Ctrl Pts',(-24.3099781253345,-7.49787641695358,
0.));
#198961=CARTESIAN_POINT('Ctrl Pts',(-24.3099781253345,-7.49787641695358,
12.));
#198962=CARTESIAN_POINT('Ctrl Pts',(-24.3365095573673,-7.49296521252329,
0.));
#198963=CARTESIAN_POINT('Ctrl Pts',(-24.3365095573673,-7.49296521252329,
12.));
#198964=CARTESIAN_POINT('Ctrl Pts',(-24.3631017084513,-7.48797986651827,
0.));
#198965=CARTESIAN_POINT('Ctrl Pts',(-24.3631017084513,-7.48797986651827,
12.));
#198966=CARTESIAN_POINT('Ctrl Pts',(-24.3897541049248,-7.48292022569253,
0.));
#198967=CARTESIAN_POINT('Ctrl Pts',(-24.3897541049248,-7.48292022569253,
12.));
#198968=CARTESIAN_POINT('Ctrl Pts',(-24.4164662871165,-7.47778614286573,
0.));
#198969=CARTESIAN_POINT('Ctrl Pts',(-24.4164662871165,-7.47778614286573,
12.));
#198970=CARTESIAN_POINT('Ctrl Pts',(-24.4432378146501,-7.47257747883318,
0.));
#198971=CARTESIAN_POINT('Ctrl Pts',(-24.4432378146501,-7.47257747883318,
12.));
#198972=CARTESIAN_POINT('Ctrl Pts',(-24.4700682684544,-7.46729410308922,
0.));
#198973=CARTESIAN_POINT('Ctrl Pts',(-24.4700682684544,-7.46729410308922,
12.));
#198974=CARTESIAN_POINT('Ctrl Pts',(-24.4969572391509,-7.46193588961641,
0.));
#198975=CARTESIAN_POINT('Ctrl Pts',(-24.4969572391509,-7.46193588961641,
12.));
#198976=CARTESIAN_POINT('Ctrl Pts',(-24.52390431731,-7.45650271336045,0.));
#198977=CARTESIAN_POINT('Ctrl Pts',(-24.52390431731,-7.45650271336045,12.));
#198978=CARTESIAN_POINT('Ctrl Pts',(-24.5509090831579,-7.45099444651295,
0.));
#198979=CARTESIAN_POINT('Ctrl Pts',(-24.5509090831579,-7.45099444651295,
12.));
#198980=CARTESIAN_POINT('Ctrl Pts',(-24.5779710960865,-7.44541095473162,
0.));
#198981=CARTESIAN_POINT('Ctrl Pts',(-24.5779710960865,-7.44541095473162,
12.));
#198982=CARTESIAN_POINT('Ctrl Pts',(-24.6050898852349,-7.43975209375374,
0.));
#198983=CARTESIAN_POINT('Ctrl Pts',(-24.6050898852349,-7.43975209375374,
12.));
#198984=CARTESIAN_POINT('Ctrl Pts',(-24.6322649369472,-7.4340177048922,
0.));
#198985=CARTESIAN_POINT('Ctrl Pts',(-24.6322649369472,-7.4340177048922,
12.));
#198986=CARTESIAN_POINT('Ctrl Pts',(-24.659495712869,-7.4282076215868,0.));
#198987=CARTESIAN_POINT('Ctrl Pts',(-24.659495712869,-7.4282076215868,12.));
#198988=CARTESIAN_POINT('Ctrl Pts',(-24.6867816727118,-7.42232167765762,
0.));
#198989=CARTESIAN_POINT('Ctrl Pts',(-24.6867816727118,-7.42232167765762,
12.));
#198990=CARTESIAN_POINT('Ctrl Pts',(-24.7141222949988,-7.41635971481243,
0.));
#198991=CARTESIAN_POINT('Ctrl Pts',(-24.7141222949988,-7.41635971481243,
12.));
#198992=CARTESIAN_POINT('Ctrl Pts',(-24.7415170994754,-7.41032159082173,
0.));
#198993=CARTESIAN_POINT('Ctrl Pts',(-24.7415170994754,-7.41032159082173,
12.));
#198994=CARTESIAN_POINT('Ctrl Pts',(-24.7689656669005,-7.40420718661754,
0.));
#198995=CARTESIAN_POINT('Ctrl Pts',(-24.7689656669005,-7.40420718661754,
12.));
#198996=CARTESIAN_POINT('Ctrl Pts',(-24.7964676646518,-7.39801641583612,
0.));
#198997=CARTESIAN_POINT('Ctrl Pts',(-24.7964676646518,-7.39801641583612,
12.));
#198998=CARTESIAN_POINT('Ctrl Pts',(-24.8240228521042,-7.39174922586841,
0.));
#198999=CARTESIAN_POINT('Ctrl Pts',(-24.8240228521042,-7.39174922586841,
12.));
#199000=CARTESIAN_POINT('Ctrl Pts',(-24.8516310625367,-7.38540558904945,
0.));
#199001=CARTESIAN_POINT('Ctrl Pts',(-24.8516310625367,-7.38540558904945,
12.));
#199002=CARTESIAN_POINT('Ctrl Pts',(-24.8792921911309,-7.3789854964161,
0.));
#199003=CARTESIAN_POINT('Ctrl Pts',(-24.8792921911309,-7.3789854964161,
12.));
#199004=CARTESIAN_POINT('Ctrl Pts',(-24.9014633826201,-7.37378825962717,
0.));
#199005=CARTESIAN_POINT('Ctrl Pts',(-24.9014633826201,-7.37378825962717,
12.));
#199006=CARTESIAN_POINT('Ctrl Pts',(-24.9181155530631,-7.36985593120696,
0.));
#199007=CARTESIAN_POINT('Ctrl Pts',(-24.9181155530631,-7.36985593120696,
12.));
#199008=CARTESIAN_POINT('Ctrl Pts',(-24.9292275670705,-7.36721909029059,
0.));
#199009=CARTESIAN_POINT('Ctrl Pts',(-24.9292275670705,-7.36721909029059,
12.));
#199010=CARTESIAN_POINT('Ctrl Pts',(-24.9347862158358,-7.36589684767343,
0.));
#199011=CARTESIAN_POINT('Ctrl Pts',(-24.9347862158358,-7.36589684767343,
12.));
#199012=CARTESIAN_POINT('',(-24.9347862158358,-7.36589684767343,0.));
#199013=CARTESIAN_POINT('Ctrl Pts',(-21.2610617890679,-7.52250298901264,
0.));
#199014=CARTESIAN_POINT('Ctrl Pts',(-21.2610673466886,-7.5225064970397,
0.));
#199015=CARTESIAN_POINT('Ctrl Pts',(-21.2611204474866,-7.52252744144903,
0.));
#199016=CARTESIAN_POINT('Ctrl Pts',(-21.261326054066,-7.5226006423166,0.));
#199017=CARTESIAN_POINT('Ctrl Pts',(-21.2618521283555,-7.52278182242669,
0.));
#199018=CARTESIAN_POINT('Ctrl Pts',(-21.262927782038,-7.52314642316199,
0.));
#199019=CARTESIAN_POINT('Ctrl Pts',(-21.2644161259962,-7.52364573027552,
0.));
#199020=CARTESIAN_POINT('Ctrl Pts',(-21.2663059157058,-7.52427261074297,
0.));
#199021=CARTESIAN_POINT('Ctrl Pts',(-21.2685823838671,-7.5250177033353,
0.));
#199022=CARTESIAN_POINT('Ctrl Pts',(-21.2712301573466,-7.52587126095529,
0.));
#199023=CARTESIAN_POINT('Ctrl Pts',(-21.2742366113579,-7.5268252691854,
0.));
#199024=CARTESIAN_POINT('Ctrl Pts',(-21.2775925269652,-7.52787386225332,
0.));
#199025=CARTESIAN_POINT('Ctrl Pts',(-21.2812902781143,-7.52901217930407,
0.));
#199026=CARTESIAN_POINT('Ctrl Pts',(-21.2853226580657,-7.53023562438229,
0.));
#199027=CARTESIAN_POINT('Ctrl Pts',(-21.2896816163842,-7.53153906987855,
0.));
#199028=CARTESIAN_POINT('Ctrl Pts',(-21.2943588989331,-7.53291726078526,
0.));
#199029=CARTESIAN_POINT('Ctrl Pts',(-21.2993464250717,-7.53436505309942,
0.));
#199030=CARTESIAN_POINT('Ctrl Pts',(-21.3046368712157,-7.53587778251735,
0.));
#199031=CARTESIAN_POINT('Ctrl Pts',(-21.310223716773,-7.53745129364616,
0.));
#199032=CARTESIAN_POINT('Ctrl Pts',(-21.3161009456256,-7.53908175169898,
0.));
#199033=CARTESIAN_POINT('Ctrl Pts',(-21.3222628524165,-7.54076552038278,
0.));
#199034=CARTESIAN_POINT('Ctrl Pts',(-21.328703791771,-7.5424990037703,0.));
#199035=CARTESIAN_POINT('Ctrl Pts',(-21.3354182340149,-7.54427868151267,
0.));
#199036=CARTESIAN_POINT('Ctrl Pts',(-21.3424008295038,-7.54610114948346,
0.));
#199037=CARTESIAN_POINT('Ctrl Pts',(-21.3496464761531,-7.5479631624633,
0.));
#199038=CARTESIAN_POINT('Ctrl Pts',(-21.3571503685855,-7.54986166521309,
0.));
#199039=CARTESIAN_POINT('Ctrl Pts',(-21.3649079431865,-7.55179375777443,
0.));
#199040=CARTESIAN_POINT('Ctrl Pts',(-21.3729148390243,-7.55375667080028,
0.));
#199041=CARTESIAN_POINT('Ctrl Pts',(-21.3811668478932,-7.55574773403502,
0.));
#199042=CARTESIAN_POINT('Ctrl Pts',(-21.3896598842117,-7.55776435731416,
0.));
#199043=CARTESIAN_POINT('Ctrl Pts',(-21.3983899952987,-7.5598040370061,
0.));
#199044=CARTESIAN_POINT('Ctrl Pts',(-21.4073533630365,-7.56186435703621,
0.));
#199045=CARTESIAN_POINT('Ctrl Pts',(-21.4165463106254,-7.56394299313684,
0.));
#199046=CARTESIAN_POINT('Ctrl Pts',(-21.4259653015736,-7.56603771218712,
0.));
#199047=CARTESIAN_POINT('Ctrl Pts',(-21.4356069261513,-7.56814636360847,
0.));
#199048=CARTESIAN_POINT('Ctrl Pts',(-21.4454678907509,-7.57026687261165,
0.));
#199049=CARTESIAN_POINT('Ctrl Pts',(-21.4555450053142,-7.57239723223505,
0.));
#199050=CARTESIAN_POINT('Ctrl Pts',(-21.4658351740128,-7.57453549743411,
0.));
#199051=CARTESIAN_POINT('Ctrl Pts',(-21.4763353936762,-7.57667978402987,
0.));
#199052=CARTESIAN_POINT('Ctrl Pts',(-21.4870427508194,-7.57882826679131,
0.));
#199053=CARTESIAN_POINT('Ctrl Pts',(-21.4979544192744,-7.58097917790744,
0.));
#199054=CARTESIAN_POINT('Ctrl Pts',(-21.5090676573873,-7.58313080519179,
0.));
#199055=CARTESIAN_POINT('Ctrl Pts',(-21.5203798035299,-7.58528148919129,
0.));
#199056=CARTESIAN_POINT('Ctrl Pts',(-21.5318882716736,-7.58742962034833,
0.));
#199057=CARTESIAN_POINT('Ctrl Pts',(-21.543590547011,-7.58957363620013,
0.));
#199058=CARTESIAN_POINT('Ctrl Pts',(-21.5554841813462,-7.59171201844776,
0.));
#199059=CARTESIAN_POINT('Ctrl Pts',(-21.5675667904726,-7.59384329124918,
0.));
#199060=CARTESIAN_POINT('Ctrl Pts',(-21.5798360518978,-7.59596601973583,
0.));
#199061=CARTESIAN_POINT('Ctrl Pts',(-21.5922897024466,-7.59807880846194,
0.));
#199062=CARTESIAN_POINT('Ctrl Pts',(-21.6049255358843,-7.6001802998824,
0.));
#199063=CARTESIAN_POINT('Ctrl Pts',(-21.617741400599,-7.60226917285428,
0.));
#199064=CARTESIAN_POINT('Ctrl Pts',(-21.6307351973822,-7.60434414118295,
0.));
#199065=CARTESIAN_POINT('Ctrl Pts',(-21.6439048771743,-7.60640395216356,
0.));
#199066=CARTESIAN_POINT('Ctrl Pts',(-21.6572484388081,-7.60844738512873,
0.));
#199067=CARTESIAN_POINT('Ctrl Pts',(-21.6707639267576,-7.61047325000955,
0.));
#199068=CARTESIAN_POINT('Ctrl Pts',(-21.6844494295815,-7.61248038630268,
0.));
#199069=CARTESIAN_POINT('Ctrl Pts',(-21.6983030783322,-7.61446766202786,
0.));
#199070=CARTESIAN_POINT('Ctrl Pts',(-21.7123230449834,-7.6164339727042,
0.));
#199071=CARTESIAN_POINT('Ctrl Pts',(-21.7265075407975,-7.61837824030537,
0.));
#199072=CARTESIAN_POINT('Ctrl Pts',(-21.7408548148656,-7.62029941230854,
0.));
#199073=CARTESIAN_POINT('Ctrl Pts',(-21.7553631528328,-7.62219646084228,
0.));
#199074=CARTESIAN_POINT('Ctrl Pts',(-21.7700308755584,-7.62406838181166,
0.));
#199075=CARTESIAN_POINT('Ctrl Pts',(-21.7848563378021,-7.62591419404512,
0.));
#199076=CARTESIAN_POINT('Ctrl Pts',(-21.799837926858,-7.62773293842389,
0.));
#199077=CARTESIAN_POINT('Ctrl Pts',(-21.814974061509,-7.62952367718126,
0.));
#199078=CARTESIAN_POINT('Ctrl Pts',(-21.8302631910195,-7.63128549323022,
0.));
#199079=CARTESIAN_POINT('Ctrl Pts',(-21.8457037941084,-7.63301748948935,
0.));
#199080=CARTESIAN_POINT('Ctrl Pts',(-21.8612943779089,-7.63471878821225,
0.));
#199081=CARTESIAN_POINT('Ctrl Pts',(-21.8770334769496,-7.63638853033399,
0.));
#199082=CARTESIAN_POINT('Ctrl Pts',(-21.8929196523514,-7.63802587492034,
0.));
#199083=CARTESIAN_POINT('Ctrl Pts',(-21.9089514909874,-7.63962999860927,
0.));
#199084=CARTESIAN_POINT('Ctrl Pts',(-21.9251276046546,-7.64120009506531,
0.));
#199085=CARTESIAN_POINT('Ctrl Pts',(-21.9414466292072,-7.64273537442682,
0.));
#199086=CARTESIAN_POINT('Ctrl Pts',(-21.9579072237651,-7.64423506279122,
0.));
#199087=CARTESIAN_POINT('Ctrl Pts',(-21.9745080700798,-7.64569840177335,
0.));
#199088=CARTESIAN_POINT('Ctrl Pts',(-21.9912478718542,-7.64712464805249,
0.));
#199089=CARTESIAN_POINT('Ctrl Pts',(-22.0081253540774,-7.64851307293351,
0.));
#199090=CARTESIAN_POINT('Ctrl Pts',(-22.0251392623209,-7.64986296190168,
0.));
#199091=CARTESIAN_POINT('Ctrl Pts',(-22.0422883621174,-7.65117361421358,
0.));
#199092=CARTESIAN_POINT('Ctrl Pts',(-22.0595714384431,-7.65244434253112,
0.));
#199093=CARTESIAN_POINT('Ctrl Pts',(-22.0769872951596,-7.65367447254949,
0.));
#199094=CARTESIAN_POINT('Ctrl Pts',(-22.094534754469,-7.65486334263643,
0.));
#199095=CARTESIAN_POINT('Ctrl Pts',(-22.1122126563329,-7.65601030346806,
0.));
#199096=CARTESIAN_POINT('Ctrl Pts',(-22.1300198579675,-7.65711471769396,
0.));
#199097=CARTESIAN_POINT('Ctrl Pts',(-22.1479552334211,-7.65817595963349,
0.));
#199098=CARTESIAN_POINT('Ctrl Pts',(-22.1660176731178,-7.6591934149693,
0.));
#199099=CARTESIAN_POINT('Ctrl Pts',(-22.1842060834091,-7.66016648045004,
0.));
#199100=CARTESIAN_POINT('Ctrl Pts',(-22.2025193860964,-7.6610945635927,
0.));
#199101=CARTESIAN_POINT('Ctrl Pts',(-22.2209565180085,-7.66197708240399,
0.));
#199102=CARTESIAN_POINT('Ctrl Pts',(-22.2395164306547,-7.66281346512508,
0.));
#199103=CARTESIAN_POINT('Ctrl Pts',(-22.258198089848,-7.6636031499764,0.));
#199104=CARTESIAN_POINT('Ctrl Pts',(-22.2770004753335,-7.66434558490978,
0.));
#199105=CARTESIAN_POINT('Ctrl Pts',(-22.2959225803937,-7.66504022736298,
0.));
#199106=CARTESIAN_POINT('Ctrl Pts',(-22.314963411484,-7.66568654402493,
0.));
#199107=CARTESIAN_POINT('Ctrl Pts',(-22.3341219879469,-7.66628401061952,
0.));
#199108=CARTESIAN_POINT('Ctrl Pts',(-22.3533973417021,-7.66683211169158,
0.));
#199109=CARTESIAN_POINT('Ctrl Pts',(-22.372788516936,-7.66733034039882,
0.));
#199110=CARTESIAN_POINT('Ctrl Pts',(-22.3922945697773,-7.66777819830789,
0.));
#199111=CARTESIAN_POINT('Ctrl Pts',(-22.4119145679758,-7.66817519519639,
0.));
#199112=CARTESIAN_POINT('Ctrl Pts',(-22.4316475906603,-7.66852084886704,
0.));
#199113=CARTESIAN_POINT('Ctrl Pts',(-22.4514927280855,-7.66881468496634,
0.));
#199114=CARTESIAN_POINT('Ctrl Pts',(-22.47144908137,-7.6690562368083,0.));
#199115=CARTESIAN_POINT('Ctrl Pts',(-22.4915157622312,-7.66924504520314,
0.));
#199116=CARTESIAN_POINT('Ctrl Pts',(-22.5116918927032,-7.66938065829107,
0.));
#199117=CARTESIAN_POINT('Ctrl Pts',(-22.53197660492,-7.66946263138143,0.));
#199118=CARTESIAN_POINT('Ctrl Pts',(-22.5523690409116,-7.66949052679692,
0.));
#199119=CARTESIAN_POINT('Ctrl Pts',(-22.5728683523831,-7.66946391372305,
0.));
#199120=CARTESIAN_POINT('Ctrl Pts',(-22.5934737004953,-7.66938236806232,
0.));
#199121=CARTESIAN_POINT('Ctrl Pts',(-22.6141842556243,-7.66924547229413,
0.));
#199122=CARTESIAN_POINT('Ctrl Pts',(-22.6349991971541,-7.66905281533714,
0.));
#199123=CARTESIAN_POINT('Ctrl Pts',(-22.6559177133127,-7.66880399241322,
0.));
#199124=CARTESIAN_POINT('Ctrl Pts',(-22.6769390009885,-7.66849860491742,
0.));
#199125=CARTESIAN_POINT('Ctrl Pts',(-22.6980622655446,-7.66813626029274,
0.));
#199126=CARTESIAN_POINT('Ctrl Pts',(-22.7192867206245,-7.66771657191027,
0.));
#199127=CARTESIAN_POINT('Ctrl Pts',(-22.7406115879513,-7.66723915895439,
0.));
#199128=CARTESIAN_POINT('Ctrl Pts',(-22.7620360971843,-7.66670364630298,
0.));
#199129=CARTESIAN_POINT('Ctrl Pts',(-22.7835594857699,-7.66610966441272,
0.));
#199130=CARTESIAN_POINT('Ctrl Pts',(-22.8051809987833,-7.66545684920987,
0.));
#199131=CARTESIAN_POINT('Ctrl Pts',(-22.8268998887678,-7.66474484198548,
0.));
#199132=CARTESIAN_POINT('Ctrl Pts',(-22.848715415557,-7.66397328929802,
0.));
#199133=CARTESIAN_POINT('Ctrl Pts',(-22.8706268461283,-7.66314184287336,
0.));
#199134=CARTESIAN_POINT('Ctrl Pts',(-22.8926334544883,-7.66225015950155,
0.));
#199135=CARTESIAN_POINT('Ctrl Pts',(-22.9147345215421,-7.66129790094107,
0.));
#199136=CARTESIAN_POINT('Ctrl Pts',(-22.9369293349593,-7.66028473382777,
0.));
#199137=CARTESIAN_POINT('Ctrl Pts',(-22.959217189033,-7.65921032958901,
0.));
#199138=CARTESIAN_POINT('Ctrl Pts',(-22.9815973845296,-7.65807436436431,
0.));
#199139=CARTESIAN_POINT('Ctrl Pts',(-23.0040692285814,-7.65687651891304,
0.));
#199140=CARTESIAN_POINT('Ctrl Pts',(-23.0266320345787,-7.65561647852533,
0.));
#199141=CARTESIAN_POINT('Ctrl Pts',(-23.0492851220528,-7.65429393293945,
0.));
#199142=CARTESIAN_POINT('Ctrl Pts',(-23.072027816555,-7.65290857626357,
0.));
#199143=CARTESIAN_POINT('Ctrl Pts',(-23.094859449525,-7.65146010690475,
0.));
#199144=CARTESIAN_POINT('Ctrl Pts',(-23.1177793581679,-7.64994822749859,
0.));
#199145=CARTESIAN_POINT('Ctrl Pts',(-23.1407868853819,-7.64837264482942,
0.));
#199146=CARTESIAN_POINT('Ctrl Pts',(-23.1638813796694,-7.64673306975804,
0.));
#199147=CARTESIAN_POINT('Ctrl Pts',(-23.1870621950452,-7.64502921715482,
0.));
#199148=CARTESIAN_POINT('Ctrl Pts',(-23.2103286909398,-7.64326080583679,
0.));
#199149=CARTESIAN_POINT('Ctrl Pts',(-23.2336802320912,-7.64142755851504,
0.));
#199150=CARTESIAN_POINT('Ctrl Pts',(-23.2571161884488,-7.63952920172835,
0.));
#199151=CARTESIAN_POINT('Ctrl Pts',(-23.2806359350855,-7.63756546576374,
0.));
#199152=CARTESIAN_POINT('Ctrl Pts',(-23.3042388521022,-7.63553608458782,
0.));
#199153=CARTESIAN_POINT('Ctrl Pts',(-23.3279243245241,-7.63344079578161,
0.));
#199154=CARTESIAN_POINT('Ctrl Pts',(-23.3516917421972,-7.63127934048136,
0.));
#199155=CARTESIAN_POINT('Ctrl Pts',(-23.3755404996636,-7.62905146332592,
0.));
#199156=CARTESIAN_POINT('Ctrl Pts',(-23.399469996112,-7.62675691240328,
0.));
#199157=CARTESIAN_POINT('Ctrl Pts',(-23.4234796353542,-7.62439543920049,
0.));
#199158=CARTESIAN_POINT('Ctrl Pts',(-23.4475688257854,-7.62196679855954,
0.));
#199159=CARTESIAN_POINT('Ctrl Pts',(-23.4717369803438,-7.61947074863976,
0.));
#199160=CARTESIAN_POINT('Ctrl Pts',(-23.4959835164609,-7.61690705088318,
0.));
#199161=CARTESIAN_POINT('Ctrl Pts',(-23.5203078560129,-7.61427546999297,
0.));
#199162=CARTESIAN_POINT('Ctrl Pts',(-23.544709425203,-7.61157577385371,
0.));
#199163=CARTESIAN_POINT('Ctrl Pts',(-23.5691876544244,-7.60880773344599,
0.));
#199164=CARTESIAN_POINT('Ctrl Pts',(-23.5937419781245,-7.60597112277093,
0.));
#199165=CARTESIAN_POINT('Ctrl Pts',(-23.6183718346576,-7.60306571877805,
0.));
#199166=CARTESIAN_POINT('Ctrl Pts',(-23.6430766661418,-7.60009130130125,
0.));
#199167=CARTESIAN_POINT('Ctrl Pts',(-23.6678559182875,-7.59704765299566,
0.));
#199168=CARTESIAN_POINT('Ctrl Pts',(-23.6927090405066,-7.59393455934034,
0.));
#199169=CARTESIAN_POINT('Ctrl Pts',(-23.7176354860457,-7.5907518086532,
0.));
#199170=CARTESIAN_POINT('Ctrl Pts',(-23.7426347121006,-7.58749919210825,
0.));
#199171=CARTESIAN_POINT('Ctrl Pts',(-23.7677061799376,-7.5841765037627,
0.));
#199172=CARTESIAN_POINT('Ctrl Pts',(-23.7928493549908,-7.58078354058212,
0.));
#199173=CARTESIAN_POINT('Ctrl Pts',(-23.8180637069976,-7.57732010249065,
0.));
#199174=CARTESIAN_POINT('Ctrl Pts',(-23.8433487096132,-7.57378599219814,
0.));
#199175=CARTESIAN_POINT('Ctrl Pts',(-23.8687038399595,-7.57018101500709,
0.));
#199176=CARTESIAN_POINT('Ctrl Pts',(-23.8941285782002,-7.5665049786379,
0.));
#199177=CARTESIAN_POINT('Ctrl Pts',(-23.9196224070759,-7.56275769304772,
0.));
#199178=CARTESIAN_POINT('Ctrl Pts',(-23.9451848115002,-7.55893897027679,
0.));
#199179=CARTESIAN_POINT('Ctrl Pts',(-23.9708152779886,-7.55504862424807,
0.));
#199180=CARTESIAN_POINT('Ctrl Pts',(-23.9965132953187,-7.55108647097431,
0.));
#199181=CARTESIAN_POINT('Ctrl Pts',(-24.0222783554531,-7.54705232885894,
0.));
#199182=CARTESIAN_POINT('Ctrl Pts',(-24.0481099543353,-7.54294601896127,
0.));
#199183=CARTESIAN_POINT('Ctrl Pts',(-24.0740075927984,-7.53876736531004,
0.));
#199184=CARTESIAN_POINT('Ctrl Pts',(-24.0999707772643,-7.53451619514658,
0.));
#199185=CARTESIAN_POINT('Ctrl Pts',(-24.1259990209211,-7.53019233935536,
0.));
#199186=CARTESIAN_POINT('Ctrl Pts',(-24.152091842537,-7.52579563201478,
0.));
#199187=CARTESIAN_POINT('Ctrl Pts',(-24.1782487641602,-7.52132590953862,
0.));
#199188=CARTESIAN_POINT('Ctrl Pts',(-24.2044693092356,-7.51678300997997,
0.));
#199189=CARTESIAN_POINT('Ctrl Pts',(-24.230753000389,-7.51216677222198,
0.));
#199190=CARTESIAN_POINT('Ctrl Pts',(-24.2570993577032,-7.50747703535114,
0.));
#199191=CARTESIAN_POINT('Ctrl Pts',(-24.2835078958966,-7.50271363765098,
0.));
#199192=CARTESIAN_POINT('Ctrl Pts',(-24.3099781253345,-7.49787641695358,
0.));
#199193=CARTESIAN_POINT('Ctrl Pts',(-24.3365095573673,-7.49296521252329,
0.));
#199194=CARTESIAN_POINT('Ctrl Pts',(-24.3631017084513,-7.48797986651827,
0.));
#199195=CARTESIAN_POINT('Ctrl Pts',(-24.3897541049248,-7.48292022569253,
0.));
#199196=CARTESIAN_POINT('Ctrl Pts',(-24.4164662871165,-7.47778614286573,
0.));
#199197=CARTESIAN_POINT('Ctrl Pts',(-24.4432378146501,-7.47257747883318,
0.));
#199198=CARTESIAN_POINT('Ctrl Pts',(-24.4700682684544,-7.46729410308922,
0.));
#199199=CARTESIAN_POINT('Ctrl Pts',(-24.4969572391509,-7.46193588961641,
0.));
#199200=CARTESIAN_POINT('Ctrl Pts',(-24.52390431731,-7.45650271336045,0.));
#199201=CARTESIAN_POINT('Ctrl Pts',(-24.5509090831579,-7.45099444651295,
0.));
#199202=CARTESIAN_POINT('Ctrl Pts',(-24.5779710960865,-7.44541095473162,
0.));
#199203=CARTESIAN_POINT('Ctrl Pts',(-24.6050898852349,-7.43975209375374,
0.));
#199204=CARTESIAN_POINT('Ctrl Pts',(-24.6322649369472,-7.4340177048922,
0.));
#199205=CARTESIAN_POINT('Ctrl Pts',(-24.659495712869,-7.4282076215868,0.));
#199206=CARTESIAN_POINT('Ctrl Pts',(-24.6867816727118,-7.42232167765762,
0.));
#199207=CARTESIAN_POINT('Ctrl Pts',(-24.7141222949988,-7.41635971481243,
0.));
#199208=CARTESIAN_POINT('Ctrl Pts',(-24.7415170994754,-7.41032159082173,
0.));
#199209=CARTESIAN_POINT('Ctrl Pts',(-24.7689656669005,-7.40420718661754,
0.));
#199210=CARTESIAN_POINT('Ctrl Pts',(-24.7964676646518,-7.39801641583612,
0.));
#199211=CARTESIAN_POINT('Ctrl Pts',(-24.8240228521042,-7.39174922586841,
0.));
#199212=CARTESIAN_POINT('Ctrl Pts',(-24.8516310625367,-7.38540558904945,
0.));
#199213=CARTESIAN_POINT('Ctrl Pts',(-24.8792921911309,-7.3789854964161,
0.));
#199214=CARTESIAN_POINT('Ctrl Pts',(-24.9014633826201,-7.37378825962717,
0.));
#199215=CARTESIAN_POINT('Ctrl Pts',(-24.9181155530631,-7.36985593120696,
0.));
#199216=CARTESIAN_POINT('Ctrl Pts',(-24.9292275670705,-7.36721909029059,
0.));
#199217=CARTESIAN_POINT('Ctrl Pts',(-24.9347862158358,-7.36589684767343,
0.));
#199218=CARTESIAN_POINT('',(-24.9347862158358,-7.36589684767343,0.));
#199219=CARTESIAN_POINT('Origin',(-21.4341755315424,-1.68110656504246,0.));
#199220=CARTESIAN_POINT('',(-22.4835757167854,-1.76341220531179,0.));
#199221=CARTESIAN_POINT('',(-22.4835757167854,-1.76341220531179,0.));
#199222=CARTESIAN_POINT('',(-10.7170877657712,-0.840553282521227,0.));
#199223=CARTESIAN_POINT('Ctrl Pts',(-25.2771067246846,-6.08833931617698,
0.));
#199224=CARTESIAN_POINT('Ctrl Pts',(-25.2771067246846,-6.08833931617698,
12.));
#199225=CARTESIAN_POINT('Ctrl Pts',(-25.2729539149479,-6.08441489609824,
0.));
#199226=CARTESIAN_POINT('Ctrl Pts',(-25.2729539149479,-6.08441489609824,
12.));
#199227=CARTESIAN_POINT('Ctrl Pts',(-25.2646490489816,-6.07657531787577,
0.));
#199228=CARTESIAN_POINT('Ctrl Pts',(-25.2646490489816,-6.07657531787577,
12.));
#199229=CARTESIAN_POINT('Ctrl Pts',(-25.2521940105523,-6.06484373634696,
0.));
#199230=CARTESIAN_POINT('Ctrl Pts',(-25.2521940105523,-6.06484373634696,
12.));
#199231=CARTESIAN_POINT('Ctrl Pts',(-25.2355918138798,-6.04925720151412,
0.));
#199232=CARTESIAN_POINT('Ctrl Pts',(-25.2355918138798,-6.04925720151412,
12.));
#199233=CARTESIAN_POINT('Ctrl Pts',(-25.2148466201368,-6.02986667390187,
0.));
#199234=CARTESIAN_POINT('Ctrl Pts',(-25.2148466201368,-6.02986667390187,
12.));
#199235=CARTESIAN_POINT('Ctrl Pts',(-25.1941090269638,-6.0105688180476,
0.));
#199236=CARTESIAN_POINT('Ctrl Pts',(-25.1941090269638,-6.0105688180476,
12.));
#199237=CARTESIAN_POINT('Ctrl Pts',(-25.1733791296154,-5.99136367859838,
0.));
#199238=CARTESIAN_POINT('Ctrl Pts',(-25.1733791296154,-5.99136367859838,
12.));
#199239=CARTESIAN_POINT('Ctrl Pts',(-25.1526570863065,-5.97225131495636,
0.));
#199240=CARTESIAN_POINT('Ctrl Pts',(-25.1526570863065,-5.97225131495636,
12.));
#199241=CARTESIAN_POINT('Ctrl Pts',(-25.1319431317273,-5.95323180187348,
0.));
#199242=CARTESIAN_POINT('Ctrl Pts',(-25.1319431317273,-5.95323180187348,
12.));
#199243=CARTESIAN_POINT('Ctrl Pts',(-25.1112375971182,-5.93430523086776,
0.));
#199244=CARTESIAN_POINT('Ctrl Pts',(-25.1112375971182,-5.93430523086776,
12.));
#199245=CARTESIAN_POINT('Ctrl Pts',(-25.0905409050863,-5.91547170844382,
0.));
#199246=CARTESIAN_POINT('Ctrl Pts',(-25.0905409050863,-5.91547170844382,
12.));
#199247=CARTESIAN_POINT('Ctrl Pts',(-25.0698535426593,-5.89673135155459,
0.));
#199248=CARTESIAN_POINT('Ctrl Pts',(-25.0698535426593,-5.89673135155459,
12.));
#199249=CARTESIAN_POINT('Ctrl Pts',(-25.0491760405965,-5.87808428385329,
0.));
#199250=CARTESIAN_POINT('Ctrl Pts',(-25.0491760405965,-5.87808428385329,
12.));
#199251=CARTESIAN_POINT('Ctrl Pts',(-25.0285089498922,-5.8595306315681,
0.));
#199252=CARTESIAN_POINT('Ctrl Pts',(-25.0285089498922,-5.8595306315681,
12.));
#199253=CARTESIAN_POINT('Ctrl Pts',(-25.0078528200558,-5.84107051963073,
0.));
#199254=CARTESIAN_POINT('Ctrl Pts',(-25.0078528200558,-5.84107051963073,
12.));
#199255=CARTESIAN_POINT('Ctrl Pts',(-24.9872081752709,-5.82270406744214,
0.));
#199256=CARTESIAN_POINT('Ctrl Pts',(-24.9872081752709,-5.82270406744214,
12.));
#199257=CARTESIAN_POINT('Ctrl Pts',(-24.9665754954462,-5.80443138549747,
0.));
#199258=CARTESIAN_POINT('Ctrl Pts',(-24.9665754954462,-5.80443138549747,
12.));
#199259=CARTESIAN_POINT('Ctrl Pts',(-24.9459552293308,-5.78625257775703,
0.));
#199260=CARTESIAN_POINT('Ctrl Pts',(-24.9459552293308,-5.78625257775703,
12.));
#199261=CARTESIAN_POINT('Ctrl Pts',(-24.9253478043632,-5.76816774342236,
0.));
#199262=CARTESIAN_POINT('Ctrl Pts',(-24.9253478043632,-5.76816774342236,
12.));
#199263=CARTESIAN_POINT('Ctrl Pts',(-24.9047536376467,-5.75017697890813,
0.));
#199264=CARTESIAN_POINT('Ctrl Pts',(-24.9047536376467,-5.75017697890813,
12.));
#199265=CARTESIAN_POINT('Ctrl Pts',(-24.8841731467219,-5.73228037976926,
0.));
#199266=CARTESIAN_POINT('Ctrl Pts',(-24.8841731467219,-5.73228037976926,
12.));
#199267=CARTESIAN_POINT('Ctrl Pts',(-24.8636067597677,-5.71447804252019,
0.));
#199268=CARTESIAN_POINT('Ctrl Pts',(-24.8636067597677,-5.71447804252019,
12.));
#199269=CARTESIAN_POINT('Ctrl Pts',(-24.8430549277634,-5.69677006679429,
0.));
#199270=CARTESIAN_POINT('Ctrl Pts',(-24.8430549277634,-5.69677006679429,
12.));
#199271=CARTESIAN_POINT('Ctrl Pts',(-24.822518122386,-5.67915655496524,
0.));
#199272=CARTESIAN_POINT('Ctrl Pts',(-24.822518122386,-5.67915655496524,
12.));
#199273=CARTESIAN_POINT('Ctrl Pts',(-24.8019968304618,-5.66163761114903,
0.));
#199274=CARTESIAN_POINT('Ctrl Pts',(-24.8019968304618,-5.66163761114903,
12.));
#199275=CARTESIAN_POINT('Ctrl Pts',(-24.7814915496728,-5.64421334042247,
0.));
#199276=CARTESIAN_POINT('Ctrl Pts',(-24.7814915496728,-5.64421334042247,
12.));
#199277=CARTESIAN_POINT('Ctrl Pts',(-24.76100278357,-5.62688384790919,0.));
#199278=CARTESIAN_POINT('Ctrl Pts',(-24.76100278357,-5.62688384790919,12.));
#199279=CARTESIAN_POINT('Ctrl Pts',(-24.7405310372736,-5.60964923798495,
0.));
#199280=CARTESIAN_POINT('Ctrl Pts',(-24.7405310372736,-5.60964923798495,
12.));
#199281=CARTESIAN_POINT('Ctrl Pts',(-24.7200768119079,-5.59250961323995,
0.));
#199282=CARTESIAN_POINT('Ctrl Pts',(-24.7200768119079,-5.59250961323995,
12.));
#199283=CARTESIAN_POINT('Ctrl Pts',(-24.6996406035507,-5.57546507427766,
0.));
#199284=CARTESIAN_POINT('Ctrl Pts',(-24.6996406035507,-5.57546507427766,
12.));
#199285=CARTESIAN_POINT('Ctrl Pts',(-24.6792229061785,-5.55851572025389,
0.));
#199286=CARTESIAN_POINT('Ctrl Pts',(-24.6792229061785,-5.55851572025389,
12.));
#199287=CARTESIAN_POINT('Ctrl Pts',(-24.6588242134733,-5.54166164919593,
0.));
#199288=CARTESIAN_POINT('Ctrl Pts',(-24.6588242134733,-5.54166164919593,
12.));
#199289=CARTESIAN_POINT('Ctrl Pts',(-24.6384450211466,-5.52490295840996,
0.));
#199290=CARTESIAN_POINT('Ctrl Pts',(-24.6384450211466,-5.52490295840996,
12.));
#199291=CARTESIAN_POINT('Ctrl Pts',(-24.618085828918,-5.50823974481959,
0.));
#199292=CARTESIAN_POINT('Ctrl Pts',(-24.618085828918,-5.50823974481959,
12.));
#199293=CARTESIAN_POINT('Ctrl Pts',(-24.5977471429365,-5.49167210537235,
0.));
#199294=CARTESIAN_POINT('Ctrl Pts',(-24.5977471429365,-5.49167210537235,
12.));
#199295=CARTESIAN_POINT('Ctrl Pts',(-24.5774294770329,-5.47520013724403,
0.));
#199296=CARTESIAN_POINT('Ctrl Pts',(-24.5774294770329,-5.47520013724403,
12.));
#199297=CARTESIAN_POINT('Ctrl Pts',(-24.5571333514841,-5.45882393762244,
0.));
#199298=CARTESIAN_POINT('Ctrl Pts',(-24.5571333514841,-5.45882393762244,
12.));
#199299=CARTESIAN_POINT('Ctrl Pts',(-24.5368592922861,-5.44254360356865,
0.));
#199300=CARTESIAN_POINT('Ctrl Pts',(-24.5368592922861,-5.44254360356865,
12.));
#199301=CARTESIAN_POINT('Ctrl Pts',(-24.5166078302107,-5.42635923183411,
0.));
#199302=CARTESIAN_POINT('Ctrl Pts',(-24.5166078302107,-5.42635923183411,
12.));
#199303=CARTESIAN_POINT('Ctrl Pts',(-24.4963794999831,-5.41027091869242,
0.));
#199304=CARTESIAN_POINT('Ctrl Pts',(-24.4963794999831,-5.41027091869242,
12.));
#199305=CARTESIAN_POINT('Ctrl Pts',(-24.4761748393322,-5.3942787597383,
0.));
#199306=CARTESIAN_POINT('Ctrl Pts',(-24.4761748393322,-5.3942787597383,
12.));
#199307=CARTESIAN_POINT('Ctrl Pts',(-24.4559943883159,-5.37838284973706,
0.));
#199308=CARTESIAN_POINT('Ctrl Pts',(-24.4559943883159,-5.37838284973706,
12.));
#199309=CARTESIAN_POINT('Ctrl Pts',(-24.4358386899152,-5.36258328273639,
0.));
#199310=CARTESIAN_POINT('Ctrl Pts',(-24.4358386899152,-5.36258328273639,
12.));
#199311=CARTESIAN_POINT('Ctrl Pts',(-24.4157082904615,-5.34688015213546,
0.));
#199312=CARTESIAN_POINT('Ctrl Pts',(-24.4157082904615,-5.34688015213546,
12.));
#199313=CARTESIAN_POINT('Ctrl Pts',(-24.3956037401293,-5.33127355076036,
0.));
#199314=CARTESIAN_POINT('Ctrl Pts',(-24.3956037401293,-5.33127355076036,
12.));
#199315=CARTESIAN_POINT('Ctrl Pts',(-24.3755255933917,-5.31576357092524,
0.));
#199316=CARTESIAN_POINT('Ctrl Pts',(-24.3755255933917,-5.31576357092524,
12.));
#199317=CARTESIAN_POINT('Ctrl Pts',(-24.3554744095075,-5.30035030449058,
0.));
#199318=CARTESIAN_POINT('Ctrl Pts',(-24.3554744095075,-5.30035030449058,
12.));
#199319=CARTESIAN_POINT('Ctrl Pts',(-24.3354507529415,-5.28503384290644,
0.));
#199320=CARTESIAN_POINT('Ctrl Pts',(-24.3354507529415,-5.28503384290644,
12.));
#199321=CARTESIAN_POINT('Ctrl Pts',(-24.3154551932222,-5.26981427718796,
0.));
#199322=CARTESIAN_POINT('Ctrl Pts',(-24.3154551932222,-5.26981427718796,
12.));
#199323=CARTESIAN_POINT('Ctrl Pts',(-24.2954883048448,-5.25469169788856,
0.));
#199324=CARTESIAN_POINT('Ctrl Pts',(-24.2954883048448,-5.25469169788856,
12.));
#199325=CARTESIAN_POINT('Ctrl Pts',(-24.2755506671526,-5.23966619506289,
0.));
#199326=CARTESIAN_POINT('Ctrl Pts',(-24.2755506671526,-5.23966619506289,
12.));
#199327=CARTESIAN_POINT('Ctrl Pts',(-24.2556428642294,-5.22473785822441,
0.));
#199328=CARTESIAN_POINT('Ctrl Pts',(-24.2556428642294,-5.22473785822441,
12.));
#199329=CARTESIAN_POINT('Ctrl Pts',(-24.2357654847765,-5.20990677629173,
0.));
#199330=CARTESIAN_POINT('Ctrl Pts',(-24.2357654847765,-5.20990677629173,
12.));
#199331=CARTESIAN_POINT('Ctrl Pts',(-24.215919122017,-5.19517303753643,
0.));
#199332=CARTESIAN_POINT('Ctrl Pts',(-24.215919122017,-5.19517303753643,
12.));
#199333=CARTESIAN_POINT('Ctrl Pts',(-24.1961043738754,-5.18053672961392,
0.));
#199334=CARTESIAN_POINT('Ctrl Pts',(-24.1961043738754,-5.18053672961392,
12.));
#199335=CARTESIAN_POINT('Ctrl Pts',(-24.1763218431343,-5.16599793957979,
0.));
#199336=CARTESIAN_POINT('Ctrl Pts',(-24.1763218431343,-5.16599793957979,
12.));
#199337=CARTESIAN_POINT('Ctrl Pts',(-24.156572137597,-5.15155675390075,
0.));
#199338=CARTESIAN_POINT('Ctrl Pts',(-24.156572137597,-5.15155675390075,
12.));
#199339=CARTESIAN_POINT('Ctrl Pts',(-24.1368558702443,-5.13721325845744,
0.));
#199340=CARTESIAN_POINT('Ctrl Pts',(-24.1368558702443,-5.13721325845744,
12.));
#199341=CARTESIAN_POINT('Ctrl Pts',(-24.117173659394,-5.12296753853859,
0.));
#199342=CARTESIAN_POINT('Ctrl Pts',(-24.117173659394,-5.12296753853859,
12.));
#199343=CARTESIAN_POINT('Ctrl Pts',(-24.0975261288446,-5.10881967883132,
0.));
#199344=CARTESIAN_POINT('Ctrl Pts',(-24.0975261288446,-5.10881967883132,
12.));
#199345=CARTESIAN_POINT('Ctrl Pts',(-24.0779139079266,-5.09476976342625,
0.));
#199346=CARTESIAN_POINT('Ctrl Pts',(-24.0779139079266,-5.09476976342625,
12.));
#199347=CARTESIAN_POINT('Ctrl Pts',(-24.0583376315638,-5.08081787581276,
0.));
#199348=CARTESIAN_POINT('Ctrl Pts',(-24.0583376315638,-5.08081787581276,
12.));
#199349=CARTESIAN_POINT('Ctrl Pts',(-24.0387979403268,-5.06696409886641,
0.));
#199350=CARTESIAN_POINT('Ctrl Pts',(-24.0387979403268,-5.06696409886641,
12.));
#199351=CARTESIAN_POINT('Ctrl Pts',(-24.0192954804896,-5.05320851483065,
0.));
#199352=CARTESIAN_POINT('Ctrl Pts',(-24.0192954804896,-5.05320851483065,
12.));
#199353=CARTESIAN_POINT('Ctrl Pts',(-23.9998309040746,-5.03955120528521,
0.));
#199354=CARTESIAN_POINT('Ctrl Pts',(-23.9998309040746,-5.03955120528521,
12.));
#199355=CARTESIAN_POINT('Ctrl Pts',(-23.9804048689227,-5.02599225112454,
0.));
#199356=CARTESIAN_POINT('Ctrl Pts',(-23.9804048689227,-5.02599225112454,
12.));
#199357=CARTESIAN_POINT('Ctrl Pts',(-23.9610180388271,-5.01253173257453,
0.));
#199358=CARTESIAN_POINT('Ctrl Pts',(-23.9610180388271,-5.01253173257453,
12.));
#199359=CARTESIAN_POINT('Ctrl Pts',(-23.9416710836529,-4.99916972919306,
0.));
#199360=CARTESIAN_POINT('Ctrl Pts',(-23.9416710836529,-4.99916972919306,
12.));
#199361=CARTESIAN_POINT('Ctrl Pts',(-23.9223646794592,-4.98590631986532,
0.));
#199362=CARTESIAN_POINT('Ctrl Pts',(-23.9223646794592,-4.98590631986532,
12.));
#199363=CARTESIAN_POINT('Ctrl Pts',(-23.9030995086163,-4.97274158279226,
0.));
#199364=CARTESIAN_POINT('Ctrl Pts',(-23.9030995086163,-4.97274158279226,
12.));
#199365=CARTESIAN_POINT('Ctrl Pts',(-23.8838762599218,-4.9596755954656,
0.));
#199366=CARTESIAN_POINT('Ctrl Pts',(-23.8838762599218,-4.9596755954656,
12.));
#199367=CARTESIAN_POINT('Ctrl Pts',(-23.8646956287168,-4.9467084346586,
0.));
#199368=CARTESIAN_POINT('Ctrl Pts',(-23.8646956287168,-4.9467084346586,
12.));
#199369=CARTESIAN_POINT('Ctrl Pts',(-23.8455583170057,-4.93384017643432,
0.));
#199370=CARTESIAN_POINT('Ctrl Pts',(-23.8455583170057,-4.93384017643432,
12.));
#199371=CARTESIAN_POINT('Ctrl Pts',(-23.8264650335717,-4.92107089613969,
0.));
#199372=CARTESIAN_POINT('Ctrl Pts',(-23.8264650335717,-4.92107089613969,
12.));
#199373=CARTESIAN_POINT('Ctrl Pts',(-23.8074164940896,-4.90840066839344,
0.));
#199374=CARTESIAN_POINT('Ctrl Pts',(-23.8074164940896,-4.90840066839344,
12.));
#199375=CARTESIAN_POINT('Ctrl Pts',(-23.7884134212384,-4.89582956706775,
0.));
#199376=CARTESIAN_POINT('Ctrl Pts',(-23.7884134212384,-4.89582956706775,
12.));
#199377=CARTESIAN_POINT('Ctrl Pts',(-23.7694565448049,-4.88335766525573,
0.));
#199378=CARTESIAN_POINT('Ctrl Pts',(-23.7694565448049,-4.88335766525573,
12.));
#199379=CARTESIAN_POINT('Ctrl Pts',(-23.7505466018245,-4.87098503527152,
0.));
#199380=CARTESIAN_POINT('Ctrl Pts',(-23.7505466018245,-4.87098503527152,
12.));
#199381=CARTESIAN_POINT('Ctrl Pts',(-23.7316843367313,-4.85871174865499,
0.));
#199382=CARTESIAN_POINT('Ctrl Pts',(-23.7316843367313,-4.85871174865499,
12.));
#199383=CARTESIAN_POINT('Ctrl Pts',(-23.7128705015017,-4.84653787616425,
0.));
#199384=CARTESIAN_POINT('Ctrl Pts',(-23.7128705015017,-4.84653787616425,
12.));
#199385=CARTESIAN_POINT('Ctrl Pts',(-23.6941058557971,-4.83446348776265,
0.));
#199386=CARTESIAN_POINT('Ctrl Pts',(-23.6941058557971,-4.83446348776265,
12.));
#199387=CARTESIAN_POINT('Ctrl Pts',(-23.675391167102,-4.82248865259562,
0.));
#199388=CARTESIAN_POINT('Ctrl Pts',(-23.675391167102,-4.82248865259562,
12.));
#199389=CARTESIAN_POINT('Ctrl Pts',(-23.6567272108628,-4.81061343896432,
0.));
#199390=CARTESIAN_POINT('Ctrl Pts',(-23.6567272108628,-4.81061343896432,
12.));
#199391=CARTESIAN_POINT('Ctrl Pts',(-23.6381147706579,-4.7988379143322,
0.));
#199392=CARTESIAN_POINT('Ctrl Pts',(-23.6381147706579,-4.7988379143322,
12.));
#199393=CARTESIAN_POINT('Ctrl Pts',(-23.6195546383624,-4.78716214532098,
0.));
#199394=CARTESIAN_POINT('Ctrl Pts',(-23.6195546383624,-4.78716214532098,
12.));
#199395=CARTESIAN_POINT('Ctrl Pts',(-23.6010476143099,-4.77558619769872,
0.));
#199396=CARTESIAN_POINT('Ctrl Pts',(-23.6010476143099,-4.77558619769872,
12.));
#199397=CARTESIAN_POINT('Ctrl Pts',(-23.5825945074535,-4.76411013636251,
0.));
#199398=CARTESIAN_POINT('Ctrl Pts',(-23.5825945074535,-4.76411013636251,
12.));
#199399=CARTESIAN_POINT('Ctrl Pts',(-23.5641961355168,-4.75273402530617,
0.));
#199400=CARTESIAN_POINT('Ctrl Pts',(-23.5641961355168,-4.75273402530617,
12.));
#199401=CARTESIAN_POINT('Ctrl Pts',(-23.545853325171,-4.74145792760698,
0.));
#199402=CARTESIAN_POINT('Ctrl Pts',(-23.545853325171,-4.74145792760698,
12.));
#199403=CARTESIAN_POINT('Ctrl Pts',(-23.5275669122372,-4.7302819054303,
0.));
#199404=CARTESIAN_POINT('Ctrl Pts',(-23.5275669122372,-4.7302819054303,
12.));
#199405=CARTESIAN_POINT('Ctrl Pts',(-23.509337741878,-4.71920602001901,
0.));
#199406=CARTESIAN_POINT('Ctrl Pts',(-23.509337741878,-4.71920602001901,
12.));
#199407=CARTESIAN_POINT('Ctrl Pts',(-23.491166668789,-4.70823033167818,
0.));
#199408=CARTESIAN_POINT('Ctrl Pts',(-23.491166668789,-4.70823033167818,
12.));
#199409=CARTESIAN_POINT('Ctrl Pts',(-23.4730545573853,-4.69735489975024,
0.));
#199410=CARTESIAN_POINT('Ctrl Pts',(-23.4730545573853,-4.69735489975024,
12.));
#199411=CARTESIAN_POINT('Ctrl Pts',(-23.455002281986,-4.68657978258303,
0.));
#199412=CARTESIAN_POINT('Ctrl Pts',(-23.455002281986,-4.68657978258303,
12.));
#199413=CARTESIAN_POINT('Ctrl Pts',(-23.4370107270451,-4.67590503753058,
0.));
#199414=CARTESIAN_POINT('Ctrl Pts',(-23.4370107270451,-4.67590503753058,
12.));
#199415=CARTESIAN_POINT('Ctrl Pts',(-23.4190807873803,-4.6653307209467,
0.));
#199416=CARTESIAN_POINT('Ctrl Pts',(-23.4190807873803,-4.6653307209467,
12.));
#199417=CARTESIAN_POINT('Ctrl Pts',(-23.4012133683959,-4.65485688816924,
0.));
#199418=CARTESIAN_POINT('Ctrl Pts',(-23.4012133683959,-4.65485688816924,
12.));
#199419=CARTESIAN_POINT('Ctrl Pts',(-23.3834093863068,-4.6444835934993,
0.));
#199420=CARTESIAN_POINT('Ctrl Pts',(-23.3834093863068,-4.6444835934993,
12.));
#199421=CARTESIAN_POINT('Ctrl Pts',(-23.3656697683489,-4.63421089016541,
0.));
#199422=CARTESIAN_POINT('Ctrl Pts',(-23.3656697683489,-4.63421089016541,
12.));
#199423=CARTESIAN_POINT('Ctrl Pts',(-23.3479954530272,-4.62403883030805,
0.));
#199424=CARTESIAN_POINT('Ctrl Pts',(-23.3479954530272,-4.62403883030805,
12.));
#199425=CARTESIAN_POINT('Ctrl Pts',(-23.3303873903938,-4.6139674649783,
0.));
#199426=CARTESIAN_POINT('Ctrl Pts',(-23.3303873903938,-4.6139674649783,
12.));
#199427=CARTESIAN_POINT('Ctrl Pts',(-23.3128465423115,-4.60399684412163,
0.));
#199428=CARTESIAN_POINT('Ctrl Pts',(-23.3128465423115,-4.60399684412163,
12.));
#199429=CARTESIAN_POINT('Ctrl Pts',(-23.2953738827191,-4.5941270165575,
0.));
#199430=CARTESIAN_POINT('Ctrl Pts',(-23.2953738827191,-4.5941270165575,
12.));
#199431=CARTESIAN_POINT('Ctrl Pts',(-23.2779703978876,-4.5843580299469,
0.));
#199432=CARTESIAN_POINT('Ctrl Pts',(-23.2779703978876,-4.5843580299469,
12.));
#199433=CARTESIAN_POINT('Ctrl Pts',(-23.2606370866866,-4.57468993076097,
0.));
#199434=CARTESIAN_POINT('Ctrl Pts',(-23.2606370866866,-4.57468993076097,
12.));
#199435=CARTESIAN_POINT('Ctrl Pts',(-23.2433749609131,-4.56512276427839,
0.));
#199436=CARTESIAN_POINT('Ctrl Pts',(-23.2433749609131,-4.56512276427839,
12.));
#199437=CARTESIAN_POINT('Ctrl Pts',(-23.2261850456064,-4.55565657456975,
0.));
#199438=CARTESIAN_POINT('Ctrl Pts',(-23.2261850456064,-4.55565657456975,
12.));
#199439=CARTESIAN_POINT('Ctrl Pts',(-23.2090683793629,-4.54629140447544,
0.));
#199440=CARTESIAN_POINT('Ctrl Pts',(-23.2090683793629,-4.54629140447544,
12.));
#199441=CARTESIAN_POINT('Ctrl Pts',(-23.1920260146465,-4.53702729557566,
0.));
#199442=CARTESIAN_POINT('Ctrl Pts',(-23.1920260146465,-4.53702729557566,
12.));
#199443=CARTESIAN_POINT('Ctrl Pts',(-23.1750590180908,-4.52786428815014,
0.));
#199444=CARTESIAN_POINT('Ctrl Pts',(-23.1750590180908,-4.52786428815014,
12.));
#199445=CARTESIAN_POINT('Ctrl Pts',(-23.1581684708761,-4.51880242116748,
0.));
#199446=CARTESIAN_POINT('Ctrl Pts',(-23.1581684708761,-4.51880242116748,
12.));
#199447=CARTESIAN_POINT('Ctrl Pts',(-23.1413554691123,-4.5098417322706,
0.));
#199448=CARTESIAN_POINT('Ctrl Pts',(-23.1413554691123,-4.5098417322706,
12.));
#199449=CARTESIAN_POINT('Ctrl Pts',(-23.1246211242115,-4.50098225775171,
0.));
#199450=CARTESIAN_POINT('Ctrl Pts',(-23.1246211242115,-4.50098225775171,
12.));
#199451=CARTESIAN_POINT('Ctrl Pts',(-23.1079665632636,-4.49222403252216,
0.));
#199452=CARTESIAN_POINT('Ctrl Pts',(-23.1079665632636,-4.49222403252216,
12.));
#199453=CARTESIAN_POINT('Ctrl Pts',(-23.0913929293922,-4.48356709006788,
0.));
#199454=CARTESIAN_POINT('Ctrl Pts',(-23.0913929293922,-4.48356709006788,
12.));
#199455=CARTESIAN_POINT('Ctrl Pts',(-23.0749013821881,-4.47501146242856,
0.));
#199456=CARTESIAN_POINT('Ctrl Pts',(-23.0749013821881,-4.47501146242856,
12.));
#199457=CARTESIAN_POINT('Ctrl Pts',(-23.0584930981732,-4.4665571801823,
0.));
#199458=CARTESIAN_POINT('Ctrl Pts',(-23.0584930981732,-4.4665571801823,
12.));
#199459=CARTESIAN_POINT('Ctrl Pts',(-23.0421692712467,-4.45820427241683,
0.));
#199460=CARTESIAN_POINT('Ctrl Pts',(-23.0421692712467,-4.45820427241683,
12.));
#199461=CARTESIAN_POINT('Ctrl Pts',(-23.0259311131392,-4.44995276669686,
0.));
#199462=CARTESIAN_POINT('Ctrl Pts',(-23.0259311131392,-4.44995276669686,
12.));
#199463=CARTESIAN_POINT('Ctrl Pts',(-23.0097798538395,-4.44180268901643,
0.));
#199464=CARTESIAN_POINT('Ctrl Pts',(-23.0097798538395,-4.44180268901643,
12.));
#199465=CARTESIAN_POINT('Ctrl Pts',(-22.9937167421006,-4.43375406376879,
0.));
#199466=CARTESIAN_POINT('Ctrl Pts',(-22.9937167421006,-4.43375406376879,
12.));
#199467=CARTESIAN_POINT('Ctrl Pts',(-22.977743046002,-4.42580691372751,
0.));
#199468=CARTESIAN_POINT('Ctrl Pts',(-22.977743046002,-4.42580691372751,
12.));
#199469=CARTESIAN_POINT('Ctrl Pts',(-22.9618600534866,-4.41796126001302,
0.));
#199470=CARTESIAN_POINT('Ctrl Pts',(-22.9618600534866,-4.41796126001302,
12.));
#199471=CARTESIAN_POINT('Ctrl Pts',(-22.9460690729093,-4.41021712205553,
0.));
#199472=CARTESIAN_POINT('Ctrl Pts',(-22.9460690729093,-4.41021712205553,
12.));
#199473=CARTESIAN_POINT('Ctrl Pts',(-22.930371433555,-4.40257451754323,
0.));
#199474=CARTESIAN_POINT('Ctrl Pts',(-22.930371433555,-4.40257451754323,
12.));
#199475=CARTESIAN_POINT('Ctrl Pts',(-22.9147684862426,-4.39503346238473,
0.));
#199476=CARTESIAN_POINT('Ctrl Pts',(-22.9147684862426,-4.39503346238473,
12.));
#199477=CARTESIAN_POINT('Ctrl Pts',(-22.8992616040108,-4.38759397068406,
0.));
#199478=CARTESIAN_POINT('Ctrl Pts',(-22.8992616040108,-4.38759397068406,
12.));
#199479=CARTESIAN_POINT('Ctrl Pts',(-22.8838521827701,-4.38025605470093,
0.));
#199480=CARTESIAN_POINT('Ctrl Pts',(-22.8838521827701,-4.38025605470093,
12.));
#199481=CARTESIAN_POINT('Ctrl Pts',(-22.8685416419725,-4.37301972480745,
0.));
#199482=CARTESIAN_POINT('Ctrl Pts',(-22.8685416419725,-4.37301972480745,
12.));
#199483=CARTESIAN_POINT('Ctrl Pts',(-22.8533314252422,-4.36588498942997,
0.));
#199484=CARTESIAN_POINT('Ctrl Pts',(-22.8533314252422,-4.36588498942997,
12.));
#199485=CARTESIAN_POINT('Ctrl Pts',(-22.8382230011184,-4.35885185500546,
0.));
#199486=CARTESIAN_POINT('Ctrl Pts',(-22.8382230011184,-4.35885185500546,
12.));
#199487=CARTESIAN_POINT('Ctrl Pts',(-22.8232178638876,-4.35192032594791,
0.));
#199488=CARTESIAN_POINT('Ctrl Pts',(-22.8232178638876,-4.35192032594791,
12.));
#199489=CARTESIAN_POINT('Ctrl Pts',(-22.8083175343791,-4.34509040460062,
0.));
#199490=CARTESIAN_POINT('Ctrl Pts',(-22.8083175343791,-4.34509040460062,
12.));
#199491=CARTESIAN_POINT('Ctrl Pts',(-22.7935235607806,-4.33836209118446,
0.));
#199492=CARTESIAN_POINT('Ctrl Pts',(-22.7935235607806,-4.33836209118446,
12.));
#199493=CARTESIAN_POINT('Ctrl Pts',(-22.7788375194076,-4.3317353837319,
0.));
#199494=CARTESIAN_POINT('Ctrl Pts',(-22.7788375194076,-4.3317353837319,
12.));
#199495=CARTESIAN_POINT('Ctrl Pts',(-22.7642610156475,-4.32521027803754,
0.));
#199496=CARTESIAN_POINT('Ctrl Pts',(-22.7642610156475,-4.32521027803754,
12.));
#199497=CARTESIAN_POINT('Ctrl Pts',(-22.7497956849848,-4.31878676761235,
0.));
#199498=CARTESIAN_POINT('Ctrl Pts',(-22.7497956849848,-4.31878676761235,
12.));
#199499=CARTESIAN_POINT('Ctrl Pts',(-22.7354431939926,-4.31246484362549,
0.));
#199500=CARTESIAN_POINT('Ctrl Pts',(-22.7354431939926,-4.31246484362549,
12.));
#199501=CARTESIAN_POINT('Ctrl Pts',(-22.7212052413386,-4.30624449484069,
0.));
#199502=CARTESIAN_POINT('Ctrl Pts',(-22.7212052413386,-4.30624449484069,
12.));
#199503=CARTESIAN_POINT('Ctrl Pts',(-22.7070835587564,-4.3001257075406,
0.));
#199504=CARTESIAN_POINT('Ctrl Pts',(-22.7070835587564,-4.3001257075406,
12.));
#199505=CARTESIAN_POINT('Ctrl Pts',(-22.6930799122548,-4.29410846547056,
0.));
#199506=CARTESIAN_POINT('Ctrl Pts',(-22.6930799122548,-4.29410846547056,
12.));
#199507=CARTESIAN_POINT('Ctrl Pts',(-22.6791961033538,-4.28819274977763,
0.));
#199508=CARTESIAN_POINT('Ctrl Pts',(-22.6791961033538,-4.28819274977763,
12.));
#199509=CARTESIAN_POINT('Ctrl Pts',(-22.6654339703109,-4.28237853894059,
0.));
#199510=CARTESIAN_POINT('Ctrl Pts',(-22.6654339703109,-4.28237853894059,
12.));
#199511=CARTESIAN_POINT('Ctrl Pts',(-22.6517953893303,-4.2766658086912,
0.));
#199512=CARTESIAN_POINT('Ctrl Pts',(-22.6517953893303,-4.2766658086912,
12.));
#199513=CARTESIAN_POINT('Ctrl Pts',(-22.6382822758172,-4.27105453193004,
0.));
#199514=CARTESIAN_POINT('Ctrl Pts',(-22.6382822758172,-4.27105453193004,
12.));
#199515=CARTESIAN_POINT('Ctrl Pts',(-22.6248965859977,-4.26554467865576,
0.));
#199516=CARTESIAN_POINT('Ctrl Pts',(-22.6248965859977,-4.26554467865576,
12.));
#199517=CARTESIAN_POINT('Ctrl Pts',(-22.6116403184821,-4.26013621588305,
0.));
#199518=CARTESIAN_POINT('Ctrl Pts',(-22.6116403184821,-4.26013621588305,
12.));
#199519=CARTESIAN_POINT('Ctrl Pts',(-22.5985155158636,-4.25482910755481,
0.));
#199520=CARTESIAN_POINT('Ctrl Pts',(-22.5985155158636,-4.25482910755481,
12.));
#199521=CARTESIAN_POINT('Ctrl Pts',(-22.5855242662477,-4.24962331444177,
0.));
#199522=CARTESIAN_POINT('Ctrl Pts',(-22.5855242662477,-4.24962331444177,
12.));
#199523=CARTESIAN_POINT('Ctrl Pts',(-22.572668704992,-4.24451879404851,
0.));
#199524=CARTESIAN_POINT('Ctrl Pts',(-22.572668704992,-4.24451879404851,
12.));
#199525=CARTESIAN_POINT('Ctrl Pts',(-22.5599510166429,-4.23951550052522,
0.));
#199526=CARTESIAN_POINT('Ctrl Pts',(-22.5599510166429,-4.23951550052522,
12.));
#199527=CARTESIAN_POINT('Ctrl Pts',(-22.5473734368086,-4.23461338456712,
0.));
#199528=CARTESIAN_POINT('Ctrl Pts',(-22.5473734368086,-4.23461338456712,
12.));
#199529=CARTESIAN_POINT('Ctrl Pts',(-22.5349382540588,-4.22981239330733,
0.));
#199530=CARTESIAN_POINT('Ctrl Pts',(-22.5349382540588,-4.22981239330733,
12.));
#199531=CARTESIAN_POINT('Ctrl Pts',(-22.5226478117886,-4.22511247020041,
0.));
#199532=CARTESIAN_POINT('Ctrl Pts',(-22.5226478117886,-4.22511247020041,
12.));
#199533=CARTESIAN_POINT('Ctrl Pts',(-22.5105045108881,-4.22051355490196,
0.));
#199534=CARTESIAN_POINT('Ctrl Pts',(-22.5105045108881,-4.22051355490196,
12.));
#199535=CARTESIAN_POINT('Ctrl Pts',(-22.4985108124228,-4.21601558313906,
0.));
#199536=CARTESIAN_POINT('Ctrl Pts',(-22.4985108124228,-4.21601558313906,
12.));
#199537=CARTESIAN_POINT('Ctrl Pts',(-22.4866692403147,-4.21161848657428,
0.));
#199538=CARTESIAN_POINT('Ctrl Pts',(-22.4866692403147,-4.21161848657428,
12.));
#199539=CARTESIAN_POINT('Ctrl Pts',(-22.4749823839917,-4.20732219265649,
0.));
#199540=CARTESIAN_POINT('Ctrl Pts',(-22.4749823839917,-4.20732219265649,
12.));
#199541=CARTESIAN_POINT('Ctrl Pts',(-22.4634529011437,-4.20312662448174,
0.));
#199542=CARTESIAN_POINT('Ctrl Pts',(-22.4634529011437,-4.20312662448174,
12.));
#199543=CARTESIAN_POINT('Ctrl Pts',(-22.4520835205422,-4.19903170066358,
0.));
#199544=CARTESIAN_POINT('Ctrl Pts',(-22.4520835205422,-4.19903170066358,
12.));
#199545=CARTESIAN_POINT('Ctrl Pts',(-22.4408770448917,-4.1950373351886,
0.));
#199546=CARTESIAN_POINT('Ctrl Pts',(-22.4408770448917,-4.1950373351886,
12.));
#199547=CARTESIAN_POINT('Ctrl Pts',(-22.4298363535416,-4.19114343726932,
0.));
#199548=CARTESIAN_POINT('Ctrl Pts',(-22.4298363535416,-4.19114343726932,
12.));
#199549=CARTESIAN_POINT('Ctrl Pts',(-22.4189644056109,-4.18734991117707,
0.));
#199550=CARTESIAN_POINT('Ctrl Pts',(-22.4189644056109,-4.18734991117707,
12.));
#199551=CARTESIAN_POINT('Ctrl Pts',(-22.4082642454448,-4.18365665600839,
0.));
#199552=CARTESIAN_POINT('Ctrl Pts',(-22.4082642454448,-4.18365665600839,
12.));
#199553=CARTESIAN_POINT('Ctrl Pts',(-22.3977390078074,-4.18006356544879,
0.));
#199554=CARTESIAN_POINT('Ctrl Pts',(-22.3977390078074,-4.18006356544879,
12.));
#199555=CARTESIAN_POINT('Ctrl Pts',(-22.3873919231339,-4.17657052752834,
0.));
#199556=CARTESIAN_POINT('Ctrl Pts',(-22.3873919231339,-4.17657052752834,
12.));
#199557=CARTESIAN_POINT('Ctrl Pts',(-22.3772263228624,-4.17317742436162,
0.));
#199558=CARTESIAN_POINT('Ctrl Pts',(-22.3772263228624,-4.17317742436162,
12.));
#199559=CARTESIAN_POINT('Ctrl Pts',(-22.3672456427605,-4.16988413199469,
0.));
#199560=CARTESIAN_POINT('Ctrl Pts',(-22.3672456427605,-4.16988413199469,
12.));
#199561=CARTESIAN_POINT('Ctrl Pts',(-22.3574534257397,-4.16669052026602,
0.));
#199562=CARTESIAN_POINT('Ctrl Pts',(-22.3574534257397,-4.16669052026602,
12.));
#199563=CARTESIAN_POINT('Ctrl Pts',(-22.3478533253886,-4.1635964526318,
0.));
#199564=CARTESIAN_POINT('Ctrl Pts',(-22.3478533253886,-4.1635964526318,
12.));
#199565=CARTESIAN_POINT('Ctrl Pts',(-22.3384491078599,-4.16060178604154,
0.));
#199566=CARTESIAN_POINT('Ctrl Pts',(-22.3384491078599,-4.16060178604154,
12.));
#199567=CARTESIAN_POINT('Ctrl Pts',(-22.3292446628957,-4.15770637047882,
0.));
#199568=CARTESIAN_POINT('Ctrl Pts',(-22.3292446628957,-4.15770637047882,
12.));
#199569=CARTESIAN_POINT('Ctrl Pts',(-22.3202440186979,-4.15491004835278,
0.));
#199570=CARTESIAN_POINT('Ctrl Pts',(-22.3202440186979,-4.15491004835278,
12.));
#199571=CARTESIAN_POINT('Ctrl Pts',(-22.3114513545186,-4.15221265396993,
0.));
#199572=CARTESIAN_POINT('Ctrl Pts',(-22.3114513545186,-4.15221265396993,
12.));
#199573=CARTESIAN_POINT('Ctrl Pts',(-22.3028710166935,-4.14961401285525,
0.));
#199574=CARTESIAN_POINT('Ctrl Pts',(-22.3028710166935,-4.14961401285525,
12.));
#199575=CARTESIAN_POINT('Ctrl Pts',(-22.2945075198468,-4.14711394168559,
0.));
#199576=CARTESIAN_POINT('Ctrl Pts',(-22.2945075198468,-4.14711394168559,
12.));
#199577=CARTESIAN_POINT('Ctrl Pts',(-22.2863655389167,-4.14471224859295,
0.));
#199578=CARTESIAN_POINT('Ctrl Pts',(-22.2863655389167,-4.14471224859295,
12.));
#199579=CARTESIAN_POINT('Ctrl Pts',(-22.2784499072026,-4.14240873321982,
0.));
#199580=CARTESIAN_POINT('Ctrl Pts',(-22.2784499072026,-4.14240873321982,
12.));
#199581=CARTESIAN_POINT('Ctrl Pts',(-22.2707656042456,-4.14020318715988,
0.));
#199582=CARTESIAN_POINT('Ctrl Pts',(-22.2707656042456,-4.14020318715988,
12.));
#199583=CARTESIAN_POINT('Ctrl Pts',(-22.263317791397,-4.13809539255418,
0.));
#199584=CARTESIAN_POINT('Ctrl Pts',(-22.263317791397,-4.13809539255418,
12.));
#199585=CARTESIAN_POINT('Ctrl Pts',(-22.2561118708422,-4.13608511977226,
0.));
#199586=CARTESIAN_POINT('Ctrl Pts',(-22.2561118708422,-4.13608511977226,
12.));
#199587=CARTESIAN_POINT('Ctrl Pts',(-22.2491535317789,-4.13417212558808,
0.));
#199588=CARTESIAN_POINT('Ctrl Pts',(-22.2491535317789,-4.13417212558808,
12.));
#199589=CARTESIAN_POINT('Ctrl Pts',(-22.2424488153523,-4.1323561506016,
0.));
#199590=CARTESIAN_POINT('Ctrl Pts',(-22.2424488153523,-4.1323561506016,
12.));
#199591=CARTESIAN_POINT('Ctrl Pts',(-22.2360040565534,-4.13063692157499,
0.));
#199592=CARTESIAN_POINT('Ctrl Pts',(-22.2360040565534,-4.13063692157499,
12.));
#199593=CARTESIAN_POINT('Ctrl Pts',(-22.2298258043947,-4.12901415463379,
0.));
#199594=CARTESIAN_POINT('Ctrl Pts',(-22.2298258043947,-4.12901415463379,
12.));
#199595=CARTESIAN_POINT('Ctrl Pts',(-22.2239207458781,-4.12748755830099,
0.));
#199596=CARTESIAN_POINT('Ctrl Pts',(-22.2239207458781,-4.12748755830099,
12.));
#199597=CARTESIAN_POINT('Ctrl Pts',(-22.2182956401341,-4.126056836133,0.));
#199598=CARTESIAN_POINT('Ctrl Pts',(-22.2182956401341,-4.126056836133,12.));
#199599=CARTESIAN_POINT('Ctrl Pts',(-22.2129576146671,-4.12472167516602,
0.));
#199600=CARTESIAN_POINT('Ctrl Pts',(-22.2129576146671,-4.12472167516602,
12.));
#199601=CARTESIAN_POINT('Ctrl Pts',(-22.2079143941719,-4.12348173702024,
0.));
#199602=CARTESIAN_POINT('Ctrl Pts',(-22.2079143941719,-4.12348173702024,
12.));
#199603=CARTESIAN_POINT('Ctrl Pts',(-22.2031746532106,-4.12233664408237,
0.));
#199604=CARTESIAN_POINT('Ctrl Pts',(-22.2031746532106,-4.12233664408237,
12.));
#199605=CARTESIAN_POINT('Ctrl Pts',(-22.1987479618246,-4.12128598183533,
0.));
#199606=CARTESIAN_POINT('Ctrl Pts',(-22.1987479618246,-4.12128598183533,
12.));
#199607=CARTESIAN_POINT('Ctrl Pts',(-22.1946440958098,-4.12032932637738,
0.));
#199608=CARTESIAN_POINT('Ctrl Pts',(-22.1946440958098,-4.12032932637738,
12.));
#199609=CARTESIAN_POINT('Ctrl Pts',(-22.1908725908525,-4.11946626228623,
0.));
#199610=CARTESIAN_POINT('Ctrl Pts',(-22.1908725908525,-4.11946626228623,
12.));
#199611=CARTESIAN_POINT('Ctrl Pts',(-22.1874419861496,-4.11869641271752,
0.));
#199612=CARTESIAN_POINT('Ctrl Pts',(-22.1874419861496,-4.11869641271752,
12.));
#199613=CARTESIAN_POINT('Ctrl Pts',(-22.1843613164855,-4.11801938107464,
0.));
#199614=CARTESIAN_POINT('Ctrl Pts',(-22.1843613164855,-4.11801938107464,
12.));
#199615=CARTESIAN_POINT('Ctrl Pts',(-22.1816414985788,-4.11743469691765,
0.));
#199616=CARTESIAN_POINT('Ctrl Pts',(-22.1816414985788,-4.11743469691765,
12.));
#199617=CARTESIAN_POINT('Ctrl Pts',(-22.179297473024,-4.11694173195041,
0.));
#199618=CARTESIAN_POINT('Ctrl Pts',(-22.179297473024,-4.11694173195041,
12.));
#199619=CARTESIAN_POINT('Ctrl Pts',(-22.177347426894,-4.11653973150558,
0.));
#199620=CARTESIAN_POINT('Ctrl Pts',(-22.177347426894,-4.11653973150558,
12.));
#199621=CARTESIAN_POINT('Ctrl Pts',(-22.1758088296598,-4.11622797217066,
0.));
#199622=CARTESIAN_POINT('Ctrl Pts',(-22.1758088296598,-4.11622797217066,
12.));
#199623=CARTESIAN_POINT('Ctrl Pts',(-22.1746949858773,-4.11600589882767,
0.));
#199624=CARTESIAN_POINT('Ctrl Pts',(-22.1746949858773,-4.11600589882767,
12.));
#199625=CARTESIAN_POINT('Ctrl Pts',(-22.174148802123,-4.11589976826061,
0.));
#199626=CARTESIAN_POINT('Ctrl Pts',(-22.174148802123,-4.11589976826061,
12.));
#199627=CARTESIAN_POINT('Ctrl Pts',(-22.1739341411684,-4.1158603587821,
0.));
#199628=CARTESIAN_POINT('Ctrl Pts',(-22.1739341411684,-4.1158603587821,
12.));
#199629=CARTESIAN_POINT('Ctrl Pts',(-22.1738776823239,-4.11585194677412,
0.));
#199630=CARTESIAN_POINT('Ctrl Pts',(-22.1738776823239,-4.11585194677412,
12.));
#199631=CARTESIAN_POINT('Ctrl Pts',(-22.1738711152697,-4.11585220600461,
0.));
#199632=CARTESIAN_POINT('Ctrl Pts',(-22.1738711152697,-4.11585220600461,
12.));
#199633=CARTESIAN_POINT('',(-25.2771067246846,-6.08833931617698,0.));
#199634=CARTESIAN_POINT('Ctrl Pts',(-25.2771067246846,-6.08833931617698,
0.));
#199635=CARTESIAN_POINT('Ctrl Pts',(-25.2729539149479,-6.08441489609824,
0.));
#199636=CARTESIAN_POINT('Ctrl Pts',(-25.2646490489816,-6.07657531787577,
0.));
#199637=CARTESIAN_POINT('Ctrl Pts',(-25.2521940105523,-6.06484373634696,
0.));
#199638=CARTESIAN_POINT('Ctrl Pts',(-25.2355918138798,-6.04925720151412,
0.));
#199639=CARTESIAN_POINT('Ctrl Pts',(-25.2148466201368,-6.02986667390187,
0.));
#199640=CARTESIAN_POINT('Ctrl Pts',(-25.1941090269638,-6.0105688180476,
0.));
#199641=CARTESIAN_POINT('Ctrl Pts',(-25.1733791296154,-5.99136367859838,
0.));
#199642=CARTESIAN_POINT('Ctrl Pts',(-25.1526570863065,-5.97225131495636,
0.));
#199643=CARTESIAN_POINT('Ctrl Pts',(-25.1319431317273,-5.95323180187348,
0.));
#199644=CARTESIAN_POINT('Ctrl Pts',(-25.1112375971182,-5.93430523086776,
0.));
#199645=CARTESIAN_POINT('Ctrl Pts',(-25.0905409050863,-5.91547170844382,
0.));
#199646=CARTESIAN_POINT('Ctrl Pts',(-25.0698535426593,-5.89673135155459,
0.));
#199647=CARTESIAN_POINT('Ctrl Pts',(-25.0491760405965,-5.87808428385329,
0.));
#199648=CARTESIAN_POINT('Ctrl Pts',(-25.0285089498922,-5.8595306315681,
0.));
#199649=CARTESIAN_POINT('Ctrl Pts',(-25.0078528200558,-5.84107051963073,
0.));
#199650=CARTESIAN_POINT('Ctrl Pts',(-24.9872081752709,-5.82270406744214,
0.));
#199651=CARTESIAN_POINT('Ctrl Pts',(-24.9665754954462,-5.80443138549747,
0.));
#199652=CARTESIAN_POINT('Ctrl Pts',(-24.9459552293308,-5.78625257775703,
0.));
#199653=CARTESIAN_POINT('Ctrl Pts',(-24.9253478043632,-5.76816774342236,
0.));
#199654=CARTESIAN_POINT('Ctrl Pts',(-24.9047536376467,-5.75017697890813,
0.));
#199655=CARTESIAN_POINT('Ctrl Pts',(-24.8841731467219,-5.73228037976926,
0.));
#199656=CARTESIAN_POINT('Ctrl Pts',(-24.8636067597677,-5.71447804252019,
0.));
#199657=CARTESIAN_POINT('Ctrl Pts',(-24.8430549277634,-5.69677006679429,
0.));
#199658=CARTESIAN_POINT('Ctrl Pts',(-24.822518122386,-5.67915655496524,
0.));
#199659=CARTESIAN_POINT('Ctrl Pts',(-24.8019968304618,-5.66163761114903,
0.));
#199660=CARTESIAN_POINT('Ctrl Pts',(-24.7814915496728,-5.64421334042247,
0.));
#199661=CARTESIAN_POINT('Ctrl Pts',(-24.76100278357,-5.62688384790919,0.));
#199662=CARTESIAN_POINT('Ctrl Pts',(-24.7405310372736,-5.60964923798495,
0.));
#199663=CARTESIAN_POINT('Ctrl Pts',(-24.7200768119079,-5.59250961323995,
0.));
#199664=CARTESIAN_POINT('Ctrl Pts',(-24.6996406035507,-5.57546507427766,
0.));
#199665=CARTESIAN_POINT('Ctrl Pts',(-24.6792229061785,-5.55851572025389,
0.));
#199666=CARTESIAN_POINT('Ctrl Pts',(-24.6588242134733,-5.54166164919593,
0.));
#199667=CARTESIAN_POINT('Ctrl Pts',(-24.6384450211466,-5.52490295840996,
0.));
#199668=CARTESIAN_POINT('Ctrl Pts',(-24.618085828918,-5.50823974481959,
0.));
#199669=CARTESIAN_POINT('Ctrl Pts',(-24.5977471429365,-5.49167210537235,
0.));
#199670=CARTESIAN_POINT('Ctrl Pts',(-24.5774294770329,-5.47520013724403,
0.));
#199671=CARTESIAN_POINT('Ctrl Pts',(-24.5571333514841,-5.45882393762244,
0.));
#199672=CARTESIAN_POINT('Ctrl Pts',(-24.5368592922861,-5.44254360356865,
0.));
#199673=CARTESIAN_POINT('Ctrl Pts',(-24.5166078302107,-5.42635923183411,
0.));
#199674=CARTESIAN_POINT('Ctrl Pts',(-24.4963794999831,-5.41027091869242,
0.));
#199675=CARTESIAN_POINT('Ctrl Pts',(-24.4761748393322,-5.3942787597383,
0.));
#199676=CARTESIAN_POINT('Ctrl Pts',(-24.4559943883159,-5.37838284973706,
0.));
#199677=CARTESIAN_POINT('Ctrl Pts',(-24.4358386899152,-5.36258328273639,
0.));
#199678=CARTESIAN_POINT('Ctrl Pts',(-24.4157082904615,-5.34688015213546,
0.));
#199679=CARTESIAN_POINT('Ctrl Pts',(-24.3956037401293,-5.33127355076036,
0.));
#199680=CARTESIAN_POINT('Ctrl Pts',(-24.3755255933917,-5.31576357092524,
0.));
#199681=CARTESIAN_POINT('Ctrl Pts',(-24.3554744095075,-5.30035030449058,
0.));
#199682=CARTESIAN_POINT('Ctrl Pts',(-24.3354507529415,-5.28503384290644,
0.));
#199683=CARTESIAN_POINT('Ctrl Pts',(-24.3154551932222,-5.26981427718796,
0.));
#199684=CARTESIAN_POINT('Ctrl Pts',(-24.2954883048448,-5.25469169788856,
0.));
#199685=CARTESIAN_POINT('Ctrl Pts',(-24.2755506671526,-5.23966619506289,
0.));
#199686=CARTESIAN_POINT('Ctrl Pts',(-24.2556428642294,-5.22473785822441,
0.));
#199687=CARTESIAN_POINT('Ctrl Pts',(-24.2357654847765,-5.20990677629173,
0.));
#199688=CARTESIAN_POINT('Ctrl Pts',(-24.215919122017,-5.19517303753643,
0.));
#199689=CARTESIAN_POINT('Ctrl Pts',(-24.1961043738754,-5.18053672961392,
0.));
#199690=CARTESIAN_POINT('Ctrl Pts',(-24.1763218431343,-5.16599793957979,
0.));
#199691=CARTESIAN_POINT('Ctrl Pts',(-24.156572137597,-5.15155675390075,
0.));
#199692=CARTESIAN_POINT('Ctrl Pts',(-24.1368558702443,-5.13721325845744,
0.));
#199693=CARTESIAN_POINT('Ctrl Pts',(-24.117173659394,-5.12296753853859,
0.));
#199694=CARTESIAN_POINT('Ctrl Pts',(-24.0975261288446,-5.10881967883132,
0.));
#199695=CARTESIAN_POINT('Ctrl Pts',(-24.0779139079266,-5.09476976342625,
0.));
#199696=CARTESIAN_POINT('Ctrl Pts',(-24.0583376315638,-5.08081787581276,
0.));
#199697=CARTESIAN_POINT('Ctrl Pts',(-24.0387979403268,-5.06696409886641,
0.));
#199698=CARTESIAN_POINT('Ctrl Pts',(-24.0192954804896,-5.05320851483065,
0.));
#199699=CARTESIAN_POINT('Ctrl Pts',(-23.9998309040746,-5.03955120528521,
0.));
#199700=CARTESIAN_POINT('Ctrl Pts',(-23.9804048689227,-5.02599225112454,
0.));
#199701=CARTESIAN_POINT('Ctrl Pts',(-23.9610180388271,-5.01253173257453,
0.));
#199702=CARTESIAN_POINT('Ctrl Pts',(-23.9416710836529,-4.99916972919306,
0.));
#199703=CARTESIAN_POINT('Ctrl Pts',(-23.9223646794592,-4.98590631986532,
0.));
#199704=CARTESIAN_POINT('Ctrl Pts',(-23.9030995086163,-4.97274158279226,
0.));
#199705=CARTESIAN_POINT('Ctrl Pts',(-23.8838762599218,-4.9596755954656,
0.));
#199706=CARTESIAN_POINT('Ctrl Pts',(-23.8646956287168,-4.9467084346586,
0.));
#199707=CARTESIAN_POINT('Ctrl Pts',(-23.8455583170057,-4.93384017643432,
0.));
#199708=CARTESIAN_POINT('Ctrl Pts',(-23.8264650335717,-4.92107089613969,
0.));
#199709=CARTESIAN_POINT('Ctrl Pts',(-23.8074164940896,-4.90840066839344,
0.));
#199710=CARTESIAN_POINT('Ctrl Pts',(-23.7884134212384,-4.89582956706775,
0.));
#199711=CARTESIAN_POINT('Ctrl Pts',(-23.7694565448049,-4.88335766525573,
0.));
#199712=CARTESIAN_POINT('Ctrl Pts',(-23.7505466018245,-4.87098503527152,
0.));
#199713=CARTESIAN_POINT('Ctrl Pts',(-23.7316843367313,-4.85871174865499,
0.));
#199714=CARTESIAN_POINT('Ctrl Pts',(-23.7128705015017,-4.84653787616425,
0.));
#199715=CARTESIAN_POINT('Ctrl Pts',(-23.6941058557971,-4.83446348776265,
0.));
#199716=CARTESIAN_POINT('Ctrl Pts',(-23.675391167102,-4.82248865259562,
0.));
#199717=CARTESIAN_POINT('Ctrl Pts',(-23.6567272108628,-4.81061343896432,
0.));
#199718=CARTESIAN_POINT('Ctrl Pts',(-23.6381147706579,-4.7988379143322,
0.));
#199719=CARTESIAN_POINT('Ctrl Pts',(-23.6195546383624,-4.78716214532098,
0.));
#199720=CARTESIAN_POINT('Ctrl Pts',(-23.6010476143099,-4.77558619769872,
0.));
#199721=CARTESIAN_POINT('Ctrl Pts',(-23.5825945074535,-4.76411013636251,
0.));
#199722=CARTESIAN_POINT('Ctrl Pts',(-23.5641961355168,-4.75273402530617,
0.));
#199723=CARTESIAN_POINT('Ctrl Pts',(-23.545853325171,-4.74145792760698,
0.));
#199724=CARTESIAN_POINT('Ctrl Pts',(-23.5275669122372,-4.7302819054303,
0.));
#199725=CARTESIAN_POINT('Ctrl Pts',(-23.509337741878,-4.71920602001901,
0.));
#199726=CARTESIAN_POINT('Ctrl Pts',(-23.491166668789,-4.70823033167818,
0.));
#199727=CARTESIAN_POINT('Ctrl Pts',(-23.4730545573853,-4.69735489975024,
0.));
#199728=CARTESIAN_POINT('Ctrl Pts',(-23.455002281986,-4.68657978258303,
0.));
#199729=CARTESIAN_POINT('Ctrl Pts',(-23.4370107270451,-4.67590503753058,
0.));
#199730=CARTESIAN_POINT('Ctrl Pts',(-23.4190807873803,-4.6653307209467,
0.));
#199731=CARTESIAN_POINT('Ctrl Pts',(-23.4012133683959,-4.65485688816924,
0.));
#199732=CARTESIAN_POINT('Ctrl Pts',(-23.3834093863068,-4.6444835934993,
0.));
#199733=CARTESIAN_POINT('Ctrl Pts',(-23.3656697683489,-4.63421089016541,
0.));
#199734=CARTESIAN_POINT('Ctrl Pts',(-23.3479954530272,-4.62403883030805,
0.));
#199735=CARTESIAN_POINT('Ctrl Pts',(-23.3303873903938,-4.6139674649783,
0.));
#199736=CARTESIAN_POINT('Ctrl Pts',(-23.3128465423115,-4.60399684412163,
0.));
#199737=CARTESIAN_POINT('Ctrl Pts',(-23.2953738827191,-4.5941270165575,
0.));
#199738=CARTESIAN_POINT('Ctrl Pts',(-23.2779703978876,-4.5843580299469,
0.));
#199739=CARTESIAN_POINT('Ctrl Pts',(-23.2606370866866,-4.57468993076097,
0.));
#199740=CARTESIAN_POINT('Ctrl Pts',(-23.2433749609131,-4.56512276427839,
0.));
#199741=CARTESIAN_POINT('Ctrl Pts',(-23.2261850456064,-4.55565657456975,
0.));
#199742=CARTESIAN_POINT('Ctrl Pts',(-23.2090683793629,-4.54629140447544,
0.));
#199743=CARTESIAN_POINT('Ctrl Pts',(-23.1920260146465,-4.53702729557566,
0.));
#199744=CARTESIAN_POINT('Ctrl Pts',(-23.1750590180908,-4.52786428815014,
0.));
#199745=CARTESIAN_POINT('Ctrl Pts',(-23.1581684708761,-4.51880242116748,
0.));
#199746=CARTESIAN_POINT('Ctrl Pts',(-23.1413554691123,-4.5098417322706,
0.));
#199747=CARTESIAN_POINT('Ctrl Pts',(-23.1246211242115,-4.50098225775171,
0.));
#199748=CARTESIAN_POINT('Ctrl Pts',(-23.1079665632636,-4.49222403252216,
0.));
#199749=CARTESIAN_POINT('Ctrl Pts',(-23.0913929293922,-4.48356709006788,
0.));
#199750=CARTESIAN_POINT('Ctrl Pts',(-23.0749013821881,-4.47501146242856,
0.));
#199751=CARTESIAN_POINT('Ctrl Pts',(-23.0584930981732,-4.4665571801823,
0.));
#199752=CARTESIAN_POINT('Ctrl Pts',(-23.0421692712467,-4.45820427241683,
0.));
#199753=CARTESIAN_POINT('Ctrl Pts',(-23.0259311131392,-4.44995276669686,
0.));
#199754=CARTESIAN_POINT('Ctrl Pts',(-23.0097798538395,-4.44180268901643,
0.));
#199755=CARTESIAN_POINT('Ctrl Pts',(-22.9937167421006,-4.43375406376879,
0.));
#199756=CARTESIAN_POINT('Ctrl Pts',(-22.977743046002,-4.42580691372751,
0.));
#199757=CARTESIAN_POINT('Ctrl Pts',(-22.9618600534866,-4.41796126001302,
0.));
#199758=CARTESIAN_POINT('Ctrl Pts',(-22.9460690729093,-4.41021712205553,
0.));
#199759=CARTESIAN_POINT('Ctrl Pts',(-22.930371433555,-4.40257451754323,
0.));
#199760=CARTESIAN_POINT('Ctrl Pts',(-22.9147684862426,-4.39503346238473,
0.));
#199761=CARTESIAN_POINT('Ctrl Pts',(-22.8992616040108,-4.38759397068406,
0.));
#199762=CARTESIAN_POINT('Ctrl Pts',(-22.8838521827701,-4.38025605470093,
0.));
#199763=CARTESIAN_POINT('Ctrl Pts',(-22.8685416419725,-4.37301972480745,
0.));
#199764=CARTESIAN_POINT('Ctrl Pts',(-22.8533314252422,-4.36588498942997,
0.));
#199765=CARTESIAN_POINT('Ctrl Pts',(-22.8382230011184,-4.35885185500546,
0.));
#199766=CARTESIAN_POINT('Ctrl Pts',(-22.8232178638876,-4.35192032594791,
0.));
#199767=CARTESIAN_POINT('Ctrl Pts',(-22.8083175343791,-4.34509040460062,
0.));
#199768=CARTESIAN_POINT('Ctrl Pts',(-22.7935235607806,-4.33836209118446,
0.));
#199769=CARTESIAN_POINT('Ctrl Pts',(-22.7788375194076,-4.3317353837319,
0.));
#199770=CARTESIAN_POINT('Ctrl Pts',(-22.7642610156475,-4.32521027803754,
0.));
#199771=CARTESIAN_POINT('Ctrl Pts',(-22.7497956849848,-4.31878676761235,
0.));
#199772=CARTESIAN_POINT('Ctrl Pts',(-22.7354431939926,-4.31246484362549,
0.));
#199773=CARTESIAN_POINT('Ctrl Pts',(-22.7212052413386,-4.30624449484069,
0.));
#199774=CARTESIAN_POINT('Ctrl Pts',(-22.7070835587564,-4.3001257075406,
0.));
#199775=CARTESIAN_POINT('Ctrl Pts',(-22.6930799122548,-4.29410846547056,
0.));
#199776=CARTESIAN_POINT('Ctrl Pts',(-22.6791961033538,-4.28819274977763,
0.));
#199777=CARTESIAN_POINT('Ctrl Pts',(-22.6654339703109,-4.28237853894059,
0.));
#199778=CARTESIAN_POINT('Ctrl Pts',(-22.6517953893303,-4.2766658086912,
0.));
#199779=CARTESIAN_POINT('Ctrl Pts',(-22.6382822758172,-4.27105453193004,
0.));
#199780=CARTESIAN_POINT('Ctrl Pts',(-22.6248965859977,-4.26554467865576,
0.));
#199781=CARTESIAN_POINT('Ctrl Pts',(-22.6116403184821,-4.26013621588305,
0.));
#199782=CARTESIAN_POINT('Ctrl Pts',(-22.5985155158636,-4.25482910755481,
0.));
#199783=CARTESIAN_POINT('Ctrl Pts',(-22.5855242662477,-4.24962331444177,
0.));
#199784=CARTESIAN_POINT('Ctrl Pts',(-22.572668704992,-4.24451879404851,
0.));
#199785=CARTESIAN_POINT('Ctrl Pts',(-22.5599510166429,-4.23951550052522,
0.));
#199786=CARTESIAN_POINT('Ctrl Pts',(-22.5473734368086,-4.23461338456712,
0.));
#199787=CARTESIAN_POINT('Ctrl Pts',(-22.5349382540588,-4.22981239330733,
0.));
#199788=CARTESIAN_POINT('Ctrl Pts',(-22.5226478117886,-4.22511247020041,
0.));
#199789=CARTESIAN_POINT('Ctrl Pts',(-22.5105045108881,-4.22051355490196,
0.));
#199790=CARTESIAN_POINT('Ctrl Pts',(-22.4985108124228,-4.21601558313906,
0.));
#199791=CARTESIAN_POINT('Ctrl Pts',(-22.4866692403147,-4.21161848657428,
0.));
#199792=CARTESIAN_POINT('Ctrl Pts',(-22.4749823839917,-4.20732219265649,
0.));
#199793=CARTESIAN_POINT('Ctrl Pts',(-22.4634529011437,-4.20312662448174,
0.));
#199794=CARTESIAN_POINT('Ctrl Pts',(-22.4520835205422,-4.19903170066358,
0.));
#199795=CARTESIAN_POINT('Ctrl Pts',(-22.4408770448917,-4.1950373351886,
0.));
#199796=CARTESIAN_POINT('Ctrl Pts',(-22.4298363535416,-4.19114343726932,
0.));
#199797=CARTESIAN_POINT('Ctrl Pts',(-22.4189644056109,-4.18734991117707,
0.));
#199798=CARTESIAN_POINT('Ctrl Pts',(-22.4082642454448,-4.18365665600839,
0.));
#199799=CARTESIAN_POINT('Ctrl Pts',(-22.3977390078074,-4.18006356544879,
0.));
#199800=CARTESIAN_POINT('Ctrl Pts',(-22.3873919231339,-4.17657052752834,
0.));
#199801=CARTESIAN_POINT('Ctrl Pts',(-22.3772263228624,-4.17317742436162,
0.));
#199802=CARTESIAN_POINT('Ctrl Pts',(-22.3672456427605,-4.16988413199469,
0.));
#199803=CARTESIAN_POINT('Ctrl Pts',(-22.3574534257397,-4.16669052026602,
0.));
#199804=CARTESIAN_POINT('Ctrl Pts',(-22.3478533253886,-4.1635964526318,
0.));
#199805=CARTESIAN_POINT('Ctrl Pts',(-22.3384491078599,-4.16060178604154,
0.));
#199806=CARTESIAN_POINT('Ctrl Pts',(-22.3292446628957,-4.15770637047882,
0.));
#199807=CARTESIAN_POINT('Ctrl Pts',(-22.3202440186979,-4.15491004835278,
0.));
#199808=CARTESIAN_POINT('Ctrl Pts',(-22.3114513545186,-4.15221265396993,
0.));
#199809=CARTESIAN_POINT('Ctrl Pts',(-22.3028710166935,-4.14961401285525,
0.));
#199810=CARTESIAN_POINT('Ctrl Pts',(-22.2945075198468,-4.14711394168559,
0.));
#199811=CARTESIAN_POINT('Ctrl Pts',(-22.2863655389167,-4.14471224859295,
0.));
#199812=CARTESIAN_POINT('Ctrl Pts',(-22.2784499072026,-4.14240873321982,
0.));
#199813=CARTESIAN_POINT('Ctrl Pts',(-22.2707656042456,-4.14020318715988,
0.));
#199814=CARTESIAN_POINT('Ctrl Pts',(-22.263317791397,-4.13809539255418,
0.));
#199815=CARTESIAN_POINT('Ctrl Pts',(-22.2561118708422,-4.13608511977226,
0.));
#199816=CARTESIAN_POINT('Ctrl Pts',(-22.2491535317789,-4.13417212558808,
0.));
#199817=CARTESIAN_POINT('Ctrl Pts',(-22.2424488153523,-4.1323561506016,
0.));
#199818=CARTESIAN_POINT('Ctrl Pts',(-22.2360040565534,-4.13063692157499,
0.));
#199819=CARTESIAN_POINT('Ctrl Pts',(-22.2298258043947,-4.12901415463379,
0.));
#199820=CARTESIAN_POINT('Ctrl Pts',(-22.2239207458781,-4.12748755830099,
0.));
#199821=CARTESIAN_POINT('Ctrl Pts',(-22.2182956401341,-4.126056836133,0.));
#199822=CARTESIAN_POINT('Ctrl Pts',(-22.2129576146671,-4.12472167516602,
0.));
#199823=CARTESIAN_POINT('Ctrl Pts',(-22.2079143941719,-4.12348173702024,
0.));
#199824=CARTESIAN_POINT('Ctrl Pts',(-22.2031746532106,-4.12233664408237,
0.));
#199825=CARTESIAN_POINT('Ctrl Pts',(-22.1987479618246,-4.12128598183533,
0.));
#199826=CARTESIAN_POINT('Ctrl Pts',(-22.1946440958098,-4.12032932637738,
0.));
#199827=CARTESIAN_POINT('Ctrl Pts',(-22.1908725908525,-4.11946626228623,
0.));
#199828=CARTESIAN_POINT('Ctrl Pts',(-22.1874419861496,-4.11869641271752,
0.));
#199829=CARTESIAN_POINT('Ctrl Pts',(-22.1843613164855,-4.11801938107464,
0.));
#199830=CARTESIAN_POINT('Ctrl Pts',(-22.1816414985788,-4.11743469691765,
0.));
#199831=CARTESIAN_POINT('Ctrl Pts',(-22.179297473024,-4.11694173195041,
0.));
#199832=CARTESIAN_POINT('Ctrl Pts',(-22.177347426894,-4.11653973150558,
0.));
#199833=CARTESIAN_POINT('Ctrl Pts',(-22.1758088296598,-4.11622797217066,
0.));
#199834=CARTESIAN_POINT('Ctrl Pts',(-22.1746949858773,-4.11600589882767,
0.));
#199835=CARTESIAN_POINT('Ctrl Pts',(-22.174148802123,-4.11589976826061,
0.));
#199836=CARTESIAN_POINT('Ctrl Pts',(-22.1739341411684,-4.1158603587821,
0.));
#199837=CARTESIAN_POINT('Ctrl Pts',(-22.1738776823239,-4.11585194677412,
0.));
#199838=CARTESIAN_POINT('Ctrl Pts',(-22.1738711152697,-4.11585220600461,
0.));
#199839=CARTESIAN_POINT('',(-25.2771067246846,-6.08833931617698,0.));
#199840=CARTESIAN_POINT('Ctrl Pts',(-22.4835757167854,-1.76341220531179,
0.));
#199841=CARTESIAN_POINT('Ctrl Pts',(-22.4835757167854,-1.76341220531179,
12.));
#199842=CARTESIAN_POINT('Ctrl Pts',(-22.483581992979,-1.76341415538764,
0.));
#199843=CARTESIAN_POINT('Ctrl Pts',(-22.483581992979,-1.76341415538764,
12.));
#199844=CARTESIAN_POINT('Ctrl Pts',(-22.4836387052232,-1.7634206426357,
0.));
#199845=CARTESIAN_POINT('Ctrl Pts',(-22.4836387052232,-1.7634206426357,
12.));
#199846=CARTESIAN_POINT('Ctrl Pts',(-22.483856251707,-1.76343813434565,
0.));
#199847=CARTESIAN_POINT('Ctrl Pts',(-22.483856251707,-1.76343813434565,
12.));
#199848=CARTESIAN_POINT('Ctrl Pts',(-22.4844112933129,-1.76347698284792,
0.));
#199849=CARTESIAN_POINT('Ctrl Pts',(-22.4844112933129,-1.76347698284792,
12.));
#199850=CARTESIAN_POINT('Ctrl Pts',(-22.4855446605991,-1.76355076045546,
0.));
#199851=CARTESIAN_POINT('Ctrl Pts',(-22.4855446605991,-1.76355076045546,
12.));
#199852=CARTESIAN_POINT('Ctrl Pts',(-22.4871115206571,-1.76364784232963,
0.));
#199853=CARTESIAN_POINT('Ctrl Pts',(-22.4871115206571,-1.76364784232963,
12.));
#199854=CARTESIAN_POINT('Ctrl Pts',(-22.4890991659478,-1.76376424879505,
0.));
#199855=CARTESIAN_POINT('Ctrl Pts',(-22.4890991659478,-1.76376424879505,
12.));
#199856=CARTESIAN_POINT('Ctrl Pts',(-22.4914909094908,-1.76389475965724,
0.));
#199857=CARTESIAN_POINT('Ctrl Pts',(-22.4914909094908,-1.76389475965724,
12.));
#199858=CARTESIAN_POINT('Ctrl Pts',(-22.4942693792449,-1.764033938803,0.));
#199859=CARTESIAN_POINT('Ctrl Pts',(-22.4942693792449,-1.764033938803,12.));
#199860=CARTESIAN_POINT('Ctrl Pts',(-22.4974203063191,-1.76417731243462,
0.));
#199861=CARTESIAN_POINT('Ctrl Pts',(-22.4974203063191,-1.76417731243462,
12.));
#199862=CARTESIAN_POINT('Ctrl Pts',(-22.5009332677316,-1.76432160068725,
0.));
#199863=CARTESIAN_POINT('Ctrl Pts',(-22.5009332677316,-1.76432160068725,
12.));
#199864=CARTESIAN_POINT('Ctrl Pts',(-22.5047996391978,-1.76446408210366,
0.));
#199865=CARTESIAN_POINT('Ctrl Pts',(-22.5047996391978,-1.76446408210366,
12.));
#199866=CARTESIAN_POINT('Ctrl Pts',(-22.5090112700212,-1.76460218257323,
0.));
#199867=CARTESIAN_POINT('Ctrl Pts',(-22.5090112700212,-1.76460218257323,
12.));
#199868=CARTESIAN_POINT('Ctrl Pts',(-22.5135590569554,-1.76473303281159,
0.));
#199869=CARTESIAN_POINT('Ctrl Pts',(-22.5135590569554,-1.76473303281159,
12.));
#199870=CARTESIAN_POINT('Ctrl Pts',(-22.5184336670207,-1.76485369319896,
0.));
#199871=CARTESIAN_POINT('Ctrl Pts',(-22.5184336670207,-1.76485369319896,
12.));
#199872=CARTESIAN_POINT('Ctrl Pts',(-22.5236259635515,-1.76496128643369,
0.));
#199873=CARTESIAN_POINT('Ctrl Pts',(-22.5236259635515,-1.76496128643369,
12.));
#199874=CARTESIAN_POINT('Ctrl Pts',(-22.529127665298,-1.76505320262751,
0.));
#199875=CARTESIAN_POINT('Ctrl Pts',(-22.529127665298,-1.76505320262751,
12.));
#199876=CARTESIAN_POINT('Ctrl Pts',(-22.5349313983571,-1.7651271156325,
0.));
#199877=CARTESIAN_POINT('Ctrl Pts',(-22.5349313983571,-1.7651271156325,
12.));
#199878=CARTESIAN_POINT('Ctrl Pts',(-22.5410303590891,-1.76518087841492,
0.));
#199879=CARTESIAN_POINT('Ctrl Pts',(-22.5410303590891,-1.76518087841492,
12.));
#199880=CARTESIAN_POINT('Ctrl Pts',(-22.5474180954006,-1.76521245524047,
0.));
#199881=CARTESIAN_POINT('Ctrl Pts',(-22.5474180954006,-1.76521245524047,
12.));
#199882=CARTESIAN_POINT('Ctrl Pts',(-22.5540882235837,-1.76521983384063,
0.));
#199883=CARTESIAN_POINT('Ctrl Pts',(-22.5540882235837,-1.76521983384063,
12.));
#199884=CARTESIAN_POINT('Ctrl Pts',(-22.5610344912501,-1.76520104500449,
0.));
#199885=CARTESIAN_POINT('Ctrl Pts',(-22.5610344912501,-1.76520104500449,
12.));
#199886=CARTESIAN_POINT('Ctrl Pts',(-22.5682508499873,-1.76515418518829,
0.));
#199887=CARTESIAN_POINT('Ctrl Pts',(-22.5682508499873,-1.76515418518829,
12.));
#199888=CARTESIAN_POINT('Ctrl Pts',(-22.5757315316355,-1.76507744026747,
0.));
#199889=CARTESIAN_POINT('Ctrl Pts',(-22.5757315316355,-1.76507744026747,
12.));
#199890=CARTESIAN_POINT('Ctrl Pts',(-22.5834711038024,-1.76496910283088,
0.));
#199891=CARTESIAN_POINT('Ctrl Pts',(-22.5834711038024,-1.76496910283088,
12.));
#199892=CARTESIAN_POINT('Ctrl Pts',(-22.5914644078106,-1.76482755288411,
0.));
#199893=CARTESIAN_POINT('Ctrl Pts',(-22.5914644078106,-1.76482755288411,
12.));
#199894=CARTESIAN_POINT('Ctrl Pts',(-22.5997065145638,-1.76465124413556,
0.));
#199895=CARTESIAN_POINT('Ctrl Pts',(-22.5997065145638,-1.76465124413556,
12.));
#199896=CARTESIAN_POINT('Ctrl Pts',(-22.6081926681342,-1.76443868648015,
0.));
#199897=CARTESIAN_POINT('Ctrl Pts',(-22.6081926681342,-1.76443868648015,
12.));
#199898=CARTESIAN_POINT('Ctrl Pts',(-22.6169182517693,-1.76418843543739,
0.));
#199899=CARTESIAN_POINT('Ctrl Pts',(-22.6169182517693,-1.76418843543739,
12.));
#199900=CARTESIAN_POINT('Ctrl Pts',(-22.6258787994847,-1.76389909571402,
0.));
#199901=CARTESIAN_POINT('Ctrl Pts',(-22.6258787994847,-1.76389909571402,
12.));
#199902=CARTESIAN_POINT('Ctrl Pts',(-22.635069997936,-1.76356932176272,
0.));
#199903=CARTESIAN_POINT('Ctrl Pts',(-22.635069997936,-1.76356932176272,
12.));
#199904=CARTESIAN_POINT('Ctrl Pts',(-22.6444876940425,-1.76319782013914,
0.));
#199905=CARTESIAN_POINT('Ctrl Pts',(-22.6444876940425,-1.76319782013914,
12.));
#199906=CARTESIAN_POINT('Ctrl Pts',(-22.6541278938413,-1.76278334912559,
0.));
#199907=CARTESIAN_POINT('Ctrl Pts',(-22.6541278938413,-1.76278334912559,
12.));
#199908=CARTESIAN_POINT('Ctrl Pts',(-22.6639867471756,-1.76232471392567,
0.));
#199909=CARTESIAN_POINT('Ctrl Pts',(-22.6639867471756,-1.76232471392567,
12.));
#199910=CARTESIAN_POINT('Ctrl Pts',(-22.6740605356699,-1.76182076289525,
0.));
#199911=CARTESIAN_POINT('Ctrl Pts',(-22.6740605356699,-1.76182076289525,
12.));
#199912=CARTESIAN_POINT('Ctrl Pts',(-22.6843456585245,-1.76127038310612,
0.));
#199913=CARTESIAN_POINT('Ctrl Pts',(-22.6843456585245,-1.76127038310612,
12.));
#199914=CARTESIAN_POINT('Ctrl Pts',(-22.6948386219843,-1.76067249704884,
0.));
#199915=CARTESIAN_POINT('Ctrl Pts',(-22.6948386219843,-1.76067249704884,
12.));
#199916=CARTESIAN_POINT('Ctrl Pts',(-22.7055360375481,-1.76002606202399,
0.));
#199917=CARTESIAN_POINT('Ctrl Pts',(-22.7055360375481,-1.76002606202399,
12.));
#199918=CARTESIAN_POINT('Ctrl Pts',(-22.7164346186007,-1.75933006905924,
0.));
#199919=CARTESIAN_POINT('Ctrl Pts',(-22.7164346186007,-1.75933006905924,
12.));
#199920=CARTESIAN_POINT('Ctrl Pts',(-22.7275311777305,-1.75858354204635,
0.));
#199921=CARTESIAN_POINT('Ctrl Pts',(-22.7275311777305,-1.75858354204635,
12.));
#199922=CARTESIAN_POINT('Ctrl Pts',(-22.7388226235565,-1.75778553673249,
0.));
#199923=CARTESIAN_POINT('Ctrl Pts',(-22.7388226235565,-1.75778553673249,
12.));
#199924=CARTESIAN_POINT('Ctrl Pts',(-22.7503059556455,-1.75693513908911,
0.));
#199925=CARTESIAN_POINT('Ctrl Pts',(-22.7503059556455,-1.75693513908911,
12.));
#199926=CARTESIAN_POINT('Ctrl Pts',(-22.7619782595013,-1.7560314637164,
0.));
#199927=CARTESIAN_POINT('Ctrl Pts',(-22.7619782595013,-1.7560314637164,
12.));
#199928=CARTESIAN_POINT('Ctrl Pts',(-22.7738367016115,-1.75507365227127,
0.));
#199929=CARTESIAN_POINT('Ctrl Pts',(-22.7738367016115,-1.75507365227127,
12.));
#199930=CARTESIAN_POINT('Ctrl Pts',(-22.7858785242358,-1.75406087182929,
0.));
#199931=CARTESIAN_POINT('Ctrl Pts',(-22.7858785242358,-1.75406087182929,
12.));
#199932=CARTESIAN_POINT('Ctrl Pts',(-22.7981010424312,-1.75299231391461,
0.));
#199933=CARTESIAN_POINT('Ctrl Pts',(-22.7981010424312,-1.75299231391461,
12.));
#199934=CARTESIAN_POINT('Ctrl Pts',(-22.8105016414712,-1.75186719365589,
0.));
#199935=CARTESIAN_POINT('Ctrl Pts',(-22.8105016414712,-1.75186719365589,
12.));
#199936=CARTESIAN_POINT('Ctrl Pts',(-22.8230777741285,-1.75068474890884,
0.));
#199937=CARTESIAN_POINT('Ctrl Pts',(-22.8230777741285,-1.75068474890884,
12.));
#199938=CARTESIAN_POINT('Ctrl Pts',(-22.8358269579854,-1.74944423940117,
0.));
#199939=CARTESIAN_POINT('Ctrl Pts',(-22.8358269579854,-1.74944423940117,
12.));
#199940=CARTESIAN_POINT('Ctrl Pts',(-22.8487467728075,-1.74814494588492,
0.));
#199941=CARTESIAN_POINT('Ctrl Pts',(-22.8487467728075,-1.74814494588492,
12.));
#199942=CARTESIAN_POINT('Ctrl Pts',(-22.8618348580234,-1.74678616930663,
0.));
#199943=CARTESIAN_POINT('Ctrl Pts',(-22.8618348580234,-1.74678616930663,
12.));
#199944=CARTESIAN_POINT('Ctrl Pts',(-22.8750889101696,-1.745367229982,0.));
#199945=CARTESIAN_POINT('Ctrl Pts',(-22.8750889101696,-1.745367229982,12.));
#199946=CARTESIAN_POINT('Ctrl Pts',(-22.8885066803351,-1.74388746677702,
0.));
#199947=CARTESIAN_POINT('Ctrl Pts',(-22.8885066803351,-1.74388746677702,
12.));
#199948=CARTESIAN_POINT('Ctrl Pts',(-22.9020859716144,-1.74234623630079,
0.));
#199949=CARTESIAN_POINT('Ctrl Pts',(-22.9020859716144,-1.74234623630079,
12.));
#199950=CARTESIAN_POINT('Ctrl Pts',(-22.9158246373365,-1.74074291231057,
0.));
#199951=CARTESIAN_POINT('Ctrl Pts',(-22.9158246373365,-1.74074291231057,
12.));
#199952=CARTESIAN_POINT('Ctrl Pts',(-22.9297205792587,-1.73907688511664,
0.));
#199953=CARTESIAN_POINT('Ctrl Pts',(-22.9297205792587,-1.73907688511664,
12.));
#199954=CARTESIAN_POINT('Ctrl Pts',(-22.9437717457825,-1.73734756100038,
0.));
#199955=CARTESIAN_POINT('Ctrl Pts',(-22.9437717457825,-1.73734756100038,
12.));
#199956=CARTESIAN_POINT('Ctrl Pts',(-22.9579761301062,-1.73555436162771,
0.));
#199957=CARTESIAN_POINT('Ctrl Pts',(-22.9579761301062,-1.73555436162771,
12.));
#199958=CARTESIAN_POINT('Ctrl Pts',(-22.9723317685688,-1.73369672350817,
0.));
#199959=CARTESIAN_POINT('Ctrl Pts',(-22.9723317685688,-1.73369672350817,
12.));
#199960=CARTESIAN_POINT('Ctrl Pts',(-22.9868367391978,-1.73177409750193,
0.));
#199961=CARTESIAN_POINT('Ctrl Pts',(-22.9868367391978,-1.73177409750193,
12.));
#199962=CARTESIAN_POINT('Ctrl Pts',(-23.0014891601891,-1.72978594832137,
0.));
#199963=CARTESIAN_POINT('Ctrl Pts',(-23.0014891601891,-1.72978594832137,
12.));
#199964=CARTESIAN_POINT('Ctrl Pts',(-23.0162871884167,-1.72773175404702,
0.));
#199965=CARTESIAN_POINT('Ctrl Pts',(-23.0162871884167,-1.72773175404702,
12.));
#199966=CARTESIAN_POINT('Ctrl Pts',(-23.031229017888,-1.72561100564033,
0.));
#199967=CARTESIAN_POINT('Ctrl Pts',(-23.031229017888,-1.72561100564033,
12.));
#199968=CARTESIAN_POINT('Ctrl Pts',(-23.0463128785528,-1.72342320653731,
0.));
#199969=CARTESIAN_POINT('Ctrl Pts',(-23.0463128785528,-1.72342320653731,
12.));
#199970=CARTESIAN_POINT('Ctrl Pts',(-23.061537035156,-1.7211678722598,0.));
#199971=CARTESIAN_POINT('Ctrl Pts',(-23.061537035156,-1.7211678722598,12.));
#199972=CARTESIAN_POINT('Ctrl Pts',(-23.0768997860709,-1.71884453003027,
0.));
#199973=CARTESIAN_POINT('Ctrl Pts',(-23.0768997860709,-1.71884453003027,
12.));
#199974=CARTESIAN_POINT('Ctrl Pts',(-23.0923994621216,-1.71645271839311,
0.));
#199975=CARTESIAN_POINT('Ctrl Pts',(-23.0923994621216,-1.71645271839311,
12.));
#199976=CARTESIAN_POINT('Ctrl Pts',(-23.1080344254291,-1.71399198684724,
0.));
#199977=CARTESIAN_POINT('Ctrl Pts',(-23.1080344254291,-1.71399198684724,
12.));
#199978=CARTESIAN_POINT('Ctrl Pts',(-23.1238030684929,-1.71146189552192,
0.));
#199979=CARTESIAN_POINT('Ctrl Pts',(-23.1238030684929,-1.71146189552192,
12.));
#199980=CARTESIAN_POINT('Ctrl Pts',(-23.1397038132358,-1.7088620148546,
0.));
#199981=CARTESIAN_POINT('Ctrl Pts',(-23.1397038132358,-1.7088620148546,
12.));
#199982=CARTESIAN_POINT('Ctrl Pts',(-23.1557351100613,-1.70619192527847,
0.));
#199983=CARTESIAN_POINT('Ctrl Pts',(-23.1557351100613,-1.70619192527847,
12.));
#199984=CARTESIAN_POINT('Ctrl Pts',(-23.1718954368749,-1.70345121691259,
0.));
#199985=CARTESIAN_POINT('Ctrl Pts',(-23.1718954368749,-1.70345121691259,
12.));
#199986=CARTESIAN_POINT('Ctrl Pts',(-23.1881832981848,-1.70063948926987,
0.));
#199987=CARTESIAN_POINT('Ctrl Pts',(-23.1881832981848,-1.70063948926987,
12.));
#199988=CARTESIAN_POINT('Ctrl Pts',(-23.2045972243765,-1.69775635099425,
0.));
#199989=CARTESIAN_POINT('Ctrl Pts',(-23.2045972243765,-1.69775635099425,
12.));
#199990=CARTESIAN_POINT('Ctrl Pts',(-23.2211357709374,-1.69480141959945,
0.));
#199991=CARTESIAN_POINT('Ctrl Pts',(-23.2211357709374,-1.69480141959945,
12.));
#199992=CARTESIAN_POINT('Ctrl Pts',(-23.2377975177014,-1.69177432121716,
0.));
#199993=CARTESIAN_POINT('Ctrl Pts',(-23.2377975177014,-1.69177432121716,
12.));
#199994=CARTESIAN_POINT('Ctrl Pts',(-23.2545810680536,-1.6886746903491,
0.));
#199995=CARTESIAN_POINT('Ctrl Pts',(-23.2545810680536,-1.6886746903491,
12.));
#199996=CARTESIAN_POINT('Ctrl Pts',(-23.2714850482245,-1.68550216963275,
0.));
#199997=CARTESIAN_POINT('Ctrl Pts',(-23.2714850482245,-1.68550216963275,
12.));
#199998=CARTESIAN_POINT('Ctrl Pts',(-23.2885081066949,-1.68225640962181,
0.));
#199999=CARTESIAN_POINT('Ctrl Pts',(-23.2885081066949,-1.68225640962181,
12.));
#200000=CARTESIAN_POINT('Ctrl Pts',(-23.3056489135611,-1.67893706857123,
0.));
#200001=CARTESIAN_POINT('Ctrl Pts',(-23.3056489135611,-1.67893706857123,
12.));
#200002=CARTESIAN_POINT('Ctrl Pts',(-23.3229061599145,-1.67554381222987,
0.));
#200003=CARTESIAN_POINT('Ctrl Pts',(-23.3229061599145,-1.67554381222987,
12.));
#200004=CARTESIAN_POINT('Ctrl Pts',(-23.3402785571866,-1.67207631363905,
0.));
#200005=CARTESIAN_POINT('Ctrl Pts',(-23.3402785571866,-1.67207631363905,
12.));
#200006=CARTESIAN_POINT('Ctrl Pts',(-23.3577648365747,-1.66853425293977,
0.));
#200007=CARTESIAN_POINT('Ctrl Pts',(-23.3577648365747,-1.66853425293977,
12.));
#200008=CARTESIAN_POINT('Ctrl Pts',(-23.375363748555,-1.66491731718864,
0.));
#200009=CARTESIAN_POINT('Ctrl Pts',(-23.375363748555,-1.66491731718864,
12.));
#200010=CARTESIAN_POINT('Ctrl Pts',(-23.3930740623622,-1.66122520018008,
0.));
#200011=CARTESIAN_POINT('Ctrl Pts',(-23.3930740623622,-1.66122520018008,
12.));
#200012=CARTESIAN_POINT('Ctrl Pts',(-23.4108945654803,-1.65745760227507,
0.));
#200013=CARTESIAN_POINT('Ctrl Pts',(-23.4108945654803,-1.65745760227507,
12.));
#200014=CARTESIAN_POINT('Ctrl Pts',(-23.4288240631034,-1.6536142302373,
0.));
#200015=CARTESIAN_POINT('Ctrl Pts',(-23.4288240631034,-1.6536142302373,
12.));
#200016=CARTESIAN_POINT('Ctrl Pts',(-23.446861377656,-1.64969479707339,
0.));
#200017=CARTESIAN_POINT('Ctrl Pts',(-23.446861377656,-1.64969479707339,
12.));
#200018=CARTESIAN_POINT('Ctrl Pts',(-23.4650053483919,-1.64569902187608,
0.));
#200019=CARTESIAN_POINT('Ctrl Pts',(-23.4650053483919,-1.64569902187608,
12.));
#200020=CARTESIAN_POINT('Ctrl Pts',(-23.4832548309638,-1.64162662967524,
0.));
#200021=CARTESIAN_POINT('Ctrl Pts',(-23.4832548309638,-1.64162662967524,
12.));
#200022=CARTESIAN_POINT('Ctrl Pts',(-23.5016086970006,-1.63747735129474,
0.));
#200023=CARTESIAN_POINT('Ctrl Pts',(-23.5016086970006,-1.63747735129474,
12.));
#200024=CARTESIAN_POINT('Ctrl Pts',(-23.5200658336624,-1.63325092321731,
0.));
#200025=CARTESIAN_POINT('Ctrl Pts',(-23.5200658336624,-1.63325092321731,
12.));
#200026=CARTESIAN_POINT('Ctrl Pts',(-23.5386251432278,-1.62894708745231,
0.));
#200027=CARTESIAN_POINT('Ctrl Pts',(-23.5386251432278,-1.62894708745231,
12.));
#200028=CARTESIAN_POINT('Ctrl Pts',(-23.5572855427617,-1.62456559140072,
0.));
#200029=CARTESIAN_POINT('Ctrl Pts',(-23.5572855427617,-1.62456559140072,
12.));
#200030=CARTESIAN_POINT('Ctrl Pts',(-23.5760459637608,-1.62010618772869,
0.));
#200031=CARTESIAN_POINT('Ctrl Pts',(-23.5760459637608,-1.62010618772869,
12.));
#200032=CARTESIAN_POINT('Ctrl Pts',(-23.5949053517996,-1.61556863424697,
0.));
#200033=CARTESIAN_POINT('Ctrl Pts',(-23.5949053517996,-1.61556863424697,
12.));
#200034=CARTESIAN_POINT('Ctrl Pts',(-23.6138626661644,-1.61095269379773,
0.));
#200035=CARTESIAN_POINT('Ctrl Pts',(-23.6138626661644,-1.61095269379773,
12.));
#200036=CARTESIAN_POINT('Ctrl Pts',(-23.6329168794916,-1.60625813414666,
0.));
#200037=CARTESIAN_POINT('Ctrl Pts',(-23.6329168794916,-1.60625813414666,
12.));
#200038=CARTESIAN_POINT('Ctrl Pts',(-23.6520669774863,-1.60148472786588,
0.));
#200039=CARTESIAN_POINT('Ctrl Pts',(-23.6520669774863,-1.60148472786588,
12.));
#200040=CARTESIAN_POINT('Ctrl Pts',(-23.6713119586302,-1.59663225222458,
0.));
#200041=CARTESIAN_POINT('Ctrl Pts',(-23.6713119586302,-1.59663225222458,
12.));
#200042=CARTESIAN_POINT('Ctrl Pts',(-23.6906508338833,-1.59170048908631,
0.));
#200043=CARTESIAN_POINT('Ctrl Pts',(-23.6906508338833,-1.59170048908631,
12.));
#200044=CARTESIAN_POINT('Ctrl Pts',(-23.7100826263835,-1.58668922481222,
0.));
#200045=CARTESIAN_POINT('Ctrl Pts',(-23.7100826263835,-1.58668922481222,
12.));
#200046=CARTESIAN_POINT('Ctrl Pts',(-23.7296063711308,-1.58159825017362,
0.));
#200047=CARTESIAN_POINT('Ctrl Pts',(-23.7296063711308,-1.58159825017362,
12.));
#200048=CARTESIAN_POINT('Ctrl Pts',(-23.7492211147369,-1.57642736025251,
0.));
#200049=CARTESIAN_POINT('Ctrl Pts',(-23.7492211147369,-1.57642736025251,
12.));
#200050=CARTESIAN_POINT('Ctrl Pts',(-23.7689259151869,-1.57117635434412,
0.));
#200051=CARTESIAN_POINT('Ctrl Pts',(-23.7689259151869,-1.57117635434412,
12.));
#200052=CARTESIAN_POINT('Ctrl Pts',(-23.788719841588,-1.56584503586844,
0.));
#200053=CARTESIAN_POINT('Ctrl Pts',(-23.788719841588,-1.56584503586844,
12.));
#200054=CARTESIAN_POINT('Ctrl Pts',(-23.8086019739192,-1.56043321228631,
0.));
#200055=CARTESIAN_POINT('Ctrl Pts',(-23.8086019739192,-1.56043321228631,
12.));
#200056=CARTESIAN_POINT('Ctrl Pts',(-23.8285714027631,-1.55494069502628,
0.));
#200057=CARTESIAN_POINT('Ctrl Pts',(-23.8285714027631,-1.55494069502628,
12.));
#200058=CARTESIAN_POINT('Ctrl Pts',(-23.8486272290698,-1.5493672994053,
0.));
#200059=CARTESIAN_POINT('Ctrl Pts',(-23.8486272290698,-1.5493672994053,
12.));
#200060=CARTESIAN_POINT('Ctrl Pts',(-23.8687685639635,-1.54371284453978,
0.));
#200061=CARTESIAN_POINT('Ctrl Pts',(-23.8687685639635,-1.54371284453978,
12.));
#200062=CARTESIAN_POINT('Ctrl Pts',(-23.8889945285313,-1.53797715326748,
0.));
#200063=CARTESIAN_POINT('Ctrl Pts',(-23.8889945285313,-1.53797715326748,
12.));
#200064=CARTESIAN_POINT('Ctrl Pts',(-23.9093042536119,-1.53216005207462,
0.));
#200065=CARTESIAN_POINT('Ctrl Pts',(-23.9093042536119,-1.53216005207462,
12.));
#200066=CARTESIAN_POINT('Ctrl Pts',(-23.9296968795761,-1.52626137103039,
0.));
#200067=CARTESIAN_POINT('Ctrl Pts',(-23.9296968795761,-1.52626137103039,
12.));
#200068=CARTESIAN_POINT('Ctrl Pts',(-23.9501715561038,-1.52028094372806,
0.));
#200069=CARTESIAN_POINT('Ctrl Pts',(-23.9501715561038,-1.52028094372806,
12.));
#200070=CARTESIAN_POINT('Ctrl Pts',(-23.9707274420145,-1.51421860720628,
0.));
#200071=CARTESIAN_POINT('Ctrl Pts',(-23.9707274420145,-1.51421860720628,
12.));
#200072=CARTESIAN_POINT('Ctrl Pts',(-23.991363705093,-1.50807420187702,
0.));
#200073=CARTESIAN_POINT('Ctrl Pts',(-23.991363705093,-1.50807420187702,
12.));
#200074=CARTESIAN_POINT('Ctrl Pts',(-24.0120795219086,-1.50184757146099,
0.));
#200075=CARTESIAN_POINT('Ctrl Pts',(-24.0120795219086,-1.50184757146099,
12.));
#200076=CARTESIAN_POINT('Ctrl Pts',(-24.0328740776331,-1.49553856292798,
0.));
#200077=CARTESIAN_POINT('Ctrl Pts',(-24.0328740776331,-1.49553856292798,
12.));
#200078=CARTESIAN_POINT('Ctrl Pts',(-24.053746565843,-1.48914702644883,
0.));
#200079=CARTESIAN_POINT('Ctrl Pts',(-24.053746565843,-1.48914702644883,
12.));
#200080=CARTESIAN_POINT('Ctrl Pts',(-24.074696188353,-1.4826728153368,0.));
#200081=CARTESIAN_POINT('Ctrl Pts',(-24.074696188353,-1.4826728153368,12.));
#200082=CARTESIAN_POINT('Ctrl Pts',(-24.0957221550782,-1.47611578597741,
0.));
#200083=CARTESIAN_POINT('Ctrl Pts',(-24.0957221550782,-1.47611578597741,
12.));
#200084=CARTESIAN_POINT('Ctrl Pts',(-24.1168236838827,-1.46947579776992,
0.));
#200085=CARTESIAN_POINT('Ctrl Pts',(-24.1168236838827,-1.46947579776992,
12.));
#200086=CARTESIAN_POINT('Ctrl Pts',(-24.1380000004272,-1.46275271307398,
0.));
#200087=CARTESIAN_POINT('Ctrl Pts',(-24.1380000004272,-1.46275271307398,
12.));
#200088=CARTESIAN_POINT('Ctrl Pts',(-24.1592503380105,-1.45594639716314,
0.));
#200089=CARTESIAN_POINT('Ctrl Pts',(-24.1592503380105,-1.45594639716314,
12.));
#200090=CARTESIAN_POINT('Ctrl Pts',(-24.1805739374033,-1.44905671818721,
0.));
#200091=CARTESIAN_POINT('Ctrl Pts',(-24.1805739374033,-1.44905671818721,
12.));
#200092=CARTESIAN_POINT('Ctrl Pts',(-24.2019700467214,-1.44208354711074,
0.));
#200093=CARTESIAN_POINT('Ctrl Pts',(-24.2019700467214,-1.44208354711074,
12.));
#200094=CARTESIAN_POINT('Ctrl Pts',(-24.2234379212978,-1.43502675765502,
0.));
#200095=CARTESIAN_POINT('Ctrl Pts',(-24.2234379212978,-1.43502675765502,
12.));
#200096=CARTESIAN_POINT('Ctrl Pts',(-24.2449768235485,-1.42788622624851,
0.));
#200097=CARTESIAN_POINT('Ctrl Pts',(-24.2449768235485,-1.42788622624851,
12.));
#200098=CARTESIAN_POINT('Ctrl Pts',(-24.2665860228357,-1.42066183198252,
0.));
#200099=CARTESIAN_POINT('Ctrl Pts',(-24.2665860228357,-1.42066183198252,
12.));
#200100=CARTESIAN_POINT('Ctrl Pts',(-24.2882647953214,-1.41335345657685,
0.));
#200101=CARTESIAN_POINT('Ctrl Pts',(-24.2882647953214,-1.41335345657685,
12.));
#200102=CARTESIAN_POINT('Ctrl Pts',(-24.3100124238316,-1.4059609843434,
0.));
#200103=CARTESIAN_POINT('Ctrl Pts',(-24.3100124238316,-1.4059609843434,
12.));
#200104=CARTESIAN_POINT('Ctrl Pts',(-24.3318281977647,-1.3984843021281,
0.));
#200105=CARTESIAN_POINT('Ctrl Pts',(-24.3318281977647,-1.3984843021281,
12.));
#200106=CARTESIAN_POINT('Ctrl Pts',(-24.3537114129877,-1.3909232992639,
0.));
#200107=CARTESIAN_POINT('Ctrl Pts',(-24.3537114129877,-1.3909232992639,
12.));
#200108=CARTESIAN_POINT('Ctrl Pts',(-24.37566137173,-1.38327786752998,0.));
#200109=CARTESIAN_POINT('Ctrl Pts',(-24.37566137173,-1.38327786752998,12.));
#200110=CARTESIAN_POINT('Ctrl Pts',(-24.3976773824731,-1.37554790111607,
0.));
#200111=CARTESIAN_POINT('Ctrl Pts',(-24.3976773824731,-1.37554790111607,
12.));
#200112=CARTESIAN_POINT('Ctrl Pts',(-24.4197587598337,-1.36773329659954,
0.));
#200113=CARTESIAN_POINT('Ctrl Pts',(-24.4197587598337,-1.36773329659954,
12.));
#200114=CARTESIAN_POINT('Ctrl Pts',(-24.4419048244524,-1.35983395290624,
0.));
#200115=CARTESIAN_POINT('Ctrl Pts',(-24.4419048244524,-1.35983395290624,
12.));
#200116=CARTESIAN_POINT('Ctrl Pts',(-24.4641149028894,-1.35184977125644,
0.));
#200117=CARTESIAN_POINT('Ctrl Pts',(-24.4641149028894,-1.35184977125644,
12.));
#200118=CARTESIAN_POINT('Ctrl Pts',(-24.4863883275135,-1.34378065512335,
0.));
#200119=CARTESIAN_POINT('Ctrl Pts',(-24.4863883275135,-1.34378065512335,
12.));
#200120=CARTESIAN_POINT('Ctrl Pts',(-24.5087244363856,-1.33562651019684,
0.));
#200121=CARTESIAN_POINT('Ctrl Pts',(-24.5087244363856,-1.33562651019684,
12.));
#200122=CARTESIAN_POINT('Ctrl Pts',(-24.5311225731434,-1.32738724435326,
0.));
#200123=CARTESIAN_POINT('Ctrl Pts',(-24.5311225731434,-1.32738724435326,
12.));
#200124=CARTESIAN_POINT('Ctrl Pts',(-24.5535820868671,-1.31906276763669,
0.));
#200125=CARTESIAN_POINT('Ctrl Pts',(-24.5535820868671,-1.31906276763669,
12.));
#200126=CARTESIAN_POINT('Ctrl Pts',(-24.576102332018,-1.31065299222023,
0.));
#200127=CARTESIAN_POINT('Ctrl Pts',(-24.576102332018,-1.31065299222023,
12.));
#200128=CARTESIAN_POINT('Ctrl Pts',(-24.5986826684025,-1.30215783236364,
0.));
#200129=CARTESIAN_POINT('Ctrl Pts',(-24.5986826684025,-1.30215783236364,
12.));
#200130=CARTESIAN_POINT('Ctrl Pts',(-24.6213224611228,-1.29357720438107,
0.));
#200131=CARTESIAN_POINT('Ctrl Pts',(-24.6213224611228,-1.29357720438107,
12.));
#200132=CARTESIAN_POINT('Ctrl Pts',(-24.6440210805278,-1.28491102661513,
0.));
#200133=CARTESIAN_POINT('Ctrl Pts',(-24.6440210805278,-1.28491102661513,
12.));
#200134=CARTESIAN_POINT('Ctrl Pts',(-24.666777902156,-1.2761592194164,0.));
#200135=CARTESIAN_POINT('Ctrl Pts',(-24.666777902156,-1.2761592194164,12.));
#200136=CARTESIAN_POINT('Ctrl Pts',(-24.6895923066837,-1.26732170513497,
0.));
#200137=CARTESIAN_POINT('Ctrl Pts',(-24.6895923066837,-1.26732170513497,
12.));
#200138=CARTESIAN_POINT('Ctrl Pts',(-24.7124636797895,-1.25839840807415,
0.));
#200139=CARTESIAN_POINT('Ctrl Pts',(-24.7124636797895,-1.25839840807415,
12.));
#200140=CARTESIAN_POINT('Ctrl Pts',(-24.7353914120012,-1.24938925444323,
0.));
#200141=CARTESIAN_POINT('Ctrl Pts',(-24.7353914120012,-1.24938925444323,
12.));
#200142=CARTESIAN_POINT('Ctrl Pts',(-24.7583748985439,-1.24029417231988,
0.));
#200143=CARTESIAN_POINT('Ctrl Pts',(-24.7583748985439,-1.24029417231988,
12.));
#200144=CARTESIAN_POINT('Ctrl Pts',(-24.78141353918,-1.23111309161843,0.));
#200145=CARTESIAN_POINT('Ctrl Pts',(-24.78141353918,-1.23111309161843,12.));
#200146=CARTESIAN_POINT('Ctrl Pts',(-24.8045067380536,-1.22184594406526,
0.));
#200147=CARTESIAN_POINT('Ctrl Pts',(-24.8045067380536,-1.22184594406526,
12.));
#200148=CARTESIAN_POINT('Ctrl Pts',(-24.8276539035092,-1.21249266318205,
0.));
#200149=CARTESIAN_POINT('Ctrl Pts',(-24.8276539035092,-1.21249266318205,
12.));
#200150=CARTESIAN_POINT('Ctrl Pts',(-24.8508544481973,-1.20305318426015,
0.));
#200151=CARTESIAN_POINT('Ctrl Pts',(-24.8508544481973,-1.20305318426015,
12.));
#200152=CARTESIAN_POINT('Ctrl Pts',(-24.8741077892074,-1.19352744434059,
0.));
#200153=CARTESIAN_POINT('Ctrl Pts',(-24.8741077892074,-1.19352744434059,
12.));
#200154=CARTESIAN_POINT('Ctrl Pts',(-24.8974133481829,-1.18391538220098,
0.));
#200155=CARTESIAN_POINT('Ctrl Pts',(-24.8974133481829,-1.18391538220098,
12.));
#200156=CARTESIAN_POINT('Ctrl Pts',(-24.9207705514449,-1.17421693835039,
0.));
#200157=CARTESIAN_POINT('Ctrl Pts',(-24.9207705514449,-1.17421693835039,
12.));
#200158=CARTESIAN_POINT('Ctrl Pts',(-24.9441788300932,-1.16443205502852,
0.));
#200159=CARTESIAN_POINT('Ctrl Pts',(-24.9441788300932,-1.16443205502852,
12.));
#200160=CARTESIAN_POINT('Ctrl Pts',(-24.9676376201501,-1.15456067621894,
0.));
#200161=CARTESIAN_POINT('Ctrl Pts',(-24.9676376201501,-1.15456067621894,
12.));
#200162=CARTESIAN_POINT('Ctrl Pts',(-24.9911463621431,-1.14460274758206,
0.));
#200163=CARTESIAN_POINT('Ctrl Pts',(-24.9911463621431,-1.14460274758206,
12.));
#200164=CARTESIAN_POINT('Ctrl Pts',(-25.0147045006193,-1.13455821638535,
0.));
#200165=CARTESIAN_POINT('Ctrl Pts',(-25.0147045006193,-1.13455821638535,
12.));
#200166=CARTESIAN_POINT('Ctrl Pts',(-25.0383114836898,-1.12442703144455,
0.));
#200167=CARTESIAN_POINT('Ctrl Pts',(-25.0383114836898,-1.12442703144455,
12.));
#200168=CARTESIAN_POINT('Ctrl Pts',(-25.0619667625336,-1.1142091430689,
0.));
#200169=CARTESIAN_POINT('Ctrl Pts',(-25.0619667625336,-1.1142091430689,
12.));
#200170=CARTESIAN_POINT('Ctrl Pts',(-25.085669790968,-1.1039045030174,0.));
#200171=CARTESIAN_POINT('Ctrl Pts',(-25.085669790968,-1.1039045030174,12.));
#200172=CARTESIAN_POINT('Ctrl Pts',(-25.1094200248448,-1.09351306445299,
0.));
#200173=CARTESIAN_POINT('Ctrl Pts',(-25.1094200248448,-1.09351306445299,
12.));
#200174=CARTESIAN_POINT('Ctrl Pts',(-25.1332169227415,-1.08303478197174,
0.));
#200175=CARTESIAN_POINT('Ctrl Pts',(-25.1332169227415,-1.08303478197174,
12.));
#200176=CARTESIAN_POINT('Ctrl Pts',(-25.1570599469311,-1.0724696116546,
0.));
#200177=CARTESIAN_POINT('Ctrl Pts',(-25.1570599469311,-1.0724696116546,
12.));
#200178=CARTESIAN_POINT('Ctrl Pts',(-25.1809485642191,-1.06181751111754,
0.));
#200179=CARTESIAN_POINT('Ctrl Pts',(-25.1809485642191,-1.06181751111754,
12.));
#200180=CARTESIAN_POINT('Ctrl Pts',(-25.2048822469027,-1.05107843957925,
0.));
#200181=CARTESIAN_POINT('Ctrl Pts',(-25.2048822469027,-1.05107843957925,
12.));
#200182=CARTESIAN_POINT('Ctrl Pts',(-25.2288604735087,-1.04025235791515,
0.));
#200183=CARTESIAN_POINT('Ctrl Pts',(-25.2288604735087,-1.04025235791515,
12.));
#200184=CARTESIAN_POINT('Ctrl Pts',(-25.2528827300427,-1.0293392287683,
0.));
#200185=CARTESIAN_POINT('Ctrl Pts',(-25.2528827300427,-1.0293392287683,
12.));
#200186=CARTESIAN_POINT('Ctrl Pts',(-25.2769485087268,-1.01833901642272,
0.));
#200187=CARTESIAN_POINT('Ctrl Pts',(-25.2769485087268,-1.01833901642272,
12.));
#200188=CARTESIAN_POINT('Ctrl Pts',(-25.3010573055557,-1.00725168656933,
0.));
#200189=CARTESIAN_POINT('Ctrl Pts',(-25.3010573055557,-1.00725168656933,
12.));
#200190=CARTESIAN_POINT('Ctrl Pts',(-25.3252086182976,-0.996077206120919,
0.));
#200191=CARTESIAN_POINT('Ctrl Pts',(-25.3252086182976,-0.996077206120919,
12.));
#200192=CARTESIAN_POINT('Ctrl Pts',(-25.3494019441444,-0.984815543004089,
0.));
#200193=CARTESIAN_POINT('Ctrl Pts',(-25.3494019441444,-0.984815543004089,
12.));
#200194=CARTESIAN_POINT('Ctrl Pts',(-25.3736367778842,-0.973466666000048,
0.));
#200195=CARTESIAN_POINT('Ctrl Pts',(-25.3736367778842,-0.973466666000048,
12.));
#200196=CARTESIAN_POINT('Ctrl Pts',(-25.3979126089155,-0.962030544502802,
0.));
#200197=CARTESIAN_POINT('Ctrl Pts',(-25.3979126089155,-0.962030544502802,
12.));
#200198=CARTESIAN_POINT('Ctrl Pts',(-25.4222289223155,-0.950507148596968,
0.));
#200199=CARTESIAN_POINT('Ctrl Pts',(-25.4222289223155,-0.950507148596968,
12.));
#200200=CARTESIAN_POINT('Ctrl Pts',(-25.4465852044835,-0.938896449495632,
0.));
#200201=CARTESIAN_POINT('Ctrl Pts',(-25.4465852044835,-0.938896449495632,
12.));
#200202=CARTESIAN_POINT('Ctrl Pts',(-25.4709809474996,-0.927198419885604,
0.));
#200203=CARTESIAN_POINT('Ctrl Pts',(-25.4709809474996,-0.927198419885604,
12.));
#200204=CARTESIAN_POINT('Ctrl Pts',(-25.4954156541787,-0.915413034335333,
0.));
#200205=CARTESIAN_POINT('Ctrl Pts',(-25.4954156541787,-0.915413034335333,
12.));
#200206=CARTESIAN_POINT('Ctrl Pts',(-25.5198888424195,-0.903540269651154,
0.));
#200207=CARTESIAN_POINT('Ctrl Pts',(-25.5198888424195,-0.903540269651154,
12.));
#200208=CARTESIAN_POINT('Ctrl Pts',(-25.5444000508223,-0.891580105349467,
0.));
#200209=CARTESIAN_POINT('Ctrl Pts',(-25.5444000508223,-0.891580105349467,
12.));
#200210=CARTESIAN_POINT('Ctrl Pts',(-25.568948840818,-0.87953252383509,
0.));
#200211=CARTESIAN_POINT('Ctrl Pts',(-25.568948840818,-0.87953252383509,
12.));
#200212=CARTESIAN_POINT('Ctrl Pts',(-25.5935347843616,-0.86739750933947,
0.));
#200213=CARTESIAN_POINT('Ctrl Pts',(-25.5935347843616,-0.86739750933947,
12.));
#200214=CARTESIAN_POINT('Ctrl Pts',(-25.618157453608,-0.855175047037614,
0.));
#200215=CARTESIAN_POINT('Ctrl Pts',(-25.618157453608,-0.855175047037614,
12.));
#200216=CARTESIAN_POINT('Ctrl Pts',(-25.6428164100078,-0.842865122121544,
0.));
#200217=CARTESIAN_POINT('Ctrl Pts',(-25.6428164100078,-0.842865122121544,
12.));
#200218=CARTESIAN_POINT('Ctrl Pts',(-25.6675111931957,-0.830467718864367,
0.));
#200219=CARTESIAN_POINT('Ctrl Pts',(-25.6675111931957,-0.830467718864367,
12.));
#200220=CARTESIAN_POINT('Ctrl Pts',(-25.6922413110172,-0.817982819786719,
0.));
#200221=CARTESIAN_POINT('Ctrl Pts',(-25.6922413110172,-0.817982819786719,
12.));
#200222=CARTESIAN_POINT('Ctrl Pts',(-25.7170062262474,-0.805410404552594,
0.));
#200223=CARTESIAN_POINT('Ctrl Pts',(-25.7170062262474,-0.805410404552594,
12.));
#200224=CARTESIAN_POINT('Ctrl Pts',(-25.7418053757671,-0.792750451613534,
0.));
#200225=CARTESIAN_POINT('Ctrl Pts',(-25.7418053757671,-0.792750451613534,
12.));
#200226=CARTESIAN_POINT('Ctrl Pts',(-25.7666381946871,-0.780002940289025,
0.));
#200227=CARTESIAN_POINT('Ctrl Pts',(-25.7666381946871,-0.780002940289025,
12.));
#200228=CARTESIAN_POINT('Ctrl Pts',(-25.7915041383304,-0.767167852648639,
0.));
#200229=CARTESIAN_POINT('Ctrl Pts',(-25.7915041383304,-0.767167852648639,
12.));
#200230=CARTESIAN_POINT('Ctrl Pts',(-25.816402705995,-0.754245175608288,
0.));
#200231=CARTESIAN_POINT('Ctrl Pts',(-25.816402705995,-0.754245175608288,
12.));
#200232=CARTESIAN_POINT('Ctrl Pts',(-25.841333461908,-0.741234902664697,
0.));
#200233=CARTESIAN_POINT('Ctrl Pts',(-25.841333461908,-0.741234902664697,
12.));
#200234=CARTESIAN_POINT('Ctrl Pts',(-25.8662960624285,-0.728137036485877,
0.));
#200235=CARTESIAN_POINT('Ctrl Pts',(-25.8662960624285,-0.728137036485877,
12.));
#200236=CARTESIAN_POINT('Ctrl Pts',(-25.8912902615141,-0.714951588533753,
0.));
#200237=CARTESIAN_POINT('Ctrl Pts',(-25.8912902615141,-0.714951588533753,
12.));
#200238=CARTESIAN_POINT('Ctrl Pts',(-25.9163158909645,-0.701678575236602,
0.));
#200239=CARTESIAN_POINT('Ctrl Pts',(-25.9163158909645,-0.701678575236602,
12.));
#200240=CARTESIAN_POINT('Ctrl Pts',(-25.941372847213,-0.688318015065678,
0.));
#200241=CARTESIAN_POINT('Ctrl Pts',(-25.941372847213,-0.688318015065678,
12.));
#200242=CARTESIAN_POINT('Ctrl Pts',(-25.9614434298092,-0.677559543215902,
0.));
#200243=CARTESIAN_POINT('Ctrl Pts',(-25.9614434298092,-0.677559543215902,
12.));
#200244=CARTESIAN_POINT('Ctrl Pts',(-25.9765104298171,-0.669451306784415,
0.));
#200245=CARTESIAN_POINT('Ctrl Pts',(-25.9765104298171,-0.669451306784415,
12.));
#200246=CARTESIAN_POINT('Ctrl Pts',(-25.9865613464809,-0.664028313188912,
0.));
#200247=CARTESIAN_POINT('Ctrl Pts',(-25.9865613464809,-0.664028313188912,
12.));
#200248=CARTESIAN_POINT('Ctrl Pts',(-25.991588367311,-0.661312440730891,
0.));
#200249=CARTESIAN_POINT('Ctrl Pts',(-25.991588367311,-0.661312440730891,
12.));
#200250=CARTESIAN_POINT('',(-25.991588367311,-0.661312440730891,0.));
#200251=CARTESIAN_POINT('Ctrl Pts',(-22.4835757167854,-1.76341220531179,
0.));
#200252=CARTESIAN_POINT('Ctrl Pts',(-22.483581992979,-1.76341415538764,
0.));
#200253=CARTESIAN_POINT('Ctrl Pts',(-22.4836387052232,-1.7634206426357,
0.));
#200254=CARTESIAN_POINT('Ctrl Pts',(-22.483856251707,-1.76343813434565,
0.));
#200255=CARTESIAN_POINT('Ctrl Pts',(-22.4844112933129,-1.76347698284792,
0.));
#200256=CARTESIAN_POINT('Ctrl Pts',(-22.4855446605991,-1.76355076045546,
0.));
#200257=CARTESIAN_POINT('Ctrl Pts',(-22.4871115206571,-1.76364784232963,
0.));
#200258=CARTESIAN_POINT('Ctrl Pts',(-22.4890991659478,-1.76376424879505,
0.));
#200259=CARTESIAN_POINT('Ctrl Pts',(-22.4914909094908,-1.76389475965724,
0.));
#200260=CARTESIAN_POINT('Ctrl Pts',(-22.4942693792449,-1.764033938803,0.));
#200261=CARTESIAN_POINT('Ctrl Pts',(-22.4974203063191,-1.76417731243462,
0.));
#200262=CARTESIAN_POINT('Ctrl Pts',(-22.5009332677316,-1.76432160068725,
0.));
#200263=CARTESIAN_POINT('Ctrl Pts',(-22.5047996391978,-1.76446408210366,
0.));
#200264=CARTESIAN_POINT('Ctrl Pts',(-22.5090112700212,-1.76460218257323,
0.));
#200265=CARTESIAN_POINT('Ctrl Pts',(-22.5135590569554,-1.76473303281159,
0.));
#200266=CARTESIAN_POINT('Ctrl Pts',(-22.5184336670207,-1.76485369319896,
0.));
#200267=CARTESIAN_POINT('Ctrl Pts',(-22.5236259635515,-1.76496128643369,
0.));
#200268=CARTESIAN_POINT('Ctrl Pts',(-22.529127665298,-1.76505320262751,
0.));
#200269=CARTESIAN_POINT('Ctrl Pts',(-22.5349313983571,-1.7651271156325,
0.));
#200270=CARTESIAN_POINT('Ctrl Pts',(-22.5410303590891,-1.76518087841492,
0.));
#200271=CARTESIAN_POINT('Ctrl Pts',(-22.5474180954006,-1.76521245524047,
0.));
#200272=CARTESIAN_POINT('Ctrl Pts',(-22.5540882235837,-1.76521983384063,
0.));
#200273=CARTESIAN_POINT('Ctrl Pts',(-22.5610344912501,-1.76520104500449,
0.));
#200274=CARTESIAN_POINT('Ctrl Pts',(-22.5682508499873,-1.76515418518829,
0.));
#200275=CARTESIAN_POINT('Ctrl Pts',(-22.5757315316355,-1.76507744026747,
0.));
#200276=CARTESIAN_POINT('Ctrl Pts',(-22.5834711038024,-1.76496910283088,
0.));
#200277=CARTESIAN_POINT('Ctrl Pts',(-22.5914644078106,-1.76482755288411,
0.));
#200278=CARTESIAN_POINT('Ctrl Pts',(-22.5997065145638,-1.76465124413556,
0.));
#200279=CARTESIAN_POINT('Ctrl Pts',(-22.6081926681342,-1.76443868648015,
0.));
#200280=CARTESIAN_POINT('Ctrl Pts',(-22.6169182517693,-1.76418843543739,
0.));
#200281=CARTESIAN_POINT('Ctrl Pts',(-22.6258787994847,-1.76389909571402,
0.));
#200282=CARTESIAN_POINT('Ctrl Pts',(-22.635069997936,-1.76356932176272,
0.));
#200283=CARTESIAN_POINT('Ctrl Pts',(-22.6444876940425,-1.76319782013914,
0.));
#200284=CARTESIAN_POINT('Ctrl Pts',(-22.6541278938413,-1.76278334912559,
0.));
#200285=CARTESIAN_POINT('Ctrl Pts',(-22.6639867471756,-1.76232471392567,
0.));
#200286=CARTESIAN_POINT('Ctrl Pts',(-22.6740605356699,-1.76182076289525,
0.));
#200287=CARTESIAN_POINT('Ctrl Pts',(-22.6843456585245,-1.76127038310612,
0.));
#200288=CARTESIAN_POINT('Ctrl Pts',(-22.6948386219843,-1.76067249704884,
0.));
#200289=CARTESIAN_POINT('Ctrl Pts',(-22.7055360375481,-1.76002606202399,
0.));
#200290=CARTESIAN_POINT('Ctrl Pts',(-22.7164346186007,-1.75933006905924,
0.));
#200291=CARTESIAN_POINT('Ctrl Pts',(-22.7275311777305,-1.75858354204635,
0.));
#200292=CARTESIAN_POINT('Ctrl Pts',(-22.7388226235565,-1.75778553673249,
0.));
#200293=CARTESIAN_POINT('Ctrl Pts',(-22.7503059556455,-1.75693513908911,
0.));
#200294=CARTESIAN_POINT('Ctrl Pts',(-22.7619782595013,-1.7560314637164,
0.));
#200295=CARTESIAN_POINT('Ctrl Pts',(-22.7738367016115,-1.75507365227127,
0.));
#200296=CARTESIAN_POINT('Ctrl Pts',(-22.7858785242358,-1.75406087182929,
0.));
#200297=CARTESIAN_POINT('Ctrl Pts',(-22.7981010424312,-1.75299231391461,
0.));
#200298=CARTESIAN_POINT('Ctrl Pts',(-22.8105016414712,-1.75186719365589,
0.));
#200299=CARTESIAN_POINT('Ctrl Pts',(-22.8230777741285,-1.75068474890884,
0.));
#200300=CARTESIAN_POINT('Ctrl Pts',(-22.8358269579854,-1.74944423940117,
0.));
#200301=CARTESIAN_POINT('Ctrl Pts',(-22.8487467728075,-1.74814494588492,
0.));
#200302=CARTESIAN_POINT('Ctrl Pts',(-22.8618348580234,-1.74678616930663,
0.));
#200303=CARTESIAN_POINT('Ctrl Pts',(-22.8750889101696,-1.745367229982,0.));
#200304=CARTESIAN_POINT('Ctrl Pts',(-22.8885066803351,-1.74388746677702,
0.));
#200305=CARTESIAN_POINT('Ctrl Pts',(-22.9020859716144,-1.74234623630079,
0.));
#200306=CARTESIAN_POINT('Ctrl Pts',(-22.9158246373365,-1.74074291231057,
0.));
#200307=CARTESIAN_POINT('Ctrl Pts',(-22.9297205792587,-1.73907688511664,
0.));
#200308=CARTESIAN_POINT('Ctrl Pts',(-22.9437717457825,-1.73734756100038,
0.));
#200309=CARTESIAN_POINT('Ctrl Pts',(-22.9579761301062,-1.73555436162771,
0.));
#200310=CARTESIAN_POINT('Ctrl Pts',(-22.9723317685688,-1.73369672350817,
0.));
#200311=CARTESIAN_POINT('Ctrl Pts',(-22.9868367391978,-1.73177409750193,
0.));
#200312=CARTESIAN_POINT('Ctrl Pts',(-23.0014891601891,-1.72978594832137,
0.));
#200313=CARTESIAN_POINT('Ctrl Pts',(-23.0162871884167,-1.72773175404702,
0.));
#200314=CARTESIAN_POINT('Ctrl Pts',(-23.031229017888,-1.72561100564033,
0.));
#200315=CARTESIAN_POINT('Ctrl Pts',(-23.0463128785528,-1.72342320653731,
0.));
#200316=CARTESIAN_POINT('Ctrl Pts',(-23.061537035156,-1.7211678722598,0.));
#200317=CARTESIAN_POINT('Ctrl Pts',(-23.0768997860709,-1.71884453003027,
0.));
#200318=CARTESIAN_POINT('Ctrl Pts',(-23.0923994621216,-1.71645271839311,
0.));
#200319=CARTESIAN_POINT('Ctrl Pts',(-23.1080344254291,-1.71399198684724,
0.));
#200320=CARTESIAN_POINT('Ctrl Pts',(-23.1238030684929,-1.71146189552192,
0.));
#200321=CARTESIAN_POINT('Ctrl Pts',(-23.1397038132358,-1.7088620148546,
0.));
#200322=CARTESIAN_POINT('Ctrl Pts',(-23.1557351100613,-1.70619192527847,
0.));
#200323=CARTESIAN_POINT('Ctrl Pts',(-23.1718954368749,-1.70345121691259,
0.));
#200324=CARTESIAN_POINT('Ctrl Pts',(-23.1881832981848,-1.70063948926987,
0.));
#200325=CARTESIAN_POINT('Ctrl Pts',(-23.2045972243765,-1.69775635099425,
0.));
#200326=CARTESIAN_POINT('Ctrl Pts',(-23.2211357709374,-1.69480141959945,
0.));
#200327=CARTESIAN_POINT('Ctrl Pts',(-23.2377975177014,-1.69177432121716,
0.));
#200328=CARTESIAN_POINT('Ctrl Pts',(-23.2545810680536,-1.6886746903491,
0.));
#200329=CARTESIAN_POINT('Ctrl Pts',(-23.2714850482245,-1.68550216963275,
0.));
#200330=CARTESIAN_POINT('Ctrl Pts',(-23.2885081066949,-1.68225640962181,
0.));
#200331=CARTESIAN_POINT('Ctrl Pts',(-23.3056489135611,-1.67893706857123,
0.));
#200332=CARTESIAN_POINT('Ctrl Pts',(-23.3229061599145,-1.67554381222987,
0.));
#200333=CARTESIAN_POINT('Ctrl Pts',(-23.3402785571866,-1.67207631363905,
0.));
#200334=CARTESIAN_POINT('Ctrl Pts',(-23.3577648365747,-1.66853425293977,
0.));
#200335=CARTESIAN_POINT('Ctrl Pts',(-23.375363748555,-1.66491731718864,
0.));
#200336=CARTESIAN_POINT('Ctrl Pts',(-23.3930740623622,-1.66122520018008,
0.));
#200337=CARTESIAN_POINT('Ctrl Pts',(-23.4108945654803,-1.65745760227507,
0.));
#200338=CARTESIAN_POINT('Ctrl Pts',(-23.4288240631034,-1.6536142302373,
0.));
#200339=CARTESIAN_POINT('Ctrl Pts',(-23.446861377656,-1.64969479707339,
0.));
#200340=CARTESIAN_POINT('Ctrl Pts',(-23.4650053483919,-1.64569902187608,
0.));
#200341=CARTESIAN_POINT('Ctrl Pts',(-23.4832548309638,-1.64162662967524,
0.));
#200342=CARTESIAN_POINT('Ctrl Pts',(-23.5016086970006,-1.63747735129474,
0.));
#200343=CARTESIAN_POINT('Ctrl Pts',(-23.5200658336624,-1.63325092321731,
0.));
#200344=CARTESIAN_POINT('Ctrl Pts',(-23.5386251432278,-1.62894708745231,
0.));
#200345=CARTESIAN_POINT('Ctrl Pts',(-23.5572855427617,-1.62456559140072,
0.));
#200346=CARTESIAN_POINT('Ctrl Pts',(-23.5760459637608,-1.62010618772869,
0.));
#200347=CARTESIAN_POINT('Ctrl Pts',(-23.5949053517996,-1.61556863424697,
0.));
#200348=CARTESIAN_POINT('Ctrl Pts',(-23.6138626661644,-1.61095269379773,
0.));
#200349=CARTESIAN_POINT('Ctrl Pts',(-23.6329168794916,-1.60625813414666,
0.));
#200350=CARTESIAN_POINT('Ctrl Pts',(-23.6520669774863,-1.60148472786588,
0.));
#200351=CARTESIAN_POINT('Ctrl Pts',(-23.6713119586302,-1.59663225222458,
0.));
#200352=CARTESIAN_POINT('Ctrl Pts',(-23.6906508338833,-1.59170048908631,
0.));
#200353=CARTESIAN_POINT('Ctrl Pts',(-23.7100826263835,-1.58668922481222,
0.));
#200354=CARTESIAN_POINT('Ctrl Pts',(-23.7296063711308,-1.58159825017362,
0.));
#200355=CARTESIAN_POINT('Ctrl Pts',(-23.7492211147369,-1.57642736025251,
0.));
#200356=CARTESIAN_POINT('Ctrl Pts',(-23.7689259151869,-1.57117635434412,
0.));
#200357=CARTESIAN_POINT('Ctrl Pts',(-23.788719841588,-1.56584503586844,
0.));
#200358=CARTESIAN_POINT('Ctrl Pts',(-23.8086019739192,-1.56043321228631,
0.));
#200359=CARTESIAN_POINT('Ctrl Pts',(-23.8285714027631,-1.55494069502628,
0.));
#200360=CARTESIAN_POINT('Ctrl Pts',(-23.8486272290698,-1.5493672994053,
0.));
#200361=CARTESIAN_POINT('Ctrl Pts',(-23.8687685639635,-1.54371284453978,
0.));
#200362=CARTESIAN_POINT('Ctrl Pts',(-23.8889945285313,-1.53797715326748,
0.));
#200363=CARTESIAN_POINT('Ctrl Pts',(-23.9093042536119,-1.53216005207462,
0.));
#200364=CARTESIAN_POINT('Ctrl Pts',(-23.9296968795761,-1.52626137103039,
0.));
#200365=CARTESIAN_POINT('Ctrl Pts',(-23.9501715561038,-1.52028094372806,
0.));
#200366=CARTESIAN_POINT('Ctrl Pts',(-23.9707274420145,-1.51421860720628,
0.));
#200367=CARTESIAN_POINT('Ctrl Pts',(-23.991363705093,-1.50807420187702,
0.));
#200368=CARTESIAN_POINT('Ctrl Pts',(-24.0120795219086,-1.50184757146099,
0.));
#200369=CARTESIAN_POINT('Ctrl Pts',(-24.0328740776331,-1.49553856292798,
0.));
#200370=CARTESIAN_POINT('Ctrl Pts',(-24.053746565843,-1.48914702644883,
0.));
#200371=CARTESIAN_POINT('Ctrl Pts',(-24.074696188353,-1.4826728153368,0.));
#200372=CARTESIAN_POINT('Ctrl Pts',(-24.0957221550782,-1.47611578597741,
0.));
#200373=CARTESIAN_POINT('Ctrl Pts',(-24.1168236838827,-1.46947579776992,
0.));
#200374=CARTESIAN_POINT('Ctrl Pts',(-24.1380000004272,-1.46275271307398,
0.));
#200375=CARTESIAN_POINT('Ctrl Pts',(-24.1592503380105,-1.45594639716314,
0.));
#200376=CARTESIAN_POINT('Ctrl Pts',(-24.1805739374033,-1.44905671818721,
0.));
#200377=CARTESIAN_POINT('Ctrl Pts',(-24.2019700467214,-1.44208354711074,
0.));
#200378=CARTESIAN_POINT('Ctrl Pts',(-24.2234379212978,-1.43502675765502,
0.));
#200379=CARTESIAN_POINT('Ctrl Pts',(-24.2449768235485,-1.42788622624851,
0.));
#200380=CARTESIAN_POINT('Ctrl Pts',(-24.2665860228357,-1.42066183198252,
0.));
#200381=CARTESIAN_POINT('Ctrl Pts',(-24.2882647953214,-1.41335345657685,
0.));
#200382=CARTESIAN_POINT('Ctrl Pts',(-24.3100124238316,-1.4059609843434,
0.));
#200383=CARTESIAN_POINT('Ctrl Pts',(-24.3318281977647,-1.3984843021281,
0.));
#200384=CARTESIAN_POINT('Ctrl Pts',(-24.3537114129877,-1.3909232992639,
0.));
#200385=CARTESIAN_POINT('Ctrl Pts',(-24.37566137173,-1.38327786752998,0.));
#200386=CARTESIAN_POINT('Ctrl Pts',(-24.3976773824731,-1.37554790111607,
0.));
#200387=CARTESIAN_POINT('Ctrl Pts',(-24.4197587598337,-1.36773329659954,
0.));
#200388=CARTESIAN_POINT('Ctrl Pts',(-24.4419048244524,-1.35983395290624,
0.));
#200389=CARTESIAN_POINT('Ctrl Pts',(-24.4641149028894,-1.35184977125644,
0.));
#200390=CARTESIAN_POINT('Ctrl Pts',(-24.4863883275135,-1.34378065512335,
0.));
#200391=CARTESIAN_POINT('Ctrl Pts',(-24.5087244363856,-1.33562651019684,
0.));
#200392=CARTESIAN_POINT('Ctrl Pts',(-24.5311225731434,-1.32738724435326,
0.));
#200393=CARTESIAN_POINT('Ctrl Pts',(-24.5535820868671,-1.31906276763669,
0.));
#200394=CARTESIAN_POINT('Ctrl Pts',(-24.576102332018,-1.31065299222023,
0.));
#200395=CARTESIAN_POINT('Ctrl Pts',(-24.5986826684025,-1.30215783236364,
0.));
#200396=CARTESIAN_POINT('Ctrl Pts',(-24.6213224611228,-1.29357720438107,
0.));
#200397=CARTESIAN_POINT('Ctrl Pts',(-24.6440210805278,-1.28491102661513,
0.));
#200398=CARTESIAN_POINT('Ctrl Pts',(-24.666777902156,-1.2761592194164,0.));
#200399=CARTESIAN_POINT('Ctrl Pts',(-24.6895923066837,-1.26732170513497,
0.));
#200400=CARTESIAN_POINT('Ctrl Pts',(-24.7124636797895,-1.25839840807415,
0.));
#200401=CARTESIAN_POINT('Ctrl Pts',(-24.7353914120012,-1.24938925444323,
0.));
#200402=CARTESIAN_POINT('Ctrl Pts',(-24.7583748985439,-1.24029417231988,
0.));
#200403=CARTESIAN_POINT('Ctrl Pts',(-24.78141353918,-1.23111309161843,0.));
#200404=CARTESIAN_POINT('Ctrl Pts',(-24.8045067380536,-1.22184594406526,
0.));
#200405=CARTESIAN_POINT('Ctrl Pts',(-24.8276539035092,-1.21249266318205,
0.));
#200406=CARTESIAN_POINT('Ctrl Pts',(-24.8508544481973,-1.20305318426015,
0.));
#200407=CARTESIAN_POINT('Ctrl Pts',(-24.8741077892074,-1.19352744434059,
0.));
#200408=CARTESIAN_POINT('Ctrl Pts',(-24.8974133481829,-1.18391538220098,
0.));
#200409=CARTESIAN_POINT('Ctrl Pts',(-24.9207705514449,-1.17421693835039,
0.));
#200410=CARTESIAN_POINT('Ctrl Pts',(-24.9441788300932,-1.16443205502852,
0.));
#200411=CARTESIAN_POINT('Ctrl Pts',(-24.9676376201501,-1.15456067621894,
0.));
#200412=CARTESIAN_POINT('Ctrl Pts',(-24.9911463621431,-1.14460274758206,
0.));
#200413=CARTESIAN_POINT('Ctrl Pts',(-25.0147045006193,-1.13455821638535,
0.));
#200414=CARTESIAN_POINT('Ctrl Pts',(-25.0383114836898,-1.12442703144455,
0.));
#200415=CARTESIAN_POINT('Ctrl Pts',(-25.0619667625336,-1.1142091430689,
0.));
#200416=CARTESIAN_POINT('Ctrl Pts',(-25.085669790968,-1.1039045030174,0.));
#200417=CARTESIAN_POINT('Ctrl Pts',(-25.1094200248448,-1.09351306445299,
0.));
#200418=CARTESIAN_POINT('Ctrl Pts',(-25.1332169227415,-1.08303478197174,
0.));
#200419=CARTESIAN_POINT('Ctrl Pts',(-25.1570599469311,-1.0724696116546,
0.));
#200420=CARTESIAN_POINT('Ctrl Pts',(-25.1809485642191,-1.06181751111754,
0.));
#200421=CARTESIAN_POINT('Ctrl Pts',(-25.2048822469027,-1.05107843957925,
0.));
#200422=CARTESIAN_POINT('Ctrl Pts',(-25.2288604735087,-1.04025235791515,
0.));
#200423=CARTESIAN_POINT('Ctrl Pts',(-25.2528827300427,-1.0293392287683,
0.));
#200424=CARTESIAN_POINT('Ctrl Pts',(-25.2769485087268,-1.01833901642272,
0.));
#200425=CARTESIAN_POINT('Ctrl Pts',(-25.3010573055557,-1.00725168656933,
0.));
#200426=CARTESIAN_POINT('Ctrl Pts',(-25.3252086182976,-0.996077206120919,
0.));
#200427=CARTESIAN_POINT('Ctrl Pts',(-25.3494019441444,-0.984815543004089,
0.));
#200428=CARTESIAN_POINT('Ctrl Pts',(-25.3736367778842,-0.973466666000048,
0.));
#200429=CARTESIAN_POINT('Ctrl Pts',(-25.3979126089155,-0.962030544502802,
0.));
#200430=CARTESIAN_POINT('Ctrl Pts',(-25.4222289223155,-0.950507148596968,
0.));
#200431=CARTESIAN_POINT('Ctrl Pts',(-25.4465852044835,-0.938896449495632,
0.));
#200432=CARTESIAN_POINT('Ctrl Pts',(-25.4709809474996,-0.927198419885604,
0.));
#200433=CARTESIAN_POINT('Ctrl Pts',(-25.4954156541787,-0.915413034335333,
0.));
#200434=CARTESIAN_POINT('Ctrl Pts',(-25.5198888424195,-0.903540269651154,
0.));
#200435=CARTESIAN_POINT('Ctrl Pts',(-25.5444000508223,-0.891580105349467,
0.));
#200436=CARTESIAN_POINT('Ctrl Pts',(-25.568948840818,-0.87953252383509,
0.));
#200437=CARTESIAN_POINT('Ctrl Pts',(-25.5935347843616,-0.86739750933947,
0.));
#200438=CARTESIAN_POINT('Ctrl Pts',(-25.618157453608,-0.855175047037614,
0.));
#200439=CARTESIAN_POINT('Ctrl Pts',(-25.6428164100078,-0.842865122121544,
0.));
#200440=CARTESIAN_POINT('Ctrl Pts',(-25.6675111931957,-0.830467718864367,
0.));
#200441=CARTESIAN_POINT('Ctrl Pts',(-25.6922413110172,-0.817982819786719,
0.));
#200442=CARTESIAN_POINT('Ctrl Pts',(-25.7170062262474,-0.805410404552594,
0.));
#200443=CARTESIAN_POINT('Ctrl Pts',(-25.7418053757671,-0.792750451613534,
0.));
#200444=CARTESIAN_POINT('Ctrl Pts',(-25.7666381946871,-0.780002940289025,
0.));
#200445=CARTESIAN_POINT('Ctrl Pts',(-25.7915041383304,-0.767167852648639,
0.));
#200446=CARTESIAN_POINT('Ctrl Pts',(-25.816402705995,-0.754245175608288,
0.));
#200447=CARTESIAN_POINT('Ctrl Pts',(-25.841333461908,-0.741234902664697,
0.));
#200448=CARTESIAN_POINT('Ctrl Pts',(-25.8662960624285,-0.728137036485877,
0.));
#200449=CARTESIAN_POINT('Ctrl Pts',(-25.8912902615141,-0.714951588533753,
0.));
#200450=CARTESIAN_POINT('Ctrl Pts',(-25.9163158909645,-0.701678575236602,
0.));
#200451=CARTESIAN_POINT('Ctrl Pts',(-25.941372847213,-0.688318015065678,
0.));
#200452=CARTESIAN_POINT('Ctrl Pts',(-25.9614434298092,-0.677559543215902,
0.));
#200453=CARTESIAN_POINT('Ctrl Pts',(-25.9765104298171,-0.669451306784415,
0.));
#200454=CARTESIAN_POINT('Ctrl Pts',(-25.9865613464809,-0.664028313188912,
0.));
#200455=CARTESIAN_POINT('Ctrl Pts',(-25.991588367311,-0.661312440730891,
0.));
#200456=CARTESIAN_POINT('',(-25.991588367311,-0.661312440730891,0.));
#200457=CARTESIAN_POINT('Origin',(-21.1389261070099,3.92374859571501,0.));
#200458=CARTESIAN_POINT('',(-22.1738711152697,4.11585220600461,0.));
#200459=CARTESIAN_POINT('',(-22.1738711152697,4.11585220600461,0.));
#200460=CARTESIAN_POINT('',(-10.5694630535049,1.96187429785751,0.));
#200461=CARTESIAN_POINT('Ctrl Pts',(-25.991588367311,0.661312440730901,
0.));
#200462=CARTESIAN_POINT('Ctrl Pts',(-25.991588367311,0.661312440730901,
12.));
#200463=CARTESIAN_POINT('Ctrl Pts',(-25.9865613464773,0.664028313187627,
0.));
#200464=CARTESIAN_POINT('Ctrl Pts',(-25.9865613464773,0.664028313187627,
12.));
#200465=CARTESIAN_POINT('Ctrl Pts',(-25.9765104298071,0.669451306780825,
0.));
#200466=CARTESIAN_POINT('Ctrl Pts',(-25.9765104298071,0.669451306780825,
12.));
#200467=CARTESIAN_POINT('Ctrl Pts',(-25.9614434297919,0.677559543209725,
0.));
#200468=CARTESIAN_POINT('Ctrl Pts',(-25.9614434297919,0.677559543209725,
12.));
#200469=CARTESIAN_POINT('Ctrl Pts',(-25.9413728471909,0.688318015057729,
0.));
#200470=CARTESIAN_POINT('Ctrl Pts',(-25.9413728471909,0.688318015057729,
12.));
#200471=CARTESIAN_POINT('Ctrl Pts',(-25.9163158909426,0.701678575228756,
0.));
#200472=CARTESIAN_POINT('Ctrl Pts',(-25.9163158909426,0.701678575228756,
12.));
#200473=CARTESIAN_POINT('Ctrl Pts',(-25.891290261497,0.714951588527638,
0.));
#200474=CARTESIAN_POINT('Ctrl Pts',(-25.891290261497,0.714951588527638,
12.));
#200475=CARTESIAN_POINT('Ctrl Pts',(-25.8662960624185,0.728137036482335,
0.));
#200476=CARTESIAN_POINT('Ctrl Pts',(-25.8662960624185,0.728137036482335,
12.));
#200477=CARTESIAN_POINT('Ctrl Pts',(-25.8413334619055,0.741234902663807,
0.));
#200478=CARTESIAN_POINT('Ctrl Pts',(-25.8413334619055,0.741234902663807,
12.));
#200479=CARTESIAN_POINT('Ctrl Pts',(-25.8164027059984,0.754245175609524,
0.));
#200480=CARTESIAN_POINT('Ctrl Pts',(-25.8164027059984,0.754245175609524,
12.));
#200481=CARTESIAN_POINT('Ctrl Pts',(-25.7915041383376,0.767167852651168,
0.));
#200482=CARTESIAN_POINT('Ctrl Pts',(-25.7915041383376,0.767167852651168,
12.));
#200483=CARTESIAN_POINT('Ctrl Pts',(-25.7666381946955,0.780002940291965,
0.));
#200484=CARTESIAN_POINT('Ctrl Pts',(-25.7666381946955,0.780002940291965,
12.));
#200485=CARTESIAN_POINT('Ctrl Pts',(-25.7418053757746,0.792750451616127,
0.));
#200486=CARTESIAN_POINT('Ctrl Pts',(-25.7418053757746,0.792750451616127,
12.));
#200487=CARTESIAN_POINT('Ctrl Pts',(-25.7170062262525,0.805410404554352,
0.));
#200488=CARTESIAN_POINT('Ctrl Pts',(-25.7170062262525,0.805410404554352,
12.));
#200489=CARTESIAN_POINT('Ctrl Pts',(-25.6922413110194,0.817982819787464,
0.));
#200490=CARTESIAN_POINT('Ctrl Pts',(-25.6922413110194,0.817982819787464,
12.));
#200491=CARTESIAN_POINT('Ctrl Pts',(-25.6675111931952,0.830467718864205,
0.));
#200492=CARTESIAN_POINT('Ctrl Pts',(-25.6675111931952,0.830467718864205,
12.));
#200493=CARTESIAN_POINT('Ctrl Pts',(-25.6428164100055,0.842865122120758,
0.));
#200494=CARTESIAN_POINT('Ctrl Pts',(-25.6428164100055,0.842865122120758,
12.));
#200495=CARTESIAN_POINT('Ctrl Pts',(-25.6181574536049,0.855175047036549,
0.));
#200496=CARTESIAN_POINT('Ctrl Pts',(-25.6181574536049,0.855175047036549,
12.));
#200497=CARTESIAN_POINT('Ctrl Pts',(-25.5935347843585,0.867397509338431,
0.));
#200498=CARTESIAN_POINT('Ctrl Pts',(-25.5935347843585,0.867397509338431,
12.));
#200499=CARTESIAN_POINT('Ctrl Pts',(-25.5689488408156,0.879532523834294,
0.));
#200500=CARTESIAN_POINT('Ctrl Pts',(-25.5689488408156,0.879532523834294,
12.));
#200501=CARTESIAN_POINT('Ctrl Pts',(-25.5444000508211,0.89158010534904,
0.));
#200502=CARTESIAN_POINT('Ctrl Pts',(-25.5444000508211,0.89158010534904,
12.));
#200503=CARTESIAN_POINT('Ctrl Pts',(-25.5198888424194,0.903540269651106,
0.));
#200504=CARTESIAN_POINT('Ctrl Pts',(-25.5198888424194,0.903540269651106,
12.));
#200505=CARTESIAN_POINT('Ctrl Pts',(-25.4954156541795,0.915413034335613,
0.));
#200506=CARTESIAN_POINT('Ctrl Pts',(-25.4954156541795,0.915413034335613,
12.));
#200507=CARTESIAN_POINT('Ctrl Pts',(-25.4709809475009,0.927198419886094,
0.));
#200508=CARTESIAN_POINT('Ctrl Pts',(-25.4709809475009,0.927198419886094,
12.));
#200509=CARTESIAN_POINT('Ctrl Pts',(-25.4465852044849,0.938896449496192,
0.));
#200510=CARTESIAN_POINT('Ctrl Pts',(-25.4465852044849,0.938896449496192,
12.));
#200511=CARTESIAN_POINT('Ctrl Pts',(-25.4222289223167,0.950507148597468,
0.));
#200512=CARTESIAN_POINT('Ctrl Pts',(-25.4222289223167,0.950507148597468,
12.));
#200513=CARTESIAN_POINT('Ctrl Pts',(-25.3979126089163,0.962030544503142,
0.));
#200514=CARTESIAN_POINT('Ctrl Pts',(-25.3979126089163,0.962030544503142,
12.));
#200515=CARTESIAN_POINT('Ctrl Pts',(-25.3736367778845,0.973466666000163,
0.));
#200516=CARTESIAN_POINT('Ctrl Pts',(-25.3736367778845,0.973466666000163,
12.));
#200517=CARTESIAN_POINT('Ctrl Pts',(-25.3494019441441,0.984815543003973,
0.));
#200518=CARTESIAN_POINT('Ctrl Pts',(-25.3494019441441,0.984815543003973,
12.));
#200519=CARTESIAN_POINT('Ctrl Pts',(-25.3252086182968,0.996077206120624,
0.));
#200520=CARTESIAN_POINT('Ctrl Pts',(-25.3252086182968,0.996077206120624,
12.));
#200521=CARTESIAN_POINT('Ctrl Pts',(-25.3010573055547,1.00725168656896,
0.));
#200522=CARTESIAN_POINT('Ctrl Pts',(-25.3010573055547,1.00725168656896,
12.));
#200523=CARTESIAN_POINT('Ctrl Pts',(-25.276948508726,1.01833901642237,0.));
#200524=CARTESIAN_POINT('Ctrl Pts',(-25.276948508726,1.01833901642237,12.));
#200525=CARTESIAN_POINT('Ctrl Pts',(-25.2528827300422,1.02933922876806,
0.));
#200526=CARTESIAN_POINT('Ctrl Pts',(-25.2528827300422,1.02933922876806,
12.));
#200527=CARTESIAN_POINT('Ctrl Pts',(-25.2288604735086,1.04025235791507,
0.));
#200528=CARTESIAN_POINT('Ctrl Pts',(-25.2288604735086,1.04025235791507,
12.));
#200529=CARTESIAN_POINT('Ctrl Pts',(-25.2048822469028,1.05107843957931,
0.));
#200530=CARTESIAN_POINT('Ctrl Pts',(-25.2048822469028,1.05107843957931,
12.));
#200531=CARTESIAN_POINT('Ctrl Pts',(-25.1809485642192,1.06181751111768,
0.));
#200532=CARTESIAN_POINT('Ctrl Pts',(-25.1809485642192,1.06181751111768,
12.));
#200533=CARTESIAN_POINT('Ctrl Pts',(-25.157059946931,1.07246961165475,0.));
#200534=CARTESIAN_POINT('Ctrl Pts',(-25.157059946931,1.07246961165475,12.));
#200535=CARTESIAN_POINT('Ctrl Pts',(-25.1332169227413,1.08303478197187,
0.));
#200536=CARTESIAN_POINT('Ctrl Pts',(-25.1332169227413,1.08303478197187,
12.));
#200537=CARTESIAN_POINT('Ctrl Pts',(-25.1094200248446,1.09351306445308,
0.));
#200538=CARTESIAN_POINT('Ctrl Pts',(-25.1094200248446,1.09351306445308,
12.));
#200539=CARTESIAN_POINT('Ctrl Pts',(-25.0856697909679,1.10390450301745,
0.));
#200540=CARTESIAN_POINT('Ctrl Pts',(-25.0856697909679,1.10390450301745,
12.));
#200541=CARTESIAN_POINT('Ctrl Pts',(-25.0619667625336,1.11420914306889,
0.));
#200542=CARTESIAN_POINT('Ctrl Pts',(-25.0619667625336,1.11420914306889,
12.));
#200543=CARTESIAN_POINT('Ctrl Pts',(-25.0383114836899,1.12442703144451,
0.));
#200544=CARTESIAN_POINT('Ctrl Pts',(-25.0383114836899,1.12442703144451,
12.));
#200545=CARTESIAN_POINT('Ctrl Pts',(-25.0147045006196,1.1345582163853,0.));
#200546=CARTESIAN_POINT('Ctrl Pts',(-25.0147045006196,1.1345582163853,12.));
#200547=CARTESIAN_POINT('Ctrl Pts',(-24.9911463621433,1.144602747582,0.));
#200548=CARTESIAN_POINT('Ctrl Pts',(-24.9911463621433,1.144602747582,12.));
#200549=CARTESIAN_POINT('Ctrl Pts',(-24.9676376201502,1.15456067621889,
0.));
#200550=CARTESIAN_POINT('Ctrl Pts',(-24.9676376201502,1.15456067621889,
12.));
#200551=CARTESIAN_POINT('Ctrl Pts',(-24.9441788300932,1.16443205502849,
0.));
#200552=CARTESIAN_POINT('Ctrl Pts',(-24.9441788300932,1.16443205502849,
12.));
#200553=CARTESIAN_POINT('Ctrl Pts',(-24.9207705514449,1.17421693835041,
0.));
#200554=CARTESIAN_POINT('Ctrl Pts',(-24.9207705514449,1.17421693835041,
12.));
#200555=CARTESIAN_POINT('Ctrl Pts',(-24.8974133481829,1.18391538220103,
0.));
#200556=CARTESIAN_POINT('Ctrl Pts',(-24.8974133481829,1.18391538220103,
12.));
#200557=CARTESIAN_POINT('Ctrl Pts',(-24.8741077892075,1.19352744434064,
0.));
#200558=CARTESIAN_POINT('Ctrl Pts',(-24.8741077892075,1.19352744434064,
12.));
#200559=CARTESIAN_POINT('Ctrl Pts',(-24.8508544481974,1.2030531842602,0.));
#200560=CARTESIAN_POINT('Ctrl Pts',(-24.8508544481974,1.2030531842602,12.));
#200561=CARTESIAN_POINT('Ctrl Pts',(-24.8276539035092,1.21249266318208,
0.));
#200562=CARTESIAN_POINT('Ctrl Pts',(-24.8276539035092,1.21249266318208,
12.));
#200563=CARTESIAN_POINT('Ctrl Pts',(-24.8045067380536,1.22184594406528,
0.));
#200564=CARTESIAN_POINT('Ctrl Pts',(-24.8045067380536,1.22184594406528,
12.));
#200565=CARTESIAN_POINT('Ctrl Pts',(-24.7814135391799,1.23111309161843,
0.));
#200566=CARTESIAN_POINT('Ctrl Pts',(-24.7814135391799,1.23111309161843,
12.));
#200567=CARTESIAN_POINT('Ctrl Pts',(-24.7583748985438,1.24029417231989,
0.));
#200568=CARTESIAN_POINT('Ctrl Pts',(-24.7583748985438,1.24029417231989,
12.));
#200569=CARTESIAN_POINT('Ctrl Pts',(-24.7353914120011,1.24938925444325,
0.));
#200570=CARTESIAN_POINT('Ctrl Pts',(-24.7353914120011,1.24938925444325,
12.));
#200571=CARTESIAN_POINT('Ctrl Pts',(-24.7124636797894,1.25839840807418,
0.));
#200572=CARTESIAN_POINT('Ctrl Pts',(-24.7124636797894,1.25839840807418,
12.));
#200573=CARTESIAN_POINT('Ctrl Pts',(-24.6895923066836,1.267321705135,0.));
#200574=CARTESIAN_POINT('Ctrl Pts',(-24.6895923066836,1.267321705135,12.));
#200575=CARTESIAN_POINT('Ctrl Pts',(-24.666777902156,1.27615921941642,0.));
#200576=CARTESIAN_POINT('Ctrl Pts',(-24.666777902156,1.27615921941642,12.));
#200577=CARTESIAN_POINT('Ctrl Pts',(-24.6440210805278,1.28491102661514,
0.));
#200578=CARTESIAN_POINT('Ctrl Pts',(-24.6440210805278,1.28491102661514,
12.));
#200579=CARTESIAN_POINT('Ctrl Pts',(-24.6213224611229,1.29357720438107,
0.));
#200580=CARTESIAN_POINT('Ctrl Pts',(-24.6213224611229,1.29357720438107,
12.));
#200581=CARTESIAN_POINT('Ctrl Pts',(-24.5986826684027,1.30215783236362,
0.));
#200582=CARTESIAN_POINT('Ctrl Pts',(-24.5986826684027,1.30215783236362,
12.));
#200583=CARTESIAN_POINT('Ctrl Pts',(-24.5761023320183,1.31065299222021,
0.));
#200584=CARTESIAN_POINT('Ctrl Pts',(-24.5761023320183,1.31065299222021,
12.));
#200585=CARTESIAN_POINT('Ctrl Pts',(-24.5535820868674,1.31906276763668,
0.));
#200586=CARTESIAN_POINT('Ctrl Pts',(-24.5535820868674,1.31906276763668,
12.));
#200587=CARTESIAN_POINT('Ctrl Pts',(-24.5311225731435,1.32738724435326,
0.));
#200588=CARTESIAN_POINT('Ctrl Pts',(-24.5311225731435,1.32738724435326,
12.));
#200589=CARTESIAN_POINT('Ctrl Pts',(-24.5087244363856,1.33562651019686,
0.));
#200590=CARTESIAN_POINT('Ctrl Pts',(-24.5087244363856,1.33562651019686,
12.));
#200591=CARTESIAN_POINT('Ctrl Pts',(-24.4863883275134,1.34378065512337,
0.));
#200592=CARTESIAN_POINT('Ctrl Pts',(-24.4863883275134,1.34378065512337,
12.));
#200593=CARTESIAN_POINT('Ctrl Pts',(-24.4641149028892,1.35184977125648,
0.));
#200594=CARTESIAN_POINT('Ctrl Pts',(-24.4641149028892,1.35184977125648,
12.));
#200595=CARTESIAN_POINT('Ctrl Pts',(-24.4419048244523,1.35983395290627,
0.));
#200596=CARTESIAN_POINT('Ctrl Pts',(-24.4419048244523,1.35983395290627,
12.));
#200597=CARTESIAN_POINT('Ctrl Pts',(-24.4197587598337,1.36773329659956,
0.));
#200598=CARTESIAN_POINT('Ctrl Pts',(-24.4197587598337,1.36773329659956,
12.));
#200599=CARTESIAN_POINT('Ctrl Pts',(-24.3976773824732,1.37554790111609,
0.));
#200600=CARTESIAN_POINT('Ctrl Pts',(-24.3976773824732,1.37554790111609,
12.));
#200601=CARTESIAN_POINT('Ctrl Pts',(-24.3756613717299,1.38327786752998,
0.));
#200602=CARTESIAN_POINT('Ctrl Pts',(-24.3756613717299,1.38327786752998,
12.));
#200603=CARTESIAN_POINT('Ctrl Pts',(-24.3537114129875,1.39092329926388,
0.));
#200604=CARTESIAN_POINT('Ctrl Pts',(-24.3537114129875,1.39092329926388,
12.));
#200605=CARTESIAN_POINT('Ctrl Pts',(-24.3318281977643,1.39848430212807,
0.));
#200606=CARTESIAN_POINT('Ctrl Pts',(-24.3318281977643,1.39848430212807,
12.));
#200607=CARTESIAN_POINT('Ctrl Pts',(-24.3100124238311,1.40596098434337,
0.));
#200608=CARTESIAN_POINT('Ctrl Pts',(-24.3100124238311,1.40596098434337,
12.));
#200609=CARTESIAN_POINT('Ctrl Pts',(-24.288264795321,1.41335345657682,0.));
#200610=CARTESIAN_POINT('Ctrl Pts',(-24.288264795321,1.41335345657682,12.));
#200611=CARTESIAN_POINT('Ctrl Pts',(-24.2665860228356,1.42066183198252,
0.));
#200612=CARTESIAN_POINT('Ctrl Pts',(-24.2665860228356,1.42066183198252,
12.));
#200613=CARTESIAN_POINT('Ctrl Pts',(-24.2449768235488,1.42788622624854,
0.));
#200614=CARTESIAN_POINT('Ctrl Pts',(-24.2449768235488,1.42788622624854,
12.));
#200615=CARTESIAN_POINT('Ctrl Pts',(-24.2234379212984,1.43502675765508,
0.));
#200616=CARTESIAN_POINT('Ctrl Pts',(-24.2234379212984,1.43502675765508,
12.));
#200617=CARTESIAN_POINT('Ctrl Pts',(-24.201970046722,1.44208354711082,0.));
#200618=CARTESIAN_POINT('Ctrl Pts',(-24.201970046722,1.44208354711082,12.));
#200619=CARTESIAN_POINT('Ctrl Pts',(-24.1805739374038,1.44905671818727,
0.));
#200620=CARTESIAN_POINT('Ctrl Pts',(-24.1805739374038,1.44905671818727,
12.));
#200621=CARTESIAN_POINT('Ctrl Pts',(-24.1592503380107,1.45594639716317,
0.));
#200622=CARTESIAN_POINT('Ctrl Pts',(-24.1592503380107,1.45594639716317,
12.));
#200623=CARTESIAN_POINT('Ctrl Pts',(-24.1380000004272,1.46275271307397,
0.));
#200624=CARTESIAN_POINT('Ctrl Pts',(-24.1380000004272,1.46275271307397,
12.));
#200625=CARTESIAN_POINT('Ctrl Pts',(-24.1168236838824,1.46947579776991,
0.));
#200626=CARTESIAN_POINT('Ctrl Pts',(-24.1168236838824,1.46947579776991,
12.));
#200627=CARTESIAN_POINT('Ctrl Pts',(-24.0957221550778,1.47611578597742,
0.));
#200628=CARTESIAN_POINT('Ctrl Pts',(-24.0957221550778,1.47611578597742,
12.));
#200629=CARTESIAN_POINT('Ctrl Pts',(-24.0746961883528,1.48267281533683,
0.));
#200630=CARTESIAN_POINT('Ctrl Pts',(-24.0746961883528,1.48267281533683,
12.));
#200631=CARTESIAN_POINT('Ctrl Pts',(-24.0537465658429,1.48914702644887,
0.));
#200632=CARTESIAN_POINT('Ctrl Pts',(-24.0537465658429,1.48914702644887,
12.));
#200633=CARTESIAN_POINT('Ctrl Pts',(-24.0328740776331,1.49553856292801,
0.));
#200634=CARTESIAN_POINT('Ctrl Pts',(-24.0328740776331,1.49553856292801,
12.));
#200635=CARTESIAN_POINT('Ctrl Pts',(-24.0120795219086,1.50184757146098,
0.));
#200636=CARTESIAN_POINT('Ctrl Pts',(-24.0120795219086,1.50184757146098,
12.));
#200637=CARTESIAN_POINT('Ctrl Pts',(-23.9913637050927,1.50807420187694,
0.));
#200638=CARTESIAN_POINT('Ctrl Pts',(-23.9913637050927,1.50807420187694,
12.));
#200639=CARTESIAN_POINT('Ctrl Pts',(-23.970727442014,1.51421860720614,0.));
#200640=CARTESIAN_POINT('Ctrl Pts',(-23.970727442014,1.51421860720614,12.));
#200641=CARTESIAN_POINT('Ctrl Pts',(-23.9501715561033,1.52028094372792,
0.));
#200642=CARTESIAN_POINT('Ctrl Pts',(-23.9501715561033,1.52028094372792,
12.));
#200643=CARTESIAN_POINT('Ctrl Pts',(-23.9296968795757,1.52626137103032,
0.));
#200644=CARTESIAN_POINT('Ctrl Pts',(-23.9296968795757,1.52626137103032,
12.));
#200645=CARTESIAN_POINT('Ctrl Pts',(-23.9093042536119,1.53216005207463,
0.));
#200646=CARTESIAN_POINT('Ctrl Pts',(-23.9093042536119,1.53216005207463,
12.));
#200647=CARTESIAN_POINT('Ctrl Pts',(-23.8889945285318,1.53797715326758,
0.));
#200648=CARTESIAN_POINT('Ctrl Pts',(-23.8889945285318,1.53797715326758,
12.));
#200649=CARTESIAN_POINT('Ctrl Pts',(-23.8687685639642,1.5437128445399,0.));
#200650=CARTESIAN_POINT('Ctrl Pts',(-23.8687685639642,1.5437128445399,12.));
#200651=CARTESIAN_POINT('Ctrl Pts',(-23.8486272290705,1.54936729940541,
0.));
#200652=CARTESIAN_POINT('Ctrl Pts',(-23.8486272290705,1.54936729940541,
12.));
#200653=CARTESIAN_POINT('Ctrl Pts',(-23.8285714027636,1.55494069502635,
0.));
#200654=CARTESIAN_POINT('Ctrl Pts',(-23.8285714027636,1.55494069502635,
12.));
#200655=CARTESIAN_POINT('Ctrl Pts',(-23.8086019739194,1.56043321228633,
0.));
#200656=CARTESIAN_POINT('Ctrl Pts',(-23.8086019739194,1.56043321228633,
12.));
#200657=CARTESIAN_POINT('Ctrl Pts',(-23.7887198415878,1.56584503586843,
0.));
#200658=CARTESIAN_POINT('Ctrl Pts',(-23.7887198415878,1.56584503586843,
12.));
#200659=CARTESIAN_POINT('Ctrl Pts',(-23.7689259151862,1.57117635434408,
0.));
#200660=CARTESIAN_POINT('Ctrl Pts',(-23.7689259151862,1.57117635434408,
12.));
#200661=CARTESIAN_POINT('Ctrl Pts',(-23.749221114736,1.57642736025246,0.));
#200662=CARTESIAN_POINT('Ctrl Pts',(-23.749221114736,1.57642736025246,12.));
#200663=CARTESIAN_POINT('Ctrl Pts',(-23.72960637113,1.58159825017358,0.));
#200664=CARTESIAN_POINT('Ctrl Pts',(-23.72960637113,1.58159825017358,12.));
#200665=CARTESIAN_POINT('Ctrl Pts',(-23.710082626383,1.58668922481221,0.));
#200666=CARTESIAN_POINT('Ctrl Pts',(-23.710082626383,1.58668922481221,12.));
#200667=CARTESIAN_POINT('Ctrl Pts',(-23.6906508338833,1.59170048908633,
0.));
#200668=CARTESIAN_POINT('Ctrl Pts',(-23.6906508338833,1.59170048908633,
12.));
#200669=CARTESIAN_POINT('Ctrl Pts',(-23.671311958631,1.59663225222463,0.));
#200670=CARTESIAN_POINT('Ctrl Pts',(-23.671311958631,1.59663225222463,12.));
#200671=CARTESIAN_POINT('Ctrl Pts',(-23.6520669774876,1.60148472786595,
0.));
#200672=CARTESIAN_POINT('Ctrl Pts',(-23.6520669774876,1.60148472786595,
12.));
#200673=CARTESIAN_POINT('Ctrl Pts',(-23.6329168794929,1.60625813414672,
0.));
#200674=CARTESIAN_POINT('Ctrl Pts',(-23.6329168794929,1.60625813414672,
12.));
#200675=CARTESIAN_POINT('Ctrl Pts',(-23.6138626661653,1.61095269379778,
0.));
#200676=CARTESIAN_POINT('Ctrl Pts',(-23.6138626661653,1.61095269379778,
12.));
#200677=CARTESIAN_POINT('Ctrl Pts',(-23.5949053517997,1.61556863424698,
0.));
#200678=CARTESIAN_POINT('Ctrl Pts',(-23.5949053517997,1.61556863424698,
12.));
#200679=CARTESIAN_POINT('Ctrl Pts',(-23.57604596376,1.62010618772866,0.));
#200680=CARTESIAN_POINT('Ctrl Pts',(-23.57604596376,1.62010618772866,12.));
#200681=CARTESIAN_POINT('Ctrl Pts',(-23.5572855427601,1.62456559140064,
0.));
#200682=CARTESIAN_POINT('Ctrl Pts',(-23.5572855427601,1.62456559140064,
12.));
#200683=CARTESIAN_POINT('Ctrl Pts',(-23.538625143226,1.62894708745223,0.));
#200684=CARTESIAN_POINT('Ctrl Pts',(-23.538625143226,1.62894708745223,12.));
#200685=CARTESIAN_POINT('Ctrl Pts',(-23.5200658336612,1.63325092321725,
0.));
#200686=CARTESIAN_POINT('Ctrl Pts',(-23.5200658336612,1.63325092321725,
12.));
#200687=CARTESIAN_POINT('Ctrl Pts',(-23.5016086970003,1.63747735129474,
0.));
#200688=CARTESIAN_POINT('Ctrl Pts',(-23.5016086970003,1.63747735129474,
12.));
#200689=CARTESIAN_POINT('Ctrl Pts',(-23.4832548309645,1.64162662967528,
0.));
#200690=CARTESIAN_POINT('Ctrl Pts',(-23.4832548309645,1.64162662967528,
12.));
#200691=CARTESIAN_POINT('Ctrl Pts',(-23.4650053483932,1.64569902187611,
0.));
#200692=CARTESIAN_POINT('Ctrl Pts',(-23.4650053483932,1.64569902187611,
12.));
#200693=CARTESIAN_POINT('Ctrl Pts',(-23.4468613776574,1.6496947970734,0.));
#200694=CARTESIAN_POINT('Ctrl Pts',(-23.4468613776574,1.6496947970734,12.));
#200695=CARTESIAN_POINT('Ctrl Pts',(-23.4288240631043,1.65361423023728,
0.));
#200696=CARTESIAN_POINT('Ctrl Pts',(-23.4288240631043,1.65361423023728,
12.));
#200697=CARTESIAN_POINT('Ctrl Pts',(-23.4108945654805,1.65745760227505,
0.));
#200698=CARTESIAN_POINT('Ctrl Pts',(-23.4108945654805,1.65745760227505,
12.));
#200699=CARTESIAN_POINT('Ctrl Pts',(-23.3930740623619,1.66122520018011,
0.));
#200700=CARTESIAN_POINT('Ctrl Pts',(-23.3930740623619,1.66122520018011,
12.));
#200701=CARTESIAN_POINT('Ctrl Pts',(-23.3753637485545,1.66491731718876,
0.));
#200702=CARTESIAN_POINT('Ctrl Pts',(-23.3753637485545,1.66491731718876,
12.));
#200703=CARTESIAN_POINT('Ctrl Pts',(-23.3577648365744,1.66853425293995,
0.));
#200704=CARTESIAN_POINT('Ctrl Pts',(-23.3577648365744,1.66853425293995,
12.));
#200705=CARTESIAN_POINT('Ctrl Pts',(-23.3402785571865,1.67207631363921,
0.));
#200706=CARTESIAN_POINT('Ctrl Pts',(-23.3402785571865,1.67207631363921,
12.));
#200707=CARTESIAN_POINT('Ctrl Pts',(-23.3229061599145,1.67554381222994,
0.));
#200708=CARTESIAN_POINT('Ctrl Pts',(-23.3229061599145,1.67554381222994,
12.));
#200709=CARTESIAN_POINT('Ctrl Pts',(-23.3056489135611,1.67893706857117,
0.));
#200710=CARTESIAN_POINT('Ctrl Pts',(-23.3056489135611,1.67893706857117,
12.));
#200711=CARTESIAN_POINT('Ctrl Pts',(-23.2885081066951,1.68225640962168,
0.));
#200712=CARTESIAN_POINT('Ctrl Pts',(-23.2885081066951,1.68225640962168,
12.));
#200713=CARTESIAN_POINT('Ctrl Pts',(-23.2714850482246,1.68550216963258,
0.));
#200714=CARTESIAN_POINT('Ctrl Pts',(-23.2714850482246,1.68550216963258,
12.));
#200715=CARTESIAN_POINT('Ctrl Pts',(-23.2545810680537,1.68867469034896,
0.));
#200716=CARTESIAN_POINT('Ctrl Pts',(-23.2545810680537,1.68867469034896,
12.));
#200717=CARTESIAN_POINT('Ctrl Pts',(-23.2377975177013,1.69177432121711,
0.));
#200718=CARTESIAN_POINT('Ctrl Pts',(-23.2377975177013,1.69177432121711,
12.));
#200719=CARTESIAN_POINT('Ctrl Pts',(-23.2211357709374,1.69480141959953,
0.));
#200720=CARTESIAN_POINT('Ctrl Pts',(-23.2211357709374,1.69480141959953,
12.));
#200721=CARTESIAN_POINT('Ctrl Pts',(-23.2045972243767,1.69775635099443,
0.));
#200722=CARTESIAN_POINT('Ctrl Pts',(-23.2045972243767,1.69775635099443,
12.));
#200723=CARTESIAN_POINT('Ctrl Pts',(-23.1881832981851,1.7006394892701,0.));
#200724=CARTESIAN_POINT('Ctrl Pts',(-23.1881832981851,1.7006394892701,12.));
#200725=CARTESIAN_POINT('Ctrl Pts',(-23.1718954368751,1.70345121691276,
0.));
#200726=CARTESIAN_POINT('Ctrl Pts',(-23.1718954368751,1.70345121691276,
12.));
#200727=CARTESIAN_POINT('Ctrl Pts',(-23.1557351100614,1.70619192527852,
0.));
#200728=CARTESIAN_POINT('Ctrl Pts',(-23.1557351100614,1.70619192527852,
12.));
#200729=CARTESIAN_POINT('Ctrl Pts',(-23.1397038132356,1.70886201485452,
0.));
#200730=CARTESIAN_POINT('Ctrl Pts',(-23.1397038132356,1.70886201485452,
12.));
#200731=CARTESIAN_POINT('Ctrl Pts',(-23.1238030684925,1.71146189552174,
0.));
#200732=CARTESIAN_POINT('Ctrl Pts',(-23.1238030684925,1.71146189552174,
12.));
#200733=CARTESIAN_POINT('Ctrl Pts',(-23.1080344254286,1.71399198684704,
0.));
#200734=CARTESIAN_POINT('Ctrl Pts',(-23.1080344254286,1.71399198684704,
12.));
#200735=CARTESIAN_POINT('Ctrl Pts',(-23.0923994621213,1.71645271839296,
0.));
#200736=CARTESIAN_POINT('Ctrl Pts',(-23.0923994621213,1.71645271839296,
12.));
#200737=CARTESIAN_POINT('Ctrl Pts',(-23.0768997860709,1.71884453003027,
0.));
#200738=CARTESIAN_POINT('Ctrl Pts',(-23.0768997860709,1.71884453003027,
12.));
#200739=CARTESIAN_POINT('Ctrl Pts',(-23.0615370351562,1.72116787225991,
0.));
#200740=CARTESIAN_POINT('Ctrl Pts',(-23.0615370351562,1.72116787225991,
12.));
#200741=CARTESIAN_POINT('Ctrl Pts',(-23.0463128785531,1.72342320653746,
0.));
#200742=CARTESIAN_POINT('Ctrl Pts',(-23.0463128785531,1.72342320653746,
12.));
#200743=CARTESIAN_POINT('Ctrl Pts',(-23.0312290178883,1.72561100564045,
0.));
#200744=CARTESIAN_POINT('Ctrl Pts',(-23.0312290178883,1.72561100564045,
12.));
#200745=CARTESIAN_POINT('Ctrl Pts',(-23.0162871884168,1.72773175404708,
0.));
#200746=CARTESIAN_POINT('Ctrl Pts',(-23.0162871884168,1.72773175404708,
12.));
#200747=CARTESIAN_POINT('Ctrl Pts',(-23.001489160189,1.72978594832136,0.));
#200748=CARTESIAN_POINT('Ctrl Pts',(-23.001489160189,1.72978594832136,12.));
#200749=CARTESIAN_POINT('Ctrl Pts',(-22.9868367391978,1.7317740975019,0.));
#200750=CARTESIAN_POINT('Ctrl Pts',(-22.9868367391978,1.7317740975019,12.));
#200751=CARTESIAN_POINT('Ctrl Pts',(-22.9723317685688,1.73369672350814,
0.));
#200752=CARTESIAN_POINT('Ctrl Pts',(-22.9723317685688,1.73369672350814,
12.));
#200753=CARTESIAN_POINT('Ctrl Pts',(-22.9579761301063,1.73555436162769,
0.));
#200754=CARTESIAN_POINT('Ctrl Pts',(-22.9579761301063,1.73555436162769,
12.));
#200755=CARTESIAN_POINT('Ctrl Pts',(-22.9437717457826,1.73734756100039,
0.));
#200756=CARTESIAN_POINT('Ctrl Pts',(-22.9437717457826,1.73734756100039,
12.));
#200757=CARTESIAN_POINT('Ctrl Pts',(-22.9297205792586,1.73907688511666,
0.));
#200758=CARTESIAN_POINT('Ctrl Pts',(-22.9297205792586,1.73907688511666,
12.));
#200759=CARTESIAN_POINT('Ctrl Pts',(-22.9158246373363,1.74074291231058,
0.));
#200760=CARTESIAN_POINT('Ctrl Pts',(-22.9158246373363,1.74074291231058,
12.));
#200761=CARTESIAN_POINT('Ctrl Pts',(-22.9020859716141,1.7423462363008,0.));
#200762=CARTESIAN_POINT('Ctrl Pts',(-22.9020859716141,1.7423462363008,12.));
#200763=CARTESIAN_POINT('Ctrl Pts',(-22.888506680335,1.74388746677702,0.));
#200764=CARTESIAN_POINT('Ctrl Pts',(-22.888506680335,1.74388746677702,12.));
#200765=CARTESIAN_POINT('Ctrl Pts',(-22.8750889101696,1.74536722998201,
0.));
#200766=CARTESIAN_POINT('Ctrl Pts',(-22.8750889101696,1.74536722998201,
12.));
#200767=CARTESIAN_POINT('Ctrl Pts',(-22.8618348580235,1.74678616930664,
0.));
#200768=CARTESIAN_POINT('Ctrl Pts',(-22.8618348580235,1.74678616930664,
12.));
#200769=CARTESIAN_POINT('Ctrl Pts',(-22.8487467728076,1.74814494588492,
0.));
#200770=CARTESIAN_POINT('Ctrl Pts',(-22.8487467728076,1.74814494588492,
12.));
#200771=CARTESIAN_POINT('Ctrl Pts',(-22.8358269579853,1.74944423940115,
0.));
#200772=CARTESIAN_POINT('Ctrl Pts',(-22.8358269579853,1.74944423940115,
12.));
#200773=CARTESIAN_POINT('Ctrl Pts',(-22.8230777741284,1.75068474890883,
0.));
#200774=CARTESIAN_POINT('Ctrl Pts',(-22.8230777741284,1.75068474890883,
12.));
#200775=CARTESIAN_POINT('Ctrl Pts',(-22.8105016414713,1.75186719365592,
0.));
#200776=CARTESIAN_POINT('Ctrl Pts',(-22.8105016414713,1.75186719365592,
12.));
#200777=CARTESIAN_POINT('Ctrl Pts',(-22.7981010424314,1.75299231391466,
0.));
#200778=CARTESIAN_POINT('Ctrl Pts',(-22.7981010424314,1.75299231391466,
12.));
#200779=CARTESIAN_POINT('Ctrl Pts',(-22.7858785242361,1.75406087182936,
0.));
#200780=CARTESIAN_POINT('Ctrl Pts',(-22.7858785242361,1.75406087182936,
12.));
#200781=CARTESIAN_POINT('Ctrl Pts',(-22.7738367016118,1.75507365227131,
0.));
#200782=CARTESIAN_POINT('Ctrl Pts',(-22.7738367016118,1.75507365227131,
12.));
#200783=CARTESIAN_POINT('Ctrl Pts',(-22.7619782595013,1.75603146371641,
0.));
#200784=CARTESIAN_POINT('Ctrl Pts',(-22.7619782595013,1.75603146371641,
12.));
#200785=CARTESIAN_POINT('Ctrl Pts',(-22.750305955645,1.75693513908907,0.));
#200786=CARTESIAN_POINT('Ctrl Pts',(-22.750305955645,1.75693513908907,12.));
#200787=CARTESIAN_POINT('Ctrl Pts',(-22.7388226235559,1.75778553673244,
0.));
#200788=CARTESIAN_POINT('Ctrl Pts',(-22.7388226235559,1.75778553673244,
12.));
#200789=CARTESIAN_POINT('Ctrl Pts',(-22.72753117773,1.75858354204633,0.));
#200790=CARTESIAN_POINT('Ctrl Pts',(-22.72753117773,1.75858354204633,12.));
#200791=CARTESIAN_POINT('Ctrl Pts',(-22.7164346186006,1.75933006905925,
0.));
#200792=CARTESIAN_POINT('Ctrl Pts',(-22.7164346186006,1.75933006905925,
12.));
#200793=CARTESIAN_POINT('Ctrl Pts',(-22.7055360375485,1.76002606202401,
0.));
#200794=CARTESIAN_POINT('Ctrl Pts',(-22.7055360375485,1.76002606202401,
12.));
#200795=CARTESIAN_POINT('Ctrl Pts',(-22.6948386219851,1.76067249704886,
0.));
#200796=CARTESIAN_POINT('Ctrl Pts',(-22.6948386219851,1.76067249704886,
12.));
#200797=CARTESIAN_POINT('Ctrl Pts',(-22.684345658525,1.76127038310614,0.));
#200798=CARTESIAN_POINT('Ctrl Pts',(-22.684345658525,1.76127038310614,12.));
#200799=CARTESIAN_POINT('Ctrl Pts',(-22.67406053567,1.76182076289525,0.));
#200800=CARTESIAN_POINT('Ctrl Pts',(-22.67406053567,1.76182076289525,12.));
#200801=CARTESIAN_POINT('Ctrl Pts',(-22.6639867471753,1.76232471392568,
0.));
#200802=CARTESIAN_POINT('Ctrl Pts',(-22.6639867471753,1.76232471392568,
12.));
#200803=CARTESIAN_POINT('Ctrl Pts',(-22.6541278938409,1.76278334912561,
0.));
#200804=CARTESIAN_POINT('Ctrl Pts',(-22.6541278938409,1.76278334912561,
12.));
#200805=CARTESIAN_POINT('Ctrl Pts',(-22.6444876940423,1.76319782013916,
0.));
#200806=CARTESIAN_POINT('Ctrl Pts',(-22.6444876940423,1.76319782013916,
12.));
#200807=CARTESIAN_POINT('Ctrl Pts',(-22.6350699979359,1.76356932176273,
0.));
#200808=CARTESIAN_POINT('Ctrl Pts',(-22.6350699979359,1.76356932176273,
12.));
#200809=CARTESIAN_POINT('Ctrl Pts',(-22.6258787994848,1.76389909571403,
0.));
#200810=CARTESIAN_POINT('Ctrl Pts',(-22.6258787994848,1.76389909571403,
12.));
#200811=CARTESIAN_POINT('Ctrl Pts',(-22.6169182517694,1.76418843543739,
0.));
#200812=CARTESIAN_POINT('Ctrl Pts',(-22.6169182517694,1.76418843543739,
12.));
#200813=CARTESIAN_POINT('Ctrl Pts',(-22.6081926681343,1.76443868648015,
0.));
#200814=CARTESIAN_POINT('Ctrl Pts',(-22.6081926681343,1.76443868648015,
12.));
#200815=CARTESIAN_POINT('Ctrl Pts',(-22.5997065145638,1.76465124413557,
0.));
#200816=CARTESIAN_POINT('Ctrl Pts',(-22.5997065145638,1.76465124413557,
12.));
#200817=CARTESIAN_POINT('Ctrl Pts',(-22.5914644078106,1.76482755288411,
0.));
#200818=CARTESIAN_POINT('Ctrl Pts',(-22.5914644078106,1.76482755288411,
12.));
#200819=CARTESIAN_POINT('Ctrl Pts',(-22.5834711038022,1.76496910283088,
0.));
#200820=CARTESIAN_POINT('Ctrl Pts',(-22.5834711038022,1.76496910283088,
12.));
#200821=CARTESIAN_POINT('Ctrl Pts',(-22.5757315316353,1.76507744026746,
0.));
#200822=CARTESIAN_POINT('Ctrl Pts',(-22.5757315316353,1.76507744026746,
12.));
#200823=CARTESIAN_POINT('Ctrl Pts',(-22.5682508499873,1.76515418518831,
0.));
#200824=CARTESIAN_POINT('Ctrl Pts',(-22.5682508499873,1.76515418518831,
12.));
#200825=CARTESIAN_POINT('Ctrl Pts',(-22.5610344912501,1.7652010450045,0.));
#200826=CARTESIAN_POINT('Ctrl Pts',(-22.5610344912501,1.7652010450045,12.));
#200827=CARTESIAN_POINT('Ctrl Pts',(-22.5540882235837,1.76521983384062,
0.));
#200828=CARTESIAN_POINT('Ctrl Pts',(-22.5540882235837,1.76521983384062,
12.));
#200829=CARTESIAN_POINT('Ctrl Pts',(-22.5474180954006,1.76521245524047,
0.));
#200830=CARTESIAN_POINT('Ctrl Pts',(-22.5474180954006,1.76521245524047,
12.));
#200831=CARTESIAN_POINT('Ctrl Pts',(-22.5410303590892,1.76518087841493,
0.));
#200832=CARTESIAN_POINT('Ctrl Pts',(-22.5410303590892,1.76518087841493,
12.));
#200833=CARTESIAN_POINT('Ctrl Pts',(-22.5349313983571,1.76512711563254,
0.));
#200834=CARTESIAN_POINT('Ctrl Pts',(-22.5349313983571,1.76512711563254,
12.));
#200835=CARTESIAN_POINT('Ctrl Pts',(-22.529127665298,1.76505320262759,0.));
#200836=CARTESIAN_POINT('Ctrl Pts',(-22.529127665298,1.76505320262759,12.));
#200837=CARTESIAN_POINT('Ctrl Pts',(-22.5236259635515,1.76496128643375,
0.));
#200838=CARTESIAN_POINT('Ctrl Pts',(-22.5236259635515,1.76496128643375,
12.));
#200839=CARTESIAN_POINT('Ctrl Pts',(-22.5184336670207,1.76485369319895,
0.));
#200840=CARTESIAN_POINT('Ctrl Pts',(-22.5184336670207,1.76485369319895,
12.));
#200841=CARTESIAN_POINT('Ctrl Pts',(-22.5135590569554,1.76473303281149,
0.));
#200842=CARTESIAN_POINT('Ctrl Pts',(-22.5135590569554,1.76473303281149,
12.));
#200843=CARTESIAN_POINT('Ctrl Pts',(-22.5090112700212,1.76460218257313,
0.));
#200844=CARTESIAN_POINT('Ctrl Pts',(-22.5090112700212,1.76460218257313,
12.));
#200845=CARTESIAN_POINT('Ctrl Pts',(-22.5047996391978,1.76446408210364,
0.));
#200846=CARTESIAN_POINT('Ctrl Pts',(-22.5047996391978,1.76446408210364,
12.));
#200847=CARTESIAN_POINT('Ctrl Pts',(-22.5009332677316,1.76432160068737,
0.));
#200848=CARTESIAN_POINT('Ctrl Pts',(-22.5009332677316,1.76432160068737,
12.));
#200849=CARTESIAN_POINT('Ctrl Pts',(-22.4974203063191,1.76417731243483,
0.));
#200850=CARTESIAN_POINT('Ctrl Pts',(-22.4974203063191,1.76417731243483,
12.));
#200851=CARTESIAN_POINT('Ctrl Pts',(-22.4942693792449,1.76403393880316,
0.));
#200852=CARTESIAN_POINT('Ctrl Pts',(-22.4942693792449,1.76403393880316,
12.));
#200853=CARTESIAN_POINT('Ctrl Pts',(-22.4914909094908,1.76389475965714,
0.));
#200854=CARTESIAN_POINT('Ctrl Pts',(-22.4914909094908,1.76389475965714,
12.));
#200855=CARTESIAN_POINT('Ctrl Pts',(-22.4890991659479,1.76376424879468,
0.));
#200856=CARTESIAN_POINT('Ctrl Pts',(-22.4890991659479,1.76376424879468,
12.));
#200857=CARTESIAN_POINT('Ctrl Pts',(-22.4871115206572,1.76364784232925,
0.));
#200858=CARTESIAN_POINT('Ctrl Pts',(-22.4871115206572,1.76364784232925,
12.));
#200859=CARTESIAN_POINT('Ctrl Pts',(-22.4855446605991,1.76355076045549,
0.));
#200860=CARTESIAN_POINT('Ctrl Pts',(-22.4855446605991,1.76355076045549,
12.));
#200861=CARTESIAN_POINT('Ctrl Pts',(-22.4844112933125,1.76347698284861,
0.));
#200862=CARTESIAN_POINT('Ctrl Pts',(-22.4844112933125,1.76347698284861,
12.));
#200863=CARTESIAN_POINT('Ctrl Pts',(-22.4838562517064,1.76343813434659,
0.));
#200864=CARTESIAN_POINT('Ctrl Pts',(-22.4838562517064,1.76343813434659,
12.));
#200865=CARTESIAN_POINT('Ctrl Pts',(-22.4836387052228,1.76342064263637,
0.));
#200866=CARTESIAN_POINT('Ctrl Pts',(-22.4836387052228,1.76342064263637,
12.));
#200867=CARTESIAN_POINT('Ctrl Pts',(-22.4835819929788,1.7634141553879,0.));
#200868=CARTESIAN_POINT('Ctrl Pts',(-22.4835819929788,1.7634141553879,12.));
#200869=CARTESIAN_POINT('Ctrl Pts',(-22.4835757167854,1.7634122053118,0.));
#200870=CARTESIAN_POINT('Ctrl Pts',(-22.4835757167854,1.7634122053118,12.));
#200871=CARTESIAN_POINT('',(-25.991588367311,0.661312440730901,0.));
#200872=CARTESIAN_POINT('Ctrl Pts',(-25.991588367311,0.661312440730901,
0.));
#200873=CARTESIAN_POINT('Ctrl Pts',(-25.9865613464773,0.664028313187627,
0.));
#200874=CARTESIAN_POINT('Ctrl Pts',(-25.9765104298071,0.669451306780825,
0.));
#200875=CARTESIAN_POINT('Ctrl Pts',(-25.9614434297919,0.677559543209725,
0.));
#200876=CARTESIAN_POINT('Ctrl Pts',(-25.9413728471909,0.688318015057729,
0.));
#200877=CARTESIAN_POINT('Ctrl Pts',(-25.9163158909426,0.701678575228756,
0.));
#200878=CARTESIAN_POINT('Ctrl Pts',(-25.891290261497,0.714951588527638,
0.));
#200879=CARTESIAN_POINT('Ctrl Pts',(-25.8662960624185,0.728137036482335,
0.));
#200880=CARTESIAN_POINT('Ctrl Pts',(-25.8413334619055,0.741234902663807,
0.));
#200881=CARTESIAN_POINT('Ctrl Pts',(-25.8164027059984,0.754245175609524,
0.));
#200882=CARTESIAN_POINT('Ctrl Pts',(-25.7915041383376,0.767167852651168,
0.));
#200883=CARTESIAN_POINT('Ctrl Pts',(-25.7666381946955,0.780002940291965,
0.));
#200884=CARTESIAN_POINT('Ctrl Pts',(-25.7418053757746,0.792750451616127,
0.));
#200885=CARTESIAN_POINT('Ctrl Pts',(-25.7170062262525,0.805410404554352,
0.));
#200886=CARTESIAN_POINT('Ctrl Pts',(-25.6922413110194,0.817982819787464,
0.));
#200887=CARTESIAN_POINT('Ctrl Pts',(-25.6675111931952,0.830467718864205,
0.));
#200888=CARTESIAN_POINT('Ctrl Pts',(-25.6428164100055,0.842865122120758,
0.));
#200889=CARTESIAN_POINT('Ctrl Pts',(-25.6181574536049,0.855175047036549,
0.));
#200890=CARTESIAN_POINT('Ctrl Pts',(-25.5935347843585,0.867397509338431,
0.));
#200891=CARTESIAN_POINT('Ctrl Pts',(-25.5689488408156,0.879532523834294,
0.));
#200892=CARTESIAN_POINT('Ctrl Pts',(-25.5444000508211,0.89158010534904,
0.));
#200893=CARTESIAN_POINT('Ctrl Pts',(-25.5198888424194,0.903540269651106,
0.));
#200894=CARTESIAN_POINT('Ctrl Pts',(-25.4954156541795,0.915413034335613,
0.));
#200895=CARTESIAN_POINT('Ctrl Pts',(-25.4709809475009,0.927198419886094,
0.));
#200896=CARTESIAN_POINT('Ctrl Pts',(-25.4465852044849,0.938896449496192,
0.));
#200897=CARTESIAN_POINT('Ctrl Pts',(-25.4222289223167,0.950507148597468,
0.));
#200898=CARTESIAN_POINT('Ctrl Pts',(-25.3979126089163,0.962030544503142,
0.));
#200899=CARTESIAN_POINT('Ctrl Pts',(-25.3736367778845,0.973466666000163,
0.));
#200900=CARTESIAN_POINT('Ctrl Pts',(-25.3494019441441,0.984815543003973,
0.));
#200901=CARTESIAN_POINT('Ctrl Pts',(-25.3252086182968,0.996077206120624,
0.));
#200902=CARTESIAN_POINT('Ctrl Pts',(-25.3010573055547,1.00725168656896,
0.));
#200903=CARTESIAN_POINT('Ctrl Pts',(-25.276948508726,1.01833901642237,0.));
#200904=CARTESIAN_POINT('Ctrl Pts',(-25.2528827300422,1.02933922876806,
0.));
#200905=CARTESIAN_POINT('Ctrl Pts',(-25.2288604735086,1.04025235791507,
0.));
#200906=CARTESIAN_POINT('Ctrl Pts',(-25.2048822469028,1.05107843957931,
0.));
#200907=CARTESIAN_POINT('Ctrl Pts',(-25.1809485642192,1.06181751111768,
0.));
#200908=CARTESIAN_POINT('Ctrl Pts',(-25.157059946931,1.07246961165475,0.));
#200909=CARTESIAN_POINT('Ctrl Pts',(-25.1332169227413,1.08303478197187,
0.));
#200910=CARTESIAN_POINT('Ctrl Pts',(-25.1094200248446,1.09351306445308,
0.));
#200911=CARTESIAN_POINT('Ctrl Pts',(-25.0856697909679,1.10390450301745,
0.));
#200912=CARTESIAN_POINT('Ctrl Pts',(-25.0619667625336,1.11420914306889,
0.));
#200913=CARTESIAN_POINT('Ctrl Pts',(-25.0383114836899,1.12442703144451,
0.));
#200914=CARTESIAN_POINT('Ctrl Pts',(-25.0147045006196,1.1345582163853,0.));
#200915=CARTESIAN_POINT('Ctrl Pts',(-24.9911463621433,1.144602747582,0.));
#200916=CARTESIAN_POINT('Ctrl Pts',(-24.9676376201502,1.15456067621889,
0.));
#200917=CARTESIAN_POINT('Ctrl Pts',(-24.9441788300932,1.16443205502849,
0.));
#200918=CARTESIAN_POINT('Ctrl Pts',(-24.9207705514449,1.17421693835041,
0.));
#200919=CARTESIAN_POINT('Ctrl Pts',(-24.8974133481829,1.18391538220103,
0.));
#200920=CARTESIAN_POINT('Ctrl Pts',(-24.8741077892075,1.19352744434064,
0.));
#200921=CARTESIAN_POINT('Ctrl Pts',(-24.8508544481974,1.2030531842602,0.));
#200922=CARTESIAN_POINT('Ctrl Pts',(-24.8276539035092,1.21249266318208,
0.));
#200923=CARTESIAN_POINT('Ctrl Pts',(-24.8045067380536,1.22184594406528,
0.));
#200924=CARTESIAN_POINT('Ctrl Pts',(-24.7814135391799,1.23111309161843,
0.));
#200925=CARTESIAN_POINT('Ctrl Pts',(-24.7583748985438,1.24029417231989,
0.));
#200926=CARTESIAN_POINT('Ctrl Pts',(-24.7353914120011,1.24938925444325,
0.));
#200927=CARTESIAN_POINT('Ctrl Pts',(-24.7124636797894,1.25839840807418,
0.));
#200928=CARTESIAN_POINT('Ctrl Pts',(-24.6895923066836,1.267321705135,0.));
#200929=CARTESIAN_POINT('Ctrl Pts',(-24.666777902156,1.27615921941642,0.));
#200930=CARTESIAN_POINT('Ctrl Pts',(-24.6440210805278,1.28491102661514,
0.));
#200931=CARTESIAN_POINT('Ctrl Pts',(-24.6213224611229,1.29357720438107,
0.));
#200932=CARTESIAN_POINT('Ctrl Pts',(-24.5986826684027,1.30215783236362,
0.));
#200933=CARTESIAN_POINT('Ctrl Pts',(-24.5761023320183,1.31065299222021,
0.));
#200934=CARTESIAN_POINT('Ctrl Pts',(-24.5535820868674,1.31906276763668,
0.));
#200935=CARTESIAN_POINT('Ctrl Pts',(-24.5311225731435,1.32738724435326,
0.));
#200936=CARTESIAN_POINT('Ctrl Pts',(-24.5087244363856,1.33562651019686,
0.));
#200937=CARTESIAN_POINT('Ctrl Pts',(-24.4863883275134,1.34378065512337,
0.));
#200938=CARTESIAN_POINT('Ctrl Pts',(-24.4641149028892,1.35184977125648,
0.));
#200939=CARTESIAN_POINT('Ctrl Pts',(-24.4419048244523,1.35983395290627,
0.));
#200940=CARTESIAN_POINT('Ctrl Pts',(-24.4197587598337,1.36773329659956,
0.));
#200941=CARTESIAN_POINT('Ctrl Pts',(-24.3976773824732,1.37554790111609,
0.));
#200942=CARTESIAN_POINT('Ctrl Pts',(-24.3756613717299,1.38327786752998,
0.));
#200943=CARTESIAN_POINT('Ctrl Pts',(-24.3537114129875,1.39092329926388,
0.));
#200944=CARTESIAN_POINT('Ctrl Pts',(-24.3318281977643,1.39848430212807,
0.));
#200945=CARTESIAN_POINT('Ctrl Pts',(-24.3100124238311,1.40596098434337,
0.));
#200946=CARTESIAN_POINT('Ctrl Pts',(-24.288264795321,1.41335345657682,0.));
#200947=CARTESIAN_POINT('Ctrl Pts',(-24.2665860228356,1.42066183198252,
0.));
#200948=CARTESIAN_POINT('Ctrl Pts',(-24.2449768235488,1.42788622624854,
0.));
#200949=CARTESIAN_POINT('Ctrl Pts',(-24.2234379212984,1.43502675765508,
0.));
#200950=CARTESIAN_POINT('Ctrl Pts',(-24.201970046722,1.44208354711082,0.));
#200951=CARTESIAN_POINT('Ctrl Pts',(-24.1805739374038,1.44905671818727,
0.));
#200952=CARTESIAN_POINT('Ctrl Pts',(-24.1592503380107,1.45594639716317,
0.));
#200953=CARTESIAN_POINT('Ctrl Pts',(-24.1380000004272,1.46275271307397,
0.));
#200954=CARTESIAN_POINT('Ctrl Pts',(-24.1168236838824,1.46947579776991,
0.));
#200955=CARTESIAN_POINT('Ctrl Pts',(-24.0957221550778,1.47611578597742,
0.));
#200956=CARTESIAN_POINT('Ctrl Pts',(-24.0746961883528,1.48267281533683,
0.));
#200957=CARTESIAN_POINT('Ctrl Pts',(-24.0537465658429,1.48914702644887,
0.));
#200958=CARTESIAN_POINT('Ctrl Pts',(-24.0328740776331,1.49553856292801,
0.));
#200959=CARTESIAN_POINT('Ctrl Pts',(-24.0120795219086,1.50184757146098,
0.));
#200960=CARTESIAN_POINT('Ctrl Pts',(-23.9913637050927,1.50807420187694,
0.));
#200961=CARTESIAN_POINT('Ctrl Pts',(-23.970727442014,1.51421860720614,0.));
#200962=CARTESIAN_POINT('Ctrl Pts',(-23.9501715561033,1.52028094372792,
0.));
#200963=CARTESIAN_POINT('Ctrl Pts',(-23.9296968795757,1.52626137103032,
0.));
#200964=CARTESIAN_POINT('Ctrl Pts',(-23.9093042536119,1.53216005207463,
0.));
#200965=CARTESIAN_POINT('Ctrl Pts',(-23.8889945285318,1.53797715326758,
0.));
#200966=CARTESIAN_POINT('Ctrl Pts',(-23.8687685639642,1.5437128445399,0.));
#200967=CARTESIAN_POINT('Ctrl Pts',(-23.8486272290705,1.54936729940541,
0.));
#200968=CARTESIAN_POINT('Ctrl Pts',(-23.8285714027636,1.55494069502635,
0.));
#200969=CARTESIAN_POINT('Ctrl Pts',(-23.8086019739194,1.56043321228633,
0.));
#200970=CARTESIAN_POINT('Ctrl Pts',(-23.7887198415878,1.56584503586843,
0.));
#200971=CARTESIAN_POINT('Ctrl Pts',(-23.7689259151862,1.57117635434408,
0.));
#200972=CARTESIAN_POINT('Ctrl Pts',(-23.749221114736,1.57642736025246,0.));
#200973=CARTESIAN_POINT('Ctrl Pts',(-23.72960637113,1.58159825017358,0.));
#200974=CARTESIAN_POINT('Ctrl Pts',(-23.710082626383,1.58668922481221,0.));
#200975=CARTESIAN_POINT('Ctrl Pts',(-23.6906508338833,1.59170048908633,
0.));
#200976=CARTESIAN_POINT('Ctrl Pts',(-23.671311958631,1.59663225222463,0.));
#200977=CARTESIAN_POINT('Ctrl Pts',(-23.6520669774876,1.60148472786595,
0.));
#200978=CARTESIAN_POINT('Ctrl Pts',(-23.6329168794929,1.60625813414672,
0.));
#200979=CARTESIAN_POINT('Ctrl Pts',(-23.6138626661653,1.61095269379778,
0.));
#200980=CARTESIAN_POINT('Ctrl Pts',(-23.5949053517997,1.61556863424698,
0.));
#200981=CARTESIAN_POINT('Ctrl Pts',(-23.57604596376,1.62010618772866,0.));
#200982=CARTESIAN_POINT('Ctrl Pts',(-23.5572855427601,1.62456559140064,
0.));
#200983=CARTESIAN_POINT('Ctrl Pts',(-23.538625143226,1.62894708745223,0.));
#200984=CARTESIAN_POINT('Ctrl Pts',(-23.5200658336612,1.63325092321725,
0.));
#200985=CARTESIAN_POINT('Ctrl Pts',(-23.5016086970003,1.63747735129474,
0.));
#200986=CARTESIAN_POINT('Ctrl Pts',(-23.4832548309645,1.64162662967528,
0.));
#200987=CARTESIAN_POINT('Ctrl Pts',(-23.4650053483932,1.64569902187611,
0.));
#200988=CARTESIAN_POINT('Ctrl Pts',(-23.4468613776574,1.6496947970734,0.));
#200989=CARTESIAN_POINT('Ctrl Pts',(-23.4288240631043,1.65361423023728,
0.));
#200990=CARTESIAN_POINT('Ctrl Pts',(-23.4108945654805,1.65745760227505,
0.));
#200991=CARTESIAN_POINT('Ctrl Pts',(-23.3930740623619,1.66122520018011,
0.));
#200992=CARTESIAN_POINT('Ctrl Pts',(-23.3753637485545,1.66491731718876,
0.));
#200993=CARTESIAN_POINT('Ctrl Pts',(-23.3577648365744,1.66853425293995,
0.));
#200994=CARTESIAN_POINT('Ctrl Pts',(-23.3402785571865,1.67207631363921,
0.));
#200995=CARTESIAN_POINT('Ctrl Pts',(-23.3229061599145,1.67554381222994,
0.));
#200996=CARTESIAN_POINT('Ctrl Pts',(-23.3056489135611,1.67893706857117,
0.));
#200997=CARTESIAN_POINT('Ctrl Pts',(-23.2885081066951,1.68225640962168,
0.));
#200998=CARTESIAN_POINT('Ctrl Pts',(-23.2714850482246,1.68550216963258,
0.));
#200999=CARTESIAN_POINT('Ctrl Pts',(-23.2545810680537,1.68867469034896,
0.));
#201000=CARTESIAN_POINT('Ctrl Pts',(-23.2377975177013,1.69177432121711,
0.));
#201001=CARTESIAN_POINT('Ctrl Pts',(-23.2211357709374,1.69480141959953,
0.));
#201002=CARTESIAN_POINT('Ctrl Pts',(-23.2045972243767,1.69775635099443,
0.));
#201003=CARTESIAN_POINT('Ctrl Pts',(-23.1881832981851,1.7006394892701,0.));
#201004=CARTESIAN_POINT('Ctrl Pts',(-23.1718954368751,1.70345121691276,
0.));
#201005=CARTESIAN_POINT('Ctrl Pts',(-23.1557351100614,1.70619192527852,
0.));
#201006=CARTESIAN_POINT('Ctrl Pts',(-23.1397038132356,1.70886201485452,
0.));
#201007=CARTESIAN_POINT('Ctrl Pts',(-23.1238030684925,1.71146189552174,
0.));
#201008=CARTESIAN_POINT('Ctrl Pts',(-23.1080344254286,1.71399198684704,
0.));
#201009=CARTESIAN_POINT('Ctrl Pts',(-23.0923994621213,1.71645271839296,
0.));
#201010=CARTESIAN_POINT('Ctrl Pts',(-23.0768997860709,1.71884453003027,
0.));
#201011=CARTESIAN_POINT('Ctrl Pts',(-23.0615370351562,1.72116787225991,
0.));
#201012=CARTESIAN_POINT('Ctrl Pts',(-23.0463128785531,1.72342320653746,
0.));
#201013=CARTESIAN_POINT('Ctrl Pts',(-23.0312290178883,1.72561100564045,
0.));
#201014=CARTESIAN_POINT('Ctrl Pts',(-23.0162871884168,1.72773175404708,
0.));
#201015=CARTESIAN_POINT('Ctrl Pts',(-23.001489160189,1.72978594832136,0.));
#201016=CARTESIAN_POINT('Ctrl Pts',(-22.9868367391978,1.7317740975019,0.));
#201017=CARTESIAN_POINT('Ctrl Pts',(-22.9723317685688,1.73369672350814,
0.));
#201018=CARTESIAN_POINT('Ctrl Pts',(-22.9579761301063,1.73555436162769,
0.));
#201019=CARTESIAN_POINT('Ctrl Pts',(-22.9437717457826,1.73734756100039,
0.));
#201020=CARTESIAN_POINT('Ctrl Pts',(-22.9297205792586,1.73907688511666,
0.));
#201021=CARTESIAN_POINT('Ctrl Pts',(-22.9158246373363,1.74074291231058,
0.));
#201022=CARTESIAN_POINT('Ctrl Pts',(-22.9020859716141,1.7423462363008,0.));
#201023=CARTESIAN_POINT('Ctrl Pts',(-22.888506680335,1.74388746677702,0.));
#201024=CARTESIAN_POINT('Ctrl Pts',(-22.8750889101696,1.74536722998201,
0.));
#201025=CARTESIAN_POINT('Ctrl Pts',(-22.8618348580235,1.74678616930664,
0.));
#201026=CARTESIAN_POINT('Ctrl Pts',(-22.8487467728076,1.74814494588492,
0.));
#201027=CARTESIAN_POINT('Ctrl Pts',(-22.8358269579853,1.74944423940115,
0.));
#201028=CARTESIAN_POINT('Ctrl Pts',(-22.8230777741284,1.75068474890883,
0.));
#201029=CARTESIAN_POINT('Ctrl Pts',(-22.8105016414713,1.75186719365592,
0.));
#201030=CARTESIAN_POINT('Ctrl Pts',(-22.7981010424314,1.75299231391466,
0.));
#201031=CARTESIAN_POINT('Ctrl Pts',(-22.7858785242361,1.75406087182936,
0.));
#201032=CARTESIAN_POINT('Ctrl Pts',(-22.7738367016118,1.75507365227131,
0.));
#201033=CARTESIAN_POINT('Ctrl Pts',(-22.7619782595013,1.75603146371641,
0.));
#201034=CARTESIAN_POINT('Ctrl Pts',(-22.750305955645,1.75693513908907,0.));
#201035=CARTESIAN_POINT('Ctrl Pts',(-22.7388226235559,1.75778553673244,
0.));
#201036=CARTESIAN_POINT('Ctrl Pts',(-22.72753117773,1.75858354204633,0.));
#201037=CARTESIAN_POINT('Ctrl Pts',(-22.7164346186006,1.75933006905925,
0.));
#201038=CARTESIAN_POINT('Ctrl Pts',(-22.7055360375485,1.76002606202401,
0.));
#201039=CARTESIAN_POINT('Ctrl Pts',(-22.6948386219851,1.76067249704886,
0.));
#201040=CARTESIAN_POINT('Ctrl Pts',(-22.684345658525,1.76127038310614,0.));
#201041=CARTESIAN_POINT('Ctrl Pts',(-22.67406053567,1.76182076289525,0.));
#201042=CARTESIAN_POINT('Ctrl Pts',(-22.6639867471753,1.76232471392568,
0.));
#201043=CARTESIAN_POINT('Ctrl Pts',(-22.6541278938409,1.76278334912561,
0.));
#201044=CARTESIAN_POINT('Ctrl Pts',(-22.6444876940423,1.76319782013916,
0.));
#201045=CARTESIAN_POINT('Ctrl Pts',(-22.6350699979359,1.76356932176273,
0.));
#201046=CARTESIAN_POINT('Ctrl Pts',(-22.6258787994848,1.76389909571403,
0.));
#201047=CARTESIAN_POINT('Ctrl Pts',(-22.6169182517694,1.76418843543739,
0.));
#201048=CARTESIAN_POINT('Ctrl Pts',(-22.6081926681343,1.76443868648015,
0.));
#201049=CARTESIAN_POINT('Ctrl Pts',(-22.5997065145638,1.76465124413557,
0.));
#201050=CARTESIAN_POINT('Ctrl Pts',(-22.5914644078106,1.76482755288411,
0.));
#201051=CARTESIAN_POINT('Ctrl Pts',(-22.5834711038022,1.76496910283088,
0.));
#201052=CARTESIAN_POINT('Ctrl Pts',(-22.5757315316353,1.76507744026746,
0.));
#201053=CARTESIAN_POINT('Ctrl Pts',(-22.5682508499873,1.76515418518831,
0.));
#201054=CARTESIAN_POINT('Ctrl Pts',(-22.5610344912501,1.7652010450045,0.));
#201055=CARTESIAN_POINT('Ctrl Pts',(-22.5540882235837,1.76521983384062,
0.));
#201056=CARTESIAN_POINT('Ctrl Pts',(-22.5474180954006,1.76521245524047,
0.));
#201057=CARTESIAN_POINT('Ctrl Pts',(-22.5410303590892,1.76518087841493,
0.));
#201058=CARTESIAN_POINT('Ctrl Pts',(-22.5349313983571,1.76512711563254,
0.));
#201059=CARTESIAN_POINT('Ctrl Pts',(-22.529127665298,1.76505320262759,0.));
#201060=CARTESIAN_POINT('Ctrl Pts',(-22.5236259635515,1.76496128643375,
0.));
#201061=CARTESIAN_POINT('Ctrl Pts',(-22.5184336670207,1.76485369319895,
0.));
#201062=CARTESIAN_POINT('Ctrl Pts',(-22.5135590569554,1.76473303281149,
0.));
#201063=CARTESIAN_POINT('Ctrl Pts',(-22.5090112700212,1.76460218257313,
0.));
#201064=CARTESIAN_POINT('Ctrl Pts',(-22.5047996391978,1.76446408210364,
0.));
#201065=CARTESIAN_POINT('Ctrl Pts',(-22.5009332677316,1.76432160068737,
0.));
#201066=CARTESIAN_POINT('Ctrl Pts',(-22.4974203063191,1.76417731243483,
0.));
#201067=CARTESIAN_POINT('Ctrl Pts',(-22.4942693792449,1.76403393880316,
0.));
#201068=CARTESIAN_POINT('Ctrl Pts',(-22.4914909094908,1.76389475965714,
0.));
#201069=CARTESIAN_POINT('Ctrl Pts',(-22.4890991659479,1.76376424879468,
0.));
#201070=CARTESIAN_POINT('Ctrl Pts',(-22.4871115206572,1.76364784232925,
0.));
#201071=CARTESIAN_POINT('Ctrl Pts',(-22.4855446605991,1.76355076045549,
0.));
#201072=CARTESIAN_POINT('Ctrl Pts',(-22.4844112933125,1.76347698284861,
0.));
#201073=CARTESIAN_POINT('Ctrl Pts',(-22.4838562517064,1.76343813434659,
0.));
#201074=CARTESIAN_POINT('Ctrl Pts',(-22.4836387052228,1.76342064263637,
0.));
#201075=CARTESIAN_POINT('Ctrl Pts',(-22.4835819929788,1.7634141553879,0.));
#201076=CARTESIAN_POINT('Ctrl Pts',(-22.4835757167854,1.7634122053118,0.));
#201077=CARTESIAN_POINT('',(-25.991588367311,0.661312440730901,0.));
#201078=CARTESIAN_POINT('Ctrl Pts',(-22.1738711152697,4.11585220600461,
0.));
#201079=CARTESIAN_POINT('Ctrl Pts',(-22.1738711152697,4.11585220600461,
12.));
#201080=CARTESIAN_POINT('Ctrl Pts',(-22.173877682324,4.11585194677442,0.));
#201081=CARTESIAN_POINT('Ctrl Pts',(-22.173877682324,4.11585194677442,12.));
#201082=CARTESIAN_POINT('Ctrl Pts',(-22.1739341411687,4.11586035878287,
0.));
#201083=CARTESIAN_POINT('Ctrl Pts',(-22.1739341411687,4.11586035878287,
12.));
#201084=CARTESIAN_POINT('Ctrl Pts',(-22.1741488021234,4.11589976826166,
0.));
#201085=CARTESIAN_POINT('Ctrl Pts',(-22.1741488021234,4.11589976826166,
12.));
#201086=CARTESIAN_POINT('Ctrl Pts',(-22.1746949858775,4.11600589882845,
0.));
#201087=CARTESIAN_POINT('Ctrl Pts',(-22.1746949858775,4.11600589882845,
12.));
#201088=CARTESIAN_POINT('Ctrl Pts',(-22.1758088296598,4.11622797217068,
0.));
#201089=CARTESIAN_POINT('Ctrl Pts',(-22.1758088296598,4.11622797217068,
12.));
#201090=CARTESIAN_POINT('Ctrl Pts',(-22.177347426894,4.11653973150518,0.));
#201091=CARTESIAN_POINT('Ctrl Pts',(-22.177347426894,4.11653973150518,12.));
#201092=CARTESIAN_POINT('Ctrl Pts',(-22.179297473024,4.11694173195003,0.));
#201093=CARTESIAN_POINT('Ctrl Pts',(-22.179297473024,4.11694173195003,12.));
#201094=CARTESIAN_POINT('Ctrl Pts',(-22.1816414985788,4.11743469691756,
0.));
#201095=CARTESIAN_POINT('Ctrl Pts',(-22.1816414985788,4.11743469691756,
12.));
#201096=CARTESIAN_POINT('Ctrl Pts',(-22.1843613164855,4.11801938107479,
0.));
#201097=CARTESIAN_POINT('Ctrl Pts',(-22.1843613164855,4.11801938107479,
12.));
#201098=CARTESIAN_POINT('Ctrl Pts',(-22.1874419861496,4.11869641271773,
0.));
#201099=CARTESIAN_POINT('Ctrl Pts',(-22.1874419861496,4.11869641271773,
12.));
#201100=CARTESIAN_POINT('Ctrl Pts',(-22.1908725908525,4.11946626228636,
0.));
#201101=CARTESIAN_POINT('Ctrl Pts',(-22.1908725908525,4.11946626228636,
12.));
#201102=CARTESIAN_POINT('Ctrl Pts',(-22.1946440958098,4.12032932637736,
0.));
#201103=CARTESIAN_POINT('Ctrl Pts',(-22.1946440958098,4.12032932637736,
12.));
#201104=CARTESIAN_POINT('Ctrl Pts',(-22.1987479618246,4.12128598183522,
0.));
#201105=CARTESIAN_POINT('Ctrl Pts',(-22.1987479618246,4.12128598183522,
12.));
#201106=CARTESIAN_POINT('Ctrl Pts',(-22.2031746532106,4.12233664408227,
0.));
#201107=CARTESIAN_POINT('Ctrl Pts',(-22.2031746532106,4.12233664408227,
12.));
#201108=CARTESIAN_POINT('Ctrl Pts',(-22.2079143941719,4.12348173702023,
0.));
#201109=CARTESIAN_POINT('Ctrl Pts',(-22.2079143941719,4.12348173702023,
12.));
#201110=CARTESIAN_POINT('Ctrl Pts',(-22.2129576146671,4.12472167516607,
0.));
#201111=CARTESIAN_POINT('Ctrl Pts',(-22.2129576146671,4.12472167516607,
12.));
#201112=CARTESIAN_POINT('Ctrl Pts',(-22.2182956401341,4.12605683613307,
0.));
#201113=CARTESIAN_POINT('Ctrl Pts',(-22.2182956401341,4.12605683613307,
12.));
#201114=CARTESIAN_POINT('Ctrl Pts',(-22.2239207458781,4.12748755830104,
0.));
#201115=CARTESIAN_POINT('Ctrl Pts',(-22.2239207458781,4.12748755830104,
12.));
#201116=CARTESIAN_POINT('Ctrl Pts',(-22.2298258043947,4.12901415463379,
0.));
#201117=CARTESIAN_POINT('Ctrl Pts',(-22.2298258043947,4.12901415463379,
12.));
#201118=CARTESIAN_POINT('Ctrl Pts',(-22.2360040565533,4.13063692157498,
0.));
#201119=CARTESIAN_POINT('Ctrl Pts',(-22.2360040565533,4.13063692157498,
12.));
#201120=CARTESIAN_POINT('Ctrl Pts',(-22.2424488153523,4.1323561506016,0.));
#201121=CARTESIAN_POINT('Ctrl Pts',(-22.2424488153523,4.1323561506016,12.));
#201122=CARTESIAN_POINT('Ctrl Pts',(-22.249153531779,4.1341721255881,0.));
#201123=CARTESIAN_POINT('Ctrl Pts',(-22.249153531779,4.1341721255881,12.));
#201124=CARTESIAN_POINT('Ctrl Pts',(-22.2561118708421,4.13608511977225,
0.));
#201125=CARTESIAN_POINT('Ctrl Pts',(-22.2561118708421,4.13608511977225,
12.));
#201126=CARTESIAN_POINT('Ctrl Pts',(-22.2633177913972,4.13809539255421,
0.));
#201127=CARTESIAN_POINT('Ctrl Pts',(-22.2633177913972,4.13809539255421,
12.));
#201128=CARTESIAN_POINT('Ctrl Pts',(-22.2707656042457,4.14020318715991,
0.));
#201129=CARTESIAN_POINT('Ctrl Pts',(-22.2707656042457,4.14020318715991,
12.));
#201130=CARTESIAN_POINT('Ctrl Pts',(-22.2784499072027,4.14240873321984,
0.));
#201131=CARTESIAN_POINT('Ctrl Pts',(-22.2784499072027,4.14240873321984,
12.));
#201132=CARTESIAN_POINT('Ctrl Pts',(-22.2863655389166,4.14471224859295,
0.));
#201133=CARTESIAN_POINT('Ctrl Pts',(-22.2863655389166,4.14471224859295,
12.));
#201134=CARTESIAN_POINT('Ctrl Pts',(-22.2945075198467,4.14711394168556,
0.));
#201135=CARTESIAN_POINT('Ctrl Pts',(-22.2945075198467,4.14711394168556,
12.));
#201136=CARTESIAN_POINT('Ctrl Pts',(-22.3028710166933,4.14961401285522,
0.));
#201137=CARTESIAN_POINT('Ctrl Pts',(-22.3028710166933,4.14961401285522,
12.));
#201138=CARTESIAN_POINT('Ctrl Pts',(-22.3114513545185,4.1522126539699,0.));
#201139=CARTESIAN_POINT('Ctrl Pts',(-22.3114513545185,4.1522126539699,12.));
#201140=CARTESIAN_POINT('Ctrl Pts',(-22.3202440186979,4.15491004835281,
0.));
#201141=CARTESIAN_POINT('Ctrl Pts',(-22.3202440186979,4.15491004835281,
12.));
#201142=CARTESIAN_POINT('Ctrl Pts',(-22.3292446628959,4.15770637047889,
0.));
#201143=CARTESIAN_POINT('Ctrl Pts',(-22.3292446628959,4.15770637047889,
12.));
#201144=CARTESIAN_POINT('Ctrl Pts',(-22.3384491078602,4.16060178604164,
0.));
#201145=CARTESIAN_POINT('Ctrl Pts',(-22.3384491078602,4.16060178604164,
12.));
#201146=CARTESIAN_POINT('Ctrl Pts',(-22.3478533253889,4.16359645263187,
0.));
#201147=CARTESIAN_POINT('Ctrl Pts',(-22.3478533253889,4.16359645263187,
12.));
#201148=CARTESIAN_POINT('Ctrl Pts',(-22.3574534257396,4.166690520266,0.));
#201149=CARTESIAN_POINT('Ctrl Pts',(-22.3574534257396,4.166690520266,12.));
#201150=CARTESIAN_POINT('Ctrl Pts',(-22.36724564276,4.16988413199457,0.));
#201151=CARTESIAN_POINT('Ctrl Pts',(-22.36724564276,4.16988413199457,12.));
#201152=CARTESIAN_POINT('Ctrl Pts',(-22.3772263228617,4.17317742436145,
0.));
#201153=CARTESIAN_POINT('Ctrl Pts',(-22.3772263228617,4.17317742436145,
12.));
#201154=CARTESIAN_POINT('Ctrl Pts',(-22.3873919231334,4.17657052752825,
0.));
#201155=CARTESIAN_POINT('Ctrl Pts',(-22.3873919231334,4.17657052752825,
12.));
#201156=CARTESIAN_POINT('Ctrl Pts',(-22.3977390078075,4.18006356544882,
0.));
#201157=CARTESIAN_POINT('Ctrl Pts',(-22.3977390078075,4.18006356544882,
12.));
#201158=CARTESIAN_POINT('Ctrl Pts',(-22.4082642454453,4.1836566560085,0.));
#201159=CARTESIAN_POINT('Ctrl Pts',(-22.4082642454453,4.1836566560085,12.));
#201160=CARTESIAN_POINT('Ctrl Pts',(-22.4189644056115,4.1873499111772,0.));
#201161=CARTESIAN_POINT('Ctrl Pts',(-22.4189644056115,4.1873499111772,12.));
#201162=CARTESIAN_POINT('Ctrl Pts',(-22.4298363535421,4.19114343726941,
0.));
#201163=CARTESIAN_POINT('Ctrl Pts',(-22.4298363535421,4.19114343726941,
12.));
#201164=CARTESIAN_POINT('Ctrl Pts',(-22.4408770448917,4.1950373351886,0.));
#201165=CARTESIAN_POINT('Ctrl Pts',(-22.4408770448917,4.1950373351886,12.));
#201166=CARTESIAN_POINT('Ctrl Pts',(-22.4520835205419,4.19903170066354,
0.));
#201167=CARTESIAN_POINT('Ctrl Pts',(-22.4520835205419,4.19903170066354,
12.));
#201168=CARTESIAN_POINT('Ctrl Pts',(-22.4634529011433,4.2031266244817,0.));
#201169=CARTESIAN_POINT('Ctrl Pts',(-22.4634529011433,4.2031266244817,12.));
#201170=CARTESIAN_POINT('Ctrl Pts',(-22.4749823839915,4.20732219265648,
0.));
#201171=CARTESIAN_POINT('Ctrl Pts',(-22.4749823839915,4.20732219265648,
12.));
#201172=CARTESIAN_POINT('Ctrl Pts',(-22.4866692403147,4.21161848657428,
0.));
#201173=CARTESIAN_POINT('Ctrl Pts',(-22.4866692403147,4.21161848657428,
12.));
#201174=CARTESIAN_POINT('Ctrl Pts',(-22.4985108124229,4.21601558313908,
0.));
#201175=CARTESIAN_POINT('Ctrl Pts',(-22.4985108124229,4.21601558313908,
12.));
#201176=CARTESIAN_POINT('Ctrl Pts',(-22.5105045108882,4.22051355490196,
0.));
#201177=CARTESIAN_POINT('Ctrl Pts',(-22.5105045108882,4.22051355490196,
12.));
#201178=CARTESIAN_POINT('Ctrl Pts',(-22.5226478117885,4.2251124702004,0.));
#201179=CARTESIAN_POINT('Ctrl Pts',(-22.5226478117885,4.2251124702004,12.));
#201180=CARTESIAN_POINT('Ctrl Pts',(-22.5349382540587,4.22981239330731,
0.));
#201181=CARTESIAN_POINT('Ctrl Pts',(-22.5349382540587,4.22981239330731,
12.));
#201182=CARTESIAN_POINT('Ctrl Pts',(-22.5473734368086,4.23461338456713,
0.));
#201183=CARTESIAN_POINT('Ctrl Pts',(-22.5473734368086,4.23461338456713,
12.));
#201184=CARTESIAN_POINT('Ctrl Pts',(-22.559951016643,4.23951550052526,0.));
#201185=CARTESIAN_POINT('Ctrl Pts',(-22.559951016643,4.23951550052526,12.));
#201186=CARTESIAN_POINT('Ctrl Pts',(-22.5726687049922,4.24451879404858,
0.));
#201187=CARTESIAN_POINT('Ctrl Pts',(-22.5726687049922,4.24451879404858,
12.));
#201188=CARTESIAN_POINT('Ctrl Pts',(-22.5855242662479,4.24962331444184,
0.));
#201189=CARTESIAN_POINT('Ctrl Pts',(-22.5855242662479,4.24962331444184,
12.));
#201190=CARTESIAN_POINT('Ctrl Pts',(-22.5985155158637,4.25482910755485,
0.));
#201191=CARTESIAN_POINT('Ctrl Pts',(-22.5985155158637,4.25482910755485,
12.));
#201192=CARTESIAN_POINT('Ctrl Pts',(-22.611640318482,4.26013621588303,0.));
#201193=CARTESIAN_POINT('Ctrl Pts',(-22.611640318482,4.26013621588303,12.));
#201194=CARTESIAN_POINT('Ctrl Pts',(-22.6248965859975,4.26554467865571,
0.));
#201195=CARTESIAN_POINT('Ctrl Pts',(-22.6248965859975,4.26554467865571,
12.));
#201196=CARTESIAN_POINT('Ctrl Pts',(-22.6382822758171,4.27105453192999,
0.));
#201197=CARTESIAN_POINT('Ctrl Pts',(-22.6382822758171,4.27105453192999,
12.));
#201198=CARTESIAN_POINT('Ctrl Pts',(-22.6517953893303,4.27666580869117,
0.));
#201199=CARTESIAN_POINT('Ctrl Pts',(-22.6517953893303,4.27666580869117,
12.));
#201200=CARTESIAN_POINT('Ctrl Pts',(-22.665433970311,4.28237853894059,0.));
#201201=CARTESIAN_POINT('Ctrl Pts',(-22.665433970311,4.28237853894059,12.));
#201202=CARTESIAN_POINT('Ctrl Pts',(-22.6791961033537,4.28819274977766,
0.));
#201203=CARTESIAN_POINT('Ctrl Pts',(-22.6791961033537,4.28819274977766,
12.));
#201204=CARTESIAN_POINT('Ctrl Pts',(-22.6930799122545,4.29410846547061,
0.));
#201205=CARTESIAN_POINT('Ctrl Pts',(-22.6930799122545,4.29410846547061,
12.));
#201206=CARTESIAN_POINT('Ctrl Pts',(-22.707083558756,4.30012570754066,0.));
#201207=CARTESIAN_POINT('Ctrl Pts',(-22.707083558756,4.30012570754066,12.));
#201208=CARTESIAN_POINT('Ctrl Pts',(-22.7212052413384,4.30624449484074,
0.));
#201209=CARTESIAN_POINT('Ctrl Pts',(-22.7212052413384,4.30624449484074,
12.));
#201210=CARTESIAN_POINT('Ctrl Pts',(-22.7354431939927,4.3124648436255,0.));
#201211=CARTESIAN_POINT('Ctrl Pts',(-22.7354431939927,4.3124648436255,12.));
#201212=CARTESIAN_POINT('Ctrl Pts',(-22.7497956849852,4.3187867676123,0.));
#201213=CARTESIAN_POINT('Ctrl Pts',(-22.7497956849852,4.3187867676123,12.));
#201214=CARTESIAN_POINT('Ctrl Pts',(-22.764261015648,4.32521027803747,0.));
#201215=CARTESIAN_POINT('Ctrl Pts',(-22.764261015648,4.32521027803747,12.));
#201216=CARTESIAN_POINT('Ctrl Pts',(-22.7788375194081,4.33173538373182,
0.));
#201217=CARTESIAN_POINT('Ctrl Pts',(-22.7788375194081,4.33173538373182,
12.));
#201218=CARTESIAN_POINT('Ctrl Pts',(-22.7935235607807,4.33836209118442,
0.));
#201219=CARTESIAN_POINT('Ctrl Pts',(-22.7935235607807,4.33836209118442,
12.));
#201220=CARTESIAN_POINT('Ctrl Pts',(-22.808317534379,4.34509040460065,0.));
#201221=CARTESIAN_POINT('Ctrl Pts',(-22.808317534379,4.34509040460065,12.));
#201222=CARTESIAN_POINT('Ctrl Pts',(-22.8232178638873,4.35192032594801,
0.));
#201223=CARTESIAN_POINT('Ctrl Pts',(-22.8232178638873,4.35192032594801,
12.));
#201224=CARTESIAN_POINT('Ctrl Pts',(-22.838223001118,4.35885185500559,0.));
#201225=CARTESIAN_POINT('Ctrl Pts',(-22.838223001118,4.35885185500559,12.));
#201226=CARTESIAN_POINT('Ctrl Pts',(-22.8533314252419,4.36588498943009,
0.));
#201227=CARTESIAN_POINT('Ctrl Pts',(-22.8533314252419,4.36588498943009,
12.));
#201228=CARTESIAN_POINT('Ctrl Pts',(-22.8685416419725,4.37301972480752,
0.));
#201229=CARTESIAN_POINT('Ctrl Pts',(-22.8685416419725,4.37301972480752,
12.));
#201230=CARTESIAN_POINT('Ctrl Pts',(-22.8838521827702,4.38025605470089,
0.));
#201231=CARTESIAN_POINT('Ctrl Pts',(-22.8838521827702,4.38025605470089,
12.));
#201232=CARTESIAN_POINT('Ctrl Pts',(-22.8992616040108,4.38759397068391,
0.));
#201233=CARTESIAN_POINT('Ctrl Pts',(-22.8992616040108,4.38759397068391,
12.));
#201234=CARTESIAN_POINT('Ctrl Pts',(-22.9147684862425,4.39503346238454,
0.));
#201235=CARTESIAN_POINT('Ctrl Pts',(-22.9147684862425,4.39503346238454,
12.));
#201236=CARTESIAN_POINT('Ctrl Pts',(-22.9303714335549,4.40257451754307,
0.));
#201237=CARTESIAN_POINT('Ctrl Pts',(-22.9303714335549,4.40257451754307,
12.));
#201238=CARTESIAN_POINT('Ctrl Pts',(-22.9460690729093,4.41021712205547,
0.));
#201239=CARTESIAN_POINT('Ctrl Pts',(-22.9460690729093,4.41021712205547,
12.));
#201240=CARTESIAN_POINT('Ctrl Pts',(-22.9618600534866,4.41796126001309,
0.));
#201241=CARTESIAN_POINT('Ctrl Pts',(-22.9618600534866,4.41796126001309,
12.));
#201242=CARTESIAN_POINT('Ctrl Pts',(-22.9777430460021,4.42580691372771,
0.));
#201243=CARTESIAN_POINT('Ctrl Pts',(-22.9777430460021,4.42580691372771,
12.));
#201244=CARTESIAN_POINT('Ctrl Pts',(-22.9937167421009,4.43375406376904,
0.));
#201245=CARTESIAN_POINT('Ctrl Pts',(-22.9937167421009,4.43375406376904,
12.));
#201246=CARTESIAN_POINT('Ctrl Pts',(-23.0097798538399,4.44180268901666,
0.));
#201247=CARTESIAN_POINT('Ctrl Pts',(-23.0097798538399,4.44180268901666,
12.));
#201248=CARTESIAN_POINT('Ctrl Pts',(-23.0259311131395,4.44995276669698,
0.));
#201249=CARTESIAN_POINT('Ctrl Pts',(-23.0259311131395,4.44995276669698,
12.));
#201250=CARTESIAN_POINT('Ctrl Pts',(-23.0421692712466,4.45820427241676,
0.));
#201251=CARTESIAN_POINT('Ctrl Pts',(-23.0421692712466,4.45820427241676,
12.));
#201252=CARTESIAN_POINT('Ctrl Pts',(-23.0584930981723,4.46655718018205,
0.));
#201253=CARTESIAN_POINT('Ctrl Pts',(-23.0584930981723,4.46655718018205,
12.));
#201254=CARTESIAN_POINT('Ctrl Pts',(-23.0749013821868,4.47501146242821,
0.));
#201255=CARTESIAN_POINT('Ctrl Pts',(-23.0749013821868,4.47501146242821,
12.));
#201256=CARTESIAN_POINT('Ctrl Pts',(-23.0913929293909,4.48356709006756,
0.));
#201257=CARTESIAN_POINT('Ctrl Pts',(-23.0913929293909,4.48356709006756,
12.));
#201258=CARTESIAN_POINT('Ctrl Pts',(-23.1079665632629,4.49222403252201,
0.));
#201259=CARTESIAN_POINT('Ctrl Pts',(-23.1079665632629,4.49222403252201,
12.));
#201260=CARTESIAN_POINT('Ctrl Pts',(-23.1246211242117,4.50098225775178,
0.));
#201261=CARTESIAN_POINT('Ctrl Pts',(-23.1246211242117,4.50098225775178,
12.));
#201262=CARTESIAN_POINT('Ctrl Pts',(-23.1413554691136,4.50984173227087,
0.));
#201263=CARTESIAN_POINT('Ctrl Pts',(-23.1413554691136,4.50984173227087,
12.));
#201264=CARTESIAN_POINT('Ctrl Pts',(-23.1581684708778,4.51880242116785,
0.));
#201265=CARTESIAN_POINT('Ctrl Pts',(-23.1581684708778,4.51880242116785,
12.));
#201266=CARTESIAN_POINT('Ctrl Pts',(-23.1750590180923,4.52786428815047,
0.));
#201267=CARTESIAN_POINT('Ctrl Pts',(-23.1750590180923,4.52786428815047,
12.));
#201268=CARTESIAN_POINT('Ctrl Pts',(-23.1920260146474,4.53702729557585,
0.));
#201269=CARTESIAN_POINT('Ctrl Pts',(-23.1920260146474,4.53702729557585,
12.));
#201270=CARTESIAN_POINT('Ctrl Pts',(-23.2090683793627,4.54629140447542,
0.));
#201271=CARTESIAN_POINT('Ctrl Pts',(-23.2090683793627,4.54629140447542,
12.));
#201272=CARTESIAN_POINT('Ctrl Pts',(-23.2261850456055,4.55565657456956,
0.));
#201273=CARTESIAN_POINT('Ctrl Pts',(-23.2261850456055,4.55565657456956,
12.));
#201274=CARTESIAN_POINT('Ctrl Pts',(-23.2433749609117,4.5651227642781,0.));
#201275=CARTESIAN_POINT('Ctrl Pts',(-23.2433749609117,4.5651227642781,12.));
#201276=CARTESIAN_POINT('Ctrl Pts',(-23.2606370866853,4.5746899307607,0.));
#201277=CARTESIAN_POINT('Ctrl Pts',(-23.2606370866853,4.5746899307607,12.));
#201278=CARTESIAN_POINT('Ctrl Pts',(-23.2779703978868,4.58435802994674,
0.));
#201279=CARTESIAN_POINT('Ctrl Pts',(-23.2779703978868,4.58435802994674,
12.));
#201280=CARTESIAN_POINT('Ctrl Pts',(-23.295373882719,4.59412701655749,0.));
#201281=CARTESIAN_POINT('Ctrl Pts',(-23.295373882719,4.59412701655749,12.));
#201282=CARTESIAN_POINT('Ctrl Pts',(-23.3128465423119,4.60399684412174,
0.));
#201283=CARTESIAN_POINT('Ctrl Pts',(-23.3128465423119,4.60399684412174,
12.));
#201284=CARTESIAN_POINT('Ctrl Pts',(-23.3303873903947,4.61396746497848,
0.));
#201285=CARTESIAN_POINT('Ctrl Pts',(-23.3303873903947,4.61396746497848,
12.));
#201286=CARTESIAN_POINT('Ctrl Pts',(-23.3479954530281,4.62403883030823,
0.));
#201287=CARTESIAN_POINT('Ctrl Pts',(-23.3479954530281,4.62403883030823,
12.));
#201288=CARTESIAN_POINT('Ctrl Pts',(-23.3656697683496,4.63421089016554,
0.));
#201289=CARTESIAN_POINT('Ctrl Pts',(-23.3656697683496,4.63421089016554,
12.));
#201290=CARTESIAN_POINT('Ctrl Pts',(-23.383409386307,4.64448359349935,0.));
#201291=CARTESIAN_POINT('Ctrl Pts',(-23.383409386307,4.64448359349935,12.));
#201292=CARTESIAN_POINT('Ctrl Pts',(-23.4012133683957,4.65485688816921,
0.));
#201293=CARTESIAN_POINT('Ctrl Pts',(-23.4012133683957,4.65485688816921,
12.));
#201294=CARTESIAN_POINT('Ctrl Pts',(-23.4190807873798,4.66533072094663,
0.));
#201295=CARTESIAN_POINT('Ctrl Pts',(-23.4190807873798,4.66533072094663,
12.));
#201296=CARTESIAN_POINT('Ctrl Pts',(-23.4370107270444,4.6759050375305,0.));
#201297=CARTESIAN_POINT('Ctrl Pts',(-23.4370107270444,4.6759050375305,12.));
#201298=CARTESIAN_POINT('Ctrl Pts',(-23.4550022819853,4.68657978258297,
0.));
#201299=CARTESIAN_POINT('Ctrl Pts',(-23.4550022819853,4.68657978258297,
12.));
#201300=CARTESIAN_POINT('Ctrl Pts',(-23.4730545573849,4.69735489975023,
0.));
#201301=CARTESIAN_POINT('Ctrl Pts',(-23.4730545573849,4.69735489975023,
12.));
#201302=CARTESIAN_POINT('Ctrl Pts',(-23.491166668789,4.7082303316782,0.));
#201303=CARTESIAN_POINT('Ctrl Pts',(-23.491166668789,4.7082303316782,12.));
#201304=CARTESIAN_POINT('Ctrl Pts',(-23.5093377418784,4.71920602001904,
0.));
#201305=CARTESIAN_POINT('Ctrl Pts',(-23.5093377418784,4.71920602001904,
12.));
#201306=CARTESIAN_POINT('Ctrl Pts',(-23.5275669122378,4.73028190543031,
0.));
#201307=CARTESIAN_POINT('Ctrl Pts',(-23.5275669122378,4.73028190543031,
12.));
#201308=CARTESIAN_POINT('Ctrl Pts',(-23.5458533251715,4.74145792760698,
0.));
#201309=CARTESIAN_POINT('Ctrl Pts',(-23.5458533251715,4.74145792760698,
12.));
#201310=CARTESIAN_POINT('Ctrl Pts',(-23.564196135517,4.75273402530615,0.));
#201311=CARTESIAN_POINT('Ctrl Pts',(-23.564196135517,4.75273402530615,12.));
#201312=CARTESIAN_POINT('Ctrl Pts',(-23.5825945074535,4.7641101363625,0.));
#201313=CARTESIAN_POINT('Ctrl Pts',(-23.5825945074535,4.7641101363625,12.));
#201314=CARTESIAN_POINT('Ctrl Pts',(-23.6010476143099,4.77558619769875,
0.));
#201315=CARTESIAN_POINT('Ctrl Pts',(-23.6010476143099,4.77558619769875,
12.));
#201316=CARTESIAN_POINT('Ctrl Pts',(-23.6195546383625,4.78716214532104,
0.));
#201317=CARTESIAN_POINT('Ctrl Pts',(-23.6195546383625,4.78716214532104,
12.));
#201318=CARTESIAN_POINT('Ctrl Pts',(-23.6381147706581,4.79883791433229,
0.));
#201319=CARTESIAN_POINT('Ctrl Pts',(-23.6381147706581,4.79883791433229,
12.));
#201320=CARTESIAN_POINT('Ctrl Pts',(-23.6567272108631,4.81061343896442,
0.));
#201321=CARTESIAN_POINT('Ctrl Pts',(-23.6567272108631,4.81061343896442,
12.));
#201322=CARTESIAN_POINT('Ctrl Pts',(-23.6753911671023,4.82248865259569,
0.));
#201323=CARTESIAN_POINT('Ctrl Pts',(-23.6753911671023,4.82248865259569,
12.));
#201324=CARTESIAN_POINT('Ctrl Pts',(-23.6941058557971,4.83446348776267,
0.));
#201325=CARTESIAN_POINT('Ctrl Pts',(-23.6941058557971,4.83446348776267,
12.));
#201326=CARTESIAN_POINT('Ctrl Pts',(-23.7128705015014,4.84653787616422,
0.));
#201327=CARTESIAN_POINT('Ctrl Pts',(-23.7128705015014,4.84653787616422,
12.));
#201328=CARTESIAN_POINT('Ctrl Pts',(-23.7316843367308,4.85871174865491,
0.));
#201329=CARTESIAN_POINT('Ctrl Pts',(-23.7316843367308,4.85871174865491,
12.));
#201330=CARTESIAN_POINT('Ctrl Pts',(-23.7505466018239,4.87098503527142,
0.));
#201331=CARTESIAN_POINT('Ctrl Pts',(-23.7505466018239,4.87098503527142,
12.));
#201332=CARTESIAN_POINT('Ctrl Pts',(-23.7694565448044,4.88335766525565,
0.));
#201333=CARTESIAN_POINT('Ctrl Pts',(-23.7694565448044,4.88335766525565,
12.));
#201334=CARTESIAN_POINT('Ctrl Pts',(-23.7884134212381,4.89582956706771,
0.));
#201335=CARTESIAN_POINT('Ctrl Pts',(-23.7884134212381,4.89582956706771,
12.));
#201336=CARTESIAN_POINT('Ctrl Pts',(-23.8074164940897,4.90840066839346,
0.));
#201337=CARTESIAN_POINT('Ctrl Pts',(-23.8074164940897,4.90840066839346,
12.));
#201338=CARTESIAN_POINT('Ctrl Pts',(-23.8264650335721,4.92107089613976,
0.));
#201339=CARTESIAN_POINT('Ctrl Pts',(-23.8264650335721,4.92107089613976,
12.));
#201340=CARTESIAN_POINT('Ctrl Pts',(-23.8455583170062,4.93384017643441,
0.));
#201341=CARTESIAN_POINT('Ctrl Pts',(-23.8455583170062,4.93384017643441,
12.));
#201342=CARTESIAN_POINT('Ctrl Pts',(-23.8646956287172,4.94670843465868,
0.));
#201343=CARTESIAN_POINT('Ctrl Pts',(-23.8646956287172,4.94670843465868,
12.));
#201344=CARTESIAN_POINT('Ctrl Pts',(-23.883876259922,4.95967559546565,0.));
#201345=CARTESIAN_POINT('Ctrl Pts',(-23.883876259922,4.95967559546565,12.));
#201346=CARTESIAN_POINT('Ctrl Pts',(-23.9030995086164,4.97274158279228,
0.));
#201347=CARTESIAN_POINT('Ctrl Pts',(-23.9030995086164,4.97274158279228,
12.));
#201348=CARTESIAN_POINT('Ctrl Pts',(-23.9223646794591,4.98590631986532,
0.));
#201349=CARTESIAN_POINT('Ctrl Pts',(-23.9223646794591,4.98590631986532,
12.));
#201350=CARTESIAN_POINT('Ctrl Pts',(-23.9416710836529,4.99916972919309,
0.));
#201351=CARTESIAN_POINT('Ctrl Pts',(-23.9416710836529,4.99916972919309,
12.));
#201352=CARTESIAN_POINT('Ctrl Pts',(-23.9610180388271,5.01253173257458,
0.));
#201353=CARTESIAN_POINT('Ctrl Pts',(-23.9610180388271,5.01253173257458,
12.));
#201354=CARTESIAN_POINT('Ctrl Pts',(-23.9804048689228,5.02599225112461,
0.));
#201355=CARTESIAN_POINT('Ctrl Pts',(-23.9804048689228,5.02599225112461,
12.));
#201356=CARTESIAN_POINT('Ctrl Pts',(-23.9998309040747,5.03955120528527,
0.));
#201357=CARTESIAN_POINT('Ctrl Pts',(-23.9998309040747,5.03955120528527,
12.));
#201358=CARTESIAN_POINT('Ctrl Pts',(-24.0192954804896,5.05320851483068,
0.));
#201359=CARTESIAN_POINT('Ctrl Pts',(-24.0192954804896,5.05320851483068,
12.));
#201360=CARTESIAN_POINT('Ctrl Pts',(-24.0387979403268,5.06696409886639,
0.));
#201361=CARTESIAN_POINT('Ctrl Pts',(-24.0387979403268,5.06696409886639,
12.));
#201362=CARTESIAN_POINT('Ctrl Pts',(-24.0583376315636,5.0808178758127,0.));
#201363=CARTESIAN_POINT('Ctrl Pts',(-24.0583376315636,5.0808178758127,12.));
#201364=CARTESIAN_POINT('Ctrl Pts',(-24.0779139079264,5.09476976342616,
0.));
#201365=CARTESIAN_POINT('Ctrl Pts',(-24.0779139079264,5.09476976342616,
12.));
#201366=CARTESIAN_POINT('Ctrl Pts',(-24.0975261288444,5.10881967883124,
0.));
#201367=CARTESIAN_POINT('Ctrl Pts',(-24.0975261288444,5.10881967883124,
12.));
#201368=CARTESIAN_POINT('Ctrl Pts',(-24.117173659394,5.12296753853857,0.));
#201369=CARTESIAN_POINT('Ctrl Pts',(-24.117173659394,5.12296753853857,12.));
#201370=CARTESIAN_POINT('Ctrl Pts',(-24.1368558702443,5.13721325845745,
0.));
#201371=CARTESIAN_POINT('Ctrl Pts',(-24.1368558702443,5.13721325845745,
12.));
#201372=CARTESIAN_POINT('Ctrl Pts',(-24.1565721375971,5.15155675390079,
0.));
#201373=CARTESIAN_POINT('Ctrl Pts',(-24.1565721375971,5.15155675390079,
12.));
#201374=CARTESIAN_POINT('Ctrl Pts',(-24.1763218431344,5.16599793957985,
0.));
#201375=CARTESIAN_POINT('Ctrl Pts',(-24.1763218431344,5.16599793957985,
12.));
#201376=CARTESIAN_POINT('Ctrl Pts',(-24.1961043738756,5.18053672961398,
0.));
#201377=CARTESIAN_POINT('Ctrl Pts',(-24.1961043738756,5.18053672961398,
12.));
#201378=CARTESIAN_POINT('Ctrl Pts',(-24.2159191220171,5.19517303753647,
0.));
#201379=CARTESIAN_POINT('Ctrl Pts',(-24.2159191220171,5.19517303753647,
12.));
#201380=CARTESIAN_POINT('Ctrl Pts',(-24.2357654847766,5.20990677629176,
0.));
#201381=CARTESIAN_POINT('Ctrl Pts',(-24.2357654847766,5.20990677629176,
12.));
#201382=CARTESIAN_POINT('Ctrl Pts',(-24.2556428642294,5.22473785822442,
0.));
#201383=CARTESIAN_POINT('Ctrl Pts',(-24.2556428642294,5.22473785822442,
12.));
#201384=CARTESIAN_POINT('Ctrl Pts',(-24.2755506671525,5.23966619506289,
0.));
#201385=CARTESIAN_POINT('Ctrl Pts',(-24.2755506671525,5.23966619506289,
12.));
#201386=CARTESIAN_POINT('Ctrl Pts',(-24.2954883048447,5.25469169788856,
0.));
#201387=CARTESIAN_POINT('Ctrl Pts',(-24.2954883048447,5.25469169788856,
12.));
#201388=CARTESIAN_POINT('Ctrl Pts',(-24.3154551932221,5.26981427718798,
0.));
#201389=CARTESIAN_POINT('Ctrl Pts',(-24.3154551932221,5.26981427718798,
12.));
#201390=CARTESIAN_POINT('Ctrl Pts',(-24.3354507529414,5.28503384290648,
0.));
#201391=CARTESIAN_POINT('Ctrl Pts',(-24.3354507529414,5.28503384290648,
12.));
#201392=CARTESIAN_POINT('Ctrl Pts',(-24.3554744095075,5.30035030449063,
0.));
#201393=CARTESIAN_POINT('Ctrl Pts',(-24.3554744095075,5.30035030449063,
12.));
#201394=CARTESIAN_POINT('Ctrl Pts',(-24.3755255933917,5.31576357092526,
0.));
#201395=CARTESIAN_POINT('Ctrl Pts',(-24.3755255933917,5.31576357092526,
12.));
#201396=CARTESIAN_POINT('Ctrl Pts',(-24.3956037401293,5.33127355076033,
0.));
#201397=CARTESIAN_POINT('Ctrl Pts',(-24.3956037401293,5.33127355076033,
12.));
#201398=CARTESIAN_POINT('Ctrl Pts',(-24.4157082904614,5.34688015213537,
0.));
#201399=CARTESIAN_POINT('Ctrl Pts',(-24.4157082904614,5.34688015213537,
12.));
#201400=CARTESIAN_POINT('Ctrl Pts',(-24.435838689915,5.36258328273627,0.));
#201401=CARTESIAN_POINT('Ctrl Pts',(-24.435838689915,5.36258328273627,12.));
#201402=CARTESIAN_POINT('Ctrl Pts',(-24.4559943883157,5.37838284973695,
0.));
#201403=CARTESIAN_POINT('Ctrl Pts',(-24.4559943883157,5.37838284973695,
12.));
#201404=CARTESIAN_POINT('Ctrl Pts',(-24.4761748393321,5.39427875973824,
0.));
#201405=CARTESIAN_POINT('Ctrl Pts',(-24.4761748393321,5.39427875973824,
12.));
#201406=CARTESIAN_POINT('Ctrl Pts',(-24.4963794999831,5.41027091869241,
0.));
#201407=CARTESIAN_POINT('Ctrl Pts',(-24.4963794999831,5.41027091869241,
12.));
#201408=CARTESIAN_POINT('Ctrl Pts',(-24.5166078302108,5.42635923183419,
0.));
#201409=CARTESIAN_POINT('Ctrl Pts',(-24.5166078302108,5.42635923183419,
12.));
#201410=CARTESIAN_POINT('Ctrl Pts',(-24.5368592922863,5.4425436035688,0.));
#201411=CARTESIAN_POINT('Ctrl Pts',(-24.5368592922863,5.4425436035688,12.));
#201412=CARTESIAN_POINT('Ctrl Pts',(-24.5571333514842,5.45882393762261,
0.));
#201413=CARTESIAN_POINT('Ctrl Pts',(-24.5571333514842,5.45882393762261,
12.));
#201414=CARTESIAN_POINT('Ctrl Pts',(-24.5774294770329,5.47520013724419,
0.));
#201415=CARTESIAN_POINT('Ctrl Pts',(-24.5774294770329,5.47520013724419,
12.));
#201416=CARTESIAN_POINT('Ctrl Pts',(-24.5977471429364,5.49167210537246,
0.));
#201417=CARTESIAN_POINT('Ctrl Pts',(-24.5977471429364,5.49167210537246,
12.));
#201418=CARTESIAN_POINT('Ctrl Pts',(-24.6180858289179,5.50823974481962,
0.));
#201419=CARTESIAN_POINT('Ctrl Pts',(-24.6180858289179,5.50823974481962,
12.));
#201420=CARTESIAN_POINT('Ctrl Pts',(-24.6384450211467,5.52490295840991,
0.));
#201421=CARTESIAN_POINT('Ctrl Pts',(-24.6384450211467,5.52490295840991,
12.));
#201422=CARTESIAN_POINT('Ctrl Pts',(-24.6588242134738,5.54166164919583,
0.));
#201423=CARTESIAN_POINT('Ctrl Pts',(-24.6588242134738,5.54166164919583,
12.));
#201424=CARTESIAN_POINT('Ctrl Pts',(-24.6792229061794,5.55851572025376,
0.));
#201425=CARTESIAN_POINT('Ctrl Pts',(-24.6792229061794,5.55851572025376,
12.));
#201426=CARTESIAN_POINT('Ctrl Pts',(-24.6996406035517,5.57546507427754,
0.));
#201427=CARTESIAN_POINT('Ctrl Pts',(-24.6996406035517,5.57546507427754,
12.));
#201428=CARTESIAN_POINT('Ctrl Pts',(-24.7200768119088,5.59250961323987,
0.));
#201429=CARTESIAN_POINT('Ctrl Pts',(-24.7200768119088,5.59250961323987,
12.));
#201430=CARTESIAN_POINT('Ctrl Pts',(-24.7405310372739,5.60964923798491,
0.));
#201431=CARTESIAN_POINT('Ctrl Pts',(-24.7405310372739,5.60964923798491,
12.));
#201432=CARTESIAN_POINT('Ctrl Pts',(-24.7610027835697,5.62688384790923,
0.));
#201433=CARTESIAN_POINT('Ctrl Pts',(-24.7610027835697,5.62688384790923,
12.));
#201434=CARTESIAN_POINT('Ctrl Pts',(-24.781491549672,5.6442133404226,0.));
#201435=CARTESIAN_POINT('Ctrl Pts',(-24.781491549672,5.6442133404226,12.));
#201436=CARTESIAN_POINT('Ctrl Pts',(-24.8019968304605,5.66163761114921,
0.));
#201437=CARTESIAN_POINT('Ctrl Pts',(-24.8019968304605,5.66163761114921,
12.));
#201438=CARTESIAN_POINT('Ctrl Pts',(-24.8225181223845,5.67915655496542,
0.));
#201439=CARTESIAN_POINT('Ctrl Pts',(-24.8225181223845,5.67915655496542,
12.));
#201440=CARTESIAN_POINT('Ctrl Pts',(-24.8430549277621,5.69677006679444,
0.));
#201441=CARTESIAN_POINT('Ctrl Pts',(-24.8430549277621,5.69677006679444,
12.));
#201442=CARTESIAN_POINT('Ctrl Pts',(-24.8636067597669,5.71447804252027,
0.));
#201443=CARTESIAN_POINT('Ctrl Pts',(-24.8636067597669,5.71447804252027,
12.));
#201444=CARTESIAN_POINT('Ctrl Pts',(-24.884173146722,5.73228037976926,0.));
#201445=CARTESIAN_POINT('Ctrl Pts',(-24.884173146722,5.73228037976926,12.));
#201446=CARTESIAN_POINT('Ctrl Pts',(-24.904753637648,5.75017697890804,0.));
#201447=CARTESIAN_POINT('Ctrl Pts',(-24.904753637648,5.75017697890804,12.));
#201448=CARTESIAN_POINT('Ctrl Pts',(-24.9253478043656,5.76816774342219,
0.));
#201449=CARTESIAN_POINT('Ctrl Pts',(-24.9253478043656,5.76816774342219,
12.));
#201450=CARTESIAN_POINT('Ctrl Pts',(-24.945955229334,5.78625257775681,0.));
#201451=CARTESIAN_POINT('Ctrl Pts',(-24.945955229334,5.78625257775681,12.));
#201452=CARTESIAN_POINT('Ctrl Pts',(-24.9665754954496,5.80443138549726,
0.));
#201453=CARTESIAN_POINT('Ctrl Pts',(-24.9665754954496,5.80443138549726,
12.));
#201454=CARTESIAN_POINT('Ctrl Pts',(-24.9872081752734,5.82270406744198,
0.));
#201455=CARTESIAN_POINT('Ctrl Pts',(-24.9872081752734,5.82270406744198,
12.));
#201456=CARTESIAN_POINT('Ctrl Pts',(-25.0078528200564,5.84107051963071,
0.));
#201457=CARTESIAN_POINT('Ctrl Pts',(-25.0078528200564,5.84107051963071,
12.));
#201458=CARTESIAN_POINT('Ctrl Pts',(-25.0285089498899,5.85953063156826,
0.));
#201459=CARTESIAN_POINT('Ctrl Pts',(-25.0285089498899,5.85953063156826,
12.));
#201460=CARTESIAN_POINT('Ctrl Pts',(-25.0491760405911,5.87808428385365,
0.));
#201461=CARTESIAN_POINT('Ctrl Pts',(-25.0491760405911,5.87808428385365,
12.));
#201462=CARTESIAN_POINT('Ctrl Pts',(-25.0698535426514,5.89673135155514,
0.));
#201463=CARTESIAN_POINT('Ctrl Pts',(-25.0698535426514,5.89673135155514,
12.));
#201464=CARTESIAN_POINT('Ctrl Pts',(-25.0905409050773,5.91547170844447,
0.));
#201465=CARTESIAN_POINT('Ctrl Pts',(-25.0905409050773,5.91547170844447,
12.));
#201466=CARTESIAN_POINT('Ctrl Pts',(-25.1112375971106,5.93430523086834,
0.));
#201467=CARTESIAN_POINT('Ctrl Pts',(-25.1112375971106,5.93430523086834,
12.));
#201468=CARTESIAN_POINT('Ctrl Pts',(-25.1319431317237,5.95323180187378,
0.));
#201469=CARTESIAN_POINT('Ctrl Pts',(-25.1319431317237,5.95323180187378,
12.));
#201470=CARTESIAN_POINT('Ctrl Pts',(-25.1526570863092,5.97225131495616,
0.));
#201471=CARTESIAN_POINT('Ctrl Pts',(-25.1526570863092,5.97225131495616,
12.));
#201472=CARTESIAN_POINT('Ctrl Pts',(-25.1733791296259,5.99136367859754,
0.));
#201473=CARTESIAN_POINT('Ctrl Pts',(-25.1733791296259,5.99136367859754,
12.));
#201474=CARTESIAN_POINT('Ctrl Pts',(-25.1941090269819,6.01056881804612,
0.));
#201475=CARTESIAN_POINT('Ctrl Pts',(-25.1941090269819,6.01056881804612,
12.));
#201476=CARTESIAN_POINT('Ctrl Pts',(-25.21484662016,6.02986667389996,0.));
#201477=CARTESIAN_POINT('Ctrl Pts',(-25.21484662016,6.02986667389996,12.));
#201478=CARTESIAN_POINT('Ctrl Pts',(-25.2355918139032,6.04925720151218,
0.));
#201479=CARTESIAN_POINT('Ctrl Pts',(-25.2355918139032,6.04925720151218,
12.));
#201480=CARTESIAN_POINT('Ctrl Pts',(-25.2521940105705,6.06484373634546,
0.));
#201481=CARTESIAN_POINT('Ctrl Pts',(-25.2521940105705,6.06484373634546,
12.));
#201482=CARTESIAN_POINT('Ctrl Pts',(-25.2646490489923,6.0765753178749,0.));
#201483=CARTESIAN_POINT('Ctrl Pts',(-25.2646490489923,6.0765753178749,12.));
#201484=CARTESIAN_POINT('Ctrl Pts',(-25.2729539149517,6.08441489609793,
0.));
#201485=CARTESIAN_POINT('Ctrl Pts',(-25.2729539149517,6.08441489609793,
12.));
#201486=CARTESIAN_POINT('Ctrl Pts',(-25.2771067246846,6.08833931617699,
0.));
#201487=CARTESIAN_POINT('Ctrl Pts',(-25.2771067246846,6.08833931617699,
12.));
#201488=CARTESIAN_POINT('',(-25.2771067246846,6.08833931617699,0.));
#201489=CARTESIAN_POINT('Ctrl Pts',(-22.1738711152697,4.11585220600461,
0.));
#201490=CARTESIAN_POINT('Ctrl Pts',(-22.173877682324,4.11585194677442,0.));
#201491=CARTESIAN_POINT('Ctrl Pts',(-22.1739341411687,4.11586035878287,
0.));
#201492=CARTESIAN_POINT('Ctrl Pts',(-22.1741488021234,4.11589976826166,
0.));
#201493=CARTESIAN_POINT('Ctrl Pts',(-22.1746949858775,4.11600589882845,
0.));
#201494=CARTESIAN_POINT('Ctrl Pts',(-22.1758088296598,4.11622797217068,
0.));
#201495=CARTESIAN_POINT('Ctrl Pts',(-22.177347426894,4.11653973150518,0.));
#201496=CARTESIAN_POINT('Ctrl Pts',(-22.179297473024,4.11694173195003,0.));
#201497=CARTESIAN_POINT('Ctrl Pts',(-22.1816414985788,4.11743469691756,
0.));
#201498=CARTESIAN_POINT('Ctrl Pts',(-22.1843613164855,4.11801938107479,
0.));
#201499=CARTESIAN_POINT('Ctrl Pts',(-22.1874419861496,4.11869641271773,
0.));
#201500=CARTESIAN_POINT('Ctrl Pts',(-22.1908725908525,4.11946626228636,
0.));
#201501=CARTESIAN_POINT('Ctrl Pts',(-22.1946440958098,4.12032932637736,
0.));
#201502=CARTESIAN_POINT('Ctrl Pts',(-22.1987479618246,4.12128598183522,
0.));
#201503=CARTESIAN_POINT('Ctrl Pts',(-22.2031746532106,4.12233664408227,
0.));
#201504=CARTESIAN_POINT('Ctrl Pts',(-22.2079143941719,4.12348173702023,
0.));
#201505=CARTESIAN_POINT('Ctrl Pts',(-22.2129576146671,4.12472167516607,
0.));
#201506=CARTESIAN_POINT('Ctrl Pts',(-22.2182956401341,4.12605683613307,
0.));
#201507=CARTESIAN_POINT('Ctrl Pts',(-22.2239207458781,4.12748755830104,
0.));
#201508=CARTESIAN_POINT('Ctrl Pts',(-22.2298258043947,4.12901415463379,
0.));
#201509=CARTESIAN_POINT('Ctrl Pts',(-22.2360040565533,4.13063692157498,
0.));
#201510=CARTESIAN_POINT('Ctrl Pts',(-22.2424488153523,4.1323561506016,0.));
#201511=CARTESIAN_POINT('Ctrl Pts',(-22.249153531779,4.1341721255881,0.));
#201512=CARTESIAN_POINT('Ctrl Pts',(-22.2561118708421,4.13608511977225,
0.));
#201513=CARTESIAN_POINT('Ctrl Pts',(-22.2633177913972,4.13809539255421,
0.));
#201514=CARTESIAN_POINT('Ctrl Pts',(-22.2707656042457,4.14020318715991,
0.));
#201515=CARTESIAN_POINT('Ctrl Pts',(-22.2784499072027,4.14240873321984,
0.));
#201516=CARTESIAN_POINT('Ctrl Pts',(-22.2863655389166,4.14471224859295,
0.));
#201517=CARTESIAN_POINT('Ctrl Pts',(-22.2945075198467,4.14711394168556,
0.));
#201518=CARTESIAN_POINT('Ctrl Pts',(-22.3028710166933,4.14961401285522,
0.));
#201519=CARTESIAN_POINT('Ctrl Pts',(-22.3114513545185,4.1522126539699,0.));
#201520=CARTESIAN_POINT('Ctrl Pts',(-22.3202440186979,4.15491004835281,
0.));
#201521=CARTESIAN_POINT('Ctrl Pts',(-22.3292446628959,4.15770637047889,
0.));
#201522=CARTESIAN_POINT('Ctrl Pts',(-22.3384491078602,4.16060178604164,
0.));
#201523=CARTESIAN_POINT('Ctrl Pts',(-22.3478533253889,4.16359645263187,
0.));
#201524=CARTESIAN_POINT('Ctrl Pts',(-22.3574534257396,4.166690520266,0.));
#201525=CARTESIAN_POINT('Ctrl Pts',(-22.36724564276,4.16988413199457,0.));
#201526=CARTESIAN_POINT('Ctrl Pts',(-22.3772263228617,4.17317742436145,
0.));
#201527=CARTESIAN_POINT('Ctrl Pts',(-22.3873919231334,4.17657052752825,
0.));
#201528=CARTESIAN_POINT('Ctrl Pts',(-22.3977390078075,4.18006356544882,
0.));
#201529=CARTESIAN_POINT('Ctrl Pts',(-22.4082642454453,4.1836566560085,0.));
#201530=CARTESIAN_POINT('Ctrl Pts',(-22.4189644056115,4.1873499111772,0.));
#201531=CARTESIAN_POINT('Ctrl Pts',(-22.4298363535421,4.19114343726941,
0.));
#201532=CARTESIAN_POINT('Ctrl Pts',(-22.4408770448917,4.1950373351886,0.));
#201533=CARTESIAN_POINT('Ctrl Pts',(-22.4520835205419,4.19903170066354,
0.));
#201534=CARTESIAN_POINT('Ctrl Pts',(-22.4634529011433,4.2031266244817,0.));
#201535=CARTESIAN_POINT('Ctrl Pts',(-22.4749823839915,4.20732219265648,
0.));
#201536=CARTESIAN_POINT('Ctrl Pts',(-22.4866692403147,4.21161848657428,
0.));
#201537=CARTESIAN_POINT('Ctrl Pts',(-22.4985108124229,4.21601558313908,
0.));
#201538=CARTESIAN_POINT('Ctrl Pts',(-22.5105045108882,4.22051355490196,
0.));
#201539=CARTESIAN_POINT('Ctrl Pts',(-22.5226478117885,4.2251124702004,0.));
#201540=CARTESIAN_POINT('Ctrl Pts',(-22.5349382540587,4.22981239330731,
0.));
#201541=CARTESIAN_POINT('Ctrl Pts',(-22.5473734368086,4.23461338456713,
0.));
#201542=CARTESIAN_POINT('Ctrl Pts',(-22.559951016643,4.23951550052526,0.));
#201543=CARTESIAN_POINT('Ctrl Pts',(-22.5726687049922,4.24451879404858,
0.));
#201544=CARTESIAN_POINT('Ctrl Pts',(-22.5855242662479,4.24962331444184,
0.));
#201545=CARTESIAN_POINT('Ctrl Pts',(-22.5985155158637,4.25482910755485,
0.));
#201546=CARTESIAN_POINT('Ctrl Pts',(-22.611640318482,4.26013621588303,0.));
#201547=CARTESIAN_POINT('Ctrl Pts',(-22.6248965859975,4.26554467865571,
0.));
#201548=CARTESIAN_POINT('Ctrl Pts',(-22.6382822758171,4.27105453192999,
0.));
#201549=CARTESIAN_POINT('Ctrl Pts',(-22.6517953893303,4.27666580869117,
0.));
#201550=CARTESIAN_POINT('Ctrl Pts',(-22.665433970311,4.28237853894059,0.));
#201551=CARTESIAN_POINT('Ctrl Pts',(-22.6791961033537,4.28819274977766,
0.));
#201552=CARTESIAN_POINT('Ctrl Pts',(-22.6930799122545,4.29410846547061,
0.));
#201553=CARTESIAN_POINT('Ctrl Pts',(-22.707083558756,4.30012570754066,0.));
#201554=CARTESIAN_POINT('Ctrl Pts',(-22.7212052413384,4.30624449484074,
0.));
#201555=CARTESIAN_POINT('Ctrl Pts',(-22.7354431939927,4.3124648436255,0.));
#201556=CARTESIAN_POINT('Ctrl Pts',(-22.7497956849852,4.3187867676123,0.));
#201557=CARTESIAN_POINT('Ctrl Pts',(-22.764261015648,4.32521027803747,0.));
#201558=CARTESIAN_POINT('Ctrl Pts',(-22.7788375194081,4.33173538373182,
0.));
#201559=CARTESIAN_POINT('Ctrl Pts',(-22.7935235607807,4.33836209118442,
0.));
#201560=CARTESIAN_POINT('Ctrl Pts',(-22.808317534379,4.34509040460065,0.));
#201561=CARTESIAN_POINT('Ctrl Pts',(-22.8232178638873,4.35192032594801,
0.));
#201562=CARTESIAN_POINT('Ctrl Pts',(-22.838223001118,4.35885185500559,0.));
#201563=CARTESIAN_POINT('Ctrl Pts',(-22.8533314252419,4.36588498943009,
0.));
#201564=CARTESIAN_POINT('Ctrl Pts',(-22.8685416419725,4.37301972480752,
0.));
#201565=CARTESIAN_POINT('Ctrl Pts',(-22.8838521827702,4.38025605470089,
0.));
#201566=CARTESIAN_POINT('Ctrl Pts',(-22.8992616040108,4.38759397068391,
0.));
#201567=CARTESIAN_POINT('Ctrl Pts',(-22.9147684862425,4.39503346238454,
0.));
#201568=CARTESIAN_POINT('Ctrl Pts',(-22.9303714335549,4.40257451754307,
0.));
#201569=CARTESIAN_POINT('Ctrl Pts',(-22.9460690729093,4.41021712205547,
0.));
#201570=CARTESIAN_POINT('Ctrl Pts',(-22.9618600534866,4.41796126001309,
0.));
#201571=CARTESIAN_POINT('Ctrl Pts',(-22.9777430460021,4.42580691372771,
0.));
#201572=CARTESIAN_POINT('Ctrl Pts',(-22.9937167421009,4.43375406376904,
0.));
#201573=CARTESIAN_POINT('Ctrl Pts',(-23.0097798538399,4.44180268901666,
0.));
#201574=CARTESIAN_POINT('Ctrl Pts',(-23.0259311131395,4.44995276669698,
0.));
#201575=CARTESIAN_POINT('Ctrl Pts',(-23.0421692712466,4.45820427241676,
0.));
#201576=CARTESIAN_POINT('Ctrl Pts',(-23.0584930981723,4.46655718018205,
0.));
#201577=CARTESIAN_POINT('Ctrl Pts',(-23.0749013821868,4.47501146242821,
0.));
#201578=CARTESIAN_POINT('Ctrl Pts',(-23.0913929293909,4.48356709006756,
0.));
#201579=CARTESIAN_POINT('Ctrl Pts',(-23.1079665632629,4.49222403252201,
0.));
#201580=CARTESIAN_POINT('Ctrl Pts',(-23.1246211242117,4.50098225775178,
0.));
#201581=CARTESIAN_POINT('Ctrl Pts',(-23.1413554691136,4.50984173227087,
0.));
#201582=CARTESIAN_POINT('Ctrl Pts',(-23.1581684708778,4.51880242116785,
0.));
#201583=CARTESIAN_POINT('Ctrl Pts',(-23.1750590180923,4.52786428815047,
0.));
#201584=CARTESIAN_POINT('Ctrl Pts',(-23.1920260146474,4.53702729557585,
0.));
#201585=CARTESIAN_POINT('Ctrl Pts',(-23.2090683793627,4.54629140447542,
0.));
#201586=CARTESIAN_POINT('Ctrl Pts',(-23.2261850456055,4.55565657456956,
0.));
#201587=CARTESIAN_POINT('Ctrl Pts',(-23.2433749609117,4.5651227642781,0.));
#201588=CARTESIAN_POINT('Ctrl Pts',(-23.2606370866853,4.5746899307607,0.));
#201589=CARTESIAN_POINT('Ctrl Pts',(-23.2779703978868,4.58435802994674,
0.));
#201590=CARTESIAN_POINT('Ctrl Pts',(-23.295373882719,4.59412701655749,0.));
#201591=CARTESIAN_POINT('Ctrl Pts',(-23.3128465423119,4.60399684412174,
0.));
#201592=CARTESIAN_POINT('Ctrl Pts',(-23.3303873903947,4.61396746497848,
0.));
#201593=CARTESIAN_POINT('Ctrl Pts',(-23.3479954530281,4.62403883030823,
0.));
#201594=CARTESIAN_POINT('Ctrl Pts',(-23.3656697683496,4.63421089016554,
0.));
#201595=CARTESIAN_POINT('Ctrl Pts',(-23.383409386307,4.64448359349935,0.));
#201596=CARTESIAN_POINT('Ctrl Pts',(-23.4012133683957,4.65485688816921,
0.));
#201597=CARTESIAN_POINT('Ctrl Pts',(-23.4190807873798,4.66533072094663,
0.));
#201598=CARTESIAN_POINT('Ctrl Pts',(-23.4370107270444,4.6759050375305,0.));
#201599=CARTESIAN_POINT('Ctrl Pts',(-23.4550022819853,4.68657978258297,
0.));
#201600=CARTESIAN_POINT('Ctrl Pts',(-23.4730545573849,4.69735489975023,
0.));
#201601=CARTESIAN_POINT('Ctrl Pts',(-23.491166668789,4.7082303316782,0.));
#201602=CARTESIAN_POINT('Ctrl Pts',(-23.5093377418784,4.71920602001904,
0.));
#201603=CARTESIAN_POINT('Ctrl Pts',(-23.5275669122378,4.73028190543031,
0.));
#201604=CARTESIAN_POINT('Ctrl Pts',(-23.5458533251715,4.74145792760698,
0.));
#201605=CARTESIAN_POINT('Ctrl Pts',(-23.564196135517,4.75273402530615,0.));
#201606=CARTESIAN_POINT('Ctrl Pts',(-23.5825945074535,4.7641101363625,0.));
#201607=CARTESIAN_POINT('Ctrl Pts',(-23.6010476143099,4.77558619769875,
0.));
#201608=CARTESIAN_POINT('Ctrl Pts',(-23.6195546383625,4.78716214532104,
0.));
#201609=CARTESIAN_POINT('Ctrl Pts',(-23.6381147706581,4.79883791433229,
0.));
#201610=CARTESIAN_POINT('Ctrl Pts',(-23.6567272108631,4.81061343896442,
0.));
#201611=CARTESIAN_POINT('Ctrl Pts',(-23.6753911671023,4.82248865259569,
0.));
#201612=CARTESIAN_POINT('Ctrl Pts',(-23.6941058557971,4.83446348776267,
0.));
#201613=CARTESIAN_POINT('Ctrl Pts',(-23.7128705015014,4.84653787616422,
0.));
#201614=CARTESIAN_POINT('Ctrl Pts',(-23.7316843367308,4.85871174865491,
0.));
#201615=CARTESIAN_POINT('Ctrl Pts',(-23.7505466018239,4.87098503527142,
0.));
#201616=CARTESIAN_POINT('Ctrl Pts',(-23.7694565448044,4.88335766525565,
0.));
#201617=CARTESIAN_POINT('Ctrl Pts',(-23.7884134212381,4.89582956706771,
0.));
#201618=CARTESIAN_POINT('Ctrl Pts',(-23.8074164940897,4.90840066839346,
0.));
#201619=CARTESIAN_POINT('Ctrl Pts',(-23.8264650335721,4.92107089613976,
0.));
#201620=CARTESIAN_POINT('Ctrl Pts',(-23.8455583170062,4.93384017643441,
0.));
#201621=CARTESIAN_POINT('Ctrl Pts',(-23.8646956287172,4.94670843465868,
0.));
#201622=CARTESIAN_POINT('Ctrl Pts',(-23.883876259922,4.95967559546565,0.));
#201623=CARTESIAN_POINT('Ctrl Pts',(-23.9030995086164,4.97274158279228,
0.));
#201624=CARTESIAN_POINT('Ctrl Pts',(-23.9223646794591,4.98590631986532,
0.));
#201625=CARTESIAN_POINT('Ctrl Pts',(-23.9416710836529,4.99916972919309,
0.));
#201626=CARTESIAN_POINT('Ctrl Pts',(-23.9610180388271,5.01253173257458,
0.));
#201627=CARTESIAN_POINT('Ctrl Pts',(-23.9804048689228,5.02599225112461,
0.));
#201628=CARTESIAN_POINT('Ctrl Pts',(-23.9998309040747,5.03955120528527,
0.));
#201629=CARTESIAN_POINT('Ctrl Pts',(-24.0192954804896,5.05320851483068,
0.));
#201630=CARTESIAN_POINT('Ctrl Pts',(-24.0387979403268,5.06696409886639,
0.));
#201631=CARTESIAN_POINT('Ctrl Pts',(-24.0583376315636,5.0808178758127,0.));
#201632=CARTESIAN_POINT('Ctrl Pts',(-24.0779139079264,5.09476976342616,
0.));
#201633=CARTESIAN_POINT('Ctrl Pts',(-24.0975261288444,5.10881967883124,
0.));
#201634=CARTESIAN_POINT('Ctrl Pts',(-24.117173659394,5.12296753853857,0.));
#201635=CARTESIAN_POINT('Ctrl Pts',(-24.1368558702443,5.13721325845745,
0.));
#201636=CARTESIAN_POINT('Ctrl Pts',(-24.1565721375971,5.15155675390079,
0.));
#201637=CARTESIAN_POINT('Ctrl Pts',(-24.1763218431344,5.16599793957985,
0.));
#201638=CARTESIAN_POINT('Ctrl Pts',(-24.1961043738756,5.18053672961398,
0.));
#201639=CARTESIAN_POINT('Ctrl Pts',(-24.2159191220171,5.19517303753647,
0.));
#201640=CARTESIAN_POINT('Ctrl Pts',(-24.2357654847766,5.20990677629176,
0.));
#201641=CARTESIAN_POINT('Ctrl Pts',(-24.2556428642294,5.22473785822442,
0.));
#201642=CARTESIAN_POINT('Ctrl Pts',(-24.2755506671525,5.23966619506289,
0.));
#201643=CARTESIAN_POINT('Ctrl Pts',(-24.2954883048447,5.25469169788856,
0.));
#201644=CARTESIAN_POINT('Ctrl Pts',(-24.3154551932221,5.26981427718798,
0.));
#201645=CARTESIAN_POINT('Ctrl Pts',(-24.3354507529414,5.28503384290648,
0.));
#201646=CARTESIAN_POINT('Ctrl Pts',(-24.3554744095075,5.30035030449063,
0.));
#201647=CARTESIAN_POINT('Ctrl Pts',(-24.3755255933917,5.31576357092526,
0.));
#201648=CARTESIAN_POINT('Ctrl Pts',(-24.3956037401293,5.33127355076033,
0.));
#201649=CARTESIAN_POINT('Ctrl Pts',(-24.4157082904614,5.34688015213537,
0.));
#201650=CARTESIAN_POINT('Ctrl Pts',(-24.435838689915,5.36258328273627,0.));
#201651=CARTESIAN_POINT('Ctrl Pts',(-24.4559943883157,5.37838284973695,
0.));
#201652=CARTESIAN_POINT('Ctrl Pts',(-24.4761748393321,5.39427875973824,
0.));
#201653=CARTESIAN_POINT('Ctrl Pts',(-24.4963794999831,5.41027091869241,
0.));
#201654=CARTESIAN_POINT('Ctrl Pts',(-24.5166078302108,5.42635923183419,
0.));
#201655=CARTESIAN_POINT('Ctrl Pts',(-24.5368592922863,5.4425436035688,0.));
#201656=CARTESIAN_POINT('Ctrl Pts',(-24.5571333514842,5.45882393762261,
0.));
#201657=CARTESIAN_POINT('Ctrl Pts',(-24.5774294770329,5.47520013724419,
0.));
#201658=CARTESIAN_POINT('Ctrl Pts',(-24.5977471429364,5.49167210537246,
0.));
#201659=CARTESIAN_POINT('Ctrl Pts',(-24.6180858289179,5.50823974481962,
0.));
#201660=CARTESIAN_POINT('Ctrl Pts',(-24.6384450211467,5.52490295840991,
0.));
#201661=CARTESIAN_POINT('Ctrl Pts',(-24.6588242134738,5.54166164919583,
0.));
#201662=CARTESIAN_POINT('Ctrl Pts',(-24.6792229061794,5.55851572025376,
0.));
#201663=CARTESIAN_POINT('Ctrl Pts',(-24.6996406035517,5.57546507427754,
0.));
#201664=CARTESIAN_POINT('Ctrl Pts',(-24.7200768119088,5.59250961323987,
0.));
#201665=CARTESIAN_POINT('Ctrl Pts',(-24.7405310372739,5.60964923798491,
0.));
#201666=CARTESIAN_POINT('Ctrl Pts',(-24.7610027835697,5.62688384790923,
0.));
#201667=CARTESIAN_POINT('Ctrl Pts',(-24.781491549672,5.6442133404226,0.));
#201668=CARTESIAN_POINT('Ctrl Pts',(-24.8019968304605,5.66163761114921,
0.));
#201669=CARTESIAN_POINT('Ctrl Pts',(-24.8225181223845,5.67915655496542,
0.));
#201670=CARTESIAN_POINT('Ctrl Pts',(-24.8430549277621,5.69677006679444,
0.));
#201671=CARTESIAN_POINT('Ctrl Pts',(-24.8636067597669,5.71447804252027,
0.));
#201672=CARTESIAN_POINT('Ctrl Pts',(-24.884173146722,5.73228037976926,0.));
#201673=CARTESIAN_POINT('Ctrl Pts',(-24.904753637648,5.75017697890804,0.));
#201674=CARTESIAN_POINT('Ctrl Pts',(-24.9253478043656,5.76816774342219,
0.));
#201675=CARTESIAN_POINT('Ctrl Pts',(-24.945955229334,5.78625257775681,0.));
#201676=CARTESIAN_POINT('Ctrl Pts',(-24.9665754954496,5.80443138549726,
0.));
#201677=CARTESIAN_POINT('Ctrl Pts',(-24.9872081752734,5.82270406744198,
0.));
#201678=CARTESIAN_POINT('Ctrl Pts',(-25.0078528200564,5.84107051963071,
0.));
#201679=CARTESIAN_POINT('Ctrl Pts',(-25.0285089498899,5.85953063156826,
0.));
#201680=CARTESIAN_POINT('Ctrl Pts',(-25.0491760405911,5.87808428385365,
0.));
#201681=CARTESIAN_POINT('Ctrl Pts',(-25.0698535426514,5.89673135155514,
0.));
#201682=CARTESIAN_POINT('Ctrl Pts',(-25.0905409050773,5.91547170844447,
0.));
#201683=CARTESIAN_POINT('Ctrl Pts',(-25.1112375971106,5.93430523086834,
0.));
#201684=CARTESIAN_POINT('Ctrl Pts',(-25.1319431317237,5.95323180187378,
0.));
#201685=CARTESIAN_POINT('Ctrl Pts',(-25.1526570863092,5.97225131495616,
0.));
#201686=CARTESIAN_POINT('Ctrl Pts',(-25.1733791296259,5.99136367859754,
0.));
#201687=CARTESIAN_POINT('Ctrl Pts',(-25.1941090269819,6.01056881804612,
0.));
#201688=CARTESIAN_POINT('Ctrl Pts',(-25.21484662016,6.02986667389996,0.));
#201689=CARTESIAN_POINT('Ctrl Pts',(-25.2355918139032,6.04925720151218,
0.));
#201690=CARTESIAN_POINT('Ctrl Pts',(-25.2521940105705,6.06484373634546,
0.));
#201691=CARTESIAN_POINT('Ctrl Pts',(-25.2646490489923,6.0765753178749,0.));
#201692=CARTESIAN_POINT('Ctrl Pts',(-25.2729539149517,6.08441489609793,
0.));
#201693=CARTESIAN_POINT('Ctrl Pts',(-25.2771067246846,6.08833931617699,
0.));
#201694=CARTESIAN_POINT('',(-25.2771067246846,6.08833931617699,0.));
#201695=CARTESIAN_POINT('Origin',(-19.4030938020118,9.26120677397565,0.));
#201696=CARTESIAN_POINT('',(-20.353053841303,9.71462809124917,0.));
#201697=CARTESIAN_POINT('',(-20.353053841303,9.71462809124917,0.));
#201698=CARTESIAN_POINT('',(-9.70154690100589,4.63060338698782,0.));
#201699=CARTESIAN_POINT('Ctrl Pts',(-24.9347862158358,7.36589684767345,
0.));
#201700=CARTESIAN_POINT('Ctrl Pts',(-24.9347862158358,7.36589684767345,
12.));
#201701=CARTESIAN_POINT('Ctrl Pts',(-24.9292275670674,7.36721909028843,
0.));
#201702=CARTESIAN_POINT('Ctrl Pts',(-24.9292275670674,7.36721909028843,
12.));
#201703=CARTESIAN_POINT('Ctrl Pts',(-24.9181155530543,7.3698559312009,0.));
#201704=CARTESIAN_POINT('Ctrl Pts',(-24.9181155530543,7.3698559312009,12.));
#201705=CARTESIAN_POINT('Ctrl Pts',(-24.901463382605,7.37378825961676,0.));
#201706=CARTESIAN_POINT('Ctrl Pts',(-24.901463382605,7.37378825961676,12.));
#201707=CARTESIAN_POINT('Ctrl Pts',(-24.8792921911115,7.3789854964027,0.));
#201708=CARTESIAN_POINT('Ctrl Pts',(-24.8792921911115,7.3789854964027,12.));
#201709=CARTESIAN_POINT('Ctrl Pts',(-24.8516310625176,7.38540558903621,
0.));
#201710=CARTESIAN_POINT('Ctrl Pts',(-24.8516310625176,7.38540558903621,
12.));
#201711=CARTESIAN_POINT('Ctrl Pts',(-24.8240228520893,7.39174922585808,
0.));
#201712=CARTESIAN_POINT('Ctrl Pts',(-24.8240228520893,7.39174922585808,
12.));
#201713=CARTESIAN_POINT('Ctrl Pts',(-24.7964676646431,7.39801641583013,
0.));
#201714=CARTESIAN_POINT('Ctrl Pts',(-24.7964676646431,7.39801641583013,
12.));
#201715=CARTESIAN_POINT('Ctrl Pts',(-24.7689656668983,7.40420718661603,
0.));
#201716=CARTESIAN_POINT('Ctrl Pts',(-24.7689656668983,7.40420718661603,
12.));
#201717=CARTESIAN_POINT('Ctrl Pts',(-24.7415170994784,7.41032159082382,
0.));
#201718=CARTESIAN_POINT('Ctrl Pts',(-24.7415170994784,7.41032159082382,
12.));
#201719=CARTESIAN_POINT('Ctrl Pts',(-24.7141222950051,7.41635971481674,
0.));
#201720=CARTESIAN_POINT('Ctrl Pts',(-24.7141222950051,7.41635971481674,
12.));
#201721=CARTESIAN_POINT('Ctrl Pts',(-24.6867816727192,7.42232167766265,
0.));
#201722=CARTESIAN_POINT('Ctrl Pts',(-24.6867816727192,7.42232167766265,
12.));
#201723=CARTESIAN_POINT('Ctrl Pts',(-24.6594957128756,7.42820762159126,
0.));
#201724=CARTESIAN_POINT('Ctrl Pts',(-24.6594957128756,7.42820762159126,
12.));
#201725=CARTESIAN_POINT('Ctrl Pts',(-24.6322649369517,7.43401770489524,
0.));
#201726=CARTESIAN_POINT('Ctrl Pts',(-24.6322649369517,7.43401770489524,
12.));
#201727=CARTESIAN_POINT('Ctrl Pts',(-24.6050898852368,7.43975209375504,
0.));
#201728=CARTESIAN_POINT('Ctrl Pts',(-24.6050898852368,7.43975209375504,
12.));
#201729=CARTESIAN_POINT('Ctrl Pts',(-24.577971096086,7.44541095473134,0.));
#201730=CARTESIAN_POINT('Ctrl Pts',(-24.577971096086,7.44541095473134,12.));
#201731=CARTESIAN_POINT('Ctrl Pts',(-24.5509090831559,7.4509944465116,0.));
#201732=CARTESIAN_POINT('Ctrl Pts',(-24.5509090831559,7.4509944465116,12.));
#201733=CARTESIAN_POINT('Ctrl Pts',(-24.5239043173072,7.45650271335862,
0.));
#201734=CARTESIAN_POINT('Ctrl Pts',(-24.5239043173072,7.45650271335862,
12.));
#201735=CARTESIAN_POINT('Ctrl Pts',(-24.4969572391483,7.46193588961463,
0.));
#201736=CARTESIAN_POINT('Ctrl Pts',(-24.4969572391483,7.46193588961463,
12.));
#201737=CARTESIAN_POINT('Ctrl Pts',(-24.4700682684524,7.46729410308786,
0.));
#201738=CARTESIAN_POINT('Ctrl Pts',(-24.4700682684524,7.46729410308786,
12.));
#201739=CARTESIAN_POINT('Ctrl Pts',(-24.443237814649,7.47257747883246,0.));
#201740=CARTESIAN_POINT('Ctrl Pts',(-24.443237814649,7.47257747883246,12.));
#201741=CARTESIAN_POINT('Ctrl Pts',(-24.4164662871163,7.47778614286565,
0.));
#201742=CARTESIAN_POINT('Ctrl Pts',(-24.4164662871163,7.47778614286565,
12.));
#201743=CARTESIAN_POINT('Ctrl Pts',(-24.3897541049254,7.48292022569301,
0.));
#201744=CARTESIAN_POINT('Ctrl Pts',(-24.3897541049254,7.48292022569301,
12.));
#201745=CARTESIAN_POINT('Ctrl Pts',(-24.3631017084524,7.48797986651908,
0.));
#201746=CARTESIAN_POINT('Ctrl Pts',(-24.3631017084524,7.48797986651908,
12.));
#201747=CARTESIAN_POINT('Ctrl Pts',(-24.3365095573685,7.4929652125242,0.));
#201748=CARTESIAN_POINT('Ctrl Pts',(-24.3365095573685,7.4929652125242,12.));
#201749=CARTESIAN_POINT('Ctrl Pts',(-24.3099781253355,7.49787641695439,
0.));
#201750=CARTESIAN_POINT('Ctrl Pts',(-24.3099781253355,7.49787641695439,
12.));
#201751=CARTESIAN_POINT('Ctrl Pts',(-24.2835078958973,7.50271363765152,
0.));
#201752=CARTESIAN_POINT('Ctrl Pts',(-24.2835078958973,7.50271363765152,
12.));
#201753=CARTESIAN_POINT('Ctrl Pts',(-24.2570993577034,7.50747703535133,
0.));
#201754=CARTESIAN_POINT('Ctrl Pts',(-24.2570993577034,7.50747703535133,
12.));
#201755=CARTESIAN_POINT('Ctrl Pts',(-24.2307530003887,7.51216677222181,
0.));
#201756=CARTESIAN_POINT('Ctrl Pts',(-24.2307530003887,7.51216677222181,
12.));
#201757=CARTESIAN_POINT('Ctrl Pts',(-24.2044693092349,7.51678300997949,
0.));
#201758=CARTESIAN_POINT('Ctrl Pts',(-24.2044693092349,7.51678300997949,
12.));
#201759=CARTESIAN_POINT('Ctrl Pts',(-24.1782487641594,7.52132590953802,
0.));
#201760=CARTESIAN_POINT('Ctrl Pts',(-24.1782487641594,7.52132590953802,
12.));
#201761=CARTESIAN_POINT('Ctrl Pts',(-24.1520918425364,7.52579563201424,
0.));
#201762=CARTESIAN_POINT('Ctrl Pts',(-24.1520918425364,7.52579563201424,
12.));
#201763=CARTESIAN_POINT('Ctrl Pts',(-24.1259990209207,7.53019233935501,
0.));
#201764=CARTESIAN_POINT('Ctrl Pts',(-24.1259990209207,7.53019233935501,
12.));
#201765=CARTESIAN_POINT('Ctrl Pts',(-24.0999707772642,7.53451619514649,
0.));
#201766=CARTESIAN_POINT('Ctrl Pts',(-24.0999707772642,7.53451619514649,
12.));
#201767=CARTESIAN_POINT('Ctrl Pts',(-24.0740075927985,7.53876736531014,
0.));
#201768=CARTESIAN_POINT('Ctrl Pts',(-24.0740075927985,7.53876736531014,
12.));
#201769=CARTESIAN_POINT('Ctrl Pts',(-24.0481099543353,7.54294601896144,
0.));
#201770=CARTESIAN_POINT('Ctrl Pts',(-24.0481099543353,7.54294601896144,
12.));
#201771=CARTESIAN_POINT('Ctrl Pts',(-24.022278355453,7.5470523288591,0.));
#201772=CARTESIAN_POINT('Ctrl Pts',(-24.022278355453,7.5470523288591,12.));
#201773=CARTESIAN_POINT('Ctrl Pts',(-23.9965132953185,7.55108647097441,
0.));
#201774=CARTESIAN_POINT('Ctrl Pts',(-23.9965132953185,7.55108647097441,
12.));
#201775=CARTESIAN_POINT('Ctrl Pts',(-23.9708152779884,7.55504862424812,
0.));
#201776=CARTESIAN_POINT('Ctrl Pts',(-23.9708152779884,7.55504862424812,
12.));
#201777=CARTESIAN_POINT('Ctrl Pts',(-23.9451848115,7.55893897027682,0.));
#201778=CARTESIAN_POINT('Ctrl Pts',(-23.9451848115,7.55893897027682,12.));
#201779=CARTESIAN_POINT('Ctrl Pts',(-23.9196224070759,7.56275769304773,
0.));
#201780=CARTESIAN_POINT('Ctrl Pts',(-23.9196224070759,7.56275769304773,
12.));
#201781=CARTESIAN_POINT('Ctrl Pts',(-23.8941285782003,7.56650497863792,
0.));
#201782=CARTESIAN_POINT('Ctrl Pts',(-23.8941285782003,7.56650497863792,
12.));
#201783=CARTESIAN_POINT('Ctrl Pts',(-23.8687038399598,7.57018101500711,
0.));
#201784=CARTESIAN_POINT('Ctrl Pts',(-23.8687038399598,7.57018101500711,
12.));
#201785=CARTESIAN_POINT('Ctrl Pts',(-23.8433487096134,7.57378599219816,
0.));
#201786=CARTESIAN_POINT('Ctrl Pts',(-23.8433487096134,7.57378599219816,
12.));
#201787=CARTESIAN_POINT('Ctrl Pts',(-23.8180637069977,7.57732010249066,
0.));
#201788=CARTESIAN_POINT('Ctrl Pts',(-23.8180637069977,7.57732010249066,
12.));
#201789=CARTESIAN_POINT('Ctrl Pts',(-23.7928493549908,7.58078354058212,
0.));
#201790=CARTESIAN_POINT('Ctrl Pts',(-23.7928493549908,7.58078354058212,
12.));
#201791=CARTESIAN_POINT('Ctrl Pts',(-23.7677061799376,7.58417650376272,
0.));
#201792=CARTESIAN_POINT('Ctrl Pts',(-23.7677061799376,7.58417650376272,
12.));
#201793=CARTESIAN_POINT('Ctrl Pts',(-23.7426347121006,7.58749919210832,
0.));
#201794=CARTESIAN_POINT('Ctrl Pts',(-23.7426347121006,7.58749919210832,
12.));
#201795=CARTESIAN_POINT('Ctrl Pts',(-23.7176354860457,7.59075180865327,
0.));
#201796=CARTESIAN_POINT('Ctrl Pts',(-23.7176354860457,7.59075180865327,
12.));
#201797=CARTESIAN_POINT('Ctrl Pts',(-23.6927090405067,7.59393455934042,
0.));
#201798=CARTESIAN_POINT('Ctrl Pts',(-23.6927090405067,7.59393455934042,
12.));
#201799=CARTESIAN_POINT('Ctrl Pts',(-23.6678559182876,7.59704765299572,
0.));
#201800=CARTESIAN_POINT('Ctrl Pts',(-23.6678559182876,7.59704765299572,
12.));
#201801=CARTESIAN_POINT('Ctrl Pts',(-23.6430766661419,7.60009130130129,
0.));
#201802=CARTESIAN_POINT('Ctrl Pts',(-23.6430766661419,7.60009130130129,
12.));
#201803=CARTESIAN_POINT('Ctrl Pts',(-23.6183718346576,7.60306571877806,
0.));
#201804=CARTESIAN_POINT('Ctrl Pts',(-23.6183718346576,7.60306571877806,
12.));
#201805=CARTESIAN_POINT('Ctrl Pts',(-23.5937419781244,7.60597112277094,
0.));
#201806=CARTESIAN_POINT('Ctrl Pts',(-23.5937419781244,7.60597112277094,
12.));
#201807=CARTESIAN_POINT('Ctrl Pts',(-23.5691876544243,7.60880773344599,
0.));
#201808=CARTESIAN_POINT('Ctrl Pts',(-23.5691876544243,7.60880773344599,
12.));
#201809=CARTESIAN_POINT('Ctrl Pts',(-23.5447094252029,7.61157577385372,
0.));
#201810=CARTESIAN_POINT('Ctrl Pts',(-23.5447094252029,7.61157577385372,
12.));
#201811=CARTESIAN_POINT('Ctrl Pts',(-23.5203078560128,7.61427546999299,
0.));
#201812=CARTESIAN_POINT('Ctrl Pts',(-23.5203078560128,7.61427546999299,
12.));
#201813=CARTESIAN_POINT('Ctrl Pts',(-23.4959835164608,7.61690705088319,
0.));
#201814=CARTESIAN_POINT('Ctrl Pts',(-23.4959835164608,7.61690705088319,
12.));
#201815=CARTESIAN_POINT('Ctrl Pts',(-23.4717369803438,7.61947074863977,
0.));
#201816=CARTESIAN_POINT('Ctrl Pts',(-23.4717369803438,7.61947074863977,
12.));
#201817=CARTESIAN_POINT('Ctrl Pts',(-23.4475688257854,7.62196679855957,
0.));
#201818=CARTESIAN_POINT('Ctrl Pts',(-23.4475688257854,7.62196679855957,
12.));
#201819=CARTESIAN_POINT('Ctrl Pts',(-23.4234796353544,7.62439543920054,
0.));
#201820=CARTESIAN_POINT('Ctrl Pts',(-23.4234796353544,7.62439543920054,
12.));
#201821=CARTESIAN_POINT('Ctrl Pts',(-23.3994699961122,7.62675691240335,
0.));
#201822=CARTESIAN_POINT('Ctrl Pts',(-23.3994699961122,7.62675691240335,
12.));
#201823=CARTESIAN_POINT('Ctrl Pts',(-23.3755404996638,7.62905146332598,
0.));
#201824=CARTESIAN_POINT('Ctrl Pts',(-23.3755404996638,7.62905146332598,
12.));
#201825=CARTESIAN_POINT('Ctrl Pts',(-23.3516917421973,7.63127934048139,
0.));
#201826=CARTESIAN_POINT('Ctrl Pts',(-23.3516917421973,7.63127934048139,
12.));
#201827=CARTESIAN_POINT('Ctrl Pts',(-23.3279243245241,7.63344079578162,
0.));
#201828=CARTESIAN_POINT('Ctrl Pts',(-23.3279243245241,7.63344079578162,
12.));
#201829=CARTESIAN_POINT('Ctrl Pts',(-23.3042388521021,7.63553608458784,
0.));
#201830=CARTESIAN_POINT('Ctrl Pts',(-23.3042388521021,7.63553608458784,
12.));
#201831=CARTESIAN_POINT('Ctrl Pts',(-23.2806359350853,7.63756546576375,
0.));
#201832=CARTESIAN_POINT('Ctrl Pts',(-23.2806359350853,7.63756546576375,
12.));
#201833=CARTESIAN_POINT('Ctrl Pts',(-23.2571161884487,7.63952920172837,
0.));
#201834=CARTESIAN_POINT('Ctrl Pts',(-23.2571161884487,7.63952920172837,
12.));
#201835=CARTESIAN_POINT('Ctrl Pts',(-23.2336802320912,7.64142755851508,
0.));
#201836=CARTESIAN_POINT('Ctrl Pts',(-23.2336802320912,7.64142755851508,
12.));
#201837=CARTESIAN_POINT('Ctrl Pts',(-23.2103286909399,7.64326080583684,
0.));
#201838=CARTESIAN_POINT('Ctrl Pts',(-23.2103286909399,7.64326080583684,
12.));
#201839=CARTESIAN_POINT('Ctrl Pts',(-23.1870621950452,7.64502921715483,
0.));
#201840=CARTESIAN_POINT('Ctrl Pts',(-23.1870621950452,7.64502921715483,
12.));
#201841=CARTESIAN_POINT('Ctrl Pts',(-23.1638813796691,7.64673306975797,
0.));
#201842=CARTESIAN_POINT('Ctrl Pts',(-23.1638813796691,7.64673306975797,
12.));
#201843=CARTESIAN_POINT('Ctrl Pts',(-23.1407868853815,7.64837264482929,
0.));
#201844=CARTESIAN_POINT('Ctrl Pts',(-23.1407868853815,7.64837264482929,
12.));
#201845=CARTESIAN_POINT('Ctrl Pts',(-23.1177793581674,7.64994822749845,
0.));
#201846=CARTESIAN_POINT('Ctrl Pts',(-23.1177793581674,7.64994822749845,
12.));
#201847=CARTESIAN_POINT('Ctrl Pts',(-23.0948594495246,7.65146010690464,
0.));
#201848=CARTESIAN_POINT('Ctrl Pts',(-23.0948594495246,7.65146010690464,
12.));
#201849=CARTESIAN_POINT('Ctrl Pts',(-23.072027816555,7.65290857626356,0.));
#201850=CARTESIAN_POINT('Ctrl Pts',(-23.072027816555,7.65290857626356,12.));
#201851=CARTESIAN_POINT('Ctrl Pts',(-23.049285122053,7.65429393293955,0.));
#201852=CARTESIAN_POINT('Ctrl Pts',(-23.049285122053,7.65429393293955,12.));
#201853=CARTESIAN_POINT('Ctrl Pts',(-23.0266320345792,7.65561647852555,
0.));
#201854=CARTESIAN_POINT('Ctrl Pts',(-23.0266320345792,7.65561647852555,
12.));
#201855=CARTESIAN_POINT('Ctrl Pts',(-23.004069228582,7.6568765189133,0.));
#201856=CARTESIAN_POINT('Ctrl Pts',(-23.004069228582,7.6568765189133,12.));
#201857=CARTESIAN_POINT('Ctrl Pts',(-22.9815973845301,7.65807436436453,
0.));
#201858=CARTESIAN_POINT('Ctrl Pts',(-22.9815973845301,7.65807436436453,
12.));
#201859=CARTESIAN_POINT('Ctrl Pts',(-22.9592171890332,7.65921032958912,
0.));
#201860=CARTESIAN_POINT('Ctrl Pts',(-22.9592171890332,7.65921032958912,
12.));
#201861=CARTESIAN_POINT('Ctrl Pts',(-22.9369293349592,7.66028473382777,
0.));
#201862=CARTESIAN_POINT('Ctrl Pts',(-22.9369293349592,7.66028473382777,
12.));
#201863=CARTESIAN_POINT('Ctrl Pts',(-22.9147345215418,7.661297900941,0.));
#201864=CARTESIAN_POINT('Ctrl Pts',(-22.9147345215418,7.661297900941,12.));
#201865=CARTESIAN_POINT('Ctrl Pts',(-22.8926334544879,7.66225015950147,
0.));
#201866=CARTESIAN_POINT('Ctrl Pts',(-22.8926334544879,7.66225015950147,
12.));
#201867=CARTESIAN_POINT('Ctrl Pts',(-22.870626846128,7.66314184287334,0.));
#201868=CARTESIAN_POINT('Ctrl Pts',(-22.870626846128,7.66314184287334,12.));
#201869=CARTESIAN_POINT('Ctrl Pts',(-22.8487154155569,7.66397328929805,
0.));
#201870=CARTESIAN_POINT('Ctrl Pts',(-22.8487154155569,7.66397328929805,
12.));
#201871=CARTESIAN_POINT('Ctrl Pts',(-22.8268998887679,7.66474484198553,
0.));
#201872=CARTESIAN_POINT('Ctrl Pts',(-22.8268998887679,7.66474484198553,
12.));
#201873=CARTESIAN_POINT('Ctrl Pts',(-22.8051809987834,7.66545684920987,
0.));
#201874=CARTESIAN_POINT('Ctrl Pts',(-22.8051809987834,7.66545684920987,
12.));
#201875=CARTESIAN_POINT('Ctrl Pts',(-22.7835594857697,7.66610966441259,
0.));
#201876=CARTESIAN_POINT('Ctrl Pts',(-22.7835594857697,7.66610966441259,
12.));
#201877=CARTESIAN_POINT('Ctrl Pts',(-22.7620360971839,7.66670364630273,
0.));
#201878=CARTESIAN_POINT('Ctrl Pts',(-22.7620360971839,7.66670364630273,
12.));
#201879=CARTESIAN_POINT('Ctrl Pts',(-22.7406115879508,7.66723915895412,
0.));
#201880=CARTESIAN_POINT('Ctrl Pts',(-22.7406115879508,7.66723915895412,
12.));
#201881=CARTESIAN_POINT('Ctrl Pts',(-22.7192867206242,7.6677165719101,0.));
#201882=CARTESIAN_POINT('Ctrl Pts',(-22.7192867206242,7.6677165719101,12.));
#201883=CARTESIAN_POINT('Ctrl Pts',(-22.6980622655446,7.66813626029276,
0.));
#201884=CARTESIAN_POINT('Ctrl Pts',(-22.6980622655446,7.66813626029276,
12.));
#201885=CARTESIAN_POINT('Ctrl Pts',(-22.6769390009889,7.66849860491763,
0.));
#201886=CARTESIAN_POINT('Ctrl Pts',(-22.6769390009889,7.66849860491763,
12.));
#201887=CARTESIAN_POINT('Ctrl Pts',(-22.6559177133133,7.66880399241354,
0.));
#201888=CARTESIAN_POINT('Ctrl Pts',(-22.6559177133133,7.66880399241354,
12.));
#201889=CARTESIAN_POINT('Ctrl Pts',(-22.6349991971547,7.66905281533745,
0.));
#201890=CARTESIAN_POINT('Ctrl Pts',(-22.6349991971547,7.66905281533745,
12.));
#201891=CARTESIAN_POINT('Ctrl Pts',(-22.6141842556248,7.66924547229435,
0.));
#201892=CARTESIAN_POINT('Ctrl Pts',(-22.6141842556248,7.66924547229435,
12.));
#201893=CARTESIAN_POINT('Ctrl Pts',(-22.5934737004955,7.66938236806241,
0.));
#201894=CARTESIAN_POINT('Ctrl Pts',(-22.5934737004955,7.66938236806241,
12.));
#201895=CARTESIAN_POINT('Ctrl Pts',(-22.5728683523829,7.66946391372299,
0.));
#201896=CARTESIAN_POINT('Ctrl Pts',(-22.5728683523829,7.66946391372299,
12.));
#201897=CARTESIAN_POINT('Ctrl Pts',(-22.5523690409109,7.66949052679671,
0.));
#201898=CARTESIAN_POINT('Ctrl Pts',(-22.5523690409109,7.66949052679671,
12.));
#201899=CARTESIAN_POINT('Ctrl Pts',(-22.5319766049191,7.66946263138116,
0.));
#201900=CARTESIAN_POINT('Ctrl Pts',(-22.5319766049191,7.66946263138116,
12.));
#201901=CARTESIAN_POINT('Ctrl Pts',(-22.5116918927023,7.66938065829082,
0.));
#201902=CARTESIAN_POINT('Ctrl Pts',(-22.5116918927023,7.66938065829082,
12.));
#201903=CARTESIAN_POINT('Ctrl Pts',(-22.4915157622308,7.66924504520302,
0.));
#201904=CARTESIAN_POINT('Ctrl Pts',(-22.4915157622308,7.66924504520302,
12.));
#201905=CARTESIAN_POINT('Ctrl Pts',(-22.47144908137,7.66905623680835,0.));
#201906=CARTESIAN_POINT('Ctrl Pts',(-22.47144908137,7.66905623680835,12.));
#201907=CARTESIAN_POINT('Ctrl Pts',(-22.4514927280863,7.6688146849666,0.));
#201908=CARTESIAN_POINT('Ctrl Pts',(-22.4514927280863,7.6688146849666,12.));
#201909=CARTESIAN_POINT('Ctrl Pts',(-22.4316475906616,7.66852084886745,
0.));
#201910=CARTESIAN_POINT('Ctrl Pts',(-22.4316475906616,7.66852084886745,
12.));
#201911=CARTESIAN_POINT('Ctrl Pts',(-22.411914567977,7.66817519519682,0.));
#201912=CARTESIAN_POINT('Ctrl Pts',(-22.411914567977,7.66817519519682,12.));
#201913=CARTESIAN_POINT('Ctrl Pts',(-22.3922945697782,7.66777819830819,
0.));
#201914=CARTESIAN_POINT('Ctrl Pts',(-22.3922945697782,7.66777819830819,
12.));
#201915=CARTESIAN_POINT('Ctrl Pts',(-22.3727885169361,7.66733034039887,
0.));
#201916=CARTESIAN_POINT('Ctrl Pts',(-22.3727885169361,7.66733034039887,
12.));
#201917=CARTESIAN_POINT('Ctrl Pts',(-22.3533973417013,7.66683211169134,
0.));
#201918=CARTESIAN_POINT('Ctrl Pts',(-22.3533973417013,7.66683211169134,
12.));
#201919=CARTESIAN_POINT('Ctrl Pts',(-22.3341219879454,7.66628401061905,
0.));
#201920=CARTESIAN_POINT('Ctrl Pts',(-22.3341219879454,7.66628401061905,
12.));
#201921=CARTESIAN_POINT('Ctrl Pts',(-22.3149634114823,7.66568654402441,
0.));
#201922=CARTESIAN_POINT('Ctrl Pts',(-22.3149634114823,7.66568654402441,
12.));
#201923=CARTESIAN_POINT('Ctrl Pts',(-22.2959225803925,7.66504022736262,
0.));
#201924=CARTESIAN_POINT('Ctrl Pts',(-22.2959225803925,7.66504022736262,
12.));
#201925=CARTESIAN_POINT('Ctrl Pts',(-22.2770004753332,7.66434558490972,
0.));
#201926=CARTESIAN_POINT('Ctrl Pts',(-22.2770004753332,7.66434558490972,
12.));
#201927=CARTESIAN_POINT('Ctrl Pts',(-22.2581980898487,7.66360314997662,
0.));
#201928=CARTESIAN_POINT('Ctrl Pts',(-22.2581980898487,7.66360314997662,
12.));
#201929=CARTESIAN_POINT('Ctrl Pts',(-22.239516430656,7.66281346512545,0.));
#201930=CARTESIAN_POINT('Ctrl Pts',(-22.239516430656,7.66281346512545,12.));
#201931=CARTESIAN_POINT('Ctrl Pts',(-22.2209565180098,7.66197708240435,
0.));
#201932=CARTESIAN_POINT('Ctrl Pts',(-22.2209565180098,7.66197708240435,
12.));
#201933=CARTESIAN_POINT('Ctrl Pts',(-22.2025193860972,7.66109456359292,
0.));
#201934=CARTESIAN_POINT('Ctrl Pts',(-22.2025193860972,7.66109456359292,
12.));
#201935=CARTESIAN_POINT('Ctrl Pts',(-22.1842060834092,7.66016648045008,
0.));
#201936=CARTESIAN_POINT('Ctrl Pts',(-22.1842060834092,7.66016648045008,
12.));
#201937=CARTESIAN_POINT('Ctrl Pts',(-22.1660176731174,7.65919341496925,
0.));
#201938=CARTESIAN_POINT('Ctrl Pts',(-22.1660176731174,7.65919341496925,
12.));
#201939=CARTESIAN_POINT('Ctrl Pts',(-22.1479552334206,7.65817595963351,
0.));
#201940=CARTESIAN_POINT('Ctrl Pts',(-22.1479552334206,7.65817595963351,
12.));
#201941=CARTESIAN_POINT('Ctrl Pts',(-22.1300198579671,7.65711471769407,
0.));
#201942=CARTESIAN_POINT('Ctrl Pts',(-22.1300198579671,7.65711471769407,
12.));
#201943=CARTESIAN_POINT('Ctrl Pts',(-22.1122126563327,7.65601030346819,
0.));
#201944=CARTESIAN_POINT('Ctrl Pts',(-22.1122126563327,7.65601030346819,
12.));
#201945=CARTESIAN_POINT('Ctrl Pts',(-22.094534754469,7.6548633426365,0.));
#201946=CARTESIAN_POINT('Ctrl Pts',(-22.094534754469,7.6548633426365,12.));
#201947=CARTESIAN_POINT('Ctrl Pts',(-22.0769872951596,7.65367447254945,
0.));
#201948=CARTESIAN_POINT('Ctrl Pts',(-22.0769872951596,7.65367447254945,
12.));
#201949=CARTESIAN_POINT('Ctrl Pts',(-22.0595714384432,7.65244434253104,
0.));
#201950=CARTESIAN_POINT('Ctrl Pts',(-22.0595714384432,7.65244434253104,
12.));
#201951=CARTESIAN_POINT('Ctrl Pts',(-22.0422883621176,7.65117361421346,
0.));
#201952=CARTESIAN_POINT('Ctrl Pts',(-22.0422883621176,7.65117361421346,
12.));
#201953=CARTESIAN_POINT('Ctrl Pts',(-22.0251392623209,7.64986296190156,
0.));
#201954=CARTESIAN_POINT('Ctrl Pts',(-22.0251392623209,7.64986296190156,
12.));
#201955=CARTESIAN_POINT('Ctrl Pts',(-22.0081253540773,7.64851307293346,
0.));
#201956=CARTESIAN_POINT('Ctrl Pts',(-22.0081253540773,7.64851307293346,
12.));
#201957=CARTESIAN_POINT('Ctrl Pts',(-21.9912478718542,7.64712464805258,
0.));
#201958=CARTESIAN_POINT('Ctrl Pts',(-21.9912478718542,7.64712464805258,
12.));
#201959=CARTESIAN_POINT('Ctrl Pts',(-21.97450807008,7.64569840177359,0.));
#201960=CARTESIAN_POINT('Ctrl Pts',(-21.97450807008,7.64569840177359,12.));
#201961=CARTESIAN_POINT('Ctrl Pts',(-21.9579072237653,7.64423506279153,
0.));
#201962=CARTESIAN_POINT('Ctrl Pts',(-21.9579072237653,7.64423506279153,
12.));
#201963=CARTESIAN_POINT('Ctrl Pts',(-21.9414466292074,7.64273537442706,
0.));
#201964=CARTESIAN_POINT('Ctrl Pts',(-21.9414466292074,7.64273537442706,
12.));
#201965=CARTESIAN_POINT('Ctrl Pts',(-21.9251276046546,7.6412000950654,0.));
#201966=CARTESIAN_POINT('Ctrl Pts',(-21.9251276046546,7.6412000950654,12.));
#201967=CARTESIAN_POINT('Ctrl Pts',(-21.9089514909873,7.63962999860916,
0.));
#201968=CARTESIAN_POINT('Ctrl Pts',(-21.9089514909873,7.63962999860916,
12.));
#201969=CARTESIAN_POINT('Ctrl Pts',(-21.8929196523511,7.63802587492007,
0.));
#201970=CARTESIAN_POINT('Ctrl Pts',(-21.8929196523511,7.63802587492007,
12.));
#201971=CARTESIAN_POINT('Ctrl Pts',(-21.8770334769492,7.63638853033367,
0.));
#201972=CARTESIAN_POINT('Ctrl Pts',(-21.8770334769492,7.63638853033367,
12.));
#201973=CARTESIAN_POINT('Ctrl Pts',(-21.8612943779086,7.63471878821203,
0.));
#201974=CARTESIAN_POINT('Ctrl Pts',(-21.8612943779086,7.63471878821203,
12.));
#201975=CARTESIAN_POINT('Ctrl Pts',(-21.8457037941084,7.63301748948936,
0.));
#201976=CARTESIAN_POINT('Ctrl Pts',(-21.8457037941084,7.63301748948936,
12.));
#201977=CARTESIAN_POINT('Ctrl Pts',(-21.8302631910197,7.6312854932304,0.));
#201978=CARTESIAN_POINT('Ctrl Pts',(-21.8302631910197,7.6312854932304,12.));
#201979=CARTESIAN_POINT('Ctrl Pts',(-21.8149740615093,7.62952367718151,
0.));
#201980=CARTESIAN_POINT('Ctrl Pts',(-21.8149740615093,7.62952367718151,
12.));
#201981=CARTESIAN_POINT('Ctrl Pts',(-21.7998379268583,7.62773293842409,
0.));
#201982=CARTESIAN_POINT('Ctrl Pts',(-21.7998379268583,7.62773293842409,
12.));
#201983=CARTESIAN_POINT('Ctrl Pts',(-21.7848563378022,7.62591419404521,
0.));
#201984=CARTESIAN_POINT('Ctrl Pts',(-21.7848563378022,7.62591419404521,
12.));
#201985=CARTESIAN_POINT('Ctrl Pts',(-21.7700308755583,7.62406838181164,
0.));
#201986=CARTESIAN_POINT('Ctrl Pts',(-21.7700308755583,7.62406838181164,
12.));
#201987=CARTESIAN_POINT('Ctrl Pts',(-21.7553631528329,7.62219646084226,
0.));
#201988=CARTESIAN_POINT('Ctrl Pts',(-21.7553631528329,7.62219646084226,
12.));
#201989=CARTESIAN_POINT('Ctrl Pts',(-21.7408548148657,7.62029941230855,
0.));
#201990=CARTESIAN_POINT('Ctrl Pts',(-21.7408548148657,7.62029941230855,
12.));
#201991=CARTESIAN_POINT('Ctrl Pts',(-21.7265075407977,7.61837824030541,
0.));
#201992=CARTESIAN_POINT('Ctrl Pts',(-21.7265075407977,7.61837824030541,
12.));
#201993=CARTESIAN_POINT('Ctrl Pts',(-21.7123230449835,7.61643397270425,
0.));
#201994=CARTESIAN_POINT('Ctrl Pts',(-21.7123230449835,7.61643397270425,
12.));
#201995=CARTESIAN_POINT('Ctrl Pts',(-21.6983030783321,7.61446766202787,
0.));
#201996=CARTESIAN_POINT('Ctrl Pts',(-21.6983030783321,7.61446766202787,
12.));
#201997=CARTESIAN_POINT('Ctrl Pts',(-21.6844494295813,7.61248038630265,
0.));
#201998=CARTESIAN_POINT('Ctrl Pts',(-21.6844494295813,7.61248038630265,
12.));
#201999=CARTESIAN_POINT('Ctrl Pts',(-21.6707639267573,7.6104732500095,0.));
#202000=CARTESIAN_POINT('Ctrl Pts',(-21.6707639267573,7.6104732500095,12.));
#202001=CARTESIAN_POINT('Ctrl Pts',(-21.6572484388079,7.60844738512872,
0.));
#202002=CARTESIAN_POINT('Ctrl Pts',(-21.6572484388079,7.60844738512872,
12.));
#202003=CARTESIAN_POINT('Ctrl Pts',(-21.6439048771743,7.60640395216358,
0.));
#202004=CARTESIAN_POINT('Ctrl Pts',(-21.6439048771743,7.60640395216358,
12.));
#202005=CARTESIAN_POINT('Ctrl Pts',(-21.6307351973823,7.604344141183,0.));
#202006=CARTESIAN_POINT('Ctrl Pts',(-21.6307351973823,7.604344141183,12.));
#202007=CARTESIAN_POINT('Ctrl Pts',(-21.6177414005991,7.60226917285432,
0.));
#202008=CARTESIAN_POINT('Ctrl Pts',(-21.6177414005991,7.60226917285432,
12.));
#202009=CARTESIAN_POINT('Ctrl Pts',(-21.6049255358843,7.60018029988238,
0.));
#202010=CARTESIAN_POINT('Ctrl Pts',(-21.6049255358843,7.60018029988238,
12.));
#202011=CARTESIAN_POINT('Ctrl Pts',(-21.5922897024466,7.59807880846192,
0.));
#202012=CARTESIAN_POINT('Ctrl Pts',(-21.5922897024466,7.59807880846192,
12.));
#202013=CARTESIAN_POINT('Ctrl Pts',(-21.5798360518978,7.59596601973588,
0.));
#202014=CARTESIAN_POINT('Ctrl Pts',(-21.5798360518978,7.59596601973588,
12.));
#202015=CARTESIAN_POINT('Ctrl Pts',(-21.5675667904728,7.5938432912493,0.));
#202016=CARTESIAN_POINT('Ctrl Pts',(-21.5675667904728,7.5938432912493,12.));
#202017=CARTESIAN_POINT('Ctrl Pts',(-21.5554841813465,7.59171201844793,
0.));
#202018=CARTESIAN_POINT('Ctrl Pts',(-21.5554841813465,7.59171201844793,
12.));
#202019=CARTESIAN_POINT('Ctrl Pts',(-21.5435905470113,7.58957363620026,
0.));
#202020=CARTESIAN_POINT('Ctrl Pts',(-21.5435905470113,7.58957363620026,
12.));
#202021=CARTESIAN_POINT('Ctrl Pts',(-21.5318882716735,7.58742962034834,
0.));
#202022=CARTESIAN_POINT('Ctrl Pts',(-21.5318882716735,7.58742962034834,
12.));
#202023=CARTESIAN_POINT('Ctrl Pts',(-21.5203798035294,7.58528148919113,
0.));
#202024=CARTESIAN_POINT('Ctrl Pts',(-21.5203798035294,7.58528148919113,
12.));
#202025=CARTESIAN_POINT('Ctrl Pts',(-21.5090676573866,7.58313080519158,
0.));
#202026=CARTESIAN_POINT('Ctrl Pts',(-21.5090676573866,7.58313080519158,
12.));
#202027=CARTESIAN_POINT('Ctrl Pts',(-21.497954419274,7.5809791779073,0.));
#202028=CARTESIAN_POINT('Ctrl Pts',(-21.497954419274,7.5809791779073,12.));
#202029=CARTESIAN_POINT('Ctrl Pts',(-21.4870427508193,7.57882826679131,
0.));
#202030=CARTESIAN_POINT('Ctrl Pts',(-21.4870427508193,7.57882826679131,
12.));
#202031=CARTESIAN_POINT('Ctrl Pts',(-21.4763353936766,7.57667978403002,
0.));
#202032=CARTESIAN_POINT('Ctrl Pts',(-21.4763353936766,7.57667978403002,
12.));
#202033=CARTESIAN_POINT('Ctrl Pts',(-21.4658351740135,7.57453549743435,
0.));
#202034=CARTESIAN_POINT('Ctrl Pts',(-21.4658351740135,7.57453549743435,
12.));
#202035=CARTESIAN_POINT('Ctrl Pts',(-21.4555450053147,7.57239723223521,
0.));
#202036=CARTESIAN_POINT('Ctrl Pts',(-21.4555450053147,7.57239723223521,
12.));
#202037=CARTESIAN_POINT('Ctrl Pts',(-21.445467890751,7.57026687261169,0.));
#202038=CARTESIAN_POINT('Ctrl Pts',(-21.445467890751,7.57026687261169,12.));
#202039=CARTESIAN_POINT('Ctrl Pts',(-21.435606926151,7.56814636360842,0.));
#202040=CARTESIAN_POINT('Ctrl Pts',(-21.435606926151,7.56814636360842,12.));
#202041=CARTESIAN_POINT('Ctrl Pts',(-21.4259653015732,7.56603771218706,
0.));
#202042=CARTESIAN_POINT('Ctrl Pts',(-21.4259653015732,7.56603771218706,
12.));
#202043=CARTESIAN_POINT('Ctrl Pts',(-21.4165463106252,7.56394299313682,
0.));
#202044=CARTESIAN_POINT('Ctrl Pts',(-21.4165463106252,7.56394299313682,
12.));
#202045=CARTESIAN_POINT('Ctrl Pts',(-21.4073533630364,7.56186435703622,
0.));
#202046=CARTESIAN_POINT('Ctrl Pts',(-21.4073533630364,7.56186435703622,
12.));
#202047=CARTESIAN_POINT('Ctrl Pts',(-21.3983899952988,7.55980403700615,
0.));
#202048=CARTESIAN_POINT('Ctrl Pts',(-21.3983899952988,7.55980403700615,
12.));
#202049=CARTESIAN_POINT('Ctrl Pts',(-21.3896598842119,7.55776435731422,
0.));
#202050=CARTESIAN_POINT('Ctrl Pts',(-21.3896598842119,7.55776435731422,
12.));
#202051=CARTESIAN_POINT('Ctrl Pts',(-21.3811668478933,7.55574773403507,
0.));
#202052=CARTESIAN_POINT('Ctrl Pts',(-21.3811668478933,7.55574773403507,
12.));
#202053=CARTESIAN_POINT('Ctrl Pts',(-21.3729148390244,7.55375667080032,
0.));
#202054=CARTESIAN_POINT('Ctrl Pts',(-21.3729148390244,7.55375667080032,
12.));
#202055=CARTESIAN_POINT('Ctrl Pts',(-21.3649079431864,7.55179375777441,
0.));
#202056=CARTESIAN_POINT('Ctrl Pts',(-21.3649079431864,7.55179375777441,
12.));
#202057=CARTESIAN_POINT('Ctrl Pts',(-21.3571503685853,7.54986166521306,
0.));
#202058=CARTESIAN_POINT('Ctrl Pts',(-21.3571503685853,7.54986166521306,
12.));
#202059=CARTESIAN_POINT('Ctrl Pts',(-21.349646476153,7.54796316246327,0.));
#202060=CARTESIAN_POINT('Ctrl Pts',(-21.349646476153,7.54796316246327,12.));
#202061=CARTESIAN_POINT('Ctrl Pts',(-21.3424008295038,7.54610114948351,
0.));
#202062=CARTESIAN_POINT('Ctrl Pts',(-21.3424008295038,7.54610114948351,
12.));
#202063=CARTESIAN_POINT('Ctrl Pts',(-21.3354182340149,7.54427868151268,
0.));
#202064=CARTESIAN_POINT('Ctrl Pts',(-21.3354182340149,7.54427868151268,
12.));
#202065=CARTESIAN_POINT('Ctrl Pts',(-21.328703791771,7.54249900377031,0.));
#202066=CARTESIAN_POINT('Ctrl Pts',(-21.328703791771,7.54249900377031,12.));
#202067=CARTESIAN_POINT('Ctrl Pts',(-21.3222628524165,7.5407655203828,0.));
#202068=CARTESIAN_POINT('Ctrl Pts',(-21.3222628524165,7.5407655203828,12.));
#202069=CARTESIAN_POINT('Ctrl Pts',(-21.3161009456256,7.53908175169899,
0.));
#202070=CARTESIAN_POINT('Ctrl Pts',(-21.3161009456256,7.53908175169899,
12.));
#202071=CARTESIAN_POINT('Ctrl Pts',(-21.3102237167729,7.53745129364619,
0.));
#202072=CARTESIAN_POINT('Ctrl Pts',(-21.3102237167729,7.53745129364619,
12.));
#202073=CARTESIAN_POINT('Ctrl Pts',(-21.3046368712156,7.53587778251743,
0.));
#202074=CARTESIAN_POINT('Ctrl Pts',(-21.3046368712156,7.53587778251743,
12.));
#202075=CARTESIAN_POINT('Ctrl Pts',(-21.2993464250717,7.53436505309949,
0.));
#202076=CARTESIAN_POINT('Ctrl Pts',(-21.2993464250717,7.53436505309949,
12.));
#202077=CARTESIAN_POINT('Ctrl Pts',(-21.2943588989331,7.53291726078526,
0.));
#202078=CARTESIAN_POINT('Ctrl Pts',(-21.2943588989331,7.53291726078526,
12.));
#202079=CARTESIAN_POINT('Ctrl Pts',(-21.2896816163843,7.53153906987847,
0.));
#202080=CARTESIAN_POINT('Ctrl Pts',(-21.2896816163843,7.53153906987847,
12.));
#202081=CARTESIAN_POINT('Ctrl Pts',(-21.2853226580658,7.53023562438221,
0.));
#202082=CARTESIAN_POINT('Ctrl Pts',(-21.2853226580658,7.53023562438221,
12.));
#202083=CARTESIAN_POINT('Ctrl Pts',(-21.2812902781143,7.52901217930407,
0.));
#202084=CARTESIAN_POINT('Ctrl Pts',(-21.2812902781143,7.52901217930407,
12.));
#202085=CARTESIAN_POINT('Ctrl Pts',(-21.2775925269651,7.52787386225343,
0.));
#202086=CARTESIAN_POINT('Ctrl Pts',(-21.2775925269651,7.52787386225343,
12.));
#202087=CARTESIAN_POINT('Ctrl Pts',(-21.2742366113578,7.5268252691856,0.));
#202088=CARTESIAN_POINT('Ctrl Pts',(-21.2742366113578,7.5268252691856,12.));
#202089=CARTESIAN_POINT('Ctrl Pts',(-21.2712301573465,7.52587126095544,
0.));
#202090=CARTESIAN_POINT('Ctrl Pts',(-21.2712301573465,7.52587126095544,
12.));
#202091=CARTESIAN_POINT('Ctrl Pts',(-21.2685823838672,7.52501770333522,
0.));
#202092=CARTESIAN_POINT('Ctrl Pts',(-21.2685823838672,7.52501770333522,
12.));
#202093=CARTESIAN_POINT('Ctrl Pts',(-21.266305915706,7.52427261074264,0.));
#202094=CARTESIAN_POINT('Ctrl Pts',(-21.266305915706,7.52427261074264,12.));
#202095=CARTESIAN_POINT('Ctrl Pts',(-21.2644161259965,7.52364573027521,
0.));
#202096=CARTESIAN_POINT('Ctrl Pts',(-21.2644161259965,7.52364573027521,
12.));
#202097=CARTESIAN_POINT('Ctrl Pts',(-21.262927782038,7.52314642316202,0.));
#202098=CARTESIAN_POINT('Ctrl Pts',(-21.262927782038,7.52314642316202,12.));
#202099=CARTESIAN_POINT('Ctrl Pts',(-21.261852128355,7.52278182242727,0.));
#202100=CARTESIAN_POINT('Ctrl Pts',(-21.261852128355,7.52278182242727,12.));
#202101=CARTESIAN_POINT('Ctrl Pts',(-21.2613260540651,7.52260064231736,
0.));
#202102=CARTESIAN_POINT('Ctrl Pts',(-21.2613260540651,7.52260064231736,
12.));
#202103=CARTESIAN_POINT('Ctrl Pts',(-21.261120447486,7.52252744144958,0.));
#202104=CARTESIAN_POINT('Ctrl Pts',(-21.261120447486,7.52252744144958,12.));
#202105=CARTESIAN_POINT('Ctrl Pts',(-21.2610673466883,7.52250649703992,
0.));
#202106=CARTESIAN_POINT('Ctrl Pts',(-21.2610673466883,7.52250649703992,
12.));
#202107=CARTESIAN_POINT('Ctrl Pts',(-21.2610617890679,7.52250298901265,
0.));
#202108=CARTESIAN_POINT('Ctrl Pts',(-21.2610617890679,7.52250298901265,
12.));
#202109=CARTESIAN_POINT('',(-24.9347862158358,7.36589684767345,0.));
#202110=CARTESIAN_POINT('Ctrl Pts',(-24.9347862158358,7.36589684767345,
0.));
#202111=CARTESIAN_POINT('Ctrl Pts',(-24.9292275670674,7.36721909028843,
0.));
#202112=CARTESIAN_POINT('Ctrl Pts',(-24.9181155530543,7.3698559312009,0.));
#202113=CARTESIAN_POINT('Ctrl Pts',(-24.901463382605,7.37378825961676,0.));
#202114=CARTESIAN_POINT('Ctrl Pts',(-24.8792921911115,7.3789854964027,0.));
#202115=CARTESIAN_POINT('Ctrl Pts',(-24.8516310625176,7.38540558903621,
0.));
#202116=CARTESIAN_POINT('Ctrl Pts',(-24.8240228520893,7.39174922585808,
0.));
#202117=CARTESIAN_POINT('Ctrl Pts',(-24.7964676646431,7.39801641583013,
0.));
#202118=CARTESIAN_POINT('Ctrl Pts',(-24.7689656668983,7.40420718661603,
0.));
#202119=CARTESIAN_POINT('Ctrl Pts',(-24.7415170994784,7.41032159082382,
0.));
#202120=CARTESIAN_POINT('Ctrl Pts',(-24.7141222950051,7.41635971481674,
0.));
#202121=CARTESIAN_POINT('Ctrl Pts',(-24.6867816727192,7.42232167766265,
0.));
#202122=CARTESIAN_POINT('Ctrl Pts',(-24.6594957128756,7.42820762159126,
0.));
#202123=CARTESIAN_POINT('Ctrl Pts',(-24.6322649369517,7.43401770489524,
0.));
#202124=CARTESIAN_POINT('Ctrl Pts',(-24.6050898852368,7.43975209375504,
0.));
#202125=CARTESIAN_POINT('Ctrl Pts',(-24.577971096086,7.44541095473134,0.));
#202126=CARTESIAN_POINT('Ctrl Pts',(-24.5509090831559,7.4509944465116,0.));
#202127=CARTESIAN_POINT('Ctrl Pts',(-24.5239043173072,7.45650271335862,
0.));
#202128=CARTESIAN_POINT('Ctrl Pts',(-24.4969572391483,7.46193588961463,
0.));
#202129=CARTESIAN_POINT('Ctrl Pts',(-24.4700682684524,7.46729410308786,
0.));
#202130=CARTESIAN_POINT('Ctrl Pts',(-24.443237814649,7.47257747883246,0.));
#202131=CARTESIAN_POINT('Ctrl Pts',(-24.4164662871163,7.47778614286565,
0.));
#202132=CARTESIAN_POINT('Ctrl Pts',(-24.3897541049254,7.48292022569301,
0.));
#202133=CARTESIAN_POINT('Ctrl Pts',(-24.3631017084524,7.48797986651908,
0.));
#202134=CARTESIAN_POINT('Ctrl Pts',(-24.3365095573685,7.4929652125242,0.));
#202135=CARTESIAN_POINT('Ctrl Pts',(-24.3099781253355,7.49787641695439,
0.));
#202136=CARTESIAN_POINT('Ctrl Pts',(-24.2835078958973,7.50271363765152,
0.));
#202137=CARTESIAN_POINT('Ctrl Pts',(-24.2570993577034,7.50747703535133,
0.));
#202138=CARTESIAN_POINT('Ctrl Pts',(-24.2307530003887,7.51216677222181,
0.));
#202139=CARTESIAN_POINT('Ctrl Pts',(-24.2044693092349,7.51678300997949,
0.));
#202140=CARTESIAN_POINT('Ctrl Pts',(-24.1782487641594,7.52132590953802,
0.));
#202141=CARTESIAN_POINT('Ctrl Pts',(-24.1520918425364,7.52579563201424,
0.));
#202142=CARTESIAN_POINT('Ctrl Pts',(-24.1259990209207,7.53019233935501,
0.));
#202143=CARTESIAN_POINT('Ctrl Pts',(-24.0999707772642,7.53451619514649,
0.));
#202144=CARTESIAN_POINT('Ctrl Pts',(-24.0740075927985,7.53876736531014,
0.));
#202145=CARTESIAN_POINT('Ctrl Pts',(-24.0481099543353,7.54294601896144,
0.));
#202146=CARTESIAN_POINT('Ctrl Pts',(-24.022278355453,7.5470523288591,0.));
#202147=CARTESIAN_POINT('Ctrl Pts',(-23.9965132953185,7.55108647097441,
0.));
#202148=CARTESIAN_POINT('Ctrl Pts',(-23.9708152779884,7.55504862424812,
0.));
#202149=CARTESIAN_POINT('Ctrl Pts',(-23.9451848115,7.55893897027682,0.));
#202150=CARTESIAN_POINT('Ctrl Pts',(-23.9196224070759,7.56275769304773,
0.));
#202151=CARTESIAN_POINT('Ctrl Pts',(-23.8941285782003,7.56650497863792,
0.));
#202152=CARTESIAN_POINT('Ctrl Pts',(-23.8687038399598,7.57018101500711,
0.));
#202153=CARTESIAN_POINT('Ctrl Pts',(-23.8433487096134,7.57378599219816,
0.));
#202154=CARTESIAN_POINT('Ctrl Pts',(-23.8180637069977,7.57732010249066,
0.));
#202155=CARTESIAN_POINT('Ctrl Pts',(-23.7928493549908,7.58078354058212,
0.));
#202156=CARTESIAN_POINT('Ctrl Pts',(-23.7677061799376,7.58417650376272,
0.));
#202157=CARTESIAN_POINT('Ctrl Pts',(-23.7426347121006,7.58749919210832,
0.));
#202158=CARTESIAN_POINT('Ctrl Pts',(-23.7176354860457,7.59075180865327,
0.));
#202159=CARTESIAN_POINT('Ctrl Pts',(-23.6927090405067,7.59393455934042,
0.));
#202160=CARTESIAN_POINT('Ctrl Pts',(-23.6678559182876,7.59704765299572,
0.));
#202161=CARTESIAN_POINT('Ctrl Pts',(-23.6430766661419,7.60009130130129,
0.));
#202162=CARTESIAN_POINT('Ctrl Pts',(-23.6183718346576,7.60306571877806,
0.));
#202163=CARTESIAN_POINT('Ctrl Pts',(-23.5937419781244,7.60597112277094,
0.));
#202164=CARTESIAN_POINT('Ctrl Pts',(-23.5691876544243,7.60880773344599,
0.));
#202165=CARTESIAN_POINT('Ctrl Pts',(-23.5447094252029,7.61157577385372,
0.));
#202166=CARTESIAN_POINT('Ctrl Pts',(-23.5203078560128,7.61427546999299,
0.));
#202167=CARTESIAN_POINT('Ctrl Pts',(-23.4959835164608,7.61690705088319,
0.));
#202168=CARTESIAN_POINT('Ctrl Pts',(-23.4717369803438,7.61947074863977,
0.));
#202169=CARTESIAN_POINT('Ctrl Pts',(-23.4475688257854,7.62196679855957,
0.));
#202170=CARTESIAN_POINT('Ctrl Pts',(-23.4234796353544,7.62439543920054,
0.));
#202171=CARTESIAN_POINT('Ctrl Pts',(-23.3994699961122,7.62675691240335,
0.));
#202172=CARTESIAN_POINT('Ctrl Pts',(-23.3755404996638,7.62905146332598,
0.));
#202173=CARTESIAN_POINT('Ctrl Pts',(-23.3516917421973,7.63127934048139,
0.));
#202174=CARTESIAN_POINT('Ctrl Pts',(-23.3279243245241,7.63344079578162,
0.));
#202175=CARTESIAN_POINT('Ctrl Pts',(-23.3042388521021,7.63553608458784,
0.));
#202176=CARTESIAN_POINT('Ctrl Pts',(-23.2806359350853,7.63756546576375,
0.));
#202177=CARTESIAN_POINT('Ctrl Pts',(-23.2571161884487,7.63952920172837,
0.));
#202178=CARTESIAN_POINT('Ctrl Pts',(-23.2336802320912,7.64142755851508,
0.));
#202179=CARTESIAN_POINT('Ctrl Pts',(-23.2103286909399,7.64326080583684,
0.));
#202180=CARTESIAN_POINT('Ctrl Pts',(-23.1870621950452,7.64502921715483,
0.));
#202181=CARTESIAN_POINT('Ctrl Pts',(-23.1638813796691,7.64673306975797,
0.));
#202182=CARTESIAN_POINT('Ctrl Pts',(-23.1407868853815,7.64837264482929,
0.));
#202183=CARTESIAN_POINT('Ctrl Pts',(-23.1177793581674,7.64994822749845,
0.));
#202184=CARTESIAN_POINT('Ctrl Pts',(-23.0948594495246,7.65146010690464,
0.));
#202185=CARTESIAN_POINT('Ctrl Pts',(-23.072027816555,7.65290857626356,0.));
#202186=CARTESIAN_POINT('Ctrl Pts',(-23.049285122053,7.65429393293955,0.));
#202187=CARTESIAN_POINT('Ctrl Pts',(-23.0266320345792,7.65561647852555,
0.));
#202188=CARTESIAN_POINT('Ctrl Pts',(-23.004069228582,7.6568765189133,0.));
#202189=CARTESIAN_POINT('Ctrl Pts',(-22.9815973845301,7.65807436436453,
0.));
#202190=CARTESIAN_POINT('Ctrl Pts',(-22.9592171890332,7.65921032958912,
0.));
#202191=CARTESIAN_POINT('Ctrl Pts',(-22.9369293349592,7.66028473382777,
0.));
#202192=CARTESIAN_POINT('Ctrl Pts',(-22.9147345215418,7.661297900941,0.));
#202193=CARTESIAN_POINT('Ctrl Pts',(-22.8926334544879,7.66225015950147,
0.));
#202194=CARTESIAN_POINT('Ctrl Pts',(-22.870626846128,7.66314184287334,0.));
#202195=CARTESIAN_POINT('Ctrl Pts',(-22.8487154155569,7.66397328929805,
0.));
#202196=CARTESIAN_POINT('Ctrl Pts',(-22.8268998887679,7.66474484198553,
0.));
#202197=CARTESIAN_POINT('Ctrl Pts',(-22.8051809987834,7.66545684920987,
0.));
#202198=CARTESIAN_POINT('Ctrl Pts',(-22.7835594857697,7.66610966441259,
0.));
#202199=CARTESIAN_POINT('Ctrl Pts',(-22.7620360971839,7.66670364630273,
0.));
#202200=CARTESIAN_POINT('Ctrl Pts',(-22.7406115879508,7.66723915895412,
0.));
#202201=CARTESIAN_POINT('Ctrl Pts',(-22.7192867206242,7.6677165719101,0.));
#202202=CARTESIAN_POINT('Ctrl Pts',(-22.6980622655446,7.66813626029276,
0.));
#202203=CARTESIAN_POINT('Ctrl Pts',(-22.6769390009889,7.66849860491763,
0.));
#202204=CARTESIAN_POINT('Ctrl Pts',(-22.6559177133133,7.66880399241354,
0.));
#202205=CARTESIAN_POINT('Ctrl Pts',(-22.6349991971547,7.66905281533745,
0.));
#202206=CARTESIAN_POINT('Ctrl Pts',(-22.6141842556248,7.66924547229435,
0.));
#202207=CARTESIAN_POINT('Ctrl Pts',(-22.5934737004955,7.66938236806241,
0.));
#202208=CARTESIAN_POINT('Ctrl Pts',(-22.5728683523829,7.66946391372299,
0.));
#202209=CARTESIAN_POINT('Ctrl Pts',(-22.5523690409109,7.66949052679671,
0.));
#202210=CARTESIAN_POINT('Ctrl Pts',(-22.5319766049191,7.66946263138116,
0.));
#202211=CARTESIAN_POINT('Ctrl Pts',(-22.5116918927023,7.66938065829082,
0.));
#202212=CARTESIAN_POINT('Ctrl Pts',(-22.4915157622308,7.66924504520302,
0.));
#202213=CARTESIAN_POINT('Ctrl Pts',(-22.47144908137,7.66905623680835,0.));
#202214=CARTESIAN_POINT('Ctrl Pts',(-22.4514927280863,7.6688146849666,0.));
#202215=CARTESIAN_POINT('Ctrl Pts',(-22.4316475906616,7.66852084886745,
0.));
#202216=CARTESIAN_POINT('Ctrl Pts',(-22.411914567977,7.66817519519682,0.));
#202217=CARTESIAN_POINT('Ctrl Pts',(-22.3922945697782,7.66777819830819,
0.));
#202218=CARTESIAN_POINT('Ctrl Pts',(-22.3727885169361,7.66733034039887,
0.));
#202219=CARTESIAN_POINT('Ctrl Pts',(-22.3533973417013,7.66683211169134,
0.));
#202220=CARTESIAN_POINT('Ctrl Pts',(-22.3341219879454,7.66628401061905,
0.));
#202221=CARTESIAN_POINT('Ctrl Pts',(-22.3149634114823,7.66568654402441,
0.));
#202222=CARTESIAN_POINT('Ctrl Pts',(-22.2959225803925,7.66504022736262,
0.));
#202223=CARTESIAN_POINT('Ctrl Pts',(-22.2770004753332,7.66434558490972,
0.));
#202224=CARTESIAN_POINT('Ctrl Pts',(-22.2581980898487,7.66360314997662,
0.));
#202225=CARTESIAN_POINT('Ctrl Pts',(-22.239516430656,7.66281346512545,0.));
#202226=CARTESIAN_POINT('Ctrl Pts',(-22.2209565180098,7.66197708240435,
0.));
#202227=CARTESIAN_POINT('Ctrl Pts',(-22.2025193860972,7.66109456359292,
0.));
#202228=CARTESIAN_POINT('Ctrl Pts',(-22.1842060834092,7.66016648045008,
0.));
#202229=CARTESIAN_POINT('Ctrl Pts',(-22.1660176731174,7.65919341496925,
0.));
#202230=CARTESIAN_POINT('Ctrl Pts',(-22.1479552334206,7.65817595963351,
0.));
#202231=CARTESIAN_POINT('Ctrl Pts',(-22.1300198579671,7.65711471769407,
0.));
#202232=CARTESIAN_POINT('Ctrl Pts',(-22.1122126563327,7.65601030346819,
0.));
#202233=CARTESIAN_POINT('Ctrl Pts',(-22.094534754469,7.6548633426365,0.));
#202234=CARTESIAN_POINT('Ctrl Pts',(-22.0769872951596,7.65367447254945,
0.));
#202235=CARTESIAN_POINT('Ctrl Pts',(-22.0595714384432,7.65244434253104,
0.));
#202236=CARTESIAN_POINT('Ctrl Pts',(-22.0422883621176,7.65117361421346,
0.));
#202237=CARTESIAN_POINT('Ctrl Pts',(-22.0251392623209,7.64986296190156,
0.));
#202238=CARTESIAN_POINT('Ctrl Pts',(-22.0081253540773,7.64851307293346,
0.));
#202239=CARTESIAN_POINT('Ctrl Pts',(-21.9912478718542,7.64712464805258,
0.));
#202240=CARTESIAN_POINT('Ctrl Pts',(-21.97450807008,7.64569840177359,0.));
#202241=CARTESIAN_POINT('Ctrl Pts',(-21.9579072237653,7.64423506279153,
0.));
#202242=CARTESIAN_POINT('Ctrl Pts',(-21.9414466292074,7.64273537442706,
0.));
#202243=CARTESIAN_POINT('Ctrl Pts',(-21.9251276046546,7.6412000950654,0.));
#202244=CARTESIAN_POINT('Ctrl Pts',(-21.9089514909873,7.63962999860916,
0.));
#202245=CARTESIAN_POINT('Ctrl Pts',(-21.8929196523511,7.63802587492007,
0.));
#202246=CARTESIAN_POINT('Ctrl Pts',(-21.8770334769492,7.63638853033367,
0.));
#202247=CARTESIAN_POINT('Ctrl Pts',(-21.8612943779086,7.63471878821203,
0.));
#202248=CARTESIAN_POINT('Ctrl Pts',(-21.8457037941084,7.63301748948936,
0.));
#202249=CARTESIAN_POINT('Ctrl Pts',(-21.8302631910197,7.6312854932304,0.));
#202250=CARTESIAN_POINT('Ctrl Pts',(-21.8149740615093,7.62952367718151,
0.));
#202251=CARTESIAN_POINT('Ctrl Pts',(-21.7998379268583,7.62773293842409,
0.));
#202252=CARTESIAN_POINT('Ctrl Pts',(-21.7848563378022,7.62591419404521,
0.));
#202253=CARTESIAN_POINT('Ctrl Pts',(-21.7700308755583,7.62406838181164,
0.));
#202254=CARTESIAN_POINT('Ctrl Pts',(-21.7553631528329,7.62219646084226,
0.));
#202255=CARTESIAN_POINT('Ctrl Pts',(-21.7408548148657,7.62029941230855,
0.));
#202256=CARTESIAN_POINT('Ctrl Pts',(-21.7265075407977,7.61837824030541,
0.));
#202257=CARTESIAN_POINT('Ctrl Pts',(-21.7123230449835,7.61643397270425,
0.));
#202258=CARTESIAN_POINT('Ctrl Pts',(-21.6983030783321,7.61446766202787,
0.));
#202259=CARTESIAN_POINT('Ctrl Pts',(-21.6844494295813,7.61248038630265,
0.));
#202260=CARTESIAN_POINT('Ctrl Pts',(-21.6707639267573,7.6104732500095,0.));
#202261=CARTESIAN_POINT('Ctrl Pts',(-21.6572484388079,7.60844738512872,
0.));
#202262=CARTESIAN_POINT('Ctrl Pts',(-21.6439048771743,7.60640395216358,
0.));
#202263=CARTESIAN_POINT('Ctrl Pts',(-21.6307351973823,7.604344141183,0.));
#202264=CARTESIAN_POINT('Ctrl Pts',(-21.6177414005991,7.60226917285432,
0.));
#202265=CARTESIAN_POINT('Ctrl Pts',(-21.6049255358843,7.60018029988238,
0.));
#202266=CARTESIAN_POINT('Ctrl Pts',(-21.5922897024466,7.59807880846192,
0.));
#202267=CARTESIAN_POINT('Ctrl Pts',(-21.5798360518978,7.59596601973588,
0.));
#202268=CARTESIAN_POINT('Ctrl Pts',(-21.5675667904728,7.5938432912493,0.));
#202269=CARTESIAN_POINT('Ctrl Pts',(-21.5554841813465,7.59171201844793,
0.));
#202270=CARTESIAN_POINT('Ctrl Pts',(-21.5435905470113,7.58957363620026,
0.));
#202271=CARTESIAN_POINT('Ctrl Pts',(-21.5318882716735,7.58742962034834,
0.));
#202272=CARTESIAN_POINT('Ctrl Pts',(-21.5203798035294,7.58528148919113,
0.));
#202273=CARTESIAN_POINT('Ctrl Pts',(-21.5090676573866,7.58313080519158,
0.));
#202274=CARTESIAN_POINT('Ctrl Pts',(-21.497954419274,7.5809791779073,0.));
#202275=CARTESIAN_POINT('Ctrl Pts',(-21.4870427508193,7.57882826679131,
0.));
#202276=CARTESIAN_POINT('Ctrl Pts',(-21.4763353936766,7.57667978403002,
0.));
#202277=CARTESIAN_POINT('Ctrl Pts',(-21.4658351740135,7.57453549743435,
0.));
#202278=CARTESIAN_POINT('Ctrl Pts',(-21.4555450053147,7.57239723223521,
0.));
#202279=CARTESIAN_POINT('Ctrl Pts',(-21.445467890751,7.57026687261169,0.));
#202280=CARTESIAN_POINT('Ctrl Pts',(-21.435606926151,7.56814636360842,0.));
#202281=CARTESIAN_POINT('Ctrl Pts',(-21.4259653015732,7.56603771218706,
0.));
#202282=CARTESIAN_POINT('Ctrl Pts',(-21.4165463106252,7.56394299313682,
0.));
#202283=CARTESIAN_POINT('Ctrl Pts',(-21.4073533630364,7.56186435703622,
0.));
#202284=CARTESIAN_POINT('Ctrl Pts',(-21.3983899952988,7.55980403700615,
0.));
#202285=CARTESIAN_POINT('Ctrl Pts',(-21.3896598842119,7.55776435731422,
0.));
#202286=CARTESIAN_POINT('Ctrl Pts',(-21.3811668478933,7.55574773403507,
0.));
#202287=CARTESIAN_POINT('Ctrl Pts',(-21.3729148390244,7.55375667080032,
0.));
#202288=CARTESIAN_POINT('Ctrl Pts',(-21.3649079431864,7.55179375777441,
0.));
#202289=CARTESIAN_POINT('Ctrl Pts',(-21.3571503685853,7.54986166521306,
0.));
#202290=CARTESIAN_POINT('Ctrl Pts',(-21.349646476153,7.54796316246327,0.));
#202291=CARTESIAN_POINT('Ctrl Pts',(-21.3424008295038,7.54610114948351,
0.));
#202292=CARTESIAN_POINT('Ctrl Pts',(-21.3354182340149,7.54427868151268,
0.));
#202293=CARTESIAN_POINT('Ctrl Pts',(-21.328703791771,7.54249900377031,0.));
#202294=CARTESIAN_POINT('Ctrl Pts',(-21.3222628524165,7.5407655203828,0.));
#202295=CARTESIAN_POINT('Ctrl Pts',(-21.3161009456256,7.53908175169899,
0.));
#202296=CARTESIAN_POINT('Ctrl Pts',(-21.3102237167729,7.53745129364619,
0.));
#202297=CARTESIAN_POINT('Ctrl Pts',(-21.3046368712156,7.53587778251743,
0.));
#202298=CARTESIAN_POINT('Ctrl Pts',(-21.2993464250717,7.53436505309949,
0.));
#202299=CARTESIAN_POINT('Ctrl Pts',(-21.2943588989331,7.53291726078526,
0.));
#202300=CARTESIAN_POINT('Ctrl Pts',(-21.2896816163843,7.53153906987847,
0.));
#202301=CARTESIAN_POINT('Ctrl Pts',(-21.2853226580658,7.53023562438221,
0.));
#202302=CARTESIAN_POINT('Ctrl Pts',(-21.2812902781143,7.52901217930407,
0.));
#202303=CARTESIAN_POINT('Ctrl Pts',(-21.2775925269651,7.52787386225343,
0.));
#202304=CARTESIAN_POINT('Ctrl Pts',(-21.2742366113578,7.5268252691856,0.));
#202305=CARTESIAN_POINT('Ctrl Pts',(-21.2712301573465,7.52587126095544,
0.));
#202306=CARTESIAN_POINT('Ctrl Pts',(-21.2685823838672,7.52501770333522,
0.));
#202307=CARTESIAN_POINT('Ctrl Pts',(-21.266305915706,7.52427261074264,0.));
#202308=CARTESIAN_POINT('Ctrl Pts',(-21.2644161259965,7.52364573027521,
0.));
#202309=CARTESIAN_POINT('Ctrl Pts',(-21.262927782038,7.52314642316202,0.));
#202310=CARTESIAN_POINT('Ctrl Pts',(-21.261852128355,7.52278182242727,0.));
#202311=CARTESIAN_POINT('Ctrl Pts',(-21.2613260540651,7.52260064231736,
0.));
#202312=CARTESIAN_POINT('Ctrl Pts',(-21.261120447486,7.52252744144958,0.));
#202313=CARTESIAN_POINT('Ctrl Pts',(-21.2610673466883,7.52250649703992,
0.));
#202314=CARTESIAN_POINT('Ctrl Pts',(-21.2610617890679,7.52250298901265,
0.));
#202315=CARTESIAN_POINT('',(-24.9347862158358,7.36589684767345,0.));
#202316=CARTESIAN_POINT('Ctrl Pts',(-20.353053841303,9.71462809124917,0.));
#202317=CARTESIAN_POINT('Ctrl Pts',(-20.353053841303,9.71462809124917,12.));
#202318=CARTESIAN_POINT('Ctrl Pts',(-20.353060251684,9.71462954053074,0.));
#202319=CARTESIAN_POINT('Ctrl Pts',(-20.353060251684,9.71462954053074,12.));
#202320=CARTESIAN_POINT('Ctrl Pts',(-20.3531126095522,9.71465227853122,
0.));
#202321=CARTESIAN_POINT('Ctrl Pts',(-20.3531126095522,9.71465227853122,
12.));
#202322=CARTESIAN_POINT('Ctrl Pts',(-20.3533097561886,9.71474590350791,
0.));
#202323=CARTESIAN_POINT('Ctrl Pts',(-20.3533097561886,9.71474590350791,
12.));
#202324=CARTESIAN_POINT('Ctrl Pts',(-20.3538098605706,9.71498978052101,
0.));
#202325=CARTESIAN_POINT('Ctrl Pts',(-20.3538098605706,9.71498978052101,
12.));
#202326=CARTESIAN_POINT('Ctrl Pts',(-20.3548282742361,9.71549257088175,
0.));
#202327=CARTESIAN_POINT('Ctrl Pts',(-20.3548282742361,9.71549257088175,
12.));
#202328=CARTESIAN_POINT('Ctrl Pts',(-20.3562337557875,9.71619192554147,
0.));
#202329=CARTESIAN_POINT('Ctrl Pts',(-20.3562337557875,9.71619192554147,
12.));
#202330=CARTESIAN_POINT('Ctrl Pts',(-20.3580133103357,9.71708493723061,
0.));
#202331=CARTESIAN_POINT('Ctrl Pts',(-20.3580133103357,9.71708493723061,
12.));
#202332=CARTESIAN_POINT('Ctrl Pts',(-20.3601498764344,9.71816778327999,
0.));
#202333=CARTESIAN_POINT('Ctrl Pts',(-20.3601498764344,9.71816778327999,
12.));
#202334=CARTESIAN_POINT('Ctrl Pts',(-20.362625691398,9.71943648548114,0.));
#202335=CARTESIAN_POINT('Ctrl Pts',(-20.362625691398,9.71943648548114,12.));
#202336=CARTESIAN_POINT('Ctrl Pts',(-20.3654261611055,9.72088778381102,
0.));
#202337=CARTESIAN_POINT('Ctrl Pts',(-20.3654261611055,9.72088778381102,
12.));
#202338=CARTESIAN_POINT('Ctrl Pts',(-20.3685406190576,9.72251930722504,
0.));
#202339=CARTESIAN_POINT('Ctrl Pts',(-20.3685406190576,9.72251930722504,
12.));
#202340=CARTESIAN_POINT('Ctrl Pts',(-20.371960235676,9.72432910043193,0.));
#202341=CARTESIAN_POINT('Ctrl Pts',(-20.371960235676,9.72432910043193,12.));
#202342=CARTESIAN_POINT('Ctrl Pts',(-20.3756766651952,9.72631531732871,
0.));
#202343=CARTESIAN_POINT('Ctrl Pts',(-20.3756766651952,9.72631531732871,
12.));
#202344=CARTESIAN_POINT('Ctrl Pts',(-20.3796805893304,9.72847589116533,
0.));
#202345=CARTESIAN_POINT('Ctrl Pts',(-20.3796805893304,9.72847589116533,
12.));
#202346=CARTESIAN_POINT('Ctrl Pts',(-20.3839624556742,9.73080870123726,
0.));
#202347=CARTESIAN_POINT('Ctrl Pts',(-20.3839624556742,9.73080870123726,
12.));
#202348=CARTESIAN_POINT('Ctrl Pts',(-20.3885129129912,9.73331167102812,
0.));
#202349=CARTESIAN_POINT('Ctrl Pts',(-20.3885129129912,9.73331167102812,
12.));
#202350=CARTESIAN_POINT('Ctrl Pts',(-20.3933234845646,9.7359829201425,0.));
#202351=CARTESIAN_POINT('Ctrl Pts',(-20.3933234845646,9.7359829201425,12.));
#202352=CARTESIAN_POINT('Ctrl Pts',(-20.3983866213331,9.73882077613206,
0.));
#202353=CARTESIAN_POINT('Ctrl Pts',(-20.3983866213331,9.73882077613206,
12.));
#202354=CARTESIAN_POINT('Ctrl Pts',(-20.4036953576549,9.74182369656272,
0.));
#202355=CARTESIAN_POINT('Ctrl Pts',(-20.4036953576549,9.74182369656272,
12.));
#202356=CARTESIAN_POINT('Ctrl Pts',(-20.4092430879861,9.74499021838536,
0.));
#202357=CARTESIAN_POINT('Ctrl Pts',(-20.4092430879861,9.74499021838536,
12.));
#202358=CARTESIAN_POINT('Ctrl Pts',(-20.4150232777393,9.74831889242175,
0.));
#202359=CARTESIAN_POINT('Ctrl Pts',(-20.4150232777393,9.74831889242175,
12.));
#202360=CARTESIAN_POINT('Ctrl Pts',(-20.4210295275818,9.75180829786433,
0.));
#202361=CARTESIAN_POINT('Ctrl Pts',(-20.4210295275818,9.75180829786433,
12.));
#202362=CARTESIAN_POINT('Ctrl Pts',(-20.4272556476629,9.75545705902416,
0.));
#202363=CARTESIAN_POINT('Ctrl Pts',(-20.4272556476629,9.75545705902416,
12.));
#202364=CARTESIAN_POINT('Ctrl Pts',(-20.4336957355474,9.7592638628993,0.));
#202365=CARTESIAN_POINT('Ctrl Pts',(-20.4336957355474,9.7592638628993,12.));
#202366=CARTESIAN_POINT('Ctrl Pts',(-20.4403442329401,9.76322747195502,
0.));
#202367=CARTESIAN_POINT('Ctrl Pts',(-20.4403442329401,9.76322747195502,
12.));
#202368=CARTESIAN_POINT('Ctrl Pts',(-20.447195862298,9.76734670980897,0.));
#202369=CARTESIAN_POINT('Ctrl Pts',(-20.447195862298,9.76734670980897,12.));
#202370=CARTESIAN_POINT('Ctrl Pts',(-20.4542455817527,9.7716204510407,0.));
#202371=CARTESIAN_POINT('Ctrl Pts',(-20.4542455817527,9.7716204510407,12.));
#202372=CARTESIAN_POINT('Ctrl Pts',(-20.4614885274973,9.77604760815523,
0.));
#202373=CARTESIAN_POINT('Ctrl Pts',(-20.4614885274973,9.77604760815523,
12.));
#202374=CARTESIAN_POINT('Ctrl Pts',(-20.4689199790668,9.78062712373313,
0.));
#202375=CARTESIAN_POINT('Ctrl Pts',(-20.4689199790668,9.78062712373313,
12.));
#202376=CARTESIAN_POINT('Ctrl Pts',(-20.4765353711585,9.78535797314162,
0.));
#202377=CARTESIAN_POINT('Ctrl Pts',(-20.4765353711585,9.78535797314162,
12.));
#202378=CARTESIAN_POINT('Ctrl Pts',(-20.4843302955329,9.7902391649866,0.));
#202379=CARTESIAN_POINT('Ctrl Pts',(-20.4843302955329,9.7902391649866,12.));
#202380=CARTESIAN_POINT('Ctrl Pts',(-20.4923005087945,9.79526974288344,
0.));
#202381=CARTESIAN_POINT('Ctrl Pts',(-20.4923005087945,9.79526974288344,
12.));
#202382=CARTESIAN_POINT('Ctrl Pts',(-20.500441931211,9.80044878520967,0.));
#202383=CARTESIAN_POINT('Ctrl Pts',(-20.500441931211,9.80044878520967,12.));
#202384=CARTESIAN_POINT('Ctrl Pts',(-20.5087506310507,9.80577540161103,
0.));
#202385=CARTESIAN_POINT('Ctrl Pts',(-20.5087506310507,9.80577540161103,
12.));
#202386=CARTESIAN_POINT('Ctrl Pts',(-20.5172228122839,9.81124873025278,
0.));
#202387=CARTESIAN_POINT('Ctrl Pts',(-20.5172228122839,9.81124873025278,
12.));
#202388=CARTESIAN_POINT('Ctrl Pts',(-20.5258548000625,9.81686793455918,
0.));
#202389=CARTESIAN_POINT('Ctrl Pts',(-20.5258548000625,9.81686793455918,
12.));
#202390=CARTESIAN_POINT('Ctrl Pts',(-20.534643029951,9.82263220080328,0.));
#202391=CARTESIAN_POINT('Ctrl Pts',(-20.534643029951,9.82263220080328,12.));
#202392=CARTESIAN_POINT('Ctrl Pts',(-20.5435840460717,9.82854073773857,
0.));
#202393=CARTESIAN_POINT('Ctrl Pts',(-20.5435840460717,9.82854073773857,
12.));
#202394=CARTESIAN_POINT('Ctrl Pts',(-20.5526744976461,9.83459277585321,
0.));
#202395=CARTESIAN_POINT('Ctrl Pts',(-20.5526744976461,9.83459277585321,
12.));
#202396=CARTESIAN_POINT('Ctrl Pts',(-20.5619111362406,9.84078756677589,
0.));
#202397=CARTESIAN_POINT('Ctrl Pts',(-20.5619111362406,9.84078756677589,
12.));
#202398=CARTESIAN_POINT('Ctrl Pts',(-20.5712908125145,9.84712438256308,
0.));
#202399=CARTESIAN_POINT('Ctrl Pts',(-20.5712908125145,9.84712438256308,
12.));
#202400=CARTESIAN_POINT('Ctrl Pts',(-20.580810471002,9.85360251457004,0.));
#202401=CARTESIAN_POINT('Ctrl Pts',(-20.580810471002,9.85360251457004,12.));
#202402=CARTESIAN_POINT('Ctrl Pts',(-20.5904671449754,9.86022127232749,
0.));
#202403=CARTESIAN_POINT('Ctrl Pts',(-20.5904671449754,9.86022127232749,
12.));
#202404=CARTESIAN_POINT('Ctrl Pts',(-20.6002579513696,9.86697998242612,
0.));
#202405=CARTESIAN_POINT('Ctrl Pts',(-20.6002579513696,9.86697998242612,
12.));
#202406=CARTESIAN_POINT('Ctrl Pts',(-20.6101800854491,9.87387798732944,
0.));
#202407=CARTESIAN_POINT('Ctrl Pts',(-20.6101800854491,9.87387798732944,
12.));
#202408=CARTESIAN_POINT('Ctrl Pts',(-20.6202308177472,9.88091464472669,
0.));
#202409=CARTESIAN_POINT('Ctrl Pts',(-20.6202308177472,9.88091464472669,
12.));
#202410=CARTESIAN_POINT('Ctrl Pts',(-20.6304074914086,9.88808932697305,
0.));
#202411=CARTESIAN_POINT('Ctrl Pts',(-20.6304074914086,9.88808932697305,
12.));
#202412=CARTESIAN_POINT('Ctrl Pts',(-20.6407075193977,9.89540142049124,
0.));
#202413=CARTESIAN_POINT('Ctrl Pts',(-20.6407075193977,9.89540142049124,
12.));
#202414=CARTESIAN_POINT('Ctrl Pts',(-20.6511283817415,9.90285032516696,
0.));
#202415=CARTESIAN_POINT('Ctrl Pts',(-20.6511283817415,9.90285032516696,
12.));
#202416=CARTESIAN_POINT('Ctrl Pts',(-20.6616676228315,9.91043545377004,
0.));
#202417=CARTESIAN_POINT('Ctrl Pts',(-20.6616676228315,9.91043545377004,
12.));
#202418=CARTESIAN_POINT('Ctrl Pts',(-20.6723228488262,9.91815623141284,
0.));
#202419=CARTESIAN_POINT('Ctrl Pts',(-20.6723228488262,9.91815623141284,
12.));
#202420=CARTESIAN_POINT('Ctrl Pts',(-20.6830917250255,9.9260120949875,0.));
#202421=CARTESIAN_POINT('Ctrl Pts',(-20.6830917250255,9.9260120949875,12.));
#202422=CARTESIAN_POINT('Ctrl Pts',(-20.6939719732485,9.93400249259736,
0.));
#202423=CARTESIAN_POINT('Ctrl Pts',(-20.6939719732485,9.93400249259736,
12.));
#202424=CARTESIAN_POINT('Ctrl Pts',(-20.7049613692237,9.94212688298251,
0.));
#202425=CARTESIAN_POINT('Ctrl Pts',(-20.7049613692237,9.94212688298251,
12.));
#202426=CARTESIAN_POINT('Ctrl Pts',(-20.716057740758,9.95038473514962,0.));
#202427=CARTESIAN_POINT('Ctrl Pts',(-20.716057740758,9.95038473514962,12.));
#202428=CARTESIAN_POINT('Ctrl Pts',(-20.7272589658752,9.95877552798403,
0.));
#202429=CARTESIAN_POINT('Ctrl Pts',(-20.7272589658752,9.95877552798403,
12.));
#202430=CARTESIAN_POINT('Ctrl Pts',(-20.7385629709795,9.96729874986198,
0.));
#202431=CARTESIAN_POINT('Ctrl Pts',(-20.7385629709795,9.96729874986198,
12.));
#202432=CARTESIAN_POINT('Ctrl Pts',(-20.7499677289625,9.97595389823461,
0.));
#202433=CARTESIAN_POINT('Ctrl Pts',(-20.7499677289625,9.97595389823461,
12.));
#202434=CARTESIAN_POINT('Ctrl Pts',(-20.7614712574989,9.98474047926846,
0.));
#202435=CARTESIAN_POINT('Ctrl Pts',(-20.7614712574989,9.98474047926846,
12.));
#202436=CARTESIAN_POINT('Ctrl Pts',(-20.7730716175417,9.99365800754638,
0.));
#202437=CARTESIAN_POINT('Ctrl Pts',(-20.7730716175417,9.99365800754638,
12.));
#202438=CARTESIAN_POINT('Ctrl Pts',(-20.7847669117568,10.0027060057389,
0.));
#202439=CARTESIAN_POINT('Ctrl Pts',(-20.7847669117568,10.0027060057389,
12.));
#202440=CARTESIAN_POINT('Ctrl Pts',(-20.7965552829907,10.0118840042786,
0.));
#202441=CARTESIAN_POINT('Ctrl Pts',(-20.7965552829907,10.0118840042786,
12.));
#202442=CARTESIAN_POINT('Ctrl Pts',(-20.8084349126885,10.0211915410095,
0.));
#202443=CARTESIAN_POINT('Ctrl Pts',(-20.8084349126885,10.0211915410095,
12.));
#202444=CARTESIAN_POINT('Ctrl Pts',(-20.8204040196599,10.0306281609435,
0.));
#202445=CARTESIAN_POINT('Ctrl Pts',(-20.8204040196599,10.0306281609435,
12.));
#202446=CARTESIAN_POINT('Ctrl Pts',(-20.8324608588906,10.0401934160234,
0.));
#202447=CARTESIAN_POINT('Ctrl Pts',(-20.8324608588906,10.0401934160234,
12.));
#202448=CARTESIAN_POINT('Ctrl Pts',(-20.8446037203402,10.0498868648733,
0.));
#202449=CARTESIAN_POINT('Ctrl Pts',(-20.8446037203402,10.0498868648733,
12.));
#202450=CARTESIAN_POINT('Ctrl Pts',(-20.856830927732,10.0597080725375,0.));
#202451=CARTESIAN_POINT('Ctrl Pts',(-20.856830927732,10.0597080725375,12.));
#202452=CARTESIAN_POINT('Ctrl Pts',(-20.8691408373705,10.0696566102219,
0.));
#202453=CARTESIAN_POINT('Ctrl Pts',(-20.8691408373705,10.0696566102219,
12.));
#202454=CARTESIAN_POINT('Ctrl Pts',(-20.8815318371844,10.0797320551154,
0.));
#202455=CARTESIAN_POINT('Ctrl Pts',(-20.8815318371844,10.0797320551154,
12.));
#202456=CARTESIAN_POINT('Ctrl Pts',(-20.8940023457371,10.0899339901916,
0.));
#202457=CARTESIAN_POINT('Ctrl Pts',(-20.8940023457371,10.0899339901916,
12.));
#202458=CARTESIAN_POINT('Ctrl Pts',(-20.9065508112556,10.1002620040076,
0.));
#202459=CARTESIAN_POINT('Ctrl Pts',(-20.9065508112556,10.1002620040076,
12.));
#202460=CARTESIAN_POINT('Ctrl Pts',(-20.9191757106266,10.1107156904836,
0.));
#202461=CARTESIAN_POINT('Ctrl Pts',(-20.9191757106266,10.1107156904836,
12.));
#202462=CARTESIAN_POINT('Ctrl Pts',(-20.931875548473,10.1212946487057,0.));
#202463=CARTESIAN_POINT('Ctrl Pts',(-20.931875548473,10.1212946487057,12.));
#202464=CARTESIAN_POINT('Ctrl Pts',(-20.944648856393,10.1319984827909,0.));
#202465=CARTESIAN_POINT('Ctrl Pts',(-20.944648856393,10.1319984827909,12.));
#202466=CARTESIAN_POINT('Ctrl Pts',(-20.9574941921591,10.1428268017257,
0.));
#202467=CARTESIAN_POINT('Ctrl Pts',(-20.9574941921591,10.1428268017257,
12.));
#202468=CARTESIAN_POINT('Ctrl Pts',(-20.970410138937,10.1537792192065,0.));
#202469=CARTESIAN_POINT('Ctrl Pts',(-20.970410138937,10.1537792192065,12.));
#202470=CARTESIAN_POINT('Ctrl Pts',(-20.9833953044737,10.1648553534567,
0.));
#202471=CARTESIAN_POINT('Ctrl Pts',(-20.9833953044737,10.1648553534567,
12.));
#202472=CARTESIAN_POINT('Ctrl Pts',(-20.9964483203685,10.1760548270765,
0.));
#202473=CARTESIAN_POINT('Ctrl Pts',(-20.9964483203685,10.1760548270765,
12.));
#202474=CARTESIAN_POINT('Ctrl Pts',(-21.0095678414486,10.1873772669358,
0.));
#202475=CARTESIAN_POINT('Ctrl Pts',(-21.0095678414486,10.1873772669358,
12.));
#202476=CARTESIAN_POINT('Ctrl Pts',(-21.0227525451107,10.1988223040425,
0.));
#202477=CARTESIAN_POINT('Ctrl Pts',(-21.0227525451107,10.1988223040425,
12.));
#202478=CARTESIAN_POINT('Ctrl Pts',(-21.0360011306814,10.2103895734123,
0.));
#202479=CARTESIAN_POINT('Ctrl Pts',(-21.0360011306814,10.2103895734123,
12.));
#202480=CARTESIAN_POINT('Ctrl Pts',(-21.0493123187483,10.2220787139157,
0.));
#202481=CARTESIAN_POINT('Ctrl Pts',(-21.0493123187483,10.2220787139157,
12.));
#202482=CARTESIAN_POINT('Ctrl Pts',(-21.0626848505665,10.233889368157,0.));
#202483=CARTESIAN_POINT('Ctrl Pts',(-21.0626848505665,10.233889368157,12.));
#202484=CARTESIAN_POINT('Ctrl Pts',(-21.0761174875448,10.2458211823915,
0.));
#202485=CARTESIAN_POINT('Ctrl Pts',(-21.0761174875448,10.2458211823915,
12.));
#202486=CARTESIAN_POINT('Ctrl Pts',(-21.0896090107066,10.2578738064183,
0.));
#202487=CARTESIAN_POINT('Ctrl Pts',(-21.0896090107066,10.2578738064183,
12.));
#202488=CARTESIAN_POINT('Ctrl Pts',(-21.1031582201625,10.2700468934743,
0.));
#202489=CARTESIAN_POINT('Ctrl Pts',(-21.1031582201625,10.2700468934743,
12.));
#202490=CARTESIAN_POINT('Ctrl Pts',(-21.1167639345623,10.2823401001067,
0.));
#202491=CARTESIAN_POINT('Ctrl Pts',(-21.1167639345623,10.2823401001067,
12.));
#202492=CARTESIAN_POINT('Ctrl Pts',(-21.130424990599,10.2947530860714,0.));
#202493=CARTESIAN_POINT('Ctrl Pts',(-21.130424990599,10.2947530860714,12.));
#202494=CARTESIAN_POINT('Ctrl Pts',(-21.1441402425831,10.307285514268,0.));
#202495=CARTESIAN_POINT('Ctrl Pts',(-21.1441402425831,10.307285514268,12.));
#202496=CARTESIAN_POINT('Ctrl Pts',(-21.1579085619959,10.3199370506541,
0.));
#202497=CARTESIAN_POINT('Ctrl Pts',(-21.1579085619959,10.3199370506541,
12.));
#202498=CARTESIAN_POINT('Ctrl Pts',(-21.1717288370512,10.3327073641574,
0.));
#202499=CARTESIAN_POINT('Ctrl Pts',(-21.1717288370512,10.3327073641574,
12.));
#202500=CARTESIAN_POINT('Ctrl Pts',(-21.1855999722427,10.3455961265706,
0.));
#202501=CARTESIAN_POINT('Ctrl Pts',(-21.1855999722427,10.3455961265706,
12.));
#202502=CARTESIAN_POINT('Ctrl Pts',(-21.1995208879205,10.3586030124595,
0.));
#202503=CARTESIAN_POINT('Ctrl Pts',(-21.1995208879205,10.3586030124595,
12.));
#202504=CARTESIAN_POINT('Ctrl Pts',(-21.2134905199359,10.3717276991137,
0.));
#202505=CARTESIAN_POINT('Ctrl Pts',(-21.2134905199359,10.3717276991137,
12.));
#202506=CARTESIAN_POINT('Ctrl Pts',(-21.2275078192708,10.384969866479,0.));
#202507=CARTESIAN_POINT('Ctrl Pts',(-21.2275078192708,10.384969866479,12.));
#202508=CARTESIAN_POINT('Ctrl Pts',(-21.2415717516713,10.3983291970846,
0.));
#202509=CARTESIAN_POINT('Ctrl Pts',(-21.2415717516713,10.3983291970846,
12.));
#202510=CARTESIAN_POINT('Ctrl Pts',(-21.2556812972741,10.4118053759584,
0.));
#202511=CARTESIAN_POINT('Ctrl Pts',(-21.2556812972741,10.4118053759584,
12.));
#202512=CARTESIAN_POINT('Ctrl Pts',(-21.2698354502391,10.4253980905394,
0.));
#202513=CARTESIAN_POINT('Ctrl Pts',(-21.2698354502391,10.4253980905394,
12.));
#202514=CARTESIAN_POINT('Ctrl Pts',(-21.2840332184471,10.4391070306385,
0.));
#202515=CARTESIAN_POINT('Ctrl Pts',(-21.2840332184471,10.4391070306385,
12.));
#202516=CARTESIAN_POINT('Ctrl Pts',(-21.2982736231924,10.452931888387,0.));
#202517=CARTESIAN_POINT('Ctrl Pts',(-21.2982736231924,10.452931888387,12.));
#202518=CARTESIAN_POINT('Ctrl Pts',(-21.312555698873,10.4668723581768,0.));
#202519=CARTESIAN_POINT('Ctrl Pts',(-21.312555698873,10.4668723581768,12.));
#202520=CARTESIAN_POINT('Ctrl Pts',(-21.3268784926823,10.4809281365933,
0.));
#202521=CARTESIAN_POINT('Ctrl Pts',(-21.3268784926823,10.4809281365933,
12.));
#202522=CARTESIAN_POINT('Ctrl Pts',(-21.3412410642912,10.4950989223341,
0.));
#202523=CARTESIAN_POINT('Ctrl Pts',(-21.3412410642912,10.4950989223341,
12.));
#202524=CARTESIAN_POINT('Ctrl Pts',(-21.3556424855822,10.5093844161689,
0.));
#202525=CARTESIAN_POINT('Ctrl Pts',(-21.3556424855822,10.5093844161689,
12.));
#202526=CARTESIAN_POINT('Ctrl Pts',(-21.3700818403942,10.523784320906,0.));
#202527=CARTESIAN_POINT('Ctrl Pts',(-21.3700818403942,10.523784320906,12.));
#202528=CARTESIAN_POINT('Ctrl Pts',(-21.3845582242604,10.5382983413422,
0.));
#202529=CARTESIAN_POINT('Ctrl Pts',(-21.3845582242604,10.5382983413422,
12.));
#202530=CARTESIAN_POINT('Ctrl Pts',(-21.3990707441495,10.5529261842107,
0.));
#202531=CARTESIAN_POINT('Ctrl Pts',(-21.3990707441495,10.5529261842107,
12.));
#202532=CARTESIAN_POINT('Ctrl Pts',(-21.4136185181974,10.5676675581106,
0.));
#202533=CARTESIAN_POINT('Ctrl Pts',(-21.4136185181974,10.5676675581106,
12.));
#202534=CARTESIAN_POINT('Ctrl Pts',(-21.4282006754624,10.582522173457,0.));
#202535=CARTESIAN_POINT('Ctrl Pts',(-21.4282006754624,10.582522173457,12.));
#202536=CARTESIAN_POINT('Ctrl Pts',(-21.4428163557137,10.597489742462,0.));
#202537=CARTESIAN_POINT('Ctrl Pts',(-21.4428163557137,10.597489742462,12.));
#202538=CARTESIAN_POINT('Ctrl Pts',(-21.4574647092093,10.612569979096,0.));
#202539=CARTESIAN_POINT('Ctrl Pts',(-21.4574647092093,10.612569979096,12.));
#202540=CARTESIAN_POINT('Ctrl Pts',(-21.4721448964766,10.6277625990457,
0.));
#202541=CARTESIAN_POINT('Ctrl Pts',(-21.4721448964766,10.6277625990457,
12.));
#202542=CARTESIAN_POINT('Ctrl Pts',(-21.4868560880893,10.6430673196609,
0.));
#202543=CARTESIAN_POINT('Ctrl Pts',(-21.4868560880893,10.6430673196609,
12.));
#202544=CARTESIAN_POINT('Ctrl Pts',(-21.5015974644454,10.658483859894,0.));
#202545=CARTESIAN_POINT('Ctrl Pts',(-21.5015974644454,10.658483859894,12.));
#202546=CARTESIAN_POINT('Ctrl Pts',(-21.5163682155805,10.6740119402835,
0.));
#202547=CARTESIAN_POINT('Ctrl Pts',(-21.5163682155805,10.6740119402835,
12.));
#202548=CARTESIAN_POINT('Ctrl Pts',(-21.531167540981,10.689651282929,0.));
#202549=CARTESIAN_POINT('Ctrl Pts',(-21.531167540981,10.689651282929,12.));
#202550=CARTESIAN_POINT('Ctrl Pts',(-21.5459946493955,10.7054016114571,
0.));
#202551=CARTESIAN_POINT('Ctrl Pts',(-21.5459946493955,10.7054016114571,
12.));
#202552=CARTESIAN_POINT('Ctrl Pts',(-21.5608487586467,10.7212626509816,
0.));
#202553=CARTESIAN_POINT('Ctrl Pts',(-21.5608487586467,10.7212626509816,
12.));
#202554=CARTESIAN_POINT('Ctrl Pts',(-21.5757290954372,10.7372341280468,
0.));
#202555=CARTESIAN_POINT('Ctrl Pts',(-21.5757290954372,10.7372341280468,
12.));
#202556=CARTESIAN_POINT('Ctrl Pts',(-21.5906348951745,10.7533157705943,
0.));
#202557=CARTESIAN_POINT('Ctrl Pts',(-21.5906348951745,10.7533157705943,
12.));
#202558=CARTESIAN_POINT('Ctrl Pts',(-21.6055654018179,10.7695073079554,
0.));
#202559=CARTESIAN_POINT('Ctrl Pts',(-21.6055654018179,10.7695073079554,
12.));
#202560=CARTESIAN_POINT('Ctrl Pts',(-21.6205198677176,10.7858084708262,
0.));
#202561=CARTESIAN_POINT('Ctrl Pts',(-21.6205198677176,10.7858084708262,
12.));
#202562=CARTESIAN_POINT('Ctrl Pts',(-21.6354975534557,10.8022189912369,
0.));
#202563=CARTESIAN_POINT('Ctrl Pts',(-21.6354975534557,10.8022189912369,
12.));
#202564=CARTESIAN_POINT('Ctrl Pts',(-21.6504977276864,10.8187386025135,
0.));
#202565=CARTESIAN_POINT('Ctrl Pts',(-21.6504977276864,10.8187386025135,
12.));
#202566=CARTESIAN_POINT('Ctrl Pts',(-21.6655196669727,10.835367039227,0.));
#202567=CARTESIAN_POINT('Ctrl Pts',(-21.6655196669727,10.835367039227,12.));
#202568=CARTESIAN_POINT('Ctrl Pts',(-21.6805626556461,10.8521040371832,
0.));
#202569=CARTESIAN_POINT('Ctrl Pts',(-21.6805626556461,10.8521040371832,
12.));
#202570=CARTESIAN_POINT('Ctrl Pts',(-21.6956259856667,10.8689493334093,
0.));
#202571=CARTESIAN_POINT('Ctrl Pts',(-21.6956259856667,10.8689493334093,
12.));
#202572=CARTESIAN_POINT('Ctrl Pts',(-21.7107089564822,10.8859026661292,
0.));
#202573=CARTESIAN_POINT('Ctrl Pts',(-21.7107089564822,10.8859026661292,
12.));
#202574=CARTESIAN_POINT('Ctrl Pts',(-21.7258108748874,10.9029637747341,
0.));
#202575=CARTESIAN_POINT('Ctrl Pts',(-21.7258108748874,10.9029637747341,
12.));
#202576=CARTESIAN_POINT('Ctrl Pts',(-21.74093105488,10.9201323997386,0.));
#202577=CARTESIAN_POINT('Ctrl Pts',(-21.74093105488,10.9201323997386,12.));
#202578=CARTESIAN_POINT('Ctrl Pts',(-21.7560688175252,10.9374082827446,
0.));
#202579=CARTESIAN_POINT('Ctrl Pts',(-21.7560688175252,10.9374082827446,
12.));
#202580=CARTESIAN_POINT('Ctrl Pts',(-21.7712234908468,10.9547911664457,
0.));
#202581=CARTESIAN_POINT('Ctrl Pts',(-21.7712234908468,10.9547911664457,
12.));
#202582=CARTESIAN_POINT('Ctrl Pts',(-21.7863944097143,10.9722807946157,
0.));
#202583=CARTESIAN_POINT('Ctrl Pts',(-21.7863944097143,10.9722807946157,
12.));
#202584=CARTESIAN_POINT('Ctrl Pts',(-21.8015809157302,10.9898769120913,
0.));
#202585=CARTESIAN_POINT('Ctrl Pts',(-21.8015809157302,10.9898769120913,
12.));
#202586=CARTESIAN_POINT('Ctrl Pts',(-21.8167823571168,11.0075792647477,
0.));
#202587=CARTESIAN_POINT('Ctrl Pts',(-21.8167823571168,11.0075792647477,
12.));
#202588=CARTESIAN_POINT('Ctrl Pts',(-21.8319980886033,11.0253875994598,
0.));
#202589=CARTESIAN_POINT('Ctrl Pts',(-21.8319980886033,11.0253875994598,
12.));
#202590=CARTESIAN_POINT('Ctrl Pts',(-21.8472274713103,11.0433016640808,
0.));
#202591=CARTESIAN_POINT('Ctrl Pts',(-21.8472274713103,11.0433016640808,
12.));
#202592=CARTESIAN_POINT('Ctrl Pts',(-21.8624698726319,11.0613212074364,
0.));
#202593=CARTESIAN_POINT('Ctrl Pts',(-21.8624698726319,11.0613212074364,
12.));
#202594=CARTESIAN_POINT('Ctrl Pts',(-21.8777246661191,11.0794459793058,
0.));
#202595=CARTESIAN_POINT('Ctrl Pts',(-21.8777246661191,11.0794459793058,
12.));
#202596=CARTESIAN_POINT('Ctrl Pts',(-21.8929912313608,11.0976757303944,
0.));
#202597=CARTESIAN_POINT('Ctrl Pts',(-21.8929912313608,11.0976757303944,
12.));
#202598=CARTESIAN_POINT('Ctrl Pts',(-21.9082689538687,11.1160102123024,
0.));
#202599=CARTESIAN_POINT('Ctrl Pts',(-21.9082689538687,11.1160102123024,
12.));
#202600=CARTESIAN_POINT('Ctrl Pts',(-21.9235572249518,11.134449177474,0.));
#202601=CARTESIAN_POINT('Ctrl Pts',(-21.9235572249518,11.134449177474,12.));
#202602=CARTESIAN_POINT('Ctrl Pts',(-21.9388554416437,11.1529923792002,
0.));
#202603=CARTESIAN_POINT('Ctrl Pts',(-21.9388554416437,11.1529923792002,
12.));
#202604=CARTESIAN_POINT('Ctrl Pts',(-21.9541630066504,11.1716395716375,
0.));
#202605=CARTESIAN_POINT('Ctrl Pts',(-21.9541630066504,11.1716395716375,
12.));
#202606=CARTESIAN_POINT('Ctrl Pts',(-21.9694793282913,11.1903905098109,
0.));
#202607=CARTESIAN_POINT('Ctrl Pts',(-21.9694793282913,11.1903905098109,
12.));
#202608=CARTESIAN_POINT('Ctrl Pts',(-21.9848038204439,11.2092449496125,
0.));
#202609=CARTESIAN_POINT('Ctrl Pts',(-21.9848038204439,11.2092449496125,
12.));
#202610=CARTESIAN_POINT('Ctrl Pts',(-22.0001359024839,11.2282026477897,
0.));
#202611=CARTESIAN_POINT('Ctrl Pts',(-22.0001359024839,11.2282026477897,
12.));
#202612=CARTESIAN_POINT('Ctrl Pts',(-22.0154749992364,11.2472633619276,
0.));
#202613=CARTESIAN_POINT('Ctrl Pts',(-22.0154749992364,11.2472633619276,
12.));
#202614=CARTESIAN_POINT('Ctrl Pts',(-22.0308205408351,11.2664268504207,
0.));
#202615=CARTESIAN_POINT('Ctrl Pts',(-22.0308205408351,11.2664268504207,
12.));
#202616=CARTESIAN_POINT('Ctrl Pts',(-22.046171962566,11.2856928724374,0.));
#202617=CARTESIAN_POINT('Ctrl Pts',(-22.046171962566,11.2856928724374,12.));
#202618=CARTESIAN_POINT('Ctrl Pts',(-22.0615287047179,11.3050611878771,
0.));
#202619=CARTESIAN_POINT('Ctrl Pts',(-22.0615287047179,11.3050611878771,
12.));
#202620=CARTESIAN_POINT('Ctrl Pts',(-22.0768902124267,11.3245315573168,
0.));
#202621=CARTESIAN_POINT('Ctrl Pts',(-22.0768902124267,11.3245315573168,
12.));
#202622=CARTESIAN_POINT('Ctrl Pts',(-22.0922559355293,11.3441037419553,
0.));
#202623=CARTESIAN_POINT('Ctrl Pts',(-22.0922559355293,11.3441037419553,
12.));
#202624=CARTESIAN_POINT('Ctrl Pts',(-22.1076253283978,11.3637775035367,
0.));
#202625=CARTESIAN_POINT('Ctrl Pts',(-22.1076253283978,11.3637775035367,
12.));
#202626=CARTESIAN_POINT('Ctrl Pts',(-22.1229978500185,11.3835526044256,
0.));
#202627=CARTESIAN_POINT('Ctrl Pts',(-22.1229978500185,11.3835526044256,
12.));
#202628=CARTESIAN_POINT('Ctrl Pts',(-22.1383729640963,11.4034288076908,
0.));
#202629=CARTESIAN_POINT('Ctrl Pts',(-22.1383729640963,11.4034288076908,
12.));
#202630=CARTESIAN_POINT('Ctrl Pts',(-22.1537501391486,11.4234058771742,
0.));
#202631=CARTESIAN_POINT('Ctrl Pts',(-22.1537501391486,11.4234058771742,
12.));
#202632=CARTESIAN_POINT('Ctrl Pts',(-22.1691288486096,11.443483577557,0.));
#202633=CARTESIAN_POINT('Ctrl Pts',(-22.1691288486096,11.443483577557,12.));
#202634=CARTESIAN_POINT('Ctrl Pts',(-22.184508570917,11.463661674411,0.));
#202635=CARTESIAN_POINT('Ctrl Pts',(-22.184508570917,11.463661674411,12.));
#202636=CARTESIAN_POINT('Ctrl Pts',(-22.1998887896435,11.4839399342589,
0.));
#202637=CARTESIAN_POINT('Ctrl Pts',(-22.1998887896435,11.4839399342589,
12.));
#202638=CARTESIAN_POINT('Ctrl Pts',(-22.215268993102,11.504318124424,0.));
#202639=CARTESIAN_POINT('Ctrl Pts',(-22.215268993102,11.504318124424,12.));
#202640=CARTESIAN_POINT('Ctrl Pts',(-22.2306486738899,11.5247960128476,
0.));
#202641=CARTESIAN_POINT('Ctrl Pts',(-22.2306486738899,11.5247960128476,
12.));
#202642=CARTESIAN_POINT('Ctrl Pts',(-22.2460273284653,11.545373367912,0.));
#202643=CARTESIAN_POINT('Ctrl Pts',(-22.2460273284653,11.545373367912,12.));
#202644=CARTESIAN_POINT('Ctrl Pts',(-22.2614044566898,11.5660499582403,
0.));
#202645=CARTESIAN_POINT('Ctrl Pts',(-22.2614044566898,11.5660499582403,
12.));
#202646=CARTESIAN_POINT('Ctrl Pts',(-22.2767795614349,11.5868255525189,
0.));
#202647=CARTESIAN_POINT('Ctrl Pts',(-22.2767795614349,11.5868255525189,
12.));
#202648=CARTESIAN_POINT('Ctrl Pts',(-22.2921521480358,11.6076999192359,
0.));
#202649=CARTESIAN_POINT('Ctrl Pts',(-22.2921521480358,11.6076999192359,
12.));
#202650=CARTESIAN_POINT('Ctrl Pts',(-22.3075217249049,11.6286728270011,
0.));
#202651=CARTESIAN_POINT('Ctrl Pts',(-22.3075217249049,11.6286728270011,
12.));
#202652=CARTESIAN_POINT('Ctrl Pts',(-22.3228878043976,11.6497440449858,
0.));
#202653=CARTESIAN_POINT('Ctrl Pts',(-22.3228878043976,11.6497440449858,
12.));
#202654=CARTESIAN_POINT('Ctrl Pts',(-22.3382499035618,11.6709133432986,
0.));
#202655=CARTESIAN_POINT('Ctrl Pts',(-22.3382499035618,11.6709133432986,
12.));
#202656=CARTESIAN_POINT('Ctrl Pts',(-22.3536075450028,11.6921804934056,
0.));
#202657=CARTESIAN_POINT('Ctrl Pts',(-22.3536075450028,11.6921804934056,
12.));
#202658=CARTESIAN_POINT('Ctrl Pts',(-22.3689602575492,11.7135452684532,
0.));
#202659=CARTESIAN_POINT('Ctrl Pts',(-22.3689602575492,11.7135452684532,
12.));
#202660=CARTESIAN_POINT('Ctrl Pts',(-22.3843075773905,11.7350074437961,
0.));
#202661=CARTESIAN_POINT('Ctrl Pts',(-22.3843075773905,11.7350074437961,
12.));
#202662=CARTESIAN_POINT('Ctrl Pts',(-22.39964904692,11.7565667964765,0.));
#202663=CARTESIAN_POINT('Ctrl Pts',(-22.39964904692,11.7565667964765,12.));
#202664=CARTESIAN_POINT('Ctrl Pts',(-22.4149842125018,11.7782231042041,
0.));
#202665=CARTESIAN_POINT('Ctrl Pts',(-22.4149842125018,11.7782231042041,
12.));
#202666=CARTESIAN_POINT('Ctrl Pts',(-22.4303126226468,11.7999761445175,
0.));
#202667=CARTESIAN_POINT('Ctrl Pts',(-22.4303126226468,11.7999761445175,
12.));
#202668=CARTESIAN_POINT('Ctrl Pts',(-22.4456338258738,11.8218256937889,
0.));
#202669=CARTESIAN_POINT('Ctrl Pts',(-22.4456338258738,11.8218256937889,
12.));
#202670=CARTESIAN_POINT('Ctrl Pts',(-22.4609473690469,11.8437715264487,
0.));
#202671=CARTESIAN_POINT('Ctrl Pts',(-22.4609473690469,11.8437715264487,
12.));
#202672=CARTESIAN_POINT('Ctrl Pts',(-22.4762527946694,11.8658134137018,
0.));
#202673=CARTESIAN_POINT('Ctrl Pts',(-22.4762527946694,11.8658134137018,
12.));
#202674=CARTESIAN_POINT('Ctrl Pts',(-22.4915496418472,11.8879511239941,
0.));
#202675=CARTESIAN_POINT('Ctrl Pts',(-22.4915496418472,11.8879511239941,
12.));
#202676=CARTESIAN_POINT('Ctrl Pts',(-22.5068374513958,11.9101844254555,
0.));
#202677=CARTESIAN_POINT('Ctrl Pts',(-22.5068374513958,11.9101844254555,
12.));
#202678=CARTESIAN_POINT('Ctrl Pts',(-22.5221157697869,11.9325130877801,
0.));
#202679=CARTESIAN_POINT('Ctrl Pts',(-22.5221157697869,11.9325130877801,
12.));
#202680=CARTESIAN_POINT('Ctrl Pts',(-22.5373841537299,11.9549368843996,
0.));
#202681=CARTESIAN_POINT('Ctrl Pts',(-22.5373841537299,11.9549368843996,
12.));
#202682=CARTESIAN_POINT('Ctrl Pts',(-22.5526421741159,11.9774555943496,
0.));
#202683=CARTESIAN_POINT('Ctrl Pts',(-22.5526421741159,11.9774555943496,
12.));
#202684=CARTESIAN_POINT('Ctrl Pts',(-22.5678894211194,12.0000690046697,
0.));
#202685=CARTESIAN_POINT('Ctrl Pts',(-22.5678894211194,12.0000690046697,
12.));
#202686=CARTESIAN_POINT('Ctrl Pts',(-22.5831255061306,12.0227769113132,
0.));
#202687=CARTESIAN_POINT('Ctrl Pts',(-22.5831255061306,12.0227769113132,
12.));
#202688=CARTESIAN_POINT('Ctrl Pts',(-22.5983500505675,12.0455791139135,
0.));
#202689=CARTESIAN_POINT('Ctrl Pts',(-22.5983500505675,12.0455791139135,
12.));
#202690=CARTESIAN_POINT('Ctrl Pts',(-22.613562676493,12.0684754113869,0.));
#202691=CARTESIAN_POINT('Ctrl Pts',(-22.613562676493,12.0684754113869,12.));
#202692=CARTESIAN_POINT('Ctrl Pts',(-22.628762996708,12.0914655972828,0.));
#202693=CARTESIAN_POINT('Ctrl Pts',(-22.628762996708,12.0914655972828,12.));
#202694=CARTESIAN_POINT('Ctrl Pts',(-22.6439506046611,12.1145494550384,
0.));
#202695=CARTESIAN_POINT('Ctrl Pts',(-22.6439506046611,12.1145494550384,
12.));
#202696=CARTESIAN_POINT('Ctrl Pts',(-22.6591250653942,12.1377267537141,
0.));
#202697=CARTESIAN_POINT('Ctrl Pts',(-22.6591250653942,12.1377267537141,
12.));
#202698=CARTESIAN_POINT('Ctrl Pts',(-22.6742859034891,12.1609972423088,
0.));
#202699=CARTESIAN_POINT('Ctrl Pts',(-22.6742859034891,12.1609972423088,
12.));
#202700=CARTESIAN_POINT('Ctrl Pts',(-22.6894326204959,12.1843606579246,
0.));
#202701=CARTESIAN_POINT('Ctrl Pts',(-22.6894326204959,12.1843606579246,
12.));
#202702=CARTESIAN_POINT('Ctrl Pts',(-22.7045647168659,12.2078167360267,
0.));
#202703=CARTESIAN_POINT('Ctrl Pts',(-22.7045647168659,12.2078167360267,
12.));
#202704=CARTESIAN_POINT('Ctrl Pts',(-22.7196817119299,12.2313652198047,
0.));
#202705=CARTESIAN_POINT('Ctrl Pts',(-22.7196817119299,12.2313652198047,
12.));
#202706=CARTESIAN_POINT('Ctrl Pts',(-22.7347831655251,12.2550058702389,
0.));
#202707=CARTESIAN_POINT('Ctrl Pts',(-22.7347831655251,12.2550058702389,
12.));
#202708=CARTESIAN_POINT('Ctrl Pts',(-22.7498686970096,12.2787384750747,
0.));
#202709=CARTESIAN_POINT('Ctrl Pts',(-22.7498686970096,12.2787384750747,
12.));
#202710=CARTESIAN_POINT('Ctrl Pts',(-22.7649380101154,12.3025628601812,
0.));
#202711=CARTESIAN_POINT('Ctrl Pts',(-22.7649380101154,12.3025628601812,
12.));
#202712=CARTESIAN_POINT('Ctrl Pts',(-22.7799908974947,12.3264788926108,
0.));
#202713=CARTESIAN_POINT('Ctrl Pts',(-22.7799908974947,12.3264788926108,
12.));
#202714=CARTESIAN_POINT('Ctrl Pts',(-22.7950272216959,12.3504864740361,
0.));
#202715=CARTESIAN_POINT('Ctrl Pts',(-22.7950272216959,12.3504864740361,
12.));
#202716=CARTESIAN_POINT('Ctrl Pts',(-22.8100469022632,12.3745855366772,
0.));
#202717=CARTESIAN_POINT('Ctrl Pts',(-22.8100469022632,12.3745855366772,
12.));
#202718=CARTESIAN_POINT('Ctrl Pts',(-22.8220493007353,12.393937937903,0.));
#202719=CARTESIAN_POINT('Ctrl Pts',(-22.8220493007353,12.393937937903,12.));
#202720=CARTESIAN_POINT('Ctrl Pts',(-22.8310435872852,12.4084933766366,
0.));
#202721=CARTESIAN_POINT('Ctrl Pts',(-22.8310435872852,12.4084933766366,
12.));
#202722=CARTESIAN_POINT('Ctrl Pts',(-22.8370364396497,12.4182152851867,
0.));
#202723=CARTESIAN_POINT('Ctrl Pts',(-22.8370364396497,12.4182152851867,
12.));
#202724=CARTESIAN_POINT('Ctrl Pts',(-22.8400320311648,12.4230808101438,
0.));
#202725=CARTESIAN_POINT('Ctrl Pts',(-22.8400320311648,12.4230808101438,
12.));
#202726=CARTESIAN_POINT('',(-22.8400320311648,12.4230808101438,0.));
#202727=CARTESIAN_POINT('Ctrl Pts',(-20.353053841303,9.71462809124917,0.));
#202728=CARTESIAN_POINT('Ctrl Pts',(-20.353060251684,9.71462954053074,0.));
#202729=CARTESIAN_POINT('Ctrl Pts',(-20.3531126095522,9.71465227853122,
0.));
#202730=CARTESIAN_POINT('Ctrl Pts',(-20.3533097561886,9.71474590350791,
0.));
#202731=CARTESIAN_POINT('Ctrl Pts',(-20.3538098605706,9.71498978052101,
0.));
#202732=CARTESIAN_POINT('Ctrl Pts',(-20.3548282742361,9.71549257088175,
0.));
#202733=CARTESIAN_POINT('Ctrl Pts',(-20.3562337557875,9.71619192554147,
0.));
#202734=CARTESIAN_POINT('Ctrl Pts',(-20.3580133103357,9.71708493723061,
0.));
#202735=CARTESIAN_POINT('Ctrl Pts',(-20.3601498764344,9.71816778327999,
0.));
#202736=CARTESIAN_POINT('Ctrl Pts',(-20.362625691398,9.71943648548114,0.));
#202737=CARTESIAN_POINT('Ctrl Pts',(-20.3654261611055,9.72088778381102,
0.));
#202738=CARTESIAN_POINT('Ctrl Pts',(-20.3685406190576,9.72251930722504,
0.));
#202739=CARTESIAN_POINT('Ctrl Pts',(-20.371960235676,9.72432910043193,0.));
#202740=CARTESIAN_POINT('Ctrl Pts',(-20.3756766651952,9.72631531732871,
0.));
#202741=CARTESIAN_POINT('Ctrl Pts',(-20.3796805893304,9.72847589116533,
0.));
#202742=CARTESIAN_POINT('Ctrl Pts',(-20.3839624556742,9.73080870123726,
0.));
#202743=CARTESIAN_POINT('Ctrl Pts',(-20.3885129129912,9.73331167102812,
0.));
#202744=CARTESIAN_POINT('Ctrl Pts',(-20.3933234845646,9.7359829201425,0.));
#202745=CARTESIAN_POINT('Ctrl Pts',(-20.3983866213331,9.73882077613206,
0.));
#202746=CARTESIAN_POINT('Ctrl Pts',(-20.4036953576549,9.74182369656272,
0.));
#202747=CARTESIAN_POINT('Ctrl Pts',(-20.4092430879861,9.74499021838536,
0.));
#202748=CARTESIAN_POINT('Ctrl Pts',(-20.4150232777393,9.74831889242175,
0.));
#202749=CARTESIAN_POINT('Ctrl Pts',(-20.4210295275818,9.75180829786433,
0.));
#202750=CARTESIAN_POINT('Ctrl Pts',(-20.4272556476629,9.75545705902416,
0.));
#202751=CARTESIAN_POINT('Ctrl Pts',(-20.4336957355474,9.7592638628993,0.));
#202752=CARTESIAN_POINT('Ctrl Pts',(-20.4403442329401,9.76322747195502,
0.));
#202753=CARTESIAN_POINT('Ctrl Pts',(-20.447195862298,9.76734670980897,0.));
#202754=CARTESIAN_POINT('Ctrl Pts',(-20.4542455817527,9.7716204510407,0.));
#202755=CARTESIAN_POINT('Ctrl Pts',(-20.4614885274973,9.77604760815523,
0.));
#202756=CARTESIAN_POINT('Ctrl Pts',(-20.4689199790668,9.78062712373313,
0.));
#202757=CARTESIAN_POINT('Ctrl Pts',(-20.4765353711585,9.78535797314162,
0.));
#202758=CARTESIAN_POINT('Ctrl Pts',(-20.4843302955329,9.7902391649866,0.));
#202759=CARTESIAN_POINT('Ctrl Pts',(-20.4923005087945,9.79526974288344,
0.));
#202760=CARTESIAN_POINT('Ctrl Pts',(-20.500441931211,9.80044878520967,0.));
#202761=CARTESIAN_POINT('Ctrl Pts',(-20.5087506310507,9.80577540161103,
0.));
#202762=CARTESIAN_POINT('Ctrl Pts',(-20.5172228122839,9.81124873025278,
0.));
#202763=CARTESIAN_POINT('Ctrl Pts',(-20.5258548000625,9.81686793455918,
0.));
#202764=CARTESIAN_POINT('Ctrl Pts',(-20.534643029951,9.82263220080328,0.));
#202765=CARTESIAN_POINT('Ctrl Pts',(-20.5435840460717,9.82854073773857,
0.));
#202766=CARTESIAN_POINT('Ctrl Pts',(-20.5526744976461,9.83459277585321,
0.));
#202767=CARTESIAN_POINT('Ctrl Pts',(-20.5619111362406,9.84078756677589,
0.));
#202768=CARTESIAN_POINT('Ctrl Pts',(-20.5712908125145,9.84712438256308,
0.));
#202769=CARTESIAN_POINT('Ctrl Pts',(-20.580810471002,9.85360251457004,0.));
#202770=CARTESIAN_POINT('Ctrl Pts',(-20.5904671449754,9.86022127232749,
0.));
#202771=CARTESIAN_POINT('Ctrl Pts',(-20.6002579513696,9.86697998242612,
0.));
#202772=CARTESIAN_POINT('Ctrl Pts',(-20.6101800854491,9.87387798732944,
0.));
#202773=CARTESIAN_POINT('Ctrl Pts',(-20.6202308177472,9.88091464472669,
0.));
#202774=CARTESIAN_POINT('Ctrl Pts',(-20.6304074914086,9.88808932697305,
0.));
#202775=CARTESIAN_POINT('Ctrl Pts',(-20.6407075193977,9.89540142049124,
0.));
#202776=CARTESIAN_POINT('Ctrl Pts',(-20.6511283817415,9.90285032516696,
0.));
#202777=CARTESIAN_POINT('Ctrl Pts',(-20.6616676228315,9.91043545377004,
0.));
#202778=CARTESIAN_POINT('Ctrl Pts',(-20.6723228488262,9.91815623141284,
0.));
#202779=CARTESIAN_POINT('Ctrl Pts',(-20.6830917250255,9.9260120949875,0.));
#202780=CARTESIAN_POINT('Ctrl Pts',(-20.6939719732485,9.93400249259736,
0.));
#202781=CARTESIAN_POINT('Ctrl Pts',(-20.7049613692237,9.94212688298251,
0.));
#202782=CARTESIAN_POINT('Ctrl Pts',(-20.716057740758,9.95038473514962,0.));
#202783=CARTESIAN_POINT('Ctrl Pts',(-20.7272589658752,9.95877552798403,
0.));
#202784=CARTESIAN_POINT('Ctrl Pts',(-20.7385629709795,9.96729874986198,
0.));
#202785=CARTESIAN_POINT('Ctrl Pts',(-20.7499677289625,9.97595389823461,
0.));
#202786=CARTESIAN_POINT('Ctrl Pts',(-20.7614712574989,9.98474047926846,
0.));
#202787=CARTESIAN_POINT('Ctrl Pts',(-20.7730716175417,9.99365800754638,
0.));
#202788=CARTESIAN_POINT('Ctrl Pts',(-20.7847669117568,10.0027060057389,
0.));
#202789=CARTESIAN_POINT('Ctrl Pts',(-20.7965552829907,10.0118840042786,
0.));
#202790=CARTESIAN_POINT('Ctrl Pts',(-20.8084349126885,10.0211915410095,
0.));
#202791=CARTESIAN_POINT('Ctrl Pts',(-20.8204040196599,10.0306281609435,
0.));
#202792=CARTESIAN_POINT('Ctrl Pts',(-20.8324608588906,10.0401934160234,
0.));
#202793=CARTESIAN_POINT('Ctrl Pts',(-20.8446037203402,10.0498868648733,
0.));
#202794=CARTESIAN_POINT('Ctrl Pts',(-20.856830927732,10.0597080725375,0.));
#202795=CARTESIAN_POINT('Ctrl Pts',(-20.8691408373705,10.0696566102219,
0.));
#202796=CARTESIAN_POINT('Ctrl Pts',(-20.8815318371844,10.0797320551154,
0.));
#202797=CARTESIAN_POINT('Ctrl Pts',(-20.8940023457371,10.0899339901916,
0.));
#202798=CARTESIAN_POINT('Ctrl Pts',(-20.9065508112556,10.1002620040076,
0.));
#202799=CARTESIAN_POINT('Ctrl Pts',(-20.9191757106266,10.1107156904836,
0.));
#202800=CARTESIAN_POINT('Ctrl Pts',(-20.931875548473,10.1212946487057,0.));
#202801=CARTESIAN_POINT('Ctrl Pts',(-20.944648856393,10.1319984827909,0.));
#202802=CARTESIAN_POINT('Ctrl Pts',(-20.9574941921591,10.1428268017257,
0.));
#202803=CARTESIAN_POINT('Ctrl Pts',(-20.970410138937,10.1537792192065,0.));
#202804=CARTESIAN_POINT('Ctrl Pts',(-20.9833953044737,10.1648553534567,
0.));
#202805=CARTESIAN_POINT('Ctrl Pts',(-20.9964483203685,10.1760548270765,
0.));
#202806=CARTESIAN_POINT('Ctrl Pts',(-21.0095678414486,10.1873772669358,
0.));
#202807=CARTESIAN_POINT('Ctrl Pts',(-21.0227525451107,10.1988223040425,
0.));
#202808=CARTESIAN_POINT('Ctrl Pts',(-21.0360011306814,10.2103895734123,
0.));
#202809=CARTESIAN_POINT('Ctrl Pts',(-21.0493123187483,10.2220787139157,
0.));
#202810=CARTESIAN_POINT('Ctrl Pts',(-21.0626848505665,10.233889368157,0.));
#202811=CARTESIAN_POINT('Ctrl Pts',(-21.0761174875448,10.2458211823915,
0.));
#202812=CARTESIAN_POINT('Ctrl Pts',(-21.0896090107066,10.2578738064183,
0.));
#202813=CARTESIAN_POINT('Ctrl Pts',(-21.1031582201625,10.2700468934743,
0.));
#202814=CARTESIAN_POINT('Ctrl Pts',(-21.1167639345623,10.2823401001067,
0.));
#202815=CARTESIAN_POINT('Ctrl Pts',(-21.130424990599,10.2947530860714,0.));
#202816=CARTESIAN_POINT('Ctrl Pts',(-21.1441402425831,10.307285514268,0.));
#202817=CARTESIAN_POINT('Ctrl Pts',(-21.1579085619959,10.3199370506541,
0.));
#202818=CARTESIAN_POINT('Ctrl Pts',(-21.1717288370512,10.3327073641574,
0.));
#202819=CARTESIAN_POINT('Ctrl Pts',(-21.1855999722427,10.3455961265706,
0.));
#202820=CARTESIAN_POINT('Ctrl Pts',(-21.1995208879205,10.3586030124595,
0.));
#202821=CARTESIAN_POINT('Ctrl Pts',(-21.2134905199359,10.3717276991137,
0.));
#202822=CARTESIAN_POINT('Ctrl Pts',(-21.2275078192708,10.384969866479,0.));
#202823=CARTESIAN_POINT('Ctrl Pts',(-21.2415717516713,10.3983291970846,
0.));
#202824=CARTESIAN_POINT('Ctrl Pts',(-21.2556812972741,10.4118053759584,
0.));
#202825=CARTESIAN_POINT('Ctrl Pts',(-21.2698354502391,10.4253980905394,
0.));
#202826=CARTESIAN_POINT('Ctrl Pts',(-21.2840332184471,10.4391070306385,
0.));
#202827=CARTESIAN_POINT('Ctrl Pts',(-21.2982736231924,10.452931888387,0.));
#202828=CARTESIAN_POINT('Ctrl Pts',(-21.312555698873,10.4668723581768,0.));
#202829=CARTESIAN_POINT('Ctrl Pts',(-21.3268784926823,10.4809281365933,
0.));
#202830=CARTESIAN_POINT('Ctrl Pts',(-21.3412410642912,10.4950989223341,
0.));
#202831=CARTESIAN_POINT('Ctrl Pts',(-21.3556424855822,10.5093844161689,
0.));
#202832=CARTESIAN_POINT('Ctrl Pts',(-21.3700818403942,10.523784320906,0.));
#202833=CARTESIAN_POINT('Ctrl Pts',(-21.3845582242604,10.5382983413422,
0.));
#202834=CARTESIAN_POINT('Ctrl Pts',(-21.3990707441495,10.5529261842107,
0.));
#202835=CARTESIAN_POINT('Ctrl Pts',(-21.4136185181974,10.5676675581106,
0.));
#202836=CARTESIAN_POINT('Ctrl Pts',(-21.4282006754624,10.582522173457,0.));
#202837=CARTESIAN_POINT('Ctrl Pts',(-21.4428163557137,10.597489742462,0.));
#202838=CARTESIAN_POINT('Ctrl Pts',(-21.4574647092093,10.612569979096,0.));
#202839=CARTESIAN_POINT('Ctrl Pts',(-21.4721448964766,10.6277625990457,
0.));
#202840=CARTESIAN_POINT('Ctrl Pts',(-21.4868560880893,10.6430673196609,
0.));
#202841=CARTESIAN_POINT('Ctrl Pts',(-21.5015974644454,10.658483859894,0.));
#202842=CARTESIAN_POINT('Ctrl Pts',(-21.5163682155805,10.6740119402835,
0.));
#202843=CARTESIAN_POINT('Ctrl Pts',(-21.531167540981,10.689651282929,0.));
#202844=CARTESIAN_POINT('Ctrl Pts',(-21.5459946493955,10.7054016114571,
0.));
#202845=CARTESIAN_POINT('Ctrl Pts',(-21.5608487586467,10.7212626509816,
0.));
#202846=CARTESIAN_POINT('Ctrl Pts',(-21.5757290954372,10.7372341280468,
0.));
#202847=CARTESIAN_POINT('Ctrl Pts',(-21.5906348951745,10.7533157705943,
0.));
#202848=CARTESIAN_POINT('Ctrl Pts',(-21.6055654018179,10.7695073079554,
0.));
#202849=CARTESIAN_POINT('Ctrl Pts',(-21.6205198677176,10.7858084708262,
0.));
#202850=CARTESIAN_POINT('Ctrl Pts',(-21.6354975534557,10.8022189912369,
0.));
#202851=CARTESIAN_POINT('Ctrl Pts',(-21.6504977276864,10.8187386025135,
0.));
#202852=CARTESIAN_POINT('Ctrl Pts',(-21.6655196669727,10.835367039227,0.));
#202853=CARTESIAN_POINT('Ctrl Pts',(-21.6805626556461,10.8521040371832,
0.));
#202854=CARTESIAN_POINT('Ctrl Pts',(-21.6956259856667,10.8689493334093,
0.));
#202855=CARTESIAN_POINT('Ctrl Pts',(-21.7107089564822,10.8859026661292,
0.));
#202856=CARTESIAN_POINT('Ctrl Pts',(-21.7258108748874,10.9029637747341,
0.));
#202857=CARTESIAN_POINT('Ctrl Pts',(-21.74093105488,10.9201323997386,0.));
#202858=CARTESIAN_POINT('Ctrl Pts',(-21.7560688175252,10.9374082827446,
0.));
#202859=CARTESIAN_POINT('Ctrl Pts',(-21.7712234908468,10.9547911664457,
0.));
#202860=CARTESIAN_POINT('Ctrl Pts',(-21.7863944097143,10.9722807946157,
0.));
#202861=CARTESIAN_POINT('Ctrl Pts',(-21.8015809157302,10.9898769120913,
0.));
#202862=CARTESIAN_POINT('Ctrl Pts',(-21.8167823571168,11.0075792647477,
0.));
#202863=CARTESIAN_POINT('Ctrl Pts',(-21.8319980886033,11.0253875994598,
0.));
#202864=CARTESIAN_POINT('Ctrl Pts',(-21.8472274713103,11.0433016640808,
0.));
#202865=CARTESIAN_POINT('Ctrl Pts',(-21.8624698726319,11.0613212074364,
0.));
#202866=CARTESIAN_POINT('Ctrl Pts',(-21.8777246661191,11.0794459793058,
0.));
#202867=CARTESIAN_POINT('Ctrl Pts',(-21.8929912313608,11.0976757303944,
0.));
#202868=CARTESIAN_POINT('Ctrl Pts',(-21.9082689538687,11.1160102123024,
0.));
#202869=CARTESIAN_POINT('Ctrl Pts',(-21.9235572249518,11.134449177474,0.));
#202870=CARTESIAN_POINT('Ctrl Pts',(-21.9388554416437,11.1529923792002,
0.));
#202871=CARTESIAN_POINT('Ctrl Pts',(-21.9541630066504,11.1716395716375,
0.));
#202872=CARTESIAN_POINT('Ctrl Pts',(-21.9694793282913,11.1903905098109,
0.));
#202873=CARTESIAN_POINT('Ctrl Pts',(-21.9848038204439,11.2092449496125,
0.));
#202874=CARTESIAN_POINT('Ctrl Pts',(-22.0001359024839,11.2282026477897,
0.));
#202875=CARTESIAN_POINT('Ctrl Pts',(-22.0154749992364,11.2472633619276,
0.));
#202876=CARTESIAN_POINT('Ctrl Pts',(-22.0308205408351,11.2664268504207,
0.));
#202877=CARTESIAN_POINT('Ctrl Pts',(-22.046171962566,11.2856928724374,0.));
#202878=CARTESIAN_POINT('Ctrl Pts',(-22.0615287047179,11.3050611878771,
0.));
#202879=CARTESIAN_POINT('Ctrl Pts',(-22.0768902124267,11.3245315573168,
0.));
#202880=CARTESIAN_POINT('Ctrl Pts',(-22.0922559355293,11.3441037419553,
0.));
#202881=CARTESIAN_POINT('Ctrl Pts',(-22.1076253283978,11.3637775035367,
0.));
#202882=CARTESIAN_POINT('Ctrl Pts',(-22.1229978500185,11.3835526044256,
0.));
#202883=CARTESIAN_POINT('Ctrl Pts',(-22.1383729640963,11.4034288076908,
0.));
#202884=CARTESIAN_POINT('Ctrl Pts',(-22.1537501391486,11.4234058771742,
0.));
#202885=CARTESIAN_POINT('Ctrl Pts',(-22.1691288486096,11.443483577557,0.));
#202886=CARTESIAN_POINT('Ctrl Pts',(-22.184508570917,11.463661674411,0.));
#202887=CARTESIAN_POINT('Ctrl Pts',(-22.1998887896435,11.4839399342589,
0.));
#202888=CARTESIAN_POINT('Ctrl Pts',(-22.215268993102,11.504318124424,0.));
#202889=CARTESIAN_POINT('Ctrl Pts',(-22.2306486738899,11.5247960128476,
0.));
#202890=CARTESIAN_POINT('Ctrl Pts',(-22.2460273284653,11.545373367912,0.));
#202891=CARTESIAN_POINT('Ctrl Pts',(-22.2614044566898,11.5660499582403,
0.));
#202892=CARTESIAN_POINT('Ctrl Pts',(-22.2767795614349,11.5868255525189,
0.));
#202893=CARTESIAN_POINT('Ctrl Pts',(-22.2921521480358,11.6076999192359,
0.));
#202894=CARTESIAN_POINT('Ctrl Pts',(-22.3075217249049,11.6286728270011,
0.));
#202895=CARTESIAN_POINT('Ctrl Pts',(-22.3228878043976,11.6497440449858,
0.));
#202896=CARTESIAN_POINT('Ctrl Pts',(-22.3382499035618,11.6709133432986,
0.));
#202897=CARTESIAN_POINT('Ctrl Pts',(-22.3536075450028,11.6921804934056,
0.));
#202898=CARTESIAN_POINT('Ctrl Pts',(-22.3689602575492,11.7135452684532,
0.));
#202899=CARTESIAN_POINT('Ctrl Pts',(-22.3843075773905,11.7350074437961,
0.));
#202900=CARTESIAN_POINT('Ctrl Pts',(-22.39964904692,11.7565667964765,0.));
#202901=CARTESIAN_POINT('Ctrl Pts',(-22.4149842125018,11.7782231042041,
0.));
#202902=CARTESIAN_POINT('Ctrl Pts',(-22.4303126226468,11.7999761445175,
0.));
#202903=CARTESIAN_POINT('Ctrl Pts',(-22.4456338258738,11.8218256937889,
0.));
#202904=CARTESIAN_POINT('Ctrl Pts',(-22.4609473690469,11.8437715264487,
0.));
#202905=CARTESIAN_POINT('Ctrl Pts',(-22.4762527946694,11.8658134137018,
0.));
#202906=CARTESIAN_POINT('Ctrl Pts',(-22.4915496418472,11.8879511239941,
0.));
#202907=CARTESIAN_POINT('Ctrl Pts',(-22.5068374513958,11.9101844254555,
0.));
#202908=CARTESIAN_POINT('Ctrl Pts',(-22.5221157697869,11.9325130877801,
0.));
#202909=CARTESIAN_POINT('Ctrl Pts',(-22.5373841537299,11.9549368843996,
0.));
#202910=CARTESIAN_POINT('Ctrl Pts',(-22.5526421741159,11.9774555943496,
0.));
#202911=CARTESIAN_POINT('Ctrl Pts',(-22.5678894211194,12.0000690046697,
0.));
#202912=CARTESIAN_POINT('Ctrl Pts',(-22.5831255061306,12.0227769113132,
0.));
#202913=CARTESIAN_POINT('Ctrl Pts',(-22.5983500505675,12.0455791139135,
0.));
#202914=CARTESIAN_POINT('Ctrl Pts',(-22.613562676493,12.0684754113869,0.));
#202915=CARTESIAN_POINT('Ctrl Pts',(-22.628762996708,12.0914655972828,0.));
#202916=CARTESIAN_POINT('Ctrl Pts',(-22.6439506046611,12.1145494550384,
0.));
#202917=CARTESIAN_POINT('Ctrl Pts',(-22.6591250653942,12.1377267537141,
0.));
#202918=CARTESIAN_POINT('Ctrl Pts',(-22.6742859034891,12.1609972423088,
0.));
#202919=CARTESIAN_POINT('Ctrl Pts',(-22.6894326204959,12.1843606579246,
0.));
#202920=CARTESIAN_POINT('Ctrl Pts',(-22.7045647168659,12.2078167360267,
0.));
#202921=CARTESIAN_POINT('Ctrl Pts',(-22.7196817119299,12.2313652198047,
0.));
#202922=CARTESIAN_POINT('Ctrl Pts',(-22.7347831655251,12.2550058702389,
0.));
#202923=CARTESIAN_POINT('Ctrl Pts',(-22.7498686970096,12.2787384750747,
0.));
#202924=CARTESIAN_POINT('Ctrl Pts',(-22.7649380101154,12.3025628601812,
0.));
#202925=CARTESIAN_POINT('Ctrl Pts',(-22.7799908974947,12.3264788926108,
0.));
#202926=CARTESIAN_POINT('Ctrl Pts',(-22.7950272216959,12.3504864740361,
0.));
#202927=CARTESIAN_POINT('Ctrl Pts',(-22.8100469022632,12.3745855366772,
0.));
#202928=CARTESIAN_POINT('Ctrl Pts',(-22.8220493007353,12.393937937903,0.));
#202929=CARTESIAN_POINT('Ctrl Pts',(-22.8310435872852,12.4084933766366,
0.));
#202930=CARTESIAN_POINT('Ctrl Pts',(-22.8370364396497,12.4182152851867,
0.));
#202931=CARTESIAN_POINT('Ctrl Pts',(-22.8400320311648,12.4230808101438,
0.));
#202932=CARTESIAN_POINT('',(-22.8400320311648,12.4230808101438,0.));
#202933=CARTESIAN_POINT('Origin',(-16.3449727195352,13.9675290154577,0.));
#202934=CARTESIAN_POINT('',(-17.1452095830633,14.6513681262571,0.));
#202935=CARTESIAN_POINT('',(-17.1452095830633,14.6513681262571,0.));
#202936=CARTESIAN_POINT('',(-8.17248635976757,6.98376450772883,0.));
#202937=CARTESIAN_POINT('Ctrl Pts',(-22.1787195904339,13.5685075571671,
0.));
#202938=CARTESIAN_POINT('Ctrl Pts',(-22.1787195904339,13.5685075571671,
12.));
#202939=CARTESIAN_POINT('Ctrl Pts',(-22.1730081264583,13.5683460612913,
0.));
#202940=CARTESIAN_POINT('Ctrl Pts',(-22.1730081264583,13.5683460612913,
12.));
#202941=CARTESIAN_POINT('Ctrl Pts',(-22.1615922804939,13.5680170531724,
0.));
#202942=CARTESIAN_POINT('Ctrl Pts',(-22.1615922804939,13.5680170531724,
12.));
#202943=CARTESIAN_POINT('Ctrl Pts',(-22.1444897575076,13.5675054918922,
0.));
#202944=CARTESIAN_POINT('Ctrl Pts',(-22.1444897575076,13.5675054918922,
12.));
#202945=CARTESIAN_POINT('Ctrl Pts',(-22.1217288871823,13.5667873105179,
0.));
#202946=CARTESIAN_POINT('Ctrl Pts',(-22.1217288871823,13.5667873105179,
12.));
#202947=CARTESIAN_POINT('Ctrl Pts',(-22.0933486464442,13.5658294169106,
0.));
#202948=CARTESIAN_POINT('Ctrl Pts',(-22.0933486464442,13.5658294169106,
12.));
#202949=CARTESIAN_POINT('Ctrl Pts',(-22.0650393089492,13.5648113688894,
0.));
#202950=CARTESIAN_POINT('Ctrl Pts',(-22.0650393089492,13.5648113688894,
12.));
#202951=CARTESIAN_POINT('Ctrl Pts',(-22.0368009736227,13.5637332022393,
0.));
#202952=CARTESIAN_POINT('Ctrl Pts',(-22.0368009736227,13.5637332022393,
12.));
#202953=CARTESIAN_POINT('Ctrl Pts',(-22.0086337943431,13.5625949868313,
0.));
#202954=CARTESIAN_POINT('Ctrl Pts',(-22.0086337943431,13.5625949868313,
12.));
#202955=CARTESIAN_POINT('Ctrl Pts',(-21.9805379899192,13.5613968357589,
0.));
#202956=CARTESIAN_POINT('Ctrl Pts',(-21.9805379899192,13.5613968357589,
12.));
#202957=CARTESIAN_POINT('Ctrl Pts',(-21.9525138592862,13.5601389185315,
0.));
#202958=CARTESIAN_POINT('Ctrl Pts',(-21.9525138592862,13.5601389185315,
12.));
#202959=CARTESIAN_POINT('Ctrl Pts',(-21.9245617765827,13.5588214586672,
0.));
#202960=CARTESIAN_POINT('Ctrl Pts',(-21.9245617765827,13.5588214586672,
12.));
#202961=CARTESIAN_POINT('Ctrl Pts',(-21.8966821688876,13.5574447178484,
0.));
#202962=CARTESIAN_POINT('Ctrl Pts',(-21.8966821688876,13.5574447178484,
12.));
#202963=CARTESIAN_POINT('Ctrl Pts',(-21.8688754989401,13.5560089839426,
0.));
#202964=CARTESIAN_POINT('Ctrl Pts',(-21.8688754989401,13.5560089839426,
12.));
#202965=CARTESIAN_POINT('Ctrl Pts',(-21.841142245609,13.5545145573048,0.));
#202966=CARTESIAN_POINT('Ctrl Pts',(-21.841142245609,13.5545145573048,12.));
#202967=CARTESIAN_POINT('Ctrl Pts',(-21.8134828857963,13.5529617381569,
0.));
#202968=CARTESIAN_POINT('Ctrl Pts',(-21.8134828857963,13.5529617381569,
12.));
#202969=CARTESIAN_POINT('Ctrl Pts',(-21.7858978745848,13.5513508127232,
0.));
#202970=CARTESIAN_POINT('Ctrl Pts',(-21.7858978745848,13.5513508127232,
12.));
#202971=CARTESIAN_POINT('Ctrl Pts',(-21.7583876294532,13.5496820422186,
0.));
#202972=CARTESIAN_POINT('Ctrl Pts',(-21.7583876294532,13.5496820422186,
12.));
#202973=CARTESIAN_POINT('Ctrl Pts',(-21.730952541226,13.5479556704457,0.));
#202974=CARTESIAN_POINT('Ctrl Pts',(-21.730952541226,13.5479556704457,12.));
#202975=CARTESIAN_POINT('Ctrl Pts',(-21.7035929822939,13.546171929503,0.));
#202976=CARTESIAN_POINT('Ctrl Pts',(-21.7035929822939,13.546171929503,12.));
#202977=CARTESIAN_POINT('Ctrl Pts',(-21.676309315769,13.5443310461516,0.));
#202978=CARTESIAN_POINT('Ctrl Pts',(-21.676309315769,13.5443310461516,12.));
#202979=CARTESIAN_POINT('Ctrl Pts',(-21.6491019044647,13.5424332480698,
0.));
#202980=CARTESIAN_POINT('Ctrl Pts',(-21.6491019044647,13.5424332480698,
12.));
#202981=CARTESIAN_POINT('Ctrl Pts',(-21.6219711193951,13.5404787697798,
0.));
#202982=CARTESIAN_POINT('Ctrl Pts',(-21.6219711193951,13.5404787697798,
12.));
#202983=CARTESIAN_POINT('Ctrl Pts',(-21.5949173499022,13.5384678597206,
0.));
#202984=CARTESIAN_POINT('Ctrl Pts',(-21.5949173499022,13.5384678597206,
12.));
#202985=CARTESIAN_POINT('Ctrl Pts',(-21.5679410019011,13.5364007790292,
0.));
#202986=CARTESIAN_POINT('Ctrl Pts',(-21.5679410019011,13.5364007790292,
12.));
#202987=CARTESIAN_POINT('Ctrl Pts',(-21.5410424932511,13.5342777983225,
0.));
#202988=CARTESIAN_POINT('Ctrl Pts',(-21.5410424932511,13.5342777983225,
12.));
#202989=CARTESIAN_POINT('Ctrl Pts',(-21.5142222501671,13.5320991952145,
0.));
#202990=CARTESIAN_POINT('Ctrl Pts',(-21.5142222501671,13.5320991952145,
12.));
#202991=CARTESIAN_POINT('Ctrl Pts',(-21.487480703047,13.5298652514357,0.));
#202992=CARTESIAN_POINT('Ctrl Pts',(-21.487480703047,13.5298652514357,12.));
#202993=CARTESIAN_POINT('Ctrl Pts',(-21.4608182828695,13.5275762503553,
0.));
#202994=CARTESIAN_POINT('Ctrl Pts',(-21.4608182828695,13.5275762503553,
12.));
#202995=CARTESIAN_POINT('Ctrl Pts',(-21.4342354165254,13.5252324737795,
0.));
#202996=CARTESIAN_POINT('Ctrl Pts',(-21.4342354165254,13.5252324737795,
12.));
#202997=CARTESIAN_POINT('Ctrl Pts',(-21.4077325259318,13.5228342013508,
0.));
#202998=CARTESIAN_POINT('Ctrl Pts',(-21.4077325259318,13.5228342013508,
12.));
#202999=CARTESIAN_POINT('Ctrl Pts',(-21.3813100304967,13.5203817122496,
0.));
#203000=CARTESIAN_POINT('Ctrl Pts',(-21.3813100304967,13.5203817122496,
12.));
#203001=CARTESIAN_POINT('Ctrl Pts',(-21.3549683486219,13.5178752862461,
0.));
#203002=CARTESIAN_POINT('Ctrl Pts',(-21.3549683486219,13.5178752862461,
12.));
#203003=CARTESIAN_POINT('Ctrl Pts',(-21.328707899634,13.5153152050554,0.));
#203004=CARTESIAN_POINT('Ctrl Pts',(-21.328707899634,13.5153152050554,12.));
#203005=CARTESIAN_POINT('Ctrl Pts',(-21.3025291054236,13.5127017534972,
0.));
#203006=CARTESIAN_POINT('Ctrl Pts',(-21.3025291054236,13.5127017534972,
12.));
#203007=CARTESIAN_POINT('Ctrl Pts',(-21.2764323924442,13.5100352209207,
0.));
#203008=CARTESIAN_POINT('Ctrl Pts',(-21.2764323924442,13.5100352209207,
12.));
#203009=CARTESIAN_POINT('Ctrl Pts',(-21.2504181927429,13.5073159019454,
0.));
#203010=CARTESIAN_POINT('Ctrl Pts',(-21.2504181927429,13.5073159019454,
12.));
#203011=CARTESIAN_POINT('Ctrl Pts',(-21.224486942933,13.5045440957404,0.));
#203012=CARTESIAN_POINT('Ctrl Pts',(-21.224486942933,13.5045440957404,12.));
#203013=CARTESIAN_POINT('Ctrl Pts',(-21.1986390835825,13.5017201056088,
0.));
#203014=CARTESIAN_POINT('Ctrl Pts',(-21.1986390835825,13.5017201056088,
12.));
#203015=CARTESIAN_POINT('Ctrl Pts',(-21.1728750584173,13.4988442384491,
0.));
#203016=CARTESIAN_POINT('Ctrl Pts',(-21.1728750584173,13.4988442384491,
12.));
#203017=CARTESIAN_POINT('Ctrl Pts',(-21.1471953136209,13.4959168042934,
0.));
#203018=CARTESIAN_POINT('Ctrl Pts',(-21.1471953136209,13.4959168042934,
12.));
#203019=CARTESIAN_POINT('Ctrl Pts',(-21.1216002970209,13.4929381157778,
0.));
#203020=CARTESIAN_POINT('Ctrl Pts',(-21.1216002970209,13.4929381157778,
12.));
#203021=CARTESIAN_POINT('Ctrl Pts',(-21.0960904575048,13.4899084877718,
0.));
#203022=CARTESIAN_POINT('Ctrl Pts',(-21.0960904575048,13.4899084877718,
12.));
#203023=CARTESIAN_POINT('Ctrl Pts',(-21.0706662455202,13.4868282377191,
0.));
#203024=CARTESIAN_POINT('Ctrl Pts',(-21.0706662455202,13.4868282377191,
12.));
#203025=CARTESIAN_POINT('Ctrl Pts',(-21.0453281134247,13.4836976858912,
0.));
#203026=CARTESIAN_POINT('Ctrl Pts',(-21.0453281134247,13.4836976858912,
12.));
#203027=CARTESIAN_POINT('Ctrl Pts',(-21.0200765158885,13.4805171556822,
0.));
#203028=CARTESIAN_POINT('Ctrl Pts',(-21.0200765158885,13.4805171556822,
12.));
#203029=CARTESIAN_POINT('Ctrl Pts',(-20.9949119102592,13.4772869738879,
0.));
#203030=CARTESIAN_POINT('Ctrl Pts',(-20.9949119102592,13.4772869738879,
12.));
#203031=CARTESIAN_POINT('Ctrl Pts',(-20.9698347569476,13.4740074710087,
0.));
#203032=CARTESIAN_POINT('Ctrl Pts',(-20.9698347569476,13.4740074710087,
12.));
#203033=CARTESIAN_POINT('Ctrl Pts',(-20.9448455197557,13.4706789815166,
0.));
#203034=CARTESIAN_POINT('Ctrl Pts',(-20.9448455197557,13.4706789815166,
12.));
#203035=CARTESIAN_POINT('Ctrl Pts',(-20.9199446657584,13.4673018437718,
0.));
#203036=CARTESIAN_POINT('Ctrl Pts',(-20.9199446657584,13.4673018437718,
12.));
#203037=CARTESIAN_POINT('Ctrl Pts',(-20.8951326652158,13.4638763999725,
0.));
#203038=CARTESIAN_POINT('Ctrl Pts',(-20.8951326652158,13.4638763999725,
12.));
#203039=CARTESIAN_POINT('Ctrl Pts',(-20.8704099914641,13.4604029960983,
0.));
#203040=CARTESIAN_POINT('Ctrl Pts',(-20.8704099914641,13.4604029960983,
12.));
#203041=CARTESIAN_POINT('Ctrl Pts',(-20.8457771208082,13.4568819818631,
0.));
#203042=CARTESIAN_POINT('Ctrl Pts',(-20.8457771208082,13.4568819818631,
12.));
#203043=CARTESIAN_POINT('Ctrl Pts',(-20.821234532398,13.4533137106667,0.));
#203044=CARTESIAN_POINT('Ctrl Pts',(-20.821234532398,13.4533137106667,12.));
#203045=CARTESIAN_POINT('Ctrl Pts',(-20.7967827081227,13.4496985395637,
0.));
#203046=CARTESIAN_POINT('Ctrl Pts',(-20.7967827081227,13.4496985395637,
12.));
#203047=CARTESIAN_POINT('Ctrl Pts',(-20.7724221327608,13.4460368293688,
0.));
#203048=CARTESIAN_POINT('Ctrl Pts',(-20.7724221327608,13.4460368293688,
12.));
#203049=CARTESIAN_POINT('Ctrl Pts',(-20.7481532941013,13.4423289447561,
0.));
#203050=CARTESIAN_POINT('Ctrl Pts',(-20.7481532941013,13.4423289447561,
12.));
#203051=CARTESIAN_POINT('Ctrl Pts',(-20.7239766830675,13.4385752543663,
0.));
#203052=CARTESIAN_POINT('Ctrl Pts',(-20.7239766830675,13.4385752543663,
12.));
#203053=CARTESIAN_POINT('Ctrl Pts',(-20.6998927938288,13.4347761309154,
0.));
#203054=CARTESIAN_POINT('Ctrl Pts',(-20.6998927938288,13.4347761309154,
12.));
#203055=CARTESIAN_POINT('Ctrl Pts',(-20.6759021239103,13.4309319513119,
0.));
#203056=CARTESIAN_POINT('Ctrl Pts',(-20.6759021239103,13.4309319513119,
12.));
#203057=CARTESIAN_POINT('Ctrl Pts',(-20.6520051742869,13.4270430967651,
0.));
#203058=CARTESIAN_POINT('Ctrl Pts',(-20.6520051742869,13.4270430967651,
12.));
#203059=CARTESIAN_POINT('Ctrl Pts',(-20.6282024494237,13.4231099528179,
0.));
#203060=CARTESIAN_POINT('Ctrl Pts',(-20.6282024494237,13.4231099528179,
12.));
#203061=CARTESIAN_POINT('Ctrl Pts',(-20.6044944573153,13.4191329093932,
0.));
#203062=CARTESIAN_POINT('Ctrl Pts',(-20.6044944573153,13.4191329093932,
12.));
#203063=CARTESIAN_POINT('Ctrl Pts',(-20.5808817095155,13.4151123608411,
0.));
#203064=CARTESIAN_POINT('Ctrl Pts',(-20.5808817095155,13.4151123608411,
12.));
#203065=CARTESIAN_POINT('Ctrl Pts',(-20.5573647211639,13.4110487059912,
0.));
#203066=CARTESIAN_POINT('Ctrl Pts',(-20.5573647211639,13.4110487059912,
12.));
#203067=CARTESIAN_POINT('Ctrl Pts',(-20.5339440109956,13.4069423482076,
0.));
#203068=CARTESIAN_POINT('Ctrl Pts',(-20.5339440109956,13.4069423482076,
12.));
#203069=CARTESIAN_POINT('Ctrl Pts',(-20.5106201013753,13.4027936954529,
0.));
#203070=CARTESIAN_POINT('Ctrl Pts',(-20.5106201013753,13.4027936954529,
12.));
#203071=CARTESIAN_POINT('Ctrl Pts',(-20.487393518404,13.3986031603716,0.));
#203072=CARTESIAN_POINT('Ctrl Pts',(-20.487393518404,13.3986031603716,12.));
#203073=CARTESIAN_POINT('Ctrl Pts',(-20.4642647920038,13.3943711603739,
0.));
#203074=CARTESIAN_POINT('Ctrl Pts',(-20.4642647920038,13.3943711603739,
12.));
#203075=CARTESIAN_POINT('Ctrl Pts',(-20.4412344560008,13.3900981177255,
0.));
#203076=CARTESIAN_POINT('Ctrl Pts',(-20.4412344560008,13.3900981177255,
12.));
#203077=CARTESIAN_POINT('Ctrl Pts',(-20.4183030482002,13.3857844596387,
0.));
#203078=CARTESIAN_POINT('Ctrl Pts',(-20.4183030482002,13.3857844596387,
12.));
#203079=CARTESIAN_POINT('Ctrl Pts',(-20.3954711104502,13.3814306183719,
0.));
#203080=CARTESIAN_POINT('Ctrl Pts',(-20.3954711104502,13.3814306183719,
12.));
#203081=CARTESIAN_POINT('Ctrl Pts',(-20.3727391887184,13.3770370313188,
0.));
#203082=CARTESIAN_POINT('Ctrl Pts',(-20.3727391887184,13.3770370313188,
12.));
#203083=CARTESIAN_POINT('Ctrl Pts',(-20.3501078331814,13.3726041410867,
0.));
#203084=CARTESIAN_POINT('Ctrl Pts',(-20.3501078331814,13.3726041410867,
12.));
#203085=CARTESIAN_POINT('Ctrl Pts',(-20.3275775983029,13.3681323955826,
0.));
#203086=CARTESIAN_POINT('Ctrl Pts',(-20.3275775983029,13.3681323955826,
12.));
#203087=CARTESIAN_POINT('Ctrl Pts',(-20.3051490429048,13.3636222481016,
0.));
#203088=CARTESIAN_POINT('Ctrl Pts',(-20.3051490429048,13.3636222481016,
12.));
#203089=CARTESIAN_POINT('Ctrl Pts',(-20.2828227302339,13.3590741574195,
0.));
#203090=CARTESIAN_POINT('Ctrl Pts',(-20.2828227302339,13.3590741574195,
12.));
#203091=CARTESIAN_POINT('Ctrl Pts',(-20.2605992280122,13.3544885878889,
0.));
#203092=CARTESIAN_POINT('Ctrl Pts',(-20.2605992280122,13.3544885878889,
12.));
#203093=CARTESIAN_POINT('Ctrl Pts',(-20.2384791085359,13.3498660095386,
0.));
#203094=CARTESIAN_POINT('Ctrl Pts',(-20.2384791085359,13.3498660095386,
12.));
#203095=CARTESIAN_POINT('Ctrl Pts',(-20.216462948786,13.3452068981766,0.));
#203096=CARTESIAN_POINT('Ctrl Pts',(-20.216462948786,13.3452068981766,12.));
#203097=CARTESIAN_POINT('Ctrl Pts',(-20.1945513305235,13.3405117354971,
0.));
#203098=CARTESIAN_POINT('Ctrl Pts',(-20.1945513305235,13.3405117354971,
12.));
#203099=CARTESIAN_POINT('Ctrl Pts',(-20.1727448403817,13.3357810091903,
0.));
#203100=CARTESIAN_POINT('Ctrl Pts',(-20.1727448403817,13.3357810091903,
12.));
#203101=CARTESIAN_POINT('Ctrl Pts',(-20.1510440699474,13.3310152130564,
0.));
#203102=CARTESIAN_POINT('Ctrl Pts',(-20.1510440699474,13.3310152130564,
12.));
#203103=CARTESIAN_POINT('Ctrl Pts',(-20.1294496158402,13.3262148471226,
0.));
#203104=CARTESIAN_POINT('Ctrl Pts',(-20.1294496158402,13.3262148471226,
12.));
#203105=CARTESIAN_POINT('Ctrl Pts',(-20.1079620798375,13.3213804177587,
0.));
#203106=CARTESIAN_POINT('Ctrl Pts',(-20.1079620798375,13.3213804177587,
12.));
#203107=CARTESIAN_POINT('Ctrl Pts',(-20.0865820689883,13.3165124377962,
0.));
#203108=CARTESIAN_POINT('Ctrl Pts',(-20.0865820689883,13.3165124377962,
12.));
#203109=CARTESIAN_POINT('Ctrl Pts',(-20.0653101957188,13.3116114266515,
0.));
#203110=CARTESIAN_POINT('Ctrl Pts',(-20.0653101957188,13.3116114266515,
12.));
#203111=CARTESIAN_POINT('Ctrl Pts',(-20.0441470779345,13.3066779104515,
0.));
#203112=CARTESIAN_POINT('Ctrl Pts',(-20.0441470779345,13.3066779104515,
12.));
#203113=CARTESIAN_POINT('Ctrl Pts',(-20.0230933391038,13.3017124221637,
0.));
#203114=CARTESIAN_POINT('Ctrl Pts',(-20.0230933391038,13.3017124221637,
12.));
#203115=CARTESIAN_POINT('Ctrl Pts',(-20.0021496083738,13.2967155017306,
0.));
#203116=CARTESIAN_POINT('Ctrl Pts',(-20.0021496083738,13.2967155017306,
12.));
#203117=CARTESIAN_POINT('Ctrl Pts',(-19.981316520717,13.2916876962094,0.));
#203118=CARTESIAN_POINT('Ctrl Pts',(-19.981316520717,13.2916876962094,12.));
#203119=CARTESIAN_POINT('Ctrl Pts',(-19.9605947170586,13.286629559915,0.));
#203120=CARTESIAN_POINT('Ctrl Pts',(-19.9605947170586,13.286629559915,12.));
#203121=CARTESIAN_POINT('Ctrl Pts',(-19.9399848444019,13.2815416545663,
0.));
#203122=CARTESIAN_POINT('Ctrl Pts',(-19.9399848444019,13.2815416545663,
12.));
#203123=CARTESIAN_POINT('Ctrl Pts',(-19.9194875559422,13.2764245494357,
0.));
#203124=CARTESIAN_POINT('Ctrl Pts',(-19.9194875559422,13.2764245494357,
12.));
#203125=CARTESIAN_POINT('Ctrl Pts',(-19.8991035111745,13.271278821502,0.));
#203126=CARTESIAN_POINT('Ctrl Pts',(-19.8991035111745,13.271278821502,12.));
#203127=CARTESIAN_POINT('Ctrl Pts',(-19.8788333760577,13.2661050556132,
0.));
#203128=CARTESIAN_POINT('Ctrl Pts',(-19.8788333760577,13.2661050556132,
12.));
#203129=CARTESIAN_POINT('Ctrl Pts',(-19.8586778231715,13.2609038446529,
0.));
#203130=CARTESIAN_POINT('Ctrl Pts',(-19.8586778231715,13.2609038446529,
12.));
#203131=CARTESIAN_POINT('Ctrl Pts',(-19.8386375318634,13.2556757897086,
0.));
#203132=CARTESIAN_POINT('Ctrl Pts',(-19.8386375318634,13.2556757897086,
12.));
#203133=CARTESIAN_POINT('Ctrl Pts',(-19.8187131883917,13.2504215002457,
0.));
#203134=CARTESIAN_POINT('Ctrl Pts',(-19.8187131883917,13.2504215002457,
12.));
#203135=CARTESIAN_POINT('Ctrl Pts',(-19.7989054860495,13.2451415942805,
0.));
#203136=CARTESIAN_POINT('Ctrl Pts',(-19.7989054860495,13.2451415942805,
12.));
#203137=CARTESIAN_POINT('Ctrl Pts',(-19.7792151253289,13.2398366985675,
0.));
#203138=CARTESIAN_POINT('Ctrl Pts',(-19.7792151253289,13.2398366985675,
12.));
#203139=CARTESIAN_POINT('Ctrl Pts',(-19.7596428141168,13.2345074487963,
0.));
#203140=CARTESIAN_POINT('Ctrl Pts',(-19.7596428141168,13.2345074487963,
12.));
#203141=CARTESIAN_POINT('Ctrl Pts',(-19.7401892678697,13.2291544897899,
0.));
#203142=CARTESIAN_POINT('Ctrl Pts',(-19.7401892678697,13.2291544897899,
12.));
#203143=CARTESIAN_POINT('Ctrl Pts',(-19.7208552097868,13.2237784757065,
0.));
#203144=CARTESIAN_POINT('Ctrl Pts',(-19.7208552097868,13.2237784757065,
12.));
#203145=CARTESIAN_POINT('Ctrl Pts',(-19.7016413709685,13.2183800702436,
0.));
#203146=CARTESIAN_POINT('Ctrl Pts',(-19.7016413709685,13.2183800702436,
12.));
#203147=CARTESIAN_POINT('Ctrl Pts',(-19.6825484905823,13.2129599468485,
0.));
#203148=CARTESIAN_POINT('Ctrl Pts',(-19.6825484905823,13.2129599468485,
12.));
#203149=CARTESIAN_POINT('Ctrl Pts',(-19.6635773160936,13.2075187889529,
0.));
#203150=CARTESIAN_POINT('Ctrl Pts',(-19.6635773160936,13.2075187889529,
12.));
#203151=CARTESIAN_POINT('Ctrl Pts',(-19.6447286034772,13.2020572902065,
0.));
#203152=CARTESIAN_POINT('Ctrl Pts',(-19.6447286034772,13.2020572902065,
12.));
#203153=CARTESIAN_POINT('Ctrl Pts',(-19.6260031174244,13.1965761547151,
0.));
#203154=CARTESIAN_POINT('Ctrl Pts',(-19.6260031174244,13.1965761547151,
12.));
#203155=CARTESIAN_POINT('Ctrl Pts',(-19.6074016315414,13.1910760972814,
0.));
#203156=CARTESIAN_POINT('Ctrl Pts',(-19.6074016315414,13.1910760972814,
12.));
#203157=CARTESIAN_POINT('Ctrl Pts',(-19.5889249285338,13.1855578436471,
0.));
#203158=CARTESIAN_POINT('Ctrl Pts',(-19.5889249285338,13.1855578436471,
12.));
#203159=CARTESIAN_POINT('Ctrl Pts',(-19.5705738004667,13.1800221307673,
0.));
#203160=CARTESIAN_POINT('Ctrl Pts',(-19.5705738004667,13.1800221307673,
12.));
#203161=CARTESIAN_POINT('Ctrl Pts',(-19.5523490490244,13.1744697070911,
0.));
#203162=CARTESIAN_POINT('Ctrl Pts',(-19.5523490490244,13.1744697070911,
12.));
#203163=CARTESIAN_POINT('Ctrl Pts',(-19.5342514857562,13.168901332843,0.));
#203164=CARTESIAN_POINT('Ctrl Pts',(-19.5342514857562,13.168901332843,12.));
#203165=CARTESIAN_POINT('Ctrl Pts',(-19.5162819323213,13.1633177803101,
0.));
#203166=CARTESIAN_POINT('Ctrl Pts',(-19.5162819323213,13.1633177803101,
12.));
#203167=CARTESIAN_POINT('Ctrl Pts',(-19.4984412207082,13.1577198341245,
0.));
#203168=CARTESIAN_POINT('Ctrl Pts',(-19.4984412207082,13.1577198341245,
12.));
#203169=CARTESIAN_POINT('Ctrl Pts',(-19.4807301935268,13.1521082915853,
0.));
#203170=CARTESIAN_POINT('Ctrl Pts',(-19.4807301935268,13.1521082915853,
12.));
#203171=CARTESIAN_POINT('Ctrl Pts',(-19.4631497043258,13.1464839629971,
0.));
#203172=CARTESIAN_POINT('Ctrl Pts',(-19.4631497043258,13.1464839629971,
12.));
#203173=CARTESIAN_POINT('Ctrl Pts',(-19.4457006178876,13.1408476720061,
0.));
#203174=CARTESIAN_POINT('Ctrl Pts',(-19.4457006178876,13.1408476720061,
12.));
#203175=CARTESIAN_POINT('Ctrl Pts',(-19.4283838105262,13.1352002559438,
0.));
#203176=CARTESIAN_POINT('Ctrl Pts',(-19.4283838105262,13.1352002559438,
12.));
#203177=CARTESIAN_POINT('Ctrl Pts',(-19.4112001703557,13.1295425661634,
0.));
#203178=CARTESIAN_POINT('Ctrl Pts',(-19.4112001703557,13.1295425661634,
12.));
#203179=CARTESIAN_POINT('Ctrl Pts',(-19.3941505976263,13.1238754684177,
0.));
#203180=CARTESIAN_POINT('Ctrl Pts',(-19.3941505976263,13.1238754684177,
12.));
#203181=CARTESIAN_POINT('Ctrl Pts',(-19.3772360051091,13.118199843271,0.));
#203182=CARTESIAN_POINT('Ctrl Pts',(-19.3772360051091,13.118199843271,12.));
#203183=CARTESIAN_POINT('Ctrl Pts',(-19.3604573184515,13.1125165865022,
0.));
#203184=CARTESIAN_POINT('Ctrl Pts',(-19.3604573184515,13.1125165865022,
12.));
#203185=CARTESIAN_POINT('Ctrl Pts',(-19.3438154765395,13.1068266095186,
0.));
#203186=CARTESIAN_POINT('Ctrl Pts',(-19.3438154765395,13.1068266095186,
12.));
#203187=CARTESIAN_POINT('Ctrl Pts',(-19.3273114318269,13.1011308397591,
0.));
#203188=CARTESIAN_POINT('Ctrl Pts',(-19.3273114318269,13.1011308397591,
12.));
#203189=CARTESIAN_POINT('Ctrl Pts',(-19.310946150736,13.0954302211479,0.));
#203190=CARTESIAN_POINT('Ctrl Pts',(-19.310946150736,13.0954302211479,12.));
#203191=CARTESIAN_POINT('Ctrl Pts',(-19.2947206141247,13.0897257145968,
0.));
#203192=CARTESIAN_POINT('Ctrl Pts',(-19.2947206141247,13.0897257145968,
12.));
#203193=CARTESIAN_POINT('Ctrl Pts',(-19.2786358177198,13.0840182984949,
0.));
#203194=CARTESIAN_POINT('Ctrl Pts',(-19.2786358177198,13.0840182984949,
12.));
#203195=CARTESIAN_POINT('Ctrl Pts',(-19.2626927725596,13.0783089692118,
0.));
#203196=CARTESIAN_POINT('Ctrl Pts',(-19.2626927725596,13.0783089692118,
12.));
#203197=CARTESIAN_POINT('Ctrl Pts',(-19.2468925053989,13.0725987415859,
0.));
#203198=CARTESIAN_POINT('Ctrl Pts',(-19.2468925053989,13.0725987415859,
12.));
#203199=CARTESIAN_POINT('Ctrl Pts',(-19.2312360592033,13.0668886494795,
0.));
#203200=CARTESIAN_POINT('Ctrl Pts',(-19.2312360592033,13.0668886494795,
12.));
#203201=CARTESIAN_POINT('Ctrl Pts',(-19.2157244937142,13.0611797463915,
0.));
#203202=CARTESIAN_POINT('Ctrl Pts',(-19.2157244937142,13.0611797463915,
12.));
#203203=CARTESIAN_POINT('Ctrl Pts',(-19.2003588859772,13.0554731060538,
0.));
#203204=CARTESIAN_POINT('Ctrl Pts',(-19.2003588859772,13.0554731060538,
12.));
#203205=CARTESIAN_POINT('Ctrl Pts',(-19.1851403308825,13.0497698230441,
0.));
#203206=CARTESIAN_POINT('Ctrl Pts',(-19.1851403308825,13.0497698230441,
12.));
#203207=CARTESIAN_POINT('Ctrl Pts',(-19.1700699416622,13.0440710133772,
0.));
#203208=CARTESIAN_POINT('Ctrl Pts',(-19.1700699416622,13.0440710133772,
12.));
#203209=CARTESIAN_POINT('Ctrl Pts',(-19.155148850523,13.0383778152068,0.));
#203210=CARTESIAN_POINT('Ctrl Pts',(-19.155148850523,13.0383778152068,12.));
#203211=CARTESIAN_POINT('Ctrl Pts',(-19.1403782093386,13.0326913895838,
0.));
#203212=CARTESIAN_POINT('Ctrl Pts',(-19.1403782093386,13.0326913895838,
12.));
#203213=CARTESIAN_POINT('Ctrl Pts',(-19.1257591903099,13.0270129211976,
0.));
#203214=CARTESIAN_POINT('Ctrl Pts',(-19.1257591903099,13.0270129211976,
12.));
#203215=CARTESIAN_POINT('Ctrl Pts',(-19.111292986631,13.0213436191328,0.));
#203216=CARTESIAN_POINT('Ctrl Pts',(-19.111292986631,13.0213436191328,12.));
#203217=CARTESIAN_POINT('Ctrl Pts',(-19.0969808131228,13.0156847176096,
0.));
#203218=CARTESIAN_POINT('Ctrl Pts',(-19.0969808131228,13.0156847176096,
12.));
#203219=CARTESIAN_POINT('Ctrl Pts',(-19.0828239070484,13.0100374768788,
0.));
#203220=CARTESIAN_POINT('Ctrl Pts',(-19.0828239070484,13.0100374768788,
12.));
#203221=CARTESIAN_POINT('Ctrl Pts',(-19.0688235289437,13.0044031841382,
0.));
#203222=CARTESIAN_POINT('Ctrl Pts',(-19.0688235289437,13.0044031841382,
12.));
#203223=CARTESIAN_POINT('Ctrl Pts',(-19.0549809634354,12.9987831544502,
0.));
#203224=CARTESIAN_POINT('Ctrl Pts',(-19.0549809634354,12.9987831544502,
12.));
#203225=CARTESIAN_POINT('Ctrl Pts',(-19.0412975200398,12.9931787316514,
0.));
#203226=CARTESIAN_POINT('Ctrl Pts',(-19.0412975200398,12.9931787316514,
12.));
#203227=CARTESIAN_POINT('Ctrl Pts',(-19.0277745339909,12.9875912893003,
0.));
#203228=CARTESIAN_POINT('Ctrl Pts',(-19.0277745339909,12.9875912893003,
12.));
#203229=CARTESIAN_POINT('Ctrl Pts',(-19.014413367335,12.9820222318716,0.));
#203230=CARTESIAN_POINT('Ctrl Pts',(-19.014413367335,12.9820222318716,12.));
#203231=CARTESIAN_POINT('Ctrl Pts',(-19.0012154099792,12.9764729959206,
0.));
#203232=CARTESIAN_POINT('Ctrl Pts',(-19.0012154099792,12.9764729959206,
12.));
#203233=CARTESIAN_POINT('Ctrl Pts',(-18.9881820807585,12.9709450512747,
0.));
#203234=CARTESIAN_POINT('Ctrl Pts',(-18.9881820807585,12.9709450512747,
12.));
#203235=CARTESIAN_POINT('Ctrl Pts',(-18.9753148284473,12.9654399021868,
0.));
#203236=CARTESIAN_POINT('Ctrl Pts',(-18.9753148284473,12.9654399021868,
12.));
#203237=CARTESIAN_POINT('Ctrl Pts',(-18.9626151329226,12.9599590886317,
0.));
#203238=CARTESIAN_POINT('Ctrl Pts',(-18.9626151329226,12.9599590886317,
12.));
#203239=CARTESIAN_POINT('Ctrl Pts',(-18.9500845064714,12.9545041877377,
0.));
#203240=CARTESIAN_POINT('Ctrl Pts',(-18.9500845064714,12.9545041877377,
12.));
#203241=CARTESIAN_POINT('Ctrl Pts',(-18.9377244950435,12.9490768151821,
0.));
#203242=CARTESIAN_POINT('Ctrl Pts',(-18.9377244950435,12.9490768151821,
12.));
#203243=CARTESIAN_POINT('Ctrl Pts',(-18.9255366795196,12.9436786266106,
0.));
#203244=CARTESIAN_POINT('Ctrl Pts',(-18.9255366795196,12.9436786266106,
12.));
#203245=CARTESIAN_POINT('Ctrl Pts',(-18.9135226769466,12.9383113190375,
0.));
#203246=CARTESIAN_POINT('Ctrl Pts',(-18.9135226769466,12.9383113190375,
12.));
#203247=CARTESIAN_POINT('Ctrl Pts',(-18.9016841423402,12.9329766328184,
0.));
#203248=CARTESIAN_POINT('Ctrl Pts',(-18.9016841423402,12.9329766328184,
12.));
#203249=CARTESIAN_POINT('Ctrl Pts',(-18.8900227704888,12.9276763536372,
0.));
#203250=CARTESIAN_POINT('Ctrl Pts',(-18.8900227704888,12.9276763536372,
12.));
#203251=CARTESIAN_POINT('Ctrl Pts',(-18.8785402977528,12.9224123144982,
0.));
#203252=CARTESIAN_POINT('Ctrl Pts',(-18.8785402977528,12.9224123144982,
12.));
#203253=CARTESIAN_POINT('Ctrl Pts',(-18.8672385038328,12.9171863977047,
0.));
#203254=CARTESIAN_POINT('Ctrl Pts',(-18.8672385038328,12.9171863977047,
12.));
#203255=CARTESIAN_POINT('Ctrl Pts',(-18.8561192136201,12.9120005369066,
0.));
#203256=CARTESIAN_POINT('Ctrl Pts',(-18.8561192136201,12.9120005369066,
12.));
#203257=CARTESIAN_POINT('Ctrl Pts',(-18.8451842990986,12.9068567191856,
0.));
#203258=CARTESIAN_POINT('Ctrl Pts',(-18.8451842990986,12.9068567191856,
12.));
#203259=CARTESIAN_POINT('Ctrl Pts',(-18.834435681259,12.9017569871738,0.));
#203260=CARTESIAN_POINT('Ctrl Pts',(-18.834435681259,12.9017569871738,12.));
#203261=CARTESIAN_POINT('Ctrl Pts',(-18.8238753319124,12.8967034410752,
0.));
#203262=CARTESIAN_POINT('Ctrl Pts',(-18.8238753319124,12.8967034410752,
12.));
#203263=CARTESIAN_POINT('Ctrl Pts',(-18.8135052757815,12.8916982409931,
0.));
#203264=CARTESIAN_POINT('Ctrl Pts',(-18.8135052757815,12.8916982409931,
12.));
#203265=CARTESIAN_POINT('Ctrl Pts',(-18.8033275941939,12.8867436109543,
0.));
#203266=CARTESIAN_POINT('Ctrl Pts',(-18.8033275941939,12.8867436109543,
12.));
#203267=CARTESIAN_POINT('Ctrl Pts',(-18.7933444285867,12.8818418427474,
0.));
#203268=CARTESIAN_POINT('Ctrl Pts',(-18.7933444285867,12.8818418427474,
12.));
#203269=CARTESIAN_POINT('Ctrl Pts',(-18.7835579840481,12.8769952998097,
0.));
#203270=CARTESIAN_POINT('Ctrl Pts',(-18.7835579840481,12.8769952998097,
12.));
#203271=CARTESIAN_POINT('Ctrl Pts',(-18.7739705329029,12.8722064211814,
0.));
#203272=CARTESIAN_POINT('Ctrl Pts',(-18.7739705329029,12.8722064211814,
12.));
#203273=CARTESIAN_POINT('Ctrl Pts',(-18.7645844169568,12.8674777239656,
0.));
#203274=CARTESIAN_POINT('Ctrl Pts',(-18.7645844169568,12.8674777239656,
12.));
#203275=CARTESIAN_POINT('Ctrl Pts',(-18.7554020493888,12.8628118054172,
0.));
#203276=CARTESIAN_POINT('Ctrl Pts',(-18.7554020493888,12.8628118054172,
12.));
#203277=CARTESIAN_POINT('Ctrl Pts',(-18.7464259171248,12.8582113455644,
0.));
#203278=CARTESIAN_POINT('Ctrl Pts',(-18.7464259171248,12.8582113455644,
12.));
#203279=CARTESIAN_POINT('Ctrl Pts',(-18.7376585820851,12.8536791086315,
0.));
#203280=CARTESIAN_POINT('Ctrl Pts',(-18.7376585820851,12.8536791086315,
12.));
#203281=CARTESIAN_POINT('Ctrl Pts',(-18.7291026886552,12.849217951159,0.));
#203282=CARTESIAN_POINT('Ctrl Pts',(-18.7291026886552,12.849217951159,12.));
#203283=CARTESIAN_POINT('Ctrl Pts',(-18.7207609737701,12.8448308329494,
0.));
#203284=CARTESIAN_POINT('Ctrl Pts',(-18.7207609737701,12.8448308329494,
12.));
#203285=CARTESIAN_POINT('Ctrl Pts',(-18.7126362754446,12.8405208263432,
0.));
#203286=CARTESIAN_POINT('Ctrl Pts',(-18.7126362754446,12.8405208263432,
12.));
#203287=CARTESIAN_POINT('Ctrl Pts',(-18.7047315436296,12.8362911280362,
0.));
#203288=CARTESIAN_POINT('Ctrl Pts',(-18.7047315436296,12.8362911280362,
12.));
#203289=CARTESIAN_POINT('Ctrl Pts',(-18.6970498410173,12.832145059979,0.));
#203290=CARTESIAN_POINT('Ctrl Pts',(-18.6970498410173,12.832145059979,12.));
#203291=CARTESIAN_POINT('Ctrl Pts',(-18.6895943376172,12.8280860635231,
0.));
#203292=CARTESIAN_POINT('Ctrl Pts',(-18.6895943376172,12.8280860635231,
12.));
#203293=CARTESIAN_POINT('Ctrl Pts',(-18.6823683094139,12.8241176980016,
0.));
#203294=CARTESIAN_POINT('Ctrl Pts',(-18.6823683094139,12.8241176980016,
12.));
#203295=CARTESIAN_POINT('Ctrl Pts',(-18.6753751301091,12.8202436318473,
0.));
#203296=CARTESIAN_POINT('Ctrl Pts',(-18.6753751301091,12.8202436318473,
12.));
#203297=CARTESIAN_POINT('Ctrl Pts',(-18.6686182952798,12.8164676687361,
0.));
#203298=CARTESIAN_POINT('Ctrl Pts',(-18.6686182952798,12.8164676687361,
12.));
#203299=CARTESIAN_POINT('Ctrl Pts',(-18.6621014624746,12.8127937909632,
0.));
#203300=CARTESIAN_POINT('Ctrl Pts',(-18.6621014624746,12.8127937909632,
12.));
#203301=CARTESIAN_POINT('Ctrl Pts',(-18.6558284825772,12.8092261933858,
0.));
#203302=CARTESIAN_POINT('Ctrl Pts',(-18.6558284825772,12.8092261933858,
12.));
#203303=CARTESIAN_POINT('Ctrl Pts',(-18.6498034438986,12.805769331162,0.));
#203304=CARTESIAN_POINT('Ctrl Pts',(-18.6498034438986,12.805769331162,12.));
#203305=CARTESIAN_POINT('Ctrl Pts',(-18.6440306327457,12.8024278770153,
0.));
#203306=CARTESIAN_POINT('Ctrl Pts',(-18.6440306327457,12.8024278770153,
12.));
#203307=CARTESIAN_POINT('Ctrl Pts',(-18.63851447924,12.7992066625264,0.));
#203308=CARTESIAN_POINT('Ctrl Pts',(-18.63851447924,12.7992066625264,12.));
#203309=CARTESIAN_POINT('Ctrl Pts',(-18.6332595057005,12.7961106222251,
0.));
#203310=CARTESIAN_POINT('Ctrl Pts',(-18.6332595057005,12.7961106222251,
12.));
#203311=CARTESIAN_POINT('Ctrl Pts',(-18.6282702819371,12.7931447451556,
0.));
#203312=CARTESIAN_POINT('Ctrl Pts',(-18.6282702819371,12.7931447451556,
12.));
#203313=CARTESIAN_POINT('Ctrl Pts',(-18.6235516265575,12.7903142925234,
0.));
#203314=CARTESIAN_POINT('Ctrl Pts',(-18.6235516265575,12.7903142925234,
12.));
#203315=CARTESIAN_POINT('Ctrl Pts',(-18.6191087624752,12.7876249657834,
0.));
#203316=CARTESIAN_POINT('Ctrl Pts',(-18.6191087624752,12.7876249657834,
12.));
#203317=CARTESIAN_POINT('Ctrl Pts',(-18.6149475565189,12.78508316579,0.));
#203318=CARTESIAN_POINT('Ctrl Pts',(-18.6149475565189,12.78508316579,12.));
#203319=CARTESIAN_POINT('Ctrl Pts',(-18.611074482622,12.7826959526924,0.));
#203320=CARTESIAN_POINT('Ctrl Pts',(-18.611074482622,12.7826959526924,12.));
#203321=CARTESIAN_POINT('Ctrl Pts',(-18.6074961535723,12.7804705387658,
0.));
#203322=CARTESIAN_POINT('Ctrl Pts',(-18.6074961535723,12.7804705387658,
12.));
#203323=CARTESIAN_POINT('Ctrl Pts',(-18.6042190183703,12.7784139605067,
0.));
#203324=CARTESIAN_POINT('Ctrl Pts',(-18.6042190183703,12.7784139605067,
12.));
#203325=CARTESIAN_POINT('Ctrl Pts',(-18.6012488486708,12.7765325225082,
0.));
#203326=CARTESIAN_POINT('Ctrl Pts',(-18.6012488486708,12.7765325225082,
12.));
#203327=CARTESIAN_POINT('Ctrl Pts',(-18.5985917525949,12.7748328937639,
0.));
#203328=CARTESIAN_POINT('Ctrl Pts',(-18.5985917525949,12.7748328937639,
12.));
#203329=CARTESIAN_POINT('Ctrl Pts',(-18.5962551167772,12.7733231262107,
0.));
#203330=CARTESIAN_POINT('Ctrl Pts',(-18.5962551167772,12.7733231262107,
12.));
#203331=CARTESIAN_POINT('Ctrl Pts',(-18.5942490615409,12.7720142287169,
0.));
#203332=CARTESIAN_POINT('Ctrl Pts',(-18.5942490615409,12.7720142287169,
12.));
#203333=CARTESIAN_POINT('Ctrl Pts',(-18.5925859134582,12.7709195951153,
0.));
#203334=CARTESIAN_POINT('Ctrl Pts',(-18.5925859134582,12.7709195951153,
12.));
#203335=CARTESIAN_POINT('Ctrl Pts',(-18.5912775137806,12.7700520897174,
0.));
#203336=CARTESIAN_POINT('Ctrl Pts',(-18.5912775137806,12.7700520897174,
12.));
#203337=CARTESIAN_POINT('Ctrl Pts',(-18.590332877722,12.7694215127923,0.));
#203338=CARTESIAN_POINT('Ctrl Pts',(-18.590332877722,12.7694215127923,12.));
#203339=CARTESIAN_POINT('Ctrl Pts',(-18.589871621842,12.7691103481996,0.));
#203340=CARTESIAN_POINT('Ctrl Pts',(-18.589871621842,12.7691103481996,12.));
#203341=CARTESIAN_POINT('Ctrl Pts',(-18.5896919669158,12.7689864266924,
0.));
#203342=CARTESIAN_POINT('Ctrl Pts',(-18.5896919669158,12.7689864266924,
12.));
#203343=CARTESIAN_POINT('Ctrl Pts',(-18.5896460962961,12.7689524524484,
0.));
#203344=CARTESIAN_POINT('Ctrl Pts',(-18.5896460962961,12.7689524524484,
12.));
#203345=CARTESIAN_POINT('Ctrl Pts',(-18.5896416359912,12.7689476255363,
0.));
#203346=CARTESIAN_POINT('Ctrl Pts',(-18.5896416359912,12.7689476255363,
12.));
#203347=CARTESIAN_POINT('',(-22.1787195904339,13.5685075571671,0.));
#203348=CARTESIAN_POINT('Ctrl Pts',(-22.1787195904339,13.5685075571671,
0.));
#203349=CARTESIAN_POINT('Ctrl Pts',(-22.1730081264583,13.5683460612913,
0.));
#203350=CARTESIAN_POINT('Ctrl Pts',(-22.1615922804939,13.5680170531724,
0.));
#203351=CARTESIAN_POINT('Ctrl Pts',(-22.1444897575076,13.5675054918922,
0.));
#203352=CARTESIAN_POINT('Ctrl Pts',(-22.1217288871823,13.5667873105179,
0.));
#203353=CARTESIAN_POINT('Ctrl Pts',(-22.0933486464442,13.5658294169106,
0.));
#203354=CARTESIAN_POINT('Ctrl Pts',(-22.0650393089492,13.5648113688894,
0.));
#203355=CARTESIAN_POINT('Ctrl Pts',(-22.0368009736227,13.5637332022393,
0.));
#203356=CARTESIAN_POINT('Ctrl Pts',(-22.0086337943431,13.5625949868313,
0.));
#203357=CARTESIAN_POINT('Ctrl Pts',(-21.9805379899192,13.5613968357589,
0.));
#203358=CARTESIAN_POINT('Ctrl Pts',(-21.9525138592862,13.5601389185315,
0.));
#203359=CARTESIAN_POINT('Ctrl Pts',(-21.9245617765827,13.5588214586672,
0.));
#203360=CARTESIAN_POINT('Ctrl Pts',(-21.8966821688876,13.5574447178484,
0.));
#203361=CARTESIAN_POINT('Ctrl Pts',(-21.8688754989401,13.5560089839426,
0.));
#203362=CARTESIAN_POINT('Ctrl Pts',(-21.841142245609,13.5545145573048,0.));
#203363=CARTESIAN_POINT('Ctrl Pts',(-21.8134828857963,13.5529617381569,
0.));
#203364=CARTESIAN_POINT('Ctrl Pts',(-21.7858978745848,13.5513508127232,
0.));
#203365=CARTESIAN_POINT('Ctrl Pts',(-21.7583876294532,13.5496820422186,
0.));
#203366=CARTESIAN_POINT('Ctrl Pts',(-21.730952541226,13.5479556704457,0.));
#203367=CARTESIAN_POINT('Ctrl Pts',(-21.7035929822939,13.546171929503,0.));
#203368=CARTESIAN_POINT('Ctrl Pts',(-21.676309315769,13.5443310461516,0.));
#203369=CARTESIAN_POINT('Ctrl Pts',(-21.6491019044647,13.5424332480698,
0.));
#203370=CARTESIAN_POINT('Ctrl Pts',(-21.6219711193951,13.5404787697798,
0.));
#203371=CARTESIAN_POINT('Ctrl Pts',(-21.5949173499022,13.5384678597206,
0.));
#203372=CARTESIAN_POINT('Ctrl Pts',(-21.5679410019011,13.5364007790292,
0.));
#203373=CARTESIAN_POINT('Ctrl Pts',(-21.5410424932511,13.5342777983225,
0.));
#203374=CARTESIAN_POINT('Ctrl Pts',(-21.5142222501671,13.5320991952145,
0.));
#203375=CARTESIAN_POINT('Ctrl Pts',(-21.487480703047,13.5298652514357,0.));
#203376=CARTESIAN_POINT('Ctrl Pts',(-21.4608182828695,13.5275762503553,
0.));
#203377=CARTESIAN_POINT('Ctrl Pts',(-21.4342354165254,13.5252324737795,
0.));
#203378=CARTESIAN_POINT('Ctrl Pts',(-21.4077325259318,13.5228342013508,
0.));
#203379=CARTESIAN_POINT('Ctrl Pts',(-21.3813100304967,13.5203817122496,
0.));
#203380=CARTESIAN_POINT('Ctrl Pts',(-21.3549683486219,13.5178752862461,
0.));
#203381=CARTESIAN_POINT('Ctrl Pts',(-21.328707899634,13.5153152050554,0.));
#203382=CARTESIAN_POINT('Ctrl Pts',(-21.3025291054236,13.5127017534972,
0.));
#203383=CARTESIAN_POINT('Ctrl Pts',(-21.2764323924442,13.5100352209207,
0.));
#203384=CARTESIAN_POINT('Ctrl Pts',(-21.2504181927429,13.5073159019454,
0.));
#203385=CARTESIAN_POINT('Ctrl Pts',(-21.224486942933,13.5045440957404,0.));
#203386=CARTESIAN_POINT('Ctrl Pts',(-21.1986390835825,13.5017201056088,
0.));
#203387=CARTESIAN_POINT('Ctrl Pts',(-21.1728750584173,13.4988442384491,
0.));
#203388=CARTESIAN_POINT('Ctrl Pts',(-21.1471953136209,13.4959168042934,
0.));
#203389=CARTESIAN_POINT('Ctrl Pts',(-21.1216002970209,13.4929381157778,
0.));
#203390=CARTESIAN_POINT('Ctrl Pts',(-21.0960904575048,13.4899084877718,
0.));
#203391=CARTESIAN_POINT('Ctrl Pts',(-21.0706662455202,13.4868282377191,
0.));
#203392=CARTESIAN_POINT('Ctrl Pts',(-21.0453281134247,13.4836976858912,
0.));
#203393=CARTESIAN_POINT('Ctrl Pts',(-21.0200765158885,13.4805171556822,
0.));
#203394=CARTESIAN_POINT('Ctrl Pts',(-20.9949119102592,13.4772869738879,
0.));
#203395=CARTESIAN_POINT('Ctrl Pts',(-20.9698347569476,13.4740074710087,
0.));
#203396=CARTESIAN_POINT('Ctrl Pts',(-20.9448455197557,13.4706789815166,
0.));
#203397=CARTESIAN_POINT('Ctrl Pts',(-20.9199446657584,13.4673018437718,
0.));
#203398=CARTESIAN_POINT('Ctrl Pts',(-20.8951326652158,13.4638763999725,
0.));
#203399=CARTESIAN_POINT('Ctrl Pts',(-20.8704099914641,13.4604029960983,
0.));
#203400=CARTESIAN_POINT('Ctrl Pts',(-20.8457771208082,13.4568819818631,
0.));
#203401=CARTESIAN_POINT('Ctrl Pts',(-20.821234532398,13.4533137106667,0.));
#203402=CARTESIAN_POINT('Ctrl Pts',(-20.7967827081227,13.4496985395637,
0.));
#203403=CARTESIAN_POINT('Ctrl Pts',(-20.7724221327608,13.4460368293688,
0.));
#203404=CARTESIAN_POINT('Ctrl Pts',(-20.7481532941013,13.4423289447561,
0.));
#203405=CARTESIAN_POINT('Ctrl Pts',(-20.7239766830675,13.4385752543663,
0.));
#203406=CARTESIAN_POINT('Ctrl Pts',(-20.6998927938288,13.4347761309154,
0.));
#203407=CARTESIAN_POINT('Ctrl Pts',(-20.6759021239103,13.4309319513119,
0.));
#203408=CARTESIAN_POINT('Ctrl Pts',(-20.6520051742869,13.4270430967651,
0.));
#203409=CARTESIAN_POINT('Ctrl Pts',(-20.6282024494237,13.4231099528179,
0.));
#203410=CARTESIAN_POINT('Ctrl Pts',(-20.6044944573153,13.4191329093932,
0.));
#203411=CARTESIAN_POINT('Ctrl Pts',(-20.5808817095155,13.4151123608411,
0.));
#203412=CARTESIAN_POINT('Ctrl Pts',(-20.5573647211639,13.4110487059912,
0.));
#203413=CARTESIAN_POINT('Ctrl Pts',(-20.5339440109956,13.4069423482076,
0.));
#203414=CARTESIAN_POINT('Ctrl Pts',(-20.5106201013753,13.4027936954529,
0.));
#203415=CARTESIAN_POINT('Ctrl Pts',(-20.487393518404,13.3986031603716,0.));
#203416=CARTESIAN_POINT('Ctrl Pts',(-20.4642647920038,13.3943711603739,
0.));
#203417=CARTESIAN_POINT('Ctrl Pts',(-20.4412344560008,13.3900981177255,
0.));
#203418=CARTESIAN_POINT('Ctrl Pts',(-20.4183030482002,13.3857844596387,
0.));
#203419=CARTESIAN_POINT('Ctrl Pts',(-20.3954711104502,13.3814306183719,
0.));
#203420=CARTESIAN_POINT('Ctrl Pts',(-20.3727391887184,13.3770370313188,
0.));
#203421=CARTESIAN_POINT('Ctrl Pts',(-20.3501078331814,13.3726041410867,
0.));
#203422=CARTESIAN_POINT('Ctrl Pts',(-20.3275775983029,13.3681323955826,
0.));
#203423=CARTESIAN_POINT('Ctrl Pts',(-20.3051490429048,13.3636222481016,
0.));
#203424=CARTESIAN_POINT('Ctrl Pts',(-20.2828227302339,13.3590741574195,
0.));
#203425=CARTESIAN_POINT('Ctrl Pts',(-20.2605992280122,13.3544885878889,
0.));
#203426=CARTESIAN_POINT('Ctrl Pts',(-20.2384791085359,13.3498660095386,
0.));
#203427=CARTESIAN_POINT('Ctrl Pts',(-20.216462948786,13.3452068981766,0.));
#203428=CARTESIAN_POINT('Ctrl Pts',(-20.1945513305235,13.3405117354971,
0.));
#203429=CARTESIAN_POINT('Ctrl Pts',(-20.1727448403817,13.3357810091903,
0.));
#203430=CARTESIAN_POINT('Ctrl Pts',(-20.1510440699474,13.3310152130564,
0.));
#203431=CARTESIAN_POINT('Ctrl Pts',(-20.1294496158402,13.3262148471226,
0.));
#203432=CARTESIAN_POINT('Ctrl Pts',(-20.1079620798375,13.3213804177587,
0.));
#203433=CARTESIAN_POINT('Ctrl Pts',(-20.0865820689883,13.3165124377962,
0.));
#203434=CARTESIAN_POINT('Ctrl Pts',(-20.0653101957188,13.3116114266515,
0.));
#203435=CARTESIAN_POINT('Ctrl Pts',(-20.0441470779345,13.3066779104515,
0.));
#203436=CARTESIAN_POINT('Ctrl Pts',(-20.0230933391038,13.3017124221637,
0.));
#203437=CARTESIAN_POINT('Ctrl Pts',(-20.0021496083738,13.2967155017306,
0.));
#203438=CARTESIAN_POINT('Ctrl Pts',(-19.981316520717,13.2916876962094,0.));
#203439=CARTESIAN_POINT('Ctrl Pts',(-19.9605947170586,13.286629559915,0.));
#203440=CARTESIAN_POINT('Ctrl Pts',(-19.9399848444019,13.2815416545663,
0.));
#203441=CARTESIAN_POINT('Ctrl Pts',(-19.9194875559422,13.2764245494357,
0.));
#203442=CARTESIAN_POINT('Ctrl Pts',(-19.8991035111745,13.271278821502,0.));
#203443=CARTESIAN_POINT('Ctrl Pts',(-19.8788333760577,13.2661050556132,
0.));
#203444=CARTESIAN_POINT('Ctrl Pts',(-19.8586778231715,13.2609038446529,
0.));
#203445=CARTESIAN_POINT('Ctrl Pts',(-19.8386375318634,13.2556757897086,
0.));
#203446=CARTESIAN_POINT('Ctrl Pts',(-19.8187131883917,13.2504215002457,
0.));
#203447=CARTESIAN_POINT('Ctrl Pts',(-19.7989054860495,13.2451415942805,
0.));
#203448=CARTESIAN_POINT('Ctrl Pts',(-19.7792151253289,13.2398366985675,
0.));
#203449=CARTESIAN_POINT('Ctrl Pts',(-19.7596428141168,13.2345074487963,
0.));
#203450=CARTESIAN_POINT('Ctrl Pts',(-19.7401892678697,13.2291544897899,
0.));
#203451=CARTESIAN_POINT('Ctrl Pts',(-19.7208552097868,13.2237784757065,
0.));
#203452=CARTESIAN_POINT('Ctrl Pts',(-19.7016413709685,13.2183800702436,
0.));
#203453=CARTESIAN_POINT('Ctrl Pts',(-19.6825484905823,13.2129599468485,
0.));
#203454=CARTESIAN_POINT('Ctrl Pts',(-19.6635773160936,13.2075187889529,
0.));
#203455=CARTESIAN_POINT('Ctrl Pts',(-19.6447286034772,13.2020572902065,
0.));
#203456=CARTESIAN_POINT('Ctrl Pts',(-19.6260031174244,13.1965761547151,
0.));
#203457=CARTESIAN_POINT('Ctrl Pts',(-19.6074016315414,13.1910760972814,
0.));
#203458=CARTESIAN_POINT('Ctrl Pts',(-19.5889249285338,13.1855578436471,
0.));
#203459=CARTESIAN_POINT('Ctrl Pts',(-19.5705738004667,13.1800221307673,
0.));
#203460=CARTESIAN_POINT('Ctrl Pts',(-19.5523490490244,13.1744697070911,
0.));
#203461=CARTESIAN_POINT('Ctrl Pts',(-19.5342514857562,13.168901332843,0.));
#203462=CARTESIAN_POINT('Ctrl Pts',(-19.5162819323213,13.1633177803101,
0.));
#203463=CARTESIAN_POINT('Ctrl Pts',(-19.4984412207082,13.1577198341245,
0.));
#203464=CARTESIAN_POINT('Ctrl Pts',(-19.4807301935268,13.1521082915853,
0.));
#203465=CARTESIAN_POINT('Ctrl Pts',(-19.4631497043258,13.1464839629971,
0.));
#203466=CARTESIAN_POINT('Ctrl Pts',(-19.4457006178876,13.1408476720061,
0.));
#203467=CARTESIAN_POINT('Ctrl Pts',(-19.4283838105262,13.1352002559438,
0.));
#203468=CARTESIAN_POINT('Ctrl Pts',(-19.4112001703557,13.1295425661634,
0.));
#203469=CARTESIAN_POINT('Ctrl Pts',(-19.3941505976263,13.1238754684177,
0.));
#203470=CARTESIAN_POINT('Ctrl Pts',(-19.3772360051091,13.118199843271,0.));
#203471=CARTESIAN_POINT('Ctrl Pts',(-19.3604573184515,13.1125165865022,
0.));
#203472=CARTESIAN_POINT('Ctrl Pts',(-19.3438154765395,13.1068266095186,
0.));
#203473=CARTESIAN_POINT('Ctrl Pts',(-19.3273114318269,13.1011308397591,
0.));
#203474=CARTESIAN_POINT('Ctrl Pts',(-19.310946150736,13.0954302211479,0.));
#203475=CARTESIAN_POINT('Ctrl Pts',(-19.2947206141247,13.0897257145968,
0.));
#203476=CARTESIAN_POINT('Ctrl Pts',(-19.2786358177198,13.0840182984949,
0.));
#203477=CARTESIAN_POINT('Ctrl Pts',(-19.2626927725596,13.0783089692118,
0.));
#203478=CARTESIAN_POINT('Ctrl Pts',(-19.2468925053989,13.0725987415859,
0.));
#203479=CARTESIAN_POINT('Ctrl Pts',(-19.2312360592033,13.0668886494795,
0.));
#203480=CARTESIAN_POINT('Ctrl Pts',(-19.2157244937142,13.0611797463915,
0.));
#203481=CARTESIAN_POINT('Ctrl Pts',(-19.2003588859772,13.0554731060538,
0.));
#203482=CARTESIAN_POINT('Ctrl Pts',(-19.1851403308825,13.0497698230441,
0.));
#203483=CARTESIAN_POINT('Ctrl Pts',(-19.1700699416622,13.0440710133772,
0.));
#203484=CARTESIAN_POINT('Ctrl Pts',(-19.155148850523,13.0383778152068,0.));
#203485=CARTESIAN_POINT('Ctrl Pts',(-19.1403782093386,13.0326913895838,
0.));
#203486=CARTESIAN_POINT('Ctrl Pts',(-19.1257591903099,13.0270129211976,
0.));
#203487=CARTESIAN_POINT('Ctrl Pts',(-19.111292986631,13.0213436191328,0.));
#203488=CARTESIAN_POINT('Ctrl Pts',(-19.0969808131228,13.0156847176096,
0.));
#203489=CARTESIAN_POINT('Ctrl Pts',(-19.0828239070484,13.0100374768788,
0.));
#203490=CARTESIAN_POINT('Ctrl Pts',(-19.0688235289437,13.0044031841382,
0.));
#203491=CARTESIAN_POINT('Ctrl Pts',(-19.0549809634354,12.9987831544502,
0.));
#203492=CARTESIAN_POINT('Ctrl Pts',(-19.0412975200398,12.9931787316514,
0.));
#203493=CARTESIAN_POINT('Ctrl Pts',(-19.0277745339909,12.9875912893003,
0.));
#203494=CARTESIAN_POINT('Ctrl Pts',(-19.014413367335,12.9820222318716,0.));
#203495=CARTESIAN_POINT('Ctrl Pts',(-19.0012154099792,12.9764729959206,
0.));
#203496=CARTESIAN_POINT('Ctrl Pts',(-18.9881820807585,12.9709450512747,
0.));
#203497=CARTESIAN_POINT('Ctrl Pts',(-18.9753148284473,12.9654399021868,
0.));
#203498=CARTESIAN_POINT('Ctrl Pts',(-18.9626151329226,12.9599590886317,
0.));
#203499=CARTESIAN_POINT('Ctrl Pts',(-18.9500845064714,12.9545041877377,
0.));
#203500=CARTESIAN_POINT('Ctrl Pts',(-18.9377244950435,12.9490768151821,
0.));
#203501=CARTESIAN_POINT('Ctrl Pts',(-18.9255366795196,12.9436786266106,
0.));
#203502=CARTESIAN_POINT('Ctrl Pts',(-18.9135226769466,12.9383113190375,
0.));
#203503=CARTESIAN_POINT('Ctrl Pts',(-18.9016841423402,12.9329766328184,
0.));
#203504=CARTESIAN_POINT('Ctrl Pts',(-18.8900227704888,12.9276763536372,
0.));
#203505=CARTESIAN_POINT('Ctrl Pts',(-18.8785402977528,12.9224123144982,
0.));
#203506=CARTESIAN_POINT('Ctrl Pts',(-18.8672385038328,12.9171863977047,
0.));
#203507=CARTESIAN_POINT('Ctrl Pts',(-18.8561192136201,12.9120005369066,
0.));
#203508=CARTESIAN_POINT('Ctrl Pts',(-18.8451842990986,12.9068567191856,
0.));
#203509=CARTESIAN_POINT('Ctrl Pts',(-18.834435681259,12.9017569871738,0.));
#203510=CARTESIAN_POINT('Ctrl Pts',(-18.8238753319124,12.8967034410752,
0.));
#203511=CARTESIAN_POINT('Ctrl Pts',(-18.8135052757815,12.8916982409931,
0.));
#203512=CARTESIAN_POINT('Ctrl Pts',(-18.8033275941939,12.8867436109543,
0.));
#203513=CARTESIAN_POINT('Ctrl Pts',(-18.7933444285867,12.8818418427474,
0.));
#203514=CARTESIAN_POINT('Ctrl Pts',(-18.7835579840481,12.8769952998097,
0.));
#203515=CARTESIAN_POINT('Ctrl Pts',(-18.7739705329029,12.8722064211814,
0.));
#203516=CARTESIAN_POINT('Ctrl Pts',(-18.7645844169568,12.8674777239656,
0.));
#203517=CARTESIAN_POINT('Ctrl Pts',(-18.7554020493888,12.8628118054172,
0.));
#203518=CARTESIAN_POINT('Ctrl Pts',(-18.7464259171248,12.8582113455644,
0.));
#203519=CARTESIAN_POINT('Ctrl Pts',(-18.7376585820851,12.8536791086315,
0.));
#203520=CARTESIAN_POINT('Ctrl Pts',(-18.7291026886552,12.849217951159,0.));
#203521=CARTESIAN_POINT('Ctrl Pts',(-18.7207609737701,12.8448308329494,
0.));
#203522=CARTESIAN_POINT('Ctrl Pts',(-18.7126362754446,12.8405208263432,
0.));
#203523=CARTESIAN_POINT('Ctrl Pts',(-18.7047315436296,12.8362911280362,
0.));
#203524=CARTESIAN_POINT('Ctrl Pts',(-18.6970498410173,12.832145059979,0.));
#203525=CARTESIAN_POINT('Ctrl Pts',(-18.6895943376172,12.8280860635231,
0.));
#203526=CARTESIAN_POINT('Ctrl Pts',(-18.6823683094139,12.8241176980016,
0.));
#203527=CARTESIAN_POINT('Ctrl Pts',(-18.6753751301091,12.8202436318473,
0.));
#203528=CARTESIAN_POINT('Ctrl Pts',(-18.6686182952798,12.8164676687361,
0.));
#203529=CARTESIAN_POINT('Ctrl Pts',(-18.6621014624746,12.8127937909632,
0.));
#203530=CARTESIAN_POINT('Ctrl Pts',(-18.6558284825772,12.8092261933858,
0.));
#203531=CARTESIAN_POINT('Ctrl Pts',(-18.6498034438986,12.805769331162,0.));
#203532=CARTESIAN_POINT('Ctrl Pts',(-18.6440306327457,12.8024278770153,
0.));
#203533=CARTESIAN_POINT('Ctrl Pts',(-18.63851447924,12.7992066625264,0.));
#203534=CARTESIAN_POINT('Ctrl Pts',(-18.6332595057005,12.7961106222251,
0.));
#203535=CARTESIAN_POINT('Ctrl Pts',(-18.6282702819371,12.7931447451556,
0.));
#203536=CARTESIAN_POINT('Ctrl Pts',(-18.6235516265575,12.7903142925234,
0.));
#203537=CARTESIAN_POINT('Ctrl Pts',(-18.6191087624752,12.7876249657834,
0.));
#203538=CARTESIAN_POINT('Ctrl Pts',(-18.6149475565189,12.78508316579,0.));
#203539=CARTESIAN_POINT('Ctrl Pts',(-18.611074482622,12.7826959526924,0.));
#203540=CARTESIAN_POINT('Ctrl Pts',(-18.6074961535723,12.7804705387658,
0.));
#203541=CARTESIAN_POINT('Ctrl Pts',(-18.6042190183703,12.7784139605067,
0.));
#203542=CARTESIAN_POINT('Ctrl Pts',(-18.6012488486708,12.7765325225082,
0.));
#203543=CARTESIAN_POINT('Ctrl Pts',(-18.5985917525949,12.7748328937639,
0.));
#203544=CARTESIAN_POINT('Ctrl Pts',(-18.5962551167772,12.7733231262107,
0.));
#203545=CARTESIAN_POINT('Ctrl Pts',(-18.5942490615409,12.7720142287169,
0.));
#203546=CARTESIAN_POINT('Ctrl Pts',(-18.5925859134582,12.7709195951153,
0.));
#203547=CARTESIAN_POINT('Ctrl Pts',(-18.5912775137806,12.7700520897174,
0.));
#203548=CARTESIAN_POINT('Ctrl Pts',(-18.590332877722,12.7694215127923,0.));
#203549=CARTESIAN_POINT('Ctrl Pts',(-18.589871621842,12.7691103481996,0.));
#203550=CARTESIAN_POINT('Ctrl Pts',(-18.5896919669158,12.7689864266924,
0.));
#203551=CARTESIAN_POINT('Ctrl Pts',(-18.5896460962961,12.7689524524484,
0.));
#203552=CARTESIAN_POINT('Ctrl Pts',(-18.5896416359912,12.7689476255363,
0.));
#203553=CARTESIAN_POINT('',(-22.1787195904339,13.5685075571671,0.));
#203554=CARTESIAN_POINT('Ctrl Pts',(-17.1452095830633,14.6513681262571,
0.));
#203555=CARTESIAN_POINT('Ctrl Pts',(-17.1452095830633,14.6513681262571,
12.));
#203556=CARTESIAN_POINT('Ctrl Pts',(-17.1452153999142,14.6513711852843,
0.));
#203557=CARTESIAN_POINT('Ctrl Pts',(-17.1452153999142,14.6513711852843,
12.));
#203558=CARTESIAN_POINT('Ctrl Pts',(-17.1452600887037,14.6514066997196,
0.));
#203559=CARTESIAN_POINT('Ctrl Pts',(-17.1452600887037,14.6514066997196,
12.));
#203560=CARTESIAN_POINT('Ctrl Pts',(-17.1454262858043,14.6515481598068,
0.));
#203561=CARTESIAN_POINT('Ctrl Pts',(-17.1454262858043,14.6515481598068,
12.));
#203562=CARTESIAN_POINT('Ctrl Pts',(-17.1458462295271,14.6519131634508,
0.));
#203563=CARTESIAN_POINT('Ctrl Pts',(-17.1458462295271,14.6519131634508,
12.));
#203564=CARTESIAN_POINT('Ctrl Pts',(-17.1466998098673,14.6526624064978,
0.));
#203565=CARTESIAN_POINT('Ctrl Pts',(-17.1466998098673,14.6526624064978,
12.));
#203566=CARTESIAN_POINT('Ctrl Pts',(-17.147876394491,14.6537016966184,0.));
#203567=CARTESIAN_POINT('Ctrl Pts',(-17.147876394491,14.6537016966184,12.));
#203568=CARTESIAN_POINT('Ctrl Pts',(-17.1493641837558,14.655024862281,0.));
#203569=CARTESIAN_POINT('Ctrl Pts',(-17.1493641837558,14.655024862281,12.));
#203570=CARTESIAN_POINT('Ctrl Pts',(-17.1511476869496,14.6566237952435,
0.));
#203571=CARTESIAN_POINT('Ctrl Pts',(-17.1511476869496,14.6566237952435,
12.));
#203572=CARTESIAN_POINT('Ctrl Pts',(-17.1532107762718,14.6584900555302,
0.));
#203573=CARTESIAN_POINT('Ctrl Pts',(-17.1532107762718,14.6584900555302,
12.));
#203574=CARTESIAN_POINT('Ctrl Pts',(-17.1555401986401,14.6606167169642,
0.));
#203575=CARTESIAN_POINT('Ctrl Pts',(-17.1555401986401,14.6606167169642,
12.));
#203576=CARTESIAN_POINT('Ctrl Pts',(-17.1581262646789,14.6629987285992,
0.));
#203577=CARTESIAN_POINT('Ctrl Pts',(-17.1581262646789,14.6629987285992,
12.));
#203578=CARTESIAN_POINT('Ctrl Pts',(-17.1609609517369,14.6656319165057,
0.));
#203579=CARTESIAN_POINT('Ctrl Pts',(-17.1609609517369,14.6656319165057,
12.));
#203580=CARTESIAN_POINT('Ctrl Pts',(-17.1640366762305,14.6685123374423,
0.));
#203581=CARTESIAN_POINT('Ctrl Pts',(-17.1640366762305,14.6685123374423,
12.));
#203582=CARTESIAN_POINT('Ctrl Pts',(-17.167344972302,14.671635583332,0.));
#203583=CARTESIAN_POINT('Ctrl Pts',(-17.167344972302,14.671635583332,12.));
#203584=CARTESIAN_POINT('Ctrl Pts',(-17.1708771619129,14.6749971333867,
0.));
#203585=CARTESIAN_POINT('Ctrl Pts',(-17.1708771619129,14.6749971333867,
12.));
#203586=CARTESIAN_POINT('Ctrl Pts',(-17.1746247499057,14.6785925615677,
0.));
#203587=CARTESIAN_POINT('Ctrl Pts',(-17.1746247499057,14.6785925615677,
12.));
#203588=CARTESIAN_POINT('Ctrl Pts',(-17.1785800350826,14.6824178576167,
0.));
#203589=CARTESIAN_POINT('Ctrl Pts',(-17.1785800350826,14.6824178576167,
12.));
#203590=CARTESIAN_POINT('Ctrl Pts',(-17.182736158472,14.686469452232,0.));
#203591=CARTESIAN_POINT('Ctrl Pts',(-17.182736158472,14.686469452232,12.));
#203592=CARTESIAN_POINT('Ctrl Pts',(-17.1870867909918,14.6907440526958,
0.));
#203593=CARTESIAN_POINT('Ctrl Pts',(-17.1870867909918,14.6907440526958,
12.));
#203594=CARTESIAN_POINT('Ctrl Pts',(-17.1916259308415,14.6952385361705,
0.));
#203595=CARTESIAN_POINT('Ctrl Pts',(-17.1916259308415,14.6952385361705,
12.));
#203596=CARTESIAN_POINT('Ctrl Pts',(-17.1963476411694,14.699949811582,0.));
#203597=CARTESIAN_POINT('Ctrl Pts',(-17.1963476411694,14.699949811582,12.));
#203598=CARTESIAN_POINT('Ctrl Pts',(-17.2012461084268,14.7048748502663,
0.));
#203599=CARTESIAN_POINT('Ctrl Pts',(-17.2012461084268,14.7048748502663,
12.));
#203600=CARTESIAN_POINT('Ctrl Pts',(-17.2063157097315,14.7100107213586,
0.));
#203601=CARTESIAN_POINT('Ctrl Pts',(-17.2063157097315,14.7100107213586,
12.));
#203602=CARTESIAN_POINT('Ctrl Pts',(-17.2115510835989,14.7153546289339,
0.));
#203603=CARTESIAN_POINT('Ctrl Pts',(-17.2115510835989,14.7153546289339,
12.));
#203604=CARTESIAN_POINT('Ctrl Pts',(-17.2169471814256,14.7209039390327,
0.));
#203605=CARTESIAN_POINT('Ctrl Pts',(-17.2169471814256,14.7209039390327,
12.));
#203606=CARTESIAN_POINT('Ctrl Pts',(-17.2224992099667,14.7266561494282,
0.));
#203607=CARTESIAN_POINT('Ctrl Pts',(-17.2224992099667,14.7266561494282,
12.));
#203608=CARTESIAN_POINT('Ctrl Pts',(-17.2282025904314,14.7326088681163,
0.));
#203609=CARTESIAN_POINT('Ctrl Pts',(-17.2282025904314,14.7326088681163,
12.));
#203610=CARTESIAN_POINT('Ctrl Pts',(-17.2340529062076,14.7387597858116,
0.));
#203611=CARTESIAN_POINT('Ctrl Pts',(-17.2340529062076,14.7387597858116,
12.));
#203612=CARTESIAN_POINT('Ctrl Pts',(-17.2400458713565,14.7451066593792,
0.));
#203613=CARTESIAN_POINT('Ctrl Pts',(-17.2400458713565,14.7451066593792,
12.));
#203614=CARTESIAN_POINT('Ctrl Pts',(-17.2461773413288,14.7516473175124,
0.));
#203615=CARTESIAN_POINT('Ctrl Pts',(-17.2461773413288,14.7516473175124,
12.));
#203616=CARTESIAN_POINT('Ctrl Pts',(-17.2524433146837,14.7583796616617,
0.));
#203617=CARTESIAN_POINT('Ctrl Pts',(-17.2524433146837,14.7583796616617,
12.));
#203618=CARTESIAN_POINT('Ctrl Pts',(-17.2588399401465,14.7653016697591,
0.));
#203619=CARTESIAN_POINT('Ctrl Pts',(-17.2588399401465,14.7653016697591,
12.));
#203620=CARTESIAN_POINT('Ctrl Pts',(-17.2653635155319,14.7724113956731,
0.));
#203621=CARTESIAN_POINT('Ctrl Pts',(-17.2653635155319,14.7724113956731,
12.));
#203622=CARTESIAN_POINT('Ctrl Pts',(-17.2720104735194,14.7797069617804,
0.));
#203623=CARTESIAN_POINT('Ctrl Pts',(-17.2720104735194,14.7797069617804,
12.));
#203624=CARTESIAN_POINT('Ctrl Pts',(-17.2787773704849,14.787186553128,0.));
#203625=CARTESIAN_POINT('Ctrl Pts',(-17.2787773704849,14.787186553128,12.));
#203626=CARTESIAN_POINT('Ctrl Pts',(-17.2856608733196,14.7948484105249,
0.));
#203627=CARTESIAN_POINT('Ctrl Pts',(-17.2856608733196,14.7948484105249,
12.));
#203628=CARTESIAN_POINT('Ctrl Pts',(-17.2926577496513,14.8026908254276,
0.));
#203629=CARTESIAN_POINT('Ctrl Pts',(-17.2926577496513,14.8026908254276,
12.));
#203630=CARTESIAN_POINT('Ctrl Pts',(-17.299764866148,14.8107121391035,0.));
#203631=CARTESIAN_POINT('Ctrl Pts',(-17.299764866148,14.8107121391035,12.));
#203632=CARTESIAN_POINT('Ctrl Pts',(-17.3069791853706,14.8189107410162,
0.));
#203633=CARTESIAN_POINT('Ctrl Pts',(-17.3069791853706,14.8189107410162,
12.));
#203634=CARTESIAN_POINT('Ctrl Pts',(-17.3142977632659,14.8272850675379,
0.));
#203635=CARTESIAN_POINT('Ctrl Pts',(-17.3142977632659,14.8272850675379,
12.));
#203636=CARTESIAN_POINT('Ctrl Pts',(-17.3217177462101,14.8358336004197,
0.));
#203637=CARTESIAN_POINT('Ctrl Pts',(-17.3217177462101,14.8358336004197,
12.));
#203638=CARTESIAN_POINT('Ctrl Pts',(-17.3292363662605,14.8445548643508,
0.));
#203639=CARTESIAN_POINT('Ctrl Pts',(-17.3292363662605,14.8445548643508,
12.));
#203640=CARTESIAN_POINT('Ctrl Pts',(-17.336850936485,14.8534474245433,0.));
#203641=CARTESIAN_POINT('Ctrl Pts',(-17.336850936485,14.8534474245433,12.));
#203642=CARTESIAN_POINT('Ctrl Pts',(-17.3445588463475,14.8625098843417,
0.));
#203643=CARTESIAN_POINT('Ctrl Pts',(-17.3445588463475,14.8625098843417,
12.));
#203644=CARTESIAN_POINT('Ctrl Pts',(-17.3523575568645,14.8717408826955,
0.));
#203645=CARTESIAN_POINT('Ctrl Pts',(-17.3523575568645,14.8717408826955,
12.));
#203646=CARTESIAN_POINT('Ctrl Pts',(-17.3602445978161,14.8811390927423,
0.));
#203647=CARTESIAN_POINT('Ctrl Pts',(-17.3602445978161,14.8811390927423,
12.));
#203648=CARTESIAN_POINT('Ctrl Pts',(-17.3682175653235,14.8907032205788,
0.));
#203649=CARTESIAN_POINT('Ctrl Pts',(-17.3682175653235,14.8907032205788,
12.));
#203650=CARTESIAN_POINT('Ctrl Pts',(-17.3762741193076,14.900432003961,0.));
#203651=CARTESIAN_POINT('Ctrl Pts',(-17.3762741193076,14.900432003961,12.));
#203652=CARTESIAN_POINT('Ctrl Pts',(-17.3844119809824,14.9103242110057,
0.));
#203653=CARTESIAN_POINT('Ctrl Pts',(-17.3844119809824,14.9103242110057,
12.));
#203654=CARTESIAN_POINT('Ctrl Pts',(-17.3926289303986,14.9203786389342,
0.));
#203655=CARTESIAN_POINT('Ctrl Pts',(-17.3926289303986,14.9203786389342,
12.));
#203656=CARTESIAN_POINT('Ctrl Pts',(-17.4009228040749,14.9305941128757,
0.));
#203657=CARTESIAN_POINT('Ctrl Pts',(-17.4009228040749,14.9305941128757,
12.));
#203658=CARTESIAN_POINT('Ctrl Pts',(-17.4092914926071,14.940969484645,0.));
#203659=CARTESIAN_POINT('Ctrl Pts',(-17.4092914926071,14.940969484645,12.));
#203660=CARTESIAN_POINT('Ctrl Pts',(-17.4177329382828,14.9515036315143,
0.));
#203661=CARTESIAN_POINT('Ctrl Pts',(-17.4177329382828,14.9515036315143,
12.));
#203662=CARTESIAN_POINT('Ctrl Pts',(-17.426245132709,14.9621954549827,0.));
#203663=CARTESIAN_POINT('Ctrl Pts',(-17.426245132709,14.9621954549827,12.));
#203664=CARTESIAN_POINT('Ctrl Pts',(-17.4348261151396,14.9730438799452,
0.));
#203665=CARTESIAN_POINT('Ctrl Pts',(-17.4348261151396,14.9730438799452,
12.));
#203666=CARTESIAN_POINT('Ctrl Pts',(-17.4434739707773,14.9840478538358,
0.));
#203667=CARTESIAN_POINT('Ctrl Pts',(-17.4434739707773,14.9840478538358,
12.));
#203668=CARTESIAN_POINT('Ctrl Pts',(-17.4521868291004,14.9952063457778,
0.));
#203669=CARTESIAN_POINT('Ctrl Pts',(-17.4521868291004,14.9952063457778,
12.));
#203670=CARTESIAN_POINT('Ctrl Pts',(-17.4609628621418,15.0065183456921,
0.));
#203671=CARTESIAN_POINT('Ctrl Pts',(-17.4609628621418,15.0065183456921,
12.));
#203672=CARTESIAN_POINT('Ctrl Pts',(-17.4698002829357,15.0179828635086,
0.));
#203673=CARTESIAN_POINT('Ctrl Pts',(-17.4698002829357,15.0179828635086,
12.));
#203674=CARTESIAN_POINT('Ctrl Pts',(-17.4786973441417,15.029598928488,0.));
#203675=CARTESIAN_POINT('Ctrl Pts',(-17.4786973441417,15.029598928488,12.));
#203676=CARTESIAN_POINT('Ctrl Pts',(-17.4876523366178,15.0413655884993,
0.));
#203677=CARTESIAN_POINT('Ctrl Pts',(-17.4876523366178,15.0413655884993,
12.));
#203678=CARTESIAN_POINT('Ctrl Pts',(-17.4966635880245,15.0532819093085,
0.));
#203679=CARTESIAN_POINT('Ctrl Pts',(-17.4966635880245,15.0532819093085,
12.));
#203680=CARTESIAN_POINT('Ctrl Pts',(-17.5057294613874,15.0653469738306,
0.));
#203681=CARTESIAN_POINT('Ctrl Pts',(-17.5057294613874,15.0653469738306,
12.));
#203682=CARTESIAN_POINT('Ctrl Pts',(-17.5148483539684,15.0775598815748,
0.));
#203683=CARTESIAN_POINT('Ctrl Pts',(-17.5148483539684,15.0775598815748,
12.));
#203684=CARTESIAN_POINT('Ctrl Pts',(-17.5240186961788,15.0899197481082,
0.));
#203685=CARTESIAN_POINT('Ctrl Pts',(-17.5240186961788,15.0899197481082,
12.));
#203686=CARTESIAN_POINT('Ctrl Pts',(-17.5332389504829,15.1024257045033,
0.));
#203687=CARTESIAN_POINT('Ctrl Pts',(-17.5332389504829,15.1024257045033,
12.));
#203688=CARTESIAN_POINT('Ctrl Pts',(-17.5425076102966,15.1150768967729,
0.));
#203689=CARTESIAN_POINT('Ctrl Pts',(-17.5425076102966,15.1150768967729,
12.));
#203690=CARTESIAN_POINT('Ctrl Pts',(-17.5518231989122,15.127872485314,0.));
#203691=CARTESIAN_POINT('Ctrl Pts',(-17.5518231989122,15.127872485314,12.));
#203692=CARTESIAN_POINT('Ctrl Pts',(-17.5611842686196,15.1408116444877,
0.));
#203693=CARTESIAN_POINT('Ctrl Pts',(-17.5611842686196,15.1408116444877,
12.));
#203694=CARTESIAN_POINT('Ctrl Pts',(-17.570589399803,15.1538935621714,0.));
#203695=CARTESIAN_POINT('Ctrl Pts',(-17.570589399803,15.1538935621714,12.));
#203696=CARTESIAN_POINT('Ctrl Pts',(-17.5800372000539,15.1671174393136,
0.));
#203697=CARTESIAN_POINT('Ctrl Pts',(-17.5800372000539,15.1671174393136,
12.));
#203698=CARTESIAN_POINT('Ctrl Pts',(-17.5895263032592,15.1804824894605,
0.));
#203699=CARTESIAN_POINT('Ctrl Pts',(-17.5895263032592,15.1804824894605,
12.));
#203700=CARTESIAN_POINT('Ctrl Pts',(-17.5990553687595,15.1939879383268,
0.));
#203701=CARTESIAN_POINT('Ctrl Pts',(-17.5990553687595,15.1939879383268,
12.));
#203702=CARTESIAN_POINT('Ctrl Pts',(-17.6086230806497,15.2076330234686,
0.));
#203703=CARTESIAN_POINT('Ctrl Pts',(-17.6086230806497,15.2076330234686,
12.));
#203704=CARTESIAN_POINT('Ctrl Pts',(-17.6182281470467,15.22141699392,0.));
#203705=CARTESIAN_POINT('Ctrl Pts',(-17.6182281470467,15.22141699392,12.));
#203706=CARTESIAN_POINT('Ctrl Pts',(-17.6278692993765,15.2353391098367,
0.));
#203707=CARTESIAN_POINT('Ctrl Pts',(-17.6278692993765,15.2353391098367,
12.));
#203708=CARTESIAN_POINT('Ctrl Pts',(-17.637545291637,15.2493986421091,0.));
#203709=CARTESIAN_POINT('Ctrl Pts',(-17.637545291637,15.2493986421091,12.));
#203710=CARTESIAN_POINT('Ctrl Pts',(-17.6472548997329,15.263594872029,0.));
#203711=CARTESIAN_POINT('Ctrl Pts',(-17.6472548997329,15.263594872029,12.));
#203712=CARTESIAN_POINT('Ctrl Pts',(-17.6569969209,15.2779270910238,0.));
#203713=CARTESIAN_POINT('Ctrl Pts',(-17.6569969209,15.2779270910238,12.));
#203714=CARTESIAN_POINT('Ctrl Pts',(-17.6667701731041,15.2923946003598,
0.));
#203715=CARTESIAN_POINT('Ctrl Pts',(-17.6667701731041,15.2923946003598,
12.));
#203716=CARTESIAN_POINT('Ctrl Pts',(-17.6765734944559,15.3069967108501,
0.));
#203717=CARTESIAN_POINT('Ctrl Pts',(-17.6765734944559,15.3069967108501,
12.));
#203718=CARTESIAN_POINT('Ctrl Pts',(-17.6864057426052,15.3217327425341,
0.));
#203719=CARTESIAN_POINT('Ctrl Pts',(-17.6864057426052,15.3217327425341,
12.));
#203720=CARTESIAN_POINT('Ctrl Pts',(-17.6962657941984,15.3366020244069,
0.));
#203721=CARTESIAN_POINT('Ctrl Pts',(-17.6962657941984,15.3366020244069,
12.));
#203722=CARTESIAN_POINT('Ctrl Pts',(-17.7061525444044,15.3516038942064,
0.));
#203723=CARTESIAN_POINT('Ctrl Pts',(-17.7061525444044,15.3516038942064,
12.));
#203724=CARTESIAN_POINT('Ctrl Pts',(-17.7160649064208,15.3667376981702,
0.));
#203725=CARTESIAN_POINT('Ctrl Pts',(-17.7160649064208,15.3667376981702,
12.));
#203726=CARTESIAN_POINT('Ctrl Pts',(-17.7260018109923,15.3820027907965,
0.));
#203727=CARTESIAN_POINT('Ctrl Pts',(-17.7260018109923,15.3820027907965,
12.));
#203728=CARTESIAN_POINT('Ctrl Pts',(-17.7359622059143,15.3973985345796,
0.));
#203729=CARTESIAN_POINT('Ctrl Pts',(-17.7359622059143,15.3973985345796,
12.));
#203730=CARTESIAN_POINT('Ctrl Pts',(-17.7459450555803,15.4129242997828,
0.));
#203731=CARTESIAN_POINT('Ctrl Pts',(-17.7459450555803,15.4129242997828,
12.));
#203732=CARTESIAN_POINT('Ctrl Pts',(-17.7559493405871,15.4285794642658,
0.));
#203733=CARTESIAN_POINT('Ctrl Pts',(-17.7559493405871,15.4285794642658,
12.));
#203734=CARTESIAN_POINT('Ctrl Pts',(-17.765974057326,15.4443634132865,0.));
#203735=CARTESIAN_POINT('Ctrl Pts',(-17.765974057326,15.4443634132865,12.));
#203736=CARTESIAN_POINT('Ctrl Pts',(-17.7760182175817,15.4602755393019,
0.));
#203737=CARTESIAN_POINT('Ctrl Pts',(-17.7760182175817,15.4602755393019,
12.));
#203738=CARTESIAN_POINT('Ctrl Pts',(-17.7860808481229,15.4763152417506,
0.));
#203739=CARTESIAN_POINT('Ctrl Pts',(-17.7860808481229,15.4763152417506,
12.));
#203740=CARTESIAN_POINT('Ctrl Pts',(-17.7961609903161,15.4924819268529,
0.));
#203741=CARTESIAN_POINT('Ctrl Pts',(-17.7961609903161,15.4924819268529,
12.));
#203742=CARTESIAN_POINT('Ctrl Pts',(-17.8062576997964,15.5087750074728,
0.));
#203743=CARTESIAN_POINT('Ctrl Pts',(-17.8062576997964,15.5087750074728,
12.));
#203744=CARTESIAN_POINT('Ctrl Pts',(-17.8163700461263,15.5251939029558,
0.));
#203745=CARTESIAN_POINT('Ctrl Pts',(-17.8163700461263,15.5251939029558,
12.));
#203746=CARTESIAN_POINT('Ctrl Pts',(-17.8264971124606,15.5417380389639,
0.));
#203747=CARTESIAN_POINT('Ctrl Pts',(-17.8264971124606,15.5417380389639,
12.));
#203748=CARTESIAN_POINT('Ctrl Pts',(-17.8366379952078,15.5584068472976,
0.));
#203749=CARTESIAN_POINT('Ctrl Pts',(-17.8366379952078,15.5584068472976,
12.));
#203750=CARTESIAN_POINT('Ctrl Pts',(-17.8467918036977,15.5751997657153,
0.));
#203751=CARTESIAN_POINT('Ctrl Pts',(-17.8467918036977,15.5751997657153,
12.));
#203752=CARTESIAN_POINT('Ctrl Pts',(-17.8569576598996,15.5921162378183,
0.));
#203753=CARTESIAN_POINT('Ctrl Pts',(-17.8569576598996,15.5921162378183,
12.));
#203754=CARTESIAN_POINT('Ctrl Pts',(-17.8671346981388,15.6091557129205,
0.));
#203755=CARTESIAN_POINT('Ctrl Pts',(-17.8671346981388,15.6091557129205,
12.));
#203756=CARTESIAN_POINT('Ctrl Pts',(-17.8773220648125,15.6263176459107,
0.));
#203757=CARTESIAN_POINT('Ctrl Pts',(-17.8773220648125,15.6263176459107,
12.));
#203758=CARTESIAN_POINT('Ctrl Pts',(-17.8875189181095,15.6436014971088,
0.));
#203759=CARTESIAN_POINT('Ctrl Pts',(-17.8875189181095,15.6436014971088,
12.));
#203760=CARTESIAN_POINT('Ctrl Pts',(-17.8977244277247,15.6610067321036,
0.));
#203761=CARTESIAN_POINT('Ctrl Pts',(-17.8977244277247,15.6610067321036,
12.));
#203762=CARTESIAN_POINT('Ctrl Pts',(-17.9079377746118,15.6785328216467,
0.));
#203763=CARTESIAN_POINT('Ctrl Pts',(-17.9079377746118,15.6785328216467,
12.));
#203764=CARTESIAN_POINT('Ctrl Pts',(-17.918158150746,15.6961792415526,0.));
#203765=CARTESIAN_POINT('Ctrl Pts',(-17.918158150746,15.6961792415526,12.));
#203766=CARTESIAN_POINT('Ctrl Pts',(-17.9283847588837,15.713945472584,0.));
#203767=CARTESIAN_POINT('Ctrl Pts',(-17.9283847588837,15.713945472584,12.));
#203768=CARTESIAN_POINT('Ctrl Pts',(-17.9386168123261,15.7318310003334,
0.));
#203769=CARTESIAN_POINT('Ctrl Pts',(-17.9386168123261,15.7318310003334,
12.));
#203770=CARTESIAN_POINT('Ctrl Pts',(-17.9488535346776,15.7498353150856,
0.));
#203771=CARTESIAN_POINT('Ctrl Pts',(-17.9488535346776,15.7498353150856,
12.));
#203772=CARTESIAN_POINT('Ctrl Pts',(-17.9590941596236,15.7679579117072,
0.));
#203773=CARTESIAN_POINT('Ctrl Pts',(-17.9590941596236,15.7679579117072,
12.));
#203774=CARTESIAN_POINT('Ctrl Pts',(-17.9693379307297,15.786198289572,0.));
#203775=CARTESIAN_POINT('Ctrl Pts',(-17.9693379307297,15.786198289572,12.));
#203776=CARTESIAN_POINT('Ctrl Pts',(-17.9795841012383,15.8045559524674,
0.));
#203777=CARTESIAN_POINT('Ctrl Pts',(-17.9795841012383,15.8045559524674,
12.));
#203778=CARTESIAN_POINT('Ctrl Pts',(-17.9898319338664,15.8230304084963,
0.));
#203779=CARTESIAN_POINT('Ctrl Pts',(-17.9898319338664,15.8230304084963,
12.));
#203780=CARTESIAN_POINT('Ctrl Pts',(-18.0000807006055,15.8416211699681,
0.));
#203781=CARTESIAN_POINT('Ctrl Pts',(-18.0000807006055,15.8416211699681,
12.));
#203782=CARTESIAN_POINT('Ctrl Pts',(-18.010329682521,15.8603277532834,0.));
#203783=CARTESIAN_POINT('Ctrl Pts',(-18.010329682521,15.8603277532834,12.));
#203784=CARTESIAN_POINT('Ctrl Pts',(-18.0205781695773,15.8791496788685,
0.));
#203785=CARTESIAN_POINT('Ctrl Pts',(-18.0205781695773,15.8791496788685,
12.));
#203786=CARTESIAN_POINT('Ctrl Pts',(-18.0308254604638,15.8980864711043,
0.));
#203787=CARTESIAN_POINT('Ctrl Pts',(-18.0308254604638,15.8980864711043,
12.));
#203788=CARTESIAN_POINT('Ctrl Pts',(-18.0410708624208,15.9171376582436,
0.));
#203789=CARTESIAN_POINT('Ctrl Pts',(-18.0410708624208,15.9171376582436,
12.));
#203790=CARTESIAN_POINT('Ctrl Pts',(-18.0513136910691,15.9363027723244,
0.));
#203791=CARTESIAN_POINT('Ctrl Pts',(-18.0513136910691,15.9363027723244,
12.));
#203792=CARTESIAN_POINT('Ctrl Pts',(-18.061553270236,15.9555813490645,0.));
#203793=CARTESIAN_POINT('Ctrl Pts',(-18.061553270236,15.9555813490645,12.));
#203794=CARTESIAN_POINT('Ctrl Pts',(-18.071788931796,15.9749729277848,0.));
#203795=CARTESIAN_POINT('Ctrl Pts',(-18.071788931796,15.9749729277848,12.));
#203796=CARTESIAN_POINT('Ctrl Pts',(-18.0820200155239,15.9944770513616,
0.));
#203797=CARTESIAN_POINT('Ctrl Pts',(-18.0820200155239,15.9944770513616,
12.));
#203798=CARTESIAN_POINT('Ctrl Pts',(-18.0922458689464,16.0140932661612,
0.));
#203799=CARTESIAN_POINT('Ctrl Pts',(-18.0922458689464,16.0140932661612,
12.));
#203800=CARTESIAN_POINT('Ctrl Pts',(-18.1024658471966,16.0338211219693,
0.));
#203801=CARTESIAN_POINT('Ctrl Pts',(-18.1024658471966,16.0338211219693,
12.));
#203802=CARTESIAN_POINT('Ctrl Pts',(-18.1126793128688,16.0536601719124,
0.));
#203803=CARTESIAN_POINT('Ctrl Pts',(-18.1126793128688,16.0536601719124,
12.));
#203804=CARTESIAN_POINT('Ctrl Pts',(-18.1228856358746,16.0736099723664,
0.));
#203805=CARTESIAN_POINT('Ctrl Pts',(-18.1228856358746,16.0736099723664,
12.));
#203806=CARTESIAN_POINT('Ctrl Pts',(-18.1330841933099,16.0936700829108,
0.));
#203807=CARTESIAN_POINT('Ctrl Pts',(-18.1330841933099,16.0936700829108,
12.));
#203808=CARTESIAN_POINT('Ctrl Pts',(-18.1432743693231,16.113840066279,0.));
#203809=CARTESIAN_POINT('Ctrl Pts',(-18.1432743693231,16.113840066279,12.));
#203810=CARTESIAN_POINT('Ctrl Pts',(-18.1534555549851,16.1341194882987,
0.));
#203811=CARTESIAN_POINT('Ctrl Pts',(-18.1534555549851,16.1341194882987,
12.));
#203812=CARTESIAN_POINT('Ctrl Pts',(-18.1636271481616,16.1545079178261,
0.));
#203813=CARTESIAN_POINT('Ctrl Pts',(-18.1636271481616,16.1545079178261,
12.));
#203814=CARTESIAN_POINT('Ctrl Pts',(-18.1737885533852,16.1750049266673,
0.));
#203815=CARTESIAN_POINT('Ctrl Pts',(-18.1737885533852,16.1750049266673,
12.));
#203816=CARTESIAN_POINT('Ctrl Pts',(-18.1839391817335,16.1956100895076,
0.));
#203817=CARTESIAN_POINT('Ctrl Pts',(-18.1839391817335,16.1956100895076,
12.));
#203818=CARTESIAN_POINT('Ctrl Pts',(-18.1940784507232,16.2163229838878,
0.));
#203819=CARTESIAN_POINT('Ctrl Pts',(-18.1940784507232,16.2163229838878,
12.));
#203820=CARTESIAN_POINT('Ctrl Pts',(-18.2042057842037,16.237143190164,0.));
#203821=CARTESIAN_POINT('Ctrl Pts',(-18.2042057842037,16.237143190164,12.));
#203822=CARTESIAN_POINT('Ctrl Pts',(-18.214320612253,16.2580702914615,0.));
#203823=CARTESIAN_POINT('Ctrl Pts',(-18.214320612253,16.2580702914615,12.));
#203824=CARTESIAN_POINT('Ctrl Pts',(-18.2244223710745,16.2791038736223,
0.));
#203825=CARTESIAN_POINT('Ctrl Pts',(-18.2244223710745,16.2791038736223,
12.));
#203826=CARTESIAN_POINT('Ctrl Pts',(-18.2345105028981,16.3002435251378,
0.));
#203827=CARTESIAN_POINT('Ctrl Pts',(-18.2345105028981,16.3002435251378,
12.));
#203828=CARTESIAN_POINT('Ctrl Pts',(-18.2445844558742,16.3214888370988,
0.));
#203829=CARTESIAN_POINT('Ctrl Pts',(-18.2445844558742,16.3214888370988,
12.));
#203830=CARTESIAN_POINT('Ctrl Pts',(-18.2546436839609,16.342839403159,0.));
#203831=CARTESIAN_POINT('Ctrl Pts',(-18.2546436839609,16.342839403159,12.));
#203832=CARTESIAN_POINT('Ctrl Pts',(-18.2646876468169,16.3642948194869,
0.));
#203833=CARTESIAN_POINT('Ctrl Pts',(-18.2646876468169,16.3642948194869,
12.));
#203834=CARTESIAN_POINT('Ctrl Pts',(-18.2747158096934,16.385854684708,0.));
#203835=CARTESIAN_POINT('Ctrl Pts',(-18.2747158096934,16.385854684708,12.));
#203836=CARTESIAN_POINT('Ctrl Pts',(-18.2847276433308,16.4075185998454,
0.));
#203837=CARTESIAN_POINT('Ctrl Pts',(-18.2847276433308,16.4075185998454,
12.));
#203838=CARTESIAN_POINT('Ctrl Pts',(-18.2947226238509,16.4292861682377,
0.));
#203839=CARTESIAN_POINT('Ctrl Pts',(-18.2947226238509,16.4292861682377,
12.));
#203840=CARTESIAN_POINT('Ctrl Pts',(-18.3047002326858,16.4511569955231,
0.));
#203841=CARTESIAN_POINT('Ctrl Pts',(-18.3047002326858,16.4511569955231,
12.));
#203842=CARTESIAN_POINT('Ctrl Pts',(-18.3146599565229,16.4731306896439,
0.));
#203843=CARTESIAN_POINT('Ctrl Pts',(-18.3146599565229,16.4731306896439,
12.));
#203844=CARTESIAN_POINT('Ctrl Pts',(-18.3246012872468,16.4952068608344,
0.));
#203845=CARTESIAN_POINT('Ctrl Pts',(-18.3246012872468,16.4952068608344,
12.));
#203846=CARTESIAN_POINT('Ctrl Pts',(-18.3345237218864,16.5173851216045,
0.));
#203847=CARTESIAN_POINT('Ctrl Pts',(-18.3345237218864,16.5173851216045,
12.));
#203848=CARTESIAN_POINT('Ctrl Pts',(-18.3444267625601,16.5396650867139,
0.));
#203849=CARTESIAN_POINT('Ctrl Pts',(-18.3444267625601,16.5396650867139,
12.));
#203850=CARTESIAN_POINT('Ctrl Pts',(-18.3543099164331,16.5620463731414,
0.));
#203851=CARTESIAN_POINT('Ctrl Pts',(-18.3543099164331,16.5620463731414,
12.));
#203852=CARTESIAN_POINT('Ctrl Pts',(-18.364172695589,16.5845286000218,0.));
#203853=CARTESIAN_POINT('Ctrl Pts',(-18.364172695589,16.5845286000218,12.));
#203854=CARTESIAN_POINT('Ctrl Pts',(-18.3740146168879,16.6071113885711,
0.));
#203855=CARTESIAN_POINT('Ctrl Pts',(-18.3740146168879,16.6071113885711,
12.));
#203856=CARTESIAN_POINT('Ctrl Pts',(-18.3838352018327,16.6297943620056,
0.));
#203857=CARTESIAN_POINT('Ctrl Pts',(-18.3838352018327,16.6297943620056,
12.));
#203858=CARTESIAN_POINT('Ctrl Pts',(-18.3936339764332,16.6525771454513,
0.));
#203859=CARTESIAN_POINT('Ctrl Pts',(-18.3936339764332,16.6525771454513,
12.));
#203860=CARTESIAN_POINT('Ctrl Pts',(-18.4034104710789,16.6754593658513,
0.));
#203861=CARTESIAN_POINT('Ctrl Pts',(-18.4034104710789,16.6754593658513,
12.));
#203862=CARTESIAN_POINT('Ctrl Pts',(-18.413164220399,16.698440651849,0.));
#203863=CARTESIAN_POINT('Ctrl Pts',(-18.413164220399,16.698440651849,12.));
#203864=CARTESIAN_POINT('Ctrl Pts',(-18.4228947633186,16.7215206338818,
0.));
#203865=CARTESIAN_POINT('Ctrl Pts',(-18.4228947633186,16.7215206338818,
12.));
#203866=CARTESIAN_POINT('Ctrl Pts',(-18.4326016431392,16.7446989442882,
0.));
#203867=CARTESIAN_POINT('Ctrl Pts',(-18.4326016431392,16.7446989442882,
12.));
#203868=CARTESIAN_POINT('Ctrl Pts',(-18.4422844076099,16.7679752173992,
0.));
#203869=CARTESIAN_POINT('Ctrl Pts',(-18.4422844076099,16.7679752173992,
12.));
#203870=CARTESIAN_POINT('Ctrl Pts',(-18.4519426090124,16.791349089629,0.));
#203871=CARTESIAN_POINT('Ctrl Pts',(-18.4519426090124,16.791349089629,12.));
#203872=CARTESIAN_POINT('Ctrl Pts',(-18.4615758042305,16.8148201995472,
0.));
#203873=CARTESIAN_POINT('Ctrl Pts',(-18.4615758042305,16.8148201995472,
12.));
#203874=CARTESIAN_POINT('Ctrl Pts',(-18.4711835548622,16.8383881879707,
0.));
#203875=CARTESIAN_POINT('Ctrl Pts',(-18.4711835548622,16.8383881879707,
12.));
#203876=CARTESIAN_POINT('Ctrl Pts',(-18.4807654268769,16.8620526977169,
0.));
#203877=CARTESIAN_POINT('Ctrl Pts',(-18.4807654268769,16.8620526977169,
12.));
#203878=CARTESIAN_POINT('Ctrl Pts',(-18.4903209902226,16.8858133733086,
0.));
#203879=CARTESIAN_POINT('Ctrl Pts',(-18.4903209902226,16.8858133733086,
12.));
#203880=CARTESIAN_POINT('Ctrl Pts',(-18.4998498184619,16.9096698606942,
0.));
#203881=CARTESIAN_POINT('Ctrl Pts',(-18.4998498184619,16.9096698606942,
12.));
#203882=CARTESIAN_POINT('Ctrl Pts',(-18.5093514883835,16.9336218069353,
0.));
#203883=CARTESIAN_POINT('Ctrl Pts',(-18.5093514883835,16.9336218069353,
12.));
#203884=CARTESIAN_POINT('Ctrl Pts',(-18.518825579666,16.957668859934,0.));
#203885=CARTESIAN_POINT('Ctrl Pts',(-18.518825579666,16.957668859934,12.));
#203886=CARTESIAN_POINT('Ctrl Pts',(-18.5282716744198,16.9818106680382,
0.));
#203887=CARTESIAN_POINT('Ctrl Pts',(-18.5282716744198,16.9818106680382,
12.));
#203888=CARTESIAN_POINT('Ctrl Pts',(-18.5376893576961,17.0060468805099,
0.));
#203889=CARTESIAN_POINT('Ctrl Pts',(-18.5376893576961,17.0060468805099,
12.));
#203890=CARTESIAN_POINT('Ctrl Pts',(-18.5470782182089,17.030377148174,0.));
#203891=CARTESIAN_POINT('Ctrl Pts',(-18.5470782182089,17.030377148174,12.));
#203892=CARTESIAN_POINT('Ctrl Pts',(-18.5564378489628,17.0548011239751,
0.));
#203893=CARTESIAN_POINT('Ctrl Pts',(-18.5564378489628,17.0548011239751,
12.));
#203894=CARTESIAN_POINT('Ctrl Pts',(-18.5657678479788,17.0793184636079,
0.));
#203895=CARTESIAN_POINT('Ctrl Pts',(-18.5657678479788,17.0793184636079,
12.));
#203896=CARTESIAN_POINT('Ctrl Pts',(-18.5750678188543,17.1039288260001,
0.));
#203897=CARTESIAN_POINT('Ctrl Pts',(-18.5750678188543,17.1039288260001,
12.));
#203898=CARTESIAN_POINT('Ctrl Pts',(-18.5843373717253,17.1286318741185,
0.));
#203899=CARTESIAN_POINT('Ctrl Pts',(-18.5843373717253,17.1286318741185,
12.));
#203900=CARTESIAN_POINT('Ctrl Pts',(-18.5935761222833,17.1534272741646,
0.));
#203901=CARTESIAN_POINT('Ctrl Pts',(-18.5935761222833,17.1534272741646,
12.));
#203902=CARTESIAN_POINT('Ctrl Pts',(-18.6027836898826,17.1783146940131,
0.));
#203903=CARTESIAN_POINT('Ctrl Pts',(-18.6027836898826,17.1783146940131,
12.));
#203904=CARTESIAN_POINT('Ctrl Pts',(-18.6119596959957,17.2032938019288,
0.));
#203905=CARTESIAN_POINT('Ctrl Pts',(-18.6119596959957,17.2032938019288,
12.));
#203906=CARTESIAN_POINT('Ctrl Pts',(-18.6211037624041,17.2283642650519,
0.));
#203907=CARTESIAN_POINT('Ctrl Pts',(-18.6211037624041,17.2283642650519,
12.));
#203908=CARTESIAN_POINT('Ctrl Pts',(-18.630215509794,17.2535257482186,0.));
#203909=CARTESIAN_POINT('Ctrl Pts',(-18.630215509794,17.2535257482186,12.));
#203910=CARTESIAN_POINT('Ctrl Pts',(-18.639294555474,17.278777912021,0.));
#203911=CARTESIAN_POINT('Ctrl Pts',(-18.639294555474,17.278777912021,12.));
#203912=CARTESIAN_POINT('Ctrl Pts',(-18.6483405141853,17.3041204135069,
0.));
#203913=CARTESIAN_POINT('Ctrl Pts',(-18.6483405141853,17.3041204135069,
12.));
#203914=CARTESIAN_POINT('Ctrl Pts',(-18.6573530024019,17.3295529098612,
0.));
#203915=CARTESIAN_POINT('Ctrl Pts',(-18.6573530024019,17.3295529098612,
12.));
#203916=CARTESIAN_POINT('Ctrl Pts',(-18.6663316416569,17.3550750612438,
0.));
#203917=CARTESIAN_POINT('Ctrl Pts',(-18.6663316416569,17.3550750612438,
12.));
#203918=CARTESIAN_POINT('Ctrl Pts',(-18.6752760624045,17.3806865340744,
0.));
#203919=CARTESIAN_POINT('Ctrl Pts',(-18.6752760624045,17.3806865340744,
12.));
#203920=CARTESIAN_POINT('Ctrl Pts',(-18.6841859073472,17.4063870038563,
0.));
#203921=CARTESIAN_POINT('Ctrl Pts',(-18.6841859073472,17.4063870038563,
12.));
#203922=CARTESIAN_POINT('Ctrl Pts',(-18.6930608357421,17.4321761588148,
0.));
#203923=CARTESIAN_POINT('Ctrl Pts',(-18.6930608357421,17.4321761588148,
12.));
#203924=CARTESIAN_POINT('Ctrl Pts',(-18.7019005250322,17.4580537012764,
0.));
#203925=CARTESIAN_POINT('Ctrl Pts',(-18.7019005250322,17.4580537012764,
12.));
#203926=CARTESIAN_POINT('Ctrl Pts',(-18.7107046613941,17.4840193397176,
0.));
#203927=CARTESIAN_POINT('Ctrl Pts',(-18.7107046613941,17.4840193397176,
12.));
#203928=CARTESIAN_POINT('Ctrl Pts',(-18.7194729318128,17.5100727820891,
0.));
#203929=CARTESIAN_POINT('Ctrl Pts',(-18.7194729318128,17.5100727820891,
12.));
#203930=CARTESIAN_POINT('Ctrl Pts',(-18.728205015716,17.5362137287604,0.));
#203931=CARTESIAN_POINT('Ctrl Pts',(-18.728205015716,17.5362137287604,12.));
#203932=CARTESIAN_POINT('Ctrl Pts',(-18.7369005764558,17.5624418653248,
0.));
#203933=CARTESIAN_POINT('Ctrl Pts',(-18.7369005764558,17.5624418653248,
12.));
#203934=CARTESIAN_POINT('Ctrl Pts',(-18.7455592536667,17.5887568561361,
0.));
#203935=CARTESIAN_POINT('Ctrl Pts',(-18.7455592536667,17.5887568561361,
12.));
#203936=CARTESIAN_POINT('Ctrl Pts',(-18.7541806530935,17.6151583356988,
0.));
#203937=CARTESIAN_POINT('Ctrl Pts',(-18.7541806530935,17.6151583356988,
12.));
#203938=CARTESIAN_POINT('Ctrl Pts',(-18.7627643613139,17.6416459210646,
0.));
#203939=CARTESIAN_POINT('Ctrl Pts',(-18.7627643613139,17.6416459210646,
12.));
#203940=CARTESIAN_POINT('Ctrl Pts',(-18.7713099642673,17.6682192274197,
0.));
#203941=CARTESIAN_POINT('Ctrl Pts',(-18.7713099642673,17.6682192274197,
12.));
#203942=CARTESIAN_POINT('Ctrl Pts',(-18.7798170641305,17.6948778822981,
0.));
#203943=CARTESIAN_POINT('Ctrl Pts',(-18.7798170641305,17.6948778822981,
12.));
#203944=CARTESIAN_POINT('Ctrl Pts',(-18.7882852976016,17.7216215409019,
0.));
#203945=CARTESIAN_POINT('Ctrl Pts',(-18.7882852976016,17.7216215409019,
12.));
#203946=CARTESIAN_POINT('Ctrl Pts',(-18.7967143519444,17.7484498996916,
0.));
#203947=CARTESIAN_POINT('Ctrl Pts',(-18.7967143519444,17.7484498996916,
12.));
#203948=CARTESIAN_POINT('Ctrl Pts',(-18.8051039860543,17.7753627137898,
0.));
#203949=CARTESIAN_POINT('Ctrl Pts',(-18.8051039860543,17.7753627137898,
12.));
#203950=CARTESIAN_POINT('Ctrl Pts',(-18.8134540340581,17.8023598011135,
0.));
#203951=CARTESIAN_POINT('Ctrl Pts',(-18.8134540340581,17.8023598011135,
12.));
#203952=CARTESIAN_POINT('Ctrl Pts',(-18.8217643886368,17.8294410311105,
0.));
#203953=CARTESIAN_POINT('Ctrl Pts',(-18.8217643886368,17.8294410311105,
12.));
#203954=CARTESIAN_POINT('Ctrl Pts',(-18.8300349896187,17.8566063174871,
0.));
#203955=CARTESIAN_POINT('Ctrl Pts',(-18.8300349896187,17.8566063174871,
12.));
#203956=CARTESIAN_POINT('Ctrl Pts',(-18.8366196462746,17.8784057509434,
0.));
#203957=CARTESIAN_POINT('Ctrl Pts',(-18.8366196462746,17.8784057509434,
12.));
#203958=CARTESIAN_POINT('Ctrl Pts',(-18.8415402351882,17.8947931177853,
0.));
#203959=CARTESIAN_POINT('Ctrl Pts',(-18.8415402351882,17.8947931177853,
12.));
#203960=CARTESIAN_POINT('Ctrl Pts',(-18.8448126709726,17.9057348246611,
0.));
#203961=CARTESIAN_POINT('Ctrl Pts',(-18.8448126709726,17.9057348246611,
12.));
#203962=CARTESIAN_POINT('Ctrl Pts',(-18.8464468996588,17.9112098770111,
0.));
#203963=CARTESIAN_POINT('Ctrl Pts',(-18.8464468996588,17.9112098770111,
12.));
#203964=CARTESIAN_POINT('',(-18.8464468996588,17.9112098770111,0.));
#203965=CARTESIAN_POINT('Ctrl Pts',(-17.1452095830633,14.6513681262571,
0.));
#203966=CARTESIAN_POINT('Ctrl Pts',(-17.1452153999142,14.6513711852843,
0.));
#203967=CARTESIAN_POINT('Ctrl Pts',(-17.1452600887037,14.6514066997196,
0.));
#203968=CARTESIAN_POINT('Ctrl Pts',(-17.1454262858043,14.6515481598068,
0.));
#203969=CARTESIAN_POINT('Ctrl Pts',(-17.1458462295271,14.6519131634508,
0.));
#203970=CARTESIAN_POINT('Ctrl Pts',(-17.1466998098673,14.6526624064978,
0.));
#203971=CARTESIAN_POINT('Ctrl Pts',(-17.147876394491,14.6537016966184,0.));
#203972=CARTESIAN_POINT('Ctrl Pts',(-17.1493641837558,14.655024862281,0.));
#203973=CARTESIAN_POINT('Ctrl Pts',(-17.1511476869496,14.6566237952435,
0.));
#203974=CARTESIAN_POINT('Ctrl Pts',(-17.1532107762718,14.6584900555302,
0.));
#203975=CARTESIAN_POINT('Ctrl Pts',(-17.1555401986401,14.6606167169642,
0.));
#203976=CARTESIAN_POINT('Ctrl Pts',(-17.1581262646789,14.6629987285992,
0.));
#203977=CARTESIAN_POINT('Ctrl Pts',(-17.1609609517369,14.6656319165057,
0.));
#203978=CARTESIAN_POINT('Ctrl Pts',(-17.1640366762305,14.6685123374423,
0.));
#203979=CARTESIAN_POINT('Ctrl Pts',(-17.167344972302,14.671635583332,0.));
#203980=CARTESIAN_POINT('Ctrl Pts',(-17.1708771619129,14.6749971333867,
0.));
#203981=CARTESIAN_POINT('Ctrl Pts',(-17.1746247499057,14.6785925615677,
0.));
#203982=CARTESIAN_POINT('Ctrl Pts',(-17.1785800350826,14.6824178576167,
0.));
#203983=CARTESIAN_POINT('Ctrl Pts',(-17.182736158472,14.686469452232,0.));
#203984=CARTESIAN_POINT('Ctrl Pts',(-17.1870867909918,14.6907440526958,
0.));
#203985=CARTESIAN_POINT('Ctrl Pts',(-17.1916259308415,14.6952385361705,
0.));
#203986=CARTESIAN_POINT('Ctrl Pts',(-17.1963476411694,14.699949811582,0.));
#203987=CARTESIAN_POINT('Ctrl Pts',(-17.2012461084268,14.7048748502663,
0.));
#203988=CARTESIAN_POINT('Ctrl Pts',(-17.2063157097315,14.7100107213586,
0.));
#203989=CARTESIAN_POINT('Ctrl Pts',(-17.2115510835989,14.7153546289339,
0.));
#203990=CARTESIAN_POINT('Ctrl Pts',(-17.2169471814256,14.7209039390327,
0.));
#203991=CARTESIAN_POINT('Ctrl Pts',(-17.2224992099667,14.7266561494282,
0.));
#203992=CARTESIAN_POINT('Ctrl Pts',(-17.2282025904314,14.7326088681163,
0.));
#203993=CARTESIAN_POINT('Ctrl Pts',(-17.2340529062076,14.7387597858116,
0.));
#203994=CARTESIAN_POINT('Ctrl Pts',(-17.2400458713565,14.7451066593792,
0.));
#203995=CARTESIAN_POINT('Ctrl Pts',(-17.2461773413288,14.7516473175124,
0.));
#203996=CARTESIAN_POINT('Ctrl Pts',(-17.2524433146837,14.7583796616617,
0.));
#203997=CARTESIAN_POINT('Ctrl Pts',(-17.2588399401465,14.7653016697591,
0.));
#203998=CARTESIAN_POINT('Ctrl Pts',(-17.2653635155319,14.7724113956731,
0.));
#203999=CARTESIAN_POINT('Ctrl Pts',(-17.2720104735194,14.7797069617804,
0.));
#204000=CARTESIAN_POINT('Ctrl Pts',(-17.2787773704849,14.787186553128,0.));
#204001=CARTESIAN_POINT('Ctrl Pts',(-17.2856608733196,14.7948484105249,
0.));
#204002=CARTESIAN_POINT('Ctrl Pts',(-17.2926577496513,14.8026908254276,
0.));
#204003=CARTESIAN_POINT('Ctrl Pts',(-17.299764866148,14.8107121391035,0.));
#204004=CARTESIAN_POINT('Ctrl Pts',(-17.3069791853706,14.8189107410162,
0.));
#204005=CARTESIAN_POINT('Ctrl Pts',(-17.3142977632659,14.8272850675379,
0.));
#204006=CARTESIAN_POINT('Ctrl Pts',(-17.3217177462101,14.8358336004197,
0.));
#204007=CARTESIAN_POINT('Ctrl Pts',(-17.3292363662605,14.8445548643508,
0.));
#204008=CARTESIAN_POINT('Ctrl Pts',(-17.336850936485,14.8534474245433,0.));
#204009=CARTESIAN_POINT('Ctrl Pts',(-17.3445588463475,14.8625098843417,
0.));
#204010=CARTESIAN_POINT('Ctrl Pts',(-17.3523575568645,14.8717408826955,
0.));
#204011=CARTESIAN_POINT('Ctrl Pts',(-17.3602445978161,14.8811390927423,
0.));
#204012=CARTESIAN_POINT('Ctrl Pts',(-17.3682175653235,14.8907032205788,
0.));
#204013=CARTESIAN_POINT('Ctrl Pts',(-17.3762741193076,14.900432003961,0.));
#204014=CARTESIAN_POINT('Ctrl Pts',(-17.3844119809824,14.9103242110057,
0.));
#204015=CARTESIAN_POINT('Ctrl Pts',(-17.3926289303986,14.9203786389342,
0.));
#204016=CARTESIAN_POINT('Ctrl Pts',(-17.4009228040749,14.9305941128757,
0.));
#204017=CARTESIAN_POINT('Ctrl Pts',(-17.4092914926071,14.940969484645,0.));
#204018=CARTESIAN_POINT('Ctrl Pts',(-17.4177329382828,14.9515036315143,
0.));
#204019=CARTESIAN_POINT('Ctrl Pts',(-17.426245132709,14.9621954549827,0.));
#204020=CARTESIAN_POINT('Ctrl Pts',(-17.4348261151396,14.9730438799452,
0.));
#204021=CARTESIAN_POINT('Ctrl Pts',(-17.4434739707773,14.9840478538358,
0.));
#204022=CARTESIAN_POINT('Ctrl Pts',(-17.4521868291004,14.9952063457778,
0.));
#204023=CARTESIAN_POINT('Ctrl Pts',(-17.4609628621418,15.0065183456921,
0.));
#204024=CARTESIAN_POINT('Ctrl Pts',(-17.4698002829357,15.0179828635086,
0.));
#204025=CARTESIAN_POINT('Ctrl Pts',(-17.4786973441417,15.029598928488,0.));
#204026=CARTESIAN_POINT('Ctrl Pts',(-17.4876523366178,15.0413655884993,
0.));
#204027=CARTESIAN_POINT('Ctrl Pts',(-17.4966635880245,15.0532819093085,
0.));
#204028=CARTESIAN_POINT('Ctrl Pts',(-17.5057294613874,15.0653469738306,
0.));
#204029=CARTESIAN_POINT('Ctrl Pts',(-17.5148483539684,15.0775598815748,
0.));
#204030=CARTESIAN_POINT('Ctrl Pts',(-17.5240186961788,15.0899197481082,
0.));
#204031=CARTESIAN_POINT('Ctrl Pts',(-17.5332389504829,15.1024257045033,
0.));
#204032=CARTESIAN_POINT('Ctrl Pts',(-17.5425076102966,15.1150768967729,
0.));
#204033=CARTESIAN_POINT('Ctrl Pts',(-17.5518231989122,15.127872485314,0.));
#204034=CARTESIAN_POINT('Ctrl Pts',(-17.5611842686196,15.1408116444877,
0.));
#204035=CARTESIAN_POINT('Ctrl Pts',(-17.570589399803,15.1538935621714,0.));
#204036=CARTESIAN_POINT('Ctrl Pts',(-17.5800372000539,15.1671174393136,
0.));
#204037=CARTESIAN_POINT('Ctrl Pts',(-17.5895263032592,15.1804824894605,
0.));
#204038=CARTESIAN_POINT('Ctrl Pts',(-17.5990553687595,15.1939879383268,
0.));
#204039=CARTESIAN_POINT('Ctrl Pts',(-17.6086230806497,15.2076330234686,
0.));
#204040=CARTESIAN_POINT('Ctrl Pts',(-17.6182281470467,15.22141699392,0.));
#204041=CARTESIAN_POINT('Ctrl Pts',(-17.6278692993765,15.2353391098367,
0.));
#204042=CARTESIAN_POINT('Ctrl Pts',(-17.637545291637,15.2493986421091,0.));
#204043=CARTESIAN_POINT('Ctrl Pts',(-17.6472548997329,15.263594872029,0.));
#204044=CARTESIAN_POINT('Ctrl Pts',(-17.6569969209,15.2779270910238,0.));
#204045=CARTESIAN_POINT('Ctrl Pts',(-17.6667701731041,15.2923946003598,
0.));
#204046=CARTESIAN_POINT('Ctrl Pts',(-17.6765734944559,15.3069967108501,
0.));
#204047=CARTESIAN_POINT('Ctrl Pts',(-17.6864057426052,15.3217327425341,
0.));
#204048=CARTESIAN_POINT('Ctrl Pts',(-17.6962657941984,15.3366020244069,
0.));
#204049=CARTESIAN_POINT('Ctrl Pts',(-17.7061525444044,15.3516038942064,
0.));
#204050=CARTESIAN_POINT('Ctrl Pts',(-17.7160649064208,15.3667376981702,
0.));
#204051=CARTESIAN_POINT('Ctrl Pts',(-17.7260018109923,15.3820027907965,
0.));
#204052=CARTESIAN_POINT('Ctrl Pts',(-17.7359622059143,15.3973985345796,
0.));
#204053=CARTESIAN_POINT('Ctrl Pts',(-17.7459450555803,15.4129242997828,
0.));
#204054=CARTESIAN_POINT('Ctrl Pts',(-17.7559493405871,15.4285794642658,
0.));
#204055=CARTESIAN_POINT('Ctrl Pts',(-17.765974057326,15.4443634132865,0.));
#204056=CARTESIAN_POINT('Ctrl Pts',(-17.7760182175817,15.4602755393019,
0.));
#204057=CARTESIAN_POINT('Ctrl Pts',(-17.7860808481229,15.4763152417506,
0.));
#204058=CARTESIAN_POINT('Ctrl Pts',(-17.7961609903161,15.4924819268529,
0.));
#204059=CARTESIAN_POINT('Ctrl Pts',(-17.8062576997964,15.5087750074728,
0.));
#204060=CARTESIAN_POINT('Ctrl Pts',(-17.8163700461263,15.5251939029558,
0.));
#204061=CARTESIAN_POINT('Ctrl Pts',(-17.8264971124606,15.5417380389639,
0.));
#204062=CARTESIAN_POINT('Ctrl Pts',(-17.8366379952078,15.5584068472976,
0.));
#204063=CARTESIAN_POINT('Ctrl Pts',(-17.8467918036977,15.5751997657153,
0.));
#204064=CARTESIAN_POINT('Ctrl Pts',(-17.8569576598996,15.5921162378183,
0.));
#204065=CARTESIAN_POINT('Ctrl Pts',(-17.8671346981388,15.6091557129205,
0.));
#204066=CARTESIAN_POINT('Ctrl Pts',(-17.8773220648125,15.6263176459107,
0.));
#204067=CARTESIAN_POINT('Ctrl Pts',(-17.8875189181095,15.6436014971088,
0.));
#204068=CARTESIAN_POINT('Ctrl Pts',(-17.8977244277247,15.6610067321036,
0.));
#204069=CARTESIAN_POINT('Ctrl Pts',(-17.9079377746118,15.6785328216467,
0.));
#204070=CARTESIAN_POINT('Ctrl Pts',(-17.918158150746,15.6961792415526,0.));
#204071=CARTESIAN_POINT('Ctrl Pts',(-17.9283847588837,15.713945472584,0.));
#204072=CARTESIAN_POINT('Ctrl Pts',(-17.9386168123261,15.7318310003334,
0.));
#204073=CARTESIAN_POINT('Ctrl Pts',(-17.9488535346776,15.7498353150856,
0.));
#204074=CARTESIAN_POINT('Ctrl Pts',(-17.9590941596236,15.7679579117072,
0.));
#204075=CARTESIAN_POINT('Ctrl Pts',(-17.9693379307297,15.786198289572,0.));
#204076=CARTESIAN_POINT('Ctrl Pts',(-17.9795841012383,15.8045559524674,
0.));
#204077=CARTESIAN_POINT('Ctrl Pts',(-17.9898319338664,15.8230304084963,
0.));
#204078=CARTESIAN_POINT('Ctrl Pts',(-18.0000807006055,15.8416211699681,
0.));
#204079=CARTESIAN_POINT('Ctrl Pts',(-18.010329682521,15.8603277532834,0.));
#204080=CARTESIAN_POINT('Ctrl Pts',(-18.0205781695773,15.8791496788685,
0.));
#204081=CARTESIAN_POINT('Ctrl Pts',(-18.0308254604638,15.8980864711043,
0.));
#204082=CARTESIAN_POINT('Ctrl Pts',(-18.0410708624208,15.9171376582436,
0.));
#204083=CARTESIAN_POINT('Ctrl Pts',(-18.0513136910691,15.9363027723244,
0.));
#204084=CARTESIAN_POINT('Ctrl Pts',(-18.061553270236,15.9555813490645,0.));
#204085=CARTESIAN_POINT('Ctrl Pts',(-18.071788931796,15.9749729277848,0.));
#204086=CARTESIAN_POINT('Ctrl Pts',(-18.0820200155239,15.9944770513616,
0.));
#204087=CARTESIAN_POINT('Ctrl Pts',(-18.0922458689464,16.0140932661612,
0.));
#204088=CARTESIAN_POINT('Ctrl Pts',(-18.1024658471966,16.0338211219693,
0.));
#204089=CARTESIAN_POINT('Ctrl Pts',(-18.1126793128688,16.0536601719124,
0.));
#204090=CARTESIAN_POINT('Ctrl Pts',(-18.1228856358746,16.0736099723664,
0.));
#204091=CARTESIAN_POINT('Ctrl Pts',(-18.1330841933099,16.0936700829108,
0.));
#204092=CARTESIAN_POINT('Ctrl Pts',(-18.1432743693231,16.113840066279,0.));
#204093=CARTESIAN_POINT('Ctrl Pts',(-18.1534555549851,16.1341194882987,
0.));
#204094=CARTESIAN_POINT('Ctrl Pts',(-18.1636271481616,16.1545079178261,
0.));
#204095=CARTESIAN_POINT('Ctrl Pts',(-18.1737885533852,16.1750049266673,
0.));
#204096=CARTESIAN_POINT('Ctrl Pts',(-18.1839391817335,16.1956100895076,
0.));
#204097=CARTESIAN_POINT('Ctrl Pts',(-18.1940784507232,16.2163229838878,
0.));
#204098=CARTESIAN_POINT('Ctrl Pts',(-18.2042057842037,16.237143190164,0.));
#204099=CARTESIAN_POINT('Ctrl Pts',(-18.214320612253,16.2580702914615,0.));
#204100=CARTESIAN_POINT('Ctrl Pts',(-18.2244223710745,16.2791038736223,
0.));
#204101=CARTESIAN_POINT('Ctrl Pts',(-18.2345105028981,16.3002435251378,
0.));
#204102=CARTESIAN_POINT('Ctrl Pts',(-18.2445844558742,16.3214888370988,
0.));
#204103=CARTESIAN_POINT('Ctrl Pts',(-18.2546436839609,16.342839403159,0.));
#204104=CARTESIAN_POINT('Ctrl Pts',(-18.2646876468169,16.3642948194869,
0.));
#204105=CARTESIAN_POINT('Ctrl Pts',(-18.2747158096934,16.385854684708,0.));
#204106=CARTESIAN_POINT('Ctrl Pts',(-18.2847276433308,16.4075185998454,
0.));
#204107=CARTESIAN_POINT('Ctrl Pts',(-18.2947226238509,16.4292861682377,
0.));
#204108=CARTESIAN_POINT('Ctrl Pts',(-18.3047002326858,16.4511569955231,
0.));
#204109=CARTESIAN_POINT('Ctrl Pts',(-18.3146599565229,16.4731306896439,
0.));
#204110=CARTESIAN_POINT('Ctrl Pts',(-18.3246012872468,16.4952068608344,
0.));
#204111=CARTESIAN_POINT('Ctrl Pts',(-18.3345237218864,16.5173851216045,
0.));
#204112=CARTESIAN_POINT('Ctrl Pts',(-18.3444267625601,16.5396650867139,
0.));
#204113=CARTESIAN_POINT('Ctrl Pts',(-18.3543099164331,16.5620463731414,
0.));
#204114=CARTESIAN_POINT('Ctrl Pts',(-18.364172695589,16.5845286000218,0.));
#204115=CARTESIAN_POINT('Ctrl Pts',(-18.3740146168879,16.6071113885711,
0.));
#204116=CARTESIAN_POINT('Ctrl Pts',(-18.3838352018327,16.6297943620056,
0.));
#204117=CARTESIAN_POINT('Ctrl Pts',(-18.3936339764332,16.6525771454513,
0.));
#204118=CARTESIAN_POINT('Ctrl Pts',(-18.4034104710789,16.6754593658513,
0.));
#204119=CARTESIAN_POINT('Ctrl Pts',(-18.413164220399,16.698440651849,0.));
#204120=CARTESIAN_POINT('Ctrl Pts',(-18.4228947633186,16.7215206338818,
0.));
#204121=CARTESIAN_POINT('Ctrl Pts',(-18.4326016431392,16.7446989442882,
0.));
#204122=CARTESIAN_POINT('Ctrl Pts',(-18.4422844076099,16.7679752173992,
0.));
#204123=CARTESIAN_POINT('Ctrl Pts',(-18.4519426090124,16.791349089629,0.));
#204124=CARTESIAN_POINT('Ctrl Pts',(-18.4615758042305,16.8148201995472,
0.));
#204125=CARTESIAN_POINT('Ctrl Pts',(-18.4711835548622,16.8383881879707,
0.));
#204126=CARTESIAN_POINT('Ctrl Pts',(-18.4807654268769,16.8620526977169,
0.));
#204127=CARTESIAN_POINT('Ctrl Pts',(-18.4903209902226,16.8858133733086,
0.));
#204128=CARTESIAN_POINT('Ctrl Pts',(-18.4998498184619,16.9096698606942,
0.));
#204129=CARTESIAN_POINT('Ctrl Pts',(-18.5093514883835,16.9336218069353,
0.));
#204130=CARTESIAN_POINT('Ctrl Pts',(-18.518825579666,16.957668859934,0.));
#204131=CARTESIAN_POINT('Ctrl Pts',(-18.5282716744198,16.9818106680382,
0.));
#204132=CARTESIAN_POINT('Ctrl Pts',(-18.5376893576961,17.0060468805099,
0.));
#204133=CARTESIAN_POINT('Ctrl Pts',(-18.5470782182089,17.030377148174,0.));
#204134=CARTESIAN_POINT('Ctrl Pts',(-18.5564378489628,17.0548011239751,
0.));
#204135=CARTESIAN_POINT('Ctrl Pts',(-18.5657678479788,17.0793184636079,
0.));
#204136=CARTESIAN_POINT('Ctrl Pts',(-18.5750678188543,17.1039288260001,
0.));
#204137=CARTESIAN_POINT('Ctrl Pts',(-18.5843373717253,17.1286318741185,
0.));
#204138=CARTESIAN_POINT('Ctrl Pts',(-18.5935761222833,17.1534272741646,
0.));
#204139=CARTESIAN_POINT('Ctrl Pts',(-18.6027836898826,17.1783146940131,
0.));
#204140=CARTESIAN_POINT('Ctrl Pts',(-18.6119596959957,17.2032938019288,
0.));
#204141=CARTESIAN_POINT('Ctrl Pts',(-18.6211037624041,17.2283642650519,
0.));
#204142=CARTESIAN_POINT('Ctrl Pts',(-18.630215509794,17.2535257482186,0.));
#204143=CARTESIAN_POINT('Ctrl Pts',(-18.639294555474,17.278777912021,0.));
#204144=CARTESIAN_POINT('Ctrl Pts',(-18.6483405141853,17.3041204135069,
0.));
#204145=CARTESIAN_POINT('Ctrl Pts',(-18.6573530024019,17.3295529098612,
0.));
#204146=CARTESIAN_POINT('Ctrl Pts',(-18.6663316416569,17.3550750612438,
0.));
#204147=CARTESIAN_POINT('Ctrl Pts',(-18.6752760624045,17.3806865340744,
0.));
#204148=CARTESIAN_POINT('Ctrl Pts',(-18.6841859073472,17.4063870038563,
0.));
#204149=CARTESIAN_POINT('Ctrl Pts',(-18.6930608357421,17.4321761588148,
0.));
#204150=CARTESIAN_POINT('Ctrl Pts',(-18.7019005250322,17.4580537012764,
0.));
#204151=CARTESIAN_POINT('Ctrl Pts',(-18.7107046613941,17.4840193397176,
0.));
#204152=CARTESIAN_POINT('Ctrl Pts',(-18.7194729318128,17.5100727820891,
0.));
#204153=CARTESIAN_POINT('Ctrl Pts',(-18.728205015716,17.5362137287604,0.));
#204154=CARTESIAN_POINT('Ctrl Pts',(-18.7369005764558,17.5624418653248,
0.));
#204155=CARTESIAN_POINT('Ctrl Pts',(-18.7455592536667,17.5887568561361,
0.));
#204156=CARTESIAN_POINT('Ctrl Pts',(-18.7541806530935,17.6151583356988,
0.));
#204157=CARTESIAN_POINT('Ctrl Pts',(-18.7627643613139,17.6416459210646,
0.));
#204158=CARTESIAN_POINT('Ctrl Pts',(-18.7713099642673,17.6682192274197,
0.));
#204159=CARTESIAN_POINT('Ctrl Pts',(-18.7798170641305,17.6948778822981,
0.));
#204160=CARTESIAN_POINT('Ctrl Pts',(-18.7882852976016,17.7216215409019,
0.));
#204161=CARTESIAN_POINT('Ctrl Pts',(-18.7967143519444,17.7484498996916,
0.));
#204162=CARTESIAN_POINT('Ctrl Pts',(-18.8051039860543,17.7753627137898,
0.));
#204163=CARTESIAN_POINT('Ctrl Pts',(-18.8134540340581,17.8023598011135,
0.));
#204164=CARTESIAN_POINT('Ctrl Pts',(-18.8217643886368,17.8294410311105,
0.));
#204165=CARTESIAN_POINT('Ctrl Pts',(-18.8300349896187,17.8566063174871,
0.));
#204166=CARTESIAN_POINT('Ctrl Pts',(-18.8366196462746,17.8784057509434,
0.));
#204167=CARTESIAN_POINT('Ctrl Pts',(-18.8415402351882,17.8947931177853,
0.));
#204168=CARTESIAN_POINT('Ctrl Pts',(-18.8448126709726,17.9057348246611,
0.));
#204169=CARTESIAN_POINT('Ctrl Pts',(-18.8464468996588,17.9112098770111,
0.));
#204170=CARTESIAN_POINT('',(-18.8464468996588,17.9112098770111,0.));
#204171=CARTESIAN_POINT('Origin',(-12.1729687575668,17.7219872369693,0.));
#204172=CARTESIAN_POINT('',(-12.7689476255363,18.5896416359912,0.));
#204173=CARTESIAN_POINT('',(-12.7689476255363,18.5896416359912,0.));
#204174=CARTESIAN_POINT('',(-6.08648437878338,8.86099361848466,0.));
#204175=CARTESIAN_POINT('Ctrl Pts',(-17.9112098770111,18.8464468996588,
0.));
#204176=CARTESIAN_POINT('Ctrl Pts',(-17.9112098770111,18.8464468996588,
12.));
#204177=CARTESIAN_POINT('Ctrl Pts',(-17.9057348246595,18.8448126709691,
0.));
#204178=CARTESIAN_POINT('Ctrl Pts',(-17.9057348246595,18.8448126709691,
12.));
#204179=CARTESIAN_POINT('Ctrl Pts',(-17.8947931177807,18.8415402351786,
0.));
#204180=CARTESIAN_POINT('Ctrl Pts',(-17.8947931177807,18.8415402351786,
12.));
#204181=CARTESIAN_POINT('Ctrl Pts',(-17.8784057509356,18.8366196462581,
0.));
#204182=CARTESIAN_POINT('Ctrl Pts',(-17.8784057509356,18.8366196462581,
12.));
#204183=CARTESIAN_POINT('Ctrl Pts',(-17.8566063174771,18.8300349895974,
0.));
#204184=CARTESIAN_POINT('Ctrl Pts',(-17.8566063174771,18.8300349895974,
12.));
#204185=CARTESIAN_POINT('Ctrl Pts',(-17.8294410311006,18.8217643886157,
0.));
#204186=CARTESIAN_POINT('Ctrl Pts',(-17.8294410311006,18.8217643886157,
12.));
#204187=CARTESIAN_POINT('Ctrl Pts',(-17.8023598011057,18.8134540340417,
0.));
#204188=CARTESIAN_POINT('Ctrl Pts',(-17.8023598011057,18.8134540340417,
12.));
#204189=CARTESIAN_POINT('Ctrl Pts',(-17.7753627137853,18.8051039860448,
0.));
#204190=CARTESIAN_POINT('Ctrl Pts',(-17.7753627137853,18.8051039860448,
12.));
#204191=CARTESIAN_POINT('Ctrl Pts',(-17.7484498996905,18.7967143519419,
0.));
#204192=CARTESIAN_POINT('Ctrl Pts',(-17.7484498996905,18.7967143519419,
12.));
#204193=CARTESIAN_POINT('Ctrl Pts',(-17.7216215409035,18.7882852976049,
0.));
#204194=CARTESIAN_POINT('Ctrl Pts',(-17.7216215409035,18.7882852976049,
12.));
#204195=CARTESIAN_POINT('Ctrl Pts',(-17.6948778823014,18.7798170641374,
0.));
#204196=CARTESIAN_POINT('Ctrl Pts',(-17.6948778823014,18.7798170641374,
12.));
#204197=CARTESIAN_POINT('Ctrl Pts',(-17.6682192274236,18.7713099642754,
0.));
#204198=CARTESIAN_POINT('Ctrl Pts',(-17.6682192274236,18.7713099642754,
12.));
#204199=CARTESIAN_POINT('Ctrl Pts',(-17.6416459210681,18.762764361321,0.));
#204200=CARTESIAN_POINT('Ctrl Pts',(-17.6416459210681,18.762764361321,12.));
#204201=CARTESIAN_POINT('Ctrl Pts',(-17.6151583357012,18.7541806530984,
0.));
#204202=CARTESIAN_POINT('Ctrl Pts',(-17.6151583357012,18.7541806530984,
12.));
#204203=CARTESIAN_POINT('Ctrl Pts',(-17.5887568561371,18.7455592536687,
0.));
#204204=CARTESIAN_POINT('Ctrl Pts',(-17.5887568561371,18.7455592536687,
12.));
#204205=CARTESIAN_POINT('Ctrl Pts',(-17.5624418653245,18.7369005764553,
0.));
#204206=CARTESIAN_POINT('Ctrl Pts',(-17.5624418653245,18.7369005764553,
12.));
#204207=CARTESIAN_POINT('Ctrl Pts',(-17.5362137287593,18.7282050157138,
0.));
#204208=CARTESIAN_POINT('Ctrl Pts',(-17.5362137287593,18.7282050157138,
12.));
#204209=CARTESIAN_POINT('Ctrl Pts',(-17.5100727820876,18.7194729318098,
0.));
#204210=CARTESIAN_POINT('Ctrl Pts',(-17.5100727820876,18.7194729318098,
12.));
#204211=CARTESIAN_POINT('Ctrl Pts',(-17.4840193397162,18.7107046613912,
0.));
#204212=CARTESIAN_POINT('Ctrl Pts',(-17.4840193397162,18.7107046613912,
12.));
#204213=CARTESIAN_POINT('Ctrl Pts',(-17.4580537012753,18.70190052503,0.));
#204214=CARTESIAN_POINT('Ctrl Pts',(-17.4580537012753,18.70190052503,12.));
#204215=CARTESIAN_POINT('Ctrl Pts',(-17.4321761588142,18.6930608357409,
0.));
#204216=CARTESIAN_POINT('Ctrl Pts',(-17.4321761588142,18.6930608357409,
12.));
#204217=CARTESIAN_POINT('Ctrl Pts',(-17.4063870038562,18.6841859073471,
0.));
#204218=CARTESIAN_POINT('Ctrl Pts',(-17.4063870038562,18.6841859073471,
12.));
#204219=CARTESIAN_POINT('Ctrl Pts',(-17.3806865340747,18.6752760624052,
0.));
#204220=CARTESIAN_POINT('Ctrl Pts',(-17.3806865340747,18.6752760624052,
12.));
#204221=CARTESIAN_POINT('Ctrl Pts',(-17.3550750612443,18.6663316416582,
0.));
#204222=CARTESIAN_POINT('Ctrl Pts',(-17.3550750612443,18.6663316416582,
12.));
#204223=CARTESIAN_POINT('Ctrl Pts',(-17.3295529098618,18.6573530024033,
0.));
#204224=CARTESIAN_POINT('Ctrl Pts',(-17.3295529098618,18.6573530024033,
12.));
#204225=CARTESIAN_POINT('Ctrl Pts',(-17.3041204135074,18.6483405141865,
0.));
#204226=CARTESIAN_POINT('Ctrl Pts',(-17.3041204135074,18.6483405141865,
12.));
#204227=CARTESIAN_POINT('Ctrl Pts',(-17.2787779120213,18.6392945554748,
0.));
#204228=CARTESIAN_POINT('Ctrl Pts',(-17.2787779120213,18.6392945554748,
12.));
#204229=CARTESIAN_POINT('Ctrl Pts',(-17.2535257482187,18.6302155097943,
0.));
#204230=CARTESIAN_POINT('Ctrl Pts',(-17.2535257482187,18.6302155097943,
12.));
#204231=CARTESIAN_POINT('Ctrl Pts',(-17.2283642650518,18.6211037624038,
0.));
#204232=CARTESIAN_POINT('Ctrl Pts',(-17.2283642650518,18.6211037624038,
12.));
#204233=CARTESIAN_POINT('Ctrl Pts',(-17.2032938019284,18.6119596959949,
0.));
#204234=CARTESIAN_POINT('Ctrl Pts',(-17.2032938019284,18.6119596959949,
12.));
#204235=CARTESIAN_POINT('Ctrl Pts',(-17.1783146940127,18.6027836898817,
0.));
#204236=CARTESIAN_POINT('Ctrl Pts',(-17.1783146940127,18.6027836898817,
12.));
#204237=CARTESIAN_POINT('Ctrl Pts',(-17.1534272741643,18.5935761222825,
0.));
#204238=CARTESIAN_POINT('Ctrl Pts',(-17.1534272741643,18.5935761222825,
12.));
#204239=CARTESIAN_POINT('Ctrl Pts',(-17.1286318741183,18.5843373717247,
0.));
#204240=CARTESIAN_POINT('Ctrl Pts',(-17.1286318741183,18.5843373717247,
12.));
#204241=CARTESIAN_POINT('Ctrl Pts',(-17.1039288260001,18.5750678188542,
0.));
#204242=CARTESIAN_POINT('Ctrl Pts',(-17.1039288260001,18.5750678188542,
12.));
#204243=CARTESIAN_POINT('Ctrl Pts',(-17.0793184636079,18.5657678479789,
0.));
#204244=CARTESIAN_POINT('Ctrl Pts',(-17.0793184636079,18.5657678479789,
12.));
#204245=CARTESIAN_POINT('Ctrl Pts',(-17.0548011239751,18.556437848963,0.));
#204246=CARTESIAN_POINT('Ctrl Pts',(-17.0548011239751,18.556437848963,12.));
#204247=CARTESIAN_POINT('Ctrl Pts',(-17.0303771481738,18.547078218209,0.));
#204248=CARTESIAN_POINT('Ctrl Pts',(-17.0303771481738,18.547078218209,12.));
#204249=CARTESIAN_POINT('Ctrl Pts',(-17.0060468805097,18.5376893576961,
0.));
#204250=CARTESIAN_POINT('Ctrl Pts',(-17.0060468805097,18.5376893576961,
12.));
#204251=CARTESIAN_POINT('Ctrl Pts',(-16.981810668038,18.5282716744197,0.));
#204252=CARTESIAN_POINT('Ctrl Pts',(-16.981810668038,18.5282716744197,12.));
#204253=CARTESIAN_POINT('Ctrl Pts',(-16.9576688599339,18.5188255796659,
0.));
#204254=CARTESIAN_POINT('Ctrl Pts',(-16.9576688599339,18.5188255796659,
12.));
#204255=CARTESIAN_POINT('Ctrl Pts',(-16.9336218069353,18.5093514883835,
0.));
#204256=CARTESIAN_POINT('Ctrl Pts',(-16.9336218069353,18.5093514883835,
12.));
#204257=CARTESIAN_POINT('Ctrl Pts',(-16.9096698606943,18.499849818462,0.));
#204258=CARTESIAN_POINT('Ctrl Pts',(-16.9096698606943,18.499849818462,12.));
#204259=CARTESIAN_POINT('Ctrl Pts',(-16.8858133733088,18.4903209902227,
0.));
#204260=CARTESIAN_POINT('Ctrl Pts',(-16.8858133733088,18.4903209902227,
12.));
#204261=CARTESIAN_POINT('Ctrl Pts',(-16.8620526977171,18.480765426877,0.));
#204262=CARTESIAN_POINT('Ctrl Pts',(-16.8620526977171,18.480765426877,12.));
#204263=CARTESIAN_POINT('Ctrl Pts',(-16.8383881879709,18.4711835548623,
0.));
#204264=CARTESIAN_POINT('Ctrl Pts',(-16.8383881879709,18.4711835548623,
12.));
#204265=CARTESIAN_POINT('Ctrl Pts',(-16.8148201995472,18.4615758042305,
0.));
#204266=CARTESIAN_POINT('Ctrl Pts',(-16.8148201995472,18.4615758042305,
12.));
#204267=CARTESIAN_POINT('Ctrl Pts',(-16.791349089629,18.4519426090123,0.));
#204268=CARTESIAN_POINT('Ctrl Pts',(-16.791349089629,18.4519426090123,12.));
#204269=CARTESIAN_POINT('Ctrl Pts',(-16.7679752173992,18.44228440761,0.));
#204270=CARTESIAN_POINT('Ctrl Pts',(-16.7679752173992,18.44228440761,12.));
#204271=CARTESIAN_POINT('Ctrl Pts',(-16.7446989442882,18.4326016431392,
0.));
#204272=CARTESIAN_POINT('Ctrl Pts',(-16.7446989442882,18.4326016431392,
12.));
#204273=CARTESIAN_POINT('Ctrl Pts',(-16.7215206338818,18.4228947633187,
0.));
#204274=CARTESIAN_POINT('Ctrl Pts',(-16.7215206338818,18.4228947633187,
12.));
#204275=CARTESIAN_POINT('Ctrl Pts',(-16.6984406518491,18.413164220399,0.));
#204276=CARTESIAN_POINT('Ctrl Pts',(-16.6984406518491,18.413164220399,12.));
#204277=CARTESIAN_POINT('Ctrl Pts',(-16.6754593658513,18.403410471079,0.));
#204278=CARTESIAN_POINT('Ctrl Pts',(-16.6754593658513,18.403410471079,12.));
#204279=CARTESIAN_POINT('Ctrl Pts',(-16.6525771454513,18.3936339764332,
0.));
#204280=CARTESIAN_POINT('Ctrl Pts',(-16.6525771454513,18.3936339764332,
12.));
#204281=CARTESIAN_POINT('Ctrl Pts',(-16.6297943620056,18.3838352018327,
0.));
#204282=CARTESIAN_POINT('Ctrl Pts',(-16.6297943620056,18.3838352018327,
12.));
#204283=CARTESIAN_POINT('Ctrl Pts',(-16.607111388571,18.3740146168879,0.));
#204284=CARTESIAN_POINT('Ctrl Pts',(-16.607111388571,18.3740146168879,12.));
#204285=CARTESIAN_POINT('Ctrl Pts',(-16.5845286000217,18.3641726955889,
0.));
#204286=CARTESIAN_POINT('Ctrl Pts',(-16.5845286000217,18.3641726955889,
12.));
#204287=CARTESIAN_POINT('Ctrl Pts',(-16.5620463731413,18.354309916433,0.));
#204288=CARTESIAN_POINT('Ctrl Pts',(-16.5620463731413,18.354309916433,12.));
#204289=CARTESIAN_POINT('Ctrl Pts',(-16.5396650867139,18.34442676256,0.));
#204290=CARTESIAN_POINT('Ctrl Pts',(-16.5396650867139,18.34442676256,12.));
#204291=CARTESIAN_POINT('Ctrl Pts',(-16.5173851216045,18.3345237218864,
0.));
#204292=CARTESIAN_POINT('Ctrl Pts',(-16.5173851216045,18.3345237218864,
12.));
#204293=CARTESIAN_POINT('Ctrl Pts',(-16.4952068608345,18.3246012872469,
0.));
#204294=CARTESIAN_POINT('Ctrl Pts',(-16.4952068608345,18.3246012872469,
12.));
#204295=CARTESIAN_POINT('Ctrl Pts',(-16.4731306896441,18.3146599565231,
0.));
#204296=CARTESIAN_POINT('Ctrl Pts',(-16.4731306896441,18.3146599565231,
12.));
#204297=CARTESIAN_POINT('Ctrl Pts',(-16.4511569955233,18.304700232686,0.));
#204298=CARTESIAN_POINT('Ctrl Pts',(-16.4511569955233,18.304700232686,12.));
#204299=CARTESIAN_POINT('Ctrl Pts',(-16.4292861682379,18.294722623851,0.));
#204300=CARTESIAN_POINT('Ctrl Pts',(-16.4292861682379,18.294722623851,12.));
#204301=CARTESIAN_POINT('Ctrl Pts',(-16.4075185998455,18.2847276433309,
0.));
#204302=CARTESIAN_POINT('Ctrl Pts',(-16.4075185998455,18.2847276433309,
12.));
#204303=CARTESIAN_POINT('Ctrl Pts',(-16.385854684708,18.2747158096934,0.));
#204304=CARTESIAN_POINT('Ctrl Pts',(-16.385854684708,18.2747158096934,12.));
#204305=CARTESIAN_POINT('Ctrl Pts',(-16.3642948194868,18.2646876468169,
0.));
#204306=CARTESIAN_POINT('Ctrl Pts',(-16.3642948194868,18.2646876468169,
12.));
#204307=CARTESIAN_POINT('Ctrl Pts',(-16.3428394031589,18.2546436839608,
0.));
#204308=CARTESIAN_POINT('Ctrl Pts',(-16.3428394031589,18.2546436839608,
12.));
#204309=CARTESIAN_POINT('Ctrl Pts',(-16.3214888370987,18.2445844558741,
0.));
#204310=CARTESIAN_POINT('Ctrl Pts',(-16.3214888370987,18.2445844558741,
12.));
#204311=CARTESIAN_POINT('Ctrl Pts',(-16.3002435251378,18.2345105028982,
0.));
#204312=CARTESIAN_POINT('Ctrl Pts',(-16.3002435251378,18.2345105028982,
12.));
#204313=CARTESIAN_POINT('Ctrl Pts',(-16.2791038736223,18.2244223710745,
0.));
#204314=CARTESIAN_POINT('Ctrl Pts',(-16.2791038736223,18.2244223710745,
12.));
#204315=CARTESIAN_POINT('Ctrl Pts',(-16.2580702914615,18.2143206122529,
0.));
#204316=CARTESIAN_POINT('Ctrl Pts',(-16.2580702914615,18.2143206122529,
12.));
#204317=CARTESIAN_POINT('Ctrl Pts',(-16.2371431901638,18.2042057842035,
0.));
#204318=CARTESIAN_POINT('Ctrl Pts',(-16.2371431901638,18.2042057842035,
12.));
#204319=CARTESIAN_POINT('Ctrl Pts',(-16.2163229838875,18.1940784507229,
0.));
#204320=CARTESIAN_POINT('Ctrl Pts',(-16.2163229838875,18.1940784507229,
12.));
#204321=CARTESIAN_POINT('Ctrl Pts',(-16.1956100895073,18.1839391817331,
0.));
#204322=CARTESIAN_POINT('Ctrl Pts',(-16.1956100895073,18.1839391817331,
12.));
#204323=CARTESIAN_POINT('Ctrl Pts',(-16.1750049266671,18.1737885533849,
0.));
#204324=CARTESIAN_POINT('Ctrl Pts',(-16.1750049266671,18.1737885533849,
12.));
#204325=CARTESIAN_POINT('Ctrl Pts',(-16.154507917826,18.1636271481615,0.));
#204326=CARTESIAN_POINT('Ctrl Pts',(-16.154507917826,18.1636271481615,12.));
#204327=CARTESIAN_POINT('Ctrl Pts',(-16.1341194882988,18.1534555549852,
0.));
#204328=CARTESIAN_POINT('Ctrl Pts',(-16.1341194882988,18.1534555549852,
12.));
#204329=CARTESIAN_POINT('Ctrl Pts',(-16.1138400662794,18.1432743693235,
0.));
#204330=CARTESIAN_POINT('Ctrl Pts',(-16.1138400662794,18.1432743693235,
12.));
#204331=CARTESIAN_POINT('Ctrl Pts',(-16.0936700829112,18.1330841933105,
0.));
#204332=CARTESIAN_POINT('Ctrl Pts',(-16.0936700829112,18.1330841933105,
12.));
#204333=CARTESIAN_POINT('Ctrl Pts',(-16.0736099723668,18.1228856358751,
0.));
#204334=CARTESIAN_POINT('Ctrl Pts',(-16.0736099723668,18.1228856358751,
12.));
#204335=CARTESIAN_POINT('Ctrl Pts',(-16.0536601719126,18.112679312869,0.));
#204336=CARTESIAN_POINT('Ctrl Pts',(-16.0536601719126,18.112679312869,12.));
#204337=CARTESIAN_POINT('Ctrl Pts',(-16.0338211219693,18.1024658471966,
0.));
#204338=CARTESIAN_POINT('Ctrl Pts',(-16.0338211219693,18.1024658471966,
12.));
#204339=CARTESIAN_POINT('Ctrl Pts',(-16.014093266161,18.0922458689462,0.));
#204340=CARTESIAN_POINT('Ctrl Pts',(-16.014093266161,18.0922458689462,12.));
#204341=CARTESIAN_POINT('Ctrl Pts',(-15.9944770513613,18.0820200155236,
0.));
#204342=CARTESIAN_POINT('Ctrl Pts',(-15.9944770513613,18.0820200155236,
12.));
#204343=CARTESIAN_POINT('Ctrl Pts',(-15.9749729277846,18.0717889317958,
0.));
#204344=CARTESIAN_POINT('Ctrl Pts',(-15.9749729277846,18.0717889317958,
12.));
#204345=CARTESIAN_POINT('Ctrl Pts',(-15.9555813490644,18.0615532702359,
0.));
#204346=CARTESIAN_POINT('Ctrl Pts',(-15.9555813490644,18.0615532702359,
12.));
#204347=CARTESIAN_POINT('Ctrl Pts',(-15.9363027723244,18.0513136910691,
0.));
#204348=CARTESIAN_POINT('Ctrl Pts',(-15.9363027723244,18.0513136910691,
12.));
#204349=CARTESIAN_POINT('Ctrl Pts',(-15.9171376582436,18.0410708624208,
0.));
#204350=CARTESIAN_POINT('Ctrl Pts',(-15.9171376582436,18.0410708624208,
12.));
#204351=CARTESIAN_POINT('Ctrl Pts',(-15.8980864711042,18.0308254604636,
0.));
#204352=CARTESIAN_POINT('Ctrl Pts',(-15.8980864711042,18.0308254604636,
12.));
#204353=CARTESIAN_POINT('Ctrl Pts',(-15.8791496788683,18.0205781695769,
0.));
#204354=CARTESIAN_POINT('Ctrl Pts',(-15.8791496788683,18.0205781695769,
12.));
#204355=CARTESIAN_POINT('Ctrl Pts',(-15.8603277532831,18.0103296825205,
0.));
#204356=CARTESIAN_POINT('Ctrl Pts',(-15.8603277532831,18.0103296825205,
12.));
#204357=CARTESIAN_POINT('Ctrl Pts',(-15.8416211699679,18.0000807006052,
0.));
#204358=CARTESIAN_POINT('Ctrl Pts',(-15.8416211699679,18.0000807006052,
12.));
#204359=CARTESIAN_POINT('Ctrl Pts',(-15.8230304084962,17.9898319338664,
0.));
#204360=CARTESIAN_POINT('Ctrl Pts',(-15.8230304084962,17.9898319338664,
12.));
#204361=CARTESIAN_POINT('Ctrl Pts',(-15.8045559524676,17.9795841012386,
0.));
#204362=CARTESIAN_POINT('Ctrl Pts',(-15.8045559524676,17.9795841012386,
12.));
#204363=CARTESIAN_POINT('Ctrl Pts',(-15.7861982895724,17.9693379307303,
0.));
#204364=CARTESIAN_POINT('Ctrl Pts',(-15.7861982895724,17.9693379307303,
12.));
#204365=CARTESIAN_POINT('Ctrl Pts',(-15.7679579117077,17.9590941596242,
0.));
#204366=CARTESIAN_POINT('Ctrl Pts',(-15.7679579117077,17.9590941596242,
12.));
#204367=CARTESIAN_POINT('Ctrl Pts',(-15.749835315086,17.9488535346781,0.));
#204368=CARTESIAN_POINT('Ctrl Pts',(-15.749835315086,17.9488535346781,12.));
#204369=CARTESIAN_POINT('Ctrl Pts',(-15.7318310003335,17.9386168123262,
0.));
#204370=CARTESIAN_POINT('Ctrl Pts',(-15.7318310003335,17.9386168123262,
12.));
#204371=CARTESIAN_POINT('Ctrl Pts',(-15.7139454725838,17.9283847588835,
0.));
#204372=CARTESIAN_POINT('Ctrl Pts',(-15.7139454725838,17.9283847588835,
12.));
#204373=CARTESIAN_POINT('Ctrl Pts',(-15.6961792415522,17.9181581507455,
0.));
#204374=CARTESIAN_POINT('Ctrl Pts',(-15.6961792415522,17.9181581507455,
12.));
#204375=CARTESIAN_POINT('Ctrl Pts',(-15.678532821646,17.9079377746111,0.));
#204376=CARTESIAN_POINT('Ctrl Pts',(-15.678532821646,17.9079377746111,12.));
#204377=CARTESIAN_POINT('Ctrl Pts',(-15.661006732103,17.897724427724,0.));
#204378=CARTESIAN_POINT('Ctrl Pts',(-15.661006732103,17.897724427724,12.));
#204379=CARTESIAN_POINT('Ctrl Pts',(-15.6436014971084,17.8875189181091,
0.));
#204380=CARTESIAN_POINT('Ctrl Pts',(-15.6436014971084,17.8875189181091,
12.));
#204381=CARTESIAN_POINT('Ctrl Pts',(-15.6263176459108,17.8773220648125,
0.));
#204382=CARTESIAN_POINT('Ctrl Pts',(-15.6263176459108,17.8773220648125,
12.));
#204383=CARTESIAN_POINT('Ctrl Pts',(-15.609155712921,17.8671346981394,0.));
#204384=CARTESIAN_POINT('Ctrl Pts',(-15.609155712921,17.8671346981394,12.));
#204385=CARTESIAN_POINT('Ctrl Pts',(-15.5921162378192,17.8569576599006,
0.));
#204386=CARTESIAN_POINT('Ctrl Pts',(-15.5921162378192,17.8569576599006,
12.));
#204387=CARTESIAN_POINT('Ctrl Pts',(-15.5751997657163,17.8467918036987,
0.));
#204388=CARTESIAN_POINT('Ctrl Pts',(-15.5751997657163,17.8467918036987,
12.));
#204389=CARTESIAN_POINT('Ctrl Pts',(-15.5584068472982,17.8366379952085,
0.));
#204390=CARTESIAN_POINT('Ctrl Pts',(-15.5584068472982,17.8366379952085,
12.));
#204391=CARTESIAN_POINT('Ctrl Pts',(-15.541738038964,17.8264971124606,0.));
#204392=CARTESIAN_POINT('Ctrl Pts',(-15.541738038964,17.8264971124606,12.));
#204393=CARTESIAN_POINT('Ctrl Pts',(-15.5251939029552,17.8163700461256,
0.));
#204394=CARTESIAN_POINT('Ctrl Pts',(-15.5251939029552,17.8163700461256,
12.));
#204395=CARTESIAN_POINT('Ctrl Pts',(-15.5087750074718,17.8062576997952,
0.));
#204396=CARTESIAN_POINT('Ctrl Pts',(-15.5087750074718,17.8062576997952,
12.));
#204397=CARTESIAN_POINT('Ctrl Pts',(-15.4924819268517,17.7961609903148,
0.));
#204398=CARTESIAN_POINT('Ctrl Pts',(-15.4924819268517,17.7961609903148,
12.));
#204399=CARTESIAN_POINT('Ctrl Pts',(-15.4763152417497,17.7860808481219,
0.));
#204400=CARTESIAN_POINT('Ctrl Pts',(-15.4763152417497,17.7860808481219,
12.));
#204401=CARTESIAN_POINT('Ctrl Pts',(-15.4602755393017,17.7760182175815,
0.));
#204402=CARTESIAN_POINT('Ctrl Pts',(-15.4602755393017,17.7760182175815,
12.));
#204403=CARTESIAN_POINT('Ctrl Pts',(-15.4443634132869,17.7659740573265,
0.));
#204404=CARTESIAN_POINT('Ctrl Pts',(-15.4443634132869,17.7659740573265,
12.));
#204405=CARTESIAN_POINT('Ctrl Pts',(-15.4285794642668,17.7559493405881,
0.));
#204406=CARTESIAN_POINT('Ctrl Pts',(-15.4285794642668,17.7559493405881,
12.));
#204407=CARTESIAN_POINT('Ctrl Pts',(-15.4129242997837,17.7459450555812,
0.));
#204408=CARTESIAN_POINT('Ctrl Pts',(-15.4129242997837,17.7459450555812,
12.));
#204409=CARTESIAN_POINT('Ctrl Pts',(-15.3973985345802,17.7359622059149,
0.));
#204410=CARTESIAN_POINT('Ctrl Pts',(-15.3973985345802,17.7359622059149,
12.));
#204411=CARTESIAN_POINT('Ctrl Pts',(-15.3820027907967,17.7260018109924,
0.));
#204412=CARTESIAN_POINT('Ctrl Pts',(-15.3820027907967,17.7260018109924,
12.));
#204413=CARTESIAN_POINT('Ctrl Pts',(-15.3667376981699,17.7160649064206,
0.));
#204414=CARTESIAN_POINT('Ctrl Pts',(-15.3667376981699,17.7160649064206,
12.));
#204415=CARTESIAN_POINT('Ctrl Pts',(-15.351603894206,17.7061525444042,0.));
#204416=CARTESIAN_POINT('Ctrl Pts',(-15.351603894206,17.7061525444042,12.));
#204417=CARTESIAN_POINT('Ctrl Pts',(-15.3366020244066,17.6962657941983,
0.));
#204418=CARTESIAN_POINT('Ctrl Pts',(-15.3366020244066,17.6962657941983,
12.));
#204419=CARTESIAN_POINT('Ctrl Pts',(-15.3217327425338,17.6864057426052,
0.));
#204420=CARTESIAN_POINT('Ctrl Pts',(-15.3217327425338,17.6864057426052,
12.));
#204421=CARTESIAN_POINT('Ctrl Pts',(-15.3069967108501,17.676573494456,0.));
#204422=CARTESIAN_POINT('Ctrl Pts',(-15.3069967108501,17.676573494456,12.));
#204423=CARTESIAN_POINT('Ctrl Pts',(-15.2923946003598,17.6667701731041,
0.));
#204424=CARTESIAN_POINT('Ctrl Pts',(-15.2923946003598,17.6667701731041,
12.));
#204425=CARTESIAN_POINT('Ctrl Pts',(-15.2779270910239,17.6569969209,0.));
#204426=CARTESIAN_POINT('Ctrl Pts',(-15.2779270910239,17.6569969209,12.));
#204427=CARTESIAN_POINT('Ctrl Pts',(-15.2635948720292,17.6472548997328,
0.));
#204428=CARTESIAN_POINT('Ctrl Pts',(-15.2635948720292,17.6472548997328,
12.));
#204429=CARTESIAN_POINT('Ctrl Pts',(-15.2493986421092,17.6375452916369,
0.));
#204430=CARTESIAN_POINT('Ctrl Pts',(-15.2493986421092,17.6375452916369,
12.));
#204431=CARTESIAN_POINT('Ctrl Pts',(-15.2353391098366,17.6278692993764,
0.));
#204432=CARTESIAN_POINT('Ctrl Pts',(-15.2353391098366,17.6278692993764,
12.));
#204433=CARTESIAN_POINT('Ctrl Pts',(-15.2214169939199,17.6182281470468,
0.));
#204434=CARTESIAN_POINT('Ctrl Pts',(-15.2214169939199,17.6182281470468,
12.));
#204435=CARTESIAN_POINT('Ctrl Pts',(-15.2076330234686,17.60862308065,0.));
#204436=CARTESIAN_POINT('Ctrl Pts',(-15.2076330234686,17.60862308065,12.));
#204437=CARTESIAN_POINT('Ctrl Pts',(-15.1939879383268,17.5990553687599,
0.));
#204438=CARTESIAN_POINT('Ctrl Pts',(-15.1939879383268,17.5990553687599,
12.));
#204439=CARTESIAN_POINT('Ctrl Pts',(-15.1804824894605,17.5895263032595,
0.));
#204440=CARTESIAN_POINT('Ctrl Pts',(-15.1804824894605,17.5895263032595,
12.));
#204441=CARTESIAN_POINT('Ctrl Pts',(-15.1671174393137,17.580037200054,0.));
#204442=CARTESIAN_POINT('Ctrl Pts',(-15.1671174393137,17.580037200054,12.));
#204443=CARTESIAN_POINT('Ctrl Pts',(-15.1538935621714,17.5705893998029,
0.));
#204444=CARTESIAN_POINT('Ctrl Pts',(-15.1538935621714,17.5705893998029,
12.));
#204445=CARTESIAN_POINT('Ctrl Pts',(-15.1408116444876,17.5611842686192,
0.));
#204446=CARTESIAN_POINT('Ctrl Pts',(-15.1408116444876,17.5611842686192,
12.));
#204447=CARTESIAN_POINT('Ctrl Pts',(-15.1278724853138,17.5518231989117,
0.));
#204448=CARTESIAN_POINT('Ctrl Pts',(-15.1278724853138,17.5518231989117,
12.));
#204449=CARTESIAN_POINT('Ctrl Pts',(-15.1150768967728,17.5425076102963,
0.));
#204450=CARTESIAN_POINT('Ctrl Pts',(-15.1150768967728,17.5425076102963,
12.));
#204451=CARTESIAN_POINT('Ctrl Pts',(-15.1024257045033,17.5332389504829,
0.));
#204452=CARTESIAN_POINT('Ctrl Pts',(-15.1024257045033,17.5332389504829,
12.));
#204453=CARTESIAN_POINT('Ctrl Pts',(-15.0899197481082,17.524018696179,0.));
#204454=CARTESIAN_POINT('Ctrl Pts',(-15.0899197481082,17.524018696179,12.));
#204455=CARTESIAN_POINT('Ctrl Pts',(-15.0775598815749,17.5148483539687,
0.));
#204456=CARTESIAN_POINT('Ctrl Pts',(-15.0775598815749,17.5148483539687,
12.));
#204457=CARTESIAN_POINT('Ctrl Pts',(-15.0653469738307,17.5057294613877,
0.));
#204458=CARTESIAN_POINT('Ctrl Pts',(-15.0653469738307,17.5057294613877,
12.));
#204459=CARTESIAN_POINT('Ctrl Pts',(-15.0532819093085,17.4966635880246,
0.));
#204460=CARTESIAN_POINT('Ctrl Pts',(-15.0532819093085,17.4966635880246,
12.));
#204461=CARTESIAN_POINT('Ctrl Pts',(-15.0413655884993,17.4876523366178,
0.));
#204462=CARTESIAN_POINT('Ctrl Pts',(-15.0413655884993,17.4876523366178,
12.));
#204463=CARTESIAN_POINT('Ctrl Pts',(-15.029598928488,17.4786973441417,0.));
#204464=CARTESIAN_POINT('Ctrl Pts',(-15.029598928488,17.4786973441417,12.));
#204465=CARTESIAN_POINT('Ctrl Pts',(-15.0179828635087,17.4698002829357,
0.));
#204466=CARTESIAN_POINT('Ctrl Pts',(-15.0179828635087,17.4698002829357,
12.));
#204467=CARTESIAN_POINT('Ctrl Pts',(-15.0065183456922,17.4609628621419,
0.));
#204468=CARTESIAN_POINT('Ctrl Pts',(-15.0065183456922,17.4609628621419,
12.));
#204469=CARTESIAN_POINT('Ctrl Pts',(-14.9952063457779,17.4521868291005,
0.));
#204470=CARTESIAN_POINT('Ctrl Pts',(-14.9952063457779,17.4521868291005,
12.));
#204471=CARTESIAN_POINT('Ctrl Pts',(-14.9840478538357,17.4434739707773,
0.));
#204472=CARTESIAN_POINT('Ctrl Pts',(-14.9840478538357,17.4434739707773,
12.));
#204473=CARTESIAN_POINT('Ctrl Pts',(-14.973043879945,17.4348261151395,0.));
#204474=CARTESIAN_POINT('Ctrl Pts',(-14.973043879945,17.4348261151395,12.));
#204475=CARTESIAN_POINT('Ctrl Pts',(-14.9621954549825,17.4262451327088,
0.));
#204476=CARTESIAN_POINT('Ctrl Pts',(-14.9621954549825,17.4262451327088,
12.));
#204477=CARTESIAN_POINT('Ctrl Pts',(-14.9515036315142,17.4177329382827,
0.));
#204478=CARTESIAN_POINT('Ctrl Pts',(-14.9515036315142,17.4177329382827,
12.));
#204479=CARTESIAN_POINT('Ctrl Pts',(-14.940969484645,17.4092914926071,0.));
#204480=CARTESIAN_POINT('Ctrl Pts',(-14.940969484645,17.4092914926071,12.));
#204481=CARTESIAN_POINT('Ctrl Pts',(-14.9305941128758,17.400922804075,0.));
#204482=CARTESIAN_POINT('Ctrl Pts',(-14.9305941128758,17.400922804075,12.));
#204483=CARTESIAN_POINT('Ctrl Pts',(-14.9203786389343,17.3926289303987,
0.));
#204484=CARTESIAN_POINT('Ctrl Pts',(-14.9203786389343,17.3926289303987,
12.));
#204485=CARTESIAN_POINT('Ctrl Pts',(-14.9103242110057,17.3844119809823,
0.));
#204486=CARTESIAN_POINT('Ctrl Pts',(-14.9103242110057,17.3844119809823,
12.));
#204487=CARTESIAN_POINT('Ctrl Pts',(-14.9004320039609,17.3762741193075,
0.));
#204488=CARTESIAN_POINT('Ctrl Pts',(-14.9004320039609,17.3762741193075,
12.));
#204489=CARTESIAN_POINT('Ctrl Pts',(-14.8907032205789,17.3682175653236,
0.));
#204490=CARTESIAN_POINT('Ctrl Pts',(-14.8907032205789,17.3682175653236,
12.));
#204491=CARTESIAN_POINT('Ctrl Pts',(-14.8811390927424,17.3602445978163,
0.));
#204492=CARTESIAN_POINT('Ctrl Pts',(-14.8811390927424,17.3602445978163,
12.));
#204493=CARTESIAN_POINT('Ctrl Pts',(-14.8717408826958,17.3523575568648,
0.));
#204494=CARTESIAN_POINT('Ctrl Pts',(-14.8717408826958,17.3523575568648,
12.));
#204495=CARTESIAN_POINT('Ctrl Pts',(-14.8625098843419,17.3445588463477,
0.));
#204496=CARTESIAN_POINT('Ctrl Pts',(-14.8625098843419,17.3445588463477,
12.));
#204497=CARTESIAN_POINT('Ctrl Pts',(-14.8534474245433,17.336850936485,0.));
#204498=CARTESIAN_POINT('Ctrl Pts',(-14.8534474245433,17.336850936485,12.));
#204499=CARTESIAN_POINT('Ctrl Pts',(-14.8445548643504,17.3292363662601,
0.));
#204500=CARTESIAN_POINT('Ctrl Pts',(-14.8445548643504,17.3292363662601,
12.));
#204501=CARTESIAN_POINT('Ctrl Pts',(-14.8358336004193,17.3217177462096,
0.));
#204502=CARTESIAN_POINT('Ctrl Pts',(-14.8358336004193,17.3217177462096,
12.));
#204503=CARTESIAN_POINT('Ctrl Pts',(-14.8272850675375,17.3142977632656,
0.));
#204504=CARTESIAN_POINT('Ctrl Pts',(-14.8272850675375,17.3142977632656,
12.));
#204505=CARTESIAN_POINT('Ctrl Pts',(-14.8189107410161,17.3069791853705,
0.));
#204506=CARTESIAN_POINT('Ctrl Pts',(-14.8189107410161,17.3069791853705,
12.));
#204507=CARTESIAN_POINT('Ctrl Pts',(-14.8107121391038,17.2997648661483,
0.));
#204508=CARTESIAN_POINT('Ctrl Pts',(-14.8107121391038,17.2997648661483,
12.));
#204509=CARTESIAN_POINT('Ctrl Pts',(-14.8026908254281,17.2926577496519,
0.));
#204510=CARTESIAN_POINT('Ctrl Pts',(-14.8026908254281,17.2926577496519,
12.));
#204511=CARTESIAN_POINT('Ctrl Pts',(-14.7948484105253,17.28566087332,0.));
#204512=CARTESIAN_POINT('Ctrl Pts',(-14.7948484105253,17.28566087332,12.));
#204513=CARTESIAN_POINT('Ctrl Pts',(-14.787186553128,17.278777370485,0.));
#204514=CARTESIAN_POINT('Ctrl Pts',(-14.787186553128,17.278777370485,12.));
#204515=CARTESIAN_POINT('Ctrl Pts',(-14.7797069617802,17.2720104735192,
0.));
#204516=CARTESIAN_POINT('Ctrl Pts',(-14.7797069617802,17.2720104735192,
12.));
#204517=CARTESIAN_POINT('Ctrl Pts',(-14.7724113956728,17.2653635155317,
0.));
#204518=CARTESIAN_POINT('Ctrl Pts',(-14.7724113956728,17.2653635155317,
12.));
#204519=CARTESIAN_POINT('Ctrl Pts',(-14.7653016697589,17.2588399401464,
0.));
#204520=CARTESIAN_POINT('Ctrl Pts',(-14.7653016697589,17.2588399401464,
12.));
#204521=CARTESIAN_POINT('Ctrl Pts',(-14.7583796616617,17.2524433146837,
0.));
#204522=CARTESIAN_POINT('Ctrl Pts',(-14.7583796616617,17.2524433146837,
12.));
#204523=CARTESIAN_POINT('Ctrl Pts',(-14.7516473175125,17.2461773413289,
0.));
#204524=CARTESIAN_POINT('Ctrl Pts',(-14.7516473175125,17.2461773413289,
12.));
#204525=CARTESIAN_POINT('Ctrl Pts',(-14.7451066593793,17.2400458713566,
0.));
#204526=CARTESIAN_POINT('Ctrl Pts',(-14.7451066593793,17.2400458713566,
12.));
#204527=CARTESIAN_POINT('Ctrl Pts',(-14.7387597858117,17.2340529062077,
0.));
#204528=CARTESIAN_POINT('Ctrl Pts',(-14.7387597858117,17.2340529062077,
12.));
#204529=CARTESIAN_POINT('Ctrl Pts',(-14.7326088681163,17.2282025904314,
0.));
#204530=CARTESIAN_POINT('Ctrl Pts',(-14.7326088681163,17.2282025904314,
12.));
#204531=CARTESIAN_POINT('Ctrl Pts',(-14.7266561494282,17.2224992099666,
0.));
#204532=CARTESIAN_POINT('Ctrl Pts',(-14.7266561494282,17.2224992099666,
12.));
#204533=CARTESIAN_POINT('Ctrl Pts',(-14.7209039390326,17.2169471814255,
0.));
#204534=CARTESIAN_POINT('Ctrl Pts',(-14.7209039390326,17.2169471814255,
12.));
#204535=CARTESIAN_POINT('Ctrl Pts',(-14.7153546289338,17.2115510835988,
0.));
#204536=CARTESIAN_POINT('Ctrl Pts',(-14.7153546289338,17.2115510835988,
12.));
#204537=CARTESIAN_POINT('Ctrl Pts',(-14.7100107213586,17.2063157097316,
0.));
#204538=CARTESIAN_POINT('Ctrl Pts',(-14.7100107213586,17.2063157097316,
12.));
#204539=CARTESIAN_POINT('Ctrl Pts',(-14.7048748502663,17.2012461084268,
0.));
#204540=CARTESIAN_POINT('Ctrl Pts',(-14.7048748502663,17.2012461084268,
12.));
#204541=CARTESIAN_POINT('Ctrl Pts',(-14.699949811582,17.1963476411694,0.));
#204542=CARTESIAN_POINT('Ctrl Pts',(-14.699949811582,17.1963476411694,12.));
#204543=CARTESIAN_POINT('Ctrl Pts',(-14.6952385361706,17.1916259308415,
0.));
#204544=CARTESIAN_POINT('Ctrl Pts',(-14.6952385361706,17.1916259308415,
12.));
#204545=CARTESIAN_POINT('Ctrl Pts',(-14.6907440526958,17.1870867909918,
0.));
#204546=CARTESIAN_POINT('Ctrl Pts',(-14.6907440526958,17.1870867909918,
12.));
#204547=CARTESIAN_POINT('Ctrl Pts',(-14.6864694522319,17.182736158472,0.));
#204548=CARTESIAN_POINT('Ctrl Pts',(-14.6864694522319,17.182736158472,12.));
#204549=CARTESIAN_POINT('Ctrl Pts',(-14.6824178576167,17.1785800350827,
0.));
#204550=CARTESIAN_POINT('Ctrl Pts',(-14.6824178576167,17.1785800350827,
12.));
#204551=CARTESIAN_POINT('Ctrl Pts',(-14.6785925615676,17.1746247499057,
0.));
#204552=CARTESIAN_POINT('Ctrl Pts',(-14.6785925615676,17.1746247499057,
12.));
#204553=CARTESIAN_POINT('Ctrl Pts',(-14.6749971333867,17.1708771619129,
0.));
#204554=CARTESIAN_POINT('Ctrl Pts',(-14.6749971333867,17.1708771619129,
12.));
#204555=CARTESIAN_POINT('Ctrl Pts',(-14.6716355833321,17.1673449723019,
0.));
#204556=CARTESIAN_POINT('Ctrl Pts',(-14.6716355833321,17.1673449723019,
12.));
#204557=CARTESIAN_POINT('Ctrl Pts',(-14.6685123374424,17.1640366762304,
0.));
#204558=CARTESIAN_POINT('Ctrl Pts',(-14.6685123374424,17.1640366762304,
12.));
#204559=CARTESIAN_POINT('Ctrl Pts',(-14.6656319165057,17.1609609517369,
0.));
#204560=CARTESIAN_POINT('Ctrl Pts',(-14.6656319165057,17.1609609517369,
12.));
#204561=CARTESIAN_POINT('Ctrl Pts',(-14.662998728599,17.1581262646789,0.));
#204562=CARTESIAN_POINT('Ctrl Pts',(-14.662998728599,17.1581262646789,12.));
#204563=CARTESIAN_POINT('Ctrl Pts',(-14.660616716964,17.1555401986403,0.));
#204564=CARTESIAN_POINT('Ctrl Pts',(-14.660616716964,17.1555401986403,12.));
#204565=CARTESIAN_POINT('Ctrl Pts',(-14.6584900555301,17.1532107762719,
0.));
#204566=CARTESIAN_POINT('Ctrl Pts',(-14.6584900555301,17.1532107762719,
12.));
#204567=CARTESIAN_POINT('Ctrl Pts',(-14.6566237952435,17.1511476869495,
0.));
#204568=CARTESIAN_POINT('Ctrl Pts',(-14.6566237952435,17.1511476869495,
12.));
#204569=CARTESIAN_POINT('Ctrl Pts',(-14.6550248622813,17.1493641837556,
0.));
#204570=CARTESIAN_POINT('Ctrl Pts',(-14.6550248622813,17.1493641837556,
12.));
#204571=CARTESIAN_POINT('Ctrl Pts',(-14.6537016966188,17.1478763944909,
0.));
#204572=CARTESIAN_POINT('Ctrl Pts',(-14.6537016966188,17.1478763944909,
12.));
#204573=CARTESIAN_POINT('Ctrl Pts',(-14.6526624064978,17.1466998098673,
0.));
#204574=CARTESIAN_POINT('Ctrl Pts',(-14.6526624064978,17.1466998098673,
12.));
#204575=CARTESIAN_POINT('Ctrl Pts',(-14.65191316345,17.1458462295273,0.));
#204576=CARTESIAN_POINT('Ctrl Pts',(-14.65191316345,17.1458462295273,12.));
#204577=CARTESIAN_POINT('Ctrl Pts',(-14.6515481598057,17.1454262858045,
0.));
#204578=CARTESIAN_POINT('Ctrl Pts',(-14.6515481598057,17.1454262858045,
12.));
#204579=CARTESIAN_POINT('Ctrl Pts',(-14.6514066997188,17.1452600887039,
0.));
#204580=CARTESIAN_POINT('Ctrl Pts',(-14.6514066997188,17.1452600887039,
12.));
#204581=CARTESIAN_POINT('Ctrl Pts',(-14.651371185284,17.1452153999142,0.));
#204582=CARTESIAN_POINT('Ctrl Pts',(-14.651371185284,17.1452153999142,12.));
#204583=CARTESIAN_POINT('Ctrl Pts',(-14.6513681262571,17.1452095830633,
0.));
#204584=CARTESIAN_POINT('Ctrl Pts',(-14.6513681262571,17.1452095830633,
12.));
#204585=CARTESIAN_POINT('',(-17.9112098770111,18.8464468996588,0.));
#204586=CARTESIAN_POINT('Ctrl Pts',(-17.9112098770111,18.8464468996588,
0.));
#204587=CARTESIAN_POINT('Ctrl Pts',(-17.9057348246595,18.8448126709691,
0.));
#204588=CARTESIAN_POINT('Ctrl Pts',(-17.8947931177807,18.8415402351786,
0.));
#204589=CARTESIAN_POINT('Ctrl Pts',(-17.8784057509356,18.8366196462581,
0.));
#204590=CARTESIAN_POINT('Ctrl Pts',(-17.8566063174771,18.8300349895974,
0.));
#204591=CARTESIAN_POINT('Ctrl Pts',(-17.8294410311006,18.8217643886157,
0.));
#204592=CARTESIAN_POINT('Ctrl Pts',(-17.8023598011057,18.8134540340417,
0.));
#204593=CARTESIAN_POINT('Ctrl Pts',(-17.7753627137853,18.8051039860448,
0.));
#204594=CARTESIAN_POINT('Ctrl Pts',(-17.7484498996905,18.7967143519419,
0.));
#204595=CARTESIAN_POINT('Ctrl Pts',(-17.7216215409035,18.7882852976049,
0.));
#204596=CARTESIAN_POINT('Ctrl Pts',(-17.6948778823014,18.7798170641374,
0.));
#204597=CARTESIAN_POINT('Ctrl Pts',(-17.6682192274236,18.7713099642754,
0.));
#204598=CARTESIAN_POINT('Ctrl Pts',(-17.6416459210681,18.762764361321,0.));
#204599=CARTESIAN_POINT('Ctrl Pts',(-17.6151583357012,18.7541806530984,
0.));
#204600=CARTESIAN_POINT('Ctrl Pts',(-17.5887568561371,18.7455592536687,
0.));
#204601=CARTESIAN_POINT('Ctrl Pts',(-17.5624418653245,18.7369005764553,
0.));
#204602=CARTESIAN_POINT('Ctrl Pts',(-17.5362137287593,18.7282050157138,
0.));
#204603=CARTESIAN_POINT('Ctrl Pts',(-17.5100727820876,18.7194729318098,
0.));
#204604=CARTESIAN_POINT('Ctrl Pts',(-17.4840193397162,18.7107046613912,
0.));
#204605=CARTESIAN_POINT('Ctrl Pts',(-17.4580537012753,18.70190052503,0.));
#204606=CARTESIAN_POINT('Ctrl Pts',(-17.4321761588142,18.6930608357409,
0.));
#204607=CARTESIAN_POINT('Ctrl Pts',(-17.4063870038562,18.6841859073471,
0.));
#204608=CARTESIAN_POINT('Ctrl Pts',(-17.3806865340747,18.6752760624052,
0.));
#204609=CARTESIAN_POINT('Ctrl Pts',(-17.3550750612443,18.6663316416582,
0.));
#204610=CARTESIAN_POINT('Ctrl Pts',(-17.3295529098618,18.6573530024033,
0.));
#204611=CARTESIAN_POINT('Ctrl Pts',(-17.3041204135074,18.6483405141865,
0.));
#204612=CARTESIAN_POINT('Ctrl Pts',(-17.2787779120213,18.6392945554748,
0.));
#204613=CARTESIAN_POINT('Ctrl Pts',(-17.2535257482187,18.6302155097943,
0.));
#204614=CARTESIAN_POINT('Ctrl Pts',(-17.2283642650518,18.6211037624038,
0.));
#204615=CARTESIAN_POINT('Ctrl Pts',(-17.2032938019284,18.6119596959949,
0.));
#204616=CARTESIAN_POINT('Ctrl Pts',(-17.1783146940127,18.6027836898817,
0.));
#204617=CARTESIAN_POINT('Ctrl Pts',(-17.1534272741643,18.5935761222825,
0.));
#204618=CARTESIAN_POINT('Ctrl Pts',(-17.1286318741183,18.5843373717247,
0.));
#204619=CARTESIAN_POINT('Ctrl Pts',(-17.1039288260001,18.5750678188542,
0.));
#204620=CARTESIAN_POINT('Ctrl Pts',(-17.0793184636079,18.5657678479789,
0.));
#204621=CARTESIAN_POINT('Ctrl Pts',(-17.0548011239751,18.556437848963,0.));
#204622=CARTESIAN_POINT('Ctrl Pts',(-17.0303771481738,18.547078218209,0.));
#204623=CARTESIAN_POINT('Ctrl Pts',(-17.0060468805097,18.5376893576961,
0.));
#204624=CARTESIAN_POINT('Ctrl Pts',(-16.981810668038,18.5282716744197,0.));
#204625=CARTESIAN_POINT('Ctrl Pts',(-16.9576688599339,18.5188255796659,
0.));
#204626=CARTESIAN_POINT('Ctrl Pts',(-16.9336218069353,18.5093514883835,
0.));
#204627=CARTESIAN_POINT('Ctrl Pts',(-16.9096698606943,18.499849818462,0.));
#204628=CARTESIAN_POINT('Ctrl Pts',(-16.8858133733088,18.4903209902227,
0.));
#204629=CARTESIAN_POINT('Ctrl Pts',(-16.8620526977171,18.480765426877,0.));
#204630=CARTESIAN_POINT('Ctrl Pts',(-16.8383881879709,18.4711835548623,
0.));
#204631=CARTESIAN_POINT('Ctrl Pts',(-16.8148201995472,18.4615758042305,
0.));
#204632=CARTESIAN_POINT('Ctrl Pts',(-16.791349089629,18.4519426090123,0.));
#204633=CARTESIAN_POINT('Ctrl Pts',(-16.7679752173992,18.44228440761,0.));
#204634=CARTESIAN_POINT('Ctrl Pts',(-16.7446989442882,18.4326016431392,
0.));
#204635=CARTESIAN_POINT('Ctrl Pts',(-16.7215206338818,18.4228947633187,
0.));
#204636=CARTESIAN_POINT('Ctrl Pts',(-16.6984406518491,18.413164220399,0.));
#204637=CARTESIAN_POINT('Ctrl Pts',(-16.6754593658513,18.403410471079,0.));
#204638=CARTESIAN_POINT('Ctrl Pts',(-16.6525771454513,18.3936339764332,
0.));
#204639=CARTESIAN_POINT('Ctrl Pts',(-16.6297943620056,18.3838352018327,
0.));
#204640=CARTESIAN_POINT('Ctrl Pts',(-16.607111388571,18.3740146168879,0.));
#204641=CARTESIAN_POINT('Ctrl Pts',(-16.5845286000217,18.3641726955889,
0.));
#204642=CARTESIAN_POINT('Ctrl Pts',(-16.5620463731413,18.354309916433,0.));
#204643=CARTESIAN_POINT('Ctrl Pts',(-16.5396650867139,18.34442676256,0.));
#204644=CARTESIAN_POINT('Ctrl Pts',(-16.5173851216045,18.3345237218864,
0.));
#204645=CARTESIAN_POINT('Ctrl Pts',(-16.4952068608345,18.3246012872469,
0.));
#204646=CARTESIAN_POINT('Ctrl Pts',(-16.4731306896441,18.3146599565231,
0.));
#204647=CARTESIAN_POINT('Ctrl Pts',(-16.4511569955233,18.304700232686,0.));
#204648=CARTESIAN_POINT('Ctrl Pts',(-16.4292861682379,18.294722623851,0.));
#204649=CARTESIAN_POINT('Ctrl Pts',(-16.4075185998455,18.2847276433309,
0.));
#204650=CARTESIAN_POINT('Ctrl Pts',(-16.385854684708,18.2747158096934,0.));
#204651=CARTESIAN_POINT('Ctrl Pts',(-16.3642948194868,18.2646876468169,
0.));
#204652=CARTESIAN_POINT('Ctrl Pts',(-16.3428394031589,18.2546436839608,
0.));
#204653=CARTESIAN_POINT('Ctrl Pts',(-16.3214888370987,18.2445844558741,
0.));
#204654=CARTESIAN_POINT('Ctrl Pts',(-16.3002435251378,18.2345105028982,
0.));
#204655=CARTESIAN_POINT('Ctrl Pts',(-16.2791038736223,18.2244223710745,
0.));
#204656=CARTESIAN_POINT('Ctrl Pts',(-16.2580702914615,18.2143206122529,
0.));
#204657=CARTESIAN_POINT('Ctrl Pts',(-16.2371431901638,18.2042057842035,
0.));
#204658=CARTESIAN_POINT('Ctrl Pts',(-16.2163229838875,18.1940784507229,
0.));
#204659=CARTESIAN_POINT('Ctrl Pts',(-16.1956100895073,18.1839391817331,
0.));
#204660=CARTESIAN_POINT('Ctrl Pts',(-16.1750049266671,18.1737885533849,
0.));
#204661=CARTESIAN_POINT('Ctrl Pts',(-16.154507917826,18.1636271481615,0.));
#204662=CARTESIAN_POINT('Ctrl Pts',(-16.1341194882988,18.1534555549852,
0.));
#204663=CARTESIAN_POINT('Ctrl Pts',(-16.1138400662794,18.1432743693235,
0.));
#204664=CARTESIAN_POINT('Ctrl Pts',(-16.0936700829112,18.1330841933105,
0.));
#204665=CARTESIAN_POINT('Ctrl Pts',(-16.0736099723668,18.1228856358751,
0.));
#204666=CARTESIAN_POINT('Ctrl Pts',(-16.0536601719126,18.112679312869,0.));
#204667=CARTESIAN_POINT('Ctrl Pts',(-16.0338211219693,18.1024658471966,
0.));
#204668=CARTESIAN_POINT('Ctrl Pts',(-16.014093266161,18.0922458689462,0.));
#204669=CARTESIAN_POINT('Ctrl Pts',(-15.9944770513613,18.0820200155236,
0.));
#204670=CARTESIAN_POINT('Ctrl Pts',(-15.9749729277846,18.0717889317958,
0.));
#204671=CARTESIAN_POINT('Ctrl Pts',(-15.9555813490644,18.0615532702359,
0.));
#204672=CARTESIAN_POINT('Ctrl Pts',(-15.9363027723244,18.0513136910691,
0.));
#204673=CARTESIAN_POINT('Ctrl Pts',(-15.9171376582436,18.0410708624208,
0.));
#204674=CARTESIAN_POINT('Ctrl Pts',(-15.8980864711042,18.0308254604636,
0.));
#204675=CARTESIAN_POINT('Ctrl Pts',(-15.8791496788683,18.0205781695769,
0.));
#204676=CARTESIAN_POINT('Ctrl Pts',(-15.8603277532831,18.0103296825205,
0.));
#204677=CARTESIAN_POINT('Ctrl Pts',(-15.8416211699679,18.0000807006052,
0.));
#204678=CARTESIAN_POINT('Ctrl Pts',(-15.8230304084962,17.9898319338664,
0.));
#204679=CARTESIAN_POINT('Ctrl Pts',(-15.8045559524676,17.9795841012386,
0.));
#204680=CARTESIAN_POINT('Ctrl Pts',(-15.7861982895724,17.9693379307303,
0.));
#204681=CARTESIAN_POINT('Ctrl Pts',(-15.7679579117077,17.9590941596242,
0.));
#204682=CARTESIAN_POINT('Ctrl Pts',(-15.749835315086,17.9488535346781,0.));
#204683=CARTESIAN_POINT('Ctrl Pts',(-15.7318310003335,17.9386168123262,
0.));
#204684=CARTESIAN_POINT('Ctrl Pts',(-15.7139454725838,17.9283847588835,
0.));
#204685=CARTESIAN_POINT('Ctrl Pts',(-15.6961792415522,17.9181581507455,
0.));
#204686=CARTESIAN_POINT('Ctrl Pts',(-15.678532821646,17.9079377746111,0.));
#204687=CARTESIAN_POINT('Ctrl Pts',(-15.661006732103,17.897724427724,0.));
#204688=CARTESIAN_POINT('Ctrl Pts',(-15.6436014971084,17.8875189181091,
0.));
#204689=CARTESIAN_POINT('Ctrl Pts',(-15.6263176459108,17.8773220648125,
0.));
#204690=CARTESIAN_POINT('Ctrl Pts',(-15.609155712921,17.8671346981394,0.));
#204691=CARTESIAN_POINT('Ctrl Pts',(-15.5921162378192,17.8569576599006,
0.));
#204692=CARTESIAN_POINT('Ctrl Pts',(-15.5751997657163,17.8467918036987,
0.));
#204693=CARTESIAN_POINT('Ctrl Pts',(-15.5584068472982,17.8366379952085,
0.));
#204694=CARTESIAN_POINT('Ctrl Pts',(-15.541738038964,17.8264971124606,0.));
#204695=CARTESIAN_POINT('Ctrl Pts',(-15.5251939029552,17.8163700461256,
0.));
#204696=CARTESIAN_POINT('Ctrl Pts',(-15.5087750074718,17.8062576997952,
0.));
#204697=CARTESIAN_POINT('Ctrl Pts',(-15.4924819268517,17.7961609903148,
0.));
#204698=CARTESIAN_POINT('Ctrl Pts',(-15.4763152417497,17.7860808481219,
0.));
#204699=CARTESIAN_POINT('Ctrl Pts',(-15.4602755393017,17.7760182175815,
0.));
#204700=CARTESIAN_POINT('Ctrl Pts',(-15.4443634132869,17.7659740573265,
0.));
#204701=CARTESIAN_POINT('Ctrl Pts',(-15.4285794642668,17.7559493405881,
0.));
#204702=CARTESIAN_POINT('Ctrl Pts',(-15.4129242997837,17.7459450555812,
0.));
#204703=CARTESIAN_POINT('Ctrl Pts',(-15.3973985345802,17.7359622059149,
0.));
#204704=CARTESIAN_POINT('Ctrl Pts',(-15.3820027907967,17.7260018109924,
0.));
#204705=CARTESIAN_POINT('Ctrl Pts',(-15.3667376981699,17.7160649064206,
0.));
#204706=CARTESIAN_POINT('Ctrl Pts',(-15.351603894206,17.7061525444042,0.));
#204707=CARTESIAN_POINT('Ctrl Pts',(-15.3366020244066,17.6962657941983,
0.));
#204708=CARTESIAN_POINT('Ctrl Pts',(-15.3217327425338,17.6864057426052,
0.));
#204709=CARTESIAN_POINT('Ctrl Pts',(-15.3069967108501,17.676573494456,0.));
#204710=CARTESIAN_POINT('Ctrl Pts',(-15.2923946003598,17.6667701731041,
0.));
#204711=CARTESIAN_POINT('Ctrl Pts',(-15.2779270910239,17.6569969209,0.));
#204712=CARTESIAN_POINT('Ctrl Pts',(-15.2635948720292,17.6472548997328,
0.));
#204713=CARTESIAN_POINT('Ctrl Pts',(-15.2493986421092,17.6375452916369,
0.));
#204714=CARTESIAN_POINT('Ctrl Pts',(-15.2353391098366,17.6278692993764,
0.));
#204715=CARTESIAN_POINT('Ctrl Pts',(-15.2214169939199,17.6182281470468,
0.));
#204716=CARTESIAN_POINT('Ctrl Pts',(-15.2076330234686,17.60862308065,0.));
#204717=CARTESIAN_POINT('Ctrl Pts',(-15.1939879383268,17.5990553687599,
0.));
#204718=CARTESIAN_POINT('Ctrl Pts',(-15.1804824894605,17.5895263032595,
0.));
#204719=CARTESIAN_POINT('Ctrl Pts',(-15.1671174393137,17.580037200054,0.));
#204720=CARTESIAN_POINT('Ctrl Pts',(-15.1538935621714,17.5705893998029,
0.));
#204721=CARTESIAN_POINT('Ctrl Pts',(-15.1408116444876,17.5611842686192,
0.));
#204722=CARTESIAN_POINT('Ctrl Pts',(-15.1278724853138,17.5518231989117,
0.));
#204723=CARTESIAN_POINT('Ctrl Pts',(-15.1150768967728,17.5425076102963,
0.));
#204724=CARTESIAN_POINT('Ctrl Pts',(-15.1024257045033,17.5332389504829,
0.));
#204725=CARTESIAN_POINT('Ctrl Pts',(-15.0899197481082,17.524018696179,0.));
#204726=CARTESIAN_POINT('Ctrl Pts',(-15.0775598815749,17.5148483539687,
0.));
#204727=CARTESIAN_POINT('Ctrl Pts',(-15.0653469738307,17.5057294613877,
0.));
#204728=CARTESIAN_POINT('Ctrl Pts',(-15.0532819093085,17.4966635880246,
0.));
#204729=CARTESIAN_POINT('Ctrl Pts',(-15.0413655884993,17.4876523366178,
0.));
#204730=CARTESIAN_POINT('Ctrl Pts',(-15.029598928488,17.4786973441417,0.));
#204731=CARTESIAN_POINT('Ctrl Pts',(-15.0179828635087,17.4698002829357,
0.));
#204732=CARTESIAN_POINT('Ctrl Pts',(-15.0065183456922,17.4609628621419,
0.));
#204733=CARTESIAN_POINT('Ctrl Pts',(-14.9952063457779,17.4521868291005,
0.));
#204734=CARTESIAN_POINT('Ctrl Pts',(-14.9840478538357,17.4434739707773,
0.));
#204735=CARTESIAN_POINT('Ctrl Pts',(-14.973043879945,17.4348261151395,0.));
#204736=CARTESIAN_POINT('Ctrl Pts',(-14.9621954549825,17.4262451327088,
0.));
#204737=CARTESIAN_POINT('Ctrl Pts',(-14.9515036315142,17.4177329382827,
0.));
#204738=CARTESIAN_POINT('Ctrl Pts',(-14.940969484645,17.4092914926071,0.));
#204739=CARTESIAN_POINT('Ctrl Pts',(-14.9305941128758,17.400922804075,0.));
#204740=CARTESIAN_POINT('Ctrl Pts',(-14.9203786389343,17.3926289303987,
0.));
#204741=CARTESIAN_POINT('Ctrl Pts',(-14.9103242110057,17.3844119809823,
0.));
#204742=CARTESIAN_POINT('Ctrl Pts',(-14.9004320039609,17.3762741193075,
0.));
#204743=CARTESIAN_POINT('Ctrl Pts',(-14.8907032205789,17.3682175653236,
0.));
#204744=CARTESIAN_POINT('Ctrl Pts',(-14.8811390927424,17.3602445978163,
0.));
#204745=CARTESIAN_POINT('Ctrl Pts',(-14.8717408826958,17.3523575568648,
0.));
#204746=CARTESIAN_POINT('Ctrl Pts',(-14.8625098843419,17.3445588463477,
0.));
#204747=CARTESIAN_POINT('Ctrl Pts',(-14.8534474245433,17.336850936485,0.));
#204748=CARTESIAN_POINT('Ctrl Pts',(-14.8445548643504,17.3292363662601,
0.));
#204749=CARTESIAN_POINT('Ctrl Pts',(-14.8358336004193,17.3217177462096,
0.));
#204750=CARTESIAN_POINT('Ctrl Pts',(-14.8272850675375,17.3142977632656,
0.));
#204751=CARTESIAN_POINT('Ctrl Pts',(-14.8189107410161,17.3069791853705,
0.));
#204752=CARTESIAN_POINT('Ctrl Pts',(-14.8107121391038,17.2997648661483,
0.));
#204753=CARTESIAN_POINT('Ctrl Pts',(-14.8026908254281,17.2926577496519,
0.));
#204754=CARTESIAN_POINT('Ctrl Pts',(-14.7948484105253,17.28566087332,0.));
#204755=CARTESIAN_POINT('Ctrl Pts',(-14.787186553128,17.278777370485,0.));
#204756=CARTESIAN_POINT('Ctrl Pts',(-14.7797069617802,17.2720104735192,
0.));
#204757=CARTESIAN_POINT('Ctrl Pts',(-14.7724113956728,17.2653635155317,
0.));
#204758=CARTESIAN_POINT('Ctrl Pts',(-14.7653016697589,17.2588399401464,
0.));
#204759=CARTESIAN_POINT('Ctrl Pts',(-14.7583796616617,17.2524433146837,
0.));
#204760=CARTESIAN_POINT('Ctrl Pts',(-14.7516473175125,17.2461773413289,
0.));
#204761=CARTESIAN_POINT('Ctrl Pts',(-14.7451066593793,17.2400458713566,
0.));
#204762=CARTESIAN_POINT('Ctrl Pts',(-14.7387597858117,17.2340529062077,
0.));
#204763=CARTESIAN_POINT('Ctrl Pts',(-14.7326088681163,17.2282025904314,
0.));
#204764=CARTESIAN_POINT('Ctrl Pts',(-14.7266561494282,17.2224992099666,
0.));
#204765=CARTESIAN_POINT('Ctrl Pts',(-14.7209039390326,17.2169471814255,
0.));
#204766=CARTESIAN_POINT('Ctrl Pts',(-14.7153546289338,17.2115510835988,
0.));
#204767=CARTESIAN_POINT('Ctrl Pts',(-14.7100107213586,17.2063157097316,
0.));
#204768=CARTESIAN_POINT('Ctrl Pts',(-14.7048748502663,17.2012461084268,
0.));
#204769=CARTESIAN_POINT('Ctrl Pts',(-14.699949811582,17.1963476411694,0.));
#204770=CARTESIAN_POINT('Ctrl Pts',(-14.6952385361706,17.1916259308415,
0.));
#204771=CARTESIAN_POINT('Ctrl Pts',(-14.6907440526958,17.1870867909918,
0.));
#204772=CARTESIAN_POINT('Ctrl Pts',(-14.6864694522319,17.182736158472,0.));
#204773=CARTESIAN_POINT('Ctrl Pts',(-14.6824178576167,17.1785800350827,
0.));
#204774=CARTESIAN_POINT('Ctrl Pts',(-14.6785925615676,17.1746247499057,
0.));
#204775=CARTESIAN_POINT('Ctrl Pts',(-14.6749971333867,17.1708771619129,
0.));
#204776=CARTESIAN_POINT('Ctrl Pts',(-14.6716355833321,17.1673449723019,
0.));
#204777=CARTESIAN_POINT('Ctrl Pts',(-14.6685123374424,17.1640366762304,
0.));
#204778=CARTESIAN_POINT('Ctrl Pts',(-14.6656319165057,17.1609609517369,
0.));
#204779=CARTESIAN_POINT('Ctrl Pts',(-14.662998728599,17.1581262646789,0.));
#204780=CARTESIAN_POINT('Ctrl Pts',(-14.660616716964,17.1555401986403,0.));
#204781=CARTESIAN_POINT('Ctrl Pts',(-14.6584900555301,17.1532107762719,
0.));
#204782=CARTESIAN_POINT('Ctrl Pts',(-14.6566237952435,17.1511476869495,
0.));
#204783=CARTESIAN_POINT('Ctrl Pts',(-14.6550248622813,17.1493641837556,
0.));
#204784=CARTESIAN_POINT('Ctrl Pts',(-14.6537016966188,17.1478763944909,
0.));
#204785=CARTESIAN_POINT('Ctrl Pts',(-14.6526624064978,17.1466998098673,
0.));
#204786=CARTESIAN_POINT('Ctrl Pts',(-14.65191316345,17.1458462295273,0.));
#204787=CARTESIAN_POINT('Ctrl Pts',(-14.6515481598057,17.1454262858045,
0.));
#204788=CARTESIAN_POINT('Ctrl Pts',(-14.6514066997188,17.1452600887039,
0.));
#204789=CARTESIAN_POINT('Ctrl Pts',(-14.651371185284,17.1452153999142,0.));
#204790=CARTESIAN_POINT('Ctrl Pts',(-14.6513681262571,17.1452095830633,
0.));
#204791=CARTESIAN_POINT('',(-17.9112098770111,18.8464468996588,0.));
#204792=CARTESIAN_POINT('Ctrl Pts',(-12.7689476255363,18.5896416359912,
0.));
#204793=CARTESIAN_POINT('Ctrl Pts',(-12.7689476255363,18.5896416359912,
12.));
#204794=CARTESIAN_POINT('Ctrl Pts',(-12.7689524524483,18.5896460962964,
0.));
#204795=CARTESIAN_POINT('Ctrl Pts',(-12.7689524524483,18.5896460962964,
12.));
#204796=CARTESIAN_POINT('Ctrl Pts',(-12.768986426692,18.5896919669165,0.));
#204797=CARTESIAN_POINT('Ctrl Pts',(-12.768986426692,18.5896919669165,12.));
#204798=CARTESIAN_POINT('Ctrl Pts',(-12.769110348199,18.589871621843,0.));
#204799=CARTESIAN_POINT('Ctrl Pts',(-12.769110348199,18.589871621843,12.));
#204800=CARTESIAN_POINT('Ctrl Pts',(-12.7694215127919,18.5903328777227,
0.));
#204801=CARTESIAN_POINT('Ctrl Pts',(-12.7694215127919,18.5903328777227,
12.));
#204802=CARTESIAN_POINT('Ctrl Pts',(-12.7700520897173,18.5912775137806,
0.));
#204803=CARTESIAN_POINT('Ctrl Pts',(-12.7700520897173,18.5912775137806,
12.));
#204804=CARTESIAN_POINT('Ctrl Pts',(-12.7709195951156,18.5925859134579,
0.));
#204805=CARTESIAN_POINT('Ctrl Pts',(-12.7709195951156,18.5925859134579,
12.));
#204806=CARTESIAN_POINT('Ctrl Pts',(-12.7720142287172,18.5942490615407,
0.));
#204807=CARTESIAN_POINT('Ctrl Pts',(-12.7720142287172,18.5942490615407,
12.));
#204808=CARTESIAN_POINT('Ctrl Pts',(-12.7733231262108,18.5962551167772,
0.));
#204809=CARTESIAN_POINT('Ctrl Pts',(-12.7733231262108,18.5962551167772,
12.));
#204810=CARTESIAN_POINT('Ctrl Pts',(-12.7748328937638,18.598591752595,0.));
#204811=CARTESIAN_POINT('Ctrl Pts',(-12.7748328937638,18.598591752595,12.));
#204812=CARTESIAN_POINT('Ctrl Pts',(-12.7765325225081,18.6012488486709,
0.));
#204813=CARTESIAN_POINT('Ctrl Pts',(-12.7765325225081,18.6012488486709,
12.));
#204814=CARTESIAN_POINT('Ctrl Pts',(-12.7784139605066,18.6042190183704,
0.));
#204815=CARTESIAN_POINT('Ctrl Pts',(-12.7784139605066,18.6042190183704,
12.));
#204816=CARTESIAN_POINT('Ctrl Pts',(-12.7804705387658,18.6074961535723,
0.));
#204817=CARTESIAN_POINT('Ctrl Pts',(-12.7804705387658,18.6074961535723,
12.));
#204818=CARTESIAN_POINT('Ctrl Pts',(-12.7826959526925,18.6110744826219,
0.));
#204819=CARTESIAN_POINT('Ctrl Pts',(-12.7826959526925,18.6110744826219,
12.));
#204820=CARTESIAN_POINT('Ctrl Pts',(-12.7850831657901,18.6149475565188,
0.));
#204821=CARTESIAN_POINT('Ctrl Pts',(-12.7850831657901,18.6149475565188,
12.));
#204822=CARTESIAN_POINT('Ctrl Pts',(-12.7876249657834,18.6191087624752,
0.));
#204823=CARTESIAN_POINT('Ctrl Pts',(-12.7876249657834,18.6191087624752,
12.));
#204824=CARTESIAN_POINT('Ctrl Pts',(-12.7903142925234,18.6235516265575,
0.));
#204825=CARTESIAN_POINT('Ctrl Pts',(-12.7903142925234,18.6235516265575,
12.));
#204826=CARTESIAN_POINT('Ctrl Pts',(-12.7931447451555,18.6282702819371,
0.));
#204827=CARTESIAN_POINT('Ctrl Pts',(-12.7931447451555,18.6282702819371,
12.));
#204828=CARTESIAN_POINT('Ctrl Pts',(-12.7961106222251,18.6332595057006,
0.));
#204829=CARTESIAN_POINT('Ctrl Pts',(-12.7961106222251,18.6332595057006,
12.));
#204830=CARTESIAN_POINT('Ctrl Pts',(-12.7992066625264,18.63851447924,0.));
#204831=CARTESIAN_POINT('Ctrl Pts',(-12.7992066625264,18.63851447924,12.));
#204832=CARTESIAN_POINT('Ctrl Pts',(-12.8024278770152,18.6440306327456,
0.));
#204833=CARTESIAN_POINT('Ctrl Pts',(-12.8024278770152,18.6440306327456,
12.));
#204834=CARTESIAN_POINT('Ctrl Pts',(-12.805769331162,18.6498034438986,0.));
#204835=CARTESIAN_POINT('Ctrl Pts',(-12.805769331162,18.6498034438986,12.));
#204836=CARTESIAN_POINT('Ctrl Pts',(-12.8092261933858,18.6558284825773,
0.));
#204837=CARTESIAN_POINT('Ctrl Pts',(-12.8092261933858,18.6558284825773,
12.));
#204838=CARTESIAN_POINT('Ctrl Pts',(-12.8127937909631,18.6621014624746,
0.));
#204839=CARTESIAN_POINT('Ctrl Pts',(-12.8127937909631,18.6621014624746,
12.));
#204840=CARTESIAN_POINT('Ctrl Pts',(-12.8164676687362,18.6686182952799,
0.));
#204841=CARTESIAN_POINT('Ctrl Pts',(-12.8164676687362,18.6686182952799,
12.));
#204842=CARTESIAN_POINT('Ctrl Pts',(-12.8202436318474,18.6753751301092,
0.));
#204843=CARTESIAN_POINT('Ctrl Pts',(-12.8202436318474,18.6753751301092,
12.));
#204844=CARTESIAN_POINT('Ctrl Pts',(-12.8241176980017,18.6823683094139,
0.));
#204845=CARTESIAN_POINT('Ctrl Pts',(-12.8241176980017,18.6823683094139,
12.));
#204846=CARTESIAN_POINT('Ctrl Pts',(-12.8280860635231,18.6895943376171,
0.));
#204847=CARTESIAN_POINT('Ctrl Pts',(-12.8280860635231,18.6895943376171,
12.));
#204848=CARTESIAN_POINT('Ctrl Pts',(-12.8321450599789,18.6970498410172,
0.));
#204849=CARTESIAN_POINT('Ctrl Pts',(-12.8321450599789,18.6970498410172,
12.));
#204850=CARTESIAN_POINT('Ctrl Pts',(-12.8362911280361,18.7047315436294,
0.));
#204851=CARTESIAN_POINT('Ctrl Pts',(-12.8362911280361,18.7047315436294,
12.));
#204852=CARTESIAN_POINT('Ctrl Pts',(-12.8405208263431,18.7126362754445,
0.));
#204853=CARTESIAN_POINT('Ctrl Pts',(-12.8405208263431,18.7126362754445,
12.));
#204854=CARTESIAN_POINT('Ctrl Pts',(-12.8448308329494,18.7207609737702,
0.));
#204855=CARTESIAN_POINT('Ctrl Pts',(-12.8448308329494,18.7207609737702,
12.));
#204856=CARTESIAN_POINT('Ctrl Pts',(-12.8492179511591,18.7291026886554,
0.));
#204857=CARTESIAN_POINT('Ctrl Pts',(-12.8492179511591,18.7291026886554,
12.));
#204858=CARTESIAN_POINT('Ctrl Pts',(-12.8536791086316,18.7376585820854,
0.));
#204859=CARTESIAN_POINT('Ctrl Pts',(-12.8536791086316,18.7376585820854,
12.));
#204860=CARTESIAN_POINT('Ctrl Pts',(-12.8582113455646,18.7464259171251,
0.));
#204861=CARTESIAN_POINT('Ctrl Pts',(-12.8582113455646,18.7464259171251,
12.));
#204862=CARTESIAN_POINT('Ctrl Pts',(-12.8628118054171,18.7554020493887,
0.));
#204863=CARTESIAN_POINT('Ctrl Pts',(-12.8628118054171,18.7554020493887,
12.));
#204864=CARTESIAN_POINT('Ctrl Pts',(-12.8674777239653,18.7645844169564,
0.));
#204865=CARTESIAN_POINT('Ctrl Pts',(-12.8674777239653,18.7645844169564,
12.));
#204866=CARTESIAN_POINT('Ctrl Pts',(-12.872206421181,18.7739705329022,0.));
#204867=CARTESIAN_POINT('Ctrl Pts',(-12.872206421181,18.7739705329022,12.));
#204868=CARTESIAN_POINT('Ctrl Pts',(-12.8769952998095,18.7835579840477,
0.));
#204869=CARTESIAN_POINT('Ctrl Pts',(-12.8769952998095,18.7835579840477,
12.));
#204870=CARTESIAN_POINT('Ctrl Pts',(-12.8818418427475,18.7933444285868,
0.));
#204871=CARTESIAN_POINT('Ctrl Pts',(-12.8818418427475,18.7933444285868,
12.));
#204872=CARTESIAN_POINT('Ctrl Pts',(-12.8867436109546,18.8033275941943,
0.));
#204873=CARTESIAN_POINT('Ctrl Pts',(-12.8867436109546,18.8033275941943,
12.));
#204874=CARTESIAN_POINT('Ctrl Pts',(-12.8916982409935,18.813505275782,0.));
#204875=CARTESIAN_POINT('Ctrl Pts',(-12.8916982409935,18.813505275782,12.));
#204876=CARTESIAN_POINT('Ctrl Pts',(-12.8967034410755,18.8238753319128,
0.));
#204877=CARTESIAN_POINT('Ctrl Pts',(-12.8967034410755,18.8238753319128,
12.));
#204878=CARTESIAN_POINT('Ctrl Pts',(-12.9017569871738,18.834435681259,0.));
#204879=CARTESIAN_POINT('Ctrl Pts',(-12.9017569871738,18.834435681259,12.));
#204880=CARTESIAN_POINT('Ctrl Pts',(-12.9068567191854,18.8451842990984,
0.));
#204881=CARTESIAN_POINT('Ctrl Pts',(-12.9068567191854,18.8451842990984,
12.));
#204882=CARTESIAN_POINT('Ctrl Pts',(-12.9120005369063,18.8561192136198,
0.));
#204883=CARTESIAN_POINT('Ctrl Pts',(-12.9120005369063,18.8561192136198,
12.));
#204884=CARTESIAN_POINT('Ctrl Pts',(-12.9171863977045,18.8672385038326,
0.));
#204885=CARTESIAN_POINT('Ctrl Pts',(-12.9171863977045,18.8672385038326,
12.));
#204886=CARTESIAN_POINT('Ctrl Pts',(-12.9224123144982,18.8785402977527,
0.));
#204887=CARTESIAN_POINT('Ctrl Pts',(-12.9224123144982,18.8785402977527,
12.));
#204888=CARTESIAN_POINT('Ctrl Pts',(-12.9276763536373,18.8900227704889,
0.));
#204889=CARTESIAN_POINT('Ctrl Pts',(-12.9276763536373,18.8900227704889,
12.));
#204890=CARTESIAN_POINT('Ctrl Pts',(-12.9329766328185,18.9016841423403,
0.));
#204891=CARTESIAN_POINT('Ctrl Pts',(-12.9329766328185,18.9016841423403,
12.));
#204892=CARTESIAN_POINT('Ctrl Pts',(-12.9383113190375,18.9135226769465,
0.));
#204893=CARTESIAN_POINT('Ctrl Pts',(-12.9383113190375,18.9135226769465,
12.));
#204894=CARTESIAN_POINT('Ctrl Pts',(-12.9436786266105,18.9255366795195,
0.));
#204895=CARTESIAN_POINT('Ctrl Pts',(-12.9436786266105,18.9255366795195,
12.));
#204896=CARTESIAN_POINT('Ctrl Pts',(-12.9490768151821,18.9377244950435,
0.));
#204897=CARTESIAN_POINT('Ctrl Pts',(-12.9490768151821,18.9377244950435,
12.));
#204898=CARTESIAN_POINT('Ctrl Pts',(-12.9545041877377,18.9500845064715,
0.));
#204899=CARTESIAN_POINT('Ctrl Pts',(-12.9545041877377,18.9500845064715,
12.));
#204900=CARTESIAN_POINT('Ctrl Pts',(-12.9599590886319,18.9626151329229,
0.));
#204901=CARTESIAN_POINT('Ctrl Pts',(-12.9599590886319,18.9626151329229,
12.));
#204902=CARTESIAN_POINT('Ctrl Pts',(-12.9654399021869,18.9753148284475,
0.));
#204903=CARTESIAN_POINT('Ctrl Pts',(-12.9654399021869,18.9753148284475,
12.));
#204904=CARTESIAN_POINT('Ctrl Pts',(-12.9709450512747,18.9881820807585,
0.));
#204905=CARTESIAN_POINT('Ctrl Pts',(-12.9709450512747,18.9881820807585,
12.));
#204906=CARTESIAN_POINT('Ctrl Pts',(-12.9764729959205,19.0012154099791,
0.));
#204907=CARTESIAN_POINT('Ctrl Pts',(-12.9764729959205,19.0012154099791,
12.));
#204908=CARTESIAN_POINT('Ctrl Pts',(-12.9820222318716,19.0144133673348,
0.));
#204909=CARTESIAN_POINT('Ctrl Pts',(-12.9820222318716,19.0144133673348,
12.));
#204910=CARTESIAN_POINT('Ctrl Pts',(-12.9875912893003,19.0277745339908,
0.));
#204911=CARTESIAN_POINT('Ctrl Pts',(-12.9875912893003,19.0277745339908,
12.));
#204912=CARTESIAN_POINT('Ctrl Pts',(-12.9931787316515,19.0412975200398,
0.));
#204913=CARTESIAN_POINT('Ctrl Pts',(-12.9931787316515,19.0412975200398,
12.));
#204914=CARTESIAN_POINT('Ctrl Pts',(-12.9987831544502,19.0549809634355,
0.));
#204915=CARTESIAN_POINT('Ctrl Pts',(-12.9987831544502,19.0549809634355,
12.));
#204916=CARTESIAN_POINT('Ctrl Pts',(-13.0044031841381,19.0688235289437,
0.));
#204917=CARTESIAN_POINT('Ctrl Pts',(-13.0044031841381,19.0688235289437,
12.));
#204918=CARTESIAN_POINT('Ctrl Pts',(-13.0100374768785,19.0828239070482,
0.));
#204919=CARTESIAN_POINT('Ctrl Pts',(-13.0100374768785,19.0828239070482,
12.));
#204920=CARTESIAN_POINT('Ctrl Pts',(-13.0156847176093,19.0969808131225,
0.));
#204921=CARTESIAN_POINT('Ctrl Pts',(-13.0156847176093,19.0969808131225,
12.));
#204922=CARTESIAN_POINT('Ctrl Pts',(-13.0213436191326,19.1112929866308,
0.));
#204923=CARTESIAN_POINT('Ctrl Pts',(-13.0213436191326,19.1112929866308,
12.));
#204924=CARTESIAN_POINT('Ctrl Pts',(-13.0270129211976,19.1257591903099,
0.));
#204925=CARTESIAN_POINT('Ctrl Pts',(-13.0270129211976,19.1257591903099,
12.));
#204926=CARTESIAN_POINT('Ctrl Pts',(-13.0326913895841,19.1403782093389,
0.));
#204927=CARTESIAN_POINT('Ctrl Pts',(-13.0326913895841,19.1403782093389,
12.));
#204928=CARTESIAN_POINT('Ctrl Pts',(-13.0383778152072,19.1551488505233,
0.));
#204929=CARTESIAN_POINT('Ctrl Pts',(-13.0383778152072,19.1551488505233,
12.));
#204930=CARTESIAN_POINT('Ctrl Pts',(-13.0440710133775,19.1700699416625,
0.));
#204931=CARTESIAN_POINT('Ctrl Pts',(-13.0440710133775,19.1700699416625,
12.));
#204932=CARTESIAN_POINT('Ctrl Pts',(-13.0497698230442,19.1851403308825,
0.));
#204933=CARTESIAN_POINT('Ctrl Pts',(-13.0497698230442,19.1851403308825,
12.));
#204934=CARTESIAN_POINT('Ctrl Pts',(-13.0554731060537,19.2003588859771,
0.));
#204935=CARTESIAN_POINT('Ctrl Pts',(-13.0554731060537,19.2003588859771,
12.));
#204936=CARTESIAN_POINT('Ctrl Pts',(-13.0611797463913,19.2157244937141,
0.));
#204937=CARTESIAN_POINT('Ctrl Pts',(-13.0611797463913,19.2157244937141,
12.));
#204938=CARTESIAN_POINT('Ctrl Pts',(-13.0668886494791,19.2312360592031,
0.));
#204939=CARTESIAN_POINT('Ctrl Pts',(-13.0668886494791,19.2312360592031,
12.));
#204940=CARTESIAN_POINT('Ctrl Pts',(-13.0725987415856,19.2468925053988,
0.));
#204941=CARTESIAN_POINT('Ctrl Pts',(-13.0725987415856,19.2468925053988,
12.));
#204942=CARTESIAN_POINT('Ctrl Pts',(-13.0783089692118,19.2626927725596,
0.));
#204943=CARTESIAN_POINT('Ctrl Pts',(-13.0783089692118,19.2626927725596,
12.));
#204944=CARTESIAN_POINT('Ctrl Pts',(-13.0840182984949,19.2786358177198,
0.));
#204945=CARTESIAN_POINT('Ctrl Pts',(-13.0840182984949,19.2786358177198,
12.));
#204946=CARTESIAN_POINT('Ctrl Pts',(-13.089725714597,19.2947206141246,0.));
#204947=CARTESIAN_POINT('Ctrl Pts',(-13.089725714597,19.2947206141246,12.));
#204948=CARTESIAN_POINT('Ctrl Pts',(-13.095430221148,19.3109461507358,0.));
#204949=CARTESIAN_POINT('Ctrl Pts',(-13.095430221148,19.3109461507358,12.));
#204950=CARTESIAN_POINT('Ctrl Pts',(-13.1011308397592,19.3273114318268,
0.));
#204951=CARTESIAN_POINT('Ctrl Pts',(-13.1011308397592,19.3273114318268,
12.));
#204952=CARTESIAN_POINT('Ctrl Pts',(-13.1068266095186,19.3438154765395,
0.));
#204953=CARTESIAN_POINT('Ctrl Pts',(-13.1068266095186,19.3438154765395,
12.));
#204954=CARTESIAN_POINT('Ctrl Pts',(-13.1125165865021,19.3604573184516,
0.));
#204955=CARTESIAN_POINT('Ctrl Pts',(-13.1125165865021,19.3604573184516,
12.));
#204956=CARTESIAN_POINT('Ctrl Pts',(-13.118199843271,19.3772360051093,0.));
#204957=CARTESIAN_POINT('Ctrl Pts',(-13.118199843271,19.3772360051093,12.));
#204958=CARTESIAN_POINT('Ctrl Pts',(-13.1238754684177,19.3941505976267,
0.));
#204959=CARTESIAN_POINT('Ctrl Pts',(-13.1238754684177,19.3941505976267,
12.));
#204960=CARTESIAN_POINT('Ctrl Pts',(-13.1295425661635,19.4112001703561,
0.));
#204961=CARTESIAN_POINT('Ctrl Pts',(-13.1295425661635,19.4112001703561,
12.));
#204962=CARTESIAN_POINT('Ctrl Pts',(-13.1352002559439,19.4283838105265,
0.));
#204963=CARTESIAN_POINT('Ctrl Pts',(-13.1352002559439,19.4283838105265,
12.));
#204964=CARTESIAN_POINT('Ctrl Pts',(-13.140847672006,19.4457006178875,0.));
#204965=CARTESIAN_POINT('Ctrl Pts',(-13.140847672006,19.4457006178875,12.));
#204966=CARTESIAN_POINT('Ctrl Pts',(-13.1464839629966,19.463149704325,0.));
#204967=CARTESIAN_POINT('Ctrl Pts',(-13.1464839629966,19.463149704325,12.));
#204968=CARTESIAN_POINT('Ctrl Pts',(-13.1521082915846,19.4807301935256,
0.));
#204969=CARTESIAN_POINT('Ctrl Pts',(-13.1521082915846,19.4807301935256,
12.));
#204970=CARTESIAN_POINT('Ctrl Pts',(-13.1577198341238,19.498441220707,0.));
#204971=CARTESIAN_POINT('Ctrl Pts',(-13.1577198341238,19.498441220707,12.));
#204972=CARTESIAN_POINT('Ctrl Pts',(-13.1633177803097,19.5162819323207,
0.));
#204973=CARTESIAN_POINT('Ctrl Pts',(-13.1633177803097,19.5162819323207,
12.));
#204974=CARTESIAN_POINT('Ctrl Pts',(-13.1689013328432,19.5342514857564,
0.));
#204975=CARTESIAN_POINT('Ctrl Pts',(-13.1689013328432,19.5342514857564,
12.));
#204976=CARTESIAN_POINT('Ctrl Pts',(-13.1744697070918,19.5523490490254,
0.));
#204977=CARTESIAN_POINT('Ctrl Pts',(-13.1744697070918,19.5523490490254,
12.));
#204978=CARTESIAN_POINT('Ctrl Pts',(-13.1800221307683,19.5705738004682,
0.));
#204979=CARTESIAN_POINT('Ctrl Pts',(-13.1800221307683,19.5705738004682,
12.));
#204980=CARTESIAN_POINT('Ctrl Pts',(-13.1855578436479,19.5889249285351,
0.));
#204981=CARTESIAN_POINT('Ctrl Pts',(-13.1855578436479,19.5889249285351,
12.));
#204982=CARTESIAN_POINT('Ctrl Pts',(-13.1910760972818,19.6074016315421,
0.));
#204983=CARTESIAN_POINT('Ctrl Pts',(-13.1910760972818,19.6074016315421,
12.));
#204984=CARTESIAN_POINT('Ctrl Pts',(-13.196576154715,19.6260031174244,0.));
#204985=CARTESIAN_POINT('Ctrl Pts',(-13.196576154715,19.6260031174244,12.));
#204986=CARTESIAN_POINT('Ctrl Pts',(-13.202057290206,19.6447286034764,0.));
#204987=CARTESIAN_POINT('Ctrl Pts',(-13.202057290206,19.6447286034764,12.));
#204988=CARTESIAN_POINT('Ctrl Pts',(-13.2075187889522,19.6635773160924,
0.));
#204989=CARTESIAN_POINT('Ctrl Pts',(-13.2075187889522,19.6635773160924,
12.));
#204990=CARTESIAN_POINT('Ctrl Pts',(-13.2129599468478,19.6825484905812,
0.));
#204991=CARTESIAN_POINT('Ctrl Pts',(-13.2129599468478,19.6825484905812,
12.));
#204992=CARTESIAN_POINT('Ctrl Pts',(-13.2183800702431,19.7016413709678,
0.));
#204993=CARTESIAN_POINT('Ctrl Pts',(-13.2183800702431,19.7016413709678,
12.));
#204994=CARTESIAN_POINT('Ctrl Pts',(-13.2237784757065,19.7208552097867,
0.));
#204995=CARTESIAN_POINT('Ctrl Pts',(-13.2237784757065,19.7208552097867,
12.));
#204996=CARTESIAN_POINT('Ctrl Pts',(-13.2291544897902,19.7401892678701,
0.));
#204997=CARTESIAN_POINT('Ctrl Pts',(-13.2291544897902,19.7401892678701,
12.));
#204998=CARTESIAN_POINT('Ctrl Pts',(-13.2345074487968,19.7596428141176,
0.));
#204999=CARTESIAN_POINT('Ctrl Pts',(-13.2345074487968,19.7596428141176,
12.));
#205000=CARTESIAN_POINT('Ctrl Pts',(-13.239836698568,19.7792151253297,0.));
#205001=CARTESIAN_POINT('Ctrl Pts',(-13.239836698568,19.7792151253297,12.));
#205002=CARTESIAN_POINT('Ctrl Pts',(-13.2451415942809,19.7989054860501,
0.));
#205003=CARTESIAN_POINT('Ctrl Pts',(-13.2451415942809,19.7989054860501,
12.));
#205004=CARTESIAN_POINT('Ctrl Pts',(-13.2504215002458,19.8187131883919,
0.));
#205005=CARTESIAN_POINT('Ctrl Pts',(-13.2504215002458,19.8187131883919,
12.));
#205006=CARTESIAN_POINT('Ctrl Pts',(-13.2556757897085,19.8386375318632,
0.));
#205007=CARTESIAN_POINT('Ctrl Pts',(-13.2556757897085,19.8386375318632,
12.));
#205008=CARTESIAN_POINT('Ctrl Pts',(-13.2609038446525,19.8586778231711,
0.));
#205009=CARTESIAN_POINT('Ctrl Pts',(-13.2609038446525,19.8586778231711,
12.));
#205010=CARTESIAN_POINT('Ctrl Pts',(-13.2661050556128,19.8788333760571,
0.));
#205011=CARTESIAN_POINT('Ctrl Pts',(-13.2661050556128,19.8788333760571,
12.));
#205012=CARTESIAN_POINT('Ctrl Pts',(-13.2712788215015,19.8991035111739,
0.));
#205013=CARTESIAN_POINT('Ctrl Pts',(-13.2712788215015,19.8991035111739,
12.));
#205014=CARTESIAN_POINT('Ctrl Pts',(-13.2764245494354,19.9194875559419,
0.));
#205015=CARTESIAN_POINT('Ctrl Pts',(-13.2764245494354,19.9194875559419,
12.));
#205016=CARTESIAN_POINT('Ctrl Pts',(-13.2815416545663,19.9399848444019,
0.));
#205017=CARTESIAN_POINT('Ctrl Pts',(-13.2815416545663,19.9399848444019,
12.));
#205018=CARTESIAN_POINT('Ctrl Pts',(-13.2866295599152,19.9605947170589,
0.));
#205019=CARTESIAN_POINT('Ctrl Pts',(-13.2866295599152,19.9605947170589,
12.));
#205020=CARTESIAN_POINT('Ctrl Pts',(-13.2916876962098,19.9813165207174,
0.));
#205021=CARTESIAN_POINT('Ctrl Pts',(-13.2916876962098,19.9813165207174,
12.));
#205022=CARTESIAN_POINT('Ctrl Pts',(-13.296715501731,20.0021496083742,0.));
#205023=CARTESIAN_POINT('Ctrl Pts',(-13.296715501731,20.0021496083742,12.));
#205024=CARTESIAN_POINT('Ctrl Pts',(-13.3017124221639,20.0230933391039,
0.));
#205025=CARTESIAN_POINT('Ctrl Pts',(-13.3017124221639,20.0230933391039,
12.));
#205026=CARTESIAN_POINT('Ctrl Pts',(-13.3066779104515,20.0441470779345,
0.));
#205027=CARTESIAN_POINT('Ctrl Pts',(-13.3066779104515,20.0441470779345,
12.));
#205028=CARTESIAN_POINT('Ctrl Pts',(-13.3116114266514,20.0653101957188,
0.));
#205029=CARTESIAN_POINT('Ctrl Pts',(-13.3116114266514,20.0653101957188,
12.));
#205030=CARTESIAN_POINT('Ctrl Pts',(-13.3165124377963,20.0865820689883,
0.));
#205031=CARTESIAN_POINT('Ctrl Pts',(-13.3165124377963,20.0865820689883,
12.));
#205032=CARTESIAN_POINT('Ctrl Pts',(-13.3213804177588,20.1079620798377,
0.));
#205033=CARTESIAN_POINT('Ctrl Pts',(-13.3213804177588,20.1079620798377,
12.));
#205034=CARTESIAN_POINT('Ctrl Pts',(-13.3262148471228,20.1294496158405,
0.));
#205035=CARTESIAN_POINT('Ctrl Pts',(-13.3262148471228,20.1294496158405,
12.));
#205036=CARTESIAN_POINT('Ctrl Pts',(-13.3310152130565,20.1510440699477,
0.));
#205037=CARTESIAN_POINT('Ctrl Pts',(-13.3310152130565,20.1510440699477,
12.));
#205038=CARTESIAN_POINT('Ctrl Pts',(-13.3357810091903,20.1727448403818,
0.));
#205039=CARTESIAN_POINT('Ctrl Pts',(-13.3357810091903,20.1727448403818,
12.));
#205040=CARTESIAN_POINT('Ctrl Pts',(-13.3405117354969,20.1945513305233,
0.));
#205041=CARTESIAN_POINT('Ctrl Pts',(-13.3405117354969,20.1945513305233,
12.));
#205042=CARTESIAN_POINT('Ctrl Pts',(-13.3452068981763,20.2164629487855,
0.));
#205043=CARTESIAN_POINT('Ctrl Pts',(-13.3452068981763,20.2164629487855,
12.));
#205044=CARTESIAN_POINT('Ctrl Pts',(-13.3498660095382,20.2384791085354,
0.));
#205045=CARTESIAN_POINT('Ctrl Pts',(-13.3498660095382,20.2384791085354,
12.));
#205046=CARTESIAN_POINT('Ctrl Pts',(-13.3544885878886,20.2605992280117,
0.));
#205047=CARTESIAN_POINT('Ctrl Pts',(-13.3544885878886,20.2605992280117,
12.));
#205048=CARTESIAN_POINT('Ctrl Pts',(-13.3590741574194,20.2828227302337,
0.));
#205049=CARTESIAN_POINT('Ctrl Pts',(-13.3590741574194,20.2828227302337,
12.));
#205050=CARTESIAN_POINT('Ctrl Pts',(-13.3636222481017,20.3051490429049,
0.));
#205051=CARTESIAN_POINT('Ctrl Pts',(-13.3636222481017,20.3051490429049,
12.));
#205052=CARTESIAN_POINT('Ctrl Pts',(-13.3681323955828,20.3275775983032,
0.));
#205053=CARTESIAN_POINT('Ctrl Pts',(-13.3681323955828,20.3275775983032,
12.));
#205054=CARTESIAN_POINT('Ctrl Pts',(-13.3726041410869,20.3501078331818,
0.));
#205055=CARTESIAN_POINT('Ctrl Pts',(-13.3726041410869,20.3501078331818,
12.));
#205056=CARTESIAN_POINT('Ctrl Pts',(-13.377037031319,20.3727391887187,0.));
#205057=CARTESIAN_POINT('Ctrl Pts',(-13.377037031319,20.3727391887187,12.));
#205058=CARTESIAN_POINT('Ctrl Pts',(-13.3814306183721,20.3954711104504,
0.));
#205059=CARTESIAN_POINT('Ctrl Pts',(-13.3814306183721,20.3954711104504,
12.));
#205060=CARTESIAN_POINT('Ctrl Pts',(-13.3857844596387,20.4183030482002,
0.));
#205061=CARTESIAN_POINT('Ctrl Pts',(-13.3857844596387,20.4183030482002,
12.));
#205062=CARTESIAN_POINT('Ctrl Pts',(-13.3900981177254,20.4412344560007,
0.));
#205063=CARTESIAN_POINT('Ctrl Pts',(-13.3900981177254,20.4412344560007,
12.));
#205064=CARTESIAN_POINT('Ctrl Pts',(-13.3943711603739,20.4642647920038,
0.));
#205065=CARTESIAN_POINT('Ctrl Pts',(-13.3943711603739,20.4642647920038,
12.));
#205066=CARTESIAN_POINT('Ctrl Pts',(-13.3986031603716,20.4873935184041,
0.));
#205067=CARTESIAN_POINT('Ctrl Pts',(-13.3986031603716,20.4873935184041,
12.));
#205068=CARTESIAN_POINT('Ctrl Pts',(-13.4027936954529,20.5106201013755,
0.));
#205069=CARTESIAN_POINT('Ctrl Pts',(-13.4027936954529,20.5106201013755,
12.));
#205070=CARTESIAN_POINT('Ctrl Pts',(-13.4069423482076,20.5339440109957,
0.));
#205071=CARTESIAN_POINT('Ctrl Pts',(-13.4069423482076,20.5339440109957,
12.));
#205072=CARTESIAN_POINT('Ctrl Pts',(-13.4110487059912,20.557364721164,0.));
#205073=CARTESIAN_POINT('Ctrl Pts',(-13.4110487059912,20.557364721164,12.));
#205074=CARTESIAN_POINT('Ctrl Pts',(-13.4151123608411,20.5808817095155,
0.));
#205075=CARTESIAN_POINT('Ctrl Pts',(-13.4151123608411,20.5808817095155,
12.));
#205076=CARTESIAN_POINT('Ctrl Pts',(-13.4191329093932,20.6044944573151,
0.));
#205077=CARTESIAN_POINT('Ctrl Pts',(-13.4191329093932,20.6044944573151,
12.));
#205078=CARTESIAN_POINT('Ctrl Pts',(-13.4231099528178,20.6282024494234,
0.));
#205079=CARTESIAN_POINT('Ctrl Pts',(-13.4231099528178,20.6282024494234,
12.));
#205080=CARTESIAN_POINT('Ctrl Pts',(-13.427043096765,20.6520051742867,0.));
#205081=CARTESIAN_POINT('Ctrl Pts',(-13.427043096765,20.6520051742867,12.));
#205082=CARTESIAN_POINT('Ctrl Pts',(-13.4309319513119,20.6759021239102,
0.));
#205083=CARTESIAN_POINT('Ctrl Pts',(-13.4309319513119,20.6759021239102,
12.));
#205084=CARTESIAN_POINT('Ctrl Pts',(-13.4347761309154,20.6998927938288,
0.));
#205085=CARTESIAN_POINT('Ctrl Pts',(-13.4347761309154,20.6998927938288,
12.));
#205086=CARTESIAN_POINT('Ctrl Pts',(-13.4385752543663,20.7239766830675,
0.));
#205087=CARTESIAN_POINT('Ctrl Pts',(-13.4385752543663,20.7239766830675,
12.));
#205088=CARTESIAN_POINT('Ctrl Pts',(-13.4423289447561,20.7481532941014,
0.));
#205089=CARTESIAN_POINT('Ctrl Pts',(-13.4423289447561,20.7481532941014,
12.));
#205090=CARTESIAN_POINT('Ctrl Pts',(-13.4460368293689,20.7724221327609,
0.));
#205091=CARTESIAN_POINT('Ctrl Pts',(-13.4460368293689,20.7724221327609,
12.));
#205092=CARTESIAN_POINT('Ctrl Pts',(-13.4496985395637,20.7967827081228,
0.));
#205093=CARTESIAN_POINT('Ctrl Pts',(-13.4496985395637,20.7967827081228,
12.));
#205094=CARTESIAN_POINT('Ctrl Pts',(-13.4533137106667,20.821234532398,0.));
#205095=CARTESIAN_POINT('Ctrl Pts',(-13.4533137106667,20.821234532398,12.));
#205096=CARTESIAN_POINT('Ctrl Pts',(-13.4568819818631,20.8457771208083,
0.));
#205097=CARTESIAN_POINT('Ctrl Pts',(-13.4568819818631,20.8457771208083,
12.));
#205098=CARTESIAN_POINT('Ctrl Pts',(-13.4604029960983,20.8704099914641,
0.));
#205099=CARTESIAN_POINT('Ctrl Pts',(-13.4604029960983,20.8704099914641,
12.));
#205100=CARTESIAN_POINT('Ctrl Pts',(-13.4638763999725,20.8951326652158,
0.));
#205101=CARTESIAN_POINT('Ctrl Pts',(-13.4638763999725,20.8951326652158,
12.));
#205102=CARTESIAN_POINT('Ctrl Pts',(-13.4673018437717,20.9199446657583,
0.));
#205103=CARTESIAN_POINT('Ctrl Pts',(-13.4673018437717,20.9199446657583,
12.));
#205104=CARTESIAN_POINT('Ctrl Pts',(-13.4706789815166,20.9448455197557,
0.));
#205105=CARTESIAN_POINT('Ctrl Pts',(-13.4706789815166,20.9448455197557,
12.));
#205106=CARTESIAN_POINT('Ctrl Pts',(-13.4740074710086,20.9698347569476,
0.));
#205107=CARTESIAN_POINT('Ctrl Pts',(-13.4740074710086,20.9698347569476,
12.));
#205108=CARTESIAN_POINT('Ctrl Pts',(-13.4772869738879,20.9949119102592,
0.));
#205109=CARTESIAN_POINT('Ctrl Pts',(-13.4772869738879,20.9949119102592,
12.));
#205110=CARTESIAN_POINT('Ctrl Pts',(-13.4805171556822,21.0200765158884,
0.));
#205111=CARTESIAN_POINT('Ctrl Pts',(-13.4805171556822,21.0200765158884,
12.));
#205112=CARTESIAN_POINT('Ctrl Pts',(-13.4836976858912,21.0453281134245,
0.));
#205113=CARTESIAN_POINT('Ctrl Pts',(-13.4836976858912,21.0453281134245,
12.));
#205114=CARTESIAN_POINT('Ctrl Pts',(-13.4868282377191,21.0706662455199,
0.));
#205115=CARTESIAN_POINT('Ctrl Pts',(-13.4868282377191,21.0706662455199,
12.));
#205116=CARTESIAN_POINT('Ctrl Pts',(-13.4899084877717,21.0960904575046,
0.));
#205117=CARTESIAN_POINT('Ctrl Pts',(-13.4899084877717,21.0960904575046,
12.));
#205118=CARTESIAN_POINT('Ctrl Pts',(-13.4929381157778,21.1216002970207,
0.));
#205119=CARTESIAN_POINT('Ctrl Pts',(-13.4929381157778,21.1216002970207,
12.));
#205120=CARTESIAN_POINT('Ctrl Pts',(-13.4959168042934,21.1471953136209,
0.));
#205121=CARTESIAN_POINT('Ctrl Pts',(-13.4959168042934,21.1471953136209,
12.));
#205122=CARTESIAN_POINT('Ctrl Pts',(-13.4988442384491,21.1728750584175,
0.));
#205123=CARTESIAN_POINT('Ctrl Pts',(-13.4988442384491,21.1728750584175,
12.));
#205124=CARTESIAN_POINT('Ctrl Pts',(-13.5017201056088,21.1986390835828,
0.));
#205125=CARTESIAN_POINT('Ctrl Pts',(-13.5017201056088,21.1986390835828,
12.));
#205126=CARTESIAN_POINT('Ctrl Pts',(-13.5045440957404,21.2244869429332,
0.));
#205127=CARTESIAN_POINT('Ctrl Pts',(-13.5045440957404,21.2244869429332,
12.));
#205128=CARTESIAN_POINT('Ctrl Pts',(-13.5073159019452,21.250418192743,0.));
#205129=CARTESIAN_POINT('Ctrl Pts',(-13.5073159019452,21.250418192743,12.));
#205130=CARTESIAN_POINT('Ctrl Pts',(-13.5100352209205,21.2764323924442,
0.));
#205131=CARTESIAN_POINT('Ctrl Pts',(-13.5100352209205,21.2764323924442,
12.));
#205132=CARTESIAN_POINT('Ctrl Pts',(-13.5127017534971,21.3025291054235,
0.));
#205133=CARTESIAN_POINT('Ctrl Pts',(-13.5127017534971,21.3025291054235,
12.));
#205134=CARTESIAN_POINT('Ctrl Pts',(-13.5153152050555,21.328707899634,0.));
#205135=CARTESIAN_POINT('Ctrl Pts',(-13.5153152050555,21.328707899634,12.));
#205136=CARTESIAN_POINT('Ctrl Pts',(-13.5178752862466,21.3549683486222,
0.));
#205137=CARTESIAN_POINT('Ctrl Pts',(-13.5178752862466,21.3549683486222,
12.));
#205138=CARTESIAN_POINT('Ctrl Pts',(-13.5203817122504,21.3813100304973,
0.));
#205139=CARTESIAN_POINT('Ctrl Pts',(-13.5203817122504,21.3813100304973,
12.));
#205140=CARTESIAN_POINT('Ctrl Pts',(-13.5228342013516,21.4077325259324,
0.));
#205141=CARTESIAN_POINT('Ctrl Pts',(-13.5228342013516,21.4077325259324,
12.));
#205142=CARTESIAN_POINT('Ctrl Pts',(-13.5252324737802,21.4342354165259,
0.));
#205143=CARTESIAN_POINT('Ctrl Pts',(-13.5252324737802,21.4342354165259,
12.));
#205144=CARTESIAN_POINT('Ctrl Pts',(-13.5275762503555,21.4608182828697,
0.));
#205145=CARTESIAN_POINT('Ctrl Pts',(-13.5275762503555,21.4608182828697,
12.));
#205146=CARTESIAN_POINT('Ctrl Pts',(-13.5298652514355,21.4874807030468,
0.));
#205147=CARTESIAN_POINT('Ctrl Pts',(-13.5298652514355,21.4874807030468,
12.));
#205148=CARTESIAN_POINT('Ctrl Pts',(-13.5320991952138,21.5142222501666,
0.));
#205149=CARTESIAN_POINT('Ctrl Pts',(-13.5320991952138,21.5142222501666,
12.));
#205150=CARTESIAN_POINT('Ctrl Pts',(-13.5342777983215,21.5410424932503,
0.));
#205151=CARTESIAN_POINT('Ctrl Pts',(-13.5342777983215,21.5410424932503,
12.));
#205152=CARTESIAN_POINT('Ctrl Pts',(-13.536400779028,21.5679410019001,0.));
#205153=CARTESIAN_POINT('Ctrl Pts',(-13.536400779028,21.5679410019001,12.));
#205154=CARTESIAN_POINT('Ctrl Pts',(-13.5384678597195,21.5949173499013,
0.));
#205155=CARTESIAN_POINT('Ctrl Pts',(-13.5384678597195,21.5949173499013,
12.));
#205156=CARTESIAN_POINT('Ctrl Pts',(-13.5404787697792,21.6219711193946,
0.));
#205157=CARTESIAN_POINT('Ctrl Pts',(-13.5404787697792,21.6219711193946,
12.));
#205158=CARTESIAN_POINT('Ctrl Pts',(-13.5424332480699,21.6491019044648,
0.));
#205159=CARTESIAN_POINT('Ctrl Pts',(-13.5424332480699,21.6491019044648,
12.));
#205160=CARTESIAN_POINT('Ctrl Pts',(-13.5443310461526,21.6763093157699,
0.));
#205161=CARTESIAN_POINT('Ctrl Pts',(-13.5443310461526,21.6763093157699,
12.));
#205162=CARTESIAN_POINT('Ctrl Pts',(-13.5461719295048,21.7035929822955,
0.));
#205163=CARTESIAN_POINT('Ctrl Pts',(-13.5461719295048,21.7035929822955,
12.));
#205164=CARTESIAN_POINT('Ctrl Pts',(-13.5479556704481,21.7309525412281,
0.));
#205165=CARTESIAN_POINT('Ctrl Pts',(-13.5479556704481,21.7309525412281,
12.));
#205166=CARTESIAN_POINT('Ctrl Pts',(-13.5496820422211,21.7583876294554,
0.));
#205167=CARTESIAN_POINT('Ctrl Pts',(-13.5496820422211,21.7583876294554,
12.));
#205168=CARTESIAN_POINT('Ctrl Pts',(-13.551350812725,21.7858978745865,0.));
#205169=CARTESIAN_POINT('Ctrl Pts',(-13.551350812725,21.7858978745865,12.));
#205170=CARTESIAN_POINT('Ctrl Pts',(-13.5529617381573,21.8134828857967,
0.));
#205171=CARTESIAN_POINT('Ctrl Pts',(-13.5529617381573,21.8134828857967,
12.));
#205172=CARTESIAN_POINT('Ctrl Pts',(-13.5545145573031,21.8411422456075,
0.));
#205173=CARTESIAN_POINT('Ctrl Pts',(-13.5545145573031,21.8411422456075,
12.));
#205174=CARTESIAN_POINT('Ctrl Pts',(-13.5560089839385,21.8688754989365,
0.));
#205175=CARTESIAN_POINT('Ctrl Pts',(-13.5560089839385,21.8688754989365,
12.));
#205176=CARTESIAN_POINT('Ctrl Pts',(-13.5574447178424,21.8966821688824,
0.));
#205177=CARTESIAN_POINT('Ctrl Pts',(-13.5574447178424,21.8966821688824,
12.));
#205178=CARTESIAN_POINT('Ctrl Pts',(-13.5588214586604,21.9245617765769,
0.));
#205179=CARTESIAN_POINT('Ctrl Pts',(-13.5588214586604,21.9245617765769,
12.));
#205180=CARTESIAN_POINT('Ctrl Pts',(-13.5601389185257,21.9525138592813,
0.));
#205181=CARTESIAN_POINT('Ctrl Pts',(-13.5601389185257,21.9525138592813,
12.));
#205182=CARTESIAN_POINT('Ctrl Pts',(-13.5613968357561,21.9805379899168,
0.));
#205183=CARTESIAN_POINT('Ctrl Pts',(-13.5613968357561,21.9805379899168,
12.));
#205184=CARTESIAN_POINT('Ctrl Pts',(-13.5625949868333,22.0086337943449,
0.));
#205185=CARTESIAN_POINT('Ctrl Pts',(-13.5625949868333,22.0086337943449,
12.));
#205186=CARTESIAN_POINT('Ctrl Pts',(-13.5637332022473,22.0368009736295,
0.));
#205187=CARTESIAN_POINT('Ctrl Pts',(-13.5637332022473,22.0368009736295,
12.));
#205188=CARTESIAN_POINT('Ctrl Pts',(-13.5648113689033,22.0650393089609,
0.));
#205189=CARTESIAN_POINT('Ctrl Pts',(-13.5648113689033,22.0650393089609,
12.));
#205190=CARTESIAN_POINT('Ctrl Pts',(-13.5658294169284,22.0933486464593,
0.));
#205191=CARTESIAN_POINT('Ctrl Pts',(-13.5658294169284,22.0933486464593,
12.));
#205192=CARTESIAN_POINT('Ctrl Pts',(-13.5667873105359,22.1217288871975,
0.));
#205193=CARTESIAN_POINT('Ctrl Pts',(-13.5667873105359,22.1217288871975,
12.));
#205194=CARTESIAN_POINT('Ctrl Pts',(-13.5675054919061,22.1444897575194,
0.));
#205195=CARTESIAN_POINT('Ctrl Pts',(-13.5675054919061,22.1444897575194,
12.));
#205196=CARTESIAN_POINT('Ctrl Pts',(-13.5680170531805,22.1615922805008,
0.));
#205197=CARTESIAN_POINT('Ctrl Pts',(-13.5680170531805,22.1615922805008,
12.));
#205198=CARTESIAN_POINT('Ctrl Pts',(-13.5683460612942,22.1730081264608,
0.));
#205199=CARTESIAN_POINT('Ctrl Pts',(-13.5683460612942,22.1730081264608,
12.));
#205200=CARTESIAN_POINT('Ctrl Pts',(-13.5685075571671,22.1787195904339,
0.));
#205201=CARTESIAN_POINT('Ctrl Pts',(-13.5685075571671,22.1787195904339,
12.));
#205202=CARTESIAN_POINT('',(-13.5685075571671,22.1787195904339,0.));
#205203=CARTESIAN_POINT('Ctrl Pts',(-12.7689476255363,18.5896416359912,
0.));
#205204=CARTESIAN_POINT('Ctrl Pts',(-12.7689524524483,18.5896460962964,
0.));
#205205=CARTESIAN_POINT('Ctrl Pts',(-12.768986426692,18.5896919669165,0.));
#205206=CARTESIAN_POINT('Ctrl Pts',(-12.769110348199,18.589871621843,0.));
#205207=CARTESIAN_POINT('Ctrl Pts',(-12.7694215127919,18.5903328777227,
0.));
#205208=CARTESIAN_POINT('Ctrl Pts',(-12.7700520897173,18.5912775137806,
0.));
#205209=CARTESIAN_POINT('Ctrl Pts',(-12.7709195951156,18.5925859134579,
0.));
#205210=CARTESIAN_POINT('Ctrl Pts',(-12.7720142287172,18.5942490615407,
0.));
#205211=CARTESIAN_POINT('Ctrl Pts',(-12.7733231262108,18.5962551167772,
0.));
#205212=CARTESIAN_POINT('Ctrl Pts',(-12.7748328937638,18.598591752595,0.));
#205213=CARTESIAN_POINT('Ctrl Pts',(-12.7765325225081,18.6012488486709,
0.));
#205214=CARTESIAN_POINT('Ctrl Pts',(-12.7784139605066,18.6042190183704,
0.));
#205215=CARTESIAN_POINT('Ctrl Pts',(-12.7804705387658,18.6074961535723,
0.));
#205216=CARTESIAN_POINT('Ctrl Pts',(-12.7826959526925,18.6110744826219,
0.));
#205217=CARTESIAN_POINT('Ctrl Pts',(-12.7850831657901,18.6149475565188,
0.));
#205218=CARTESIAN_POINT('Ctrl Pts',(-12.7876249657834,18.6191087624752,
0.));
#205219=CARTESIAN_POINT('Ctrl Pts',(-12.7903142925234,18.6235516265575,
0.));
#205220=CARTESIAN_POINT('Ctrl Pts',(-12.7931447451555,18.6282702819371,
0.));
#205221=CARTESIAN_POINT('Ctrl Pts',(-12.7961106222251,18.6332595057006,
0.));
#205222=CARTESIAN_POINT('Ctrl Pts',(-12.7992066625264,18.63851447924,0.));
#205223=CARTESIAN_POINT('Ctrl Pts',(-12.8024278770152,18.6440306327456,
0.));
#205224=CARTESIAN_POINT('Ctrl Pts',(-12.805769331162,18.6498034438986,0.));
#205225=CARTESIAN_POINT('Ctrl Pts',(-12.8092261933858,18.6558284825773,
0.));
#205226=CARTESIAN_POINT('Ctrl Pts',(-12.8127937909631,18.6621014624746,
0.));
#205227=CARTESIAN_POINT('Ctrl Pts',(-12.8164676687362,18.6686182952799,
0.));
#205228=CARTESIAN_POINT('Ctrl Pts',(-12.8202436318474,18.6753751301092,
0.));
#205229=CARTESIAN_POINT('Ctrl Pts',(-12.8241176980017,18.6823683094139,
0.));
#205230=CARTESIAN_POINT('Ctrl Pts',(-12.8280860635231,18.6895943376171,
0.));
#205231=CARTESIAN_POINT('Ctrl Pts',(-12.8321450599789,18.6970498410172,
0.));
#205232=CARTESIAN_POINT('Ctrl Pts',(-12.8362911280361,18.7047315436294,
0.));
#205233=CARTESIAN_POINT('Ctrl Pts',(-12.8405208263431,18.7126362754445,
0.));
#205234=CARTESIAN_POINT('Ctrl Pts',(-12.8448308329494,18.7207609737702,
0.));
#205235=CARTESIAN_POINT('Ctrl Pts',(-12.8492179511591,18.7291026886554,
0.));
#205236=CARTESIAN_POINT('Ctrl Pts',(-12.8536791086316,18.7376585820854,
0.));
#205237=CARTESIAN_POINT('Ctrl Pts',(-12.8582113455646,18.7464259171251,
0.));
#205238=CARTESIAN_POINT('Ctrl Pts',(-12.8628118054171,18.7554020493887,
0.));
#205239=CARTESIAN_POINT('Ctrl Pts',(-12.8674777239653,18.7645844169564,
0.));
#205240=CARTESIAN_POINT('Ctrl Pts',(-12.872206421181,18.7739705329022,0.));
#205241=CARTESIAN_POINT('Ctrl Pts',(-12.8769952998095,18.7835579840477,
0.));
#205242=CARTESIAN_POINT('Ctrl Pts',(-12.8818418427475,18.7933444285868,
0.));
#205243=CARTESIAN_POINT('Ctrl Pts',(-12.8867436109546,18.8033275941943,
0.));
#205244=CARTESIAN_POINT('Ctrl Pts',(-12.8916982409935,18.813505275782,0.));
#205245=CARTESIAN_POINT('Ctrl Pts',(-12.8967034410755,18.8238753319128,
0.));
#205246=CARTESIAN_POINT('Ctrl Pts',(-12.9017569871738,18.834435681259,0.));
#205247=CARTESIAN_POINT('Ctrl Pts',(-12.9068567191854,18.8451842990984,
0.));
#205248=CARTESIAN_POINT('Ctrl Pts',(-12.9120005369063,18.8561192136198,
0.));
#205249=CARTESIAN_POINT('Ctrl Pts',(-12.9171863977045,18.8672385038326,
0.));
#205250=CARTESIAN_POINT('Ctrl Pts',(-12.9224123144982,18.8785402977527,
0.));
#205251=CARTESIAN_POINT('Ctrl Pts',(-12.9276763536373,18.8900227704889,
0.));
#205252=CARTESIAN_POINT('Ctrl Pts',(-12.9329766328185,18.9016841423403,
0.));
#205253=CARTESIAN_POINT('Ctrl Pts',(-12.9383113190375,18.9135226769465,
0.));
#205254=CARTESIAN_POINT('Ctrl Pts',(-12.9436786266105,18.9255366795195,
0.));
#205255=CARTESIAN_POINT('Ctrl Pts',(-12.9490768151821,18.9377244950435,
0.));
#205256=CARTESIAN_POINT('Ctrl Pts',(-12.9545041877377,18.9500845064715,
0.));
#205257=CARTESIAN_POINT('Ctrl Pts',(-12.9599590886319,18.9626151329229,
0.));
#205258=CARTESIAN_POINT('Ctrl Pts',(-12.9654399021869,18.9753148284475,
0.));
#205259=CARTESIAN_POINT('Ctrl Pts',(-12.9709450512747,18.9881820807585,
0.));
#205260=CARTESIAN_POINT('Ctrl Pts',(-12.9764729959205,19.0012154099791,
0.));
#205261=CARTESIAN_POINT('Ctrl Pts',(-12.9820222318716,19.0144133673348,
0.));
#205262=CARTESIAN_POINT('Ctrl Pts',(-12.9875912893003,19.0277745339908,
0.));
#205263=CARTESIAN_POINT('Ctrl Pts',(-12.9931787316515,19.0412975200398,
0.));
#205264=CARTESIAN_POINT('Ctrl Pts',(-12.9987831544502,19.0549809634355,
0.));
#205265=CARTESIAN_POINT('Ctrl Pts',(-13.0044031841381,19.0688235289437,
0.));
#205266=CARTESIAN_POINT('Ctrl Pts',(-13.0100374768785,19.0828239070482,
0.));
#205267=CARTESIAN_POINT('Ctrl Pts',(-13.0156847176093,19.0969808131225,
0.));
#205268=CARTESIAN_POINT('Ctrl Pts',(-13.0213436191326,19.1112929866308,
0.));
#205269=CARTESIAN_POINT('Ctrl Pts',(-13.0270129211976,19.1257591903099,
0.));
#205270=CARTESIAN_POINT('Ctrl Pts',(-13.0326913895841,19.1403782093389,
0.));
#205271=CARTESIAN_POINT('Ctrl Pts',(-13.0383778152072,19.1551488505233,
0.));
#205272=CARTESIAN_POINT('Ctrl Pts',(-13.0440710133775,19.1700699416625,
0.));
#205273=CARTESIAN_POINT('Ctrl Pts',(-13.0497698230442,19.1851403308825,
0.));
#205274=CARTESIAN_POINT('Ctrl Pts',(-13.0554731060537,19.2003588859771,
0.));
#205275=CARTESIAN_POINT('Ctrl Pts',(-13.0611797463913,19.2157244937141,
0.));
#205276=CARTESIAN_POINT('Ctrl Pts',(-13.0668886494791,19.2312360592031,
0.));
#205277=CARTESIAN_POINT('Ctrl Pts',(-13.0725987415856,19.2468925053988,
0.));
#205278=CARTESIAN_POINT('Ctrl Pts',(-13.0783089692118,19.2626927725596,
0.));
#205279=CARTESIAN_POINT('Ctrl Pts',(-13.0840182984949,19.2786358177198,
0.));
#205280=CARTESIAN_POINT('Ctrl Pts',(-13.089725714597,19.2947206141246,0.));
#205281=CARTESIAN_POINT('Ctrl Pts',(-13.095430221148,19.3109461507358,0.));
#205282=CARTESIAN_POINT('Ctrl Pts',(-13.1011308397592,19.3273114318268,
0.));
#205283=CARTESIAN_POINT('Ctrl Pts',(-13.1068266095186,19.3438154765395,
0.));
#205284=CARTESIAN_POINT('Ctrl Pts',(-13.1125165865021,19.3604573184516,
0.));
#205285=CARTESIAN_POINT('Ctrl Pts',(-13.118199843271,19.3772360051093,0.));
#205286=CARTESIAN_POINT('Ctrl Pts',(-13.1238754684177,19.3941505976267,
0.));
#205287=CARTESIAN_POINT('Ctrl Pts',(-13.1295425661635,19.4112001703561,
0.));
#205288=CARTESIAN_POINT('Ctrl Pts',(-13.1352002559439,19.4283838105265,
0.));
#205289=CARTESIAN_POINT('Ctrl Pts',(-13.140847672006,19.4457006178875,0.));
#205290=CARTESIAN_POINT('Ctrl Pts',(-13.1464839629966,19.463149704325,0.));
#205291=CARTESIAN_POINT('Ctrl Pts',(-13.1521082915846,19.4807301935256,
0.));
#205292=CARTESIAN_POINT('Ctrl Pts',(-13.1577198341238,19.498441220707,0.));
#205293=CARTESIAN_POINT('Ctrl Pts',(-13.1633177803097,19.5162819323207,
0.));
#205294=CARTESIAN_POINT('Ctrl Pts',(-13.1689013328432,19.5342514857564,
0.));
#205295=CARTESIAN_POINT('Ctrl Pts',(-13.1744697070918,19.5523490490254,
0.));
#205296=CARTESIAN_POINT('Ctrl Pts',(-13.1800221307683,19.5705738004682,
0.));
#205297=CARTESIAN_POINT('Ctrl Pts',(-13.1855578436479,19.5889249285351,
0.));
#205298=CARTESIAN_POINT('Ctrl Pts',(-13.1910760972818,19.6074016315421,
0.));
#205299=CARTESIAN_POINT('Ctrl Pts',(-13.196576154715,19.6260031174244,0.));
#205300=CARTESIAN_POINT('Ctrl Pts',(-13.202057290206,19.6447286034764,0.));
#205301=CARTESIAN_POINT('Ctrl Pts',(-13.2075187889522,19.6635773160924,
0.));
#205302=CARTESIAN_POINT('Ctrl Pts',(-13.2129599468478,19.6825484905812,
0.));
#205303=CARTESIAN_POINT('Ctrl Pts',(-13.2183800702431,19.7016413709678,
0.));
#205304=CARTESIAN_POINT('Ctrl Pts',(-13.2237784757065,19.7208552097867,
0.));
#205305=CARTESIAN_POINT('Ctrl Pts',(-13.2291544897902,19.7401892678701,
0.));
#205306=CARTESIAN_POINT('Ctrl Pts',(-13.2345074487968,19.7596428141176,
0.));
#205307=CARTESIAN_POINT('Ctrl Pts',(-13.239836698568,19.7792151253297,0.));
#205308=CARTESIAN_POINT('Ctrl Pts',(-13.2451415942809,19.7989054860501,
0.));
#205309=CARTESIAN_POINT('Ctrl Pts',(-13.2504215002458,19.8187131883919,
0.));
#205310=CARTESIAN_POINT('Ctrl Pts',(-13.2556757897085,19.8386375318632,
0.));
#205311=CARTESIAN_POINT('Ctrl Pts',(-13.2609038446525,19.8586778231711,
0.));
#205312=CARTESIAN_POINT('Ctrl Pts',(-13.2661050556128,19.8788333760571,
0.));
#205313=CARTESIAN_POINT('Ctrl Pts',(-13.2712788215015,19.8991035111739,
0.));
#205314=CARTESIAN_POINT('Ctrl Pts',(-13.2764245494354,19.9194875559419,
0.));
#205315=CARTESIAN_POINT('Ctrl Pts',(-13.2815416545663,19.9399848444019,
0.));
#205316=CARTESIAN_POINT('Ctrl Pts',(-13.2866295599152,19.9605947170589,
0.));
#205317=CARTESIAN_POINT('Ctrl Pts',(-13.2916876962098,19.9813165207174,
0.));
#205318=CARTESIAN_POINT('Ctrl Pts',(-13.296715501731,20.0021496083742,0.));
#205319=CARTESIAN_POINT('Ctrl Pts',(-13.3017124221639,20.0230933391039,
0.));
#205320=CARTESIAN_POINT('Ctrl Pts',(-13.3066779104515,20.0441470779345,
0.));
#205321=CARTESIAN_POINT('Ctrl Pts',(-13.3116114266514,20.0653101957188,
0.));
#205322=CARTESIAN_POINT('Ctrl Pts',(-13.3165124377963,20.0865820689883,
0.));
#205323=CARTESIAN_POINT('Ctrl Pts',(-13.3213804177588,20.1079620798377,
0.));
#205324=CARTESIAN_POINT('Ctrl Pts',(-13.3262148471228,20.1294496158405,
0.));
#205325=CARTESIAN_POINT('Ctrl Pts',(-13.3310152130565,20.1510440699477,
0.));
#205326=CARTESIAN_POINT('Ctrl Pts',(-13.3357810091903,20.1727448403818,
0.));
#205327=CARTESIAN_POINT('Ctrl Pts',(-13.3405117354969,20.1945513305233,
0.));
#205328=CARTESIAN_POINT('Ctrl Pts',(-13.3452068981763,20.2164629487855,
0.));
#205329=CARTESIAN_POINT('Ctrl Pts',(-13.3498660095382,20.2384791085354,
0.));
#205330=CARTESIAN_POINT('Ctrl Pts',(-13.3544885878886,20.2605992280117,
0.));
#205331=CARTESIAN_POINT('Ctrl Pts',(-13.3590741574194,20.2828227302337,
0.));
#205332=CARTESIAN_POINT('Ctrl Pts',(-13.3636222481017,20.3051490429049,
0.));
#205333=CARTESIAN_POINT('Ctrl Pts',(-13.3681323955828,20.3275775983032,
0.));
#205334=CARTESIAN_POINT('Ctrl Pts',(-13.3726041410869,20.3501078331818,
0.));
#205335=CARTESIAN_POINT('Ctrl Pts',(-13.377037031319,20.3727391887187,0.));
#205336=CARTESIAN_POINT('Ctrl Pts',(-13.3814306183721,20.3954711104504,
0.));
#205337=CARTESIAN_POINT('Ctrl Pts',(-13.3857844596387,20.4183030482002,
0.));
#205338=CARTESIAN_POINT('Ctrl Pts',(-13.3900981177254,20.4412344560007,
0.));
#205339=CARTESIAN_POINT('Ctrl Pts',(-13.3943711603739,20.4642647920038,
0.));
#205340=CARTESIAN_POINT('Ctrl Pts',(-13.3986031603716,20.4873935184041,
0.));
#205341=CARTESIAN_POINT('Ctrl Pts',(-13.4027936954529,20.5106201013755,
0.));
#205342=CARTESIAN_POINT('Ctrl Pts',(-13.4069423482076,20.5339440109957,
0.));
#205343=CARTESIAN_POINT('Ctrl Pts',(-13.4110487059912,20.557364721164,0.));
#205344=CARTESIAN_POINT('Ctrl Pts',(-13.4151123608411,20.5808817095155,
0.));
#205345=CARTESIAN_POINT('Ctrl Pts',(-13.4191329093932,20.6044944573151,
0.));
#205346=CARTESIAN_POINT('Ctrl Pts',(-13.4231099528178,20.6282024494234,
0.));
#205347=CARTESIAN_POINT('Ctrl Pts',(-13.427043096765,20.6520051742867,0.));
#205348=CARTESIAN_POINT('Ctrl Pts',(-13.4309319513119,20.6759021239102,
0.));
#205349=CARTESIAN_POINT('Ctrl Pts',(-13.4347761309154,20.6998927938288,
0.));
#205350=CARTESIAN_POINT('Ctrl Pts',(-13.4385752543663,20.7239766830675,
0.));
#205351=CARTESIAN_POINT('Ctrl Pts',(-13.4423289447561,20.7481532941014,
0.));
#205352=CARTESIAN_POINT('Ctrl Pts',(-13.4460368293689,20.7724221327609,
0.));
#205353=CARTESIAN_POINT('Ctrl Pts',(-13.4496985395637,20.7967827081228,
0.));
#205354=CARTESIAN_POINT('Ctrl Pts',(-13.4533137106667,20.821234532398,0.));
#205355=CARTESIAN_POINT('Ctrl Pts',(-13.4568819818631,20.8457771208083,
0.));
#205356=CARTESIAN_POINT('Ctrl Pts',(-13.4604029960983,20.8704099914641,
0.));
#205357=CARTESIAN_POINT('Ctrl Pts',(-13.4638763999725,20.8951326652158,
0.));
#205358=CARTESIAN_POINT('Ctrl Pts',(-13.4673018437717,20.9199446657583,
0.));
#205359=CARTESIAN_POINT('Ctrl Pts',(-13.4706789815166,20.9448455197557,
0.));
#205360=CARTESIAN_POINT('Ctrl Pts',(-13.4740074710086,20.9698347569476,
0.));
#205361=CARTESIAN_POINT('Ctrl Pts',(-13.4772869738879,20.9949119102592,
0.));
#205362=CARTESIAN_POINT('Ctrl Pts',(-13.4805171556822,21.0200765158884,
0.));
#205363=CARTESIAN_POINT('Ctrl Pts',(-13.4836976858912,21.0453281134245,
0.));
#205364=CARTESIAN_POINT('Ctrl Pts',(-13.4868282377191,21.0706662455199,
0.));
#205365=CARTESIAN_POINT('Ctrl Pts',(-13.4899084877717,21.0960904575046,
0.));
#205366=CARTESIAN_POINT('Ctrl Pts',(-13.4929381157778,21.1216002970207,
0.));
#205367=CARTESIAN_POINT('Ctrl Pts',(-13.4959168042934,21.1471953136209,
0.));
#205368=CARTESIAN_POINT('Ctrl Pts',(-13.4988442384491,21.1728750584175,
0.));
#205369=CARTESIAN_POINT('Ctrl Pts',(-13.5017201056088,21.1986390835828,
0.));
#205370=CARTESIAN_POINT('Ctrl Pts',(-13.5045440957404,21.2244869429332,
0.));
#205371=CARTESIAN_POINT('Ctrl Pts',(-13.5073159019452,21.250418192743,0.));
#205372=CARTESIAN_POINT('Ctrl Pts',(-13.5100352209205,21.2764323924442,
0.));
#205373=CARTESIAN_POINT('Ctrl Pts',(-13.5127017534971,21.3025291054235,
0.));
#205374=CARTESIAN_POINT('Ctrl Pts',(-13.5153152050555,21.328707899634,0.));
#205375=CARTESIAN_POINT('Ctrl Pts',(-13.5178752862466,21.3549683486222,
0.));
#205376=CARTESIAN_POINT('Ctrl Pts',(-13.5203817122504,21.3813100304973,
0.));
#205377=CARTESIAN_POINT('Ctrl Pts',(-13.5228342013516,21.4077325259324,
0.));
#205378=CARTESIAN_POINT('Ctrl Pts',(-13.5252324737802,21.4342354165259,
0.));
#205379=CARTESIAN_POINT('Ctrl Pts',(-13.5275762503555,21.4608182828697,
0.));
#205380=CARTESIAN_POINT('Ctrl Pts',(-13.5298652514355,21.4874807030468,
0.));
#205381=CARTESIAN_POINT('Ctrl Pts',(-13.5320991952138,21.5142222501666,
0.));
#205382=CARTESIAN_POINT('Ctrl Pts',(-13.5342777983215,21.5410424932503,
0.));
#205383=CARTESIAN_POINT('Ctrl Pts',(-13.536400779028,21.5679410019001,0.));
#205384=CARTESIAN_POINT('Ctrl Pts',(-13.5384678597195,21.5949173499013,
0.));
#205385=CARTESIAN_POINT('Ctrl Pts',(-13.5404787697792,21.6219711193946,
0.));
#205386=CARTESIAN_POINT('Ctrl Pts',(-13.5424332480699,21.6491019044648,
0.));
#205387=CARTESIAN_POINT('Ctrl Pts',(-13.5443310461526,21.6763093157699,
0.));
#205388=CARTESIAN_POINT('Ctrl Pts',(-13.5461719295048,21.7035929822955,
0.));
#205389=CARTESIAN_POINT('Ctrl Pts',(-13.5479556704481,21.7309525412281,
0.));
#205390=CARTESIAN_POINT('Ctrl Pts',(-13.5496820422211,21.7583876294554,
0.));
#205391=CARTESIAN_POINT('Ctrl Pts',(-13.551350812725,21.7858978745865,0.));
#205392=CARTESIAN_POINT('Ctrl Pts',(-13.5529617381573,21.8134828857967,
0.));
#205393=CARTESIAN_POINT('Ctrl Pts',(-13.5545145573031,21.8411422456075,
0.));
#205394=CARTESIAN_POINT('Ctrl Pts',(-13.5560089839385,21.8688754989365,
0.));
#205395=CARTESIAN_POINT('Ctrl Pts',(-13.5574447178424,21.8966821688824,
0.));
#205396=CARTESIAN_POINT('Ctrl Pts',(-13.5588214586604,21.9245617765769,
0.));
#205397=CARTESIAN_POINT('Ctrl Pts',(-13.5601389185257,21.9525138592813,
0.));
#205398=CARTESIAN_POINT('Ctrl Pts',(-13.5613968357561,21.9805379899168,
0.));
#205399=CARTESIAN_POINT('Ctrl Pts',(-13.5625949868333,22.0086337943449,
0.));
#205400=CARTESIAN_POINT('Ctrl Pts',(-13.5637332022473,22.0368009736295,
0.));
#205401=CARTESIAN_POINT('Ctrl Pts',(-13.5648113689033,22.0650393089609,
0.));
#205402=CARTESIAN_POINT('Ctrl Pts',(-13.5658294169284,22.0933486464593,
0.));
#205403=CARTESIAN_POINT('Ctrl Pts',(-13.5667873105359,22.1217288871975,
0.));
#205404=CARTESIAN_POINT('Ctrl Pts',(-13.5675054919061,22.1444897575194,
0.));
#205405=CARTESIAN_POINT('Ctrl Pts',(-13.5680170531805,22.1615922805008,
0.));
#205406=CARTESIAN_POINT('Ctrl Pts',(-13.5683460612942,22.1730081264608,
0.));
#205407=CARTESIAN_POINT('Ctrl Pts',(-13.5685075571671,22.1787195904339,
0.));
#205408=CARTESIAN_POINT('',(-13.5685075571671,22.1787195904339,0.));
#205409=CARTESIAN_POINT('Origin',(-7.17139709155223,20.2687213152502,0.));
#205410=CARTESIAN_POINT('',(-7.52250298901264,21.2610617890679,0.));
#205411=CARTESIAN_POINT('',(-7.52250298901264,21.2610617890679,0.));
#205412=CARTESIAN_POINT('',(-3.58569854577611,10.1343606576251,0.));
#205413=CARTESIAN_POINT('Ctrl Pts',(-12.4230808101438,22.8400320311648,
0.));
#205414=CARTESIAN_POINT('Ctrl Pts',(-12.4230808101438,22.8400320311648,
12.));
#205415=CARTESIAN_POINT('Ctrl Pts',(-12.418215285186,22.8370364396459,0.));
#205416=CARTESIAN_POINT('Ctrl Pts',(-12.418215285186,22.8370364396459,12.));
#205417=CARTESIAN_POINT('Ctrl Pts',(-12.4084933766347,22.8310435872747,
0.));
#205418=CARTESIAN_POINT('Ctrl Pts',(-12.4084933766347,22.8310435872747,
12.));
#205419=CARTESIAN_POINT('Ctrl Pts',(-12.3939379378998,22.8220493007173,
0.));
#205420=CARTESIAN_POINT('Ctrl Pts',(-12.3939379378998,22.8220493007173,
12.));
#205421=CARTESIAN_POINT('Ctrl Pts',(-12.374585536673,22.81004690224,0.));
#205422=CARTESIAN_POINT('Ctrl Pts',(-12.374585536673,22.81004690224,12.));
#205423=CARTESIAN_POINT('Ctrl Pts',(-12.3504864740319,22.795027221673,0.));
#205424=CARTESIAN_POINT('Ctrl Pts',(-12.3504864740319,22.795027221673,12.));
#205425=CARTESIAN_POINT('Ctrl Pts',(-12.3264788926075,22.7799908974768,
0.));
#205426=CARTESIAN_POINT('Ctrl Pts',(-12.3264788926075,22.7799908974768,
12.));
#205427=CARTESIAN_POINT('Ctrl Pts',(-12.3025628601792,22.764938010105,0.));
#205428=CARTESIAN_POINT('Ctrl Pts',(-12.3025628601792,22.764938010105,12.));
#205429=CARTESIAN_POINT('Ctrl Pts',(-12.2787384750742,22.7498686970069,
0.));
#205430=CARTESIAN_POINT('Ctrl Pts',(-12.2787384750742,22.7498686970069,
12.));
#205431=CARTESIAN_POINT('Ctrl Pts',(-12.2550058702395,22.7347831655287,
0.));
#205432=CARTESIAN_POINT('Ctrl Pts',(-12.2550058702395,22.7347831655287,
12.));
#205433=CARTESIAN_POINT('Ctrl Pts',(-12.2313652198061,22.7196817119374,
0.));
#205434=CARTESIAN_POINT('Ctrl Pts',(-12.2313652198061,22.7196817119374,
12.));
#205435=CARTESIAN_POINT('Ctrl Pts',(-12.2078167360284,22.7045647168747,
0.));
#205436=CARTESIAN_POINT('Ctrl Pts',(-12.2078167360284,22.7045647168747,
12.));
#205437=CARTESIAN_POINT('Ctrl Pts',(-12.1843606579262,22.6894326205037,
0.));
#205438=CARTESIAN_POINT('Ctrl Pts',(-12.1843606579262,22.6894326205037,
12.));
#205439=CARTESIAN_POINT('Ctrl Pts',(-12.1609972423099,22.6742859034944,
0.));
#205440=CARTESIAN_POINT('Ctrl Pts',(-12.1609972423099,22.6742859034944,
12.));
#205441=CARTESIAN_POINT('Ctrl Pts',(-12.1377267537145,22.6591250653965,
0.));
#205442=CARTESIAN_POINT('Ctrl Pts',(-12.1377267537145,22.6591250653965,
12.));
#205443=CARTESIAN_POINT('Ctrl Pts',(-12.1145494550383,22.6439506046605,
0.));
#205444=CARTESIAN_POINT('Ctrl Pts',(-12.1145494550383,22.6439506046605,
12.));
#205445=CARTESIAN_POINT('Ctrl Pts',(-12.0914655972823,22.6287629967056,
0.));
#205446=CARTESIAN_POINT('Ctrl Pts',(-12.0914655972823,22.6287629967056,
12.));
#205447=CARTESIAN_POINT('Ctrl Pts',(-12.0684754113862,22.6135626764898,
0.));
#205448=CARTESIAN_POINT('Ctrl Pts',(-12.0684754113862,22.6135626764898,
12.));
#205449=CARTESIAN_POINT('Ctrl Pts',(-12.0455791139128,22.5983500505644,
0.));
#205450=CARTESIAN_POINT('Ctrl Pts',(-12.0455791139128,22.5983500505644,
12.));
#205451=CARTESIAN_POINT('Ctrl Pts',(-12.0227769113127,22.5831255061282,
0.));
#205452=CARTESIAN_POINT('Ctrl Pts',(-12.0227769113127,22.5831255061282,
12.));
#205453=CARTESIAN_POINT('Ctrl Pts',(-12.0000690046695,22.5678894211181,
0.));
#205454=CARTESIAN_POINT('Ctrl Pts',(-12.0000690046695,22.5678894211181,
12.));
#205455=CARTESIAN_POINT('Ctrl Pts',(-11.9774555943496,22.5526421741158,
0.));
#205456=CARTESIAN_POINT('Ctrl Pts',(-11.9774555943496,22.5526421741158,
12.));
#205457=CARTESIAN_POINT('Ctrl Pts',(-11.9549368843997,22.5373841537307,
0.));
#205458=CARTESIAN_POINT('Ctrl Pts',(-11.9549368843997,22.5373841537307,
12.));
#205459=CARTESIAN_POINT('Ctrl Pts',(-11.9325130877803,22.5221157697883,
0.));
#205460=CARTESIAN_POINT('Ctrl Pts',(-11.9325130877803,22.5221157697883,
12.));
#205461=CARTESIAN_POINT('Ctrl Pts',(-11.9101844254557,22.5068374513973,
0.));
#205462=CARTESIAN_POINT('Ctrl Pts',(-11.9101844254557,22.5068374513973,
12.));
#205463=CARTESIAN_POINT('Ctrl Pts',(-11.8879511239943,22.4915496418485,
0.));
#205464=CARTESIAN_POINT('Ctrl Pts',(-11.8879511239943,22.4915496418485,
12.));
#205465=CARTESIAN_POINT('Ctrl Pts',(-11.8658134137019,22.4762527946702,
0.));
#205466=CARTESIAN_POINT('Ctrl Pts',(-11.8658134137019,22.4762527946702,
12.));
#205467=CARTESIAN_POINT('Ctrl Pts',(-11.8437715264487,22.4609473690471,
0.));
#205468=CARTESIAN_POINT('Ctrl Pts',(-11.8437715264487,22.4609473690471,
12.));
#205469=CARTESIAN_POINT('Ctrl Pts',(-11.8218256937889,22.4456338258735,
0.));
#205470=CARTESIAN_POINT('Ctrl Pts',(-11.8218256937889,22.4456338258735,
12.));
#205471=CARTESIAN_POINT('Ctrl Pts',(-11.7999761445173,22.430312622646,0.));
#205472=CARTESIAN_POINT('Ctrl Pts',(-11.7999761445173,22.430312622646,12.));
#205473=CARTESIAN_POINT('Ctrl Pts',(-11.7782231042039,22.4149842125008,
0.));
#205474=CARTESIAN_POINT('Ctrl Pts',(-11.7782231042039,22.4149842125008,
12.));
#205475=CARTESIAN_POINT('Ctrl Pts',(-11.7565667964764,22.3996490469191,
0.));
#205476=CARTESIAN_POINT('Ctrl Pts',(-11.7565667964764,22.3996490469191,
12.));
#205477=CARTESIAN_POINT('Ctrl Pts',(-11.7350074437961,22.3843075773899,
0.));
#205478=CARTESIAN_POINT('Ctrl Pts',(-11.7350074437961,22.3843075773899,
12.));
#205479=CARTESIAN_POINT('Ctrl Pts',(-11.7135452684532,22.3689602575491,
0.));
#205480=CARTESIAN_POINT('Ctrl Pts',(-11.7135452684532,22.3689602575491,
12.));
#205481=CARTESIAN_POINT('Ctrl Pts',(-11.6921804934056,22.3536075450029,
0.));
#205482=CARTESIAN_POINT('Ctrl Pts',(-11.6921804934056,22.3536075450029,
12.));
#205483=CARTESIAN_POINT('Ctrl Pts',(-11.6709133432985,22.3382499035619,
0.));
#205484=CARTESIAN_POINT('Ctrl Pts',(-11.6709133432985,22.3382499035619,
12.));
#205485=CARTESIAN_POINT('Ctrl Pts',(-11.6497440449857,22.3228878043976,
0.));
#205486=CARTESIAN_POINT('Ctrl Pts',(-11.6497440449857,22.3228878043976,
12.));
#205487=CARTESIAN_POINT('Ctrl Pts',(-11.6286728270009,22.3075217249049,
0.));
#205488=CARTESIAN_POINT('Ctrl Pts',(-11.6286728270009,22.3075217249049,
12.));
#205489=CARTESIAN_POINT('Ctrl Pts',(-11.6076999192357,22.2921521480356,
0.));
#205490=CARTESIAN_POINT('Ctrl Pts',(-11.6076999192357,22.2921521480356,
12.));
#205491=CARTESIAN_POINT('Ctrl Pts',(-11.5868255525188,22.2767795614348,
0.));
#205492=CARTESIAN_POINT('Ctrl Pts',(-11.5868255525188,22.2767795614348,
12.));
#205493=CARTESIAN_POINT('Ctrl Pts',(-11.5660499582403,22.2614044566898,
0.));
#205494=CARTESIAN_POINT('Ctrl Pts',(-11.5660499582403,22.2614044566898,
12.));
#205495=CARTESIAN_POINT('Ctrl Pts',(-11.5453733679121,22.2460273284654,
0.));
#205496=CARTESIAN_POINT('Ctrl Pts',(-11.5453733679121,22.2460273284654,
12.));
#205497=CARTESIAN_POINT('Ctrl Pts',(-11.5247960128477,22.2306486738901,
0.));
#205498=CARTESIAN_POINT('Ctrl Pts',(-11.5247960128477,22.2306486738901,
12.));
#205499=CARTESIAN_POINT('Ctrl Pts',(-11.5043181244242,22.2152689931022,
0.));
#205500=CARTESIAN_POINT('Ctrl Pts',(-11.5043181244242,22.2152689931022,
12.));
#205501=CARTESIAN_POINT('Ctrl Pts',(-11.483939934259,22.1998887896436,0.));
#205502=CARTESIAN_POINT('Ctrl Pts',(-11.483939934259,22.1998887896436,12.));
#205503=CARTESIAN_POINT('Ctrl Pts',(-11.463661674411,22.184508570917,0.));
#205504=CARTESIAN_POINT('Ctrl Pts',(-11.463661674411,22.184508570917,12.));
#205505=CARTESIAN_POINT('Ctrl Pts',(-11.443483577557,22.1691288486096,0.));
#205506=CARTESIAN_POINT('Ctrl Pts',(-11.443483577557,22.1691288486096,12.));
#205507=CARTESIAN_POINT('Ctrl Pts',(-11.4234058771742,22.1537501391487,
0.));
#205508=CARTESIAN_POINT('Ctrl Pts',(-11.4234058771742,22.1537501391487,
12.));
#205509=CARTESIAN_POINT('Ctrl Pts',(-11.4034288076908,22.1383729640964,
0.));
#205510=CARTESIAN_POINT('Ctrl Pts',(-11.4034288076908,22.1383729640964,
12.));
#205511=CARTESIAN_POINT('Ctrl Pts',(-11.3835526044256,22.1229978500186,
0.));
#205512=CARTESIAN_POINT('Ctrl Pts',(-11.3835526044256,22.1229978500186,
12.));
#205513=CARTESIAN_POINT('Ctrl Pts',(-11.3637775035367,22.1076253283979,
0.));
#205514=CARTESIAN_POINT('Ctrl Pts',(-11.3637775035367,22.1076253283979,
12.));
#205515=CARTESIAN_POINT('Ctrl Pts',(-11.3441037419553,22.0922559355294,
0.));
#205516=CARTESIAN_POINT('Ctrl Pts',(-11.3441037419553,22.0922559355294,
12.));
#205517=CARTESIAN_POINT('Ctrl Pts',(-11.3245315573168,22.0768902124267,
0.));
#205518=CARTESIAN_POINT('Ctrl Pts',(-11.3245315573168,22.0768902124267,
12.));
#205519=CARTESIAN_POINT('Ctrl Pts',(-11.3050611878771,22.0615287047179,
0.));
#205520=CARTESIAN_POINT('Ctrl Pts',(-11.3050611878771,22.0615287047179,
12.));
#205521=CARTESIAN_POINT('Ctrl Pts',(-11.2856928724374,22.046171962566,0.));
#205522=CARTESIAN_POINT('Ctrl Pts',(-11.2856928724374,22.046171962566,12.));
#205523=CARTESIAN_POINT('Ctrl Pts',(-11.2664268504206,22.030820540835,0.));
#205524=CARTESIAN_POINT('Ctrl Pts',(-11.2664268504206,22.030820540835,12.));
#205525=CARTESIAN_POINT('Ctrl Pts',(-11.2472633619275,22.0154749992363,
0.));
#205526=CARTESIAN_POINT('Ctrl Pts',(-11.2472633619275,22.0154749992363,
12.));
#205527=CARTESIAN_POINT('Ctrl Pts',(-11.2282026477896,22.0001359024839,
0.));
#205528=CARTESIAN_POINT('Ctrl Pts',(-11.2282026477896,22.0001359024839,
12.));
#205529=CARTESIAN_POINT('Ctrl Pts',(-11.2092449496125,21.9848038204439,
0.));
#205530=CARTESIAN_POINT('Ctrl Pts',(-11.2092449496125,21.9848038204439,
12.));
#205531=CARTESIAN_POINT('Ctrl Pts',(-11.190390509811,21.9694793282914,0.));
#205532=CARTESIAN_POINT('Ctrl Pts',(-11.190390509811,21.9694793282914,12.));
#205533=CARTESIAN_POINT('Ctrl Pts',(-11.1716395716376,21.9541630066506,
0.));
#205534=CARTESIAN_POINT('Ctrl Pts',(-11.1716395716376,21.9541630066506,
12.));
#205535=CARTESIAN_POINT('Ctrl Pts',(-11.1529923792003,21.9388554416439,
0.));
#205536=CARTESIAN_POINT('Ctrl Pts',(-11.1529923792003,21.9388554416439,
12.));
#205537=CARTESIAN_POINT('Ctrl Pts',(-11.1344491774741,21.923557224952,0.));
#205538=CARTESIAN_POINT('Ctrl Pts',(-11.1344491774741,21.923557224952,12.));
#205539=CARTESIAN_POINT('Ctrl Pts',(-11.1160102123024,21.9082689538688,
0.));
#205540=CARTESIAN_POINT('Ctrl Pts',(-11.1160102123024,21.9082689538688,
12.));
#205541=CARTESIAN_POINT('Ctrl Pts',(-11.0976757303944,21.8929912313608,
0.));
#205542=CARTESIAN_POINT('Ctrl Pts',(-11.0976757303944,21.8929912313608,
12.));
#205543=CARTESIAN_POINT('Ctrl Pts',(-11.0794459793057,21.877724666119,0.));
#205544=CARTESIAN_POINT('Ctrl Pts',(-11.0794459793057,21.877724666119,12.));
#205545=CARTESIAN_POINT('Ctrl Pts',(-11.0613212074363,21.8624698726318,
0.));
#205546=CARTESIAN_POINT('Ctrl Pts',(-11.0613212074363,21.8624698726318,
12.));
#205547=CARTESIAN_POINT('Ctrl Pts',(-11.0433016640807,21.8472274713103,
0.));
#205548=CARTESIAN_POINT('Ctrl Pts',(-11.0433016640807,21.8472274713103,
12.));
#205549=CARTESIAN_POINT('Ctrl Pts',(-11.0253875994598,21.8319980886033,
0.));
#205550=CARTESIAN_POINT('Ctrl Pts',(-11.0253875994598,21.8319980886033,
12.));
#205551=CARTESIAN_POINT('Ctrl Pts',(-11.0075792647477,21.8167823571168,
0.));
#205552=CARTESIAN_POINT('Ctrl Pts',(-11.0075792647477,21.8167823571168,
12.));
#205553=CARTESIAN_POINT('Ctrl Pts',(-10.9898769120912,21.8015809157301,
0.));
#205554=CARTESIAN_POINT('Ctrl Pts',(-10.9898769120912,21.8015809157301,
12.));
#205555=CARTESIAN_POINT('Ctrl Pts',(-10.9722807946156,21.7863944097141,
0.));
#205556=CARTESIAN_POINT('Ctrl Pts',(-10.9722807946156,21.7863944097141,
12.));
#205557=CARTESIAN_POINT('Ctrl Pts',(-10.9547911664455,21.7712234908464,
0.));
#205558=CARTESIAN_POINT('Ctrl Pts',(-10.9547911664455,21.7712234908464,
12.));
#205559=CARTESIAN_POINT('Ctrl Pts',(-10.9374082827444,21.7560688175247,
0.));
#205560=CARTESIAN_POINT('Ctrl Pts',(-10.9374082827444,21.7560688175247,
12.));
#205561=CARTESIAN_POINT('Ctrl Pts',(-10.9201323997384,21.7409310548797,
0.));
#205562=CARTESIAN_POINT('Ctrl Pts',(-10.9201323997384,21.7409310548797,
12.));
#205563=CARTESIAN_POINT('Ctrl Pts',(-10.902963774734,21.7258108748873,0.));
#205564=CARTESIAN_POINT('Ctrl Pts',(-10.902963774734,21.7258108748873,12.));
#205565=CARTESIAN_POINT('Ctrl Pts',(-10.8859026661293,21.7107089564825,
0.));
#205566=CARTESIAN_POINT('Ctrl Pts',(-10.8859026661293,21.7107089564825,
12.));
#205567=CARTESIAN_POINT('Ctrl Pts',(-10.8689493334095,21.6956259856672,
0.));
#205568=CARTESIAN_POINT('Ctrl Pts',(-10.8689493334095,21.6956259856672,
12.));
#205569=CARTESIAN_POINT('Ctrl Pts',(-10.8521040371835,21.6805626556467,
0.));
#205570=CARTESIAN_POINT('Ctrl Pts',(-10.8521040371835,21.6805626556467,
12.));
#205571=CARTESIAN_POINT('Ctrl Pts',(-10.8353670392272,21.6655196669732,
0.));
#205572=CARTESIAN_POINT('Ctrl Pts',(-10.8353670392272,21.6655196669732,
12.));
#205573=CARTESIAN_POINT('Ctrl Pts',(-10.8187386025136,21.6504977276866,
0.));
#205574=CARTESIAN_POINT('Ctrl Pts',(-10.8187386025136,21.6504977276866,
12.));
#205575=CARTESIAN_POINT('Ctrl Pts',(-10.8022189912369,21.6354975534557,
0.));
#205576=CARTESIAN_POINT('Ctrl Pts',(-10.8022189912369,21.6354975534557,
12.));
#205577=CARTESIAN_POINT('Ctrl Pts',(-10.7858084708261,21.6205198677173,
0.));
#205578=CARTESIAN_POINT('Ctrl Pts',(-10.7858084708261,21.6205198677173,
12.));
#205579=CARTESIAN_POINT('Ctrl Pts',(-10.7695073079552,21.6055654018176,
0.));
#205580=CARTESIAN_POINT('Ctrl Pts',(-10.7695073079552,21.6055654018176,
12.));
#205581=CARTESIAN_POINT('Ctrl Pts',(-10.7533157705941,21.5906348951743,
0.));
#205582=CARTESIAN_POINT('Ctrl Pts',(-10.7533157705941,21.5906348951743,
12.));
#205583=CARTESIAN_POINT('Ctrl Pts',(-10.7372341280467,21.5757290954371,
0.));
#205584=CARTESIAN_POINT('Ctrl Pts',(-10.7372341280467,21.5757290954371,
12.));
#205585=CARTESIAN_POINT('Ctrl Pts',(-10.7212626509816,21.5608487586468,
0.));
#205586=CARTESIAN_POINT('Ctrl Pts',(-10.7212626509816,21.5608487586468,
12.));
#205587=CARTESIAN_POINT('Ctrl Pts',(-10.7054016114571,21.5459946493955,
0.));
#205588=CARTESIAN_POINT('Ctrl Pts',(-10.7054016114571,21.5459946493955,
12.));
#205589=CARTESIAN_POINT('Ctrl Pts',(-10.689651282929,21.5311675409807,0.));
#205590=CARTESIAN_POINT('Ctrl Pts',(-10.689651282929,21.5311675409807,12.));
#205591=CARTESIAN_POINT('Ctrl Pts',(-10.6740119402834,21.51636821558,0.));
#205592=CARTESIAN_POINT('Ctrl Pts',(-10.6740119402834,21.51636821558,12.));
#205593=CARTESIAN_POINT('Ctrl Pts',(-10.6584838598939,21.5015974644449,
0.));
#205594=CARTESIAN_POINT('Ctrl Pts',(-10.6584838598939,21.5015974644449,
12.));
#205595=CARTESIAN_POINT('Ctrl Pts',(-10.6430673196607,21.4868560880889,
0.));
#205596=CARTESIAN_POINT('Ctrl Pts',(-10.6430673196607,21.4868560880889,
12.));
#205597=CARTESIAN_POINT('Ctrl Pts',(-10.6277625990456,21.4721448964766,
0.));
#205598=CARTESIAN_POINT('Ctrl Pts',(-10.6277625990456,21.4721448964766,
12.));
#205599=CARTESIAN_POINT('Ctrl Pts',(-10.6125699790961,21.4574647092097,
0.));
#205600=CARTESIAN_POINT('Ctrl Pts',(-10.6125699790961,21.4574647092097,
12.));
#205601=CARTESIAN_POINT('Ctrl Pts',(-10.5974897424622,21.4428163557144,
0.));
#205602=CARTESIAN_POINT('Ctrl Pts',(-10.5974897424622,21.4428163557144,
12.));
#205603=CARTESIAN_POINT('Ctrl Pts',(-10.5825221734573,21.4282006754631,
0.));
#205604=CARTESIAN_POINT('Ctrl Pts',(-10.5825221734573,21.4282006754631,
12.));
#205605=CARTESIAN_POINT('Ctrl Pts',(-10.5676675581108,21.4136185181979,
0.));
#205606=CARTESIAN_POINT('Ctrl Pts',(-10.5676675581108,21.4136185181979,
12.));
#205607=CARTESIAN_POINT('Ctrl Pts',(-10.5529261842108,21.3990707441497,
0.));
#205608=CARTESIAN_POINT('Ctrl Pts',(-10.5529261842108,21.3990707441497,
12.));
#205609=CARTESIAN_POINT('Ctrl Pts',(-10.5382983413421,21.3845582242602,
0.));
#205610=CARTESIAN_POINT('Ctrl Pts',(-10.5382983413421,21.3845582242602,
12.));
#205611=CARTESIAN_POINT('Ctrl Pts',(-10.5237843209057,21.3700818403936,
0.));
#205612=CARTESIAN_POINT('Ctrl Pts',(-10.5237843209057,21.3700818403936,
12.));
#205613=CARTESIAN_POINT('Ctrl Pts',(-10.5093844161685,21.3556424855814,
0.));
#205614=CARTESIAN_POINT('Ctrl Pts',(-10.5093844161685,21.3556424855814,
12.));
#205615=CARTESIAN_POINT('Ctrl Pts',(-10.4950989223337,21.3412410642904,
0.));
#205616=CARTESIAN_POINT('Ctrl Pts',(-10.4950989223337,21.3412410642904,
12.));
#205617=CARTESIAN_POINT('Ctrl Pts',(-10.4809281365931,21.3268784926819,
0.));
#205618=CARTESIAN_POINT('Ctrl Pts',(-10.4809281365931,21.3268784926819,
12.));
#205619=CARTESIAN_POINT('Ctrl Pts',(-10.4668723581768,21.3125556988731,
0.));
#205620=CARTESIAN_POINT('Ctrl Pts',(-10.4668723581768,21.3125556988731,
12.));
#205621=CARTESIAN_POINT('Ctrl Pts',(-10.4529318883874,21.2982736231931,
0.));
#205622=CARTESIAN_POINT('Ctrl Pts',(-10.4529318883874,21.2982736231931,
12.));
#205623=CARTESIAN_POINT('Ctrl Pts',(-10.4391070306391,21.2840332184483,
0.));
#205624=CARTESIAN_POINT('Ctrl Pts',(-10.4391070306391,21.2840332184483,
12.));
#205625=CARTESIAN_POINT('Ctrl Pts',(-10.42539809054,21.2698354502403,0.));
#205626=CARTESIAN_POINT('Ctrl Pts',(-10.42539809054,21.2698354502403,12.));
#205627=CARTESIAN_POINT('Ctrl Pts',(-10.4118053759588,21.255681297275,0.));
#205628=CARTESIAN_POINT('Ctrl Pts',(-10.4118053759588,21.255681297275,12.));
#205629=CARTESIAN_POINT('Ctrl Pts',(-10.3983291970846,21.2415717516714,
0.));
#205630=CARTESIAN_POINT('Ctrl Pts',(-10.3983291970846,21.2415717516714,
12.));
#205631=CARTESIAN_POINT('Ctrl Pts',(-10.3849698664786,21.22750781927,0.));
#205632=CARTESIAN_POINT('Ctrl Pts',(-10.3849698664786,21.22750781927,12.));
#205633=CARTESIAN_POINT('Ctrl Pts',(-10.371727699113,21.2134905199345,0.));
#205634=CARTESIAN_POINT('Ctrl Pts',(-10.371727699113,21.2134905199345,12.));
#205635=CARTESIAN_POINT('Ctrl Pts',(-10.3586030124587,21.199520887919,0.));
#205636=CARTESIAN_POINT('Ctrl Pts',(-10.3586030124587,21.199520887919,12.));
#205637=CARTESIAN_POINT('Ctrl Pts',(-10.3455961265701,21.1855999722416,
0.));
#205638=CARTESIAN_POINT('Ctrl Pts',(-10.3455961265701,21.1855999722416,
12.));
#205639=CARTESIAN_POINT('Ctrl Pts',(-10.3327073641572,21.1717288370509,
0.));
#205640=CARTESIAN_POINT('Ctrl Pts',(-10.3327073641572,21.1717288370509,
12.));
#205641=CARTESIAN_POINT('Ctrl Pts',(-10.3199370506544,21.1579085619965,
0.));
#205642=CARTESIAN_POINT('Ctrl Pts',(-10.3199370506544,21.1579085619965,
12.));
#205643=CARTESIAN_POINT('Ctrl Pts',(-10.3072855142687,21.1441402425843,
0.));
#205644=CARTESIAN_POINT('Ctrl Pts',(-10.3072855142687,21.1441402425843,
12.));
#205645=CARTESIAN_POINT('Ctrl Pts',(-10.2947530860721,21.1304249906002,
0.));
#205646=CARTESIAN_POINT('Ctrl Pts',(-10.2947530860721,21.1304249906002,
12.));
#205647=CARTESIAN_POINT('Ctrl Pts',(-10.2823401001072,21.1167639345631,
0.));
#205648=CARTESIAN_POINT('Ctrl Pts',(-10.2823401001072,21.1167639345631,
12.));
#205649=CARTESIAN_POINT('Ctrl Pts',(-10.2700468934744,21.1031582201627,
0.));
#205650=CARTESIAN_POINT('Ctrl Pts',(-10.2700468934744,21.1031582201627,
12.));
#205651=CARTESIAN_POINT('Ctrl Pts',(-10.2578738064181,21.0896090107063,
0.));
#205652=CARTESIAN_POINT('Ctrl Pts',(-10.2578738064181,21.0896090107063,
12.));
#205653=CARTESIAN_POINT('Ctrl Pts',(-10.2458211823912,21.0761174875445,
0.));
#205654=CARTESIAN_POINT('Ctrl Pts',(-10.2458211823912,21.0761174875445,
12.));
#205655=CARTESIAN_POINT('Ctrl Pts',(-10.2338893681567,21.0626848505663,
0.));
#205656=CARTESIAN_POINT('Ctrl Pts',(-10.2338893681567,21.0626848505663,
12.));
#205657=CARTESIAN_POINT('Ctrl Pts',(-10.2220787139155,21.0493123187483,
0.));
#205658=CARTESIAN_POINT('Ctrl Pts',(-10.2220787139155,21.0493123187483,
12.));
#205659=CARTESIAN_POINT('Ctrl Pts',(-10.2103895734123,21.0360011306815,
0.));
#205660=CARTESIAN_POINT('Ctrl Pts',(-10.2103895734123,21.0360011306815,
12.));
#205661=CARTESIAN_POINT('Ctrl Pts',(-10.1988223040425,21.0227525451107,
0.));
#205662=CARTESIAN_POINT('Ctrl Pts',(-10.1988223040425,21.0227525451107,
12.));
#205663=CARTESIAN_POINT('Ctrl Pts',(-10.187377266936,21.0095678414486,0.));
#205664=CARTESIAN_POINT('Ctrl Pts',(-10.187377266936,21.0095678414486,12.));
#205665=CARTESIAN_POINT('Ctrl Pts',(-10.1760548270767,20.9964483203686,
0.));
#205666=CARTESIAN_POINT('Ctrl Pts',(-10.1760548270767,20.9964483203686,
12.));
#205667=CARTESIAN_POINT('Ctrl Pts',(-10.1648553534568,20.9833953044736,
0.));
#205668=CARTESIAN_POINT('Ctrl Pts',(-10.1648553534568,20.9833953044736,
12.));
#205669=CARTESIAN_POINT('Ctrl Pts',(-10.1537792192065,20.9704101389369,
0.));
#205670=CARTESIAN_POINT('Ctrl Pts',(-10.1537792192065,20.9704101389369,
12.));
#205671=CARTESIAN_POINT('Ctrl Pts',(-10.1428268017256,20.9574941921591,
0.));
#205672=CARTESIAN_POINT('Ctrl Pts',(-10.1428268017256,20.9574941921591,
12.));
#205673=CARTESIAN_POINT('Ctrl Pts',(-10.1319984827908,20.9446488563933,
0.));
#205674=CARTESIAN_POINT('Ctrl Pts',(-10.1319984827908,20.9446488563933,
12.));
#205675=CARTESIAN_POINT('Ctrl Pts',(-10.1212946487057,20.9318755484734,
0.));
#205676=CARTESIAN_POINT('Ctrl Pts',(-10.1212946487057,20.9318755484734,
12.));
#205677=CARTESIAN_POINT('Ctrl Pts',(-10.1107156904836,20.919175710627,0.));
#205678=CARTESIAN_POINT('Ctrl Pts',(-10.1107156904836,20.919175710627,12.));
#205679=CARTESIAN_POINT('Ctrl Pts',(-10.1002620040076,20.9065508112557,
0.));
#205680=CARTESIAN_POINT('Ctrl Pts',(-10.1002620040076,20.9065508112557,
12.));
#205681=CARTESIAN_POINT('Ctrl Pts',(-10.0899339901916,20.894002345737,0.));
#205682=CARTESIAN_POINT('Ctrl Pts',(-10.0899339901916,20.894002345737,12.));
#205683=CARTESIAN_POINT('Ctrl Pts',(-10.0797320551154,20.881531837184,0.));
#205684=CARTESIAN_POINT('Ctrl Pts',(-10.0797320551154,20.881531837184,12.));
#205685=CARTESIAN_POINT('Ctrl Pts',(-10.0696566102218,20.86914083737,0.));
#205686=CARTESIAN_POINT('Ctrl Pts',(-10.0696566102218,20.86914083737,12.));
#205687=CARTESIAN_POINT('Ctrl Pts',(-10.0597080725375,20.8568309277316,
0.));
#205688=CARTESIAN_POINT('Ctrl Pts',(-10.0597080725375,20.8568309277316,
12.));
#205689=CARTESIAN_POINT('Ctrl Pts',(-10.0498868648733,20.8446037203402,
0.));
#205690=CARTESIAN_POINT('Ctrl Pts',(-10.0498868648733,20.8446037203402,
12.));
#205691=CARTESIAN_POINT('Ctrl Pts',(-10.0401934160234,20.8324608588909,
0.));
#205692=CARTESIAN_POINT('Ctrl Pts',(-10.0401934160234,20.8324608588909,
12.));
#205693=CARTESIAN_POINT('Ctrl Pts',(-10.0306281609435,20.8204040196602,
0.));
#205694=CARTESIAN_POINT('Ctrl Pts',(-10.0306281609435,20.8204040196602,
12.));
#205695=CARTESIAN_POINT('Ctrl Pts',(-10.0211915410095,20.8084349126888,
0.));
#205696=CARTESIAN_POINT('Ctrl Pts',(-10.0211915410095,20.8084349126888,
12.));
#205697=CARTESIAN_POINT('Ctrl Pts',(-10.0118840042786,20.7965552829908,
0.));
#205698=CARTESIAN_POINT('Ctrl Pts',(-10.0118840042786,20.7965552829908,
12.));
#205699=CARTESIAN_POINT('Ctrl Pts',(-10.0027060057389,20.7847669117568,
0.));
#205700=CARTESIAN_POINT('Ctrl Pts',(-10.0027060057389,20.7847669117568,
12.));
#205701=CARTESIAN_POINT('Ctrl Pts',(-9.9936580075464,20.7730716175417,0.));
#205702=CARTESIAN_POINT('Ctrl Pts',(-9.9936580075464,20.7730716175417,12.));
#205703=CARTESIAN_POINT('Ctrl Pts',(-9.98474047926852,20.761471257499,0.));
#205704=CARTESIAN_POINT('Ctrl Pts',(-9.98474047926852,20.761471257499,12.));
#205705=CARTESIAN_POINT('Ctrl Pts',(-9.9759538982347,20.7499677289627,0.));
#205706=CARTESIAN_POINT('Ctrl Pts',(-9.9759538982347,20.7499677289627,12.));
#205707=CARTESIAN_POINT('Ctrl Pts',(-9.96729874986202,20.7385629709795,
0.));
#205708=CARTESIAN_POINT('Ctrl Pts',(-9.96729874986202,20.7385629709795,
12.));
#205709=CARTESIAN_POINT('Ctrl Pts',(-9.95877552798398,20.7272589658751,
0.));
#205710=CARTESIAN_POINT('Ctrl Pts',(-9.95877552798398,20.7272589658751,
12.));
#205711=CARTESIAN_POINT('Ctrl Pts',(-9.95038473514949,20.7160577407579,
0.));
#205712=CARTESIAN_POINT('Ctrl Pts',(-9.95038473514949,20.7160577407579,
12.));
#205713=CARTESIAN_POINT('Ctrl Pts',(-9.94212688298236,20.7049613692234,
0.));
#205714=CARTESIAN_POINT('Ctrl Pts',(-9.94212688298236,20.7049613692234,
12.));
#205715=CARTESIAN_POINT('Ctrl Pts',(-9.9340024925973,20.6939719732484,0.));
#205716=CARTESIAN_POINT('Ctrl Pts',(-9.9340024925973,20.6939719732484,12.));
#205717=CARTESIAN_POINT('Ctrl Pts',(-9.92601209498749,20.6830917250255,
0.));
#205718=CARTESIAN_POINT('Ctrl Pts',(-9.92601209498749,20.6830917250255,
12.));
#205719=CARTESIAN_POINT('Ctrl Pts',(-9.91815623141289,20.6723228488263,
0.));
#205720=CARTESIAN_POINT('Ctrl Pts',(-9.91815623141289,20.6723228488263,
12.));
#205721=CARTESIAN_POINT('Ctrl Pts',(-9.91043545377007,20.6616676228315,
0.));
#205722=CARTESIAN_POINT('Ctrl Pts',(-9.91043545377007,20.6616676228315,
12.));
#205723=CARTESIAN_POINT('Ctrl Pts',(-9.90285032516693,20.6511283817414,
0.));
#205724=CARTESIAN_POINT('Ctrl Pts',(-9.90285032516693,20.6511283817414,
12.));
#205725=CARTESIAN_POINT('Ctrl Pts',(-9.8954014204912,20.6407075193976,0.));
#205726=CARTESIAN_POINT('Ctrl Pts',(-9.8954014204912,20.6407075193976,12.));
#205727=CARTESIAN_POINT('Ctrl Pts',(-9.88808932697306,20.6304074914087,
0.));
#205728=CARTESIAN_POINT('Ctrl Pts',(-9.88808932697306,20.6304074914087,
12.));
#205729=CARTESIAN_POINT('Ctrl Pts',(-9.88091464472676,20.6202308177474,
0.));
#205730=CARTESIAN_POINT('Ctrl Pts',(-9.88091464472676,20.6202308177474,
12.));
#205731=CARTESIAN_POINT('Ctrl Pts',(-9.87387798732956,20.6101800854494,
0.));
#205732=CARTESIAN_POINT('Ctrl Pts',(-9.87387798732956,20.6101800854494,
12.));
#205733=CARTESIAN_POINT('Ctrl Pts',(-9.86697998242623,20.6002579513699,
0.));
#205734=CARTESIAN_POINT('Ctrl Pts',(-9.86697998242623,20.6002579513699,
12.));
#205735=CARTESIAN_POINT('Ctrl Pts',(-9.86022127232748,20.5904671449754,
0.));
#205736=CARTESIAN_POINT('Ctrl Pts',(-9.86022127232748,20.5904671449754,
12.));
#205737=CARTESIAN_POINT('Ctrl Pts',(-9.85360251456981,20.5808104710015,
0.));
#205738=CARTESIAN_POINT('Ctrl Pts',(-9.85360251456981,20.5808104710015,
12.));
#205739=CARTESIAN_POINT('Ctrl Pts',(-9.84712438256278,20.5712908125139,
0.));
#205740=CARTESIAN_POINT('Ctrl Pts',(-9.84712438256278,20.5712908125139,
12.));
#205741=CARTESIAN_POINT('Ctrl Pts',(-9.84078756677565,20.5619111362402,
0.));
#205742=CARTESIAN_POINT('Ctrl Pts',(-9.84078756677565,20.5619111362402,
12.));
#205743=CARTESIAN_POINT('Ctrl Pts',(-9.83459277585315,20.552674497646,0.));
#205744=CARTESIAN_POINT('Ctrl Pts',(-9.83459277585315,20.552674497646,12.));
#205745=CARTESIAN_POINT('Ctrl Pts',(-9.82854073773877,20.5435840460721,
0.));
#205746=CARTESIAN_POINT('Ctrl Pts',(-9.82854073773877,20.5435840460721,
12.));
#205747=CARTESIAN_POINT('Ctrl Pts',(-9.82263220080363,20.5346430299517,
0.));
#205748=CARTESIAN_POINT('Ctrl Pts',(-9.82263220080363,20.5346430299517,
12.));
#205749=CARTESIAN_POINT('Ctrl Pts',(-9.81686793455943,20.5258548000629,
0.));
#205750=CARTESIAN_POINT('Ctrl Pts',(-9.81686793455943,20.5258548000629,
12.));
#205751=CARTESIAN_POINT('Ctrl Pts',(-9.81124873025282,20.517222812284,0.));
#205752=CARTESIAN_POINT('Ctrl Pts',(-9.81124873025282,20.517222812284,12.));
#205753=CARTESIAN_POINT('Ctrl Pts',(-9.80577540161088,20.5087506310505,
0.));
#205754=CARTESIAN_POINT('Ctrl Pts',(-9.80577540161088,20.5087506310505,
12.));
#205755=CARTESIAN_POINT('Ctrl Pts',(-9.80044878520949,20.5004419312107,
0.));
#205756=CARTESIAN_POINT('Ctrl Pts',(-9.80044878520949,20.5004419312107,
12.));
#205757=CARTESIAN_POINT('Ctrl Pts',(-9.79526974288331,20.4923005087943,
0.));
#205758=CARTESIAN_POINT('Ctrl Pts',(-9.79526974288331,20.4923005087943,
12.));
#205759=CARTESIAN_POINT('Ctrl Pts',(-9.79023916498656,20.4843302955329,
0.));
#205760=CARTESIAN_POINT('Ctrl Pts',(-9.79023916498656,20.4843302955329,
12.));
#205761=CARTESIAN_POINT('Ctrl Pts',(-9.78535797314167,20.4765353711586,
0.));
#205762=CARTESIAN_POINT('Ctrl Pts',(-9.78535797314167,20.4765353711586,
12.));
#205763=CARTESIAN_POINT('Ctrl Pts',(-9.78062712373321,20.4689199790669,
0.));
#205764=CARTESIAN_POINT('Ctrl Pts',(-9.78062712373321,20.4689199790669,
12.));
#205765=CARTESIAN_POINT('Ctrl Pts',(-9.77604760815529,20.4614885274975,
0.));
#205766=CARTESIAN_POINT('Ctrl Pts',(-9.77604760815529,20.4614885274975,
12.));
#205767=CARTESIAN_POINT('Ctrl Pts',(-9.7716204510407,20.4542455817527,0.));
#205768=CARTESIAN_POINT('Ctrl Pts',(-9.7716204510407,20.4542455817527,12.));
#205769=CARTESIAN_POINT('Ctrl Pts',(-9.76734670980892,20.447195862298,0.));
#205770=CARTESIAN_POINT('Ctrl Pts',(-9.76734670980892,20.447195862298,12.));
#205771=CARTESIAN_POINT('Ctrl Pts',(-9.76322747195495,20.44034423294,0.));
#205772=CARTESIAN_POINT('Ctrl Pts',(-9.76322747195495,20.44034423294,12.));
#205773=CARTESIAN_POINT('Ctrl Pts',(-9.75926386289923,20.4336957355473,
0.));
#205774=CARTESIAN_POINT('Ctrl Pts',(-9.75926386289923,20.4336957355473,
12.));
#205775=CARTESIAN_POINT('Ctrl Pts',(-9.75545705902418,20.4272556476629,
0.));
#205776=CARTESIAN_POINT('Ctrl Pts',(-9.75545705902418,20.4272556476629,
12.));
#205777=CARTESIAN_POINT('Ctrl Pts',(-9.7518082978643,20.4210295275817,0.));
#205778=CARTESIAN_POINT('Ctrl Pts',(-9.7518082978643,20.4210295275817,12.));
#205779=CARTESIAN_POINT('Ctrl Pts',(-9.74831889242174,20.4150232777393,
0.));
#205780=CARTESIAN_POINT('Ctrl Pts',(-9.74831889242174,20.4150232777393,
12.));
#205781=CARTESIAN_POINT('Ctrl Pts',(-9.74499021838538,20.4092430879861,
0.));
#205782=CARTESIAN_POINT('Ctrl Pts',(-9.74499021838538,20.4092430879861,
12.));
#205783=CARTESIAN_POINT('Ctrl Pts',(-9.74182369656272,20.4036953576549,
0.));
#205784=CARTESIAN_POINT('Ctrl Pts',(-9.74182369656272,20.4036953576549,
12.));
#205785=CARTESIAN_POINT('Ctrl Pts',(-9.73882077613201,20.3983866213331,
0.));
#205786=CARTESIAN_POINT('Ctrl Pts',(-9.73882077613201,20.3983866213331,
12.));
#205787=CARTESIAN_POINT('Ctrl Pts',(-9.73598292014243,20.3933234845647,
0.));
#205788=CARTESIAN_POINT('Ctrl Pts',(-9.73598292014243,20.3933234845647,
12.));
#205789=CARTESIAN_POINT('Ctrl Pts',(-9.73331167102808,20.3885129129912,
0.));
#205790=CARTESIAN_POINT('Ctrl Pts',(-9.73331167102808,20.3885129129912,
12.));
#205791=CARTESIAN_POINT('Ctrl Pts',(-9.73080870123727,20.3839624556742,
0.));
#205792=CARTESIAN_POINT('Ctrl Pts',(-9.73080870123727,20.3839624556742,
12.));
#205793=CARTESIAN_POINT('Ctrl Pts',(-9.72847589116542,20.3796805893304,
0.));
#205794=CARTESIAN_POINT('Ctrl Pts',(-9.72847589116542,20.3796805893304,
12.));
#205795=CARTESIAN_POINT('Ctrl Pts',(-9.7263153173288,20.3756766651951,0.));
#205796=CARTESIAN_POINT('Ctrl Pts',(-9.7263153173288,20.3756766651951,12.));
#205797=CARTESIAN_POINT('Ctrl Pts',(-9.72432910043194,20.371960235676,0.));
#205798=CARTESIAN_POINT('Ctrl Pts',(-9.72432910043194,20.371960235676,12.));
#205799=CARTESIAN_POINT('Ctrl Pts',(-9.7225193072249,20.3685406190576,0.));
#205800=CARTESIAN_POINT('Ctrl Pts',(-9.7225193072249,20.3685406190576,12.));
#205801=CARTESIAN_POINT('Ctrl Pts',(-9.72088778381081,20.3654261611056,
0.));
#205802=CARTESIAN_POINT('Ctrl Pts',(-9.72088778381081,20.3654261611056,
12.));
#205803=CARTESIAN_POINT('Ctrl Pts',(-9.71943648548099,20.3626256913981,
0.));
#205804=CARTESIAN_POINT('Ctrl Pts',(-9.71943648548099,20.3626256913981,
12.));
#205805=CARTESIAN_POINT('Ctrl Pts',(-9.71816778328006,20.3601498764344,
0.));
#205806=CARTESIAN_POINT('Ctrl Pts',(-9.71816778328006,20.3601498764344,
12.));
#205807=CARTESIAN_POINT('Ctrl Pts',(-9.71708493723096,20.3580133103356,
0.));
#205808=CARTESIAN_POINT('Ctrl Pts',(-9.71708493723096,20.3580133103356,
12.));
#205809=CARTESIAN_POINT('Ctrl Pts',(-9.71619192554186,20.3562337557875,
0.));
#205810=CARTESIAN_POINT('Ctrl Pts',(-9.71619192554186,20.3562337557875,
12.));
#205811=CARTESIAN_POINT('Ctrl Pts',(-9.71549257088172,20.3548282742361,
0.));
#205812=CARTESIAN_POINT('Ctrl Pts',(-9.71549257088172,20.3548282742361,
12.));
#205813=CARTESIAN_POINT('Ctrl Pts',(-9.71498978052021,20.3538098605706,
0.));
#205814=CARTESIAN_POINT('Ctrl Pts',(-9.71498978052021,20.3538098605706,
12.));
#205815=CARTESIAN_POINT('Ctrl Pts',(-9.71474590350681,20.3533097561886,
0.));
#205816=CARTESIAN_POINT('Ctrl Pts',(-9.71474590350681,20.3533097561886,
12.));
#205817=CARTESIAN_POINT('Ctrl Pts',(-9.71465227853041,20.3531126095522,
0.));
#205818=CARTESIAN_POINT('Ctrl Pts',(-9.71465227853041,20.3531126095522,
12.));
#205819=CARTESIAN_POINT('Ctrl Pts',(-9.71462954053042,20.353060251684,0.));
#205820=CARTESIAN_POINT('Ctrl Pts',(-9.71462954053042,20.353060251684,12.));
#205821=CARTESIAN_POINT('Ctrl Pts',(-9.71462809124916,20.353053841303,0.));
#205822=CARTESIAN_POINT('Ctrl Pts',(-9.71462809124916,20.353053841303,12.));
#205823=CARTESIAN_POINT('',(-12.4230808101438,22.8400320311648,0.));
#205824=CARTESIAN_POINT('Ctrl Pts',(-12.4230808101438,22.8400320311648,
0.));
#205825=CARTESIAN_POINT('Ctrl Pts',(-12.418215285186,22.8370364396459,0.));
#205826=CARTESIAN_POINT('Ctrl Pts',(-12.4084933766347,22.8310435872747,
0.));
#205827=CARTESIAN_POINT('Ctrl Pts',(-12.3939379378998,22.8220493007173,
0.));
#205828=CARTESIAN_POINT('Ctrl Pts',(-12.374585536673,22.81004690224,0.));
#205829=CARTESIAN_POINT('Ctrl Pts',(-12.3504864740319,22.795027221673,0.));
#205830=CARTESIAN_POINT('Ctrl Pts',(-12.3264788926075,22.7799908974768,
0.));
#205831=CARTESIAN_POINT('Ctrl Pts',(-12.3025628601792,22.764938010105,0.));
#205832=CARTESIAN_POINT('Ctrl Pts',(-12.2787384750742,22.7498686970069,
0.));
#205833=CARTESIAN_POINT('Ctrl Pts',(-12.2550058702395,22.7347831655287,
0.));
#205834=CARTESIAN_POINT('Ctrl Pts',(-12.2313652198061,22.7196817119374,
0.));
#205835=CARTESIAN_POINT('Ctrl Pts',(-12.2078167360284,22.7045647168747,
0.));
#205836=CARTESIAN_POINT('Ctrl Pts',(-12.1843606579262,22.6894326205037,
0.));
#205837=CARTESIAN_POINT('Ctrl Pts',(-12.1609972423099,22.6742859034944,
0.));
#205838=CARTESIAN_POINT('Ctrl Pts',(-12.1377267537145,22.6591250653965,
0.));
#205839=CARTESIAN_POINT('Ctrl Pts',(-12.1145494550383,22.6439506046605,
0.));
#205840=CARTESIAN_POINT('Ctrl Pts',(-12.0914655972823,22.6287629967056,
0.));
#205841=CARTESIAN_POINT('Ctrl Pts',(-12.0684754113862,22.6135626764898,
0.));
#205842=CARTESIAN_POINT('Ctrl Pts',(-12.0455791139128,22.5983500505644,
0.));
#205843=CARTESIAN_POINT('Ctrl Pts',(-12.0227769113127,22.5831255061282,
0.));
#205844=CARTESIAN_POINT('Ctrl Pts',(-12.0000690046695,22.5678894211181,
0.));
#205845=CARTESIAN_POINT('Ctrl Pts',(-11.9774555943496,22.5526421741158,
0.));
#205846=CARTESIAN_POINT('Ctrl Pts',(-11.9549368843997,22.5373841537307,
0.));
#205847=CARTESIAN_POINT('Ctrl Pts',(-11.9325130877803,22.5221157697883,
0.));
#205848=CARTESIAN_POINT('Ctrl Pts',(-11.9101844254557,22.5068374513973,
0.));
#205849=CARTESIAN_POINT('Ctrl Pts',(-11.8879511239943,22.4915496418485,
0.));
#205850=CARTESIAN_POINT('Ctrl Pts',(-11.8658134137019,22.4762527946702,
0.));
#205851=CARTESIAN_POINT('Ctrl Pts',(-11.8437715264487,22.4609473690471,
0.));
#205852=CARTESIAN_POINT('Ctrl Pts',(-11.8218256937889,22.4456338258735,
0.));
#205853=CARTESIAN_POINT('Ctrl Pts',(-11.7999761445173,22.430312622646,0.));
#205854=CARTESIAN_POINT('Ctrl Pts',(-11.7782231042039,22.4149842125008,
0.));
#205855=CARTESIAN_POINT('Ctrl Pts',(-11.7565667964764,22.3996490469191,
0.));
#205856=CARTESIAN_POINT('Ctrl Pts',(-11.7350074437961,22.3843075773899,
0.));
#205857=CARTESIAN_POINT('Ctrl Pts',(-11.7135452684532,22.3689602575491,
0.));
#205858=CARTESIAN_POINT('Ctrl Pts',(-11.6921804934056,22.3536075450029,
0.));
#205859=CARTESIAN_POINT('Ctrl Pts',(-11.6709133432985,22.3382499035619,
0.));
#205860=CARTESIAN_POINT('Ctrl Pts',(-11.6497440449857,22.3228878043976,
0.));
#205861=CARTESIAN_POINT('Ctrl Pts',(-11.6286728270009,22.3075217249049,
0.));
#205862=CARTESIAN_POINT('Ctrl Pts',(-11.6076999192357,22.2921521480356,
0.));
#205863=CARTESIAN_POINT('Ctrl Pts',(-11.5868255525188,22.2767795614348,
0.));
#205864=CARTESIAN_POINT('Ctrl Pts',(-11.5660499582403,22.2614044566898,
0.));
#205865=CARTESIAN_POINT('Ctrl Pts',(-11.5453733679121,22.2460273284654,
0.));
#205866=CARTESIAN_POINT('Ctrl Pts',(-11.5247960128477,22.2306486738901,
0.));
#205867=CARTESIAN_POINT('Ctrl Pts',(-11.5043181244242,22.2152689931022,
0.));
#205868=CARTESIAN_POINT('Ctrl Pts',(-11.483939934259,22.1998887896436,0.));
#205869=CARTESIAN_POINT('Ctrl Pts',(-11.463661674411,22.184508570917,0.));
#205870=CARTESIAN_POINT('Ctrl Pts',(-11.443483577557,22.1691288486096,0.));
#205871=CARTESIAN_POINT('Ctrl Pts',(-11.4234058771742,22.1537501391487,
0.));
#205872=CARTESIAN_POINT('Ctrl Pts',(-11.4034288076908,22.1383729640964,
0.));
#205873=CARTESIAN_POINT('Ctrl Pts',(-11.3835526044256,22.1229978500186,
0.));
#205874=CARTESIAN_POINT('Ctrl Pts',(-11.3637775035367,22.1076253283979,
0.));
#205875=CARTESIAN_POINT('Ctrl Pts',(-11.3441037419553,22.0922559355294,
0.));
#205876=CARTESIAN_POINT('Ctrl Pts',(-11.3245315573168,22.0768902124267,
0.));
#205877=CARTESIAN_POINT('Ctrl Pts',(-11.3050611878771,22.0615287047179,
0.));
#205878=CARTESIAN_POINT('Ctrl Pts',(-11.2856928724374,22.046171962566,0.));
#205879=CARTESIAN_POINT('Ctrl Pts',(-11.2664268504206,22.030820540835,0.));
#205880=CARTESIAN_POINT('Ctrl Pts',(-11.2472633619275,22.0154749992363,
0.));
#205881=CARTESIAN_POINT('Ctrl Pts',(-11.2282026477896,22.0001359024839,
0.));
#205882=CARTESIAN_POINT('Ctrl Pts',(-11.2092449496125,21.9848038204439,
0.));
#205883=CARTESIAN_POINT('Ctrl Pts',(-11.190390509811,21.9694793282914,0.));
#205884=CARTESIAN_POINT('Ctrl Pts',(-11.1716395716376,21.9541630066506,
0.));
#205885=CARTESIAN_POINT('Ctrl Pts',(-11.1529923792003,21.9388554416439,
0.));
#205886=CARTESIAN_POINT('Ctrl Pts',(-11.1344491774741,21.923557224952,0.));
#205887=CARTESIAN_POINT('Ctrl Pts',(-11.1160102123024,21.9082689538688,
0.));
#205888=CARTESIAN_POINT('Ctrl Pts',(-11.0976757303944,21.8929912313608,
0.));
#205889=CARTESIAN_POINT('Ctrl Pts',(-11.0794459793057,21.877724666119,0.));
#205890=CARTESIAN_POINT('Ctrl Pts',(-11.0613212074363,21.8624698726318,
0.));
#205891=CARTESIAN_POINT('Ctrl Pts',(-11.0433016640807,21.8472274713103,
0.));
#205892=CARTESIAN_POINT('Ctrl Pts',(-11.0253875994598,21.8319980886033,
0.));
#205893=CARTESIAN_POINT('Ctrl Pts',(-11.0075792647477,21.8167823571168,
0.));
#205894=CARTESIAN_POINT('Ctrl Pts',(-10.9898769120912,21.8015809157301,
0.));
#205895=CARTESIAN_POINT('Ctrl Pts',(-10.9722807946156,21.7863944097141,
0.));
#205896=CARTESIAN_POINT('Ctrl Pts',(-10.9547911664455,21.7712234908464,
0.));
#205897=CARTESIAN_POINT('Ctrl Pts',(-10.9374082827444,21.7560688175247,
0.));
#205898=CARTESIAN_POINT('Ctrl Pts',(-10.9201323997384,21.7409310548797,
0.));
#205899=CARTESIAN_POINT('Ctrl Pts',(-10.902963774734,21.7258108748873,0.));
#205900=CARTESIAN_POINT('Ctrl Pts',(-10.8859026661293,21.7107089564825,
0.));
#205901=CARTESIAN_POINT('Ctrl Pts',(-10.8689493334095,21.6956259856672,
0.));
#205902=CARTESIAN_POINT('Ctrl Pts',(-10.8521040371835,21.6805626556467,
0.));
#205903=CARTESIAN_POINT('Ctrl Pts',(-10.8353670392272,21.6655196669732,
0.));
#205904=CARTESIAN_POINT('Ctrl Pts',(-10.8187386025136,21.6504977276866,
0.));
#205905=CARTESIAN_POINT('Ctrl Pts',(-10.8022189912369,21.6354975534557,
0.));
#205906=CARTESIAN_POINT('Ctrl Pts',(-10.7858084708261,21.6205198677173,
0.));
#205907=CARTESIAN_POINT('Ctrl Pts',(-10.7695073079552,21.6055654018176,
0.));
#205908=CARTESIAN_POINT('Ctrl Pts',(-10.7533157705941,21.5906348951743,
0.));
#205909=CARTESIAN_POINT('Ctrl Pts',(-10.7372341280467,21.5757290954371,
0.));
#205910=CARTESIAN_POINT('Ctrl Pts',(-10.7212626509816,21.5608487586468,
0.));
#205911=CARTESIAN_POINT('Ctrl Pts',(-10.7054016114571,21.5459946493955,
0.));
#205912=CARTESIAN_POINT('Ctrl Pts',(-10.689651282929,21.5311675409807,0.));
#205913=CARTESIAN_POINT('Ctrl Pts',(-10.6740119402834,21.51636821558,0.));
#205914=CARTESIAN_POINT('Ctrl Pts',(-10.6584838598939,21.5015974644449,
0.));
#205915=CARTESIAN_POINT('Ctrl Pts',(-10.6430673196607,21.4868560880889,
0.));
#205916=CARTESIAN_POINT('Ctrl Pts',(-10.6277625990456,21.4721448964766,
0.));
#205917=CARTESIAN_POINT('Ctrl Pts',(-10.6125699790961,21.4574647092097,
0.));
#205918=CARTESIAN_POINT('Ctrl Pts',(-10.5974897424622,21.4428163557144,
0.));
#205919=CARTESIAN_POINT('Ctrl Pts',(-10.5825221734573,21.4282006754631,
0.));
#205920=CARTESIAN_POINT('Ctrl Pts',(-10.5676675581108,21.4136185181979,
0.));
#205921=CARTESIAN_POINT('Ctrl Pts',(-10.5529261842108,21.3990707441497,
0.));
#205922=CARTESIAN_POINT('Ctrl Pts',(-10.5382983413421,21.3845582242602,
0.));
#205923=CARTESIAN_POINT('Ctrl Pts',(-10.5237843209057,21.3700818403936,
0.));
#205924=CARTESIAN_POINT('Ctrl Pts',(-10.5093844161685,21.3556424855814,
0.));
#205925=CARTESIAN_POINT('Ctrl Pts',(-10.4950989223337,21.3412410642904,
0.));
#205926=CARTESIAN_POINT('Ctrl Pts',(-10.4809281365931,21.3268784926819,
0.));
#205927=CARTESIAN_POINT('Ctrl Pts',(-10.4668723581768,21.3125556988731,
0.));
#205928=CARTESIAN_POINT('Ctrl Pts',(-10.4529318883874,21.2982736231931,
0.));
#205929=CARTESIAN_POINT('Ctrl Pts',(-10.4391070306391,21.2840332184483,
0.));
#205930=CARTESIAN_POINT('Ctrl Pts',(-10.42539809054,21.2698354502403,0.));
#205931=CARTESIAN_POINT('Ctrl Pts',(-10.4118053759588,21.255681297275,0.));
#205932=CARTESIAN_POINT('Ctrl Pts',(-10.3983291970846,21.2415717516714,
0.));
#205933=CARTESIAN_POINT('Ctrl Pts',(-10.3849698664786,21.22750781927,0.));
#205934=CARTESIAN_POINT('Ctrl Pts',(-10.371727699113,21.2134905199345,0.));
#205935=CARTESIAN_POINT('Ctrl Pts',(-10.3586030124587,21.199520887919,0.));
#205936=CARTESIAN_POINT('Ctrl Pts',(-10.3455961265701,21.1855999722416,
0.));
#205937=CARTESIAN_POINT('Ctrl Pts',(-10.3327073641572,21.1717288370509,
0.));
#205938=CARTESIAN_POINT('Ctrl Pts',(-10.3199370506544,21.1579085619965,
0.));
#205939=CARTESIAN_POINT('Ctrl Pts',(-10.3072855142687,21.1441402425843,
0.));
#205940=CARTESIAN_POINT('Ctrl Pts',(-10.2947530860721,21.1304249906002,
0.));
#205941=CARTESIAN_POINT('Ctrl Pts',(-10.2823401001072,21.1167639345631,
0.));
#205942=CARTESIAN_POINT('Ctrl Pts',(-10.2700468934744,21.1031582201627,
0.));
#205943=CARTESIAN_POINT('Ctrl Pts',(-10.2578738064181,21.0896090107063,
0.));
#205944=CARTESIAN_POINT('Ctrl Pts',(-10.2458211823912,21.0761174875445,
0.));
#205945=CARTESIAN_POINT('Ctrl Pts',(-10.2338893681567,21.0626848505663,
0.));
#205946=CARTESIAN_POINT('Ctrl Pts',(-10.2220787139155,21.0493123187483,
0.));
#205947=CARTESIAN_POINT('Ctrl Pts',(-10.2103895734123,21.0360011306815,
0.));
#205948=CARTESIAN_POINT('Ctrl Pts',(-10.1988223040425,21.0227525451107,
0.));
#205949=CARTESIAN_POINT('Ctrl Pts',(-10.187377266936,21.0095678414486,0.));
#205950=CARTESIAN_POINT('Ctrl Pts',(-10.1760548270767,20.9964483203686,
0.));
#205951=CARTESIAN_POINT('Ctrl Pts',(-10.1648553534568,20.9833953044736,
0.));
#205952=CARTESIAN_POINT('Ctrl Pts',(-10.1537792192065,20.9704101389369,
0.));
#205953=CARTESIAN_POINT('Ctrl Pts',(-10.1428268017256,20.9574941921591,
0.));
#205954=CARTESIAN_POINT('Ctrl Pts',(-10.1319984827908,20.9446488563933,
0.));
#205955=CARTESIAN_POINT('Ctrl Pts',(-10.1212946487057,20.9318755484734,
0.));
#205956=CARTESIAN_POINT('Ctrl Pts',(-10.1107156904836,20.919175710627,0.));
#205957=CARTESIAN_POINT('Ctrl Pts',(-10.1002620040076,20.9065508112557,
0.));
#205958=CARTESIAN_POINT('Ctrl Pts',(-10.0899339901916,20.894002345737,0.));
#205959=CARTESIAN_POINT('Ctrl Pts',(-10.0797320551154,20.881531837184,0.));
#205960=CARTESIAN_POINT('Ctrl Pts',(-10.0696566102218,20.86914083737,0.));
#205961=CARTESIAN_POINT('Ctrl Pts',(-10.0597080725375,20.8568309277316,
0.));
#205962=CARTESIAN_POINT('Ctrl Pts',(-10.0498868648733,20.8446037203402,
0.));
#205963=CARTESIAN_POINT('Ctrl Pts',(-10.0401934160234,20.8324608588909,
0.));
#205964=CARTESIAN_POINT('Ctrl Pts',(-10.0306281609435,20.8204040196602,
0.));
#205965=CARTESIAN_POINT('Ctrl Pts',(-10.0211915410095,20.8084349126888,
0.));
#205966=CARTESIAN_POINT('Ctrl Pts',(-10.0118840042786,20.7965552829908,
0.));
#205967=CARTESIAN_POINT('Ctrl Pts',(-10.0027060057389,20.7847669117568,
0.));
#205968=CARTESIAN_POINT('Ctrl Pts',(-9.9936580075464,20.7730716175417,0.));
#205969=CARTESIAN_POINT('Ctrl Pts',(-9.98474047926852,20.761471257499,0.));
#205970=CARTESIAN_POINT('Ctrl Pts',(-9.9759538982347,20.7499677289627,0.));
#205971=CARTESIAN_POINT('Ctrl Pts',(-9.96729874986202,20.7385629709795,
0.));
#205972=CARTESIAN_POINT('Ctrl Pts',(-9.95877552798398,20.7272589658751,
0.));
#205973=CARTESIAN_POINT('Ctrl Pts',(-9.95038473514949,20.7160577407579,
0.));
#205974=CARTESIAN_POINT('Ctrl Pts',(-9.94212688298236,20.7049613692234,
0.));
#205975=CARTESIAN_POINT('Ctrl Pts',(-9.9340024925973,20.6939719732484,0.));
#205976=CARTESIAN_POINT('Ctrl Pts',(-9.92601209498749,20.6830917250255,
0.));
#205977=CARTESIAN_POINT('Ctrl Pts',(-9.91815623141289,20.6723228488263,
0.));
#205978=CARTESIAN_POINT('Ctrl Pts',(-9.91043545377007,20.6616676228315,
0.));
#205979=CARTESIAN_POINT('Ctrl Pts',(-9.90285032516693,20.6511283817414,
0.));
#205980=CARTESIAN_POINT('Ctrl Pts',(-9.8954014204912,20.6407075193976,0.));
#205981=CARTESIAN_POINT('Ctrl Pts',(-9.88808932697306,20.6304074914087,
0.));
#205982=CARTESIAN_POINT('Ctrl Pts',(-9.88091464472676,20.6202308177474,
0.));
#205983=CARTESIAN_POINT('Ctrl Pts',(-9.87387798732956,20.6101800854494,
0.));
#205984=CARTESIAN_POINT('Ctrl Pts',(-9.86697998242623,20.6002579513699,
0.));
#205985=CARTESIAN_POINT('Ctrl Pts',(-9.86022127232748,20.5904671449754,
0.));
#205986=CARTESIAN_POINT('Ctrl Pts',(-9.85360251456981,20.5808104710015,
0.));
#205987=CARTESIAN_POINT('Ctrl Pts',(-9.84712438256278,20.5712908125139,
0.));
#205988=CARTESIAN_POINT('Ctrl Pts',(-9.84078756677565,20.5619111362402,
0.));
#205989=CARTESIAN_POINT('Ctrl Pts',(-9.83459277585315,20.552674497646,0.));
#205990=CARTESIAN_POINT('Ctrl Pts',(-9.82854073773877,20.5435840460721,
0.));
#205991=CARTESIAN_POINT('Ctrl Pts',(-9.82263220080363,20.5346430299517,
0.));
#205992=CARTESIAN_POINT('Ctrl Pts',(-9.81686793455943,20.5258548000629,
0.));
#205993=CARTESIAN_POINT('Ctrl Pts',(-9.81124873025282,20.517222812284,0.));
#205994=CARTESIAN_POINT('Ctrl Pts',(-9.80577540161088,20.5087506310505,
0.));
#205995=CARTESIAN_POINT('Ctrl Pts',(-9.80044878520949,20.5004419312107,
0.));
#205996=CARTESIAN_POINT('Ctrl Pts',(-9.79526974288331,20.4923005087943,
0.));
#205997=CARTESIAN_POINT('Ctrl Pts',(-9.79023916498656,20.4843302955329,
0.));
#205998=CARTESIAN_POINT('Ctrl Pts',(-9.78535797314167,20.4765353711586,
0.));
#205999=CARTESIAN_POINT('Ctrl Pts',(-9.78062712373321,20.4689199790669,
0.));
#206000=CARTESIAN_POINT('Ctrl Pts',(-9.77604760815529,20.4614885274975,
0.));
#206001=CARTESIAN_POINT('Ctrl Pts',(-9.7716204510407,20.4542455817527,0.));
#206002=CARTESIAN_POINT('Ctrl Pts',(-9.76734670980892,20.447195862298,0.));
#206003=CARTESIAN_POINT('Ctrl Pts',(-9.76322747195495,20.44034423294,0.));
#206004=CARTESIAN_POINT('Ctrl Pts',(-9.75926386289923,20.4336957355473,
0.));
#206005=CARTESIAN_POINT('Ctrl Pts',(-9.75545705902418,20.4272556476629,
0.));
#206006=CARTESIAN_POINT('Ctrl Pts',(-9.7518082978643,20.4210295275817,0.));
#206007=CARTESIAN_POINT('Ctrl Pts',(-9.74831889242174,20.4150232777393,
0.));
#206008=CARTESIAN_POINT('Ctrl Pts',(-9.74499021838538,20.4092430879861,
0.));
#206009=CARTESIAN_POINT('Ctrl Pts',(-9.74182369656272,20.4036953576549,
0.));
#206010=CARTESIAN_POINT('Ctrl Pts',(-9.73882077613201,20.3983866213331,
0.));
#206011=CARTESIAN_POINT('Ctrl Pts',(-9.73598292014243,20.3933234845647,
0.));
#206012=CARTESIAN_POINT('Ctrl Pts',(-9.73331167102808,20.3885129129912,
0.));
#206013=CARTESIAN_POINT('Ctrl Pts',(-9.73080870123727,20.3839624556742,
0.));
#206014=CARTESIAN_POINT('Ctrl Pts',(-9.72847589116542,20.3796805893304,
0.));
#206015=CARTESIAN_POINT('Ctrl Pts',(-9.7263153173288,20.3756766651951,0.));
#206016=CARTESIAN_POINT('Ctrl Pts',(-9.72432910043194,20.371960235676,0.));
#206017=CARTESIAN_POINT('Ctrl Pts',(-9.7225193072249,20.3685406190576,0.));
#206018=CARTESIAN_POINT('Ctrl Pts',(-9.72088778381081,20.3654261611056,
0.));
#206019=CARTESIAN_POINT('Ctrl Pts',(-9.71943648548099,20.3626256913981,
0.));
#206020=CARTESIAN_POINT('Ctrl Pts',(-9.71816778328006,20.3601498764344,
0.));
#206021=CARTESIAN_POINT('Ctrl Pts',(-9.71708493723096,20.3580133103356,
0.));
#206022=CARTESIAN_POINT('Ctrl Pts',(-9.71619192554186,20.3562337557875,
0.));
#206023=CARTESIAN_POINT('Ctrl Pts',(-9.71549257088172,20.3548282742361,
0.));
#206024=CARTESIAN_POINT('Ctrl Pts',(-9.71498978052021,20.3538098605706,
0.));
#206025=CARTESIAN_POINT('Ctrl Pts',(-9.71474590350681,20.3533097561886,
0.));
#206026=CARTESIAN_POINT('Ctrl Pts',(-9.71465227853041,20.3531126095522,
0.));
#206027=CARTESIAN_POINT('Ctrl Pts',(-9.71462954053042,20.353060251684,0.));
#206028=CARTESIAN_POINT('Ctrl Pts',(-9.71462809124916,20.353053841303,0.));
#206029=CARTESIAN_POINT('',(-12.4230808101438,22.8400320311648,0.));
#206030=CARTESIAN_POINT('Ctrl Pts',(-7.52250298901264,21.2610617890679,
0.));
#206031=CARTESIAN_POINT('Ctrl Pts',(-7.52250298901264,21.2610617890679,
12.));
#206032=CARTESIAN_POINT('Ctrl Pts',(-7.5225064970397,21.2610673466886,0.));
#206033=CARTESIAN_POINT('Ctrl Pts',(-7.5225064970397,21.2610673466886,12.));
#206034=CARTESIAN_POINT('Ctrl Pts',(-7.52252744144904,21.2611204474866,
0.));
#206035=CARTESIAN_POINT('Ctrl Pts',(-7.52252744144904,21.2611204474866,
12.));
#206036=CARTESIAN_POINT('Ctrl Pts',(-7.52260064231661,21.261326054066,0.));
#206037=CARTESIAN_POINT('Ctrl Pts',(-7.52260064231661,21.261326054066,12.));
#206038=CARTESIAN_POINT('Ctrl Pts',(-7.5227818224267,21.2618521283555,0.));
#206039=CARTESIAN_POINT('Ctrl Pts',(-7.5227818224267,21.2618521283555,12.));
#206040=CARTESIAN_POINT('Ctrl Pts',(-7.52314642316199,21.262927782038,0.));
#206041=CARTESIAN_POINT('Ctrl Pts',(-7.52314642316199,21.262927782038,12.));
#206042=CARTESIAN_POINT('Ctrl Pts',(-7.52364573027553,21.2644161259962,
0.));
#206043=CARTESIAN_POINT('Ctrl Pts',(-7.52364573027553,21.2644161259962,
12.));
#206044=CARTESIAN_POINT('Ctrl Pts',(-7.52427261074298,21.2663059157058,
0.));
#206045=CARTESIAN_POINT('Ctrl Pts',(-7.52427261074298,21.2663059157058,
12.));
#206046=CARTESIAN_POINT('Ctrl Pts',(-7.5250177033353,21.2685823838671,0.));
#206047=CARTESIAN_POINT('Ctrl Pts',(-7.5250177033353,21.2685823838671,12.));
#206048=CARTESIAN_POINT('Ctrl Pts',(-7.5258712609553,21.2712301573466,0.));
#206049=CARTESIAN_POINT('Ctrl Pts',(-7.5258712609553,21.2712301573466,12.));
#206050=CARTESIAN_POINT('Ctrl Pts',(-7.52682526918541,21.2742366113579,
0.));
#206051=CARTESIAN_POINT('Ctrl Pts',(-7.52682526918541,21.2742366113579,
12.));
#206052=CARTESIAN_POINT('Ctrl Pts',(-7.52787386225333,21.2775925269652,
0.));
#206053=CARTESIAN_POINT('Ctrl Pts',(-7.52787386225333,21.2775925269652,
12.));
#206054=CARTESIAN_POINT('Ctrl Pts',(-7.52901217930408,21.2812902781143,
0.));
#206055=CARTESIAN_POINT('Ctrl Pts',(-7.52901217930408,21.2812902781143,
12.));
#206056=CARTESIAN_POINT('Ctrl Pts',(-7.53023562438229,21.2853226580657,
0.));
#206057=CARTESIAN_POINT('Ctrl Pts',(-7.53023562438229,21.2853226580657,
12.));
#206058=CARTESIAN_POINT('Ctrl Pts',(-7.53153906987855,21.2896816163842,
0.));
#206059=CARTESIAN_POINT('Ctrl Pts',(-7.53153906987855,21.2896816163842,
12.));
#206060=CARTESIAN_POINT('Ctrl Pts',(-7.53291726078527,21.2943588989331,
0.));
#206061=CARTESIAN_POINT('Ctrl Pts',(-7.53291726078527,21.2943588989331,
12.));
#206062=CARTESIAN_POINT('Ctrl Pts',(-7.53436505309943,21.2993464250717,
0.));
#206063=CARTESIAN_POINT('Ctrl Pts',(-7.53436505309943,21.2993464250717,
12.));
#206064=CARTESIAN_POINT('Ctrl Pts',(-7.53587778251736,21.3046368712157,
0.));
#206065=CARTESIAN_POINT('Ctrl Pts',(-7.53587778251736,21.3046368712157,
12.));
#206066=CARTESIAN_POINT('Ctrl Pts',(-7.53745129364616,21.310223716773,0.));
#206067=CARTESIAN_POINT('Ctrl Pts',(-7.53745129364616,21.310223716773,12.));
#206068=CARTESIAN_POINT('Ctrl Pts',(-7.53908175169898,21.3161009456256,
0.));
#206069=CARTESIAN_POINT('Ctrl Pts',(-7.53908175169898,21.3161009456256,
12.));
#206070=CARTESIAN_POINT('Ctrl Pts',(-7.54076552038279,21.3222628524165,
0.));
#206071=CARTESIAN_POINT('Ctrl Pts',(-7.54076552038279,21.3222628524165,
12.));
#206072=CARTESIAN_POINT('Ctrl Pts',(-7.54249900377031,21.328703791771,0.));
#206073=CARTESIAN_POINT('Ctrl Pts',(-7.54249900377031,21.328703791771,12.));
#206074=CARTESIAN_POINT('Ctrl Pts',(-7.54427868151268,21.3354182340149,
0.));
#206075=CARTESIAN_POINT('Ctrl Pts',(-7.54427868151268,21.3354182340149,
12.));
#206076=CARTESIAN_POINT('Ctrl Pts',(-7.54610114948347,21.3424008295038,
0.));
#206077=CARTESIAN_POINT('Ctrl Pts',(-7.54610114948347,21.3424008295038,
12.));
#206078=CARTESIAN_POINT('Ctrl Pts',(-7.5479631624633,21.3496464761531,0.));
#206079=CARTESIAN_POINT('Ctrl Pts',(-7.5479631624633,21.3496464761531,12.));
#206080=CARTESIAN_POINT('Ctrl Pts',(-7.5498616652131,21.3571503685855,0.));
#206081=CARTESIAN_POINT('Ctrl Pts',(-7.5498616652131,21.3571503685855,12.));
#206082=CARTESIAN_POINT('Ctrl Pts',(-7.55179375777444,21.3649079431865,
0.));
#206083=CARTESIAN_POINT('Ctrl Pts',(-7.55179375777444,21.3649079431865,
12.));
#206084=CARTESIAN_POINT('Ctrl Pts',(-7.55375667080029,21.3729148390243,
0.));
#206085=CARTESIAN_POINT('Ctrl Pts',(-7.55375667080029,21.3729148390243,
12.));
#206086=CARTESIAN_POINT('Ctrl Pts',(-7.55574773403503,21.3811668478932,
0.));
#206087=CARTESIAN_POINT('Ctrl Pts',(-7.55574773403503,21.3811668478932,
12.));
#206088=CARTESIAN_POINT('Ctrl Pts',(-7.55776435731417,21.3896598842117,
0.));
#206089=CARTESIAN_POINT('Ctrl Pts',(-7.55776435731417,21.3896598842117,
12.));
#206090=CARTESIAN_POINT('Ctrl Pts',(-7.55980403700611,21.3983899952987,
0.));
#206091=CARTESIAN_POINT('Ctrl Pts',(-7.55980403700611,21.3983899952987,
12.));
#206092=CARTESIAN_POINT('Ctrl Pts',(-7.56186435703622,21.4073533630365,
0.));
#206093=CARTESIAN_POINT('Ctrl Pts',(-7.56186435703622,21.4073533630365,
12.));
#206094=CARTESIAN_POINT('Ctrl Pts',(-7.56394299313685,21.4165463106254,
0.));
#206095=CARTESIAN_POINT('Ctrl Pts',(-7.56394299313685,21.4165463106254,
12.));
#206096=CARTESIAN_POINT('Ctrl Pts',(-7.56603771218712,21.4259653015736,
0.));
#206097=CARTESIAN_POINT('Ctrl Pts',(-7.56603771218712,21.4259653015736,
12.));
#206098=CARTESIAN_POINT('Ctrl Pts',(-7.56814636360847,21.4356069261513,
0.));
#206099=CARTESIAN_POINT('Ctrl Pts',(-7.56814636360847,21.4356069261513,
12.));
#206100=CARTESIAN_POINT('Ctrl Pts',(-7.57026687261166,21.4454678907509,
0.));
#206101=CARTESIAN_POINT('Ctrl Pts',(-7.57026687261166,21.4454678907509,
12.));
#206102=CARTESIAN_POINT('Ctrl Pts',(-7.57239723223506,21.4555450053142,
0.));
#206103=CARTESIAN_POINT('Ctrl Pts',(-7.57239723223506,21.4555450053142,
12.));
#206104=CARTESIAN_POINT('Ctrl Pts',(-7.57453549743412,21.4658351740128,
0.));
#206105=CARTESIAN_POINT('Ctrl Pts',(-7.57453549743412,21.4658351740128,
12.));
#206106=CARTESIAN_POINT('Ctrl Pts',(-7.57667978402987,21.4763353936762,
0.));
#206107=CARTESIAN_POINT('Ctrl Pts',(-7.57667978402987,21.4763353936762,
12.));
#206108=CARTESIAN_POINT('Ctrl Pts',(-7.57882826679132,21.4870427508194,
0.));
#206109=CARTESIAN_POINT('Ctrl Pts',(-7.57882826679132,21.4870427508194,
12.));
#206110=CARTESIAN_POINT('Ctrl Pts',(-7.58097917790744,21.4979544192744,
0.));
#206111=CARTESIAN_POINT('Ctrl Pts',(-7.58097917790744,21.4979544192744,
12.));
#206112=CARTESIAN_POINT('Ctrl Pts',(-7.5831308051918,21.5090676573873,0.));
#206113=CARTESIAN_POINT('Ctrl Pts',(-7.5831308051918,21.5090676573873,12.));
#206114=CARTESIAN_POINT('Ctrl Pts',(-7.5852814891913,21.5203798035299,0.));
#206115=CARTESIAN_POINT('Ctrl Pts',(-7.5852814891913,21.5203798035299,12.));
#206116=CARTESIAN_POINT('Ctrl Pts',(-7.58742962034834,21.5318882716736,
0.));
#206117=CARTESIAN_POINT('Ctrl Pts',(-7.58742962034834,21.5318882716736,
12.));
#206118=CARTESIAN_POINT('Ctrl Pts',(-7.58957363620014,21.543590547011,0.));
#206119=CARTESIAN_POINT('Ctrl Pts',(-7.58957363620014,21.543590547011,12.));
#206120=CARTESIAN_POINT('Ctrl Pts',(-7.59171201844777,21.5554841813462,
0.));
#206121=CARTESIAN_POINT('Ctrl Pts',(-7.59171201844777,21.5554841813462,
12.));
#206122=CARTESIAN_POINT('Ctrl Pts',(-7.59384329124918,21.5675667904726,
0.));
#206123=CARTESIAN_POINT('Ctrl Pts',(-7.59384329124918,21.5675667904726,
12.));
#206124=CARTESIAN_POINT('Ctrl Pts',(-7.59596601973584,21.5798360518978,
0.));
#206125=CARTESIAN_POINT('Ctrl Pts',(-7.59596601973584,21.5798360518978,
12.));
#206126=CARTESIAN_POINT('Ctrl Pts',(-7.59807880846195,21.5922897024466,
0.));
#206127=CARTESIAN_POINT('Ctrl Pts',(-7.59807880846195,21.5922897024466,
12.));
#206128=CARTESIAN_POINT('Ctrl Pts',(-7.60018029988241,21.6049255358843,
0.));
#206129=CARTESIAN_POINT('Ctrl Pts',(-7.60018029988241,21.6049255358843,
12.));
#206130=CARTESIAN_POINT('Ctrl Pts',(-7.60226917285429,21.617741400599,0.));
#206131=CARTESIAN_POINT('Ctrl Pts',(-7.60226917285429,21.617741400599,12.));
#206132=CARTESIAN_POINT('Ctrl Pts',(-7.60434414118296,21.6307351973822,
0.));
#206133=CARTESIAN_POINT('Ctrl Pts',(-7.60434414118296,21.6307351973822,
12.));
#206134=CARTESIAN_POINT('Ctrl Pts',(-7.60640395216357,21.6439048771743,
0.));
#206135=CARTESIAN_POINT('Ctrl Pts',(-7.60640395216357,21.6439048771743,
12.));
#206136=CARTESIAN_POINT('Ctrl Pts',(-7.60844738512874,21.6572484388081,
0.));
#206137=CARTESIAN_POINT('Ctrl Pts',(-7.60844738512874,21.6572484388081,
12.));
#206138=CARTESIAN_POINT('Ctrl Pts',(-7.61047325000956,21.6707639267576,
0.));
#206139=CARTESIAN_POINT('Ctrl Pts',(-7.61047325000956,21.6707639267576,
12.));
#206140=CARTESIAN_POINT('Ctrl Pts',(-7.61248038630268,21.6844494295815,
0.));
#206141=CARTESIAN_POINT('Ctrl Pts',(-7.61248038630268,21.6844494295815,
12.));
#206142=CARTESIAN_POINT('Ctrl Pts',(-7.61446766202787,21.6983030783322,
0.));
#206143=CARTESIAN_POINT('Ctrl Pts',(-7.61446766202787,21.6983030783322,
12.));
#206144=CARTESIAN_POINT('Ctrl Pts',(-7.61643397270421,21.7123230449834,
0.));
#206145=CARTESIAN_POINT('Ctrl Pts',(-7.61643397270421,21.7123230449834,
12.));
#206146=CARTESIAN_POINT('Ctrl Pts',(-7.61837824030538,21.7265075407975,
0.));
#206147=CARTESIAN_POINT('Ctrl Pts',(-7.61837824030538,21.7265075407975,
12.));
#206148=CARTESIAN_POINT('Ctrl Pts',(-7.62029941230855,21.7408548148656,
0.));
#206149=CARTESIAN_POINT('Ctrl Pts',(-7.62029941230855,21.7408548148656,
12.));
#206150=CARTESIAN_POINT('Ctrl Pts',(-7.62219646084228,21.7553631528328,
0.));
#206151=CARTESIAN_POINT('Ctrl Pts',(-7.62219646084228,21.7553631528328,
12.));
#206152=CARTESIAN_POINT('Ctrl Pts',(-7.62406838181166,21.7700308755584,
0.));
#206153=CARTESIAN_POINT('Ctrl Pts',(-7.62406838181166,21.7700308755584,
12.));
#206154=CARTESIAN_POINT('Ctrl Pts',(-7.62591419404512,21.7848563378021,
0.));
#206155=CARTESIAN_POINT('Ctrl Pts',(-7.62591419404512,21.7848563378021,
12.));
#206156=CARTESIAN_POINT('Ctrl Pts',(-7.62773293842389,21.799837926858,0.));
#206157=CARTESIAN_POINT('Ctrl Pts',(-7.62773293842389,21.799837926858,12.));
#206158=CARTESIAN_POINT('Ctrl Pts',(-7.62952367718127,21.814974061509,0.));
#206159=CARTESIAN_POINT('Ctrl Pts',(-7.62952367718127,21.814974061509,12.));
#206160=CARTESIAN_POINT('Ctrl Pts',(-7.63128549323023,21.8302631910195,
0.));
#206161=CARTESIAN_POINT('Ctrl Pts',(-7.63128549323023,21.8302631910195,
12.));
#206162=CARTESIAN_POINT('Ctrl Pts',(-7.63301748948936,21.8457037941084,
0.));
#206163=CARTESIAN_POINT('Ctrl Pts',(-7.63301748948936,21.8457037941084,
12.));
#206164=CARTESIAN_POINT('Ctrl Pts',(-7.63471878821226,21.8612943779089,
0.));
#206165=CARTESIAN_POINT('Ctrl Pts',(-7.63471878821226,21.8612943779089,
12.));
#206166=CARTESIAN_POINT('Ctrl Pts',(-7.636388530334,21.8770334769496,0.));
#206167=CARTESIAN_POINT('Ctrl Pts',(-7.636388530334,21.8770334769496,12.));
#206168=CARTESIAN_POINT('Ctrl Pts',(-7.63802587492035,21.8929196523514,
0.));
#206169=CARTESIAN_POINT('Ctrl Pts',(-7.63802587492035,21.8929196523514,
12.));
#206170=CARTESIAN_POINT('Ctrl Pts',(-7.63962999860927,21.9089514909874,
0.));
#206171=CARTESIAN_POINT('Ctrl Pts',(-7.63962999860927,21.9089514909874,
12.));
#206172=CARTESIAN_POINT('Ctrl Pts',(-7.64120009506532,21.9251276046546,
0.));
#206173=CARTESIAN_POINT('Ctrl Pts',(-7.64120009506532,21.9251276046546,
12.));
#206174=CARTESIAN_POINT('Ctrl Pts',(-7.64273537442682,21.9414466292072,
0.));
#206175=CARTESIAN_POINT('Ctrl Pts',(-7.64273537442682,21.9414466292072,
12.));
#206176=CARTESIAN_POINT('Ctrl Pts',(-7.64423506279123,21.9579072237651,
0.));
#206177=CARTESIAN_POINT('Ctrl Pts',(-7.64423506279123,21.9579072237651,
12.));
#206178=CARTESIAN_POINT('Ctrl Pts',(-7.64569840177336,21.9745080700798,
0.));
#206179=CARTESIAN_POINT('Ctrl Pts',(-7.64569840177336,21.9745080700798,
12.));
#206180=CARTESIAN_POINT('Ctrl Pts',(-7.6471246480525,21.9912478718542,0.));
#206181=CARTESIAN_POINT('Ctrl Pts',(-7.6471246480525,21.9912478718542,12.));
#206182=CARTESIAN_POINT('Ctrl Pts',(-7.64851307293352,22.0081253540774,
0.));
#206183=CARTESIAN_POINT('Ctrl Pts',(-7.64851307293352,22.0081253540774,
12.));
#206184=CARTESIAN_POINT('Ctrl Pts',(-7.64986296190168,22.0251392623209,
0.));
#206185=CARTESIAN_POINT('Ctrl Pts',(-7.64986296190168,22.0251392623209,
12.));
#206186=CARTESIAN_POINT('Ctrl Pts',(-7.65117361421358,22.0422883621174,
0.));
#206187=CARTESIAN_POINT('Ctrl Pts',(-7.65117361421358,22.0422883621174,
12.));
#206188=CARTESIAN_POINT('Ctrl Pts',(-7.65244434253113,22.0595714384431,
0.));
#206189=CARTESIAN_POINT('Ctrl Pts',(-7.65244434253113,22.0595714384431,
12.));
#206190=CARTESIAN_POINT('Ctrl Pts',(-7.65367447254949,22.0769872951596,
0.));
#206191=CARTESIAN_POINT('Ctrl Pts',(-7.65367447254949,22.0769872951596,
12.));
#206192=CARTESIAN_POINT('Ctrl Pts',(-7.65486334263644,22.094534754469,0.));
#206193=CARTESIAN_POINT('Ctrl Pts',(-7.65486334263644,22.094534754469,12.));
#206194=CARTESIAN_POINT('Ctrl Pts',(-7.65601030346807,22.1122126563329,
0.));
#206195=CARTESIAN_POINT('Ctrl Pts',(-7.65601030346807,22.1122126563329,
12.));
#206196=CARTESIAN_POINT('Ctrl Pts',(-7.65711471769397,22.1300198579675,
0.));
#206197=CARTESIAN_POINT('Ctrl Pts',(-7.65711471769397,22.1300198579675,
12.));
#206198=CARTESIAN_POINT('Ctrl Pts',(-7.65817595963349,22.1479552334211,
0.));
#206199=CARTESIAN_POINT('Ctrl Pts',(-7.65817595963349,22.1479552334211,
12.));
#206200=CARTESIAN_POINT('Ctrl Pts',(-7.6591934149693,22.1660176731178,0.));
#206201=CARTESIAN_POINT('Ctrl Pts',(-7.6591934149693,22.1660176731178,12.));
#206202=CARTESIAN_POINT('Ctrl Pts',(-7.66016648045005,22.1842060834091,
0.));
#206203=CARTESIAN_POINT('Ctrl Pts',(-7.66016648045005,22.1842060834091,
12.));
#206204=CARTESIAN_POINT('Ctrl Pts',(-7.66109456359271,22.2025193860964,
0.));
#206205=CARTESIAN_POINT('Ctrl Pts',(-7.66109456359271,22.2025193860964,
12.));
#206206=CARTESIAN_POINT('Ctrl Pts',(-7.661977082404,22.2209565180085,0.));
#206207=CARTESIAN_POINT('Ctrl Pts',(-7.661977082404,22.2209565180085,12.));
#206208=CARTESIAN_POINT('Ctrl Pts',(-7.66281346512509,22.2395164306547,
0.));
#206209=CARTESIAN_POINT('Ctrl Pts',(-7.66281346512509,22.2395164306547,
12.));
#206210=CARTESIAN_POINT('Ctrl Pts',(-7.66360314997641,22.258198089848,0.));
#206211=CARTESIAN_POINT('Ctrl Pts',(-7.66360314997641,22.258198089848,12.));
#206212=CARTESIAN_POINT('Ctrl Pts',(-7.66434558490979,22.2770004753335,
0.));
#206213=CARTESIAN_POINT('Ctrl Pts',(-7.66434558490979,22.2770004753335,
12.));
#206214=CARTESIAN_POINT('Ctrl Pts',(-7.66504022736299,22.2959225803937,
0.));
#206215=CARTESIAN_POINT('Ctrl Pts',(-7.66504022736299,22.2959225803937,
12.));
#206216=CARTESIAN_POINT('Ctrl Pts',(-7.66568654402494,22.314963411484,0.));
#206217=CARTESIAN_POINT('Ctrl Pts',(-7.66568654402494,22.314963411484,12.));
#206218=CARTESIAN_POINT('Ctrl Pts',(-7.66628401061952,22.3341219879469,
0.));
#206219=CARTESIAN_POINT('Ctrl Pts',(-7.66628401061952,22.3341219879469,
12.));
#206220=CARTESIAN_POINT('Ctrl Pts',(-7.66683211169158,22.3533973417021,
0.));
#206221=CARTESIAN_POINT('Ctrl Pts',(-7.66683211169158,22.3533973417021,
12.));
#206222=CARTESIAN_POINT('Ctrl Pts',(-7.66733034039883,22.372788516936,0.));
#206223=CARTESIAN_POINT('Ctrl Pts',(-7.66733034039883,22.372788516936,12.));
#206224=CARTESIAN_POINT('Ctrl Pts',(-7.6677781983079,22.3922945697773,0.));
#206225=CARTESIAN_POINT('Ctrl Pts',(-7.6677781983079,22.3922945697773,12.));
#206226=CARTESIAN_POINT('Ctrl Pts',(-7.6681751951964,22.4119145679758,0.));
#206227=CARTESIAN_POINT('Ctrl Pts',(-7.6681751951964,22.4119145679758,12.));
#206228=CARTESIAN_POINT('Ctrl Pts',(-7.66852084886704,22.4316475906603,
0.));
#206229=CARTESIAN_POINT('Ctrl Pts',(-7.66852084886704,22.4316475906603,
12.));
#206230=CARTESIAN_POINT('Ctrl Pts',(-7.66881468496635,22.4514927280855,
0.));
#206231=CARTESIAN_POINT('Ctrl Pts',(-7.66881468496635,22.4514927280855,
12.));
#206232=CARTESIAN_POINT('Ctrl Pts',(-7.66905623680831,22.47144908137,0.));
#206233=CARTESIAN_POINT('Ctrl Pts',(-7.66905623680831,22.47144908137,12.));
#206234=CARTESIAN_POINT('Ctrl Pts',(-7.66924504520315,22.4915157622312,
0.));
#206235=CARTESIAN_POINT('Ctrl Pts',(-7.66924504520315,22.4915157622312,
12.));
#206236=CARTESIAN_POINT('Ctrl Pts',(-7.66938065829108,22.5116918927031,
0.));
#206237=CARTESIAN_POINT('Ctrl Pts',(-7.66938065829108,22.5116918927031,
12.));
#206238=CARTESIAN_POINT('Ctrl Pts',(-7.66946263138144,22.53197660492,0.));
#206239=CARTESIAN_POINT('Ctrl Pts',(-7.66946263138144,22.53197660492,12.));
#206240=CARTESIAN_POINT('Ctrl Pts',(-7.66949052679693,22.5523690409116,
0.));
#206241=CARTESIAN_POINT('Ctrl Pts',(-7.66949052679693,22.5523690409116,
12.));
#206242=CARTESIAN_POINT('Ctrl Pts',(-7.66946391372306,22.5728683523831,
0.));
#206243=CARTESIAN_POINT('Ctrl Pts',(-7.66946391372306,22.5728683523831,
12.));
#206244=CARTESIAN_POINT('Ctrl Pts',(-7.66938236806233,22.5934737004953,
0.));
#206245=CARTESIAN_POINT('Ctrl Pts',(-7.66938236806233,22.5934737004953,
12.));
#206246=CARTESIAN_POINT('Ctrl Pts',(-7.66924547229414,22.6141842556243,
0.));
#206247=CARTESIAN_POINT('Ctrl Pts',(-7.66924547229414,22.6141842556243,
12.));
#206248=CARTESIAN_POINT('Ctrl Pts',(-7.66905281533715,22.6349991971541,
0.));
#206249=CARTESIAN_POINT('Ctrl Pts',(-7.66905281533715,22.6349991971541,
12.));
#206250=CARTESIAN_POINT('Ctrl Pts',(-7.66880399241323,22.6559177133127,
0.));
#206251=CARTESIAN_POINT('Ctrl Pts',(-7.66880399241323,22.6559177133127,
12.));
#206252=CARTESIAN_POINT('Ctrl Pts',(-7.66849860491743,22.6769390009885,
0.));
#206253=CARTESIAN_POINT('Ctrl Pts',(-7.66849860491743,22.6769390009885,
12.));
#206254=CARTESIAN_POINT('Ctrl Pts',(-7.66813626029275,22.6980622655446,
0.));
#206255=CARTESIAN_POINT('Ctrl Pts',(-7.66813626029275,22.6980622655446,
12.));
#206256=CARTESIAN_POINT('Ctrl Pts',(-7.66771657191027,22.7192867206245,
0.));
#206257=CARTESIAN_POINT('Ctrl Pts',(-7.66771657191027,22.7192867206245,
12.));
#206258=CARTESIAN_POINT('Ctrl Pts',(-7.6672391589544,22.7406115879513,0.));
#206259=CARTESIAN_POINT('Ctrl Pts',(-7.6672391589544,22.7406115879513,12.));
#206260=CARTESIAN_POINT('Ctrl Pts',(-7.66670364630299,22.7620360971843,
0.));
#206261=CARTESIAN_POINT('Ctrl Pts',(-7.66670364630299,22.7620360971843,
12.));
#206262=CARTESIAN_POINT('Ctrl Pts',(-7.66610966441273,22.7835594857699,
0.));
#206263=CARTESIAN_POINT('Ctrl Pts',(-7.66610966441273,22.7835594857699,
12.));
#206264=CARTESIAN_POINT('Ctrl Pts',(-7.66545684920987,22.8051809987833,
0.));
#206265=CARTESIAN_POINT('Ctrl Pts',(-7.66545684920987,22.8051809987833,
12.));
#206266=CARTESIAN_POINT('Ctrl Pts',(-7.66474484198549,22.8268998887678,
0.));
#206267=CARTESIAN_POINT('Ctrl Pts',(-7.66474484198549,22.8268998887678,
12.));
#206268=CARTESIAN_POINT('Ctrl Pts',(-7.66397328929803,22.848715415557,0.));
#206269=CARTESIAN_POINT('Ctrl Pts',(-7.66397328929803,22.848715415557,12.));
#206270=CARTESIAN_POINT('Ctrl Pts',(-7.66314184287337,22.8706268461283,
0.));
#206271=CARTESIAN_POINT('Ctrl Pts',(-7.66314184287337,22.8706268461283,
12.));
#206272=CARTESIAN_POINT('Ctrl Pts',(-7.66225015950156,22.8926334544883,
0.));
#206273=CARTESIAN_POINT('Ctrl Pts',(-7.66225015950156,22.8926334544883,
12.));
#206274=CARTESIAN_POINT('Ctrl Pts',(-7.66129790094108,22.9147345215421,
0.));
#206275=CARTESIAN_POINT('Ctrl Pts',(-7.66129790094108,22.9147345215421,
12.));
#206276=CARTESIAN_POINT('Ctrl Pts',(-7.66028473382778,22.9369293349593,
0.));
#206277=CARTESIAN_POINT('Ctrl Pts',(-7.66028473382778,22.9369293349593,
12.));
#206278=CARTESIAN_POINT('Ctrl Pts',(-7.65921032958902,22.959217189033,0.));
#206279=CARTESIAN_POINT('Ctrl Pts',(-7.65921032958902,22.959217189033,12.));
#206280=CARTESIAN_POINT('Ctrl Pts',(-7.65807436436432,22.9815973845296,
0.));
#206281=CARTESIAN_POINT('Ctrl Pts',(-7.65807436436432,22.9815973845296,
12.));
#206282=CARTESIAN_POINT('Ctrl Pts',(-7.65687651891304,23.0040692285814,
0.));
#206283=CARTESIAN_POINT('Ctrl Pts',(-7.65687651891304,23.0040692285814,
12.));
#206284=CARTESIAN_POINT('Ctrl Pts',(-7.65561647852534,23.0266320345787,
0.));
#206285=CARTESIAN_POINT('Ctrl Pts',(-7.65561647852534,23.0266320345787,
12.));
#206286=CARTESIAN_POINT('Ctrl Pts',(-7.65429393293946,23.0492851220528,
0.));
#206287=CARTESIAN_POINT('Ctrl Pts',(-7.65429393293946,23.0492851220528,
12.));
#206288=CARTESIAN_POINT('Ctrl Pts',(-7.65290857626358,23.072027816555,0.));
#206289=CARTESIAN_POINT('Ctrl Pts',(-7.65290857626358,23.072027816555,12.));
#206290=CARTESIAN_POINT('Ctrl Pts',(-7.65146010690476,23.094859449525,0.));
#206291=CARTESIAN_POINT('Ctrl Pts',(-7.65146010690476,23.094859449525,12.));
#206292=CARTESIAN_POINT('Ctrl Pts',(-7.6499482274986,23.1177793581679,0.));
#206293=CARTESIAN_POINT('Ctrl Pts',(-7.6499482274986,23.1177793581679,12.));
#206294=CARTESIAN_POINT('Ctrl Pts',(-7.64837264482943,23.1407868853819,
0.));
#206295=CARTESIAN_POINT('Ctrl Pts',(-7.64837264482943,23.1407868853819,
12.));
#206296=CARTESIAN_POINT('Ctrl Pts',(-7.64673306975805,23.1638813796694,
0.));
#206297=CARTESIAN_POINT('Ctrl Pts',(-7.64673306975805,23.1638813796694,
12.));
#206298=CARTESIAN_POINT('Ctrl Pts',(-7.64502921715483,23.1870621950452,
0.));
#206299=CARTESIAN_POINT('Ctrl Pts',(-7.64502921715483,23.1870621950452,
12.));
#206300=CARTESIAN_POINT('Ctrl Pts',(-7.6432608058368,23.2103286909398,0.));
#206301=CARTESIAN_POINT('Ctrl Pts',(-7.6432608058368,23.2103286909398,12.));
#206302=CARTESIAN_POINT('Ctrl Pts',(-7.64142755851504,23.2336802320912,
0.));
#206303=CARTESIAN_POINT('Ctrl Pts',(-7.64142755851504,23.2336802320912,
12.));
#206304=CARTESIAN_POINT('Ctrl Pts',(-7.63952920172835,23.2571161884488,
0.));
#206305=CARTESIAN_POINT('Ctrl Pts',(-7.63952920172835,23.2571161884488,
12.));
#206306=CARTESIAN_POINT('Ctrl Pts',(-7.63756546576374,23.2806359350855,
0.));
#206307=CARTESIAN_POINT('Ctrl Pts',(-7.63756546576374,23.2806359350855,
12.));
#206308=CARTESIAN_POINT('Ctrl Pts',(-7.63553608458783,23.3042388521022,
0.));
#206309=CARTESIAN_POINT('Ctrl Pts',(-7.63553608458783,23.3042388521022,
12.));
#206310=CARTESIAN_POINT('Ctrl Pts',(-7.63344079578161,23.3279243245241,
0.));
#206311=CARTESIAN_POINT('Ctrl Pts',(-7.63344079578161,23.3279243245241,
12.));
#206312=CARTESIAN_POINT('Ctrl Pts',(-7.63127934048136,23.3516917421972,
0.));
#206313=CARTESIAN_POINT('Ctrl Pts',(-7.63127934048136,23.3516917421972,
12.));
#206314=CARTESIAN_POINT('Ctrl Pts',(-7.62905146332593,23.3755404996636,
0.));
#206315=CARTESIAN_POINT('Ctrl Pts',(-7.62905146332593,23.3755404996636,
12.));
#206316=CARTESIAN_POINT('Ctrl Pts',(-7.62675691240329,23.399469996112,0.));
#206317=CARTESIAN_POINT('Ctrl Pts',(-7.62675691240329,23.399469996112,12.));
#206318=CARTESIAN_POINT('Ctrl Pts',(-7.6243954392005,23.4234796353542,0.));
#206319=CARTESIAN_POINT('Ctrl Pts',(-7.6243954392005,23.4234796353542,12.));
#206320=CARTESIAN_POINT('Ctrl Pts',(-7.62196679855955,23.4475688257854,
0.));
#206321=CARTESIAN_POINT('Ctrl Pts',(-7.62196679855955,23.4475688257854,
12.));
#206322=CARTESIAN_POINT('Ctrl Pts',(-7.61947074863977,23.4717369803438,
0.));
#206323=CARTESIAN_POINT('Ctrl Pts',(-7.61947074863977,23.4717369803438,
12.));
#206324=CARTESIAN_POINT('Ctrl Pts',(-7.61690705088319,23.4959835164609,
0.));
#206325=CARTESIAN_POINT('Ctrl Pts',(-7.61690705088319,23.4959835164609,
12.));
#206326=CARTESIAN_POINT('Ctrl Pts',(-7.61427546999298,23.5203078560129,
0.));
#206327=CARTESIAN_POINT('Ctrl Pts',(-7.61427546999298,23.5203078560129,
12.));
#206328=CARTESIAN_POINT('Ctrl Pts',(-7.61157577385372,23.544709425203,0.));
#206329=CARTESIAN_POINT('Ctrl Pts',(-7.61157577385372,23.544709425203,12.));
#206330=CARTESIAN_POINT('Ctrl Pts',(-7.608807733446,23.5691876544244,0.));
#206331=CARTESIAN_POINT('Ctrl Pts',(-7.608807733446,23.5691876544244,12.));
#206332=CARTESIAN_POINT('Ctrl Pts',(-7.60597112277094,23.5937419781245,
0.));
#206333=CARTESIAN_POINT('Ctrl Pts',(-7.60597112277094,23.5937419781245,
12.));
#206334=CARTESIAN_POINT('Ctrl Pts',(-7.60306571877806,23.6183718346576,
0.));
#206335=CARTESIAN_POINT('Ctrl Pts',(-7.60306571877806,23.6183718346576,
12.));
#206336=CARTESIAN_POINT('Ctrl Pts',(-7.60009130130126,23.6430766661418,
0.));
#206337=CARTESIAN_POINT('Ctrl Pts',(-7.60009130130126,23.6430766661418,
12.));
#206338=CARTESIAN_POINT('Ctrl Pts',(-7.59704765299567,23.6678559182875,
0.));
#206339=CARTESIAN_POINT('Ctrl Pts',(-7.59704765299567,23.6678559182875,
12.));
#206340=CARTESIAN_POINT('Ctrl Pts',(-7.59393455934035,23.6927090405066,
0.));
#206341=CARTESIAN_POINT('Ctrl Pts',(-7.59393455934035,23.6927090405066,
12.));
#206342=CARTESIAN_POINT('Ctrl Pts',(-7.5907518086532,23.7176354860456,0.));
#206343=CARTESIAN_POINT('Ctrl Pts',(-7.5907518086532,23.7176354860456,12.));
#206344=CARTESIAN_POINT('Ctrl Pts',(-7.58749919210826,23.7426347121006,
0.));
#206345=CARTESIAN_POINT('Ctrl Pts',(-7.58749919210826,23.7426347121006,
12.));
#206346=CARTESIAN_POINT('Ctrl Pts',(-7.58417650376271,23.7677061799376,
0.));
#206347=CARTESIAN_POINT('Ctrl Pts',(-7.58417650376271,23.7677061799376,
12.));
#206348=CARTESIAN_POINT('Ctrl Pts',(-7.58078354058213,23.7928493549908,
0.));
#206349=CARTESIAN_POINT('Ctrl Pts',(-7.58078354058213,23.7928493549908,
12.));
#206350=CARTESIAN_POINT('Ctrl Pts',(-7.57732010249066,23.8180637069976,
0.));
#206351=CARTESIAN_POINT('Ctrl Pts',(-7.57732010249066,23.8180637069976,
12.));
#206352=CARTESIAN_POINT('Ctrl Pts',(-7.57378599219814,23.8433487096132,
0.));
#206353=CARTESIAN_POINT('Ctrl Pts',(-7.57378599219814,23.8433487096132,
12.));
#206354=CARTESIAN_POINT('Ctrl Pts',(-7.57018101500709,23.8687038399595,
0.));
#206355=CARTESIAN_POINT('Ctrl Pts',(-7.57018101500709,23.8687038399595,
12.));
#206356=CARTESIAN_POINT('Ctrl Pts',(-7.56650497863791,23.8941285782002,
0.));
#206357=CARTESIAN_POINT('Ctrl Pts',(-7.56650497863791,23.8941285782002,
12.));
#206358=CARTESIAN_POINT('Ctrl Pts',(-7.56275769304773,23.9196224070759,
0.));
#206359=CARTESIAN_POINT('Ctrl Pts',(-7.56275769304773,23.9196224070759,
12.));
#206360=CARTESIAN_POINT('Ctrl Pts',(-7.5589389702768,23.9451848115002,0.));
#206361=CARTESIAN_POINT('Ctrl Pts',(-7.5589389702768,23.9451848115002,12.));
#206362=CARTESIAN_POINT('Ctrl Pts',(-7.55504862424808,23.9708152779886,
0.));
#206363=CARTESIAN_POINT('Ctrl Pts',(-7.55504862424808,23.9708152779886,
12.));
#206364=CARTESIAN_POINT('Ctrl Pts',(-7.55108647097432,23.9965132953187,
0.));
#206365=CARTESIAN_POINT('Ctrl Pts',(-7.55108647097432,23.9965132953187,
12.));
#206366=CARTESIAN_POINT('Ctrl Pts',(-7.54705232885895,24.0222783554531,
0.));
#206367=CARTESIAN_POINT('Ctrl Pts',(-7.54705232885895,24.0222783554531,
12.));
#206368=CARTESIAN_POINT('Ctrl Pts',(-7.54294601896128,24.0481099543353,
0.));
#206369=CARTESIAN_POINT('Ctrl Pts',(-7.54294601896128,24.0481099543353,
12.));
#206370=CARTESIAN_POINT('Ctrl Pts',(-7.53876736531005,24.0740075927984,
0.));
#206371=CARTESIAN_POINT('Ctrl Pts',(-7.53876736531005,24.0740075927984,
12.));
#206372=CARTESIAN_POINT('Ctrl Pts',(-7.53451619514658,24.0999707772643,
0.));
#206373=CARTESIAN_POINT('Ctrl Pts',(-7.53451619514658,24.0999707772643,
12.));
#206374=CARTESIAN_POINT('Ctrl Pts',(-7.53019233935536,24.1259990209211,
0.));
#206375=CARTESIAN_POINT('Ctrl Pts',(-7.53019233935536,24.1259990209211,
12.));
#206376=CARTESIAN_POINT('Ctrl Pts',(-7.52579563201479,24.152091842537,0.));
#206377=CARTESIAN_POINT('Ctrl Pts',(-7.52579563201479,24.152091842537,12.));
#206378=CARTESIAN_POINT('Ctrl Pts',(-7.52132590953862,24.1782487641602,
0.));
#206379=CARTESIAN_POINT('Ctrl Pts',(-7.52132590953862,24.1782487641602,
12.));
#206380=CARTESIAN_POINT('Ctrl Pts',(-7.51678300997998,24.2044693092356,
0.));
#206381=CARTESIAN_POINT('Ctrl Pts',(-7.51678300997998,24.2044693092356,
12.));
#206382=CARTESIAN_POINT('Ctrl Pts',(-7.51216677222199,24.230753000389,0.));
#206383=CARTESIAN_POINT('Ctrl Pts',(-7.51216677222199,24.230753000389,12.));
#206384=CARTESIAN_POINT('Ctrl Pts',(-7.50747703535115,24.2570993577032,
0.));
#206385=CARTESIAN_POINT('Ctrl Pts',(-7.50747703535115,24.2570993577032,
12.));
#206386=CARTESIAN_POINT('Ctrl Pts',(-7.50271363765098,24.2835078958966,
0.));
#206387=CARTESIAN_POINT('Ctrl Pts',(-7.50271363765098,24.2835078958966,
12.));
#206388=CARTESIAN_POINT('Ctrl Pts',(-7.49787641695359,24.3099781253345,
0.));
#206389=CARTESIAN_POINT('Ctrl Pts',(-7.49787641695359,24.3099781253345,
12.));
#206390=CARTESIAN_POINT('Ctrl Pts',(-7.4929652125233,24.3365095573673,0.));
#206391=CARTESIAN_POINT('Ctrl Pts',(-7.4929652125233,24.3365095573673,12.));
#206392=CARTESIAN_POINT('Ctrl Pts',(-7.48797986651828,24.3631017084513,
0.));
#206393=CARTESIAN_POINT('Ctrl Pts',(-7.48797986651828,24.3631017084513,
12.));
#206394=CARTESIAN_POINT('Ctrl Pts',(-7.48292022569254,24.3897541049248,
0.));
#206395=CARTESIAN_POINT('Ctrl Pts',(-7.48292022569254,24.3897541049248,
12.));
#206396=CARTESIAN_POINT('Ctrl Pts',(-7.47778614286573,24.4164662871165,
0.));
#206397=CARTESIAN_POINT('Ctrl Pts',(-7.47778614286573,24.4164662871165,
12.));
#206398=CARTESIAN_POINT('Ctrl Pts',(-7.47257747883319,24.4432378146501,
0.));
#206399=CARTESIAN_POINT('Ctrl Pts',(-7.47257747883319,24.4432378146501,
12.));
#206400=CARTESIAN_POINT('Ctrl Pts',(-7.46729410308923,24.4700682684544,
0.));
#206401=CARTESIAN_POINT('Ctrl Pts',(-7.46729410308923,24.4700682684544,
12.));
#206402=CARTESIAN_POINT('Ctrl Pts',(-7.46193588961642,24.4969572391509,
0.));
#206403=CARTESIAN_POINT('Ctrl Pts',(-7.46193588961642,24.4969572391509,
12.));
#206404=CARTESIAN_POINT('Ctrl Pts',(-7.45650271336045,24.52390431731,0.));
#206405=CARTESIAN_POINT('Ctrl Pts',(-7.45650271336045,24.52390431731,12.));
#206406=CARTESIAN_POINT('Ctrl Pts',(-7.45099444651296,24.5509090831579,
0.));
#206407=CARTESIAN_POINT('Ctrl Pts',(-7.45099444651296,24.5509090831579,
12.));
#206408=CARTESIAN_POINT('Ctrl Pts',(-7.44541095473163,24.5779710960865,
0.));
#206409=CARTESIAN_POINT('Ctrl Pts',(-7.44541095473163,24.5779710960865,
12.));
#206410=CARTESIAN_POINT('Ctrl Pts',(-7.43975209375375,24.6050898852349,
0.));
#206411=CARTESIAN_POINT('Ctrl Pts',(-7.43975209375375,24.6050898852349,
12.));
#206412=CARTESIAN_POINT('Ctrl Pts',(-7.4340177048922,24.6322649369472,0.));
#206413=CARTESIAN_POINT('Ctrl Pts',(-7.4340177048922,24.6322649369472,12.));
#206414=CARTESIAN_POINT('Ctrl Pts',(-7.42820762158681,24.659495712869,0.));
#206415=CARTESIAN_POINT('Ctrl Pts',(-7.42820762158681,24.659495712869,12.));
#206416=CARTESIAN_POINT('Ctrl Pts',(-7.42232167765763,24.6867816727118,
0.));
#206417=CARTESIAN_POINT('Ctrl Pts',(-7.42232167765763,24.6867816727118,
12.));
#206418=CARTESIAN_POINT('Ctrl Pts',(-7.41635971481243,24.7141222949988,
0.));
#206419=CARTESIAN_POINT('Ctrl Pts',(-7.41635971481243,24.7141222949988,
12.));
#206420=CARTESIAN_POINT('Ctrl Pts',(-7.41032159082173,24.7415170994754,
0.));
#206421=CARTESIAN_POINT('Ctrl Pts',(-7.41032159082173,24.7415170994754,
12.));
#206422=CARTESIAN_POINT('Ctrl Pts',(-7.40420718661754,24.7689656669005,
0.));
#206423=CARTESIAN_POINT('Ctrl Pts',(-7.40420718661754,24.7689656669005,
12.));
#206424=CARTESIAN_POINT('Ctrl Pts',(-7.39801641583612,24.7964676646518,
0.));
#206425=CARTESIAN_POINT('Ctrl Pts',(-7.39801641583612,24.7964676646518,
12.));
#206426=CARTESIAN_POINT('Ctrl Pts',(-7.39174922586841,24.8240228521042,
0.));
#206427=CARTESIAN_POINT('Ctrl Pts',(-7.39174922586841,24.8240228521042,
12.));
#206428=CARTESIAN_POINT('Ctrl Pts',(-7.38540558904946,24.8516310625367,
0.));
#206429=CARTESIAN_POINT('Ctrl Pts',(-7.38540558904946,24.8516310625367,
12.));
#206430=CARTESIAN_POINT('Ctrl Pts',(-7.3789854964161,24.8792921911309,0.));
#206431=CARTESIAN_POINT('Ctrl Pts',(-7.3789854964161,24.8792921911309,12.));
#206432=CARTESIAN_POINT('Ctrl Pts',(-7.37378825962718,24.9014633826201,
0.));
#206433=CARTESIAN_POINT('Ctrl Pts',(-7.37378825962718,24.9014633826201,
12.));
#206434=CARTESIAN_POINT('Ctrl Pts',(-7.36985593120696,24.9181155530631,
0.));
#206435=CARTESIAN_POINT('Ctrl Pts',(-7.36985593120696,24.9181155530631,
12.));
#206436=CARTESIAN_POINT('Ctrl Pts',(-7.3672190902906,24.9292275670705,0.));
#206437=CARTESIAN_POINT('Ctrl Pts',(-7.3672190902906,24.9292275670705,12.));
#206438=CARTESIAN_POINT('Ctrl Pts',(-7.36589684767344,24.9347862158358,
0.));
#206439=CARTESIAN_POINT('Ctrl Pts',(-7.36589684767344,24.9347862158358,
12.));
#206440=CARTESIAN_POINT('',(-7.36589684767344,24.9347862158358,0.));
#206441=CARTESIAN_POINT('Ctrl Pts',(-7.52250298901264,21.2610617890679,
0.));
#206442=CARTESIAN_POINT('Ctrl Pts',(-7.5225064970397,21.2610673466886,0.));
#206443=CARTESIAN_POINT('Ctrl Pts',(-7.52252744144904,21.2611204474866,
0.));
#206444=CARTESIAN_POINT('Ctrl Pts',(-7.52260064231661,21.261326054066,0.));
#206445=CARTESIAN_POINT('Ctrl Pts',(-7.5227818224267,21.2618521283555,0.));
#206446=CARTESIAN_POINT('Ctrl Pts',(-7.52314642316199,21.262927782038,0.));
#206447=CARTESIAN_POINT('Ctrl Pts',(-7.52364573027553,21.2644161259962,
0.));
#206448=CARTESIAN_POINT('Ctrl Pts',(-7.52427261074298,21.2663059157058,
0.));
#206449=CARTESIAN_POINT('Ctrl Pts',(-7.5250177033353,21.2685823838671,0.));
#206450=CARTESIAN_POINT('Ctrl Pts',(-7.5258712609553,21.2712301573466,0.));
#206451=CARTESIAN_POINT('Ctrl Pts',(-7.52682526918541,21.2742366113579,
0.));
#206452=CARTESIAN_POINT('Ctrl Pts',(-7.52787386225333,21.2775925269652,
0.));
#206453=CARTESIAN_POINT('Ctrl Pts',(-7.52901217930408,21.2812902781143,
0.));
#206454=CARTESIAN_POINT('Ctrl Pts',(-7.53023562438229,21.2853226580657,
0.));
#206455=CARTESIAN_POINT('Ctrl Pts',(-7.53153906987855,21.2896816163842,
0.));
#206456=CARTESIAN_POINT('Ctrl Pts',(-7.53291726078527,21.2943588989331,
0.));
#206457=CARTESIAN_POINT('Ctrl Pts',(-7.53436505309943,21.2993464250717,
0.));
#206458=CARTESIAN_POINT('Ctrl Pts',(-7.53587778251736,21.3046368712157,
0.));
#206459=CARTESIAN_POINT('Ctrl Pts',(-7.53745129364616,21.310223716773,0.));
#206460=CARTESIAN_POINT('Ctrl Pts',(-7.53908175169898,21.3161009456256,
0.));
#206461=CARTESIAN_POINT('Ctrl Pts',(-7.54076552038279,21.3222628524165,
0.));
#206462=CARTESIAN_POINT('Ctrl Pts',(-7.54249900377031,21.328703791771,0.));
#206463=CARTESIAN_POINT('Ctrl Pts',(-7.54427868151268,21.3354182340149,
0.));
#206464=CARTESIAN_POINT('Ctrl Pts',(-7.54610114948347,21.3424008295038,
0.));
#206465=CARTESIAN_POINT('Ctrl Pts',(-7.5479631624633,21.3496464761531,0.));
#206466=CARTESIAN_POINT('Ctrl Pts',(-7.5498616652131,21.3571503685855,0.));
#206467=CARTESIAN_POINT('Ctrl Pts',(-7.55179375777444,21.3649079431865,
0.));
#206468=CARTESIAN_POINT('Ctrl Pts',(-7.55375667080029,21.3729148390243,
0.));
#206469=CARTESIAN_POINT('Ctrl Pts',(-7.55574773403503,21.3811668478932,
0.));
#206470=CARTESIAN_POINT('Ctrl Pts',(-7.55776435731417,21.3896598842117,
0.));
#206471=CARTESIAN_POINT('Ctrl Pts',(-7.55980403700611,21.3983899952987,
0.));
#206472=CARTESIAN_POINT('Ctrl Pts',(-7.56186435703622,21.4073533630365,
0.));
#206473=CARTESIAN_POINT('Ctrl Pts',(-7.56394299313685,21.4165463106254,
0.));
#206474=CARTESIAN_POINT('Ctrl Pts',(-7.56603771218712,21.4259653015736,
0.));
#206475=CARTESIAN_POINT('Ctrl Pts',(-7.56814636360847,21.4356069261513,
0.));
#206476=CARTESIAN_POINT('Ctrl Pts',(-7.57026687261166,21.4454678907509,
0.));
#206477=CARTESIAN_POINT('Ctrl Pts',(-7.57239723223506,21.4555450053142,
0.));
#206478=CARTESIAN_POINT('Ctrl Pts',(-7.57453549743412,21.4658351740128,
0.));
#206479=CARTESIAN_POINT('Ctrl Pts',(-7.57667978402987,21.4763353936762,
0.));
#206480=CARTESIAN_POINT('Ctrl Pts',(-7.57882826679132,21.4870427508194,
0.));
#206481=CARTESIAN_POINT('Ctrl Pts',(-7.58097917790744,21.4979544192744,
0.));
#206482=CARTESIAN_POINT('Ctrl Pts',(-7.5831308051918,21.5090676573873,0.));
#206483=CARTESIAN_POINT('Ctrl Pts',(-7.5852814891913,21.5203798035299,0.));
#206484=CARTESIAN_POINT('Ctrl Pts',(-7.58742962034834,21.5318882716736,
0.));
#206485=CARTESIAN_POINT('Ctrl Pts',(-7.58957363620014,21.543590547011,0.));
#206486=CARTESIAN_POINT('Ctrl Pts',(-7.59171201844777,21.5554841813462,
0.));
#206487=CARTESIAN_POINT('Ctrl Pts',(-7.59384329124918,21.5675667904726,
0.));
#206488=CARTESIAN_POINT('Ctrl Pts',(-7.59596601973584,21.5798360518978,
0.));
#206489=CARTESIAN_POINT('Ctrl Pts',(-7.59807880846195,21.5922897024466,
0.));
#206490=CARTESIAN_POINT('Ctrl Pts',(-7.60018029988241,21.6049255358843,
0.));
#206491=CARTESIAN_POINT('Ctrl Pts',(-7.60226917285429,21.617741400599,0.));
#206492=CARTESIAN_POINT('Ctrl Pts',(-7.60434414118296,21.6307351973822,
0.));
#206493=CARTESIAN_POINT('Ctrl Pts',(-7.60640395216357,21.6439048771743,
0.));
#206494=CARTESIAN_POINT('Ctrl Pts',(-7.60844738512874,21.6572484388081,
0.));
#206495=CARTESIAN_POINT('Ctrl Pts',(-7.61047325000956,21.6707639267576,
0.));
#206496=CARTESIAN_POINT('Ctrl Pts',(-7.61248038630268,21.6844494295815,
0.));
#206497=CARTESIAN_POINT('Ctrl Pts',(-7.61446766202787,21.6983030783322,
0.));
#206498=CARTESIAN_POINT('Ctrl Pts',(-7.61643397270421,21.7123230449834,
0.));
#206499=CARTESIAN_POINT('Ctrl Pts',(-7.61837824030538,21.7265075407975,
0.));
#206500=CARTESIAN_POINT('Ctrl Pts',(-7.62029941230855,21.7408548148656,
0.));
#206501=CARTESIAN_POINT('Ctrl Pts',(-7.62219646084228,21.7553631528328,
0.));
#206502=CARTESIAN_POINT('Ctrl Pts',(-7.62406838181166,21.7700308755584,
0.));
#206503=CARTESIAN_POINT('Ctrl Pts',(-7.62591419404512,21.7848563378021,
0.));
#206504=CARTESIAN_POINT('Ctrl Pts',(-7.62773293842389,21.799837926858,0.));
#206505=CARTESIAN_POINT('Ctrl Pts',(-7.62952367718127,21.814974061509,0.));
#206506=CARTESIAN_POINT('Ctrl Pts',(-7.63128549323023,21.8302631910195,
0.));
#206507=CARTESIAN_POINT('Ctrl Pts',(-7.63301748948936,21.8457037941084,
0.));
#206508=CARTESIAN_POINT('Ctrl Pts',(-7.63471878821226,21.8612943779089,
0.));
#206509=CARTESIAN_POINT('Ctrl Pts',(-7.636388530334,21.8770334769496,0.));
#206510=CARTESIAN_POINT('Ctrl Pts',(-7.63802587492035,21.8929196523514,
0.));
#206511=CARTESIAN_POINT('Ctrl Pts',(-7.63962999860927,21.9089514909874,
0.));
#206512=CARTESIAN_POINT('Ctrl Pts',(-7.64120009506532,21.9251276046546,
0.));
#206513=CARTESIAN_POINT('Ctrl Pts',(-7.64273537442682,21.9414466292072,
0.));
#206514=CARTESIAN_POINT('Ctrl Pts',(-7.64423506279123,21.9579072237651,
0.));
#206515=CARTESIAN_POINT('Ctrl Pts',(-7.64569840177336,21.9745080700798,
0.));
#206516=CARTESIAN_POINT('Ctrl Pts',(-7.6471246480525,21.9912478718542,0.));
#206517=CARTESIAN_POINT('Ctrl Pts',(-7.64851307293352,22.0081253540774,
0.));
#206518=CARTESIAN_POINT('Ctrl Pts',(-7.64986296190168,22.0251392623209,
0.));
#206519=CARTESIAN_POINT('Ctrl Pts',(-7.65117361421358,22.0422883621174,
0.));
#206520=CARTESIAN_POINT('Ctrl Pts',(-7.65244434253113,22.0595714384431,
0.));
#206521=CARTESIAN_POINT('Ctrl Pts',(-7.65367447254949,22.0769872951596,
0.));
#206522=CARTESIAN_POINT('Ctrl Pts',(-7.65486334263644,22.094534754469,0.));
#206523=CARTESIAN_POINT('Ctrl Pts',(-7.65601030346807,22.1122126563329,
0.));
#206524=CARTESIAN_POINT('Ctrl Pts',(-7.65711471769397,22.1300198579675,
0.));
#206525=CARTESIAN_POINT('Ctrl Pts',(-7.65817595963349,22.1479552334211,
0.));
#206526=CARTESIAN_POINT('Ctrl Pts',(-7.6591934149693,22.1660176731178,0.));
#206527=CARTESIAN_POINT('Ctrl Pts',(-7.66016648045005,22.1842060834091,
0.));
#206528=CARTESIAN_POINT('Ctrl Pts',(-7.66109456359271,22.2025193860964,
0.));
#206529=CARTESIAN_POINT('Ctrl Pts',(-7.661977082404,22.2209565180085,0.));
#206530=CARTESIAN_POINT('Ctrl Pts',(-7.66281346512509,22.2395164306547,
0.));
#206531=CARTESIAN_POINT('Ctrl Pts',(-7.66360314997641,22.258198089848,0.));
#206532=CARTESIAN_POINT('Ctrl Pts',(-7.66434558490979,22.2770004753335,
0.));
#206533=CARTESIAN_POINT('Ctrl Pts',(-7.66504022736299,22.2959225803937,
0.));
#206534=CARTESIAN_POINT('Ctrl Pts',(-7.66568654402494,22.314963411484,0.));
#206535=CARTESIAN_POINT('Ctrl Pts',(-7.66628401061952,22.3341219879469,
0.));
#206536=CARTESIAN_POINT('Ctrl Pts',(-7.66683211169158,22.3533973417021,
0.));
#206537=CARTESIAN_POINT('Ctrl Pts',(-7.66733034039883,22.372788516936,0.));
#206538=CARTESIAN_POINT('Ctrl Pts',(-7.6677781983079,22.3922945697773,0.));
#206539=CARTESIAN_POINT('Ctrl Pts',(-7.6681751951964,22.4119145679758,0.));
#206540=CARTESIAN_POINT('Ctrl Pts',(-7.66852084886704,22.4316475906603,
0.));
#206541=CARTESIAN_POINT('Ctrl Pts',(-7.66881468496635,22.4514927280855,
0.));
#206542=CARTESIAN_POINT('Ctrl Pts',(-7.66905623680831,22.47144908137,0.));
#206543=CARTESIAN_POINT('Ctrl Pts',(-7.66924504520315,22.4915157622312,
0.));
#206544=CARTESIAN_POINT('Ctrl Pts',(-7.66938065829108,22.5116918927031,
0.));
#206545=CARTESIAN_POINT('Ctrl Pts',(-7.66946263138144,22.53197660492,0.));
#206546=CARTESIAN_POINT('Ctrl Pts',(-7.66949052679693,22.5523690409116,
0.));
#206547=CARTESIAN_POINT('Ctrl Pts',(-7.66946391372306,22.5728683523831,
0.));
#206548=CARTESIAN_POINT('Ctrl Pts',(-7.66938236806233,22.5934737004953,
0.));
#206549=CARTESIAN_POINT('Ctrl Pts',(-7.66924547229414,22.6141842556243,
0.));
#206550=CARTESIAN_POINT('Ctrl Pts',(-7.66905281533715,22.6349991971541,
0.));
#206551=CARTESIAN_POINT('Ctrl Pts',(-7.66880399241323,22.6559177133127,
0.));
#206552=CARTESIAN_POINT('Ctrl Pts',(-7.66849860491743,22.6769390009885,
0.));
#206553=CARTESIAN_POINT('Ctrl Pts',(-7.66813626029275,22.6980622655446,
0.));
#206554=CARTESIAN_POINT('Ctrl Pts',(-7.66771657191027,22.7192867206245,
0.));
#206555=CARTESIAN_POINT('Ctrl Pts',(-7.6672391589544,22.7406115879513,0.));
#206556=CARTESIAN_POINT('Ctrl Pts',(-7.66670364630299,22.7620360971843,
0.));
#206557=CARTESIAN_POINT('Ctrl Pts',(-7.66610966441273,22.7835594857699,
0.));
#206558=CARTESIAN_POINT('Ctrl Pts',(-7.66545684920987,22.8051809987833,
0.));
#206559=CARTESIAN_POINT('Ctrl Pts',(-7.66474484198549,22.8268998887678,
0.));
#206560=CARTESIAN_POINT('Ctrl Pts',(-7.66397328929803,22.848715415557,0.));
#206561=CARTESIAN_POINT('Ctrl Pts',(-7.66314184287337,22.8706268461283,
0.));
#206562=CARTESIAN_POINT('Ctrl Pts',(-7.66225015950156,22.8926334544883,
0.));
#206563=CARTESIAN_POINT('Ctrl Pts',(-7.66129790094108,22.9147345215421,
0.));
#206564=CARTESIAN_POINT('Ctrl Pts',(-7.66028473382778,22.9369293349593,
0.));
#206565=CARTESIAN_POINT('Ctrl Pts',(-7.65921032958902,22.959217189033,0.));
#206566=CARTESIAN_POINT('Ctrl Pts',(-7.65807436436432,22.9815973845296,
0.));
#206567=CARTESIAN_POINT('Ctrl Pts',(-7.65687651891304,23.0040692285814,
0.));
#206568=CARTESIAN_POINT('Ctrl Pts',(-7.65561647852534,23.0266320345787,
0.));
#206569=CARTESIAN_POINT('Ctrl Pts',(-7.65429393293946,23.0492851220528,
0.));
#206570=CARTESIAN_POINT('Ctrl Pts',(-7.65290857626358,23.072027816555,0.));
#206571=CARTESIAN_POINT('Ctrl Pts',(-7.65146010690476,23.094859449525,0.));
#206572=CARTESIAN_POINT('Ctrl Pts',(-7.6499482274986,23.1177793581679,0.));
#206573=CARTESIAN_POINT('Ctrl Pts',(-7.64837264482943,23.1407868853819,
0.));
#206574=CARTESIAN_POINT('Ctrl Pts',(-7.64673306975805,23.1638813796694,
0.));
#206575=CARTESIAN_POINT('Ctrl Pts',(-7.64502921715483,23.1870621950452,
0.));
#206576=CARTESIAN_POINT('Ctrl Pts',(-7.6432608058368,23.2103286909398,0.));
#206577=CARTESIAN_POINT('Ctrl Pts',(-7.64142755851504,23.2336802320912,
0.));
#206578=CARTESIAN_POINT('Ctrl Pts',(-7.63952920172835,23.2571161884488,
0.));
#206579=CARTESIAN_POINT('Ctrl Pts',(-7.63756546576374,23.2806359350855,
0.));
#206580=CARTESIAN_POINT('Ctrl Pts',(-7.63553608458783,23.3042388521022,
0.));
#206581=CARTESIAN_POINT('Ctrl Pts',(-7.63344079578161,23.3279243245241,
0.));
#206582=CARTESIAN_POINT('Ctrl Pts',(-7.63127934048136,23.3516917421972,
0.));
#206583=CARTESIAN_POINT('Ctrl Pts',(-7.62905146332593,23.3755404996636,
0.));
#206584=CARTESIAN_POINT('Ctrl Pts',(-7.62675691240329,23.399469996112,0.));
#206585=CARTESIAN_POINT('Ctrl Pts',(-7.6243954392005,23.4234796353542,0.));
#206586=CARTESIAN_POINT('Ctrl Pts',(-7.62196679855955,23.4475688257854,
0.));
#206587=CARTESIAN_POINT('Ctrl Pts',(-7.61947074863977,23.4717369803438,
0.));
#206588=CARTESIAN_POINT('Ctrl Pts',(-7.61690705088319,23.4959835164609,
0.));
#206589=CARTESIAN_POINT('Ctrl Pts',(-7.61427546999298,23.5203078560129,
0.));
#206590=CARTESIAN_POINT('Ctrl Pts',(-7.61157577385372,23.544709425203,0.));
#206591=CARTESIAN_POINT('Ctrl Pts',(-7.608807733446,23.5691876544244,0.));
#206592=CARTESIAN_POINT('Ctrl Pts',(-7.60597112277094,23.5937419781245,
0.));
#206593=CARTESIAN_POINT('Ctrl Pts',(-7.60306571877806,23.6183718346576,
0.));
#206594=CARTESIAN_POINT('Ctrl Pts',(-7.60009130130126,23.6430766661418,
0.));
#206595=CARTESIAN_POINT('Ctrl Pts',(-7.59704765299567,23.6678559182875,
0.));
#206596=CARTESIAN_POINT('Ctrl Pts',(-7.59393455934035,23.6927090405066,
0.));
#206597=CARTESIAN_POINT('Ctrl Pts',(-7.5907518086532,23.7176354860456,0.));
#206598=CARTESIAN_POINT('Ctrl Pts',(-7.58749919210826,23.7426347121006,
0.));
#206599=CARTESIAN_POINT('Ctrl Pts',(-7.58417650376271,23.7677061799376,
0.));
#206600=CARTESIAN_POINT('Ctrl Pts',(-7.58078354058213,23.7928493549908,
0.));
#206601=CARTESIAN_POINT('Ctrl Pts',(-7.57732010249066,23.8180637069976,
0.));
#206602=CARTESIAN_POINT('Ctrl Pts',(-7.57378599219814,23.8433487096132,
0.));
#206603=CARTESIAN_POINT('Ctrl Pts',(-7.57018101500709,23.8687038399595,
0.));
#206604=CARTESIAN_POINT('Ctrl Pts',(-7.56650497863791,23.8941285782002,
0.));
#206605=CARTESIAN_POINT('Ctrl Pts',(-7.56275769304773,23.9196224070759,
0.));
#206606=CARTESIAN_POINT('Ctrl Pts',(-7.5589389702768,23.9451848115002,0.));
#206607=CARTESIAN_POINT('Ctrl Pts',(-7.55504862424808,23.9708152779886,
0.));
#206608=CARTESIAN_POINT('Ctrl Pts',(-7.55108647097432,23.9965132953187,
0.));
#206609=CARTESIAN_POINT('Ctrl Pts',(-7.54705232885895,24.0222783554531,
0.));
#206610=CARTESIAN_POINT('Ctrl Pts',(-7.54294601896128,24.0481099543353,
0.));
#206611=CARTESIAN_POINT('Ctrl Pts',(-7.53876736531005,24.0740075927984,
0.));
#206612=CARTESIAN_POINT('Ctrl Pts',(-7.53451619514658,24.0999707772643,
0.));
#206613=CARTESIAN_POINT('Ctrl Pts',(-7.53019233935536,24.1259990209211,
0.));
#206614=CARTESIAN_POINT('Ctrl Pts',(-7.52579563201479,24.152091842537,0.));
#206615=CARTESIAN_POINT('Ctrl Pts',(-7.52132590953862,24.1782487641602,
0.));
#206616=CARTESIAN_POINT('Ctrl Pts',(-7.51678300997998,24.2044693092356,
0.));
#206617=CARTESIAN_POINT('Ctrl Pts',(-7.51216677222199,24.230753000389,0.));
#206618=CARTESIAN_POINT('Ctrl Pts',(-7.50747703535115,24.2570993577032,
0.));
#206619=CARTESIAN_POINT('Ctrl Pts',(-7.50271363765098,24.2835078958966,
0.));
#206620=CARTESIAN_POINT('Ctrl Pts',(-7.49787641695359,24.3099781253345,
0.));
#206621=CARTESIAN_POINT('Ctrl Pts',(-7.4929652125233,24.3365095573673,0.));
#206622=CARTESIAN_POINT('Ctrl Pts',(-7.48797986651828,24.3631017084513,
0.));
#206623=CARTESIAN_POINT('Ctrl Pts',(-7.48292022569254,24.3897541049248,
0.));
#206624=CARTESIAN_POINT('Ctrl Pts',(-7.47778614286573,24.4164662871165,
0.));
#206625=CARTESIAN_POINT('Ctrl Pts',(-7.47257747883319,24.4432378146501,
0.));
#206626=CARTESIAN_POINT('Ctrl Pts',(-7.46729410308923,24.4700682684544,
0.));
#206627=CARTESIAN_POINT('Ctrl Pts',(-7.46193588961642,24.4969572391509,
0.));
#206628=CARTESIAN_POINT('Ctrl Pts',(-7.45650271336045,24.52390431731,0.));
#206629=CARTESIAN_POINT('Ctrl Pts',(-7.45099444651296,24.5509090831579,
0.));
#206630=CARTESIAN_POINT('Ctrl Pts',(-7.44541095473163,24.5779710960865,
0.));
#206631=CARTESIAN_POINT('Ctrl Pts',(-7.43975209375375,24.6050898852349,
0.));
#206632=CARTESIAN_POINT('Ctrl Pts',(-7.4340177048922,24.6322649369472,0.));
#206633=CARTESIAN_POINT('Ctrl Pts',(-7.42820762158681,24.659495712869,0.));
#206634=CARTESIAN_POINT('Ctrl Pts',(-7.42232167765763,24.6867816727118,
0.));
#206635=CARTESIAN_POINT('Ctrl Pts',(-7.41635971481243,24.7141222949988,
0.));
#206636=CARTESIAN_POINT('Ctrl Pts',(-7.41032159082173,24.7415170994754,
0.));
#206637=CARTESIAN_POINT('Ctrl Pts',(-7.40420718661754,24.7689656669005,
0.));
#206638=CARTESIAN_POINT('Ctrl Pts',(-7.39801641583612,24.7964676646518,
0.));
#206639=CARTESIAN_POINT('Ctrl Pts',(-7.39174922586841,24.8240228521042,
0.));
#206640=CARTESIAN_POINT('Ctrl Pts',(-7.38540558904946,24.8516310625367,
0.));
#206641=CARTESIAN_POINT('Ctrl Pts',(-7.3789854964161,24.8792921911309,0.));
#206642=CARTESIAN_POINT('Ctrl Pts',(-7.37378825962718,24.9014633826201,
0.));
#206643=CARTESIAN_POINT('Ctrl Pts',(-7.36985593120696,24.9181155530631,
0.));
#206644=CARTESIAN_POINT('Ctrl Pts',(-7.3672190902906,24.9292275670705,0.));
#206645=CARTESIAN_POINT('Ctrl Pts',(-7.36589684767344,24.9347862158358,
0.));
#206646=CARTESIAN_POINT('',(-7.36589684767344,24.9347862158358,0.));
#206647=CARTESIAN_POINT('Origin',(-1.68110656504246,21.4341755315424,0.));
#206648=CARTESIAN_POINT('',(-1.76341220531179,22.4835757167854,0.));
#206649=CARTESIAN_POINT('',(-1.76341220531179,22.4835757167854,0.));
#206650=CARTESIAN_POINT('',(-0.840553282521227,10.7170877657712,0.));
#206651=CARTESIAN_POINT('Ctrl Pts',(-6.08833931617698,25.2771067246846,
0.));
#206652=CARTESIAN_POINT('Ctrl Pts',(-6.08833931617698,25.2771067246846,
12.));
#206653=CARTESIAN_POINT('Ctrl Pts',(-6.08441489609824,25.2729539149479,
0.));
#206654=CARTESIAN_POINT('Ctrl Pts',(-6.08441489609824,25.2729539149479,
12.));
#206655=CARTESIAN_POINT('Ctrl Pts',(-6.07657531787578,25.2646490489816,
0.));
#206656=CARTESIAN_POINT('Ctrl Pts',(-6.07657531787578,25.2646490489816,
12.));
#206657=CARTESIAN_POINT('Ctrl Pts',(-6.06484373634697,25.2521940105523,
0.));
#206658=CARTESIAN_POINT('Ctrl Pts',(-6.06484373634697,25.2521940105523,
12.));
#206659=CARTESIAN_POINT('Ctrl Pts',(-6.04925720151412,25.2355918138798,
0.));
#206660=CARTESIAN_POINT('Ctrl Pts',(-6.04925720151412,25.2355918138798,
12.));
#206661=CARTESIAN_POINT('Ctrl Pts',(-6.02986667390187,25.2148466201368,
0.));
#206662=CARTESIAN_POINT('Ctrl Pts',(-6.02986667390187,25.2148466201368,
12.));
#206663=CARTESIAN_POINT('Ctrl Pts',(-6.0105688180476,25.1941090269638,0.));
#206664=CARTESIAN_POINT('Ctrl Pts',(-6.0105688180476,25.1941090269638,12.));
#206665=CARTESIAN_POINT('Ctrl Pts',(-5.99136367859838,25.1733791296154,
0.));
#206666=CARTESIAN_POINT('Ctrl Pts',(-5.99136367859838,25.1733791296154,
12.));
#206667=CARTESIAN_POINT('Ctrl Pts',(-5.97225131495636,25.1526570863065,
0.));
#206668=CARTESIAN_POINT('Ctrl Pts',(-5.97225131495636,25.1526570863065,
12.));
#206669=CARTESIAN_POINT('Ctrl Pts',(-5.95323180187348,25.1319431317273,
0.));
#206670=CARTESIAN_POINT('Ctrl Pts',(-5.95323180187348,25.1319431317273,
12.));
#206671=CARTESIAN_POINT('Ctrl Pts',(-5.93430523086776,25.1112375971182,
0.));
#206672=CARTESIAN_POINT('Ctrl Pts',(-5.93430523086776,25.1112375971182,
12.));
#206673=CARTESIAN_POINT('Ctrl Pts',(-5.91547170844382,25.0905409050863,
0.));
#206674=CARTESIAN_POINT('Ctrl Pts',(-5.91547170844382,25.0905409050863,
12.));
#206675=CARTESIAN_POINT('Ctrl Pts',(-5.89673135155459,25.0698535426593,
0.));
#206676=CARTESIAN_POINT('Ctrl Pts',(-5.89673135155459,25.0698535426593,
12.));
#206677=CARTESIAN_POINT('Ctrl Pts',(-5.87808428385329,25.0491760405965,
0.));
#206678=CARTESIAN_POINT('Ctrl Pts',(-5.87808428385329,25.0491760405965,
12.));
#206679=CARTESIAN_POINT('Ctrl Pts',(-5.8595306315681,25.0285089498922,0.));
#206680=CARTESIAN_POINT('Ctrl Pts',(-5.8595306315681,25.0285089498922,12.));
#206681=CARTESIAN_POINT('Ctrl Pts',(-5.84107051963073,25.0078528200558,
0.));
#206682=CARTESIAN_POINT('Ctrl Pts',(-5.84107051963073,25.0078528200558,
12.));
#206683=CARTESIAN_POINT('Ctrl Pts',(-5.82270406744214,24.9872081752709,
0.));
#206684=CARTESIAN_POINT('Ctrl Pts',(-5.82270406744214,24.9872081752709,
12.));
#206685=CARTESIAN_POINT('Ctrl Pts',(-5.80443138549747,24.9665754954462,
0.));
#206686=CARTESIAN_POINT('Ctrl Pts',(-5.80443138549747,24.9665754954462,
12.));
#206687=CARTESIAN_POINT('Ctrl Pts',(-5.78625257775703,24.9459552293308,
0.));
#206688=CARTESIAN_POINT('Ctrl Pts',(-5.78625257775703,24.9459552293308,
12.));
#206689=CARTESIAN_POINT('Ctrl Pts',(-5.76816774342236,24.9253478043632,
0.));
#206690=CARTESIAN_POINT('Ctrl Pts',(-5.76816774342236,24.9253478043632,
12.));
#206691=CARTESIAN_POINT('Ctrl Pts',(-5.75017697890813,24.9047536376467,
0.));
#206692=CARTESIAN_POINT('Ctrl Pts',(-5.75017697890813,24.9047536376467,
12.));
#206693=CARTESIAN_POINT('Ctrl Pts',(-5.73228037976927,24.8841731467219,
0.));
#206694=CARTESIAN_POINT('Ctrl Pts',(-5.73228037976927,24.8841731467219,
12.));
#206695=CARTESIAN_POINT('Ctrl Pts',(-5.71447804252019,24.8636067597677,
0.));
#206696=CARTESIAN_POINT('Ctrl Pts',(-5.71447804252019,24.8636067597677,
12.));
#206697=CARTESIAN_POINT('Ctrl Pts',(-5.69677006679429,24.8430549277634,
0.));
#206698=CARTESIAN_POINT('Ctrl Pts',(-5.69677006679429,24.8430549277634,
12.));
#206699=CARTESIAN_POINT('Ctrl Pts',(-5.67915655496524,24.822518122386,0.));
#206700=CARTESIAN_POINT('Ctrl Pts',(-5.67915655496524,24.822518122386,12.));
#206701=CARTESIAN_POINT('Ctrl Pts',(-5.66163761114903,24.8019968304618,
0.));
#206702=CARTESIAN_POINT('Ctrl Pts',(-5.66163761114903,24.8019968304618,
12.));
#206703=CARTESIAN_POINT('Ctrl Pts',(-5.64421334042248,24.7814915496728,
0.));
#206704=CARTESIAN_POINT('Ctrl Pts',(-5.64421334042248,24.7814915496728,
12.));
#206705=CARTESIAN_POINT('Ctrl Pts',(-5.62688384790919,24.76100278357,0.));
#206706=CARTESIAN_POINT('Ctrl Pts',(-5.62688384790919,24.76100278357,12.));
#206707=CARTESIAN_POINT('Ctrl Pts',(-5.60964923798495,24.7405310372736,
0.));
#206708=CARTESIAN_POINT('Ctrl Pts',(-5.60964923798495,24.7405310372736,
12.));
#206709=CARTESIAN_POINT('Ctrl Pts',(-5.59250961323995,24.7200768119079,
0.));
#206710=CARTESIAN_POINT('Ctrl Pts',(-5.59250961323995,24.7200768119079,
12.));
#206711=CARTESIAN_POINT('Ctrl Pts',(-5.57546507427767,24.6996406035507,
0.));
#206712=CARTESIAN_POINT('Ctrl Pts',(-5.57546507427767,24.6996406035507,
12.));
#206713=CARTESIAN_POINT('Ctrl Pts',(-5.55851572025389,24.6792229061785,
0.));
#206714=CARTESIAN_POINT('Ctrl Pts',(-5.55851572025389,24.6792229061785,
12.));
#206715=CARTESIAN_POINT('Ctrl Pts',(-5.54166164919593,24.6588242134733,
0.));
#206716=CARTESIAN_POINT('Ctrl Pts',(-5.54166164919593,24.6588242134733,
12.));
#206717=CARTESIAN_POINT('Ctrl Pts',(-5.52490295840996,24.6384450211466,
0.));
#206718=CARTESIAN_POINT('Ctrl Pts',(-5.52490295840996,24.6384450211466,
12.));
#206719=CARTESIAN_POINT('Ctrl Pts',(-5.50823974481959,24.618085828918,0.));
#206720=CARTESIAN_POINT('Ctrl Pts',(-5.50823974481959,24.618085828918,12.));
#206721=CARTESIAN_POINT('Ctrl Pts',(-5.49167210537235,24.5977471429365,
0.));
#206722=CARTESIAN_POINT('Ctrl Pts',(-5.49167210537235,24.5977471429365,
12.));
#206723=CARTESIAN_POINT('Ctrl Pts',(-5.47520013724403,24.5774294770329,
0.));
#206724=CARTESIAN_POINT('Ctrl Pts',(-5.47520013724403,24.5774294770329,
12.));
#206725=CARTESIAN_POINT('Ctrl Pts',(-5.45882393762244,24.5571333514841,
0.));
#206726=CARTESIAN_POINT('Ctrl Pts',(-5.45882393762244,24.5571333514841,
12.));
#206727=CARTESIAN_POINT('Ctrl Pts',(-5.44254360356865,24.5368592922861,
0.));
#206728=CARTESIAN_POINT('Ctrl Pts',(-5.44254360356865,24.5368592922861,
12.));
#206729=CARTESIAN_POINT('Ctrl Pts',(-5.42635923183411,24.5166078302107,
0.));
#206730=CARTESIAN_POINT('Ctrl Pts',(-5.42635923183411,24.5166078302107,
12.));
#206731=CARTESIAN_POINT('Ctrl Pts',(-5.41027091869242,24.4963794999831,
0.));
#206732=CARTESIAN_POINT('Ctrl Pts',(-5.41027091869242,24.4963794999831,
12.));
#206733=CARTESIAN_POINT('Ctrl Pts',(-5.3942787597383,24.4761748393322,0.));
#206734=CARTESIAN_POINT('Ctrl Pts',(-5.3942787597383,24.4761748393322,12.));
#206735=CARTESIAN_POINT('Ctrl Pts',(-5.37838284973706,24.4559943883159,
0.));
#206736=CARTESIAN_POINT('Ctrl Pts',(-5.37838284973706,24.4559943883159,
12.));
#206737=CARTESIAN_POINT('Ctrl Pts',(-5.36258328273639,24.4358386899152,
0.));
#206738=CARTESIAN_POINT('Ctrl Pts',(-5.36258328273639,24.4358386899152,
12.));
#206739=CARTESIAN_POINT('Ctrl Pts',(-5.34688015213546,24.4157082904615,
0.));
#206740=CARTESIAN_POINT('Ctrl Pts',(-5.34688015213546,24.4157082904615,
12.));
#206741=CARTESIAN_POINT('Ctrl Pts',(-5.33127355076037,24.3956037401293,
0.));
#206742=CARTESIAN_POINT('Ctrl Pts',(-5.33127355076037,24.3956037401293,
12.));
#206743=CARTESIAN_POINT('Ctrl Pts',(-5.31576357092524,24.3755255933917,
0.));
#206744=CARTESIAN_POINT('Ctrl Pts',(-5.31576357092524,24.3755255933917,
12.));
#206745=CARTESIAN_POINT('Ctrl Pts',(-5.30035030449059,24.3554744095075,
0.));
#206746=CARTESIAN_POINT('Ctrl Pts',(-5.30035030449059,24.3554744095075,
12.));
#206747=CARTESIAN_POINT('Ctrl Pts',(-5.28503384290644,24.3354507529415,
0.));
#206748=CARTESIAN_POINT('Ctrl Pts',(-5.28503384290644,24.3354507529415,
12.));
#206749=CARTESIAN_POINT('Ctrl Pts',(-5.26981427718796,24.3154551932222,
0.));
#206750=CARTESIAN_POINT('Ctrl Pts',(-5.26981427718796,24.3154551932222,
12.));
#206751=CARTESIAN_POINT('Ctrl Pts',(-5.25469169788856,24.2954883048448,
0.));
#206752=CARTESIAN_POINT('Ctrl Pts',(-5.25469169788856,24.2954883048448,
12.));
#206753=CARTESIAN_POINT('Ctrl Pts',(-5.23966619506289,24.2755506671526,
0.));
#206754=CARTESIAN_POINT('Ctrl Pts',(-5.23966619506289,24.2755506671526,
12.));
#206755=CARTESIAN_POINT('Ctrl Pts',(-5.22473785822441,24.2556428642294,
0.));
#206756=CARTESIAN_POINT('Ctrl Pts',(-5.22473785822441,24.2556428642294,
12.));
#206757=CARTESIAN_POINT('Ctrl Pts',(-5.20990677629173,24.2357654847765,
0.));
#206758=CARTESIAN_POINT('Ctrl Pts',(-5.20990677629173,24.2357654847765,
12.));
#206759=CARTESIAN_POINT('Ctrl Pts',(-5.19517303753643,24.215919122017,0.));
#206760=CARTESIAN_POINT('Ctrl Pts',(-5.19517303753643,24.215919122017,12.));
#206761=CARTESIAN_POINT('Ctrl Pts',(-5.18053672961392,24.1961043738754,
0.));
#206762=CARTESIAN_POINT('Ctrl Pts',(-5.18053672961392,24.1961043738754,
12.));
#206763=CARTESIAN_POINT('Ctrl Pts',(-5.16599793957979,24.1763218431343,
0.));
#206764=CARTESIAN_POINT('Ctrl Pts',(-5.16599793957979,24.1763218431343,
12.));
#206765=CARTESIAN_POINT('Ctrl Pts',(-5.15155675390075,24.156572137597,0.));
#206766=CARTESIAN_POINT('Ctrl Pts',(-5.15155675390075,24.156572137597,12.));
#206767=CARTESIAN_POINT('Ctrl Pts',(-5.13721325845745,24.1368558702443,
0.));
#206768=CARTESIAN_POINT('Ctrl Pts',(-5.13721325845745,24.1368558702443,
12.));
#206769=CARTESIAN_POINT('Ctrl Pts',(-5.12296753853859,24.117173659394,0.));
#206770=CARTESIAN_POINT('Ctrl Pts',(-5.12296753853859,24.117173659394,12.));
#206771=CARTESIAN_POINT('Ctrl Pts',(-5.10881967883132,24.0975261288446,
0.));
#206772=CARTESIAN_POINT('Ctrl Pts',(-5.10881967883132,24.0975261288446,
12.));
#206773=CARTESIAN_POINT('Ctrl Pts',(-5.09476976342625,24.0779139079266,
0.));
#206774=CARTESIAN_POINT('Ctrl Pts',(-5.09476976342625,24.0779139079266,
12.));
#206775=CARTESIAN_POINT('Ctrl Pts',(-5.08081787581276,24.0583376315638,
0.));
#206776=CARTESIAN_POINT('Ctrl Pts',(-5.08081787581276,24.0583376315638,
12.));
#206777=CARTESIAN_POINT('Ctrl Pts',(-5.06696409886641,24.0387979403268,
0.));
#206778=CARTESIAN_POINT('Ctrl Pts',(-5.06696409886641,24.0387979403268,
12.));
#206779=CARTESIAN_POINT('Ctrl Pts',(-5.05320851483065,24.0192954804896,
0.));
#206780=CARTESIAN_POINT('Ctrl Pts',(-5.05320851483065,24.0192954804896,
12.));
#206781=CARTESIAN_POINT('Ctrl Pts',(-5.03955120528521,23.9998309040746,
0.));
#206782=CARTESIAN_POINT('Ctrl Pts',(-5.03955120528521,23.9998309040746,
12.));
#206783=CARTESIAN_POINT('Ctrl Pts',(-5.02599225112454,23.9804048689227,
0.));
#206784=CARTESIAN_POINT('Ctrl Pts',(-5.02599225112454,23.9804048689227,
12.));
#206785=CARTESIAN_POINT('Ctrl Pts',(-5.01253173257453,23.9610180388271,
0.));
#206786=CARTESIAN_POINT('Ctrl Pts',(-5.01253173257453,23.9610180388271,
12.));
#206787=CARTESIAN_POINT('Ctrl Pts',(-4.99916972919307,23.9416710836529,
0.));
#206788=CARTESIAN_POINT('Ctrl Pts',(-4.99916972919307,23.9416710836529,
12.));
#206789=CARTESIAN_POINT('Ctrl Pts',(-4.98590631986533,23.9223646794592,
0.));
#206790=CARTESIAN_POINT('Ctrl Pts',(-4.98590631986533,23.9223646794592,
12.));
#206791=CARTESIAN_POINT('Ctrl Pts',(-4.97274158279227,23.9030995086163,
0.));
#206792=CARTESIAN_POINT('Ctrl Pts',(-4.97274158279227,23.9030995086163,
12.));
#206793=CARTESIAN_POINT('Ctrl Pts',(-4.95967559546561,23.8838762599218,
0.));
#206794=CARTESIAN_POINT('Ctrl Pts',(-4.95967559546561,23.8838762599218,
12.));
#206795=CARTESIAN_POINT('Ctrl Pts',(-4.9467084346586,23.8646956287168,0.));
#206796=CARTESIAN_POINT('Ctrl Pts',(-4.9467084346586,23.8646956287168,12.));
#206797=CARTESIAN_POINT('Ctrl Pts',(-4.93384017643432,23.8455583170057,
0.));
#206798=CARTESIAN_POINT('Ctrl Pts',(-4.93384017643432,23.8455583170057,
12.));
#206799=CARTESIAN_POINT('Ctrl Pts',(-4.92107089613969,23.8264650335717,
0.));
#206800=CARTESIAN_POINT('Ctrl Pts',(-4.92107089613969,23.8264650335717,
12.));
#206801=CARTESIAN_POINT('Ctrl Pts',(-4.90840066839344,23.8074164940896,
0.));
#206802=CARTESIAN_POINT('Ctrl Pts',(-4.90840066839344,23.8074164940896,
12.));
#206803=CARTESIAN_POINT('Ctrl Pts',(-4.89582956706775,23.7884134212384,
0.));
#206804=CARTESIAN_POINT('Ctrl Pts',(-4.89582956706775,23.7884134212384,
12.));
#206805=CARTESIAN_POINT('Ctrl Pts',(-4.88335766525573,23.7694565448049,
0.));
#206806=CARTESIAN_POINT('Ctrl Pts',(-4.88335766525573,23.7694565448049,
12.));
#206807=CARTESIAN_POINT('Ctrl Pts',(-4.87098503527152,23.7505466018245,
0.));
#206808=CARTESIAN_POINT('Ctrl Pts',(-4.87098503527152,23.7505466018245,
12.));
#206809=CARTESIAN_POINT('Ctrl Pts',(-4.85871174865499,23.7316843367313,
0.));
#206810=CARTESIAN_POINT('Ctrl Pts',(-4.85871174865499,23.7316843367313,
12.));
#206811=CARTESIAN_POINT('Ctrl Pts',(-4.84653787616425,23.7128705015017,
0.));
#206812=CARTESIAN_POINT('Ctrl Pts',(-4.84653787616425,23.7128705015017,
12.));
#206813=CARTESIAN_POINT('Ctrl Pts',(-4.83446348776266,23.6941058557971,
0.));
#206814=CARTESIAN_POINT('Ctrl Pts',(-4.83446348776266,23.6941058557971,
12.));
#206815=CARTESIAN_POINT('Ctrl Pts',(-4.82248865259562,23.675391167102,0.));
#206816=CARTESIAN_POINT('Ctrl Pts',(-4.82248865259562,23.675391167102,12.));
#206817=CARTESIAN_POINT('Ctrl Pts',(-4.81061343896432,23.6567272108628,
0.));
#206818=CARTESIAN_POINT('Ctrl Pts',(-4.81061343896432,23.6567272108628,
12.));
#206819=CARTESIAN_POINT('Ctrl Pts',(-4.7988379143322,23.6381147706579,0.));
#206820=CARTESIAN_POINT('Ctrl Pts',(-4.7988379143322,23.6381147706579,12.));
#206821=CARTESIAN_POINT('Ctrl Pts',(-4.78716214532098,23.6195546383624,
0.));
#206822=CARTESIAN_POINT('Ctrl Pts',(-4.78716214532098,23.6195546383624,
12.));
#206823=CARTESIAN_POINT('Ctrl Pts',(-4.77558619769872,23.6010476143099,
0.));
#206824=CARTESIAN_POINT('Ctrl Pts',(-4.77558619769872,23.6010476143099,
12.));
#206825=CARTESIAN_POINT('Ctrl Pts',(-4.76411013636251,23.5825945074535,
0.));
#206826=CARTESIAN_POINT('Ctrl Pts',(-4.76411013636251,23.5825945074535,
12.));
#206827=CARTESIAN_POINT('Ctrl Pts',(-4.75273402530617,23.5641961355168,
0.));
#206828=CARTESIAN_POINT('Ctrl Pts',(-4.75273402530617,23.5641961355168,
12.));
#206829=CARTESIAN_POINT('Ctrl Pts',(-4.74145792760698,23.545853325171,0.));
#206830=CARTESIAN_POINT('Ctrl Pts',(-4.74145792760698,23.545853325171,12.));
#206831=CARTESIAN_POINT('Ctrl Pts',(-4.7302819054303,23.5275669122372,0.));
#206832=CARTESIAN_POINT('Ctrl Pts',(-4.7302819054303,23.5275669122372,12.));
#206833=CARTESIAN_POINT('Ctrl Pts',(-4.71920602001902,23.509337741878,0.));
#206834=CARTESIAN_POINT('Ctrl Pts',(-4.71920602001902,23.509337741878,12.));
#206835=CARTESIAN_POINT('Ctrl Pts',(-4.70823033167819,23.491166668789,0.));
#206836=CARTESIAN_POINT('Ctrl Pts',(-4.70823033167819,23.491166668789,12.));
#206837=CARTESIAN_POINT('Ctrl Pts',(-4.69735489975024,23.4730545573853,
0.));
#206838=CARTESIAN_POINT('Ctrl Pts',(-4.69735489975024,23.4730545573853,
12.));
#206839=CARTESIAN_POINT('Ctrl Pts',(-4.68657978258303,23.455002281986,0.));
#206840=CARTESIAN_POINT('Ctrl Pts',(-4.68657978258303,23.455002281986,12.));
#206841=CARTESIAN_POINT('Ctrl Pts',(-4.67590503753058,23.4370107270451,
0.));
#206842=CARTESIAN_POINT('Ctrl Pts',(-4.67590503753058,23.4370107270451,
12.));
#206843=CARTESIAN_POINT('Ctrl Pts',(-4.6653307209467,23.4190807873803,0.));
#206844=CARTESIAN_POINT('Ctrl Pts',(-4.6653307209467,23.4190807873803,12.));
#206845=CARTESIAN_POINT('Ctrl Pts',(-4.65485688816924,23.4012133683959,
0.));
#206846=CARTESIAN_POINT('Ctrl Pts',(-4.65485688816924,23.4012133683959,
12.));
#206847=CARTESIAN_POINT('Ctrl Pts',(-4.6444835934993,23.3834093863068,0.));
#206848=CARTESIAN_POINT('Ctrl Pts',(-4.6444835934993,23.3834093863068,12.));
#206849=CARTESIAN_POINT('Ctrl Pts',(-4.63421089016541,23.3656697683489,
0.));
#206850=CARTESIAN_POINT('Ctrl Pts',(-4.63421089016541,23.3656697683489,
12.));
#206851=CARTESIAN_POINT('Ctrl Pts',(-4.62403883030805,23.3479954530272,
0.));
#206852=CARTESIAN_POINT('Ctrl Pts',(-4.62403883030805,23.3479954530272,
12.));
#206853=CARTESIAN_POINT('Ctrl Pts',(-4.6139674649783,23.3303873903938,0.));
#206854=CARTESIAN_POINT('Ctrl Pts',(-4.6139674649783,23.3303873903938,12.));
#206855=CARTESIAN_POINT('Ctrl Pts',(-4.60399684412163,23.3128465423115,
0.));
#206856=CARTESIAN_POINT('Ctrl Pts',(-4.60399684412163,23.3128465423115,
12.));
#206857=CARTESIAN_POINT('Ctrl Pts',(-4.5941270165575,23.2953738827191,0.));
#206858=CARTESIAN_POINT('Ctrl Pts',(-4.5941270165575,23.2953738827191,12.));
#206859=CARTESIAN_POINT('Ctrl Pts',(-4.5843580299469,23.2779703978876,0.));
#206860=CARTESIAN_POINT('Ctrl Pts',(-4.5843580299469,23.2779703978876,12.));
#206861=CARTESIAN_POINT('Ctrl Pts',(-4.57468993076097,23.2606370866866,
0.));
#206862=CARTESIAN_POINT('Ctrl Pts',(-4.57468993076097,23.2606370866866,
12.));
#206863=CARTESIAN_POINT('Ctrl Pts',(-4.56512276427839,23.2433749609131,
0.));
#206864=CARTESIAN_POINT('Ctrl Pts',(-4.56512276427839,23.2433749609131,
12.));
#206865=CARTESIAN_POINT('Ctrl Pts',(-4.55565657456975,23.2261850456064,
0.));
#206866=CARTESIAN_POINT('Ctrl Pts',(-4.55565657456975,23.2261850456064,
12.));
#206867=CARTESIAN_POINT('Ctrl Pts',(-4.54629140447544,23.2090683793629,
0.));
#206868=CARTESIAN_POINT('Ctrl Pts',(-4.54629140447544,23.2090683793629,
12.));
#206869=CARTESIAN_POINT('Ctrl Pts',(-4.53702729557566,23.1920260146465,
0.));
#206870=CARTESIAN_POINT('Ctrl Pts',(-4.53702729557566,23.1920260146465,
12.));
#206871=CARTESIAN_POINT('Ctrl Pts',(-4.52786428815015,23.1750590180908,
0.));
#206872=CARTESIAN_POINT('Ctrl Pts',(-4.52786428815015,23.1750590180908,
12.));
#206873=CARTESIAN_POINT('Ctrl Pts',(-4.51880242116748,23.1581684708761,
0.));
#206874=CARTESIAN_POINT('Ctrl Pts',(-4.51880242116748,23.1581684708761,
12.));
#206875=CARTESIAN_POINT('Ctrl Pts',(-4.5098417322706,23.1413554691123,0.));
#206876=CARTESIAN_POINT('Ctrl Pts',(-4.5098417322706,23.1413554691123,12.));
#206877=CARTESIAN_POINT('Ctrl Pts',(-4.50098225775171,23.1246211242115,
0.));
#206878=CARTESIAN_POINT('Ctrl Pts',(-4.50098225775171,23.1246211242115,
12.));
#206879=CARTESIAN_POINT('Ctrl Pts',(-4.49222403252216,23.1079665632636,
0.));
#206880=CARTESIAN_POINT('Ctrl Pts',(-4.49222403252216,23.1079665632636,
12.));
#206881=CARTESIAN_POINT('Ctrl Pts',(-4.48356709006788,23.0913929293922,
0.));
#206882=CARTESIAN_POINT('Ctrl Pts',(-4.48356709006788,23.0913929293922,
12.));
#206883=CARTESIAN_POINT('Ctrl Pts',(-4.47501146242856,23.0749013821881,
0.));
#206884=CARTESIAN_POINT('Ctrl Pts',(-4.47501146242856,23.0749013821881,
12.));
#206885=CARTESIAN_POINT('Ctrl Pts',(-4.4665571801823,23.0584930981732,0.));
#206886=CARTESIAN_POINT('Ctrl Pts',(-4.4665571801823,23.0584930981732,12.));
#206887=CARTESIAN_POINT('Ctrl Pts',(-4.45820427241683,23.0421692712467,
0.));
#206888=CARTESIAN_POINT('Ctrl Pts',(-4.45820427241683,23.0421692712467,
12.));
#206889=CARTESIAN_POINT('Ctrl Pts',(-4.44995276669686,23.0259311131392,
0.));
#206890=CARTESIAN_POINT('Ctrl Pts',(-4.44995276669686,23.0259311131392,
12.));
#206891=CARTESIAN_POINT('Ctrl Pts',(-4.44180268901643,23.0097798538395,
0.));
#206892=CARTESIAN_POINT('Ctrl Pts',(-4.44180268901643,23.0097798538395,
12.));
#206893=CARTESIAN_POINT('Ctrl Pts',(-4.43375406376879,22.9937167421006,
0.));
#206894=CARTESIAN_POINT('Ctrl Pts',(-4.43375406376879,22.9937167421006,
12.));
#206895=CARTESIAN_POINT('Ctrl Pts',(-4.42580691372751,22.977743046002,0.));
#206896=CARTESIAN_POINT('Ctrl Pts',(-4.42580691372751,22.977743046002,12.));
#206897=CARTESIAN_POINT('Ctrl Pts',(-4.41796126001302,22.9618600534866,
0.));
#206898=CARTESIAN_POINT('Ctrl Pts',(-4.41796126001302,22.9618600534866,
12.));
#206899=CARTESIAN_POINT('Ctrl Pts',(-4.41021712205553,22.9460690729093,
0.));
#206900=CARTESIAN_POINT('Ctrl Pts',(-4.41021712205553,22.9460690729093,
12.));
#206901=CARTESIAN_POINT('Ctrl Pts',(-4.40257451754323,22.930371433555,0.));
#206902=CARTESIAN_POINT('Ctrl Pts',(-4.40257451754323,22.930371433555,12.));
#206903=CARTESIAN_POINT('Ctrl Pts',(-4.39503346238473,22.9147684862426,
0.));
#206904=CARTESIAN_POINT('Ctrl Pts',(-4.39503346238473,22.9147684862426,
12.));
#206905=CARTESIAN_POINT('Ctrl Pts',(-4.38759397068406,22.8992616040108,
0.));
#206906=CARTESIAN_POINT('Ctrl Pts',(-4.38759397068406,22.8992616040108,
12.));
#206907=CARTESIAN_POINT('Ctrl Pts',(-4.38025605470093,22.8838521827701,
0.));
#206908=CARTESIAN_POINT('Ctrl Pts',(-4.38025605470093,22.8838521827701,
12.));
#206909=CARTESIAN_POINT('Ctrl Pts',(-4.37301972480746,22.8685416419725,
0.));
#206910=CARTESIAN_POINT('Ctrl Pts',(-4.37301972480746,22.8685416419725,
12.));
#206911=CARTESIAN_POINT('Ctrl Pts',(-4.36588498942997,22.8533314252422,
0.));
#206912=CARTESIAN_POINT('Ctrl Pts',(-4.36588498942997,22.8533314252422,
12.));
#206913=CARTESIAN_POINT('Ctrl Pts',(-4.35885185500546,22.8382230011184,
0.));
#206914=CARTESIAN_POINT('Ctrl Pts',(-4.35885185500546,22.8382230011184,
12.));
#206915=CARTESIAN_POINT('Ctrl Pts',(-4.35192032594791,22.8232178638876,
0.));
#206916=CARTESIAN_POINT('Ctrl Pts',(-4.35192032594791,22.8232178638876,
12.));
#206917=CARTESIAN_POINT('Ctrl Pts',(-4.34509040460062,22.8083175343791,
0.));
#206918=CARTESIAN_POINT('Ctrl Pts',(-4.34509040460062,22.8083175343791,
12.));
#206919=CARTESIAN_POINT('Ctrl Pts',(-4.33836209118446,22.7935235607806,
0.));
#206920=CARTESIAN_POINT('Ctrl Pts',(-4.33836209118446,22.7935235607806,
12.));
#206921=CARTESIAN_POINT('Ctrl Pts',(-4.3317353837319,22.7788375194076,0.));
#206922=CARTESIAN_POINT('Ctrl Pts',(-4.3317353837319,22.7788375194076,12.));
#206923=CARTESIAN_POINT('Ctrl Pts',(-4.32521027803754,22.7642610156475,
0.));
#206924=CARTESIAN_POINT('Ctrl Pts',(-4.32521027803754,22.7642610156475,
12.));
#206925=CARTESIAN_POINT('Ctrl Pts',(-4.31878676761235,22.7497956849848,
0.));
#206926=CARTESIAN_POINT('Ctrl Pts',(-4.31878676761235,22.7497956849848,
12.));
#206927=CARTESIAN_POINT('Ctrl Pts',(-4.31246484362549,22.7354431939926,
0.));
#206928=CARTESIAN_POINT('Ctrl Pts',(-4.31246484362549,22.7354431939926,
12.));
#206929=CARTESIAN_POINT('Ctrl Pts',(-4.30624449484069,22.7212052413386,
0.));
#206930=CARTESIAN_POINT('Ctrl Pts',(-4.30624449484069,22.7212052413386,
12.));
#206931=CARTESIAN_POINT('Ctrl Pts',(-4.3001257075406,22.7070835587564,0.));
#206932=CARTESIAN_POINT('Ctrl Pts',(-4.3001257075406,22.7070835587564,12.));
#206933=CARTESIAN_POINT('Ctrl Pts',(-4.29410846547056,22.6930799122548,
0.));
#206934=CARTESIAN_POINT('Ctrl Pts',(-4.29410846547056,22.6930799122548,
12.));
#206935=CARTESIAN_POINT('Ctrl Pts',(-4.28819274977763,22.6791961033538,
0.));
#206936=CARTESIAN_POINT('Ctrl Pts',(-4.28819274977763,22.6791961033538,
12.));
#206937=CARTESIAN_POINT('Ctrl Pts',(-4.28237853894059,22.6654339703109,
0.));
#206938=CARTESIAN_POINT('Ctrl Pts',(-4.28237853894059,22.6654339703109,
12.));
#206939=CARTESIAN_POINT('Ctrl Pts',(-4.2766658086912,22.6517953893303,0.));
#206940=CARTESIAN_POINT('Ctrl Pts',(-4.2766658086912,22.6517953893303,12.));
#206941=CARTESIAN_POINT('Ctrl Pts',(-4.27105453193004,22.6382822758172,
0.));
#206942=CARTESIAN_POINT('Ctrl Pts',(-4.27105453193004,22.6382822758172,
12.));
#206943=CARTESIAN_POINT('Ctrl Pts',(-4.26554467865576,22.6248965859977,
0.));
#206944=CARTESIAN_POINT('Ctrl Pts',(-4.26554467865576,22.6248965859977,
12.));
#206945=CARTESIAN_POINT('Ctrl Pts',(-4.26013621588305,22.6116403184821,
0.));
#206946=CARTESIAN_POINT('Ctrl Pts',(-4.26013621588305,22.6116403184821,
12.));
#206947=CARTESIAN_POINT('Ctrl Pts',(-4.25482910755481,22.5985155158636,
0.));
#206948=CARTESIAN_POINT('Ctrl Pts',(-4.25482910755481,22.5985155158636,
12.));
#206949=CARTESIAN_POINT('Ctrl Pts',(-4.24962331444177,22.5855242662477,
0.));
#206950=CARTESIAN_POINT('Ctrl Pts',(-4.24962331444177,22.5855242662477,
12.));
#206951=CARTESIAN_POINT('Ctrl Pts',(-4.24451879404851,22.572668704992,0.));
#206952=CARTESIAN_POINT('Ctrl Pts',(-4.24451879404851,22.572668704992,12.));
#206953=CARTESIAN_POINT('Ctrl Pts',(-4.23951550052523,22.5599510166429,
0.));
#206954=CARTESIAN_POINT('Ctrl Pts',(-4.23951550052523,22.5599510166429,
12.));
#206955=CARTESIAN_POINT('Ctrl Pts',(-4.23461338456712,22.5473734368086,
0.));
#206956=CARTESIAN_POINT('Ctrl Pts',(-4.23461338456712,22.5473734368086,
12.));
#206957=CARTESIAN_POINT('Ctrl Pts',(-4.22981239330733,22.5349382540588,
0.));
#206958=CARTESIAN_POINT('Ctrl Pts',(-4.22981239330733,22.5349382540588,
12.));
#206959=CARTESIAN_POINT('Ctrl Pts',(-4.22511247020041,22.5226478117886,
0.));
#206960=CARTESIAN_POINT('Ctrl Pts',(-4.22511247020041,22.5226478117886,
12.));
#206961=CARTESIAN_POINT('Ctrl Pts',(-4.22051355490196,22.5105045108881,
0.));
#206962=CARTESIAN_POINT('Ctrl Pts',(-4.22051355490196,22.5105045108881,
12.));
#206963=CARTESIAN_POINT('Ctrl Pts',(-4.21601558313906,22.4985108124228,
0.));
#206964=CARTESIAN_POINT('Ctrl Pts',(-4.21601558313906,22.4985108124228,
12.));
#206965=CARTESIAN_POINT('Ctrl Pts',(-4.21161848657428,22.4866692403147,
0.));
#206966=CARTESIAN_POINT('Ctrl Pts',(-4.21161848657428,22.4866692403147,
12.));
#206967=CARTESIAN_POINT('Ctrl Pts',(-4.20732219265649,22.4749823839917,
0.));
#206968=CARTESIAN_POINT('Ctrl Pts',(-4.20732219265649,22.4749823839917,
12.));
#206969=CARTESIAN_POINT('Ctrl Pts',(-4.20312662448174,22.4634529011437,
0.));
#206970=CARTESIAN_POINT('Ctrl Pts',(-4.20312662448174,22.4634529011437,
12.));
#206971=CARTESIAN_POINT('Ctrl Pts',(-4.19903170066358,22.4520835205422,
0.));
#206972=CARTESIAN_POINT('Ctrl Pts',(-4.19903170066358,22.4520835205422,
12.));
#206973=CARTESIAN_POINT('Ctrl Pts',(-4.1950373351886,22.4408770448917,0.));
#206974=CARTESIAN_POINT('Ctrl Pts',(-4.1950373351886,22.4408770448917,12.));
#206975=CARTESIAN_POINT('Ctrl Pts',(-4.19114343726932,22.4298363535416,
0.));
#206976=CARTESIAN_POINT('Ctrl Pts',(-4.19114343726932,22.4298363535416,
12.));
#206977=CARTESIAN_POINT('Ctrl Pts',(-4.18734991117707,22.4189644056109,
0.));
#206978=CARTESIAN_POINT('Ctrl Pts',(-4.18734991117707,22.4189644056109,
12.));
#206979=CARTESIAN_POINT('Ctrl Pts',(-4.18365665600839,22.4082642454448,
0.));
#206980=CARTESIAN_POINT('Ctrl Pts',(-4.18365665600839,22.4082642454448,
12.));
#206981=CARTESIAN_POINT('Ctrl Pts',(-4.18006356544879,22.3977390078074,
0.));
#206982=CARTESIAN_POINT('Ctrl Pts',(-4.18006356544879,22.3977390078074,
12.));
#206983=CARTESIAN_POINT('Ctrl Pts',(-4.17657052752834,22.3873919231339,
0.));
#206984=CARTESIAN_POINT('Ctrl Pts',(-4.17657052752834,22.3873919231339,
12.));
#206985=CARTESIAN_POINT('Ctrl Pts',(-4.17317742436162,22.3772263228624,
0.));
#206986=CARTESIAN_POINT('Ctrl Pts',(-4.17317742436162,22.3772263228624,
12.));
#206987=CARTESIAN_POINT('Ctrl Pts',(-4.1698841319947,22.3672456427605,0.));
#206988=CARTESIAN_POINT('Ctrl Pts',(-4.1698841319947,22.3672456427605,12.));
#206989=CARTESIAN_POINT('Ctrl Pts',(-4.16669052026602,22.3574534257397,
0.));
#206990=CARTESIAN_POINT('Ctrl Pts',(-4.16669052026602,22.3574534257397,
12.));
#206991=CARTESIAN_POINT('Ctrl Pts',(-4.1635964526318,22.3478533253886,0.));
#206992=CARTESIAN_POINT('Ctrl Pts',(-4.1635964526318,22.3478533253886,12.));
#206993=CARTESIAN_POINT('Ctrl Pts',(-4.16060178604154,22.3384491078599,
0.));
#206994=CARTESIAN_POINT('Ctrl Pts',(-4.16060178604154,22.3384491078599,
12.));
#206995=CARTESIAN_POINT('Ctrl Pts',(-4.15770637047882,22.3292446628957,
0.));
#206996=CARTESIAN_POINT('Ctrl Pts',(-4.15770637047882,22.3292446628957,
12.));
#206997=CARTESIAN_POINT('Ctrl Pts',(-4.15491004835278,22.3202440186979,
0.));
#206998=CARTESIAN_POINT('Ctrl Pts',(-4.15491004835278,22.3202440186979,
12.));
#206999=CARTESIAN_POINT('Ctrl Pts',(-4.15221265396992,22.3114513545186,
0.));
#207000=CARTESIAN_POINT('Ctrl Pts',(-4.15221265396992,22.3114513545186,
12.));
#207001=CARTESIAN_POINT('Ctrl Pts',(-4.14961401285526,22.3028710166935,
0.));
#207002=CARTESIAN_POINT('Ctrl Pts',(-4.14961401285526,22.3028710166935,
12.));
#207003=CARTESIAN_POINT('Ctrl Pts',(-4.14711394168559,22.2945075198468,
0.));
#207004=CARTESIAN_POINT('Ctrl Pts',(-4.14711394168559,22.2945075198468,
12.));
#207005=CARTESIAN_POINT('Ctrl Pts',(-4.14471224859295,22.2863655389166,
0.));
#207006=CARTESIAN_POINT('Ctrl Pts',(-4.14471224859295,22.2863655389166,
12.));
#207007=CARTESIAN_POINT('Ctrl Pts',(-4.14240873321982,22.2784499072026,
0.));
#207008=CARTESIAN_POINT('Ctrl Pts',(-4.14240873321982,22.2784499072026,
12.));
#207009=CARTESIAN_POINT('Ctrl Pts',(-4.14020318715988,22.2707656042456,
0.));
#207010=CARTESIAN_POINT('Ctrl Pts',(-4.14020318715988,22.2707656042456,
12.));
#207011=CARTESIAN_POINT('Ctrl Pts',(-4.13809539255419,22.263317791397,0.));
#207012=CARTESIAN_POINT('Ctrl Pts',(-4.13809539255419,22.263317791397,12.));
#207013=CARTESIAN_POINT('Ctrl Pts',(-4.13608511977226,22.2561118708422,
0.));
#207014=CARTESIAN_POINT('Ctrl Pts',(-4.13608511977226,22.2561118708422,
12.));
#207015=CARTESIAN_POINT('Ctrl Pts',(-4.13417212558808,22.2491535317789,
0.));
#207016=CARTESIAN_POINT('Ctrl Pts',(-4.13417212558808,22.2491535317789,
12.));
#207017=CARTESIAN_POINT('Ctrl Pts',(-4.1323561506016,22.2424488153523,0.));
#207018=CARTESIAN_POINT('Ctrl Pts',(-4.1323561506016,22.2424488153523,12.));
#207019=CARTESIAN_POINT('Ctrl Pts',(-4.13063692157499,22.2360040565534,
0.));
#207020=CARTESIAN_POINT('Ctrl Pts',(-4.13063692157499,22.2360040565534,
12.));
#207021=CARTESIAN_POINT('Ctrl Pts',(-4.12901415463379,22.2298258043947,
0.));
#207022=CARTESIAN_POINT('Ctrl Pts',(-4.12901415463379,22.2298258043947,
12.));
#207023=CARTESIAN_POINT('Ctrl Pts',(-4.12748755830099,22.2239207458781,
0.));
#207024=CARTESIAN_POINT('Ctrl Pts',(-4.12748755830099,22.2239207458781,
12.));
#207025=CARTESIAN_POINT('Ctrl Pts',(-4.126056836133,22.2182956401341,0.));
#207026=CARTESIAN_POINT('Ctrl Pts',(-4.126056836133,22.2182956401341,12.));
#207027=CARTESIAN_POINT('Ctrl Pts',(-4.12472167516602,22.2129576146671,
0.));
#207028=CARTESIAN_POINT('Ctrl Pts',(-4.12472167516602,22.2129576146671,
12.));
#207029=CARTESIAN_POINT('Ctrl Pts',(-4.12348173702025,22.2079143941719,
0.));
#207030=CARTESIAN_POINT('Ctrl Pts',(-4.12348173702025,22.2079143941719,
12.));
#207031=CARTESIAN_POINT('Ctrl Pts',(-4.12233664408237,22.2031746532106,
0.));
#207032=CARTESIAN_POINT('Ctrl Pts',(-4.12233664408237,22.2031746532106,
12.));
#207033=CARTESIAN_POINT('Ctrl Pts',(-4.12128598183533,22.1987479618246,
0.));
#207034=CARTESIAN_POINT('Ctrl Pts',(-4.12128598183533,22.1987479618246,
12.));
#207035=CARTESIAN_POINT('Ctrl Pts',(-4.12032932637738,22.1946440958098,
0.));
#207036=CARTESIAN_POINT('Ctrl Pts',(-4.12032932637738,22.1946440958098,
12.));
#207037=CARTESIAN_POINT('Ctrl Pts',(-4.11946626228623,22.1908725908525,
0.));
#207038=CARTESIAN_POINT('Ctrl Pts',(-4.11946626228623,22.1908725908525,
12.));
#207039=CARTESIAN_POINT('Ctrl Pts',(-4.11869641271752,22.1874419861496,
0.));
#207040=CARTESIAN_POINT('Ctrl Pts',(-4.11869641271752,22.1874419861496,
12.));
#207041=CARTESIAN_POINT('Ctrl Pts',(-4.11801938107464,22.1843613164855,
0.));
#207042=CARTESIAN_POINT('Ctrl Pts',(-4.11801938107464,22.1843613164855,
12.));
#207043=CARTESIAN_POINT('Ctrl Pts',(-4.11743469691765,22.1816414985788,
0.));
#207044=CARTESIAN_POINT('Ctrl Pts',(-4.11743469691765,22.1816414985788,
12.));
#207045=CARTESIAN_POINT('Ctrl Pts',(-4.11694173195041,22.179297473024,0.));
#207046=CARTESIAN_POINT('Ctrl Pts',(-4.11694173195041,22.179297473024,12.));
#207047=CARTESIAN_POINT('Ctrl Pts',(-4.11653973150558,22.177347426894,0.));
#207048=CARTESIAN_POINT('Ctrl Pts',(-4.11653973150558,22.177347426894,12.));
#207049=CARTESIAN_POINT('Ctrl Pts',(-4.11622797217066,22.1758088296598,
0.));
#207050=CARTESIAN_POINT('Ctrl Pts',(-4.11622797217066,22.1758088296598,
12.));
#207051=CARTESIAN_POINT('Ctrl Pts',(-4.11600589882767,22.1746949858773,
0.));
#207052=CARTESIAN_POINT('Ctrl Pts',(-4.11600589882767,22.1746949858773,
12.));
#207053=CARTESIAN_POINT('Ctrl Pts',(-4.11589976826061,22.174148802123,0.));
#207054=CARTESIAN_POINT('Ctrl Pts',(-4.11589976826061,22.174148802123,12.));
#207055=CARTESIAN_POINT('Ctrl Pts',(-4.1158603587821,22.1739341411684,0.));
#207056=CARTESIAN_POINT('Ctrl Pts',(-4.1158603587821,22.1739341411684,12.));
#207057=CARTESIAN_POINT('Ctrl Pts',(-4.11585194677412,22.1738776823239,
0.));
#207058=CARTESIAN_POINT('Ctrl Pts',(-4.11585194677412,22.1738776823239,
12.));
#207059=CARTESIAN_POINT('Ctrl Pts',(-4.11585220600461,22.1738711152697,
0.));
#207060=CARTESIAN_POINT('Ctrl Pts',(-4.11585220600461,22.1738711152697,
12.));
#207061=CARTESIAN_POINT('',(-6.08833931617698,25.2771067246846,0.));
#207062=CARTESIAN_POINT('Ctrl Pts',(-6.08833931617698,25.2771067246846,
0.));
#207063=CARTESIAN_POINT('Ctrl Pts',(-6.08441489609824,25.2729539149479,
0.));
#207064=CARTESIAN_POINT('Ctrl Pts',(-6.07657531787578,25.2646490489816,
0.));
#207065=CARTESIAN_POINT('Ctrl Pts',(-6.06484373634697,25.2521940105523,
0.));
#207066=CARTESIAN_POINT('Ctrl Pts',(-6.04925720151412,25.2355918138798,
0.));
#207067=CARTESIAN_POINT('Ctrl Pts',(-6.02986667390187,25.2148466201368,
0.));
#207068=CARTESIAN_POINT('Ctrl Pts',(-6.0105688180476,25.1941090269638,0.));
#207069=CARTESIAN_POINT('Ctrl Pts',(-5.99136367859838,25.1733791296154,
0.));
#207070=CARTESIAN_POINT('Ctrl Pts',(-5.97225131495636,25.1526570863065,
0.));
#207071=CARTESIAN_POINT('Ctrl Pts',(-5.95323180187348,25.1319431317273,
0.));
#207072=CARTESIAN_POINT('Ctrl Pts',(-5.93430523086776,25.1112375971182,
0.));
#207073=CARTESIAN_POINT('Ctrl Pts',(-5.91547170844382,25.0905409050863,
0.));
#207074=CARTESIAN_POINT('Ctrl Pts',(-5.89673135155459,25.0698535426593,
0.));
#207075=CARTESIAN_POINT('Ctrl Pts',(-5.87808428385329,25.0491760405965,
0.));
#207076=CARTESIAN_POINT('Ctrl Pts',(-5.8595306315681,25.0285089498922,0.));
#207077=CARTESIAN_POINT('Ctrl Pts',(-5.84107051963073,25.0078528200558,
0.));
#207078=CARTESIAN_POINT('Ctrl Pts',(-5.82270406744214,24.9872081752709,
0.));
#207079=CARTESIAN_POINT('Ctrl Pts',(-5.80443138549747,24.9665754954462,
0.));
#207080=CARTESIAN_POINT('Ctrl Pts',(-5.78625257775703,24.9459552293308,
0.));
#207081=CARTESIAN_POINT('Ctrl Pts',(-5.76816774342236,24.9253478043632,
0.));
#207082=CARTESIAN_POINT('Ctrl Pts',(-5.75017697890813,24.9047536376467,
0.));
#207083=CARTESIAN_POINT('Ctrl Pts',(-5.73228037976927,24.8841731467219,
0.));
#207084=CARTESIAN_POINT('Ctrl Pts',(-5.71447804252019,24.8636067597677,
0.));
#207085=CARTESIAN_POINT('Ctrl Pts',(-5.69677006679429,24.8430549277634,
0.));
#207086=CARTESIAN_POINT('Ctrl Pts',(-5.67915655496524,24.822518122386,0.));
#207087=CARTESIAN_POINT('Ctrl Pts',(-5.66163761114903,24.8019968304618,
0.));
#207088=CARTESIAN_POINT('Ctrl Pts',(-5.64421334042248,24.7814915496728,
0.));
#207089=CARTESIAN_POINT('Ctrl Pts',(-5.62688384790919,24.76100278357,0.));
#207090=CARTESIAN_POINT('Ctrl Pts',(-5.60964923798495,24.7405310372736,
0.));
#207091=CARTESIAN_POINT('Ctrl Pts',(-5.59250961323995,24.7200768119079,
0.));
#207092=CARTESIAN_POINT('Ctrl Pts',(-5.57546507427767,24.6996406035507,
0.));
#207093=CARTESIAN_POINT('Ctrl Pts',(-5.55851572025389,24.6792229061785,
0.));
#207094=CARTESIAN_POINT('Ctrl Pts',(-5.54166164919593,24.6588242134733,
0.));
#207095=CARTESIAN_POINT('Ctrl Pts',(-5.52490295840996,24.6384450211466,
0.));
#207096=CARTESIAN_POINT('Ctrl Pts',(-5.50823974481959,24.618085828918,0.));
#207097=CARTESIAN_POINT('Ctrl Pts',(-5.49167210537235,24.5977471429365,
0.));
#207098=CARTESIAN_POINT('Ctrl Pts',(-5.47520013724403,24.5774294770329,
0.));
#207099=CARTESIAN_POINT('Ctrl Pts',(-5.45882393762244,24.5571333514841,
0.));
#207100=CARTESIAN_POINT('Ctrl Pts',(-5.44254360356865,24.5368592922861,
0.));
#207101=CARTESIAN_POINT('Ctrl Pts',(-5.42635923183411,24.5166078302107,
0.));
#207102=CARTESIAN_POINT('Ctrl Pts',(-5.41027091869242,24.4963794999831,
0.));
#207103=CARTESIAN_POINT('Ctrl Pts',(-5.3942787597383,24.4761748393322,0.));
#207104=CARTESIAN_POINT('Ctrl Pts',(-5.37838284973706,24.4559943883159,
0.));
#207105=CARTESIAN_POINT('Ctrl Pts',(-5.36258328273639,24.4358386899152,
0.));
#207106=CARTESIAN_POINT('Ctrl Pts',(-5.34688015213546,24.4157082904615,
0.));
#207107=CARTESIAN_POINT('Ctrl Pts',(-5.33127355076037,24.3956037401293,
0.));
#207108=CARTESIAN_POINT('Ctrl Pts',(-5.31576357092524,24.3755255933917,
0.));
#207109=CARTESIAN_POINT('Ctrl Pts',(-5.30035030449059,24.3554744095075,
0.));
#207110=CARTESIAN_POINT('Ctrl Pts',(-5.28503384290644,24.3354507529415,
0.));
#207111=CARTESIAN_POINT('Ctrl Pts',(-5.26981427718796,24.3154551932222,
0.));
#207112=CARTESIAN_POINT('Ctrl Pts',(-5.25469169788856,24.2954883048448,
0.));
#207113=CARTESIAN_POINT('Ctrl Pts',(-5.23966619506289,24.2755506671526,
0.));
#207114=CARTESIAN_POINT('Ctrl Pts',(-5.22473785822441,24.2556428642294,
0.));
#207115=CARTESIAN_POINT('Ctrl Pts',(-5.20990677629173,24.2357654847765,
0.));
#207116=CARTESIAN_POINT('Ctrl Pts',(-5.19517303753643,24.215919122017,0.));
#207117=CARTESIAN_POINT('Ctrl Pts',(-5.18053672961392,24.1961043738754,
0.));
#207118=CARTESIAN_POINT('Ctrl Pts',(-5.16599793957979,24.1763218431343,
0.));
#207119=CARTESIAN_POINT('Ctrl Pts',(-5.15155675390075,24.156572137597,0.));
#207120=CARTESIAN_POINT('Ctrl Pts',(-5.13721325845745,24.1368558702443,
0.));
#207121=CARTESIAN_POINT('Ctrl Pts',(-5.12296753853859,24.117173659394,0.));
#207122=CARTESIAN_POINT('Ctrl Pts',(-5.10881967883132,24.0975261288446,
0.));
#207123=CARTESIAN_POINT('Ctrl Pts',(-5.09476976342625,24.0779139079266,
0.));
#207124=CARTESIAN_POINT('Ctrl Pts',(-5.08081787581276,24.0583376315638,
0.));
#207125=CARTESIAN_POINT('Ctrl Pts',(-5.06696409886641,24.0387979403268,
0.));
#207126=CARTESIAN_POINT('Ctrl Pts',(-5.05320851483065,24.0192954804896,
0.));
#207127=CARTESIAN_POINT('Ctrl Pts',(-5.03955120528521,23.9998309040746,
0.));
#207128=CARTESIAN_POINT('Ctrl Pts',(-5.02599225112454,23.9804048689227,
0.));
#207129=CARTESIAN_POINT('Ctrl Pts',(-5.01253173257453,23.9610180388271,
0.));
#207130=CARTESIAN_POINT('Ctrl Pts',(-4.99916972919307,23.9416710836529,
0.));
#207131=CARTESIAN_POINT('Ctrl Pts',(-4.98590631986533,23.9223646794592,
0.));
#207132=CARTESIAN_POINT('Ctrl Pts',(-4.97274158279227,23.9030995086163,
0.));
#207133=CARTESIAN_POINT('Ctrl Pts',(-4.95967559546561,23.8838762599218,
0.));
#207134=CARTESIAN_POINT('Ctrl Pts',(-4.9467084346586,23.8646956287168,0.));
#207135=CARTESIAN_POINT('Ctrl Pts',(-4.93384017643432,23.8455583170057,
0.));
#207136=CARTESIAN_POINT('Ctrl Pts',(-4.92107089613969,23.8264650335717,
0.));
#207137=CARTESIAN_POINT('Ctrl Pts',(-4.90840066839344,23.8074164940896,
0.));
#207138=CARTESIAN_POINT('Ctrl Pts',(-4.89582956706775,23.7884134212384,
0.));
#207139=CARTESIAN_POINT('Ctrl Pts',(-4.88335766525573,23.7694565448049,
0.));
#207140=CARTESIAN_POINT('Ctrl Pts',(-4.87098503527152,23.7505466018245,
0.));
#207141=CARTESIAN_POINT('Ctrl Pts',(-4.85871174865499,23.7316843367313,
0.));
#207142=CARTESIAN_POINT('Ctrl Pts',(-4.84653787616425,23.7128705015017,
0.));
#207143=CARTESIAN_POINT('Ctrl Pts',(-4.83446348776266,23.6941058557971,
0.));
#207144=CARTESIAN_POINT('Ctrl Pts',(-4.82248865259562,23.675391167102,0.));
#207145=CARTESIAN_POINT('Ctrl Pts',(-4.81061343896432,23.6567272108628,
0.));
#207146=CARTESIAN_POINT('Ctrl Pts',(-4.7988379143322,23.6381147706579,0.));
#207147=CARTESIAN_POINT('Ctrl Pts',(-4.78716214532098,23.6195546383624,
0.));
#207148=CARTESIAN_POINT('Ctrl Pts',(-4.77558619769872,23.6010476143099,
0.));
#207149=CARTESIAN_POINT('Ctrl Pts',(-4.76411013636251,23.5825945074535,
0.));
#207150=CARTESIAN_POINT('Ctrl Pts',(-4.75273402530617,23.5641961355168,
0.));
#207151=CARTESIAN_POINT('Ctrl Pts',(-4.74145792760698,23.545853325171,0.));
#207152=CARTESIAN_POINT('Ctrl Pts',(-4.7302819054303,23.5275669122372,0.));
#207153=CARTESIAN_POINT('Ctrl Pts',(-4.71920602001902,23.509337741878,0.));
#207154=CARTESIAN_POINT('Ctrl Pts',(-4.70823033167819,23.491166668789,0.));
#207155=CARTESIAN_POINT('Ctrl Pts',(-4.69735489975024,23.4730545573853,
0.));
#207156=CARTESIAN_POINT('Ctrl Pts',(-4.68657978258303,23.455002281986,0.));
#207157=CARTESIAN_POINT('Ctrl Pts',(-4.67590503753058,23.4370107270451,
0.));
#207158=CARTESIAN_POINT('Ctrl Pts',(-4.6653307209467,23.4190807873803,0.));
#207159=CARTESIAN_POINT('Ctrl Pts',(-4.65485688816924,23.4012133683959,
0.));
#207160=CARTESIAN_POINT('Ctrl Pts',(-4.6444835934993,23.3834093863068,0.));
#207161=CARTESIAN_POINT('Ctrl Pts',(-4.63421089016541,23.3656697683489,
0.));
#207162=CARTESIAN_POINT('Ctrl Pts',(-4.62403883030805,23.3479954530272,
0.));
#207163=CARTESIAN_POINT('Ctrl Pts',(-4.6139674649783,23.3303873903938,0.));
#207164=CARTESIAN_POINT('Ctrl Pts',(-4.60399684412163,23.3128465423115,
0.));
#207165=CARTESIAN_POINT('Ctrl Pts',(-4.5941270165575,23.2953738827191,0.));
#207166=CARTESIAN_POINT('Ctrl Pts',(-4.5843580299469,23.2779703978876,0.));
#207167=CARTESIAN_POINT('Ctrl Pts',(-4.57468993076097,23.2606370866866,
0.));
#207168=CARTESIAN_POINT('Ctrl Pts',(-4.56512276427839,23.2433749609131,
0.));
#207169=CARTESIAN_POINT('Ctrl Pts',(-4.55565657456975,23.2261850456064,
0.));
#207170=CARTESIAN_POINT('Ctrl Pts',(-4.54629140447544,23.2090683793629,
0.));
#207171=CARTESIAN_POINT('Ctrl Pts',(-4.53702729557566,23.1920260146465,
0.));
#207172=CARTESIAN_POINT('Ctrl Pts',(-4.52786428815015,23.1750590180908,
0.));
#207173=CARTESIAN_POINT('Ctrl Pts',(-4.51880242116748,23.1581684708761,
0.));
#207174=CARTESIAN_POINT('Ctrl Pts',(-4.5098417322706,23.1413554691123,0.));
#207175=CARTESIAN_POINT('Ctrl Pts',(-4.50098225775171,23.1246211242115,
0.));
#207176=CARTESIAN_POINT('Ctrl Pts',(-4.49222403252216,23.1079665632636,
0.));
#207177=CARTESIAN_POINT('Ctrl Pts',(-4.48356709006788,23.0913929293922,
0.));
#207178=CARTESIAN_POINT('Ctrl Pts',(-4.47501146242856,23.0749013821881,
0.));
#207179=CARTESIAN_POINT('Ctrl Pts',(-4.4665571801823,23.0584930981732,0.));
#207180=CARTESIAN_POINT('Ctrl Pts',(-4.45820427241683,23.0421692712467,
0.));
#207181=CARTESIAN_POINT('Ctrl Pts',(-4.44995276669686,23.0259311131392,
0.));
#207182=CARTESIAN_POINT('Ctrl Pts',(-4.44180268901643,23.0097798538395,
0.));
#207183=CARTESIAN_POINT('Ctrl Pts',(-4.43375406376879,22.9937167421006,
0.));
#207184=CARTESIAN_POINT('Ctrl Pts',(-4.42580691372751,22.977743046002,0.));
#207185=CARTESIAN_POINT('Ctrl Pts',(-4.41796126001302,22.9618600534866,
0.));
#207186=CARTESIAN_POINT('Ctrl Pts',(-4.41021712205553,22.9460690729093,
0.));
#207187=CARTESIAN_POINT('Ctrl Pts',(-4.40257451754323,22.930371433555,0.));
#207188=CARTESIAN_POINT('Ctrl Pts',(-4.39503346238473,22.9147684862426,
0.));
#207189=CARTESIAN_POINT('Ctrl Pts',(-4.38759397068406,22.8992616040108,
0.));
#207190=CARTESIAN_POINT('Ctrl Pts',(-4.38025605470093,22.8838521827701,
0.));
#207191=CARTESIAN_POINT('Ctrl Pts',(-4.37301972480746,22.8685416419725,
0.));
#207192=CARTESIAN_POINT('Ctrl Pts',(-4.36588498942997,22.8533314252422,
0.));
#207193=CARTESIAN_POINT('Ctrl Pts',(-4.35885185500546,22.8382230011184,
0.));
#207194=CARTESIAN_POINT('Ctrl Pts',(-4.35192032594791,22.8232178638876,
0.));
#207195=CARTESIAN_POINT('Ctrl Pts',(-4.34509040460062,22.8083175343791,
0.));
#207196=CARTESIAN_POINT('Ctrl Pts',(-4.33836209118446,22.7935235607806,
0.));
#207197=CARTESIAN_POINT('Ctrl Pts',(-4.3317353837319,22.7788375194076,0.));
#207198=CARTESIAN_POINT('Ctrl Pts',(-4.32521027803754,22.7642610156475,
0.));
#207199=CARTESIAN_POINT('Ctrl Pts',(-4.31878676761235,22.7497956849848,
0.));
#207200=CARTESIAN_POINT('Ctrl Pts',(-4.31246484362549,22.7354431939926,
0.));
#207201=CARTESIAN_POINT('Ctrl Pts',(-4.30624449484069,22.7212052413386,
0.));
#207202=CARTESIAN_POINT('Ctrl Pts',(-4.3001257075406,22.7070835587564,0.));
#207203=CARTESIAN_POINT('Ctrl Pts',(-4.29410846547056,22.6930799122548,
0.));
#207204=CARTESIAN_POINT('Ctrl Pts',(-4.28819274977763,22.6791961033538,
0.));
#207205=CARTESIAN_POINT('Ctrl Pts',(-4.28237853894059,22.6654339703109,
0.));
#207206=CARTESIAN_POINT('Ctrl Pts',(-4.2766658086912,22.6517953893303,0.));
#207207=CARTESIAN_POINT('Ctrl Pts',(-4.27105453193004,22.6382822758172,
0.));
#207208=CARTESIAN_POINT('Ctrl Pts',(-4.26554467865576,22.6248965859977,
0.));
#207209=CARTESIAN_POINT('Ctrl Pts',(-4.26013621588305,22.6116403184821,
0.));
#207210=CARTESIAN_POINT('Ctrl Pts',(-4.25482910755481,22.5985155158636,
0.));
#207211=CARTESIAN_POINT('Ctrl Pts',(-4.24962331444177,22.5855242662477,
0.));
#207212=CARTESIAN_POINT('Ctrl Pts',(-4.24451879404851,22.572668704992,0.));
#207213=CARTESIAN_POINT('Ctrl Pts',(-4.23951550052523,22.5599510166429,
0.));
#207214=CARTESIAN_POINT('Ctrl Pts',(-4.23461338456712,22.5473734368086,
0.));
#207215=CARTESIAN_POINT('Ctrl Pts',(-4.22981239330733,22.5349382540588,
0.));
#207216=CARTESIAN_POINT('Ctrl Pts',(-4.22511247020041,22.5226478117886,
0.));
#207217=CARTESIAN_POINT('Ctrl Pts',(-4.22051355490196,22.5105045108881,
0.));
#207218=CARTESIAN_POINT('Ctrl Pts',(-4.21601558313906,22.4985108124228,
0.));
#207219=CARTESIAN_POINT('Ctrl Pts',(-4.21161848657428,22.4866692403147,
0.));
#207220=CARTESIAN_POINT('Ctrl Pts',(-4.20732219265649,22.4749823839917,
0.));
#207221=CARTESIAN_POINT('Ctrl Pts',(-4.20312662448174,22.4634529011437,
0.));
#207222=CARTESIAN_POINT('Ctrl Pts',(-4.19903170066358,22.4520835205422,
0.));
#207223=CARTESIAN_POINT('Ctrl Pts',(-4.1950373351886,22.4408770448917,0.));
#207224=CARTESIAN_POINT('Ctrl Pts',(-4.19114343726932,22.4298363535416,
0.));
#207225=CARTESIAN_POINT('Ctrl Pts',(-4.18734991117707,22.4189644056109,
0.));
#207226=CARTESIAN_POINT('Ctrl Pts',(-4.18365665600839,22.4082642454448,
0.));
#207227=CARTESIAN_POINT('Ctrl Pts',(-4.18006356544879,22.3977390078074,
0.));
#207228=CARTESIAN_POINT('Ctrl Pts',(-4.17657052752834,22.3873919231339,
0.));
#207229=CARTESIAN_POINT('Ctrl Pts',(-4.17317742436162,22.3772263228624,
0.));
#207230=CARTESIAN_POINT('Ctrl Pts',(-4.1698841319947,22.3672456427605,0.));
#207231=CARTESIAN_POINT('Ctrl Pts',(-4.16669052026602,22.3574534257397,
0.));
#207232=CARTESIAN_POINT('Ctrl Pts',(-4.1635964526318,22.3478533253886,0.));
#207233=CARTESIAN_POINT('Ctrl Pts',(-4.16060178604154,22.3384491078599,
0.));
#207234=CARTESIAN_POINT('Ctrl Pts',(-4.15770637047882,22.3292446628957,
0.));
#207235=CARTESIAN_POINT('Ctrl Pts',(-4.15491004835278,22.3202440186979,
0.));
#207236=CARTESIAN_POINT('Ctrl Pts',(-4.15221265396992,22.3114513545186,
0.));
#207237=CARTESIAN_POINT('Ctrl Pts',(-4.14961401285526,22.3028710166935,
0.));
#207238=CARTESIAN_POINT('Ctrl Pts',(-4.14711394168559,22.2945075198468,
0.));
#207239=CARTESIAN_POINT('Ctrl Pts',(-4.14471224859295,22.2863655389166,
0.));
#207240=CARTESIAN_POINT('Ctrl Pts',(-4.14240873321982,22.2784499072026,
0.));
#207241=CARTESIAN_POINT('Ctrl Pts',(-4.14020318715988,22.2707656042456,
0.));
#207242=CARTESIAN_POINT('Ctrl Pts',(-4.13809539255419,22.263317791397,0.));
#207243=CARTESIAN_POINT('Ctrl Pts',(-4.13608511977226,22.2561118708422,
0.));
#207244=CARTESIAN_POINT('Ctrl Pts',(-4.13417212558808,22.2491535317789,
0.));
#207245=CARTESIAN_POINT('Ctrl Pts',(-4.1323561506016,22.2424488153523,0.));
#207246=CARTESIAN_POINT('Ctrl Pts',(-4.13063692157499,22.2360040565534,
0.));
#207247=CARTESIAN_POINT('Ctrl Pts',(-4.12901415463379,22.2298258043947,
0.));
#207248=CARTESIAN_POINT('Ctrl Pts',(-4.12748755830099,22.2239207458781,
0.));
#207249=CARTESIAN_POINT('Ctrl Pts',(-4.126056836133,22.2182956401341,0.));
#207250=CARTESIAN_POINT('Ctrl Pts',(-4.12472167516602,22.2129576146671,
0.));
#207251=CARTESIAN_POINT('Ctrl Pts',(-4.12348173702025,22.2079143941719,
0.));
#207252=CARTESIAN_POINT('Ctrl Pts',(-4.12233664408237,22.2031746532106,
0.));
#207253=CARTESIAN_POINT('Ctrl Pts',(-4.12128598183533,22.1987479618246,
0.));
#207254=CARTESIAN_POINT('Ctrl Pts',(-4.12032932637738,22.1946440958098,
0.));
#207255=CARTESIAN_POINT('Ctrl Pts',(-4.11946626228623,22.1908725908525,
0.));
#207256=CARTESIAN_POINT('Ctrl Pts',(-4.11869641271752,22.1874419861496,
0.));
#207257=CARTESIAN_POINT('Ctrl Pts',(-4.11801938107464,22.1843613164855,
0.));
#207258=CARTESIAN_POINT('Ctrl Pts',(-4.11743469691765,22.1816414985788,
0.));
#207259=CARTESIAN_POINT('Ctrl Pts',(-4.11694173195041,22.179297473024,0.));
#207260=CARTESIAN_POINT('Ctrl Pts',(-4.11653973150558,22.177347426894,0.));
#207261=CARTESIAN_POINT('Ctrl Pts',(-4.11622797217066,22.1758088296598,
0.));
#207262=CARTESIAN_POINT('Ctrl Pts',(-4.11600589882767,22.1746949858773,
0.));
#207263=CARTESIAN_POINT('Ctrl Pts',(-4.11589976826061,22.174148802123,0.));
#207264=CARTESIAN_POINT('Ctrl Pts',(-4.1158603587821,22.1739341411684,0.));
#207265=CARTESIAN_POINT('Ctrl Pts',(-4.11585194677412,22.1738776823239,
0.));
#207266=CARTESIAN_POINT('Ctrl Pts',(-4.11585220600461,22.1738711152697,
0.));
#207267=CARTESIAN_POINT('',(-6.08833931617698,25.2771067246846,0.));
#207268=CARTESIAN_POINT('Ctrl Pts',(-1.76341220531179,22.4835757167854,
0.));
#207269=CARTESIAN_POINT('Ctrl Pts',(-1.76341220531179,22.4835757167854,
12.));
#207270=CARTESIAN_POINT('Ctrl Pts',(-1.76341415538764,22.483581992979,0.));
#207271=CARTESIAN_POINT('Ctrl Pts',(-1.76341415538764,22.483581992979,12.));
#207272=CARTESIAN_POINT('Ctrl Pts',(-1.7634206426357,22.4836387052232,0.));
#207273=CARTESIAN_POINT('Ctrl Pts',(-1.7634206426357,22.4836387052232,12.));
#207274=CARTESIAN_POINT('Ctrl Pts',(-1.76343813434565,22.483856251707,0.));
#207275=CARTESIAN_POINT('Ctrl Pts',(-1.76343813434565,22.483856251707,12.));
#207276=CARTESIAN_POINT('Ctrl Pts',(-1.76347698284792,22.4844112933129,
0.));
#207277=CARTESIAN_POINT('Ctrl Pts',(-1.76347698284792,22.4844112933129,
12.));
#207278=CARTESIAN_POINT('Ctrl Pts',(-1.76355076045546,22.4855446605991,
0.));
#207279=CARTESIAN_POINT('Ctrl Pts',(-1.76355076045546,22.4855446605991,
12.));
#207280=CARTESIAN_POINT('Ctrl Pts',(-1.76364784232963,22.4871115206571,
0.));
#207281=CARTESIAN_POINT('Ctrl Pts',(-1.76364784232963,22.4871115206571,
12.));
#207282=CARTESIAN_POINT('Ctrl Pts',(-1.76376424879505,22.4890991659478,
0.));
#207283=CARTESIAN_POINT('Ctrl Pts',(-1.76376424879505,22.4890991659478,
12.));
#207284=CARTESIAN_POINT('Ctrl Pts',(-1.76389475965724,22.4914909094908,
0.));
#207285=CARTESIAN_POINT('Ctrl Pts',(-1.76389475965724,22.4914909094908,
12.));
#207286=CARTESIAN_POINT('Ctrl Pts',(-1.76403393880301,22.4942693792449,
0.));
#207287=CARTESIAN_POINT('Ctrl Pts',(-1.76403393880301,22.4942693792449,
12.));
#207288=CARTESIAN_POINT('Ctrl Pts',(-1.76417731243462,22.4974203063191,
0.));
#207289=CARTESIAN_POINT('Ctrl Pts',(-1.76417731243462,22.4974203063191,
12.));
#207290=CARTESIAN_POINT('Ctrl Pts',(-1.76432160068725,22.5009332677316,
0.));
#207291=CARTESIAN_POINT('Ctrl Pts',(-1.76432160068725,22.5009332677316,
12.));
#207292=CARTESIAN_POINT('Ctrl Pts',(-1.76446408210366,22.5047996391978,
0.));
#207293=CARTESIAN_POINT('Ctrl Pts',(-1.76446408210366,22.5047996391978,
12.));
#207294=CARTESIAN_POINT('Ctrl Pts',(-1.76460218257323,22.5090112700212,
0.));
#207295=CARTESIAN_POINT('Ctrl Pts',(-1.76460218257323,22.5090112700212,
12.));
#207296=CARTESIAN_POINT('Ctrl Pts',(-1.76473303281159,22.5135590569554,
0.));
#207297=CARTESIAN_POINT('Ctrl Pts',(-1.76473303281159,22.5135590569554,
12.));
#207298=CARTESIAN_POINT('Ctrl Pts',(-1.76485369319896,22.5184336670207,
0.));
#207299=CARTESIAN_POINT('Ctrl Pts',(-1.76485369319896,22.5184336670207,
12.));
#207300=CARTESIAN_POINT('Ctrl Pts',(-1.76496128643369,22.5236259635515,
0.));
#207301=CARTESIAN_POINT('Ctrl Pts',(-1.76496128643369,22.5236259635515,
12.));
#207302=CARTESIAN_POINT('Ctrl Pts',(-1.76505320262752,22.529127665298,0.));
#207303=CARTESIAN_POINT('Ctrl Pts',(-1.76505320262752,22.529127665298,12.));
#207304=CARTESIAN_POINT('Ctrl Pts',(-1.7651271156325,22.5349313983571,0.));
#207305=CARTESIAN_POINT('Ctrl Pts',(-1.7651271156325,22.5349313983571,12.));
#207306=CARTESIAN_POINT('Ctrl Pts',(-1.76518087841493,22.5410303590891,
0.));
#207307=CARTESIAN_POINT('Ctrl Pts',(-1.76518087841493,22.5410303590891,
12.));
#207308=CARTESIAN_POINT('Ctrl Pts',(-1.76521245524047,22.5474180954006,
0.));
#207309=CARTESIAN_POINT('Ctrl Pts',(-1.76521245524047,22.5474180954006,
12.));
#207310=CARTESIAN_POINT('Ctrl Pts',(-1.76521983384063,22.5540882235837,
0.));
#207311=CARTESIAN_POINT('Ctrl Pts',(-1.76521983384063,22.5540882235837,
12.));
#207312=CARTESIAN_POINT('Ctrl Pts',(-1.76520104500449,22.5610344912501,
0.));
#207313=CARTESIAN_POINT('Ctrl Pts',(-1.76520104500449,22.5610344912501,
12.));
#207314=CARTESIAN_POINT('Ctrl Pts',(-1.76515418518829,22.5682508499873,
0.));
#207315=CARTESIAN_POINT('Ctrl Pts',(-1.76515418518829,22.5682508499873,
12.));
#207316=CARTESIAN_POINT('Ctrl Pts',(-1.76507744026747,22.5757315316355,
0.));
#207317=CARTESIAN_POINT('Ctrl Pts',(-1.76507744026747,22.5757315316355,
12.));
#207318=CARTESIAN_POINT('Ctrl Pts',(-1.76496910283088,22.5834711038024,
0.));
#207319=CARTESIAN_POINT('Ctrl Pts',(-1.76496910283088,22.5834711038024,
12.));
#207320=CARTESIAN_POINT('Ctrl Pts',(-1.76482755288411,22.5914644078106,
0.));
#207321=CARTESIAN_POINT('Ctrl Pts',(-1.76482755288411,22.5914644078106,
12.));
#207322=CARTESIAN_POINT('Ctrl Pts',(-1.76465124413556,22.5997065145638,
0.));
#207323=CARTESIAN_POINT('Ctrl Pts',(-1.76465124413556,22.5997065145638,
12.));
#207324=CARTESIAN_POINT('Ctrl Pts',(-1.76443868648015,22.6081926681342,
0.));
#207325=CARTESIAN_POINT('Ctrl Pts',(-1.76443868648015,22.6081926681342,
12.));
#207326=CARTESIAN_POINT('Ctrl Pts',(-1.76418843543739,22.6169182517693,
0.));
#207327=CARTESIAN_POINT('Ctrl Pts',(-1.76418843543739,22.6169182517693,
12.));
#207328=CARTESIAN_POINT('Ctrl Pts',(-1.76389909571402,22.6258787994847,
0.));
#207329=CARTESIAN_POINT('Ctrl Pts',(-1.76389909571402,22.6258787994847,
12.));
#207330=CARTESIAN_POINT('Ctrl Pts',(-1.76356932176272,22.635069997936,0.));
#207331=CARTESIAN_POINT('Ctrl Pts',(-1.76356932176272,22.635069997936,12.));
#207332=CARTESIAN_POINT('Ctrl Pts',(-1.76319782013914,22.6444876940425,
0.));
#207333=CARTESIAN_POINT('Ctrl Pts',(-1.76319782013914,22.6444876940425,
12.));
#207334=CARTESIAN_POINT('Ctrl Pts',(-1.76278334912559,22.6541278938413,
0.));
#207335=CARTESIAN_POINT('Ctrl Pts',(-1.76278334912559,22.6541278938413,
12.));
#207336=CARTESIAN_POINT('Ctrl Pts',(-1.76232471392567,22.6639867471756,
0.));
#207337=CARTESIAN_POINT('Ctrl Pts',(-1.76232471392567,22.6639867471756,
12.));
#207338=CARTESIAN_POINT('Ctrl Pts',(-1.76182076289525,22.6740605356699,
0.));
#207339=CARTESIAN_POINT('Ctrl Pts',(-1.76182076289525,22.6740605356699,
12.));
#207340=CARTESIAN_POINT('Ctrl Pts',(-1.76127038310613,22.6843456585245,
0.));
#207341=CARTESIAN_POINT('Ctrl Pts',(-1.76127038310613,22.6843456585245,
12.));
#207342=CARTESIAN_POINT('Ctrl Pts',(-1.76067249704884,22.6948386219843,
0.));
#207343=CARTESIAN_POINT('Ctrl Pts',(-1.76067249704884,22.6948386219843,
12.));
#207344=CARTESIAN_POINT('Ctrl Pts',(-1.76002606202399,22.7055360375481,
0.));
#207345=CARTESIAN_POINT('Ctrl Pts',(-1.76002606202399,22.7055360375481,
12.));
#207346=CARTESIAN_POINT('Ctrl Pts',(-1.75933006905924,22.7164346186007,
0.));
#207347=CARTESIAN_POINT('Ctrl Pts',(-1.75933006905924,22.7164346186007,
12.));
#207348=CARTESIAN_POINT('Ctrl Pts',(-1.75858354204635,22.7275311777305,
0.));
#207349=CARTESIAN_POINT('Ctrl Pts',(-1.75858354204635,22.7275311777305,
12.));
#207350=CARTESIAN_POINT('Ctrl Pts',(-1.75778553673249,22.7388226235565,
0.));
#207351=CARTESIAN_POINT('Ctrl Pts',(-1.75778553673249,22.7388226235565,
12.));
#207352=CARTESIAN_POINT('Ctrl Pts',(-1.75693513908911,22.7503059556455,
0.));
#207353=CARTESIAN_POINT('Ctrl Pts',(-1.75693513908911,22.7503059556455,
12.));
#207354=CARTESIAN_POINT('Ctrl Pts',(-1.7560314637164,22.7619782595013,0.));
#207355=CARTESIAN_POINT('Ctrl Pts',(-1.7560314637164,22.7619782595013,12.));
#207356=CARTESIAN_POINT('Ctrl Pts',(-1.75507365227127,22.7738367016115,
0.));
#207357=CARTESIAN_POINT('Ctrl Pts',(-1.75507365227127,22.7738367016115,
12.));
#207358=CARTESIAN_POINT('Ctrl Pts',(-1.7540608718293,22.7858785242358,0.));
#207359=CARTESIAN_POINT('Ctrl Pts',(-1.7540608718293,22.7858785242358,12.));
#207360=CARTESIAN_POINT('Ctrl Pts',(-1.75299231391461,22.7981010424312,
0.));
#207361=CARTESIAN_POINT('Ctrl Pts',(-1.75299231391461,22.7981010424312,
12.));
#207362=CARTESIAN_POINT('Ctrl Pts',(-1.7518671936559,22.8105016414712,0.));
#207363=CARTESIAN_POINT('Ctrl Pts',(-1.7518671936559,22.8105016414712,12.));
#207364=CARTESIAN_POINT('Ctrl Pts',(-1.75068474890884,22.8230777741285,
0.));
#207365=CARTESIAN_POINT('Ctrl Pts',(-1.75068474890884,22.8230777741285,
12.));
#207366=CARTESIAN_POINT('Ctrl Pts',(-1.74944423940117,22.8358269579854,
0.));
#207367=CARTESIAN_POINT('Ctrl Pts',(-1.74944423940117,22.8358269579854,
12.));
#207368=CARTESIAN_POINT('Ctrl Pts',(-1.74814494588492,22.8487467728075,
0.));
#207369=CARTESIAN_POINT('Ctrl Pts',(-1.74814494588492,22.8487467728075,
12.));
#207370=CARTESIAN_POINT('Ctrl Pts',(-1.74678616930663,22.8618348580234,
0.));
#207371=CARTESIAN_POINT('Ctrl Pts',(-1.74678616930663,22.8618348580234,
12.));
#207372=CARTESIAN_POINT('Ctrl Pts',(-1.745367229982,22.8750889101696,0.));
#207373=CARTESIAN_POINT('Ctrl Pts',(-1.745367229982,22.8750889101696,12.));
#207374=CARTESIAN_POINT('Ctrl Pts',(-1.74388746677702,22.8885066803351,
0.));
#207375=CARTESIAN_POINT('Ctrl Pts',(-1.74388746677702,22.8885066803351,
12.));
#207376=CARTESIAN_POINT('Ctrl Pts',(-1.74234623630079,22.9020859716144,
0.));
#207377=CARTESIAN_POINT('Ctrl Pts',(-1.74234623630079,22.9020859716144,
12.));
#207378=CARTESIAN_POINT('Ctrl Pts',(-1.74074291231057,22.9158246373365,
0.));
#207379=CARTESIAN_POINT('Ctrl Pts',(-1.74074291231057,22.9158246373365,
12.));
#207380=CARTESIAN_POINT('Ctrl Pts',(-1.73907688511664,22.9297205792587,
0.));
#207381=CARTESIAN_POINT('Ctrl Pts',(-1.73907688511664,22.9297205792587,
12.));
#207382=CARTESIAN_POINT('Ctrl Pts',(-1.73734756100038,22.9437717457825,
0.));
#207383=CARTESIAN_POINT('Ctrl Pts',(-1.73734756100038,22.9437717457825,
12.));
#207384=CARTESIAN_POINT('Ctrl Pts',(-1.73555436162771,22.9579761301062,
0.));
#207385=CARTESIAN_POINT('Ctrl Pts',(-1.73555436162771,22.9579761301062,
12.));
#207386=CARTESIAN_POINT('Ctrl Pts',(-1.73369672350818,22.9723317685688,
0.));
#207387=CARTESIAN_POINT('Ctrl Pts',(-1.73369672350818,22.9723317685688,
12.));
#207388=CARTESIAN_POINT('Ctrl Pts',(-1.73177409750194,22.9868367391978,
0.));
#207389=CARTESIAN_POINT('Ctrl Pts',(-1.73177409750194,22.9868367391978,
12.));
#207390=CARTESIAN_POINT('Ctrl Pts',(-1.72978594832137,23.0014891601891,
0.));
#207391=CARTESIAN_POINT('Ctrl Pts',(-1.72978594832137,23.0014891601891,
12.));
#207392=CARTESIAN_POINT('Ctrl Pts',(-1.72773175404703,23.0162871884167,
0.));
#207393=CARTESIAN_POINT('Ctrl Pts',(-1.72773175404703,23.0162871884167,
12.));
#207394=CARTESIAN_POINT('Ctrl Pts',(-1.72561100564033,23.031229017888,0.));
#207395=CARTESIAN_POINT('Ctrl Pts',(-1.72561100564033,23.031229017888,12.));
#207396=CARTESIAN_POINT('Ctrl Pts',(-1.72342320653731,23.0463128785528,
0.));
#207397=CARTESIAN_POINT('Ctrl Pts',(-1.72342320653731,23.0463128785528,
12.));
#207398=CARTESIAN_POINT('Ctrl Pts',(-1.7211678722598,23.061537035156,0.));
#207399=CARTESIAN_POINT('Ctrl Pts',(-1.7211678722598,23.061537035156,12.));
#207400=CARTESIAN_POINT('Ctrl Pts',(-1.71884453003027,23.0768997860709,
0.));
#207401=CARTESIAN_POINT('Ctrl Pts',(-1.71884453003027,23.0768997860709,
12.));
#207402=CARTESIAN_POINT('Ctrl Pts',(-1.71645271839311,23.0923994621216,
0.));
#207403=CARTESIAN_POINT('Ctrl Pts',(-1.71645271839311,23.0923994621216,
12.));
#207404=CARTESIAN_POINT('Ctrl Pts',(-1.71399198684725,23.1080344254291,
0.));
#207405=CARTESIAN_POINT('Ctrl Pts',(-1.71399198684725,23.1080344254291,
12.));
#207406=CARTESIAN_POINT('Ctrl Pts',(-1.71146189552192,23.1238030684929,
0.));
#207407=CARTESIAN_POINT('Ctrl Pts',(-1.71146189552192,23.1238030684929,
12.));
#207408=CARTESIAN_POINT('Ctrl Pts',(-1.7088620148546,23.1397038132358,0.));
#207409=CARTESIAN_POINT('Ctrl Pts',(-1.7088620148546,23.1397038132358,12.));
#207410=CARTESIAN_POINT('Ctrl Pts',(-1.70619192527847,23.1557351100613,
0.));
#207411=CARTESIAN_POINT('Ctrl Pts',(-1.70619192527847,23.1557351100613,
12.));
#207412=CARTESIAN_POINT('Ctrl Pts',(-1.70345121691259,23.1718954368749,
0.));
#207413=CARTESIAN_POINT('Ctrl Pts',(-1.70345121691259,23.1718954368749,
12.));
#207414=CARTESIAN_POINT('Ctrl Pts',(-1.70063948926987,23.1881832981848,
0.));
#207415=CARTESIAN_POINT('Ctrl Pts',(-1.70063948926987,23.1881832981848,
12.));
#207416=CARTESIAN_POINT('Ctrl Pts',(-1.69775635099425,23.2045972243765,
0.));
#207417=CARTESIAN_POINT('Ctrl Pts',(-1.69775635099425,23.2045972243765,
12.));
#207418=CARTESIAN_POINT('Ctrl Pts',(-1.69480141959946,23.2211357709374,
0.));
#207419=CARTESIAN_POINT('Ctrl Pts',(-1.69480141959946,23.2211357709374,
12.));
#207420=CARTESIAN_POINT('Ctrl Pts',(-1.69177432121716,23.2377975177014,
0.));
#207421=CARTESIAN_POINT('Ctrl Pts',(-1.69177432121716,23.2377975177014,
12.));
#207422=CARTESIAN_POINT('Ctrl Pts',(-1.6886746903491,23.2545810680536,0.));
#207423=CARTESIAN_POINT('Ctrl Pts',(-1.6886746903491,23.2545810680536,12.));
#207424=CARTESIAN_POINT('Ctrl Pts',(-1.68550216963275,23.2714850482245,
0.));
#207425=CARTESIAN_POINT('Ctrl Pts',(-1.68550216963275,23.2714850482245,
12.));
#207426=CARTESIAN_POINT('Ctrl Pts',(-1.68225640962181,23.2885081066949,
0.));
#207427=CARTESIAN_POINT('Ctrl Pts',(-1.68225640962181,23.2885081066949,
12.));
#207428=CARTESIAN_POINT('Ctrl Pts',(-1.67893706857123,23.3056489135611,
0.));
#207429=CARTESIAN_POINT('Ctrl Pts',(-1.67893706857123,23.3056489135611,
12.));
#207430=CARTESIAN_POINT('Ctrl Pts',(-1.67554381222987,23.3229061599145,
0.));
#207431=CARTESIAN_POINT('Ctrl Pts',(-1.67554381222987,23.3229061599145,
12.));
#207432=CARTESIAN_POINT('Ctrl Pts',(-1.67207631363905,23.3402785571866,
0.));
#207433=CARTESIAN_POINT('Ctrl Pts',(-1.67207631363905,23.3402785571866,
12.));
#207434=CARTESIAN_POINT('Ctrl Pts',(-1.66853425293978,23.3577648365747,
0.));
#207435=CARTESIAN_POINT('Ctrl Pts',(-1.66853425293978,23.3577648365747,
12.));
#207436=CARTESIAN_POINT('Ctrl Pts',(-1.66491731718864,23.375363748555,0.));
#207437=CARTESIAN_POINT('Ctrl Pts',(-1.66491731718864,23.375363748555,12.));
#207438=CARTESIAN_POINT('Ctrl Pts',(-1.66122520018008,23.3930740623622,
0.));
#207439=CARTESIAN_POINT('Ctrl Pts',(-1.66122520018008,23.3930740623622,
12.));
#207440=CARTESIAN_POINT('Ctrl Pts',(-1.65745760227507,23.4108945654803,
0.));
#207441=CARTESIAN_POINT('Ctrl Pts',(-1.65745760227507,23.4108945654803,
12.));
#207442=CARTESIAN_POINT('Ctrl Pts',(-1.6536142302373,23.4288240631034,0.));
#207443=CARTESIAN_POINT('Ctrl Pts',(-1.6536142302373,23.4288240631034,12.));
#207444=CARTESIAN_POINT('Ctrl Pts',(-1.6496947970734,23.446861377656,0.));
#207445=CARTESIAN_POINT('Ctrl Pts',(-1.6496947970734,23.446861377656,12.));
#207446=CARTESIAN_POINT('Ctrl Pts',(-1.64569902187608,23.4650053483919,
0.));
#207447=CARTESIAN_POINT('Ctrl Pts',(-1.64569902187608,23.4650053483919,
12.));
#207448=CARTESIAN_POINT('Ctrl Pts',(-1.64162662967525,23.4832548309638,
0.));
#207449=CARTESIAN_POINT('Ctrl Pts',(-1.64162662967525,23.4832548309638,
12.));
#207450=CARTESIAN_POINT('Ctrl Pts',(-1.63747735129474,23.5016086970006,
0.));
#207451=CARTESIAN_POINT('Ctrl Pts',(-1.63747735129474,23.5016086970006,
12.));
#207452=CARTESIAN_POINT('Ctrl Pts',(-1.63325092321731,23.5200658336624,
0.));
#207453=CARTESIAN_POINT('Ctrl Pts',(-1.63325092321731,23.5200658336624,
12.));
#207454=CARTESIAN_POINT('Ctrl Pts',(-1.62894708745231,23.5386251432278,
0.));
#207455=CARTESIAN_POINT('Ctrl Pts',(-1.62894708745231,23.5386251432278,
12.));
#207456=CARTESIAN_POINT('Ctrl Pts',(-1.62456559140072,23.5572855427617,
0.));
#207457=CARTESIAN_POINT('Ctrl Pts',(-1.62456559140072,23.5572855427617,
12.));
#207458=CARTESIAN_POINT('Ctrl Pts',(-1.62010618772869,23.5760459637608,
0.));
#207459=CARTESIAN_POINT('Ctrl Pts',(-1.62010618772869,23.5760459637608,
12.));
#207460=CARTESIAN_POINT('Ctrl Pts',(-1.61556863424697,23.5949053517996,
0.));
#207461=CARTESIAN_POINT('Ctrl Pts',(-1.61556863424697,23.5949053517996,
12.));
#207462=CARTESIAN_POINT('Ctrl Pts',(-1.61095269379773,23.6138626661644,
0.));
#207463=CARTESIAN_POINT('Ctrl Pts',(-1.61095269379773,23.6138626661644,
12.));
#207464=CARTESIAN_POINT('Ctrl Pts',(-1.60625813414666,23.6329168794916,
0.));
#207465=CARTESIAN_POINT('Ctrl Pts',(-1.60625813414666,23.6329168794916,
12.));
#207466=CARTESIAN_POINT('Ctrl Pts',(-1.60148472786588,23.6520669774863,
0.));
#207467=CARTESIAN_POINT('Ctrl Pts',(-1.60148472786588,23.6520669774863,
12.));
#207468=CARTESIAN_POINT('Ctrl Pts',(-1.59663225222458,23.6713119586302,
0.));
#207469=CARTESIAN_POINT('Ctrl Pts',(-1.59663225222458,23.6713119586302,
12.));
#207470=CARTESIAN_POINT('Ctrl Pts',(-1.59170048908632,23.6906508338833,
0.));
#207471=CARTESIAN_POINT('Ctrl Pts',(-1.59170048908632,23.6906508338833,
12.));
#207472=CARTESIAN_POINT('Ctrl Pts',(-1.58668922481222,23.7100826263835,
0.));
#207473=CARTESIAN_POINT('Ctrl Pts',(-1.58668922481222,23.7100826263835,
12.));
#207474=CARTESIAN_POINT('Ctrl Pts',(-1.58159825017362,23.7296063711308,
0.));
#207475=CARTESIAN_POINT('Ctrl Pts',(-1.58159825017362,23.7296063711308,
12.));
#207476=CARTESIAN_POINT('Ctrl Pts',(-1.57642736025251,23.7492211147369,
0.));
#207477=CARTESIAN_POINT('Ctrl Pts',(-1.57642736025251,23.7492211147369,
12.));
#207478=CARTESIAN_POINT('Ctrl Pts',(-1.57117635434412,23.7689259151869,
0.));
#207479=CARTESIAN_POINT('Ctrl Pts',(-1.57117635434412,23.7689259151869,
12.));
#207480=CARTESIAN_POINT('Ctrl Pts',(-1.56584503586844,23.788719841588,0.));
#207481=CARTESIAN_POINT('Ctrl Pts',(-1.56584503586844,23.788719841588,12.));
#207482=CARTESIAN_POINT('Ctrl Pts',(-1.56043321228631,23.8086019739192,
0.));
#207483=CARTESIAN_POINT('Ctrl Pts',(-1.56043321228631,23.8086019739192,
12.));
#207484=CARTESIAN_POINT('Ctrl Pts',(-1.55494069502628,23.8285714027631,
0.));
#207485=CARTESIAN_POINT('Ctrl Pts',(-1.55494069502628,23.8285714027631,
12.));
#207486=CARTESIAN_POINT('Ctrl Pts',(-1.5493672994053,23.8486272290698,0.));
#207487=CARTESIAN_POINT('Ctrl Pts',(-1.5493672994053,23.8486272290698,12.));
#207488=CARTESIAN_POINT('Ctrl Pts',(-1.54371284453978,23.8687685639635,
0.));
#207489=CARTESIAN_POINT('Ctrl Pts',(-1.54371284453978,23.8687685639635,
12.));
#207490=CARTESIAN_POINT('Ctrl Pts',(-1.53797715326748,23.8889945285313,
0.));
#207491=CARTESIAN_POINT('Ctrl Pts',(-1.53797715326748,23.8889945285313,
12.));
#207492=CARTESIAN_POINT('Ctrl Pts',(-1.53216005207462,23.9093042536119,
0.));
#207493=CARTESIAN_POINT('Ctrl Pts',(-1.53216005207462,23.9093042536119,
12.));
#207494=CARTESIAN_POINT('Ctrl Pts',(-1.5262613710304,23.9296968795761,0.));
#207495=CARTESIAN_POINT('Ctrl Pts',(-1.5262613710304,23.9296968795761,12.));
#207496=CARTESIAN_POINT('Ctrl Pts',(-1.52028094372806,23.9501715561038,
0.));
#207497=CARTESIAN_POINT('Ctrl Pts',(-1.52028094372806,23.9501715561038,
12.));
#207498=CARTESIAN_POINT('Ctrl Pts',(-1.51421860720628,23.9707274420145,
0.));
#207499=CARTESIAN_POINT('Ctrl Pts',(-1.51421860720628,23.9707274420145,
12.));
#207500=CARTESIAN_POINT('Ctrl Pts',(-1.50807420187703,23.991363705093,0.));
#207501=CARTESIAN_POINT('Ctrl Pts',(-1.50807420187703,23.991363705093,12.));
#207502=CARTESIAN_POINT('Ctrl Pts',(-1.50184757146099,24.0120795219086,
0.));
#207503=CARTESIAN_POINT('Ctrl Pts',(-1.50184757146099,24.0120795219086,
12.));
#207504=CARTESIAN_POINT('Ctrl Pts',(-1.49553856292798,24.0328740776331,
0.));
#207505=CARTESIAN_POINT('Ctrl Pts',(-1.49553856292798,24.0328740776331,
12.));
#207506=CARTESIAN_POINT('Ctrl Pts',(-1.48914702644883,24.053746565843,0.));
#207507=CARTESIAN_POINT('Ctrl Pts',(-1.48914702644883,24.053746565843,12.));
#207508=CARTESIAN_POINT('Ctrl Pts',(-1.4826728153368,24.074696188353,0.));
#207509=CARTESIAN_POINT('Ctrl Pts',(-1.4826728153368,24.074696188353,12.));
#207510=CARTESIAN_POINT('Ctrl Pts',(-1.47611578597741,24.0957221550782,
0.));
#207511=CARTESIAN_POINT('Ctrl Pts',(-1.47611578597741,24.0957221550782,
12.));
#207512=CARTESIAN_POINT('Ctrl Pts',(-1.46947579776992,24.1168236838827,
0.));
#207513=CARTESIAN_POINT('Ctrl Pts',(-1.46947579776992,24.1168236838827,
12.));
#207514=CARTESIAN_POINT('Ctrl Pts',(-1.46275271307398,24.1380000004272,
0.));
#207515=CARTESIAN_POINT('Ctrl Pts',(-1.46275271307398,24.1380000004272,
12.));
#207516=CARTESIAN_POINT('Ctrl Pts',(-1.45594639716314,24.1592503380105,
0.));
#207517=CARTESIAN_POINT('Ctrl Pts',(-1.45594639716314,24.1592503380105,
12.));
#207518=CARTESIAN_POINT('Ctrl Pts',(-1.44905671818721,24.1805739374033,
0.));
#207519=CARTESIAN_POINT('Ctrl Pts',(-1.44905671818721,24.1805739374033,
12.));
#207520=CARTESIAN_POINT('Ctrl Pts',(-1.44208354711074,24.2019700467214,
0.));
#207521=CARTESIAN_POINT('Ctrl Pts',(-1.44208354711074,24.2019700467214,
12.));
#207522=CARTESIAN_POINT('Ctrl Pts',(-1.43502675765502,24.2234379212978,
0.));
#207523=CARTESIAN_POINT('Ctrl Pts',(-1.43502675765502,24.2234379212978,
12.));
#207524=CARTESIAN_POINT('Ctrl Pts',(-1.42788622624851,24.2449768235485,
0.));
#207525=CARTESIAN_POINT('Ctrl Pts',(-1.42788622624851,24.2449768235485,
12.));
#207526=CARTESIAN_POINT('Ctrl Pts',(-1.42066183198252,24.2665860228357,
0.));
#207527=CARTESIAN_POINT('Ctrl Pts',(-1.42066183198252,24.2665860228357,
12.));
#207528=CARTESIAN_POINT('Ctrl Pts',(-1.41335345657685,24.2882647953214,
0.));
#207529=CARTESIAN_POINT('Ctrl Pts',(-1.41335345657685,24.2882647953214,
12.));
#207530=CARTESIAN_POINT('Ctrl Pts',(-1.40596098434341,24.3100124238316,
0.));
#207531=CARTESIAN_POINT('Ctrl Pts',(-1.40596098434341,24.3100124238316,
12.));
#207532=CARTESIAN_POINT('Ctrl Pts',(-1.3984843021281,24.3318281977647,0.));
#207533=CARTESIAN_POINT('Ctrl Pts',(-1.3984843021281,24.3318281977647,12.));
#207534=CARTESIAN_POINT('Ctrl Pts',(-1.3909232992639,24.3537114129877,0.));
#207535=CARTESIAN_POINT('Ctrl Pts',(-1.3909232992639,24.3537114129877,12.));
#207536=CARTESIAN_POINT('Ctrl Pts',(-1.38327786752998,24.37566137173,0.));
#207537=CARTESIAN_POINT('Ctrl Pts',(-1.38327786752998,24.37566137173,12.));
#207538=CARTESIAN_POINT('Ctrl Pts',(-1.37554790111608,24.3976773824731,
0.));
#207539=CARTESIAN_POINT('Ctrl Pts',(-1.37554790111608,24.3976773824731,
12.));
#207540=CARTESIAN_POINT('Ctrl Pts',(-1.36773329659954,24.4197587598337,
0.));
#207541=CARTESIAN_POINT('Ctrl Pts',(-1.36773329659954,24.4197587598337,
12.));
#207542=CARTESIAN_POINT('Ctrl Pts',(-1.35983395290624,24.4419048244524,
0.));
#207543=CARTESIAN_POINT('Ctrl Pts',(-1.35983395290624,24.4419048244524,
12.));
#207544=CARTESIAN_POINT('Ctrl Pts',(-1.35184977125645,24.4641149028894,
0.));
#207545=CARTESIAN_POINT('Ctrl Pts',(-1.35184977125645,24.4641149028894,
12.));
#207546=CARTESIAN_POINT('Ctrl Pts',(-1.34378065512335,24.4863883275135,
0.));
#207547=CARTESIAN_POINT('Ctrl Pts',(-1.34378065512335,24.4863883275135,
12.));
#207548=CARTESIAN_POINT('Ctrl Pts',(-1.33562651019684,24.5087244363856,
0.));
#207549=CARTESIAN_POINT('Ctrl Pts',(-1.33562651019684,24.5087244363856,
12.));
#207550=CARTESIAN_POINT('Ctrl Pts',(-1.32738724435326,24.5311225731434,
0.));
#207551=CARTESIAN_POINT('Ctrl Pts',(-1.32738724435326,24.5311225731434,
12.));
#207552=CARTESIAN_POINT('Ctrl Pts',(-1.31906276763669,24.5535820868671,
0.));
#207553=CARTESIAN_POINT('Ctrl Pts',(-1.31906276763669,24.5535820868671,
12.));
#207554=CARTESIAN_POINT('Ctrl Pts',(-1.31065299222023,24.576102332018,0.));
#207555=CARTESIAN_POINT('Ctrl Pts',(-1.31065299222023,24.576102332018,12.));
#207556=CARTESIAN_POINT('Ctrl Pts',(-1.30215783236364,24.5986826684025,
0.));
#207557=CARTESIAN_POINT('Ctrl Pts',(-1.30215783236364,24.5986826684025,
12.));
#207558=CARTESIAN_POINT('Ctrl Pts',(-1.29357720438108,24.6213224611228,
0.));
#207559=CARTESIAN_POINT('Ctrl Pts',(-1.29357720438108,24.6213224611228,
12.));
#207560=CARTESIAN_POINT('Ctrl Pts',(-1.28491102661514,24.6440210805278,
0.));
#207561=CARTESIAN_POINT('Ctrl Pts',(-1.28491102661514,24.6440210805278,
12.));
#207562=CARTESIAN_POINT('Ctrl Pts',(-1.2761592194164,24.666777902156,0.));
#207563=CARTESIAN_POINT('Ctrl Pts',(-1.2761592194164,24.666777902156,12.));
#207564=CARTESIAN_POINT('Ctrl Pts',(-1.26732170513497,24.6895923066837,
0.));
#207565=CARTESIAN_POINT('Ctrl Pts',(-1.26732170513497,24.6895923066837,
12.));
#207566=CARTESIAN_POINT('Ctrl Pts',(-1.25839840807415,24.7124636797895,
0.));
#207567=CARTESIAN_POINT('Ctrl Pts',(-1.25839840807415,24.7124636797895,
12.));
#207568=CARTESIAN_POINT('Ctrl Pts',(-1.24938925444324,24.7353914120012,
0.));
#207569=CARTESIAN_POINT('Ctrl Pts',(-1.24938925444324,24.7353914120012,
12.));
#207570=CARTESIAN_POINT('Ctrl Pts',(-1.24029417231988,24.7583748985439,
0.));
#207571=CARTESIAN_POINT('Ctrl Pts',(-1.24029417231988,24.7583748985439,
12.));
#207572=CARTESIAN_POINT('Ctrl Pts',(-1.23111309161843,24.78141353918,0.));
#207573=CARTESIAN_POINT('Ctrl Pts',(-1.23111309161843,24.78141353918,12.));
#207574=CARTESIAN_POINT('Ctrl Pts',(-1.22184594406526,24.8045067380536,
0.));
#207575=CARTESIAN_POINT('Ctrl Pts',(-1.22184594406526,24.8045067380536,
12.));
#207576=CARTESIAN_POINT('Ctrl Pts',(-1.21249266318205,24.8276539035092,
0.));
#207577=CARTESIAN_POINT('Ctrl Pts',(-1.21249266318205,24.8276539035092,
12.));
#207578=CARTESIAN_POINT('Ctrl Pts',(-1.20305318426015,24.8508544481973,
0.));
#207579=CARTESIAN_POINT('Ctrl Pts',(-1.20305318426015,24.8508544481973,
12.));
#207580=CARTESIAN_POINT('Ctrl Pts',(-1.19352744434059,24.8741077892074,
0.));
#207581=CARTESIAN_POINT('Ctrl Pts',(-1.19352744434059,24.8741077892074,
12.));
#207582=CARTESIAN_POINT('Ctrl Pts',(-1.18391538220098,24.8974133481829,
0.));
#207583=CARTESIAN_POINT('Ctrl Pts',(-1.18391538220098,24.8974133481829,
12.));
#207584=CARTESIAN_POINT('Ctrl Pts',(-1.17421693835039,24.9207705514449,
0.));
#207585=CARTESIAN_POINT('Ctrl Pts',(-1.17421693835039,24.9207705514449,
12.));
#207586=CARTESIAN_POINT('Ctrl Pts',(-1.16443205502852,24.9441788300932,
0.));
#207587=CARTESIAN_POINT('Ctrl Pts',(-1.16443205502852,24.9441788300932,
12.));
#207588=CARTESIAN_POINT('Ctrl Pts',(-1.15456067621894,24.9676376201501,
0.));
#207589=CARTESIAN_POINT('Ctrl Pts',(-1.15456067621894,24.9676376201501,
12.));
#207590=CARTESIAN_POINT('Ctrl Pts',(-1.14460274758206,24.9911463621431,
0.));
#207591=CARTESIAN_POINT('Ctrl Pts',(-1.14460274758206,24.9911463621431,
12.));
#207592=CARTESIAN_POINT('Ctrl Pts',(-1.13455821638536,25.0147045006193,
0.));
#207593=CARTESIAN_POINT('Ctrl Pts',(-1.13455821638536,25.0147045006193,
12.));
#207594=CARTESIAN_POINT('Ctrl Pts',(-1.12442703144455,25.0383114836898,
0.));
#207595=CARTESIAN_POINT('Ctrl Pts',(-1.12442703144455,25.0383114836898,
12.));
#207596=CARTESIAN_POINT('Ctrl Pts',(-1.1142091430689,25.0619667625336,0.));
#207597=CARTESIAN_POINT('Ctrl Pts',(-1.1142091430689,25.0619667625336,12.));
#207598=CARTESIAN_POINT('Ctrl Pts',(-1.1039045030174,25.085669790968,0.));
#207599=CARTESIAN_POINT('Ctrl Pts',(-1.1039045030174,25.085669790968,12.));
#207600=CARTESIAN_POINT('Ctrl Pts',(-1.09351306445299,25.1094200248448,
0.));
#207601=CARTESIAN_POINT('Ctrl Pts',(-1.09351306445299,25.1094200248448,
12.));
#207602=CARTESIAN_POINT('Ctrl Pts',(-1.08303478197174,25.1332169227415,
0.));
#207603=CARTESIAN_POINT('Ctrl Pts',(-1.08303478197174,25.1332169227415,
12.));
#207604=CARTESIAN_POINT('Ctrl Pts',(-1.0724696116546,25.1570599469311,0.));
#207605=CARTESIAN_POINT('Ctrl Pts',(-1.0724696116546,25.1570599469311,12.));
#207606=CARTESIAN_POINT('Ctrl Pts',(-1.06181751111754,25.1809485642191,
0.));
#207607=CARTESIAN_POINT('Ctrl Pts',(-1.06181751111754,25.1809485642191,
12.));
#207608=CARTESIAN_POINT('Ctrl Pts',(-1.05107843957926,25.2048822469027,
0.));
#207609=CARTESIAN_POINT('Ctrl Pts',(-1.05107843957926,25.2048822469027,
12.));
#207610=CARTESIAN_POINT('Ctrl Pts',(-1.04025235791515,25.2288604735087,
0.));
#207611=CARTESIAN_POINT('Ctrl Pts',(-1.04025235791515,25.2288604735087,
12.));
#207612=CARTESIAN_POINT('Ctrl Pts',(-1.0293392287683,25.2528827300427,0.));
#207613=CARTESIAN_POINT('Ctrl Pts',(-1.0293392287683,25.2528827300427,12.));
#207614=CARTESIAN_POINT('Ctrl Pts',(-1.01833901642272,25.2769485087268,
0.));
#207615=CARTESIAN_POINT('Ctrl Pts',(-1.01833901642272,25.2769485087268,
12.));
#207616=CARTESIAN_POINT('Ctrl Pts',(-1.00725168656934,25.3010573055557,
0.));
#207617=CARTESIAN_POINT('Ctrl Pts',(-1.00725168656934,25.3010573055557,
12.));
#207618=CARTESIAN_POINT('Ctrl Pts',(-0.99607720612092,25.3252086182976,
0.));
#207619=CARTESIAN_POINT('Ctrl Pts',(-0.99607720612092,25.3252086182976,
12.));
#207620=CARTESIAN_POINT('Ctrl Pts',(-0.984815543004092,25.3494019441444,
0.));
#207621=CARTESIAN_POINT('Ctrl Pts',(-0.984815543004092,25.3494019441444,
12.));
#207622=CARTESIAN_POINT('Ctrl Pts',(-0.973466666000049,25.3736367778842,
0.));
#207623=CARTESIAN_POINT('Ctrl Pts',(-0.973466666000049,25.3736367778842,
12.));
#207624=CARTESIAN_POINT('Ctrl Pts',(-0.962030544502803,25.3979126089155,
0.));
#207625=CARTESIAN_POINT('Ctrl Pts',(-0.962030544502803,25.3979126089155,
12.));
#207626=CARTESIAN_POINT('Ctrl Pts',(-0.95050714859697,25.4222289223155,
0.));
#207627=CARTESIAN_POINT('Ctrl Pts',(-0.95050714859697,25.4222289223155,
12.));
#207628=CARTESIAN_POINT('Ctrl Pts',(-0.938896449495633,25.4465852044835,
0.));
#207629=CARTESIAN_POINT('Ctrl Pts',(-0.938896449495633,25.4465852044835,
12.));
#207630=CARTESIAN_POINT('Ctrl Pts',(-0.927198419885605,25.4709809474996,
0.));
#207631=CARTESIAN_POINT('Ctrl Pts',(-0.927198419885605,25.4709809474996,
12.));
#207632=CARTESIAN_POINT('Ctrl Pts',(-0.915413034335334,25.4954156541787,
0.));
#207633=CARTESIAN_POINT('Ctrl Pts',(-0.915413034335334,25.4954156541787,
12.));
#207634=CARTESIAN_POINT('Ctrl Pts',(-0.903540269651155,25.5198888424195,
0.));
#207635=CARTESIAN_POINT('Ctrl Pts',(-0.903540269651155,25.5198888424195,
12.));
#207636=CARTESIAN_POINT('Ctrl Pts',(-0.891580105349468,25.5444000508223,
0.));
#207637=CARTESIAN_POINT('Ctrl Pts',(-0.891580105349468,25.5444000508223,
12.));
#207638=CARTESIAN_POINT('Ctrl Pts',(-0.879532523835092,25.568948840818,
0.));
#207639=CARTESIAN_POINT('Ctrl Pts',(-0.879532523835092,25.568948840818,
12.));
#207640=CARTESIAN_POINT('Ctrl Pts',(-0.86739750933947,25.5935347843616,
0.));
#207641=CARTESIAN_POINT('Ctrl Pts',(-0.86739750933947,25.5935347843616,
12.));
#207642=CARTESIAN_POINT('Ctrl Pts',(-0.855175047037615,25.618157453608,
0.));
#207643=CARTESIAN_POINT('Ctrl Pts',(-0.855175047037615,25.618157453608,
12.));
#207644=CARTESIAN_POINT('Ctrl Pts',(-0.842865122121547,25.6428164100078,
0.));
#207645=CARTESIAN_POINT('Ctrl Pts',(-0.842865122121547,25.6428164100078,
12.));
#207646=CARTESIAN_POINT('Ctrl Pts',(-0.830467718864369,25.6675111931957,
0.));
#207647=CARTESIAN_POINT('Ctrl Pts',(-0.830467718864369,25.6675111931957,
12.));
#207648=CARTESIAN_POINT('Ctrl Pts',(-0.81798281978672,25.6922413110172,
0.));
#207649=CARTESIAN_POINT('Ctrl Pts',(-0.81798281978672,25.6922413110172,
12.));
#207650=CARTESIAN_POINT('Ctrl Pts',(-0.805410404552596,25.7170062262474,
0.));
#207651=CARTESIAN_POINT('Ctrl Pts',(-0.805410404552596,25.7170062262474,
12.));
#207652=CARTESIAN_POINT('Ctrl Pts',(-0.792750451613536,25.7418053757671,
0.));
#207653=CARTESIAN_POINT('Ctrl Pts',(-0.792750451613536,25.7418053757671,
12.));
#207654=CARTESIAN_POINT('Ctrl Pts',(-0.780002940289027,25.7666381946871,
0.));
#207655=CARTESIAN_POINT('Ctrl Pts',(-0.780002940289027,25.7666381946871,
12.));
#207656=CARTESIAN_POINT('Ctrl Pts',(-0.767167852648641,25.7915041383304,
0.));
#207657=CARTESIAN_POINT('Ctrl Pts',(-0.767167852648641,25.7915041383304,
12.));
#207658=CARTESIAN_POINT('Ctrl Pts',(-0.75424517560829,25.816402705995,0.));
#207659=CARTESIAN_POINT('Ctrl Pts',(-0.75424517560829,25.816402705995,12.));
#207660=CARTESIAN_POINT('Ctrl Pts',(-0.741234902664698,25.841333461908,
0.));
#207661=CARTESIAN_POINT('Ctrl Pts',(-0.741234902664698,25.841333461908,
12.));
#207662=CARTESIAN_POINT('Ctrl Pts',(-0.728137036485879,25.8662960624285,
0.));
#207663=CARTESIAN_POINT('Ctrl Pts',(-0.728137036485879,25.8662960624285,
12.));
#207664=CARTESIAN_POINT('Ctrl Pts',(-0.714951588533753,25.8912902615141,
0.));
#207665=CARTESIAN_POINT('Ctrl Pts',(-0.714951588533753,25.8912902615141,
12.));
#207666=CARTESIAN_POINT('Ctrl Pts',(-0.701678575236603,25.9163158909645,
0.));
#207667=CARTESIAN_POINT('Ctrl Pts',(-0.701678575236603,25.9163158909645,
12.));
#207668=CARTESIAN_POINT('Ctrl Pts',(-0.688318015065679,25.941372847213,
0.));
#207669=CARTESIAN_POINT('Ctrl Pts',(-0.688318015065679,25.941372847213,
12.));
#207670=CARTESIAN_POINT('Ctrl Pts',(-0.677559543215903,25.9614434298092,
0.));
#207671=CARTESIAN_POINT('Ctrl Pts',(-0.677559543215903,25.9614434298092,
12.));
#207672=CARTESIAN_POINT('Ctrl Pts',(-0.669451306784418,25.9765104298171,
0.));
#207673=CARTESIAN_POINT('Ctrl Pts',(-0.669451306784418,25.9765104298171,
12.));
#207674=CARTESIAN_POINT('Ctrl Pts',(-0.664028313188914,25.9865613464809,
0.));
#207675=CARTESIAN_POINT('Ctrl Pts',(-0.664028313188914,25.9865613464809,
12.));
#207676=CARTESIAN_POINT('Ctrl Pts',(-0.661312440730891,25.991588367311,
0.));
#207677=CARTESIAN_POINT('Ctrl Pts',(-0.661312440730891,25.991588367311,
12.));
#207678=CARTESIAN_POINT('',(-0.661312440730891,25.991588367311,0.));
#207679=CARTESIAN_POINT('Ctrl Pts',(-1.76341220531179,22.4835757167854,
0.));
#207680=CARTESIAN_POINT('Ctrl Pts',(-1.76341415538764,22.483581992979,0.));
#207681=CARTESIAN_POINT('Ctrl Pts',(-1.7634206426357,22.4836387052232,0.));
#207682=CARTESIAN_POINT('Ctrl Pts',(-1.76343813434565,22.483856251707,0.));
#207683=CARTESIAN_POINT('Ctrl Pts',(-1.76347698284792,22.4844112933129,
0.));
#207684=CARTESIAN_POINT('Ctrl Pts',(-1.76355076045546,22.4855446605991,
0.));
#207685=CARTESIAN_POINT('Ctrl Pts',(-1.76364784232963,22.4871115206571,
0.));
#207686=CARTESIAN_POINT('Ctrl Pts',(-1.76376424879505,22.4890991659478,
0.));
#207687=CARTESIAN_POINT('Ctrl Pts',(-1.76389475965724,22.4914909094908,
0.));
#207688=CARTESIAN_POINT('Ctrl Pts',(-1.76403393880301,22.4942693792449,
0.));
#207689=CARTESIAN_POINT('Ctrl Pts',(-1.76417731243462,22.4974203063191,
0.));
#207690=CARTESIAN_POINT('Ctrl Pts',(-1.76432160068725,22.5009332677316,
0.));
#207691=CARTESIAN_POINT('Ctrl Pts',(-1.76446408210366,22.5047996391978,
0.));
#207692=CARTESIAN_POINT('Ctrl Pts',(-1.76460218257323,22.5090112700212,
0.));
#207693=CARTESIAN_POINT('Ctrl Pts',(-1.76473303281159,22.5135590569554,
0.));
#207694=CARTESIAN_POINT('Ctrl Pts',(-1.76485369319896,22.5184336670207,
0.));
#207695=CARTESIAN_POINT('Ctrl Pts',(-1.76496128643369,22.5236259635515,
0.));
#207696=CARTESIAN_POINT('Ctrl Pts',(-1.76505320262752,22.529127665298,0.));
#207697=CARTESIAN_POINT('Ctrl Pts',(-1.7651271156325,22.5349313983571,0.));
#207698=CARTESIAN_POINT('Ctrl Pts',(-1.76518087841493,22.5410303590891,
0.));
#207699=CARTESIAN_POINT('Ctrl Pts',(-1.76521245524047,22.5474180954006,
0.));
#207700=CARTESIAN_POINT('Ctrl Pts',(-1.76521983384063,22.5540882235837,
0.));
#207701=CARTESIAN_POINT('Ctrl Pts',(-1.76520104500449,22.5610344912501,
0.));
#207702=CARTESIAN_POINT('Ctrl Pts',(-1.76515418518829,22.5682508499873,
0.));
#207703=CARTESIAN_POINT('Ctrl Pts',(-1.76507744026747,22.5757315316355,
0.));
#207704=CARTESIAN_POINT('Ctrl Pts',(-1.76496910283088,22.5834711038024,
0.));
#207705=CARTESIAN_POINT('Ctrl Pts',(-1.76482755288411,22.5914644078106,
0.));
#207706=CARTESIAN_POINT('Ctrl Pts',(-1.76465124413556,22.5997065145638,
0.));
#207707=CARTESIAN_POINT('Ctrl Pts',(-1.76443868648015,22.6081926681342,
0.));
#207708=CARTESIAN_POINT('Ctrl Pts',(-1.76418843543739,22.6169182517693,
0.));
#207709=CARTESIAN_POINT('Ctrl Pts',(-1.76389909571402,22.6258787994847,
0.));
#207710=CARTESIAN_POINT('Ctrl Pts',(-1.76356932176272,22.635069997936,0.));
#207711=CARTESIAN_POINT('Ctrl Pts',(-1.76319782013914,22.6444876940425,
0.));
#207712=CARTESIAN_POINT('Ctrl Pts',(-1.76278334912559,22.6541278938413,
0.));
#207713=CARTESIAN_POINT('Ctrl Pts',(-1.76232471392567,22.6639867471756,
0.));
#207714=CARTESIAN_POINT('Ctrl Pts',(-1.76182076289525,22.6740605356699,
0.));
#207715=CARTESIAN_POINT('Ctrl Pts',(-1.76127038310613,22.6843456585245,
0.));
#207716=CARTESIAN_POINT('Ctrl Pts',(-1.76067249704884,22.6948386219843,
0.));
#207717=CARTESIAN_POINT('Ctrl Pts',(-1.76002606202399,22.7055360375481,
0.));
#207718=CARTESIAN_POINT('Ctrl Pts',(-1.75933006905924,22.7164346186007,
0.));
#207719=CARTESIAN_POINT('Ctrl Pts',(-1.75858354204635,22.7275311777305,
0.));
#207720=CARTESIAN_POINT('Ctrl Pts',(-1.75778553673249,22.7388226235565,
0.));
#207721=CARTESIAN_POINT('Ctrl Pts',(-1.75693513908911,22.7503059556455,
0.));
#207722=CARTESIAN_POINT('Ctrl Pts',(-1.7560314637164,22.7619782595013,0.));
#207723=CARTESIAN_POINT('Ctrl Pts',(-1.75507365227127,22.7738367016115,
0.));
#207724=CARTESIAN_POINT('Ctrl Pts',(-1.7540608718293,22.7858785242358,0.));
#207725=CARTESIAN_POINT('Ctrl Pts',(-1.75299231391461,22.7981010424312,
0.));
#207726=CARTESIAN_POINT('Ctrl Pts',(-1.7518671936559,22.8105016414712,0.));
#207727=CARTESIAN_POINT('Ctrl Pts',(-1.75068474890884,22.8230777741285,
0.));
#207728=CARTESIAN_POINT('Ctrl Pts',(-1.74944423940117,22.8358269579854,
0.));
#207729=CARTESIAN_POINT('Ctrl Pts',(-1.74814494588492,22.8487467728075,
0.));
#207730=CARTESIAN_POINT('Ctrl Pts',(-1.74678616930663,22.8618348580234,
0.));
#207731=CARTESIAN_POINT('Ctrl Pts',(-1.745367229982,22.8750889101696,0.));
#207732=CARTESIAN_POINT('Ctrl Pts',(-1.74388746677702,22.8885066803351,
0.));
#207733=CARTESIAN_POINT('Ctrl Pts',(-1.74234623630079,22.9020859716144,
0.));
#207734=CARTESIAN_POINT('Ctrl Pts',(-1.74074291231057,22.9158246373365,
0.));
#207735=CARTESIAN_POINT('Ctrl Pts',(-1.73907688511664,22.9297205792587,
0.));
#207736=CARTESIAN_POINT('Ctrl Pts',(-1.73734756100038,22.9437717457825,
0.));
#207737=CARTESIAN_POINT('Ctrl Pts',(-1.73555436162771,22.9579761301062,
0.));
#207738=CARTESIAN_POINT('Ctrl Pts',(-1.73369672350818,22.9723317685688,
0.));
#207739=CARTESIAN_POINT('Ctrl Pts',(-1.73177409750194,22.9868367391978,
0.));
#207740=CARTESIAN_POINT('Ctrl Pts',(-1.72978594832137,23.0014891601891,
0.));
#207741=CARTESIAN_POINT('Ctrl Pts',(-1.72773175404703,23.0162871884167,
0.));
#207742=CARTESIAN_POINT('Ctrl Pts',(-1.72561100564033,23.031229017888,0.));
#207743=CARTESIAN_POINT('Ctrl Pts',(-1.72342320653731,23.0463128785528,
0.));
#207744=CARTESIAN_POINT('Ctrl Pts',(-1.7211678722598,23.061537035156,0.));
#207745=CARTESIAN_POINT('Ctrl Pts',(-1.71884453003027,23.0768997860709,
0.));
#207746=CARTESIAN_POINT('Ctrl Pts',(-1.71645271839311,23.0923994621216,
0.));
#207747=CARTESIAN_POINT('Ctrl Pts',(-1.71399198684725,23.1080344254291,
0.));
#207748=CARTESIAN_POINT('Ctrl Pts',(-1.71146189552192,23.1238030684929,
0.));
#207749=CARTESIAN_POINT('Ctrl Pts',(-1.7088620148546,23.1397038132358,0.));
#207750=CARTESIAN_POINT('Ctrl Pts',(-1.70619192527847,23.1557351100613,
0.));
#207751=CARTESIAN_POINT('Ctrl Pts',(-1.70345121691259,23.1718954368749,
0.));
#207752=CARTESIAN_POINT('Ctrl Pts',(-1.70063948926987,23.1881832981848,
0.));
#207753=CARTESIAN_POINT('Ctrl Pts',(-1.69775635099425,23.2045972243765,
0.));
#207754=CARTESIAN_POINT('Ctrl Pts',(-1.69480141959946,23.2211357709374,
0.));
#207755=CARTESIAN_POINT('Ctrl Pts',(-1.69177432121716,23.2377975177014,
0.));
#207756=CARTESIAN_POINT('Ctrl Pts',(-1.6886746903491,23.2545810680536,0.));
#207757=CARTESIAN_POINT('Ctrl Pts',(-1.68550216963275,23.2714850482245,
0.));
#207758=CARTESIAN_POINT('Ctrl Pts',(-1.68225640962181,23.2885081066949,
0.));
#207759=CARTESIAN_POINT('Ctrl Pts',(-1.67893706857123,23.3056489135611,
0.));
#207760=CARTESIAN_POINT('Ctrl Pts',(-1.67554381222987,23.3229061599145,
0.));
#207761=CARTESIAN_POINT('Ctrl Pts',(-1.67207631363905,23.3402785571866,
0.));
#207762=CARTESIAN_POINT('Ctrl Pts',(-1.66853425293978,23.3577648365747,
0.));
#207763=CARTESIAN_POINT('Ctrl Pts',(-1.66491731718864,23.375363748555,0.));
#207764=CARTESIAN_POINT('Ctrl Pts',(-1.66122520018008,23.3930740623622,
0.));
#207765=CARTESIAN_POINT('Ctrl Pts',(-1.65745760227507,23.4108945654803,
0.));
#207766=CARTESIAN_POINT('Ctrl Pts',(-1.6536142302373,23.4288240631034,0.));
#207767=CARTESIAN_POINT('Ctrl Pts',(-1.6496947970734,23.446861377656,0.));
#207768=CARTESIAN_POINT('Ctrl Pts',(-1.64569902187608,23.4650053483919,
0.));
#207769=CARTESIAN_POINT('Ctrl Pts',(-1.64162662967525,23.4832548309638,
0.));
#207770=CARTESIAN_POINT('Ctrl Pts',(-1.63747735129474,23.5016086970006,
0.));
#207771=CARTESIAN_POINT('Ctrl Pts',(-1.63325092321731,23.5200658336624,
0.));
#207772=CARTESIAN_POINT('Ctrl Pts',(-1.62894708745231,23.5386251432278,
0.));
#207773=CARTESIAN_POINT('Ctrl Pts',(-1.62456559140072,23.5572855427617,
0.));
#207774=CARTESIAN_POINT('Ctrl Pts',(-1.62010618772869,23.5760459637608,
0.));
#207775=CARTESIAN_POINT('Ctrl Pts',(-1.61556863424697,23.5949053517996,
0.));
#207776=CARTESIAN_POINT('Ctrl Pts',(-1.61095269379773,23.6138626661644,
0.));
#207777=CARTESIAN_POINT('Ctrl Pts',(-1.60625813414666,23.6329168794916,
0.));
#207778=CARTESIAN_POINT('Ctrl Pts',(-1.60148472786588,23.6520669774863,
0.));
#207779=CARTESIAN_POINT('Ctrl Pts',(-1.59663225222458,23.6713119586302,
0.));
#207780=CARTESIAN_POINT('Ctrl Pts',(-1.59170048908632,23.6906508338833,
0.));
#207781=CARTESIAN_POINT('Ctrl Pts',(-1.58668922481222,23.7100826263835,
0.));
#207782=CARTESIAN_POINT('Ctrl Pts',(-1.58159825017362,23.7296063711308,
0.));
#207783=CARTESIAN_POINT('Ctrl Pts',(-1.57642736025251,23.7492211147369,
0.));
#207784=CARTESIAN_POINT('Ctrl Pts',(-1.57117635434412,23.7689259151869,
0.));
#207785=CARTESIAN_POINT('Ctrl Pts',(-1.56584503586844,23.788719841588,0.));
#207786=CARTESIAN_POINT('Ctrl Pts',(-1.56043321228631,23.8086019739192,
0.));
#207787=CARTESIAN_POINT('Ctrl Pts',(-1.55494069502628,23.8285714027631,
0.));
#207788=CARTESIAN_POINT('Ctrl Pts',(-1.5493672994053,23.8486272290698,0.));
#207789=CARTESIAN_POINT('Ctrl Pts',(-1.54371284453978,23.8687685639635,
0.));
#207790=CARTESIAN_POINT('Ctrl Pts',(-1.53797715326748,23.8889945285313,
0.));
#207791=CARTESIAN_POINT('Ctrl Pts',(-1.53216005207462,23.9093042536119,
0.));
#207792=CARTESIAN_POINT('Ctrl Pts',(-1.5262613710304,23.9296968795761,0.));
#207793=CARTESIAN_POINT('Ctrl Pts',(-1.52028094372806,23.9501715561038,
0.));
#207794=CARTESIAN_POINT('Ctrl Pts',(-1.51421860720628,23.9707274420145,
0.));
#207795=CARTESIAN_POINT('Ctrl Pts',(-1.50807420187703,23.991363705093,0.));
#207796=CARTESIAN_POINT('Ctrl Pts',(-1.50184757146099,24.0120795219086,
0.));
#207797=CARTESIAN_POINT('Ctrl Pts',(-1.49553856292798,24.0328740776331,
0.));
#207798=CARTESIAN_POINT('Ctrl Pts',(-1.48914702644883,24.053746565843,0.));
#207799=CARTESIAN_POINT('Ctrl Pts',(-1.4826728153368,24.074696188353,0.));
#207800=CARTESIAN_POINT('Ctrl Pts',(-1.47611578597741,24.0957221550782,
0.));
#207801=CARTESIAN_POINT('Ctrl Pts',(-1.46947579776992,24.1168236838827,
0.));
#207802=CARTESIAN_POINT('Ctrl Pts',(-1.46275271307398,24.1380000004272,
0.));
#207803=CARTESIAN_POINT('Ctrl Pts',(-1.45594639716314,24.1592503380105,
0.));
#207804=CARTESIAN_POINT('Ctrl Pts',(-1.44905671818721,24.1805739374033,
0.));
#207805=CARTESIAN_POINT('Ctrl Pts',(-1.44208354711074,24.2019700467214,
0.));
#207806=CARTESIAN_POINT('Ctrl Pts',(-1.43502675765502,24.2234379212978,
0.));
#207807=CARTESIAN_POINT('Ctrl Pts',(-1.42788622624851,24.2449768235485,
0.));
#207808=CARTESIAN_POINT('Ctrl Pts',(-1.42066183198252,24.2665860228357,
0.));
#207809=CARTESIAN_POINT('Ctrl Pts',(-1.41335345657685,24.2882647953214,
0.));
#207810=CARTESIAN_POINT('Ctrl Pts',(-1.40596098434341,24.3100124238316,
0.));
#207811=CARTESIAN_POINT('Ctrl Pts',(-1.3984843021281,24.3318281977647,0.));
#207812=CARTESIAN_POINT('Ctrl Pts',(-1.3909232992639,24.3537114129877,0.));
#207813=CARTESIAN_POINT('Ctrl Pts',(-1.38327786752998,24.37566137173,0.));
#207814=CARTESIAN_POINT('Ctrl Pts',(-1.37554790111608,24.3976773824731,
0.));
#207815=CARTESIAN_POINT('Ctrl Pts',(-1.36773329659954,24.4197587598337,
0.));
#207816=CARTESIAN_POINT('Ctrl Pts',(-1.35983395290624,24.4419048244524,
0.));
#207817=CARTESIAN_POINT('Ctrl Pts',(-1.35184977125645,24.4641149028894,
0.));
#207818=CARTESIAN_POINT('Ctrl Pts',(-1.34378065512335,24.4863883275135,
0.));
#207819=CARTESIAN_POINT('Ctrl Pts',(-1.33562651019684,24.5087244363856,
0.));
#207820=CARTESIAN_POINT('Ctrl Pts',(-1.32738724435326,24.5311225731434,
0.));
#207821=CARTESIAN_POINT('Ctrl Pts',(-1.31906276763669,24.5535820868671,
0.));
#207822=CARTESIAN_POINT('Ctrl Pts',(-1.31065299222023,24.576102332018,0.));
#207823=CARTESIAN_POINT('Ctrl Pts',(-1.30215783236364,24.5986826684025,
0.));
#207824=CARTESIAN_POINT('Ctrl Pts',(-1.29357720438108,24.6213224611228,
0.));
#207825=CARTESIAN_POINT('Ctrl Pts',(-1.28491102661514,24.6440210805278,
0.));
#207826=CARTESIAN_POINT('Ctrl Pts',(-1.2761592194164,24.666777902156,0.));
#207827=CARTESIAN_POINT('Ctrl Pts',(-1.26732170513497,24.6895923066837,
0.));
#207828=CARTESIAN_POINT('Ctrl Pts',(-1.25839840807415,24.7124636797895,
0.));
#207829=CARTESIAN_POINT('Ctrl Pts',(-1.24938925444324,24.7353914120012,
0.));
#207830=CARTESIAN_POINT('Ctrl Pts',(-1.24029417231988,24.7583748985439,
0.));
#207831=CARTESIAN_POINT('Ctrl Pts',(-1.23111309161843,24.78141353918,0.));
#207832=CARTESIAN_POINT('Ctrl Pts',(-1.22184594406526,24.8045067380536,
0.));
#207833=CARTESIAN_POINT('Ctrl Pts',(-1.21249266318205,24.8276539035092,
0.));
#207834=CARTESIAN_POINT('Ctrl Pts',(-1.20305318426015,24.8508544481973,
0.));
#207835=CARTESIAN_POINT('Ctrl Pts',(-1.19352744434059,24.8741077892074,
0.));
#207836=CARTESIAN_POINT('Ctrl Pts',(-1.18391538220098,24.8974133481829,
0.));
#207837=CARTESIAN_POINT('Ctrl Pts',(-1.17421693835039,24.9207705514449,
0.));
#207838=CARTESIAN_POINT('Ctrl Pts',(-1.16443205502852,24.9441788300932,
0.));
#207839=CARTESIAN_POINT('Ctrl Pts',(-1.15456067621894,24.9676376201501,
0.));
#207840=CARTESIAN_POINT('Ctrl Pts',(-1.14460274758206,24.9911463621431,
0.));
#207841=CARTESIAN_POINT('Ctrl Pts',(-1.13455821638536,25.0147045006193,
0.));
#207842=CARTESIAN_POINT('Ctrl Pts',(-1.12442703144455,25.0383114836898,
0.));
#207843=CARTESIAN_POINT('Ctrl Pts',(-1.1142091430689,25.0619667625336,0.));
#207844=CARTESIAN_POINT('Ctrl Pts',(-1.1039045030174,25.085669790968,0.));
#207845=CARTESIAN_POINT('Ctrl Pts',(-1.09351306445299,25.1094200248448,
0.));
#207846=CARTESIAN_POINT('Ctrl Pts',(-1.08303478197174,25.1332169227415,
0.));
#207847=CARTESIAN_POINT('Ctrl Pts',(-1.0724696116546,25.1570599469311,0.));
#207848=CARTESIAN_POINT('Ctrl Pts',(-1.06181751111754,25.1809485642191,
0.));
#207849=CARTESIAN_POINT('Ctrl Pts',(-1.05107843957926,25.2048822469027,
0.));
#207850=CARTESIAN_POINT('Ctrl Pts',(-1.04025235791515,25.2288604735087,
0.));
#207851=CARTESIAN_POINT('Ctrl Pts',(-1.0293392287683,25.2528827300427,0.));
#207852=CARTESIAN_POINT('Ctrl Pts',(-1.01833901642272,25.2769485087268,
0.));
#207853=CARTESIAN_POINT('Ctrl Pts',(-1.00725168656934,25.3010573055557,
0.));
#207854=CARTESIAN_POINT('Ctrl Pts',(-0.99607720612092,25.3252086182976,
0.));
#207855=CARTESIAN_POINT('Ctrl Pts',(-0.984815543004092,25.3494019441444,
0.));
#207856=CARTESIAN_POINT('Ctrl Pts',(-0.973466666000049,25.3736367778842,
0.));
#207857=CARTESIAN_POINT('Ctrl Pts',(-0.962030544502803,25.3979126089155,
0.));
#207858=CARTESIAN_POINT('Ctrl Pts',(-0.95050714859697,25.4222289223155,
0.));
#207859=CARTESIAN_POINT('Ctrl Pts',(-0.938896449495633,25.4465852044835,
0.));
#207860=CARTESIAN_POINT('Ctrl Pts',(-0.927198419885605,25.4709809474996,
0.));
#207861=CARTESIAN_POINT('Ctrl Pts',(-0.915413034335334,25.4954156541787,
0.));
#207862=CARTESIAN_POINT('Ctrl Pts',(-0.903540269651155,25.5198888424195,
0.));
#207863=CARTESIAN_POINT('Ctrl Pts',(-0.891580105349468,25.5444000508223,
0.));
#207864=CARTESIAN_POINT('Ctrl Pts',(-0.879532523835092,25.568948840818,
0.));
#207865=CARTESIAN_POINT('Ctrl Pts',(-0.86739750933947,25.5935347843616,
0.));
#207866=CARTESIAN_POINT('Ctrl Pts',(-0.855175047037615,25.618157453608,
0.));
#207867=CARTESIAN_POINT('Ctrl Pts',(-0.842865122121547,25.6428164100078,
0.));
#207868=CARTESIAN_POINT('Ctrl Pts',(-0.830467718864369,25.6675111931957,
0.));
#207869=CARTESIAN_POINT('Ctrl Pts',(-0.81798281978672,25.6922413110172,
0.));
#207870=CARTESIAN_POINT('Ctrl Pts',(-0.805410404552596,25.7170062262474,
0.));
#207871=CARTESIAN_POINT('Ctrl Pts',(-0.792750451613536,25.7418053757671,
0.));
#207872=CARTESIAN_POINT('Ctrl Pts',(-0.780002940289027,25.7666381946871,
0.));
#207873=CARTESIAN_POINT('Ctrl Pts',(-0.767167852648641,25.7915041383304,
0.));
#207874=CARTESIAN_POINT('Ctrl Pts',(-0.75424517560829,25.816402705995,0.));
#207875=CARTESIAN_POINT('Ctrl Pts',(-0.741234902664698,25.841333461908,
0.));
#207876=CARTESIAN_POINT('Ctrl Pts',(-0.728137036485879,25.8662960624285,
0.));
#207877=CARTESIAN_POINT('Ctrl Pts',(-0.714951588533753,25.8912902615141,
0.));
#207878=CARTESIAN_POINT('Ctrl Pts',(-0.701678575236603,25.9163158909645,
0.));
#207879=CARTESIAN_POINT('Ctrl Pts',(-0.688318015065679,25.941372847213,
0.));
#207880=CARTESIAN_POINT('Ctrl Pts',(-0.677559543215903,25.9614434298092,
0.));
#207881=CARTESIAN_POINT('Ctrl Pts',(-0.669451306784418,25.9765104298171,
0.));
#207882=CARTESIAN_POINT('Ctrl Pts',(-0.664028313188914,25.9865613464809,
0.));
#207883=CARTESIAN_POINT('Ctrl Pts',(-0.661312440730891,25.991588367311,
0.));
#207884=CARTESIAN_POINT('',(-0.661312440730891,25.991588367311,0.));
#207885=CARTESIAN_POINT('Origin',(3.92374859571501,21.1389261070099,0.));
#207886=CARTESIAN_POINT('',(4.11585220600461,22.1738711152697,0.));
#207887=CARTESIAN_POINT('',(4.11585220600461,22.1738711152697,0.));
#207888=CARTESIAN_POINT('',(1.96187429785751,10.5694630535049,0.));
#207889=CARTESIAN_POINT('Ctrl Pts',(0.661312440730901,25.991588367311,0.));
#207890=CARTESIAN_POINT('Ctrl Pts',(0.661312440730901,25.991588367311,12.));
#207891=CARTESIAN_POINT('Ctrl Pts',(0.664028313187627,25.9865613464773,
0.));
#207892=CARTESIAN_POINT('Ctrl Pts',(0.664028313187627,25.9865613464773,
12.));
#207893=CARTESIAN_POINT('Ctrl Pts',(0.669451306780825,25.9765104298071,
0.));
#207894=CARTESIAN_POINT('Ctrl Pts',(0.669451306780825,25.9765104298071,
12.));
#207895=CARTESIAN_POINT('Ctrl Pts',(0.677559543209725,25.9614434297919,
0.));
#207896=CARTESIAN_POINT('Ctrl Pts',(0.677559543209725,25.9614434297919,
12.));
#207897=CARTESIAN_POINT('Ctrl Pts',(0.688318015057729,25.9413728471909,
0.));
#207898=CARTESIAN_POINT('Ctrl Pts',(0.688318015057729,25.9413728471909,
12.));
#207899=CARTESIAN_POINT('Ctrl Pts',(0.701678575228756,25.9163158909426,
0.));
#207900=CARTESIAN_POINT('Ctrl Pts',(0.701678575228756,25.9163158909426,
12.));
#207901=CARTESIAN_POINT('Ctrl Pts',(0.714951588527638,25.891290261497,0.));
#207902=CARTESIAN_POINT('Ctrl Pts',(0.714951588527638,25.891290261497,12.));
#207903=CARTESIAN_POINT('Ctrl Pts',(0.728137036482335,25.8662960624185,
0.));
#207904=CARTESIAN_POINT('Ctrl Pts',(0.728137036482335,25.8662960624185,
12.));
#207905=CARTESIAN_POINT('Ctrl Pts',(0.741234902663807,25.8413334619055,
0.));
#207906=CARTESIAN_POINT('Ctrl Pts',(0.741234902663807,25.8413334619055,
12.));
#207907=CARTESIAN_POINT('Ctrl Pts',(0.754245175609524,25.8164027059984,
0.));
#207908=CARTESIAN_POINT('Ctrl Pts',(0.754245175609524,25.8164027059984,
12.));
#207909=CARTESIAN_POINT('Ctrl Pts',(0.767167852651168,25.7915041383376,
0.));
#207910=CARTESIAN_POINT('Ctrl Pts',(0.767167852651168,25.7915041383376,
12.));
#207911=CARTESIAN_POINT('Ctrl Pts',(0.780002940291965,25.7666381946955,
0.));
#207912=CARTESIAN_POINT('Ctrl Pts',(0.780002940291965,25.7666381946955,
12.));
#207913=CARTESIAN_POINT('Ctrl Pts',(0.792750451616127,25.7418053757746,
0.));
#207914=CARTESIAN_POINT('Ctrl Pts',(0.792750451616127,25.7418053757746,
12.));
#207915=CARTESIAN_POINT('Ctrl Pts',(0.805410404554352,25.7170062262525,
0.));
#207916=CARTESIAN_POINT('Ctrl Pts',(0.805410404554352,25.7170062262525,
12.));
#207917=CARTESIAN_POINT('Ctrl Pts',(0.817982819787464,25.6922413110194,
0.));
#207918=CARTESIAN_POINT('Ctrl Pts',(0.817982819787464,25.6922413110194,
12.));
#207919=CARTESIAN_POINT('Ctrl Pts',(0.830467718864205,25.6675111931952,
0.));
#207920=CARTESIAN_POINT('Ctrl Pts',(0.830467718864205,25.6675111931952,
12.));
#207921=CARTESIAN_POINT('Ctrl Pts',(0.842865122120758,25.6428164100055,
0.));
#207922=CARTESIAN_POINT('Ctrl Pts',(0.842865122120758,25.6428164100055,
12.));
#207923=CARTESIAN_POINT('Ctrl Pts',(0.855175047036549,25.6181574536049,
0.));
#207924=CARTESIAN_POINT('Ctrl Pts',(0.855175047036549,25.6181574536049,
12.));
#207925=CARTESIAN_POINT('Ctrl Pts',(0.867397509338431,25.5935347843585,
0.));
#207926=CARTESIAN_POINT('Ctrl Pts',(0.867397509338431,25.5935347843585,
12.));
#207927=CARTESIAN_POINT('Ctrl Pts',(0.879532523834294,25.5689488408156,
0.));
#207928=CARTESIAN_POINT('Ctrl Pts',(0.879532523834294,25.5689488408156,
12.));
#207929=CARTESIAN_POINT('Ctrl Pts',(0.89158010534904,25.5444000508211,0.));
#207930=CARTESIAN_POINT('Ctrl Pts',(0.89158010534904,25.5444000508211,12.));
#207931=CARTESIAN_POINT('Ctrl Pts',(0.903540269651106,25.5198888424194,
0.));
#207932=CARTESIAN_POINT('Ctrl Pts',(0.903540269651106,25.5198888424194,
12.));
#207933=CARTESIAN_POINT('Ctrl Pts',(0.915413034335613,25.4954156541795,
0.));
#207934=CARTESIAN_POINT('Ctrl Pts',(0.915413034335613,25.4954156541795,
12.));
#207935=CARTESIAN_POINT('Ctrl Pts',(0.927198419886094,25.4709809475009,
0.));
#207936=CARTESIAN_POINT('Ctrl Pts',(0.927198419886094,25.4709809475009,
12.));
#207937=CARTESIAN_POINT('Ctrl Pts',(0.938896449496192,25.4465852044849,
0.));
#207938=CARTESIAN_POINT('Ctrl Pts',(0.938896449496192,25.4465852044849,
12.));
#207939=CARTESIAN_POINT('Ctrl Pts',(0.950507148597468,25.4222289223167,
0.));
#207940=CARTESIAN_POINT('Ctrl Pts',(0.950507148597468,25.4222289223167,
12.));
#207941=CARTESIAN_POINT('Ctrl Pts',(0.962030544503142,25.3979126089163,
0.));
#207942=CARTESIAN_POINT('Ctrl Pts',(0.962030544503142,25.3979126089163,
12.));
#207943=CARTESIAN_POINT('Ctrl Pts',(0.973466666000163,25.3736367778845,
0.));
#207944=CARTESIAN_POINT('Ctrl Pts',(0.973466666000163,25.3736367778845,
12.));
#207945=CARTESIAN_POINT('Ctrl Pts',(0.984815543003973,25.3494019441441,
0.));
#207946=CARTESIAN_POINT('Ctrl Pts',(0.984815543003973,25.3494019441441,
12.));
#207947=CARTESIAN_POINT('Ctrl Pts',(0.996077206120624,25.3252086182968,
0.));
#207948=CARTESIAN_POINT('Ctrl Pts',(0.996077206120624,25.3252086182968,
12.));
#207949=CARTESIAN_POINT('Ctrl Pts',(1.00725168656896,25.3010573055547,0.));
#207950=CARTESIAN_POINT('Ctrl Pts',(1.00725168656896,25.3010573055547,12.));
#207951=CARTESIAN_POINT('Ctrl Pts',(1.01833901642237,25.276948508726,0.));
#207952=CARTESIAN_POINT('Ctrl Pts',(1.01833901642237,25.276948508726,12.));
#207953=CARTESIAN_POINT('Ctrl Pts',(1.02933922876806,25.2528827300422,0.));
#207954=CARTESIAN_POINT('Ctrl Pts',(1.02933922876806,25.2528827300422,12.));
#207955=CARTESIAN_POINT('Ctrl Pts',(1.04025235791507,25.2288604735086,0.));
#207956=CARTESIAN_POINT('Ctrl Pts',(1.04025235791507,25.2288604735086,12.));
#207957=CARTESIAN_POINT('Ctrl Pts',(1.05107843957931,25.2048822469028,0.));
#207958=CARTESIAN_POINT('Ctrl Pts',(1.05107843957931,25.2048822469028,12.));
#207959=CARTESIAN_POINT('Ctrl Pts',(1.06181751111768,25.1809485642192,0.));
#207960=CARTESIAN_POINT('Ctrl Pts',(1.06181751111768,25.1809485642192,12.));
#207961=CARTESIAN_POINT('Ctrl Pts',(1.07246961165475,25.157059946931,0.));
#207962=CARTESIAN_POINT('Ctrl Pts',(1.07246961165475,25.157059946931,12.));
#207963=CARTESIAN_POINT('Ctrl Pts',(1.08303478197187,25.1332169227413,0.));
#207964=CARTESIAN_POINT('Ctrl Pts',(1.08303478197187,25.1332169227413,12.));
#207965=CARTESIAN_POINT('Ctrl Pts',(1.09351306445308,25.1094200248446,0.));
#207966=CARTESIAN_POINT('Ctrl Pts',(1.09351306445308,25.1094200248446,12.));
#207967=CARTESIAN_POINT('Ctrl Pts',(1.10390450301745,25.0856697909679,0.));
#207968=CARTESIAN_POINT('Ctrl Pts',(1.10390450301745,25.0856697909679,12.));
#207969=CARTESIAN_POINT('Ctrl Pts',(1.11420914306889,25.0619667625336,0.));
#207970=CARTESIAN_POINT('Ctrl Pts',(1.11420914306889,25.0619667625336,12.));
#207971=CARTESIAN_POINT('Ctrl Pts',(1.12442703144451,25.0383114836899,0.));
#207972=CARTESIAN_POINT('Ctrl Pts',(1.12442703144451,25.0383114836899,12.));
#207973=CARTESIAN_POINT('Ctrl Pts',(1.1345582163853,25.0147045006196,0.));
#207974=CARTESIAN_POINT('Ctrl Pts',(1.1345582163853,25.0147045006196,12.));
#207975=CARTESIAN_POINT('Ctrl Pts',(1.144602747582,24.9911463621433,0.));
#207976=CARTESIAN_POINT('Ctrl Pts',(1.144602747582,24.9911463621433,12.));
#207977=CARTESIAN_POINT('Ctrl Pts',(1.15456067621889,24.9676376201502,0.));
#207978=CARTESIAN_POINT('Ctrl Pts',(1.15456067621889,24.9676376201502,12.));
#207979=CARTESIAN_POINT('Ctrl Pts',(1.16443205502849,24.9441788300932,0.));
#207980=CARTESIAN_POINT('Ctrl Pts',(1.16443205502849,24.9441788300932,12.));
#207981=CARTESIAN_POINT('Ctrl Pts',(1.17421693835041,24.9207705514449,0.));
#207982=CARTESIAN_POINT('Ctrl Pts',(1.17421693835041,24.9207705514449,12.));
#207983=CARTESIAN_POINT('Ctrl Pts',(1.18391538220103,24.8974133481829,0.));
#207984=CARTESIAN_POINT('Ctrl Pts',(1.18391538220103,24.8974133481829,12.));
#207985=CARTESIAN_POINT('Ctrl Pts',(1.19352744434064,24.8741077892075,0.));
#207986=CARTESIAN_POINT('Ctrl Pts',(1.19352744434064,24.8741077892075,12.));
#207987=CARTESIAN_POINT('Ctrl Pts',(1.2030531842602,24.8508544481974,0.));
#207988=CARTESIAN_POINT('Ctrl Pts',(1.2030531842602,24.8508544481974,12.));
#207989=CARTESIAN_POINT('Ctrl Pts',(1.21249266318208,24.8276539035092,0.));
#207990=CARTESIAN_POINT('Ctrl Pts',(1.21249266318208,24.8276539035092,12.));
#207991=CARTESIAN_POINT('Ctrl Pts',(1.22184594406528,24.8045067380536,0.));
#207992=CARTESIAN_POINT('Ctrl Pts',(1.22184594406528,24.8045067380536,12.));
#207993=CARTESIAN_POINT('Ctrl Pts',(1.23111309161843,24.7814135391799,0.));
#207994=CARTESIAN_POINT('Ctrl Pts',(1.23111309161843,24.7814135391799,12.));
#207995=CARTESIAN_POINT('Ctrl Pts',(1.24029417231989,24.7583748985438,0.));
#207996=CARTESIAN_POINT('Ctrl Pts',(1.24029417231989,24.7583748985438,12.));
#207997=CARTESIAN_POINT('Ctrl Pts',(1.24938925444325,24.7353914120011,0.));
#207998=CARTESIAN_POINT('Ctrl Pts',(1.24938925444325,24.7353914120011,12.));
#207999=CARTESIAN_POINT('Ctrl Pts',(1.25839840807418,24.7124636797894,0.));
#208000=CARTESIAN_POINT('Ctrl Pts',(1.25839840807418,24.7124636797894,12.));
#208001=CARTESIAN_POINT('Ctrl Pts',(1.267321705135,24.6895923066836,0.));
#208002=CARTESIAN_POINT('Ctrl Pts',(1.267321705135,24.6895923066836,12.));
#208003=CARTESIAN_POINT('Ctrl Pts',(1.27615921941642,24.666777902156,0.));
#208004=CARTESIAN_POINT('Ctrl Pts',(1.27615921941642,24.666777902156,12.));
#208005=CARTESIAN_POINT('Ctrl Pts',(1.28491102661514,24.6440210805278,0.));
#208006=CARTESIAN_POINT('Ctrl Pts',(1.28491102661514,24.6440210805278,12.));
#208007=CARTESIAN_POINT('Ctrl Pts',(1.29357720438107,24.6213224611229,0.));
#208008=CARTESIAN_POINT('Ctrl Pts',(1.29357720438107,24.6213224611229,12.));
#208009=CARTESIAN_POINT('Ctrl Pts',(1.30215783236362,24.5986826684027,0.));
#208010=CARTESIAN_POINT('Ctrl Pts',(1.30215783236362,24.5986826684027,12.));
#208011=CARTESIAN_POINT('Ctrl Pts',(1.31065299222021,24.5761023320183,0.));
#208012=CARTESIAN_POINT('Ctrl Pts',(1.31065299222021,24.5761023320183,12.));
#208013=CARTESIAN_POINT('Ctrl Pts',(1.31906276763668,24.5535820868674,0.));
#208014=CARTESIAN_POINT('Ctrl Pts',(1.31906276763668,24.5535820868674,12.));
#208015=CARTESIAN_POINT('Ctrl Pts',(1.32738724435326,24.5311225731435,0.));
#208016=CARTESIAN_POINT('Ctrl Pts',(1.32738724435326,24.5311225731435,12.));
#208017=CARTESIAN_POINT('Ctrl Pts',(1.33562651019686,24.5087244363856,0.));
#208018=CARTESIAN_POINT('Ctrl Pts',(1.33562651019686,24.5087244363856,12.));
#208019=CARTESIAN_POINT('Ctrl Pts',(1.34378065512337,24.4863883275134,0.));
#208020=CARTESIAN_POINT('Ctrl Pts',(1.34378065512337,24.4863883275134,12.));
#208021=CARTESIAN_POINT('Ctrl Pts',(1.35184977125648,24.4641149028892,0.));
#208022=CARTESIAN_POINT('Ctrl Pts',(1.35184977125648,24.4641149028892,12.));
#208023=CARTESIAN_POINT('Ctrl Pts',(1.35983395290627,24.4419048244523,0.));
#208024=CARTESIAN_POINT('Ctrl Pts',(1.35983395290627,24.4419048244523,12.));
#208025=CARTESIAN_POINT('Ctrl Pts',(1.36773329659956,24.4197587598337,0.));
#208026=CARTESIAN_POINT('Ctrl Pts',(1.36773329659956,24.4197587598337,12.));
#208027=CARTESIAN_POINT('Ctrl Pts',(1.37554790111609,24.3976773824732,0.));
#208028=CARTESIAN_POINT('Ctrl Pts',(1.37554790111609,24.3976773824732,12.));
#208029=CARTESIAN_POINT('Ctrl Pts',(1.38327786752998,24.3756613717299,0.));
#208030=CARTESIAN_POINT('Ctrl Pts',(1.38327786752998,24.3756613717299,12.));
#208031=CARTESIAN_POINT('Ctrl Pts',(1.39092329926388,24.3537114129875,0.));
#208032=CARTESIAN_POINT('Ctrl Pts',(1.39092329926388,24.3537114129875,12.));
#208033=CARTESIAN_POINT('Ctrl Pts',(1.39848430212807,24.3318281977643,0.));
#208034=CARTESIAN_POINT('Ctrl Pts',(1.39848430212807,24.3318281977643,12.));
#208035=CARTESIAN_POINT('Ctrl Pts',(1.40596098434337,24.3100124238311,0.));
#208036=CARTESIAN_POINT('Ctrl Pts',(1.40596098434337,24.3100124238311,12.));
#208037=CARTESIAN_POINT('Ctrl Pts',(1.41335345657682,24.288264795321,0.));
#208038=CARTESIAN_POINT('Ctrl Pts',(1.41335345657682,24.288264795321,12.));
#208039=CARTESIAN_POINT('Ctrl Pts',(1.42066183198252,24.2665860228356,0.));
#208040=CARTESIAN_POINT('Ctrl Pts',(1.42066183198252,24.2665860228356,12.));
#208041=CARTESIAN_POINT('Ctrl Pts',(1.42788622624854,24.2449768235488,0.));
#208042=CARTESIAN_POINT('Ctrl Pts',(1.42788622624854,24.2449768235488,12.));
#208043=CARTESIAN_POINT('Ctrl Pts',(1.43502675765508,24.2234379212984,0.));
#208044=CARTESIAN_POINT('Ctrl Pts',(1.43502675765508,24.2234379212984,12.));
#208045=CARTESIAN_POINT('Ctrl Pts',(1.44208354711082,24.201970046722,0.));
#208046=CARTESIAN_POINT('Ctrl Pts',(1.44208354711082,24.201970046722,12.));
#208047=CARTESIAN_POINT('Ctrl Pts',(1.44905671818727,24.1805739374038,0.));
#208048=CARTESIAN_POINT('Ctrl Pts',(1.44905671818727,24.1805739374038,12.));
#208049=CARTESIAN_POINT('Ctrl Pts',(1.45594639716317,24.1592503380107,0.));
#208050=CARTESIAN_POINT('Ctrl Pts',(1.45594639716317,24.1592503380107,12.));
#208051=CARTESIAN_POINT('Ctrl Pts',(1.46275271307397,24.1380000004272,0.));
#208052=CARTESIAN_POINT('Ctrl Pts',(1.46275271307397,24.1380000004272,12.));
#208053=CARTESIAN_POINT('Ctrl Pts',(1.46947579776991,24.1168236838824,0.));
#208054=CARTESIAN_POINT('Ctrl Pts',(1.46947579776991,24.1168236838824,12.));
#208055=CARTESIAN_POINT('Ctrl Pts',(1.47611578597742,24.0957221550778,0.));
#208056=CARTESIAN_POINT('Ctrl Pts',(1.47611578597742,24.0957221550778,12.));
#208057=CARTESIAN_POINT('Ctrl Pts',(1.48267281533683,24.0746961883528,0.));
#208058=CARTESIAN_POINT('Ctrl Pts',(1.48267281533683,24.0746961883528,12.));
#208059=CARTESIAN_POINT('Ctrl Pts',(1.48914702644887,24.0537465658429,0.));
#208060=CARTESIAN_POINT('Ctrl Pts',(1.48914702644887,24.0537465658429,12.));
#208061=CARTESIAN_POINT('Ctrl Pts',(1.49553856292801,24.0328740776331,0.));
#208062=CARTESIAN_POINT('Ctrl Pts',(1.49553856292801,24.0328740776331,12.));
#208063=CARTESIAN_POINT('Ctrl Pts',(1.50184757146098,24.0120795219086,0.));
#208064=CARTESIAN_POINT('Ctrl Pts',(1.50184757146098,24.0120795219086,12.));
#208065=CARTESIAN_POINT('Ctrl Pts',(1.50807420187694,23.9913637050927,0.));
#208066=CARTESIAN_POINT('Ctrl Pts',(1.50807420187694,23.9913637050927,12.));
#208067=CARTESIAN_POINT('Ctrl Pts',(1.51421860720614,23.970727442014,0.));
#208068=CARTESIAN_POINT('Ctrl Pts',(1.51421860720614,23.970727442014,12.));
#208069=CARTESIAN_POINT('Ctrl Pts',(1.52028094372792,23.9501715561033,0.));
#208070=CARTESIAN_POINT('Ctrl Pts',(1.52028094372792,23.9501715561033,12.));
#208071=CARTESIAN_POINT('Ctrl Pts',(1.52626137103032,23.9296968795757,0.));
#208072=CARTESIAN_POINT('Ctrl Pts',(1.52626137103032,23.9296968795757,12.));
#208073=CARTESIAN_POINT('Ctrl Pts',(1.53216005207463,23.9093042536119,0.));
#208074=CARTESIAN_POINT('Ctrl Pts',(1.53216005207463,23.9093042536119,12.));
#208075=CARTESIAN_POINT('Ctrl Pts',(1.53797715326758,23.8889945285318,0.));
#208076=CARTESIAN_POINT('Ctrl Pts',(1.53797715326758,23.8889945285318,12.));
#208077=CARTESIAN_POINT('Ctrl Pts',(1.5437128445399,23.8687685639642,0.));
#208078=CARTESIAN_POINT('Ctrl Pts',(1.5437128445399,23.8687685639642,12.));
#208079=CARTESIAN_POINT('Ctrl Pts',(1.54936729940541,23.8486272290705,0.));
#208080=CARTESIAN_POINT('Ctrl Pts',(1.54936729940541,23.8486272290705,12.));
#208081=CARTESIAN_POINT('Ctrl Pts',(1.55494069502635,23.8285714027636,0.));
#208082=CARTESIAN_POINT('Ctrl Pts',(1.55494069502635,23.8285714027636,12.));
#208083=CARTESIAN_POINT('Ctrl Pts',(1.56043321228633,23.8086019739194,0.));
#208084=CARTESIAN_POINT('Ctrl Pts',(1.56043321228633,23.8086019739194,12.));
#208085=CARTESIAN_POINT('Ctrl Pts',(1.56584503586843,23.7887198415878,0.));
#208086=CARTESIAN_POINT('Ctrl Pts',(1.56584503586843,23.7887198415878,12.));
#208087=CARTESIAN_POINT('Ctrl Pts',(1.57117635434408,23.7689259151862,0.));
#208088=CARTESIAN_POINT('Ctrl Pts',(1.57117635434408,23.7689259151862,12.));
#208089=CARTESIAN_POINT('Ctrl Pts',(1.57642736025246,23.749221114736,0.));
#208090=CARTESIAN_POINT('Ctrl Pts',(1.57642736025246,23.749221114736,12.));
#208091=CARTESIAN_POINT('Ctrl Pts',(1.58159825017358,23.72960637113,0.));
#208092=CARTESIAN_POINT('Ctrl Pts',(1.58159825017358,23.72960637113,12.));
#208093=CARTESIAN_POINT('Ctrl Pts',(1.58668922481221,23.710082626383,0.));
#208094=CARTESIAN_POINT('Ctrl Pts',(1.58668922481221,23.710082626383,12.));
#208095=CARTESIAN_POINT('Ctrl Pts',(1.59170048908633,23.6906508338833,0.));
#208096=CARTESIAN_POINT('Ctrl Pts',(1.59170048908633,23.6906508338833,12.));
#208097=CARTESIAN_POINT('Ctrl Pts',(1.59663225222463,23.671311958631,0.));
#208098=CARTESIAN_POINT('Ctrl Pts',(1.59663225222463,23.671311958631,12.));
#208099=CARTESIAN_POINT('Ctrl Pts',(1.60148472786595,23.6520669774876,0.));
#208100=CARTESIAN_POINT('Ctrl Pts',(1.60148472786595,23.6520669774876,12.));
#208101=CARTESIAN_POINT('Ctrl Pts',(1.60625813414672,23.6329168794929,0.));
#208102=CARTESIAN_POINT('Ctrl Pts',(1.60625813414672,23.6329168794929,12.));
#208103=CARTESIAN_POINT('Ctrl Pts',(1.61095269379778,23.6138626661653,0.));
#208104=CARTESIAN_POINT('Ctrl Pts',(1.61095269379778,23.6138626661653,12.));
#208105=CARTESIAN_POINT('Ctrl Pts',(1.61556863424698,23.5949053517997,0.));
#208106=CARTESIAN_POINT('Ctrl Pts',(1.61556863424698,23.5949053517997,12.));
#208107=CARTESIAN_POINT('Ctrl Pts',(1.62010618772866,23.57604596376,0.));
#208108=CARTESIAN_POINT('Ctrl Pts',(1.62010618772866,23.57604596376,12.));
#208109=CARTESIAN_POINT('Ctrl Pts',(1.62456559140064,23.5572855427601,0.));
#208110=CARTESIAN_POINT('Ctrl Pts',(1.62456559140064,23.5572855427601,12.));
#208111=CARTESIAN_POINT('Ctrl Pts',(1.62894708745223,23.538625143226,0.));
#208112=CARTESIAN_POINT('Ctrl Pts',(1.62894708745223,23.538625143226,12.));
#208113=CARTESIAN_POINT('Ctrl Pts',(1.63325092321725,23.5200658336612,0.));
#208114=CARTESIAN_POINT('Ctrl Pts',(1.63325092321725,23.5200658336612,12.));
#208115=CARTESIAN_POINT('Ctrl Pts',(1.63747735129474,23.5016086970003,0.));
#208116=CARTESIAN_POINT('Ctrl Pts',(1.63747735129474,23.5016086970003,12.));
#208117=CARTESIAN_POINT('Ctrl Pts',(1.64162662967528,23.4832548309645,0.));
#208118=CARTESIAN_POINT('Ctrl Pts',(1.64162662967528,23.4832548309645,12.));
#208119=CARTESIAN_POINT('Ctrl Pts',(1.64569902187611,23.4650053483932,0.));
#208120=CARTESIAN_POINT('Ctrl Pts',(1.64569902187611,23.4650053483932,12.));
#208121=CARTESIAN_POINT('Ctrl Pts',(1.6496947970734,23.4468613776574,0.));
#208122=CARTESIAN_POINT('Ctrl Pts',(1.6496947970734,23.4468613776574,12.));
#208123=CARTESIAN_POINT('Ctrl Pts',(1.65361423023728,23.4288240631043,0.));
#208124=CARTESIAN_POINT('Ctrl Pts',(1.65361423023728,23.4288240631043,12.));
#208125=CARTESIAN_POINT('Ctrl Pts',(1.65745760227505,23.4108945654805,0.));
#208126=CARTESIAN_POINT('Ctrl Pts',(1.65745760227505,23.4108945654805,12.));
#208127=CARTESIAN_POINT('Ctrl Pts',(1.66122520018011,23.3930740623619,0.));
#208128=CARTESIAN_POINT('Ctrl Pts',(1.66122520018011,23.3930740623619,12.));
#208129=CARTESIAN_POINT('Ctrl Pts',(1.66491731718876,23.3753637485545,0.));
#208130=CARTESIAN_POINT('Ctrl Pts',(1.66491731718876,23.3753637485545,12.));
#208131=CARTESIAN_POINT('Ctrl Pts',(1.66853425293995,23.3577648365744,0.));
#208132=CARTESIAN_POINT('Ctrl Pts',(1.66853425293995,23.3577648365744,12.));
#208133=CARTESIAN_POINT('Ctrl Pts',(1.67207631363921,23.3402785571865,0.));
#208134=CARTESIAN_POINT('Ctrl Pts',(1.67207631363921,23.3402785571865,12.));
#208135=CARTESIAN_POINT('Ctrl Pts',(1.67554381222994,23.3229061599145,0.));
#208136=CARTESIAN_POINT('Ctrl Pts',(1.67554381222994,23.3229061599145,12.));
#208137=CARTESIAN_POINT('Ctrl Pts',(1.67893706857117,23.3056489135611,0.));
#208138=CARTESIAN_POINT('Ctrl Pts',(1.67893706857117,23.3056489135611,12.));
#208139=CARTESIAN_POINT('Ctrl Pts',(1.68225640962168,23.2885081066951,0.));
#208140=CARTESIAN_POINT('Ctrl Pts',(1.68225640962168,23.2885081066951,12.));
#208141=CARTESIAN_POINT('Ctrl Pts',(1.68550216963258,23.2714850482246,0.));
#208142=CARTESIAN_POINT('Ctrl Pts',(1.68550216963258,23.2714850482246,12.));
#208143=CARTESIAN_POINT('Ctrl Pts',(1.68867469034896,23.2545810680537,0.));
#208144=CARTESIAN_POINT('Ctrl Pts',(1.68867469034896,23.2545810680537,12.));
#208145=CARTESIAN_POINT('Ctrl Pts',(1.69177432121711,23.2377975177013,0.));
#208146=CARTESIAN_POINT('Ctrl Pts',(1.69177432121711,23.2377975177013,12.));
#208147=CARTESIAN_POINT('Ctrl Pts',(1.69480141959953,23.2211357709374,0.));
#208148=CARTESIAN_POINT('Ctrl Pts',(1.69480141959953,23.2211357709374,12.));
#208149=CARTESIAN_POINT('Ctrl Pts',(1.69775635099443,23.2045972243767,0.));
#208150=CARTESIAN_POINT('Ctrl Pts',(1.69775635099443,23.2045972243767,12.));
#208151=CARTESIAN_POINT('Ctrl Pts',(1.7006394892701,23.1881832981851,0.));
#208152=CARTESIAN_POINT('Ctrl Pts',(1.7006394892701,23.1881832981851,12.));
#208153=CARTESIAN_POINT('Ctrl Pts',(1.70345121691276,23.1718954368751,0.));
#208154=CARTESIAN_POINT('Ctrl Pts',(1.70345121691276,23.1718954368751,12.));
#208155=CARTESIAN_POINT('Ctrl Pts',(1.70619192527852,23.1557351100614,0.));
#208156=CARTESIAN_POINT('Ctrl Pts',(1.70619192527852,23.1557351100614,12.));
#208157=CARTESIAN_POINT('Ctrl Pts',(1.70886201485452,23.1397038132356,0.));
#208158=CARTESIAN_POINT('Ctrl Pts',(1.70886201485452,23.1397038132356,12.));
#208159=CARTESIAN_POINT('Ctrl Pts',(1.71146189552174,23.1238030684925,0.));
#208160=CARTESIAN_POINT('Ctrl Pts',(1.71146189552174,23.1238030684925,12.));
#208161=CARTESIAN_POINT('Ctrl Pts',(1.71399198684704,23.1080344254286,0.));
#208162=CARTESIAN_POINT('Ctrl Pts',(1.71399198684704,23.1080344254286,12.));
#208163=CARTESIAN_POINT('Ctrl Pts',(1.71645271839296,23.0923994621213,0.));
#208164=CARTESIAN_POINT('Ctrl Pts',(1.71645271839296,23.0923994621213,12.));
#208165=CARTESIAN_POINT('Ctrl Pts',(1.71884453003027,23.0768997860709,0.));
#208166=CARTESIAN_POINT('Ctrl Pts',(1.71884453003027,23.0768997860709,12.));
#208167=CARTESIAN_POINT('Ctrl Pts',(1.72116787225991,23.0615370351562,0.));
#208168=CARTESIAN_POINT('Ctrl Pts',(1.72116787225991,23.0615370351562,12.));
#208169=CARTESIAN_POINT('Ctrl Pts',(1.72342320653746,23.0463128785531,0.));
#208170=CARTESIAN_POINT('Ctrl Pts',(1.72342320653746,23.0463128785531,12.));
#208171=CARTESIAN_POINT('Ctrl Pts',(1.72561100564045,23.0312290178883,0.));
#208172=CARTESIAN_POINT('Ctrl Pts',(1.72561100564045,23.0312290178883,12.));
#208173=CARTESIAN_POINT('Ctrl Pts',(1.72773175404708,23.0162871884168,0.));
#208174=CARTESIAN_POINT('Ctrl Pts',(1.72773175404708,23.0162871884168,12.));
#208175=CARTESIAN_POINT('Ctrl Pts',(1.72978594832136,23.001489160189,0.));
#208176=CARTESIAN_POINT('Ctrl Pts',(1.72978594832136,23.001489160189,12.));
#208177=CARTESIAN_POINT('Ctrl Pts',(1.7317740975019,22.9868367391978,0.));
#208178=CARTESIAN_POINT('Ctrl Pts',(1.7317740975019,22.9868367391978,12.));
#208179=CARTESIAN_POINT('Ctrl Pts',(1.73369672350814,22.9723317685688,0.));
#208180=CARTESIAN_POINT('Ctrl Pts',(1.73369672350814,22.9723317685688,12.));
#208181=CARTESIAN_POINT('Ctrl Pts',(1.73555436162769,22.9579761301063,0.));
#208182=CARTESIAN_POINT('Ctrl Pts',(1.73555436162769,22.9579761301063,12.));
#208183=CARTESIAN_POINT('Ctrl Pts',(1.73734756100039,22.9437717457826,0.));
#208184=CARTESIAN_POINT('Ctrl Pts',(1.73734756100039,22.9437717457826,12.));
#208185=CARTESIAN_POINT('Ctrl Pts',(1.73907688511666,22.9297205792586,0.));
#208186=CARTESIAN_POINT('Ctrl Pts',(1.73907688511666,22.9297205792586,12.));
#208187=CARTESIAN_POINT('Ctrl Pts',(1.74074291231058,22.9158246373363,0.));
#208188=CARTESIAN_POINT('Ctrl Pts',(1.74074291231058,22.9158246373363,12.));
#208189=CARTESIAN_POINT('Ctrl Pts',(1.7423462363008,22.9020859716141,0.));
#208190=CARTESIAN_POINT('Ctrl Pts',(1.7423462363008,22.9020859716141,12.));
#208191=CARTESIAN_POINT('Ctrl Pts',(1.74388746677702,22.888506680335,0.));
#208192=CARTESIAN_POINT('Ctrl Pts',(1.74388746677702,22.888506680335,12.));
#208193=CARTESIAN_POINT('Ctrl Pts',(1.74536722998201,22.8750889101696,0.));
#208194=CARTESIAN_POINT('Ctrl Pts',(1.74536722998201,22.8750889101696,12.));
#208195=CARTESIAN_POINT('Ctrl Pts',(1.74678616930664,22.8618348580235,0.));
#208196=CARTESIAN_POINT('Ctrl Pts',(1.74678616930664,22.8618348580235,12.));
#208197=CARTESIAN_POINT('Ctrl Pts',(1.74814494588492,22.8487467728076,0.));
#208198=CARTESIAN_POINT('Ctrl Pts',(1.74814494588492,22.8487467728076,12.));
#208199=CARTESIAN_POINT('Ctrl Pts',(1.74944423940115,22.8358269579853,0.));
#208200=CARTESIAN_POINT('Ctrl Pts',(1.74944423940115,22.8358269579853,12.));
#208201=CARTESIAN_POINT('Ctrl Pts',(1.75068474890883,22.8230777741284,0.));
#208202=CARTESIAN_POINT('Ctrl Pts',(1.75068474890883,22.8230777741284,12.));
#208203=CARTESIAN_POINT('Ctrl Pts',(1.75186719365592,22.8105016414713,0.));
#208204=CARTESIAN_POINT('Ctrl Pts',(1.75186719365592,22.8105016414713,12.));
#208205=CARTESIAN_POINT('Ctrl Pts',(1.75299231391466,22.7981010424314,0.));
#208206=CARTESIAN_POINT('Ctrl Pts',(1.75299231391466,22.7981010424314,12.));
#208207=CARTESIAN_POINT('Ctrl Pts',(1.75406087182936,22.7858785242361,0.));
#208208=CARTESIAN_POINT('Ctrl Pts',(1.75406087182936,22.7858785242361,12.));
#208209=CARTESIAN_POINT('Ctrl Pts',(1.75507365227131,22.7738367016118,0.));
#208210=CARTESIAN_POINT('Ctrl Pts',(1.75507365227131,22.7738367016118,12.));
#208211=CARTESIAN_POINT('Ctrl Pts',(1.75603146371641,22.7619782595013,0.));
#208212=CARTESIAN_POINT('Ctrl Pts',(1.75603146371641,22.7619782595013,12.));
#208213=CARTESIAN_POINT('Ctrl Pts',(1.75693513908907,22.750305955645,0.));
#208214=CARTESIAN_POINT('Ctrl Pts',(1.75693513908907,22.750305955645,12.));
#208215=CARTESIAN_POINT('Ctrl Pts',(1.75778553673244,22.7388226235559,0.));
#208216=CARTESIAN_POINT('Ctrl Pts',(1.75778553673244,22.7388226235559,12.));
#208217=CARTESIAN_POINT('Ctrl Pts',(1.75858354204633,22.72753117773,0.));
#208218=CARTESIAN_POINT('Ctrl Pts',(1.75858354204633,22.72753117773,12.));
#208219=CARTESIAN_POINT('Ctrl Pts',(1.75933006905925,22.7164346186006,0.));
#208220=CARTESIAN_POINT('Ctrl Pts',(1.75933006905925,22.7164346186006,12.));
#208221=CARTESIAN_POINT('Ctrl Pts',(1.76002606202401,22.7055360375485,0.));
#208222=CARTESIAN_POINT('Ctrl Pts',(1.76002606202401,22.7055360375485,12.));
#208223=CARTESIAN_POINT('Ctrl Pts',(1.76067249704886,22.6948386219851,0.));
#208224=CARTESIAN_POINT('Ctrl Pts',(1.76067249704886,22.6948386219851,12.));
#208225=CARTESIAN_POINT('Ctrl Pts',(1.76127038310614,22.684345658525,0.));
#208226=CARTESIAN_POINT('Ctrl Pts',(1.76127038310614,22.684345658525,12.));
#208227=CARTESIAN_POINT('Ctrl Pts',(1.76182076289525,22.67406053567,0.));
#208228=CARTESIAN_POINT('Ctrl Pts',(1.76182076289525,22.67406053567,12.));
#208229=CARTESIAN_POINT('Ctrl Pts',(1.76232471392568,22.6639867471753,0.));
#208230=CARTESIAN_POINT('Ctrl Pts',(1.76232471392568,22.6639867471753,12.));
#208231=CARTESIAN_POINT('Ctrl Pts',(1.76278334912561,22.6541278938409,0.));
#208232=CARTESIAN_POINT('Ctrl Pts',(1.76278334912561,22.6541278938409,12.));
#208233=CARTESIAN_POINT('Ctrl Pts',(1.76319782013916,22.6444876940423,0.));
#208234=CARTESIAN_POINT('Ctrl Pts',(1.76319782013916,22.6444876940423,12.));
#208235=CARTESIAN_POINT('Ctrl Pts',(1.76356932176273,22.6350699979359,0.));
#208236=CARTESIAN_POINT('Ctrl Pts',(1.76356932176273,22.6350699979359,12.));
#208237=CARTESIAN_POINT('Ctrl Pts',(1.76389909571403,22.6258787994848,0.));
#208238=CARTESIAN_POINT('Ctrl Pts',(1.76389909571403,22.6258787994848,12.));
#208239=CARTESIAN_POINT('Ctrl Pts',(1.76418843543739,22.6169182517694,0.));
#208240=CARTESIAN_POINT('Ctrl Pts',(1.76418843543739,22.6169182517694,12.));
#208241=CARTESIAN_POINT('Ctrl Pts',(1.76443868648015,22.6081926681343,0.));
#208242=CARTESIAN_POINT('Ctrl Pts',(1.76443868648015,22.6081926681343,12.));
#208243=CARTESIAN_POINT('Ctrl Pts',(1.76465124413557,22.5997065145638,0.));
#208244=CARTESIAN_POINT('Ctrl Pts',(1.76465124413557,22.5997065145638,12.));
#208245=CARTESIAN_POINT('Ctrl Pts',(1.76482755288411,22.5914644078106,0.));
#208246=CARTESIAN_POINT('Ctrl Pts',(1.76482755288411,22.5914644078106,12.));
#208247=CARTESIAN_POINT('Ctrl Pts',(1.76496910283088,22.5834711038022,0.));
#208248=CARTESIAN_POINT('Ctrl Pts',(1.76496910283088,22.5834711038022,12.));
#208249=CARTESIAN_POINT('Ctrl Pts',(1.76507744026746,22.5757315316353,0.));
#208250=CARTESIAN_POINT('Ctrl Pts',(1.76507744026746,22.5757315316353,12.));
#208251=CARTESIAN_POINT('Ctrl Pts',(1.76515418518831,22.5682508499873,0.));
#208252=CARTESIAN_POINT('Ctrl Pts',(1.76515418518831,22.5682508499873,12.));
#208253=CARTESIAN_POINT('Ctrl Pts',(1.7652010450045,22.5610344912501,0.));
#208254=CARTESIAN_POINT('Ctrl Pts',(1.7652010450045,22.5610344912501,12.));
#208255=CARTESIAN_POINT('Ctrl Pts',(1.76521983384062,22.5540882235837,0.));
#208256=CARTESIAN_POINT('Ctrl Pts',(1.76521983384062,22.5540882235837,12.));
#208257=CARTESIAN_POINT('Ctrl Pts',(1.76521245524047,22.5474180954006,0.));
#208258=CARTESIAN_POINT('Ctrl Pts',(1.76521245524047,22.5474180954006,12.));
#208259=CARTESIAN_POINT('Ctrl Pts',(1.76518087841493,22.5410303590892,0.));
#208260=CARTESIAN_POINT('Ctrl Pts',(1.76518087841493,22.5410303590892,12.));
#208261=CARTESIAN_POINT('Ctrl Pts',(1.76512711563254,22.5349313983571,0.));
#208262=CARTESIAN_POINT('Ctrl Pts',(1.76512711563254,22.5349313983571,12.));
#208263=CARTESIAN_POINT('Ctrl Pts',(1.76505320262759,22.529127665298,0.));
#208264=CARTESIAN_POINT('Ctrl Pts',(1.76505320262759,22.529127665298,12.));
#208265=CARTESIAN_POINT('Ctrl Pts',(1.76496128643375,22.5236259635515,0.));
#208266=CARTESIAN_POINT('Ctrl Pts',(1.76496128643375,22.5236259635515,12.));
#208267=CARTESIAN_POINT('Ctrl Pts',(1.76485369319895,22.5184336670207,0.));
#208268=CARTESIAN_POINT('Ctrl Pts',(1.76485369319895,22.5184336670207,12.));
#208269=CARTESIAN_POINT('Ctrl Pts',(1.76473303281149,22.5135590569554,0.));
#208270=CARTESIAN_POINT('Ctrl Pts',(1.76473303281149,22.5135590569554,12.));
#208271=CARTESIAN_POINT('Ctrl Pts',(1.76460218257313,22.5090112700212,0.));
#208272=CARTESIAN_POINT('Ctrl Pts',(1.76460218257313,22.5090112700212,12.));
#208273=CARTESIAN_POINT('Ctrl Pts',(1.76446408210364,22.5047996391978,0.));
#208274=CARTESIAN_POINT('Ctrl Pts',(1.76446408210364,22.5047996391978,12.));
#208275=CARTESIAN_POINT('Ctrl Pts',(1.76432160068737,22.5009332677316,0.));
#208276=CARTESIAN_POINT('Ctrl Pts',(1.76432160068737,22.5009332677316,12.));
#208277=CARTESIAN_POINT('Ctrl Pts',(1.76417731243483,22.4974203063191,0.));
#208278=CARTESIAN_POINT('Ctrl Pts',(1.76417731243483,22.4974203063191,12.));
#208279=CARTESIAN_POINT('Ctrl Pts',(1.76403393880316,22.4942693792449,0.));
#208280=CARTESIAN_POINT('Ctrl Pts',(1.76403393880316,22.4942693792449,12.));
#208281=CARTESIAN_POINT('Ctrl Pts',(1.76389475965714,22.4914909094908,0.));
#208282=CARTESIAN_POINT('Ctrl Pts',(1.76389475965714,22.4914909094908,12.));
#208283=CARTESIAN_POINT('Ctrl Pts',(1.76376424879468,22.4890991659479,0.));
#208284=CARTESIAN_POINT('Ctrl Pts',(1.76376424879468,22.4890991659479,12.));
#208285=CARTESIAN_POINT('Ctrl Pts',(1.76364784232925,22.4871115206572,0.));
#208286=CARTESIAN_POINT('Ctrl Pts',(1.76364784232925,22.4871115206572,12.));
#208287=CARTESIAN_POINT('Ctrl Pts',(1.76355076045549,22.4855446605991,0.));
#208288=CARTESIAN_POINT('Ctrl Pts',(1.76355076045549,22.4855446605991,12.));
#208289=CARTESIAN_POINT('Ctrl Pts',(1.76347698284861,22.4844112933125,0.));
#208290=CARTESIAN_POINT('Ctrl Pts',(1.76347698284861,22.4844112933125,12.));
#208291=CARTESIAN_POINT('Ctrl Pts',(1.76343813434659,22.4838562517064,0.));
#208292=CARTESIAN_POINT('Ctrl Pts',(1.76343813434659,22.4838562517064,12.));
#208293=CARTESIAN_POINT('Ctrl Pts',(1.76342064263637,22.4836387052228,0.));
#208294=CARTESIAN_POINT('Ctrl Pts',(1.76342064263637,22.4836387052228,12.));
#208295=CARTESIAN_POINT('Ctrl Pts',(1.7634141553879,22.4835819929788,0.));
#208296=CARTESIAN_POINT('Ctrl Pts',(1.7634141553879,22.4835819929788,12.));
#208297=CARTESIAN_POINT('Ctrl Pts',(1.7634122053118,22.4835757167854,0.));
#208298=CARTESIAN_POINT('Ctrl Pts',(1.7634122053118,22.4835757167854,12.));
#208299=CARTESIAN_POINT('',(0.661312440730901,25.991588367311,0.));
#208300=CARTESIAN_POINT('Ctrl Pts',(0.661312440730901,25.991588367311,0.));
#208301=CARTESIAN_POINT('Ctrl Pts',(0.664028313187627,25.9865613464773,
0.));
#208302=CARTESIAN_POINT('Ctrl Pts',(0.669451306780825,25.9765104298071,
0.));
#208303=CARTESIAN_POINT('Ctrl Pts',(0.677559543209725,25.9614434297919,
0.));
#208304=CARTESIAN_POINT('Ctrl Pts',(0.688318015057729,25.9413728471909,
0.));
#208305=CARTESIAN_POINT('Ctrl Pts',(0.701678575228756,25.9163158909426,
0.));
#208306=CARTESIAN_POINT('Ctrl Pts',(0.714951588527638,25.891290261497,0.));
#208307=CARTESIAN_POINT('Ctrl Pts',(0.728137036482335,25.8662960624185,
0.));
#208308=CARTESIAN_POINT('Ctrl Pts',(0.741234902663807,25.8413334619055,
0.));
#208309=CARTESIAN_POINT('Ctrl Pts',(0.754245175609524,25.8164027059984,
0.));
#208310=CARTESIAN_POINT('Ctrl Pts',(0.767167852651168,25.7915041383376,
0.));
#208311=CARTESIAN_POINT('Ctrl Pts',(0.780002940291965,25.7666381946955,
0.));
#208312=CARTESIAN_POINT('Ctrl Pts',(0.792750451616127,25.7418053757746,
0.));
#208313=CARTESIAN_POINT('Ctrl Pts',(0.805410404554352,25.7170062262525,
0.));
#208314=CARTESIAN_POINT('Ctrl Pts',(0.817982819787464,25.6922413110194,
0.));
#208315=CARTESIAN_POINT('Ctrl Pts',(0.830467718864205,25.6675111931952,
0.));
#208316=CARTESIAN_POINT('Ctrl Pts',(0.842865122120758,25.6428164100055,
0.));
#208317=CARTESIAN_POINT('Ctrl Pts',(0.855175047036549,25.6181574536049,
0.));
#208318=CARTESIAN_POINT('Ctrl Pts',(0.867397509338431,25.5935347843585,
0.));
#208319=CARTESIAN_POINT('Ctrl Pts',(0.879532523834294,25.5689488408156,
0.));
#208320=CARTESIAN_POINT('Ctrl Pts',(0.89158010534904,25.5444000508211,0.));
#208321=CARTESIAN_POINT('Ctrl Pts',(0.903540269651106,25.5198888424194,
0.));
#208322=CARTESIAN_POINT('Ctrl Pts',(0.915413034335613,25.4954156541795,
0.));
#208323=CARTESIAN_POINT('Ctrl Pts',(0.927198419886094,25.4709809475009,
0.));
#208324=CARTESIAN_POINT('Ctrl Pts',(0.938896449496192,25.4465852044849,
0.));
#208325=CARTESIAN_POINT('Ctrl Pts',(0.950507148597468,25.4222289223167,
0.));
#208326=CARTESIAN_POINT('Ctrl Pts',(0.962030544503142,25.3979126089163,
0.));
#208327=CARTESIAN_POINT('Ctrl Pts',(0.973466666000163,25.3736367778845,
0.));
#208328=CARTESIAN_POINT('Ctrl Pts',(0.984815543003973,25.3494019441441,
0.));
#208329=CARTESIAN_POINT('Ctrl Pts',(0.996077206120624,25.3252086182968,
0.));
#208330=CARTESIAN_POINT('Ctrl Pts',(1.00725168656896,25.3010573055547,0.));
#208331=CARTESIAN_POINT('Ctrl Pts',(1.01833901642237,25.276948508726,0.));
#208332=CARTESIAN_POINT('Ctrl Pts',(1.02933922876806,25.2528827300422,0.));
#208333=CARTESIAN_POINT('Ctrl Pts',(1.04025235791507,25.2288604735086,0.));
#208334=CARTESIAN_POINT('Ctrl Pts',(1.05107843957931,25.2048822469028,0.));
#208335=CARTESIAN_POINT('Ctrl Pts',(1.06181751111768,25.1809485642192,0.));
#208336=CARTESIAN_POINT('Ctrl Pts',(1.07246961165475,25.157059946931,0.));
#208337=CARTESIAN_POINT('Ctrl Pts',(1.08303478197187,25.1332169227413,0.));
#208338=CARTESIAN_POINT('Ctrl Pts',(1.09351306445308,25.1094200248446,0.));
#208339=CARTESIAN_POINT('Ctrl Pts',(1.10390450301745,25.0856697909679,0.));
#208340=CARTESIAN_POINT('Ctrl Pts',(1.11420914306889,25.0619667625336,0.));
#208341=CARTESIAN_POINT('Ctrl Pts',(1.12442703144451,25.0383114836899,0.));
#208342=CARTESIAN_POINT('Ctrl Pts',(1.1345582163853,25.0147045006196,0.));
#208343=CARTESIAN_POINT('Ctrl Pts',(1.144602747582,24.9911463621433,0.));
#208344=CARTESIAN_POINT('Ctrl Pts',(1.15456067621889,24.9676376201502,0.));
#208345=CARTESIAN_POINT('Ctrl Pts',(1.16443205502849,24.9441788300932,0.));
#208346=CARTESIAN_POINT('Ctrl Pts',(1.17421693835041,24.9207705514449,0.));
#208347=CARTESIAN_POINT('Ctrl Pts',(1.18391538220103,24.8974133481829,0.));
#208348=CARTESIAN_POINT('Ctrl Pts',(1.19352744434064,24.8741077892075,0.));
#208349=CARTESIAN_POINT('Ctrl Pts',(1.2030531842602,24.8508544481974,0.));
#208350=CARTESIAN_POINT('Ctrl Pts',(1.21249266318208,24.8276539035092,0.));
#208351=CARTESIAN_POINT('Ctrl Pts',(1.22184594406528,24.8045067380536,0.));
#208352=CARTESIAN_POINT('Ctrl Pts',(1.23111309161843,24.7814135391799,0.));
#208353=CARTESIAN_POINT('Ctrl Pts',(1.24029417231989,24.7583748985438,0.));
#208354=CARTESIAN_POINT('Ctrl Pts',(1.24938925444325,24.7353914120011,0.));
#208355=CARTESIAN_POINT('Ctrl Pts',(1.25839840807418,24.7124636797894,0.));
#208356=CARTESIAN_POINT('Ctrl Pts',(1.267321705135,24.6895923066836,0.));
#208357=CARTESIAN_POINT('Ctrl Pts',(1.27615921941642,24.666777902156,0.));
#208358=CARTESIAN_POINT('Ctrl Pts',(1.28491102661514,24.6440210805278,0.));
#208359=CARTESIAN_POINT('Ctrl Pts',(1.29357720438107,24.6213224611229,0.));
#208360=CARTESIAN_POINT('Ctrl Pts',(1.30215783236362,24.5986826684027,0.));
#208361=CARTESIAN_POINT('Ctrl Pts',(1.31065299222021,24.5761023320183,0.));
#208362=CARTESIAN_POINT('Ctrl Pts',(1.31906276763668,24.5535820868674,0.));
#208363=CARTESIAN_POINT('Ctrl Pts',(1.32738724435326,24.5311225731435,0.));
#208364=CARTESIAN_POINT('Ctrl Pts',(1.33562651019686,24.5087244363856,0.));
#208365=CARTESIAN_POINT('Ctrl Pts',(1.34378065512337,24.4863883275134,0.));
#208366=CARTESIAN_POINT('Ctrl Pts',(1.35184977125648,24.4641149028892,0.));
#208367=CARTESIAN_POINT('Ctrl Pts',(1.35983395290627,24.4419048244523,0.));
#208368=CARTESIAN_POINT('Ctrl Pts',(1.36773329659956,24.4197587598337,0.));
#208369=CARTESIAN_POINT('Ctrl Pts',(1.37554790111609,24.3976773824732,0.));
#208370=CARTESIAN_POINT('Ctrl Pts',(1.38327786752998,24.3756613717299,0.));
#208371=CARTESIAN_POINT('Ctrl Pts',(1.39092329926388,24.3537114129875,0.));
#208372=CARTESIAN_POINT('Ctrl Pts',(1.39848430212807,24.3318281977643,0.));
#208373=CARTESIAN_POINT('Ctrl Pts',(1.40596098434337,24.3100124238311,0.));
#208374=CARTESIAN_POINT('Ctrl Pts',(1.41335345657682,24.288264795321,0.));
#208375=CARTESIAN_POINT('Ctrl Pts',(1.42066183198252,24.2665860228356,0.));
#208376=CARTESIAN_POINT('Ctrl Pts',(1.42788622624854,24.2449768235488,0.));
#208377=CARTESIAN_POINT('Ctrl Pts',(1.43502675765508,24.2234379212984,0.));
#208378=CARTESIAN_POINT('Ctrl Pts',(1.44208354711082,24.201970046722,0.));
#208379=CARTESIAN_POINT('Ctrl Pts',(1.44905671818727,24.1805739374038,0.));
#208380=CARTESIAN_POINT('Ctrl Pts',(1.45594639716317,24.1592503380107,0.));
#208381=CARTESIAN_POINT('Ctrl Pts',(1.46275271307397,24.1380000004272,0.));
#208382=CARTESIAN_POINT('Ctrl Pts',(1.46947579776991,24.1168236838824,0.));
#208383=CARTESIAN_POINT('Ctrl Pts',(1.47611578597742,24.0957221550778,0.));
#208384=CARTESIAN_POINT('Ctrl Pts',(1.48267281533683,24.0746961883528,0.));
#208385=CARTESIAN_POINT('Ctrl Pts',(1.48914702644887,24.0537465658429,0.));
#208386=CARTESIAN_POINT('Ctrl Pts',(1.49553856292801,24.0328740776331,0.));
#208387=CARTESIAN_POINT('Ctrl Pts',(1.50184757146098,24.0120795219086,0.));
#208388=CARTESIAN_POINT('Ctrl Pts',(1.50807420187694,23.9913637050927,0.));
#208389=CARTESIAN_POINT('Ctrl Pts',(1.51421860720614,23.970727442014,0.));
#208390=CARTESIAN_POINT('Ctrl Pts',(1.52028094372792,23.9501715561033,0.));
#208391=CARTESIAN_POINT('Ctrl Pts',(1.52626137103032,23.9296968795757,0.));
#208392=CARTESIAN_POINT('Ctrl Pts',(1.53216005207463,23.9093042536119,0.));
#208393=CARTESIAN_POINT('Ctrl Pts',(1.53797715326758,23.8889945285318,0.));
#208394=CARTESIAN_POINT('Ctrl Pts',(1.5437128445399,23.8687685639642,0.));
#208395=CARTESIAN_POINT('Ctrl Pts',(1.54936729940541,23.8486272290705,0.));
#208396=CARTESIAN_POINT('Ctrl Pts',(1.55494069502635,23.8285714027636,0.));
#208397=CARTESIAN_POINT('Ctrl Pts',(1.56043321228633,23.8086019739194,0.));
#208398=CARTESIAN_POINT('Ctrl Pts',(1.56584503586843,23.7887198415878,0.));
#208399=CARTESIAN_POINT('Ctrl Pts',(1.57117635434408,23.7689259151862,0.));
#208400=CARTESIAN_POINT('Ctrl Pts',(1.57642736025246,23.749221114736,0.));
#208401=CARTESIAN_POINT('Ctrl Pts',(1.58159825017358,23.72960637113,0.));
#208402=CARTESIAN_POINT('Ctrl Pts',(1.58668922481221,23.710082626383,0.));
#208403=CARTESIAN_POINT('Ctrl Pts',(1.59170048908633,23.6906508338833,0.));
#208404=CARTESIAN_POINT('Ctrl Pts',(1.59663225222463,23.671311958631,0.));
#208405=CARTESIAN_POINT('Ctrl Pts',(1.60148472786595,23.6520669774876,0.));
#208406=CARTESIAN_POINT('Ctrl Pts',(1.60625813414672,23.6329168794929,0.));
#208407=CARTESIAN_POINT('Ctrl Pts',(1.61095269379778,23.6138626661653,0.));
#208408=CARTESIAN_POINT('Ctrl Pts',(1.61556863424698,23.5949053517997,0.));
#208409=CARTESIAN_POINT('Ctrl Pts',(1.62010618772866,23.57604596376,0.));
#208410=CARTESIAN_POINT('Ctrl Pts',(1.62456559140064,23.5572855427601,0.));
#208411=CARTESIAN_POINT('Ctrl Pts',(1.62894708745223,23.538625143226,0.));
#208412=CARTESIAN_POINT('Ctrl Pts',(1.63325092321725,23.5200658336612,0.));
#208413=CARTESIAN_POINT('Ctrl Pts',(1.63747735129474,23.5016086970003,0.));
#208414=CARTESIAN_POINT('Ctrl Pts',(1.64162662967528,23.4832548309645,0.));
#208415=CARTESIAN_POINT('Ctrl Pts',(1.64569902187611,23.4650053483932,0.));
#208416=CARTESIAN_POINT('Ctrl Pts',(1.6496947970734,23.4468613776574,0.));
#208417=CARTESIAN_POINT('Ctrl Pts',(1.65361423023728,23.4288240631043,0.));
#208418=CARTESIAN_POINT('Ctrl Pts',(1.65745760227505,23.4108945654805,0.));
#208419=CARTESIAN_POINT('Ctrl Pts',(1.66122520018011,23.3930740623619,0.));
#208420=CARTESIAN_POINT('Ctrl Pts',(1.66491731718876,23.3753637485545,0.));
#208421=CARTESIAN_POINT('Ctrl Pts',(1.66853425293995,23.3577648365744,0.));
#208422=CARTESIAN_POINT('Ctrl Pts',(1.67207631363921,23.3402785571865,0.));
#208423=CARTESIAN_POINT('Ctrl Pts',(1.67554381222994,23.3229061599145,0.));
#208424=CARTESIAN_POINT('Ctrl Pts',(1.67893706857117,23.3056489135611,0.));
#208425=CARTESIAN_POINT('Ctrl Pts',(1.68225640962168,23.2885081066951,0.));
#208426=CARTESIAN_POINT('Ctrl Pts',(1.68550216963258,23.2714850482246,0.));
#208427=CARTESIAN_POINT('Ctrl Pts',(1.68867469034896,23.2545810680537,0.));
#208428=CARTESIAN_POINT('Ctrl Pts',(1.69177432121711,23.2377975177013,0.));
#208429=CARTESIAN_POINT('Ctrl Pts',(1.69480141959953,23.2211357709374,0.));
#208430=CARTESIAN_POINT('Ctrl Pts',(1.69775635099443,23.2045972243767,0.));
#208431=CARTESIAN_POINT('Ctrl Pts',(1.7006394892701,23.1881832981851,0.));
#208432=CARTESIAN_POINT('Ctrl Pts',(1.70345121691276,23.1718954368751,0.));
#208433=CARTESIAN_POINT('Ctrl Pts',(1.70619192527852,23.1557351100614,0.));
#208434=CARTESIAN_POINT('Ctrl Pts',(1.70886201485452,23.1397038132356,0.));
#208435=CARTESIAN_POINT('Ctrl Pts',(1.71146189552174,23.1238030684925,0.));
#208436=CARTESIAN_POINT('Ctrl Pts',(1.71399198684704,23.1080344254286,0.));
#208437=CARTESIAN_POINT('Ctrl Pts',(1.71645271839296,23.0923994621213,0.));
#208438=CARTESIAN_POINT('Ctrl Pts',(1.71884453003027,23.0768997860709,0.));
#208439=CARTESIAN_POINT('Ctrl Pts',(1.72116787225991,23.0615370351562,0.));
#208440=CARTESIAN_POINT('Ctrl Pts',(1.72342320653746,23.0463128785531,0.));
#208441=CARTESIAN_POINT('Ctrl Pts',(1.72561100564045,23.0312290178883,0.));
#208442=CARTESIAN_POINT('Ctrl Pts',(1.72773175404708,23.0162871884168,0.));
#208443=CARTESIAN_POINT('Ctrl Pts',(1.72978594832136,23.001489160189,0.));
#208444=CARTESIAN_POINT('Ctrl Pts',(1.7317740975019,22.9868367391978,0.));
#208445=CARTESIAN_POINT('Ctrl Pts',(1.73369672350814,22.9723317685688,0.));
#208446=CARTESIAN_POINT('Ctrl Pts',(1.73555436162769,22.9579761301063,0.));
#208447=CARTESIAN_POINT('Ctrl Pts',(1.73734756100039,22.9437717457826,0.));
#208448=CARTESIAN_POINT('Ctrl Pts',(1.73907688511666,22.9297205792586,0.));
#208449=CARTESIAN_POINT('Ctrl Pts',(1.74074291231058,22.9158246373363,0.));
#208450=CARTESIAN_POINT('Ctrl Pts',(1.7423462363008,22.9020859716141,0.));
#208451=CARTESIAN_POINT('Ctrl Pts',(1.74388746677702,22.888506680335,0.));
#208452=CARTESIAN_POINT('Ctrl Pts',(1.74536722998201,22.8750889101696,0.));
#208453=CARTESIAN_POINT('Ctrl Pts',(1.74678616930664,22.8618348580235,0.));
#208454=CARTESIAN_POINT('Ctrl Pts',(1.74814494588492,22.8487467728076,0.));
#208455=CARTESIAN_POINT('Ctrl Pts',(1.74944423940115,22.8358269579853,0.));
#208456=CARTESIAN_POINT('Ctrl Pts',(1.75068474890883,22.8230777741284,0.));
#208457=CARTESIAN_POINT('Ctrl Pts',(1.75186719365592,22.8105016414713,0.));
#208458=CARTESIAN_POINT('Ctrl Pts',(1.75299231391466,22.7981010424314,0.));
#208459=CARTESIAN_POINT('Ctrl Pts',(1.75406087182936,22.7858785242361,0.));
#208460=CARTESIAN_POINT('Ctrl Pts',(1.75507365227131,22.7738367016118,0.));
#208461=CARTESIAN_POINT('Ctrl Pts',(1.75603146371641,22.7619782595013,0.));
#208462=CARTESIAN_POINT('Ctrl Pts',(1.75693513908907,22.750305955645,0.));
#208463=CARTESIAN_POINT('Ctrl Pts',(1.75778553673244,22.7388226235559,0.));
#208464=CARTESIAN_POINT('Ctrl Pts',(1.75858354204633,22.72753117773,0.));
#208465=CARTESIAN_POINT('Ctrl Pts',(1.75933006905925,22.7164346186006,0.));
#208466=CARTESIAN_POINT('Ctrl Pts',(1.76002606202401,22.7055360375485,0.));
#208467=CARTESIAN_POINT('Ctrl Pts',(1.76067249704886,22.6948386219851,0.));
#208468=CARTESIAN_POINT('Ctrl Pts',(1.76127038310614,22.684345658525,0.));
#208469=CARTESIAN_POINT('Ctrl Pts',(1.76182076289525,22.67406053567,0.));
#208470=CARTESIAN_POINT('Ctrl Pts',(1.76232471392568,22.6639867471753,0.));
#208471=CARTESIAN_POINT('Ctrl Pts',(1.76278334912561,22.6541278938409,0.));
#208472=CARTESIAN_POINT('Ctrl Pts',(1.76319782013916,22.6444876940423,0.));
#208473=CARTESIAN_POINT('Ctrl Pts',(1.76356932176273,22.6350699979359,0.));
#208474=CARTESIAN_POINT('Ctrl Pts',(1.76389909571403,22.6258787994848,0.));
#208475=CARTESIAN_POINT('Ctrl Pts',(1.76418843543739,22.6169182517694,0.));
#208476=CARTESIAN_POINT('Ctrl Pts',(1.76443868648015,22.6081926681343,0.));
#208477=CARTESIAN_POINT('Ctrl Pts',(1.76465124413557,22.5997065145638,0.));
#208478=CARTESIAN_POINT('Ctrl Pts',(1.76482755288411,22.5914644078106,0.));
#208479=CARTESIAN_POINT('Ctrl Pts',(1.76496910283088,22.5834711038022,0.));
#208480=CARTESIAN_POINT('Ctrl Pts',(1.76507744026746,22.5757315316353,0.));
#208481=CARTESIAN_POINT('Ctrl Pts',(1.76515418518831,22.5682508499873,0.));
#208482=CARTESIAN_POINT('Ctrl Pts',(1.7652010450045,22.5610344912501,0.));
#208483=CARTESIAN_POINT('Ctrl Pts',(1.76521983384062,22.5540882235837,0.));
#208484=CARTESIAN_POINT('Ctrl Pts',(1.76521245524047,22.5474180954006,0.));
#208485=CARTESIAN_POINT('Ctrl Pts',(1.76518087841493,22.5410303590892,0.));
#208486=CARTESIAN_POINT('Ctrl Pts',(1.76512711563254,22.5349313983571,0.));
#208487=CARTESIAN_POINT('Ctrl Pts',(1.76505320262759,22.529127665298,0.));
#208488=CARTESIAN_POINT('Ctrl Pts',(1.76496128643375,22.5236259635515,0.));
#208489=CARTESIAN_POINT('Ctrl Pts',(1.76485369319895,22.5184336670207,0.));
#208490=CARTESIAN_POINT('Ctrl Pts',(1.76473303281149,22.5135590569554,0.));
#208491=CARTESIAN_POINT('Ctrl Pts',(1.76460218257313,22.5090112700212,0.));
#208492=CARTESIAN_POINT('Ctrl Pts',(1.76446408210364,22.5047996391978,0.));
#208493=CARTESIAN_POINT('Ctrl Pts',(1.76432160068737,22.5009332677316,0.));
#208494=CARTESIAN_POINT('Ctrl Pts',(1.76417731243483,22.4974203063191,0.));
#208495=CARTESIAN_POINT('Ctrl Pts',(1.76403393880316,22.4942693792449,0.));
#208496=CARTESIAN_POINT('Ctrl Pts',(1.76389475965714,22.4914909094908,0.));
#208497=CARTESIAN_POINT('Ctrl Pts',(1.76376424879468,22.4890991659479,0.));
#208498=CARTESIAN_POINT('Ctrl Pts',(1.76364784232925,22.4871115206572,0.));
#208499=CARTESIAN_POINT('Ctrl Pts',(1.76355076045549,22.4855446605991,0.));
#208500=CARTESIAN_POINT('Ctrl Pts',(1.76347698284861,22.4844112933125,0.));
#208501=CARTESIAN_POINT('Ctrl Pts',(1.76343813434659,22.4838562517064,0.));
#208502=CARTESIAN_POINT('Ctrl Pts',(1.76342064263637,22.4836387052228,0.));
#208503=CARTESIAN_POINT('Ctrl Pts',(1.7634141553879,22.4835819929788,0.));
#208504=CARTESIAN_POINT('Ctrl Pts',(1.7634122053118,22.4835757167854,0.));
#208505=CARTESIAN_POINT('',(0.661312440730901,25.991588367311,0.));
#208506=CARTESIAN_POINT('Ctrl Pts',(4.11585220600461,22.1738711152697,0.));
#208507=CARTESIAN_POINT('Ctrl Pts',(4.11585220600461,22.1738711152697,12.));
#208508=CARTESIAN_POINT('Ctrl Pts',(4.11585194677442,22.173877682324,0.));
#208509=CARTESIAN_POINT('Ctrl Pts',(4.11585194677442,22.173877682324,12.));
#208510=CARTESIAN_POINT('Ctrl Pts',(4.11586035878287,22.1739341411687,0.));
#208511=CARTESIAN_POINT('Ctrl Pts',(4.11586035878287,22.1739341411687,12.));
#208512=CARTESIAN_POINT('Ctrl Pts',(4.11589976826166,22.1741488021234,0.));
#208513=CARTESIAN_POINT('Ctrl Pts',(4.11589976826166,22.1741488021234,12.));
#208514=CARTESIAN_POINT('Ctrl Pts',(4.11600589882845,22.1746949858775,0.));
#208515=CARTESIAN_POINT('Ctrl Pts',(4.11600589882845,22.1746949858775,12.));
#208516=CARTESIAN_POINT('Ctrl Pts',(4.11622797217068,22.1758088296598,0.));
#208517=CARTESIAN_POINT('Ctrl Pts',(4.11622797217068,22.1758088296598,12.));
#208518=CARTESIAN_POINT('Ctrl Pts',(4.11653973150518,22.177347426894,0.));
#208519=CARTESIAN_POINT('Ctrl Pts',(4.11653973150518,22.177347426894,12.));
#208520=CARTESIAN_POINT('Ctrl Pts',(4.11694173195003,22.179297473024,0.));
#208521=CARTESIAN_POINT('Ctrl Pts',(4.11694173195003,22.179297473024,12.));
#208522=CARTESIAN_POINT('Ctrl Pts',(4.11743469691756,22.1816414985788,0.));
#208523=CARTESIAN_POINT('Ctrl Pts',(4.11743469691756,22.1816414985788,12.));
#208524=CARTESIAN_POINT('Ctrl Pts',(4.11801938107479,22.1843613164855,0.));
#208525=CARTESIAN_POINT('Ctrl Pts',(4.11801938107479,22.1843613164855,12.));
#208526=CARTESIAN_POINT('Ctrl Pts',(4.11869641271773,22.1874419861496,0.));
#208527=CARTESIAN_POINT('Ctrl Pts',(4.11869641271773,22.1874419861496,12.));
#208528=CARTESIAN_POINT('Ctrl Pts',(4.11946626228636,22.1908725908525,0.));
#208529=CARTESIAN_POINT('Ctrl Pts',(4.11946626228636,22.1908725908525,12.));
#208530=CARTESIAN_POINT('Ctrl Pts',(4.12032932637736,22.1946440958098,0.));
#208531=CARTESIAN_POINT('Ctrl Pts',(4.12032932637736,22.1946440958098,12.));
#208532=CARTESIAN_POINT('Ctrl Pts',(4.12128598183522,22.1987479618246,0.));
#208533=CARTESIAN_POINT('Ctrl Pts',(4.12128598183522,22.1987479618246,12.));
#208534=CARTESIAN_POINT('Ctrl Pts',(4.12233664408227,22.2031746532106,0.));
#208535=CARTESIAN_POINT('Ctrl Pts',(4.12233664408227,22.2031746532106,12.));
#208536=CARTESIAN_POINT('Ctrl Pts',(4.12348173702023,22.2079143941719,0.));
#208537=CARTESIAN_POINT('Ctrl Pts',(4.12348173702023,22.2079143941719,12.));
#208538=CARTESIAN_POINT('Ctrl Pts',(4.12472167516607,22.2129576146671,0.));
#208539=CARTESIAN_POINT('Ctrl Pts',(4.12472167516607,22.2129576146671,12.));
#208540=CARTESIAN_POINT('Ctrl Pts',(4.12605683613307,22.2182956401341,0.));
#208541=CARTESIAN_POINT('Ctrl Pts',(4.12605683613307,22.2182956401341,12.));
#208542=CARTESIAN_POINT('Ctrl Pts',(4.12748755830104,22.2239207458781,0.));
#208543=CARTESIAN_POINT('Ctrl Pts',(4.12748755830104,22.2239207458781,12.));
#208544=CARTESIAN_POINT('Ctrl Pts',(4.12901415463379,22.2298258043947,0.));
#208545=CARTESIAN_POINT('Ctrl Pts',(4.12901415463379,22.2298258043947,12.));
#208546=CARTESIAN_POINT('Ctrl Pts',(4.13063692157498,22.2360040565533,0.));
#208547=CARTESIAN_POINT('Ctrl Pts',(4.13063692157498,22.2360040565533,12.));
#208548=CARTESIAN_POINT('Ctrl Pts',(4.1323561506016,22.2424488153523,0.));
#208549=CARTESIAN_POINT('Ctrl Pts',(4.1323561506016,22.2424488153523,12.));
#208550=CARTESIAN_POINT('Ctrl Pts',(4.1341721255881,22.249153531779,0.));
#208551=CARTESIAN_POINT('Ctrl Pts',(4.1341721255881,22.249153531779,12.));
#208552=CARTESIAN_POINT('Ctrl Pts',(4.13608511977225,22.2561118708421,0.));
#208553=CARTESIAN_POINT('Ctrl Pts',(4.13608511977225,22.2561118708421,12.));
#208554=CARTESIAN_POINT('Ctrl Pts',(4.13809539255421,22.2633177913972,0.));
#208555=CARTESIAN_POINT('Ctrl Pts',(4.13809539255421,22.2633177913972,12.));
#208556=CARTESIAN_POINT('Ctrl Pts',(4.14020318715991,22.2707656042457,0.));
#208557=CARTESIAN_POINT('Ctrl Pts',(4.14020318715991,22.2707656042457,12.));
#208558=CARTESIAN_POINT('Ctrl Pts',(4.14240873321984,22.2784499072027,0.));
#208559=CARTESIAN_POINT('Ctrl Pts',(4.14240873321984,22.2784499072027,12.));
#208560=CARTESIAN_POINT('Ctrl Pts',(4.14471224859295,22.2863655389166,0.));
#208561=CARTESIAN_POINT('Ctrl Pts',(4.14471224859295,22.2863655389166,12.));
#208562=CARTESIAN_POINT('Ctrl Pts',(4.14711394168556,22.2945075198467,0.));
#208563=CARTESIAN_POINT('Ctrl Pts',(4.14711394168556,22.2945075198467,12.));
#208564=CARTESIAN_POINT('Ctrl Pts',(4.14961401285522,22.3028710166933,0.));
#208565=CARTESIAN_POINT('Ctrl Pts',(4.14961401285522,22.3028710166933,12.));
#208566=CARTESIAN_POINT('Ctrl Pts',(4.1522126539699,22.3114513545185,0.));
#208567=CARTESIAN_POINT('Ctrl Pts',(4.1522126539699,22.3114513545185,12.));
#208568=CARTESIAN_POINT('Ctrl Pts',(4.15491004835281,22.3202440186979,0.));
#208569=CARTESIAN_POINT('Ctrl Pts',(4.15491004835281,22.3202440186979,12.));
#208570=CARTESIAN_POINT('Ctrl Pts',(4.15770637047889,22.3292446628959,0.));
#208571=CARTESIAN_POINT('Ctrl Pts',(4.15770637047889,22.3292446628959,12.));
#208572=CARTESIAN_POINT('Ctrl Pts',(4.16060178604164,22.3384491078602,0.));
#208573=CARTESIAN_POINT('Ctrl Pts',(4.16060178604164,22.3384491078602,12.));
#208574=CARTESIAN_POINT('Ctrl Pts',(4.16359645263187,22.3478533253889,0.));
#208575=CARTESIAN_POINT('Ctrl Pts',(4.16359645263187,22.3478533253889,12.));
#208576=CARTESIAN_POINT('Ctrl Pts',(4.166690520266,22.3574534257396,0.));
#208577=CARTESIAN_POINT('Ctrl Pts',(4.166690520266,22.3574534257396,12.));
#208578=CARTESIAN_POINT('Ctrl Pts',(4.16988413199457,22.36724564276,0.));
#208579=CARTESIAN_POINT('Ctrl Pts',(4.16988413199457,22.36724564276,12.));
#208580=CARTESIAN_POINT('Ctrl Pts',(4.17317742436145,22.3772263228617,0.));
#208581=CARTESIAN_POINT('Ctrl Pts',(4.17317742436145,22.3772263228617,12.));
#208582=CARTESIAN_POINT('Ctrl Pts',(4.17657052752825,22.3873919231334,0.));
#208583=CARTESIAN_POINT('Ctrl Pts',(4.17657052752825,22.3873919231334,12.));
#208584=CARTESIAN_POINT('Ctrl Pts',(4.18006356544882,22.3977390078075,0.));
#208585=CARTESIAN_POINT('Ctrl Pts',(4.18006356544882,22.3977390078075,12.));
#208586=CARTESIAN_POINT('Ctrl Pts',(4.1836566560085,22.4082642454453,0.));
#208587=CARTESIAN_POINT('Ctrl Pts',(4.1836566560085,22.4082642454453,12.));
#208588=CARTESIAN_POINT('Ctrl Pts',(4.1873499111772,22.4189644056115,0.));
#208589=CARTESIAN_POINT('Ctrl Pts',(4.1873499111772,22.4189644056115,12.));
#208590=CARTESIAN_POINT('Ctrl Pts',(4.19114343726941,22.4298363535421,0.));
#208591=CARTESIAN_POINT('Ctrl Pts',(4.19114343726941,22.4298363535421,12.));
#208592=CARTESIAN_POINT('Ctrl Pts',(4.1950373351886,22.4408770448917,0.));
#208593=CARTESIAN_POINT('Ctrl Pts',(4.1950373351886,22.4408770448917,12.));
#208594=CARTESIAN_POINT('Ctrl Pts',(4.19903170066354,22.4520835205419,0.));
#208595=CARTESIAN_POINT('Ctrl Pts',(4.19903170066354,22.4520835205419,12.));
#208596=CARTESIAN_POINT('Ctrl Pts',(4.2031266244817,22.4634529011433,0.));
#208597=CARTESIAN_POINT('Ctrl Pts',(4.2031266244817,22.4634529011433,12.));
#208598=CARTESIAN_POINT('Ctrl Pts',(4.20732219265648,22.4749823839915,0.));
#208599=CARTESIAN_POINT('Ctrl Pts',(4.20732219265648,22.4749823839915,12.));
#208600=CARTESIAN_POINT('Ctrl Pts',(4.21161848657428,22.4866692403147,0.));
#208601=CARTESIAN_POINT('Ctrl Pts',(4.21161848657428,22.4866692403147,12.));
#208602=CARTESIAN_POINT('Ctrl Pts',(4.21601558313908,22.4985108124229,0.));
#208603=CARTESIAN_POINT('Ctrl Pts',(4.21601558313908,22.4985108124229,12.));
#208604=CARTESIAN_POINT('Ctrl Pts',(4.22051355490196,22.5105045108882,0.));
#208605=CARTESIAN_POINT('Ctrl Pts',(4.22051355490196,22.5105045108882,12.));
#208606=CARTESIAN_POINT('Ctrl Pts',(4.2251124702004,22.5226478117885,0.));
#208607=CARTESIAN_POINT('Ctrl Pts',(4.2251124702004,22.5226478117885,12.));
#208608=CARTESIAN_POINT('Ctrl Pts',(4.22981239330731,22.5349382540587,0.));
#208609=CARTESIAN_POINT('Ctrl Pts',(4.22981239330731,22.5349382540587,12.));
#208610=CARTESIAN_POINT('Ctrl Pts',(4.23461338456713,22.5473734368086,0.));
#208611=CARTESIAN_POINT('Ctrl Pts',(4.23461338456713,22.5473734368086,12.));
#208612=CARTESIAN_POINT('Ctrl Pts',(4.23951550052526,22.559951016643,0.));
#208613=CARTESIAN_POINT('Ctrl Pts',(4.23951550052526,22.559951016643,12.));
#208614=CARTESIAN_POINT('Ctrl Pts',(4.24451879404858,22.5726687049922,0.));
#208615=CARTESIAN_POINT('Ctrl Pts',(4.24451879404858,22.5726687049922,12.));
#208616=CARTESIAN_POINT('Ctrl Pts',(4.24962331444184,22.5855242662479,0.));
#208617=CARTESIAN_POINT('Ctrl Pts',(4.24962331444184,22.5855242662479,12.));
#208618=CARTESIAN_POINT('Ctrl Pts',(4.25482910755485,22.5985155158637,0.));
#208619=CARTESIAN_POINT('Ctrl Pts',(4.25482910755485,22.5985155158637,12.));
#208620=CARTESIAN_POINT('Ctrl Pts',(4.26013621588303,22.611640318482,0.));
#208621=CARTESIAN_POINT('Ctrl Pts',(4.26013621588303,22.611640318482,12.));
#208622=CARTESIAN_POINT('Ctrl Pts',(4.26554467865571,22.6248965859975,0.));
#208623=CARTESIAN_POINT('Ctrl Pts',(4.26554467865571,22.6248965859975,12.));
#208624=CARTESIAN_POINT('Ctrl Pts',(4.27105453192999,22.6382822758171,0.));
#208625=CARTESIAN_POINT('Ctrl Pts',(4.27105453192999,22.6382822758171,12.));
#208626=CARTESIAN_POINT('Ctrl Pts',(4.27666580869117,22.6517953893303,0.));
#208627=CARTESIAN_POINT('Ctrl Pts',(4.27666580869117,22.6517953893303,12.));
#208628=CARTESIAN_POINT('Ctrl Pts',(4.28237853894059,22.665433970311,0.));
#208629=CARTESIAN_POINT('Ctrl Pts',(4.28237853894059,22.665433970311,12.));
#208630=CARTESIAN_POINT('Ctrl Pts',(4.28819274977766,22.6791961033537,0.));
#208631=CARTESIAN_POINT('Ctrl Pts',(4.28819274977766,22.6791961033537,12.));
#208632=CARTESIAN_POINT('Ctrl Pts',(4.29410846547061,22.6930799122545,0.));
#208633=CARTESIAN_POINT('Ctrl Pts',(4.29410846547061,22.6930799122545,12.));
#208634=CARTESIAN_POINT('Ctrl Pts',(4.30012570754066,22.707083558756,0.));
#208635=CARTESIAN_POINT('Ctrl Pts',(4.30012570754066,22.707083558756,12.));
#208636=CARTESIAN_POINT('Ctrl Pts',(4.30624449484074,22.7212052413384,0.));
#208637=CARTESIAN_POINT('Ctrl Pts',(4.30624449484074,22.7212052413384,12.));
#208638=CARTESIAN_POINT('Ctrl Pts',(4.3124648436255,22.7354431939927,0.));
#208639=CARTESIAN_POINT('Ctrl Pts',(4.3124648436255,22.7354431939927,12.));
#208640=CARTESIAN_POINT('Ctrl Pts',(4.3187867676123,22.7497956849852,0.));
#208641=CARTESIAN_POINT('Ctrl Pts',(4.3187867676123,22.7497956849852,12.));
#208642=CARTESIAN_POINT('Ctrl Pts',(4.32521027803747,22.764261015648,0.));
#208643=CARTESIAN_POINT('Ctrl Pts',(4.32521027803747,22.764261015648,12.));
#208644=CARTESIAN_POINT('Ctrl Pts',(4.33173538373182,22.7788375194081,0.));
#208645=CARTESIAN_POINT('Ctrl Pts',(4.33173538373182,22.7788375194081,12.));
#208646=CARTESIAN_POINT('Ctrl Pts',(4.33836209118442,22.7935235607807,0.));
#208647=CARTESIAN_POINT('Ctrl Pts',(4.33836209118442,22.7935235607807,12.));
#208648=CARTESIAN_POINT('Ctrl Pts',(4.34509040460065,22.808317534379,0.));
#208649=CARTESIAN_POINT('Ctrl Pts',(4.34509040460065,22.808317534379,12.));
#208650=CARTESIAN_POINT('Ctrl Pts',(4.35192032594801,22.8232178638873,0.));
#208651=CARTESIAN_POINT('Ctrl Pts',(4.35192032594801,22.8232178638873,12.));
#208652=CARTESIAN_POINT('Ctrl Pts',(4.35885185500559,22.838223001118,0.));
#208653=CARTESIAN_POINT('Ctrl Pts',(4.35885185500559,22.838223001118,12.));
#208654=CARTESIAN_POINT('Ctrl Pts',(4.36588498943009,22.8533314252419,0.));
#208655=CARTESIAN_POINT('Ctrl Pts',(4.36588498943009,22.8533314252419,12.));
#208656=CARTESIAN_POINT('Ctrl Pts',(4.37301972480752,22.8685416419725,0.));
#208657=CARTESIAN_POINT('Ctrl Pts',(4.37301972480752,22.8685416419725,12.));
#208658=CARTESIAN_POINT('Ctrl Pts',(4.38025605470089,22.8838521827702,0.));
#208659=CARTESIAN_POINT('Ctrl Pts',(4.38025605470089,22.8838521827702,12.));
#208660=CARTESIAN_POINT('Ctrl Pts',(4.38759397068391,22.8992616040108,0.));
#208661=CARTESIAN_POINT('Ctrl Pts',(4.38759397068391,22.8992616040108,12.));
#208662=CARTESIAN_POINT('Ctrl Pts',(4.39503346238454,22.9147684862425,0.));
#208663=CARTESIAN_POINT('Ctrl Pts',(4.39503346238454,22.9147684862425,12.));
#208664=CARTESIAN_POINT('Ctrl Pts',(4.40257451754307,22.9303714335549,0.));
#208665=CARTESIAN_POINT('Ctrl Pts',(4.40257451754307,22.9303714335549,12.));
#208666=CARTESIAN_POINT('Ctrl Pts',(4.41021712205547,22.9460690729093,0.));
#208667=CARTESIAN_POINT('Ctrl Pts',(4.41021712205547,22.9460690729093,12.));
#208668=CARTESIAN_POINT('Ctrl Pts',(4.41796126001309,22.9618600534866,0.));
#208669=CARTESIAN_POINT('Ctrl Pts',(4.41796126001309,22.9618600534866,12.));
#208670=CARTESIAN_POINT('Ctrl Pts',(4.42580691372771,22.9777430460021,0.));
#208671=CARTESIAN_POINT('Ctrl Pts',(4.42580691372771,22.9777430460021,12.));
#208672=CARTESIAN_POINT('Ctrl Pts',(4.43375406376904,22.9937167421009,0.));
#208673=CARTESIAN_POINT('Ctrl Pts',(4.43375406376904,22.9937167421009,12.));
#208674=CARTESIAN_POINT('Ctrl Pts',(4.44180268901666,23.0097798538399,0.));
#208675=CARTESIAN_POINT('Ctrl Pts',(4.44180268901666,23.0097798538399,12.));
#208676=CARTESIAN_POINT('Ctrl Pts',(4.44995276669698,23.0259311131395,0.));
#208677=CARTESIAN_POINT('Ctrl Pts',(4.44995276669698,23.0259311131395,12.));
#208678=CARTESIAN_POINT('Ctrl Pts',(4.45820427241676,23.0421692712466,0.));
#208679=CARTESIAN_POINT('Ctrl Pts',(4.45820427241676,23.0421692712466,12.));
#208680=CARTESIAN_POINT('Ctrl Pts',(4.46655718018205,23.0584930981723,0.));
#208681=CARTESIAN_POINT('Ctrl Pts',(4.46655718018205,23.0584930981723,12.));
#208682=CARTESIAN_POINT('Ctrl Pts',(4.47501146242821,23.0749013821868,0.));
#208683=CARTESIAN_POINT('Ctrl Pts',(4.47501146242821,23.0749013821868,12.));
#208684=CARTESIAN_POINT('Ctrl Pts',(4.48356709006756,23.0913929293909,0.));
#208685=CARTESIAN_POINT('Ctrl Pts',(4.48356709006756,23.0913929293909,12.));
#208686=CARTESIAN_POINT('Ctrl Pts',(4.49222403252201,23.1079665632629,0.));
#208687=CARTESIAN_POINT('Ctrl Pts',(4.49222403252201,23.1079665632629,12.));
#208688=CARTESIAN_POINT('Ctrl Pts',(4.50098225775178,23.1246211242117,0.));
#208689=CARTESIAN_POINT('Ctrl Pts',(4.50098225775178,23.1246211242117,12.));
#208690=CARTESIAN_POINT('Ctrl Pts',(4.50984173227087,23.1413554691136,0.));
#208691=CARTESIAN_POINT('Ctrl Pts',(4.50984173227087,23.1413554691136,12.));
#208692=CARTESIAN_POINT('Ctrl Pts',(4.51880242116785,23.1581684708778,0.));
#208693=CARTESIAN_POINT('Ctrl Pts',(4.51880242116785,23.1581684708778,12.));
#208694=CARTESIAN_POINT('Ctrl Pts',(4.52786428815047,23.1750590180923,0.));
#208695=CARTESIAN_POINT('Ctrl Pts',(4.52786428815047,23.1750590180923,12.));
#208696=CARTESIAN_POINT('Ctrl Pts',(4.53702729557585,23.1920260146474,0.));
#208697=CARTESIAN_POINT('Ctrl Pts',(4.53702729557585,23.1920260146474,12.));
#208698=CARTESIAN_POINT('Ctrl Pts',(4.54629140447542,23.2090683793627,0.));
#208699=CARTESIAN_POINT('Ctrl Pts',(4.54629140447542,23.2090683793627,12.));
#208700=CARTESIAN_POINT('Ctrl Pts',(4.55565657456956,23.2261850456055,0.));
#208701=CARTESIAN_POINT('Ctrl Pts',(4.55565657456956,23.2261850456055,12.));
#208702=CARTESIAN_POINT('Ctrl Pts',(4.5651227642781,23.2433749609117,0.));
#208703=CARTESIAN_POINT('Ctrl Pts',(4.5651227642781,23.2433749609117,12.));
#208704=CARTESIAN_POINT('Ctrl Pts',(4.5746899307607,23.2606370866853,0.));
#208705=CARTESIAN_POINT('Ctrl Pts',(4.5746899307607,23.2606370866853,12.));
#208706=CARTESIAN_POINT('Ctrl Pts',(4.58435802994674,23.2779703978868,0.));
#208707=CARTESIAN_POINT('Ctrl Pts',(4.58435802994674,23.2779703978868,12.));
#208708=CARTESIAN_POINT('Ctrl Pts',(4.59412701655749,23.295373882719,0.));
#208709=CARTESIAN_POINT('Ctrl Pts',(4.59412701655749,23.295373882719,12.));
#208710=CARTESIAN_POINT('Ctrl Pts',(4.60399684412174,23.3128465423119,0.));
#208711=CARTESIAN_POINT('Ctrl Pts',(4.60399684412174,23.3128465423119,12.));
#208712=CARTESIAN_POINT('Ctrl Pts',(4.61396746497848,23.3303873903947,0.));
#208713=CARTESIAN_POINT('Ctrl Pts',(4.61396746497848,23.3303873903947,12.));
#208714=CARTESIAN_POINT('Ctrl Pts',(4.62403883030823,23.3479954530281,0.));
#208715=CARTESIAN_POINT('Ctrl Pts',(4.62403883030823,23.3479954530281,12.));
#208716=CARTESIAN_POINT('Ctrl Pts',(4.63421089016554,23.3656697683496,0.));
#208717=CARTESIAN_POINT('Ctrl Pts',(4.63421089016554,23.3656697683496,12.));
#208718=CARTESIAN_POINT('Ctrl Pts',(4.64448359349935,23.383409386307,0.));
#208719=CARTESIAN_POINT('Ctrl Pts',(4.64448359349935,23.383409386307,12.));
#208720=CARTESIAN_POINT('Ctrl Pts',(4.65485688816921,23.4012133683957,0.));
#208721=CARTESIAN_POINT('Ctrl Pts',(4.65485688816921,23.4012133683957,12.));
#208722=CARTESIAN_POINT('Ctrl Pts',(4.66533072094663,23.4190807873798,0.));
#208723=CARTESIAN_POINT('Ctrl Pts',(4.66533072094663,23.4190807873798,12.));
#208724=CARTESIAN_POINT('Ctrl Pts',(4.6759050375305,23.4370107270444,0.));
#208725=CARTESIAN_POINT('Ctrl Pts',(4.6759050375305,23.4370107270444,12.));
#208726=CARTESIAN_POINT('Ctrl Pts',(4.68657978258297,23.4550022819853,0.));
#208727=CARTESIAN_POINT('Ctrl Pts',(4.68657978258297,23.4550022819853,12.));
#208728=CARTESIAN_POINT('Ctrl Pts',(4.69735489975023,23.4730545573849,0.));
#208729=CARTESIAN_POINT('Ctrl Pts',(4.69735489975023,23.4730545573849,12.));
#208730=CARTESIAN_POINT('Ctrl Pts',(4.7082303316782,23.491166668789,0.));
#208731=CARTESIAN_POINT('Ctrl Pts',(4.7082303316782,23.491166668789,12.));
#208732=CARTESIAN_POINT('Ctrl Pts',(4.71920602001904,23.5093377418784,0.));
#208733=CARTESIAN_POINT('Ctrl Pts',(4.71920602001904,23.5093377418784,12.));
#208734=CARTESIAN_POINT('Ctrl Pts',(4.73028190543031,23.5275669122378,0.));
#208735=CARTESIAN_POINT('Ctrl Pts',(4.73028190543031,23.5275669122378,12.));
#208736=CARTESIAN_POINT('Ctrl Pts',(4.74145792760698,23.5458533251715,0.));
#208737=CARTESIAN_POINT('Ctrl Pts',(4.74145792760698,23.5458533251715,12.));
#208738=CARTESIAN_POINT('Ctrl Pts',(4.75273402530615,23.564196135517,0.));
#208739=CARTESIAN_POINT('Ctrl Pts',(4.75273402530615,23.564196135517,12.));
#208740=CARTESIAN_POINT('Ctrl Pts',(4.7641101363625,23.5825945074535,0.));
#208741=CARTESIAN_POINT('Ctrl Pts',(4.7641101363625,23.5825945074535,12.));
#208742=CARTESIAN_POINT('Ctrl Pts',(4.77558619769875,23.6010476143099,0.));
#208743=CARTESIAN_POINT('Ctrl Pts',(4.77558619769875,23.6010476143099,12.));
#208744=CARTESIAN_POINT('Ctrl Pts',(4.78716214532104,23.6195546383625,0.));
#208745=CARTESIAN_POINT('Ctrl Pts',(4.78716214532104,23.6195546383625,12.));
#208746=CARTESIAN_POINT('Ctrl Pts',(4.79883791433229,23.6381147706581,0.));
#208747=CARTESIAN_POINT('Ctrl Pts',(4.79883791433229,23.6381147706581,12.));
#208748=CARTESIAN_POINT('Ctrl Pts',(4.81061343896442,23.6567272108631,0.));
#208749=CARTESIAN_POINT('Ctrl Pts',(4.81061343896442,23.6567272108631,12.));
#208750=CARTESIAN_POINT('Ctrl Pts',(4.82248865259569,23.6753911671023,0.));
#208751=CARTESIAN_POINT('Ctrl Pts',(4.82248865259569,23.6753911671023,12.));
#208752=CARTESIAN_POINT('Ctrl Pts',(4.83446348776267,23.6941058557971,0.));
#208753=CARTESIAN_POINT('Ctrl Pts',(4.83446348776267,23.6941058557971,12.));
#208754=CARTESIAN_POINT('Ctrl Pts',(4.84653787616422,23.7128705015014,0.));
#208755=CARTESIAN_POINT('Ctrl Pts',(4.84653787616422,23.7128705015014,12.));
#208756=CARTESIAN_POINT('Ctrl Pts',(4.85871174865491,23.7316843367308,0.));
#208757=CARTESIAN_POINT('Ctrl Pts',(4.85871174865491,23.7316843367308,12.));
#208758=CARTESIAN_POINT('Ctrl Pts',(4.87098503527142,23.7505466018239,0.));
#208759=CARTESIAN_POINT('Ctrl Pts',(4.87098503527142,23.7505466018239,12.));
#208760=CARTESIAN_POINT('Ctrl Pts',(4.88335766525565,23.7694565448044,0.));
#208761=CARTESIAN_POINT('Ctrl Pts',(4.88335766525565,23.7694565448044,12.));
#208762=CARTESIAN_POINT('Ctrl Pts',(4.89582956706771,23.7884134212381,0.));
#208763=CARTESIAN_POINT('Ctrl Pts',(4.89582956706771,23.7884134212381,12.));
#208764=CARTESIAN_POINT('Ctrl Pts',(4.90840066839346,23.8074164940897,0.));
#208765=CARTESIAN_POINT('Ctrl Pts',(4.90840066839346,23.8074164940897,12.));
#208766=CARTESIAN_POINT('Ctrl Pts',(4.92107089613976,23.8264650335721,0.));
#208767=CARTESIAN_POINT('Ctrl Pts',(4.92107089613976,23.8264650335721,12.));
#208768=CARTESIAN_POINT('Ctrl Pts',(4.93384017643441,23.8455583170062,0.));
#208769=CARTESIAN_POINT('Ctrl Pts',(4.93384017643441,23.8455583170062,12.));
#208770=CARTESIAN_POINT('Ctrl Pts',(4.94670843465868,23.8646956287172,0.));
#208771=CARTESIAN_POINT('Ctrl Pts',(4.94670843465868,23.8646956287172,12.));
#208772=CARTESIAN_POINT('Ctrl Pts',(4.95967559546565,23.883876259922,0.));
#208773=CARTESIAN_POINT('Ctrl Pts',(4.95967559546565,23.883876259922,12.));
#208774=CARTESIAN_POINT('Ctrl Pts',(4.97274158279228,23.9030995086164,0.));
#208775=CARTESIAN_POINT('Ctrl Pts',(4.97274158279228,23.9030995086164,12.));
#208776=CARTESIAN_POINT('Ctrl Pts',(4.98590631986532,23.9223646794591,0.));
#208777=CARTESIAN_POINT('Ctrl Pts',(4.98590631986532,23.9223646794591,12.));
#208778=CARTESIAN_POINT('Ctrl Pts',(4.99916972919309,23.9416710836529,0.));
#208779=CARTESIAN_POINT('Ctrl Pts',(4.99916972919309,23.9416710836529,12.));
#208780=CARTESIAN_POINT('Ctrl Pts',(5.01253173257458,23.9610180388271,0.));
#208781=CARTESIAN_POINT('Ctrl Pts',(5.01253173257458,23.9610180388271,12.));
#208782=CARTESIAN_POINT('Ctrl Pts',(5.02599225112461,23.9804048689228,0.));
#208783=CARTESIAN_POINT('Ctrl Pts',(5.02599225112461,23.9804048689228,12.));
#208784=CARTESIAN_POINT('Ctrl Pts',(5.03955120528527,23.9998309040747,0.));
#208785=CARTESIAN_POINT('Ctrl Pts',(5.03955120528527,23.9998309040747,12.));
#208786=CARTESIAN_POINT('Ctrl Pts',(5.05320851483068,24.0192954804896,0.));
#208787=CARTESIAN_POINT('Ctrl Pts',(5.05320851483068,24.0192954804896,12.));
#208788=CARTESIAN_POINT('Ctrl Pts',(5.06696409886639,24.0387979403268,0.));
#208789=CARTESIAN_POINT('Ctrl Pts',(5.06696409886639,24.0387979403268,12.));
#208790=CARTESIAN_POINT('Ctrl Pts',(5.0808178758127,24.0583376315636,0.));
#208791=CARTESIAN_POINT('Ctrl Pts',(5.0808178758127,24.0583376315636,12.));
#208792=CARTESIAN_POINT('Ctrl Pts',(5.09476976342616,24.0779139079264,0.));
#208793=CARTESIAN_POINT('Ctrl Pts',(5.09476976342616,24.0779139079264,12.));
#208794=CARTESIAN_POINT('Ctrl Pts',(5.10881967883124,24.0975261288444,0.));
#208795=CARTESIAN_POINT('Ctrl Pts',(5.10881967883124,24.0975261288444,12.));
#208796=CARTESIAN_POINT('Ctrl Pts',(5.12296753853857,24.117173659394,0.));
#208797=CARTESIAN_POINT('Ctrl Pts',(5.12296753853857,24.117173659394,12.));
#208798=CARTESIAN_POINT('Ctrl Pts',(5.13721325845745,24.1368558702443,0.));
#208799=CARTESIAN_POINT('Ctrl Pts',(5.13721325845745,24.1368558702443,12.));
#208800=CARTESIAN_POINT('Ctrl Pts',(5.15155675390079,24.1565721375971,0.));
#208801=CARTESIAN_POINT('Ctrl Pts',(5.15155675390079,24.1565721375971,12.));
#208802=CARTESIAN_POINT('Ctrl Pts',(5.16599793957985,24.1763218431344,0.));
#208803=CARTESIAN_POINT('Ctrl Pts',(5.16599793957985,24.1763218431344,12.));
#208804=CARTESIAN_POINT('Ctrl Pts',(5.18053672961398,24.1961043738756,0.));
#208805=CARTESIAN_POINT('Ctrl Pts',(5.18053672961398,24.1961043738756,12.));
#208806=CARTESIAN_POINT('Ctrl Pts',(5.19517303753647,24.2159191220171,0.));
#208807=CARTESIAN_POINT('Ctrl Pts',(5.19517303753647,24.2159191220171,12.));
#208808=CARTESIAN_POINT('Ctrl Pts',(5.20990677629176,24.2357654847766,0.));
#208809=CARTESIAN_POINT('Ctrl Pts',(5.20990677629176,24.2357654847766,12.));
#208810=CARTESIAN_POINT('Ctrl Pts',(5.22473785822442,24.2556428642294,0.));
#208811=CARTESIAN_POINT('Ctrl Pts',(5.22473785822442,24.2556428642294,12.));
#208812=CARTESIAN_POINT('Ctrl Pts',(5.23966619506289,24.2755506671525,0.));
#208813=CARTESIAN_POINT('Ctrl Pts',(5.23966619506289,24.2755506671525,12.));
#208814=CARTESIAN_POINT('Ctrl Pts',(5.25469169788856,24.2954883048447,0.));
#208815=CARTESIAN_POINT('Ctrl Pts',(5.25469169788856,24.2954883048447,12.));
#208816=CARTESIAN_POINT('Ctrl Pts',(5.26981427718798,24.3154551932221,0.));
#208817=CARTESIAN_POINT('Ctrl Pts',(5.26981427718798,24.3154551932221,12.));
#208818=CARTESIAN_POINT('Ctrl Pts',(5.28503384290648,24.3354507529414,0.));
#208819=CARTESIAN_POINT('Ctrl Pts',(5.28503384290648,24.3354507529414,12.));
#208820=CARTESIAN_POINT('Ctrl Pts',(5.30035030449063,24.3554744095075,0.));
#208821=CARTESIAN_POINT('Ctrl Pts',(5.30035030449063,24.3554744095075,12.));
#208822=CARTESIAN_POINT('Ctrl Pts',(5.31576357092526,24.3755255933917,0.));
#208823=CARTESIAN_POINT('Ctrl Pts',(5.31576357092526,24.3755255933917,12.));
#208824=CARTESIAN_POINT('Ctrl Pts',(5.33127355076033,24.3956037401293,0.));
#208825=CARTESIAN_POINT('Ctrl Pts',(5.33127355076033,24.3956037401293,12.));
#208826=CARTESIAN_POINT('Ctrl Pts',(5.34688015213537,24.4157082904614,0.));
#208827=CARTESIAN_POINT('Ctrl Pts',(5.34688015213537,24.4157082904614,12.));
#208828=CARTESIAN_POINT('Ctrl Pts',(5.36258328273627,24.435838689915,0.));
#208829=CARTESIAN_POINT('Ctrl Pts',(5.36258328273627,24.435838689915,12.));
#208830=CARTESIAN_POINT('Ctrl Pts',(5.37838284973695,24.4559943883157,0.));
#208831=CARTESIAN_POINT('Ctrl Pts',(5.37838284973695,24.4559943883157,12.));
#208832=CARTESIAN_POINT('Ctrl Pts',(5.39427875973824,24.4761748393321,0.));
#208833=CARTESIAN_POINT('Ctrl Pts',(5.39427875973824,24.4761748393321,12.));
#208834=CARTESIAN_POINT('Ctrl Pts',(5.41027091869241,24.4963794999831,0.));
#208835=CARTESIAN_POINT('Ctrl Pts',(5.41027091869241,24.4963794999831,12.));
#208836=CARTESIAN_POINT('Ctrl Pts',(5.42635923183419,24.5166078302108,0.));
#208837=CARTESIAN_POINT('Ctrl Pts',(5.42635923183419,24.5166078302108,12.));
#208838=CARTESIAN_POINT('Ctrl Pts',(5.4425436035688,24.5368592922863,0.));
#208839=CARTESIAN_POINT('Ctrl Pts',(5.4425436035688,24.5368592922863,12.));
#208840=CARTESIAN_POINT('Ctrl Pts',(5.45882393762261,24.5571333514842,0.));
#208841=CARTESIAN_POINT('Ctrl Pts',(5.45882393762261,24.5571333514842,12.));
#208842=CARTESIAN_POINT('Ctrl Pts',(5.47520013724419,24.5774294770329,0.));
#208843=CARTESIAN_POINT('Ctrl Pts',(5.47520013724419,24.5774294770329,12.));
#208844=CARTESIAN_POINT('Ctrl Pts',(5.49167210537246,24.5977471429364,0.));
#208845=CARTESIAN_POINT('Ctrl Pts',(5.49167210537246,24.5977471429364,12.));
#208846=CARTESIAN_POINT('Ctrl Pts',(5.50823974481962,24.6180858289179,0.));
#208847=CARTESIAN_POINT('Ctrl Pts',(5.50823974481962,24.6180858289179,12.));
#208848=CARTESIAN_POINT('Ctrl Pts',(5.52490295840991,24.6384450211467,0.));
#208849=CARTESIAN_POINT('Ctrl Pts',(5.52490295840991,24.6384450211467,12.));
#208850=CARTESIAN_POINT('Ctrl Pts',(5.54166164919583,24.6588242134738,0.));
#208851=CARTESIAN_POINT('Ctrl Pts',(5.54166164919583,24.6588242134738,12.));
#208852=CARTESIAN_POINT('Ctrl Pts',(5.55851572025376,24.6792229061794,0.));
#208853=CARTESIAN_POINT('Ctrl Pts',(5.55851572025376,24.6792229061794,12.));
#208854=CARTESIAN_POINT('Ctrl Pts',(5.57546507427754,24.6996406035517,0.));
#208855=CARTESIAN_POINT('Ctrl Pts',(5.57546507427754,24.6996406035517,12.));
#208856=CARTESIAN_POINT('Ctrl Pts',(5.59250961323987,24.7200768119088,0.));
#208857=CARTESIAN_POINT('Ctrl Pts',(5.59250961323987,24.7200768119088,12.));
#208858=CARTESIAN_POINT('Ctrl Pts',(5.60964923798491,24.7405310372739,0.));
#208859=CARTESIAN_POINT('Ctrl Pts',(5.60964923798491,24.7405310372739,12.));
#208860=CARTESIAN_POINT('Ctrl Pts',(5.62688384790923,24.7610027835697,0.));
#208861=CARTESIAN_POINT('Ctrl Pts',(5.62688384790923,24.7610027835697,12.));
#208862=CARTESIAN_POINT('Ctrl Pts',(5.6442133404226,24.781491549672,0.));
#208863=CARTESIAN_POINT('Ctrl Pts',(5.6442133404226,24.781491549672,12.));
#208864=CARTESIAN_POINT('Ctrl Pts',(5.66163761114921,24.8019968304605,0.));
#208865=CARTESIAN_POINT('Ctrl Pts',(5.66163761114921,24.8019968304605,12.));
#208866=CARTESIAN_POINT('Ctrl Pts',(5.67915655496542,24.8225181223845,0.));
#208867=CARTESIAN_POINT('Ctrl Pts',(5.67915655496542,24.8225181223845,12.));
#208868=CARTESIAN_POINT('Ctrl Pts',(5.69677006679444,24.8430549277621,0.));
#208869=CARTESIAN_POINT('Ctrl Pts',(5.69677006679444,24.8430549277621,12.));
#208870=CARTESIAN_POINT('Ctrl Pts',(5.71447804252027,24.8636067597669,0.));
#208871=CARTESIAN_POINT('Ctrl Pts',(5.71447804252027,24.8636067597669,12.));
#208872=CARTESIAN_POINT('Ctrl Pts',(5.73228037976926,24.884173146722,0.));
#208873=CARTESIAN_POINT('Ctrl Pts',(5.73228037976926,24.884173146722,12.));
#208874=CARTESIAN_POINT('Ctrl Pts',(5.75017697890804,24.904753637648,0.));
#208875=CARTESIAN_POINT('Ctrl Pts',(5.75017697890804,24.904753637648,12.));
#208876=CARTESIAN_POINT('Ctrl Pts',(5.76816774342219,24.9253478043656,0.));
#208877=CARTESIAN_POINT('Ctrl Pts',(5.76816774342219,24.9253478043656,12.));
#208878=CARTESIAN_POINT('Ctrl Pts',(5.78625257775681,24.945955229334,0.));
#208879=CARTESIAN_POINT('Ctrl Pts',(5.78625257775681,24.945955229334,12.));
#208880=CARTESIAN_POINT('Ctrl Pts',(5.80443138549726,24.9665754954496,0.));
#208881=CARTESIAN_POINT('Ctrl Pts',(5.80443138549726,24.9665754954496,12.));
#208882=CARTESIAN_POINT('Ctrl Pts',(5.82270406744198,24.9872081752734,0.));
#208883=CARTESIAN_POINT('Ctrl Pts',(5.82270406744198,24.9872081752734,12.));
#208884=CARTESIAN_POINT('Ctrl Pts',(5.84107051963071,25.0078528200564,0.));
#208885=CARTESIAN_POINT('Ctrl Pts',(5.84107051963071,25.0078528200564,12.));
#208886=CARTESIAN_POINT('Ctrl Pts',(5.85953063156826,25.0285089498899,0.));
#208887=CARTESIAN_POINT('Ctrl Pts',(5.85953063156826,25.0285089498899,12.));
#208888=CARTESIAN_POINT('Ctrl Pts',(5.87808428385365,25.0491760405911,0.));
#208889=CARTESIAN_POINT('Ctrl Pts',(5.87808428385365,25.0491760405911,12.));
#208890=CARTESIAN_POINT('Ctrl Pts',(5.89673135155514,25.0698535426514,0.));
#208891=CARTESIAN_POINT('Ctrl Pts',(5.89673135155514,25.0698535426514,12.));
#208892=CARTESIAN_POINT('Ctrl Pts',(5.91547170844447,25.0905409050773,0.));
#208893=CARTESIAN_POINT('Ctrl Pts',(5.91547170844447,25.0905409050773,12.));
#208894=CARTESIAN_POINT('Ctrl Pts',(5.93430523086834,25.1112375971106,0.));
#208895=CARTESIAN_POINT('Ctrl Pts',(5.93430523086834,25.1112375971106,12.));
#208896=CARTESIAN_POINT('Ctrl Pts',(5.95323180187378,25.1319431317237,0.));
#208897=CARTESIAN_POINT('Ctrl Pts',(5.95323180187378,25.1319431317237,12.));
#208898=CARTESIAN_POINT('Ctrl Pts',(5.97225131495616,25.1526570863092,0.));
#208899=CARTESIAN_POINT('Ctrl Pts',(5.97225131495616,25.1526570863092,12.));
#208900=CARTESIAN_POINT('Ctrl Pts',(5.99136367859754,25.1733791296259,0.));
#208901=CARTESIAN_POINT('Ctrl Pts',(5.99136367859754,25.1733791296259,12.));
#208902=CARTESIAN_POINT('Ctrl Pts',(6.01056881804612,25.1941090269819,0.));
#208903=CARTESIAN_POINT('Ctrl Pts',(6.01056881804612,25.1941090269819,12.));
#208904=CARTESIAN_POINT('Ctrl Pts',(6.02986667389996,25.21484662016,0.));
#208905=CARTESIAN_POINT('Ctrl Pts',(6.02986667389996,25.21484662016,12.));
#208906=CARTESIAN_POINT('Ctrl Pts',(6.04925720151218,25.2355918139032,0.));
#208907=CARTESIAN_POINT('Ctrl Pts',(6.04925720151218,25.2355918139032,12.));
#208908=CARTESIAN_POINT('Ctrl Pts',(6.06484373634546,25.2521940105705,0.));
#208909=CARTESIAN_POINT('Ctrl Pts',(6.06484373634546,25.2521940105705,12.));
#208910=CARTESIAN_POINT('Ctrl Pts',(6.0765753178749,25.2646490489923,0.));
#208911=CARTESIAN_POINT('Ctrl Pts',(6.0765753178749,25.2646490489923,12.));
#208912=CARTESIAN_POINT('Ctrl Pts',(6.08441489609793,25.2729539149517,0.));
#208913=CARTESIAN_POINT('Ctrl Pts',(6.08441489609793,25.2729539149517,12.));
#208914=CARTESIAN_POINT('Ctrl Pts',(6.08833931617699,25.2771067246846,0.));
#208915=CARTESIAN_POINT('Ctrl Pts',(6.08833931617699,25.2771067246846,12.));
#208916=CARTESIAN_POINT('',(6.08833931617699,25.2771067246846,0.));
#208917=CARTESIAN_POINT('Ctrl Pts',(4.11585220600461,22.1738711152697,0.));
#208918=CARTESIAN_POINT('Ctrl Pts',(4.11585194677442,22.173877682324,0.));
#208919=CARTESIAN_POINT('Ctrl Pts',(4.11586035878287,22.1739341411687,0.));
#208920=CARTESIAN_POINT('Ctrl Pts',(4.11589976826166,22.1741488021234,0.));
#208921=CARTESIAN_POINT('Ctrl Pts',(4.11600589882845,22.1746949858775,0.));
#208922=CARTESIAN_POINT('Ctrl Pts',(4.11622797217068,22.1758088296598,0.));
#208923=CARTESIAN_POINT('Ctrl Pts',(4.11653973150518,22.177347426894,0.));
#208924=CARTESIAN_POINT('Ctrl Pts',(4.11694173195003,22.179297473024,0.));
#208925=CARTESIAN_POINT('Ctrl Pts',(4.11743469691756,22.1816414985788,0.));
#208926=CARTESIAN_POINT('Ctrl Pts',(4.11801938107479,22.1843613164855,0.));
#208927=CARTESIAN_POINT('Ctrl Pts',(4.11869641271773,22.1874419861496,0.));
#208928=CARTESIAN_POINT('Ctrl Pts',(4.11946626228636,22.1908725908525,0.));
#208929=CARTESIAN_POINT('Ctrl Pts',(4.12032932637736,22.1946440958098,0.));
#208930=CARTESIAN_POINT('Ctrl Pts',(4.12128598183522,22.1987479618246,0.));
#208931=CARTESIAN_POINT('Ctrl Pts',(4.12233664408227,22.2031746532106,0.));
#208932=CARTESIAN_POINT('Ctrl Pts',(4.12348173702023,22.2079143941719,0.));
#208933=CARTESIAN_POINT('Ctrl Pts',(4.12472167516607,22.2129576146671,0.));
#208934=CARTESIAN_POINT('Ctrl Pts',(4.12605683613307,22.2182956401341,0.));
#208935=CARTESIAN_POINT('Ctrl Pts',(4.12748755830104,22.2239207458781,0.));
#208936=CARTESIAN_POINT('Ctrl Pts',(4.12901415463379,22.2298258043947,0.));
#208937=CARTESIAN_POINT('Ctrl Pts',(4.13063692157498,22.2360040565533,0.));
#208938=CARTESIAN_POINT('Ctrl Pts',(4.1323561506016,22.2424488153523,0.));
#208939=CARTESIAN_POINT('Ctrl Pts',(4.1341721255881,22.249153531779,0.));
#208940=CARTESIAN_POINT('Ctrl Pts',(4.13608511977225,22.2561118708421,0.));
#208941=CARTESIAN_POINT('Ctrl Pts',(4.13809539255421,22.2633177913972,0.));
#208942=CARTESIAN_POINT('Ctrl Pts',(4.14020318715991,22.2707656042457,0.));
#208943=CARTESIAN_POINT('Ctrl Pts',(4.14240873321984,22.2784499072027,0.));
#208944=CARTESIAN_POINT('Ctrl Pts',(4.14471224859295,22.2863655389166,0.));
#208945=CARTESIAN_POINT('Ctrl Pts',(4.14711394168556,22.2945075198467,0.));
#208946=CARTESIAN_POINT('Ctrl Pts',(4.14961401285522,22.3028710166933,0.));
#208947=CARTESIAN_POINT('Ctrl Pts',(4.1522126539699,22.3114513545185,0.));
#208948=CARTESIAN_POINT('Ctrl Pts',(4.15491004835281,22.3202440186979,0.));
#208949=CARTESIAN_POINT('Ctrl Pts',(4.15770637047889,22.3292446628959,0.));
#208950=CARTESIAN_POINT('Ctrl Pts',(4.16060178604164,22.3384491078602,0.));
#208951=CARTESIAN_POINT('Ctrl Pts',(4.16359645263187,22.3478533253889,0.));
#208952=CARTESIAN_POINT('Ctrl Pts',(4.166690520266,22.3574534257396,0.));
#208953=CARTESIAN_POINT('Ctrl Pts',(4.16988413199457,22.36724564276,0.));
#208954=CARTESIAN_POINT('Ctrl Pts',(4.17317742436145,22.3772263228617,0.));
#208955=CARTESIAN_POINT('Ctrl Pts',(4.17657052752825,22.3873919231334,0.));
#208956=CARTESIAN_POINT('Ctrl Pts',(4.18006356544882,22.3977390078075,0.));
#208957=CARTESIAN_POINT('Ctrl Pts',(4.1836566560085,22.4082642454453,0.));
#208958=CARTESIAN_POINT('Ctrl Pts',(4.1873499111772,22.4189644056115,0.));
#208959=CARTESIAN_POINT('Ctrl Pts',(4.19114343726941,22.4298363535421,0.));
#208960=CARTESIAN_POINT('Ctrl Pts',(4.1950373351886,22.4408770448917,0.));
#208961=CARTESIAN_POINT('Ctrl Pts',(4.19903170066354,22.4520835205419,0.));
#208962=CARTESIAN_POINT('Ctrl Pts',(4.2031266244817,22.4634529011433,0.));
#208963=CARTESIAN_POINT('Ctrl Pts',(4.20732219265648,22.4749823839915,0.));
#208964=CARTESIAN_POINT('Ctrl Pts',(4.21161848657428,22.4866692403147,0.));
#208965=CARTESIAN_POINT('Ctrl Pts',(4.21601558313908,22.4985108124229,0.));
#208966=CARTESIAN_POINT('Ctrl Pts',(4.22051355490196,22.5105045108882,0.));
#208967=CARTESIAN_POINT('Ctrl Pts',(4.2251124702004,22.5226478117885,0.));
#208968=CARTESIAN_POINT('Ctrl Pts',(4.22981239330731,22.5349382540587,0.));
#208969=CARTESIAN_POINT('Ctrl Pts',(4.23461338456713,22.5473734368086,0.));
#208970=CARTESIAN_POINT('Ctrl Pts',(4.23951550052526,22.559951016643,0.));
#208971=CARTESIAN_POINT('Ctrl Pts',(4.24451879404858,22.5726687049922,0.));
#208972=CARTESIAN_POINT('Ctrl Pts',(4.24962331444184,22.5855242662479,0.));
#208973=CARTESIAN_POINT('Ctrl Pts',(4.25482910755485,22.5985155158637,0.));
#208974=CARTESIAN_POINT('Ctrl Pts',(4.26013621588303,22.611640318482,0.));
#208975=CARTESIAN_POINT('Ctrl Pts',(4.26554467865571,22.6248965859975,0.));
#208976=CARTESIAN_POINT('Ctrl Pts',(4.27105453192999,22.6382822758171,0.));
#208977=CARTESIAN_POINT('Ctrl Pts',(4.27666580869117,22.6517953893303,0.));
#208978=CARTESIAN_POINT('Ctrl Pts',(4.28237853894059,22.665433970311,0.));
#208979=CARTESIAN_POINT('Ctrl Pts',(4.28819274977766,22.6791961033537,0.));
#208980=CARTESIAN_POINT('Ctrl Pts',(4.29410846547061,22.6930799122545,0.));
#208981=CARTESIAN_POINT('Ctrl Pts',(4.30012570754066,22.707083558756,0.));
#208982=CARTESIAN_POINT('Ctrl Pts',(4.30624449484074,22.7212052413384,0.));
#208983=CARTESIAN_POINT('Ctrl Pts',(4.3124648436255,22.7354431939927,0.));
#208984=CARTESIAN_POINT('Ctrl Pts',(4.3187867676123,22.7497956849852,0.));
#208985=CARTESIAN_POINT('Ctrl Pts',(4.32521027803747,22.764261015648,0.));
#208986=CARTESIAN_POINT('Ctrl Pts',(4.33173538373182,22.7788375194081,0.));
#208987=CARTESIAN_POINT('Ctrl Pts',(4.33836209118442,22.7935235607807,0.));
#208988=CARTESIAN_POINT('Ctrl Pts',(4.34509040460065,22.808317534379,0.));
#208989=CARTESIAN_POINT('Ctrl Pts',(4.35192032594801,22.8232178638873,0.));
#208990=CARTESIAN_POINT('Ctrl Pts',(4.35885185500559,22.838223001118,0.));
#208991=CARTESIAN_POINT('Ctrl Pts',(4.36588498943009,22.8533314252419,0.));
#208992=CARTESIAN_POINT('Ctrl Pts',(4.37301972480752,22.8685416419725,0.));
#208993=CARTESIAN_POINT('Ctrl Pts',(4.38025605470089,22.8838521827702,0.));
#208994=CARTESIAN_POINT('Ctrl Pts',(4.38759397068391,22.8992616040108,0.));
#208995=CARTESIAN_POINT('Ctrl Pts',(4.39503346238454,22.9147684862425,0.));
#208996=CARTESIAN_POINT('Ctrl Pts',(4.40257451754307,22.9303714335549,0.));
#208997=CARTESIAN_POINT('Ctrl Pts',(4.41021712205547,22.9460690729093,0.));
#208998=CARTESIAN_POINT('Ctrl Pts',(4.41796126001309,22.9618600534866,0.));
#208999=CARTESIAN_POINT('Ctrl Pts',(4.42580691372771,22.9777430460021,0.));
#209000=CARTESIAN_POINT('Ctrl Pts',(4.43375406376904,22.9937167421009,0.));
#209001=CARTESIAN_POINT('Ctrl Pts',(4.44180268901666,23.0097798538399,0.));
#209002=CARTESIAN_POINT('Ctrl Pts',(4.44995276669698,23.0259311131395,0.));
#209003=CARTESIAN_POINT('Ctrl Pts',(4.45820427241676,23.0421692712466,0.));
#209004=CARTESIAN_POINT('Ctrl Pts',(4.46655718018205,23.0584930981723,0.));
#209005=CARTESIAN_POINT('Ctrl Pts',(4.47501146242821,23.0749013821868,0.));
#209006=CARTESIAN_POINT('Ctrl Pts',(4.48356709006756,23.0913929293909,0.));
#209007=CARTESIAN_POINT('Ctrl Pts',(4.49222403252201,23.1079665632629,0.));
#209008=CARTESIAN_POINT('Ctrl Pts',(4.50098225775178,23.1246211242117,0.));
#209009=CARTESIAN_POINT('Ctrl Pts',(4.50984173227087,23.1413554691136,0.));
#209010=CARTESIAN_POINT('Ctrl Pts',(4.51880242116785,23.1581684708778,0.));
#209011=CARTESIAN_POINT('Ctrl Pts',(4.52786428815047,23.1750590180923,0.));
#209012=CARTESIAN_POINT('Ctrl Pts',(4.53702729557585,23.1920260146474,0.));
#209013=CARTESIAN_POINT('Ctrl Pts',(4.54629140447542,23.2090683793627,0.));
#209014=CARTESIAN_POINT('Ctrl Pts',(4.55565657456956,23.2261850456055,0.));
#209015=CARTESIAN_POINT('Ctrl Pts',(4.5651227642781,23.2433749609117,0.));
#209016=CARTESIAN_POINT('Ctrl Pts',(4.5746899307607,23.2606370866853,0.));
#209017=CARTESIAN_POINT('Ctrl Pts',(4.58435802994674,23.2779703978868,0.));
#209018=CARTESIAN_POINT('Ctrl Pts',(4.59412701655749,23.295373882719,0.));
#209019=CARTESIAN_POINT('Ctrl Pts',(4.60399684412174,23.3128465423119,0.));
#209020=CARTESIAN_POINT('Ctrl Pts',(4.61396746497848,23.3303873903947,0.));
#209021=CARTESIAN_POINT('Ctrl Pts',(4.62403883030823,23.3479954530281,0.));
#209022=CARTESIAN_POINT('Ctrl Pts',(4.63421089016554,23.3656697683496,0.));
#209023=CARTESIAN_POINT('Ctrl Pts',(4.64448359349935,23.383409386307,0.));
#209024=CARTESIAN_POINT('Ctrl Pts',(4.65485688816921,23.4012133683957,0.));
#209025=CARTESIAN_POINT('Ctrl Pts',(4.66533072094663,23.4190807873798,0.));
#209026=CARTESIAN_POINT('Ctrl Pts',(4.6759050375305,23.4370107270444,0.));
#209027=CARTESIAN_POINT('Ctrl Pts',(4.68657978258297,23.4550022819853,0.));
#209028=CARTESIAN_POINT('Ctrl Pts',(4.69735489975023,23.4730545573849,0.));
#209029=CARTESIAN_POINT('Ctrl Pts',(4.7082303316782,23.491166668789,0.));
#209030=CARTESIAN_POINT('Ctrl Pts',(4.71920602001904,23.5093377418784,0.));
#209031=CARTESIAN_POINT('Ctrl Pts',(4.73028190543031,23.5275669122378,0.));
#209032=CARTESIAN_POINT('Ctrl Pts',(4.74145792760698,23.5458533251715,0.));
#209033=CARTESIAN_POINT('Ctrl Pts',(4.75273402530615,23.564196135517,0.));
#209034=CARTESIAN_POINT('Ctrl Pts',(4.7641101363625,23.5825945074535,0.));
#209035=CARTESIAN_POINT('Ctrl Pts',(4.77558619769875,23.6010476143099,0.));
#209036=CARTESIAN_POINT('Ctrl Pts',(4.78716214532104,23.6195546383625,0.));
#209037=CARTESIAN_POINT('Ctrl Pts',(4.79883791433229,23.6381147706581,0.));
#209038=CARTESIAN_POINT('Ctrl Pts',(4.81061343896442,23.6567272108631,0.));
#209039=CARTESIAN_POINT('Ctrl Pts',(4.82248865259569,23.6753911671023,0.));
#209040=CARTESIAN_POINT('Ctrl Pts',(4.83446348776267,23.6941058557971,0.));
#209041=CARTESIAN_POINT('Ctrl Pts',(4.84653787616422,23.7128705015014,0.));
#209042=CARTESIAN_POINT('Ctrl Pts',(4.85871174865491,23.7316843367308,0.));
#209043=CARTESIAN_POINT('Ctrl Pts',(4.87098503527142,23.7505466018239,0.));
#209044=CARTESIAN_POINT('Ctrl Pts',(4.88335766525565,23.7694565448044,0.));
#209045=CARTESIAN_POINT('Ctrl Pts',(4.89582956706771,23.7884134212381,0.));
#209046=CARTESIAN_POINT('Ctrl Pts',(4.90840066839346,23.8074164940897,0.));
#209047=CARTESIAN_POINT('Ctrl Pts',(4.92107089613976,23.8264650335721,0.));
#209048=CARTESIAN_POINT('Ctrl Pts',(4.93384017643441,23.8455583170062,0.));
#209049=CARTESIAN_POINT('Ctrl Pts',(4.94670843465868,23.8646956287172,0.));
#209050=CARTESIAN_POINT('Ctrl Pts',(4.95967559546565,23.883876259922,0.));
#209051=CARTESIAN_POINT('Ctrl Pts',(4.97274158279228,23.9030995086164,0.));
#209052=CARTESIAN_POINT('Ctrl Pts',(4.98590631986532,23.9223646794591,0.));
#209053=CARTESIAN_POINT('Ctrl Pts',(4.99916972919309,23.9416710836529,0.));
#209054=CARTESIAN_POINT('Ctrl Pts',(5.01253173257458,23.9610180388271,0.));
#209055=CARTESIAN_POINT('Ctrl Pts',(5.02599225112461,23.9804048689228,0.));
#209056=CARTESIAN_POINT('Ctrl Pts',(5.03955120528527,23.9998309040747,0.));
#209057=CARTESIAN_POINT('Ctrl Pts',(5.05320851483068,24.0192954804896,0.));
#209058=CARTESIAN_POINT('Ctrl Pts',(5.06696409886639,24.0387979403268,0.));
#209059=CARTESIAN_POINT('Ctrl Pts',(5.0808178758127,24.0583376315636,0.));
#209060=CARTESIAN_POINT('Ctrl Pts',(5.09476976342616,24.0779139079264,0.));
#209061=CARTESIAN_POINT('Ctrl Pts',(5.10881967883124,24.0975261288444,0.));
#209062=CARTESIAN_POINT('Ctrl Pts',(5.12296753853857,24.117173659394,0.));
#209063=CARTESIAN_POINT('Ctrl Pts',(5.13721325845745,24.1368558702443,0.));
#209064=CARTESIAN_POINT('Ctrl Pts',(5.15155675390079,24.1565721375971,0.));
#209065=CARTESIAN_POINT('Ctrl Pts',(5.16599793957985,24.1763218431344,0.));
#209066=CARTESIAN_POINT('Ctrl Pts',(5.18053672961398,24.1961043738756,0.));
#209067=CARTESIAN_POINT('Ctrl Pts',(5.19517303753647,24.2159191220171,0.));
#209068=CARTESIAN_POINT('Ctrl Pts',(5.20990677629176,24.2357654847766,0.));
#209069=CARTESIAN_POINT('Ctrl Pts',(5.22473785822442,24.2556428642294,0.));
#209070=CARTESIAN_POINT('Ctrl Pts',(5.23966619506289,24.2755506671525,0.));
#209071=CARTESIAN_POINT('Ctrl Pts',(5.25469169788856,24.2954883048447,0.));
#209072=CARTESIAN_POINT('Ctrl Pts',(5.26981427718798,24.3154551932221,0.));
#209073=CARTESIAN_POINT('Ctrl Pts',(5.28503384290648,24.3354507529414,0.));
#209074=CARTESIAN_POINT('Ctrl Pts',(5.30035030449063,24.3554744095075,0.));
#209075=CARTESIAN_POINT('Ctrl Pts',(5.31576357092526,24.3755255933917,0.));
#209076=CARTESIAN_POINT('Ctrl Pts',(5.33127355076033,24.3956037401293,0.));
#209077=CARTESIAN_POINT('Ctrl Pts',(5.34688015213537,24.4157082904614,0.));
#209078=CARTESIAN_POINT('Ctrl Pts',(5.36258328273627,24.435838689915,0.));
#209079=CARTESIAN_POINT('Ctrl Pts',(5.37838284973695,24.4559943883157,0.));
#209080=CARTESIAN_POINT('Ctrl Pts',(5.39427875973824,24.4761748393321,0.));
#209081=CARTESIAN_POINT('Ctrl Pts',(5.41027091869241,24.4963794999831,0.));
#209082=CARTESIAN_POINT('Ctrl Pts',(5.42635923183419,24.5166078302108,0.));
#209083=CARTESIAN_POINT('Ctrl Pts',(5.4425436035688,24.5368592922863,0.));
#209084=CARTESIAN_POINT('Ctrl Pts',(5.45882393762261,24.5571333514842,0.));
#209085=CARTESIAN_POINT('Ctrl Pts',(5.47520013724419,24.5774294770329,0.));
#209086=CARTESIAN_POINT('Ctrl Pts',(5.49167210537246,24.5977471429364,0.));
#209087=CARTESIAN_POINT('Ctrl Pts',(5.50823974481962,24.6180858289179,0.));
#209088=CARTESIAN_POINT('Ctrl Pts',(5.52490295840991,24.6384450211467,0.));
#209089=CARTESIAN_POINT('Ctrl Pts',(5.54166164919583,24.6588242134738,0.));
#209090=CARTESIAN_POINT('Ctrl Pts',(5.55851572025376,24.6792229061794,0.));
#209091=CARTESIAN_POINT('Ctrl Pts',(5.57546507427754,24.6996406035517,0.));
#209092=CARTESIAN_POINT('Ctrl Pts',(5.59250961323987,24.7200768119088,0.));
#209093=CARTESIAN_POINT('Ctrl Pts',(5.60964923798491,24.7405310372739,0.));
#209094=CARTESIAN_POINT('Ctrl Pts',(5.62688384790923,24.7610027835697,0.));
#209095=CARTESIAN_POINT('Ctrl Pts',(5.6442133404226,24.781491549672,0.));
#209096=CARTESIAN_POINT('Ctrl Pts',(5.66163761114921,24.8019968304605,0.));
#209097=CARTESIAN_POINT('Ctrl Pts',(5.67915655496542,24.8225181223845,0.));
#209098=CARTESIAN_POINT('Ctrl Pts',(5.69677006679444,24.8430549277621,0.));
#209099=CARTESIAN_POINT('Ctrl Pts',(5.71447804252027,24.8636067597669,0.));
#209100=CARTESIAN_POINT('Ctrl Pts',(5.73228037976926,24.884173146722,0.));
#209101=CARTESIAN_POINT('Ctrl Pts',(5.75017697890804,24.904753637648,0.));
#209102=CARTESIAN_POINT('Ctrl Pts',(5.76816774342219,24.9253478043656,0.));
#209103=CARTESIAN_POINT('Ctrl Pts',(5.78625257775681,24.945955229334,0.));
#209104=CARTESIAN_POINT('Ctrl Pts',(5.80443138549726,24.9665754954496,0.));
#209105=CARTESIAN_POINT('Ctrl Pts',(5.82270406744198,24.9872081752734,0.));
#209106=CARTESIAN_POINT('Ctrl Pts',(5.84107051963071,25.0078528200564,0.));
#209107=CARTESIAN_POINT('Ctrl Pts',(5.85953063156826,25.0285089498899,0.));
#209108=CARTESIAN_POINT('Ctrl Pts',(5.87808428385365,25.0491760405911,0.));
#209109=CARTESIAN_POINT('Ctrl Pts',(5.89673135155514,25.0698535426514,0.));
#209110=CARTESIAN_POINT('Ctrl Pts',(5.91547170844447,25.0905409050773,0.));
#209111=CARTESIAN_POINT('Ctrl Pts',(5.93430523086834,25.1112375971106,0.));
#209112=CARTESIAN_POINT('Ctrl Pts',(5.95323180187378,25.1319431317237,0.));
#209113=CARTESIAN_POINT('Ctrl Pts',(5.97225131495616,25.1526570863092,0.));
#209114=CARTESIAN_POINT('Ctrl Pts',(5.99136367859754,25.1733791296259,0.));
#209115=CARTESIAN_POINT('Ctrl Pts',(6.01056881804612,25.1941090269819,0.));
#209116=CARTESIAN_POINT('Ctrl Pts',(6.02986667389996,25.21484662016,0.));
#209117=CARTESIAN_POINT('Ctrl Pts',(6.04925720151218,25.2355918139032,0.));
#209118=CARTESIAN_POINT('Ctrl Pts',(6.06484373634546,25.2521940105705,0.));
#209119=CARTESIAN_POINT('Ctrl Pts',(6.0765753178749,25.2646490489923,0.));
#209120=CARTESIAN_POINT('Ctrl Pts',(6.08441489609793,25.2729539149517,0.));
#209121=CARTESIAN_POINT('Ctrl Pts',(6.08833931617699,25.2771067246846,0.));
#209122=CARTESIAN_POINT('',(6.08833931617699,25.2771067246846,0.));
#209123=CARTESIAN_POINT('Origin',(9.26120677397564,19.4030938020118,0.));
#209124=CARTESIAN_POINT('',(9.71462809124917,20.353053841303,0.));
#209125=CARTESIAN_POINT('',(9.71462809124917,20.353053841303,0.));
#209126=CARTESIAN_POINT('',(4.63060338698782,9.70154690100589,0.));
#209127=CARTESIAN_POINT('Ctrl Pts',(7.36589684767344,24.9347862158358,0.));
#209128=CARTESIAN_POINT('Ctrl Pts',(7.36589684767344,24.9347862158358,12.));
#209129=CARTESIAN_POINT('Ctrl Pts',(7.36721909028842,24.9292275670674,0.));
#209130=CARTESIAN_POINT('Ctrl Pts',(7.36721909028842,24.9292275670674,12.));
#209131=CARTESIAN_POINT('Ctrl Pts',(7.3698559312009,24.9181155530543,0.));
#209132=CARTESIAN_POINT('Ctrl Pts',(7.3698559312009,24.9181155530543,12.));
#209133=CARTESIAN_POINT('Ctrl Pts',(7.37378825961676,24.901463382605,0.));
#209134=CARTESIAN_POINT('Ctrl Pts',(7.37378825961676,24.901463382605,12.));
#209135=CARTESIAN_POINT('Ctrl Pts',(7.37898549640269,24.8792921911115,0.));
#209136=CARTESIAN_POINT('Ctrl Pts',(7.37898549640269,24.8792921911115,12.));
#209137=CARTESIAN_POINT('Ctrl Pts',(7.3854055890362,24.8516310625176,0.));
#209138=CARTESIAN_POINT('Ctrl Pts',(7.3854055890362,24.8516310625176,12.));
#209139=CARTESIAN_POINT('Ctrl Pts',(7.39174922585808,24.8240228520893,0.));
#209140=CARTESIAN_POINT('Ctrl Pts',(7.39174922585808,24.8240228520893,12.));
#209141=CARTESIAN_POINT('Ctrl Pts',(7.39801641583012,24.7964676646431,0.));
#209142=CARTESIAN_POINT('Ctrl Pts',(7.39801641583012,24.7964676646431,12.));
#209143=CARTESIAN_POINT('Ctrl Pts',(7.40420718661602,24.7689656668983,0.));
#209144=CARTESIAN_POINT('Ctrl Pts',(7.40420718661602,24.7689656668983,12.));
#209145=CARTESIAN_POINT('Ctrl Pts',(7.41032159082381,24.7415170994784,0.));
#209146=CARTESIAN_POINT('Ctrl Pts',(7.41032159082381,24.7415170994784,12.));
#209147=CARTESIAN_POINT('Ctrl Pts',(7.41635971481674,24.7141222950051,0.));
#209148=CARTESIAN_POINT('Ctrl Pts',(7.41635971481674,24.7141222950051,12.));
#209149=CARTESIAN_POINT('Ctrl Pts',(7.42232167766265,24.6867816727192,0.));
#209150=CARTESIAN_POINT('Ctrl Pts',(7.42232167766265,24.6867816727192,12.));
#209151=CARTESIAN_POINT('Ctrl Pts',(7.42820762159125,24.6594957128756,0.));
#209152=CARTESIAN_POINT('Ctrl Pts',(7.42820762159125,24.6594957128756,12.));
#209153=CARTESIAN_POINT('Ctrl Pts',(7.43401770489523,24.6322649369517,0.));
#209154=CARTESIAN_POINT('Ctrl Pts',(7.43401770489523,24.6322649369517,12.));
#209155=CARTESIAN_POINT('Ctrl Pts',(7.43975209375503,24.6050898852368,0.));
#209156=CARTESIAN_POINT('Ctrl Pts',(7.43975209375503,24.6050898852368,12.));
#209157=CARTESIAN_POINT('Ctrl Pts',(7.44541095473134,24.577971096086,0.));
#209158=CARTESIAN_POINT('Ctrl Pts',(7.44541095473134,24.577971096086,12.));
#209159=CARTESIAN_POINT('Ctrl Pts',(7.4509944465116,24.5509090831559,0.));
#209160=CARTESIAN_POINT('Ctrl Pts',(7.4509944465116,24.5509090831559,12.));
#209161=CARTESIAN_POINT('Ctrl Pts',(7.45650271335861,24.5239043173072,0.));
#209162=CARTESIAN_POINT('Ctrl Pts',(7.45650271335861,24.5239043173072,12.));
#209163=CARTESIAN_POINT('Ctrl Pts',(7.46193588961463,24.4969572391483,0.));
#209164=CARTESIAN_POINT('Ctrl Pts',(7.46193588961463,24.4969572391483,12.));
#209165=CARTESIAN_POINT('Ctrl Pts',(7.46729410308786,24.4700682684524,0.));
#209166=CARTESIAN_POINT('Ctrl Pts',(7.46729410308786,24.4700682684524,12.));
#209167=CARTESIAN_POINT('Ctrl Pts',(7.47257747883246,24.443237814649,0.));
#209168=CARTESIAN_POINT('Ctrl Pts',(7.47257747883246,24.443237814649,12.));
#209169=CARTESIAN_POINT('Ctrl Pts',(7.47778614286564,24.4164662871163,0.));
#209170=CARTESIAN_POINT('Ctrl Pts',(7.47778614286564,24.4164662871163,12.));
#209171=CARTESIAN_POINT('Ctrl Pts',(7.482920225693,24.3897541049254,0.));
#209172=CARTESIAN_POINT('Ctrl Pts',(7.482920225693,24.3897541049254,12.));
#209173=CARTESIAN_POINT('Ctrl Pts',(7.48797986651908,24.3631017084524,0.));
#209174=CARTESIAN_POINT('Ctrl Pts',(7.48797986651908,24.3631017084524,12.));
#209175=CARTESIAN_POINT('Ctrl Pts',(7.4929652125242,24.3365095573685,0.));
#209176=CARTESIAN_POINT('Ctrl Pts',(7.4929652125242,24.3365095573685,12.));
#209177=CARTESIAN_POINT('Ctrl Pts',(7.49787641695438,24.3099781253355,0.));
#209178=CARTESIAN_POINT('Ctrl Pts',(7.49787641695438,24.3099781253355,12.));
#209179=CARTESIAN_POINT('Ctrl Pts',(7.50271363765151,24.2835078958973,0.));
#209180=CARTESIAN_POINT('Ctrl Pts',(7.50271363765151,24.2835078958973,12.));
#209181=CARTESIAN_POINT('Ctrl Pts',(7.50747703535133,24.2570993577034,0.));
#209182=CARTESIAN_POINT('Ctrl Pts',(7.50747703535133,24.2570993577034,12.));
#209183=CARTESIAN_POINT('Ctrl Pts',(7.5121667722218,24.2307530003887,0.));
#209184=CARTESIAN_POINT('Ctrl Pts',(7.5121667722218,24.2307530003887,12.));
#209185=CARTESIAN_POINT('Ctrl Pts',(7.51678300997949,24.2044693092349,0.));
#209186=CARTESIAN_POINT('Ctrl Pts',(7.51678300997949,24.2044693092349,12.));
#209187=CARTESIAN_POINT('Ctrl Pts',(7.52132590953801,24.1782487641594,0.));
#209188=CARTESIAN_POINT('Ctrl Pts',(7.52132590953801,24.1782487641594,12.));
#209189=CARTESIAN_POINT('Ctrl Pts',(7.52579563201423,24.1520918425364,0.));
#209190=CARTESIAN_POINT('Ctrl Pts',(7.52579563201423,24.1520918425364,12.));
#209191=CARTESIAN_POINT('Ctrl Pts',(7.53019233935501,24.1259990209207,0.));
#209192=CARTESIAN_POINT('Ctrl Pts',(7.53019233935501,24.1259990209207,12.));
#209193=CARTESIAN_POINT('Ctrl Pts',(7.53451619514649,24.0999707772642,0.));
#209194=CARTESIAN_POINT('Ctrl Pts',(7.53451619514649,24.0999707772642,12.));
#209195=CARTESIAN_POINT('Ctrl Pts',(7.53876736531013,24.0740075927985,0.));
#209196=CARTESIAN_POINT('Ctrl Pts',(7.53876736531013,24.0740075927985,12.));
#209197=CARTESIAN_POINT('Ctrl Pts',(7.54294601896144,24.0481099543353,0.));
#209198=CARTESIAN_POINT('Ctrl Pts',(7.54294601896144,24.0481099543353,12.));
#209199=CARTESIAN_POINT('Ctrl Pts',(7.5470523288591,24.022278355453,0.));
#209200=CARTESIAN_POINT('Ctrl Pts',(7.5470523288591,24.022278355453,12.));
#209201=CARTESIAN_POINT('Ctrl Pts',(7.5510864709744,23.9965132953185,0.));
#209202=CARTESIAN_POINT('Ctrl Pts',(7.5510864709744,23.9965132953185,12.));
#209203=CARTESIAN_POINT('Ctrl Pts',(7.55504862424811,23.9708152779884,0.));
#209204=CARTESIAN_POINT('Ctrl Pts',(7.55504862424811,23.9708152779884,12.));
#209205=CARTESIAN_POINT('Ctrl Pts',(7.55893897027682,23.9451848115,0.));
#209206=CARTESIAN_POINT('Ctrl Pts',(7.55893897027682,23.9451848115,12.));
#209207=CARTESIAN_POINT('Ctrl Pts',(7.56275769304773,23.9196224070759,0.));
#209208=CARTESIAN_POINT('Ctrl Pts',(7.56275769304773,23.9196224070759,12.));
#209209=CARTESIAN_POINT('Ctrl Pts',(7.56650497863791,23.8941285782003,0.));
#209210=CARTESIAN_POINT('Ctrl Pts',(7.56650497863791,23.8941285782003,12.));
#209211=CARTESIAN_POINT('Ctrl Pts',(7.5701810150071,23.8687038399598,0.));
#209212=CARTESIAN_POINT('Ctrl Pts',(7.5701810150071,23.8687038399598,12.));
#209213=CARTESIAN_POINT('Ctrl Pts',(7.57378599219816,23.8433487096134,0.));
#209214=CARTESIAN_POINT('Ctrl Pts',(7.57378599219816,23.8433487096134,12.));
#209215=CARTESIAN_POINT('Ctrl Pts',(7.57732010249065,23.8180637069977,0.));
#209216=CARTESIAN_POINT('Ctrl Pts',(7.57732010249065,23.8180637069977,12.));
#209217=CARTESIAN_POINT('Ctrl Pts',(7.58078354058211,23.7928493549908,0.));
#209218=CARTESIAN_POINT('Ctrl Pts',(7.58078354058211,23.7928493549908,12.));
#209219=CARTESIAN_POINT('Ctrl Pts',(7.58417650376271,23.7677061799376,0.));
#209220=CARTESIAN_POINT('Ctrl Pts',(7.58417650376271,23.7677061799376,12.));
#209221=CARTESIAN_POINT('Ctrl Pts',(7.58749919210831,23.7426347121006,0.));
#209222=CARTESIAN_POINT('Ctrl Pts',(7.58749919210831,23.7426347121006,12.));
#209223=CARTESIAN_POINT('Ctrl Pts',(7.59075180865326,23.7176354860457,0.));
#209224=CARTESIAN_POINT('Ctrl Pts',(7.59075180865326,23.7176354860457,12.));
#209225=CARTESIAN_POINT('Ctrl Pts',(7.59393455934041,23.6927090405067,0.));
#209226=CARTESIAN_POINT('Ctrl Pts',(7.59393455934041,23.6927090405067,12.));
#209227=CARTESIAN_POINT('Ctrl Pts',(7.59704765299572,23.6678559182876,0.));
#209228=CARTESIAN_POINT('Ctrl Pts',(7.59704765299572,23.6678559182876,12.));
#209229=CARTESIAN_POINT('Ctrl Pts',(7.60009130130129,23.6430766661419,0.));
#209230=CARTESIAN_POINT('Ctrl Pts',(7.60009130130129,23.6430766661419,12.));
#209231=CARTESIAN_POINT('Ctrl Pts',(7.60306571877806,23.6183718346576,0.));
#209232=CARTESIAN_POINT('Ctrl Pts',(7.60306571877806,23.6183718346576,12.));
#209233=CARTESIAN_POINT('Ctrl Pts',(7.60597112277094,23.5937419781244,0.));
#209234=CARTESIAN_POINT('Ctrl Pts',(7.60597112277094,23.5937419781244,12.));
#209235=CARTESIAN_POINT('Ctrl Pts',(7.60880773344599,23.5691876544243,0.));
#209236=CARTESIAN_POINT('Ctrl Pts',(7.60880773344599,23.5691876544243,12.));
#209237=CARTESIAN_POINT('Ctrl Pts',(7.61157577385371,23.5447094252029,0.));
#209238=CARTESIAN_POINT('Ctrl Pts',(7.61157577385371,23.5447094252029,12.));
#209239=CARTESIAN_POINT('Ctrl Pts',(7.61427546999298,23.5203078560128,0.));
#209240=CARTESIAN_POINT('Ctrl Pts',(7.61427546999298,23.5203078560128,12.));
#209241=CARTESIAN_POINT('Ctrl Pts',(7.61690705088318,23.4959835164608,0.));
#209242=CARTESIAN_POINT('Ctrl Pts',(7.61690705088318,23.4959835164608,12.));
#209243=CARTESIAN_POINT('Ctrl Pts',(7.61947074863977,23.4717369803438,0.));
#209244=CARTESIAN_POINT('Ctrl Pts',(7.61947074863977,23.4717369803438,12.));
#209245=CARTESIAN_POINT('Ctrl Pts',(7.62196679855957,23.4475688257855,0.));
#209246=CARTESIAN_POINT('Ctrl Pts',(7.62196679855957,23.4475688257855,12.));
#209247=CARTESIAN_POINT('Ctrl Pts',(7.62439543920053,23.4234796353544,0.));
#209248=CARTESIAN_POINT('Ctrl Pts',(7.62439543920053,23.4234796353544,12.));
#209249=CARTESIAN_POINT('Ctrl Pts',(7.62675691240334,23.3994699961122,0.));
#209250=CARTESIAN_POINT('Ctrl Pts',(7.62675691240334,23.3994699961122,12.));
#209251=CARTESIAN_POINT('Ctrl Pts',(7.62905146332597,23.3755404996638,0.));
#209252=CARTESIAN_POINT('Ctrl Pts',(7.62905146332597,23.3755404996638,12.));
#209253=CARTESIAN_POINT('Ctrl Pts',(7.63127934048138,23.3516917421973,0.));
#209254=CARTESIAN_POINT('Ctrl Pts',(7.63127934048138,23.3516917421973,12.));
#209255=CARTESIAN_POINT('Ctrl Pts',(7.63344079578162,23.3279243245241,0.));
#209256=CARTESIAN_POINT('Ctrl Pts',(7.63344079578162,23.3279243245241,12.));
#209257=CARTESIAN_POINT('Ctrl Pts',(7.63553608458783,23.3042388521021,0.));
#209258=CARTESIAN_POINT('Ctrl Pts',(7.63553608458783,23.3042388521021,12.));
#209259=CARTESIAN_POINT('Ctrl Pts',(7.63756546576374,23.2806359350853,0.));
#209260=CARTESIAN_POINT('Ctrl Pts',(7.63756546576374,23.2806359350853,12.));
#209261=CARTESIAN_POINT('Ctrl Pts',(7.63952920172837,23.2571161884487,0.));
#209262=CARTESIAN_POINT('Ctrl Pts',(7.63952920172837,23.2571161884487,12.));
#209263=CARTESIAN_POINT('Ctrl Pts',(7.64142755851507,23.2336802320912,0.));
#209264=CARTESIAN_POINT('Ctrl Pts',(7.64142755851507,23.2336802320912,12.));
#209265=CARTESIAN_POINT('Ctrl Pts',(7.64326080583683,23.2103286909399,0.));
#209266=CARTESIAN_POINT('Ctrl Pts',(7.64326080583683,23.2103286909399,12.));
#209267=CARTESIAN_POINT('Ctrl Pts',(7.64502921715482,23.1870621950452,0.));
#209268=CARTESIAN_POINT('Ctrl Pts',(7.64502921715482,23.1870621950452,12.));
#209269=CARTESIAN_POINT('Ctrl Pts',(7.64673306975796,23.1638813796691,0.));
#209270=CARTESIAN_POINT('Ctrl Pts',(7.64673306975796,23.1638813796691,12.));
#209271=CARTESIAN_POINT('Ctrl Pts',(7.64837264482929,23.1407868853815,0.));
#209272=CARTESIAN_POINT('Ctrl Pts',(7.64837264482929,23.1407868853815,12.));
#209273=CARTESIAN_POINT('Ctrl Pts',(7.64994822749844,23.1177793581674,0.));
#209274=CARTESIAN_POINT('Ctrl Pts',(7.64994822749844,23.1177793581674,12.));
#209275=CARTESIAN_POINT('Ctrl Pts',(7.65146010690464,23.0948594495246,0.));
#209276=CARTESIAN_POINT('Ctrl Pts',(7.65146010690464,23.0948594495246,12.));
#209277=CARTESIAN_POINT('Ctrl Pts',(7.65290857626356,23.072027816555,0.));
#209278=CARTESIAN_POINT('Ctrl Pts',(7.65290857626356,23.072027816555,12.));
#209279=CARTESIAN_POINT('Ctrl Pts',(7.65429393293955,23.049285122053,0.));
#209280=CARTESIAN_POINT('Ctrl Pts',(7.65429393293955,23.049285122053,12.));
#209281=CARTESIAN_POINT('Ctrl Pts',(7.65561647852554,23.0266320345792,0.));
#209282=CARTESIAN_POINT('Ctrl Pts',(7.65561647852554,23.0266320345792,12.));
#209283=CARTESIAN_POINT('Ctrl Pts',(7.6568765189133,23.004069228582,0.));
#209284=CARTESIAN_POINT('Ctrl Pts',(7.6568765189133,23.004069228582,12.));
#209285=CARTESIAN_POINT('Ctrl Pts',(7.65807436436452,22.9815973845301,0.));
#209286=CARTESIAN_POINT('Ctrl Pts',(7.65807436436452,22.9815973845301,12.));
#209287=CARTESIAN_POINT('Ctrl Pts',(7.65921032958911,22.9592171890332,0.));
#209288=CARTESIAN_POINT('Ctrl Pts',(7.65921032958911,22.9592171890332,12.));
#209289=CARTESIAN_POINT('Ctrl Pts',(7.66028473382776,22.9369293349592,0.));
#209290=CARTESIAN_POINT('Ctrl Pts',(7.66028473382776,22.9369293349592,12.));
#209291=CARTESIAN_POINT('Ctrl Pts',(7.66129790094099,22.9147345215418,0.));
#209292=CARTESIAN_POINT('Ctrl Pts',(7.66129790094099,22.9147345215418,12.));
#209293=CARTESIAN_POINT('Ctrl Pts',(7.66225015950147,22.8926334544879,0.));
#209294=CARTESIAN_POINT('Ctrl Pts',(7.66225015950147,22.8926334544879,12.));
#209295=CARTESIAN_POINT('Ctrl Pts',(7.66314184287333,22.870626846128,0.));
#209296=CARTESIAN_POINT('Ctrl Pts',(7.66314184287333,22.870626846128,12.));
#209297=CARTESIAN_POINT('Ctrl Pts',(7.66397328929805,22.8487154155569,0.));
#209298=CARTESIAN_POINT('Ctrl Pts',(7.66397328929805,22.8487154155569,12.));
#209299=CARTESIAN_POINT('Ctrl Pts',(7.66474484198552,22.8268998887679,0.));
#209300=CARTESIAN_POINT('Ctrl Pts',(7.66474484198552,22.8268998887679,12.));
#209301=CARTESIAN_POINT('Ctrl Pts',(7.66545684920987,22.8051809987834,0.));
#209302=CARTESIAN_POINT('Ctrl Pts',(7.66545684920987,22.8051809987834,12.));
#209303=CARTESIAN_POINT('Ctrl Pts',(7.66610966441259,22.7835594857697,0.));
#209304=CARTESIAN_POINT('Ctrl Pts',(7.66610966441259,22.7835594857697,12.));
#209305=CARTESIAN_POINT('Ctrl Pts',(7.66670364630273,22.7620360971839,0.));
#209306=CARTESIAN_POINT('Ctrl Pts',(7.66670364630273,22.7620360971839,12.));
#209307=CARTESIAN_POINT('Ctrl Pts',(7.66723915895412,22.7406115879508,0.));
#209308=CARTESIAN_POINT('Ctrl Pts',(7.66723915895412,22.7406115879508,12.));
#209309=CARTESIAN_POINT('Ctrl Pts',(7.6677165719101,22.7192867206242,0.));
#209310=CARTESIAN_POINT('Ctrl Pts',(7.6677165719101,22.7192867206242,12.));
#209311=CARTESIAN_POINT('Ctrl Pts',(7.66813626029276,22.6980622655446,0.));
#209312=CARTESIAN_POINT('Ctrl Pts',(7.66813626029276,22.6980622655446,12.));
#209313=CARTESIAN_POINT('Ctrl Pts',(7.66849860491762,22.6769390009889,0.));
#209314=CARTESIAN_POINT('Ctrl Pts',(7.66849860491762,22.6769390009889,12.));
#209315=CARTESIAN_POINT('Ctrl Pts',(7.66880399241353,22.6559177133133,0.));
#209316=CARTESIAN_POINT('Ctrl Pts',(7.66880399241353,22.6559177133133,12.));
#209317=CARTESIAN_POINT('Ctrl Pts',(7.66905281533744,22.6349991971548,0.));
#209318=CARTESIAN_POINT('Ctrl Pts',(7.66905281533744,22.6349991971548,12.));
#209319=CARTESIAN_POINT('Ctrl Pts',(7.66924547229434,22.6141842556248,0.));
#209320=CARTESIAN_POINT('Ctrl Pts',(7.66924547229434,22.6141842556248,12.));
#209321=CARTESIAN_POINT('Ctrl Pts',(7.6693823680624,22.5934737004955,0.));
#209322=CARTESIAN_POINT('Ctrl Pts',(7.6693823680624,22.5934737004955,12.));
#209323=CARTESIAN_POINT('Ctrl Pts',(7.66946391372299,22.5728683523829,0.));
#209324=CARTESIAN_POINT('Ctrl Pts',(7.66946391372299,22.5728683523829,12.));
#209325=CARTESIAN_POINT('Ctrl Pts',(7.66949052679671,22.5523690409109,0.));
#209326=CARTESIAN_POINT('Ctrl Pts',(7.66949052679671,22.5523690409109,12.));
#209327=CARTESIAN_POINT('Ctrl Pts',(7.66946263138115,22.5319766049191,0.));
#209328=CARTESIAN_POINT('Ctrl Pts',(7.66946263138115,22.5319766049191,12.));
#209329=CARTESIAN_POINT('Ctrl Pts',(7.66938065829082,22.5116918927023,0.));
#209330=CARTESIAN_POINT('Ctrl Pts',(7.66938065829082,22.5116918927023,12.));
#209331=CARTESIAN_POINT('Ctrl Pts',(7.66924504520301,22.4915157622308,0.));
#209332=CARTESIAN_POINT('Ctrl Pts',(7.66924504520301,22.4915157622308,12.));
#209333=CARTESIAN_POINT('Ctrl Pts',(7.66905623680835,22.47144908137,0.));
#209334=CARTESIAN_POINT('Ctrl Pts',(7.66905623680835,22.47144908137,12.));
#209335=CARTESIAN_POINT('Ctrl Pts',(7.66881468496659,22.4514927280863,0.));
#209336=CARTESIAN_POINT('Ctrl Pts',(7.66881468496659,22.4514927280863,12.));
#209337=CARTESIAN_POINT('Ctrl Pts',(7.66852084886745,22.4316475906616,0.));
#209338=CARTESIAN_POINT('Ctrl Pts',(7.66852084886745,22.4316475906616,12.));
#209339=CARTESIAN_POINT('Ctrl Pts',(7.66817519519681,22.411914567977,0.));
#209340=CARTESIAN_POINT('Ctrl Pts',(7.66817519519681,22.411914567977,12.));
#209341=CARTESIAN_POINT('Ctrl Pts',(7.66777819830819,22.3922945697782,0.));
#209342=CARTESIAN_POINT('Ctrl Pts',(7.66777819830819,22.3922945697782,12.));
#209343=CARTESIAN_POINT('Ctrl Pts',(7.66733034039887,22.3727885169361,0.));
#209344=CARTESIAN_POINT('Ctrl Pts',(7.66733034039887,22.3727885169361,12.));
#209345=CARTESIAN_POINT('Ctrl Pts',(7.66683211169133,22.3533973417013,0.));
#209346=CARTESIAN_POINT('Ctrl Pts',(7.66683211169133,22.3533973417013,12.));
#209347=CARTESIAN_POINT('Ctrl Pts',(7.66628401061905,22.3341219879454,0.));
#209348=CARTESIAN_POINT('Ctrl Pts',(7.66628401061905,22.3341219879454,12.));
#209349=CARTESIAN_POINT('Ctrl Pts',(7.66568654402441,22.3149634114823,0.));
#209350=CARTESIAN_POINT('Ctrl Pts',(7.66568654402441,22.3149634114823,12.));
#209351=CARTESIAN_POINT('Ctrl Pts',(7.66504022736262,22.2959225803925,0.));
#209352=CARTESIAN_POINT('Ctrl Pts',(7.66504022736262,22.2959225803925,12.));
#209353=CARTESIAN_POINT('Ctrl Pts',(7.66434558490972,22.2770004753332,0.));
#209354=CARTESIAN_POINT('Ctrl Pts',(7.66434558490972,22.2770004753332,12.));
#209355=CARTESIAN_POINT('Ctrl Pts',(7.66360314997661,22.2581980898487,0.));
#209356=CARTESIAN_POINT('Ctrl Pts',(7.66360314997661,22.2581980898487,12.));
#209357=CARTESIAN_POINT('Ctrl Pts',(7.66281346512545,22.239516430656,0.));
#209358=CARTESIAN_POINT('Ctrl Pts',(7.66281346512545,22.239516430656,12.));
#209359=CARTESIAN_POINT('Ctrl Pts',(7.66197708240435,22.2209565180098,0.));
#209360=CARTESIAN_POINT('Ctrl Pts',(7.66197708240435,22.2209565180098,12.));
#209361=CARTESIAN_POINT('Ctrl Pts',(7.66109456359292,22.2025193860972,0.));
#209362=CARTESIAN_POINT('Ctrl Pts',(7.66109456359292,22.2025193860972,12.));
#209363=CARTESIAN_POINT('Ctrl Pts',(7.66016648045007,22.1842060834093,0.));
#209364=CARTESIAN_POINT('Ctrl Pts',(7.66016648045007,22.1842060834093,12.));
#209365=CARTESIAN_POINT('Ctrl Pts',(7.65919341496925,22.1660176731174,0.));
#209366=CARTESIAN_POINT('Ctrl Pts',(7.65919341496925,22.1660176731174,12.));
#209367=CARTESIAN_POINT('Ctrl Pts',(7.6581759596335,22.1479552334206,0.));
#209368=CARTESIAN_POINT('Ctrl Pts',(7.6581759596335,22.1479552334206,12.));
#209369=CARTESIAN_POINT('Ctrl Pts',(7.65711471769406,22.1300198579671,0.));
#209370=CARTESIAN_POINT('Ctrl Pts',(7.65711471769406,22.1300198579671,12.));
#209371=CARTESIAN_POINT('Ctrl Pts',(7.65601030346818,22.1122126563327,0.));
#209372=CARTESIAN_POINT('Ctrl Pts',(7.65601030346818,22.1122126563327,12.));
#209373=CARTESIAN_POINT('Ctrl Pts',(7.6548633426365,22.094534754469,0.));
#209374=CARTESIAN_POINT('Ctrl Pts',(7.6548633426365,22.094534754469,12.));
#209375=CARTESIAN_POINT('Ctrl Pts',(7.65367447254944,22.0769872951596,0.));
#209376=CARTESIAN_POINT('Ctrl Pts',(7.65367447254944,22.0769872951596,12.));
#209377=CARTESIAN_POINT('Ctrl Pts',(7.65244434253103,22.0595714384432,0.));
#209378=CARTESIAN_POINT('Ctrl Pts',(7.65244434253103,22.0595714384432,12.));
#209379=CARTESIAN_POINT('Ctrl Pts',(7.65117361421346,22.0422883621176,0.));
#209380=CARTESIAN_POINT('Ctrl Pts',(7.65117361421346,22.0422883621176,12.));
#209381=CARTESIAN_POINT('Ctrl Pts',(7.64986296190156,22.025139262321,0.));
#209382=CARTESIAN_POINT('Ctrl Pts',(7.64986296190156,22.025139262321,12.));
#209383=CARTESIAN_POINT('Ctrl Pts',(7.64851307293345,22.0081253540774,0.));
#209384=CARTESIAN_POINT('Ctrl Pts',(7.64851307293345,22.0081253540774,12.));
#209385=CARTESIAN_POINT('Ctrl Pts',(7.64712464805257,21.9912478718542,0.));
#209386=CARTESIAN_POINT('Ctrl Pts',(7.64712464805257,21.9912478718542,12.));
#209387=CARTESIAN_POINT('Ctrl Pts',(7.64569840177359,21.97450807008,0.));
#209388=CARTESIAN_POINT('Ctrl Pts',(7.64569840177359,21.97450807008,12.));
#209389=CARTESIAN_POINT('Ctrl Pts',(7.64423506279153,21.9579072237653,0.));
#209390=CARTESIAN_POINT('Ctrl Pts',(7.64423506279153,21.9579072237653,12.));
#209391=CARTESIAN_POINT('Ctrl Pts',(7.64273537442706,21.9414466292074,0.));
#209392=CARTESIAN_POINT('Ctrl Pts',(7.64273537442706,21.9414466292074,12.));
#209393=CARTESIAN_POINT('Ctrl Pts',(7.64120009506539,21.9251276046546,0.));
#209394=CARTESIAN_POINT('Ctrl Pts',(7.64120009506539,21.9251276046546,12.));
#209395=CARTESIAN_POINT('Ctrl Pts',(7.63962999860916,21.9089514909873,0.));
#209396=CARTESIAN_POINT('Ctrl Pts',(7.63962999860916,21.9089514909873,12.));
#209397=CARTESIAN_POINT('Ctrl Pts',(7.63802587492007,21.8929196523511,0.));
#209398=CARTESIAN_POINT('Ctrl Pts',(7.63802587492007,21.8929196523511,12.));
#209399=CARTESIAN_POINT('Ctrl Pts',(7.63638853033367,21.8770334769492,0.));
#209400=CARTESIAN_POINT('Ctrl Pts',(7.63638853033367,21.8770334769492,12.));
#209401=CARTESIAN_POINT('Ctrl Pts',(7.63471878821203,21.8612943779086,0.));
#209402=CARTESIAN_POINT('Ctrl Pts',(7.63471878821203,21.8612943779086,12.));
#209403=CARTESIAN_POINT('Ctrl Pts',(7.63301748948936,21.8457037941084,0.));
#209404=CARTESIAN_POINT('Ctrl Pts',(7.63301748948936,21.8457037941084,12.));
#209405=CARTESIAN_POINT('Ctrl Pts',(7.6312854932304,21.8302631910197,0.));
#209406=CARTESIAN_POINT('Ctrl Pts',(7.6312854932304,21.8302631910197,12.));
#209407=CARTESIAN_POINT('Ctrl Pts',(7.62952367718151,21.8149740615093,0.));
#209408=CARTESIAN_POINT('Ctrl Pts',(7.62952367718151,21.8149740615093,12.));
#209409=CARTESIAN_POINT('Ctrl Pts',(7.62773293842409,21.7998379268583,0.));
#209410=CARTESIAN_POINT('Ctrl Pts',(7.62773293842409,21.7998379268583,12.));
#209411=CARTESIAN_POINT('Ctrl Pts',(7.6259141940452,21.7848563378022,0.));
#209412=CARTESIAN_POINT('Ctrl Pts',(7.6259141940452,21.7848563378022,12.));
#209413=CARTESIAN_POINT('Ctrl Pts',(7.62406838181164,21.7700308755584,0.));
#209414=CARTESIAN_POINT('Ctrl Pts',(7.62406838181164,21.7700308755584,12.));
#209415=CARTESIAN_POINT('Ctrl Pts',(7.62219646084225,21.7553631528329,0.));
#209416=CARTESIAN_POINT('Ctrl Pts',(7.62219646084225,21.7553631528329,12.));
#209417=CARTESIAN_POINT('Ctrl Pts',(7.62029941230854,21.7408548148657,0.));
#209418=CARTESIAN_POINT('Ctrl Pts',(7.62029941230854,21.7408548148657,12.));
#209419=CARTESIAN_POINT('Ctrl Pts',(7.61837824030541,21.7265075407977,0.));
#209420=CARTESIAN_POINT('Ctrl Pts',(7.61837824030541,21.7265075407977,12.));
#209421=CARTESIAN_POINT('Ctrl Pts',(7.61643397270424,21.7123230449835,0.));
#209422=CARTESIAN_POINT('Ctrl Pts',(7.61643397270424,21.7123230449835,12.));
#209423=CARTESIAN_POINT('Ctrl Pts',(7.61446766202786,21.6983030783321,0.));
#209424=CARTESIAN_POINT('Ctrl Pts',(7.61446766202786,21.6983030783321,12.));
#209425=CARTESIAN_POINT('Ctrl Pts',(7.61248038630264,21.6844494295813,0.));
#209426=CARTESIAN_POINT('Ctrl Pts',(7.61248038630264,21.6844494295813,12.));
#209427=CARTESIAN_POINT('Ctrl Pts',(7.61047325000949,21.6707639267573,0.));
#209428=CARTESIAN_POINT('Ctrl Pts',(7.61047325000949,21.6707639267573,12.));
#209429=CARTESIAN_POINT('Ctrl Pts',(7.60844738512871,21.6572484388079,0.));
#209430=CARTESIAN_POINT('Ctrl Pts',(7.60844738512871,21.6572484388079,12.));
#209431=CARTESIAN_POINT('Ctrl Pts',(7.60640395216358,21.6439048771743,0.));
#209432=CARTESIAN_POINT('Ctrl Pts',(7.60640395216358,21.6439048771743,12.));
#209433=CARTESIAN_POINT('Ctrl Pts',(7.60434414118299,21.6307351973823,0.));
#209434=CARTESIAN_POINT('Ctrl Pts',(7.60434414118299,21.6307351973823,12.));
#209435=CARTESIAN_POINT('Ctrl Pts',(7.60226917285431,21.6177414005991,0.));
#209436=CARTESIAN_POINT('Ctrl Pts',(7.60226917285431,21.6177414005991,12.));
#209437=CARTESIAN_POINT('Ctrl Pts',(7.60018029988238,21.6049255358843,0.));
#209438=CARTESIAN_POINT('Ctrl Pts',(7.60018029988238,21.6049255358843,12.));
#209439=CARTESIAN_POINT('Ctrl Pts',(7.59807880846192,21.5922897024466,0.));
#209440=CARTESIAN_POINT('Ctrl Pts',(7.59807880846192,21.5922897024466,12.));
#209441=CARTESIAN_POINT('Ctrl Pts',(7.59596601973588,21.5798360518978,0.));
#209442=CARTESIAN_POINT('Ctrl Pts',(7.59596601973588,21.5798360518978,12.));
#209443=CARTESIAN_POINT('Ctrl Pts',(7.59384329124929,21.5675667904728,0.));
#209444=CARTESIAN_POINT('Ctrl Pts',(7.59384329124929,21.5675667904728,12.));
#209445=CARTESIAN_POINT('Ctrl Pts',(7.59171201844792,21.5554841813466,0.));
#209446=CARTESIAN_POINT('Ctrl Pts',(7.59171201844792,21.5554841813466,12.));
#209447=CARTESIAN_POINT('Ctrl Pts',(7.58957363620026,21.5435905470113,0.));
#209448=CARTESIAN_POINT('Ctrl Pts',(7.58957363620026,21.5435905470113,12.));
#209449=CARTESIAN_POINT('Ctrl Pts',(7.58742962034834,21.5318882716736,0.));
#209450=CARTESIAN_POINT('Ctrl Pts',(7.58742962034834,21.5318882716736,12.));
#209451=CARTESIAN_POINT('Ctrl Pts',(7.58528148919113,21.5203798035294,0.));
#209452=CARTESIAN_POINT('Ctrl Pts',(7.58528148919113,21.5203798035294,12.));
#209453=CARTESIAN_POINT('Ctrl Pts',(7.58313080519158,21.5090676573866,0.));
#209454=CARTESIAN_POINT('Ctrl Pts',(7.58313080519158,21.5090676573866,12.));
#209455=CARTESIAN_POINT('Ctrl Pts',(7.58097917790729,21.497954419274,0.));
#209456=CARTESIAN_POINT('Ctrl Pts',(7.58097917790729,21.497954419274,12.));
#209457=CARTESIAN_POINT('Ctrl Pts',(7.57882826679131,21.4870427508193,0.));
#209458=CARTESIAN_POINT('Ctrl Pts',(7.57882826679131,21.4870427508193,12.));
#209459=CARTESIAN_POINT('Ctrl Pts',(7.57667978403001,21.4763353936766,0.));
#209460=CARTESIAN_POINT('Ctrl Pts',(7.57667978403001,21.4763353936766,12.));
#209461=CARTESIAN_POINT('Ctrl Pts',(7.57453549743434,21.4658351740135,0.));
#209462=CARTESIAN_POINT('Ctrl Pts',(7.57453549743434,21.4658351740135,12.));
#209463=CARTESIAN_POINT('Ctrl Pts',(7.57239723223521,21.4555450053147,0.));
#209464=CARTESIAN_POINT('Ctrl Pts',(7.57239723223521,21.4555450053147,12.));
#209465=CARTESIAN_POINT('Ctrl Pts',(7.57026687261169,21.445467890751,0.));
#209466=CARTESIAN_POINT('Ctrl Pts',(7.57026687261169,21.445467890751,12.));
#209467=CARTESIAN_POINT('Ctrl Pts',(7.56814636360841,21.435606926151,0.));
#209468=CARTESIAN_POINT('Ctrl Pts',(7.56814636360841,21.435606926151,12.));
#209469=CARTESIAN_POINT('Ctrl Pts',(7.56603771218706,21.4259653015732,0.));
#209470=CARTESIAN_POINT('Ctrl Pts',(7.56603771218706,21.4259653015732,12.));
#209471=CARTESIAN_POINT('Ctrl Pts',(7.56394299313682,21.4165463106252,0.));
#209472=CARTESIAN_POINT('Ctrl Pts',(7.56394299313682,21.4165463106252,12.));
#209473=CARTESIAN_POINT('Ctrl Pts',(7.56186435703622,21.4073533630364,0.));
#209474=CARTESIAN_POINT('Ctrl Pts',(7.56186435703622,21.4073533630364,12.));
#209475=CARTESIAN_POINT('Ctrl Pts',(7.55980403700614,21.3983899952988,0.));
#209476=CARTESIAN_POINT('Ctrl Pts',(7.55980403700614,21.3983899952988,12.));
#209477=CARTESIAN_POINT('Ctrl Pts',(7.55776435731421,21.3896598842119,0.));
#209478=CARTESIAN_POINT('Ctrl Pts',(7.55776435731421,21.3896598842119,12.));
#209479=CARTESIAN_POINT('Ctrl Pts',(7.55574773403507,21.3811668478933,0.));
#209480=CARTESIAN_POINT('Ctrl Pts',(7.55574773403507,21.3811668478933,12.));
#209481=CARTESIAN_POINT('Ctrl Pts',(7.55375667080031,21.3729148390244,0.));
#209482=CARTESIAN_POINT('Ctrl Pts',(7.55375667080031,21.3729148390244,12.));
#209483=CARTESIAN_POINT('Ctrl Pts',(7.55179375777441,21.3649079431864,0.));
#209484=CARTESIAN_POINT('Ctrl Pts',(7.55179375777441,21.3649079431864,12.));
#209485=CARTESIAN_POINT('Ctrl Pts',(7.54986166521306,21.3571503685853,0.));
#209486=CARTESIAN_POINT('Ctrl Pts',(7.54986166521306,21.3571503685853,12.));
#209487=CARTESIAN_POINT('Ctrl Pts',(7.54796316246326,21.349646476153,0.));
#209488=CARTESIAN_POINT('Ctrl Pts',(7.54796316246326,21.349646476153,12.));
#209489=CARTESIAN_POINT('Ctrl Pts',(7.5461011494835,21.3424008295038,0.));
#209490=CARTESIAN_POINT('Ctrl Pts',(7.5461011494835,21.3424008295038,12.));
#209491=CARTESIAN_POINT('Ctrl Pts',(7.54427868151268,21.3354182340149,0.));
#209492=CARTESIAN_POINT('Ctrl Pts',(7.54427868151268,21.3354182340149,12.));
#209493=CARTESIAN_POINT('Ctrl Pts',(7.54249900377031,21.328703791771,0.));
#209494=CARTESIAN_POINT('Ctrl Pts',(7.54249900377031,21.328703791771,12.));
#209495=CARTESIAN_POINT('Ctrl Pts',(7.54076552038279,21.3222628524165,0.));
#209496=CARTESIAN_POINT('Ctrl Pts',(7.54076552038279,21.3222628524165,12.));
#209497=CARTESIAN_POINT('Ctrl Pts',(7.53908175169898,21.3161009456256,0.));
#209498=CARTESIAN_POINT('Ctrl Pts',(7.53908175169898,21.3161009456256,12.));
#209499=CARTESIAN_POINT('Ctrl Pts',(7.53745129364619,21.3102237167729,0.));
#209500=CARTESIAN_POINT('Ctrl Pts',(7.53745129364619,21.3102237167729,12.));
#209501=CARTESIAN_POINT('Ctrl Pts',(7.53587778251743,21.3046368712157,0.));
#209502=CARTESIAN_POINT('Ctrl Pts',(7.53587778251743,21.3046368712157,12.));
#209503=CARTESIAN_POINT('Ctrl Pts',(7.53436505309948,21.2993464250717,0.));
#209504=CARTESIAN_POINT('Ctrl Pts',(7.53436505309948,21.2993464250717,12.));
#209505=CARTESIAN_POINT('Ctrl Pts',(7.53291726078526,21.2943588989331,0.));
#209506=CARTESIAN_POINT('Ctrl Pts',(7.53291726078526,21.2943588989331,12.));
#209507=CARTESIAN_POINT('Ctrl Pts',(7.53153906987846,21.2896816163843,0.));
#209508=CARTESIAN_POINT('Ctrl Pts',(7.53153906987846,21.2896816163843,12.));
#209509=CARTESIAN_POINT('Ctrl Pts',(7.5302356243822,21.2853226580658,0.));
#209510=CARTESIAN_POINT('Ctrl Pts',(7.5302356243822,21.2853226580658,12.));
#209511=CARTESIAN_POINT('Ctrl Pts',(7.52901217930407,21.2812902781143,0.));
#209512=CARTESIAN_POINT('Ctrl Pts',(7.52901217930407,21.2812902781143,12.));
#209513=CARTESIAN_POINT('Ctrl Pts',(7.52787386225343,21.2775925269652,0.));
#209514=CARTESIAN_POINT('Ctrl Pts',(7.52787386225343,21.2775925269652,12.));
#209515=CARTESIAN_POINT('Ctrl Pts',(7.5268252691856,21.2742366113578,0.));
#209516=CARTESIAN_POINT('Ctrl Pts',(7.5268252691856,21.2742366113578,12.));
#209517=CARTESIAN_POINT('Ctrl Pts',(7.52587126095544,21.2712301573465,0.));
#209518=CARTESIAN_POINT('Ctrl Pts',(7.52587126095544,21.2712301573465,12.));
#209519=CARTESIAN_POINT('Ctrl Pts',(7.52501770333521,21.2685823838672,0.));
#209520=CARTESIAN_POINT('Ctrl Pts',(7.52501770333521,21.2685823838672,12.));
#209521=CARTESIAN_POINT('Ctrl Pts',(7.52427261074263,21.266305915706,0.));
#209522=CARTESIAN_POINT('Ctrl Pts',(7.52427261074263,21.266305915706,12.));
#209523=CARTESIAN_POINT('Ctrl Pts',(7.52364573027521,21.2644161259965,0.));
#209524=CARTESIAN_POINT('Ctrl Pts',(7.52364573027521,21.2644161259965,12.));
#209525=CARTESIAN_POINT('Ctrl Pts',(7.52314642316202,21.262927782038,0.));
#209526=CARTESIAN_POINT('Ctrl Pts',(7.52314642316202,21.262927782038,12.));
#209527=CARTESIAN_POINT('Ctrl Pts',(7.52278182242727,21.261852128355,0.));
#209528=CARTESIAN_POINT('Ctrl Pts',(7.52278182242727,21.261852128355,12.));
#209529=CARTESIAN_POINT('Ctrl Pts',(7.52260064231736,21.2613260540651,0.));
#209530=CARTESIAN_POINT('Ctrl Pts',(7.52260064231736,21.2613260540651,12.));
#209531=CARTESIAN_POINT('Ctrl Pts',(7.52252744144957,21.261120447486,0.));
#209532=CARTESIAN_POINT('Ctrl Pts',(7.52252744144957,21.261120447486,12.));
#209533=CARTESIAN_POINT('Ctrl Pts',(7.52250649703991,21.2610673466883,0.));
#209534=CARTESIAN_POINT('Ctrl Pts',(7.52250649703991,21.2610673466883,12.));
#209535=CARTESIAN_POINT('Ctrl Pts',(7.52250298901265,21.2610617890679,0.));
#209536=CARTESIAN_POINT('Ctrl Pts',(7.52250298901265,21.2610617890679,12.));
#209537=CARTESIAN_POINT('',(7.36589684767344,24.9347862158358,0.));
#209538=CARTESIAN_POINT('Ctrl Pts',(7.36589684767344,24.9347862158358,0.));
#209539=CARTESIAN_POINT('Ctrl Pts',(7.36721909028842,24.9292275670674,0.));
#209540=CARTESIAN_POINT('Ctrl Pts',(7.3698559312009,24.9181155530543,0.));
#209541=CARTESIAN_POINT('Ctrl Pts',(7.37378825961676,24.901463382605,0.));
#209542=CARTESIAN_POINT('Ctrl Pts',(7.37898549640269,24.8792921911115,0.));
#209543=CARTESIAN_POINT('Ctrl Pts',(7.3854055890362,24.8516310625176,0.));
#209544=CARTESIAN_POINT('Ctrl Pts',(7.39174922585808,24.8240228520893,0.));
#209545=CARTESIAN_POINT('Ctrl Pts',(7.39801641583012,24.7964676646431,0.));
#209546=CARTESIAN_POINT('Ctrl Pts',(7.40420718661602,24.7689656668983,0.));
#209547=CARTESIAN_POINT('Ctrl Pts',(7.41032159082381,24.7415170994784,0.));
#209548=CARTESIAN_POINT('Ctrl Pts',(7.41635971481674,24.7141222950051,0.));
#209549=CARTESIAN_POINT('Ctrl Pts',(7.42232167766265,24.6867816727192,0.));
#209550=CARTESIAN_POINT('Ctrl Pts',(7.42820762159125,24.6594957128756,0.));
#209551=CARTESIAN_POINT('Ctrl Pts',(7.43401770489523,24.6322649369517,0.));
#209552=CARTESIAN_POINT('Ctrl Pts',(7.43975209375503,24.6050898852368,0.));
#209553=CARTESIAN_POINT('Ctrl Pts',(7.44541095473134,24.577971096086,0.));
#209554=CARTESIAN_POINT('Ctrl Pts',(7.4509944465116,24.5509090831559,0.));
#209555=CARTESIAN_POINT('Ctrl Pts',(7.45650271335861,24.5239043173072,0.));
#209556=CARTESIAN_POINT('Ctrl Pts',(7.46193588961463,24.4969572391483,0.));
#209557=CARTESIAN_POINT('Ctrl Pts',(7.46729410308786,24.4700682684524,0.));
#209558=CARTESIAN_POINT('Ctrl Pts',(7.47257747883246,24.443237814649,0.));
#209559=CARTESIAN_POINT('Ctrl Pts',(7.47778614286564,24.4164662871163,0.));
#209560=CARTESIAN_POINT('Ctrl Pts',(7.482920225693,24.3897541049254,0.));
#209561=CARTESIAN_POINT('Ctrl Pts',(7.48797986651908,24.3631017084524,0.));
#209562=CARTESIAN_POINT('Ctrl Pts',(7.4929652125242,24.3365095573685,0.));
#209563=CARTESIAN_POINT('Ctrl Pts',(7.49787641695438,24.3099781253355,0.));
#209564=CARTESIAN_POINT('Ctrl Pts',(7.50271363765151,24.2835078958973,0.));
#209565=CARTESIAN_POINT('Ctrl Pts',(7.50747703535133,24.2570993577034,0.));
#209566=CARTESIAN_POINT('Ctrl Pts',(7.5121667722218,24.2307530003887,0.));
#209567=CARTESIAN_POINT('Ctrl Pts',(7.51678300997949,24.2044693092349,0.));
#209568=CARTESIAN_POINT('Ctrl Pts',(7.52132590953801,24.1782487641594,0.));
#209569=CARTESIAN_POINT('Ctrl Pts',(7.52579563201423,24.1520918425364,0.));
#209570=CARTESIAN_POINT('Ctrl Pts',(7.53019233935501,24.1259990209207,0.));
#209571=CARTESIAN_POINT('Ctrl Pts',(7.53451619514649,24.0999707772642,0.));
#209572=CARTESIAN_POINT('Ctrl Pts',(7.53876736531013,24.0740075927985,0.));
#209573=CARTESIAN_POINT('Ctrl Pts',(7.54294601896144,24.0481099543353,0.));
#209574=CARTESIAN_POINT('Ctrl Pts',(7.5470523288591,24.022278355453,0.));
#209575=CARTESIAN_POINT('Ctrl Pts',(7.5510864709744,23.9965132953185,0.));
#209576=CARTESIAN_POINT('Ctrl Pts',(7.55504862424811,23.9708152779884,0.));
#209577=CARTESIAN_POINT('Ctrl Pts',(7.55893897027682,23.9451848115,0.));
#209578=CARTESIAN_POINT('Ctrl Pts',(7.56275769304773,23.9196224070759,0.));
#209579=CARTESIAN_POINT('Ctrl Pts',(7.56650497863791,23.8941285782003,0.));
#209580=CARTESIAN_POINT('Ctrl Pts',(7.5701810150071,23.8687038399598,0.));
#209581=CARTESIAN_POINT('Ctrl Pts',(7.57378599219816,23.8433487096134,0.));
#209582=CARTESIAN_POINT('Ctrl Pts',(7.57732010249065,23.8180637069977,0.));
#209583=CARTESIAN_POINT('Ctrl Pts',(7.58078354058211,23.7928493549908,0.));
#209584=CARTESIAN_POINT('Ctrl Pts',(7.58417650376271,23.7677061799376,0.));
#209585=CARTESIAN_POINT('Ctrl Pts',(7.58749919210831,23.7426347121006,0.));
#209586=CARTESIAN_POINT('Ctrl Pts',(7.59075180865326,23.7176354860457,0.));
#209587=CARTESIAN_POINT('Ctrl Pts',(7.59393455934041,23.6927090405067,0.));
#209588=CARTESIAN_POINT('Ctrl Pts',(7.59704765299572,23.6678559182876,0.));
#209589=CARTESIAN_POINT('Ctrl Pts',(7.60009130130129,23.6430766661419,0.));
#209590=CARTESIAN_POINT('Ctrl Pts',(7.60306571877806,23.6183718346576,0.));
#209591=CARTESIAN_POINT('Ctrl Pts',(7.60597112277094,23.5937419781244,0.));
#209592=CARTESIAN_POINT('Ctrl Pts',(7.60880773344599,23.5691876544243,0.));
#209593=CARTESIAN_POINT('Ctrl Pts',(7.61157577385371,23.5447094252029,0.));
#209594=CARTESIAN_POINT('Ctrl Pts',(7.61427546999298,23.5203078560128,0.));
#209595=CARTESIAN_POINT('Ctrl Pts',(7.61690705088318,23.4959835164608,0.));
#209596=CARTESIAN_POINT('Ctrl Pts',(7.61947074863977,23.4717369803438,0.));
#209597=CARTESIAN_POINT('Ctrl Pts',(7.62196679855957,23.4475688257855,0.));
#209598=CARTESIAN_POINT('Ctrl Pts',(7.62439543920053,23.4234796353544,0.));
#209599=CARTESIAN_POINT('Ctrl Pts',(7.62675691240334,23.3994699961122,0.));
#209600=CARTESIAN_POINT('Ctrl Pts',(7.62905146332597,23.3755404996638,0.));
#209601=CARTESIAN_POINT('Ctrl Pts',(7.63127934048138,23.3516917421973,0.));
#209602=CARTESIAN_POINT('Ctrl Pts',(7.63344079578162,23.3279243245241,0.));
#209603=CARTESIAN_POINT('Ctrl Pts',(7.63553608458783,23.3042388521021,0.));
#209604=CARTESIAN_POINT('Ctrl Pts',(7.63756546576374,23.2806359350853,0.));
#209605=CARTESIAN_POINT('Ctrl Pts',(7.63952920172837,23.2571161884487,0.));
#209606=CARTESIAN_POINT('Ctrl Pts',(7.64142755851507,23.2336802320912,0.));
#209607=CARTESIAN_POINT('Ctrl Pts',(7.64326080583683,23.2103286909399,0.));
#209608=CARTESIAN_POINT('Ctrl Pts',(7.64502921715482,23.1870621950452,0.));
#209609=CARTESIAN_POINT('Ctrl Pts',(7.64673306975796,23.1638813796691,0.));
#209610=CARTESIAN_POINT('Ctrl Pts',(7.64837264482929,23.1407868853815,0.));
#209611=CARTESIAN_POINT('Ctrl Pts',(7.64994822749844,23.1177793581674,0.));
#209612=CARTESIAN_POINT('Ctrl Pts',(7.65146010690464,23.0948594495246,0.));
#209613=CARTESIAN_POINT('Ctrl Pts',(7.65290857626356,23.072027816555,0.));
#209614=CARTESIAN_POINT('Ctrl Pts',(7.65429393293955,23.049285122053,0.));
#209615=CARTESIAN_POINT('Ctrl Pts',(7.65561647852554,23.0266320345792,0.));
#209616=CARTESIAN_POINT('Ctrl Pts',(7.6568765189133,23.004069228582,0.));
#209617=CARTESIAN_POINT('Ctrl Pts',(7.65807436436452,22.9815973845301,0.));
#209618=CARTESIAN_POINT('Ctrl Pts',(7.65921032958911,22.9592171890332,0.));
#209619=CARTESIAN_POINT('Ctrl Pts',(7.66028473382776,22.9369293349592,0.));
#209620=CARTESIAN_POINT('Ctrl Pts',(7.66129790094099,22.9147345215418,0.));
#209621=CARTESIAN_POINT('Ctrl Pts',(7.66225015950147,22.8926334544879,0.));
#209622=CARTESIAN_POINT('Ctrl Pts',(7.66314184287333,22.870626846128,0.));
#209623=CARTESIAN_POINT('Ctrl Pts',(7.66397328929805,22.8487154155569,0.));
#209624=CARTESIAN_POINT('Ctrl Pts',(7.66474484198552,22.8268998887679,0.));
#209625=CARTESIAN_POINT('Ctrl Pts',(7.66545684920987,22.8051809987834,0.));
#209626=CARTESIAN_POINT('Ctrl Pts',(7.66610966441259,22.7835594857697,0.));
#209627=CARTESIAN_POINT('Ctrl Pts',(7.66670364630273,22.7620360971839,0.));
#209628=CARTESIAN_POINT('Ctrl Pts',(7.66723915895412,22.7406115879508,0.));
#209629=CARTESIAN_POINT('Ctrl Pts',(7.6677165719101,22.7192867206242,0.));
#209630=CARTESIAN_POINT('Ctrl Pts',(7.66813626029276,22.6980622655446,0.));
#209631=CARTESIAN_POINT('Ctrl Pts',(7.66849860491762,22.6769390009889,0.));
#209632=CARTESIAN_POINT('Ctrl Pts',(7.66880399241353,22.6559177133133,0.));
#209633=CARTESIAN_POINT('Ctrl Pts',(7.66905281533744,22.6349991971548,0.));
#209634=CARTESIAN_POINT('Ctrl Pts',(7.66924547229434,22.6141842556248,0.));
#209635=CARTESIAN_POINT('Ctrl Pts',(7.6693823680624,22.5934737004955,0.));
#209636=CARTESIAN_POINT('Ctrl Pts',(7.66946391372299,22.5728683523829,0.));
#209637=CARTESIAN_POINT('Ctrl Pts',(7.66949052679671,22.5523690409109,0.));
#209638=CARTESIAN_POINT('Ctrl Pts',(7.66946263138115,22.5319766049191,0.));
#209639=CARTESIAN_POINT('Ctrl Pts',(7.66938065829082,22.5116918927023,0.));
#209640=CARTESIAN_POINT('Ctrl Pts',(7.66924504520301,22.4915157622308,0.));
#209641=CARTESIAN_POINT('Ctrl Pts',(7.66905623680835,22.47144908137,0.));
#209642=CARTESIAN_POINT('Ctrl Pts',(7.66881468496659,22.4514927280863,0.));
#209643=CARTESIAN_POINT('Ctrl Pts',(7.66852084886745,22.4316475906616,0.));
#209644=CARTESIAN_POINT('Ctrl Pts',(7.66817519519681,22.411914567977,0.));
#209645=CARTESIAN_POINT('Ctrl Pts',(7.66777819830819,22.3922945697782,0.));
#209646=CARTESIAN_POINT('Ctrl Pts',(7.66733034039887,22.3727885169361,0.));
#209647=CARTESIAN_POINT('Ctrl Pts',(7.66683211169133,22.3533973417013,0.));
#209648=CARTESIAN_POINT('Ctrl Pts',(7.66628401061905,22.3341219879454,0.));
#209649=CARTESIAN_POINT('Ctrl Pts',(7.66568654402441,22.3149634114823,0.));
#209650=CARTESIAN_POINT('Ctrl Pts',(7.66504022736262,22.2959225803925,0.));
#209651=CARTESIAN_POINT('Ctrl Pts',(7.66434558490972,22.2770004753332,0.));
#209652=CARTESIAN_POINT('Ctrl Pts',(7.66360314997661,22.2581980898487,0.));
#209653=CARTESIAN_POINT('Ctrl Pts',(7.66281346512545,22.239516430656,0.));
#209654=CARTESIAN_POINT('Ctrl Pts',(7.66197708240435,22.2209565180098,0.));
#209655=CARTESIAN_POINT('Ctrl Pts',(7.66109456359292,22.2025193860972,0.));
#209656=CARTESIAN_POINT('Ctrl Pts',(7.66016648045007,22.1842060834093,0.));
#209657=CARTESIAN_POINT('Ctrl Pts',(7.65919341496925,22.1660176731174,0.));
#209658=CARTESIAN_POINT('Ctrl Pts',(7.6581759596335,22.1479552334206,0.));
#209659=CARTESIAN_POINT('Ctrl Pts',(7.65711471769406,22.1300198579671,0.));
#209660=CARTESIAN_POINT('Ctrl Pts',(7.65601030346818,22.1122126563327,0.));
#209661=CARTESIAN_POINT('Ctrl Pts',(7.6548633426365,22.094534754469,0.));
#209662=CARTESIAN_POINT('Ctrl Pts',(7.65367447254944,22.0769872951596,0.));
#209663=CARTESIAN_POINT('Ctrl Pts',(7.65244434253103,22.0595714384432,0.));
#209664=CARTESIAN_POINT('Ctrl Pts',(7.65117361421346,22.0422883621176,0.));
#209665=CARTESIAN_POINT('Ctrl Pts',(7.64986296190156,22.025139262321,0.));
#209666=CARTESIAN_POINT('Ctrl Pts',(7.64851307293345,22.0081253540774,0.));
#209667=CARTESIAN_POINT('Ctrl Pts',(7.64712464805257,21.9912478718542,0.));
#209668=CARTESIAN_POINT('Ctrl Pts',(7.64569840177359,21.97450807008,0.));
#209669=CARTESIAN_POINT('Ctrl Pts',(7.64423506279153,21.9579072237653,0.));
#209670=CARTESIAN_POINT('Ctrl Pts',(7.64273537442706,21.9414466292074,0.));
#209671=CARTESIAN_POINT('Ctrl Pts',(7.64120009506539,21.9251276046546,0.));
#209672=CARTESIAN_POINT('Ctrl Pts',(7.63962999860916,21.9089514909873,0.));
#209673=CARTESIAN_POINT('Ctrl Pts',(7.63802587492007,21.8929196523511,0.));
#209674=CARTESIAN_POINT('Ctrl Pts',(7.63638853033367,21.8770334769492,0.));
#209675=CARTESIAN_POINT('Ctrl Pts',(7.63471878821203,21.8612943779086,0.));
#209676=CARTESIAN_POINT('Ctrl Pts',(7.63301748948936,21.8457037941084,0.));
#209677=CARTESIAN_POINT('Ctrl Pts',(7.6312854932304,21.8302631910197,0.));
#209678=CARTESIAN_POINT('Ctrl Pts',(7.62952367718151,21.8149740615093,0.));
#209679=CARTESIAN_POINT('Ctrl Pts',(7.62773293842409,21.7998379268583,0.));
#209680=CARTESIAN_POINT('Ctrl Pts',(7.6259141940452,21.7848563378022,0.));
#209681=CARTESIAN_POINT('Ctrl Pts',(7.62406838181164,21.7700308755584,0.));
#209682=CARTESIAN_POINT('Ctrl Pts',(7.62219646084225,21.7553631528329,0.));
#209683=CARTESIAN_POINT('Ctrl Pts',(7.62029941230854,21.7408548148657,0.));
#209684=CARTESIAN_POINT('Ctrl Pts',(7.61837824030541,21.7265075407977,0.));
#209685=CARTESIAN_POINT('Ctrl Pts',(7.61643397270424,21.7123230449835,0.));
#209686=CARTESIAN_POINT('Ctrl Pts',(7.61446766202786,21.6983030783321,0.));
#209687=CARTESIAN_POINT('Ctrl Pts',(7.61248038630264,21.6844494295813,0.));
#209688=CARTESIAN_POINT('Ctrl Pts',(7.61047325000949,21.6707639267573,0.));
#209689=CARTESIAN_POINT('Ctrl Pts',(7.60844738512871,21.6572484388079,0.));
#209690=CARTESIAN_POINT('Ctrl Pts',(7.60640395216358,21.6439048771743,0.));
#209691=CARTESIAN_POINT('Ctrl Pts',(7.60434414118299,21.6307351973823,0.));
#209692=CARTESIAN_POINT('Ctrl Pts',(7.60226917285431,21.6177414005991,0.));
#209693=CARTESIAN_POINT('Ctrl Pts',(7.60018029988238,21.6049255358843,0.));
#209694=CARTESIAN_POINT('Ctrl Pts',(7.59807880846192,21.5922897024466,0.));
#209695=CARTESIAN_POINT('Ctrl Pts',(7.59596601973588,21.5798360518978,0.));
#209696=CARTESIAN_POINT('Ctrl Pts',(7.59384329124929,21.5675667904728,0.));
#209697=CARTESIAN_POINT('Ctrl Pts',(7.59171201844792,21.5554841813466,0.));
#209698=CARTESIAN_POINT('Ctrl Pts',(7.58957363620026,21.5435905470113,0.));
#209699=CARTESIAN_POINT('Ctrl Pts',(7.58742962034834,21.5318882716736,0.));
#209700=CARTESIAN_POINT('Ctrl Pts',(7.58528148919113,21.5203798035294,0.));
#209701=CARTESIAN_POINT('Ctrl Pts',(7.58313080519158,21.5090676573866,0.));
#209702=CARTESIAN_POINT('Ctrl Pts',(7.58097917790729,21.497954419274,0.));
#209703=CARTESIAN_POINT('Ctrl Pts',(7.57882826679131,21.4870427508193,0.));
#209704=CARTESIAN_POINT('Ctrl Pts',(7.57667978403001,21.4763353936766,0.));
#209705=CARTESIAN_POINT('Ctrl Pts',(7.57453549743434,21.4658351740135,0.));
#209706=CARTESIAN_POINT('Ctrl Pts',(7.57239723223521,21.4555450053147,0.));
#209707=CARTESIAN_POINT('Ctrl Pts',(7.57026687261169,21.445467890751,0.));
#209708=CARTESIAN_POINT('Ctrl Pts',(7.56814636360841,21.435606926151,0.));
#209709=CARTESIAN_POINT('Ctrl Pts',(7.56603771218706,21.4259653015732,0.));
#209710=CARTESIAN_POINT('Ctrl Pts',(7.56394299313682,21.4165463106252,0.));
#209711=CARTESIAN_POINT('Ctrl Pts',(7.56186435703622,21.4073533630364,0.));
#209712=CARTESIAN_POINT('Ctrl Pts',(7.55980403700614,21.3983899952988,0.));
#209713=CARTESIAN_POINT('Ctrl Pts',(7.55776435731421,21.3896598842119,0.));
#209714=CARTESIAN_POINT('Ctrl Pts',(7.55574773403507,21.3811668478933,0.));
#209715=CARTESIAN_POINT('Ctrl Pts',(7.55375667080031,21.3729148390244,0.));
#209716=CARTESIAN_POINT('Ctrl Pts',(7.55179375777441,21.3649079431864,0.));
#209717=CARTESIAN_POINT('Ctrl Pts',(7.54986166521306,21.3571503685853,0.));
#209718=CARTESIAN_POINT('Ctrl Pts',(7.54796316246326,21.349646476153,0.));
#209719=CARTESIAN_POINT('Ctrl Pts',(7.5461011494835,21.3424008295038,0.));
#209720=CARTESIAN_POINT('Ctrl Pts',(7.54427868151268,21.3354182340149,0.));
#209721=CARTESIAN_POINT('Ctrl Pts',(7.54249900377031,21.328703791771,0.));
#209722=CARTESIAN_POINT('Ctrl Pts',(7.54076552038279,21.3222628524165,0.));
#209723=CARTESIAN_POINT('Ctrl Pts',(7.53908175169898,21.3161009456256,0.));
#209724=CARTESIAN_POINT('Ctrl Pts',(7.53745129364619,21.3102237167729,0.));
#209725=CARTESIAN_POINT('Ctrl Pts',(7.53587778251743,21.3046368712157,0.));
#209726=CARTESIAN_POINT('Ctrl Pts',(7.53436505309948,21.2993464250717,0.));
#209727=CARTESIAN_POINT('Ctrl Pts',(7.53291726078526,21.2943588989331,0.));
#209728=CARTESIAN_POINT('Ctrl Pts',(7.53153906987846,21.2896816163843,0.));
#209729=CARTESIAN_POINT('Ctrl Pts',(7.5302356243822,21.2853226580658,0.));
#209730=CARTESIAN_POINT('Ctrl Pts',(7.52901217930407,21.2812902781143,0.));
#209731=CARTESIAN_POINT('Ctrl Pts',(7.52787386225343,21.2775925269652,0.));
#209732=CARTESIAN_POINT('Ctrl Pts',(7.5268252691856,21.2742366113578,0.));
#209733=CARTESIAN_POINT('Ctrl Pts',(7.52587126095544,21.2712301573465,0.));
#209734=CARTESIAN_POINT('Ctrl Pts',(7.52501770333521,21.2685823838672,0.));
#209735=CARTESIAN_POINT('Ctrl Pts',(7.52427261074263,21.266305915706,0.));
#209736=CARTESIAN_POINT('Ctrl Pts',(7.52364573027521,21.2644161259965,0.));
#209737=CARTESIAN_POINT('Ctrl Pts',(7.52314642316202,21.262927782038,0.));
#209738=CARTESIAN_POINT('Ctrl Pts',(7.52278182242727,21.261852128355,0.));
#209739=CARTESIAN_POINT('Ctrl Pts',(7.52260064231736,21.2613260540651,0.));
#209740=CARTESIAN_POINT('Ctrl Pts',(7.52252744144957,21.261120447486,0.));
#209741=CARTESIAN_POINT('Ctrl Pts',(7.52250649703991,21.2610673466883,0.));
#209742=CARTESIAN_POINT('Ctrl Pts',(7.52250298901265,21.2610617890679,0.));
#209743=CARTESIAN_POINT('',(7.36589684767344,24.9347862158358,0.));
#209744=CARTESIAN_POINT('Ctrl Pts',(9.71462809124917,20.353053841303,0.));
#209745=CARTESIAN_POINT('Ctrl Pts',(9.71462809124917,20.353053841303,12.));
#209746=CARTESIAN_POINT('Ctrl Pts',(9.71462954053074,20.353060251684,0.));
#209747=CARTESIAN_POINT('Ctrl Pts',(9.71462954053074,20.353060251684,12.));
#209748=CARTESIAN_POINT('Ctrl Pts',(9.71465227853122,20.3531126095522,0.));
#209749=CARTESIAN_POINT('Ctrl Pts',(9.71465227853122,20.3531126095522,12.));
#209750=CARTESIAN_POINT('Ctrl Pts',(9.71474590350791,20.3533097561886,0.));
#209751=CARTESIAN_POINT('Ctrl Pts',(9.71474590350791,20.3533097561886,12.));
#209752=CARTESIAN_POINT('Ctrl Pts',(9.714989780521,20.3538098605706,0.));
#209753=CARTESIAN_POINT('Ctrl Pts',(9.714989780521,20.3538098605706,12.));
#209754=CARTESIAN_POINT('Ctrl Pts',(9.71549257088174,20.3548282742361,0.));
#209755=CARTESIAN_POINT('Ctrl Pts',(9.71549257088174,20.3548282742361,12.));
#209756=CARTESIAN_POINT('Ctrl Pts',(9.71619192554146,20.3562337557875,0.));
#209757=CARTESIAN_POINT('Ctrl Pts',(9.71619192554146,20.3562337557875,12.));
#209758=CARTESIAN_POINT('Ctrl Pts',(9.71708493723061,20.3580133103357,0.));
#209759=CARTESIAN_POINT('Ctrl Pts',(9.71708493723061,20.3580133103357,12.));
#209760=CARTESIAN_POINT('Ctrl Pts',(9.71816778327998,20.3601498764344,0.));
#209761=CARTESIAN_POINT('Ctrl Pts',(9.71816778327998,20.3601498764344,12.));
#209762=CARTESIAN_POINT('Ctrl Pts',(9.71943648548114,20.362625691398,0.));
#209763=CARTESIAN_POINT('Ctrl Pts',(9.71943648548114,20.362625691398,12.));
#209764=CARTESIAN_POINT('Ctrl Pts',(9.72088778381101,20.3654261611055,0.));
#209765=CARTESIAN_POINT('Ctrl Pts',(9.72088778381101,20.3654261611055,12.));
#209766=CARTESIAN_POINT('Ctrl Pts',(9.72251930722503,20.3685406190576,0.));
#209767=CARTESIAN_POINT('Ctrl Pts',(9.72251930722503,20.3685406190576,12.));
#209768=CARTESIAN_POINT('Ctrl Pts',(9.72432910043192,20.371960235676,0.));
#209769=CARTESIAN_POINT('Ctrl Pts',(9.72432910043192,20.371960235676,12.));
#209770=CARTESIAN_POINT('Ctrl Pts',(9.7263153173287,20.3756766651952,0.));
#209771=CARTESIAN_POINT('Ctrl Pts',(9.7263153173287,20.3756766651952,12.));
#209772=CARTESIAN_POINT('Ctrl Pts',(9.72847589116532,20.3796805893304,0.));
#209773=CARTESIAN_POINT('Ctrl Pts',(9.72847589116532,20.3796805893304,12.));
#209774=CARTESIAN_POINT('Ctrl Pts',(9.73080870123726,20.3839624556742,0.));
#209775=CARTESIAN_POINT('Ctrl Pts',(9.73080870123726,20.3839624556742,12.));
#209776=CARTESIAN_POINT('Ctrl Pts',(9.73331167102812,20.3885129129912,0.));
#209777=CARTESIAN_POINT('Ctrl Pts',(9.73331167102812,20.3885129129912,12.));
#209778=CARTESIAN_POINT('Ctrl Pts',(9.73598292014249,20.3933234845646,0.));
#209779=CARTESIAN_POINT('Ctrl Pts',(9.73598292014249,20.3933234845646,12.));
#209780=CARTESIAN_POINT('Ctrl Pts',(9.73882077613206,20.3983866213331,0.));
#209781=CARTESIAN_POINT('Ctrl Pts',(9.73882077613206,20.3983866213331,12.));
#209782=CARTESIAN_POINT('Ctrl Pts',(9.74182369656272,20.4036953576549,0.));
#209783=CARTESIAN_POINT('Ctrl Pts',(9.74182369656272,20.4036953576549,12.));
#209784=CARTESIAN_POINT('Ctrl Pts',(9.74499021838536,20.4092430879861,0.));
#209785=CARTESIAN_POINT('Ctrl Pts',(9.74499021838536,20.4092430879861,12.));
#209786=CARTESIAN_POINT('Ctrl Pts',(9.74831889242174,20.4150232777393,0.));
#209787=CARTESIAN_POINT('Ctrl Pts',(9.74831889242174,20.4150232777393,12.));
#209788=CARTESIAN_POINT('Ctrl Pts',(9.75180829786433,20.4210295275818,0.));
#209789=CARTESIAN_POINT('Ctrl Pts',(9.75180829786433,20.4210295275818,12.));
#209790=CARTESIAN_POINT('Ctrl Pts',(9.75545705902416,20.4272556476629,0.));
#209791=CARTESIAN_POINT('Ctrl Pts',(9.75545705902416,20.4272556476629,12.));
#209792=CARTESIAN_POINT('Ctrl Pts',(9.75926386289929,20.4336957355474,0.));
#209793=CARTESIAN_POINT('Ctrl Pts',(9.75926386289929,20.4336957355474,12.));
#209794=CARTESIAN_POINT('Ctrl Pts',(9.76322747195502,20.4403442329401,0.));
#209795=CARTESIAN_POINT('Ctrl Pts',(9.76322747195502,20.4403442329401,12.));
#209796=CARTESIAN_POINT('Ctrl Pts',(9.76734670980896,20.447195862298,0.));
#209797=CARTESIAN_POINT('Ctrl Pts',(9.76734670980896,20.447195862298,12.));
#209798=CARTESIAN_POINT('Ctrl Pts',(9.77162045104069,20.4542455817527,0.));
#209799=CARTESIAN_POINT('Ctrl Pts',(9.77162045104069,20.4542455817527,12.));
#209800=CARTESIAN_POINT('Ctrl Pts',(9.77604760815522,20.4614885274973,0.));
#209801=CARTESIAN_POINT('Ctrl Pts',(9.77604760815522,20.4614885274973,12.));
#209802=CARTESIAN_POINT('Ctrl Pts',(9.78062712373313,20.4689199790668,0.));
#209803=CARTESIAN_POINT('Ctrl Pts',(9.78062712373313,20.4689199790668,12.));
#209804=CARTESIAN_POINT('Ctrl Pts',(9.78535797314162,20.4765353711585,0.));
#209805=CARTESIAN_POINT('Ctrl Pts',(9.78535797314162,20.4765353711585,12.));
#209806=CARTESIAN_POINT('Ctrl Pts',(9.79023916498659,20.4843302955329,0.));
#209807=CARTESIAN_POINT('Ctrl Pts',(9.79023916498659,20.4843302955329,12.));
#209808=CARTESIAN_POINT('Ctrl Pts',(9.79526974288343,20.4923005087945,0.));
#209809=CARTESIAN_POINT('Ctrl Pts',(9.79526974288343,20.4923005087945,12.));
#209810=CARTESIAN_POINT('Ctrl Pts',(9.80044878520967,20.500441931211,0.));
#209811=CARTESIAN_POINT('Ctrl Pts',(9.80044878520967,20.500441931211,12.));
#209812=CARTESIAN_POINT('Ctrl Pts',(9.80577540161102,20.5087506310507,0.));
#209813=CARTESIAN_POINT('Ctrl Pts',(9.80577540161102,20.5087506310507,12.));
#209814=CARTESIAN_POINT('Ctrl Pts',(9.81124873025278,20.5172228122839,0.));
#209815=CARTESIAN_POINT('Ctrl Pts',(9.81124873025278,20.5172228122839,12.));
#209816=CARTESIAN_POINT('Ctrl Pts',(9.81686793455918,20.5258548000625,0.));
#209817=CARTESIAN_POINT('Ctrl Pts',(9.81686793455918,20.5258548000625,12.));
#209818=CARTESIAN_POINT('Ctrl Pts',(9.82263220080327,20.534643029951,0.));
#209819=CARTESIAN_POINT('Ctrl Pts',(9.82263220080327,20.534643029951,12.));
#209820=CARTESIAN_POINT('Ctrl Pts',(9.82854073773857,20.5435840460717,0.));
#209821=CARTESIAN_POINT('Ctrl Pts',(9.82854073773857,20.5435840460717,12.));
#209822=CARTESIAN_POINT('Ctrl Pts',(9.8345927758532,20.5526744976461,0.));
#209823=CARTESIAN_POINT('Ctrl Pts',(9.8345927758532,20.5526744976461,12.));
#209824=CARTESIAN_POINT('Ctrl Pts',(9.84078756677589,20.5619111362406,0.));
#209825=CARTESIAN_POINT('Ctrl Pts',(9.84078756677589,20.5619111362406,12.));
#209826=CARTESIAN_POINT('Ctrl Pts',(9.84712438256308,20.5712908125145,0.));
#209827=CARTESIAN_POINT('Ctrl Pts',(9.84712438256308,20.5712908125145,12.));
#209828=CARTESIAN_POINT('Ctrl Pts',(9.85360251457004,20.580810471002,0.));
#209829=CARTESIAN_POINT('Ctrl Pts',(9.85360251457004,20.580810471002,12.));
#209830=CARTESIAN_POINT('Ctrl Pts',(9.86022127232749,20.5904671449755,0.));
#209831=CARTESIAN_POINT('Ctrl Pts',(9.86022127232749,20.5904671449755,12.));
#209832=CARTESIAN_POINT('Ctrl Pts',(9.86697998242612,20.6002579513696,0.));
#209833=CARTESIAN_POINT('Ctrl Pts',(9.86697998242612,20.6002579513696,12.));
#209834=CARTESIAN_POINT('Ctrl Pts',(9.87387798732943,20.6101800854491,0.));
#209835=CARTESIAN_POINT('Ctrl Pts',(9.87387798732943,20.6101800854491,12.));
#209836=CARTESIAN_POINT('Ctrl Pts',(9.88091464472669,20.6202308177472,0.));
#209837=CARTESIAN_POINT('Ctrl Pts',(9.88091464472669,20.6202308177472,12.));
#209838=CARTESIAN_POINT('Ctrl Pts',(9.88808932697304,20.6304074914086,0.));
#209839=CARTESIAN_POINT('Ctrl Pts',(9.88808932697304,20.6304074914086,12.));
#209840=CARTESIAN_POINT('Ctrl Pts',(9.89540142049123,20.6407075193977,0.));
#209841=CARTESIAN_POINT('Ctrl Pts',(9.89540142049123,20.6407075193977,12.));
#209842=CARTESIAN_POINT('Ctrl Pts',(9.90285032516695,20.6511283817415,0.));
#209843=CARTESIAN_POINT('Ctrl Pts',(9.90285032516695,20.6511283817415,12.));
#209844=CARTESIAN_POINT('Ctrl Pts',(9.91043545377004,20.6616676228315,0.));
#209845=CARTESIAN_POINT('Ctrl Pts',(9.91043545377004,20.6616676228315,12.));
#209846=CARTESIAN_POINT('Ctrl Pts',(9.91815623141284,20.6723228488262,0.));
#209847=CARTESIAN_POINT('Ctrl Pts',(9.91815623141284,20.6723228488262,12.));
#209848=CARTESIAN_POINT('Ctrl Pts',(9.9260120949875,20.6830917250255,0.));
#209849=CARTESIAN_POINT('Ctrl Pts',(9.9260120949875,20.6830917250255,12.));
#209850=CARTESIAN_POINT('Ctrl Pts',(9.93400249259736,20.6939719732485,0.));
#209851=CARTESIAN_POINT('Ctrl Pts',(9.93400249259736,20.6939719732485,12.));
#209852=CARTESIAN_POINT('Ctrl Pts',(9.9421268829825,20.7049613692237,0.));
#209853=CARTESIAN_POINT('Ctrl Pts',(9.9421268829825,20.7049613692237,12.));
#209854=CARTESIAN_POINT('Ctrl Pts',(9.95038473514962,20.7160577407581,0.));
#209855=CARTESIAN_POINT('Ctrl Pts',(9.95038473514962,20.7160577407581,12.));
#209856=CARTESIAN_POINT('Ctrl Pts',(9.95877552798403,20.7272589658752,0.));
#209857=CARTESIAN_POINT('Ctrl Pts',(9.95877552798403,20.7272589658752,12.));
#209858=CARTESIAN_POINT('Ctrl Pts',(9.96729874986198,20.7385629709795,0.));
#209859=CARTESIAN_POINT('Ctrl Pts',(9.96729874986198,20.7385629709795,12.));
#209860=CARTESIAN_POINT('Ctrl Pts',(9.97595389823461,20.7499677289626,0.));
#209861=CARTESIAN_POINT('Ctrl Pts',(9.97595389823461,20.7499677289626,12.));
#209862=CARTESIAN_POINT('Ctrl Pts',(9.98474047926846,20.7614712574989,0.));
#209863=CARTESIAN_POINT('Ctrl Pts',(9.98474047926846,20.7614712574989,12.));
#209864=CARTESIAN_POINT('Ctrl Pts',(9.99365800754637,20.7730716175417,0.));
#209865=CARTESIAN_POINT('Ctrl Pts',(9.99365800754637,20.7730716175417,12.));
#209866=CARTESIAN_POINT('Ctrl Pts',(10.0027060057389,20.7847669117568,0.));
#209867=CARTESIAN_POINT('Ctrl Pts',(10.0027060057389,20.7847669117568,12.));
#209868=CARTESIAN_POINT('Ctrl Pts',(10.0118840042786,20.7965552829907,0.));
#209869=CARTESIAN_POINT('Ctrl Pts',(10.0118840042786,20.7965552829907,12.));
#209870=CARTESIAN_POINT('Ctrl Pts',(10.0211915410095,20.8084349126885,0.));
#209871=CARTESIAN_POINT('Ctrl Pts',(10.0211915410095,20.8084349126885,12.));
#209872=CARTESIAN_POINT('Ctrl Pts',(10.0306281609435,20.8204040196599,0.));
#209873=CARTESIAN_POINT('Ctrl Pts',(10.0306281609435,20.8204040196599,12.));
#209874=CARTESIAN_POINT('Ctrl Pts',(10.0401934160234,20.8324608588906,0.));
#209875=CARTESIAN_POINT('Ctrl Pts',(10.0401934160234,20.8324608588906,12.));
#209876=CARTESIAN_POINT('Ctrl Pts',(10.0498868648733,20.8446037203402,0.));
#209877=CARTESIAN_POINT('Ctrl Pts',(10.0498868648733,20.8446037203402,12.));
#209878=CARTESIAN_POINT('Ctrl Pts',(10.0597080725375,20.856830927732,0.));
#209879=CARTESIAN_POINT('Ctrl Pts',(10.0597080725375,20.856830927732,12.));
#209880=CARTESIAN_POINT('Ctrl Pts',(10.0696566102219,20.8691408373705,0.));
#209881=CARTESIAN_POINT('Ctrl Pts',(10.0696566102219,20.8691408373705,12.));
#209882=CARTESIAN_POINT('Ctrl Pts',(10.0797320551154,20.8815318371844,0.));
#209883=CARTESIAN_POINT('Ctrl Pts',(10.0797320551154,20.8815318371844,12.));
#209884=CARTESIAN_POINT('Ctrl Pts',(10.0899339901916,20.8940023457371,0.));
#209885=CARTESIAN_POINT('Ctrl Pts',(10.0899339901916,20.8940023457371,12.));
#209886=CARTESIAN_POINT('Ctrl Pts',(10.1002620040076,20.9065508112556,0.));
#209887=CARTESIAN_POINT('Ctrl Pts',(10.1002620040076,20.9065508112556,12.));
#209888=CARTESIAN_POINT('Ctrl Pts',(10.1107156904836,20.9191757106266,0.));
#209889=CARTESIAN_POINT('Ctrl Pts',(10.1107156904836,20.9191757106266,12.));
#209890=CARTESIAN_POINT('Ctrl Pts',(10.1212946487057,20.931875548473,0.));
#209891=CARTESIAN_POINT('Ctrl Pts',(10.1212946487057,20.931875548473,12.));
#209892=CARTESIAN_POINT('Ctrl Pts',(10.1319984827909,20.944648856393,0.));
#209893=CARTESIAN_POINT('Ctrl Pts',(10.1319984827909,20.944648856393,12.));
#209894=CARTESIAN_POINT('Ctrl Pts',(10.1428268017257,20.9574941921591,0.));
#209895=CARTESIAN_POINT('Ctrl Pts',(10.1428268017257,20.9574941921591,12.));
#209896=CARTESIAN_POINT('Ctrl Pts',(10.1537792192065,20.970410138937,0.));
#209897=CARTESIAN_POINT('Ctrl Pts',(10.1537792192065,20.970410138937,12.));
#209898=CARTESIAN_POINT('Ctrl Pts',(10.1648553534567,20.9833953044737,0.));
#209899=CARTESIAN_POINT('Ctrl Pts',(10.1648553534567,20.9833953044737,12.));
#209900=CARTESIAN_POINT('Ctrl Pts',(10.1760548270765,20.9964483203685,0.));
#209901=CARTESIAN_POINT('Ctrl Pts',(10.1760548270765,20.9964483203685,12.));
#209902=CARTESIAN_POINT('Ctrl Pts',(10.1873772669358,21.0095678414486,0.));
#209903=CARTESIAN_POINT('Ctrl Pts',(10.1873772669358,21.0095678414486,12.));
#209904=CARTESIAN_POINT('Ctrl Pts',(10.1988223040425,21.0227525451107,0.));
#209905=CARTESIAN_POINT('Ctrl Pts',(10.1988223040425,21.0227525451107,12.));
#209906=CARTESIAN_POINT('Ctrl Pts',(10.2103895734123,21.0360011306814,0.));
#209907=CARTESIAN_POINT('Ctrl Pts',(10.2103895734123,21.0360011306814,12.));
#209908=CARTESIAN_POINT('Ctrl Pts',(10.2220787139157,21.0493123187484,0.));
#209909=CARTESIAN_POINT('Ctrl Pts',(10.2220787139157,21.0493123187484,12.));
#209910=CARTESIAN_POINT('Ctrl Pts',(10.233889368157,21.0626848505665,0.));
#209911=CARTESIAN_POINT('Ctrl Pts',(10.233889368157,21.0626848505665,12.));
#209912=CARTESIAN_POINT('Ctrl Pts',(10.2458211823915,21.0761174875448,0.));
#209913=CARTESIAN_POINT('Ctrl Pts',(10.2458211823915,21.0761174875448,12.));
#209914=CARTESIAN_POINT('Ctrl Pts',(10.2578738064183,21.0896090107066,0.));
#209915=CARTESIAN_POINT('Ctrl Pts',(10.2578738064183,21.0896090107066,12.));
#209916=CARTESIAN_POINT('Ctrl Pts',(10.2700468934743,21.1031582201625,0.));
#209917=CARTESIAN_POINT('Ctrl Pts',(10.2700468934743,21.1031582201625,12.));
#209918=CARTESIAN_POINT('Ctrl Pts',(10.2823401001067,21.1167639345623,0.));
#209919=CARTESIAN_POINT('Ctrl Pts',(10.2823401001067,21.1167639345623,12.));
#209920=CARTESIAN_POINT('Ctrl Pts',(10.2947530860714,21.130424990599,0.));
#209921=CARTESIAN_POINT('Ctrl Pts',(10.2947530860714,21.130424990599,12.));
#209922=CARTESIAN_POINT('Ctrl Pts',(10.307285514268,21.1441402425831,0.));
#209923=CARTESIAN_POINT('Ctrl Pts',(10.307285514268,21.1441402425831,12.));
#209924=CARTESIAN_POINT('Ctrl Pts',(10.3199370506541,21.1579085619959,0.));
#209925=CARTESIAN_POINT('Ctrl Pts',(10.3199370506541,21.1579085619959,12.));
#209926=CARTESIAN_POINT('Ctrl Pts',(10.3327073641574,21.1717288370512,0.));
#209927=CARTESIAN_POINT('Ctrl Pts',(10.3327073641574,21.1717288370512,12.));
#209928=CARTESIAN_POINT('Ctrl Pts',(10.3455961265706,21.1855999722427,0.));
#209929=CARTESIAN_POINT('Ctrl Pts',(10.3455961265706,21.1855999722427,12.));
#209930=CARTESIAN_POINT('Ctrl Pts',(10.3586030124595,21.1995208879205,0.));
#209931=CARTESIAN_POINT('Ctrl Pts',(10.3586030124595,21.1995208879205,12.));
#209932=CARTESIAN_POINT('Ctrl Pts',(10.3717276991137,21.2134905199359,0.));
#209933=CARTESIAN_POINT('Ctrl Pts',(10.3717276991137,21.2134905199359,12.));
#209934=CARTESIAN_POINT('Ctrl Pts',(10.384969866479,21.2275078192708,0.));
#209935=CARTESIAN_POINT('Ctrl Pts',(10.384969866479,21.2275078192708,12.));
#209936=CARTESIAN_POINT('Ctrl Pts',(10.3983291970846,21.2415717516713,0.));
#209937=CARTESIAN_POINT('Ctrl Pts',(10.3983291970846,21.2415717516713,12.));
#209938=CARTESIAN_POINT('Ctrl Pts',(10.4118053759584,21.2556812972741,0.));
#209939=CARTESIAN_POINT('Ctrl Pts',(10.4118053759584,21.2556812972741,12.));
#209940=CARTESIAN_POINT('Ctrl Pts',(10.4253980905394,21.2698354502391,0.));
#209941=CARTESIAN_POINT('Ctrl Pts',(10.4253980905394,21.2698354502391,12.));
#209942=CARTESIAN_POINT('Ctrl Pts',(10.4391070306385,21.2840332184471,0.));
#209943=CARTESIAN_POINT('Ctrl Pts',(10.4391070306385,21.2840332184471,12.));
#209944=CARTESIAN_POINT('Ctrl Pts',(10.452931888387,21.2982736231924,0.));
#209945=CARTESIAN_POINT('Ctrl Pts',(10.452931888387,21.2982736231924,12.));
#209946=CARTESIAN_POINT('Ctrl Pts',(10.4668723581768,21.312555698873,0.));
#209947=CARTESIAN_POINT('Ctrl Pts',(10.4668723581768,21.312555698873,12.));
#209948=CARTESIAN_POINT('Ctrl Pts',(10.4809281365933,21.3268784926823,0.));
#209949=CARTESIAN_POINT('Ctrl Pts',(10.4809281365933,21.3268784926823,12.));
#209950=CARTESIAN_POINT('Ctrl Pts',(10.4950989223341,21.3412410642912,0.));
#209951=CARTESIAN_POINT('Ctrl Pts',(10.4950989223341,21.3412410642912,12.));
#209952=CARTESIAN_POINT('Ctrl Pts',(10.5093844161689,21.3556424855822,0.));
#209953=CARTESIAN_POINT('Ctrl Pts',(10.5093844161689,21.3556424855822,12.));
#209954=CARTESIAN_POINT('Ctrl Pts',(10.523784320906,21.3700818403942,0.));
#209955=CARTESIAN_POINT('Ctrl Pts',(10.523784320906,21.3700818403942,12.));
#209956=CARTESIAN_POINT('Ctrl Pts',(10.5382983413422,21.3845582242604,0.));
#209957=CARTESIAN_POINT('Ctrl Pts',(10.5382983413422,21.3845582242604,12.));
#209958=CARTESIAN_POINT('Ctrl Pts',(10.5529261842107,21.3990707441495,0.));
#209959=CARTESIAN_POINT('Ctrl Pts',(10.5529261842107,21.3990707441495,12.));
#209960=CARTESIAN_POINT('Ctrl Pts',(10.5676675581106,21.4136185181974,0.));
#209961=CARTESIAN_POINT('Ctrl Pts',(10.5676675581106,21.4136185181974,12.));
#209962=CARTESIAN_POINT('Ctrl Pts',(10.582522173457,21.4282006754624,0.));
#209963=CARTESIAN_POINT('Ctrl Pts',(10.582522173457,21.4282006754624,12.));
#209964=CARTESIAN_POINT('Ctrl Pts',(10.597489742462,21.4428163557137,0.));
#209965=CARTESIAN_POINT('Ctrl Pts',(10.597489742462,21.4428163557137,12.));
#209966=CARTESIAN_POINT('Ctrl Pts',(10.612569979096,21.4574647092093,0.));
#209967=CARTESIAN_POINT('Ctrl Pts',(10.612569979096,21.4574647092093,12.));
#209968=CARTESIAN_POINT('Ctrl Pts',(10.6277625990456,21.4721448964766,0.));
#209969=CARTESIAN_POINT('Ctrl Pts',(10.6277625990456,21.4721448964766,12.));
#209970=CARTESIAN_POINT('Ctrl Pts',(10.6430673196609,21.4868560880893,0.));
#209971=CARTESIAN_POINT('Ctrl Pts',(10.6430673196609,21.4868560880893,12.));
#209972=CARTESIAN_POINT('Ctrl Pts',(10.658483859894,21.5015974644454,0.));
#209973=CARTESIAN_POINT('Ctrl Pts',(10.658483859894,21.5015974644454,12.));
#209974=CARTESIAN_POINT('Ctrl Pts',(10.6740119402835,21.5163682155805,0.));
#209975=CARTESIAN_POINT('Ctrl Pts',(10.6740119402835,21.5163682155805,12.));
#209976=CARTESIAN_POINT('Ctrl Pts',(10.689651282929,21.531167540981,0.));
#209977=CARTESIAN_POINT('Ctrl Pts',(10.689651282929,21.531167540981,12.));
#209978=CARTESIAN_POINT('Ctrl Pts',(10.7054016114571,21.5459946493955,0.));
#209979=CARTESIAN_POINT('Ctrl Pts',(10.7054016114571,21.5459946493955,12.));
#209980=CARTESIAN_POINT('Ctrl Pts',(10.7212626509816,21.5608487586467,0.));
#209981=CARTESIAN_POINT('Ctrl Pts',(10.7212626509816,21.5608487586467,12.));
#209982=CARTESIAN_POINT('Ctrl Pts',(10.7372341280468,21.5757290954372,0.));
#209983=CARTESIAN_POINT('Ctrl Pts',(10.7372341280468,21.5757290954372,12.));
#209984=CARTESIAN_POINT('Ctrl Pts',(10.7533157705943,21.5906348951745,0.));
#209985=CARTESIAN_POINT('Ctrl Pts',(10.7533157705943,21.5906348951745,12.));
#209986=CARTESIAN_POINT('Ctrl Pts',(10.7695073079554,21.6055654018179,0.));
#209987=CARTESIAN_POINT('Ctrl Pts',(10.7695073079554,21.6055654018179,12.));
#209988=CARTESIAN_POINT('Ctrl Pts',(10.7858084708262,21.6205198677176,0.));
#209989=CARTESIAN_POINT('Ctrl Pts',(10.7858084708262,21.6205198677176,12.));
#209990=CARTESIAN_POINT('Ctrl Pts',(10.8022189912369,21.6354975534558,0.));
#209991=CARTESIAN_POINT('Ctrl Pts',(10.8022189912369,21.6354975534558,12.));
#209992=CARTESIAN_POINT('Ctrl Pts',(10.8187386025135,21.6504977276864,0.));
#209993=CARTESIAN_POINT('Ctrl Pts',(10.8187386025135,21.6504977276864,12.));
#209994=CARTESIAN_POINT('Ctrl Pts',(10.835367039227,21.6655196669727,0.));
#209995=CARTESIAN_POINT('Ctrl Pts',(10.835367039227,21.6655196669727,12.));
#209996=CARTESIAN_POINT('Ctrl Pts',(10.8521040371832,21.6805626556461,0.));
#209997=CARTESIAN_POINT('Ctrl Pts',(10.8521040371832,21.6805626556461,12.));
#209998=CARTESIAN_POINT('Ctrl Pts',(10.8689493334093,21.6956259856667,0.));
#209999=CARTESIAN_POINT('Ctrl Pts',(10.8689493334093,21.6956259856667,12.));
#210000=CARTESIAN_POINT('Ctrl Pts',(10.8859026661292,21.7107089564822,0.));
#210001=CARTESIAN_POINT('Ctrl Pts',(10.8859026661292,21.7107089564822,12.));
#210002=CARTESIAN_POINT('Ctrl Pts',(10.9029637747341,21.7258108748874,0.));
#210003=CARTESIAN_POINT('Ctrl Pts',(10.9029637747341,21.7258108748874,12.));
#210004=CARTESIAN_POINT('Ctrl Pts',(10.9201323997386,21.74093105488,0.));
#210005=CARTESIAN_POINT('Ctrl Pts',(10.9201323997386,21.74093105488,12.));
#210006=CARTESIAN_POINT('Ctrl Pts',(10.9374082827446,21.7560688175252,0.));
#210007=CARTESIAN_POINT('Ctrl Pts',(10.9374082827446,21.7560688175252,12.));
#210008=CARTESIAN_POINT('Ctrl Pts',(10.9547911664457,21.7712234908468,0.));
#210009=CARTESIAN_POINT('Ctrl Pts',(10.9547911664457,21.7712234908468,12.));
#210010=CARTESIAN_POINT('Ctrl Pts',(10.9722807946157,21.7863944097143,0.));
#210011=CARTESIAN_POINT('Ctrl Pts',(10.9722807946157,21.7863944097143,12.));
#210012=CARTESIAN_POINT('Ctrl Pts',(10.9898769120913,21.8015809157302,0.));
#210013=CARTESIAN_POINT('Ctrl Pts',(10.9898769120913,21.8015809157302,12.));
#210014=CARTESIAN_POINT('Ctrl Pts',(11.0075792647477,21.8167823571168,0.));
#210015=CARTESIAN_POINT('Ctrl Pts',(11.0075792647477,21.8167823571168,12.));
#210016=CARTESIAN_POINT('Ctrl Pts',(11.0253875994598,21.8319980886033,0.));
#210017=CARTESIAN_POINT('Ctrl Pts',(11.0253875994598,21.8319980886033,12.));
#210018=CARTESIAN_POINT('Ctrl Pts',(11.0433016640808,21.8472274713103,0.));
#210019=CARTESIAN_POINT('Ctrl Pts',(11.0433016640808,21.8472274713103,12.));
#210020=CARTESIAN_POINT('Ctrl Pts',(11.0613212074364,21.8624698726319,0.));
#210021=CARTESIAN_POINT('Ctrl Pts',(11.0613212074364,21.8624698726319,12.));
#210022=CARTESIAN_POINT('Ctrl Pts',(11.0794459793058,21.8777246661191,0.));
#210023=CARTESIAN_POINT('Ctrl Pts',(11.0794459793058,21.8777246661191,12.));
#210024=CARTESIAN_POINT('Ctrl Pts',(11.0976757303944,21.8929912313608,0.));
#210025=CARTESIAN_POINT('Ctrl Pts',(11.0976757303944,21.8929912313608,12.));
#210026=CARTESIAN_POINT('Ctrl Pts',(11.1160102123024,21.9082689538687,0.));
#210027=CARTESIAN_POINT('Ctrl Pts',(11.1160102123024,21.9082689538687,12.));
#210028=CARTESIAN_POINT('Ctrl Pts',(11.134449177474,21.9235572249518,0.));
#210029=CARTESIAN_POINT('Ctrl Pts',(11.134449177474,21.9235572249518,12.));
#210030=CARTESIAN_POINT('Ctrl Pts',(11.1529923792002,21.9388554416437,0.));
#210031=CARTESIAN_POINT('Ctrl Pts',(11.1529923792002,21.9388554416437,12.));
#210032=CARTESIAN_POINT('Ctrl Pts',(11.1716395716375,21.9541630066504,0.));
#210033=CARTESIAN_POINT('Ctrl Pts',(11.1716395716375,21.9541630066504,12.));
#210034=CARTESIAN_POINT('Ctrl Pts',(11.1903905098109,21.9694793282913,0.));
#210035=CARTESIAN_POINT('Ctrl Pts',(11.1903905098109,21.9694793282913,12.));
#210036=CARTESIAN_POINT('Ctrl Pts',(11.2092449496125,21.9848038204439,0.));
#210037=CARTESIAN_POINT('Ctrl Pts',(11.2092449496125,21.9848038204439,12.));
#210038=CARTESIAN_POINT('Ctrl Pts',(11.2282026477897,22.000135902484,0.));
#210039=CARTESIAN_POINT('Ctrl Pts',(11.2282026477897,22.000135902484,12.));
#210040=CARTESIAN_POINT('Ctrl Pts',(11.2472633619276,22.0154749992364,0.));
#210041=CARTESIAN_POINT('Ctrl Pts',(11.2472633619276,22.0154749992364,12.));
#210042=CARTESIAN_POINT('Ctrl Pts',(11.2664268504207,22.0308205408351,0.));
#210043=CARTESIAN_POINT('Ctrl Pts',(11.2664268504207,22.0308205408351,12.));
#210044=CARTESIAN_POINT('Ctrl Pts',(11.2856928724374,22.0461719625661,0.));
#210045=CARTESIAN_POINT('Ctrl Pts',(11.2856928724374,22.0461719625661,12.));
#210046=CARTESIAN_POINT('Ctrl Pts',(11.3050611878771,22.0615287047179,0.));
#210047=CARTESIAN_POINT('Ctrl Pts',(11.3050611878771,22.0615287047179,12.));
#210048=CARTESIAN_POINT('Ctrl Pts',(11.3245315573168,22.0768902124267,0.));
#210049=CARTESIAN_POINT('Ctrl Pts',(11.3245315573168,22.0768902124267,12.));
#210050=CARTESIAN_POINT('Ctrl Pts',(11.3441037419553,22.0922559355293,0.));
#210051=CARTESIAN_POINT('Ctrl Pts',(11.3441037419553,22.0922559355293,12.));
#210052=CARTESIAN_POINT('Ctrl Pts',(11.3637775035367,22.1076253283978,0.));
#210053=CARTESIAN_POINT('Ctrl Pts',(11.3637775035367,22.1076253283978,12.));
#210054=CARTESIAN_POINT('Ctrl Pts',(11.3835526044256,22.1229978500185,0.));
#210055=CARTESIAN_POINT('Ctrl Pts',(11.3835526044256,22.1229978500185,12.));
#210056=CARTESIAN_POINT('Ctrl Pts',(11.4034288076908,22.1383729640963,0.));
#210057=CARTESIAN_POINT('Ctrl Pts',(11.4034288076908,22.1383729640963,12.));
#210058=CARTESIAN_POINT('Ctrl Pts',(11.4234058771742,22.1537501391486,0.));
#210059=CARTESIAN_POINT('Ctrl Pts',(11.4234058771742,22.1537501391486,12.));
#210060=CARTESIAN_POINT('Ctrl Pts',(11.443483577557,22.1691288486096,0.));
#210061=CARTESIAN_POINT('Ctrl Pts',(11.443483577557,22.1691288486096,12.));
#210062=CARTESIAN_POINT('Ctrl Pts',(11.463661674411,22.184508570917,0.));
#210063=CARTESIAN_POINT('Ctrl Pts',(11.463661674411,22.184508570917,12.));
#210064=CARTESIAN_POINT('Ctrl Pts',(11.4839399342589,22.1998887896435,0.));
#210065=CARTESIAN_POINT('Ctrl Pts',(11.4839399342589,22.1998887896435,12.));
#210066=CARTESIAN_POINT('Ctrl Pts',(11.504318124424,22.215268993102,0.));
#210067=CARTESIAN_POINT('Ctrl Pts',(11.504318124424,22.215268993102,12.));
#210068=CARTESIAN_POINT('Ctrl Pts',(11.5247960128476,22.2306486738899,0.));
#210069=CARTESIAN_POINT('Ctrl Pts',(11.5247960128476,22.2306486738899,12.));
#210070=CARTESIAN_POINT('Ctrl Pts',(11.545373367912,22.2460273284653,0.));
#210071=CARTESIAN_POINT('Ctrl Pts',(11.545373367912,22.2460273284653,12.));
#210072=CARTESIAN_POINT('Ctrl Pts',(11.5660499582403,22.2614044566898,0.));
#210073=CARTESIAN_POINT('Ctrl Pts',(11.5660499582403,22.2614044566898,12.));
#210074=CARTESIAN_POINT('Ctrl Pts',(11.5868255525189,22.2767795614349,0.));
#210075=CARTESIAN_POINT('Ctrl Pts',(11.5868255525189,22.2767795614349,12.));
#210076=CARTESIAN_POINT('Ctrl Pts',(11.6076999192359,22.2921521480358,0.));
#210077=CARTESIAN_POINT('Ctrl Pts',(11.6076999192359,22.2921521480358,12.));
#210078=CARTESIAN_POINT('Ctrl Pts',(11.6286728270011,22.3075217249049,0.));
#210079=CARTESIAN_POINT('Ctrl Pts',(11.6286728270011,22.3075217249049,12.));
#210080=CARTESIAN_POINT('Ctrl Pts',(11.6497440449858,22.3228878043976,0.));
#210081=CARTESIAN_POINT('Ctrl Pts',(11.6497440449858,22.3228878043976,12.));
#210082=CARTESIAN_POINT('Ctrl Pts',(11.6709133432986,22.3382499035618,0.));
#210083=CARTESIAN_POINT('Ctrl Pts',(11.6709133432986,22.3382499035618,12.));
#210084=CARTESIAN_POINT('Ctrl Pts',(11.6921804934056,22.3536075450028,0.));
#210085=CARTESIAN_POINT('Ctrl Pts',(11.6921804934056,22.3536075450028,12.));
#210086=CARTESIAN_POINT('Ctrl Pts',(11.7135452684532,22.3689602575492,0.));
#210087=CARTESIAN_POINT('Ctrl Pts',(11.7135452684532,22.3689602575492,12.));
#210088=CARTESIAN_POINT('Ctrl Pts',(11.7350074437961,22.3843075773905,0.));
#210089=CARTESIAN_POINT('Ctrl Pts',(11.7350074437961,22.3843075773905,12.));
#210090=CARTESIAN_POINT('Ctrl Pts',(11.7565667964765,22.39964904692,0.));
#210091=CARTESIAN_POINT('Ctrl Pts',(11.7565667964765,22.39964904692,12.));
#210092=CARTESIAN_POINT('Ctrl Pts',(11.7782231042041,22.4149842125018,0.));
#210093=CARTESIAN_POINT('Ctrl Pts',(11.7782231042041,22.4149842125018,12.));
#210094=CARTESIAN_POINT('Ctrl Pts',(11.7999761445175,22.4303126226468,0.));
#210095=CARTESIAN_POINT('Ctrl Pts',(11.7999761445175,22.4303126226468,12.));
#210096=CARTESIAN_POINT('Ctrl Pts',(11.8218256937889,22.4456338258738,0.));
#210097=CARTESIAN_POINT('Ctrl Pts',(11.8218256937889,22.4456338258738,12.));
#210098=CARTESIAN_POINT('Ctrl Pts',(11.8437715264487,22.4609473690469,0.));
#210099=CARTESIAN_POINT('Ctrl Pts',(11.8437715264487,22.4609473690469,12.));
#210100=CARTESIAN_POINT('Ctrl Pts',(11.8658134137018,22.4762527946694,0.));
#210101=CARTESIAN_POINT('Ctrl Pts',(11.8658134137018,22.4762527946694,12.));
#210102=CARTESIAN_POINT('Ctrl Pts',(11.8879511239941,22.4915496418472,0.));
#210103=CARTESIAN_POINT('Ctrl Pts',(11.8879511239941,22.4915496418472,12.));
#210104=CARTESIAN_POINT('Ctrl Pts',(11.9101844254555,22.5068374513958,0.));
#210105=CARTESIAN_POINT('Ctrl Pts',(11.9101844254555,22.5068374513958,12.));
#210106=CARTESIAN_POINT('Ctrl Pts',(11.9325130877801,22.5221157697869,0.));
#210107=CARTESIAN_POINT('Ctrl Pts',(11.9325130877801,22.5221157697869,12.));
#210108=CARTESIAN_POINT('Ctrl Pts',(11.9549368843996,22.5373841537299,0.));
#210109=CARTESIAN_POINT('Ctrl Pts',(11.9549368843996,22.5373841537299,12.));
#210110=CARTESIAN_POINT('Ctrl Pts',(11.9774555943496,22.5526421741159,0.));
#210111=CARTESIAN_POINT('Ctrl Pts',(11.9774555943496,22.5526421741159,12.));
#210112=CARTESIAN_POINT('Ctrl Pts',(12.0000690046697,22.5678894211194,0.));
#210113=CARTESIAN_POINT('Ctrl Pts',(12.0000690046697,22.5678894211194,12.));
#210114=CARTESIAN_POINT('Ctrl Pts',(12.0227769113132,22.5831255061306,0.));
#210115=CARTESIAN_POINT('Ctrl Pts',(12.0227769113132,22.5831255061306,12.));
#210116=CARTESIAN_POINT('Ctrl Pts',(12.0455791139135,22.5983500505675,0.));
#210117=CARTESIAN_POINT('Ctrl Pts',(12.0455791139135,22.5983500505675,12.));
#210118=CARTESIAN_POINT('Ctrl Pts',(12.0684754113869,22.613562676493,0.));
#210119=CARTESIAN_POINT('Ctrl Pts',(12.0684754113869,22.613562676493,12.));
#210120=CARTESIAN_POINT('Ctrl Pts',(12.0914655972828,22.628762996708,0.));
#210121=CARTESIAN_POINT('Ctrl Pts',(12.0914655972828,22.628762996708,12.));
#210122=CARTESIAN_POINT('Ctrl Pts',(12.1145494550384,22.6439506046611,0.));
#210123=CARTESIAN_POINT('Ctrl Pts',(12.1145494550384,22.6439506046611,12.));
#210124=CARTESIAN_POINT('Ctrl Pts',(12.1377267537141,22.6591250653942,0.));
#210125=CARTESIAN_POINT('Ctrl Pts',(12.1377267537141,22.6591250653942,12.));
#210126=CARTESIAN_POINT('Ctrl Pts',(12.1609972423088,22.6742859034891,0.));
#210127=CARTESIAN_POINT('Ctrl Pts',(12.1609972423088,22.6742859034891,12.));
#210128=CARTESIAN_POINT('Ctrl Pts',(12.1843606579246,22.6894326204959,0.));
#210129=CARTESIAN_POINT('Ctrl Pts',(12.1843606579246,22.6894326204959,12.));
#210130=CARTESIAN_POINT('Ctrl Pts',(12.2078167360267,22.7045647168659,0.));
#210131=CARTESIAN_POINT('Ctrl Pts',(12.2078167360267,22.7045647168659,12.));
#210132=CARTESIAN_POINT('Ctrl Pts',(12.2313652198047,22.7196817119299,0.));
#210133=CARTESIAN_POINT('Ctrl Pts',(12.2313652198047,22.7196817119299,12.));
#210134=CARTESIAN_POINT('Ctrl Pts',(12.2550058702389,22.7347831655251,0.));
#210135=CARTESIAN_POINT('Ctrl Pts',(12.2550058702389,22.7347831655251,12.));
#210136=CARTESIAN_POINT('Ctrl Pts',(12.2787384750747,22.7498686970096,0.));
#210137=CARTESIAN_POINT('Ctrl Pts',(12.2787384750747,22.7498686970096,12.));
#210138=CARTESIAN_POINT('Ctrl Pts',(12.3025628601811,22.7649380101154,0.));
#210139=CARTESIAN_POINT('Ctrl Pts',(12.3025628601811,22.7649380101154,12.));
#210140=CARTESIAN_POINT('Ctrl Pts',(12.3264788926108,22.7799908974947,0.));
#210141=CARTESIAN_POINT('Ctrl Pts',(12.3264788926108,22.7799908974947,12.));
#210142=CARTESIAN_POINT('Ctrl Pts',(12.3504864740361,22.7950272216959,0.));
#210143=CARTESIAN_POINT('Ctrl Pts',(12.3504864740361,22.7950272216959,12.));
#210144=CARTESIAN_POINT('Ctrl Pts',(12.3745855366772,22.8100469022632,0.));
#210145=CARTESIAN_POINT('Ctrl Pts',(12.3745855366772,22.8100469022632,12.));
#210146=CARTESIAN_POINT('Ctrl Pts',(12.393937937903,22.8220493007353,0.));
#210147=CARTESIAN_POINT('Ctrl Pts',(12.393937937903,22.8220493007353,12.));
#210148=CARTESIAN_POINT('Ctrl Pts',(12.4084933766366,22.8310435872852,0.));
#210149=CARTESIAN_POINT('Ctrl Pts',(12.4084933766366,22.8310435872852,12.));
#210150=CARTESIAN_POINT('Ctrl Pts',(12.4182152851867,22.8370364396497,0.));
#210151=CARTESIAN_POINT('Ctrl Pts',(12.4182152851867,22.8370364396497,12.));
#210152=CARTESIAN_POINT('Ctrl Pts',(12.4230808101438,22.8400320311648,0.));
#210153=CARTESIAN_POINT('Ctrl Pts',(12.4230808101438,22.8400320311648,12.));
#210154=CARTESIAN_POINT('',(12.4230808101438,22.8400320311648,0.));
#210155=CARTESIAN_POINT('Ctrl Pts',(9.71462809124917,20.353053841303,0.));
#210156=CARTESIAN_POINT('Ctrl Pts',(9.71462954053074,20.353060251684,0.));
#210157=CARTESIAN_POINT('Ctrl Pts',(9.71465227853122,20.3531126095522,0.));
#210158=CARTESIAN_POINT('Ctrl Pts',(9.71474590350791,20.3533097561886,0.));
#210159=CARTESIAN_POINT('Ctrl Pts',(9.714989780521,20.3538098605706,0.));
#210160=CARTESIAN_POINT('Ctrl Pts',(9.71549257088174,20.3548282742361,0.));
#210161=CARTESIAN_POINT('Ctrl Pts',(9.71619192554146,20.3562337557875,0.));
#210162=CARTESIAN_POINT('Ctrl Pts',(9.71708493723061,20.3580133103357,0.));
#210163=CARTESIAN_POINT('Ctrl Pts',(9.71816778327998,20.3601498764344,0.));
#210164=CARTESIAN_POINT('Ctrl Pts',(9.71943648548114,20.362625691398,0.));
#210165=CARTESIAN_POINT('Ctrl Pts',(9.72088778381101,20.3654261611055,0.));
#210166=CARTESIAN_POINT('Ctrl Pts',(9.72251930722503,20.3685406190576,0.));
#210167=CARTESIAN_POINT('Ctrl Pts',(9.72432910043192,20.371960235676,0.));
#210168=CARTESIAN_POINT('Ctrl Pts',(9.7263153173287,20.3756766651952,0.));
#210169=CARTESIAN_POINT('Ctrl Pts',(9.72847589116532,20.3796805893304,0.));
#210170=CARTESIAN_POINT('Ctrl Pts',(9.73080870123726,20.3839624556742,0.));
#210171=CARTESIAN_POINT('Ctrl Pts',(9.73331167102812,20.3885129129912,0.));
#210172=CARTESIAN_POINT('Ctrl Pts',(9.73598292014249,20.3933234845646,0.));
#210173=CARTESIAN_POINT('Ctrl Pts',(9.73882077613206,20.3983866213331,0.));
#210174=CARTESIAN_POINT('Ctrl Pts',(9.74182369656272,20.4036953576549,0.));
#210175=CARTESIAN_POINT('Ctrl Pts',(9.74499021838536,20.4092430879861,0.));
#210176=CARTESIAN_POINT('Ctrl Pts',(9.74831889242174,20.4150232777393,0.));
#210177=CARTESIAN_POINT('Ctrl Pts',(9.75180829786433,20.4210295275818,0.));
#210178=CARTESIAN_POINT('Ctrl Pts',(9.75545705902416,20.4272556476629,0.));
#210179=CARTESIAN_POINT('Ctrl Pts',(9.75926386289929,20.4336957355474,0.));
#210180=CARTESIAN_POINT('Ctrl Pts',(9.76322747195502,20.4403442329401,0.));
#210181=CARTESIAN_POINT('Ctrl Pts',(9.76734670980896,20.447195862298,0.));
#210182=CARTESIAN_POINT('Ctrl Pts',(9.77162045104069,20.4542455817527,0.));
#210183=CARTESIAN_POINT('Ctrl Pts',(9.77604760815522,20.4614885274973,0.));
#210184=CARTESIAN_POINT('Ctrl Pts',(9.78062712373313,20.4689199790668,0.));
#210185=CARTESIAN_POINT('Ctrl Pts',(9.78535797314162,20.4765353711585,0.));
#210186=CARTESIAN_POINT('Ctrl Pts',(9.79023916498659,20.4843302955329,0.));
#210187=CARTESIAN_POINT('Ctrl Pts',(9.79526974288343,20.4923005087945,0.));
#210188=CARTESIAN_POINT('Ctrl Pts',(9.80044878520967,20.500441931211,0.));
#210189=CARTESIAN_POINT('Ctrl Pts',(9.80577540161102,20.5087506310507,0.));
#210190=CARTESIAN_POINT('Ctrl Pts',(9.81124873025278,20.5172228122839,0.));
#210191=CARTESIAN_POINT('Ctrl Pts',(9.81686793455918,20.5258548000625,0.));
#210192=CARTESIAN_POINT('Ctrl Pts',(9.82263220080327,20.534643029951,0.));
#210193=CARTESIAN_POINT('Ctrl Pts',(9.82854073773857,20.5435840460717,0.));
#210194=CARTESIAN_POINT('Ctrl Pts',(9.8345927758532,20.5526744976461,0.));
#210195=CARTESIAN_POINT('Ctrl Pts',(9.84078756677589,20.5619111362406,0.));
#210196=CARTESIAN_POINT('Ctrl Pts',(9.84712438256308,20.5712908125145,0.));
#210197=CARTESIAN_POINT('Ctrl Pts',(9.85360251457004,20.580810471002,0.));
#210198=CARTESIAN_POINT('Ctrl Pts',(9.86022127232749,20.5904671449755,0.));
#210199=CARTESIAN_POINT('Ctrl Pts',(9.86697998242612,20.6002579513696,0.));
#210200=CARTESIAN_POINT('Ctrl Pts',(9.87387798732943,20.6101800854491,0.));
#210201=CARTESIAN_POINT('Ctrl Pts',(9.88091464472669,20.6202308177472,0.));
#210202=CARTESIAN_POINT('Ctrl Pts',(9.88808932697304,20.6304074914086,0.));
#210203=CARTESIAN_POINT('Ctrl Pts',(9.89540142049123,20.6407075193977,0.));
#210204=CARTESIAN_POINT('Ctrl Pts',(9.90285032516695,20.6511283817415,0.));
#210205=CARTESIAN_POINT('Ctrl Pts',(9.91043545377004,20.6616676228315,0.));
#210206=CARTESIAN_POINT('Ctrl Pts',(9.91815623141284,20.6723228488262,0.));
#210207=CARTESIAN_POINT('Ctrl Pts',(9.9260120949875,20.6830917250255,0.));
#210208=CARTESIAN_POINT('Ctrl Pts',(9.93400249259736,20.6939719732485,0.));
#210209=CARTESIAN_POINT('Ctrl Pts',(9.9421268829825,20.7049613692237,0.));
#210210=CARTESIAN_POINT('Ctrl Pts',(9.95038473514962,20.7160577407581,0.));
#210211=CARTESIAN_POINT('Ctrl Pts',(9.95877552798403,20.7272589658752,0.));
#210212=CARTESIAN_POINT('Ctrl Pts',(9.96729874986198,20.7385629709795,0.));
#210213=CARTESIAN_POINT('Ctrl Pts',(9.97595389823461,20.7499677289626,0.));
#210214=CARTESIAN_POINT('Ctrl Pts',(9.98474047926846,20.7614712574989,0.));
#210215=CARTESIAN_POINT('Ctrl Pts',(9.99365800754637,20.7730716175417,0.));
#210216=CARTESIAN_POINT('Ctrl Pts',(10.0027060057389,20.7847669117568,0.));
#210217=CARTESIAN_POINT('Ctrl Pts',(10.0118840042786,20.7965552829907,0.));
#210218=CARTESIAN_POINT('Ctrl Pts',(10.0211915410095,20.8084349126885,0.));
#210219=CARTESIAN_POINT('Ctrl Pts',(10.0306281609435,20.8204040196599,0.));
#210220=CARTESIAN_POINT('Ctrl Pts',(10.0401934160234,20.8324608588906,0.));
#210221=CARTESIAN_POINT('Ctrl Pts',(10.0498868648733,20.8446037203402,0.));
#210222=CARTESIAN_POINT('Ctrl Pts',(10.0597080725375,20.856830927732,0.));
#210223=CARTESIAN_POINT('Ctrl Pts',(10.0696566102219,20.8691408373705,0.));
#210224=CARTESIAN_POINT('Ctrl Pts',(10.0797320551154,20.8815318371844,0.));
#210225=CARTESIAN_POINT('Ctrl Pts',(10.0899339901916,20.8940023457371,0.));
#210226=CARTESIAN_POINT('Ctrl Pts',(10.1002620040076,20.9065508112556,0.));
#210227=CARTESIAN_POINT('Ctrl Pts',(10.1107156904836,20.9191757106266,0.));
#210228=CARTESIAN_POINT('Ctrl Pts',(10.1212946487057,20.931875548473,0.));
#210229=CARTESIAN_POINT('Ctrl Pts',(10.1319984827909,20.944648856393,0.));
#210230=CARTESIAN_POINT('Ctrl Pts',(10.1428268017257,20.9574941921591,0.));
#210231=CARTESIAN_POINT('Ctrl Pts',(10.1537792192065,20.970410138937,0.));
#210232=CARTESIAN_POINT('Ctrl Pts',(10.1648553534567,20.9833953044737,0.));
#210233=CARTESIAN_POINT('Ctrl Pts',(10.1760548270765,20.9964483203685,0.));
#210234=CARTESIAN_POINT('Ctrl Pts',(10.1873772669358,21.0095678414486,0.));
#210235=CARTESIAN_POINT('Ctrl Pts',(10.1988223040425,21.0227525451107,0.));
#210236=CARTESIAN_POINT('Ctrl Pts',(10.2103895734123,21.0360011306814,0.));
#210237=CARTESIAN_POINT('Ctrl Pts',(10.2220787139157,21.0493123187484,0.));
#210238=CARTESIAN_POINT('Ctrl Pts',(10.233889368157,21.0626848505665,0.));
#210239=CARTESIAN_POINT('Ctrl Pts',(10.2458211823915,21.0761174875448,0.));
#210240=CARTESIAN_POINT('Ctrl Pts',(10.2578738064183,21.0896090107066,0.));
#210241=CARTESIAN_POINT('Ctrl Pts',(10.2700468934743,21.1031582201625,0.));
#210242=CARTESIAN_POINT('Ctrl Pts',(10.2823401001067,21.1167639345623,0.));
#210243=CARTESIAN_POINT('Ctrl Pts',(10.2947530860714,21.130424990599,0.));
#210244=CARTESIAN_POINT('Ctrl Pts',(10.307285514268,21.1441402425831,0.));
#210245=CARTESIAN_POINT('Ctrl Pts',(10.3199370506541,21.1579085619959,0.));
#210246=CARTESIAN_POINT('Ctrl Pts',(10.3327073641574,21.1717288370512,0.));
#210247=CARTESIAN_POINT('Ctrl Pts',(10.3455961265706,21.1855999722427,0.));
#210248=CARTESIAN_POINT('Ctrl Pts',(10.3586030124595,21.1995208879205,0.));
#210249=CARTESIAN_POINT('Ctrl Pts',(10.3717276991137,21.2134905199359,0.));
#210250=CARTESIAN_POINT('Ctrl Pts',(10.384969866479,21.2275078192708,0.));
#210251=CARTESIAN_POINT('Ctrl Pts',(10.3983291970846,21.2415717516713,0.));
#210252=CARTESIAN_POINT('Ctrl Pts',(10.4118053759584,21.2556812972741,0.));
#210253=CARTESIAN_POINT('Ctrl Pts',(10.4253980905394,21.2698354502391,0.));
#210254=CARTESIAN_POINT('Ctrl Pts',(10.4391070306385,21.2840332184471,0.));
#210255=CARTESIAN_POINT('Ctrl Pts',(10.452931888387,21.2982736231924,0.));
#210256=CARTESIAN_POINT('Ctrl Pts',(10.4668723581768,21.312555698873,0.));
#210257=CARTESIAN_POINT('Ctrl Pts',(10.4809281365933,21.3268784926823,0.));
#210258=CARTESIAN_POINT('Ctrl Pts',(10.4950989223341,21.3412410642912,0.));
#210259=CARTESIAN_POINT('Ctrl Pts',(10.5093844161689,21.3556424855822,0.));
#210260=CARTESIAN_POINT('Ctrl Pts',(10.523784320906,21.3700818403942,0.));
#210261=CARTESIAN_POINT('Ctrl Pts',(10.5382983413422,21.3845582242604,0.));
#210262=CARTESIAN_POINT('Ctrl Pts',(10.5529261842107,21.3990707441495,0.));
#210263=CARTESIAN_POINT('Ctrl Pts',(10.5676675581106,21.4136185181974,0.));
#210264=CARTESIAN_POINT('Ctrl Pts',(10.582522173457,21.4282006754624,0.));
#210265=CARTESIAN_POINT('Ctrl Pts',(10.597489742462,21.4428163557137,0.));
#210266=CARTESIAN_POINT('Ctrl Pts',(10.612569979096,21.4574647092093,0.));
#210267=CARTESIAN_POINT('Ctrl Pts',(10.6277625990456,21.4721448964766,0.));
#210268=CARTESIAN_POINT('Ctrl Pts',(10.6430673196609,21.4868560880893,0.));
#210269=CARTESIAN_POINT('Ctrl Pts',(10.658483859894,21.5015974644454,0.));
#210270=CARTESIAN_POINT('Ctrl Pts',(10.6740119402835,21.5163682155805,0.));
#210271=CARTESIAN_POINT('Ctrl Pts',(10.689651282929,21.531167540981,0.));
#210272=CARTESIAN_POINT('Ctrl Pts',(10.7054016114571,21.5459946493955,0.));
#210273=CARTESIAN_POINT('Ctrl Pts',(10.7212626509816,21.5608487586467,0.));
#210274=CARTESIAN_POINT('Ctrl Pts',(10.7372341280468,21.5757290954372,0.));
#210275=CARTESIAN_POINT('Ctrl Pts',(10.7533157705943,21.5906348951745,0.));
#210276=CARTESIAN_POINT('Ctrl Pts',(10.7695073079554,21.6055654018179,0.));
#210277=CARTESIAN_POINT('Ctrl Pts',(10.7858084708262,21.6205198677176,0.));
#210278=CARTESIAN_POINT('Ctrl Pts',(10.8022189912369,21.6354975534558,0.));
#210279=CARTESIAN_POINT('Ctrl Pts',(10.8187386025135,21.6504977276864,0.));
#210280=CARTESIAN_POINT('Ctrl Pts',(10.835367039227,21.6655196669727,0.));
#210281=CARTESIAN_POINT('Ctrl Pts',(10.8521040371832,21.6805626556461,0.));
#210282=CARTESIAN_POINT('Ctrl Pts',(10.8689493334093,21.6956259856667,0.));
#210283=CARTESIAN_POINT('Ctrl Pts',(10.8859026661292,21.7107089564822,0.));
#210284=CARTESIAN_POINT('Ctrl Pts',(10.9029637747341,21.7258108748874,0.));
#210285=CARTESIAN_POINT('Ctrl Pts',(10.9201323997386,21.74093105488,0.));
#210286=CARTESIAN_POINT('Ctrl Pts',(10.9374082827446,21.7560688175252,0.));
#210287=CARTESIAN_POINT('Ctrl Pts',(10.9547911664457,21.7712234908468,0.));
#210288=CARTESIAN_POINT('Ctrl Pts',(10.9722807946157,21.7863944097143,0.));
#210289=CARTESIAN_POINT('Ctrl Pts',(10.9898769120913,21.8015809157302,0.));
#210290=CARTESIAN_POINT('Ctrl Pts',(11.0075792647477,21.8167823571168,0.));
#210291=CARTESIAN_POINT('Ctrl Pts',(11.0253875994598,21.8319980886033,0.));
#210292=CARTESIAN_POINT('Ctrl Pts',(11.0433016640808,21.8472274713103,0.));
#210293=CARTESIAN_POINT('Ctrl Pts',(11.0613212074364,21.8624698726319,0.));
#210294=CARTESIAN_POINT('Ctrl Pts',(11.0794459793058,21.8777246661191,0.));
#210295=CARTESIAN_POINT('Ctrl Pts',(11.0976757303944,21.8929912313608,0.));
#210296=CARTESIAN_POINT('Ctrl Pts',(11.1160102123024,21.9082689538687,0.));
#210297=CARTESIAN_POINT('Ctrl Pts',(11.134449177474,21.9235572249518,0.));
#210298=CARTESIAN_POINT('Ctrl Pts',(11.1529923792002,21.9388554416437,0.));
#210299=CARTESIAN_POINT('Ctrl Pts',(11.1716395716375,21.9541630066504,0.));
#210300=CARTESIAN_POINT('Ctrl Pts',(11.1903905098109,21.9694793282913,0.));
#210301=CARTESIAN_POINT('Ctrl Pts',(11.2092449496125,21.9848038204439,0.));
#210302=CARTESIAN_POINT('Ctrl Pts',(11.2282026477897,22.000135902484,0.));
#210303=CARTESIAN_POINT('Ctrl Pts',(11.2472633619276,22.0154749992364,0.));
#210304=CARTESIAN_POINT('Ctrl Pts',(11.2664268504207,22.0308205408351,0.));
#210305=CARTESIAN_POINT('Ctrl Pts',(11.2856928724374,22.0461719625661,0.));
#210306=CARTESIAN_POINT('Ctrl Pts',(11.3050611878771,22.0615287047179,0.));
#210307=CARTESIAN_POINT('Ctrl Pts',(11.3245315573168,22.0768902124267,0.));
#210308=CARTESIAN_POINT('Ctrl Pts',(11.3441037419553,22.0922559355293,0.));
#210309=CARTESIAN_POINT('Ctrl Pts',(11.3637775035367,22.1076253283978,0.));
#210310=CARTESIAN_POINT('Ctrl Pts',(11.3835526044256,22.1229978500185,0.));
#210311=CARTESIAN_POINT('Ctrl Pts',(11.4034288076908,22.1383729640963,0.));
#210312=CARTESIAN_POINT('Ctrl Pts',(11.4234058771742,22.1537501391486,0.));
#210313=CARTESIAN_POINT('Ctrl Pts',(11.443483577557,22.1691288486096,0.));
#210314=CARTESIAN_POINT('Ctrl Pts',(11.463661674411,22.184508570917,0.));
#210315=CARTESIAN_POINT('Ctrl Pts',(11.4839399342589,22.1998887896435,0.));
#210316=CARTESIAN_POINT('Ctrl Pts',(11.504318124424,22.215268993102,0.));
#210317=CARTESIAN_POINT('Ctrl Pts',(11.5247960128476,22.2306486738899,0.));
#210318=CARTESIAN_POINT('Ctrl Pts',(11.545373367912,22.2460273284653,0.));
#210319=CARTESIAN_POINT('Ctrl Pts',(11.5660499582403,22.2614044566898,0.));
#210320=CARTESIAN_POINT('Ctrl Pts',(11.5868255525189,22.2767795614349,0.));
#210321=CARTESIAN_POINT('Ctrl Pts',(11.6076999192359,22.2921521480358,0.));
#210322=CARTESIAN_POINT('Ctrl Pts',(11.6286728270011,22.3075217249049,0.));
#210323=CARTESIAN_POINT('Ctrl Pts',(11.6497440449858,22.3228878043976,0.));
#210324=CARTESIAN_POINT('Ctrl Pts',(11.6709133432986,22.3382499035618,0.));
#210325=CARTESIAN_POINT('Ctrl Pts',(11.6921804934056,22.3536075450028,0.));
#210326=CARTESIAN_POINT('Ctrl Pts',(11.7135452684532,22.3689602575492,0.));
#210327=CARTESIAN_POINT('Ctrl Pts',(11.7350074437961,22.3843075773905,0.));
#210328=CARTESIAN_POINT('Ctrl Pts',(11.7565667964765,22.39964904692,0.));
#210329=CARTESIAN_POINT('Ctrl Pts',(11.7782231042041,22.4149842125018,0.));
#210330=CARTESIAN_POINT('Ctrl Pts',(11.7999761445175,22.4303126226468,0.));
#210331=CARTESIAN_POINT('Ctrl Pts',(11.8218256937889,22.4456338258738,0.));
#210332=CARTESIAN_POINT('Ctrl Pts',(11.8437715264487,22.4609473690469,0.));
#210333=CARTESIAN_POINT('Ctrl Pts',(11.8658134137018,22.4762527946694,0.));
#210334=CARTESIAN_POINT('Ctrl Pts',(11.8879511239941,22.4915496418472,0.));
#210335=CARTESIAN_POINT('Ctrl Pts',(11.9101844254555,22.5068374513958,0.));
#210336=CARTESIAN_POINT('Ctrl Pts',(11.9325130877801,22.5221157697869,0.));
#210337=CARTESIAN_POINT('Ctrl Pts',(11.9549368843996,22.5373841537299,0.));
#210338=CARTESIAN_POINT('Ctrl Pts',(11.9774555943496,22.5526421741159,0.));
#210339=CARTESIAN_POINT('Ctrl Pts',(12.0000690046697,22.5678894211194,0.));
#210340=CARTESIAN_POINT('Ctrl Pts',(12.0227769113132,22.5831255061306,0.));
#210341=CARTESIAN_POINT('Ctrl Pts',(12.0455791139135,22.5983500505675,0.));
#210342=CARTESIAN_POINT('Ctrl Pts',(12.0684754113869,22.613562676493,0.));
#210343=CARTESIAN_POINT('Ctrl Pts',(12.0914655972828,22.628762996708,0.));
#210344=CARTESIAN_POINT('Ctrl Pts',(12.1145494550384,22.6439506046611,0.));
#210345=CARTESIAN_POINT('Ctrl Pts',(12.1377267537141,22.6591250653942,0.));
#210346=CARTESIAN_POINT('Ctrl Pts',(12.1609972423088,22.6742859034891,0.));
#210347=CARTESIAN_POINT('Ctrl Pts',(12.1843606579246,22.6894326204959,0.));
#210348=CARTESIAN_POINT('Ctrl Pts',(12.2078167360267,22.7045647168659,0.));
#210349=CARTESIAN_POINT('Ctrl Pts',(12.2313652198047,22.7196817119299,0.));
#210350=CARTESIAN_POINT('Ctrl Pts',(12.2550058702389,22.7347831655251,0.));
#210351=CARTESIAN_POINT('Ctrl Pts',(12.2787384750747,22.7498686970096,0.));
#210352=CARTESIAN_POINT('Ctrl Pts',(12.3025628601811,22.7649380101154,0.));
#210353=CARTESIAN_POINT('Ctrl Pts',(12.3264788926108,22.7799908974947,0.));
#210354=CARTESIAN_POINT('Ctrl Pts',(12.3504864740361,22.7950272216959,0.));
#210355=CARTESIAN_POINT('Ctrl Pts',(12.3745855366772,22.8100469022632,0.));
#210356=CARTESIAN_POINT('Ctrl Pts',(12.393937937903,22.8220493007353,0.));
#210357=CARTESIAN_POINT('Ctrl Pts',(12.4084933766366,22.8310435872852,0.));
#210358=CARTESIAN_POINT('Ctrl Pts',(12.4182152851867,22.8370364396497,0.));
#210359=CARTESIAN_POINT('Ctrl Pts',(12.4230808101438,22.8400320311648,0.));
#210360=CARTESIAN_POINT('',(12.4230808101438,22.8400320311648,0.));
#210361=CARTESIAN_POINT('Origin',(13.9675290154577,16.3449727195352,0.));
#210362=CARTESIAN_POINT('',(14.6513681262571,17.1452095830633,0.));
#210363=CARTESIAN_POINT('',(14.6513681262571,17.1452095830633,0.));
#210364=CARTESIAN_POINT('',(6.98376450772883,8.17248635976757,0.));
#210365=CARTESIAN_POINT('Ctrl Pts',(13.5685075571671,22.1787195904339,0.));
#210366=CARTESIAN_POINT('Ctrl Pts',(13.5685075571671,22.1787195904339,12.));
#210367=CARTESIAN_POINT('Ctrl Pts',(13.5683460612913,22.1730081264583,0.));
#210368=CARTESIAN_POINT('Ctrl Pts',(13.5683460612913,22.1730081264583,12.));
#210369=CARTESIAN_POINT('Ctrl Pts',(13.5680170531724,22.1615922804939,0.));
#210370=CARTESIAN_POINT('Ctrl Pts',(13.5680170531724,22.1615922804939,12.));
#210371=CARTESIAN_POINT('Ctrl Pts',(13.5675054918922,22.1444897575076,0.));
#210372=CARTESIAN_POINT('Ctrl Pts',(13.5675054918922,22.1444897575076,12.));
#210373=CARTESIAN_POINT('Ctrl Pts',(13.5667873105179,22.1217288871823,0.));
#210374=CARTESIAN_POINT('Ctrl Pts',(13.5667873105179,22.1217288871823,12.));
#210375=CARTESIAN_POINT('Ctrl Pts',(13.5658294169106,22.0933486464442,0.));
#210376=CARTESIAN_POINT('Ctrl Pts',(13.5658294169106,22.0933486464442,12.));
#210377=CARTESIAN_POINT('Ctrl Pts',(13.5648113688894,22.0650393089492,0.));
#210378=CARTESIAN_POINT('Ctrl Pts',(13.5648113688894,22.0650393089492,12.));
#210379=CARTESIAN_POINT('Ctrl Pts',(13.5637332022393,22.0368009736227,0.));
#210380=CARTESIAN_POINT('Ctrl Pts',(13.5637332022393,22.0368009736227,12.));
#210381=CARTESIAN_POINT('Ctrl Pts',(13.5625949868313,22.0086337943431,0.));
#210382=CARTESIAN_POINT('Ctrl Pts',(13.5625949868313,22.0086337943431,12.));
#210383=CARTESIAN_POINT('Ctrl Pts',(13.5613968357589,21.9805379899192,0.));
#210384=CARTESIAN_POINT('Ctrl Pts',(13.5613968357589,21.9805379899192,12.));
#210385=CARTESIAN_POINT('Ctrl Pts',(13.5601389185315,21.9525138592862,0.));
#210386=CARTESIAN_POINT('Ctrl Pts',(13.5601389185315,21.9525138592862,12.));
#210387=CARTESIAN_POINT('Ctrl Pts',(13.5588214586672,21.9245617765827,0.));
#210388=CARTESIAN_POINT('Ctrl Pts',(13.5588214586672,21.9245617765827,12.));
#210389=CARTESIAN_POINT('Ctrl Pts',(13.5574447178484,21.8966821688876,0.));
#210390=CARTESIAN_POINT('Ctrl Pts',(13.5574447178484,21.8966821688876,12.));
#210391=CARTESIAN_POINT('Ctrl Pts',(13.5560089839426,21.8688754989401,0.));
#210392=CARTESIAN_POINT('Ctrl Pts',(13.5560089839426,21.8688754989401,12.));
#210393=CARTESIAN_POINT('Ctrl Pts',(13.5545145573048,21.841142245609,0.));
#210394=CARTESIAN_POINT('Ctrl Pts',(13.5545145573048,21.841142245609,12.));
#210395=CARTESIAN_POINT('Ctrl Pts',(13.5529617381569,21.8134828857963,0.));
#210396=CARTESIAN_POINT('Ctrl Pts',(13.5529617381569,21.8134828857963,12.));
#210397=CARTESIAN_POINT('Ctrl Pts',(13.5513508127232,21.7858978745848,0.));
#210398=CARTESIAN_POINT('Ctrl Pts',(13.5513508127232,21.7858978745848,12.));
#210399=CARTESIAN_POINT('Ctrl Pts',(13.5496820422186,21.7583876294532,0.));
#210400=CARTESIAN_POINT('Ctrl Pts',(13.5496820422186,21.7583876294532,12.));
#210401=CARTESIAN_POINT('Ctrl Pts',(13.5479556704457,21.730952541226,0.));
#210402=CARTESIAN_POINT('Ctrl Pts',(13.5479556704457,21.730952541226,12.));
#210403=CARTESIAN_POINT('Ctrl Pts',(13.546171929503,21.7035929822939,0.));
#210404=CARTESIAN_POINT('Ctrl Pts',(13.546171929503,21.7035929822939,12.));
#210405=CARTESIAN_POINT('Ctrl Pts',(13.5443310461516,21.676309315769,0.));
#210406=CARTESIAN_POINT('Ctrl Pts',(13.5443310461516,21.676309315769,12.));
#210407=CARTESIAN_POINT('Ctrl Pts',(13.5424332480698,21.6491019044647,0.));
#210408=CARTESIAN_POINT('Ctrl Pts',(13.5424332480698,21.6491019044647,12.));
#210409=CARTESIAN_POINT('Ctrl Pts',(13.5404787697798,21.6219711193951,0.));
#210410=CARTESIAN_POINT('Ctrl Pts',(13.5404787697798,21.6219711193951,12.));
#210411=CARTESIAN_POINT('Ctrl Pts',(13.5384678597206,21.5949173499022,0.));
#210412=CARTESIAN_POINT('Ctrl Pts',(13.5384678597206,21.5949173499022,12.));
#210413=CARTESIAN_POINT('Ctrl Pts',(13.5364007790292,21.5679410019011,0.));
#210414=CARTESIAN_POINT('Ctrl Pts',(13.5364007790292,21.5679410019011,12.));
#210415=CARTESIAN_POINT('Ctrl Pts',(13.5342777983225,21.5410424932511,0.));
#210416=CARTESIAN_POINT('Ctrl Pts',(13.5342777983225,21.5410424932511,12.));
#210417=CARTESIAN_POINT('Ctrl Pts',(13.5320991952145,21.5142222501671,0.));
#210418=CARTESIAN_POINT('Ctrl Pts',(13.5320991952145,21.5142222501671,12.));
#210419=CARTESIAN_POINT('Ctrl Pts',(13.5298652514357,21.487480703047,0.));
#210420=CARTESIAN_POINT('Ctrl Pts',(13.5298652514357,21.487480703047,12.));
#210421=CARTESIAN_POINT('Ctrl Pts',(13.5275762503553,21.4608182828695,0.));
#210422=CARTESIAN_POINT('Ctrl Pts',(13.5275762503553,21.4608182828695,12.));
#210423=CARTESIAN_POINT('Ctrl Pts',(13.5252324737795,21.4342354165254,0.));
#210424=CARTESIAN_POINT('Ctrl Pts',(13.5252324737795,21.4342354165254,12.));
#210425=CARTESIAN_POINT('Ctrl Pts',(13.5228342013508,21.4077325259318,0.));
#210426=CARTESIAN_POINT('Ctrl Pts',(13.5228342013508,21.4077325259318,12.));
#210427=CARTESIAN_POINT('Ctrl Pts',(13.5203817122496,21.3813100304967,0.));
#210428=CARTESIAN_POINT('Ctrl Pts',(13.5203817122496,21.3813100304967,12.));
#210429=CARTESIAN_POINT('Ctrl Pts',(13.5178752862461,21.3549683486219,0.));
#210430=CARTESIAN_POINT('Ctrl Pts',(13.5178752862461,21.3549683486219,12.));
#210431=CARTESIAN_POINT('Ctrl Pts',(13.5153152050554,21.328707899634,0.));
#210432=CARTESIAN_POINT('Ctrl Pts',(13.5153152050554,21.328707899634,12.));
#210433=CARTESIAN_POINT('Ctrl Pts',(13.5127017534972,21.3025291054236,0.));
#210434=CARTESIAN_POINT('Ctrl Pts',(13.5127017534972,21.3025291054236,12.));
#210435=CARTESIAN_POINT('Ctrl Pts',(13.5100352209207,21.2764323924442,0.));
#210436=CARTESIAN_POINT('Ctrl Pts',(13.5100352209207,21.2764323924442,12.));
#210437=CARTESIAN_POINT('Ctrl Pts',(13.5073159019454,21.2504181927429,0.));
#210438=CARTESIAN_POINT('Ctrl Pts',(13.5073159019454,21.2504181927429,12.));
#210439=CARTESIAN_POINT('Ctrl Pts',(13.5045440957404,21.224486942933,0.));
#210440=CARTESIAN_POINT('Ctrl Pts',(13.5045440957404,21.224486942933,12.));
#210441=CARTESIAN_POINT('Ctrl Pts',(13.5017201056088,21.1986390835825,0.));
#210442=CARTESIAN_POINT('Ctrl Pts',(13.5017201056088,21.1986390835825,12.));
#210443=CARTESIAN_POINT('Ctrl Pts',(13.4988442384491,21.1728750584173,0.));
#210444=CARTESIAN_POINT('Ctrl Pts',(13.4988442384491,21.1728750584173,12.));
#210445=CARTESIAN_POINT('Ctrl Pts',(13.4959168042934,21.1471953136209,0.));
#210446=CARTESIAN_POINT('Ctrl Pts',(13.4959168042934,21.1471953136209,12.));
#210447=CARTESIAN_POINT('Ctrl Pts',(13.4929381157778,21.1216002970209,0.));
#210448=CARTESIAN_POINT('Ctrl Pts',(13.4929381157778,21.1216002970209,12.));
#210449=CARTESIAN_POINT('Ctrl Pts',(13.4899084877718,21.0960904575048,0.));
#210450=CARTESIAN_POINT('Ctrl Pts',(13.4899084877718,21.0960904575048,12.));
#210451=CARTESIAN_POINT('Ctrl Pts',(13.4868282377191,21.0706662455202,0.));
#210452=CARTESIAN_POINT('Ctrl Pts',(13.4868282377191,21.0706662455202,12.));
#210453=CARTESIAN_POINT('Ctrl Pts',(13.4836976858912,21.0453281134247,0.));
#210454=CARTESIAN_POINT('Ctrl Pts',(13.4836976858912,21.0453281134247,12.));
#210455=CARTESIAN_POINT('Ctrl Pts',(13.4805171556822,21.0200765158885,0.));
#210456=CARTESIAN_POINT('Ctrl Pts',(13.4805171556822,21.0200765158885,12.));
#210457=CARTESIAN_POINT('Ctrl Pts',(13.4772869738879,20.9949119102592,0.));
#210458=CARTESIAN_POINT('Ctrl Pts',(13.4772869738879,20.9949119102592,12.));
#210459=CARTESIAN_POINT('Ctrl Pts',(13.4740074710087,20.9698347569476,0.));
#210460=CARTESIAN_POINT('Ctrl Pts',(13.4740074710087,20.9698347569476,12.));
#210461=CARTESIAN_POINT('Ctrl Pts',(13.4706789815166,20.9448455197557,0.));
#210462=CARTESIAN_POINT('Ctrl Pts',(13.4706789815166,20.9448455197557,12.));
#210463=CARTESIAN_POINT('Ctrl Pts',(13.4673018437718,20.9199446657584,0.));
#210464=CARTESIAN_POINT('Ctrl Pts',(13.4673018437718,20.9199446657584,12.));
#210465=CARTESIAN_POINT('Ctrl Pts',(13.4638763999725,20.8951326652158,0.));
#210466=CARTESIAN_POINT('Ctrl Pts',(13.4638763999725,20.8951326652158,12.));
#210467=CARTESIAN_POINT('Ctrl Pts',(13.4604029960983,20.8704099914641,0.));
#210468=CARTESIAN_POINT('Ctrl Pts',(13.4604029960983,20.8704099914641,12.));
#210469=CARTESIAN_POINT('Ctrl Pts',(13.4568819818631,20.8457771208082,0.));
#210470=CARTESIAN_POINT('Ctrl Pts',(13.4568819818631,20.8457771208082,12.));
#210471=CARTESIAN_POINT('Ctrl Pts',(13.4533137106667,20.821234532398,0.));
#210472=CARTESIAN_POINT('Ctrl Pts',(13.4533137106667,20.821234532398,12.));
#210473=CARTESIAN_POINT('Ctrl Pts',(13.4496985395637,20.7967827081227,0.));
#210474=CARTESIAN_POINT('Ctrl Pts',(13.4496985395637,20.7967827081227,12.));
#210475=CARTESIAN_POINT('Ctrl Pts',(13.4460368293688,20.7724221327608,0.));
#210476=CARTESIAN_POINT('Ctrl Pts',(13.4460368293688,20.7724221327608,12.));
#210477=CARTESIAN_POINT('Ctrl Pts',(13.4423289447561,20.7481532941013,0.));
#210478=CARTESIAN_POINT('Ctrl Pts',(13.4423289447561,20.7481532941013,12.));
#210479=CARTESIAN_POINT('Ctrl Pts',(13.4385752543663,20.7239766830675,0.));
#210480=CARTESIAN_POINT('Ctrl Pts',(13.4385752543663,20.7239766830675,12.));
#210481=CARTESIAN_POINT('Ctrl Pts',(13.4347761309154,20.6998927938288,0.));
#210482=CARTESIAN_POINT('Ctrl Pts',(13.4347761309154,20.6998927938288,12.));
#210483=CARTESIAN_POINT('Ctrl Pts',(13.4309319513119,20.6759021239103,0.));
#210484=CARTESIAN_POINT('Ctrl Pts',(13.4309319513119,20.6759021239103,12.));
#210485=CARTESIAN_POINT('Ctrl Pts',(13.4270430967651,20.6520051742869,0.));
#210486=CARTESIAN_POINT('Ctrl Pts',(13.4270430967651,20.6520051742869,12.));
#210487=CARTESIAN_POINT('Ctrl Pts',(13.4231099528179,20.6282024494237,0.));
#210488=CARTESIAN_POINT('Ctrl Pts',(13.4231099528179,20.6282024494237,12.));
#210489=CARTESIAN_POINT('Ctrl Pts',(13.4191329093932,20.6044944573153,0.));
#210490=CARTESIAN_POINT('Ctrl Pts',(13.4191329093932,20.6044944573153,12.));
#210491=CARTESIAN_POINT('Ctrl Pts',(13.4151123608411,20.5808817095155,0.));
#210492=CARTESIAN_POINT('Ctrl Pts',(13.4151123608411,20.5808817095155,12.));
#210493=CARTESIAN_POINT('Ctrl Pts',(13.4110487059912,20.5573647211639,0.));
#210494=CARTESIAN_POINT('Ctrl Pts',(13.4110487059912,20.5573647211639,12.));
#210495=CARTESIAN_POINT('Ctrl Pts',(13.4069423482076,20.5339440109956,0.));
#210496=CARTESIAN_POINT('Ctrl Pts',(13.4069423482076,20.5339440109956,12.));
#210497=CARTESIAN_POINT('Ctrl Pts',(13.4027936954529,20.5106201013753,0.));
#210498=CARTESIAN_POINT('Ctrl Pts',(13.4027936954529,20.5106201013753,12.));
#210499=CARTESIAN_POINT('Ctrl Pts',(13.3986031603716,20.487393518404,0.));
#210500=CARTESIAN_POINT('Ctrl Pts',(13.3986031603716,20.487393518404,12.));
#210501=CARTESIAN_POINT('Ctrl Pts',(13.3943711603739,20.4642647920038,0.));
#210502=CARTESIAN_POINT('Ctrl Pts',(13.3943711603739,20.4642647920038,12.));
#210503=CARTESIAN_POINT('Ctrl Pts',(13.3900981177255,20.4412344560008,0.));
#210504=CARTESIAN_POINT('Ctrl Pts',(13.3900981177255,20.4412344560008,12.));
#210505=CARTESIAN_POINT('Ctrl Pts',(13.3857844596387,20.4183030482002,0.));
#210506=CARTESIAN_POINT('Ctrl Pts',(13.3857844596387,20.4183030482002,12.));
#210507=CARTESIAN_POINT('Ctrl Pts',(13.3814306183719,20.3954711104502,0.));
#210508=CARTESIAN_POINT('Ctrl Pts',(13.3814306183719,20.3954711104502,12.));
#210509=CARTESIAN_POINT('Ctrl Pts',(13.3770370313188,20.3727391887184,0.));
#210510=CARTESIAN_POINT('Ctrl Pts',(13.3770370313188,20.3727391887184,12.));
#210511=CARTESIAN_POINT('Ctrl Pts',(13.3726041410867,20.3501078331814,0.));
#210512=CARTESIAN_POINT('Ctrl Pts',(13.3726041410867,20.3501078331814,12.));
#210513=CARTESIAN_POINT('Ctrl Pts',(13.3681323955826,20.3275775983029,0.));
#210514=CARTESIAN_POINT('Ctrl Pts',(13.3681323955826,20.3275775983029,12.));
#210515=CARTESIAN_POINT('Ctrl Pts',(13.3636222481016,20.3051490429048,0.));
#210516=CARTESIAN_POINT('Ctrl Pts',(13.3636222481016,20.3051490429048,12.));
#210517=CARTESIAN_POINT('Ctrl Pts',(13.3590741574195,20.2828227302339,0.));
#210518=CARTESIAN_POINT('Ctrl Pts',(13.3590741574195,20.2828227302339,12.));
#210519=CARTESIAN_POINT('Ctrl Pts',(13.3544885878889,20.2605992280122,0.));
#210520=CARTESIAN_POINT('Ctrl Pts',(13.3544885878889,20.2605992280122,12.));
#210521=CARTESIAN_POINT('Ctrl Pts',(13.3498660095386,20.2384791085359,0.));
#210522=CARTESIAN_POINT('Ctrl Pts',(13.3498660095386,20.2384791085359,12.));
#210523=CARTESIAN_POINT('Ctrl Pts',(13.3452068981766,20.216462948786,0.));
#210524=CARTESIAN_POINT('Ctrl Pts',(13.3452068981766,20.216462948786,12.));
#210525=CARTESIAN_POINT('Ctrl Pts',(13.3405117354971,20.1945513305235,0.));
#210526=CARTESIAN_POINT('Ctrl Pts',(13.3405117354971,20.1945513305235,12.));
#210527=CARTESIAN_POINT('Ctrl Pts',(13.3357810091903,20.1727448403817,0.));
#210528=CARTESIAN_POINT('Ctrl Pts',(13.3357810091903,20.1727448403817,12.));
#210529=CARTESIAN_POINT('Ctrl Pts',(13.3310152130564,20.1510440699474,0.));
#210530=CARTESIAN_POINT('Ctrl Pts',(13.3310152130564,20.1510440699474,12.));
#210531=CARTESIAN_POINT('Ctrl Pts',(13.3262148471226,20.1294496158402,0.));
#210532=CARTESIAN_POINT('Ctrl Pts',(13.3262148471226,20.1294496158402,12.));
#210533=CARTESIAN_POINT('Ctrl Pts',(13.3213804177587,20.1079620798375,0.));
#210534=CARTESIAN_POINT('Ctrl Pts',(13.3213804177587,20.1079620798375,12.));
#210535=CARTESIAN_POINT('Ctrl Pts',(13.3165124377962,20.0865820689883,0.));
#210536=CARTESIAN_POINT('Ctrl Pts',(13.3165124377962,20.0865820689883,12.));
#210537=CARTESIAN_POINT('Ctrl Pts',(13.3116114266515,20.0653101957188,0.));
#210538=CARTESIAN_POINT('Ctrl Pts',(13.3116114266515,20.0653101957188,12.));
#210539=CARTESIAN_POINT('Ctrl Pts',(13.3066779104515,20.0441470779345,0.));
#210540=CARTESIAN_POINT('Ctrl Pts',(13.3066779104515,20.0441470779345,12.));
#210541=CARTESIAN_POINT('Ctrl Pts',(13.3017124221637,20.0230933391038,0.));
#210542=CARTESIAN_POINT('Ctrl Pts',(13.3017124221637,20.0230933391038,12.));
#210543=CARTESIAN_POINT('Ctrl Pts',(13.2967155017306,20.0021496083738,0.));
#210544=CARTESIAN_POINT('Ctrl Pts',(13.2967155017306,20.0021496083738,12.));
#210545=CARTESIAN_POINT('Ctrl Pts',(13.2916876962094,19.981316520717,0.));
#210546=CARTESIAN_POINT('Ctrl Pts',(13.2916876962094,19.981316520717,12.));
#210547=CARTESIAN_POINT('Ctrl Pts',(13.286629559915,19.9605947170586,0.));
#210548=CARTESIAN_POINT('Ctrl Pts',(13.286629559915,19.9605947170586,12.));
#210549=CARTESIAN_POINT('Ctrl Pts',(13.2815416545663,19.9399848444019,0.));
#210550=CARTESIAN_POINT('Ctrl Pts',(13.2815416545663,19.9399848444019,12.));
#210551=CARTESIAN_POINT('Ctrl Pts',(13.2764245494357,19.9194875559422,0.));
#210552=CARTESIAN_POINT('Ctrl Pts',(13.2764245494357,19.9194875559422,12.));
#210553=CARTESIAN_POINT('Ctrl Pts',(13.271278821502,19.8991035111745,0.));
#210554=CARTESIAN_POINT('Ctrl Pts',(13.271278821502,19.8991035111745,12.));
#210555=CARTESIAN_POINT('Ctrl Pts',(13.2661050556132,19.8788333760577,0.));
#210556=CARTESIAN_POINT('Ctrl Pts',(13.2661050556132,19.8788333760577,12.));
#210557=CARTESIAN_POINT('Ctrl Pts',(13.2609038446529,19.8586778231715,0.));
#210558=CARTESIAN_POINT('Ctrl Pts',(13.2609038446529,19.8586778231715,12.));
#210559=CARTESIAN_POINT('Ctrl Pts',(13.2556757897086,19.8386375318634,0.));
#210560=CARTESIAN_POINT('Ctrl Pts',(13.2556757897086,19.8386375318634,12.));
#210561=CARTESIAN_POINT('Ctrl Pts',(13.2504215002457,19.8187131883917,0.));
#210562=CARTESIAN_POINT('Ctrl Pts',(13.2504215002457,19.8187131883917,12.));
#210563=CARTESIAN_POINT('Ctrl Pts',(13.2451415942805,19.7989054860495,0.));
#210564=CARTESIAN_POINT('Ctrl Pts',(13.2451415942805,19.7989054860495,12.));
#210565=CARTESIAN_POINT('Ctrl Pts',(13.2398366985675,19.7792151253289,0.));
#210566=CARTESIAN_POINT('Ctrl Pts',(13.2398366985675,19.7792151253289,12.));
#210567=CARTESIAN_POINT('Ctrl Pts',(13.2345074487963,19.7596428141168,0.));
#210568=CARTESIAN_POINT('Ctrl Pts',(13.2345074487963,19.7596428141168,12.));
#210569=CARTESIAN_POINT('Ctrl Pts',(13.2291544897899,19.7401892678697,0.));
#210570=CARTESIAN_POINT('Ctrl Pts',(13.2291544897899,19.7401892678697,12.));
#210571=CARTESIAN_POINT('Ctrl Pts',(13.2237784757065,19.7208552097868,0.));
#210572=CARTESIAN_POINT('Ctrl Pts',(13.2237784757065,19.7208552097868,12.));
#210573=CARTESIAN_POINT('Ctrl Pts',(13.2183800702436,19.7016413709685,0.));
#210574=CARTESIAN_POINT('Ctrl Pts',(13.2183800702436,19.7016413709685,12.));
#210575=CARTESIAN_POINT('Ctrl Pts',(13.2129599468485,19.6825484905823,0.));
#210576=CARTESIAN_POINT('Ctrl Pts',(13.2129599468485,19.6825484905823,12.));
#210577=CARTESIAN_POINT('Ctrl Pts',(13.2075187889529,19.6635773160936,0.));
#210578=CARTESIAN_POINT('Ctrl Pts',(13.2075187889529,19.6635773160936,12.));
#210579=CARTESIAN_POINT('Ctrl Pts',(13.2020572902065,19.6447286034772,0.));
#210580=CARTESIAN_POINT('Ctrl Pts',(13.2020572902065,19.6447286034772,12.));
#210581=CARTESIAN_POINT('Ctrl Pts',(13.1965761547151,19.6260031174244,0.));
#210582=CARTESIAN_POINT('Ctrl Pts',(13.1965761547151,19.6260031174244,12.));
#210583=CARTESIAN_POINT('Ctrl Pts',(13.1910760972814,19.6074016315414,0.));
#210584=CARTESIAN_POINT('Ctrl Pts',(13.1910760972814,19.6074016315414,12.));
#210585=CARTESIAN_POINT('Ctrl Pts',(13.1855578436471,19.5889249285338,0.));
#210586=CARTESIAN_POINT('Ctrl Pts',(13.1855578436471,19.5889249285338,12.));
#210587=CARTESIAN_POINT('Ctrl Pts',(13.1800221307673,19.5705738004667,0.));
#210588=CARTESIAN_POINT('Ctrl Pts',(13.1800221307673,19.5705738004667,12.));
#210589=CARTESIAN_POINT('Ctrl Pts',(13.1744697070911,19.5523490490244,0.));
#210590=CARTESIAN_POINT('Ctrl Pts',(13.1744697070911,19.5523490490244,12.));
#210591=CARTESIAN_POINT('Ctrl Pts',(13.168901332843,19.5342514857562,0.));
#210592=CARTESIAN_POINT('Ctrl Pts',(13.168901332843,19.5342514857562,12.));
#210593=CARTESIAN_POINT('Ctrl Pts',(13.1633177803101,19.5162819323213,0.));
#210594=CARTESIAN_POINT('Ctrl Pts',(13.1633177803101,19.5162819323213,12.));
#210595=CARTESIAN_POINT('Ctrl Pts',(13.1577198341245,19.4984412207082,0.));
#210596=CARTESIAN_POINT('Ctrl Pts',(13.1577198341245,19.4984412207082,12.));
#210597=CARTESIAN_POINT('Ctrl Pts',(13.1521082915853,19.4807301935268,0.));
#210598=CARTESIAN_POINT('Ctrl Pts',(13.1521082915853,19.4807301935268,12.));
#210599=CARTESIAN_POINT('Ctrl Pts',(13.1464839629971,19.4631497043258,0.));
#210600=CARTESIAN_POINT('Ctrl Pts',(13.1464839629971,19.4631497043258,12.));
#210601=CARTESIAN_POINT('Ctrl Pts',(13.1408476720061,19.4457006178876,0.));
#210602=CARTESIAN_POINT('Ctrl Pts',(13.1408476720061,19.4457006178876,12.));
#210603=CARTESIAN_POINT('Ctrl Pts',(13.1352002559438,19.4283838105262,0.));
#210604=CARTESIAN_POINT('Ctrl Pts',(13.1352002559438,19.4283838105262,12.));
#210605=CARTESIAN_POINT('Ctrl Pts',(13.1295425661634,19.4112001703557,0.));
#210606=CARTESIAN_POINT('Ctrl Pts',(13.1295425661634,19.4112001703557,12.));
#210607=CARTESIAN_POINT('Ctrl Pts',(13.1238754684177,19.3941505976263,0.));
#210608=CARTESIAN_POINT('Ctrl Pts',(13.1238754684177,19.3941505976263,12.));
#210609=CARTESIAN_POINT('Ctrl Pts',(13.118199843271,19.3772360051091,0.));
#210610=CARTESIAN_POINT('Ctrl Pts',(13.118199843271,19.3772360051091,12.));
#210611=CARTESIAN_POINT('Ctrl Pts',(13.1125165865022,19.3604573184515,0.));
#210612=CARTESIAN_POINT('Ctrl Pts',(13.1125165865022,19.3604573184515,12.));
#210613=CARTESIAN_POINT('Ctrl Pts',(13.1068266095186,19.3438154765395,0.));
#210614=CARTESIAN_POINT('Ctrl Pts',(13.1068266095186,19.3438154765395,12.));
#210615=CARTESIAN_POINT('Ctrl Pts',(13.1011308397591,19.3273114318269,0.));
#210616=CARTESIAN_POINT('Ctrl Pts',(13.1011308397591,19.3273114318269,12.));
#210617=CARTESIAN_POINT('Ctrl Pts',(13.0954302211479,19.310946150736,0.));
#210618=CARTESIAN_POINT('Ctrl Pts',(13.0954302211479,19.310946150736,12.));
#210619=CARTESIAN_POINT('Ctrl Pts',(13.0897257145968,19.2947206141247,0.));
#210620=CARTESIAN_POINT('Ctrl Pts',(13.0897257145968,19.2947206141247,12.));
#210621=CARTESIAN_POINT('Ctrl Pts',(13.0840182984949,19.2786358177198,0.));
#210622=CARTESIAN_POINT('Ctrl Pts',(13.0840182984949,19.2786358177198,12.));
#210623=CARTESIAN_POINT('Ctrl Pts',(13.0783089692118,19.2626927725596,0.));
#210624=CARTESIAN_POINT('Ctrl Pts',(13.0783089692118,19.2626927725596,12.));
#210625=CARTESIAN_POINT('Ctrl Pts',(13.0725987415859,19.2468925053989,0.));
#210626=CARTESIAN_POINT('Ctrl Pts',(13.0725987415859,19.2468925053989,12.));
#210627=CARTESIAN_POINT('Ctrl Pts',(13.0668886494795,19.2312360592033,0.));
#210628=CARTESIAN_POINT('Ctrl Pts',(13.0668886494795,19.2312360592033,12.));
#210629=CARTESIAN_POINT('Ctrl Pts',(13.0611797463915,19.2157244937142,0.));
#210630=CARTESIAN_POINT('Ctrl Pts',(13.0611797463915,19.2157244937142,12.));
#210631=CARTESIAN_POINT('Ctrl Pts',(13.0554731060538,19.2003588859772,0.));
#210632=CARTESIAN_POINT('Ctrl Pts',(13.0554731060538,19.2003588859772,12.));
#210633=CARTESIAN_POINT('Ctrl Pts',(13.0497698230441,19.1851403308825,0.));
#210634=CARTESIAN_POINT('Ctrl Pts',(13.0497698230441,19.1851403308825,12.));
#210635=CARTESIAN_POINT('Ctrl Pts',(13.0440710133772,19.1700699416622,0.));
#210636=CARTESIAN_POINT('Ctrl Pts',(13.0440710133772,19.1700699416622,12.));
#210637=CARTESIAN_POINT('Ctrl Pts',(13.0383778152068,19.155148850523,0.));
#210638=CARTESIAN_POINT('Ctrl Pts',(13.0383778152068,19.155148850523,12.));
#210639=CARTESIAN_POINT('Ctrl Pts',(13.0326913895838,19.1403782093386,0.));
#210640=CARTESIAN_POINT('Ctrl Pts',(13.0326913895838,19.1403782093386,12.));
#210641=CARTESIAN_POINT('Ctrl Pts',(13.0270129211976,19.1257591903099,0.));
#210642=CARTESIAN_POINT('Ctrl Pts',(13.0270129211976,19.1257591903099,12.));
#210643=CARTESIAN_POINT('Ctrl Pts',(13.0213436191328,19.111292986631,0.));
#210644=CARTESIAN_POINT('Ctrl Pts',(13.0213436191328,19.111292986631,12.));
#210645=CARTESIAN_POINT('Ctrl Pts',(13.0156847176096,19.0969808131228,0.));
#210646=CARTESIAN_POINT('Ctrl Pts',(13.0156847176096,19.0969808131228,12.));
#210647=CARTESIAN_POINT('Ctrl Pts',(13.0100374768788,19.0828239070484,0.));
#210648=CARTESIAN_POINT('Ctrl Pts',(13.0100374768788,19.0828239070484,12.));
#210649=CARTESIAN_POINT('Ctrl Pts',(13.0044031841382,19.0688235289437,0.));
#210650=CARTESIAN_POINT('Ctrl Pts',(13.0044031841382,19.0688235289437,12.));
#210651=CARTESIAN_POINT('Ctrl Pts',(12.9987831544502,19.0549809634354,0.));
#210652=CARTESIAN_POINT('Ctrl Pts',(12.9987831544502,19.0549809634354,12.));
#210653=CARTESIAN_POINT('Ctrl Pts',(12.9931787316514,19.0412975200398,0.));
#210654=CARTESIAN_POINT('Ctrl Pts',(12.9931787316514,19.0412975200398,12.));
#210655=CARTESIAN_POINT('Ctrl Pts',(12.9875912893003,19.0277745339909,0.));
#210656=CARTESIAN_POINT('Ctrl Pts',(12.9875912893003,19.0277745339909,12.));
#210657=CARTESIAN_POINT('Ctrl Pts',(12.9820222318716,19.014413367335,0.));
#210658=CARTESIAN_POINT('Ctrl Pts',(12.9820222318716,19.014413367335,12.));
#210659=CARTESIAN_POINT('Ctrl Pts',(12.9764729959206,19.0012154099792,0.));
#210660=CARTESIAN_POINT('Ctrl Pts',(12.9764729959206,19.0012154099792,12.));
#210661=CARTESIAN_POINT('Ctrl Pts',(12.9709450512747,18.9881820807585,0.));
#210662=CARTESIAN_POINT('Ctrl Pts',(12.9709450512747,18.9881820807585,12.));
#210663=CARTESIAN_POINT('Ctrl Pts',(12.9654399021868,18.9753148284473,0.));
#210664=CARTESIAN_POINT('Ctrl Pts',(12.9654399021868,18.9753148284473,12.));
#210665=CARTESIAN_POINT('Ctrl Pts',(12.9599590886317,18.9626151329226,0.));
#210666=CARTESIAN_POINT('Ctrl Pts',(12.9599590886317,18.9626151329226,12.));
#210667=CARTESIAN_POINT('Ctrl Pts',(12.9545041877377,18.9500845064714,0.));
#210668=CARTESIAN_POINT('Ctrl Pts',(12.9545041877377,18.9500845064714,12.));
#210669=CARTESIAN_POINT('Ctrl Pts',(12.9490768151821,18.9377244950435,0.));
#210670=CARTESIAN_POINT('Ctrl Pts',(12.9490768151821,18.9377244950435,12.));
#210671=CARTESIAN_POINT('Ctrl Pts',(12.9436786266106,18.9255366795196,0.));
#210672=CARTESIAN_POINT('Ctrl Pts',(12.9436786266106,18.9255366795196,12.));
#210673=CARTESIAN_POINT('Ctrl Pts',(12.9383113190375,18.9135226769466,0.));
#210674=CARTESIAN_POINT('Ctrl Pts',(12.9383113190375,18.9135226769466,12.));
#210675=CARTESIAN_POINT('Ctrl Pts',(12.9329766328184,18.9016841423402,0.));
#210676=CARTESIAN_POINT('Ctrl Pts',(12.9329766328184,18.9016841423402,12.));
#210677=CARTESIAN_POINT('Ctrl Pts',(12.9276763536372,18.8900227704888,0.));
#210678=CARTESIAN_POINT('Ctrl Pts',(12.9276763536372,18.8900227704888,12.));
#210679=CARTESIAN_POINT('Ctrl Pts',(12.9224123144982,18.8785402977528,0.));
#210680=CARTESIAN_POINT('Ctrl Pts',(12.9224123144982,18.8785402977528,12.));
#210681=CARTESIAN_POINT('Ctrl Pts',(12.9171863977047,18.8672385038328,0.));
#210682=CARTESIAN_POINT('Ctrl Pts',(12.9171863977047,18.8672385038328,12.));
#210683=CARTESIAN_POINT('Ctrl Pts',(12.9120005369066,18.8561192136201,0.));
#210684=CARTESIAN_POINT('Ctrl Pts',(12.9120005369066,18.8561192136201,12.));
#210685=CARTESIAN_POINT('Ctrl Pts',(12.9068567191856,18.8451842990986,0.));
#210686=CARTESIAN_POINT('Ctrl Pts',(12.9068567191856,18.8451842990986,12.));
#210687=CARTESIAN_POINT('Ctrl Pts',(12.9017569871738,18.834435681259,0.));
#210688=CARTESIAN_POINT('Ctrl Pts',(12.9017569871738,18.834435681259,12.));
#210689=CARTESIAN_POINT('Ctrl Pts',(12.8967034410752,18.8238753319124,0.));
#210690=CARTESIAN_POINT('Ctrl Pts',(12.8967034410752,18.8238753319124,12.));
#210691=CARTESIAN_POINT('Ctrl Pts',(12.8916982409931,18.8135052757815,0.));
#210692=CARTESIAN_POINT('Ctrl Pts',(12.8916982409931,18.8135052757815,12.));
#210693=CARTESIAN_POINT('Ctrl Pts',(12.8867436109543,18.8033275941939,0.));
#210694=CARTESIAN_POINT('Ctrl Pts',(12.8867436109543,18.8033275941939,12.));
#210695=CARTESIAN_POINT('Ctrl Pts',(12.8818418427474,18.7933444285867,0.));
#210696=CARTESIAN_POINT('Ctrl Pts',(12.8818418427474,18.7933444285867,12.));
#210697=CARTESIAN_POINT('Ctrl Pts',(12.8769952998097,18.7835579840481,0.));
#210698=CARTESIAN_POINT('Ctrl Pts',(12.8769952998097,18.7835579840481,12.));
#210699=CARTESIAN_POINT('Ctrl Pts',(12.8722064211814,18.7739705329029,0.));
#210700=CARTESIAN_POINT('Ctrl Pts',(12.8722064211814,18.7739705329029,12.));
#210701=CARTESIAN_POINT('Ctrl Pts',(12.8674777239656,18.7645844169568,0.));
#210702=CARTESIAN_POINT('Ctrl Pts',(12.8674777239656,18.7645844169568,12.));
#210703=CARTESIAN_POINT('Ctrl Pts',(12.8628118054172,18.7554020493888,0.));
#210704=CARTESIAN_POINT('Ctrl Pts',(12.8628118054172,18.7554020493888,12.));
#210705=CARTESIAN_POINT('Ctrl Pts',(12.8582113455644,18.7464259171248,0.));
#210706=CARTESIAN_POINT('Ctrl Pts',(12.8582113455644,18.7464259171248,12.));
#210707=CARTESIAN_POINT('Ctrl Pts',(12.8536791086315,18.7376585820851,0.));
#210708=CARTESIAN_POINT('Ctrl Pts',(12.8536791086315,18.7376585820851,12.));
#210709=CARTESIAN_POINT('Ctrl Pts',(12.849217951159,18.7291026886552,0.));
#210710=CARTESIAN_POINT('Ctrl Pts',(12.849217951159,18.7291026886552,12.));
#210711=CARTESIAN_POINT('Ctrl Pts',(12.8448308329494,18.7207609737701,0.));
#210712=CARTESIAN_POINT('Ctrl Pts',(12.8448308329494,18.7207609737701,12.));
#210713=CARTESIAN_POINT('Ctrl Pts',(12.8405208263432,18.7126362754446,0.));
#210714=CARTESIAN_POINT('Ctrl Pts',(12.8405208263432,18.7126362754446,12.));
#210715=CARTESIAN_POINT('Ctrl Pts',(12.8362911280362,18.7047315436296,0.));
#210716=CARTESIAN_POINT('Ctrl Pts',(12.8362911280362,18.7047315436296,12.));
#210717=CARTESIAN_POINT('Ctrl Pts',(12.832145059979,18.6970498410173,0.));
#210718=CARTESIAN_POINT('Ctrl Pts',(12.832145059979,18.6970498410173,12.));
#210719=CARTESIAN_POINT('Ctrl Pts',(12.8280860635231,18.6895943376172,0.));
#210720=CARTESIAN_POINT('Ctrl Pts',(12.8280860635231,18.6895943376172,12.));
#210721=CARTESIAN_POINT('Ctrl Pts',(12.8241176980016,18.6823683094139,0.));
#210722=CARTESIAN_POINT('Ctrl Pts',(12.8241176980016,18.6823683094139,12.));
#210723=CARTESIAN_POINT('Ctrl Pts',(12.8202436318473,18.6753751301091,0.));
#210724=CARTESIAN_POINT('Ctrl Pts',(12.8202436318473,18.6753751301091,12.));
#210725=CARTESIAN_POINT('Ctrl Pts',(12.8164676687361,18.6686182952798,0.));
#210726=CARTESIAN_POINT('Ctrl Pts',(12.8164676687361,18.6686182952798,12.));
#210727=CARTESIAN_POINT('Ctrl Pts',(12.8127937909632,18.6621014624746,0.));
#210728=CARTESIAN_POINT('Ctrl Pts',(12.8127937909632,18.6621014624746,12.));
#210729=CARTESIAN_POINT('Ctrl Pts',(12.8092261933858,18.6558284825772,0.));
#210730=CARTESIAN_POINT('Ctrl Pts',(12.8092261933858,18.6558284825772,12.));
#210731=CARTESIAN_POINT('Ctrl Pts',(12.805769331162,18.6498034438986,0.));
#210732=CARTESIAN_POINT('Ctrl Pts',(12.805769331162,18.6498034438986,12.));
#210733=CARTESIAN_POINT('Ctrl Pts',(12.8024278770153,18.6440306327457,0.));
#210734=CARTESIAN_POINT('Ctrl Pts',(12.8024278770153,18.6440306327457,12.));
#210735=CARTESIAN_POINT('Ctrl Pts',(12.7992066625264,18.63851447924,0.));
#210736=CARTESIAN_POINT('Ctrl Pts',(12.7992066625264,18.63851447924,12.));
#210737=CARTESIAN_POINT('Ctrl Pts',(12.7961106222251,18.6332595057005,0.));
#210738=CARTESIAN_POINT('Ctrl Pts',(12.7961106222251,18.6332595057005,12.));
#210739=CARTESIAN_POINT('Ctrl Pts',(12.7931447451556,18.6282702819371,0.));
#210740=CARTESIAN_POINT('Ctrl Pts',(12.7931447451556,18.6282702819371,12.));
#210741=CARTESIAN_POINT('Ctrl Pts',(12.7903142925234,18.6235516265575,0.));
#210742=CARTESIAN_POINT('Ctrl Pts',(12.7903142925234,18.6235516265575,12.));
#210743=CARTESIAN_POINT('Ctrl Pts',(12.7876249657834,18.6191087624752,0.));
#210744=CARTESIAN_POINT('Ctrl Pts',(12.7876249657834,18.6191087624752,12.));
#210745=CARTESIAN_POINT('Ctrl Pts',(12.78508316579,18.6149475565189,0.));
#210746=CARTESIAN_POINT('Ctrl Pts',(12.78508316579,18.6149475565189,12.));
#210747=CARTESIAN_POINT('Ctrl Pts',(12.7826959526924,18.611074482622,0.));
#210748=CARTESIAN_POINT('Ctrl Pts',(12.7826959526924,18.611074482622,12.));
#210749=CARTESIAN_POINT('Ctrl Pts',(12.7804705387658,18.6074961535723,0.));
#210750=CARTESIAN_POINT('Ctrl Pts',(12.7804705387658,18.6074961535723,12.));
#210751=CARTESIAN_POINT('Ctrl Pts',(12.7784139605067,18.6042190183703,0.));
#210752=CARTESIAN_POINT('Ctrl Pts',(12.7784139605067,18.6042190183703,12.));
#210753=CARTESIAN_POINT('Ctrl Pts',(12.7765325225082,18.6012488486708,0.));
#210754=CARTESIAN_POINT('Ctrl Pts',(12.7765325225082,18.6012488486708,12.));
#210755=CARTESIAN_POINT('Ctrl Pts',(12.7748328937639,18.5985917525949,0.));
#210756=CARTESIAN_POINT('Ctrl Pts',(12.7748328937639,18.5985917525949,12.));
#210757=CARTESIAN_POINT('Ctrl Pts',(12.7733231262107,18.5962551167772,0.));
#210758=CARTESIAN_POINT('Ctrl Pts',(12.7733231262107,18.5962551167772,12.));
#210759=CARTESIAN_POINT('Ctrl Pts',(12.7720142287169,18.5942490615409,0.));
#210760=CARTESIAN_POINT('Ctrl Pts',(12.7720142287169,18.5942490615409,12.));
#210761=CARTESIAN_POINT('Ctrl Pts',(12.7709195951153,18.5925859134582,0.));
#210762=CARTESIAN_POINT('Ctrl Pts',(12.7709195951153,18.5925859134582,12.));
#210763=CARTESIAN_POINT('Ctrl Pts',(12.7700520897174,18.5912775137806,0.));
#210764=CARTESIAN_POINT('Ctrl Pts',(12.7700520897174,18.5912775137806,12.));
#210765=CARTESIAN_POINT('Ctrl Pts',(12.7694215127923,18.590332877722,0.));
#210766=CARTESIAN_POINT('Ctrl Pts',(12.7694215127923,18.590332877722,12.));
#210767=CARTESIAN_POINT('Ctrl Pts',(12.7691103481996,18.589871621842,0.));
#210768=CARTESIAN_POINT('Ctrl Pts',(12.7691103481996,18.589871621842,12.));
#210769=CARTESIAN_POINT('Ctrl Pts',(12.7689864266924,18.5896919669158,0.));
#210770=CARTESIAN_POINT('Ctrl Pts',(12.7689864266924,18.5896919669158,12.));
#210771=CARTESIAN_POINT('Ctrl Pts',(12.7689524524484,18.5896460962961,0.));
#210772=CARTESIAN_POINT('Ctrl Pts',(12.7689524524484,18.5896460962961,12.));
#210773=CARTESIAN_POINT('Ctrl Pts',(12.7689476255363,18.5896416359912,0.));
#210774=CARTESIAN_POINT('Ctrl Pts',(12.7689476255363,18.5896416359912,12.));
#210775=CARTESIAN_POINT('',(13.5685075571671,22.1787195904339,0.));
#210776=CARTESIAN_POINT('Ctrl Pts',(13.5685075571671,22.1787195904339,0.));
#210777=CARTESIAN_POINT('Ctrl Pts',(13.5683460612913,22.1730081264583,0.));
#210778=CARTESIAN_POINT('Ctrl Pts',(13.5680170531724,22.1615922804939,0.));
#210779=CARTESIAN_POINT('Ctrl Pts',(13.5675054918922,22.1444897575076,0.));
#210780=CARTESIAN_POINT('Ctrl Pts',(13.5667873105179,22.1217288871823,0.));
#210781=CARTESIAN_POINT('Ctrl Pts',(13.5658294169106,22.0933486464442,0.));
#210782=CARTESIAN_POINT('Ctrl Pts',(13.5648113688894,22.0650393089492,0.));
#210783=CARTESIAN_POINT('Ctrl Pts',(13.5637332022393,22.0368009736227,0.));
#210784=CARTESIAN_POINT('Ctrl Pts',(13.5625949868313,22.0086337943431,0.));
#210785=CARTESIAN_POINT('Ctrl Pts',(13.5613968357589,21.9805379899192,0.));
#210786=CARTESIAN_POINT('Ctrl Pts',(13.5601389185315,21.9525138592862,0.));
#210787=CARTESIAN_POINT('Ctrl Pts',(13.5588214586672,21.9245617765827,0.));
#210788=CARTESIAN_POINT('Ctrl Pts',(13.5574447178484,21.8966821688876,0.));
#210789=CARTESIAN_POINT('Ctrl Pts',(13.5560089839426,21.8688754989401,0.));
#210790=CARTESIAN_POINT('Ctrl Pts',(13.5545145573048,21.841142245609,0.));
#210791=CARTESIAN_POINT('Ctrl Pts',(13.5529617381569,21.8134828857963,0.));
#210792=CARTESIAN_POINT('Ctrl Pts',(13.5513508127232,21.7858978745848,0.));
#210793=CARTESIAN_POINT('Ctrl Pts',(13.5496820422186,21.7583876294532,0.));
#210794=CARTESIAN_POINT('Ctrl Pts',(13.5479556704457,21.730952541226,0.));
#210795=CARTESIAN_POINT('Ctrl Pts',(13.546171929503,21.7035929822939,0.));
#210796=CARTESIAN_POINT('Ctrl Pts',(13.5443310461516,21.676309315769,0.));
#210797=CARTESIAN_POINT('Ctrl Pts',(13.5424332480698,21.6491019044647,0.));
#210798=CARTESIAN_POINT('Ctrl Pts',(13.5404787697798,21.6219711193951,0.));
#210799=CARTESIAN_POINT('Ctrl Pts',(13.5384678597206,21.5949173499022,0.));
#210800=CARTESIAN_POINT('Ctrl Pts',(13.5364007790292,21.5679410019011,0.));
#210801=CARTESIAN_POINT('Ctrl Pts',(13.5342777983225,21.5410424932511,0.));
#210802=CARTESIAN_POINT('Ctrl Pts',(13.5320991952145,21.5142222501671,0.));
#210803=CARTESIAN_POINT('Ctrl Pts',(13.5298652514357,21.487480703047,0.));
#210804=CARTESIAN_POINT('Ctrl Pts',(13.5275762503553,21.4608182828695,0.));
#210805=CARTESIAN_POINT('Ctrl Pts',(13.5252324737795,21.4342354165254,0.));
#210806=CARTESIAN_POINT('Ctrl Pts',(13.5228342013508,21.4077325259318,0.));
#210807=CARTESIAN_POINT('Ctrl Pts',(13.5203817122496,21.3813100304967,0.));
#210808=CARTESIAN_POINT('Ctrl Pts',(13.5178752862461,21.3549683486219,0.));
#210809=CARTESIAN_POINT('Ctrl Pts',(13.5153152050554,21.328707899634,0.));
#210810=CARTESIAN_POINT('Ctrl Pts',(13.5127017534972,21.3025291054236,0.));
#210811=CARTESIAN_POINT('Ctrl Pts',(13.5100352209207,21.2764323924442,0.));
#210812=CARTESIAN_POINT('Ctrl Pts',(13.5073159019454,21.2504181927429,0.));
#210813=CARTESIAN_POINT('Ctrl Pts',(13.5045440957404,21.224486942933,0.));
#210814=CARTESIAN_POINT('Ctrl Pts',(13.5017201056088,21.1986390835825,0.));
#210815=CARTESIAN_POINT('Ctrl Pts',(13.4988442384491,21.1728750584173,0.));
#210816=CARTESIAN_POINT('Ctrl Pts',(13.4959168042934,21.1471953136209,0.));
#210817=CARTESIAN_POINT('Ctrl Pts',(13.4929381157778,21.1216002970209,0.));
#210818=CARTESIAN_POINT('Ctrl Pts',(13.4899084877718,21.0960904575048,0.));
#210819=CARTESIAN_POINT('Ctrl Pts',(13.4868282377191,21.0706662455202,0.));
#210820=CARTESIAN_POINT('Ctrl Pts',(13.4836976858912,21.0453281134247,0.));
#210821=CARTESIAN_POINT('Ctrl Pts',(13.4805171556822,21.0200765158885,0.));
#210822=CARTESIAN_POINT('Ctrl Pts',(13.4772869738879,20.9949119102592,0.));
#210823=CARTESIAN_POINT('Ctrl Pts',(13.4740074710087,20.9698347569476,0.));
#210824=CARTESIAN_POINT('Ctrl Pts',(13.4706789815166,20.9448455197557,0.));
#210825=CARTESIAN_POINT('Ctrl Pts',(13.4673018437718,20.9199446657584,0.));
#210826=CARTESIAN_POINT('Ctrl Pts',(13.4638763999725,20.8951326652158,0.));
#210827=CARTESIAN_POINT('Ctrl Pts',(13.4604029960983,20.8704099914641,0.));
#210828=CARTESIAN_POINT('Ctrl Pts',(13.4568819818631,20.8457771208082,0.));
#210829=CARTESIAN_POINT('Ctrl Pts',(13.4533137106667,20.821234532398,0.));
#210830=CARTESIAN_POINT('Ctrl Pts',(13.4496985395637,20.7967827081227,0.));
#210831=CARTESIAN_POINT('Ctrl Pts',(13.4460368293688,20.7724221327608,0.));
#210832=CARTESIAN_POINT('Ctrl Pts',(13.4423289447561,20.7481532941013,0.));
#210833=CARTESIAN_POINT('Ctrl Pts',(13.4385752543663,20.7239766830675,0.));
#210834=CARTESIAN_POINT('Ctrl Pts',(13.4347761309154,20.6998927938288,0.));
#210835=CARTESIAN_POINT('Ctrl Pts',(13.4309319513119,20.6759021239103,0.));
#210836=CARTESIAN_POINT('Ctrl Pts',(13.4270430967651,20.6520051742869,0.));
#210837=CARTESIAN_POINT('Ctrl Pts',(13.4231099528179,20.6282024494237,0.));
#210838=CARTESIAN_POINT('Ctrl Pts',(13.4191329093932,20.6044944573153,0.));
#210839=CARTESIAN_POINT('Ctrl Pts',(13.4151123608411,20.5808817095155,0.));
#210840=CARTESIAN_POINT('Ctrl Pts',(13.4110487059912,20.5573647211639,0.));
#210841=CARTESIAN_POINT('Ctrl Pts',(13.4069423482076,20.5339440109956,0.));
#210842=CARTESIAN_POINT('Ctrl Pts',(13.4027936954529,20.5106201013753,0.));
#210843=CARTESIAN_POINT('Ctrl Pts',(13.3986031603716,20.487393518404,0.));
#210844=CARTESIAN_POINT('Ctrl Pts',(13.3943711603739,20.4642647920038,0.));
#210845=CARTESIAN_POINT('Ctrl Pts',(13.3900981177255,20.4412344560008,0.));
#210846=CARTESIAN_POINT('Ctrl Pts',(13.3857844596387,20.4183030482002,0.));
#210847=CARTESIAN_POINT('Ctrl Pts',(13.3814306183719,20.3954711104502,0.));
#210848=CARTESIAN_POINT('Ctrl Pts',(13.3770370313188,20.3727391887184,0.));
#210849=CARTESIAN_POINT('Ctrl Pts',(13.3726041410867,20.3501078331814,0.));
#210850=CARTESIAN_POINT('Ctrl Pts',(13.3681323955826,20.3275775983029,0.));
#210851=CARTESIAN_POINT('Ctrl Pts',(13.3636222481016,20.3051490429048,0.));
#210852=CARTESIAN_POINT('Ctrl Pts',(13.3590741574195,20.2828227302339,0.));
#210853=CARTESIAN_POINT('Ctrl Pts',(13.3544885878889,20.2605992280122,0.));
#210854=CARTESIAN_POINT('Ctrl Pts',(13.3498660095386,20.2384791085359,0.));
#210855=CARTESIAN_POINT('Ctrl Pts',(13.3452068981766,20.216462948786,0.));
#210856=CARTESIAN_POINT('Ctrl Pts',(13.3405117354971,20.1945513305235,0.));
#210857=CARTESIAN_POINT('Ctrl Pts',(13.3357810091903,20.1727448403817,0.));
#210858=CARTESIAN_POINT('Ctrl Pts',(13.3310152130564,20.1510440699474,0.));
#210859=CARTESIAN_POINT('Ctrl Pts',(13.3262148471226,20.1294496158402,0.));
#210860=CARTESIAN_POINT('Ctrl Pts',(13.3213804177587,20.1079620798375,0.));
#210861=CARTESIAN_POINT('Ctrl Pts',(13.3165124377962,20.0865820689883,0.));
#210862=CARTESIAN_POINT('Ctrl Pts',(13.3116114266515,20.0653101957188,0.));
#210863=CARTESIAN_POINT('Ctrl Pts',(13.3066779104515,20.0441470779345,0.));
#210864=CARTESIAN_POINT('Ctrl Pts',(13.3017124221637,20.0230933391038,0.));
#210865=CARTESIAN_POINT('Ctrl Pts',(13.2967155017306,20.0021496083738,0.));
#210866=CARTESIAN_POINT('Ctrl Pts',(13.2916876962094,19.981316520717,0.));
#210867=CARTESIAN_POINT('Ctrl Pts',(13.286629559915,19.9605947170586,0.));
#210868=CARTESIAN_POINT('Ctrl Pts',(13.2815416545663,19.9399848444019,0.));
#210869=CARTESIAN_POINT('Ctrl Pts',(13.2764245494357,19.9194875559422,0.));
#210870=CARTESIAN_POINT('Ctrl Pts',(13.271278821502,19.8991035111745,0.));
#210871=CARTESIAN_POINT('Ctrl Pts',(13.2661050556132,19.8788333760577,0.));
#210872=CARTESIAN_POINT('Ctrl Pts',(13.2609038446529,19.8586778231715,0.));
#210873=CARTESIAN_POINT('Ctrl Pts',(13.2556757897086,19.8386375318634,0.));
#210874=CARTESIAN_POINT('Ctrl Pts',(13.2504215002457,19.8187131883917,0.));
#210875=CARTESIAN_POINT('Ctrl Pts',(13.2451415942805,19.7989054860495,0.));
#210876=CARTESIAN_POINT('Ctrl Pts',(13.2398366985675,19.7792151253289,0.));
#210877=CARTESIAN_POINT('Ctrl Pts',(13.2345074487963,19.7596428141168,0.));
#210878=CARTESIAN_POINT('Ctrl Pts',(13.2291544897899,19.7401892678697,0.));
#210879=CARTESIAN_POINT('Ctrl Pts',(13.2237784757065,19.7208552097868,0.));
#210880=CARTESIAN_POINT('Ctrl Pts',(13.2183800702436,19.7016413709685,0.));
#210881=CARTESIAN_POINT('Ctrl Pts',(13.2129599468485,19.6825484905823,0.));
#210882=CARTESIAN_POINT('Ctrl Pts',(13.2075187889529,19.6635773160936,0.));
#210883=CARTESIAN_POINT('Ctrl Pts',(13.2020572902065,19.6447286034772,0.));
#210884=CARTESIAN_POINT('Ctrl Pts',(13.1965761547151,19.6260031174244,0.));
#210885=CARTESIAN_POINT('Ctrl Pts',(13.1910760972814,19.6074016315414,0.));
#210886=CARTESIAN_POINT('Ctrl Pts',(13.1855578436471,19.5889249285338,0.));
#210887=CARTESIAN_POINT('Ctrl Pts',(13.1800221307673,19.5705738004667,0.));
#210888=CARTESIAN_POINT('Ctrl Pts',(13.1744697070911,19.5523490490244,0.));
#210889=CARTESIAN_POINT('Ctrl Pts',(13.168901332843,19.5342514857562,0.));
#210890=CARTESIAN_POINT('Ctrl Pts',(13.1633177803101,19.5162819323213,0.));
#210891=CARTESIAN_POINT('Ctrl Pts',(13.1577198341245,19.4984412207082,0.));
#210892=CARTESIAN_POINT('Ctrl Pts',(13.1521082915853,19.4807301935268,0.));
#210893=CARTESIAN_POINT('Ctrl Pts',(13.1464839629971,19.4631497043258,0.));
#210894=CARTESIAN_POINT('Ctrl Pts',(13.1408476720061,19.4457006178876,0.));
#210895=CARTESIAN_POINT('Ctrl Pts',(13.1352002559438,19.4283838105262,0.));
#210896=CARTESIAN_POINT('Ctrl Pts',(13.1295425661634,19.4112001703557,0.));
#210897=CARTESIAN_POINT('Ctrl Pts',(13.1238754684177,19.3941505976263,0.));
#210898=CARTESIAN_POINT('Ctrl Pts',(13.118199843271,19.3772360051091,0.));
#210899=CARTESIAN_POINT('Ctrl Pts',(13.1125165865022,19.3604573184515,0.));
#210900=CARTESIAN_POINT('Ctrl Pts',(13.1068266095186,19.3438154765395,0.));
#210901=CARTESIAN_POINT('Ctrl Pts',(13.1011308397591,19.3273114318269,0.));
#210902=CARTESIAN_POINT('Ctrl Pts',(13.0954302211479,19.310946150736,0.));
#210903=CARTESIAN_POINT('Ctrl Pts',(13.0897257145968,19.2947206141247,0.));
#210904=CARTESIAN_POINT('Ctrl Pts',(13.0840182984949,19.2786358177198,0.));
#210905=CARTESIAN_POINT('Ctrl Pts',(13.0783089692118,19.2626927725596,0.));
#210906=CARTESIAN_POINT('Ctrl Pts',(13.0725987415859,19.2468925053989,0.));
#210907=CARTESIAN_POINT('Ctrl Pts',(13.0668886494795,19.2312360592033,0.));
#210908=CARTESIAN_POINT('Ctrl Pts',(13.0611797463915,19.2157244937142,0.));
#210909=CARTESIAN_POINT('Ctrl Pts',(13.0554731060538,19.2003588859772,0.));
#210910=CARTESIAN_POINT('Ctrl Pts',(13.0497698230441,19.1851403308825,0.));
#210911=CARTESIAN_POINT('Ctrl Pts',(13.0440710133772,19.1700699416622,0.));
#210912=CARTESIAN_POINT('Ctrl Pts',(13.0383778152068,19.155148850523,0.));
#210913=CARTESIAN_POINT('Ctrl Pts',(13.0326913895838,19.1403782093386,0.));
#210914=CARTESIAN_POINT('Ctrl Pts',(13.0270129211976,19.1257591903099,0.));
#210915=CARTESIAN_POINT('Ctrl Pts',(13.0213436191328,19.111292986631,0.));
#210916=CARTESIAN_POINT('Ctrl Pts',(13.0156847176096,19.0969808131228,0.));
#210917=CARTESIAN_POINT('Ctrl Pts',(13.0100374768788,19.0828239070484,0.));
#210918=CARTESIAN_POINT('Ctrl Pts',(13.0044031841382,19.0688235289437,0.));
#210919=CARTESIAN_POINT('Ctrl Pts',(12.9987831544502,19.0549809634354,0.));
#210920=CARTESIAN_POINT('Ctrl Pts',(12.9931787316514,19.0412975200398,0.));
#210921=CARTESIAN_POINT('Ctrl Pts',(12.9875912893003,19.0277745339909,0.));
#210922=CARTESIAN_POINT('Ctrl Pts',(12.9820222318716,19.014413367335,0.));
#210923=CARTESIAN_POINT('Ctrl Pts',(12.9764729959206,19.0012154099792,0.));
#210924=CARTESIAN_POINT('Ctrl Pts',(12.9709450512747,18.9881820807585,0.));
#210925=CARTESIAN_POINT('Ctrl Pts',(12.9654399021868,18.9753148284473,0.));
#210926=CARTESIAN_POINT('Ctrl Pts',(12.9599590886317,18.9626151329226,0.));
#210927=CARTESIAN_POINT('Ctrl Pts',(12.9545041877377,18.9500845064714,0.));
#210928=CARTESIAN_POINT('Ctrl Pts',(12.9490768151821,18.9377244950435,0.));
#210929=CARTESIAN_POINT('Ctrl Pts',(12.9436786266106,18.9255366795196,0.));
#210930=CARTESIAN_POINT('Ctrl Pts',(12.9383113190375,18.9135226769466,0.));
#210931=CARTESIAN_POINT('Ctrl Pts',(12.9329766328184,18.9016841423402,0.));
#210932=CARTESIAN_POINT('Ctrl Pts',(12.9276763536372,18.8900227704888,0.));
#210933=CARTESIAN_POINT('Ctrl Pts',(12.9224123144982,18.8785402977528,0.));
#210934=CARTESIAN_POINT('Ctrl Pts',(12.9171863977047,18.8672385038328,0.));
#210935=CARTESIAN_POINT('Ctrl Pts',(12.9120005369066,18.8561192136201,0.));
#210936=CARTESIAN_POINT('Ctrl Pts',(12.9068567191856,18.8451842990986,0.));
#210937=CARTESIAN_POINT('Ctrl Pts',(12.9017569871738,18.834435681259,0.));
#210938=CARTESIAN_POINT('Ctrl Pts',(12.8967034410752,18.8238753319124,0.));
#210939=CARTESIAN_POINT('Ctrl Pts',(12.8916982409931,18.8135052757815,0.));
#210940=CARTESIAN_POINT('Ctrl Pts',(12.8867436109543,18.8033275941939,0.));
#210941=CARTESIAN_POINT('Ctrl Pts',(12.8818418427474,18.7933444285867,0.));
#210942=CARTESIAN_POINT('Ctrl Pts',(12.8769952998097,18.7835579840481,0.));
#210943=CARTESIAN_POINT('Ctrl Pts',(12.8722064211814,18.7739705329029,0.));
#210944=CARTESIAN_POINT('Ctrl Pts',(12.8674777239656,18.7645844169568,0.));
#210945=CARTESIAN_POINT('Ctrl Pts',(12.8628118054172,18.7554020493888,0.));
#210946=CARTESIAN_POINT('Ctrl Pts',(12.8582113455644,18.7464259171248,0.));
#210947=CARTESIAN_POINT('Ctrl Pts',(12.8536791086315,18.7376585820851,0.));
#210948=CARTESIAN_POINT('Ctrl Pts',(12.849217951159,18.7291026886552,0.));
#210949=CARTESIAN_POINT('Ctrl Pts',(12.8448308329494,18.7207609737701,0.));
#210950=CARTESIAN_POINT('Ctrl Pts',(12.8405208263432,18.7126362754446,0.));
#210951=CARTESIAN_POINT('Ctrl Pts',(12.8362911280362,18.7047315436296,0.));
#210952=CARTESIAN_POINT('Ctrl Pts',(12.832145059979,18.6970498410173,0.));
#210953=CARTESIAN_POINT('Ctrl Pts',(12.8280860635231,18.6895943376172,0.));
#210954=CARTESIAN_POINT('Ctrl Pts',(12.8241176980016,18.6823683094139,0.));
#210955=CARTESIAN_POINT('Ctrl Pts',(12.8202436318473,18.6753751301091,0.));
#210956=CARTESIAN_POINT('Ctrl Pts',(12.8164676687361,18.6686182952798,0.));
#210957=CARTESIAN_POINT('Ctrl Pts',(12.8127937909632,18.6621014624746,0.));
#210958=CARTESIAN_POINT('Ctrl Pts',(12.8092261933858,18.6558284825772,0.));
#210959=CARTESIAN_POINT('Ctrl Pts',(12.805769331162,18.6498034438986,0.));
#210960=CARTESIAN_POINT('Ctrl Pts',(12.8024278770153,18.6440306327457,0.));
#210961=CARTESIAN_POINT('Ctrl Pts',(12.7992066625264,18.63851447924,0.));
#210962=CARTESIAN_POINT('Ctrl Pts',(12.7961106222251,18.6332595057005,0.));
#210963=CARTESIAN_POINT('Ctrl Pts',(12.7931447451556,18.6282702819371,0.));
#210964=CARTESIAN_POINT('Ctrl Pts',(12.7903142925234,18.6235516265575,0.));
#210965=CARTESIAN_POINT('Ctrl Pts',(12.7876249657834,18.6191087624752,0.));
#210966=CARTESIAN_POINT('Ctrl Pts',(12.78508316579,18.6149475565189,0.));
#210967=CARTESIAN_POINT('Ctrl Pts',(12.7826959526924,18.611074482622,0.));
#210968=CARTESIAN_POINT('Ctrl Pts',(12.7804705387658,18.6074961535723,0.));
#210969=CARTESIAN_POINT('Ctrl Pts',(12.7784139605067,18.6042190183703,0.));
#210970=CARTESIAN_POINT('Ctrl Pts',(12.7765325225082,18.6012488486708,0.));
#210971=CARTESIAN_POINT('Ctrl Pts',(12.7748328937639,18.5985917525949,0.));
#210972=CARTESIAN_POINT('Ctrl Pts',(12.7733231262107,18.5962551167772,0.));
#210973=CARTESIAN_POINT('Ctrl Pts',(12.7720142287169,18.5942490615409,0.));
#210974=CARTESIAN_POINT('Ctrl Pts',(12.7709195951153,18.5925859134582,0.));
#210975=CARTESIAN_POINT('Ctrl Pts',(12.7700520897174,18.5912775137806,0.));
#210976=CARTESIAN_POINT('Ctrl Pts',(12.7694215127923,18.590332877722,0.));
#210977=CARTESIAN_POINT('Ctrl Pts',(12.7691103481996,18.589871621842,0.));
#210978=CARTESIAN_POINT('Ctrl Pts',(12.7689864266924,18.5896919669158,0.));
#210979=CARTESIAN_POINT('Ctrl Pts',(12.7689524524484,18.5896460962961,0.));
#210980=CARTESIAN_POINT('Ctrl Pts',(12.7689476255363,18.5896416359912,0.));
#210981=CARTESIAN_POINT('',(13.5685075571671,22.1787195904339,0.));
#210982=CARTESIAN_POINT('Ctrl Pts',(14.6513681262571,17.1452095830633,0.));
#210983=CARTESIAN_POINT('Ctrl Pts',(14.6513681262571,17.1452095830633,12.));
#210984=CARTESIAN_POINT('Ctrl Pts',(14.6513711852843,17.1452153999142,0.));
#210985=CARTESIAN_POINT('Ctrl Pts',(14.6513711852843,17.1452153999142,12.));
#210986=CARTESIAN_POINT('Ctrl Pts',(14.6514066997196,17.1452600887037,0.));
#210987=CARTESIAN_POINT('Ctrl Pts',(14.6514066997196,17.1452600887037,12.));
#210988=CARTESIAN_POINT('Ctrl Pts',(14.6515481598068,17.1454262858043,0.));
#210989=CARTESIAN_POINT('Ctrl Pts',(14.6515481598068,17.1454262858043,12.));
#210990=CARTESIAN_POINT('Ctrl Pts',(14.6519131634508,17.1458462295271,0.));
#210991=CARTESIAN_POINT('Ctrl Pts',(14.6519131634508,17.1458462295271,12.));
#210992=CARTESIAN_POINT('Ctrl Pts',(14.6526624064978,17.1466998098673,0.));
#210993=CARTESIAN_POINT('Ctrl Pts',(14.6526624064978,17.1466998098673,12.));
#210994=CARTESIAN_POINT('Ctrl Pts',(14.6537016966184,17.147876394491,0.));
#210995=CARTESIAN_POINT('Ctrl Pts',(14.6537016966184,17.147876394491,12.));
#210996=CARTESIAN_POINT('Ctrl Pts',(14.655024862281,17.1493641837558,0.));
#210997=CARTESIAN_POINT('Ctrl Pts',(14.655024862281,17.1493641837558,12.));
#210998=CARTESIAN_POINT('Ctrl Pts',(14.6566237952435,17.1511476869496,0.));
#210999=CARTESIAN_POINT('Ctrl Pts',(14.6566237952435,17.1511476869496,12.));
#211000=CARTESIAN_POINT('Ctrl Pts',(14.6584900555302,17.1532107762718,0.));
#211001=CARTESIAN_POINT('Ctrl Pts',(14.6584900555302,17.1532107762718,12.));
#211002=CARTESIAN_POINT('Ctrl Pts',(14.6606167169642,17.1555401986401,0.));
#211003=CARTESIAN_POINT('Ctrl Pts',(14.6606167169642,17.1555401986401,12.));
#211004=CARTESIAN_POINT('Ctrl Pts',(14.6629987285992,17.1581262646789,0.));
#211005=CARTESIAN_POINT('Ctrl Pts',(14.6629987285992,17.1581262646789,12.));
#211006=CARTESIAN_POINT('Ctrl Pts',(14.6656319165057,17.1609609517369,0.));
#211007=CARTESIAN_POINT('Ctrl Pts',(14.6656319165057,17.1609609517369,12.));
#211008=CARTESIAN_POINT('Ctrl Pts',(14.6685123374423,17.1640366762305,0.));
#211009=CARTESIAN_POINT('Ctrl Pts',(14.6685123374423,17.1640366762305,12.));
#211010=CARTESIAN_POINT('Ctrl Pts',(14.671635583332,17.167344972302,0.));
#211011=CARTESIAN_POINT('Ctrl Pts',(14.671635583332,17.167344972302,12.));
#211012=CARTESIAN_POINT('Ctrl Pts',(14.6749971333867,17.1708771619129,0.));
#211013=CARTESIAN_POINT('Ctrl Pts',(14.6749971333867,17.1708771619129,12.));
#211014=CARTESIAN_POINT('Ctrl Pts',(14.6785925615677,17.1746247499057,0.));
#211015=CARTESIAN_POINT('Ctrl Pts',(14.6785925615677,17.1746247499057,12.));
#211016=CARTESIAN_POINT('Ctrl Pts',(14.6824178576167,17.1785800350826,0.));
#211017=CARTESIAN_POINT('Ctrl Pts',(14.6824178576167,17.1785800350826,12.));
#211018=CARTESIAN_POINT('Ctrl Pts',(14.686469452232,17.182736158472,0.));
#211019=CARTESIAN_POINT('Ctrl Pts',(14.686469452232,17.182736158472,12.));
#211020=CARTESIAN_POINT('Ctrl Pts',(14.6907440526958,17.1870867909918,0.));
#211021=CARTESIAN_POINT('Ctrl Pts',(14.6907440526958,17.1870867909918,12.));
#211022=CARTESIAN_POINT('Ctrl Pts',(14.6952385361705,17.1916259308415,0.));
#211023=CARTESIAN_POINT('Ctrl Pts',(14.6952385361705,17.1916259308415,12.));
#211024=CARTESIAN_POINT('Ctrl Pts',(14.699949811582,17.1963476411694,0.));
#211025=CARTESIAN_POINT('Ctrl Pts',(14.699949811582,17.1963476411694,12.));
#211026=CARTESIAN_POINT('Ctrl Pts',(14.7048748502663,17.2012461084268,0.));
#211027=CARTESIAN_POINT('Ctrl Pts',(14.7048748502663,17.2012461084268,12.));
#211028=CARTESIAN_POINT('Ctrl Pts',(14.7100107213586,17.2063157097315,0.));
#211029=CARTESIAN_POINT('Ctrl Pts',(14.7100107213586,17.2063157097315,12.));
#211030=CARTESIAN_POINT('Ctrl Pts',(14.7153546289339,17.2115510835989,0.));
#211031=CARTESIAN_POINT('Ctrl Pts',(14.7153546289339,17.2115510835989,12.));
#211032=CARTESIAN_POINT('Ctrl Pts',(14.7209039390327,17.2169471814256,0.));
#211033=CARTESIAN_POINT('Ctrl Pts',(14.7209039390327,17.2169471814256,12.));
#211034=CARTESIAN_POINT('Ctrl Pts',(14.7266561494282,17.2224992099667,0.));
#211035=CARTESIAN_POINT('Ctrl Pts',(14.7266561494282,17.2224992099667,12.));
#211036=CARTESIAN_POINT('Ctrl Pts',(14.7326088681163,17.2282025904314,0.));
#211037=CARTESIAN_POINT('Ctrl Pts',(14.7326088681163,17.2282025904314,12.));
#211038=CARTESIAN_POINT('Ctrl Pts',(14.7387597858116,17.2340529062076,0.));
#211039=CARTESIAN_POINT('Ctrl Pts',(14.7387597858116,17.2340529062076,12.));
#211040=CARTESIAN_POINT('Ctrl Pts',(14.7451066593792,17.2400458713565,0.));
#211041=CARTESIAN_POINT('Ctrl Pts',(14.7451066593792,17.2400458713565,12.));
#211042=CARTESIAN_POINT('Ctrl Pts',(14.7516473175124,17.2461773413288,0.));
#211043=CARTESIAN_POINT('Ctrl Pts',(14.7516473175124,17.2461773413288,12.));
#211044=CARTESIAN_POINT('Ctrl Pts',(14.7583796616617,17.2524433146837,0.));
#211045=CARTESIAN_POINT('Ctrl Pts',(14.7583796616617,17.2524433146837,12.));
#211046=CARTESIAN_POINT('Ctrl Pts',(14.7653016697591,17.2588399401465,0.));
#211047=CARTESIAN_POINT('Ctrl Pts',(14.7653016697591,17.2588399401465,12.));
#211048=CARTESIAN_POINT('Ctrl Pts',(14.7724113956731,17.2653635155319,0.));
#211049=CARTESIAN_POINT('Ctrl Pts',(14.7724113956731,17.2653635155319,12.));
#211050=CARTESIAN_POINT('Ctrl Pts',(14.7797069617804,17.2720104735194,0.));
#211051=CARTESIAN_POINT('Ctrl Pts',(14.7797069617804,17.2720104735194,12.));
#211052=CARTESIAN_POINT('Ctrl Pts',(14.787186553128,17.2787773704849,0.));
#211053=CARTESIAN_POINT('Ctrl Pts',(14.787186553128,17.2787773704849,12.));
#211054=CARTESIAN_POINT('Ctrl Pts',(14.7948484105249,17.2856608733196,0.));
#211055=CARTESIAN_POINT('Ctrl Pts',(14.7948484105249,17.2856608733196,12.));
#211056=CARTESIAN_POINT('Ctrl Pts',(14.8026908254276,17.2926577496513,0.));
#211057=CARTESIAN_POINT('Ctrl Pts',(14.8026908254276,17.2926577496513,12.));
#211058=CARTESIAN_POINT('Ctrl Pts',(14.8107121391035,17.299764866148,0.));
#211059=CARTESIAN_POINT('Ctrl Pts',(14.8107121391035,17.299764866148,12.));
#211060=CARTESIAN_POINT('Ctrl Pts',(14.8189107410162,17.3069791853706,0.));
#211061=CARTESIAN_POINT('Ctrl Pts',(14.8189107410162,17.3069791853706,12.));
#211062=CARTESIAN_POINT('Ctrl Pts',(14.8272850675379,17.3142977632659,0.));
#211063=CARTESIAN_POINT('Ctrl Pts',(14.8272850675379,17.3142977632659,12.));
#211064=CARTESIAN_POINT('Ctrl Pts',(14.8358336004197,17.3217177462101,0.));
#211065=CARTESIAN_POINT('Ctrl Pts',(14.8358336004197,17.3217177462101,12.));
#211066=CARTESIAN_POINT('Ctrl Pts',(14.8445548643508,17.3292363662605,0.));
#211067=CARTESIAN_POINT('Ctrl Pts',(14.8445548643508,17.3292363662605,12.));
#211068=CARTESIAN_POINT('Ctrl Pts',(14.8534474245433,17.336850936485,0.));
#211069=CARTESIAN_POINT('Ctrl Pts',(14.8534474245433,17.336850936485,12.));
#211070=CARTESIAN_POINT('Ctrl Pts',(14.8625098843417,17.3445588463475,0.));
#211071=CARTESIAN_POINT('Ctrl Pts',(14.8625098843417,17.3445588463475,12.));
#211072=CARTESIAN_POINT('Ctrl Pts',(14.8717408826955,17.3523575568645,0.));
#211073=CARTESIAN_POINT('Ctrl Pts',(14.8717408826955,17.3523575568645,12.));
#211074=CARTESIAN_POINT('Ctrl Pts',(14.8811390927423,17.3602445978161,0.));
#211075=CARTESIAN_POINT('Ctrl Pts',(14.8811390927423,17.3602445978161,12.));
#211076=CARTESIAN_POINT('Ctrl Pts',(14.8907032205788,17.3682175653235,0.));
#211077=CARTESIAN_POINT('Ctrl Pts',(14.8907032205788,17.3682175653235,12.));
#211078=CARTESIAN_POINT('Ctrl Pts',(14.900432003961,17.3762741193076,0.));
#211079=CARTESIAN_POINT('Ctrl Pts',(14.900432003961,17.3762741193076,12.));
#211080=CARTESIAN_POINT('Ctrl Pts',(14.9103242110057,17.3844119809824,0.));
#211081=CARTESIAN_POINT('Ctrl Pts',(14.9103242110057,17.3844119809824,12.));
#211082=CARTESIAN_POINT('Ctrl Pts',(14.9203786389342,17.3926289303986,0.));
#211083=CARTESIAN_POINT('Ctrl Pts',(14.9203786389342,17.3926289303986,12.));
#211084=CARTESIAN_POINT('Ctrl Pts',(14.9305941128757,17.4009228040749,0.));
#211085=CARTESIAN_POINT('Ctrl Pts',(14.9305941128757,17.4009228040749,12.));
#211086=CARTESIAN_POINT('Ctrl Pts',(14.940969484645,17.4092914926071,0.));
#211087=CARTESIAN_POINT('Ctrl Pts',(14.940969484645,17.4092914926071,12.));
#211088=CARTESIAN_POINT('Ctrl Pts',(14.9515036315143,17.4177329382828,0.));
#211089=CARTESIAN_POINT('Ctrl Pts',(14.9515036315143,17.4177329382828,12.));
#211090=CARTESIAN_POINT('Ctrl Pts',(14.9621954549827,17.426245132709,0.));
#211091=CARTESIAN_POINT('Ctrl Pts',(14.9621954549827,17.426245132709,12.));
#211092=CARTESIAN_POINT('Ctrl Pts',(14.9730438799452,17.4348261151396,0.));
#211093=CARTESIAN_POINT('Ctrl Pts',(14.9730438799452,17.4348261151396,12.));
#211094=CARTESIAN_POINT('Ctrl Pts',(14.9840478538358,17.4434739707773,0.));
#211095=CARTESIAN_POINT('Ctrl Pts',(14.9840478538358,17.4434739707773,12.));
#211096=CARTESIAN_POINT('Ctrl Pts',(14.9952063457778,17.4521868291004,0.));
#211097=CARTESIAN_POINT('Ctrl Pts',(14.9952063457778,17.4521868291004,12.));
#211098=CARTESIAN_POINT('Ctrl Pts',(15.0065183456921,17.4609628621418,0.));
#211099=CARTESIAN_POINT('Ctrl Pts',(15.0065183456921,17.4609628621418,12.));
#211100=CARTESIAN_POINT('Ctrl Pts',(15.0179828635086,17.4698002829357,0.));
#211101=CARTESIAN_POINT('Ctrl Pts',(15.0179828635086,17.4698002829357,12.));
#211102=CARTESIAN_POINT('Ctrl Pts',(15.029598928488,17.4786973441417,0.));
#211103=CARTESIAN_POINT('Ctrl Pts',(15.029598928488,17.4786973441417,12.));
#211104=CARTESIAN_POINT('Ctrl Pts',(15.0413655884993,17.4876523366178,0.));
#211105=CARTESIAN_POINT('Ctrl Pts',(15.0413655884993,17.4876523366178,12.));
#211106=CARTESIAN_POINT('Ctrl Pts',(15.0532819093085,17.4966635880245,0.));
#211107=CARTESIAN_POINT('Ctrl Pts',(15.0532819093085,17.4966635880245,12.));
#211108=CARTESIAN_POINT('Ctrl Pts',(15.0653469738306,17.5057294613874,0.));
#211109=CARTESIAN_POINT('Ctrl Pts',(15.0653469738306,17.5057294613874,12.));
#211110=CARTESIAN_POINT('Ctrl Pts',(15.0775598815748,17.5148483539684,0.));
#211111=CARTESIAN_POINT('Ctrl Pts',(15.0775598815748,17.5148483539684,12.));
#211112=CARTESIAN_POINT('Ctrl Pts',(15.0899197481082,17.5240186961788,0.));
#211113=CARTESIAN_POINT('Ctrl Pts',(15.0899197481082,17.5240186961788,12.));
#211114=CARTESIAN_POINT('Ctrl Pts',(15.1024257045033,17.5332389504829,0.));
#211115=CARTESIAN_POINT('Ctrl Pts',(15.1024257045033,17.5332389504829,12.));
#211116=CARTESIAN_POINT('Ctrl Pts',(15.1150768967729,17.5425076102966,0.));
#211117=CARTESIAN_POINT('Ctrl Pts',(15.1150768967729,17.5425076102966,12.));
#211118=CARTESIAN_POINT('Ctrl Pts',(15.127872485314,17.5518231989122,0.));
#211119=CARTESIAN_POINT('Ctrl Pts',(15.127872485314,17.5518231989122,12.));
#211120=CARTESIAN_POINT('Ctrl Pts',(15.1408116444877,17.5611842686196,0.));
#211121=CARTESIAN_POINT('Ctrl Pts',(15.1408116444877,17.5611842686196,12.));
#211122=CARTESIAN_POINT('Ctrl Pts',(15.1538935621714,17.570589399803,0.));
#211123=CARTESIAN_POINT('Ctrl Pts',(15.1538935621714,17.570589399803,12.));
#211124=CARTESIAN_POINT('Ctrl Pts',(15.1671174393136,17.5800372000539,0.));
#211125=CARTESIAN_POINT('Ctrl Pts',(15.1671174393136,17.5800372000539,12.));
#211126=CARTESIAN_POINT('Ctrl Pts',(15.1804824894605,17.5895263032592,0.));
#211127=CARTESIAN_POINT('Ctrl Pts',(15.1804824894605,17.5895263032592,12.));
#211128=CARTESIAN_POINT('Ctrl Pts',(15.1939879383268,17.5990553687595,0.));
#211129=CARTESIAN_POINT('Ctrl Pts',(15.1939879383268,17.5990553687595,12.));
#211130=CARTESIAN_POINT('Ctrl Pts',(15.2076330234686,17.6086230806497,0.));
#211131=CARTESIAN_POINT('Ctrl Pts',(15.2076330234686,17.6086230806497,12.));
#211132=CARTESIAN_POINT('Ctrl Pts',(15.22141699392,17.6182281470467,0.));
#211133=CARTESIAN_POINT('Ctrl Pts',(15.22141699392,17.6182281470467,12.));
#211134=CARTESIAN_POINT('Ctrl Pts',(15.2353391098367,17.6278692993765,0.));
#211135=CARTESIAN_POINT('Ctrl Pts',(15.2353391098367,17.6278692993765,12.));
#211136=CARTESIAN_POINT('Ctrl Pts',(15.2493986421091,17.637545291637,0.));
#211137=CARTESIAN_POINT('Ctrl Pts',(15.2493986421091,17.637545291637,12.));
#211138=CARTESIAN_POINT('Ctrl Pts',(15.263594872029,17.6472548997329,0.));
#211139=CARTESIAN_POINT('Ctrl Pts',(15.263594872029,17.6472548997329,12.));
#211140=CARTESIAN_POINT('Ctrl Pts',(15.2779270910238,17.6569969209,0.));
#211141=CARTESIAN_POINT('Ctrl Pts',(15.2779270910238,17.6569969209,12.));
#211142=CARTESIAN_POINT('Ctrl Pts',(15.2923946003598,17.6667701731041,0.));
#211143=CARTESIAN_POINT('Ctrl Pts',(15.2923946003598,17.6667701731041,12.));
#211144=CARTESIAN_POINT('Ctrl Pts',(15.3069967108501,17.6765734944559,0.));
#211145=CARTESIAN_POINT('Ctrl Pts',(15.3069967108501,17.6765734944559,12.));
#211146=CARTESIAN_POINT('Ctrl Pts',(15.3217327425341,17.6864057426052,0.));
#211147=CARTESIAN_POINT('Ctrl Pts',(15.3217327425341,17.6864057426052,12.));
#211148=CARTESIAN_POINT('Ctrl Pts',(15.3366020244069,17.6962657941984,0.));
#211149=CARTESIAN_POINT('Ctrl Pts',(15.3366020244069,17.6962657941984,12.));
#211150=CARTESIAN_POINT('Ctrl Pts',(15.3516038942064,17.7061525444044,0.));
#211151=CARTESIAN_POINT('Ctrl Pts',(15.3516038942064,17.7061525444044,12.));
#211152=CARTESIAN_POINT('Ctrl Pts',(15.3667376981702,17.7160649064208,0.));
#211153=CARTESIAN_POINT('Ctrl Pts',(15.3667376981702,17.7160649064208,12.));
#211154=CARTESIAN_POINT('Ctrl Pts',(15.3820027907965,17.7260018109923,0.));
#211155=CARTESIAN_POINT('Ctrl Pts',(15.3820027907965,17.7260018109923,12.));
#211156=CARTESIAN_POINT('Ctrl Pts',(15.3973985345796,17.7359622059143,0.));
#211157=CARTESIAN_POINT('Ctrl Pts',(15.3973985345796,17.7359622059143,12.));
#211158=CARTESIAN_POINT('Ctrl Pts',(15.4129242997828,17.7459450555803,0.));
#211159=CARTESIAN_POINT('Ctrl Pts',(15.4129242997828,17.7459450555803,12.));
#211160=CARTESIAN_POINT('Ctrl Pts',(15.4285794642658,17.7559493405871,0.));
#211161=CARTESIAN_POINT('Ctrl Pts',(15.4285794642658,17.7559493405871,12.));
#211162=CARTESIAN_POINT('Ctrl Pts',(15.4443634132865,17.765974057326,0.));
#211163=CARTESIAN_POINT('Ctrl Pts',(15.4443634132865,17.765974057326,12.));
#211164=CARTESIAN_POINT('Ctrl Pts',(15.4602755393019,17.7760182175817,0.));
#211165=CARTESIAN_POINT('Ctrl Pts',(15.4602755393019,17.7760182175817,12.));
#211166=CARTESIAN_POINT('Ctrl Pts',(15.4763152417506,17.7860808481229,0.));
#211167=CARTESIAN_POINT('Ctrl Pts',(15.4763152417506,17.7860808481229,12.));
#211168=CARTESIAN_POINT('Ctrl Pts',(15.4924819268529,17.7961609903161,0.));
#211169=CARTESIAN_POINT('Ctrl Pts',(15.4924819268529,17.7961609903161,12.));
#211170=CARTESIAN_POINT('Ctrl Pts',(15.5087750074728,17.8062576997964,0.));
#211171=CARTESIAN_POINT('Ctrl Pts',(15.5087750074728,17.8062576997964,12.));
#211172=CARTESIAN_POINT('Ctrl Pts',(15.5251939029558,17.8163700461263,0.));
#211173=CARTESIAN_POINT('Ctrl Pts',(15.5251939029558,17.8163700461263,12.));
#211174=CARTESIAN_POINT('Ctrl Pts',(15.5417380389639,17.8264971124606,0.));
#211175=CARTESIAN_POINT('Ctrl Pts',(15.5417380389639,17.8264971124606,12.));
#211176=CARTESIAN_POINT('Ctrl Pts',(15.5584068472976,17.8366379952078,0.));
#211177=CARTESIAN_POINT('Ctrl Pts',(15.5584068472976,17.8366379952078,12.));
#211178=CARTESIAN_POINT('Ctrl Pts',(15.5751997657153,17.8467918036977,0.));
#211179=CARTESIAN_POINT('Ctrl Pts',(15.5751997657153,17.8467918036977,12.));
#211180=CARTESIAN_POINT('Ctrl Pts',(15.5921162378183,17.8569576598996,0.));
#211181=CARTESIAN_POINT('Ctrl Pts',(15.5921162378183,17.8569576598996,12.));
#211182=CARTESIAN_POINT('Ctrl Pts',(15.6091557129205,17.8671346981388,0.));
#211183=CARTESIAN_POINT('Ctrl Pts',(15.6091557129205,17.8671346981388,12.));
#211184=CARTESIAN_POINT('Ctrl Pts',(15.6263176459107,17.8773220648125,0.));
#211185=CARTESIAN_POINT('Ctrl Pts',(15.6263176459107,17.8773220648125,12.));
#211186=CARTESIAN_POINT('Ctrl Pts',(15.6436014971088,17.8875189181095,0.));
#211187=CARTESIAN_POINT('Ctrl Pts',(15.6436014971088,17.8875189181095,12.));
#211188=CARTESIAN_POINT('Ctrl Pts',(15.6610067321036,17.8977244277247,0.));
#211189=CARTESIAN_POINT('Ctrl Pts',(15.6610067321036,17.8977244277247,12.));
#211190=CARTESIAN_POINT('Ctrl Pts',(15.6785328216467,17.9079377746118,0.));
#211191=CARTESIAN_POINT('Ctrl Pts',(15.6785328216467,17.9079377746118,12.));
#211192=CARTESIAN_POINT('Ctrl Pts',(15.6961792415526,17.918158150746,0.));
#211193=CARTESIAN_POINT('Ctrl Pts',(15.6961792415526,17.918158150746,12.));
#211194=CARTESIAN_POINT('Ctrl Pts',(15.713945472584,17.9283847588837,0.));
#211195=CARTESIAN_POINT('Ctrl Pts',(15.713945472584,17.9283847588837,12.));
#211196=CARTESIAN_POINT('Ctrl Pts',(15.7318310003334,17.9386168123261,0.));
#211197=CARTESIAN_POINT('Ctrl Pts',(15.7318310003334,17.9386168123261,12.));
#211198=CARTESIAN_POINT('Ctrl Pts',(15.7498353150856,17.9488535346776,0.));
#211199=CARTESIAN_POINT('Ctrl Pts',(15.7498353150856,17.9488535346776,12.));
#211200=CARTESIAN_POINT('Ctrl Pts',(15.7679579117072,17.9590941596236,0.));
#211201=CARTESIAN_POINT('Ctrl Pts',(15.7679579117072,17.9590941596236,12.));
#211202=CARTESIAN_POINT('Ctrl Pts',(15.786198289572,17.9693379307297,0.));
#211203=CARTESIAN_POINT('Ctrl Pts',(15.786198289572,17.9693379307297,12.));
#211204=CARTESIAN_POINT('Ctrl Pts',(15.8045559524674,17.9795841012383,0.));
#211205=CARTESIAN_POINT('Ctrl Pts',(15.8045559524674,17.9795841012383,12.));
#211206=CARTESIAN_POINT('Ctrl Pts',(15.8230304084963,17.9898319338664,0.));
#211207=CARTESIAN_POINT('Ctrl Pts',(15.8230304084963,17.9898319338664,12.));
#211208=CARTESIAN_POINT('Ctrl Pts',(15.8416211699681,18.0000807006055,0.));
#211209=CARTESIAN_POINT('Ctrl Pts',(15.8416211699681,18.0000807006055,12.));
#211210=CARTESIAN_POINT('Ctrl Pts',(15.8603277532834,18.010329682521,0.));
#211211=CARTESIAN_POINT('Ctrl Pts',(15.8603277532834,18.010329682521,12.));
#211212=CARTESIAN_POINT('Ctrl Pts',(15.8791496788685,18.0205781695773,0.));
#211213=CARTESIAN_POINT('Ctrl Pts',(15.8791496788685,18.0205781695773,12.));
#211214=CARTESIAN_POINT('Ctrl Pts',(15.8980864711043,18.0308254604638,0.));
#211215=CARTESIAN_POINT('Ctrl Pts',(15.8980864711043,18.0308254604638,12.));
#211216=CARTESIAN_POINT('Ctrl Pts',(15.9171376582436,18.0410708624208,0.));
#211217=CARTESIAN_POINT('Ctrl Pts',(15.9171376582436,18.0410708624208,12.));
#211218=CARTESIAN_POINT('Ctrl Pts',(15.9363027723244,18.0513136910691,0.));
#211219=CARTESIAN_POINT('Ctrl Pts',(15.9363027723244,18.0513136910691,12.));
#211220=CARTESIAN_POINT('Ctrl Pts',(15.9555813490645,18.061553270236,0.));
#211221=CARTESIAN_POINT('Ctrl Pts',(15.9555813490645,18.061553270236,12.));
#211222=CARTESIAN_POINT('Ctrl Pts',(15.9749729277848,18.071788931796,0.));
#211223=CARTESIAN_POINT('Ctrl Pts',(15.9749729277848,18.071788931796,12.));
#211224=CARTESIAN_POINT('Ctrl Pts',(15.9944770513616,18.0820200155239,0.));
#211225=CARTESIAN_POINT('Ctrl Pts',(15.9944770513616,18.0820200155239,12.));
#211226=CARTESIAN_POINT('Ctrl Pts',(16.0140932661612,18.0922458689464,0.));
#211227=CARTESIAN_POINT('Ctrl Pts',(16.0140932661612,18.0922458689464,12.));
#211228=CARTESIAN_POINT('Ctrl Pts',(16.0338211219693,18.1024658471966,0.));
#211229=CARTESIAN_POINT('Ctrl Pts',(16.0338211219693,18.1024658471966,12.));
#211230=CARTESIAN_POINT('Ctrl Pts',(16.0536601719124,18.1126793128688,0.));
#211231=CARTESIAN_POINT('Ctrl Pts',(16.0536601719124,18.1126793128688,12.));
#211232=CARTESIAN_POINT('Ctrl Pts',(16.0736099723664,18.1228856358746,0.));
#211233=CARTESIAN_POINT('Ctrl Pts',(16.0736099723664,18.1228856358746,12.));
#211234=CARTESIAN_POINT('Ctrl Pts',(16.0936700829108,18.1330841933099,0.));
#211235=CARTESIAN_POINT('Ctrl Pts',(16.0936700829108,18.1330841933099,12.));
#211236=CARTESIAN_POINT('Ctrl Pts',(16.113840066279,18.1432743693231,0.));
#211237=CARTESIAN_POINT('Ctrl Pts',(16.113840066279,18.1432743693231,12.));
#211238=CARTESIAN_POINT('Ctrl Pts',(16.1341194882987,18.1534555549851,0.));
#211239=CARTESIAN_POINT('Ctrl Pts',(16.1341194882987,18.1534555549851,12.));
#211240=CARTESIAN_POINT('Ctrl Pts',(16.1545079178261,18.1636271481616,0.));
#211241=CARTESIAN_POINT('Ctrl Pts',(16.1545079178261,18.1636271481616,12.));
#211242=CARTESIAN_POINT('Ctrl Pts',(16.1750049266673,18.1737885533852,0.));
#211243=CARTESIAN_POINT('Ctrl Pts',(16.1750049266673,18.1737885533852,12.));
#211244=CARTESIAN_POINT('Ctrl Pts',(16.1956100895076,18.1839391817335,0.));
#211245=CARTESIAN_POINT('Ctrl Pts',(16.1956100895076,18.1839391817335,12.));
#211246=CARTESIAN_POINT('Ctrl Pts',(16.2163229838878,18.1940784507232,0.));
#211247=CARTESIAN_POINT('Ctrl Pts',(16.2163229838878,18.1940784507232,12.));
#211248=CARTESIAN_POINT('Ctrl Pts',(16.237143190164,18.2042057842037,0.));
#211249=CARTESIAN_POINT('Ctrl Pts',(16.237143190164,18.2042057842037,12.));
#211250=CARTESIAN_POINT('Ctrl Pts',(16.2580702914615,18.214320612253,0.));
#211251=CARTESIAN_POINT('Ctrl Pts',(16.2580702914615,18.214320612253,12.));
#211252=CARTESIAN_POINT('Ctrl Pts',(16.2791038736223,18.2244223710745,0.));
#211253=CARTESIAN_POINT('Ctrl Pts',(16.2791038736223,18.2244223710745,12.));
#211254=CARTESIAN_POINT('Ctrl Pts',(16.3002435251378,18.2345105028981,0.));
#211255=CARTESIAN_POINT('Ctrl Pts',(16.3002435251378,18.2345105028981,12.));
#211256=CARTESIAN_POINT('Ctrl Pts',(16.3214888370988,18.2445844558742,0.));
#211257=CARTESIAN_POINT('Ctrl Pts',(16.3214888370988,18.2445844558742,12.));
#211258=CARTESIAN_POINT('Ctrl Pts',(16.342839403159,18.2546436839609,0.));
#211259=CARTESIAN_POINT('Ctrl Pts',(16.342839403159,18.2546436839609,12.));
#211260=CARTESIAN_POINT('Ctrl Pts',(16.3642948194869,18.2646876468169,0.));
#211261=CARTESIAN_POINT('Ctrl Pts',(16.3642948194869,18.2646876468169,12.));
#211262=CARTESIAN_POINT('Ctrl Pts',(16.385854684708,18.2747158096934,0.));
#211263=CARTESIAN_POINT('Ctrl Pts',(16.385854684708,18.2747158096934,12.));
#211264=CARTESIAN_POINT('Ctrl Pts',(16.4075185998454,18.2847276433308,0.));
#211265=CARTESIAN_POINT('Ctrl Pts',(16.4075185998454,18.2847276433308,12.));
#211266=CARTESIAN_POINT('Ctrl Pts',(16.4292861682377,18.2947226238509,0.));
#211267=CARTESIAN_POINT('Ctrl Pts',(16.4292861682377,18.2947226238509,12.));
#211268=CARTESIAN_POINT('Ctrl Pts',(16.4511569955231,18.3047002326858,0.));
#211269=CARTESIAN_POINT('Ctrl Pts',(16.4511569955231,18.3047002326858,12.));
#211270=CARTESIAN_POINT('Ctrl Pts',(16.4731306896439,18.3146599565229,0.));
#211271=CARTESIAN_POINT('Ctrl Pts',(16.4731306896439,18.3146599565229,12.));
#211272=CARTESIAN_POINT('Ctrl Pts',(16.4952068608344,18.3246012872468,0.));
#211273=CARTESIAN_POINT('Ctrl Pts',(16.4952068608344,18.3246012872468,12.));
#211274=CARTESIAN_POINT('Ctrl Pts',(16.5173851216045,18.3345237218864,0.));
#211275=CARTESIAN_POINT('Ctrl Pts',(16.5173851216045,18.3345237218864,12.));
#211276=CARTESIAN_POINT('Ctrl Pts',(16.5396650867139,18.3444267625601,0.));
#211277=CARTESIAN_POINT('Ctrl Pts',(16.5396650867139,18.3444267625601,12.));
#211278=CARTESIAN_POINT('Ctrl Pts',(16.5620463731414,18.3543099164331,0.));
#211279=CARTESIAN_POINT('Ctrl Pts',(16.5620463731414,18.3543099164331,12.));
#211280=CARTESIAN_POINT('Ctrl Pts',(16.5845286000218,18.364172695589,0.));
#211281=CARTESIAN_POINT('Ctrl Pts',(16.5845286000218,18.364172695589,12.));
#211282=CARTESIAN_POINT('Ctrl Pts',(16.6071113885711,18.3740146168879,0.));
#211283=CARTESIAN_POINT('Ctrl Pts',(16.6071113885711,18.3740146168879,12.));
#211284=CARTESIAN_POINT('Ctrl Pts',(16.6297943620056,18.3838352018327,0.));
#211285=CARTESIAN_POINT('Ctrl Pts',(16.6297943620056,18.3838352018327,12.));
#211286=CARTESIAN_POINT('Ctrl Pts',(16.6525771454513,18.3936339764332,0.));
#211287=CARTESIAN_POINT('Ctrl Pts',(16.6525771454513,18.3936339764332,12.));
#211288=CARTESIAN_POINT('Ctrl Pts',(16.6754593658513,18.4034104710789,0.));
#211289=CARTESIAN_POINT('Ctrl Pts',(16.6754593658513,18.4034104710789,12.));
#211290=CARTESIAN_POINT('Ctrl Pts',(16.698440651849,18.413164220399,0.));
#211291=CARTESIAN_POINT('Ctrl Pts',(16.698440651849,18.413164220399,12.));
#211292=CARTESIAN_POINT('Ctrl Pts',(16.7215206338818,18.4228947633186,0.));
#211293=CARTESIAN_POINT('Ctrl Pts',(16.7215206338818,18.4228947633186,12.));
#211294=CARTESIAN_POINT('Ctrl Pts',(16.7446989442882,18.4326016431392,0.));
#211295=CARTESIAN_POINT('Ctrl Pts',(16.7446989442882,18.4326016431392,12.));
#211296=CARTESIAN_POINT('Ctrl Pts',(16.7679752173992,18.4422844076099,0.));
#211297=CARTESIAN_POINT('Ctrl Pts',(16.7679752173992,18.4422844076099,12.));
#211298=CARTESIAN_POINT('Ctrl Pts',(16.791349089629,18.4519426090124,0.));
#211299=CARTESIAN_POINT('Ctrl Pts',(16.791349089629,18.4519426090124,12.));
#211300=CARTESIAN_POINT('Ctrl Pts',(16.8148201995472,18.4615758042305,0.));
#211301=CARTESIAN_POINT('Ctrl Pts',(16.8148201995472,18.4615758042305,12.));
#211302=CARTESIAN_POINT('Ctrl Pts',(16.8383881879707,18.4711835548622,0.));
#211303=CARTESIAN_POINT('Ctrl Pts',(16.8383881879707,18.4711835548622,12.));
#211304=CARTESIAN_POINT('Ctrl Pts',(16.8620526977169,18.4807654268769,0.));
#211305=CARTESIAN_POINT('Ctrl Pts',(16.8620526977169,18.4807654268769,12.));
#211306=CARTESIAN_POINT('Ctrl Pts',(16.8858133733086,18.4903209902226,0.));
#211307=CARTESIAN_POINT('Ctrl Pts',(16.8858133733086,18.4903209902226,12.));
#211308=CARTESIAN_POINT('Ctrl Pts',(16.9096698606942,18.4998498184619,0.));
#211309=CARTESIAN_POINT('Ctrl Pts',(16.9096698606942,18.4998498184619,12.));
#211310=CARTESIAN_POINT('Ctrl Pts',(16.9336218069353,18.5093514883835,0.));
#211311=CARTESIAN_POINT('Ctrl Pts',(16.9336218069353,18.5093514883835,12.));
#211312=CARTESIAN_POINT('Ctrl Pts',(16.957668859934,18.518825579666,0.));
#211313=CARTESIAN_POINT('Ctrl Pts',(16.957668859934,18.518825579666,12.));
#211314=CARTESIAN_POINT('Ctrl Pts',(16.9818106680382,18.5282716744198,0.));
#211315=CARTESIAN_POINT('Ctrl Pts',(16.9818106680382,18.5282716744198,12.));
#211316=CARTESIAN_POINT('Ctrl Pts',(17.0060468805099,18.5376893576961,0.));
#211317=CARTESIAN_POINT('Ctrl Pts',(17.0060468805099,18.5376893576961,12.));
#211318=CARTESIAN_POINT('Ctrl Pts',(17.030377148174,18.5470782182089,0.));
#211319=CARTESIAN_POINT('Ctrl Pts',(17.030377148174,18.5470782182089,12.));
#211320=CARTESIAN_POINT('Ctrl Pts',(17.0548011239751,18.5564378489628,0.));
#211321=CARTESIAN_POINT('Ctrl Pts',(17.0548011239751,18.5564378489628,12.));
#211322=CARTESIAN_POINT('Ctrl Pts',(17.0793184636079,18.5657678479788,0.));
#211323=CARTESIAN_POINT('Ctrl Pts',(17.0793184636079,18.5657678479788,12.));
#211324=CARTESIAN_POINT('Ctrl Pts',(17.1039288260001,18.5750678188543,0.));
#211325=CARTESIAN_POINT('Ctrl Pts',(17.1039288260001,18.5750678188543,12.));
#211326=CARTESIAN_POINT('Ctrl Pts',(17.1286318741185,18.5843373717253,0.));
#211327=CARTESIAN_POINT('Ctrl Pts',(17.1286318741185,18.5843373717253,12.));
#211328=CARTESIAN_POINT('Ctrl Pts',(17.1534272741646,18.5935761222833,0.));
#211329=CARTESIAN_POINT('Ctrl Pts',(17.1534272741646,18.5935761222833,12.));
#211330=CARTESIAN_POINT('Ctrl Pts',(17.1783146940131,18.6027836898826,0.));
#211331=CARTESIAN_POINT('Ctrl Pts',(17.1783146940131,18.6027836898826,12.));
#211332=CARTESIAN_POINT('Ctrl Pts',(17.2032938019288,18.6119596959957,0.));
#211333=CARTESIAN_POINT('Ctrl Pts',(17.2032938019288,18.6119596959957,12.));
#211334=CARTESIAN_POINT('Ctrl Pts',(17.2283642650519,18.6211037624041,0.));
#211335=CARTESIAN_POINT('Ctrl Pts',(17.2283642650519,18.6211037624041,12.));
#211336=CARTESIAN_POINT('Ctrl Pts',(17.2535257482186,18.630215509794,0.));
#211337=CARTESIAN_POINT('Ctrl Pts',(17.2535257482186,18.630215509794,12.));
#211338=CARTESIAN_POINT('Ctrl Pts',(17.278777912021,18.639294555474,0.));
#211339=CARTESIAN_POINT('Ctrl Pts',(17.278777912021,18.639294555474,12.));
#211340=CARTESIAN_POINT('Ctrl Pts',(17.3041204135069,18.6483405141853,0.));
#211341=CARTESIAN_POINT('Ctrl Pts',(17.3041204135069,18.6483405141853,12.));
#211342=CARTESIAN_POINT('Ctrl Pts',(17.3295529098612,18.6573530024019,0.));
#211343=CARTESIAN_POINT('Ctrl Pts',(17.3295529098612,18.6573530024019,12.));
#211344=CARTESIAN_POINT('Ctrl Pts',(17.3550750612438,18.6663316416569,0.));
#211345=CARTESIAN_POINT('Ctrl Pts',(17.3550750612438,18.6663316416569,12.));
#211346=CARTESIAN_POINT('Ctrl Pts',(17.3806865340744,18.6752760624045,0.));
#211347=CARTESIAN_POINT('Ctrl Pts',(17.3806865340744,18.6752760624045,12.));
#211348=CARTESIAN_POINT('Ctrl Pts',(17.4063870038563,18.6841859073472,0.));
#211349=CARTESIAN_POINT('Ctrl Pts',(17.4063870038563,18.6841859073472,12.));
#211350=CARTESIAN_POINT('Ctrl Pts',(17.4321761588148,18.6930608357421,0.));
#211351=CARTESIAN_POINT('Ctrl Pts',(17.4321761588148,18.6930608357421,12.));
#211352=CARTESIAN_POINT('Ctrl Pts',(17.4580537012764,18.7019005250322,0.));
#211353=CARTESIAN_POINT('Ctrl Pts',(17.4580537012764,18.7019005250322,12.));
#211354=CARTESIAN_POINT('Ctrl Pts',(17.4840193397176,18.7107046613941,0.));
#211355=CARTESIAN_POINT('Ctrl Pts',(17.4840193397176,18.7107046613941,12.));
#211356=CARTESIAN_POINT('Ctrl Pts',(17.5100727820891,18.7194729318128,0.));
#211357=CARTESIAN_POINT('Ctrl Pts',(17.5100727820891,18.7194729318128,12.));
#211358=CARTESIAN_POINT('Ctrl Pts',(17.5362137287604,18.728205015716,0.));
#211359=CARTESIAN_POINT('Ctrl Pts',(17.5362137287604,18.728205015716,12.));
#211360=CARTESIAN_POINT('Ctrl Pts',(17.5624418653248,18.7369005764558,0.));
#211361=CARTESIAN_POINT('Ctrl Pts',(17.5624418653248,18.7369005764558,12.));
#211362=CARTESIAN_POINT('Ctrl Pts',(17.5887568561361,18.7455592536667,0.));
#211363=CARTESIAN_POINT('Ctrl Pts',(17.5887568561361,18.7455592536667,12.));
#211364=CARTESIAN_POINT('Ctrl Pts',(17.6151583356988,18.7541806530935,0.));
#211365=CARTESIAN_POINT('Ctrl Pts',(17.6151583356988,18.7541806530935,12.));
#211366=CARTESIAN_POINT('Ctrl Pts',(17.6416459210646,18.7627643613139,0.));
#211367=CARTESIAN_POINT('Ctrl Pts',(17.6416459210646,18.7627643613139,12.));
#211368=CARTESIAN_POINT('Ctrl Pts',(17.6682192274197,18.7713099642673,0.));
#211369=CARTESIAN_POINT('Ctrl Pts',(17.6682192274197,18.7713099642673,12.));
#211370=CARTESIAN_POINT('Ctrl Pts',(17.6948778822981,18.7798170641305,0.));
#211371=CARTESIAN_POINT('Ctrl Pts',(17.6948778822981,18.7798170641305,12.));
#211372=CARTESIAN_POINT('Ctrl Pts',(17.7216215409019,18.7882852976016,0.));
#211373=CARTESIAN_POINT('Ctrl Pts',(17.7216215409019,18.7882852976016,12.));
#211374=CARTESIAN_POINT('Ctrl Pts',(17.7484498996916,18.7967143519444,0.));
#211375=CARTESIAN_POINT('Ctrl Pts',(17.7484498996916,18.7967143519444,12.));
#211376=CARTESIAN_POINT('Ctrl Pts',(17.7753627137898,18.8051039860543,0.));
#211377=CARTESIAN_POINT('Ctrl Pts',(17.7753627137898,18.8051039860543,12.));
#211378=CARTESIAN_POINT('Ctrl Pts',(17.8023598011135,18.8134540340581,0.));
#211379=CARTESIAN_POINT('Ctrl Pts',(17.8023598011135,18.8134540340581,12.));
#211380=CARTESIAN_POINT('Ctrl Pts',(17.8294410311105,18.8217643886368,0.));
#211381=CARTESIAN_POINT('Ctrl Pts',(17.8294410311105,18.8217643886368,12.));
#211382=CARTESIAN_POINT('Ctrl Pts',(17.8566063174871,18.8300349896187,0.));
#211383=CARTESIAN_POINT('Ctrl Pts',(17.8566063174871,18.8300349896187,12.));
#211384=CARTESIAN_POINT('Ctrl Pts',(17.8784057509434,18.8366196462746,0.));
#211385=CARTESIAN_POINT('Ctrl Pts',(17.8784057509434,18.8366196462746,12.));
#211386=CARTESIAN_POINT('Ctrl Pts',(17.8947931177853,18.8415402351882,0.));
#211387=CARTESIAN_POINT('Ctrl Pts',(17.8947931177853,18.8415402351882,12.));
#211388=CARTESIAN_POINT('Ctrl Pts',(17.9057348246611,18.8448126709726,0.));
#211389=CARTESIAN_POINT('Ctrl Pts',(17.9057348246611,18.8448126709726,12.));
#211390=CARTESIAN_POINT('Ctrl Pts',(17.9112098770111,18.8464468996588,0.));
#211391=CARTESIAN_POINT('Ctrl Pts',(17.9112098770111,18.8464468996588,12.));
#211392=CARTESIAN_POINT('',(17.9112098770111,18.8464468996588,0.));
#211393=CARTESIAN_POINT('Ctrl Pts',(14.6513681262571,17.1452095830633,0.));
#211394=CARTESIAN_POINT('Ctrl Pts',(14.6513711852843,17.1452153999142,0.));
#211395=CARTESIAN_POINT('Ctrl Pts',(14.6514066997196,17.1452600887037,0.));
#211396=CARTESIAN_POINT('Ctrl Pts',(14.6515481598068,17.1454262858043,0.));
#211397=CARTESIAN_POINT('Ctrl Pts',(14.6519131634508,17.1458462295271,0.));
#211398=CARTESIAN_POINT('Ctrl Pts',(14.6526624064978,17.1466998098673,0.));
#211399=CARTESIAN_POINT('Ctrl Pts',(14.6537016966184,17.147876394491,0.));
#211400=CARTESIAN_POINT('Ctrl Pts',(14.655024862281,17.1493641837558,0.));
#211401=CARTESIAN_POINT('Ctrl Pts',(14.6566237952435,17.1511476869496,0.));
#211402=CARTESIAN_POINT('Ctrl Pts',(14.6584900555302,17.1532107762718,0.));
#211403=CARTESIAN_POINT('Ctrl Pts',(14.6606167169642,17.1555401986401,0.));
#211404=CARTESIAN_POINT('Ctrl Pts',(14.6629987285992,17.1581262646789,0.));
#211405=CARTESIAN_POINT('Ctrl Pts',(14.6656319165057,17.1609609517369,0.));
#211406=CARTESIAN_POINT('Ctrl Pts',(14.6685123374423,17.1640366762305,0.));
#211407=CARTESIAN_POINT('Ctrl Pts',(14.671635583332,17.167344972302,0.));
#211408=CARTESIAN_POINT('Ctrl Pts',(14.6749971333867,17.1708771619129,0.));
#211409=CARTESIAN_POINT('Ctrl Pts',(14.6785925615677,17.1746247499057,0.));
#211410=CARTESIAN_POINT('Ctrl Pts',(14.6824178576167,17.1785800350826,0.));
#211411=CARTESIAN_POINT('Ctrl Pts',(14.686469452232,17.182736158472,0.));
#211412=CARTESIAN_POINT('Ctrl Pts',(14.6907440526958,17.1870867909918,0.));
#211413=CARTESIAN_POINT('Ctrl Pts',(14.6952385361705,17.1916259308415,0.));
#211414=CARTESIAN_POINT('Ctrl Pts',(14.699949811582,17.1963476411694,0.));
#211415=CARTESIAN_POINT('Ctrl Pts',(14.7048748502663,17.2012461084268,0.));
#211416=CARTESIAN_POINT('Ctrl Pts',(14.7100107213586,17.2063157097315,0.));
#211417=CARTESIAN_POINT('Ctrl Pts',(14.7153546289339,17.2115510835989,0.));
#211418=CARTESIAN_POINT('Ctrl Pts',(14.7209039390327,17.2169471814256,0.));
#211419=CARTESIAN_POINT('Ctrl Pts',(14.7266561494282,17.2224992099667,0.));
#211420=CARTESIAN_POINT('Ctrl Pts',(14.7326088681163,17.2282025904314,0.));
#211421=CARTESIAN_POINT('Ctrl Pts',(14.7387597858116,17.2340529062076,0.));
#211422=CARTESIAN_POINT('Ctrl Pts',(14.7451066593792,17.2400458713565,0.));
#211423=CARTESIAN_POINT('Ctrl Pts',(14.7516473175124,17.2461773413288,0.));
#211424=CARTESIAN_POINT('Ctrl Pts',(14.7583796616617,17.2524433146837,0.));
#211425=CARTESIAN_POINT('Ctrl Pts',(14.7653016697591,17.2588399401465,0.));
#211426=CARTESIAN_POINT('Ctrl Pts',(14.7724113956731,17.2653635155319,0.));
#211427=CARTESIAN_POINT('Ctrl Pts',(14.7797069617804,17.2720104735194,0.));
#211428=CARTESIAN_POINT('Ctrl Pts',(14.787186553128,17.2787773704849,0.));
#211429=CARTESIAN_POINT('Ctrl Pts',(14.7948484105249,17.2856608733196,0.));
#211430=CARTESIAN_POINT('Ctrl Pts',(14.8026908254276,17.2926577496513,0.));
#211431=CARTESIAN_POINT('Ctrl Pts',(14.8107121391035,17.299764866148,0.));
#211432=CARTESIAN_POINT('Ctrl Pts',(14.8189107410162,17.3069791853706,0.));
#211433=CARTESIAN_POINT('Ctrl Pts',(14.8272850675379,17.3142977632659,0.));
#211434=CARTESIAN_POINT('Ctrl Pts',(14.8358336004197,17.3217177462101,0.));
#211435=CARTESIAN_POINT('Ctrl Pts',(14.8445548643508,17.3292363662605,0.));
#211436=CARTESIAN_POINT('Ctrl Pts',(14.8534474245433,17.336850936485,0.));
#211437=CARTESIAN_POINT('Ctrl Pts',(14.8625098843417,17.3445588463475,0.));
#211438=CARTESIAN_POINT('Ctrl Pts',(14.8717408826955,17.3523575568645,0.));
#211439=CARTESIAN_POINT('Ctrl Pts',(14.8811390927423,17.3602445978161,0.));
#211440=CARTESIAN_POINT('Ctrl Pts',(14.8907032205788,17.3682175653235,0.));
#211441=CARTESIAN_POINT('Ctrl Pts',(14.900432003961,17.3762741193076,0.));
#211442=CARTESIAN_POINT('Ctrl Pts',(14.9103242110057,17.3844119809824,0.));
#211443=CARTESIAN_POINT('Ctrl Pts',(14.9203786389342,17.3926289303986,0.));
#211444=CARTESIAN_POINT('Ctrl Pts',(14.9305941128757,17.4009228040749,0.));
#211445=CARTESIAN_POINT('Ctrl Pts',(14.940969484645,17.4092914926071,0.));
#211446=CARTESIAN_POINT('Ctrl Pts',(14.9515036315143,17.4177329382828,0.));
#211447=CARTESIAN_POINT('Ctrl Pts',(14.9621954549827,17.426245132709,0.));
#211448=CARTESIAN_POINT('Ctrl Pts',(14.9730438799452,17.4348261151396,0.));
#211449=CARTESIAN_POINT('Ctrl Pts',(14.9840478538358,17.4434739707773,0.));
#211450=CARTESIAN_POINT('Ctrl Pts',(14.9952063457778,17.4521868291004,0.));
#211451=CARTESIAN_POINT('Ctrl Pts',(15.0065183456921,17.4609628621418,0.));
#211452=CARTESIAN_POINT('Ctrl Pts',(15.0179828635086,17.4698002829357,0.));
#211453=CARTESIAN_POINT('Ctrl Pts',(15.029598928488,17.4786973441417,0.));
#211454=CARTESIAN_POINT('Ctrl Pts',(15.0413655884993,17.4876523366178,0.));
#211455=CARTESIAN_POINT('Ctrl Pts',(15.0532819093085,17.4966635880245,0.));
#211456=CARTESIAN_POINT('Ctrl Pts',(15.0653469738306,17.5057294613874,0.));
#211457=CARTESIAN_POINT('Ctrl Pts',(15.0775598815748,17.5148483539684,0.));
#211458=CARTESIAN_POINT('Ctrl Pts',(15.0899197481082,17.5240186961788,0.));
#211459=CARTESIAN_POINT('Ctrl Pts',(15.1024257045033,17.5332389504829,0.));
#211460=CARTESIAN_POINT('Ctrl Pts',(15.1150768967729,17.5425076102966,0.));
#211461=CARTESIAN_POINT('Ctrl Pts',(15.127872485314,17.5518231989122,0.));
#211462=CARTESIAN_POINT('Ctrl Pts',(15.1408116444877,17.5611842686196,0.));
#211463=CARTESIAN_POINT('Ctrl Pts',(15.1538935621714,17.570589399803,0.));
#211464=CARTESIAN_POINT('Ctrl Pts',(15.1671174393136,17.5800372000539,0.));
#211465=CARTESIAN_POINT('Ctrl Pts',(15.1804824894605,17.5895263032592,0.));
#211466=CARTESIAN_POINT('Ctrl Pts',(15.1939879383268,17.5990553687595,0.));
#211467=CARTESIAN_POINT('Ctrl Pts',(15.2076330234686,17.6086230806497,0.));
#211468=CARTESIAN_POINT('Ctrl Pts',(15.22141699392,17.6182281470467,0.));
#211469=CARTESIAN_POINT('Ctrl Pts',(15.2353391098367,17.6278692993765,0.));
#211470=CARTESIAN_POINT('Ctrl Pts',(15.2493986421091,17.637545291637,0.));
#211471=CARTESIAN_POINT('Ctrl Pts',(15.263594872029,17.6472548997329,0.));
#211472=CARTESIAN_POINT('Ctrl Pts',(15.2779270910238,17.6569969209,0.));
#211473=CARTESIAN_POINT('Ctrl Pts',(15.2923946003598,17.6667701731041,0.));
#211474=CARTESIAN_POINT('Ctrl Pts',(15.3069967108501,17.6765734944559,0.));
#211475=CARTESIAN_POINT('Ctrl Pts',(15.3217327425341,17.6864057426052,0.));
#211476=CARTESIAN_POINT('Ctrl Pts',(15.3366020244069,17.6962657941984,0.));
#211477=CARTESIAN_POINT('Ctrl Pts',(15.3516038942064,17.7061525444044,0.));
#211478=CARTESIAN_POINT('Ctrl Pts',(15.3667376981702,17.7160649064208,0.));
#211479=CARTESIAN_POINT('Ctrl Pts',(15.3820027907965,17.7260018109923,0.));
#211480=CARTESIAN_POINT('Ctrl Pts',(15.3973985345796,17.7359622059143,0.));
#211481=CARTESIAN_POINT('Ctrl Pts',(15.4129242997828,17.7459450555803,0.));
#211482=CARTESIAN_POINT('Ctrl Pts',(15.4285794642658,17.7559493405871,0.));
#211483=CARTESIAN_POINT('Ctrl Pts',(15.4443634132865,17.765974057326,0.));
#211484=CARTESIAN_POINT('Ctrl Pts',(15.4602755393019,17.7760182175817,0.));
#211485=CARTESIAN_POINT('Ctrl Pts',(15.4763152417506,17.7860808481229,0.));
#211486=CARTESIAN_POINT('Ctrl Pts',(15.4924819268529,17.7961609903161,0.));
#211487=CARTESIAN_POINT('Ctrl Pts',(15.5087750074728,17.8062576997964,0.));
#211488=CARTESIAN_POINT('Ctrl Pts',(15.5251939029558,17.8163700461263,0.));
#211489=CARTESIAN_POINT('Ctrl Pts',(15.5417380389639,17.8264971124606,0.));
#211490=CARTESIAN_POINT('Ctrl Pts',(15.5584068472976,17.8366379952078,0.));
#211491=CARTESIAN_POINT('Ctrl Pts',(15.5751997657153,17.8467918036977,0.));
#211492=CARTESIAN_POINT('Ctrl Pts',(15.5921162378183,17.8569576598996,0.));
#211493=CARTESIAN_POINT('Ctrl Pts',(15.6091557129205,17.8671346981388,0.));
#211494=CARTESIAN_POINT('Ctrl Pts',(15.6263176459107,17.8773220648125,0.));
#211495=CARTESIAN_POINT('Ctrl Pts',(15.6436014971088,17.8875189181095,0.));
#211496=CARTESIAN_POINT('Ctrl Pts',(15.6610067321036,17.8977244277247,0.));
#211497=CARTESIAN_POINT('Ctrl Pts',(15.6785328216467,17.9079377746118,0.));
#211498=CARTESIAN_POINT('Ctrl Pts',(15.6961792415526,17.918158150746,0.));
#211499=CARTESIAN_POINT('Ctrl Pts',(15.713945472584,17.9283847588837,0.));
#211500=CARTESIAN_POINT('Ctrl Pts',(15.7318310003334,17.9386168123261,0.));
#211501=CARTESIAN_POINT('Ctrl Pts',(15.7498353150856,17.9488535346776,0.));
#211502=CARTESIAN_POINT('Ctrl Pts',(15.7679579117072,17.9590941596236,0.));
#211503=CARTESIAN_POINT('Ctrl Pts',(15.786198289572,17.9693379307297,0.));
#211504=CARTESIAN_POINT('Ctrl Pts',(15.8045559524674,17.9795841012383,0.));
#211505=CARTESIAN_POINT('Ctrl Pts',(15.8230304084963,17.9898319338664,0.));
#211506=CARTESIAN_POINT('Ctrl Pts',(15.8416211699681,18.0000807006055,0.));
#211507=CARTESIAN_POINT('Ctrl Pts',(15.8603277532834,18.010329682521,0.));
#211508=CARTESIAN_POINT('Ctrl Pts',(15.8791496788685,18.0205781695773,0.));
#211509=CARTESIAN_POINT('Ctrl Pts',(15.8980864711043,18.0308254604638,0.));
#211510=CARTESIAN_POINT('Ctrl Pts',(15.9171376582436,18.0410708624208,0.));
#211511=CARTESIAN_POINT('Ctrl Pts',(15.9363027723244,18.0513136910691,0.));
#211512=CARTESIAN_POINT('Ctrl Pts',(15.9555813490645,18.061553270236,0.));
#211513=CARTESIAN_POINT('Ctrl Pts',(15.9749729277848,18.071788931796,0.));
#211514=CARTESIAN_POINT('Ctrl Pts',(15.9944770513616,18.0820200155239,0.));
#211515=CARTESIAN_POINT('Ctrl Pts',(16.0140932661612,18.0922458689464,0.));
#211516=CARTESIAN_POINT('Ctrl Pts',(16.0338211219693,18.1024658471966,0.));
#211517=CARTESIAN_POINT('Ctrl Pts',(16.0536601719124,18.1126793128688,0.));
#211518=CARTESIAN_POINT('Ctrl Pts',(16.0736099723664,18.1228856358746,0.));
#211519=CARTESIAN_POINT('Ctrl Pts',(16.0936700829108,18.1330841933099,0.));
#211520=CARTESIAN_POINT('Ctrl Pts',(16.113840066279,18.1432743693231,0.));
#211521=CARTESIAN_POINT('Ctrl Pts',(16.1341194882987,18.1534555549851,0.));
#211522=CARTESIAN_POINT('Ctrl Pts',(16.1545079178261,18.1636271481616,0.));
#211523=CARTESIAN_POINT('Ctrl Pts',(16.1750049266673,18.1737885533852,0.));
#211524=CARTESIAN_POINT('Ctrl Pts',(16.1956100895076,18.1839391817335,0.));
#211525=CARTESIAN_POINT('Ctrl Pts',(16.2163229838878,18.1940784507232,0.));
#211526=CARTESIAN_POINT('Ctrl Pts',(16.237143190164,18.2042057842037,0.));
#211527=CARTESIAN_POINT('Ctrl Pts',(16.2580702914615,18.214320612253,0.));
#211528=CARTESIAN_POINT('Ctrl Pts',(16.2791038736223,18.2244223710745,0.));
#211529=CARTESIAN_POINT('Ctrl Pts',(16.3002435251378,18.2345105028981,0.));
#211530=CARTESIAN_POINT('Ctrl Pts',(16.3214888370988,18.2445844558742,0.));
#211531=CARTESIAN_POINT('Ctrl Pts',(16.342839403159,18.2546436839609,0.));
#211532=CARTESIAN_POINT('Ctrl Pts',(16.3642948194869,18.2646876468169,0.));
#211533=CARTESIAN_POINT('Ctrl Pts',(16.385854684708,18.2747158096934,0.));
#211534=CARTESIAN_POINT('Ctrl Pts',(16.4075185998454,18.2847276433308,0.));
#211535=CARTESIAN_POINT('Ctrl Pts',(16.4292861682377,18.2947226238509,0.));
#211536=CARTESIAN_POINT('Ctrl Pts',(16.4511569955231,18.3047002326858,0.));
#211537=CARTESIAN_POINT('Ctrl Pts',(16.4731306896439,18.3146599565229,0.));
#211538=CARTESIAN_POINT('Ctrl Pts',(16.4952068608344,18.3246012872468,0.));
#211539=CARTESIAN_POINT('Ctrl Pts',(16.5173851216045,18.3345237218864,0.));
#211540=CARTESIAN_POINT('Ctrl Pts',(16.5396650867139,18.3444267625601,0.));
#211541=CARTESIAN_POINT('Ctrl Pts',(16.5620463731414,18.3543099164331,0.));
#211542=CARTESIAN_POINT('Ctrl Pts',(16.5845286000218,18.364172695589,0.));
#211543=CARTESIAN_POINT('Ctrl Pts',(16.6071113885711,18.3740146168879,0.));
#211544=CARTESIAN_POINT('Ctrl Pts',(16.6297943620056,18.3838352018327,0.));
#211545=CARTESIAN_POINT('Ctrl Pts',(16.6525771454513,18.3936339764332,0.));
#211546=CARTESIAN_POINT('Ctrl Pts',(16.6754593658513,18.4034104710789,0.));
#211547=CARTESIAN_POINT('Ctrl Pts',(16.698440651849,18.413164220399,0.));
#211548=CARTESIAN_POINT('Ctrl Pts',(16.7215206338818,18.4228947633186,0.));
#211549=CARTESIAN_POINT('Ctrl Pts',(16.7446989442882,18.4326016431392,0.));
#211550=CARTESIAN_POINT('Ctrl Pts',(16.7679752173992,18.4422844076099,0.));
#211551=CARTESIAN_POINT('Ctrl Pts',(16.791349089629,18.4519426090124,0.));
#211552=CARTESIAN_POINT('Ctrl Pts',(16.8148201995472,18.4615758042305,0.));
#211553=CARTESIAN_POINT('Ctrl Pts',(16.8383881879707,18.4711835548622,0.));
#211554=CARTESIAN_POINT('Ctrl Pts',(16.8620526977169,18.4807654268769,0.));
#211555=CARTESIAN_POINT('Ctrl Pts',(16.8858133733086,18.4903209902226,0.));
#211556=CARTESIAN_POINT('Ctrl Pts',(16.9096698606942,18.4998498184619,0.));
#211557=CARTESIAN_POINT('Ctrl Pts',(16.9336218069353,18.5093514883835,0.));
#211558=CARTESIAN_POINT('Ctrl Pts',(16.957668859934,18.518825579666,0.));
#211559=CARTESIAN_POINT('Ctrl Pts',(16.9818106680382,18.5282716744198,0.));
#211560=CARTESIAN_POINT('Ctrl Pts',(17.0060468805099,18.5376893576961,0.));
#211561=CARTESIAN_POINT('Ctrl Pts',(17.030377148174,18.5470782182089,0.));
#211562=CARTESIAN_POINT('Ctrl Pts',(17.0548011239751,18.5564378489628,0.));
#211563=CARTESIAN_POINT('Ctrl Pts',(17.0793184636079,18.5657678479788,0.));
#211564=CARTESIAN_POINT('Ctrl Pts',(17.1039288260001,18.5750678188543,0.));
#211565=CARTESIAN_POINT('Ctrl Pts',(17.1286318741185,18.5843373717253,0.));
#211566=CARTESIAN_POINT('Ctrl Pts',(17.1534272741646,18.5935761222833,0.));
#211567=CARTESIAN_POINT('Ctrl Pts',(17.1783146940131,18.6027836898826,0.));
#211568=CARTESIAN_POINT('Ctrl Pts',(17.2032938019288,18.6119596959957,0.));
#211569=CARTESIAN_POINT('Ctrl Pts',(17.2283642650519,18.6211037624041,0.));
#211570=CARTESIAN_POINT('Ctrl Pts',(17.2535257482186,18.630215509794,0.));
#211571=CARTESIAN_POINT('Ctrl Pts',(17.278777912021,18.639294555474,0.));
#211572=CARTESIAN_POINT('Ctrl Pts',(17.3041204135069,18.6483405141853,0.));
#211573=CARTESIAN_POINT('Ctrl Pts',(17.3295529098612,18.6573530024019,0.));
#211574=CARTESIAN_POINT('Ctrl Pts',(17.3550750612438,18.6663316416569,0.));
#211575=CARTESIAN_POINT('Ctrl Pts',(17.3806865340744,18.6752760624045,0.));
#211576=CARTESIAN_POINT('Ctrl Pts',(17.4063870038563,18.6841859073472,0.));
#211577=CARTESIAN_POINT('Ctrl Pts',(17.4321761588148,18.6930608357421,0.));
#211578=CARTESIAN_POINT('Ctrl Pts',(17.4580537012764,18.7019005250322,0.));
#211579=CARTESIAN_POINT('Ctrl Pts',(17.4840193397176,18.7107046613941,0.));
#211580=CARTESIAN_POINT('Ctrl Pts',(17.5100727820891,18.7194729318128,0.));
#211581=CARTESIAN_POINT('Ctrl Pts',(17.5362137287604,18.728205015716,0.));
#211582=CARTESIAN_POINT('Ctrl Pts',(17.5624418653248,18.7369005764558,0.));
#211583=CARTESIAN_POINT('Ctrl Pts',(17.5887568561361,18.7455592536667,0.));
#211584=CARTESIAN_POINT('Ctrl Pts',(17.6151583356988,18.7541806530935,0.));
#211585=CARTESIAN_POINT('Ctrl Pts',(17.6416459210646,18.7627643613139,0.));
#211586=CARTESIAN_POINT('Ctrl Pts',(17.6682192274197,18.7713099642673,0.));
#211587=CARTESIAN_POINT('Ctrl Pts',(17.6948778822981,18.7798170641305,0.));
#211588=CARTESIAN_POINT('Ctrl Pts',(17.7216215409019,18.7882852976016,0.));
#211589=CARTESIAN_POINT('Ctrl Pts',(17.7484498996916,18.7967143519444,0.));
#211590=CARTESIAN_POINT('Ctrl Pts',(17.7753627137898,18.8051039860543,0.));
#211591=CARTESIAN_POINT('Ctrl Pts',(17.8023598011135,18.8134540340581,0.));
#211592=CARTESIAN_POINT('Ctrl Pts',(17.8294410311105,18.8217643886368,0.));
#211593=CARTESIAN_POINT('Ctrl Pts',(17.8566063174871,18.8300349896187,0.));
#211594=CARTESIAN_POINT('Ctrl Pts',(17.8784057509434,18.8366196462746,0.));
#211595=CARTESIAN_POINT('Ctrl Pts',(17.8947931177853,18.8415402351882,0.));
#211596=CARTESIAN_POINT('Ctrl Pts',(17.9057348246611,18.8448126709726,0.));
#211597=CARTESIAN_POINT('Ctrl Pts',(17.9112098770111,18.8464468996588,0.));
#211598=CARTESIAN_POINT('',(17.9112098770111,18.8464468996588,0.));
#211599=CARTESIAN_POINT('Origin',(17.7219872369693,12.1729687575668,0.));
#211600=CARTESIAN_POINT('',(18.5896416359912,12.7689476255363,0.));
#211601=CARTESIAN_POINT('',(18.5896416359912,12.7689476255363,0.));
#211602=CARTESIAN_POINT('',(8.86099361848466,6.08648437878338,0.));
#211603=CARTESIAN_POINT('Ctrl Pts',(18.8464468996588,17.9112098770111,0.));
#211604=CARTESIAN_POINT('Ctrl Pts',(18.8464468996588,17.9112098770111,12.));
#211605=CARTESIAN_POINT('Ctrl Pts',(18.8448126709691,17.9057348246595,0.));
#211606=CARTESIAN_POINT('Ctrl Pts',(18.8448126709691,17.9057348246595,12.));
#211607=CARTESIAN_POINT('Ctrl Pts',(18.8415402351786,17.8947931177807,0.));
#211608=CARTESIAN_POINT('Ctrl Pts',(18.8415402351786,17.8947931177807,12.));
#211609=CARTESIAN_POINT('Ctrl Pts',(18.8366196462581,17.8784057509356,0.));
#211610=CARTESIAN_POINT('Ctrl Pts',(18.8366196462581,17.8784057509356,12.));
#211611=CARTESIAN_POINT('Ctrl Pts',(18.8300349895974,17.8566063174771,0.));
#211612=CARTESIAN_POINT('Ctrl Pts',(18.8300349895974,17.8566063174771,12.));
#211613=CARTESIAN_POINT('Ctrl Pts',(18.8217643886157,17.8294410311006,0.));
#211614=CARTESIAN_POINT('Ctrl Pts',(18.8217643886157,17.8294410311006,12.));
#211615=CARTESIAN_POINT('Ctrl Pts',(18.8134540340417,17.8023598011057,0.));
#211616=CARTESIAN_POINT('Ctrl Pts',(18.8134540340417,17.8023598011057,12.));
#211617=CARTESIAN_POINT('Ctrl Pts',(18.8051039860448,17.7753627137853,0.));
#211618=CARTESIAN_POINT('Ctrl Pts',(18.8051039860448,17.7753627137853,12.));
#211619=CARTESIAN_POINT('Ctrl Pts',(18.7967143519419,17.7484498996905,0.));
#211620=CARTESIAN_POINT('Ctrl Pts',(18.7967143519419,17.7484498996905,12.));
#211621=CARTESIAN_POINT('Ctrl Pts',(18.7882852976049,17.7216215409035,0.));
#211622=CARTESIAN_POINT('Ctrl Pts',(18.7882852976049,17.7216215409035,12.));
#211623=CARTESIAN_POINT('Ctrl Pts',(18.7798170641374,17.6948778823014,0.));
#211624=CARTESIAN_POINT('Ctrl Pts',(18.7798170641374,17.6948778823014,12.));
#211625=CARTESIAN_POINT('Ctrl Pts',(18.7713099642754,17.6682192274236,0.));
#211626=CARTESIAN_POINT('Ctrl Pts',(18.7713099642754,17.6682192274236,12.));
#211627=CARTESIAN_POINT('Ctrl Pts',(18.762764361321,17.6416459210681,0.));
#211628=CARTESIAN_POINT('Ctrl Pts',(18.762764361321,17.6416459210681,12.));
#211629=CARTESIAN_POINT('Ctrl Pts',(18.7541806530984,17.6151583357012,0.));
#211630=CARTESIAN_POINT('Ctrl Pts',(18.7541806530984,17.6151583357012,12.));
#211631=CARTESIAN_POINT('Ctrl Pts',(18.7455592536687,17.5887568561371,0.));
#211632=CARTESIAN_POINT('Ctrl Pts',(18.7455592536687,17.5887568561371,12.));
#211633=CARTESIAN_POINT('Ctrl Pts',(18.7369005764553,17.5624418653245,0.));
#211634=CARTESIAN_POINT('Ctrl Pts',(18.7369005764553,17.5624418653245,12.));
#211635=CARTESIAN_POINT('Ctrl Pts',(18.7282050157138,17.5362137287593,0.));
#211636=CARTESIAN_POINT('Ctrl Pts',(18.7282050157138,17.5362137287593,12.));
#211637=CARTESIAN_POINT('Ctrl Pts',(18.7194729318098,17.5100727820876,0.));
#211638=CARTESIAN_POINT('Ctrl Pts',(18.7194729318098,17.5100727820876,12.));
#211639=CARTESIAN_POINT('Ctrl Pts',(18.7107046613912,17.4840193397162,0.));
#211640=CARTESIAN_POINT('Ctrl Pts',(18.7107046613912,17.4840193397162,12.));
#211641=CARTESIAN_POINT('Ctrl Pts',(18.70190052503,17.4580537012753,0.));
#211642=CARTESIAN_POINT('Ctrl Pts',(18.70190052503,17.4580537012753,12.));
#211643=CARTESIAN_POINT('Ctrl Pts',(18.6930608357409,17.4321761588142,0.));
#211644=CARTESIAN_POINT('Ctrl Pts',(18.6930608357409,17.4321761588142,12.));
#211645=CARTESIAN_POINT('Ctrl Pts',(18.6841859073471,17.4063870038562,0.));
#211646=CARTESIAN_POINT('Ctrl Pts',(18.6841859073471,17.4063870038562,12.));
#211647=CARTESIAN_POINT('Ctrl Pts',(18.6752760624052,17.3806865340747,0.));
#211648=CARTESIAN_POINT('Ctrl Pts',(18.6752760624052,17.3806865340747,12.));
#211649=CARTESIAN_POINT('Ctrl Pts',(18.6663316416582,17.3550750612443,0.));
#211650=CARTESIAN_POINT('Ctrl Pts',(18.6663316416582,17.3550750612443,12.));
#211651=CARTESIAN_POINT('Ctrl Pts',(18.6573530024033,17.3295529098618,0.));
#211652=CARTESIAN_POINT('Ctrl Pts',(18.6573530024033,17.3295529098618,12.));
#211653=CARTESIAN_POINT('Ctrl Pts',(18.6483405141865,17.3041204135074,0.));
#211654=CARTESIAN_POINT('Ctrl Pts',(18.6483405141865,17.3041204135074,12.));
#211655=CARTESIAN_POINT('Ctrl Pts',(18.6392945554748,17.2787779120213,0.));
#211656=CARTESIAN_POINT('Ctrl Pts',(18.6392945554748,17.2787779120213,12.));
#211657=CARTESIAN_POINT('Ctrl Pts',(18.6302155097943,17.2535257482187,0.));
#211658=CARTESIAN_POINT('Ctrl Pts',(18.6302155097943,17.2535257482187,12.));
#211659=CARTESIAN_POINT('Ctrl Pts',(18.6211037624038,17.2283642650518,0.));
#211660=CARTESIAN_POINT('Ctrl Pts',(18.6211037624038,17.2283642650518,12.));
#211661=CARTESIAN_POINT('Ctrl Pts',(18.6119596959949,17.2032938019284,0.));
#211662=CARTESIAN_POINT('Ctrl Pts',(18.6119596959949,17.2032938019284,12.));
#211663=CARTESIAN_POINT('Ctrl Pts',(18.6027836898817,17.1783146940127,0.));
#211664=CARTESIAN_POINT('Ctrl Pts',(18.6027836898817,17.1783146940127,12.));
#211665=CARTESIAN_POINT('Ctrl Pts',(18.5935761222825,17.1534272741643,0.));
#211666=CARTESIAN_POINT('Ctrl Pts',(18.5935761222825,17.1534272741643,12.));
#211667=CARTESIAN_POINT('Ctrl Pts',(18.5843373717247,17.1286318741183,0.));
#211668=CARTESIAN_POINT('Ctrl Pts',(18.5843373717247,17.1286318741183,12.));
#211669=CARTESIAN_POINT('Ctrl Pts',(18.5750678188542,17.1039288260001,0.));
#211670=CARTESIAN_POINT('Ctrl Pts',(18.5750678188542,17.1039288260001,12.));
#211671=CARTESIAN_POINT('Ctrl Pts',(18.5657678479789,17.0793184636079,0.));
#211672=CARTESIAN_POINT('Ctrl Pts',(18.5657678479789,17.0793184636079,12.));
#211673=CARTESIAN_POINT('Ctrl Pts',(18.556437848963,17.0548011239751,0.));
#211674=CARTESIAN_POINT('Ctrl Pts',(18.556437848963,17.0548011239751,12.));
#211675=CARTESIAN_POINT('Ctrl Pts',(18.547078218209,17.0303771481738,0.));
#211676=CARTESIAN_POINT('Ctrl Pts',(18.547078218209,17.0303771481738,12.));
#211677=CARTESIAN_POINT('Ctrl Pts',(18.5376893576961,17.0060468805097,0.));
#211678=CARTESIAN_POINT('Ctrl Pts',(18.5376893576961,17.0060468805097,12.));
#211679=CARTESIAN_POINT('Ctrl Pts',(18.5282716744197,16.981810668038,0.));
#211680=CARTESIAN_POINT('Ctrl Pts',(18.5282716744197,16.981810668038,12.));
#211681=CARTESIAN_POINT('Ctrl Pts',(18.5188255796659,16.9576688599339,0.));
#211682=CARTESIAN_POINT('Ctrl Pts',(18.5188255796659,16.9576688599339,12.));
#211683=CARTESIAN_POINT('Ctrl Pts',(18.5093514883835,16.9336218069353,0.));
#211684=CARTESIAN_POINT('Ctrl Pts',(18.5093514883835,16.9336218069353,12.));
#211685=CARTESIAN_POINT('Ctrl Pts',(18.499849818462,16.9096698606943,0.));
#211686=CARTESIAN_POINT('Ctrl Pts',(18.499849818462,16.9096698606943,12.));
#211687=CARTESIAN_POINT('Ctrl Pts',(18.4903209902227,16.8858133733088,0.));
#211688=CARTESIAN_POINT('Ctrl Pts',(18.4903209902227,16.8858133733088,12.));
#211689=CARTESIAN_POINT('Ctrl Pts',(18.4807654268771,16.8620526977171,0.));
#211690=CARTESIAN_POINT('Ctrl Pts',(18.4807654268771,16.8620526977171,12.));
#211691=CARTESIAN_POINT('Ctrl Pts',(18.4711835548623,16.8383881879709,0.));
#211692=CARTESIAN_POINT('Ctrl Pts',(18.4711835548623,16.8383881879709,12.));
#211693=CARTESIAN_POINT('Ctrl Pts',(18.4615758042305,16.8148201995472,0.));
#211694=CARTESIAN_POINT('Ctrl Pts',(18.4615758042305,16.8148201995472,12.));
#211695=CARTESIAN_POINT('Ctrl Pts',(18.4519426090123,16.791349089629,0.));
#211696=CARTESIAN_POINT('Ctrl Pts',(18.4519426090123,16.791349089629,12.));
#211697=CARTESIAN_POINT('Ctrl Pts',(18.44228440761,16.7679752173992,0.));
#211698=CARTESIAN_POINT('Ctrl Pts',(18.44228440761,16.7679752173992,12.));
#211699=CARTESIAN_POINT('Ctrl Pts',(18.4326016431392,16.7446989442882,0.));
#211700=CARTESIAN_POINT('Ctrl Pts',(18.4326016431392,16.7446989442882,12.));
#211701=CARTESIAN_POINT('Ctrl Pts',(18.4228947633187,16.7215206338818,0.));
#211702=CARTESIAN_POINT('Ctrl Pts',(18.4228947633187,16.7215206338818,12.));
#211703=CARTESIAN_POINT('Ctrl Pts',(18.413164220399,16.6984406518491,0.));
#211704=CARTESIAN_POINT('Ctrl Pts',(18.413164220399,16.6984406518491,12.));
#211705=CARTESIAN_POINT('Ctrl Pts',(18.403410471079,16.6754593658513,0.));
#211706=CARTESIAN_POINT('Ctrl Pts',(18.403410471079,16.6754593658513,12.));
#211707=CARTESIAN_POINT('Ctrl Pts',(18.3936339764332,16.6525771454513,0.));
#211708=CARTESIAN_POINT('Ctrl Pts',(18.3936339764332,16.6525771454513,12.));
#211709=CARTESIAN_POINT('Ctrl Pts',(18.3838352018327,16.6297943620056,0.));
#211710=CARTESIAN_POINT('Ctrl Pts',(18.3838352018327,16.6297943620056,12.));
#211711=CARTESIAN_POINT('Ctrl Pts',(18.3740146168879,16.607111388571,0.));
#211712=CARTESIAN_POINT('Ctrl Pts',(18.3740146168879,16.607111388571,12.));
#211713=CARTESIAN_POINT('Ctrl Pts',(18.3641726955889,16.5845286000217,0.));
#211714=CARTESIAN_POINT('Ctrl Pts',(18.3641726955889,16.5845286000217,12.));
#211715=CARTESIAN_POINT('Ctrl Pts',(18.354309916433,16.5620463731413,0.));
#211716=CARTESIAN_POINT('Ctrl Pts',(18.354309916433,16.5620463731413,12.));
#211717=CARTESIAN_POINT('Ctrl Pts',(18.34442676256,16.5396650867139,0.));
#211718=CARTESIAN_POINT('Ctrl Pts',(18.34442676256,16.5396650867139,12.));
#211719=CARTESIAN_POINT('Ctrl Pts',(18.3345237218864,16.5173851216045,0.));
#211720=CARTESIAN_POINT('Ctrl Pts',(18.3345237218864,16.5173851216045,12.));
#211721=CARTESIAN_POINT('Ctrl Pts',(18.3246012872469,16.4952068608345,0.));
#211722=CARTESIAN_POINT('Ctrl Pts',(18.3246012872469,16.4952068608345,12.));
#211723=CARTESIAN_POINT('Ctrl Pts',(18.3146599565231,16.4731306896441,0.));
#211724=CARTESIAN_POINT('Ctrl Pts',(18.3146599565231,16.4731306896441,12.));
#211725=CARTESIAN_POINT('Ctrl Pts',(18.304700232686,16.4511569955233,0.));
#211726=CARTESIAN_POINT('Ctrl Pts',(18.304700232686,16.4511569955233,12.));
#211727=CARTESIAN_POINT('Ctrl Pts',(18.294722623851,16.4292861682379,0.));
#211728=CARTESIAN_POINT('Ctrl Pts',(18.294722623851,16.4292861682379,12.));
#211729=CARTESIAN_POINT('Ctrl Pts',(18.2847276433309,16.4075185998455,0.));
#211730=CARTESIAN_POINT('Ctrl Pts',(18.2847276433309,16.4075185998455,12.));
#211731=CARTESIAN_POINT('Ctrl Pts',(18.2747158096934,16.385854684708,0.));
#211732=CARTESIAN_POINT('Ctrl Pts',(18.2747158096934,16.385854684708,12.));
#211733=CARTESIAN_POINT('Ctrl Pts',(18.2646876468169,16.3642948194868,0.));
#211734=CARTESIAN_POINT('Ctrl Pts',(18.2646876468169,16.3642948194868,12.));
#211735=CARTESIAN_POINT('Ctrl Pts',(18.2546436839608,16.3428394031589,0.));
#211736=CARTESIAN_POINT('Ctrl Pts',(18.2546436839608,16.3428394031589,12.));
#211737=CARTESIAN_POINT('Ctrl Pts',(18.2445844558742,16.3214888370987,0.));
#211738=CARTESIAN_POINT('Ctrl Pts',(18.2445844558742,16.3214888370987,12.));
#211739=CARTESIAN_POINT('Ctrl Pts',(18.2345105028982,16.3002435251378,0.));
#211740=CARTESIAN_POINT('Ctrl Pts',(18.2345105028982,16.3002435251378,12.));
#211741=CARTESIAN_POINT('Ctrl Pts',(18.2244223710745,16.2791038736223,0.));
#211742=CARTESIAN_POINT('Ctrl Pts',(18.2244223710745,16.2791038736223,12.));
#211743=CARTESIAN_POINT('Ctrl Pts',(18.2143206122529,16.2580702914615,0.));
#211744=CARTESIAN_POINT('Ctrl Pts',(18.2143206122529,16.2580702914615,12.));
#211745=CARTESIAN_POINT('Ctrl Pts',(18.2042057842035,16.2371431901638,0.));
#211746=CARTESIAN_POINT('Ctrl Pts',(18.2042057842035,16.2371431901638,12.));
#211747=CARTESIAN_POINT('Ctrl Pts',(18.1940784507229,16.2163229838875,0.));
#211748=CARTESIAN_POINT('Ctrl Pts',(18.1940784507229,16.2163229838875,12.));
#211749=CARTESIAN_POINT('Ctrl Pts',(18.1839391817331,16.1956100895073,0.));
#211750=CARTESIAN_POINT('Ctrl Pts',(18.1839391817331,16.1956100895073,12.));
#211751=CARTESIAN_POINT('Ctrl Pts',(18.1737885533849,16.1750049266671,0.));
#211752=CARTESIAN_POINT('Ctrl Pts',(18.1737885533849,16.1750049266671,12.));
#211753=CARTESIAN_POINT('Ctrl Pts',(18.1636271481615,16.154507917826,0.));
#211754=CARTESIAN_POINT('Ctrl Pts',(18.1636271481615,16.154507917826,12.));
#211755=CARTESIAN_POINT('Ctrl Pts',(18.1534555549852,16.1341194882988,0.));
#211756=CARTESIAN_POINT('Ctrl Pts',(18.1534555549852,16.1341194882988,12.));
#211757=CARTESIAN_POINT('Ctrl Pts',(18.1432743693235,16.1138400662794,0.));
#211758=CARTESIAN_POINT('Ctrl Pts',(18.1432743693235,16.1138400662794,12.));
#211759=CARTESIAN_POINT('Ctrl Pts',(18.1330841933105,16.0936700829112,0.));
#211760=CARTESIAN_POINT('Ctrl Pts',(18.1330841933105,16.0936700829112,12.));
#211761=CARTESIAN_POINT('Ctrl Pts',(18.1228856358751,16.0736099723668,0.));
#211762=CARTESIAN_POINT('Ctrl Pts',(18.1228856358751,16.0736099723668,12.));
#211763=CARTESIAN_POINT('Ctrl Pts',(18.112679312869,16.0536601719126,0.));
#211764=CARTESIAN_POINT('Ctrl Pts',(18.112679312869,16.0536601719126,12.));
#211765=CARTESIAN_POINT('Ctrl Pts',(18.1024658471966,16.0338211219693,0.));
#211766=CARTESIAN_POINT('Ctrl Pts',(18.1024658471966,16.0338211219693,12.));
#211767=CARTESIAN_POINT('Ctrl Pts',(18.0922458689462,16.014093266161,0.));
#211768=CARTESIAN_POINT('Ctrl Pts',(18.0922458689462,16.014093266161,12.));
#211769=CARTESIAN_POINT('Ctrl Pts',(18.0820200155236,15.9944770513613,0.));
#211770=CARTESIAN_POINT('Ctrl Pts',(18.0820200155236,15.9944770513613,12.));
#211771=CARTESIAN_POINT('Ctrl Pts',(18.0717889317958,15.9749729277846,0.));
#211772=CARTESIAN_POINT('Ctrl Pts',(18.0717889317958,15.9749729277846,12.));
#211773=CARTESIAN_POINT('Ctrl Pts',(18.061553270236,15.9555813490644,0.));
#211774=CARTESIAN_POINT('Ctrl Pts',(18.061553270236,15.9555813490644,12.));
#211775=CARTESIAN_POINT('Ctrl Pts',(18.0513136910691,15.9363027723244,0.));
#211776=CARTESIAN_POINT('Ctrl Pts',(18.0513136910691,15.9363027723244,12.));
#211777=CARTESIAN_POINT('Ctrl Pts',(18.0410708624208,15.9171376582436,0.));
#211778=CARTESIAN_POINT('Ctrl Pts',(18.0410708624208,15.9171376582436,12.));
#211779=CARTESIAN_POINT('Ctrl Pts',(18.0308254604636,15.8980864711042,0.));
#211780=CARTESIAN_POINT('Ctrl Pts',(18.0308254604636,15.8980864711042,12.));
#211781=CARTESIAN_POINT('Ctrl Pts',(18.0205781695769,15.8791496788683,0.));
#211782=CARTESIAN_POINT('Ctrl Pts',(18.0205781695769,15.8791496788683,12.));
#211783=CARTESIAN_POINT('Ctrl Pts',(18.0103296825205,15.8603277532831,0.));
#211784=CARTESIAN_POINT('Ctrl Pts',(18.0103296825205,15.8603277532831,12.));
#211785=CARTESIAN_POINT('Ctrl Pts',(18.0000807006052,15.8416211699679,0.));
#211786=CARTESIAN_POINT('Ctrl Pts',(18.0000807006052,15.8416211699679,12.));
#211787=CARTESIAN_POINT('Ctrl Pts',(17.9898319338664,15.8230304084962,0.));
#211788=CARTESIAN_POINT('Ctrl Pts',(17.9898319338664,15.8230304084962,12.));
#211789=CARTESIAN_POINT('Ctrl Pts',(17.9795841012386,15.8045559524677,0.));
#211790=CARTESIAN_POINT('Ctrl Pts',(17.9795841012386,15.8045559524677,12.));
#211791=CARTESIAN_POINT('Ctrl Pts',(17.9693379307303,15.7861982895724,0.));
#211792=CARTESIAN_POINT('Ctrl Pts',(17.9693379307303,15.7861982895724,12.));
#211793=CARTESIAN_POINT('Ctrl Pts',(17.9590941596242,15.7679579117077,0.));
#211794=CARTESIAN_POINT('Ctrl Pts',(17.9590941596242,15.7679579117077,12.));
#211795=CARTESIAN_POINT('Ctrl Pts',(17.9488535346781,15.749835315086,0.));
#211796=CARTESIAN_POINT('Ctrl Pts',(17.9488535346781,15.749835315086,12.));
#211797=CARTESIAN_POINT('Ctrl Pts',(17.9386168123262,15.7318310003335,0.));
#211798=CARTESIAN_POINT('Ctrl Pts',(17.9386168123262,15.7318310003335,12.));
#211799=CARTESIAN_POINT('Ctrl Pts',(17.9283847588836,15.7139454725839,0.));
#211800=CARTESIAN_POINT('Ctrl Pts',(17.9283847588836,15.7139454725839,12.));
#211801=CARTESIAN_POINT('Ctrl Pts',(17.9181581507455,15.6961792415522,0.));
#211802=CARTESIAN_POINT('Ctrl Pts',(17.9181581507455,15.6961792415522,12.));
#211803=CARTESIAN_POINT('Ctrl Pts',(17.9079377746111,15.6785328216461,0.));
#211804=CARTESIAN_POINT('Ctrl Pts',(17.9079377746111,15.6785328216461,12.));
#211805=CARTESIAN_POINT('Ctrl Pts',(17.897724427724,15.661006732103,0.));
#211806=CARTESIAN_POINT('Ctrl Pts',(17.897724427724,15.661006732103,12.));
#211807=CARTESIAN_POINT('Ctrl Pts',(17.8875189181091,15.6436014971085,0.));
#211808=CARTESIAN_POINT('Ctrl Pts',(17.8875189181091,15.6436014971085,12.));
#211809=CARTESIAN_POINT('Ctrl Pts',(17.8773220648125,15.6263176459108,0.));
#211810=CARTESIAN_POINT('Ctrl Pts',(17.8773220648125,15.6263176459108,12.));
#211811=CARTESIAN_POINT('Ctrl Pts',(17.8671346981394,15.609155712921,0.));
#211812=CARTESIAN_POINT('Ctrl Pts',(17.8671346981394,15.609155712921,12.));
#211813=CARTESIAN_POINT('Ctrl Pts',(17.8569576599006,15.5921162378192,0.));
#211814=CARTESIAN_POINT('Ctrl Pts',(17.8569576599006,15.5921162378192,12.));
#211815=CARTESIAN_POINT('Ctrl Pts',(17.8467918036987,15.5751997657163,0.));
#211816=CARTESIAN_POINT('Ctrl Pts',(17.8467918036987,15.5751997657163,12.));
#211817=CARTESIAN_POINT('Ctrl Pts',(17.8366379952085,15.5584068472982,0.));
#211818=CARTESIAN_POINT('Ctrl Pts',(17.8366379952085,15.5584068472982,12.));
#211819=CARTESIAN_POINT('Ctrl Pts',(17.8264971124606,15.541738038964,0.));
#211820=CARTESIAN_POINT('Ctrl Pts',(17.8264971124606,15.541738038964,12.));
#211821=CARTESIAN_POINT('Ctrl Pts',(17.8163700461256,15.5251939029552,0.));
#211822=CARTESIAN_POINT('Ctrl Pts',(17.8163700461256,15.5251939029552,12.));
#211823=CARTESIAN_POINT('Ctrl Pts',(17.8062576997952,15.5087750074718,0.));
#211824=CARTESIAN_POINT('Ctrl Pts',(17.8062576997952,15.5087750074718,12.));
#211825=CARTESIAN_POINT('Ctrl Pts',(17.7961609903148,15.4924819268517,0.));
#211826=CARTESIAN_POINT('Ctrl Pts',(17.7961609903148,15.4924819268517,12.));
#211827=CARTESIAN_POINT('Ctrl Pts',(17.7860808481219,15.4763152417497,0.));
#211828=CARTESIAN_POINT('Ctrl Pts',(17.7860808481219,15.4763152417497,12.));
#211829=CARTESIAN_POINT('Ctrl Pts',(17.7760182175815,15.4602755393018,0.));
#211830=CARTESIAN_POINT('Ctrl Pts',(17.7760182175815,15.4602755393018,12.));
#211831=CARTESIAN_POINT('Ctrl Pts',(17.7659740573265,15.4443634132869,0.));
#211832=CARTESIAN_POINT('Ctrl Pts',(17.7659740573265,15.4443634132869,12.));
#211833=CARTESIAN_POINT('Ctrl Pts',(17.7559493405881,15.4285794642668,0.));
#211834=CARTESIAN_POINT('Ctrl Pts',(17.7559493405881,15.4285794642668,12.));
#211835=CARTESIAN_POINT('Ctrl Pts',(17.7459450555812,15.4129242997837,0.));
#211836=CARTESIAN_POINT('Ctrl Pts',(17.7459450555812,15.4129242997837,12.));
#211837=CARTESIAN_POINT('Ctrl Pts',(17.7359622059149,15.3973985345802,0.));
#211838=CARTESIAN_POINT('Ctrl Pts',(17.7359622059149,15.3973985345802,12.));
#211839=CARTESIAN_POINT('Ctrl Pts',(17.7260018109924,15.3820027907967,0.));
#211840=CARTESIAN_POINT('Ctrl Pts',(17.7260018109924,15.3820027907967,12.));
#211841=CARTESIAN_POINT('Ctrl Pts',(17.7160649064206,15.3667376981699,0.));
#211842=CARTESIAN_POINT('Ctrl Pts',(17.7160649064206,15.3667376981699,12.));
#211843=CARTESIAN_POINT('Ctrl Pts',(17.7061525444042,15.351603894206,0.));
#211844=CARTESIAN_POINT('Ctrl Pts',(17.7061525444042,15.351603894206,12.));
#211845=CARTESIAN_POINT('Ctrl Pts',(17.6962657941983,15.3366020244066,0.));
#211846=CARTESIAN_POINT('Ctrl Pts',(17.6962657941983,15.3366020244066,12.));
#211847=CARTESIAN_POINT('Ctrl Pts',(17.6864057426052,15.3217327425338,0.));
#211848=CARTESIAN_POINT('Ctrl Pts',(17.6864057426052,15.3217327425338,12.));
#211849=CARTESIAN_POINT('Ctrl Pts',(17.676573494456,15.3069967108501,0.));
#211850=CARTESIAN_POINT('Ctrl Pts',(17.676573494456,15.3069967108501,12.));
#211851=CARTESIAN_POINT('Ctrl Pts',(17.6667701731041,15.2923946003598,0.));
#211852=CARTESIAN_POINT('Ctrl Pts',(17.6667701731041,15.2923946003598,12.));
#211853=CARTESIAN_POINT('Ctrl Pts',(17.6569969209,15.2779270910239,0.));
#211854=CARTESIAN_POINT('Ctrl Pts',(17.6569969209,15.2779270910239,12.));
#211855=CARTESIAN_POINT('Ctrl Pts',(17.6472548997328,15.2635948720292,0.));
#211856=CARTESIAN_POINT('Ctrl Pts',(17.6472548997328,15.2635948720292,12.));
#211857=CARTESIAN_POINT('Ctrl Pts',(17.6375452916369,15.2493986421092,0.));
#211858=CARTESIAN_POINT('Ctrl Pts',(17.6375452916369,15.2493986421092,12.));
#211859=CARTESIAN_POINT('Ctrl Pts',(17.6278692993764,15.2353391098367,0.));
#211860=CARTESIAN_POINT('Ctrl Pts',(17.6278692993764,15.2353391098367,12.));
#211861=CARTESIAN_POINT('Ctrl Pts',(17.6182281470468,15.22141699392,0.));
#211862=CARTESIAN_POINT('Ctrl Pts',(17.6182281470468,15.22141699392,12.));
#211863=CARTESIAN_POINT('Ctrl Pts',(17.60862308065,15.2076330234686,0.));
#211864=CARTESIAN_POINT('Ctrl Pts',(17.60862308065,15.2076330234686,12.));
#211865=CARTESIAN_POINT('Ctrl Pts',(17.5990553687599,15.1939879383268,0.));
#211866=CARTESIAN_POINT('Ctrl Pts',(17.5990553687599,15.1939879383268,12.));
#211867=CARTESIAN_POINT('Ctrl Pts',(17.5895263032595,15.1804824894605,0.));
#211868=CARTESIAN_POINT('Ctrl Pts',(17.5895263032595,15.1804824894605,12.));
#211869=CARTESIAN_POINT('Ctrl Pts',(17.580037200054,15.1671174393137,0.));
#211870=CARTESIAN_POINT('Ctrl Pts',(17.580037200054,15.1671174393137,12.));
#211871=CARTESIAN_POINT('Ctrl Pts',(17.5705893998029,15.1538935621714,0.));
#211872=CARTESIAN_POINT('Ctrl Pts',(17.5705893998029,15.1538935621714,12.));
#211873=CARTESIAN_POINT('Ctrl Pts',(17.5611842686192,15.1408116444876,0.));
#211874=CARTESIAN_POINT('Ctrl Pts',(17.5611842686192,15.1408116444876,12.));
#211875=CARTESIAN_POINT('Ctrl Pts',(17.5518231989117,15.1278724853138,0.));
#211876=CARTESIAN_POINT('Ctrl Pts',(17.5518231989117,15.1278724853138,12.));
#211877=CARTESIAN_POINT('Ctrl Pts',(17.5425076102963,15.1150768967728,0.));
#211878=CARTESIAN_POINT('Ctrl Pts',(17.5425076102963,15.1150768967728,12.));
#211879=CARTESIAN_POINT('Ctrl Pts',(17.5332389504829,15.1024257045033,0.));
#211880=CARTESIAN_POINT('Ctrl Pts',(17.5332389504829,15.1024257045033,12.));
#211881=CARTESIAN_POINT('Ctrl Pts',(17.524018696179,15.0899197481082,0.));
#211882=CARTESIAN_POINT('Ctrl Pts',(17.524018696179,15.0899197481082,12.));
#211883=CARTESIAN_POINT('Ctrl Pts',(17.5148483539687,15.0775598815749,0.));
#211884=CARTESIAN_POINT('Ctrl Pts',(17.5148483539687,15.0775598815749,12.));
#211885=CARTESIAN_POINT('Ctrl Pts',(17.5057294613877,15.0653469738307,0.));
#211886=CARTESIAN_POINT('Ctrl Pts',(17.5057294613877,15.0653469738307,12.));
#211887=CARTESIAN_POINT('Ctrl Pts',(17.4966635880246,15.0532819093085,0.));
#211888=CARTESIAN_POINT('Ctrl Pts',(17.4966635880246,15.0532819093085,12.));
#211889=CARTESIAN_POINT('Ctrl Pts',(17.4876523366178,15.0413655884993,0.));
#211890=CARTESIAN_POINT('Ctrl Pts',(17.4876523366178,15.0413655884993,12.));
#211891=CARTESIAN_POINT('Ctrl Pts',(17.4786973441417,15.029598928488,0.));
#211892=CARTESIAN_POINT('Ctrl Pts',(17.4786973441417,15.029598928488,12.));
#211893=CARTESIAN_POINT('Ctrl Pts',(17.4698002829357,15.0179828635087,0.));
#211894=CARTESIAN_POINT('Ctrl Pts',(17.4698002829357,15.0179828635087,12.));
#211895=CARTESIAN_POINT('Ctrl Pts',(17.4609628621419,15.0065183456923,0.));
#211896=CARTESIAN_POINT('Ctrl Pts',(17.4609628621419,15.0065183456923,12.));
#211897=CARTESIAN_POINT('Ctrl Pts',(17.4521868291005,14.9952063457779,0.));
#211898=CARTESIAN_POINT('Ctrl Pts',(17.4521868291005,14.9952063457779,12.));
#211899=CARTESIAN_POINT('Ctrl Pts',(17.4434739707773,14.9840478538357,0.));
#211900=CARTESIAN_POINT('Ctrl Pts',(17.4434739707773,14.9840478538357,12.));
#211901=CARTESIAN_POINT('Ctrl Pts',(17.4348261151395,14.973043879945,0.));
#211902=CARTESIAN_POINT('Ctrl Pts',(17.4348261151395,14.973043879945,12.));
#211903=CARTESIAN_POINT('Ctrl Pts',(17.4262451327088,14.9621954549825,0.));
#211904=CARTESIAN_POINT('Ctrl Pts',(17.4262451327088,14.9621954549825,12.));
#211905=CARTESIAN_POINT('Ctrl Pts',(17.4177329382827,14.9515036315142,0.));
#211906=CARTESIAN_POINT('Ctrl Pts',(17.4177329382827,14.9515036315142,12.));
#211907=CARTESIAN_POINT('Ctrl Pts',(17.4092914926071,14.940969484645,0.));
#211908=CARTESIAN_POINT('Ctrl Pts',(17.4092914926071,14.940969484645,12.));
#211909=CARTESIAN_POINT('Ctrl Pts',(17.400922804075,14.9305941128758,0.));
#211910=CARTESIAN_POINT('Ctrl Pts',(17.400922804075,14.9305941128758,12.));
#211911=CARTESIAN_POINT('Ctrl Pts',(17.3926289303987,14.9203786389343,0.));
#211912=CARTESIAN_POINT('Ctrl Pts',(17.3926289303987,14.9203786389343,12.));
#211913=CARTESIAN_POINT('Ctrl Pts',(17.3844119809823,14.9103242110057,0.));
#211914=CARTESIAN_POINT('Ctrl Pts',(17.3844119809823,14.9103242110057,12.));
#211915=CARTESIAN_POINT('Ctrl Pts',(17.3762741193075,14.9004320039609,0.));
#211916=CARTESIAN_POINT('Ctrl Pts',(17.3762741193075,14.9004320039609,12.));
#211917=CARTESIAN_POINT('Ctrl Pts',(17.3682175653236,14.8907032205789,0.));
#211918=CARTESIAN_POINT('Ctrl Pts',(17.3682175653236,14.8907032205789,12.));
#211919=CARTESIAN_POINT('Ctrl Pts',(17.3602445978163,14.8811390927424,0.));
#211920=CARTESIAN_POINT('Ctrl Pts',(17.3602445978163,14.8811390927424,12.));
#211921=CARTESIAN_POINT('Ctrl Pts',(17.3523575568648,14.8717408826958,0.));
#211922=CARTESIAN_POINT('Ctrl Pts',(17.3523575568648,14.8717408826958,12.));
#211923=CARTESIAN_POINT('Ctrl Pts',(17.3445588463477,14.8625098843419,0.));
#211924=CARTESIAN_POINT('Ctrl Pts',(17.3445588463477,14.8625098843419,12.));
#211925=CARTESIAN_POINT('Ctrl Pts',(17.336850936485,14.8534474245433,0.));
#211926=CARTESIAN_POINT('Ctrl Pts',(17.336850936485,14.8534474245433,12.));
#211927=CARTESIAN_POINT('Ctrl Pts',(17.3292363662601,14.8445548643505,0.));
#211928=CARTESIAN_POINT('Ctrl Pts',(17.3292363662601,14.8445548643505,12.));
#211929=CARTESIAN_POINT('Ctrl Pts',(17.3217177462096,14.8358336004193,0.));
#211930=CARTESIAN_POINT('Ctrl Pts',(17.3217177462096,14.8358336004193,12.));
#211931=CARTESIAN_POINT('Ctrl Pts',(17.3142977632656,14.8272850675375,0.));
#211932=CARTESIAN_POINT('Ctrl Pts',(17.3142977632656,14.8272850675375,12.));
#211933=CARTESIAN_POINT('Ctrl Pts',(17.3069791853705,14.8189107410161,0.));
#211934=CARTESIAN_POINT('Ctrl Pts',(17.3069791853705,14.8189107410161,12.));
#211935=CARTESIAN_POINT('Ctrl Pts',(17.2997648661483,14.8107121391038,0.));
#211936=CARTESIAN_POINT('Ctrl Pts',(17.2997648661483,14.8107121391038,12.));
#211937=CARTESIAN_POINT('Ctrl Pts',(17.2926577496519,14.8026908254281,0.));
#211938=CARTESIAN_POINT('Ctrl Pts',(17.2926577496519,14.8026908254281,12.));
#211939=CARTESIAN_POINT('Ctrl Pts',(17.28566087332,14.7948484105253,0.));
#211940=CARTESIAN_POINT('Ctrl Pts',(17.28566087332,14.7948484105253,12.));
#211941=CARTESIAN_POINT('Ctrl Pts',(17.278777370485,14.787186553128,0.));
#211942=CARTESIAN_POINT('Ctrl Pts',(17.278777370485,14.787186553128,12.));
#211943=CARTESIAN_POINT('Ctrl Pts',(17.2720104735192,14.7797069617802,0.));
#211944=CARTESIAN_POINT('Ctrl Pts',(17.2720104735192,14.7797069617802,12.));
#211945=CARTESIAN_POINT('Ctrl Pts',(17.2653635155317,14.7724113956728,0.));
#211946=CARTESIAN_POINT('Ctrl Pts',(17.2653635155317,14.7724113956728,12.));
#211947=CARTESIAN_POINT('Ctrl Pts',(17.2588399401464,14.7653016697589,0.));
#211948=CARTESIAN_POINT('Ctrl Pts',(17.2588399401464,14.7653016697589,12.));
#211949=CARTESIAN_POINT('Ctrl Pts',(17.2524433146837,14.7583796616617,0.));
#211950=CARTESIAN_POINT('Ctrl Pts',(17.2524433146837,14.7583796616617,12.));
#211951=CARTESIAN_POINT('Ctrl Pts',(17.2461773413289,14.7516473175125,0.));
#211952=CARTESIAN_POINT('Ctrl Pts',(17.2461773413289,14.7516473175125,12.));
#211953=CARTESIAN_POINT('Ctrl Pts',(17.2400458713566,14.7451066593793,0.));
#211954=CARTESIAN_POINT('Ctrl Pts',(17.2400458713566,14.7451066593793,12.));
#211955=CARTESIAN_POINT('Ctrl Pts',(17.2340529062077,14.7387597858117,0.));
#211956=CARTESIAN_POINT('Ctrl Pts',(17.2340529062077,14.7387597858117,12.));
#211957=CARTESIAN_POINT('Ctrl Pts',(17.2282025904314,14.7326088681163,0.));
#211958=CARTESIAN_POINT('Ctrl Pts',(17.2282025904314,14.7326088681163,12.));
#211959=CARTESIAN_POINT('Ctrl Pts',(17.2224992099666,14.7266561494282,0.));
#211960=CARTESIAN_POINT('Ctrl Pts',(17.2224992099666,14.7266561494282,12.));
#211961=CARTESIAN_POINT('Ctrl Pts',(17.2169471814255,14.7209039390326,0.));
#211962=CARTESIAN_POINT('Ctrl Pts',(17.2169471814255,14.7209039390326,12.));
#211963=CARTESIAN_POINT('Ctrl Pts',(17.2115510835988,14.7153546289338,0.));
#211964=CARTESIAN_POINT('Ctrl Pts',(17.2115510835988,14.7153546289338,12.));
#211965=CARTESIAN_POINT('Ctrl Pts',(17.2063157097316,14.7100107213587,0.));
#211966=CARTESIAN_POINT('Ctrl Pts',(17.2063157097316,14.7100107213587,12.));
#211967=CARTESIAN_POINT('Ctrl Pts',(17.2012461084268,14.7048748502663,0.));
#211968=CARTESIAN_POINT('Ctrl Pts',(17.2012461084268,14.7048748502663,12.));
#211969=CARTESIAN_POINT('Ctrl Pts',(17.1963476411694,14.699949811582,0.));
#211970=CARTESIAN_POINT('Ctrl Pts',(17.1963476411694,14.699949811582,12.));
#211971=CARTESIAN_POINT('Ctrl Pts',(17.1916259308415,14.6952385361706,0.));
#211972=CARTESIAN_POINT('Ctrl Pts',(17.1916259308415,14.6952385361706,12.));
#211973=CARTESIAN_POINT('Ctrl Pts',(17.1870867909918,14.6907440526958,0.));
#211974=CARTESIAN_POINT('Ctrl Pts',(17.1870867909918,14.6907440526958,12.));
#211975=CARTESIAN_POINT('Ctrl Pts',(17.182736158472,14.6864694522319,0.));
#211976=CARTESIAN_POINT('Ctrl Pts',(17.182736158472,14.6864694522319,12.));
#211977=CARTESIAN_POINT('Ctrl Pts',(17.1785800350827,14.6824178576167,0.));
#211978=CARTESIAN_POINT('Ctrl Pts',(17.1785800350827,14.6824178576167,12.));
#211979=CARTESIAN_POINT('Ctrl Pts',(17.1746247499057,14.6785925615676,0.));
#211980=CARTESIAN_POINT('Ctrl Pts',(17.1746247499057,14.6785925615676,12.));
#211981=CARTESIAN_POINT('Ctrl Pts',(17.1708771619129,14.6749971333867,0.));
#211982=CARTESIAN_POINT('Ctrl Pts',(17.1708771619129,14.6749971333867,12.));
#211983=CARTESIAN_POINT('Ctrl Pts',(17.1673449723019,14.6716355833321,0.));
#211984=CARTESIAN_POINT('Ctrl Pts',(17.1673449723019,14.6716355833321,12.));
#211985=CARTESIAN_POINT('Ctrl Pts',(17.1640366762304,14.6685123374424,0.));
#211986=CARTESIAN_POINT('Ctrl Pts',(17.1640366762304,14.6685123374424,12.));
#211987=CARTESIAN_POINT('Ctrl Pts',(17.1609609517369,14.6656319165057,0.));
#211988=CARTESIAN_POINT('Ctrl Pts',(17.1609609517369,14.6656319165057,12.));
#211989=CARTESIAN_POINT('Ctrl Pts',(17.1581262646789,14.662998728599,0.));
#211990=CARTESIAN_POINT('Ctrl Pts',(17.1581262646789,14.662998728599,12.));
#211991=CARTESIAN_POINT('Ctrl Pts',(17.1555401986403,14.660616716964,0.));
#211992=CARTESIAN_POINT('Ctrl Pts',(17.1555401986403,14.660616716964,12.));
#211993=CARTESIAN_POINT('Ctrl Pts',(17.1532107762719,14.6584900555301,0.));
#211994=CARTESIAN_POINT('Ctrl Pts',(17.1532107762719,14.6584900555301,12.));
#211995=CARTESIAN_POINT('Ctrl Pts',(17.1511476869495,14.6566237952435,0.));
#211996=CARTESIAN_POINT('Ctrl Pts',(17.1511476869495,14.6566237952435,12.));
#211997=CARTESIAN_POINT('Ctrl Pts',(17.1493641837556,14.6550248622813,0.));
#211998=CARTESIAN_POINT('Ctrl Pts',(17.1493641837556,14.6550248622813,12.));
#211999=CARTESIAN_POINT('Ctrl Pts',(17.1478763944909,14.6537016966188,0.));
#212000=CARTESIAN_POINT('Ctrl Pts',(17.1478763944909,14.6537016966188,12.));
#212001=CARTESIAN_POINT('Ctrl Pts',(17.1466998098673,14.6526624064978,0.));
#212002=CARTESIAN_POINT('Ctrl Pts',(17.1466998098673,14.6526624064978,12.));
#212003=CARTESIAN_POINT('Ctrl Pts',(17.1458462295273,14.65191316345,0.));
#212004=CARTESIAN_POINT('Ctrl Pts',(17.1458462295273,14.65191316345,12.));
#212005=CARTESIAN_POINT('Ctrl Pts',(17.1454262858045,14.6515481598057,0.));
#212006=CARTESIAN_POINT('Ctrl Pts',(17.1454262858045,14.6515481598057,12.));
#212007=CARTESIAN_POINT('Ctrl Pts',(17.1452600887039,14.6514066997188,0.));
#212008=CARTESIAN_POINT('Ctrl Pts',(17.1452600887039,14.6514066997188,12.));
#212009=CARTESIAN_POINT('Ctrl Pts',(17.1452153999142,14.651371185284,0.));
#212010=CARTESIAN_POINT('Ctrl Pts',(17.1452153999142,14.651371185284,12.));
#212011=CARTESIAN_POINT('Ctrl Pts',(17.1452095830633,14.6513681262571,0.));
#212012=CARTESIAN_POINT('Ctrl Pts',(17.1452095830633,14.6513681262571,12.));
#212013=CARTESIAN_POINT('',(18.8464468996588,17.9112098770111,0.));
#212014=CARTESIAN_POINT('Ctrl Pts',(18.8464468996588,17.9112098770111,0.));
#212015=CARTESIAN_POINT('Ctrl Pts',(18.8448126709691,17.9057348246595,0.));
#212016=CARTESIAN_POINT('Ctrl Pts',(18.8415402351786,17.8947931177807,0.));
#212017=CARTESIAN_POINT('Ctrl Pts',(18.8366196462581,17.8784057509356,0.));
#212018=CARTESIAN_POINT('Ctrl Pts',(18.8300349895974,17.8566063174771,0.));
#212019=CARTESIAN_POINT('Ctrl Pts',(18.8217643886157,17.8294410311006,0.));
#212020=CARTESIAN_POINT('Ctrl Pts',(18.8134540340417,17.8023598011057,0.));
#212021=CARTESIAN_POINT('Ctrl Pts',(18.8051039860448,17.7753627137853,0.));
#212022=CARTESIAN_POINT('Ctrl Pts',(18.7967143519419,17.7484498996905,0.));
#212023=CARTESIAN_POINT('Ctrl Pts',(18.7882852976049,17.7216215409035,0.));
#212024=CARTESIAN_POINT('Ctrl Pts',(18.7798170641374,17.6948778823014,0.));
#212025=CARTESIAN_POINT('Ctrl Pts',(18.7713099642754,17.6682192274236,0.));
#212026=CARTESIAN_POINT('Ctrl Pts',(18.762764361321,17.6416459210681,0.));
#212027=CARTESIAN_POINT('Ctrl Pts',(18.7541806530984,17.6151583357012,0.));
#212028=CARTESIAN_POINT('Ctrl Pts',(18.7455592536687,17.5887568561371,0.));
#212029=CARTESIAN_POINT('Ctrl Pts',(18.7369005764553,17.5624418653245,0.));
#212030=CARTESIAN_POINT('Ctrl Pts',(18.7282050157138,17.5362137287593,0.));
#212031=CARTESIAN_POINT('Ctrl Pts',(18.7194729318098,17.5100727820876,0.));
#212032=CARTESIAN_POINT('Ctrl Pts',(18.7107046613912,17.4840193397162,0.));
#212033=CARTESIAN_POINT('Ctrl Pts',(18.70190052503,17.4580537012753,0.));
#212034=CARTESIAN_POINT('Ctrl Pts',(18.6930608357409,17.4321761588142,0.));
#212035=CARTESIAN_POINT('Ctrl Pts',(18.6841859073471,17.4063870038562,0.));
#212036=CARTESIAN_POINT('Ctrl Pts',(18.6752760624052,17.3806865340747,0.));
#212037=CARTESIAN_POINT('Ctrl Pts',(18.6663316416582,17.3550750612443,0.));
#212038=CARTESIAN_POINT('Ctrl Pts',(18.6573530024033,17.3295529098618,0.));
#212039=CARTESIAN_POINT('Ctrl Pts',(18.6483405141865,17.3041204135074,0.));
#212040=CARTESIAN_POINT('Ctrl Pts',(18.6392945554748,17.2787779120213,0.));
#212041=CARTESIAN_POINT('Ctrl Pts',(18.6302155097943,17.2535257482187,0.));
#212042=CARTESIAN_POINT('Ctrl Pts',(18.6211037624038,17.2283642650518,0.));
#212043=CARTESIAN_POINT('Ctrl Pts',(18.6119596959949,17.2032938019284,0.));
#212044=CARTESIAN_POINT('Ctrl Pts',(18.6027836898817,17.1783146940127,0.));
#212045=CARTESIAN_POINT('Ctrl Pts',(18.5935761222825,17.1534272741643,0.));
#212046=CARTESIAN_POINT('Ctrl Pts',(18.5843373717247,17.1286318741183,0.));
#212047=CARTESIAN_POINT('Ctrl Pts',(18.5750678188542,17.1039288260001,0.));
#212048=CARTESIAN_POINT('Ctrl Pts',(18.5657678479789,17.0793184636079,0.));
#212049=CARTESIAN_POINT('Ctrl Pts',(18.556437848963,17.0548011239751,0.));
#212050=CARTESIAN_POINT('Ctrl Pts',(18.547078218209,17.0303771481738,0.));
#212051=CARTESIAN_POINT('Ctrl Pts',(18.5376893576961,17.0060468805097,0.));
#212052=CARTESIAN_POINT('Ctrl Pts',(18.5282716744197,16.981810668038,0.));
#212053=CARTESIAN_POINT('Ctrl Pts',(18.5188255796659,16.9576688599339,0.));
#212054=CARTESIAN_POINT('Ctrl Pts',(18.5093514883835,16.9336218069353,0.));
#212055=CARTESIAN_POINT('Ctrl Pts',(18.499849818462,16.9096698606943,0.));
#212056=CARTESIAN_POINT('Ctrl Pts',(18.4903209902227,16.8858133733088,0.));
#212057=CARTESIAN_POINT('Ctrl Pts',(18.4807654268771,16.8620526977171,0.));
#212058=CARTESIAN_POINT('Ctrl Pts',(18.4711835548623,16.8383881879709,0.));
#212059=CARTESIAN_POINT('Ctrl Pts',(18.4615758042305,16.8148201995472,0.));
#212060=CARTESIAN_POINT('Ctrl Pts',(18.4519426090123,16.791349089629,0.));
#212061=CARTESIAN_POINT('Ctrl Pts',(18.44228440761,16.7679752173992,0.));
#212062=CARTESIAN_POINT('Ctrl Pts',(18.4326016431392,16.7446989442882,0.));
#212063=CARTESIAN_POINT('Ctrl Pts',(18.4228947633187,16.7215206338818,0.));
#212064=CARTESIAN_POINT('Ctrl Pts',(18.413164220399,16.6984406518491,0.));
#212065=CARTESIAN_POINT('Ctrl Pts',(18.403410471079,16.6754593658513,0.));
#212066=CARTESIAN_POINT('Ctrl Pts',(18.3936339764332,16.6525771454513,0.));
#212067=CARTESIAN_POINT('Ctrl Pts',(18.3838352018327,16.6297943620056,0.));
#212068=CARTESIAN_POINT('Ctrl Pts',(18.3740146168879,16.607111388571,0.));
#212069=CARTESIAN_POINT('Ctrl Pts',(18.3641726955889,16.5845286000217,0.));
#212070=CARTESIAN_POINT('Ctrl Pts',(18.354309916433,16.5620463731413,0.));
#212071=CARTESIAN_POINT('Ctrl Pts',(18.34442676256,16.5396650867139,0.));
#212072=CARTESIAN_POINT('Ctrl Pts',(18.3345237218864,16.5173851216045,0.));
#212073=CARTESIAN_POINT('Ctrl Pts',(18.3246012872469,16.4952068608345,0.));
#212074=CARTESIAN_POINT('Ctrl Pts',(18.3146599565231,16.4731306896441,0.));
#212075=CARTESIAN_POINT('Ctrl Pts',(18.304700232686,16.4511569955233,0.));
#212076=CARTESIAN_POINT('Ctrl Pts',(18.294722623851,16.4292861682379,0.));
#212077=CARTESIAN_POINT('Ctrl Pts',(18.2847276433309,16.4075185998455,0.));
#212078=CARTESIAN_POINT('Ctrl Pts',(18.2747158096934,16.385854684708,0.));
#212079=CARTESIAN_POINT('Ctrl Pts',(18.2646876468169,16.3642948194868,0.));
#212080=CARTESIAN_POINT('Ctrl Pts',(18.2546436839608,16.3428394031589,0.));
#212081=CARTESIAN_POINT('Ctrl Pts',(18.2445844558742,16.3214888370987,0.));
#212082=CARTESIAN_POINT('Ctrl Pts',(18.2345105028982,16.3002435251378,0.));
#212083=CARTESIAN_POINT('Ctrl Pts',(18.2244223710745,16.2791038736223,0.));
#212084=CARTESIAN_POINT('Ctrl Pts',(18.2143206122529,16.2580702914615,0.));
#212085=CARTESIAN_POINT('Ctrl Pts',(18.2042057842035,16.2371431901638,0.));
#212086=CARTESIAN_POINT('Ctrl Pts',(18.1940784507229,16.2163229838875,0.));
#212087=CARTESIAN_POINT('Ctrl Pts',(18.1839391817331,16.1956100895073,0.));
#212088=CARTESIAN_POINT('Ctrl Pts',(18.1737885533849,16.1750049266671,0.));
#212089=CARTESIAN_POINT('Ctrl Pts',(18.1636271481615,16.154507917826,0.));
#212090=CARTESIAN_POINT('Ctrl Pts',(18.1534555549852,16.1341194882988,0.));
#212091=CARTESIAN_POINT('Ctrl Pts',(18.1432743693235,16.1138400662794,0.));
#212092=CARTESIAN_POINT('Ctrl Pts',(18.1330841933105,16.0936700829112,0.));
#212093=CARTESIAN_POINT('Ctrl Pts',(18.1228856358751,16.0736099723668,0.));
#212094=CARTESIAN_POINT('Ctrl Pts',(18.112679312869,16.0536601719126,0.));
#212095=CARTESIAN_POINT('Ctrl Pts',(18.1024658471966,16.0338211219693,0.));
#212096=CARTESIAN_POINT('Ctrl Pts',(18.0922458689462,16.014093266161,0.));
#212097=CARTESIAN_POINT('Ctrl Pts',(18.0820200155236,15.9944770513613,0.));
#212098=CARTESIAN_POINT('Ctrl Pts',(18.0717889317958,15.9749729277846,0.));
#212099=CARTESIAN_POINT('Ctrl Pts',(18.061553270236,15.9555813490644,0.));
#212100=CARTESIAN_POINT('Ctrl Pts',(18.0513136910691,15.9363027723244,0.));
#212101=CARTESIAN_POINT('Ctrl Pts',(18.0410708624208,15.9171376582436,0.));
#212102=CARTESIAN_POINT('Ctrl Pts',(18.0308254604636,15.8980864711042,0.));
#212103=CARTESIAN_POINT('Ctrl Pts',(18.0205781695769,15.8791496788683,0.));
#212104=CARTESIAN_POINT('Ctrl Pts',(18.0103296825205,15.8603277532831,0.));
#212105=CARTESIAN_POINT('Ctrl Pts',(18.0000807006052,15.8416211699679,0.));
#212106=CARTESIAN_POINT('Ctrl Pts',(17.9898319338664,15.8230304084962,0.));
#212107=CARTESIAN_POINT('Ctrl Pts',(17.9795841012386,15.8045559524677,0.));
#212108=CARTESIAN_POINT('Ctrl Pts',(17.9693379307303,15.7861982895724,0.));
#212109=CARTESIAN_POINT('Ctrl Pts',(17.9590941596242,15.7679579117077,0.));
#212110=CARTESIAN_POINT('Ctrl Pts',(17.9488535346781,15.749835315086,0.));
#212111=CARTESIAN_POINT('Ctrl Pts',(17.9386168123262,15.7318310003335,0.));
#212112=CARTESIAN_POINT('Ctrl Pts',(17.9283847588836,15.7139454725839,0.));
#212113=CARTESIAN_POINT('Ctrl Pts',(17.9181581507455,15.6961792415522,0.));
#212114=CARTESIAN_POINT('Ctrl Pts',(17.9079377746111,15.6785328216461,0.));
#212115=CARTESIAN_POINT('Ctrl Pts',(17.897724427724,15.661006732103,0.));
#212116=CARTESIAN_POINT('Ctrl Pts',(17.8875189181091,15.6436014971085,0.));
#212117=CARTESIAN_POINT('Ctrl Pts',(17.8773220648125,15.6263176459108,0.));
#212118=CARTESIAN_POINT('Ctrl Pts',(17.8671346981394,15.609155712921,0.));
#212119=CARTESIAN_POINT('Ctrl Pts',(17.8569576599006,15.5921162378192,0.));
#212120=CARTESIAN_POINT('Ctrl Pts',(17.8467918036987,15.5751997657163,0.));
#212121=CARTESIAN_POINT('Ctrl Pts',(17.8366379952085,15.5584068472982,0.));
#212122=CARTESIAN_POINT('Ctrl Pts',(17.8264971124606,15.541738038964,0.));
#212123=CARTESIAN_POINT('Ctrl Pts',(17.8163700461256,15.5251939029552,0.));
#212124=CARTESIAN_POINT('Ctrl Pts',(17.8062576997952,15.5087750074718,0.));
#212125=CARTESIAN_POINT('Ctrl Pts',(17.7961609903148,15.4924819268517,0.));
#212126=CARTESIAN_POINT('Ctrl Pts',(17.7860808481219,15.4763152417497,0.));
#212127=CARTESIAN_POINT('Ctrl Pts',(17.7760182175815,15.4602755393018,0.));
#212128=CARTESIAN_POINT('Ctrl Pts',(17.7659740573265,15.4443634132869,0.));
#212129=CARTESIAN_POINT('Ctrl Pts',(17.7559493405881,15.4285794642668,0.));
#212130=CARTESIAN_POINT('Ctrl Pts',(17.7459450555812,15.4129242997837,0.));
#212131=CARTESIAN_POINT('Ctrl Pts',(17.7359622059149,15.3973985345802,0.));
#212132=CARTESIAN_POINT('Ctrl Pts',(17.7260018109924,15.3820027907967,0.));
#212133=CARTESIAN_POINT('Ctrl Pts',(17.7160649064206,15.3667376981699,0.));
#212134=CARTESIAN_POINT('Ctrl Pts',(17.7061525444042,15.351603894206,0.));
#212135=CARTESIAN_POINT('Ctrl Pts',(17.6962657941983,15.3366020244066,0.));
#212136=CARTESIAN_POINT('Ctrl Pts',(17.6864057426052,15.3217327425338,0.));
#212137=CARTESIAN_POINT('Ctrl Pts',(17.676573494456,15.3069967108501,0.));
#212138=CARTESIAN_POINT('Ctrl Pts',(17.6667701731041,15.2923946003598,0.));
#212139=CARTESIAN_POINT('Ctrl Pts',(17.6569969209,15.2779270910239,0.));
#212140=CARTESIAN_POINT('Ctrl Pts',(17.6472548997328,15.2635948720292,0.));
#212141=CARTESIAN_POINT('Ctrl Pts',(17.6375452916369,15.2493986421092,0.));
#212142=CARTESIAN_POINT('Ctrl Pts',(17.6278692993764,15.2353391098367,0.));
#212143=CARTESIAN_POINT('Ctrl Pts',(17.6182281470468,15.22141699392,0.));
#212144=CARTESIAN_POINT('Ctrl Pts',(17.60862308065,15.2076330234686,0.));
#212145=CARTESIAN_POINT('Ctrl Pts',(17.5990553687599,15.1939879383268,0.));
#212146=CARTESIAN_POINT('Ctrl Pts',(17.5895263032595,15.1804824894605,0.));
#212147=CARTESIAN_POINT('Ctrl Pts',(17.580037200054,15.1671174393137,0.));
#212148=CARTESIAN_POINT('Ctrl Pts',(17.5705893998029,15.1538935621714,0.));
#212149=CARTESIAN_POINT('Ctrl Pts',(17.5611842686192,15.1408116444876,0.));
#212150=CARTESIAN_POINT('Ctrl Pts',(17.5518231989117,15.1278724853138,0.));
#212151=CARTESIAN_POINT('Ctrl Pts',(17.5425076102963,15.1150768967728,0.));
#212152=CARTESIAN_POINT('Ctrl Pts',(17.5332389504829,15.1024257045033,0.));
#212153=CARTESIAN_POINT('Ctrl Pts',(17.524018696179,15.0899197481082,0.));
#212154=CARTESIAN_POINT('Ctrl Pts',(17.5148483539687,15.0775598815749,0.));
#212155=CARTESIAN_POINT('Ctrl Pts',(17.5057294613877,15.0653469738307,0.));
#212156=CARTESIAN_POINT('Ctrl Pts',(17.4966635880246,15.0532819093085,0.));
#212157=CARTESIAN_POINT('Ctrl Pts',(17.4876523366178,15.0413655884993,0.));
#212158=CARTESIAN_POINT('Ctrl Pts',(17.4786973441417,15.029598928488,0.));
#212159=CARTESIAN_POINT('Ctrl Pts',(17.4698002829357,15.0179828635087,0.));
#212160=CARTESIAN_POINT('Ctrl Pts',(17.4609628621419,15.0065183456923,0.));
#212161=CARTESIAN_POINT('Ctrl Pts',(17.4521868291005,14.9952063457779,0.));
#212162=CARTESIAN_POINT('Ctrl Pts',(17.4434739707773,14.9840478538357,0.));
#212163=CARTESIAN_POINT('Ctrl Pts',(17.4348261151395,14.973043879945,0.));
#212164=CARTESIAN_POINT('Ctrl Pts',(17.4262451327088,14.9621954549825,0.));
#212165=CARTESIAN_POINT('Ctrl Pts',(17.4177329382827,14.9515036315142,0.));
#212166=CARTESIAN_POINT('Ctrl Pts',(17.4092914926071,14.940969484645,0.));
#212167=CARTESIAN_POINT('Ctrl Pts',(17.400922804075,14.9305941128758,0.));
#212168=CARTESIAN_POINT('Ctrl Pts',(17.3926289303987,14.9203786389343,0.));
#212169=CARTESIAN_POINT('Ctrl Pts',(17.3844119809823,14.9103242110057,0.));
#212170=CARTESIAN_POINT('Ctrl Pts',(17.3762741193075,14.9004320039609,0.));
#212171=CARTESIAN_POINT('Ctrl Pts',(17.3682175653236,14.8907032205789,0.));
#212172=CARTESIAN_POINT('Ctrl Pts',(17.3602445978163,14.8811390927424,0.));
#212173=CARTESIAN_POINT('Ctrl Pts',(17.3523575568648,14.8717408826958,0.));
#212174=CARTESIAN_POINT('Ctrl Pts',(17.3445588463477,14.8625098843419,0.));
#212175=CARTESIAN_POINT('Ctrl Pts',(17.336850936485,14.8534474245433,0.));
#212176=CARTESIAN_POINT('Ctrl Pts',(17.3292363662601,14.8445548643505,0.));
#212177=CARTESIAN_POINT('Ctrl Pts',(17.3217177462096,14.8358336004193,0.));
#212178=CARTESIAN_POINT('Ctrl Pts',(17.3142977632656,14.8272850675375,0.));
#212179=CARTESIAN_POINT('Ctrl Pts',(17.3069791853705,14.8189107410161,0.));
#212180=CARTESIAN_POINT('Ctrl Pts',(17.2997648661483,14.8107121391038,0.));
#212181=CARTESIAN_POINT('Ctrl Pts',(17.2926577496519,14.8026908254281,0.));
#212182=CARTESIAN_POINT('Ctrl Pts',(17.28566087332,14.7948484105253,0.));
#212183=CARTESIAN_POINT('Ctrl Pts',(17.278777370485,14.787186553128,0.));
#212184=CARTESIAN_POINT('Ctrl Pts',(17.2720104735192,14.7797069617802,0.));
#212185=CARTESIAN_POINT('Ctrl Pts',(17.2653635155317,14.7724113956728,0.));
#212186=CARTESIAN_POINT('Ctrl Pts',(17.2588399401464,14.7653016697589,0.));
#212187=CARTESIAN_POINT('Ctrl Pts',(17.2524433146837,14.7583796616617,0.));
#212188=CARTESIAN_POINT('Ctrl Pts',(17.2461773413289,14.7516473175125,0.));
#212189=CARTESIAN_POINT('Ctrl Pts',(17.2400458713566,14.7451066593793,0.));
#212190=CARTESIAN_POINT('Ctrl Pts',(17.2340529062077,14.7387597858117,0.));
#212191=CARTESIAN_POINT('Ctrl Pts',(17.2282025904314,14.7326088681163,0.));
#212192=CARTESIAN_POINT('Ctrl Pts',(17.2224992099666,14.7266561494282,0.));
#212193=CARTESIAN_POINT('Ctrl Pts',(17.2169471814255,14.7209039390326,0.));
#212194=CARTESIAN_POINT('Ctrl Pts',(17.2115510835988,14.7153546289338,0.));
#212195=CARTESIAN_POINT('Ctrl Pts',(17.2063157097316,14.7100107213587,0.));
#212196=CARTESIAN_POINT('Ctrl Pts',(17.2012461084268,14.7048748502663,0.));
#212197=CARTESIAN_POINT('Ctrl Pts',(17.1963476411694,14.699949811582,0.));
#212198=CARTESIAN_POINT('Ctrl Pts',(17.1916259308415,14.6952385361706,0.));
#212199=CARTESIAN_POINT('Ctrl Pts',(17.1870867909918,14.6907440526958,0.));
#212200=CARTESIAN_POINT('Ctrl Pts',(17.182736158472,14.6864694522319,0.));
#212201=CARTESIAN_POINT('Ctrl Pts',(17.1785800350827,14.6824178576167,0.));
#212202=CARTESIAN_POINT('Ctrl Pts',(17.1746247499057,14.6785925615676,0.));
#212203=CARTESIAN_POINT('Ctrl Pts',(17.1708771619129,14.6749971333867,0.));
#212204=CARTESIAN_POINT('Ctrl Pts',(17.1673449723019,14.6716355833321,0.));
#212205=CARTESIAN_POINT('Ctrl Pts',(17.1640366762304,14.6685123374424,0.));
#212206=CARTESIAN_POINT('Ctrl Pts',(17.1609609517369,14.6656319165057,0.));
#212207=CARTESIAN_POINT('Ctrl Pts',(17.1581262646789,14.662998728599,0.));
#212208=CARTESIAN_POINT('Ctrl Pts',(17.1555401986403,14.660616716964,0.));
#212209=CARTESIAN_POINT('Ctrl Pts',(17.1532107762719,14.6584900555301,0.));
#212210=CARTESIAN_POINT('Ctrl Pts',(17.1511476869495,14.6566237952435,0.));
#212211=CARTESIAN_POINT('Ctrl Pts',(17.1493641837556,14.6550248622813,0.));
#212212=CARTESIAN_POINT('Ctrl Pts',(17.1478763944909,14.6537016966188,0.));
#212213=CARTESIAN_POINT('Ctrl Pts',(17.1466998098673,14.6526624064978,0.));
#212214=CARTESIAN_POINT('Ctrl Pts',(17.1458462295273,14.65191316345,0.));
#212215=CARTESIAN_POINT('Ctrl Pts',(17.1454262858045,14.6515481598057,0.));
#212216=CARTESIAN_POINT('Ctrl Pts',(17.1452600887039,14.6514066997188,0.));
#212217=CARTESIAN_POINT('Ctrl Pts',(17.1452153999142,14.651371185284,0.));
#212218=CARTESIAN_POINT('Ctrl Pts',(17.1452095830633,14.6513681262571,0.));
#212219=CARTESIAN_POINT('',(18.8464468996588,17.9112098770111,0.));
#212220=CARTESIAN_POINT('Ctrl Pts',(18.5896416359912,12.7689476255363,0.));
#212221=CARTESIAN_POINT('Ctrl Pts',(18.5896416359912,12.7689476255363,12.));
#212222=CARTESIAN_POINT('Ctrl Pts',(18.5896460962964,12.7689524524483,0.));
#212223=CARTESIAN_POINT('Ctrl Pts',(18.5896460962964,12.7689524524483,12.));
#212224=CARTESIAN_POINT('Ctrl Pts',(18.5896919669165,12.768986426692,0.));
#212225=CARTESIAN_POINT('Ctrl Pts',(18.5896919669165,12.768986426692,12.));
#212226=CARTESIAN_POINT('Ctrl Pts',(18.589871621843,12.769110348199,0.));
#212227=CARTESIAN_POINT('Ctrl Pts',(18.589871621843,12.769110348199,12.));
#212228=CARTESIAN_POINT('Ctrl Pts',(18.5903328777227,12.7694215127919,0.));
#212229=CARTESIAN_POINT('Ctrl Pts',(18.5903328777227,12.7694215127919,12.));
#212230=CARTESIAN_POINT('Ctrl Pts',(18.5912775137806,12.7700520897173,0.));
#212231=CARTESIAN_POINT('Ctrl Pts',(18.5912775137806,12.7700520897173,12.));
#212232=CARTESIAN_POINT('Ctrl Pts',(18.5925859134579,12.7709195951156,0.));
#212233=CARTESIAN_POINT('Ctrl Pts',(18.5925859134579,12.7709195951156,12.));
#212234=CARTESIAN_POINT('Ctrl Pts',(18.5942490615407,12.7720142287172,0.));
#212235=CARTESIAN_POINT('Ctrl Pts',(18.5942490615407,12.7720142287172,12.));
#212236=CARTESIAN_POINT('Ctrl Pts',(18.5962551167772,12.7733231262108,0.));
#212237=CARTESIAN_POINT('Ctrl Pts',(18.5962551167772,12.7733231262108,12.));
#212238=CARTESIAN_POINT('Ctrl Pts',(18.598591752595,12.7748328937638,0.));
#212239=CARTESIAN_POINT('Ctrl Pts',(18.598591752595,12.7748328937638,12.));
#212240=CARTESIAN_POINT('Ctrl Pts',(18.6012488486709,12.7765325225081,0.));
#212241=CARTESIAN_POINT('Ctrl Pts',(18.6012488486709,12.7765325225081,12.));
#212242=CARTESIAN_POINT('Ctrl Pts',(18.6042190183704,12.7784139605066,0.));
#212243=CARTESIAN_POINT('Ctrl Pts',(18.6042190183704,12.7784139605066,12.));
#212244=CARTESIAN_POINT('Ctrl Pts',(18.6074961535723,12.7804705387658,0.));
#212245=CARTESIAN_POINT('Ctrl Pts',(18.6074961535723,12.7804705387658,12.));
#212246=CARTESIAN_POINT('Ctrl Pts',(18.6110744826219,12.7826959526925,0.));
#212247=CARTESIAN_POINT('Ctrl Pts',(18.6110744826219,12.7826959526925,12.));
#212248=CARTESIAN_POINT('Ctrl Pts',(18.6149475565188,12.7850831657901,0.));
#212249=CARTESIAN_POINT('Ctrl Pts',(18.6149475565188,12.7850831657901,12.));
#212250=CARTESIAN_POINT('Ctrl Pts',(18.6191087624752,12.7876249657834,0.));
#212251=CARTESIAN_POINT('Ctrl Pts',(18.6191087624752,12.7876249657834,12.));
#212252=CARTESIAN_POINT('Ctrl Pts',(18.6235516265575,12.7903142925234,0.));
#212253=CARTESIAN_POINT('Ctrl Pts',(18.6235516265575,12.7903142925234,12.));
#212254=CARTESIAN_POINT('Ctrl Pts',(18.6282702819371,12.7931447451555,0.));
#212255=CARTESIAN_POINT('Ctrl Pts',(18.6282702819371,12.7931447451555,12.));
#212256=CARTESIAN_POINT('Ctrl Pts',(18.6332595057006,12.7961106222251,0.));
#212257=CARTESIAN_POINT('Ctrl Pts',(18.6332595057006,12.7961106222251,12.));
#212258=CARTESIAN_POINT('Ctrl Pts',(18.63851447924,12.7992066625264,0.));
#212259=CARTESIAN_POINT('Ctrl Pts',(18.63851447924,12.7992066625264,12.));
#212260=CARTESIAN_POINT('Ctrl Pts',(18.6440306327456,12.8024278770153,0.));
#212261=CARTESIAN_POINT('Ctrl Pts',(18.6440306327456,12.8024278770153,12.));
#212262=CARTESIAN_POINT('Ctrl Pts',(18.6498034438987,12.805769331162,0.));
#212263=CARTESIAN_POINT('Ctrl Pts',(18.6498034438987,12.805769331162,12.));
#212264=CARTESIAN_POINT('Ctrl Pts',(18.6558284825773,12.8092261933858,0.));
#212265=CARTESIAN_POINT('Ctrl Pts',(18.6558284825773,12.8092261933858,12.));
#212266=CARTESIAN_POINT('Ctrl Pts',(18.6621014624746,12.8127937909631,0.));
#212267=CARTESIAN_POINT('Ctrl Pts',(18.6621014624746,12.8127937909631,12.));
#212268=CARTESIAN_POINT('Ctrl Pts',(18.6686182952799,12.8164676687362,0.));
#212269=CARTESIAN_POINT('Ctrl Pts',(18.6686182952799,12.8164676687362,12.));
#212270=CARTESIAN_POINT('Ctrl Pts',(18.6753751301092,12.8202436318474,0.));
#212271=CARTESIAN_POINT('Ctrl Pts',(18.6753751301092,12.8202436318474,12.));
#212272=CARTESIAN_POINT('Ctrl Pts',(18.6823683094139,12.8241176980017,0.));
#212273=CARTESIAN_POINT('Ctrl Pts',(18.6823683094139,12.8241176980017,12.));
#212274=CARTESIAN_POINT('Ctrl Pts',(18.6895943376171,12.8280860635231,0.));
#212275=CARTESIAN_POINT('Ctrl Pts',(18.6895943376171,12.8280860635231,12.));
#212276=CARTESIAN_POINT('Ctrl Pts',(18.6970498410172,12.8321450599789,0.));
#212277=CARTESIAN_POINT('Ctrl Pts',(18.6970498410172,12.8321450599789,12.));
#212278=CARTESIAN_POINT('Ctrl Pts',(18.7047315436294,12.8362911280361,0.));
#212279=CARTESIAN_POINT('Ctrl Pts',(18.7047315436294,12.8362911280361,12.));
#212280=CARTESIAN_POINT('Ctrl Pts',(18.7126362754445,12.8405208263431,0.));
#212281=CARTESIAN_POINT('Ctrl Pts',(18.7126362754445,12.8405208263431,12.));
#212282=CARTESIAN_POINT('Ctrl Pts',(18.7207609737702,12.8448308329494,0.));
#212283=CARTESIAN_POINT('Ctrl Pts',(18.7207609737702,12.8448308329494,12.));
#212284=CARTESIAN_POINT('Ctrl Pts',(18.7291026886554,12.8492179511591,0.));
#212285=CARTESIAN_POINT('Ctrl Pts',(18.7291026886554,12.8492179511591,12.));
#212286=CARTESIAN_POINT('Ctrl Pts',(18.7376585820854,12.8536791086316,0.));
#212287=CARTESIAN_POINT('Ctrl Pts',(18.7376585820854,12.8536791086316,12.));
#212288=CARTESIAN_POINT('Ctrl Pts',(18.7464259171251,12.8582113455646,0.));
#212289=CARTESIAN_POINT('Ctrl Pts',(18.7464259171251,12.8582113455646,12.));
#212290=CARTESIAN_POINT('Ctrl Pts',(18.7554020493887,12.8628118054171,0.));
#212291=CARTESIAN_POINT('Ctrl Pts',(18.7554020493887,12.8628118054171,12.));
#212292=CARTESIAN_POINT('Ctrl Pts',(18.7645844169564,12.8674777239653,0.));
#212293=CARTESIAN_POINT('Ctrl Pts',(18.7645844169564,12.8674777239653,12.));
#212294=CARTESIAN_POINT('Ctrl Pts',(18.7739705329022,12.872206421181,0.));
#212295=CARTESIAN_POINT('Ctrl Pts',(18.7739705329022,12.872206421181,12.));
#212296=CARTESIAN_POINT('Ctrl Pts',(18.7835579840477,12.8769952998095,0.));
#212297=CARTESIAN_POINT('Ctrl Pts',(18.7835579840477,12.8769952998095,12.));
#212298=CARTESIAN_POINT('Ctrl Pts',(18.7933444285868,12.8818418427475,0.));
#212299=CARTESIAN_POINT('Ctrl Pts',(18.7933444285868,12.8818418427475,12.));
#212300=CARTESIAN_POINT('Ctrl Pts',(18.8033275941943,12.8867436109546,0.));
#212301=CARTESIAN_POINT('Ctrl Pts',(18.8033275941943,12.8867436109546,12.));
#212302=CARTESIAN_POINT('Ctrl Pts',(18.813505275782,12.8916982409935,0.));
#212303=CARTESIAN_POINT('Ctrl Pts',(18.813505275782,12.8916982409935,12.));
#212304=CARTESIAN_POINT('Ctrl Pts',(18.8238753319129,12.8967034410755,0.));
#212305=CARTESIAN_POINT('Ctrl Pts',(18.8238753319129,12.8967034410755,12.));
#212306=CARTESIAN_POINT('Ctrl Pts',(18.834435681259,12.9017569871738,0.));
#212307=CARTESIAN_POINT('Ctrl Pts',(18.834435681259,12.9017569871738,12.));
#212308=CARTESIAN_POINT('Ctrl Pts',(18.8451842990984,12.9068567191854,0.));
#212309=CARTESIAN_POINT('Ctrl Pts',(18.8451842990984,12.9068567191854,12.));
#212310=CARTESIAN_POINT('Ctrl Pts',(18.8561192136198,12.9120005369063,0.));
#212311=CARTESIAN_POINT('Ctrl Pts',(18.8561192136198,12.9120005369063,12.));
#212312=CARTESIAN_POINT('Ctrl Pts',(18.8672385038326,12.9171863977045,0.));
#212313=CARTESIAN_POINT('Ctrl Pts',(18.8672385038326,12.9171863977045,12.));
#212314=CARTESIAN_POINT('Ctrl Pts',(18.8785402977527,12.9224123144982,0.));
#212315=CARTESIAN_POINT('Ctrl Pts',(18.8785402977527,12.9224123144982,12.));
#212316=CARTESIAN_POINT('Ctrl Pts',(18.8900227704889,12.9276763536373,0.));
#212317=CARTESIAN_POINT('Ctrl Pts',(18.8900227704889,12.9276763536373,12.));
#212318=CARTESIAN_POINT('Ctrl Pts',(18.9016841423403,12.9329766328185,0.));
#212319=CARTESIAN_POINT('Ctrl Pts',(18.9016841423403,12.9329766328185,12.));
#212320=CARTESIAN_POINT('Ctrl Pts',(18.9135226769465,12.9383113190375,0.));
#212321=CARTESIAN_POINT('Ctrl Pts',(18.9135226769465,12.9383113190375,12.));
#212322=CARTESIAN_POINT('Ctrl Pts',(18.9255366795195,12.9436786266105,0.));
#212323=CARTESIAN_POINT('Ctrl Pts',(18.9255366795195,12.9436786266105,12.));
#212324=CARTESIAN_POINT('Ctrl Pts',(18.9377244950435,12.9490768151821,0.));
#212325=CARTESIAN_POINT('Ctrl Pts',(18.9377244950435,12.9490768151821,12.));
#212326=CARTESIAN_POINT('Ctrl Pts',(18.9500845064715,12.9545041877377,0.));
#212327=CARTESIAN_POINT('Ctrl Pts',(18.9500845064715,12.9545041877377,12.));
#212328=CARTESIAN_POINT('Ctrl Pts',(18.9626151329229,12.9599590886319,0.));
#212329=CARTESIAN_POINT('Ctrl Pts',(18.9626151329229,12.9599590886319,12.));
#212330=CARTESIAN_POINT('Ctrl Pts',(18.9753148284475,12.9654399021869,0.));
#212331=CARTESIAN_POINT('Ctrl Pts',(18.9753148284475,12.9654399021869,12.));
#212332=CARTESIAN_POINT('Ctrl Pts',(18.9881820807585,12.9709450512747,0.));
#212333=CARTESIAN_POINT('Ctrl Pts',(18.9881820807585,12.9709450512747,12.));
#212334=CARTESIAN_POINT('Ctrl Pts',(19.0012154099791,12.9764729959205,0.));
#212335=CARTESIAN_POINT('Ctrl Pts',(19.0012154099791,12.9764729959205,12.));
#212336=CARTESIAN_POINT('Ctrl Pts',(19.0144133673348,12.9820222318716,0.));
#212337=CARTESIAN_POINT('Ctrl Pts',(19.0144133673348,12.9820222318716,12.));
#212338=CARTESIAN_POINT('Ctrl Pts',(19.0277745339908,12.9875912893003,0.));
#212339=CARTESIAN_POINT('Ctrl Pts',(19.0277745339908,12.9875912893003,12.));
#212340=CARTESIAN_POINT('Ctrl Pts',(19.0412975200398,12.9931787316515,0.));
#212341=CARTESIAN_POINT('Ctrl Pts',(19.0412975200398,12.9931787316515,12.));
#212342=CARTESIAN_POINT('Ctrl Pts',(19.0549809634355,12.9987831544502,0.));
#212343=CARTESIAN_POINT('Ctrl Pts',(19.0549809634355,12.9987831544502,12.));
#212344=CARTESIAN_POINT('Ctrl Pts',(19.0688235289437,13.0044031841381,0.));
#212345=CARTESIAN_POINT('Ctrl Pts',(19.0688235289437,13.0044031841381,12.));
#212346=CARTESIAN_POINT('Ctrl Pts',(19.0828239070482,13.0100374768786,0.));
#212347=CARTESIAN_POINT('Ctrl Pts',(19.0828239070482,13.0100374768786,12.));
#212348=CARTESIAN_POINT('Ctrl Pts',(19.0969808131226,13.0156847176094,0.));
#212349=CARTESIAN_POINT('Ctrl Pts',(19.0969808131226,13.0156847176094,12.));
#212350=CARTESIAN_POINT('Ctrl Pts',(19.1112929866308,13.0213436191326,0.));
#212351=CARTESIAN_POINT('Ctrl Pts',(19.1112929866308,13.0213436191326,12.));
#212352=CARTESIAN_POINT('Ctrl Pts',(19.1257591903099,13.0270129211976,0.));
#212353=CARTESIAN_POINT('Ctrl Pts',(19.1257591903099,13.0270129211976,12.));
#212354=CARTESIAN_POINT('Ctrl Pts',(19.1403782093389,13.0326913895841,0.));
#212355=CARTESIAN_POINT('Ctrl Pts',(19.1403782093389,13.0326913895841,12.));
#212356=CARTESIAN_POINT('Ctrl Pts',(19.1551488505233,13.0383778152072,0.));
#212357=CARTESIAN_POINT('Ctrl Pts',(19.1551488505233,13.0383778152072,12.));
#212358=CARTESIAN_POINT('Ctrl Pts',(19.1700699416625,13.0440710133775,0.));
#212359=CARTESIAN_POINT('Ctrl Pts',(19.1700699416625,13.0440710133775,12.));
#212360=CARTESIAN_POINT('Ctrl Pts',(19.1851403308825,13.0497698230442,0.));
#212361=CARTESIAN_POINT('Ctrl Pts',(19.1851403308825,13.0497698230442,12.));
#212362=CARTESIAN_POINT('Ctrl Pts',(19.2003588859771,13.0554731060537,0.));
#212363=CARTESIAN_POINT('Ctrl Pts',(19.2003588859771,13.0554731060537,12.));
#212364=CARTESIAN_POINT('Ctrl Pts',(19.2157244937141,13.0611797463913,0.));
#212365=CARTESIAN_POINT('Ctrl Pts',(19.2157244937141,13.0611797463913,12.));
#212366=CARTESIAN_POINT('Ctrl Pts',(19.2312360592031,13.0668886494791,0.));
#212367=CARTESIAN_POINT('Ctrl Pts',(19.2312360592031,13.0668886494791,12.));
#212368=CARTESIAN_POINT('Ctrl Pts',(19.2468925053988,13.0725987415856,0.));
#212369=CARTESIAN_POINT('Ctrl Pts',(19.2468925053988,13.0725987415856,12.));
#212370=CARTESIAN_POINT('Ctrl Pts',(19.2626927725596,13.0783089692118,0.));
#212371=CARTESIAN_POINT('Ctrl Pts',(19.2626927725596,13.0783089692118,12.));
#212372=CARTESIAN_POINT('Ctrl Pts',(19.2786358177198,13.0840182984949,0.));
#212373=CARTESIAN_POINT('Ctrl Pts',(19.2786358177198,13.0840182984949,12.));
#212374=CARTESIAN_POINT('Ctrl Pts',(19.2947206141246,13.089725714597,0.));
#212375=CARTESIAN_POINT('Ctrl Pts',(19.2947206141246,13.089725714597,12.));
#212376=CARTESIAN_POINT('Ctrl Pts',(19.3109461507358,13.095430221148,0.));
#212377=CARTESIAN_POINT('Ctrl Pts',(19.3109461507358,13.095430221148,12.));
#212378=CARTESIAN_POINT('Ctrl Pts',(19.3273114318268,13.1011308397592,0.));
#212379=CARTESIAN_POINT('Ctrl Pts',(19.3273114318268,13.1011308397592,12.));
#212380=CARTESIAN_POINT('Ctrl Pts',(19.3438154765395,13.1068266095186,0.));
#212381=CARTESIAN_POINT('Ctrl Pts',(19.3438154765395,13.1068266095186,12.));
#212382=CARTESIAN_POINT('Ctrl Pts',(19.3604573184516,13.1125165865021,0.));
#212383=CARTESIAN_POINT('Ctrl Pts',(19.3604573184516,13.1125165865021,12.));
#212384=CARTESIAN_POINT('Ctrl Pts',(19.3772360051093,13.118199843271,0.));
#212385=CARTESIAN_POINT('Ctrl Pts',(19.3772360051093,13.118199843271,12.));
#212386=CARTESIAN_POINT('Ctrl Pts',(19.3941505976267,13.1238754684177,0.));
#212387=CARTESIAN_POINT('Ctrl Pts',(19.3941505976267,13.1238754684177,12.));
#212388=CARTESIAN_POINT('Ctrl Pts',(19.4112001703561,13.1295425661635,0.));
#212389=CARTESIAN_POINT('Ctrl Pts',(19.4112001703561,13.1295425661635,12.));
#212390=CARTESIAN_POINT('Ctrl Pts',(19.4283838105265,13.135200255944,0.));
#212391=CARTESIAN_POINT('Ctrl Pts',(19.4283838105265,13.135200255944,12.));
#212392=CARTESIAN_POINT('Ctrl Pts',(19.4457006178875,13.140847672006,0.));
#212393=CARTESIAN_POINT('Ctrl Pts',(19.4457006178875,13.140847672006,12.));
#212394=CARTESIAN_POINT('Ctrl Pts',(19.463149704325,13.1464839629966,0.));
#212395=CARTESIAN_POINT('Ctrl Pts',(19.463149704325,13.1464839629966,12.));
#212396=CARTESIAN_POINT('Ctrl Pts',(19.4807301935256,13.1521082915846,0.));
#212397=CARTESIAN_POINT('Ctrl Pts',(19.4807301935256,13.1521082915846,12.));
#212398=CARTESIAN_POINT('Ctrl Pts',(19.498441220707,13.1577198341238,0.));
#212399=CARTESIAN_POINT('Ctrl Pts',(19.498441220707,13.1577198341238,12.));
#212400=CARTESIAN_POINT('Ctrl Pts',(19.5162819323207,13.1633177803097,0.));
#212401=CARTESIAN_POINT('Ctrl Pts',(19.5162819323207,13.1633177803097,12.));
#212402=CARTESIAN_POINT('Ctrl Pts',(19.5342514857564,13.1689013328432,0.));
#212403=CARTESIAN_POINT('Ctrl Pts',(19.5342514857564,13.1689013328432,12.));
#212404=CARTESIAN_POINT('Ctrl Pts',(19.5523490490254,13.1744697070918,0.));
#212405=CARTESIAN_POINT('Ctrl Pts',(19.5523490490254,13.1744697070918,12.));
#212406=CARTESIAN_POINT('Ctrl Pts',(19.5705738004682,13.1800221307683,0.));
#212407=CARTESIAN_POINT('Ctrl Pts',(19.5705738004682,13.1800221307683,12.));
#212408=CARTESIAN_POINT('Ctrl Pts',(19.5889249285352,13.185557843648,0.));
#212409=CARTESIAN_POINT('Ctrl Pts',(19.5889249285352,13.185557843648,12.));
#212410=CARTESIAN_POINT('Ctrl Pts',(19.6074016315421,13.1910760972818,0.));
#212411=CARTESIAN_POINT('Ctrl Pts',(19.6074016315421,13.1910760972818,12.));
#212412=CARTESIAN_POINT('Ctrl Pts',(19.6260031174244,13.196576154715,0.));
#212413=CARTESIAN_POINT('Ctrl Pts',(19.6260031174244,13.196576154715,12.));
#212414=CARTESIAN_POINT('Ctrl Pts',(19.6447286034764,13.202057290206,0.));
#212415=CARTESIAN_POINT('Ctrl Pts',(19.6447286034764,13.202057290206,12.));
#212416=CARTESIAN_POINT('Ctrl Pts',(19.6635773160924,13.2075187889522,0.));
#212417=CARTESIAN_POINT('Ctrl Pts',(19.6635773160924,13.2075187889522,12.));
#212418=CARTESIAN_POINT('Ctrl Pts',(19.6825484905812,13.2129599468478,0.));
#212419=CARTESIAN_POINT('Ctrl Pts',(19.6825484905812,13.2129599468478,12.));
#212420=CARTESIAN_POINT('Ctrl Pts',(19.7016413709678,13.2183800702431,0.));
#212421=CARTESIAN_POINT('Ctrl Pts',(19.7016413709678,13.2183800702431,12.));
#212422=CARTESIAN_POINT('Ctrl Pts',(19.7208552097867,13.2237784757065,0.));
#212423=CARTESIAN_POINT('Ctrl Pts',(19.7208552097867,13.2237784757065,12.));
#212424=CARTESIAN_POINT('Ctrl Pts',(19.7401892678701,13.2291544897902,0.));
#212425=CARTESIAN_POINT('Ctrl Pts',(19.7401892678701,13.2291544897902,12.));
#212426=CARTESIAN_POINT('Ctrl Pts',(19.7596428141176,13.2345074487968,0.));
#212427=CARTESIAN_POINT('Ctrl Pts',(19.7596428141176,13.2345074487968,12.));
#212428=CARTESIAN_POINT('Ctrl Pts',(19.7792151253297,13.239836698568,0.));
#212429=CARTESIAN_POINT('Ctrl Pts',(19.7792151253297,13.239836698568,12.));
#212430=CARTESIAN_POINT('Ctrl Pts',(19.7989054860501,13.2451415942809,0.));
#212431=CARTESIAN_POINT('Ctrl Pts',(19.7989054860501,13.2451415942809,12.));
#212432=CARTESIAN_POINT('Ctrl Pts',(19.8187131883919,13.2504215002458,0.));
#212433=CARTESIAN_POINT('Ctrl Pts',(19.8187131883919,13.2504215002458,12.));
#212434=CARTESIAN_POINT('Ctrl Pts',(19.8386375318632,13.2556757897085,0.));
#212435=CARTESIAN_POINT('Ctrl Pts',(19.8386375318632,13.2556757897085,12.));
#212436=CARTESIAN_POINT('Ctrl Pts',(19.8586778231711,13.2609038446525,0.));
#212437=CARTESIAN_POINT('Ctrl Pts',(19.8586778231711,13.2609038446525,12.));
#212438=CARTESIAN_POINT('Ctrl Pts',(19.8788333760571,13.2661050556128,0.));
#212439=CARTESIAN_POINT('Ctrl Pts',(19.8788333760571,13.2661050556128,12.));
#212440=CARTESIAN_POINT('Ctrl Pts',(19.8991035111739,13.2712788215015,0.));
#212441=CARTESIAN_POINT('Ctrl Pts',(19.8991035111739,13.2712788215015,12.));
#212442=CARTESIAN_POINT('Ctrl Pts',(19.9194875559419,13.2764245494354,0.));
#212443=CARTESIAN_POINT('Ctrl Pts',(19.9194875559419,13.2764245494354,12.));
#212444=CARTESIAN_POINT('Ctrl Pts',(19.9399848444019,13.2815416545663,0.));
#212445=CARTESIAN_POINT('Ctrl Pts',(19.9399848444019,13.2815416545663,12.));
#212446=CARTESIAN_POINT('Ctrl Pts',(19.9605947170589,13.2866295599152,0.));
#212447=CARTESIAN_POINT('Ctrl Pts',(19.9605947170589,13.2866295599152,12.));
#212448=CARTESIAN_POINT('Ctrl Pts',(19.9813165207174,13.2916876962098,0.));
#212449=CARTESIAN_POINT('Ctrl Pts',(19.9813165207174,13.2916876962098,12.));
#212450=CARTESIAN_POINT('Ctrl Pts',(20.0021496083742,13.296715501731,0.));
#212451=CARTESIAN_POINT('Ctrl Pts',(20.0021496083742,13.296715501731,12.));
#212452=CARTESIAN_POINT('Ctrl Pts',(20.0230933391039,13.3017124221639,0.));
#212453=CARTESIAN_POINT('Ctrl Pts',(20.0230933391039,13.3017124221639,12.));
#212454=CARTESIAN_POINT('Ctrl Pts',(20.0441470779345,13.3066779104515,0.));
#212455=CARTESIAN_POINT('Ctrl Pts',(20.0441470779345,13.3066779104515,12.));
#212456=CARTESIAN_POINT('Ctrl Pts',(20.0653101957188,13.3116114266514,0.));
#212457=CARTESIAN_POINT('Ctrl Pts',(20.0653101957188,13.3116114266514,12.));
#212458=CARTESIAN_POINT('Ctrl Pts',(20.0865820689883,13.3165124377963,0.));
#212459=CARTESIAN_POINT('Ctrl Pts',(20.0865820689883,13.3165124377963,12.));
#212460=CARTESIAN_POINT('Ctrl Pts',(20.1079620798377,13.3213804177588,0.));
#212461=CARTESIAN_POINT('Ctrl Pts',(20.1079620798377,13.3213804177588,12.));
#212462=CARTESIAN_POINT('Ctrl Pts',(20.1294496158405,13.3262148471228,0.));
#212463=CARTESIAN_POINT('Ctrl Pts',(20.1294496158405,13.3262148471228,12.));
#212464=CARTESIAN_POINT('Ctrl Pts',(20.1510440699477,13.3310152130565,0.));
#212465=CARTESIAN_POINT('Ctrl Pts',(20.1510440699477,13.3310152130565,12.));
#212466=CARTESIAN_POINT('Ctrl Pts',(20.1727448403818,13.3357810091903,0.));
#212467=CARTESIAN_POINT('Ctrl Pts',(20.1727448403818,13.3357810091903,12.));
#212468=CARTESIAN_POINT('Ctrl Pts',(20.1945513305233,13.3405117354969,0.));
#212469=CARTESIAN_POINT('Ctrl Pts',(20.1945513305233,13.3405117354969,12.));
#212470=CARTESIAN_POINT('Ctrl Pts',(20.2164629487855,13.3452068981763,0.));
#212471=CARTESIAN_POINT('Ctrl Pts',(20.2164629487855,13.3452068981763,12.));
#212472=CARTESIAN_POINT('Ctrl Pts',(20.2384791085354,13.3498660095382,0.));
#212473=CARTESIAN_POINT('Ctrl Pts',(20.2384791085354,13.3498660095382,12.));
#212474=CARTESIAN_POINT('Ctrl Pts',(20.2605992280117,13.3544885878886,0.));
#212475=CARTESIAN_POINT('Ctrl Pts',(20.2605992280117,13.3544885878886,12.));
#212476=CARTESIAN_POINT('Ctrl Pts',(20.2828227302337,13.3590741574194,0.));
#212477=CARTESIAN_POINT('Ctrl Pts',(20.2828227302337,13.3590741574194,12.));
#212478=CARTESIAN_POINT('Ctrl Pts',(20.3051490429049,13.3636222481017,0.));
#212479=CARTESIAN_POINT('Ctrl Pts',(20.3051490429049,13.3636222481017,12.));
#212480=CARTESIAN_POINT('Ctrl Pts',(20.3275775983032,13.3681323955828,0.));
#212481=CARTESIAN_POINT('Ctrl Pts',(20.3275775983032,13.3681323955828,12.));
#212482=CARTESIAN_POINT('Ctrl Pts',(20.3501078331818,13.372604141087,0.));
#212483=CARTESIAN_POINT('Ctrl Pts',(20.3501078331818,13.372604141087,12.));
#212484=CARTESIAN_POINT('Ctrl Pts',(20.3727391887187,13.377037031319,0.));
#212485=CARTESIAN_POINT('Ctrl Pts',(20.3727391887187,13.377037031319,12.));
#212486=CARTESIAN_POINT('Ctrl Pts',(20.3954711104504,13.3814306183721,0.));
#212487=CARTESIAN_POINT('Ctrl Pts',(20.3954711104504,13.3814306183721,12.));
#212488=CARTESIAN_POINT('Ctrl Pts',(20.4183030482002,13.3857844596387,0.));
#212489=CARTESIAN_POINT('Ctrl Pts',(20.4183030482002,13.3857844596387,12.));
#212490=CARTESIAN_POINT('Ctrl Pts',(20.4412344560007,13.3900981177254,0.));
#212491=CARTESIAN_POINT('Ctrl Pts',(20.4412344560007,13.3900981177254,12.));
#212492=CARTESIAN_POINT('Ctrl Pts',(20.4642647920038,13.3943711603739,0.));
#212493=CARTESIAN_POINT('Ctrl Pts',(20.4642647920038,13.3943711603739,12.));
#212494=CARTESIAN_POINT('Ctrl Pts',(20.4873935184041,13.3986031603716,0.));
#212495=CARTESIAN_POINT('Ctrl Pts',(20.4873935184041,13.3986031603716,12.));
#212496=CARTESIAN_POINT('Ctrl Pts',(20.5106201013755,13.4027936954529,0.));
#212497=CARTESIAN_POINT('Ctrl Pts',(20.5106201013755,13.4027936954529,12.));
#212498=CARTESIAN_POINT('Ctrl Pts',(20.5339440109957,13.4069423482077,0.));
#212499=CARTESIAN_POINT('Ctrl Pts',(20.5339440109957,13.4069423482077,12.));
#212500=CARTESIAN_POINT('Ctrl Pts',(20.557364721164,13.4110487059912,0.));
#212501=CARTESIAN_POINT('Ctrl Pts',(20.557364721164,13.4110487059912,12.));
#212502=CARTESIAN_POINT('Ctrl Pts',(20.5808817095155,13.4151123608411,0.));
#212503=CARTESIAN_POINT('Ctrl Pts',(20.5808817095155,13.4151123608411,12.));
#212504=CARTESIAN_POINT('Ctrl Pts',(20.6044944573151,13.4191329093932,0.));
#212505=CARTESIAN_POINT('Ctrl Pts',(20.6044944573151,13.4191329093932,12.));
#212506=CARTESIAN_POINT('Ctrl Pts',(20.6282024494234,13.4231099528178,0.));
#212507=CARTESIAN_POINT('Ctrl Pts',(20.6282024494234,13.4231099528178,12.));
#212508=CARTESIAN_POINT('Ctrl Pts',(20.6520051742867,13.4270430967651,0.));
#212509=CARTESIAN_POINT('Ctrl Pts',(20.6520051742867,13.4270430967651,12.));
#212510=CARTESIAN_POINT('Ctrl Pts',(20.6759021239102,13.4309319513119,0.));
#212511=CARTESIAN_POINT('Ctrl Pts',(20.6759021239102,13.4309319513119,12.));
#212512=CARTESIAN_POINT('Ctrl Pts',(20.6998927938288,13.4347761309154,0.));
#212513=CARTESIAN_POINT('Ctrl Pts',(20.6998927938288,13.4347761309154,12.));
#212514=CARTESIAN_POINT('Ctrl Pts',(20.7239766830675,13.4385752543663,0.));
#212515=CARTESIAN_POINT('Ctrl Pts',(20.7239766830675,13.4385752543663,12.));
#212516=CARTESIAN_POINT('Ctrl Pts',(20.7481532941014,13.4423289447561,0.));
#212517=CARTESIAN_POINT('Ctrl Pts',(20.7481532941014,13.4423289447561,12.));
#212518=CARTESIAN_POINT('Ctrl Pts',(20.7724221327609,13.4460368293689,0.));
#212519=CARTESIAN_POINT('Ctrl Pts',(20.7724221327609,13.4460368293689,12.));
#212520=CARTESIAN_POINT('Ctrl Pts',(20.7967827081228,13.4496985395637,0.));
#212521=CARTESIAN_POINT('Ctrl Pts',(20.7967827081228,13.4496985395637,12.));
#212522=CARTESIAN_POINT('Ctrl Pts',(20.821234532398,13.4533137106667,0.));
#212523=CARTESIAN_POINT('Ctrl Pts',(20.821234532398,13.4533137106667,12.));
#212524=CARTESIAN_POINT('Ctrl Pts',(20.8457771208083,13.4568819818631,0.));
#212525=CARTESIAN_POINT('Ctrl Pts',(20.8457771208083,13.4568819818631,12.));
#212526=CARTESIAN_POINT('Ctrl Pts',(20.8704099914641,13.4604029960983,0.));
#212527=CARTESIAN_POINT('Ctrl Pts',(20.8704099914641,13.4604029960983,12.));
#212528=CARTESIAN_POINT('Ctrl Pts',(20.8951326652158,13.4638763999725,0.));
#212529=CARTESIAN_POINT('Ctrl Pts',(20.8951326652158,13.4638763999725,12.));
#212530=CARTESIAN_POINT('Ctrl Pts',(20.9199446657583,13.4673018437717,0.));
#212531=CARTESIAN_POINT('Ctrl Pts',(20.9199446657583,13.4673018437717,12.));
#212532=CARTESIAN_POINT('Ctrl Pts',(20.9448455197557,13.4706789815166,0.));
#212533=CARTESIAN_POINT('Ctrl Pts',(20.9448455197557,13.4706789815166,12.));
#212534=CARTESIAN_POINT('Ctrl Pts',(20.9698347569477,13.4740074710086,0.));
#212535=CARTESIAN_POINT('Ctrl Pts',(20.9698347569477,13.4740074710086,12.));
#212536=CARTESIAN_POINT('Ctrl Pts',(20.9949119102592,13.4772869738879,0.));
#212537=CARTESIAN_POINT('Ctrl Pts',(20.9949119102592,13.4772869738879,12.));
#212538=CARTESIAN_POINT('Ctrl Pts',(21.0200765158884,13.4805171556822,0.));
#212539=CARTESIAN_POINT('Ctrl Pts',(21.0200765158884,13.4805171556822,12.));
#212540=CARTESIAN_POINT('Ctrl Pts',(21.0453281134245,13.4836976858912,0.));
#212541=CARTESIAN_POINT('Ctrl Pts',(21.0453281134245,13.4836976858912,12.));
#212542=CARTESIAN_POINT('Ctrl Pts',(21.0706662455199,13.4868282377191,0.));
#212543=CARTESIAN_POINT('Ctrl Pts',(21.0706662455199,13.4868282377191,12.));
#212544=CARTESIAN_POINT('Ctrl Pts',(21.0960904575046,13.4899084877717,0.));
#212545=CARTESIAN_POINT('Ctrl Pts',(21.0960904575046,13.4899084877717,12.));
#212546=CARTESIAN_POINT('Ctrl Pts',(21.1216002970207,13.4929381157778,0.));
#212547=CARTESIAN_POINT('Ctrl Pts',(21.1216002970207,13.4929381157778,12.));
#212548=CARTESIAN_POINT('Ctrl Pts',(21.1471953136209,13.4959168042934,0.));
#212549=CARTESIAN_POINT('Ctrl Pts',(21.1471953136209,13.4959168042934,12.));
#212550=CARTESIAN_POINT('Ctrl Pts',(21.1728750584175,13.4988442384491,0.));
#212551=CARTESIAN_POINT('Ctrl Pts',(21.1728750584175,13.4988442384491,12.));
#212552=CARTESIAN_POINT('Ctrl Pts',(21.1986390835828,13.5017201056088,0.));
#212553=CARTESIAN_POINT('Ctrl Pts',(21.1986390835828,13.5017201056088,12.));
#212554=CARTESIAN_POINT('Ctrl Pts',(21.2244869429332,13.5045440957404,0.));
#212555=CARTESIAN_POINT('Ctrl Pts',(21.2244869429332,13.5045440957404,12.));
#212556=CARTESIAN_POINT('Ctrl Pts',(21.250418192743,13.5073159019452,0.));
#212557=CARTESIAN_POINT('Ctrl Pts',(21.250418192743,13.5073159019452,12.));
#212558=CARTESIAN_POINT('Ctrl Pts',(21.2764323924442,13.5100352209205,0.));
#212559=CARTESIAN_POINT('Ctrl Pts',(21.2764323924442,13.5100352209205,12.));
#212560=CARTESIAN_POINT('Ctrl Pts',(21.3025291054235,13.5127017534971,0.));
#212561=CARTESIAN_POINT('Ctrl Pts',(21.3025291054235,13.5127017534971,12.));
#212562=CARTESIAN_POINT('Ctrl Pts',(21.3287078996341,13.5153152050555,0.));
#212563=CARTESIAN_POINT('Ctrl Pts',(21.3287078996341,13.5153152050555,12.));
#212564=CARTESIAN_POINT('Ctrl Pts',(21.3549683486222,13.5178752862466,0.));
#212565=CARTESIAN_POINT('Ctrl Pts',(21.3549683486222,13.5178752862466,12.));
#212566=CARTESIAN_POINT('Ctrl Pts',(21.3813100304973,13.5203817122504,0.));
#212567=CARTESIAN_POINT('Ctrl Pts',(21.3813100304973,13.5203817122504,12.));
#212568=CARTESIAN_POINT('Ctrl Pts',(21.4077325259324,13.5228342013516,0.));
#212569=CARTESIAN_POINT('Ctrl Pts',(21.4077325259324,13.5228342013516,12.));
#212570=CARTESIAN_POINT('Ctrl Pts',(21.4342354165259,13.5252324737802,0.));
#212571=CARTESIAN_POINT('Ctrl Pts',(21.4342354165259,13.5252324737802,12.));
#212572=CARTESIAN_POINT('Ctrl Pts',(21.4608182828697,13.5275762503555,0.));
#212573=CARTESIAN_POINT('Ctrl Pts',(21.4608182828697,13.5275762503555,12.));
#212574=CARTESIAN_POINT('Ctrl Pts',(21.4874807030468,13.5298652514355,0.));
#212575=CARTESIAN_POINT('Ctrl Pts',(21.4874807030468,13.5298652514355,12.));
#212576=CARTESIAN_POINT('Ctrl Pts',(21.5142222501666,13.5320991952138,0.));
#212577=CARTESIAN_POINT('Ctrl Pts',(21.5142222501666,13.5320991952138,12.));
#212578=CARTESIAN_POINT('Ctrl Pts',(21.5410424932503,13.5342777983215,0.));
#212579=CARTESIAN_POINT('Ctrl Pts',(21.5410424932503,13.5342777983215,12.));
#212580=CARTESIAN_POINT('Ctrl Pts',(21.5679410019001,13.536400779028,0.));
#212581=CARTESIAN_POINT('Ctrl Pts',(21.5679410019001,13.536400779028,12.));
#212582=CARTESIAN_POINT('Ctrl Pts',(21.5949173499013,13.5384678597195,0.));
#212583=CARTESIAN_POINT('Ctrl Pts',(21.5949173499013,13.5384678597195,12.));
#212584=CARTESIAN_POINT('Ctrl Pts',(21.6219711193946,13.5404787697792,0.));
#212585=CARTESIAN_POINT('Ctrl Pts',(21.6219711193946,13.5404787697792,12.));
#212586=CARTESIAN_POINT('Ctrl Pts',(21.6491019044648,13.5424332480699,0.));
#212587=CARTESIAN_POINT('Ctrl Pts',(21.6491019044648,13.5424332480699,12.));
#212588=CARTESIAN_POINT('Ctrl Pts',(21.6763093157699,13.5443310461526,0.));
#212589=CARTESIAN_POINT('Ctrl Pts',(21.6763093157699,13.5443310461526,12.));
#212590=CARTESIAN_POINT('Ctrl Pts',(21.7035929822955,13.5461719295048,0.));
#212591=CARTESIAN_POINT('Ctrl Pts',(21.7035929822955,13.5461719295048,12.));
#212592=CARTESIAN_POINT('Ctrl Pts',(21.7309525412281,13.5479556704481,0.));
#212593=CARTESIAN_POINT('Ctrl Pts',(21.7309525412281,13.5479556704481,12.));
#212594=CARTESIAN_POINT('Ctrl Pts',(21.7583876294554,13.5496820422211,0.));
#212595=CARTESIAN_POINT('Ctrl Pts',(21.7583876294554,13.5496820422211,12.));
#212596=CARTESIAN_POINT('Ctrl Pts',(21.7858978745865,13.551350812725,0.));
#212597=CARTESIAN_POINT('Ctrl Pts',(21.7858978745865,13.551350812725,12.));
#212598=CARTESIAN_POINT('Ctrl Pts',(21.8134828857967,13.5529617381573,0.));
#212599=CARTESIAN_POINT('Ctrl Pts',(21.8134828857967,13.5529617381573,12.));
#212600=CARTESIAN_POINT('Ctrl Pts',(21.8411422456075,13.5545145573031,0.));
#212601=CARTESIAN_POINT('Ctrl Pts',(21.8411422456075,13.5545145573031,12.));
#212602=CARTESIAN_POINT('Ctrl Pts',(21.8688754989365,13.5560089839385,0.));
#212603=CARTESIAN_POINT('Ctrl Pts',(21.8688754989365,13.5560089839385,12.));
#212604=CARTESIAN_POINT('Ctrl Pts',(21.8966821688824,13.5574447178425,0.));
#212605=CARTESIAN_POINT('Ctrl Pts',(21.8966821688824,13.5574447178425,12.));
#212606=CARTESIAN_POINT('Ctrl Pts',(21.9245617765769,13.5588214586604,0.));
#212607=CARTESIAN_POINT('Ctrl Pts',(21.9245617765769,13.5588214586604,12.));
#212608=CARTESIAN_POINT('Ctrl Pts',(21.9525138592813,13.5601389185257,0.));
#212609=CARTESIAN_POINT('Ctrl Pts',(21.9525138592813,13.5601389185257,12.));
#212610=CARTESIAN_POINT('Ctrl Pts',(21.9805379899168,13.5613968357561,0.));
#212611=CARTESIAN_POINT('Ctrl Pts',(21.9805379899168,13.5613968357561,12.));
#212612=CARTESIAN_POINT('Ctrl Pts',(22.0086337943449,13.5625949868333,0.));
#212613=CARTESIAN_POINT('Ctrl Pts',(22.0086337943449,13.5625949868333,12.));
#212614=CARTESIAN_POINT('Ctrl Pts',(22.0368009736295,13.5637332022473,0.));
#212615=CARTESIAN_POINT('Ctrl Pts',(22.0368009736295,13.5637332022473,12.));
#212616=CARTESIAN_POINT('Ctrl Pts',(22.0650393089609,13.5648113689033,0.));
#212617=CARTESIAN_POINT('Ctrl Pts',(22.0650393089609,13.5648113689033,12.));
#212618=CARTESIAN_POINT('Ctrl Pts',(22.0933486464593,13.5658294169284,0.));
#212619=CARTESIAN_POINT('Ctrl Pts',(22.0933486464593,13.5658294169284,12.));
#212620=CARTESIAN_POINT('Ctrl Pts',(22.1217288871975,13.5667873105359,0.));
#212621=CARTESIAN_POINT('Ctrl Pts',(22.1217288871975,13.5667873105359,12.));
#212622=CARTESIAN_POINT('Ctrl Pts',(22.1444897575194,13.5675054919061,0.));
#212623=CARTESIAN_POINT('Ctrl Pts',(22.1444897575194,13.5675054919061,12.));
#212624=CARTESIAN_POINT('Ctrl Pts',(22.1615922805008,13.5680170531805,0.));
#212625=CARTESIAN_POINT('Ctrl Pts',(22.1615922805008,13.5680170531805,12.));
#212626=CARTESIAN_POINT('Ctrl Pts',(22.1730081264608,13.5683460612942,0.));
#212627=CARTESIAN_POINT('Ctrl Pts',(22.1730081264608,13.5683460612942,12.));
#212628=CARTESIAN_POINT('Ctrl Pts',(22.1787195904339,13.5685075571671,0.));
#212629=CARTESIAN_POINT('Ctrl Pts',(22.1787195904339,13.5685075571671,12.));
#212630=CARTESIAN_POINT('',(22.1787195904339,13.5685075571671,0.));
#212631=CARTESIAN_POINT('Ctrl Pts',(18.5896416359912,12.7689476255363,0.));
#212632=CARTESIAN_POINT('Ctrl Pts',(18.5896460962964,12.7689524524483,0.));
#212633=CARTESIAN_POINT('Ctrl Pts',(18.5896919669165,12.768986426692,0.));
#212634=CARTESIAN_POINT('Ctrl Pts',(18.589871621843,12.769110348199,0.));
#212635=CARTESIAN_POINT('Ctrl Pts',(18.5903328777227,12.7694215127919,0.));
#212636=CARTESIAN_POINT('Ctrl Pts',(18.5912775137806,12.7700520897173,0.));
#212637=CARTESIAN_POINT('Ctrl Pts',(18.5925859134579,12.7709195951156,0.));
#212638=CARTESIAN_POINT('Ctrl Pts',(18.5942490615407,12.7720142287172,0.));
#212639=CARTESIAN_POINT('Ctrl Pts',(18.5962551167772,12.7733231262108,0.));
#212640=CARTESIAN_POINT('Ctrl Pts',(18.598591752595,12.7748328937638,0.));
#212641=CARTESIAN_POINT('Ctrl Pts',(18.6012488486709,12.7765325225081,0.));
#212642=CARTESIAN_POINT('Ctrl Pts',(18.6042190183704,12.7784139605066,0.));
#212643=CARTESIAN_POINT('Ctrl Pts',(18.6074961535723,12.7804705387658,0.));
#212644=CARTESIAN_POINT('Ctrl Pts',(18.6110744826219,12.7826959526925,0.));
#212645=CARTESIAN_POINT('Ctrl Pts',(18.6149475565188,12.7850831657901,0.));
#212646=CARTESIAN_POINT('Ctrl Pts',(18.6191087624752,12.7876249657834,0.));
#212647=CARTESIAN_POINT('Ctrl Pts',(18.6235516265575,12.7903142925234,0.));
#212648=CARTESIAN_POINT('Ctrl Pts',(18.6282702819371,12.7931447451555,0.));
#212649=CARTESIAN_POINT('Ctrl Pts',(18.6332595057006,12.7961106222251,0.));
#212650=CARTESIAN_POINT('Ctrl Pts',(18.63851447924,12.7992066625264,0.));
#212651=CARTESIAN_POINT('Ctrl Pts',(18.6440306327456,12.8024278770153,0.));
#212652=CARTESIAN_POINT('Ctrl Pts',(18.6498034438987,12.805769331162,0.));
#212653=CARTESIAN_POINT('Ctrl Pts',(18.6558284825773,12.8092261933858,0.));
#212654=CARTESIAN_POINT('Ctrl Pts',(18.6621014624746,12.8127937909631,0.));
#212655=CARTESIAN_POINT('Ctrl Pts',(18.6686182952799,12.8164676687362,0.));
#212656=CARTESIAN_POINT('Ctrl Pts',(18.6753751301092,12.8202436318474,0.));
#212657=CARTESIAN_POINT('Ctrl Pts',(18.6823683094139,12.8241176980017,0.));
#212658=CARTESIAN_POINT('Ctrl Pts',(18.6895943376171,12.8280860635231,0.));
#212659=CARTESIAN_POINT('Ctrl Pts',(18.6970498410172,12.8321450599789,0.));
#212660=CARTESIAN_POINT('Ctrl Pts',(18.7047315436294,12.8362911280361,0.));
#212661=CARTESIAN_POINT('Ctrl Pts',(18.7126362754445,12.8405208263431,0.));
#212662=CARTESIAN_POINT('Ctrl Pts',(18.7207609737702,12.8448308329494,0.));
#212663=CARTESIAN_POINT('Ctrl Pts',(18.7291026886554,12.8492179511591,0.));
#212664=CARTESIAN_POINT('Ctrl Pts',(18.7376585820854,12.8536791086316,0.));
#212665=CARTESIAN_POINT('Ctrl Pts',(18.7464259171251,12.8582113455646,0.));
#212666=CARTESIAN_POINT('Ctrl Pts',(18.7554020493887,12.8628118054171,0.));
#212667=CARTESIAN_POINT('Ctrl Pts',(18.7645844169564,12.8674777239653,0.));
#212668=CARTESIAN_POINT('Ctrl Pts',(18.7739705329022,12.872206421181,0.));
#212669=CARTESIAN_POINT('Ctrl Pts',(18.7835579840477,12.8769952998095,0.));
#212670=CARTESIAN_POINT('Ctrl Pts',(18.7933444285868,12.8818418427475,0.));
#212671=CARTESIAN_POINT('Ctrl Pts',(18.8033275941943,12.8867436109546,0.));
#212672=CARTESIAN_POINT('Ctrl Pts',(18.813505275782,12.8916982409935,0.));
#212673=CARTESIAN_POINT('Ctrl Pts',(18.8238753319129,12.8967034410755,0.));
#212674=CARTESIAN_POINT('Ctrl Pts',(18.834435681259,12.9017569871738,0.));
#212675=CARTESIAN_POINT('Ctrl Pts',(18.8451842990984,12.9068567191854,0.));
#212676=CARTESIAN_POINT('Ctrl Pts',(18.8561192136198,12.9120005369063,0.));
#212677=CARTESIAN_POINT('Ctrl Pts',(18.8672385038326,12.9171863977045,0.));
#212678=CARTESIAN_POINT('Ctrl Pts',(18.8785402977527,12.9224123144982,0.));
#212679=CARTESIAN_POINT('Ctrl Pts',(18.8900227704889,12.9276763536373,0.));
#212680=CARTESIAN_POINT('Ctrl Pts',(18.9016841423403,12.9329766328185,0.));
#212681=CARTESIAN_POINT('Ctrl Pts',(18.9135226769465,12.9383113190375,0.));
#212682=CARTESIAN_POINT('Ctrl Pts',(18.9255366795195,12.9436786266105,0.));
#212683=CARTESIAN_POINT('Ctrl Pts',(18.9377244950435,12.9490768151821,0.));
#212684=CARTESIAN_POINT('Ctrl Pts',(18.9500845064715,12.9545041877377,0.));
#212685=CARTESIAN_POINT('Ctrl Pts',(18.9626151329229,12.9599590886319,0.));
#212686=CARTESIAN_POINT('Ctrl Pts',(18.9753148284475,12.9654399021869,0.));
#212687=CARTESIAN_POINT('Ctrl Pts',(18.9881820807585,12.9709450512747,0.));
#212688=CARTESIAN_POINT('Ctrl Pts',(19.0012154099791,12.9764729959205,0.));
#212689=CARTESIAN_POINT('Ctrl Pts',(19.0144133673348,12.9820222318716,0.));
#212690=CARTESIAN_POINT('Ctrl Pts',(19.0277745339908,12.9875912893003,0.));
#212691=CARTESIAN_POINT('Ctrl Pts',(19.0412975200398,12.9931787316515,0.));
#212692=CARTESIAN_POINT('Ctrl Pts',(19.0549809634355,12.9987831544502,0.));
#212693=CARTESIAN_POINT('Ctrl Pts',(19.0688235289437,13.0044031841381,0.));
#212694=CARTESIAN_POINT('Ctrl Pts',(19.0828239070482,13.0100374768786,0.));
#212695=CARTESIAN_POINT('Ctrl Pts',(19.0969808131226,13.0156847176094,0.));
#212696=CARTESIAN_POINT('Ctrl Pts',(19.1112929866308,13.0213436191326,0.));
#212697=CARTESIAN_POINT('Ctrl Pts',(19.1257591903099,13.0270129211976,0.));
#212698=CARTESIAN_POINT('Ctrl Pts',(19.1403782093389,13.0326913895841,0.));
#212699=CARTESIAN_POINT('Ctrl Pts',(19.1551488505233,13.0383778152072,0.));
#212700=CARTESIAN_POINT('Ctrl Pts',(19.1700699416625,13.0440710133775,0.));
#212701=CARTESIAN_POINT('Ctrl Pts',(19.1851403308825,13.0497698230442,0.));
#212702=CARTESIAN_POINT('Ctrl Pts',(19.2003588859771,13.0554731060537,0.));
#212703=CARTESIAN_POINT('Ctrl Pts',(19.2157244937141,13.0611797463913,0.));
#212704=CARTESIAN_POINT('Ctrl Pts',(19.2312360592031,13.0668886494791,0.));
#212705=CARTESIAN_POINT('Ctrl Pts',(19.2468925053988,13.0725987415856,0.));
#212706=CARTESIAN_POINT('Ctrl Pts',(19.2626927725596,13.0783089692118,0.));
#212707=CARTESIAN_POINT('Ctrl Pts',(19.2786358177198,13.0840182984949,0.));
#212708=CARTESIAN_POINT('Ctrl Pts',(19.2947206141246,13.089725714597,0.));
#212709=CARTESIAN_POINT('Ctrl Pts',(19.3109461507358,13.095430221148,0.));
#212710=CARTESIAN_POINT('Ctrl Pts',(19.3273114318268,13.1011308397592,0.));
#212711=CARTESIAN_POINT('Ctrl Pts',(19.3438154765395,13.1068266095186,0.));
#212712=CARTESIAN_POINT('Ctrl Pts',(19.3604573184516,13.1125165865021,0.));
#212713=CARTESIAN_POINT('Ctrl Pts',(19.3772360051093,13.118199843271,0.));
#212714=CARTESIAN_POINT('Ctrl Pts',(19.3941505976267,13.1238754684177,0.));
#212715=CARTESIAN_POINT('Ctrl Pts',(19.4112001703561,13.1295425661635,0.));
#212716=CARTESIAN_POINT('Ctrl Pts',(19.4283838105265,13.135200255944,0.));
#212717=CARTESIAN_POINT('Ctrl Pts',(19.4457006178875,13.140847672006,0.));
#212718=CARTESIAN_POINT('Ctrl Pts',(19.463149704325,13.1464839629966,0.));
#212719=CARTESIAN_POINT('Ctrl Pts',(19.4807301935256,13.1521082915846,0.));
#212720=CARTESIAN_POINT('Ctrl Pts',(19.498441220707,13.1577198341238,0.));
#212721=CARTESIAN_POINT('Ctrl Pts',(19.5162819323207,13.1633177803097,0.));
#212722=CARTESIAN_POINT('Ctrl Pts',(19.5342514857564,13.1689013328432,0.));
#212723=CARTESIAN_POINT('Ctrl Pts',(19.5523490490254,13.1744697070918,0.));
#212724=CARTESIAN_POINT('Ctrl Pts',(19.5705738004682,13.1800221307683,0.));
#212725=CARTESIAN_POINT('Ctrl Pts',(19.5889249285352,13.185557843648,0.));
#212726=CARTESIAN_POINT('Ctrl Pts',(19.6074016315421,13.1910760972818,0.));
#212727=CARTESIAN_POINT('Ctrl Pts',(19.6260031174244,13.196576154715,0.));
#212728=CARTESIAN_POINT('Ctrl Pts',(19.6447286034764,13.202057290206,0.));
#212729=CARTESIAN_POINT('Ctrl Pts',(19.6635773160924,13.2075187889522,0.));
#212730=CARTESIAN_POINT('Ctrl Pts',(19.6825484905812,13.2129599468478,0.));
#212731=CARTESIAN_POINT('Ctrl Pts',(19.7016413709678,13.2183800702431,0.));
#212732=CARTESIAN_POINT('Ctrl Pts',(19.7208552097867,13.2237784757065,0.));
#212733=CARTESIAN_POINT('Ctrl Pts',(19.7401892678701,13.2291544897902,0.));
#212734=CARTESIAN_POINT('Ctrl Pts',(19.7596428141176,13.2345074487968,0.));
#212735=CARTESIAN_POINT('Ctrl Pts',(19.7792151253297,13.239836698568,0.));
#212736=CARTESIAN_POINT('Ctrl Pts',(19.7989054860501,13.2451415942809,0.));
#212737=CARTESIAN_POINT('Ctrl Pts',(19.8187131883919,13.2504215002458,0.));
#212738=CARTESIAN_POINT('Ctrl Pts',(19.8386375318632,13.2556757897085,0.));
#212739=CARTESIAN_POINT('Ctrl Pts',(19.8586778231711,13.2609038446525,0.));
#212740=CARTESIAN_POINT('Ctrl Pts',(19.8788333760571,13.2661050556128,0.));
#212741=CARTESIAN_POINT('Ctrl Pts',(19.8991035111739,13.2712788215015,0.));
#212742=CARTESIAN_POINT('Ctrl Pts',(19.9194875559419,13.2764245494354,0.));
#212743=CARTESIAN_POINT('Ctrl Pts',(19.9399848444019,13.2815416545663,0.));
#212744=CARTESIAN_POINT('Ctrl Pts',(19.9605947170589,13.2866295599152,0.));
#212745=CARTESIAN_POINT('Ctrl Pts',(19.9813165207174,13.2916876962098,0.));
#212746=CARTESIAN_POINT('Ctrl Pts',(20.0021496083742,13.296715501731,0.));
#212747=CARTESIAN_POINT('Ctrl Pts',(20.0230933391039,13.3017124221639,0.));
#212748=CARTESIAN_POINT('Ctrl Pts',(20.0441470779345,13.3066779104515,0.));
#212749=CARTESIAN_POINT('Ctrl Pts',(20.0653101957188,13.3116114266514,0.));
#212750=CARTESIAN_POINT('Ctrl Pts',(20.0865820689883,13.3165124377963,0.));
#212751=CARTESIAN_POINT('Ctrl Pts',(20.1079620798377,13.3213804177588,0.));
#212752=CARTESIAN_POINT('Ctrl Pts',(20.1294496158405,13.3262148471228,0.));
#212753=CARTESIAN_POINT('Ctrl Pts',(20.1510440699477,13.3310152130565,0.));
#212754=CARTESIAN_POINT('Ctrl Pts',(20.1727448403818,13.3357810091903,0.));
#212755=CARTESIAN_POINT('Ctrl Pts',(20.1945513305233,13.3405117354969,0.));
#212756=CARTESIAN_POINT('Ctrl Pts',(20.2164629487855,13.3452068981763,0.));
#212757=CARTESIAN_POINT('Ctrl Pts',(20.2384791085354,13.3498660095382,0.));
#212758=CARTESIAN_POINT('Ctrl Pts',(20.2605992280117,13.3544885878886,0.));
#212759=CARTESIAN_POINT('Ctrl Pts',(20.2828227302337,13.3590741574194,0.));
#212760=CARTESIAN_POINT('Ctrl Pts',(20.3051490429049,13.3636222481017,0.));
#212761=CARTESIAN_POINT('Ctrl Pts',(20.3275775983032,13.3681323955828,0.));
#212762=CARTESIAN_POINT('Ctrl Pts',(20.3501078331818,13.372604141087,0.));
#212763=CARTESIAN_POINT('Ctrl Pts',(20.3727391887187,13.377037031319,0.));
#212764=CARTESIAN_POINT('Ctrl Pts',(20.3954711104504,13.3814306183721,0.));
#212765=CARTESIAN_POINT('Ctrl Pts',(20.4183030482002,13.3857844596387,0.));
#212766=CARTESIAN_POINT('Ctrl Pts',(20.4412344560007,13.3900981177254,0.));
#212767=CARTESIAN_POINT('Ctrl Pts',(20.4642647920038,13.3943711603739,0.));
#212768=CARTESIAN_POINT('Ctrl Pts',(20.4873935184041,13.3986031603716,0.));
#212769=CARTESIAN_POINT('Ctrl Pts',(20.5106201013755,13.4027936954529,0.));
#212770=CARTESIAN_POINT('Ctrl Pts',(20.5339440109957,13.4069423482077,0.));
#212771=CARTESIAN_POINT('Ctrl Pts',(20.557364721164,13.4110487059912,0.));
#212772=CARTESIAN_POINT('Ctrl Pts',(20.5808817095155,13.4151123608411,0.));
#212773=CARTESIAN_POINT('Ctrl Pts',(20.6044944573151,13.4191329093932,0.));
#212774=CARTESIAN_POINT('Ctrl Pts',(20.6282024494234,13.4231099528178,0.));
#212775=CARTESIAN_POINT('Ctrl Pts',(20.6520051742867,13.4270430967651,0.));
#212776=CARTESIAN_POINT('Ctrl Pts',(20.6759021239102,13.4309319513119,0.));
#212777=CARTESIAN_POINT('Ctrl Pts',(20.6998927938288,13.4347761309154,0.));
#212778=CARTESIAN_POINT('Ctrl Pts',(20.7239766830675,13.4385752543663,0.));
#212779=CARTESIAN_POINT('Ctrl Pts',(20.7481532941014,13.4423289447561,0.));
#212780=CARTESIAN_POINT('Ctrl Pts',(20.7724221327609,13.4460368293689,0.));
#212781=CARTESIAN_POINT('Ctrl Pts',(20.7967827081228,13.4496985395637,0.));
#212782=CARTESIAN_POINT('Ctrl Pts',(20.821234532398,13.4533137106667,0.));
#212783=CARTESIAN_POINT('Ctrl Pts',(20.8457771208083,13.4568819818631,0.));
#212784=CARTESIAN_POINT('Ctrl Pts',(20.8704099914641,13.4604029960983,0.));
#212785=CARTESIAN_POINT('Ctrl Pts',(20.8951326652158,13.4638763999725,0.));
#212786=CARTESIAN_POINT('Ctrl Pts',(20.9199446657583,13.4673018437717,0.));
#212787=CARTESIAN_POINT('Ctrl Pts',(20.9448455197557,13.4706789815166,0.));
#212788=CARTESIAN_POINT('Ctrl Pts',(20.9698347569477,13.4740074710086,0.));
#212789=CARTESIAN_POINT('Ctrl Pts',(20.9949119102592,13.4772869738879,0.));
#212790=CARTESIAN_POINT('Ctrl Pts',(21.0200765158884,13.4805171556822,0.));
#212791=CARTESIAN_POINT('Ctrl Pts',(21.0453281134245,13.4836976858912,0.));
#212792=CARTESIAN_POINT('Ctrl Pts',(21.0706662455199,13.4868282377191,0.));
#212793=CARTESIAN_POINT('Ctrl Pts',(21.0960904575046,13.4899084877717,0.));
#212794=CARTESIAN_POINT('Ctrl Pts',(21.1216002970207,13.4929381157778,0.));
#212795=CARTESIAN_POINT('Ctrl Pts',(21.1471953136209,13.4959168042934,0.));
#212796=CARTESIAN_POINT('Ctrl Pts',(21.1728750584175,13.4988442384491,0.));
#212797=CARTESIAN_POINT('Ctrl Pts',(21.1986390835828,13.5017201056088,0.));
#212798=CARTESIAN_POINT('Ctrl Pts',(21.2244869429332,13.5045440957404,0.));
#212799=CARTESIAN_POINT('Ctrl Pts',(21.250418192743,13.5073159019452,0.));
#212800=CARTESIAN_POINT('Ctrl Pts',(21.2764323924442,13.5100352209205,0.));
#212801=CARTESIAN_POINT('Ctrl Pts',(21.3025291054235,13.5127017534971,0.));
#212802=CARTESIAN_POINT('Ctrl Pts',(21.3287078996341,13.5153152050555,0.));
#212803=CARTESIAN_POINT('Ctrl Pts',(21.3549683486222,13.5178752862466,0.));
#212804=CARTESIAN_POINT('Ctrl Pts',(21.3813100304973,13.5203817122504,0.));
#212805=CARTESIAN_POINT('Ctrl Pts',(21.4077325259324,13.5228342013516,0.));
#212806=CARTESIAN_POINT('Ctrl Pts',(21.4342354165259,13.5252324737802,0.));
#212807=CARTESIAN_POINT('Ctrl Pts',(21.4608182828697,13.5275762503555,0.));
#212808=CARTESIAN_POINT('Ctrl Pts',(21.4874807030468,13.5298652514355,0.));
#212809=CARTESIAN_POINT('Ctrl Pts',(21.5142222501666,13.5320991952138,0.));
#212810=CARTESIAN_POINT('Ctrl Pts',(21.5410424932503,13.5342777983215,0.));
#212811=CARTESIAN_POINT('Ctrl Pts',(21.5679410019001,13.536400779028,0.));
#212812=CARTESIAN_POINT('Ctrl Pts',(21.5949173499013,13.5384678597195,0.));
#212813=CARTESIAN_POINT('Ctrl Pts',(21.6219711193946,13.5404787697792,0.));
#212814=CARTESIAN_POINT('Ctrl Pts',(21.6491019044648,13.5424332480699,0.));
#212815=CARTESIAN_POINT('Ctrl Pts',(21.6763093157699,13.5443310461526,0.));
#212816=CARTESIAN_POINT('Ctrl Pts',(21.7035929822955,13.5461719295048,0.));
#212817=CARTESIAN_POINT('Ctrl Pts',(21.7309525412281,13.5479556704481,0.));
#212818=CARTESIAN_POINT('Ctrl Pts',(21.7583876294554,13.5496820422211,0.));
#212819=CARTESIAN_POINT('Ctrl Pts',(21.7858978745865,13.551350812725,0.));
#212820=CARTESIAN_POINT('Ctrl Pts',(21.8134828857967,13.5529617381573,0.));
#212821=CARTESIAN_POINT('Ctrl Pts',(21.8411422456075,13.5545145573031,0.));
#212822=CARTESIAN_POINT('Ctrl Pts',(21.8688754989365,13.5560089839385,0.));
#212823=CARTESIAN_POINT('Ctrl Pts',(21.8966821688824,13.5574447178425,0.));
#212824=CARTESIAN_POINT('Ctrl Pts',(21.9245617765769,13.5588214586604,0.));
#212825=CARTESIAN_POINT('Ctrl Pts',(21.9525138592813,13.5601389185257,0.));
#212826=CARTESIAN_POINT('Ctrl Pts',(21.9805379899168,13.5613968357561,0.));
#212827=CARTESIAN_POINT('Ctrl Pts',(22.0086337943449,13.5625949868333,0.));
#212828=CARTESIAN_POINT('Ctrl Pts',(22.0368009736295,13.5637332022473,0.));
#212829=CARTESIAN_POINT('Ctrl Pts',(22.0650393089609,13.5648113689033,0.));
#212830=CARTESIAN_POINT('Ctrl Pts',(22.0933486464593,13.5658294169284,0.));
#212831=CARTESIAN_POINT('Ctrl Pts',(22.1217288871975,13.5667873105359,0.));
#212832=CARTESIAN_POINT('Ctrl Pts',(22.1444897575194,13.5675054919061,0.));
#212833=CARTESIAN_POINT('Ctrl Pts',(22.1615922805008,13.5680170531805,0.));
#212834=CARTESIAN_POINT('Ctrl Pts',(22.1730081264608,13.5683460612942,0.));
#212835=CARTESIAN_POINT('Ctrl Pts',(22.1787195904339,13.5685075571671,0.));
#212836=CARTESIAN_POINT('',(22.1787195904339,13.5685075571671,0.));
#212837=CARTESIAN_POINT('Origin',(20.2687213152502,7.17139709155223,0.));
#212838=CARTESIAN_POINT('',(21.2610617890679,7.52250298901264,0.));
#212839=CARTESIAN_POINT('',(21.2610617890679,7.52250298901264,0.));
#212840=CARTESIAN_POINT('',(10.1343606576251,3.58569854577611,0.));
#212841=CARTESIAN_POINT('Ctrl Pts',(22.8400320311648,12.4230808101438,0.));
#212842=CARTESIAN_POINT('Ctrl Pts',(22.8400320311648,12.4230808101438,12.));
#212843=CARTESIAN_POINT('Ctrl Pts',(22.8370364396459,12.418215285186,0.));
#212844=CARTESIAN_POINT('Ctrl Pts',(22.8370364396459,12.418215285186,12.));
#212845=CARTESIAN_POINT('Ctrl Pts',(22.8310435872747,12.4084933766347,0.));
#212846=CARTESIAN_POINT('Ctrl Pts',(22.8310435872747,12.4084933766347,12.));
#212847=CARTESIAN_POINT('Ctrl Pts',(22.8220493007173,12.3939379378998,0.));
#212848=CARTESIAN_POINT('Ctrl Pts',(22.8220493007173,12.3939379378998,12.));
#212849=CARTESIAN_POINT('Ctrl Pts',(22.81004690224,12.374585536673,0.));
#212850=CARTESIAN_POINT('Ctrl Pts',(22.81004690224,12.374585536673,12.));
#212851=CARTESIAN_POINT('Ctrl Pts',(22.795027221673,12.3504864740319,0.));
#212852=CARTESIAN_POINT('Ctrl Pts',(22.795027221673,12.3504864740319,12.));
#212853=CARTESIAN_POINT('Ctrl Pts',(22.7799908974768,12.3264788926075,0.));
#212854=CARTESIAN_POINT('Ctrl Pts',(22.7799908974768,12.3264788926075,12.));
#212855=CARTESIAN_POINT('Ctrl Pts',(22.764938010105,12.3025628601792,0.));
#212856=CARTESIAN_POINT('Ctrl Pts',(22.764938010105,12.3025628601792,12.));
#212857=CARTESIAN_POINT('Ctrl Pts',(22.7498686970069,12.2787384750742,0.));
#212858=CARTESIAN_POINT('Ctrl Pts',(22.7498686970069,12.2787384750742,12.));
#212859=CARTESIAN_POINT('Ctrl Pts',(22.7347831655287,12.2550058702395,0.));
#212860=CARTESIAN_POINT('Ctrl Pts',(22.7347831655287,12.2550058702395,12.));
#212861=CARTESIAN_POINT('Ctrl Pts',(22.7196817119374,12.2313652198061,0.));
#212862=CARTESIAN_POINT('Ctrl Pts',(22.7196817119374,12.2313652198061,12.));
#212863=CARTESIAN_POINT('Ctrl Pts',(22.7045647168747,12.2078167360284,0.));
#212864=CARTESIAN_POINT('Ctrl Pts',(22.7045647168747,12.2078167360284,12.));
#212865=CARTESIAN_POINT('Ctrl Pts',(22.6894326205037,12.1843606579262,0.));
#212866=CARTESIAN_POINT('Ctrl Pts',(22.6894326205037,12.1843606579262,12.));
#212867=CARTESIAN_POINT('Ctrl Pts',(22.6742859034944,12.1609972423099,0.));
#212868=CARTESIAN_POINT('Ctrl Pts',(22.6742859034944,12.1609972423099,12.));
#212869=CARTESIAN_POINT('Ctrl Pts',(22.6591250653965,12.1377267537145,0.));
#212870=CARTESIAN_POINT('Ctrl Pts',(22.6591250653965,12.1377267537145,12.));
#212871=CARTESIAN_POINT('Ctrl Pts',(22.6439506046605,12.1145494550383,0.));
#212872=CARTESIAN_POINT('Ctrl Pts',(22.6439506046605,12.1145494550383,12.));
#212873=CARTESIAN_POINT('Ctrl Pts',(22.6287629967056,12.0914655972823,0.));
#212874=CARTESIAN_POINT('Ctrl Pts',(22.6287629967056,12.0914655972823,12.));
#212875=CARTESIAN_POINT('Ctrl Pts',(22.6135626764898,12.0684754113862,0.));
#212876=CARTESIAN_POINT('Ctrl Pts',(22.6135626764898,12.0684754113862,12.));
#212877=CARTESIAN_POINT('Ctrl Pts',(22.5983500505644,12.0455791139128,0.));
#212878=CARTESIAN_POINT('Ctrl Pts',(22.5983500505644,12.0455791139128,12.));
#212879=CARTESIAN_POINT('Ctrl Pts',(22.5831255061282,12.0227769113127,0.));
#212880=CARTESIAN_POINT('Ctrl Pts',(22.5831255061282,12.0227769113127,12.));
#212881=CARTESIAN_POINT('Ctrl Pts',(22.5678894211181,12.0000690046695,0.));
#212882=CARTESIAN_POINT('Ctrl Pts',(22.5678894211181,12.0000690046695,12.));
#212883=CARTESIAN_POINT('Ctrl Pts',(22.5526421741158,11.9774555943496,0.));
#212884=CARTESIAN_POINT('Ctrl Pts',(22.5526421741158,11.9774555943496,12.));
#212885=CARTESIAN_POINT('Ctrl Pts',(22.5373841537307,11.9549368843997,0.));
#212886=CARTESIAN_POINT('Ctrl Pts',(22.5373841537307,11.9549368843997,12.));
#212887=CARTESIAN_POINT('Ctrl Pts',(22.5221157697883,11.9325130877803,0.));
#212888=CARTESIAN_POINT('Ctrl Pts',(22.5221157697883,11.9325130877803,12.));
#212889=CARTESIAN_POINT('Ctrl Pts',(22.5068374513973,11.9101844254557,0.));
#212890=CARTESIAN_POINT('Ctrl Pts',(22.5068374513973,11.9101844254557,12.));
#212891=CARTESIAN_POINT('Ctrl Pts',(22.4915496418485,11.8879511239943,0.));
#212892=CARTESIAN_POINT('Ctrl Pts',(22.4915496418485,11.8879511239943,12.));
#212893=CARTESIAN_POINT('Ctrl Pts',(22.4762527946702,11.8658134137019,0.));
#212894=CARTESIAN_POINT('Ctrl Pts',(22.4762527946702,11.8658134137019,12.));
#212895=CARTESIAN_POINT('Ctrl Pts',(22.4609473690471,11.8437715264487,0.));
#212896=CARTESIAN_POINT('Ctrl Pts',(22.4609473690471,11.8437715264487,12.));
#212897=CARTESIAN_POINT('Ctrl Pts',(22.4456338258735,11.8218256937889,0.));
#212898=CARTESIAN_POINT('Ctrl Pts',(22.4456338258735,11.8218256937889,12.));
#212899=CARTESIAN_POINT('Ctrl Pts',(22.430312622646,11.7999761445173,0.));
#212900=CARTESIAN_POINT('Ctrl Pts',(22.430312622646,11.7999761445173,12.));
#212901=CARTESIAN_POINT('Ctrl Pts',(22.4149842125008,11.7782231042039,0.));
#212902=CARTESIAN_POINT('Ctrl Pts',(22.4149842125008,11.7782231042039,12.));
#212903=CARTESIAN_POINT('Ctrl Pts',(22.3996490469191,11.7565667964764,0.));
#212904=CARTESIAN_POINT('Ctrl Pts',(22.3996490469191,11.7565667964764,12.));
#212905=CARTESIAN_POINT('Ctrl Pts',(22.3843075773899,11.7350074437961,0.));
#212906=CARTESIAN_POINT('Ctrl Pts',(22.3843075773899,11.7350074437961,12.));
#212907=CARTESIAN_POINT('Ctrl Pts',(22.3689602575491,11.7135452684532,0.));
#212908=CARTESIAN_POINT('Ctrl Pts',(22.3689602575491,11.7135452684532,12.));
#212909=CARTESIAN_POINT('Ctrl Pts',(22.3536075450029,11.6921804934056,0.));
#212910=CARTESIAN_POINT('Ctrl Pts',(22.3536075450029,11.6921804934056,12.));
#212911=CARTESIAN_POINT('Ctrl Pts',(22.3382499035619,11.6709133432985,0.));
#212912=CARTESIAN_POINT('Ctrl Pts',(22.3382499035619,11.6709133432985,12.));
#212913=CARTESIAN_POINT('Ctrl Pts',(22.3228878043976,11.6497440449857,0.));
#212914=CARTESIAN_POINT('Ctrl Pts',(22.3228878043976,11.6497440449857,12.));
#212915=CARTESIAN_POINT('Ctrl Pts',(22.3075217249049,11.6286728270009,0.));
#212916=CARTESIAN_POINT('Ctrl Pts',(22.3075217249049,11.6286728270009,12.));
#212917=CARTESIAN_POINT('Ctrl Pts',(22.2921521480356,11.6076999192357,0.));
#212918=CARTESIAN_POINT('Ctrl Pts',(22.2921521480356,11.6076999192357,12.));
#212919=CARTESIAN_POINT('Ctrl Pts',(22.2767795614348,11.5868255525188,0.));
#212920=CARTESIAN_POINT('Ctrl Pts',(22.2767795614348,11.5868255525188,12.));
#212921=CARTESIAN_POINT('Ctrl Pts',(22.2614044566898,11.5660499582403,0.));
#212922=CARTESIAN_POINT('Ctrl Pts',(22.2614044566898,11.5660499582403,12.));
#212923=CARTESIAN_POINT('Ctrl Pts',(22.2460273284654,11.5453733679121,0.));
#212924=CARTESIAN_POINT('Ctrl Pts',(22.2460273284654,11.5453733679121,12.));
#212925=CARTESIAN_POINT('Ctrl Pts',(22.2306486738901,11.5247960128477,0.));
#212926=CARTESIAN_POINT('Ctrl Pts',(22.2306486738901,11.5247960128477,12.));
#212927=CARTESIAN_POINT('Ctrl Pts',(22.2152689931022,11.5043181244242,0.));
#212928=CARTESIAN_POINT('Ctrl Pts',(22.2152689931022,11.5043181244242,12.));
#212929=CARTESIAN_POINT('Ctrl Pts',(22.1998887896436,11.483939934259,0.));
#212930=CARTESIAN_POINT('Ctrl Pts',(22.1998887896436,11.483939934259,12.));
#212931=CARTESIAN_POINT('Ctrl Pts',(22.184508570917,11.463661674411,0.));
#212932=CARTESIAN_POINT('Ctrl Pts',(22.184508570917,11.463661674411,12.));
#212933=CARTESIAN_POINT('Ctrl Pts',(22.1691288486096,11.443483577557,0.));
#212934=CARTESIAN_POINT('Ctrl Pts',(22.1691288486096,11.443483577557,12.));
#212935=CARTESIAN_POINT('Ctrl Pts',(22.1537501391487,11.4234058771742,0.));
#212936=CARTESIAN_POINT('Ctrl Pts',(22.1537501391487,11.4234058771742,12.));
#212937=CARTESIAN_POINT('Ctrl Pts',(22.1383729640964,11.4034288076908,0.));
#212938=CARTESIAN_POINT('Ctrl Pts',(22.1383729640964,11.4034288076908,12.));
#212939=CARTESIAN_POINT('Ctrl Pts',(22.1229978500186,11.3835526044256,0.));
#212940=CARTESIAN_POINT('Ctrl Pts',(22.1229978500186,11.3835526044256,12.));
#212941=CARTESIAN_POINT('Ctrl Pts',(22.1076253283979,11.3637775035367,0.));
#212942=CARTESIAN_POINT('Ctrl Pts',(22.1076253283979,11.3637775035367,12.));
#212943=CARTESIAN_POINT('Ctrl Pts',(22.0922559355294,11.3441037419553,0.));
#212944=CARTESIAN_POINT('Ctrl Pts',(22.0922559355294,11.3441037419553,12.));
#212945=CARTESIAN_POINT('Ctrl Pts',(22.0768902124267,11.3245315573168,0.));
#212946=CARTESIAN_POINT('Ctrl Pts',(22.0768902124267,11.3245315573168,12.));
#212947=CARTESIAN_POINT('Ctrl Pts',(22.0615287047179,11.3050611878771,0.));
#212948=CARTESIAN_POINT('Ctrl Pts',(22.0615287047179,11.3050611878771,12.));
#212949=CARTESIAN_POINT('Ctrl Pts',(22.046171962566,11.2856928724374,0.));
#212950=CARTESIAN_POINT('Ctrl Pts',(22.046171962566,11.2856928724374,12.));
#212951=CARTESIAN_POINT('Ctrl Pts',(22.030820540835,11.2664268504206,0.));
#212952=CARTESIAN_POINT('Ctrl Pts',(22.030820540835,11.2664268504206,12.));
#212953=CARTESIAN_POINT('Ctrl Pts',(22.0154749992363,11.2472633619275,0.));
#212954=CARTESIAN_POINT('Ctrl Pts',(22.0154749992363,11.2472633619275,12.));
#212955=CARTESIAN_POINT('Ctrl Pts',(22.0001359024839,11.2282026477896,0.));
#212956=CARTESIAN_POINT('Ctrl Pts',(22.0001359024839,11.2282026477896,12.));
#212957=CARTESIAN_POINT('Ctrl Pts',(21.9848038204439,11.2092449496125,0.));
#212958=CARTESIAN_POINT('Ctrl Pts',(21.9848038204439,11.2092449496125,12.));
#212959=CARTESIAN_POINT('Ctrl Pts',(21.9694793282914,11.190390509811,0.));
#212960=CARTESIAN_POINT('Ctrl Pts',(21.9694793282914,11.190390509811,12.));
#212961=CARTESIAN_POINT('Ctrl Pts',(21.9541630066506,11.1716395716376,0.));
#212962=CARTESIAN_POINT('Ctrl Pts',(21.9541630066506,11.1716395716376,12.));
#212963=CARTESIAN_POINT('Ctrl Pts',(21.9388554416439,11.1529923792003,0.));
#212964=CARTESIAN_POINT('Ctrl Pts',(21.9388554416439,11.1529923792003,12.));
#212965=CARTESIAN_POINT('Ctrl Pts',(21.923557224952,11.1344491774741,0.));
#212966=CARTESIAN_POINT('Ctrl Pts',(21.923557224952,11.1344491774741,12.));
#212967=CARTESIAN_POINT('Ctrl Pts',(21.9082689538688,11.1160102123024,0.));
#212968=CARTESIAN_POINT('Ctrl Pts',(21.9082689538688,11.1160102123024,12.));
#212969=CARTESIAN_POINT('Ctrl Pts',(21.8929912313608,11.0976757303944,0.));
#212970=CARTESIAN_POINT('Ctrl Pts',(21.8929912313608,11.0976757303944,12.));
#212971=CARTESIAN_POINT('Ctrl Pts',(21.877724666119,11.0794459793057,0.));
#212972=CARTESIAN_POINT('Ctrl Pts',(21.877724666119,11.0794459793057,12.));
#212973=CARTESIAN_POINT('Ctrl Pts',(21.8624698726318,11.0613212074363,0.));
#212974=CARTESIAN_POINT('Ctrl Pts',(21.8624698726318,11.0613212074363,12.));
#212975=CARTESIAN_POINT('Ctrl Pts',(21.8472274713103,11.0433016640807,0.));
#212976=CARTESIAN_POINT('Ctrl Pts',(21.8472274713103,11.0433016640807,12.));
#212977=CARTESIAN_POINT('Ctrl Pts',(21.8319980886033,11.0253875994598,0.));
#212978=CARTESIAN_POINT('Ctrl Pts',(21.8319980886033,11.0253875994598,12.));
#212979=CARTESIAN_POINT('Ctrl Pts',(21.8167823571168,11.0075792647477,0.));
#212980=CARTESIAN_POINT('Ctrl Pts',(21.8167823571168,11.0075792647477,12.));
#212981=CARTESIAN_POINT('Ctrl Pts',(21.8015809157301,10.9898769120912,0.));
#212982=CARTESIAN_POINT('Ctrl Pts',(21.8015809157301,10.9898769120912,12.));
#212983=CARTESIAN_POINT('Ctrl Pts',(21.7863944097141,10.9722807946156,0.));
#212984=CARTESIAN_POINT('Ctrl Pts',(21.7863944097141,10.9722807946156,12.));
#212985=CARTESIAN_POINT('Ctrl Pts',(21.7712234908464,10.9547911664455,0.));
#212986=CARTESIAN_POINT('Ctrl Pts',(21.7712234908464,10.9547911664455,12.));
#212987=CARTESIAN_POINT('Ctrl Pts',(21.7560688175247,10.9374082827444,0.));
#212988=CARTESIAN_POINT('Ctrl Pts',(21.7560688175247,10.9374082827444,12.));
#212989=CARTESIAN_POINT('Ctrl Pts',(21.7409310548797,10.9201323997384,0.));
#212990=CARTESIAN_POINT('Ctrl Pts',(21.7409310548797,10.9201323997384,12.));
#212991=CARTESIAN_POINT('Ctrl Pts',(21.7258108748873,10.902963774734,0.));
#212992=CARTESIAN_POINT('Ctrl Pts',(21.7258108748873,10.902963774734,12.));
#212993=CARTESIAN_POINT('Ctrl Pts',(21.7107089564825,10.8859026661293,0.));
#212994=CARTESIAN_POINT('Ctrl Pts',(21.7107089564825,10.8859026661293,12.));
#212995=CARTESIAN_POINT('Ctrl Pts',(21.6956259856672,10.8689493334095,0.));
#212996=CARTESIAN_POINT('Ctrl Pts',(21.6956259856672,10.8689493334095,12.));
#212997=CARTESIAN_POINT('Ctrl Pts',(21.6805626556467,10.8521040371835,0.));
#212998=CARTESIAN_POINT('Ctrl Pts',(21.6805626556467,10.8521040371835,12.));
#212999=CARTESIAN_POINT('Ctrl Pts',(21.6655196669732,10.8353670392272,0.));
#213000=CARTESIAN_POINT('Ctrl Pts',(21.6655196669732,10.8353670392272,12.));
#213001=CARTESIAN_POINT('Ctrl Pts',(21.6504977276866,10.8187386025136,0.));
#213002=CARTESIAN_POINT('Ctrl Pts',(21.6504977276866,10.8187386025136,12.));
#213003=CARTESIAN_POINT('Ctrl Pts',(21.6354975534557,10.8022189912369,0.));
#213004=CARTESIAN_POINT('Ctrl Pts',(21.6354975534557,10.8022189912369,12.));
#213005=CARTESIAN_POINT('Ctrl Pts',(21.6205198677173,10.7858084708261,0.));
#213006=CARTESIAN_POINT('Ctrl Pts',(21.6205198677173,10.7858084708261,12.));
#213007=CARTESIAN_POINT('Ctrl Pts',(21.6055654018176,10.7695073079552,0.));
#213008=CARTESIAN_POINT('Ctrl Pts',(21.6055654018176,10.7695073079552,12.));
#213009=CARTESIAN_POINT('Ctrl Pts',(21.5906348951743,10.7533157705941,0.));
#213010=CARTESIAN_POINT('Ctrl Pts',(21.5906348951743,10.7533157705941,12.));
#213011=CARTESIAN_POINT('Ctrl Pts',(21.5757290954371,10.7372341280467,0.));
#213012=CARTESIAN_POINT('Ctrl Pts',(21.5757290954371,10.7372341280467,12.));
#213013=CARTESIAN_POINT('Ctrl Pts',(21.5608487586468,10.7212626509816,0.));
#213014=CARTESIAN_POINT('Ctrl Pts',(21.5608487586468,10.7212626509816,12.));
#213015=CARTESIAN_POINT('Ctrl Pts',(21.5459946493955,10.7054016114571,0.));
#213016=CARTESIAN_POINT('Ctrl Pts',(21.5459946493955,10.7054016114571,12.));
#213017=CARTESIAN_POINT('Ctrl Pts',(21.5311675409807,10.689651282929,0.));
#213018=CARTESIAN_POINT('Ctrl Pts',(21.5311675409807,10.689651282929,12.));
#213019=CARTESIAN_POINT('Ctrl Pts',(21.51636821558,10.6740119402834,0.));
#213020=CARTESIAN_POINT('Ctrl Pts',(21.51636821558,10.6740119402834,12.));
#213021=CARTESIAN_POINT('Ctrl Pts',(21.5015974644449,10.6584838598939,0.));
#213022=CARTESIAN_POINT('Ctrl Pts',(21.5015974644449,10.6584838598939,12.));
#213023=CARTESIAN_POINT('Ctrl Pts',(21.4868560880889,10.6430673196607,0.));
#213024=CARTESIAN_POINT('Ctrl Pts',(21.4868560880889,10.6430673196607,12.));
#213025=CARTESIAN_POINT('Ctrl Pts',(21.4721448964766,10.6277625990456,0.));
#213026=CARTESIAN_POINT('Ctrl Pts',(21.4721448964766,10.6277625990456,12.));
#213027=CARTESIAN_POINT('Ctrl Pts',(21.4574647092097,10.6125699790961,0.));
#213028=CARTESIAN_POINT('Ctrl Pts',(21.4574647092097,10.6125699790961,12.));
#213029=CARTESIAN_POINT('Ctrl Pts',(21.4428163557144,10.5974897424622,0.));
#213030=CARTESIAN_POINT('Ctrl Pts',(21.4428163557144,10.5974897424622,12.));
#213031=CARTESIAN_POINT('Ctrl Pts',(21.4282006754631,10.5825221734573,0.));
#213032=CARTESIAN_POINT('Ctrl Pts',(21.4282006754631,10.5825221734573,12.));
#213033=CARTESIAN_POINT('Ctrl Pts',(21.4136185181979,10.5676675581108,0.));
#213034=CARTESIAN_POINT('Ctrl Pts',(21.4136185181979,10.5676675581108,12.));
#213035=CARTESIAN_POINT('Ctrl Pts',(21.3990707441497,10.5529261842108,0.));
#213036=CARTESIAN_POINT('Ctrl Pts',(21.3990707441497,10.5529261842108,12.));
#213037=CARTESIAN_POINT('Ctrl Pts',(21.3845582242602,10.5382983413421,0.));
#213038=CARTESIAN_POINT('Ctrl Pts',(21.3845582242602,10.5382983413421,12.));
#213039=CARTESIAN_POINT('Ctrl Pts',(21.3700818403936,10.5237843209057,0.));
#213040=CARTESIAN_POINT('Ctrl Pts',(21.3700818403936,10.5237843209057,12.));
#213041=CARTESIAN_POINT('Ctrl Pts',(21.3556424855814,10.5093844161685,0.));
#213042=CARTESIAN_POINT('Ctrl Pts',(21.3556424855814,10.5093844161685,12.));
#213043=CARTESIAN_POINT('Ctrl Pts',(21.3412410642904,10.4950989223337,0.));
#213044=CARTESIAN_POINT('Ctrl Pts',(21.3412410642904,10.4950989223337,12.));
#213045=CARTESIAN_POINT('Ctrl Pts',(21.3268784926819,10.4809281365931,0.));
#213046=CARTESIAN_POINT('Ctrl Pts',(21.3268784926819,10.4809281365931,12.));
#213047=CARTESIAN_POINT('Ctrl Pts',(21.3125556988731,10.4668723581768,0.));
#213048=CARTESIAN_POINT('Ctrl Pts',(21.3125556988731,10.4668723581768,12.));
#213049=CARTESIAN_POINT('Ctrl Pts',(21.2982736231931,10.4529318883874,0.));
#213050=CARTESIAN_POINT('Ctrl Pts',(21.2982736231931,10.4529318883874,12.));
#213051=CARTESIAN_POINT('Ctrl Pts',(21.2840332184483,10.4391070306391,0.));
#213052=CARTESIAN_POINT('Ctrl Pts',(21.2840332184483,10.4391070306391,12.));
#213053=CARTESIAN_POINT('Ctrl Pts',(21.2698354502403,10.42539809054,0.));
#213054=CARTESIAN_POINT('Ctrl Pts',(21.2698354502403,10.42539809054,12.));
#213055=CARTESIAN_POINT('Ctrl Pts',(21.255681297275,10.4118053759588,0.));
#213056=CARTESIAN_POINT('Ctrl Pts',(21.255681297275,10.4118053759588,12.));
#213057=CARTESIAN_POINT('Ctrl Pts',(21.2415717516714,10.3983291970846,0.));
#213058=CARTESIAN_POINT('Ctrl Pts',(21.2415717516714,10.3983291970846,12.));
#213059=CARTESIAN_POINT('Ctrl Pts',(21.22750781927,10.3849698664786,0.));
#213060=CARTESIAN_POINT('Ctrl Pts',(21.22750781927,10.3849698664786,12.));
#213061=CARTESIAN_POINT('Ctrl Pts',(21.2134905199345,10.371727699113,0.));
#213062=CARTESIAN_POINT('Ctrl Pts',(21.2134905199345,10.371727699113,12.));
#213063=CARTESIAN_POINT('Ctrl Pts',(21.199520887919,10.3586030124587,0.));
#213064=CARTESIAN_POINT('Ctrl Pts',(21.199520887919,10.3586030124587,12.));
#213065=CARTESIAN_POINT('Ctrl Pts',(21.1855999722416,10.3455961265701,0.));
#213066=CARTESIAN_POINT('Ctrl Pts',(21.1855999722416,10.3455961265701,12.));
#213067=CARTESIAN_POINT('Ctrl Pts',(21.1717288370509,10.3327073641572,0.));
#213068=CARTESIAN_POINT('Ctrl Pts',(21.1717288370509,10.3327073641572,12.));
#213069=CARTESIAN_POINT('Ctrl Pts',(21.1579085619965,10.3199370506544,0.));
#213070=CARTESIAN_POINT('Ctrl Pts',(21.1579085619965,10.3199370506544,12.));
#213071=CARTESIAN_POINT('Ctrl Pts',(21.1441402425843,10.3072855142687,0.));
#213072=CARTESIAN_POINT('Ctrl Pts',(21.1441402425843,10.3072855142687,12.));
#213073=CARTESIAN_POINT('Ctrl Pts',(21.1304249906002,10.2947530860721,0.));
#213074=CARTESIAN_POINT('Ctrl Pts',(21.1304249906002,10.2947530860721,12.));
#213075=CARTESIAN_POINT('Ctrl Pts',(21.1167639345631,10.2823401001072,0.));
#213076=CARTESIAN_POINT('Ctrl Pts',(21.1167639345631,10.2823401001072,12.));
#213077=CARTESIAN_POINT('Ctrl Pts',(21.1031582201627,10.2700468934744,0.));
#213078=CARTESIAN_POINT('Ctrl Pts',(21.1031582201627,10.2700468934744,12.));
#213079=CARTESIAN_POINT('Ctrl Pts',(21.0896090107063,10.2578738064181,0.));
#213080=CARTESIAN_POINT('Ctrl Pts',(21.0896090107063,10.2578738064181,12.));
#213081=CARTESIAN_POINT('Ctrl Pts',(21.0761174875444,10.2458211823912,0.));
#213082=CARTESIAN_POINT('Ctrl Pts',(21.0761174875444,10.2458211823912,12.));
#213083=CARTESIAN_POINT('Ctrl Pts',(21.0626848505663,10.2338893681567,0.));
#213084=CARTESIAN_POINT('Ctrl Pts',(21.0626848505663,10.2338893681567,12.));
#213085=CARTESIAN_POINT('Ctrl Pts',(21.0493123187483,10.2220787139155,0.));
#213086=CARTESIAN_POINT('Ctrl Pts',(21.0493123187483,10.2220787139155,12.));
#213087=CARTESIAN_POINT('Ctrl Pts',(21.0360011306815,10.2103895734123,0.));
#213088=CARTESIAN_POINT('Ctrl Pts',(21.0360011306815,10.2103895734123,12.));
#213089=CARTESIAN_POINT('Ctrl Pts',(21.0227525451107,10.1988223040425,0.));
#213090=CARTESIAN_POINT('Ctrl Pts',(21.0227525451107,10.1988223040425,12.));
#213091=CARTESIAN_POINT('Ctrl Pts',(21.0095678414486,10.187377266936,0.));
#213092=CARTESIAN_POINT('Ctrl Pts',(21.0095678414486,10.187377266936,12.));
#213093=CARTESIAN_POINT('Ctrl Pts',(20.9964483203686,10.1760548270767,0.));
#213094=CARTESIAN_POINT('Ctrl Pts',(20.9964483203686,10.1760548270767,12.));
#213095=CARTESIAN_POINT('Ctrl Pts',(20.9833953044736,10.1648553534568,0.));
#213096=CARTESIAN_POINT('Ctrl Pts',(20.9833953044736,10.1648553534568,12.));
#213097=CARTESIAN_POINT('Ctrl Pts',(20.9704101389369,10.1537792192065,0.));
#213098=CARTESIAN_POINT('Ctrl Pts',(20.9704101389369,10.1537792192065,12.));
#213099=CARTESIAN_POINT('Ctrl Pts',(20.9574941921591,10.1428268017256,0.));
#213100=CARTESIAN_POINT('Ctrl Pts',(20.9574941921591,10.1428268017256,12.));
#213101=CARTESIAN_POINT('Ctrl Pts',(20.9446488563933,10.1319984827908,0.));
#213102=CARTESIAN_POINT('Ctrl Pts',(20.9446488563933,10.1319984827908,12.));
#213103=CARTESIAN_POINT('Ctrl Pts',(20.9318755484734,10.1212946487057,0.));
#213104=CARTESIAN_POINT('Ctrl Pts',(20.9318755484734,10.1212946487057,12.));
#213105=CARTESIAN_POINT('Ctrl Pts',(20.919175710627,10.1107156904836,0.));
#213106=CARTESIAN_POINT('Ctrl Pts',(20.919175710627,10.1107156904836,12.));
#213107=CARTESIAN_POINT('Ctrl Pts',(20.9065508112557,10.1002620040076,0.));
#213108=CARTESIAN_POINT('Ctrl Pts',(20.9065508112557,10.1002620040076,12.));
#213109=CARTESIAN_POINT('Ctrl Pts',(20.894002345737,10.0899339901916,0.));
#213110=CARTESIAN_POINT('Ctrl Pts',(20.894002345737,10.0899339901916,12.));
#213111=CARTESIAN_POINT('Ctrl Pts',(20.881531837184,10.0797320551154,0.));
#213112=CARTESIAN_POINT('Ctrl Pts',(20.881531837184,10.0797320551154,12.));
#213113=CARTESIAN_POINT('Ctrl Pts',(20.86914083737,10.0696566102218,0.));
#213114=CARTESIAN_POINT('Ctrl Pts',(20.86914083737,10.0696566102218,12.));
#213115=CARTESIAN_POINT('Ctrl Pts',(20.8568309277316,10.0597080725375,0.));
#213116=CARTESIAN_POINT('Ctrl Pts',(20.8568309277316,10.0597080725375,12.));
#213117=CARTESIAN_POINT('Ctrl Pts',(20.8446037203402,10.0498868648733,0.));
#213118=CARTESIAN_POINT('Ctrl Pts',(20.8446037203402,10.0498868648733,12.));
#213119=CARTESIAN_POINT('Ctrl Pts',(20.8324608588909,10.0401934160234,0.));
#213120=CARTESIAN_POINT('Ctrl Pts',(20.8324608588909,10.0401934160234,12.));
#213121=CARTESIAN_POINT('Ctrl Pts',(20.8204040196602,10.0306281609435,0.));
#213122=CARTESIAN_POINT('Ctrl Pts',(20.8204040196602,10.0306281609435,12.));
#213123=CARTESIAN_POINT('Ctrl Pts',(20.8084349126888,10.0211915410095,0.));
#213124=CARTESIAN_POINT('Ctrl Pts',(20.8084349126888,10.0211915410095,12.));
#213125=CARTESIAN_POINT('Ctrl Pts',(20.7965552829908,10.0118840042786,0.));
#213126=CARTESIAN_POINT('Ctrl Pts',(20.7965552829908,10.0118840042786,12.));
#213127=CARTESIAN_POINT('Ctrl Pts',(20.7847669117568,10.0027060057389,0.));
#213128=CARTESIAN_POINT('Ctrl Pts',(20.7847669117568,10.0027060057389,12.));
#213129=CARTESIAN_POINT('Ctrl Pts',(20.7730716175417,9.9936580075464,0.));
#213130=CARTESIAN_POINT('Ctrl Pts',(20.7730716175417,9.9936580075464,12.));
#213131=CARTESIAN_POINT('Ctrl Pts',(20.761471257499,9.98474047926853,0.));
#213132=CARTESIAN_POINT('Ctrl Pts',(20.761471257499,9.98474047926853,12.));
#213133=CARTESIAN_POINT('Ctrl Pts',(20.7499677289627,9.9759538982347,0.));
#213134=CARTESIAN_POINT('Ctrl Pts',(20.7499677289627,9.9759538982347,12.));
#213135=CARTESIAN_POINT('Ctrl Pts',(20.7385629709795,9.96729874986202,0.));
#213136=CARTESIAN_POINT('Ctrl Pts',(20.7385629709795,9.96729874986202,12.));
#213137=CARTESIAN_POINT('Ctrl Pts',(20.7272589658751,9.95877552798398,0.));
#213138=CARTESIAN_POINT('Ctrl Pts',(20.7272589658751,9.95877552798398,12.));
#213139=CARTESIAN_POINT('Ctrl Pts',(20.7160577407579,9.95038473514949,0.));
#213140=CARTESIAN_POINT('Ctrl Pts',(20.7160577407579,9.95038473514949,12.));
#213141=CARTESIAN_POINT('Ctrl Pts',(20.7049613692234,9.94212688298236,0.));
#213142=CARTESIAN_POINT('Ctrl Pts',(20.7049613692234,9.94212688298236,12.));
#213143=CARTESIAN_POINT('Ctrl Pts',(20.6939719732484,9.9340024925973,0.));
#213144=CARTESIAN_POINT('Ctrl Pts',(20.6939719732484,9.9340024925973,12.));
#213145=CARTESIAN_POINT('Ctrl Pts',(20.6830917250255,9.92601209498749,0.));
#213146=CARTESIAN_POINT('Ctrl Pts',(20.6830917250255,9.92601209498749,12.));
#213147=CARTESIAN_POINT('Ctrl Pts',(20.6723228488263,9.91815623141289,0.));
#213148=CARTESIAN_POINT('Ctrl Pts',(20.6723228488263,9.91815623141289,12.));
#213149=CARTESIAN_POINT('Ctrl Pts',(20.6616676228315,9.91043545377008,0.));
#213150=CARTESIAN_POINT('Ctrl Pts',(20.6616676228315,9.91043545377008,12.));
#213151=CARTESIAN_POINT('Ctrl Pts',(20.6511283817414,9.90285032516693,0.));
#213152=CARTESIAN_POINT('Ctrl Pts',(20.6511283817414,9.90285032516693,12.));
#213153=CARTESIAN_POINT('Ctrl Pts',(20.6407075193976,9.8954014204912,0.));
#213154=CARTESIAN_POINT('Ctrl Pts',(20.6407075193976,9.8954014204912,12.));
#213155=CARTESIAN_POINT('Ctrl Pts',(20.6304074914087,9.88808932697306,0.));
#213156=CARTESIAN_POINT('Ctrl Pts',(20.6304074914087,9.88808932697306,12.));
#213157=CARTESIAN_POINT('Ctrl Pts',(20.6202308177474,9.88091464472676,0.));
#213158=CARTESIAN_POINT('Ctrl Pts',(20.6202308177474,9.88091464472676,12.));
#213159=CARTESIAN_POINT('Ctrl Pts',(20.6101800854494,9.87387798732956,0.));
#213160=CARTESIAN_POINT('Ctrl Pts',(20.6101800854494,9.87387798732956,12.));
#213161=CARTESIAN_POINT('Ctrl Pts',(20.6002579513699,9.86697998242623,0.));
#213162=CARTESIAN_POINT('Ctrl Pts',(20.6002579513699,9.86697998242623,12.));
#213163=CARTESIAN_POINT('Ctrl Pts',(20.5904671449754,9.86022127232748,0.));
#213164=CARTESIAN_POINT('Ctrl Pts',(20.5904671449754,9.86022127232748,12.));
#213165=CARTESIAN_POINT('Ctrl Pts',(20.5808104710015,9.85360251456981,0.));
#213166=CARTESIAN_POINT('Ctrl Pts',(20.5808104710015,9.85360251456981,12.));
#213167=CARTESIAN_POINT('Ctrl Pts',(20.5712908125139,9.84712438256278,0.));
#213168=CARTESIAN_POINT('Ctrl Pts',(20.5712908125139,9.84712438256278,12.));
#213169=CARTESIAN_POINT('Ctrl Pts',(20.5619111362402,9.84078756677565,0.));
#213170=CARTESIAN_POINT('Ctrl Pts',(20.5619111362402,9.84078756677565,12.));
#213171=CARTESIAN_POINT('Ctrl Pts',(20.552674497646,9.83459277585315,0.));
#213172=CARTESIAN_POINT('Ctrl Pts',(20.552674497646,9.83459277585315,12.));
#213173=CARTESIAN_POINT('Ctrl Pts',(20.5435840460721,9.82854073773878,0.));
#213174=CARTESIAN_POINT('Ctrl Pts',(20.5435840460721,9.82854073773878,12.));
#213175=CARTESIAN_POINT('Ctrl Pts',(20.5346430299517,9.82263220080363,0.));
#213176=CARTESIAN_POINT('Ctrl Pts',(20.5346430299517,9.82263220080363,12.));
#213177=CARTESIAN_POINT('Ctrl Pts',(20.5258548000629,9.81686793455943,0.));
#213178=CARTESIAN_POINT('Ctrl Pts',(20.5258548000629,9.81686793455943,12.));
#213179=CARTESIAN_POINT('Ctrl Pts',(20.517222812284,9.81124873025282,0.));
#213180=CARTESIAN_POINT('Ctrl Pts',(20.517222812284,9.81124873025282,12.));
#213181=CARTESIAN_POINT('Ctrl Pts',(20.5087506310505,9.80577540161088,0.));
#213182=CARTESIAN_POINT('Ctrl Pts',(20.5087506310505,9.80577540161088,12.));
#213183=CARTESIAN_POINT('Ctrl Pts',(20.5004419312107,9.80044878520949,0.));
#213184=CARTESIAN_POINT('Ctrl Pts',(20.5004419312107,9.80044878520949,12.));
#213185=CARTESIAN_POINT('Ctrl Pts',(20.4923005087943,9.79526974288331,0.));
#213186=CARTESIAN_POINT('Ctrl Pts',(20.4923005087943,9.79526974288331,12.));
#213187=CARTESIAN_POINT('Ctrl Pts',(20.4843302955329,9.79023916498656,0.));
#213188=CARTESIAN_POINT('Ctrl Pts',(20.4843302955329,9.79023916498656,12.));
#213189=CARTESIAN_POINT('Ctrl Pts',(20.4765353711586,9.78535797314167,0.));
#213190=CARTESIAN_POINT('Ctrl Pts',(20.4765353711586,9.78535797314167,12.));
#213191=CARTESIAN_POINT('Ctrl Pts',(20.4689199790669,9.78062712373321,0.));
#213192=CARTESIAN_POINT('Ctrl Pts',(20.4689199790669,9.78062712373321,12.));
#213193=CARTESIAN_POINT('Ctrl Pts',(20.4614885274975,9.77604760815529,0.));
#213194=CARTESIAN_POINT('Ctrl Pts',(20.4614885274975,9.77604760815529,12.));
#213195=CARTESIAN_POINT('Ctrl Pts',(20.4542455817527,9.7716204510407,0.));
#213196=CARTESIAN_POINT('Ctrl Pts',(20.4542455817527,9.7716204510407,12.));
#213197=CARTESIAN_POINT('Ctrl Pts',(20.447195862298,9.76734670980892,0.));
#213198=CARTESIAN_POINT('Ctrl Pts',(20.447195862298,9.76734670980892,12.));
#213199=CARTESIAN_POINT('Ctrl Pts',(20.44034423294,9.76322747195495,0.));
#213200=CARTESIAN_POINT('Ctrl Pts',(20.44034423294,9.76322747195495,12.));
#213201=CARTESIAN_POINT('Ctrl Pts',(20.4336957355473,9.75926386289923,0.));
#213202=CARTESIAN_POINT('Ctrl Pts',(20.4336957355473,9.75926386289923,12.));
#213203=CARTESIAN_POINT('Ctrl Pts',(20.4272556476629,9.75545705902418,0.));
#213204=CARTESIAN_POINT('Ctrl Pts',(20.4272556476629,9.75545705902418,12.));
#213205=CARTESIAN_POINT('Ctrl Pts',(20.4210295275817,9.7518082978643,0.));
#213206=CARTESIAN_POINT('Ctrl Pts',(20.4210295275817,9.7518082978643,12.));
#213207=CARTESIAN_POINT('Ctrl Pts',(20.4150232777393,9.74831889242174,0.));
#213208=CARTESIAN_POINT('Ctrl Pts',(20.4150232777393,9.74831889242174,12.));
#213209=CARTESIAN_POINT('Ctrl Pts',(20.4092430879861,9.74499021838538,0.));
#213210=CARTESIAN_POINT('Ctrl Pts',(20.4092430879861,9.74499021838538,12.));
#213211=CARTESIAN_POINT('Ctrl Pts',(20.4036953576549,9.74182369656272,0.));
#213212=CARTESIAN_POINT('Ctrl Pts',(20.4036953576549,9.74182369656272,12.));
#213213=CARTESIAN_POINT('Ctrl Pts',(20.3983866213331,9.73882077613201,0.));
#213214=CARTESIAN_POINT('Ctrl Pts',(20.3983866213331,9.73882077613201,12.));
#213215=CARTESIAN_POINT('Ctrl Pts',(20.3933234845647,9.73598292014243,0.));
#213216=CARTESIAN_POINT('Ctrl Pts',(20.3933234845647,9.73598292014243,12.));
#213217=CARTESIAN_POINT('Ctrl Pts',(20.3885129129912,9.73331167102808,0.));
#213218=CARTESIAN_POINT('Ctrl Pts',(20.3885129129912,9.73331167102808,12.));
#213219=CARTESIAN_POINT('Ctrl Pts',(20.3839624556742,9.73080870123727,0.));
#213220=CARTESIAN_POINT('Ctrl Pts',(20.3839624556742,9.73080870123727,12.));
#213221=CARTESIAN_POINT('Ctrl Pts',(20.3796805893304,9.72847589116542,0.));
#213222=CARTESIAN_POINT('Ctrl Pts',(20.3796805893304,9.72847589116542,12.));
#213223=CARTESIAN_POINT('Ctrl Pts',(20.3756766651951,9.72631531732881,0.));
#213224=CARTESIAN_POINT('Ctrl Pts',(20.3756766651951,9.72631531732881,12.));
#213225=CARTESIAN_POINT('Ctrl Pts',(20.371960235676,9.72432910043194,0.));
#213226=CARTESIAN_POINT('Ctrl Pts',(20.371960235676,9.72432910043194,12.));
#213227=CARTESIAN_POINT('Ctrl Pts',(20.3685406190576,9.7225193072249,0.));
#213228=CARTESIAN_POINT('Ctrl Pts',(20.3685406190576,9.7225193072249,12.));
#213229=CARTESIAN_POINT('Ctrl Pts',(20.3654261611056,9.72088778381081,0.));
#213230=CARTESIAN_POINT('Ctrl Pts',(20.3654261611056,9.72088778381081,12.));
#213231=CARTESIAN_POINT('Ctrl Pts',(20.3626256913981,9.71943648548099,0.));
#213232=CARTESIAN_POINT('Ctrl Pts',(20.3626256913981,9.71943648548099,12.));
#213233=CARTESIAN_POINT('Ctrl Pts',(20.3601498764344,9.71816778328007,0.));
#213234=CARTESIAN_POINT('Ctrl Pts',(20.3601498764344,9.71816778328007,12.));
#213235=CARTESIAN_POINT('Ctrl Pts',(20.3580133103356,9.71708493723096,0.));
#213236=CARTESIAN_POINT('Ctrl Pts',(20.3580133103356,9.71708493723096,12.));
#213237=CARTESIAN_POINT('Ctrl Pts',(20.3562337557875,9.71619192554186,0.));
#213238=CARTESIAN_POINT('Ctrl Pts',(20.3562337557875,9.71619192554186,12.));
#213239=CARTESIAN_POINT('Ctrl Pts',(20.3548282742361,9.71549257088173,0.));
#213240=CARTESIAN_POINT('Ctrl Pts',(20.3548282742361,9.71549257088173,12.));
#213241=CARTESIAN_POINT('Ctrl Pts',(20.3538098605706,9.71498978052021,0.));
#213242=CARTESIAN_POINT('Ctrl Pts',(20.3538098605706,9.71498978052021,12.));
#213243=CARTESIAN_POINT('Ctrl Pts',(20.3533097561886,9.71474590350681,0.));
#213244=CARTESIAN_POINT('Ctrl Pts',(20.3533097561886,9.71474590350681,12.));
#213245=CARTESIAN_POINT('Ctrl Pts',(20.3531126095522,9.71465227853042,0.));
#213246=CARTESIAN_POINT('Ctrl Pts',(20.3531126095522,9.71465227853042,12.));
#213247=CARTESIAN_POINT('Ctrl Pts',(20.353060251684,9.71462954053042,0.));
#213248=CARTESIAN_POINT('Ctrl Pts',(20.353060251684,9.71462954053042,12.));
#213249=CARTESIAN_POINT('Ctrl Pts',(20.353053841303,9.71462809124916,0.));
#213250=CARTESIAN_POINT('Ctrl Pts',(20.353053841303,9.71462809124916,12.));
#213251=CARTESIAN_POINT('',(22.8400320311648,12.4230808101438,0.));
#213252=CARTESIAN_POINT('Ctrl Pts',(22.8400320311648,12.4230808101438,0.));
#213253=CARTESIAN_POINT('Ctrl Pts',(22.8370364396459,12.418215285186,0.));
#213254=CARTESIAN_POINT('Ctrl Pts',(22.8310435872747,12.4084933766347,0.));
#213255=CARTESIAN_POINT('Ctrl Pts',(22.8220493007173,12.3939379378998,0.));
#213256=CARTESIAN_POINT('Ctrl Pts',(22.81004690224,12.374585536673,0.));
#213257=CARTESIAN_POINT('Ctrl Pts',(22.795027221673,12.3504864740319,0.));
#213258=CARTESIAN_POINT('Ctrl Pts',(22.7799908974768,12.3264788926075,0.));
#213259=CARTESIAN_POINT('Ctrl Pts',(22.764938010105,12.3025628601792,0.));
#213260=CARTESIAN_POINT('Ctrl Pts',(22.7498686970069,12.2787384750742,0.));
#213261=CARTESIAN_POINT('Ctrl Pts',(22.7347831655287,12.2550058702395,0.));
#213262=CARTESIAN_POINT('Ctrl Pts',(22.7196817119374,12.2313652198061,0.));
#213263=CARTESIAN_POINT('Ctrl Pts',(22.7045647168747,12.2078167360284,0.));
#213264=CARTESIAN_POINT('Ctrl Pts',(22.6894326205037,12.1843606579262,0.));
#213265=CARTESIAN_POINT('Ctrl Pts',(22.6742859034944,12.1609972423099,0.));
#213266=CARTESIAN_POINT('Ctrl Pts',(22.6591250653965,12.1377267537145,0.));
#213267=CARTESIAN_POINT('Ctrl Pts',(22.6439506046605,12.1145494550383,0.));
#213268=CARTESIAN_POINT('Ctrl Pts',(22.6287629967056,12.0914655972823,0.));
#213269=CARTESIAN_POINT('Ctrl Pts',(22.6135626764898,12.0684754113862,0.));
#213270=CARTESIAN_POINT('Ctrl Pts',(22.5983500505644,12.0455791139128,0.));
#213271=CARTESIAN_POINT('Ctrl Pts',(22.5831255061282,12.0227769113127,0.));
#213272=CARTESIAN_POINT('Ctrl Pts',(22.5678894211181,12.0000690046695,0.));
#213273=CARTESIAN_POINT('Ctrl Pts',(22.5526421741158,11.9774555943496,0.));
#213274=CARTESIAN_POINT('Ctrl Pts',(22.5373841537307,11.9549368843997,0.));
#213275=CARTESIAN_POINT('Ctrl Pts',(22.5221157697883,11.9325130877803,0.));
#213276=CARTESIAN_POINT('Ctrl Pts',(22.5068374513973,11.9101844254557,0.));
#213277=CARTESIAN_POINT('Ctrl Pts',(22.4915496418485,11.8879511239943,0.));
#213278=CARTESIAN_POINT('Ctrl Pts',(22.4762527946702,11.8658134137019,0.));
#213279=CARTESIAN_POINT('Ctrl Pts',(22.4609473690471,11.8437715264487,0.));
#213280=CARTESIAN_POINT('Ctrl Pts',(22.4456338258735,11.8218256937889,0.));
#213281=CARTESIAN_POINT('Ctrl Pts',(22.430312622646,11.7999761445173,0.));
#213282=CARTESIAN_POINT('Ctrl Pts',(22.4149842125008,11.7782231042039,0.));
#213283=CARTESIAN_POINT('Ctrl Pts',(22.3996490469191,11.7565667964764,0.));
#213284=CARTESIAN_POINT('Ctrl Pts',(22.3843075773899,11.7350074437961,0.));
#213285=CARTESIAN_POINT('Ctrl Pts',(22.3689602575491,11.7135452684532,0.));
#213286=CARTESIAN_POINT('Ctrl Pts',(22.3536075450029,11.6921804934056,0.));
#213287=CARTESIAN_POINT('Ctrl Pts',(22.3382499035619,11.6709133432985,0.));
#213288=CARTESIAN_POINT('Ctrl Pts',(22.3228878043976,11.6497440449857,0.));
#213289=CARTESIAN_POINT('Ctrl Pts',(22.3075217249049,11.6286728270009,0.));
#213290=CARTESIAN_POINT('Ctrl Pts',(22.2921521480356,11.6076999192357,0.));
#213291=CARTESIAN_POINT('Ctrl Pts',(22.2767795614348,11.5868255525188,0.));
#213292=CARTESIAN_POINT('Ctrl Pts',(22.2614044566898,11.5660499582403,0.));
#213293=CARTESIAN_POINT('Ctrl Pts',(22.2460273284654,11.5453733679121,0.));
#213294=CARTESIAN_POINT('Ctrl Pts',(22.2306486738901,11.5247960128477,0.));
#213295=CARTESIAN_POINT('Ctrl Pts',(22.2152689931022,11.5043181244242,0.));
#213296=CARTESIAN_POINT('Ctrl Pts',(22.1998887896436,11.483939934259,0.));
#213297=CARTESIAN_POINT('Ctrl Pts',(22.184508570917,11.463661674411,0.));
#213298=CARTESIAN_POINT('Ctrl Pts',(22.1691288486096,11.443483577557,0.));
#213299=CARTESIAN_POINT('Ctrl Pts',(22.1537501391487,11.4234058771742,0.));
#213300=CARTESIAN_POINT('Ctrl Pts',(22.1383729640964,11.4034288076908,0.));
#213301=CARTESIAN_POINT('Ctrl Pts',(22.1229978500186,11.3835526044256,0.));
#213302=CARTESIAN_POINT('Ctrl Pts',(22.1076253283979,11.3637775035367,0.));
#213303=CARTESIAN_POINT('Ctrl Pts',(22.0922559355294,11.3441037419553,0.));
#213304=CARTESIAN_POINT('Ctrl Pts',(22.0768902124267,11.3245315573168,0.));
#213305=CARTESIAN_POINT('Ctrl Pts',(22.0615287047179,11.3050611878771,0.));
#213306=CARTESIAN_POINT('Ctrl Pts',(22.046171962566,11.2856928724374,0.));
#213307=CARTESIAN_POINT('Ctrl Pts',(22.030820540835,11.2664268504206,0.));
#213308=CARTESIAN_POINT('Ctrl Pts',(22.0154749992363,11.2472633619275,0.));
#213309=CARTESIAN_POINT('Ctrl Pts',(22.0001359024839,11.2282026477896,0.));
#213310=CARTESIAN_POINT('Ctrl Pts',(21.9848038204439,11.2092449496125,0.));
#213311=CARTESIAN_POINT('Ctrl Pts',(21.9694793282914,11.190390509811,0.));
#213312=CARTESIAN_POINT('Ctrl Pts',(21.9541630066506,11.1716395716376,0.));
#213313=CARTESIAN_POINT('Ctrl Pts',(21.9388554416439,11.1529923792003,0.));
#213314=CARTESIAN_POINT('Ctrl Pts',(21.923557224952,11.1344491774741,0.));
#213315=CARTESIAN_POINT('Ctrl Pts',(21.9082689538688,11.1160102123024,0.));
#213316=CARTESIAN_POINT('Ctrl Pts',(21.8929912313608,11.0976757303944,0.));
#213317=CARTESIAN_POINT('Ctrl Pts',(21.877724666119,11.0794459793057,0.));
#213318=CARTESIAN_POINT('Ctrl Pts',(21.8624698726318,11.0613212074363,0.));
#213319=CARTESIAN_POINT('Ctrl Pts',(21.8472274713103,11.0433016640807,0.));
#213320=CARTESIAN_POINT('Ctrl Pts',(21.8319980886033,11.0253875994598,0.));
#213321=CARTESIAN_POINT('Ctrl Pts',(21.8167823571168,11.0075792647477,0.));
#213322=CARTESIAN_POINT('Ctrl Pts',(21.8015809157301,10.9898769120912,0.));
#213323=CARTESIAN_POINT('Ctrl Pts',(21.7863944097141,10.9722807946156,0.));
#213324=CARTESIAN_POINT('Ctrl Pts',(21.7712234908464,10.9547911664455,0.));
#213325=CARTESIAN_POINT('Ctrl Pts',(21.7560688175247,10.9374082827444,0.));
#213326=CARTESIAN_POINT('Ctrl Pts',(21.7409310548797,10.9201323997384,0.));
#213327=CARTESIAN_POINT('Ctrl Pts',(21.7258108748873,10.902963774734,0.));
#213328=CARTESIAN_POINT('Ctrl Pts',(21.7107089564825,10.8859026661293,0.));
#213329=CARTESIAN_POINT('Ctrl Pts',(21.6956259856672,10.8689493334095,0.));
#213330=CARTESIAN_POINT('Ctrl Pts',(21.6805626556467,10.8521040371835,0.));
#213331=CARTESIAN_POINT('Ctrl Pts',(21.6655196669732,10.8353670392272,0.));
#213332=CARTESIAN_POINT('Ctrl Pts',(21.6504977276866,10.8187386025136,0.));
#213333=CARTESIAN_POINT('Ctrl Pts',(21.6354975534557,10.8022189912369,0.));
#213334=CARTESIAN_POINT('Ctrl Pts',(21.6205198677173,10.7858084708261,0.));
#213335=CARTESIAN_POINT('Ctrl Pts',(21.6055654018176,10.7695073079552,0.));
#213336=CARTESIAN_POINT('Ctrl Pts',(21.5906348951743,10.7533157705941,0.));
#213337=CARTESIAN_POINT('Ctrl Pts',(21.5757290954371,10.7372341280467,0.));
#213338=CARTESIAN_POINT('Ctrl Pts',(21.5608487586468,10.7212626509816,0.));
#213339=CARTESIAN_POINT('Ctrl Pts',(21.5459946493955,10.7054016114571,0.));
#213340=CARTESIAN_POINT('Ctrl Pts',(21.5311675409807,10.689651282929,0.));
#213341=CARTESIAN_POINT('Ctrl Pts',(21.51636821558,10.6740119402834,0.));
#213342=CARTESIAN_POINT('Ctrl Pts',(21.5015974644449,10.6584838598939,0.));
#213343=CARTESIAN_POINT('Ctrl Pts',(21.4868560880889,10.6430673196607,0.));
#213344=CARTESIAN_POINT('Ctrl Pts',(21.4721448964766,10.6277625990456,0.));
#213345=CARTESIAN_POINT('Ctrl Pts',(21.4574647092097,10.6125699790961,0.));
#213346=CARTESIAN_POINT('Ctrl Pts',(21.4428163557144,10.5974897424622,0.));
#213347=CARTESIAN_POINT('Ctrl Pts',(21.4282006754631,10.5825221734573,0.));
#213348=CARTESIAN_POINT('Ctrl Pts',(21.4136185181979,10.5676675581108,0.));
#213349=CARTESIAN_POINT('Ctrl Pts',(21.3990707441497,10.5529261842108,0.));
#213350=CARTESIAN_POINT('Ctrl Pts',(21.3845582242602,10.5382983413421,0.));
#213351=CARTESIAN_POINT('Ctrl Pts',(21.3700818403936,10.5237843209057,0.));
#213352=CARTESIAN_POINT('Ctrl Pts',(21.3556424855814,10.5093844161685,0.));
#213353=CARTESIAN_POINT('Ctrl Pts',(21.3412410642904,10.4950989223337,0.));
#213354=CARTESIAN_POINT('Ctrl Pts',(21.3268784926819,10.4809281365931,0.));
#213355=CARTESIAN_POINT('Ctrl Pts',(21.3125556988731,10.4668723581768,0.));
#213356=CARTESIAN_POINT('Ctrl Pts',(21.2982736231931,10.4529318883874,0.));
#213357=CARTESIAN_POINT('Ctrl Pts',(21.2840332184483,10.4391070306391,0.));
#213358=CARTESIAN_POINT('Ctrl Pts',(21.2698354502403,10.42539809054,0.));
#213359=CARTESIAN_POINT('Ctrl Pts',(21.255681297275,10.4118053759588,0.));
#213360=CARTESIAN_POINT('Ctrl Pts',(21.2415717516714,10.3983291970846,0.));
#213361=CARTESIAN_POINT('Ctrl Pts',(21.22750781927,10.3849698664786,0.));
#213362=CARTESIAN_POINT('Ctrl Pts',(21.2134905199345,10.371727699113,0.));
#213363=CARTESIAN_POINT('Ctrl Pts',(21.199520887919,10.3586030124587,0.));
#213364=CARTESIAN_POINT('Ctrl Pts',(21.1855999722416,10.3455961265701,0.));
#213365=CARTESIAN_POINT('Ctrl Pts',(21.1717288370509,10.3327073641572,0.));
#213366=CARTESIAN_POINT('Ctrl Pts',(21.1579085619965,10.3199370506544,0.));
#213367=CARTESIAN_POINT('Ctrl Pts',(21.1441402425843,10.3072855142687,0.));
#213368=CARTESIAN_POINT('Ctrl Pts',(21.1304249906002,10.2947530860721,0.));
#213369=CARTESIAN_POINT('Ctrl Pts',(21.1167639345631,10.2823401001072,0.));
#213370=CARTESIAN_POINT('Ctrl Pts',(21.1031582201627,10.2700468934744,0.));
#213371=CARTESIAN_POINT('Ctrl Pts',(21.0896090107063,10.2578738064181,0.));
#213372=CARTESIAN_POINT('Ctrl Pts',(21.0761174875444,10.2458211823912,0.));
#213373=CARTESIAN_POINT('Ctrl Pts',(21.0626848505663,10.2338893681567,0.));
#213374=CARTESIAN_POINT('Ctrl Pts',(21.0493123187483,10.2220787139155,0.));
#213375=CARTESIAN_POINT('Ctrl Pts',(21.0360011306815,10.2103895734123,0.));
#213376=CARTESIAN_POINT('Ctrl Pts',(21.0227525451107,10.1988223040425,0.));
#213377=CARTESIAN_POINT('Ctrl Pts',(21.0095678414486,10.187377266936,0.));
#213378=CARTESIAN_POINT('Ctrl Pts',(20.9964483203686,10.1760548270767,0.));
#213379=CARTESIAN_POINT('Ctrl Pts',(20.9833953044736,10.1648553534568,0.));
#213380=CARTESIAN_POINT('Ctrl Pts',(20.9704101389369,10.1537792192065,0.));
#213381=CARTESIAN_POINT('Ctrl Pts',(20.9574941921591,10.1428268017256,0.));
#213382=CARTESIAN_POINT('Ctrl Pts',(20.9446488563933,10.1319984827908,0.));
#213383=CARTESIAN_POINT('Ctrl Pts',(20.9318755484734,10.1212946487057,0.));
#213384=CARTESIAN_POINT('Ctrl Pts',(20.919175710627,10.1107156904836,0.));
#213385=CARTESIAN_POINT('Ctrl Pts',(20.9065508112557,10.1002620040076,0.));
#213386=CARTESIAN_POINT('Ctrl Pts',(20.894002345737,10.0899339901916,0.));
#213387=CARTESIAN_POINT('Ctrl Pts',(20.881531837184,10.0797320551154,0.));
#213388=CARTESIAN_POINT('Ctrl Pts',(20.86914083737,10.0696566102218,0.));
#213389=CARTESIAN_POINT('Ctrl Pts',(20.8568309277316,10.0597080725375,0.));
#213390=CARTESIAN_POINT('Ctrl Pts',(20.8446037203402,10.0498868648733,0.));
#213391=CARTESIAN_POINT('Ctrl Pts',(20.8324608588909,10.0401934160234,0.));
#213392=CARTESIAN_POINT('Ctrl Pts',(20.8204040196602,10.0306281609435,0.));
#213393=CARTESIAN_POINT('Ctrl Pts',(20.8084349126888,10.0211915410095,0.));
#213394=CARTESIAN_POINT('Ctrl Pts',(20.7965552829908,10.0118840042786,0.));
#213395=CARTESIAN_POINT('Ctrl Pts',(20.7847669117568,10.0027060057389,0.));
#213396=CARTESIAN_POINT('Ctrl Pts',(20.7730716175417,9.9936580075464,0.));
#213397=CARTESIAN_POINT('Ctrl Pts',(20.761471257499,9.98474047926853,0.));
#213398=CARTESIAN_POINT('Ctrl Pts',(20.7499677289627,9.9759538982347,0.));
#213399=CARTESIAN_POINT('Ctrl Pts',(20.7385629709795,9.96729874986202,0.));
#213400=CARTESIAN_POINT('Ctrl Pts',(20.7272589658751,9.95877552798398,0.));
#213401=CARTESIAN_POINT('Ctrl Pts',(20.7160577407579,9.95038473514949,0.));
#213402=CARTESIAN_POINT('Ctrl Pts',(20.7049613692234,9.94212688298236,0.));
#213403=CARTESIAN_POINT('Ctrl Pts',(20.6939719732484,9.9340024925973,0.));
#213404=CARTESIAN_POINT('Ctrl Pts',(20.6830917250255,9.92601209498749,0.));
#213405=CARTESIAN_POINT('Ctrl Pts',(20.6723228488263,9.91815623141289,0.));
#213406=CARTESIAN_POINT('Ctrl Pts',(20.6616676228315,9.91043545377008,0.));
#213407=CARTESIAN_POINT('Ctrl Pts',(20.6511283817414,9.90285032516693,0.));
#213408=CARTESIAN_POINT('Ctrl Pts',(20.6407075193976,9.8954014204912,0.));
#213409=CARTESIAN_POINT('Ctrl Pts',(20.6304074914087,9.88808932697306,0.));
#213410=CARTESIAN_POINT('Ctrl Pts',(20.6202308177474,9.88091464472676,0.));
#213411=CARTESIAN_POINT('Ctrl Pts',(20.6101800854494,9.87387798732956,0.));
#213412=CARTESIAN_POINT('Ctrl Pts',(20.6002579513699,9.86697998242623,0.));
#213413=CARTESIAN_POINT('Ctrl Pts',(20.5904671449754,9.86022127232748,0.));
#213414=CARTESIAN_POINT('Ctrl Pts',(20.5808104710015,9.85360251456981,0.));
#213415=CARTESIAN_POINT('Ctrl Pts',(20.5712908125139,9.84712438256278,0.));
#213416=CARTESIAN_POINT('Ctrl Pts',(20.5619111362402,9.84078756677565,0.));
#213417=CARTESIAN_POINT('Ctrl Pts',(20.552674497646,9.83459277585315,0.));
#213418=CARTESIAN_POINT('Ctrl Pts',(20.5435840460721,9.82854073773878,0.));
#213419=CARTESIAN_POINT('Ctrl Pts',(20.5346430299517,9.82263220080363,0.));
#213420=CARTESIAN_POINT('Ctrl Pts',(20.5258548000629,9.81686793455943,0.));
#213421=CARTESIAN_POINT('Ctrl Pts',(20.517222812284,9.81124873025282,0.));
#213422=CARTESIAN_POINT('Ctrl Pts',(20.5087506310505,9.80577540161088,0.));
#213423=CARTESIAN_POINT('Ctrl Pts',(20.5004419312107,9.80044878520949,0.));
#213424=CARTESIAN_POINT('Ctrl Pts',(20.4923005087943,9.79526974288331,0.));
#213425=CARTESIAN_POINT('Ctrl Pts',(20.4843302955329,9.79023916498656,0.));
#213426=CARTESIAN_POINT('Ctrl Pts',(20.4765353711586,9.78535797314167,0.));
#213427=CARTESIAN_POINT('Ctrl Pts',(20.4689199790669,9.78062712373321,0.));
#213428=CARTESIAN_POINT('Ctrl Pts',(20.4614885274975,9.77604760815529,0.));
#213429=CARTESIAN_POINT('Ctrl Pts',(20.4542455817527,9.7716204510407,0.));
#213430=CARTESIAN_POINT('Ctrl Pts',(20.447195862298,9.76734670980892,0.));
#213431=CARTESIAN_POINT('Ctrl Pts',(20.44034423294,9.76322747195495,0.));
#213432=CARTESIAN_POINT('Ctrl Pts',(20.4336957355473,9.75926386289923,0.));
#213433=CARTESIAN_POINT('Ctrl Pts',(20.4272556476629,9.75545705902418,0.));
#213434=CARTESIAN_POINT('Ctrl Pts',(20.4210295275817,9.7518082978643,0.));
#213435=CARTESIAN_POINT('Ctrl Pts',(20.4150232777393,9.74831889242174,0.));
#213436=CARTESIAN_POINT('Ctrl Pts',(20.4092430879861,9.74499021838538,0.));
#213437=CARTESIAN_POINT('Ctrl Pts',(20.4036953576549,9.74182369656272,0.));
#213438=CARTESIAN_POINT('Ctrl Pts',(20.3983866213331,9.73882077613201,0.));
#213439=CARTESIAN_POINT('Ctrl Pts',(20.3933234845647,9.73598292014243,0.));
#213440=CARTESIAN_POINT('Ctrl Pts',(20.3885129129912,9.73331167102808,0.));
#213441=CARTESIAN_POINT('Ctrl Pts',(20.3839624556742,9.73080870123727,0.));
#213442=CARTESIAN_POINT('Ctrl Pts',(20.3796805893304,9.72847589116542,0.));
#213443=CARTESIAN_POINT('Ctrl Pts',(20.3756766651951,9.72631531732881,0.));
#213444=CARTESIAN_POINT('Ctrl Pts',(20.371960235676,9.72432910043194,0.));
#213445=CARTESIAN_POINT('Ctrl Pts',(20.3685406190576,9.7225193072249,0.));
#213446=CARTESIAN_POINT('Ctrl Pts',(20.3654261611056,9.72088778381081,0.));
#213447=CARTESIAN_POINT('Ctrl Pts',(20.3626256913981,9.71943648548099,0.));
#213448=CARTESIAN_POINT('Ctrl Pts',(20.3601498764344,9.71816778328007,0.));
#213449=CARTESIAN_POINT('Ctrl Pts',(20.3580133103356,9.71708493723096,0.));
#213450=CARTESIAN_POINT('Ctrl Pts',(20.3562337557875,9.71619192554186,0.));
#213451=CARTESIAN_POINT('Ctrl Pts',(20.3548282742361,9.71549257088173,0.));
#213452=CARTESIAN_POINT('Ctrl Pts',(20.3538098605706,9.71498978052021,0.));
#213453=CARTESIAN_POINT('Ctrl Pts',(20.3533097561886,9.71474590350681,0.));
#213454=CARTESIAN_POINT('Ctrl Pts',(20.3531126095522,9.71465227853042,0.));
#213455=CARTESIAN_POINT('Ctrl Pts',(20.353060251684,9.71462954053042,0.));
#213456=CARTESIAN_POINT('Ctrl Pts',(20.353053841303,9.71462809124916,0.));
#213457=CARTESIAN_POINT('',(22.8400320311648,12.4230808101438,0.));
#213458=CARTESIAN_POINT('Ctrl Pts',(21.2610617890679,7.52250298901264,0.));
#213459=CARTESIAN_POINT('Ctrl Pts',(21.2610617890679,7.52250298901264,12.));
#213460=CARTESIAN_POINT('Ctrl Pts',(21.2610673466886,7.5225064970397,0.));
#213461=CARTESIAN_POINT('Ctrl Pts',(21.2610673466886,7.5225064970397,12.));
#213462=CARTESIAN_POINT('Ctrl Pts',(21.2611204474866,7.52252744144904,0.));
#213463=CARTESIAN_POINT('Ctrl Pts',(21.2611204474866,7.52252744144904,12.));
#213464=CARTESIAN_POINT('Ctrl Pts',(21.261326054066,7.52260064231661,0.));
#213465=CARTESIAN_POINT('Ctrl Pts',(21.261326054066,7.52260064231661,12.));
#213466=CARTESIAN_POINT('Ctrl Pts',(21.2618521283555,7.5227818224267,0.));
#213467=CARTESIAN_POINT('Ctrl Pts',(21.2618521283555,7.5227818224267,12.));
#213468=CARTESIAN_POINT('Ctrl Pts',(21.262927782038,7.52314642316199,0.));
#213469=CARTESIAN_POINT('Ctrl Pts',(21.262927782038,7.52314642316199,12.));
#213470=CARTESIAN_POINT('Ctrl Pts',(21.2644161259962,7.52364573027553,0.));
#213471=CARTESIAN_POINT('Ctrl Pts',(21.2644161259962,7.52364573027553,12.));
#213472=CARTESIAN_POINT('Ctrl Pts',(21.2663059157058,7.52427261074298,0.));
#213473=CARTESIAN_POINT('Ctrl Pts',(21.2663059157058,7.52427261074298,12.));
#213474=CARTESIAN_POINT('Ctrl Pts',(21.2685823838671,7.52501770333531,0.));
#213475=CARTESIAN_POINT('Ctrl Pts',(21.2685823838671,7.52501770333531,12.));
#213476=CARTESIAN_POINT('Ctrl Pts',(21.2712301573466,7.5258712609553,0.));
#213477=CARTESIAN_POINT('Ctrl Pts',(21.2712301573466,7.5258712609553,12.));
#213478=CARTESIAN_POINT('Ctrl Pts',(21.2742366113579,7.52682526918541,0.));
#213479=CARTESIAN_POINT('Ctrl Pts',(21.2742366113579,7.52682526918541,12.));
#213480=CARTESIAN_POINT('Ctrl Pts',(21.2775925269652,7.52787386225333,0.));
#213481=CARTESIAN_POINT('Ctrl Pts',(21.2775925269652,7.52787386225333,12.));
#213482=CARTESIAN_POINT('Ctrl Pts',(21.2812902781143,7.52901217930408,0.));
#213483=CARTESIAN_POINT('Ctrl Pts',(21.2812902781143,7.52901217930408,12.));
#213484=CARTESIAN_POINT('Ctrl Pts',(21.2853226580657,7.5302356243823,0.));
#213485=CARTESIAN_POINT('Ctrl Pts',(21.2853226580657,7.5302356243823,12.));
#213486=CARTESIAN_POINT('Ctrl Pts',(21.2896816163842,7.53153906987856,0.));
#213487=CARTESIAN_POINT('Ctrl Pts',(21.2896816163842,7.53153906987856,12.));
#213488=CARTESIAN_POINT('Ctrl Pts',(21.2943588989331,7.53291726078527,0.));
#213489=CARTESIAN_POINT('Ctrl Pts',(21.2943588989331,7.53291726078527,12.));
#213490=CARTESIAN_POINT('Ctrl Pts',(21.2993464250717,7.53436505309943,0.));
#213491=CARTESIAN_POINT('Ctrl Pts',(21.2993464250717,7.53436505309943,12.));
#213492=CARTESIAN_POINT('Ctrl Pts',(21.3046368712157,7.53587778251736,0.));
#213493=CARTESIAN_POINT('Ctrl Pts',(21.3046368712157,7.53587778251736,12.));
#213494=CARTESIAN_POINT('Ctrl Pts',(21.310223716773,7.53745129364616,0.));
#213495=CARTESIAN_POINT('Ctrl Pts',(21.310223716773,7.53745129364616,12.));
#213496=CARTESIAN_POINT('Ctrl Pts',(21.3161009456256,7.53908175169899,0.));
#213497=CARTESIAN_POINT('Ctrl Pts',(21.3161009456256,7.53908175169899,12.));
#213498=CARTESIAN_POINT('Ctrl Pts',(21.3222628524165,7.54076552038279,0.));
#213499=CARTESIAN_POINT('Ctrl Pts',(21.3222628524165,7.54076552038279,12.));
#213500=CARTESIAN_POINT('Ctrl Pts',(21.328703791771,7.54249900377031,0.));
#213501=CARTESIAN_POINT('Ctrl Pts',(21.328703791771,7.54249900377031,12.));
#213502=CARTESIAN_POINT('Ctrl Pts',(21.3354182340149,7.54427868151268,0.));
#213503=CARTESIAN_POINT('Ctrl Pts',(21.3354182340149,7.54427868151268,12.));
#213504=CARTESIAN_POINT('Ctrl Pts',(21.3424008295038,7.54610114948347,0.));
#213505=CARTESIAN_POINT('Ctrl Pts',(21.3424008295038,7.54610114948347,12.));
#213506=CARTESIAN_POINT('Ctrl Pts',(21.3496464761531,7.54796316246331,0.));
#213507=CARTESIAN_POINT('Ctrl Pts',(21.3496464761531,7.54796316246331,12.));
#213508=CARTESIAN_POINT('Ctrl Pts',(21.3571503685855,7.5498616652131,0.));
#213509=CARTESIAN_POINT('Ctrl Pts',(21.3571503685855,7.5498616652131,12.));
#213510=CARTESIAN_POINT('Ctrl Pts',(21.3649079431865,7.55179375777444,0.));
#213511=CARTESIAN_POINT('Ctrl Pts',(21.3649079431865,7.55179375777444,12.));
#213512=CARTESIAN_POINT('Ctrl Pts',(21.3729148390243,7.55375667080029,0.));
#213513=CARTESIAN_POINT('Ctrl Pts',(21.3729148390243,7.55375667080029,12.));
#213514=CARTESIAN_POINT('Ctrl Pts',(21.3811668478932,7.55574773403503,0.));
#213515=CARTESIAN_POINT('Ctrl Pts',(21.3811668478932,7.55574773403503,12.));
#213516=CARTESIAN_POINT('Ctrl Pts',(21.3896598842117,7.55776435731417,0.));
#213517=CARTESIAN_POINT('Ctrl Pts',(21.3896598842117,7.55776435731417,12.));
#213518=CARTESIAN_POINT('Ctrl Pts',(21.3983899952987,7.55980403700611,0.));
#213519=CARTESIAN_POINT('Ctrl Pts',(21.3983899952987,7.55980403700611,12.));
#213520=CARTESIAN_POINT('Ctrl Pts',(21.4073533630365,7.56186435703622,0.));
#213521=CARTESIAN_POINT('Ctrl Pts',(21.4073533630365,7.56186435703622,12.));
#213522=CARTESIAN_POINT('Ctrl Pts',(21.4165463106254,7.56394299313685,0.));
#213523=CARTESIAN_POINT('Ctrl Pts',(21.4165463106254,7.56394299313685,12.));
#213524=CARTESIAN_POINT('Ctrl Pts',(21.4259653015736,7.56603771218712,0.));
#213525=CARTESIAN_POINT('Ctrl Pts',(21.4259653015736,7.56603771218712,12.));
#213526=CARTESIAN_POINT('Ctrl Pts',(21.4356069261513,7.56814636360848,0.));
#213527=CARTESIAN_POINT('Ctrl Pts',(21.4356069261513,7.56814636360848,12.));
#213528=CARTESIAN_POINT('Ctrl Pts',(21.4454678907509,7.57026687261166,0.));
#213529=CARTESIAN_POINT('Ctrl Pts',(21.4454678907509,7.57026687261166,12.));
#213530=CARTESIAN_POINT('Ctrl Pts',(21.4555450053142,7.57239723223506,0.));
#213531=CARTESIAN_POINT('Ctrl Pts',(21.4555450053142,7.57239723223506,12.));
#213532=CARTESIAN_POINT('Ctrl Pts',(21.4658351740128,7.57453549743412,0.));
#213533=CARTESIAN_POINT('Ctrl Pts',(21.4658351740128,7.57453549743412,12.));
#213534=CARTESIAN_POINT('Ctrl Pts',(21.4763353936762,7.57667978402987,0.));
#213535=CARTESIAN_POINT('Ctrl Pts',(21.4763353936762,7.57667978402987,12.));
#213536=CARTESIAN_POINT('Ctrl Pts',(21.4870427508194,7.57882826679132,0.));
#213537=CARTESIAN_POINT('Ctrl Pts',(21.4870427508194,7.57882826679132,12.));
#213538=CARTESIAN_POINT('Ctrl Pts',(21.4979544192744,7.58097917790744,0.));
#213539=CARTESIAN_POINT('Ctrl Pts',(21.4979544192744,7.58097917790744,12.));
#213540=CARTESIAN_POINT('Ctrl Pts',(21.5090676573873,7.5831308051918,0.));
#213541=CARTESIAN_POINT('Ctrl Pts',(21.5090676573873,7.5831308051918,12.));
#213542=CARTESIAN_POINT('Ctrl Pts',(21.5203798035299,7.5852814891913,0.));
#213543=CARTESIAN_POINT('Ctrl Pts',(21.5203798035299,7.5852814891913,12.));
#213544=CARTESIAN_POINT('Ctrl Pts',(21.5318882716736,7.58742962034834,0.));
#213545=CARTESIAN_POINT('Ctrl Pts',(21.5318882716736,7.58742962034834,12.));
#213546=CARTESIAN_POINT('Ctrl Pts',(21.543590547011,7.58957363620014,0.));
#213547=CARTESIAN_POINT('Ctrl Pts',(21.543590547011,7.58957363620014,12.));
#213548=CARTESIAN_POINT('Ctrl Pts',(21.5554841813462,7.59171201844777,0.));
#213549=CARTESIAN_POINT('Ctrl Pts',(21.5554841813462,7.59171201844777,12.));
#213550=CARTESIAN_POINT('Ctrl Pts',(21.5675667904726,7.59384329124918,0.));
#213551=CARTESIAN_POINT('Ctrl Pts',(21.5675667904726,7.59384329124918,12.));
#213552=CARTESIAN_POINT('Ctrl Pts',(21.5798360518978,7.59596601973584,0.));
#213553=CARTESIAN_POINT('Ctrl Pts',(21.5798360518978,7.59596601973584,12.));
#213554=CARTESIAN_POINT('Ctrl Pts',(21.5922897024466,7.59807880846195,0.));
#213555=CARTESIAN_POINT('Ctrl Pts',(21.5922897024466,7.59807880846195,12.));
#213556=CARTESIAN_POINT('Ctrl Pts',(21.6049255358843,7.60018029988241,0.));
#213557=CARTESIAN_POINT('Ctrl Pts',(21.6049255358843,7.60018029988241,12.));
#213558=CARTESIAN_POINT('Ctrl Pts',(21.617741400599,7.60226917285429,0.));
#213559=CARTESIAN_POINT('Ctrl Pts',(21.617741400599,7.60226917285429,12.));
#213560=CARTESIAN_POINT('Ctrl Pts',(21.6307351973822,7.60434414118296,0.));
#213561=CARTESIAN_POINT('Ctrl Pts',(21.6307351973822,7.60434414118296,12.));
#213562=CARTESIAN_POINT('Ctrl Pts',(21.6439048771743,7.60640395216357,0.));
#213563=CARTESIAN_POINT('Ctrl Pts',(21.6439048771743,7.60640395216357,12.));
#213564=CARTESIAN_POINT('Ctrl Pts',(21.6572484388081,7.60844738512874,0.));
#213565=CARTESIAN_POINT('Ctrl Pts',(21.6572484388081,7.60844738512874,12.));
#213566=CARTESIAN_POINT('Ctrl Pts',(21.6707639267576,7.61047325000956,0.));
#213567=CARTESIAN_POINT('Ctrl Pts',(21.6707639267576,7.61047325000956,12.));
#213568=CARTESIAN_POINT('Ctrl Pts',(21.6844494295815,7.61248038630269,0.));
#213569=CARTESIAN_POINT('Ctrl Pts',(21.6844494295815,7.61248038630269,12.));
#213570=CARTESIAN_POINT('Ctrl Pts',(21.6983030783322,7.61446766202787,0.));
#213571=CARTESIAN_POINT('Ctrl Pts',(21.6983030783322,7.61446766202787,12.));
#213572=CARTESIAN_POINT('Ctrl Pts',(21.7123230449834,7.61643397270421,0.));
#213573=CARTESIAN_POINT('Ctrl Pts',(21.7123230449834,7.61643397270421,12.));
#213574=CARTESIAN_POINT('Ctrl Pts',(21.7265075407975,7.61837824030538,0.));
#213575=CARTESIAN_POINT('Ctrl Pts',(21.7265075407975,7.61837824030538,12.));
#213576=CARTESIAN_POINT('Ctrl Pts',(21.7408548148656,7.62029941230855,0.));
#213577=CARTESIAN_POINT('Ctrl Pts',(21.7408548148656,7.62029941230855,12.));
#213578=CARTESIAN_POINT('Ctrl Pts',(21.7553631528328,7.62219646084229,0.));
#213579=CARTESIAN_POINT('Ctrl Pts',(21.7553631528328,7.62219646084229,12.));
#213580=CARTESIAN_POINT('Ctrl Pts',(21.7700308755584,7.62406838181166,0.));
#213581=CARTESIAN_POINT('Ctrl Pts',(21.7700308755584,7.62406838181166,12.));
#213582=CARTESIAN_POINT('Ctrl Pts',(21.7848563378021,7.62591419404513,0.));
#213583=CARTESIAN_POINT('Ctrl Pts',(21.7848563378021,7.62591419404513,12.));
#213584=CARTESIAN_POINT('Ctrl Pts',(21.799837926858,7.62773293842389,0.));
#213585=CARTESIAN_POINT('Ctrl Pts',(21.799837926858,7.62773293842389,12.));
#213586=CARTESIAN_POINT('Ctrl Pts',(21.814974061509,7.62952367718127,0.));
#213587=CARTESIAN_POINT('Ctrl Pts',(21.814974061509,7.62952367718127,12.));
#213588=CARTESIAN_POINT('Ctrl Pts',(21.8302631910195,7.63128549323023,0.));
#213589=CARTESIAN_POINT('Ctrl Pts',(21.8302631910195,7.63128549323023,12.));
#213590=CARTESIAN_POINT('Ctrl Pts',(21.8457037941084,7.63301748948936,0.));
#213591=CARTESIAN_POINT('Ctrl Pts',(21.8457037941084,7.63301748948936,12.));
#213592=CARTESIAN_POINT('Ctrl Pts',(21.8612943779089,7.63471878821226,0.));
#213593=CARTESIAN_POINT('Ctrl Pts',(21.8612943779089,7.63471878821226,12.));
#213594=CARTESIAN_POINT('Ctrl Pts',(21.8770334769496,7.636388530334,0.));
#213595=CARTESIAN_POINT('Ctrl Pts',(21.8770334769496,7.636388530334,12.));
#213596=CARTESIAN_POINT('Ctrl Pts',(21.8929196523514,7.63802587492035,0.));
#213597=CARTESIAN_POINT('Ctrl Pts',(21.8929196523514,7.63802587492035,12.));
#213598=CARTESIAN_POINT('Ctrl Pts',(21.9089514909874,7.63962999860927,0.));
#213599=CARTESIAN_POINT('Ctrl Pts',(21.9089514909874,7.63962999860927,12.));
#213600=CARTESIAN_POINT('Ctrl Pts',(21.9251276046545,7.64120009506532,0.));
#213601=CARTESIAN_POINT('Ctrl Pts',(21.9251276046545,7.64120009506532,12.));
#213602=CARTESIAN_POINT('Ctrl Pts',(21.9414466292072,7.64273537442682,0.));
#213603=CARTESIAN_POINT('Ctrl Pts',(21.9414466292072,7.64273537442682,12.));
#213604=CARTESIAN_POINT('Ctrl Pts',(21.9579072237651,7.64423506279123,0.));
#213605=CARTESIAN_POINT('Ctrl Pts',(21.9579072237651,7.64423506279123,12.));
#213606=CARTESIAN_POINT('Ctrl Pts',(21.9745080700798,7.64569840177336,0.));
#213607=CARTESIAN_POINT('Ctrl Pts',(21.9745080700798,7.64569840177336,12.));
#213608=CARTESIAN_POINT('Ctrl Pts',(21.9912478718542,7.6471246480525,0.));
#213609=CARTESIAN_POINT('Ctrl Pts',(21.9912478718542,7.6471246480525,12.));
#213610=CARTESIAN_POINT('Ctrl Pts',(22.0081253540774,7.64851307293352,0.));
#213611=CARTESIAN_POINT('Ctrl Pts',(22.0081253540774,7.64851307293352,12.));
#213612=CARTESIAN_POINT('Ctrl Pts',(22.0251392623209,7.64986296190169,0.));
#213613=CARTESIAN_POINT('Ctrl Pts',(22.0251392623209,7.64986296190169,12.));
#213614=CARTESIAN_POINT('Ctrl Pts',(22.0422883621174,7.65117361421359,0.));
#213615=CARTESIAN_POINT('Ctrl Pts',(22.0422883621174,7.65117361421359,12.));
#213616=CARTESIAN_POINT('Ctrl Pts',(22.0595714384431,7.65244434253113,0.));
#213617=CARTESIAN_POINT('Ctrl Pts',(22.0595714384431,7.65244434253113,12.));
#213618=CARTESIAN_POINT('Ctrl Pts',(22.0769872951596,7.65367447254949,0.));
#213619=CARTESIAN_POINT('Ctrl Pts',(22.0769872951596,7.65367447254949,12.));
#213620=CARTESIAN_POINT('Ctrl Pts',(22.094534754469,7.65486334263644,0.));
#213621=CARTESIAN_POINT('Ctrl Pts',(22.094534754469,7.65486334263644,12.));
#213622=CARTESIAN_POINT('Ctrl Pts',(22.1122126563329,7.65601030346807,0.));
#213623=CARTESIAN_POINT('Ctrl Pts',(22.1122126563329,7.65601030346807,12.));
#213624=CARTESIAN_POINT('Ctrl Pts',(22.1300198579675,7.65711471769397,0.));
#213625=CARTESIAN_POINT('Ctrl Pts',(22.1300198579675,7.65711471769397,12.));
#213626=CARTESIAN_POINT('Ctrl Pts',(22.1479552334211,7.65817595963349,0.));
#213627=CARTESIAN_POINT('Ctrl Pts',(22.1479552334211,7.65817595963349,12.));
#213628=CARTESIAN_POINT('Ctrl Pts',(22.1660176731178,7.65919341496931,0.));
#213629=CARTESIAN_POINT('Ctrl Pts',(22.1660176731178,7.65919341496931,12.));
#213630=CARTESIAN_POINT('Ctrl Pts',(22.1842060834091,7.66016648045005,0.));
#213631=CARTESIAN_POINT('Ctrl Pts',(22.1842060834091,7.66016648045005,12.));
#213632=CARTESIAN_POINT('Ctrl Pts',(22.2025193860964,7.66109456359271,0.));
#213633=CARTESIAN_POINT('Ctrl Pts',(22.2025193860964,7.66109456359271,12.));
#213634=CARTESIAN_POINT('Ctrl Pts',(22.2209565180085,7.661977082404,0.));
#213635=CARTESIAN_POINT('Ctrl Pts',(22.2209565180085,7.661977082404,12.));
#213636=CARTESIAN_POINT('Ctrl Pts',(22.2395164306547,7.66281346512509,0.));
#213637=CARTESIAN_POINT('Ctrl Pts',(22.2395164306547,7.66281346512509,12.));
#213638=CARTESIAN_POINT('Ctrl Pts',(22.258198089848,7.66360314997641,0.));
#213639=CARTESIAN_POINT('Ctrl Pts',(22.258198089848,7.66360314997641,12.));
#213640=CARTESIAN_POINT('Ctrl Pts',(22.2770004753335,7.66434558490979,0.));
#213641=CARTESIAN_POINT('Ctrl Pts',(22.2770004753335,7.66434558490979,12.));
#213642=CARTESIAN_POINT('Ctrl Pts',(22.2959225803937,7.66504022736299,0.));
#213643=CARTESIAN_POINT('Ctrl Pts',(22.2959225803937,7.66504022736299,12.));
#213644=CARTESIAN_POINT('Ctrl Pts',(22.314963411484,7.66568654402494,0.));
#213645=CARTESIAN_POINT('Ctrl Pts',(22.314963411484,7.66568654402494,12.));
#213646=CARTESIAN_POINT('Ctrl Pts',(22.3341219879469,7.66628401061952,0.));
#213647=CARTESIAN_POINT('Ctrl Pts',(22.3341219879469,7.66628401061952,12.));
#213648=CARTESIAN_POINT('Ctrl Pts',(22.3533973417021,7.66683211169159,0.));
#213649=CARTESIAN_POINT('Ctrl Pts',(22.3533973417021,7.66683211169159,12.));
#213650=CARTESIAN_POINT('Ctrl Pts',(22.372788516936,7.66733034039883,0.));
#213651=CARTESIAN_POINT('Ctrl Pts',(22.372788516936,7.66733034039883,12.));
#213652=CARTESIAN_POINT('Ctrl Pts',(22.3922945697773,7.6677781983079,0.));
#213653=CARTESIAN_POINT('Ctrl Pts',(22.3922945697773,7.6677781983079,12.));
#213654=CARTESIAN_POINT('Ctrl Pts',(22.4119145679758,7.6681751951964,0.));
#213655=CARTESIAN_POINT('Ctrl Pts',(22.4119145679758,7.6681751951964,12.));
#213656=CARTESIAN_POINT('Ctrl Pts',(22.4316475906603,7.66852084886704,0.));
#213657=CARTESIAN_POINT('Ctrl Pts',(22.4316475906603,7.66852084886704,12.));
#213658=CARTESIAN_POINT('Ctrl Pts',(22.4514927280855,7.66881468496635,0.));
#213659=CARTESIAN_POINT('Ctrl Pts',(22.4514927280855,7.66881468496635,12.));
#213660=CARTESIAN_POINT('Ctrl Pts',(22.4714490813699,7.66905623680831,0.));
#213661=CARTESIAN_POINT('Ctrl Pts',(22.4714490813699,7.66905623680831,12.));
#213662=CARTESIAN_POINT('Ctrl Pts',(22.4915157622312,7.66924504520315,0.));
#213663=CARTESIAN_POINT('Ctrl Pts',(22.4915157622312,7.66924504520315,12.));
#213664=CARTESIAN_POINT('Ctrl Pts',(22.5116918927031,7.66938065829108,0.));
#213665=CARTESIAN_POINT('Ctrl Pts',(22.5116918927031,7.66938065829108,12.));
#213666=CARTESIAN_POINT('Ctrl Pts',(22.53197660492,7.66946263138144,0.));
#213667=CARTESIAN_POINT('Ctrl Pts',(22.53197660492,7.66946263138144,12.));
#213668=CARTESIAN_POINT('Ctrl Pts',(22.5523690409116,7.66949052679693,0.));
#213669=CARTESIAN_POINT('Ctrl Pts',(22.5523690409116,7.66949052679693,12.));
#213670=CARTESIAN_POINT('Ctrl Pts',(22.5728683523831,7.66946391372306,0.));
#213671=CARTESIAN_POINT('Ctrl Pts',(22.5728683523831,7.66946391372306,12.));
#213672=CARTESIAN_POINT('Ctrl Pts',(22.5934737004953,7.66938236806233,0.));
#213673=CARTESIAN_POINT('Ctrl Pts',(22.5934737004953,7.66938236806233,12.));
#213674=CARTESIAN_POINT('Ctrl Pts',(22.6141842556243,7.66924547229414,0.));
#213675=CARTESIAN_POINT('Ctrl Pts',(22.6141842556243,7.66924547229414,12.));
#213676=CARTESIAN_POINT('Ctrl Pts',(22.6349991971541,7.66905281533715,0.));
#213677=CARTESIAN_POINT('Ctrl Pts',(22.6349991971541,7.66905281533715,12.));
#213678=CARTESIAN_POINT('Ctrl Pts',(22.6559177133127,7.66880399241323,0.));
#213679=CARTESIAN_POINT('Ctrl Pts',(22.6559177133127,7.66880399241323,12.));
#213680=CARTESIAN_POINT('Ctrl Pts',(22.6769390009885,7.66849860491743,0.));
#213681=CARTESIAN_POINT('Ctrl Pts',(22.6769390009885,7.66849860491743,12.));
#213682=CARTESIAN_POINT('Ctrl Pts',(22.6980622655446,7.66813626029275,0.));
#213683=CARTESIAN_POINT('Ctrl Pts',(22.6980622655446,7.66813626029275,12.));
#213684=CARTESIAN_POINT('Ctrl Pts',(22.7192867206245,7.66771657191028,0.));
#213685=CARTESIAN_POINT('Ctrl Pts',(22.7192867206245,7.66771657191028,12.));
#213686=CARTESIAN_POINT('Ctrl Pts',(22.7406115879513,7.6672391589544,0.));
#213687=CARTESIAN_POINT('Ctrl Pts',(22.7406115879513,7.6672391589544,12.));
#213688=CARTESIAN_POINT('Ctrl Pts',(22.7620360971843,7.66670364630299,0.));
#213689=CARTESIAN_POINT('Ctrl Pts',(22.7620360971843,7.66670364630299,12.));
#213690=CARTESIAN_POINT('Ctrl Pts',(22.7835594857699,7.66610966441273,0.));
#213691=CARTESIAN_POINT('Ctrl Pts',(22.7835594857699,7.66610966441273,12.));
#213692=CARTESIAN_POINT('Ctrl Pts',(22.8051809987833,7.66545684920987,0.));
#213693=CARTESIAN_POINT('Ctrl Pts',(22.8051809987833,7.66545684920987,12.));
#213694=CARTESIAN_POINT('Ctrl Pts',(22.8268998887678,7.66474484198549,0.));
#213695=CARTESIAN_POINT('Ctrl Pts',(22.8268998887678,7.66474484198549,12.));
#213696=CARTESIAN_POINT('Ctrl Pts',(22.848715415557,7.66397328929803,0.));
#213697=CARTESIAN_POINT('Ctrl Pts',(22.848715415557,7.66397328929803,12.));
#213698=CARTESIAN_POINT('Ctrl Pts',(22.8706268461283,7.66314184287337,0.));
#213699=CARTESIAN_POINT('Ctrl Pts',(22.8706268461283,7.66314184287337,12.));
#213700=CARTESIAN_POINT('Ctrl Pts',(22.8926334544883,7.66225015950156,0.));
#213701=CARTESIAN_POINT('Ctrl Pts',(22.8926334544883,7.66225015950156,12.));
#213702=CARTESIAN_POINT('Ctrl Pts',(22.9147345215421,7.66129790094108,0.));
#213703=CARTESIAN_POINT('Ctrl Pts',(22.9147345215421,7.66129790094108,12.));
#213704=CARTESIAN_POINT('Ctrl Pts',(22.9369293349593,7.66028473382778,0.));
#213705=CARTESIAN_POINT('Ctrl Pts',(22.9369293349593,7.66028473382778,12.));
#213706=CARTESIAN_POINT('Ctrl Pts',(22.959217189033,7.65921032958902,0.));
#213707=CARTESIAN_POINT('Ctrl Pts',(22.959217189033,7.65921032958902,12.));
#213708=CARTESIAN_POINT('Ctrl Pts',(22.9815973845296,7.65807436436432,0.));
#213709=CARTESIAN_POINT('Ctrl Pts',(22.9815973845296,7.65807436436432,12.));
#213710=CARTESIAN_POINT('Ctrl Pts',(23.0040692285814,7.65687651891305,0.));
#213711=CARTESIAN_POINT('Ctrl Pts',(23.0040692285814,7.65687651891305,12.));
#213712=CARTESIAN_POINT('Ctrl Pts',(23.0266320345787,7.65561647852534,0.));
#213713=CARTESIAN_POINT('Ctrl Pts',(23.0266320345787,7.65561647852534,12.));
#213714=CARTESIAN_POINT('Ctrl Pts',(23.0492851220528,7.65429393293946,0.));
#213715=CARTESIAN_POINT('Ctrl Pts',(23.0492851220528,7.65429393293946,12.));
#213716=CARTESIAN_POINT('Ctrl Pts',(23.072027816555,7.65290857626358,0.));
#213717=CARTESIAN_POINT('Ctrl Pts',(23.072027816555,7.65290857626358,12.));
#213718=CARTESIAN_POINT('Ctrl Pts',(23.094859449525,7.65146010690476,0.));
#213719=CARTESIAN_POINT('Ctrl Pts',(23.094859449525,7.65146010690476,12.));
#213720=CARTESIAN_POINT('Ctrl Pts',(23.1177793581679,7.6499482274986,0.));
#213721=CARTESIAN_POINT('Ctrl Pts',(23.1177793581679,7.6499482274986,12.));
#213722=CARTESIAN_POINT('Ctrl Pts',(23.1407868853819,7.64837264482943,0.));
#213723=CARTESIAN_POINT('Ctrl Pts',(23.1407868853819,7.64837264482943,12.));
#213724=CARTESIAN_POINT('Ctrl Pts',(23.1638813796694,7.64673306975805,0.));
#213725=CARTESIAN_POINT('Ctrl Pts',(23.1638813796694,7.64673306975805,12.));
#213726=CARTESIAN_POINT('Ctrl Pts',(23.1870621950452,7.64502921715483,0.));
#213727=CARTESIAN_POINT('Ctrl Pts',(23.1870621950452,7.64502921715483,12.));
#213728=CARTESIAN_POINT('Ctrl Pts',(23.2103286909398,7.6432608058368,0.));
#213729=CARTESIAN_POINT('Ctrl Pts',(23.2103286909398,7.6432608058368,12.));
#213730=CARTESIAN_POINT('Ctrl Pts',(23.2336802320912,7.64142755851505,0.));
#213731=CARTESIAN_POINT('Ctrl Pts',(23.2336802320912,7.64142755851505,12.));
#213732=CARTESIAN_POINT('Ctrl Pts',(23.2571161884488,7.63952920172835,0.));
#213733=CARTESIAN_POINT('Ctrl Pts',(23.2571161884488,7.63952920172835,12.));
#213734=CARTESIAN_POINT('Ctrl Pts',(23.2806359350855,7.63756546576374,0.));
#213735=CARTESIAN_POINT('Ctrl Pts',(23.2806359350855,7.63756546576374,12.));
#213736=CARTESIAN_POINT('Ctrl Pts',(23.3042388521022,7.63553608458783,0.));
#213737=CARTESIAN_POINT('Ctrl Pts',(23.3042388521022,7.63553608458783,12.));
#213738=CARTESIAN_POINT('Ctrl Pts',(23.3279243245241,7.63344079578162,0.));
#213739=CARTESIAN_POINT('Ctrl Pts',(23.3279243245241,7.63344079578162,12.));
#213740=CARTESIAN_POINT('Ctrl Pts',(23.3516917421972,7.63127934048137,0.));
#213741=CARTESIAN_POINT('Ctrl Pts',(23.3516917421972,7.63127934048137,12.));
#213742=CARTESIAN_POINT('Ctrl Pts',(23.3755404996636,7.62905146332593,0.));
#213743=CARTESIAN_POINT('Ctrl Pts',(23.3755404996636,7.62905146332593,12.));
#213744=CARTESIAN_POINT('Ctrl Pts',(23.399469996112,7.62675691240329,0.));
#213745=CARTESIAN_POINT('Ctrl Pts',(23.399469996112,7.62675691240329,12.));
#213746=CARTESIAN_POINT('Ctrl Pts',(23.4234796353542,7.6243954392005,0.));
#213747=CARTESIAN_POINT('Ctrl Pts',(23.4234796353542,7.6243954392005,12.));
#213748=CARTESIAN_POINT('Ctrl Pts',(23.4475688257854,7.62196679855955,0.));
#213749=CARTESIAN_POINT('Ctrl Pts',(23.4475688257854,7.62196679855955,12.));
#213750=CARTESIAN_POINT('Ctrl Pts',(23.4717369803438,7.61947074863977,0.));
#213751=CARTESIAN_POINT('Ctrl Pts',(23.4717369803438,7.61947074863977,12.));
#213752=CARTESIAN_POINT('Ctrl Pts',(23.4959835164609,7.61690705088319,0.));
#213753=CARTESIAN_POINT('Ctrl Pts',(23.4959835164609,7.61690705088319,12.));
#213754=CARTESIAN_POINT('Ctrl Pts',(23.5203078560129,7.61427546999298,0.));
#213755=CARTESIAN_POINT('Ctrl Pts',(23.5203078560129,7.61427546999298,12.));
#213756=CARTESIAN_POINT('Ctrl Pts',(23.544709425203,7.61157577385372,0.));
#213757=CARTESIAN_POINT('Ctrl Pts',(23.544709425203,7.61157577385372,12.));
#213758=CARTESIAN_POINT('Ctrl Pts',(23.5691876544244,7.608807733446,0.));
#213759=CARTESIAN_POINT('Ctrl Pts',(23.5691876544244,7.608807733446,12.));
#213760=CARTESIAN_POINT('Ctrl Pts',(23.5937419781245,7.60597112277094,0.));
#213761=CARTESIAN_POINT('Ctrl Pts',(23.5937419781245,7.60597112277094,12.));
#213762=CARTESIAN_POINT('Ctrl Pts',(23.6183718346576,7.60306571877806,0.));
#213763=CARTESIAN_POINT('Ctrl Pts',(23.6183718346576,7.60306571877806,12.));
#213764=CARTESIAN_POINT('Ctrl Pts',(23.6430766661418,7.60009130130126,0.));
#213765=CARTESIAN_POINT('Ctrl Pts',(23.6430766661418,7.60009130130126,12.));
#213766=CARTESIAN_POINT('Ctrl Pts',(23.6678559182875,7.59704765299567,0.));
#213767=CARTESIAN_POINT('Ctrl Pts',(23.6678559182875,7.59704765299567,12.));
#213768=CARTESIAN_POINT('Ctrl Pts',(23.6927090405066,7.59393455934035,0.));
#213769=CARTESIAN_POINT('Ctrl Pts',(23.6927090405066,7.59393455934035,12.));
#213770=CARTESIAN_POINT('Ctrl Pts',(23.7176354860456,7.59075180865321,0.));
#213771=CARTESIAN_POINT('Ctrl Pts',(23.7176354860456,7.59075180865321,12.));
#213772=CARTESIAN_POINT('Ctrl Pts',(23.7426347121006,7.58749919210826,0.));
#213773=CARTESIAN_POINT('Ctrl Pts',(23.7426347121006,7.58749919210826,12.));
#213774=CARTESIAN_POINT('Ctrl Pts',(23.7677061799376,7.58417650376271,0.));
#213775=CARTESIAN_POINT('Ctrl Pts',(23.7677061799376,7.58417650376271,12.));
#213776=CARTESIAN_POINT('Ctrl Pts',(23.7928493549908,7.58078354058213,0.));
#213777=CARTESIAN_POINT('Ctrl Pts',(23.7928493549908,7.58078354058213,12.));
#213778=CARTESIAN_POINT('Ctrl Pts',(23.8180637069976,7.57732010249066,0.));
#213779=CARTESIAN_POINT('Ctrl Pts',(23.8180637069976,7.57732010249066,12.));
#213780=CARTESIAN_POINT('Ctrl Pts',(23.8433487096132,7.57378599219814,0.));
#213781=CARTESIAN_POINT('Ctrl Pts',(23.8433487096132,7.57378599219814,12.));
#213782=CARTESIAN_POINT('Ctrl Pts',(23.8687038399595,7.57018101500709,0.));
#213783=CARTESIAN_POINT('Ctrl Pts',(23.8687038399595,7.57018101500709,12.));
#213784=CARTESIAN_POINT('Ctrl Pts',(23.8941285782002,7.56650497863791,0.));
#213785=CARTESIAN_POINT('Ctrl Pts',(23.8941285782002,7.56650497863791,12.));
#213786=CARTESIAN_POINT('Ctrl Pts',(23.9196224070759,7.56275769304773,0.));
#213787=CARTESIAN_POINT('Ctrl Pts',(23.9196224070759,7.56275769304773,12.));
#213788=CARTESIAN_POINT('Ctrl Pts',(23.9451848115002,7.5589389702768,0.));
#213789=CARTESIAN_POINT('Ctrl Pts',(23.9451848115002,7.5589389702768,12.));
#213790=CARTESIAN_POINT('Ctrl Pts',(23.9708152779886,7.55504862424808,0.));
#213791=CARTESIAN_POINT('Ctrl Pts',(23.9708152779886,7.55504862424808,12.));
#213792=CARTESIAN_POINT('Ctrl Pts',(23.9965132953187,7.55108647097432,0.));
#213793=CARTESIAN_POINT('Ctrl Pts',(23.9965132953187,7.55108647097432,12.));
#213794=CARTESIAN_POINT('Ctrl Pts',(24.0222783554531,7.54705232885895,0.));
#213795=CARTESIAN_POINT('Ctrl Pts',(24.0222783554531,7.54705232885895,12.));
#213796=CARTESIAN_POINT('Ctrl Pts',(24.0481099543353,7.54294601896128,0.));
#213797=CARTESIAN_POINT('Ctrl Pts',(24.0481099543353,7.54294601896128,12.));
#213798=CARTESIAN_POINT('Ctrl Pts',(24.0740075927984,7.53876736531005,0.));
#213799=CARTESIAN_POINT('Ctrl Pts',(24.0740075927984,7.53876736531005,12.));
#213800=CARTESIAN_POINT('Ctrl Pts',(24.0999707772642,7.53451619514659,0.));
#213801=CARTESIAN_POINT('Ctrl Pts',(24.0999707772642,7.53451619514659,12.));
#213802=CARTESIAN_POINT('Ctrl Pts',(24.1259990209211,7.53019233935537,0.));
#213803=CARTESIAN_POINT('Ctrl Pts',(24.1259990209211,7.53019233935537,12.));
#213804=CARTESIAN_POINT('Ctrl Pts',(24.152091842537,7.52579563201479,0.));
#213805=CARTESIAN_POINT('Ctrl Pts',(24.152091842537,7.52579563201479,12.));
#213806=CARTESIAN_POINT('Ctrl Pts',(24.1782487641602,7.52132590953863,0.));
#213807=CARTESIAN_POINT('Ctrl Pts',(24.1782487641602,7.52132590953863,12.));
#213808=CARTESIAN_POINT('Ctrl Pts',(24.2044693092356,7.51678300997998,0.));
#213809=CARTESIAN_POINT('Ctrl Pts',(24.2044693092356,7.51678300997998,12.));
#213810=CARTESIAN_POINT('Ctrl Pts',(24.230753000389,7.51216677222199,0.));
#213811=CARTESIAN_POINT('Ctrl Pts',(24.230753000389,7.51216677222199,12.));
#213812=CARTESIAN_POINT('Ctrl Pts',(24.2570993577032,7.50747703535115,0.));
#213813=CARTESIAN_POINT('Ctrl Pts',(24.2570993577032,7.50747703535115,12.));
#213814=CARTESIAN_POINT('Ctrl Pts',(24.2835078958966,7.50271363765099,0.));
#213815=CARTESIAN_POINT('Ctrl Pts',(24.2835078958966,7.50271363765099,12.));
#213816=CARTESIAN_POINT('Ctrl Pts',(24.3099781253345,7.49787641695359,0.));
#213817=CARTESIAN_POINT('Ctrl Pts',(24.3099781253345,7.49787641695359,12.));
#213818=CARTESIAN_POINT('Ctrl Pts',(24.3365095573673,7.4929652125233,0.));
#213819=CARTESIAN_POINT('Ctrl Pts',(24.3365095573673,7.4929652125233,12.));
#213820=CARTESIAN_POINT('Ctrl Pts',(24.3631017084513,7.48797986651828,0.));
#213821=CARTESIAN_POINT('Ctrl Pts',(24.3631017084513,7.48797986651828,12.));
#213822=CARTESIAN_POINT('Ctrl Pts',(24.3897541049248,7.48292022569254,0.));
#213823=CARTESIAN_POINT('Ctrl Pts',(24.3897541049248,7.48292022569254,12.));
#213824=CARTESIAN_POINT('Ctrl Pts',(24.4164662871165,7.47778614286574,0.));
#213825=CARTESIAN_POINT('Ctrl Pts',(24.4164662871165,7.47778614286574,12.));
#213826=CARTESIAN_POINT('Ctrl Pts',(24.4432378146501,7.47257747883319,0.));
#213827=CARTESIAN_POINT('Ctrl Pts',(24.4432378146501,7.47257747883319,12.));
#213828=CARTESIAN_POINT('Ctrl Pts',(24.4700682684544,7.46729410308923,0.));
#213829=CARTESIAN_POINT('Ctrl Pts',(24.4700682684544,7.46729410308923,12.));
#213830=CARTESIAN_POINT('Ctrl Pts',(24.4969572391509,7.46193588961642,0.));
#213831=CARTESIAN_POINT('Ctrl Pts',(24.4969572391509,7.46193588961642,12.));
#213832=CARTESIAN_POINT('Ctrl Pts',(24.52390431731,7.45650271336046,0.));
#213833=CARTESIAN_POINT('Ctrl Pts',(24.52390431731,7.45650271336046,12.));
#213834=CARTESIAN_POINT('Ctrl Pts',(24.5509090831579,7.45099444651296,0.));
#213835=CARTESIAN_POINT('Ctrl Pts',(24.5509090831579,7.45099444651296,12.));
#213836=CARTESIAN_POINT('Ctrl Pts',(24.5779710960865,7.44541095473163,0.));
#213837=CARTESIAN_POINT('Ctrl Pts',(24.5779710960865,7.44541095473163,12.));
#213838=CARTESIAN_POINT('Ctrl Pts',(24.6050898852349,7.43975209375375,0.));
#213839=CARTESIAN_POINT('Ctrl Pts',(24.6050898852349,7.43975209375375,12.));
#213840=CARTESIAN_POINT('Ctrl Pts',(24.6322649369472,7.43401770489221,0.));
#213841=CARTESIAN_POINT('Ctrl Pts',(24.6322649369472,7.43401770489221,12.));
#213842=CARTESIAN_POINT('Ctrl Pts',(24.659495712869,7.42820762158681,0.));
#213843=CARTESIAN_POINT('Ctrl Pts',(24.659495712869,7.42820762158681,12.));
#213844=CARTESIAN_POINT('Ctrl Pts',(24.6867816727118,7.42232167765763,0.));
#213845=CARTESIAN_POINT('Ctrl Pts',(24.6867816727118,7.42232167765763,12.));
#213846=CARTESIAN_POINT('Ctrl Pts',(24.7141222949988,7.41635971481243,0.));
#213847=CARTESIAN_POINT('Ctrl Pts',(24.7141222949988,7.41635971481243,12.));
#213848=CARTESIAN_POINT('Ctrl Pts',(24.7415170994754,7.41032159082173,0.));
#213849=CARTESIAN_POINT('Ctrl Pts',(24.7415170994754,7.41032159082173,12.));
#213850=CARTESIAN_POINT('Ctrl Pts',(24.7689656669005,7.40420718661755,0.));
#213851=CARTESIAN_POINT('Ctrl Pts',(24.7689656669005,7.40420718661755,12.));
#213852=CARTESIAN_POINT('Ctrl Pts',(24.7964676646518,7.39801641583613,0.));
#213853=CARTESIAN_POINT('Ctrl Pts',(24.7964676646518,7.39801641583613,12.));
#213854=CARTESIAN_POINT('Ctrl Pts',(24.8240228521042,7.39174922586841,0.));
#213855=CARTESIAN_POINT('Ctrl Pts',(24.8240228521042,7.39174922586841,12.));
#213856=CARTESIAN_POINT('Ctrl Pts',(24.8516310625367,7.38540558904946,0.));
#213857=CARTESIAN_POINT('Ctrl Pts',(24.8516310625367,7.38540558904946,12.));
#213858=CARTESIAN_POINT('Ctrl Pts',(24.8792921911309,7.3789854964161,0.));
#213859=CARTESIAN_POINT('Ctrl Pts',(24.8792921911309,7.3789854964161,12.));
#213860=CARTESIAN_POINT('Ctrl Pts',(24.9014633826201,7.37378825962718,0.));
#213861=CARTESIAN_POINT('Ctrl Pts',(24.9014633826201,7.37378825962718,12.));
#213862=CARTESIAN_POINT('Ctrl Pts',(24.9181155530631,7.36985593120697,0.));
#213863=CARTESIAN_POINT('Ctrl Pts',(24.9181155530631,7.36985593120697,12.));
#213864=CARTESIAN_POINT('Ctrl Pts',(24.9292275670705,7.3672190902906,0.));
#213865=CARTESIAN_POINT('Ctrl Pts',(24.9292275670705,7.3672190902906,12.));
#213866=CARTESIAN_POINT('Ctrl Pts',(24.9347862158358,7.36589684767344,0.));
#213867=CARTESIAN_POINT('Ctrl Pts',(24.9347862158358,7.36589684767344,12.));
#213868=CARTESIAN_POINT('',(24.9347862158358,7.36589684767344,0.));
#213869=CARTESIAN_POINT('Ctrl Pts',(21.2610617890679,7.52250298901264,0.));
#213870=CARTESIAN_POINT('Ctrl Pts',(21.2610673466886,7.5225064970397,0.));
#213871=CARTESIAN_POINT('Ctrl Pts',(21.2611204474866,7.52252744144904,0.));
#213872=CARTESIAN_POINT('Ctrl Pts',(21.261326054066,7.52260064231661,0.));
#213873=CARTESIAN_POINT('Ctrl Pts',(21.2618521283555,7.5227818224267,0.));
#213874=CARTESIAN_POINT('Ctrl Pts',(21.262927782038,7.52314642316199,0.));
#213875=CARTESIAN_POINT('Ctrl Pts',(21.2644161259962,7.52364573027553,0.));
#213876=CARTESIAN_POINT('Ctrl Pts',(21.2663059157058,7.52427261074298,0.));
#213877=CARTESIAN_POINT('Ctrl Pts',(21.2685823838671,7.52501770333531,0.));
#213878=CARTESIAN_POINT('Ctrl Pts',(21.2712301573466,7.5258712609553,0.));
#213879=CARTESIAN_POINT('Ctrl Pts',(21.2742366113579,7.52682526918541,0.));
#213880=CARTESIAN_POINT('Ctrl Pts',(21.2775925269652,7.52787386225333,0.));
#213881=CARTESIAN_POINT('Ctrl Pts',(21.2812902781143,7.52901217930408,0.));
#213882=CARTESIAN_POINT('Ctrl Pts',(21.2853226580657,7.5302356243823,0.));
#213883=CARTESIAN_POINT('Ctrl Pts',(21.2896816163842,7.53153906987856,0.));
#213884=CARTESIAN_POINT('Ctrl Pts',(21.2943588989331,7.53291726078527,0.));
#213885=CARTESIAN_POINT('Ctrl Pts',(21.2993464250717,7.53436505309943,0.));
#213886=CARTESIAN_POINT('Ctrl Pts',(21.3046368712157,7.53587778251736,0.));
#213887=CARTESIAN_POINT('Ctrl Pts',(21.310223716773,7.53745129364616,0.));
#213888=CARTESIAN_POINT('Ctrl Pts',(21.3161009456256,7.53908175169899,0.));
#213889=CARTESIAN_POINT('Ctrl Pts',(21.3222628524165,7.54076552038279,0.));
#213890=CARTESIAN_POINT('Ctrl Pts',(21.328703791771,7.54249900377031,0.));
#213891=CARTESIAN_POINT('Ctrl Pts',(21.3354182340149,7.54427868151268,0.));
#213892=CARTESIAN_POINT('Ctrl Pts',(21.3424008295038,7.54610114948347,0.));
#213893=CARTESIAN_POINT('Ctrl Pts',(21.3496464761531,7.54796316246331,0.));
#213894=CARTESIAN_POINT('Ctrl Pts',(21.3571503685855,7.5498616652131,0.));
#213895=CARTESIAN_POINT('Ctrl Pts',(21.3649079431865,7.55179375777444,0.));
#213896=CARTESIAN_POINT('Ctrl Pts',(21.3729148390243,7.55375667080029,0.));
#213897=CARTESIAN_POINT('Ctrl Pts',(21.3811668478932,7.55574773403503,0.));
#213898=CARTESIAN_POINT('Ctrl Pts',(21.3896598842117,7.55776435731417,0.));
#213899=CARTESIAN_POINT('Ctrl Pts',(21.3983899952987,7.55980403700611,0.));
#213900=CARTESIAN_POINT('Ctrl Pts',(21.4073533630365,7.56186435703622,0.));
#213901=CARTESIAN_POINT('Ctrl Pts',(21.4165463106254,7.56394299313685,0.));
#213902=CARTESIAN_POINT('Ctrl Pts',(21.4259653015736,7.56603771218712,0.));
#213903=CARTESIAN_POINT('Ctrl Pts',(21.4356069261513,7.56814636360848,0.));
#213904=CARTESIAN_POINT('Ctrl Pts',(21.4454678907509,7.57026687261166,0.));
#213905=CARTESIAN_POINT('Ctrl Pts',(21.4555450053142,7.57239723223506,0.));
#213906=CARTESIAN_POINT('Ctrl Pts',(21.4658351740128,7.57453549743412,0.));
#213907=CARTESIAN_POINT('Ctrl Pts',(21.4763353936762,7.57667978402987,0.));
#213908=CARTESIAN_POINT('Ctrl Pts',(21.4870427508194,7.57882826679132,0.));
#213909=CARTESIAN_POINT('Ctrl Pts',(21.4979544192744,7.58097917790744,0.));
#213910=CARTESIAN_POINT('Ctrl Pts',(21.5090676573873,7.5831308051918,0.));
#213911=CARTESIAN_POINT('Ctrl Pts',(21.5203798035299,7.5852814891913,0.));
#213912=CARTESIAN_POINT('Ctrl Pts',(21.5318882716736,7.58742962034834,0.));
#213913=CARTESIAN_POINT('Ctrl Pts',(21.543590547011,7.58957363620014,0.));
#213914=CARTESIAN_POINT('Ctrl Pts',(21.5554841813462,7.59171201844777,0.));
#213915=CARTESIAN_POINT('Ctrl Pts',(21.5675667904726,7.59384329124918,0.));
#213916=CARTESIAN_POINT('Ctrl Pts',(21.5798360518978,7.59596601973584,0.));
#213917=CARTESIAN_POINT('Ctrl Pts',(21.5922897024466,7.59807880846195,0.));
#213918=CARTESIAN_POINT('Ctrl Pts',(21.6049255358843,7.60018029988241,0.));
#213919=CARTESIAN_POINT('Ctrl Pts',(21.617741400599,7.60226917285429,0.));
#213920=CARTESIAN_POINT('Ctrl Pts',(21.6307351973822,7.60434414118296,0.));
#213921=CARTESIAN_POINT('Ctrl Pts',(21.6439048771743,7.60640395216357,0.));
#213922=CARTESIAN_POINT('Ctrl Pts',(21.6572484388081,7.60844738512874,0.));
#213923=CARTESIAN_POINT('Ctrl Pts',(21.6707639267576,7.61047325000956,0.));
#213924=CARTESIAN_POINT('Ctrl Pts',(21.6844494295815,7.61248038630269,0.));
#213925=CARTESIAN_POINT('Ctrl Pts',(21.6983030783322,7.61446766202787,0.));
#213926=CARTESIAN_POINT('Ctrl Pts',(21.7123230449834,7.61643397270421,0.));
#213927=CARTESIAN_POINT('Ctrl Pts',(21.7265075407975,7.61837824030538,0.));
#213928=CARTESIAN_POINT('Ctrl Pts',(21.7408548148656,7.62029941230855,0.));
#213929=CARTESIAN_POINT('Ctrl Pts',(21.7553631528328,7.62219646084229,0.));
#213930=CARTESIAN_POINT('Ctrl Pts',(21.7700308755584,7.62406838181166,0.));
#213931=CARTESIAN_POINT('Ctrl Pts',(21.7848563378021,7.62591419404513,0.));
#213932=CARTESIAN_POINT('Ctrl Pts',(21.799837926858,7.62773293842389,0.));
#213933=CARTESIAN_POINT('Ctrl Pts',(21.814974061509,7.62952367718127,0.));
#213934=CARTESIAN_POINT('Ctrl Pts',(21.8302631910195,7.63128549323023,0.));
#213935=CARTESIAN_POINT('Ctrl Pts',(21.8457037941084,7.63301748948936,0.));
#213936=CARTESIAN_POINT('Ctrl Pts',(21.8612943779089,7.63471878821226,0.));
#213937=CARTESIAN_POINT('Ctrl Pts',(21.8770334769496,7.636388530334,0.));
#213938=CARTESIAN_POINT('Ctrl Pts',(21.8929196523514,7.63802587492035,0.));
#213939=CARTESIAN_POINT('Ctrl Pts',(21.9089514909874,7.63962999860927,0.));
#213940=CARTESIAN_POINT('Ctrl Pts',(21.9251276046545,7.64120009506532,0.));
#213941=CARTESIAN_POINT('Ctrl Pts',(21.9414466292072,7.64273537442682,0.));
#213942=CARTESIAN_POINT('Ctrl Pts',(21.9579072237651,7.64423506279123,0.));
#213943=CARTESIAN_POINT('Ctrl Pts',(21.9745080700798,7.64569840177336,0.));
#213944=CARTESIAN_POINT('Ctrl Pts',(21.9912478718542,7.6471246480525,0.));
#213945=CARTESIAN_POINT('Ctrl Pts',(22.0081253540774,7.64851307293352,0.));
#213946=CARTESIAN_POINT('Ctrl Pts',(22.0251392623209,7.64986296190169,0.));
#213947=CARTESIAN_POINT('Ctrl Pts',(22.0422883621174,7.65117361421359,0.));
#213948=CARTESIAN_POINT('Ctrl Pts',(22.0595714384431,7.65244434253113,0.));
#213949=CARTESIAN_POINT('Ctrl Pts',(22.0769872951596,7.65367447254949,0.));
#213950=CARTESIAN_POINT('Ctrl Pts',(22.094534754469,7.65486334263644,0.));
#213951=CARTESIAN_POINT('Ctrl Pts',(22.1122126563329,7.65601030346807,0.));
#213952=CARTESIAN_POINT('Ctrl Pts',(22.1300198579675,7.65711471769397,0.));
#213953=CARTESIAN_POINT('Ctrl Pts',(22.1479552334211,7.65817595963349,0.));
#213954=CARTESIAN_POINT('Ctrl Pts',(22.1660176731178,7.65919341496931,0.));
#213955=CARTESIAN_POINT('Ctrl Pts',(22.1842060834091,7.66016648045005,0.));
#213956=CARTESIAN_POINT('Ctrl Pts',(22.2025193860964,7.66109456359271,0.));
#213957=CARTESIAN_POINT('Ctrl Pts',(22.2209565180085,7.661977082404,0.));
#213958=CARTESIAN_POINT('Ctrl Pts',(22.2395164306547,7.66281346512509,0.));
#213959=CARTESIAN_POINT('Ctrl Pts',(22.258198089848,7.66360314997641,0.));
#213960=CARTESIAN_POINT('Ctrl Pts',(22.2770004753335,7.66434558490979,0.));
#213961=CARTESIAN_POINT('Ctrl Pts',(22.2959225803937,7.66504022736299,0.));
#213962=CARTESIAN_POINT('Ctrl Pts',(22.314963411484,7.66568654402494,0.));
#213963=CARTESIAN_POINT('Ctrl Pts',(22.3341219879469,7.66628401061952,0.));
#213964=CARTESIAN_POINT('Ctrl Pts',(22.3533973417021,7.66683211169159,0.));
#213965=CARTESIAN_POINT('Ctrl Pts',(22.372788516936,7.66733034039883,0.));
#213966=CARTESIAN_POINT('Ctrl Pts',(22.3922945697773,7.6677781983079,0.));
#213967=CARTESIAN_POINT('Ctrl Pts',(22.4119145679758,7.6681751951964,0.));
#213968=CARTESIAN_POINT('Ctrl Pts',(22.4316475906603,7.66852084886704,0.));
#213969=CARTESIAN_POINT('Ctrl Pts',(22.4514927280855,7.66881468496635,0.));
#213970=CARTESIAN_POINT('Ctrl Pts',(22.4714490813699,7.66905623680831,0.));
#213971=CARTESIAN_POINT('Ctrl Pts',(22.4915157622312,7.66924504520315,0.));
#213972=CARTESIAN_POINT('Ctrl Pts',(22.5116918927031,7.66938065829108,0.));
#213973=CARTESIAN_POINT('Ctrl Pts',(22.53197660492,7.66946263138144,0.));
#213974=CARTESIAN_POINT('Ctrl Pts',(22.5523690409116,7.66949052679693,0.));
#213975=CARTESIAN_POINT('Ctrl Pts',(22.5728683523831,7.66946391372306,0.));
#213976=CARTESIAN_POINT('Ctrl Pts',(22.5934737004953,7.66938236806233,0.));
#213977=CARTESIAN_POINT('Ctrl Pts',(22.6141842556243,7.66924547229414,0.));
#213978=CARTESIAN_POINT('Ctrl Pts',(22.6349991971541,7.66905281533715,0.));
#213979=CARTESIAN_POINT('Ctrl Pts',(22.6559177133127,7.66880399241323,0.));
#213980=CARTESIAN_POINT('Ctrl Pts',(22.6769390009885,7.66849860491743,0.));
#213981=CARTESIAN_POINT('Ctrl Pts',(22.6980622655446,7.66813626029275,0.));
#213982=CARTESIAN_POINT('Ctrl Pts',(22.7192867206245,7.66771657191028,0.));
#213983=CARTESIAN_POINT('Ctrl Pts',(22.7406115879513,7.6672391589544,0.));
#213984=CARTESIAN_POINT('Ctrl Pts',(22.7620360971843,7.66670364630299,0.));
#213985=CARTESIAN_POINT('Ctrl Pts',(22.7835594857699,7.66610966441273,0.));
#213986=CARTESIAN_POINT('Ctrl Pts',(22.8051809987833,7.66545684920987,0.));
#213987=CARTESIAN_POINT('Ctrl Pts',(22.8268998887678,7.66474484198549,0.));
#213988=CARTESIAN_POINT('Ctrl Pts',(22.848715415557,7.66397328929803,0.));
#213989=CARTESIAN_POINT('Ctrl Pts',(22.8706268461283,7.66314184287337,0.));
#213990=CARTESIAN_POINT('Ctrl Pts',(22.8926334544883,7.66225015950156,0.));
#213991=CARTESIAN_POINT('Ctrl Pts',(22.9147345215421,7.66129790094108,0.));
#213992=CARTESIAN_POINT('Ctrl Pts',(22.9369293349593,7.66028473382778,0.));
#213993=CARTESIAN_POINT('Ctrl Pts',(22.959217189033,7.65921032958902,0.));
#213994=CARTESIAN_POINT('Ctrl Pts',(22.9815973845296,7.65807436436432,0.));
#213995=CARTESIAN_POINT('Ctrl Pts',(23.0040692285814,7.65687651891305,0.));
#213996=CARTESIAN_POINT('Ctrl Pts',(23.0266320345787,7.65561647852534,0.));
#213997=CARTESIAN_POINT('Ctrl Pts',(23.0492851220528,7.65429393293946,0.));
#213998=CARTESIAN_POINT('Ctrl Pts',(23.072027816555,7.65290857626358,0.));
#213999=CARTESIAN_POINT('Ctrl Pts',(23.094859449525,7.65146010690476,0.));
#214000=CARTESIAN_POINT('Ctrl Pts',(23.1177793581679,7.6499482274986,0.));
#214001=CARTESIAN_POINT('Ctrl Pts',(23.1407868853819,7.64837264482943,0.));
#214002=CARTESIAN_POINT('Ctrl Pts',(23.1638813796694,7.64673306975805,0.));
#214003=CARTESIAN_POINT('Ctrl Pts',(23.1870621950452,7.64502921715483,0.));
#214004=CARTESIAN_POINT('Ctrl Pts',(23.2103286909398,7.6432608058368,0.));
#214005=CARTESIAN_POINT('Ctrl Pts',(23.2336802320912,7.64142755851505,0.));
#214006=CARTESIAN_POINT('Ctrl Pts',(23.2571161884488,7.63952920172835,0.));
#214007=CARTESIAN_POINT('Ctrl Pts',(23.2806359350855,7.63756546576374,0.));
#214008=CARTESIAN_POINT('Ctrl Pts',(23.3042388521022,7.63553608458783,0.));
#214009=CARTESIAN_POINT('Ctrl Pts',(23.3279243245241,7.63344079578162,0.));
#214010=CARTESIAN_POINT('Ctrl Pts',(23.3516917421972,7.63127934048137,0.));
#214011=CARTESIAN_POINT('Ctrl Pts',(23.3755404996636,7.62905146332593,0.));
#214012=CARTESIAN_POINT('Ctrl Pts',(23.399469996112,7.62675691240329,0.));
#214013=CARTESIAN_POINT('Ctrl Pts',(23.4234796353542,7.6243954392005,0.));
#214014=CARTESIAN_POINT('Ctrl Pts',(23.4475688257854,7.62196679855955,0.));
#214015=CARTESIAN_POINT('Ctrl Pts',(23.4717369803438,7.61947074863977,0.));
#214016=CARTESIAN_POINT('Ctrl Pts',(23.4959835164609,7.61690705088319,0.));
#214017=CARTESIAN_POINT('Ctrl Pts',(23.5203078560129,7.61427546999298,0.));
#214018=CARTESIAN_POINT('Ctrl Pts',(23.544709425203,7.61157577385372,0.));
#214019=CARTESIAN_POINT('Ctrl Pts',(23.5691876544244,7.608807733446,0.));
#214020=CARTESIAN_POINT('Ctrl Pts',(23.5937419781245,7.60597112277094,0.));
#214021=CARTESIAN_POINT('Ctrl Pts',(23.6183718346576,7.60306571877806,0.));
#214022=CARTESIAN_POINT('Ctrl Pts',(23.6430766661418,7.60009130130126,0.));
#214023=CARTESIAN_POINT('Ctrl Pts',(23.6678559182875,7.59704765299567,0.));
#214024=CARTESIAN_POINT('Ctrl Pts',(23.6927090405066,7.59393455934035,0.));
#214025=CARTESIAN_POINT('Ctrl Pts',(23.7176354860456,7.59075180865321,0.));
#214026=CARTESIAN_POINT('Ctrl Pts',(23.7426347121006,7.58749919210826,0.));
#214027=CARTESIAN_POINT('Ctrl Pts',(23.7677061799376,7.58417650376271,0.));
#214028=CARTESIAN_POINT('Ctrl Pts',(23.7928493549908,7.58078354058213,0.));
#214029=CARTESIAN_POINT('Ctrl Pts',(23.8180637069976,7.57732010249066,0.));
#214030=CARTESIAN_POINT('Ctrl Pts',(23.8433487096132,7.57378599219814,0.));
#214031=CARTESIAN_POINT('Ctrl Pts',(23.8687038399595,7.57018101500709,0.));
#214032=CARTESIAN_POINT('Ctrl Pts',(23.8941285782002,7.56650497863791,0.));
#214033=CARTESIAN_POINT('Ctrl Pts',(23.9196224070759,7.56275769304773,0.));
#214034=CARTESIAN_POINT('Ctrl Pts',(23.9451848115002,7.5589389702768,0.));
#214035=CARTESIAN_POINT('Ctrl Pts',(23.9708152779886,7.55504862424808,0.));
#214036=CARTESIAN_POINT('Ctrl Pts',(23.9965132953187,7.55108647097432,0.));
#214037=CARTESIAN_POINT('Ctrl Pts',(24.0222783554531,7.54705232885895,0.));
#214038=CARTESIAN_POINT('Ctrl Pts',(24.0481099543353,7.54294601896128,0.));
#214039=CARTESIAN_POINT('Ctrl Pts',(24.0740075927984,7.53876736531005,0.));
#214040=CARTESIAN_POINT('Ctrl Pts',(24.0999707772642,7.53451619514659,0.));
#214041=CARTESIAN_POINT('Ctrl Pts',(24.1259990209211,7.53019233935537,0.));
#214042=CARTESIAN_POINT('Ctrl Pts',(24.152091842537,7.52579563201479,0.));
#214043=CARTESIAN_POINT('Ctrl Pts',(24.1782487641602,7.52132590953863,0.));
#214044=CARTESIAN_POINT('Ctrl Pts',(24.2044693092356,7.51678300997998,0.));
#214045=CARTESIAN_POINT('Ctrl Pts',(24.230753000389,7.51216677222199,0.));
#214046=CARTESIAN_POINT('Ctrl Pts',(24.2570993577032,7.50747703535115,0.));
#214047=CARTESIAN_POINT('Ctrl Pts',(24.2835078958966,7.50271363765099,0.));
#214048=CARTESIAN_POINT('Ctrl Pts',(24.3099781253345,7.49787641695359,0.));
#214049=CARTESIAN_POINT('Ctrl Pts',(24.3365095573673,7.4929652125233,0.));
#214050=CARTESIAN_POINT('Ctrl Pts',(24.3631017084513,7.48797986651828,0.));
#214051=CARTESIAN_POINT('Ctrl Pts',(24.3897541049248,7.48292022569254,0.));
#214052=CARTESIAN_POINT('Ctrl Pts',(24.4164662871165,7.47778614286574,0.));
#214053=CARTESIAN_POINT('Ctrl Pts',(24.4432378146501,7.47257747883319,0.));
#214054=CARTESIAN_POINT('Ctrl Pts',(24.4700682684544,7.46729410308923,0.));
#214055=CARTESIAN_POINT('Ctrl Pts',(24.4969572391509,7.46193588961642,0.));
#214056=CARTESIAN_POINT('Ctrl Pts',(24.52390431731,7.45650271336046,0.));
#214057=CARTESIAN_POINT('Ctrl Pts',(24.5509090831579,7.45099444651296,0.));
#214058=CARTESIAN_POINT('Ctrl Pts',(24.5779710960865,7.44541095473163,0.));
#214059=CARTESIAN_POINT('Ctrl Pts',(24.6050898852349,7.43975209375375,0.));
#214060=CARTESIAN_POINT('Ctrl Pts',(24.6322649369472,7.43401770489221,0.));
#214061=CARTESIAN_POINT('Ctrl Pts',(24.659495712869,7.42820762158681,0.));
#214062=CARTESIAN_POINT('Ctrl Pts',(24.6867816727118,7.42232167765763,0.));
#214063=CARTESIAN_POINT('Ctrl Pts',(24.7141222949988,7.41635971481243,0.));
#214064=CARTESIAN_POINT('Ctrl Pts',(24.7415170994754,7.41032159082173,0.));
#214065=CARTESIAN_POINT('Ctrl Pts',(24.7689656669005,7.40420718661755,0.));
#214066=CARTESIAN_POINT('Ctrl Pts',(24.7964676646518,7.39801641583613,0.));
#214067=CARTESIAN_POINT('Ctrl Pts',(24.8240228521042,7.39174922586841,0.));
#214068=CARTESIAN_POINT('Ctrl Pts',(24.8516310625367,7.38540558904946,0.));
#214069=CARTESIAN_POINT('Ctrl Pts',(24.8792921911309,7.3789854964161,0.));
#214070=CARTESIAN_POINT('Ctrl Pts',(24.9014633826201,7.37378825962718,0.));
#214071=CARTESIAN_POINT('Ctrl Pts',(24.9181155530631,7.36985593120697,0.));
#214072=CARTESIAN_POINT('Ctrl Pts',(24.9292275670705,7.3672190902906,0.));
#214073=CARTESIAN_POINT('Ctrl Pts',(24.9347862158358,7.36589684767344,0.));
#214074=CARTESIAN_POINT('',(24.9347862158358,7.36589684767344,0.));
#214075=CARTESIAN_POINT('Origin',(0.,0.,0.));
#214076=CARTESIAN_POINT('Origin',(0.,0.,0.));
#214077=CARTESIAN_POINT('Origin',(0.,0.,0.));
#214078=CARTESIAN_POINT('Origin',(0.,0.,0.));
#214079=CARTESIAN_POINT('Origin',(0.,0.,0.));
#214080=CARTESIAN_POINT('Origin',(0.,0.,0.));
#214081=CARTESIAN_POINT('Origin',(0.,0.,0.));
#214082=CARTESIAN_POINT('Origin',(0.,0.,0.));
#214083=CARTESIAN_POINT('Origin',(0.,0.,0.));
#214084=CARTESIAN_POINT('Origin',(0.,0.,0.));
#214085=CARTESIAN_POINT('Origin',(0.,0.,0.));
#214086=CARTESIAN_POINT('Origin',(0.,0.,0.));
#214087=CARTESIAN_POINT('Origin',(0.,0.,0.));
#214088=CARTESIAN_POINT('Origin',(0.,0.,0.));
#214089=CARTESIAN_POINT('Origin',(0.,0.,0.));
#214090=CARTESIAN_POINT('Origin',(0.,0.,0.));
#214091=CARTESIAN_POINT('Origin',(0.,0.,0.));
#214092=CARTESIAN_POINT('Origin',(0.,0.,0.));
#214093=CARTESIAN_POINT('Origin',(0.,0.,0.));
#214094=CARTESIAN_POINT('Origin',(0.,0.,0.));
#214095=CARTESIAN_POINT('Origin',(0.,0.,0.));
#214096=CARTESIAN_POINT('Origin',(0.,0.,0.));
#214097=CARTESIAN_POINT('Origin',(0.,0.,0.));
#214098=CARTESIAN_POINT('',(25.2771067246846,6.08833931617698,0.));
#214099=CARTESIAN_POINT('Origin',(0.,0.,0.));
#214100=CARTESIAN_POINT('',(22.1738711152697,4.11585220600461,0.));
#214101=CARTESIAN_POINT('Ctrl Pts',(25.2771067246846,6.08833931617698,0.));
#214102=CARTESIAN_POINT('Ctrl Pts',(25.2729539149479,6.08441489609824,0.));
#214103=CARTESIAN_POINT('Ctrl Pts',(25.2646490489816,6.07657531787578,0.));
#214104=CARTESIAN_POINT('Ctrl Pts',(25.2521940105523,6.06484373634697,0.));
#214105=CARTESIAN_POINT('Ctrl Pts',(25.2355918138798,6.04925720151412,0.));
#214106=CARTESIAN_POINT('Ctrl Pts',(25.2148466201368,6.02986667390187,0.));
#214107=CARTESIAN_POINT('Ctrl Pts',(25.1941090269638,6.0105688180476,0.));
#214108=CARTESIAN_POINT('Ctrl Pts',(25.1733791296154,5.99136367859839,0.));
#214109=CARTESIAN_POINT('Ctrl Pts',(25.1526570863065,5.97225131495636,0.));
#214110=CARTESIAN_POINT('Ctrl Pts',(25.1319431317273,5.95323180187348,0.));
#214111=CARTESIAN_POINT('Ctrl Pts',(25.1112375971182,5.93430523086776,0.));
#214112=CARTESIAN_POINT('Ctrl Pts',(25.0905409050863,5.91547170844382,0.));
#214113=CARTESIAN_POINT('Ctrl Pts',(25.0698535426593,5.89673135155459,0.));
#214114=CARTESIAN_POINT('Ctrl Pts',(25.0491760405965,5.87808428385329,0.));
#214115=CARTESIAN_POINT('Ctrl Pts',(25.0285089498922,5.8595306315681,0.));
#214116=CARTESIAN_POINT('Ctrl Pts',(25.0078528200558,5.84107051963074,0.));
#214117=CARTESIAN_POINT('Ctrl Pts',(24.9872081752709,5.82270406744214,0.));
#214118=CARTESIAN_POINT('Ctrl Pts',(24.9665754954462,5.80443138549747,0.));
#214119=CARTESIAN_POINT('Ctrl Pts',(24.9459552293308,5.78625257775703,0.));
#214120=CARTESIAN_POINT('Ctrl Pts',(24.9253478043632,5.76816774342236,0.));
#214121=CARTESIAN_POINT('Ctrl Pts',(24.9047536376467,5.75017697890813,0.));
#214122=CARTESIAN_POINT('Ctrl Pts',(24.8841731467219,5.73228037976927,0.));
#214123=CARTESIAN_POINT('Ctrl Pts',(24.8636067597677,5.71447804252019,0.));
#214124=CARTESIAN_POINT('Ctrl Pts',(24.8430549277634,5.6967700667943,0.));
#214125=CARTESIAN_POINT('Ctrl Pts',(24.822518122386,5.67915655496524,0.));
#214126=CARTESIAN_POINT('Ctrl Pts',(24.8019968304618,5.66163761114903,0.));
#214127=CARTESIAN_POINT('Ctrl Pts',(24.7814915496728,5.64421334042248,0.));
#214128=CARTESIAN_POINT('Ctrl Pts',(24.76100278357,5.62688384790919,0.));
#214129=CARTESIAN_POINT('Ctrl Pts',(24.7405310372736,5.60964923798495,0.));
#214130=CARTESIAN_POINT('Ctrl Pts',(24.7200768119079,5.59250961323995,0.));
#214131=CARTESIAN_POINT('Ctrl Pts',(24.6996406035507,5.57546507427767,0.));
#214132=CARTESIAN_POINT('Ctrl Pts',(24.6792229061785,5.55851572025389,0.));
#214133=CARTESIAN_POINT('Ctrl Pts',(24.6588242134733,5.54166164919593,0.));
#214134=CARTESIAN_POINT('Ctrl Pts',(24.6384450211466,5.52490295840996,0.));
#214135=CARTESIAN_POINT('Ctrl Pts',(24.618085828918,5.50823974481959,0.));
#214136=CARTESIAN_POINT('Ctrl Pts',(24.5977471429365,5.49167210537235,0.));
#214137=CARTESIAN_POINT('Ctrl Pts',(24.5774294770329,5.47520013724403,0.));
#214138=CARTESIAN_POINT('Ctrl Pts',(24.5571333514841,5.45882393762244,0.));
#214139=CARTESIAN_POINT('Ctrl Pts',(24.5368592922861,5.44254360356866,0.));
#214140=CARTESIAN_POINT('Ctrl Pts',(24.5166078302107,5.42635923183411,0.));
#214141=CARTESIAN_POINT('Ctrl Pts',(24.4963794999831,5.41027091869242,0.));
#214142=CARTESIAN_POINT('Ctrl Pts',(24.4761748393322,5.39427875973831,0.));
#214143=CARTESIAN_POINT('Ctrl Pts',(24.4559943883159,5.37838284973706,0.));
#214144=CARTESIAN_POINT('Ctrl Pts',(24.4358386899152,5.36258328273639,0.));
#214145=CARTESIAN_POINT('Ctrl Pts',(24.4157082904615,5.34688015213546,0.));
#214146=CARTESIAN_POINT('Ctrl Pts',(24.3956037401293,5.33127355076037,0.));
#214147=CARTESIAN_POINT('Ctrl Pts',(24.3755255933917,5.31576357092525,0.));
#214148=CARTESIAN_POINT('Ctrl Pts',(24.3554744095075,5.30035030449059,0.));
#214149=CARTESIAN_POINT('Ctrl Pts',(24.3354507529415,5.28503384290644,0.));
#214150=CARTESIAN_POINT('Ctrl Pts',(24.3154551932222,5.26981427718796,0.));
#214151=CARTESIAN_POINT('Ctrl Pts',(24.2954883048448,5.25469169788856,0.));
#214152=CARTESIAN_POINT('Ctrl Pts',(24.2755506671526,5.23966619506289,0.));
#214153=CARTESIAN_POINT('Ctrl Pts',(24.2556428642294,5.22473785822441,0.));
#214154=CARTESIAN_POINT('Ctrl Pts',(24.2357654847765,5.20990677629173,0.));
#214155=CARTESIAN_POINT('Ctrl Pts',(24.215919122017,5.19517303753643,0.));
#214156=CARTESIAN_POINT('Ctrl Pts',(24.1961043738754,5.18053672961392,0.));
#214157=CARTESIAN_POINT('Ctrl Pts',(24.1763218431343,5.16599793957979,0.));
#214158=CARTESIAN_POINT('Ctrl Pts',(24.156572137597,5.15155675390075,0.));
#214159=CARTESIAN_POINT('Ctrl Pts',(24.1368558702443,5.13721325845745,0.));
#214160=CARTESIAN_POINT('Ctrl Pts',(24.117173659394,5.1229675385386,0.));
#214161=CARTESIAN_POINT('Ctrl Pts',(24.0975261288446,5.10881967883132,0.));
#214162=CARTESIAN_POINT('Ctrl Pts',(24.0779139079266,5.09476976342625,0.));
#214163=CARTESIAN_POINT('Ctrl Pts',(24.0583376315638,5.08081787581277,0.));
#214164=CARTESIAN_POINT('Ctrl Pts',(24.0387979403268,5.06696409886641,0.));
#214165=CARTESIAN_POINT('Ctrl Pts',(24.0192954804896,5.05320851483065,0.));
#214166=CARTESIAN_POINT('Ctrl Pts',(23.9998309040746,5.03955120528521,0.));
#214167=CARTESIAN_POINT('Ctrl Pts',(23.9804048689227,5.02599225112454,0.));
#214168=CARTESIAN_POINT('Ctrl Pts',(23.961018038827,5.01253173257453,0.));
#214169=CARTESIAN_POINT('Ctrl Pts',(23.9416710836529,4.99916972919307,0.));
#214170=CARTESIAN_POINT('Ctrl Pts',(23.9223646794592,4.98590631986533,0.));
#214171=CARTESIAN_POINT('Ctrl Pts',(23.9030995086163,4.97274158279227,0.));
#214172=CARTESIAN_POINT('Ctrl Pts',(23.8838762599218,4.95967559546561,0.));
#214173=CARTESIAN_POINT('Ctrl Pts',(23.8646956287168,4.9467084346586,0.));
#214174=CARTESIAN_POINT('Ctrl Pts',(23.8455583170057,4.93384017643432,0.));
#214175=CARTESIAN_POINT('Ctrl Pts',(23.8264650335717,4.92107089613969,0.));
#214176=CARTESIAN_POINT('Ctrl Pts',(23.8074164940896,4.90840066839344,0.));
#214177=CARTESIAN_POINT('Ctrl Pts',(23.7884134212384,4.89582956706775,0.));
#214178=CARTESIAN_POINT('Ctrl Pts',(23.7694565448049,4.88335766525573,0.));
#214179=CARTESIAN_POINT('Ctrl Pts',(23.7505466018245,4.87098503527152,0.));
#214180=CARTESIAN_POINT('Ctrl Pts',(23.7316843367313,4.85871174865499,0.));
#214181=CARTESIAN_POINT('Ctrl Pts',(23.7128705015017,4.84653787616426,0.));
#214182=CARTESIAN_POINT('Ctrl Pts',(23.6941058557971,4.83446348776266,0.));
#214183=CARTESIAN_POINT('Ctrl Pts',(23.675391167102,4.82248865259562,0.));
#214184=CARTESIAN_POINT('Ctrl Pts',(23.6567272108628,4.81061343896432,0.));
#214185=CARTESIAN_POINT('Ctrl Pts',(23.6381147706579,4.7988379143322,0.));
#214186=CARTESIAN_POINT('Ctrl Pts',(23.6195546383624,4.78716214532098,0.));
#214187=CARTESIAN_POINT('Ctrl Pts',(23.6010476143099,4.77558619769872,0.));
#214188=CARTESIAN_POINT('Ctrl Pts',(23.5825945074535,4.76411013636251,0.));
#214189=CARTESIAN_POINT('Ctrl Pts',(23.5641961355168,4.75273402530617,0.));
#214190=CARTESIAN_POINT('Ctrl Pts',(23.545853325171,4.74145792760699,0.));
#214191=CARTESIAN_POINT('Ctrl Pts',(23.5275669122372,4.7302819054303,0.));
#214192=CARTESIAN_POINT('Ctrl Pts',(23.509337741878,4.71920602001902,0.));
#214193=CARTESIAN_POINT('Ctrl Pts',(23.491166668789,4.70823033167819,0.));
#214194=CARTESIAN_POINT('Ctrl Pts',(23.4730545573853,4.69735489975024,0.));
#214195=CARTESIAN_POINT('Ctrl Pts',(23.455002281986,4.68657978258303,0.));
#214196=CARTESIAN_POINT('Ctrl Pts',(23.4370107270451,4.67590503753059,0.));
#214197=CARTESIAN_POINT('Ctrl Pts',(23.4190807873803,4.6653307209467,0.));
#214198=CARTESIAN_POINT('Ctrl Pts',(23.4012133683959,4.65485688816924,0.));
#214199=CARTESIAN_POINT('Ctrl Pts',(23.3834093863068,4.6444835934993,0.));
#214200=CARTESIAN_POINT('Ctrl Pts',(23.3656697683489,4.63421089016541,0.));
#214201=CARTESIAN_POINT('Ctrl Pts',(23.3479954530272,4.62403883030805,0.));
#214202=CARTESIAN_POINT('Ctrl Pts',(23.3303873903938,4.6139674649783,0.));
#214203=CARTESIAN_POINT('Ctrl Pts',(23.3128465423115,4.60399684412163,0.));
#214204=CARTESIAN_POINT('Ctrl Pts',(23.2953738827191,4.5941270165575,0.));
#214205=CARTESIAN_POINT('Ctrl Pts',(23.2779703978876,4.5843580299469,0.));
#214206=CARTESIAN_POINT('Ctrl Pts',(23.2606370866866,4.57468993076097,0.));
#214207=CARTESIAN_POINT('Ctrl Pts',(23.2433749609131,4.56512276427839,0.));
#214208=CARTESIAN_POINT('Ctrl Pts',(23.2261850456064,4.55565657456975,0.));
#214209=CARTESIAN_POINT('Ctrl Pts',(23.2090683793629,4.54629140447544,0.));
#214210=CARTESIAN_POINT('Ctrl Pts',(23.1920260146465,4.53702729557566,0.));
#214211=CARTESIAN_POINT('Ctrl Pts',(23.1750590180908,4.52786428815015,0.));
#214212=CARTESIAN_POINT('Ctrl Pts',(23.1581684708761,4.51880242116748,0.));
#214213=CARTESIAN_POINT('Ctrl Pts',(23.1413554691123,4.5098417322706,0.));
#214214=CARTESIAN_POINT('Ctrl Pts',(23.1246211242115,4.50098225775171,0.));
#214215=CARTESIAN_POINT('Ctrl Pts',(23.1079665632636,4.49222403252216,0.));
#214216=CARTESIAN_POINT('Ctrl Pts',(23.0913929293922,4.48356709006788,0.));
#214217=CARTESIAN_POINT('Ctrl Pts',(23.0749013821881,4.47501146242856,0.));
#214218=CARTESIAN_POINT('Ctrl Pts',(23.0584930981732,4.46655718018231,0.));
#214219=CARTESIAN_POINT('Ctrl Pts',(23.0421692712467,4.45820427241683,0.));
#214220=CARTESIAN_POINT('Ctrl Pts',(23.0259311131392,4.44995276669687,0.));
#214221=CARTESIAN_POINT('Ctrl Pts',(23.0097798538395,4.44180268901643,0.));
#214222=CARTESIAN_POINT('Ctrl Pts',(22.9937167421006,4.43375406376879,0.));
#214223=CARTESIAN_POINT('Ctrl Pts',(22.977743046002,4.42580691372752,0.));
#214224=CARTESIAN_POINT('Ctrl Pts',(22.9618600534866,4.41796126001302,0.));
#214225=CARTESIAN_POINT('Ctrl Pts',(22.9460690729093,4.41021712205554,0.));
#214226=CARTESIAN_POINT('Ctrl Pts',(22.930371433555,4.40257451754324,0.));
#214227=CARTESIAN_POINT('Ctrl Pts',(22.9147684862426,4.39503346238473,0.));
#214228=CARTESIAN_POINT('Ctrl Pts',(22.8992616040108,4.38759397068406,0.));
#214229=CARTESIAN_POINT('Ctrl Pts',(22.8838521827701,4.38025605470093,0.));
#214230=CARTESIAN_POINT('Ctrl Pts',(22.8685416419725,4.37301972480746,0.));
#214231=CARTESIAN_POINT('Ctrl Pts',(22.8533314252422,4.36588498942997,0.));
#214232=CARTESIAN_POINT('Ctrl Pts',(22.8382230011184,4.35885185500546,0.));
#214233=CARTESIAN_POINT('Ctrl Pts',(22.8232178638876,4.35192032594791,0.));
#214234=CARTESIAN_POINT('Ctrl Pts',(22.8083175343791,4.34509040460062,0.));
#214235=CARTESIAN_POINT('Ctrl Pts',(22.7935235607806,4.33836209118446,0.));
#214236=CARTESIAN_POINT('Ctrl Pts',(22.7788375194076,4.3317353837319,0.));
#214237=CARTESIAN_POINT('Ctrl Pts',(22.7642610156475,4.32521027803754,0.));
#214238=CARTESIAN_POINT('Ctrl Pts',(22.7497956849848,4.31878676761235,0.));
#214239=CARTESIAN_POINT('Ctrl Pts',(22.7354431939926,4.31246484362549,0.));
#214240=CARTESIAN_POINT('Ctrl Pts',(22.7212052413386,4.30624449484069,0.));
#214241=CARTESIAN_POINT('Ctrl Pts',(22.7070835587564,4.3001257075406,0.));
#214242=CARTESIAN_POINT('Ctrl Pts',(22.6930799122548,4.29410846547056,0.));
#214243=CARTESIAN_POINT('Ctrl Pts',(22.6791961033537,4.28819274977763,0.));
#214244=CARTESIAN_POINT('Ctrl Pts',(22.6654339703109,4.28237853894059,0.));
#214245=CARTESIAN_POINT('Ctrl Pts',(22.6517953893303,4.2766658086912,0.));
#214246=CARTESIAN_POINT('Ctrl Pts',(22.6382822758172,4.27105453193004,0.));
#214247=CARTESIAN_POINT('Ctrl Pts',(22.6248965859977,4.26554467865576,0.));
#214248=CARTESIAN_POINT('Ctrl Pts',(22.6116403184821,4.26013621588305,0.));
#214249=CARTESIAN_POINT('Ctrl Pts',(22.5985155158636,4.25482910755481,0.));
#214250=CARTESIAN_POINT('Ctrl Pts',(22.5855242662477,4.24962331444177,0.));
#214251=CARTESIAN_POINT('Ctrl Pts',(22.572668704992,4.24451879404851,0.));
#214252=CARTESIAN_POINT('Ctrl Pts',(22.5599510166429,4.23951550052523,0.));
#214253=CARTESIAN_POINT('Ctrl Pts',(22.5473734368086,4.23461338456712,0.));
#214254=CARTESIAN_POINT('Ctrl Pts',(22.5349382540588,4.22981239330733,0.));
#214255=CARTESIAN_POINT('Ctrl Pts',(22.5226478117886,4.22511247020041,0.));
#214256=CARTESIAN_POINT('Ctrl Pts',(22.5105045108881,4.22051355490196,0.));
#214257=CARTESIAN_POINT('Ctrl Pts',(22.4985108124228,4.21601558313906,0.));
#214258=CARTESIAN_POINT('Ctrl Pts',(22.4866692403147,4.21161848657428,0.));
#214259=CARTESIAN_POINT('Ctrl Pts',(22.4749823839917,4.20732219265649,0.));
#214260=CARTESIAN_POINT('Ctrl Pts',(22.4634529011437,4.20312662448174,0.));
#214261=CARTESIAN_POINT('Ctrl Pts',(22.4520835205422,4.19903170066358,0.));
#214262=CARTESIAN_POINT('Ctrl Pts',(22.4408770448917,4.1950373351886,0.));
#214263=CARTESIAN_POINT('Ctrl Pts',(22.4298363535416,4.19114343726932,0.));
#214264=CARTESIAN_POINT('Ctrl Pts',(22.4189644056109,4.18734991117707,0.));
#214265=CARTESIAN_POINT('Ctrl Pts',(22.4082642454448,4.18365665600839,0.));
#214266=CARTESIAN_POINT('Ctrl Pts',(22.3977390078074,4.18006356544879,0.));
#214267=CARTESIAN_POINT('Ctrl Pts',(22.3873919231339,4.17657052752834,0.));
#214268=CARTESIAN_POINT('Ctrl Pts',(22.3772263228624,4.17317742436162,0.));
#214269=CARTESIAN_POINT('Ctrl Pts',(22.3672456427605,4.1698841319947,0.));
#214270=CARTESIAN_POINT('Ctrl Pts',(22.3574534257397,4.16669052026602,0.));
#214271=CARTESIAN_POINT('Ctrl Pts',(22.3478533253886,4.1635964526318,0.));
#214272=CARTESIAN_POINT('Ctrl Pts',(22.3384491078599,4.16060178604154,0.));
#214273=CARTESIAN_POINT('Ctrl Pts',(22.3292446628957,4.15770637047882,0.));
#214274=CARTESIAN_POINT('Ctrl Pts',(22.3202440186979,4.15491004835278,0.));
#214275=CARTESIAN_POINT('Ctrl Pts',(22.3114513545186,4.15221265396993,0.));
#214276=CARTESIAN_POINT('Ctrl Pts',(22.3028710166935,4.14961401285526,0.));
#214277=CARTESIAN_POINT('Ctrl Pts',(22.2945075198468,4.14711394168559,0.));
#214278=CARTESIAN_POINT('Ctrl Pts',(22.2863655389167,4.14471224859295,0.));
#214279=CARTESIAN_POINT('Ctrl Pts',(22.2784499072026,4.14240873321982,0.));
#214280=CARTESIAN_POINT('Ctrl Pts',(22.2707656042456,4.14020318715988,0.));
#214281=CARTESIAN_POINT('Ctrl Pts',(22.263317791397,4.13809539255419,0.));
#214282=CARTESIAN_POINT('Ctrl Pts',(22.2561118708422,4.13608511977226,0.));
#214283=CARTESIAN_POINT('Ctrl Pts',(22.2491535317789,4.13417212558809,0.));
#214284=CARTESIAN_POINT('Ctrl Pts',(22.2424488153523,4.1323561506016,0.));
#214285=CARTESIAN_POINT('Ctrl Pts',(22.2360040565534,4.13063692157499,0.));
#214286=CARTESIAN_POINT('Ctrl Pts',(22.2298258043947,4.12901415463379,0.));
#214287=CARTESIAN_POINT('Ctrl Pts',(22.2239207458781,4.127487558301,0.));
#214288=CARTESIAN_POINT('Ctrl Pts',(22.2182956401341,4.126056836133,0.));
#214289=CARTESIAN_POINT('Ctrl Pts',(22.2129576146671,4.12472167516602,0.));
#214290=CARTESIAN_POINT('Ctrl Pts',(22.2079143941719,4.12348173702025,0.));
#214291=CARTESIAN_POINT('Ctrl Pts',(22.2031746532106,4.12233664408237,0.));
#214292=CARTESIAN_POINT('Ctrl Pts',(22.1987479618246,4.12128598183533,0.));
#214293=CARTESIAN_POINT('Ctrl Pts',(22.1946440958098,4.12032932637738,0.));
#214294=CARTESIAN_POINT('Ctrl Pts',(22.1908725908525,4.11946626228623,0.));
#214295=CARTESIAN_POINT('Ctrl Pts',(22.1874419861496,4.11869641271752,0.));
#214296=CARTESIAN_POINT('Ctrl Pts',(22.1843613164855,4.11801938107464,0.));
#214297=CARTESIAN_POINT('Ctrl Pts',(22.1816414985788,4.11743469691765,0.));
#214298=CARTESIAN_POINT('Ctrl Pts',(22.179297473024,4.11694173195041,0.));
#214299=CARTESIAN_POINT('Ctrl Pts',(22.177347426894,4.11653973150558,0.));
#214300=CARTESIAN_POINT('Ctrl Pts',(22.1758088296598,4.11622797217066,0.));
#214301=CARTESIAN_POINT('Ctrl Pts',(22.1746949858773,4.11600589882768,0.));
#214302=CARTESIAN_POINT('Ctrl Pts',(22.174148802123,4.11589976826061,0.));
#214303=CARTESIAN_POINT('Ctrl Pts',(22.1739341411684,4.1158603587821,0.));
#214304=CARTESIAN_POINT('Ctrl Pts',(22.1738776823239,4.11585194677412,0.));
#214305=CARTESIAN_POINT('Ctrl Pts',(22.1738711152697,4.11585220600461,0.));
#214306=CARTESIAN_POINT('',(21.624941921198,4.01396149767428,0.));
#214307=CARTESIAN_POINT('',(11.0869355576349,2.05792610300232,0.));
#214308=CARTESIAN_POINT('',(21.2226420728916,3.44230496120419,0.));
#214309=CARTESIAN_POINT('Origin',(21.7161918885402,3.52235856495312,0.));
#214310=CARTESIAN_POINT('',(21.3904321633055,2.16781269186828,0.));
#214311=CARTESIAN_POINT('Origin',(7.7715611723761E-13,7.16093850883226E-14,
0.));
#214312=CARTESIAN_POINT('',(21.9269795755927,1.71975774210841,0.));
#214313=CARTESIAN_POINT('Origin',(21.8878840740801,2.21822694051638,0.));
#214314=CARTESIAN_POINT('',(22.4835757167854,1.76341220531179,0.));
#214315=CARTESIAN_POINT('',(10.7170877657712,0.840553282521227,0.));
#214316=CARTESIAN_POINT('',(25.991588367311,0.661312440730894,0.));
#214317=CARTESIAN_POINT('Ctrl Pts',(22.4835757167854,1.76341220531179,0.));
#214318=CARTESIAN_POINT('Ctrl Pts',(22.483581992979,1.76341415538764,0.));
#214319=CARTESIAN_POINT('Ctrl Pts',(22.4836387052232,1.7634206426357,0.));
#214320=CARTESIAN_POINT('Ctrl Pts',(22.4838562517069,1.76343813434565,0.));
#214321=CARTESIAN_POINT('Ctrl Pts',(22.4844112933129,1.76347698284792,0.));
#214322=CARTESIAN_POINT('Ctrl Pts',(22.4855446605991,1.76355076045546,0.));
#214323=CARTESIAN_POINT('Ctrl Pts',(22.4871115206571,1.76364784232963,0.));
#214324=CARTESIAN_POINT('Ctrl Pts',(22.4890991659478,1.76376424879505,0.));
#214325=CARTESIAN_POINT('Ctrl Pts',(22.4914909094908,1.76389475965724,0.));
#214326=CARTESIAN_POINT('Ctrl Pts',(22.4942693792449,1.76403393880301,0.));
#214327=CARTESIAN_POINT('Ctrl Pts',(22.4974203063191,1.76417731243462,0.));
#214328=CARTESIAN_POINT('Ctrl Pts',(22.5009332677316,1.76432160068726,0.));
#214329=CARTESIAN_POINT('Ctrl Pts',(22.5047996391978,1.76446408210366,0.));
#214330=CARTESIAN_POINT('Ctrl Pts',(22.5090112700212,1.76460218257323,0.));
#214331=CARTESIAN_POINT('Ctrl Pts',(22.5135590569554,1.76473303281159,0.));
#214332=CARTESIAN_POINT('Ctrl Pts',(22.5184336670207,1.76485369319896,0.));
#214333=CARTESIAN_POINT('Ctrl Pts',(22.5236259635515,1.76496128643369,0.));
#214334=CARTESIAN_POINT('Ctrl Pts',(22.529127665298,1.76505320262752,0.));
#214335=CARTESIAN_POINT('Ctrl Pts',(22.5349313983571,1.7651271156325,0.));
#214336=CARTESIAN_POINT('Ctrl Pts',(22.5410303590891,1.76518087841493,0.));
#214337=CARTESIAN_POINT('Ctrl Pts',(22.5474180954006,1.76521245524047,0.));
#214338=CARTESIAN_POINT('Ctrl Pts',(22.5540882235837,1.76521983384063,0.));
#214339=CARTESIAN_POINT('Ctrl Pts',(22.5610344912501,1.7652010450045,0.));
#214340=CARTESIAN_POINT('Ctrl Pts',(22.5682508499873,1.76515418518829,0.));
#214341=CARTESIAN_POINT('Ctrl Pts',(22.5757315316355,1.76507744026747,0.));
#214342=CARTESIAN_POINT('Ctrl Pts',(22.5834711038024,1.76496910283089,0.));
#214343=CARTESIAN_POINT('Ctrl Pts',(22.5914644078106,1.76482755288411,0.));
#214344=CARTESIAN_POINT('Ctrl Pts',(22.5997065145638,1.76465124413556,0.));
#214345=CARTESIAN_POINT('Ctrl Pts',(22.6081926681342,1.76443868648015,0.));
#214346=CARTESIAN_POINT('Ctrl Pts',(22.6169182517693,1.76418843543739,0.));
#214347=CARTESIAN_POINT('Ctrl Pts',(22.6258787994847,1.76389909571402,0.));
#214348=CARTESIAN_POINT('Ctrl Pts',(22.635069997936,1.76356932176272,0.));
#214349=CARTESIAN_POINT('Ctrl Pts',(22.6444876940425,1.76319782013914,0.));
#214350=CARTESIAN_POINT('Ctrl Pts',(22.6541278938413,1.76278334912559,0.));
#214351=CARTESIAN_POINT('Ctrl Pts',(22.6639867471756,1.76232471392568,0.));
#214352=CARTESIAN_POINT('Ctrl Pts',(22.6740605356699,1.76182076289525,0.));
#214353=CARTESIAN_POINT('Ctrl Pts',(22.6843456585245,1.76127038310613,0.));
#214354=CARTESIAN_POINT('Ctrl Pts',(22.6948386219843,1.76067249704884,0.));
#214355=CARTESIAN_POINT('Ctrl Pts',(22.7055360375481,1.76002606202399,0.));
#214356=CARTESIAN_POINT('Ctrl Pts',(22.7164346186007,1.75933006905924,0.));
#214357=CARTESIAN_POINT('Ctrl Pts',(22.7275311777305,1.75858354204635,0.));
#214358=CARTESIAN_POINT('Ctrl Pts',(22.7388226235565,1.75778553673249,0.));
#214359=CARTESIAN_POINT('Ctrl Pts',(22.7503059556455,1.75693513908911,0.));
#214360=CARTESIAN_POINT('Ctrl Pts',(22.7619782595013,1.75603146371641,0.));
#214361=CARTESIAN_POINT('Ctrl Pts',(22.7738367016115,1.75507365227127,0.));
#214362=CARTESIAN_POINT('Ctrl Pts',(22.7858785242358,1.7540608718293,0.));
#214363=CARTESIAN_POINT('Ctrl Pts',(22.7981010424312,1.75299231391461,0.));
#214364=CARTESIAN_POINT('Ctrl Pts',(22.8105016414712,1.7518671936559,0.));
#214365=CARTESIAN_POINT('Ctrl Pts',(22.8230777741285,1.75068474890884,0.));
#214366=CARTESIAN_POINT('Ctrl Pts',(22.8358269579854,1.74944423940117,0.));
#214367=CARTESIAN_POINT('Ctrl Pts',(22.8487467728075,1.74814494588492,0.));
#214368=CARTESIAN_POINT('Ctrl Pts',(22.8618348580234,1.74678616930663,0.));
#214369=CARTESIAN_POINT('Ctrl Pts',(22.8750889101696,1.745367229982,0.));
#214370=CARTESIAN_POINT('Ctrl Pts',(22.8885066803351,1.74388746677702,0.));
#214371=CARTESIAN_POINT('Ctrl Pts',(22.9020859716144,1.74234623630079,0.));
#214372=CARTESIAN_POINT('Ctrl Pts',(22.9158246373365,1.74074291231057,0.));
#214373=CARTESIAN_POINT('Ctrl Pts',(22.9297205792587,1.73907688511665,0.));
#214374=CARTESIAN_POINT('Ctrl Pts',(22.9437717457825,1.73734756100038,0.));
#214375=CARTESIAN_POINT('Ctrl Pts',(22.9579761301062,1.73555436162771,0.));
#214376=CARTESIAN_POINT('Ctrl Pts',(22.9723317685688,1.73369672350818,0.));
#214377=CARTESIAN_POINT('Ctrl Pts',(22.9868367391978,1.73177409750194,0.));
#214378=CARTESIAN_POINT('Ctrl Pts',(23.0014891601891,1.72978594832137,0.));
#214379=CARTESIAN_POINT('Ctrl Pts',(23.0162871884167,1.72773175404703,0.));
#214380=CARTESIAN_POINT('Ctrl Pts',(23.031229017888,1.72561100564033,0.));
#214381=CARTESIAN_POINT('Ctrl Pts',(23.0463128785528,1.72342320653731,0.));
#214382=CARTESIAN_POINT('Ctrl Pts',(23.0615370351559,1.72116787225981,0.));
#214383=CARTESIAN_POINT('Ctrl Pts',(23.0768997860709,1.71884453003027,0.));
#214384=CARTESIAN_POINT('Ctrl Pts',(23.0923994621216,1.71645271839311,0.));
#214385=CARTESIAN_POINT('Ctrl Pts',(23.1080344254291,1.71399198684725,0.));
#214386=CARTESIAN_POINT('Ctrl Pts',(23.1238030684929,1.71146189552192,0.));
#214387=CARTESIAN_POINT('Ctrl Pts',(23.1397038132358,1.7088620148546,0.));
#214388=CARTESIAN_POINT('Ctrl Pts',(23.1557351100613,1.70619192527847,0.));
#214389=CARTESIAN_POINT('Ctrl Pts',(23.1718954368749,1.70345121691259,0.));
#214390=CARTESIAN_POINT('Ctrl Pts',(23.1881832981848,1.70063948926988,0.));
#214391=CARTESIAN_POINT('Ctrl Pts',(23.2045972243765,1.69775635099425,0.));
#214392=CARTESIAN_POINT('Ctrl Pts',(23.2211357709374,1.69480141959946,0.));
#214393=CARTESIAN_POINT('Ctrl Pts',(23.2377975177014,1.69177432121716,0.));
#214394=CARTESIAN_POINT('Ctrl Pts',(23.2545810680536,1.6886746903491,0.));
#214395=CARTESIAN_POINT('Ctrl Pts',(23.2714850482245,1.68550216963275,0.));
#214396=CARTESIAN_POINT('Ctrl Pts',(23.2885081066949,1.68225640962181,0.));
#214397=CARTESIAN_POINT('Ctrl Pts',(23.3056489135611,1.67893706857123,0.));
#214398=CARTESIAN_POINT('Ctrl Pts',(23.3229061599145,1.67554381222988,0.));
#214399=CARTESIAN_POINT('Ctrl Pts',(23.3402785571866,1.67207631363905,0.));
#214400=CARTESIAN_POINT('Ctrl Pts',(23.3577648365747,1.66853425293978,0.));
#214401=CARTESIAN_POINT('Ctrl Pts',(23.375363748555,1.66491731718864,0.));
#214402=CARTESIAN_POINT('Ctrl Pts',(23.3930740623622,1.66122520018008,0.));
#214403=CARTESIAN_POINT('Ctrl Pts',(23.4108945654803,1.65745760227507,0.));
#214404=CARTESIAN_POINT('Ctrl Pts',(23.4288240631034,1.6536142302373,0.));
#214405=CARTESIAN_POINT('Ctrl Pts',(23.446861377656,1.6496947970734,0.));
#214406=CARTESIAN_POINT('Ctrl Pts',(23.4650053483919,1.64569902187608,0.));
#214407=CARTESIAN_POINT('Ctrl Pts',(23.4832548309638,1.64162662967525,0.));
#214408=CARTESIAN_POINT('Ctrl Pts',(23.5016086970006,1.63747735129474,0.));
#214409=CARTESIAN_POINT('Ctrl Pts',(23.5200658336624,1.63325092321731,0.));
#214410=CARTESIAN_POINT('Ctrl Pts',(23.5386251432278,1.62894708745231,0.));
#214411=CARTESIAN_POINT('Ctrl Pts',(23.5572855427617,1.62456559140072,0.));
#214412=CARTESIAN_POINT('Ctrl Pts',(23.5760459637608,1.62010618772869,0.));
#214413=CARTESIAN_POINT('Ctrl Pts',(23.5949053517996,1.61556863424697,0.));
#214414=CARTESIAN_POINT('Ctrl Pts',(23.6138626661644,1.61095269379773,0.));
#214415=CARTESIAN_POINT('Ctrl Pts',(23.6329168794916,1.60625813414666,0.));
#214416=CARTESIAN_POINT('Ctrl Pts',(23.6520669774863,1.60148472786588,0.));
#214417=CARTESIAN_POINT('Ctrl Pts',(23.6713119586302,1.59663225222459,0.));
#214418=CARTESIAN_POINT('Ctrl Pts',(23.6906508338832,1.59170048908631,0.));
#214419=CARTESIAN_POINT('Ctrl Pts',(23.7100826263835,1.58668922481222,0.));
#214420=CARTESIAN_POINT('Ctrl Pts',(23.7296063711308,1.58159825017362,0.));
#214421=CARTESIAN_POINT('Ctrl Pts',(23.7492211147369,1.57642736025251,0.));
#214422=CARTESIAN_POINT('Ctrl Pts',(23.7689259151869,1.57117635434412,0.));
#214423=CARTESIAN_POINT('Ctrl Pts',(23.788719841588,1.56584503586844,0.));
#214424=CARTESIAN_POINT('Ctrl Pts',(23.8086019739192,1.56043321228631,0.));
#214425=CARTESIAN_POINT('Ctrl Pts',(23.8285714027631,1.55494069502628,0.));
#214426=CARTESIAN_POINT('Ctrl Pts',(23.8486272290698,1.5493672994053,0.));
#214427=CARTESIAN_POINT('Ctrl Pts',(23.8687685639635,1.54371284453978,0.));
#214428=CARTESIAN_POINT('Ctrl Pts',(23.8889945285313,1.53797715326748,0.));
#214429=CARTESIAN_POINT('Ctrl Pts',(23.9093042536119,1.53216005207462,0.));
#214430=CARTESIAN_POINT('Ctrl Pts',(23.9296968795761,1.5262613710304,0.));
#214431=CARTESIAN_POINT('Ctrl Pts',(23.9501715561038,1.52028094372806,0.));
#214432=CARTESIAN_POINT('Ctrl Pts',(23.9707274420145,1.51421860720628,0.));
#214433=CARTESIAN_POINT('Ctrl Pts',(23.991363705093,1.50807420187703,0.));
#214434=CARTESIAN_POINT('Ctrl Pts',(24.0120795219086,1.50184757146099,0.));
#214435=CARTESIAN_POINT('Ctrl Pts',(24.0328740776331,1.49553856292798,0.));
#214436=CARTESIAN_POINT('Ctrl Pts',(24.053746565843,1.48914702644883,0.));
#214437=CARTESIAN_POINT('Ctrl Pts',(24.074696188353,1.4826728153368,0.));
#214438=CARTESIAN_POINT('Ctrl Pts',(24.0957221550782,1.47611578597742,0.));
#214439=CARTESIAN_POINT('Ctrl Pts',(24.1168236838827,1.46947579776992,0.));
#214440=CARTESIAN_POINT('Ctrl Pts',(24.1380000004272,1.46275271307398,0.));
#214441=CARTESIAN_POINT('Ctrl Pts',(24.1592503380105,1.45594639716314,0.));
#214442=CARTESIAN_POINT('Ctrl Pts',(24.1805739374033,1.44905671818721,0.));
#214443=CARTESIAN_POINT('Ctrl Pts',(24.2019700467214,1.44208354711074,0.));
#214444=CARTESIAN_POINT('Ctrl Pts',(24.2234379212978,1.43502675765502,0.));
#214445=CARTESIAN_POINT('Ctrl Pts',(24.2449768235485,1.42788622624851,0.));
#214446=CARTESIAN_POINT('Ctrl Pts',(24.2665860228357,1.42066183198252,0.));
#214447=CARTESIAN_POINT('Ctrl Pts',(24.2882647953214,1.41335345657685,0.));
#214448=CARTESIAN_POINT('Ctrl Pts',(24.3100124238316,1.40596098434341,0.));
#214449=CARTESIAN_POINT('Ctrl Pts',(24.3318281977647,1.3984843021281,0.));
#214450=CARTESIAN_POINT('Ctrl Pts',(24.3537114129877,1.3909232992639,0.));
#214451=CARTESIAN_POINT('Ctrl Pts',(24.37566137173,1.38327786752998,0.));
#214452=CARTESIAN_POINT('Ctrl Pts',(24.3976773824731,1.37554790111608,0.));
#214453=CARTESIAN_POINT('Ctrl Pts',(24.4197587598337,1.36773329659954,0.));
#214454=CARTESIAN_POINT('Ctrl Pts',(24.4419048244524,1.35983395290624,0.));
#214455=CARTESIAN_POINT('Ctrl Pts',(24.4641149028894,1.35184977125645,0.));
#214456=CARTESIAN_POINT('Ctrl Pts',(24.4863883275135,1.34378065512335,0.));
#214457=CARTESIAN_POINT('Ctrl Pts',(24.5087244363856,1.33562651019684,0.));
#214458=CARTESIAN_POINT('Ctrl Pts',(24.5311225731434,1.32738724435326,0.));
#214459=CARTESIAN_POINT('Ctrl Pts',(24.5535820868671,1.31906276763669,0.));
#214460=CARTESIAN_POINT('Ctrl Pts',(24.576102332018,1.31065299222023,0.));
#214461=CARTESIAN_POINT('Ctrl Pts',(24.5986826684025,1.30215783236364,0.));
#214462=CARTESIAN_POINT('Ctrl Pts',(24.6213224611228,1.29357720438108,0.));
#214463=CARTESIAN_POINT('Ctrl Pts',(24.6440210805278,1.28491102661514,0.));
#214464=CARTESIAN_POINT('Ctrl Pts',(24.666777902156,1.2761592194164,0.));
#214465=CARTESIAN_POINT('Ctrl Pts',(24.6895923066837,1.26732170513497,0.));
#214466=CARTESIAN_POINT('Ctrl Pts',(24.7124636797895,1.25839840807415,0.));
#214467=CARTESIAN_POINT('Ctrl Pts',(24.7353914120012,1.24938925444324,0.));
#214468=CARTESIAN_POINT('Ctrl Pts',(24.7583748985439,1.24029417231988,0.));
#214469=CARTESIAN_POINT('Ctrl Pts',(24.78141353918,1.23111309161843,0.));
#214470=CARTESIAN_POINT('Ctrl Pts',(24.8045067380536,1.22184594406527,0.));
#214471=CARTESIAN_POINT('Ctrl Pts',(24.8276539035092,1.21249266318205,0.));
#214472=CARTESIAN_POINT('Ctrl Pts',(24.8508544481973,1.20305318426016,0.));
#214473=CARTESIAN_POINT('Ctrl Pts',(24.8741077892074,1.19352744434059,0.));
#214474=CARTESIAN_POINT('Ctrl Pts',(24.8974133481829,1.18391538220098,0.));
#214475=CARTESIAN_POINT('Ctrl Pts',(24.9207705514449,1.1742169383504,0.));
#214476=CARTESIAN_POINT('Ctrl Pts',(24.9441788300932,1.16443205502852,0.));
#214477=CARTESIAN_POINT('Ctrl Pts',(24.9676376201501,1.15456067621894,0.));
#214478=CARTESIAN_POINT('Ctrl Pts',(24.9911463621431,1.14460274758206,0.));
#214479=CARTESIAN_POINT('Ctrl Pts',(25.0147045006193,1.13455821638536,0.));
#214480=CARTESIAN_POINT('Ctrl Pts',(25.0383114836898,1.12442703144455,0.));
#214481=CARTESIAN_POINT('Ctrl Pts',(25.0619667625336,1.1142091430689,0.));
#214482=CARTESIAN_POINT('Ctrl Pts',(25.085669790968,1.10390450301741,0.));
#214483=CARTESIAN_POINT('Ctrl Pts',(25.1094200248448,1.09351306445299,0.));
#214484=CARTESIAN_POINT('Ctrl Pts',(25.1332169227415,1.08303478197174,0.));
#214485=CARTESIAN_POINT('Ctrl Pts',(25.1570599469311,1.0724696116546,0.));
#214486=CARTESIAN_POINT('Ctrl Pts',(25.1809485642191,1.06181751111754,0.));
#214487=CARTESIAN_POINT('Ctrl Pts',(25.2048822469027,1.05107843957926,0.));
#214488=CARTESIAN_POINT('Ctrl Pts',(25.2288604735087,1.04025235791515,0.));
#214489=CARTESIAN_POINT('Ctrl Pts',(25.2528827300427,1.0293392287683,0.));
#214490=CARTESIAN_POINT('Ctrl Pts',(25.2769485087268,1.01833901642273,0.));
#214491=CARTESIAN_POINT('Ctrl Pts',(25.3010573055557,1.00725168656934,0.));
#214492=CARTESIAN_POINT('Ctrl Pts',(25.3252086182976,0.996077206120921,
0.));
#214493=CARTESIAN_POINT('Ctrl Pts',(25.3494019441444,0.984815543004091,
0.));
#214494=CARTESIAN_POINT('Ctrl Pts',(25.3736367778842,0.97346666600005,0.));
#214495=CARTESIAN_POINT('Ctrl Pts',(25.3979126089155,0.962030544502806,
0.));
#214496=CARTESIAN_POINT('Ctrl Pts',(25.4222289223155,0.950507148596971,
0.));
#214497=CARTESIAN_POINT('Ctrl Pts',(25.4465852044835,0.938896449495636,
0.));
#214498=CARTESIAN_POINT('Ctrl Pts',(25.4709809474996,0.927198419885607,
0.));
#214499=CARTESIAN_POINT('Ctrl Pts',(25.4954156541787,0.915413034335334,
0.));
#214500=CARTESIAN_POINT('Ctrl Pts',(25.5198888424195,0.903540269651155,
0.));
#214501=CARTESIAN_POINT('Ctrl Pts',(25.5444000508223,0.891580105349469,
0.));
#214502=CARTESIAN_POINT('Ctrl Pts',(25.568948840818,0.879532523835094,0.));
#214503=CARTESIAN_POINT('Ctrl Pts',(25.5935347843616,0.867397509339473,
0.));
#214504=CARTESIAN_POINT('Ctrl Pts',(25.618157453608,0.855175047037618,0.));
#214505=CARTESIAN_POINT('Ctrl Pts',(25.6428164100078,0.842865122121547,
0.));
#214506=CARTESIAN_POINT('Ctrl Pts',(25.6675111931957,0.83046771886437,0.));
#214507=CARTESIAN_POINT('Ctrl Pts',(25.6922413110172,0.817982819786722,
0.));
#214508=CARTESIAN_POINT('Ctrl Pts',(25.7170062262474,0.805410404552597,
0.));
#214509=CARTESIAN_POINT('Ctrl Pts',(25.7418053757671,0.792750451613538,
0.));
#214510=CARTESIAN_POINT('Ctrl Pts',(25.7666381946871,0.780002940289028,
0.));
#214511=CARTESIAN_POINT('Ctrl Pts',(25.7915041383304,0.767167852648643,
0.));
#214512=CARTESIAN_POINT('Ctrl Pts',(25.816402705995,0.754245175608291,0.));
#214513=CARTESIAN_POINT('Ctrl Pts',(25.841333461908,0.741234902664698,0.));
#214514=CARTESIAN_POINT('Ctrl Pts',(25.8662960624285,0.728137036485881,
0.));
#214515=CARTESIAN_POINT('Ctrl Pts',(25.8912902615141,0.714951588533756,
0.));
#214516=CARTESIAN_POINT('Ctrl Pts',(25.9163158909645,0.701678575236605,
0.));
#214517=CARTESIAN_POINT('Ctrl Pts',(25.941372847213,0.68831801506568,0.));
#214518=CARTESIAN_POINT('Ctrl Pts',(25.9614434298092,0.677559543215907,
0.));
#214519=CARTESIAN_POINT('Ctrl Pts',(25.9765104298171,0.669451306784419,
0.));
#214520=CARTESIAN_POINT('Ctrl Pts',(25.9865613464809,0.664028313188916,
0.));
#214521=CARTESIAN_POINT('Ctrl Pts',(25.991588367311,0.661312440730894,0.));
#214522=CARTESIAN_POINT('Origin',(0.,0.,0.));
#214523=CARTESIAN_POINT('Origin',(0.,0.,0.));
#214524=CARTESIAN_POINT('',(25.2771067246846,6.08833931617698,0.));
#214525=CARTESIAN_POINT('Origin',(0.,0.,0.));
#214526=CARTESIAN_POINT('Origin',(0.,0.,0.));
#214527=CARTESIAN_POINT('Origin',(0.,0.,0.));
#214528=CARTESIAN_POINT('Origin',(0.,0.,0.));
#214529=CARTESIAN_POINT('Origin',(0.,0.,0.));
#214530=CARTESIAN_POINT('Origin',(0.,0.,0.));
#214531=CARTESIAN_POINT('Origin',(0.,0.,0.));
#214532=CARTESIAN_POINT('Origin',(0.,0.,0.));
#214533=CARTESIAN_POINT('Origin',(0.,0.,0.));
#214534=CARTESIAN_POINT('Origin',(0.,0.,0.));
#214535=CARTESIAN_POINT('Origin',(0.,0.,0.));
#214536=CARTESIAN_POINT('Origin',(0.,0.,0.));
#214537=CARTESIAN_POINT('Origin',(0.,0.,0.));
#214538=CARTESIAN_POINT('Origin',(0.,0.,0.));
#214539=CARTESIAN_POINT('Origin',(0.,0.,0.));
#214540=CARTESIAN_POINT('Origin',(0.,0.,0.));
#214541=CARTESIAN_POINT('Origin',(0.,0.,0.));
#214542=CARTESIAN_POINT('Origin',(0.,0.,0.));
#214543=CARTESIAN_POINT('Origin',(0.,0.,0.));
#214544=CARTESIAN_POINT('Origin',(0.,0.,0.));
#214545=CARTESIAN_POINT('Origin',(0.,0.,0.));
#214546=CARTESIAN_POINT('Origin',(0.,0.,0.));
#214547=CARTESIAN_POINT('Origin',(21.7161918885402,3.52235856495312,0.));
#214548=CARTESIAN_POINT('',(21.624941921198,4.01396149767428,0.));
#214549=CARTESIAN_POINT('',(21.2226420728916,3.44230496120418,0.));
#214550=CARTESIAN_POINT('Origin',(22.1738711152697,4.11585220600461,0.));
#214551=CARTESIAN_POINT('',(22.1738711152697,4.11585220600461,0.));
#214552=CARTESIAN_POINT('Origin',(21.8878840740801,2.21822694051638,0.));
#214553=CARTESIAN_POINT('',(21.3904321633055,2.16781269186828,0.));
#214554=CARTESIAN_POINT('',(21.9269795755927,1.71975774210841,0.));
#214555=CARTESIAN_POINT('Origin',(7.7715611723761E-13,7.16093850883226E-14,
0.));
#214556=CARTESIAN_POINT('Origin',(21.4341755315424,1.68110656504246,0.));
#214557=CARTESIAN_POINT('',(22.4835757167854,1.76341220531179,0.));
#214558=CARTESIAN_POINT('Ctrl Pts',(25.2771067246846,6.08833931617698,0.));
#214559=CARTESIAN_POINT('Ctrl Pts',(25.2771067246846,6.08833931617698,12.));
#214560=CARTESIAN_POINT('Ctrl Pts',(25.2729539149479,6.08441489609824,0.));
#214561=CARTESIAN_POINT('Ctrl Pts',(25.2729539149479,6.08441489609824,12.));
#214562=CARTESIAN_POINT('Ctrl Pts',(25.2646490489816,6.07657531787578,0.));
#214563=CARTESIAN_POINT('Ctrl Pts',(25.2646490489816,6.07657531787578,12.));
#214564=CARTESIAN_POINT('Ctrl Pts',(25.2521940105523,6.06484373634697,0.));
#214565=CARTESIAN_POINT('Ctrl Pts',(25.2521940105523,6.06484373634697,12.));
#214566=CARTESIAN_POINT('Ctrl Pts',(25.2355918138798,6.04925720151412,0.));
#214567=CARTESIAN_POINT('Ctrl Pts',(25.2355918138798,6.04925720151412,12.));
#214568=CARTESIAN_POINT('Ctrl Pts',(25.2148466201368,6.02986667390187,0.));
#214569=CARTESIAN_POINT('Ctrl Pts',(25.2148466201368,6.02986667390187,12.));
#214570=CARTESIAN_POINT('Ctrl Pts',(25.1941090269638,6.0105688180476,0.));
#214571=CARTESIAN_POINT('Ctrl Pts',(25.1941090269638,6.0105688180476,12.));
#214572=CARTESIAN_POINT('Ctrl Pts',(25.1733791296154,5.99136367859839,0.));
#214573=CARTESIAN_POINT('Ctrl Pts',(25.1733791296154,5.99136367859839,12.));
#214574=CARTESIAN_POINT('Ctrl Pts',(25.1526570863065,5.97225131495636,0.));
#214575=CARTESIAN_POINT('Ctrl Pts',(25.1526570863065,5.97225131495636,12.));
#214576=CARTESIAN_POINT('Ctrl Pts',(25.1319431317273,5.95323180187348,0.));
#214577=CARTESIAN_POINT('Ctrl Pts',(25.1319431317273,5.95323180187348,12.));
#214578=CARTESIAN_POINT('Ctrl Pts',(25.1112375971182,5.93430523086776,0.));
#214579=CARTESIAN_POINT('Ctrl Pts',(25.1112375971182,5.93430523086776,12.));
#214580=CARTESIAN_POINT('Ctrl Pts',(25.0905409050863,5.91547170844382,0.));
#214581=CARTESIAN_POINT('Ctrl Pts',(25.0905409050863,5.91547170844382,12.));
#214582=CARTESIAN_POINT('Ctrl Pts',(25.0698535426593,5.89673135155459,0.));
#214583=CARTESIAN_POINT('Ctrl Pts',(25.0698535426593,5.89673135155459,12.));
#214584=CARTESIAN_POINT('Ctrl Pts',(25.0491760405965,5.87808428385329,0.));
#214585=CARTESIAN_POINT('Ctrl Pts',(25.0491760405965,5.87808428385329,12.));
#214586=CARTESIAN_POINT('Ctrl Pts',(25.0285089498922,5.8595306315681,0.));
#214587=CARTESIAN_POINT('Ctrl Pts',(25.0285089498922,5.8595306315681,12.));
#214588=CARTESIAN_POINT('Ctrl Pts',(25.0078528200558,5.84107051963074,0.));
#214589=CARTESIAN_POINT('Ctrl Pts',(25.0078528200558,5.84107051963074,12.));
#214590=CARTESIAN_POINT('Ctrl Pts',(24.9872081752709,5.82270406744214,0.));
#214591=CARTESIAN_POINT('Ctrl Pts',(24.9872081752709,5.82270406744214,12.));
#214592=CARTESIAN_POINT('Ctrl Pts',(24.9665754954462,5.80443138549747,0.));
#214593=CARTESIAN_POINT('Ctrl Pts',(24.9665754954462,5.80443138549747,12.));
#214594=CARTESIAN_POINT('Ctrl Pts',(24.9459552293308,5.78625257775703,0.));
#214595=CARTESIAN_POINT('Ctrl Pts',(24.9459552293308,5.78625257775703,12.));
#214596=CARTESIAN_POINT('Ctrl Pts',(24.9253478043632,5.76816774342236,0.));
#214597=CARTESIAN_POINT('Ctrl Pts',(24.9253478043632,5.76816774342236,12.));
#214598=CARTESIAN_POINT('Ctrl Pts',(24.9047536376467,5.75017697890813,0.));
#214599=CARTESIAN_POINT('Ctrl Pts',(24.9047536376467,5.75017697890813,12.));
#214600=CARTESIAN_POINT('Ctrl Pts',(24.8841731467219,5.73228037976927,0.));
#214601=CARTESIAN_POINT('Ctrl Pts',(24.8841731467219,5.73228037976927,12.));
#214602=CARTESIAN_POINT('Ctrl Pts',(24.8636067597677,5.71447804252019,0.));
#214603=CARTESIAN_POINT('Ctrl Pts',(24.8636067597677,5.71447804252019,12.));
#214604=CARTESIAN_POINT('Ctrl Pts',(24.8430549277634,5.6967700667943,0.));
#214605=CARTESIAN_POINT('Ctrl Pts',(24.8430549277634,5.6967700667943,12.));
#214606=CARTESIAN_POINT('Ctrl Pts',(24.822518122386,5.67915655496524,0.));
#214607=CARTESIAN_POINT('Ctrl Pts',(24.822518122386,5.67915655496524,12.));
#214608=CARTESIAN_POINT('Ctrl Pts',(24.8019968304618,5.66163761114903,0.));
#214609=CARTESIAN_POINT('Ctrl Pts',(24.8019968304618,5.66163761114903,12.));
#214610=CARTESIAN_POINT('Ctrl Pts',(24.7814915496728,5.64421334042248,0.));
#214611=CARTESIAN_POINT('Ctrl Pts',(24.7814915496728,5.64421334042248,12.));
#214612=CARTESIAN_POINT('Ctrl Pts',(24.76100278357,5.62688384790919,0.));
#214613=CARTESIAN_POINT('Ctrl Pts',(24.76100278357,5.62688384790919,12.));
#214614=CARTESIAN_POINT('Ctrl Pts',(24.7405310372736,5.60964923798495,0.));
#214615=CARTESIAN_POINT('Ctrl Pts',(24.7405310372736,5.60964923798495,12.));
#214616=CARTESIAN_POINT('Ctrl Pts',(24.7200768119079,5.59250961323995,0.));
#214617=CARTESIAN_POINT('Ctrl Pts',(24.7200768119079,5.59250961323995,12.));
#214618=CARTESIAN_POINT('Ctrl Pts',(24.6996406035507,5.57546507427767,0.));
#214619=CARTESIAN_POINT('Ctrl Pts',(24.6996406035507,5.57546507427767,12.));
#214620=CARTESIAN_POINT('Ctrl Pts',(24.6792229061785,5.55851572025389,0.));
#214621=CARTESIAN_POINT('Ctrl Pts',(24.6792229061785,5.55851572025389,12.));
#214622=CARTESIAN_POINT('Ctrl Pts',(24.6588242134733,5.54166164919593,0.));
#214623=CARTESIAN_POINT('Ctrl Pts',(24.6588242134733,5.54166164919593,12.));
#214624=CARTESIAN_POINT('Ctrl Pts',(24.6384450211466,5.52490295840996,0.));
#214625=CARTESIAN_POINT('Ctrl Pts',(24.6384450211466,5.52490295840996,12.));
#214626=CARTESIAN_POINT('Ctrl Pts',(24.618085828918,5.50823974481959,0.));
#214627=CARTESIAN_POINT('Ctrl Pts',(24.618085828918,5.50823974481959,12.));
#214628=CARTESIAN_POINT('Ctrl Pts',(24.5977471429365,5.49167210537235,0.));
#214629=CARTESIAN_POINT('Ctrl Pts',(24.5977471429365,5.49167210537235,12.));
#214630=CARTESIAN_POINT('Ctrl Pts',(24.5774294770329,5.47520013724403,0.));
#214631=CARTESIAN_POINT('Ctrl Pts',(24.5774294770329,5.47520013724403,12.));
#214632=CARTESIAN_POINT('Ctrl Pts',(24.5571333514841,5.45882393762244,0.));
#214633=CARTESIAN_POINT('Ctrl Pts',(24.5571333514841,5.45882393762244,12.));
#214634=CARTESIAN_POINT('Ctrl Pts',(24.5368592922861,5.44254360356866,0.));
#214635=CARTESIAN_POINT('Ctrl Pts',(24.5368592922861,5.44254360356866,12.));
#214636=CARTESIAN_POINT('Ctrl Pts',(24.5166078302107,5.42635923183411,0.));
#214637=CARTESIAN_POINT('Ctrl Pts',(24.5166078302107,5.42635923183411,12.));
#214638=CARTESIAN_POINT('Ctrl Pts',(24.4963794999831,5.41027091869242,0.));
#214639=CARTESIAN_POINT('Ctrl Pts',(24.4963794999831,5.41027091869242,12.));
#214640=CARTESIAN_POINT('Ctrl Pts',(24.4761748393322,5.39427875973831,0.));
#214641=CARTESIAN_POINT('Ctrl Pts',(24.4761748393322,5.39427875973831,12.));
#214642=CARTESIAN_POINT('Ctrl Pts',(24.4559943883159,5.37838284973706,0.));
#214643=CARTESIAN_POINT('Ctrl Pts',(24.4559943883159,5.37838284973706,12.));
#214644=CARTESIAN_POINT('Ctrl Pts',(24.4358386899152,5.36258328273639,0.));
#214645=CARTESIAN_POINT('Ctrl Pts',(24.4358386899152,5.36258328273639,12.));
#214646=CARTESIAN_POINT('Ctrl Pts',(24.4157082904615,5.34688015213546,0.));
#214647=CARTESIAN_POINT('Ctrl Pts',(24.4157082904615,5.34688015213546,12.));
#214648=CARTESIAN_POINT('Ctrl Pts',(24.3956037401293,5.33127355076037,0.));
#214649=CARTESIAN_POINT('Ctrl Pts',(24.3956037401293,5.33127355076037,12.));
#214650=CARTESIAN_POINT('Ctrl Pts',(24.3755255933917,5.31576357092525,0.));
#214651=CARTESIAN_POINT('Ctrl Pts',(24.3755255933917,5.31576357092525,12.));
#214652=CARTESIAN_POINT('Ctrl Pts',(24.3554744095075,5.30035030449059,0.));
#214653=CARTESIAN_POINT('Ctrl Pts',(24.3554744095075,5.30035030449059,12.));
#214654=CARTESIAN_POINT('Ctrl Pts',(24.3354507529415,5.28503384290644,0.));
#214655=CARTESIAN_POINT('Ctrl Pts',(24.3354507529415,5.28503384290644,12.));
#214656=CARTESIAN_POINT('Ctrl Pts',(24.3154551932222,5.26981427718796,0.));
#214657=CARTESIAN_POINT('Ctrl Pts',(24.3154551932222,5.26981427718796,12.));
#214658=CARTESIAN_POINT('Ctrl Pts',(24.2954883048448,5.25469169788856,0.));
#214659=CARTESIAN_POINT('Ctrl Pts',(24.2954883048448,5.25469169788856,12.));
#214660=CARTESIAN_POINT('Ctrl Pts',(24.2755506671526,5.23966619506289,0.));
#214661=CARTESIAN_POINT('Ctrl Pts',(24.2755506671526,5.23966619506289,12.));
#214662=CARTESIAN_POINT('Ctrl Pts',(24.2556428642294,5.22473785822441,0.));
#214663=CARTESIAN_POINT('Ctrl Pts',(24.2556428642294,5.22473785822441,12.));
#214664=CARTESIAN_POINT('Ctrl Pts',(24.2357654847765,5.20990677629173,0.));
#214665=CARTESIAN_POINT('Ctrl Pts',(24.2357654847765,5.20990677629173,12.));
#214666=CARTESIAN_POINT('Ctrl Pts',(24.215919122017,5.19517303753643,0.));
#214667=CARTESIAN_POINT('Ctrl Pts',(24.215919122017,5.19517303753643,12.));
#214668=CARTESIAN_POINT('Ctrl Pts',(24.1961043738754,5.18053672961392,0.));
#214669=CARTESIAN_POINT('Ctrl Pts',(24.1961043738754,5.18053672961392,12.));
#214670=CARTESIAN_POINT('Ctrl Pts',(24.1763218431343,5.16599793957979,0.));
#214671=CARTESIAN_POINT('Ctrl Pts',(24.1763218431343,5.16599793957979,12.));
#214672=CARTESIAN_POINT('Ctrl Pts',(24.156572137597,5.15155675390075,0.));
#214673=CARTESIAN_POINT('Ctrl Pts',(24.156572137597,5.15155675390075,12.));
#214674=CARTESIAN_POINT('Ctrl Pts',(24.1368558702443,5.13721325845745,0.));
#214675=CARTESIAN_POINT('Ctrl Pts',(24.1368558702443,5.13721325845745,12.));
#214676=CARTESIAN_POINT('Ctrl Pts',(24.117173659394,5.1229675385386,0.));
#214677=CARTESIAN_POINT('Ctrl Pts',(24.117173659394,5.1229675385386,12.));
#214678=CARTESIAN_POINT('Ctrl Pts',(24.0975261288446,5.10881967883132,0.));
#214679=CARTESIAN_POINT('Ctrl Pts',(24.0975261288446,5.10881967883132,12.));
#214680=CARTESIAN_POINT('Ctrl Pts',(24.0779139079266,5.09476976342625,0.));
#214681=CARTESIAN_POINT('Ctrl Pts',(24.0779139079266,5.09476976342625,12.));
#214682=CARTESIAN_POINT('Ctrl Pts',(24.0583376315638,5.08081787581277,0.));
#214683=CARTESIAN_POINT('Ctrl Pts',(24.0583376315638,5.08081787581277,12.));
#214684=CARTESIAN_POINT('Ctrl Pts',(24.0387979403268,5.06696409886641,0.));
#214685=CARTESIAN_POINT('Ctrl Pts',(24.0387979403268,5.06696409886641,12.));
#214686=CARTESIAN_POINT('Ctrl Pts',(24.0192954804896,5.05320851483065,0.));
#214687=CARTESIAN_POINT('Ctrl Pts',(24.0192954804896,5.05320851483065,12.));
#214688=CARTESIAN_POINT('Ctrl Pts',(23.9998309040746,5.03955120528521,0.));
#214689=CARTESIAN_POINT('Ctrl Pts',(23.9998309040746,5.03955120528521,12.));
#214690=CARTESIAN_POINT('Ctrl Pts',(23.9804048689227,5.02599225112454,0.));
#214691=CARTESIAN_POINT('Ctrl Pts',(23.9804048689227,5.02599225112454,12.));
#214692=CARTESIAN_POINT('Ctrl Pts',(23.961018038827,5.01253173257453,0.));
#214693=CARTESIAN_POINT('Ctrl Pts',(23.961018038827,5.01253173257453,12.));
#214694=CARTESIAN_POINT('Ctrl Pts',(23.9416710836529,4.99916972919307,0.));
#214695=CARTESIAN_POINT('Ctrl Pts',(23.9416710836529,4.99916972919307,12.));
#214696=CARTESIAN_POINT('Ctrl Pts',(23.9223646794592,4.98590631986533,0.));
#214697=CARTESIAN_POINT('Ctrl Pts',(23.9223646794592,4.98590631986533,12.));
#214698=CARTESIAN_POINT('Ctrl Pts',(23.9030995086163,4.97274158279227,0.));
#214699=CARTESIAN_POINT('Ctrl Pts',(23.9030995086163,4.97274158279227,12.));
#214700=CARTESIAN_POINT('Ctrl Pts',(23.8838762599218,4.95967559546561,0.));
#214701=CARTESIAN_POINT('Ctrl Pts',(23.8838762599218,4.95967559546561,12.));
#214702=CARTESIAN_POINT('Ctrl Pts',(23.8646956287168,4.9467084346586,0.));
#214703=CARTESIAN_POINT('Ctrl Pts',(23.8646956287168,4.9467084346586,12.));
#214704=CARTESIAN_POINT('Ctrl Pts',(23.8455583170057,4.93384017643432,0.));
#214705=CARTESIAN_POINT('Ctrl Pts',(23.8455583170057,4.93384017643432,12.));
#214706=CARTESIAN_POINT('Ctrl Pts',(23.8264650335717,4.92107089613969,0.));
#214707=CARTESIAN_POINT('Ctrl Pts',(23.8264650335717,4.92107089613969,12.));
#214708=CARTESIAN_POINT('Ctrl Pts',(23.8074164940896,4.90840066839344,0.));
#214709=CARTESIAN_POINT('Ctrl Pts',(23.8074164940896,4.90840066839344,12.));
#214710=CARTESIAN_POINT('Ctrl Pts',(23.7884134212384,4.89582956706775,0.));
#214711=CARTESIAN_POINT('Ctrl Pts',(23.7884134212384,4.89582956706775,12.));
#214712=CARTESIAN_POINT('Ctrl Pts',(23.7694565448049,4.88335766525573,0.));
#214713=CARTESIAN_POINT('Ctrl Pts',(23.7694565448049,4.88335766525573,12.));
#214714=CARTESIAN_POINT('Ctrl Pts',(23.7505466018245,4.87098503527152,0.));
#214715=CARTESIAN_POINT('Ctrl Pts',(23.7505466018245,4.87098503527152,12.));
#214716=CARTESIAN_POINT('Ctrl Pts',(23.7316843367313,4.85871174865499,0.));
#214717=CARTESIAN_POINT('Ctrl Pts',(23.7316843367313,4.85871174865499,12.));
#214718=CARTESIAN_POINT('Ctrl Pts',(23.7128705015017,4.84653787616426,0.));
#214719=CARTESIAN_POINT('Ctrl Pts',(23.7128705015017,4.84653787616426,12.));
#214720=CARTESIAN_POINT('Ctrl Pts',(23.6941058557971,4.83446348776266,0.));
#214721=CARTESIAN_POINT('Ctrl Pts',(23.6941058557971,4.83446348776266,12.));
#214722=CARTESIAN_POINT('Ctrl Pts',(23.675391167102,4.82248865259562,0.));
#214723=CARTESIAN_POINT('Ctrl Pts',(23.675391167102,4.82248865259562,12.));
#214724=CARTESIAN_POINT('Ctrl Pts',(23.6567272108628,4.81061343896432,0.));
#214725=CARTESIAN_POINT('Ctrl Pts',(23.6567272108628,4.81061343896432,12.));
#214726=CARTESIAN_POINT('Ctrl Pts',(23.6381147706579,4.7988379143322,0.));
#214727=CARTESIAN_POINT('Ctrl Pts',(23.6381147706579,4.7988379143322,12.));
#214728=CARTESIAN_POINT('Ctrl Pts',(23.6195546383624,4.78716214532098,0.));
#214729=CARTESIAN_POINT('Ctrl Pts',(23.6195546383624,4.78716214532098,12.));
#214730=CARTESIAN_POINT('Ctrl Pts',(23.6010476143099,4.77558619769872,0.));
#214731=CARTESIAN_POINT('Ctrl Pts',(23.6010476143099,4.77558619769872,12.));
#214732=CARTESIAN_POINT('Ctrl Pts',(23.5825945074535,4.76411013636251,0.));
#214733=CARTESIAN_POINT('Ctrl Pts',(23.5825945074535,4.76411013636251,12.));
#214734=CARTESIAN_POINT('Ctrl Pts',(23.5641961355168,4.75273402530617,0.));
#214735=CARTESIAN_POINT('Ctrl Pts',(23.5641961355168,4.75273402530617,12.));
#214736=CARTESIAN_POINT('Ctrl Pts',(23.545853325171,4.74145792760699,0.));
#214737=CARTESIAN_POINT('Ctrl Pts',(23.545853325171,4.74145792760699,12.));
#214738=CARTESIAN_POINT('Ctrl Pts',(23.5275669122372,4.7302819054303,0.));
#214739=CARTESIAN_POINT('Ctrl Pts',(23.5275669122372,4.7302819054303,12.));
#214740=CARTESIAN_POINT('Ctrl Pts',(23.509337741878,4.71920602001902,0.));
#214741=CARTESIAN_POINT('Ctrl Pts',(23.509337741878,4.71920602001902,12.));
#214742=CARTESIAN_POINT('Ctrl Pts',(23.491166668789,4.70823033167819,0.));
#214743=CARTESIAN_POINT('Ctrl Pts',(23.491166668789,4.70823033167819,12.));
#214744=CARTESIAN_POINT('Ctrl Pts',(23.4730545573853,4.69735489975024,0.));
#214745=CARTESIAN_POINT('Ctrl Pts',(23.4730545573853,4.69735489975024,12.));
#214746=CARTESIAN_POINT('Ctrl Pts',(23.455002281986,4.68657978258303,0.));
#214747=CARTESIAN_POINT('Ctrl Pts',(23.455002281986,4.68657978258303,12.));
#214748=CARTESIAN_POINT('Ctrl Pts',(23.4370107270451,4.67590503753059,0.));
#214749=CARTESIAN_POINT('Ctrl Pts',(23.4370107270451,4.67590503753059,12.));
#214750=CARTESIAN_POINT('Ctrl Pts',(23.4190807873803,4.6653307209467,0.));
#214751=CARTESIAN_POINT('Ctrl Pts',(23.4190807873803,4.6653307209467,12.));
#214752=CARTESIAN_POINT('Ctrl Pts',(23.4012133683959,4.65485688816924,0.));
#214753=CARTESIAN_POINT('Ctrl Pts',(23.4012133683959,4.65485688816924,12.));
#214754=CARTESIAN_POINT('Ctrl Pts',(23.3834093863068,4.6444835934993,0.));
#214755=CARTESIAN_POINT('Ctrl Pts',(23.3834093863068,4.6444835934993,12.));
#214756=CARTESIAN_POINT('Ctrl Pts',(23.3656697683489,4.63421089016541,0.));
#214757=CARTESIAN_POINT('Ctrl Pts',(23.3656697683489,4.63421089016541,12.));
#214758=CARTESIAN_POINT('Ctrl Pts',(23.3479954530272,4.62403883030805,0.));
#214759=CARTESIAN_POINT('Ctrl Pts',(23.3479954530272,4.62403883030805,12.));
#214760=CARTESIAN_POINT('Ctrl Pts',(23.3303873903938,4.6139674649783,0.));
#214761=CARTESIAN_POINT('Ctrl Pts',(23.3303873903938,4.6139674649783,12.));
#214762=CARTESIAN_POINT('Ctrl Pts',(23.3128465423115,4.60399684412163,0.));
#214763=CARTESIAN_POINT('Ctrl Pts',(23.3128465423115,4.60399684412163,12.));
#214764=CARTESIAN_POINT('Ctrl Pts',(23.2953738827191,4.5941270165575,0.));
#214765=CARTESIAN_POINT('Ctrl Pts',(23.2953738827191,4.5941270165575,12.));
#214766=CARTESIAN_POINT('Ctrl Pts',(23.2779703978876,4.5843580299469,0.));
#214767=CARTESIAN_POINT('Ctrl Pts',(23.2779703978876,4.5843580299469,12.));
#214768=CARTESIAN_POINT('Ctrl Pts',(23.2606370866866,4.57468993076097,0.));
#214769=CARTESIAN_POINT('Ctrl Pts',(23.2606370866866,4.57468993076097,12.));
#214770=CARTESIAN_POINT('Ctrl Pts',(23.2433749609131,4.56512276427839,0.));
#214771=CARTESIAN_POINT('Ctrl Pts',(23.2433749609131,4.56512276427839,12.));
#214772=CARTESIAN_POINT('Ctrl Pts',(23.2261850456064,4.55565657456975,0.));
#214773=CARTESIAN_POINT('Ctrl Pts',(23.2261850456064,4.55565657456975,12.));
#214774=CARTESIAN_POINT('Ctrl Pts',(23.2090683793629,4.54629140447544,0.));
#214775=CARTESIAN_POINT('Ctrl Pts',(23.2090683793629,4.54629140447544,12.));
#214776=CARTESIAN_POINT('Ctrl Pts',(23.1920260146465,4.53702729557566,0.));
#214777=CARTESIAN_POINT('Ctrl Pts',(23.1920260146465,4.53702729557566,12.));
#214778=CARTESIAN_POINT('Ctrl Pts',(23.1750590180908,4.52786428815015,0.));
#214779=CARTESIAN_POINT('Ctrl Pts',(23.1750590180908,4.52786428815015,12.));
#214780=CARTESIAN_POINT('Ctrl Pts',(23.1581684708761,4.51880242116748,0.));
#214781=CARTESIAN_POINT('Ctrl Pts',(23.1581684708761,4.51880242116748,12.));
#214782=CARTESIAN_POINT('Ctrl Pts',(23.1413554691123,4.5098417322706,0.));
#214783=CARTESIAN_POINT('Ctrl Pts',(23.1413554691123,4.5098417322706,12.));
#214784=CARTESIAN_POINT('Ctrl Pts',(23.1246211242115,4.50098225775171,0.));
#214785=CARTESIAN_POINT('Ctrl Pts',(23.1246211242115,4.50098225775171,12.));
#214786=CARTESIAN_POINT('Ctrl Pts',(23.1079665632636,4.49222403252216,0.));
#214787=CARTESIAN_POINT('Ctrl Pts',(23.1079665632636,4.49222403252216,12.));
#214788=CARTESIAN_POINT('Ctrl Pts',(23.0913929293922,4.48356709006788,0.));
#214789=CARTESIAN_POINT('Ctrl Pts',(23.0913929293922,4.48356709006788,12.));
#214790=CARTESIAN_POINT('Ctrl Pts',(23.0749013821881,4.47501146242856,0.));
#214791=CARTESIAN_POINT('Ctrl Pts',(23.0749013821881,4.47501146242856,12.));
#214792=CARTESIAN_POINT('Ctrl Pts',(23.0584930981732,4.46655718018231,0.));
#214793=CARTESIAN_POINT('Ctrl Pts',(23.0584930981732,4.46655718018231,12.));
#214794=CARTESIAN_POINT('Ctrl Pts',(23.0421692712467,4.45820427241683,0.));
#214795=CARTESIAN_POINT('Ctrl Pts',(23.0421692712467,4.45820427241683,12.));
#214796=CARTESIAN_POINT('Ctrl Pts',(23.0259311131392,4.44995276669687,0.));
#214797=CARTESIAN_POINT('Ctrl Pts',(23.0259311131392,4.44995276669687,12.));
#214798=CARTESIAN_POINT('Ctrl Pts',(23.0097798538395,4.44180268901643,0.));
#214799=CARTESIAN_POINT('Ctrl Pts',(23.0097798538395,4.44180268901643,12.));
#214800=CARTESIAN_POINT('Ctrl Pts',(22.9937167421006,4.43375406376879,0.));
#214801=CARTESIAN_POINT('Ctrl Pts',(22.9937167421006,4.43375406376879,12.));
#214802=CARTESIAN_POINT('Ctrl Pts',(22.977743046002,4.42580691372752,0.));
#214803=CARTESIAN_POINT('Ctrl Pts',(22.977743046002,4.42580691372752,12.));
#214804=CARTESIAN_POINT('Ctrl Pts',(22.9618600534866,4.41796126001302,0.));
#214805=CARTESIAN_POINT('Ctrl Pts',(22.9618600534866,4.41796126001302,12.));
#214806=CARTESIAN_POINT('Ctrl Pts',(22.9460690729093,4.41021712205554,0.));
#214807=CARTESIAN_POINT('Ctrl Pts',(22.9460690729093,4.41021712205554,12.));
#214808=CARTESIAN_POINT('Ctrl Pts',(22.930371433555,4.40257451754324,0.));
#214809=CARTESIAN_POINT('Ctrl Pts',(22.930371433555,4.40257451754324,12.));
#214810=CARTESIAN_POINT('Ctrl Pts',(22.9147684862426,4.39503346238473,0.));
#214811=CARTESIAN_POINT('Ctrl Pts',(22.9147684862426,4.39503346238473,12.));
#214812=CARTESIAN_POINT('Ctrl Pts',(22.8992616040108,4.38759397068406,0.));
#214813=CARTESIAN_POINT('Ctrl Pts',(22.8992616040108,4.38759397068406,12.));
#214814=CARTESIAN_POINT('Ctrl Pts',(22.8838521827701,4.38025605470093,0.));
#214815=CARTESIAN_POINT('Ctrl Pts',(22.8838521827701,4.38025605470093,12.));
#214816=CARTESIAN_POINT('Ctrl Pts',(22.8685416419725,4.37301972480746,0.));
#214817=CARTESIAN_POINT('Ctrl Pts',(22.8685416419725,4.37301972480746,12.));
#214818=CARTESIAN_POINT('Ctrl Pts',(22.8533314252422,4.36588498942997,0.));
#214819=CARTESIAN_POINT('Ctrl Pts',(22.8533314252422,4.36588498942997,12.));
#214820=CARTESIAN_POINT('Ctrl Pts',(22.8382230011184,4.35885185500546,0.));
#214821=CARTESIAN_POINT('Ctrl Pts',(22.8382230011184,4.35885185500546,12.));
#214822=CARTESIAN_POINT('Ctrl Pts',(22.8232178638876,4.35192032594791,0.));
#214823=CARTESIAN_POINT('Ctrl Pts',(22.8232178638876,4.35192032594791,12.));
#214824=CARTESIAN_POINT('Ctrl Pts',(22.8083175343791,4.34509040460062,0.));
#214825=CARTESIAN_POINT('Ctrl Pts',(22.8083175343791,4.34509040460062,12.));
#214826=CARTESIAN_POINT('Ctrl Pts',(22.7935235607806,4.33836209118446,0.));
#214827=CARTESIAN_POINT('Ctrl Pts',(22.7935235607806,4.33836209118446,12.));
#214828=CARTESIAN_POINT('Ctrl Pts',(22.7788375194076,4.3317353837319,0.));
#214829=CARTESIAN_POINT('Ctrl Pts',(22.7788375194076,4.3317353837319,12.));
#214830=CARTESIAN_POINT('Ctrl Pts',(22.7642610156475,4.32521027803754,0.));
#214831=CARTESIAN_POINT('Ctrl Pts',(22.7642610156475,4.32521027803754,12.));
#214832=CARTESIAN_POINT('Ctrl Pts',(22.7497956849848,4.31878676761235,0.));
#214833=CARTESIAN_POINT('Ctrl Pts',(22.7497956849848,4.31878676761235,12.));
#214834=CARTESIAN_POINT('Ctrl Pts',(22.7354431939926,4.31246484362549,0.));
#214835=CARTESIAN_POINT('Ctrl Pts',(22.7354431939926,4.31246484362549,12.));
#214836=CARTESIAN_POINT('Ctrl Pts',(22.7212052413386,4.30624449484069,0.));
#214837=CARTESIAN_POINT('Ctrl Pts',(22.7212052413386,4.30624449484069,12.));
#214838=CARTESIAN_POINT('Ctrl Pts',(22.7070835587564,4.3001257075406,0.));
#214839=CARTESIAN_POINT('Ctrl Pts',(22.7070835587564,4.3001257075406,12.));
#214840=CARTESIAN_POINT('Ctrl Pts',(22.6930799122548,4.29410846547056,0.));
#214841=CARTESIAN_POINT('Ctrl Pts',(22.6930799122548,4.29410846547056,12.));
#214842=CARTESIAN_POINT('Ctrl Pts',(22.6791961033537,4.28819274977763,0.));
#214843=CARTESIAN_POINT('Ctrl Pts',(22.6791961033537,4.28819274977763,12.));
#214844=CARTESIAN_POINT('Ctrl Pts',(22.6654339703109,4.28237853894059,0.));
#214845=CARTESIAN_POINT('Ctrl Pts',(22.6654339703109,4.28237853894059,12.));
#214846=CARTESIAN_POINT('Ctrl Pts',(22.6517953893303,4.2766658086912,0.));
#214847=CARTESIAN_POINT('Ctrl Pts',(22.6517953893303,4.2766658086912,12.));
#214848=CARTESIAN_POINT('Ctrl Pts',(22.6382822758172,4.27105453193004,0.));
#214849=CARTESIAN_POINT('Ctrl Pts',(22.6382822758172,4.27105453193004,12.));
#214850=CARTESIAN_POINT('Ctrl Pts',(22.6248965859977,4.26554467865576,0.));
#214851=CARTESIAN_POINT('Ctrl Pts',(22.6248965859977,4.26554467865576,12.));
#214852=CARTESIAN_POINT('Ctrl Pts',(22.6116403184821,4.26013621588305,0.));
#214853=CARTESIAN_POINT('Ctrl Pts',(22.6116403184821,4.26013621588305,12.));
#214854=CARTESIAN_POINT('Ctrl Pts',(22.5985155158636,4.25482910755481,0.));
#214855=CARTESIAN_POINT('Ctrl Pts',(22.5985155158636,4.25482910755481,12.));
#214856=CARTESIAN_POINT('Ctrl Pts',(22.5855242662477,4.24962331444177,0.));
#214857=CARTESIAN_POINT('Ctrl Pts',(22.5855242662477,4.24962331444177,12.));
#214858=CARTESIAN_POINT('Ctrl Pts',(22.572668704992,4.24451879404851,0.));
#214859=CARTESIAN_POINT('Ctrl Pts',(22.572668704992,4.24451879404851,12.));
#214860=CARTESIAN_POINT('Ctrl Pts',(22.5599510166429,4.23951550052523,0.));
#214861=CARTESIAN_POINT('Ctrl Pts',(22.5599510166429,4.23951550052523,12.));
#214862=CARTESIAN_POINT('Ctrl Pts',(22.5473734368086,4.23461338456712,0.));
#214863=CARTESIAN_POINT('Ctrl Pts',(22.5473734368086,4.23461338456712,12.));
#214864=CARTESIAN_POINT('Ctrl Pts',(22.5349382540588,4.22981239330733,0.));
#214865=CARTESIAN_POINT('Ctrl Pts',(22.5349382540588,4.22981239330733,12.));
#214866=CARTESIAN_POINT('Ctrl Pts',(22.5226478117886,4.22511247020041,0.));
#214867=CARTESIAN_POINT('Ctrl Pts',(22.5226478117886,4.22511247020041,12.));
#214868=CARTESIAN_POINT('Ctrl Pts',(22.5105045108881,4.22051355490196,0.));
#214869=CARTESIAN_POINT('Ctrl Pts',(22.5105045108881,4.22051355490196,12.));
#214870=CARTESIAN_POINT('Ctrl Pts',(22.4985108124228,4.21601558313906,0.));
#214871=CARTESIAN_POINT('Ctrl Pts',(22.4985108124228,4.21601558313906,12.));
#214872=CARTESIAN_POINT('Ctrl Pts',(22.4866692403147,4.21161848657428,0.));
#214873=CARTESIAN_POINT('Ctrl Pts',(22.4866692403147,4.21161848657428,12.));
#214874=CARTESIAN_POINT('Ctrl Pts',(22.4749823839917,4.20732219265649,0.));
#214875=CARTESIAN_POINT('Ctrl Pts',(22.4749823839917,4.20732219265649,12.));
#214876=CARTESIAN_POINT('Ctrl Pts',(22.4634529011437,4.20312662448174,0.));
#214877=CARTESIAN_POINT('Ctrl Pts',(22.4634529011437,4.20312662448174,12.));
#214878=CARTESIAN_POINT('Ctrl Pts',(22.4520835205422,4.19903170066358,0.));
#214879=CARTESIAN_POINT('Ctrl Pts',(22.4520835205422,4.19903170066358,12.));
#214880=CARTESIAN_POINT('Ctrl Pts',(22.4408770448917,4.1950373351886,0.));
#214881=CARTESIAN_POINT('Ctrl Pts',(22.4408770448917,4.1950373351886,12.));
#214882=CARTESIAN_POINT('Ctrl Pts',(22.4298363535416,4.19114343726932,0.));
#214883=CARTESIAN_POINT('Ctrl Pts',(22.4298363535416,4.19114343726932,12.));
#214884=CARTESIAN_POINT('Ctrl Pts',(22.4189644056109,4.18734991117707,0.));
#214885=CARTESIAN_POINT('Ctrl Pts',(22.4189644056109,4.18734991117707,12.));
#214886=CARTESIAN_POINT('Ctrl Pts',(22.4082642454448,4.18365665600839,0.));
#214887=CARTESIAN_POINT('Ctrl Pts',(22.4082642454448,4.18365665600839,12.));
#214888=CARTESIAN_POINT('Ctrl Pts',(22.3977390078074,4.18006356544879,0.));
#214889=CARTESIAN_POINT('Ctrl Pts',(22.3977390078074,4.18006356544879,12.));
#214890=CARTESIAN_POINT('Ctrl Pts',(22.3873919231339,4.17657052752834,0.));
#214891=CARTESIAN_POINT('Ctrl Pts',(22.3873919231339,4.17657052752834,12.));
#214892=CARTESIAN_POINT('Ctrl Pts',(22.3772263228624,4.17317742436162,0.));
#214893=CARTESIAN_POINT('Ctrl Pts',(22.3772263228624,4.17317742436162,12.));
#214894=CARTESIAN_POINT('Ctrl Pts',(22.3672456427605,4.1698841319947,0.));
#214895=CARTESIAN_POINT('Ctrl Pts',(22.3672456427605,4.1698841319947,12.));
#214896=CARTESIAN_POINT('Ctrl Pts',(22.3574534257397,4.16669052026602,0.));
#214897=CARTESIAN_POINT('Ctrl Pts',(22.3574534257397,4.16669052026602,12.));
#214898=CARTESIAN_POINT('Ctrl Pts',(22.3478533253886,4.1635964526318,0.));
#214899=CARTESIAN_POINT('Ctrl Pts',(22.3478533253886,4.1635964526318,12.));
#214900=CARTESIAN_POINT('Ctrl Pts',(22.3384491078599,4.16060178604154,0.));
#214901=CARTESIAN_POINT('Ctrl Pts',(22.3384491078599,4.16060178604154,12.));
#214902=CARTESIAN_POINT('Ctrl Pts',(22.3292446628957,4.15770637047882,0.));
#214903=CARTESIAN_POINT('Ctrl Pts',(22.3292446628957,4.15770637047882,12.));
#214904=CARTESIAN_POINT('Ctrl Pts',(22.3202440186979,4.15491004835278,0.));
#214905=CARTESIAN_POINT('Ctrl Pts',(22.3202440186979,4.15491004835278,12.));
#214906=CARTESIAN_POINT('Ctrl Pts',(22.3114513545186,4.15221265396993,0.));
#214907=CARTESIAN_POINT('Ctrl Pts',(22.3114513545186,4.15221265396993,12.));
#214908=CARTESIAN_POINT('Ctrl Pts',(22.3028710166935,4.14961401285526,0.));
#214909=CARTESIAN_POINT('Ctrl Pts',(22.3028710166935,4.14961401285526,12.));
#214910=CARTESIAN_POINT('Ctrl Pts',(22.2945075198468,4.14711394168559,0.));
#214911=CARTESIAN_POINT('Ctrl Pts',(22.2945075198468,4.14711394168559,12.));
#214912=CARTESIAN_POINT('Ctrl Pts',(22.2863655389167,4.14471224859295,0.));
#214913=CARTESIAN_POINT('Ctrl Pts',(22.2863655389167,4.14471224859295,12.));
#214914=CARTESIAN_POINT('Ctrl Pts',(22.2784499072026,4.14240873321982,0.));
#214915=CARTESIAN_POINT('Ctrl Pts',(22.2784499072026,4.14240873321982,12.));
#214916=CARTESIAN_POINT('Ctrl Pts',(22.2707656042456,4.14020318715988,0.));
#214917=CARTESIAN_POINT('Ctrl Pts',(22.2707656042456,4.14020318715988,12.));
#214918=CARTESIAN_POINT('Ctrl Pts',(22.263317791397,4.13809539255419,0.));
#214919=CARTESIAN_POINT('Ctrl Pts',(22.263317791397,4.13809539255419,12.));
#214920=CARTESIAN_POINT('Ctrl Pts',(22.2561118708422,4.13608511977226,0.));
#214921=CARTESIAN_POINT('Ctrl Pts',(22.2561118708422,4.13608511977226,12.));
#214922=CARTESIAN_POINT('Ctrl Pts',(22.2491535317789,4.13417212558809,0.));
#214923=CARTESIAN_POINT('Ctrl Pts',(22.2491535317789,4.13417212558809,12.));
#214924=CARTESIAN_POINT('Ctrl Pts',(22.2424488153523,4.1323561506016,0.));
#214925=CARTESIAN_POINT('Ctrl Pts',(22.2424488153523,4.1323561506016,12.));
#214926=CARTESIAN_POINT('Ctrl Pts',(22.2360040565534,4.13063692157499,0.));
#214927=CARTESIAN_POINT('Ctrl Pts',(22.2360040565534,4.13063692157499,12.));
#214928=CARTESIAN_POINT('Ctrl Pts',(22.2298258043947,4.12901415463379,0.));
#214929=CARTESIAN_POINT('Ctrl Pts',(22.2298258043947,4.12901415463379,12.));
#214930=CARTESIAN_POINT('Ctrl Pts',(22.2239207458781,4.127487558301,0.));
#214931=CARTESIAN_POINT('Ctrl Pts',(22.2239207458781,4.127487558301,12.));
#214932=CARTESIAN_POINT('Ctrl Pts',(22.2182956401341,4.126056836133,0.));
#214933=CARTESIAN_POINT('Ctrl Pts',(22.2182956401341,4.126056836133,12.));
#214934=CARTESIAN_POINT('Ctrl Pts',(22.2129576146671,4.12472167516602,0.));
#214935=CARTESIAN_POINT('Ctrl Pts',(22.2129576146671,4.12472167516602,12.));
#214936=CARTESIAN_POINT('Ctrl Pts',(22.2079143941719,4.12348173702025,0.));
#214937=CARTESIAN_POINT('Ctrl Pts',(22.2079143941719,4.12348173702025,12.));
#214938=CARTESIAN_POINT('Ctrl Pts',(22.2031746532106,4.12233664408237,0.));
#214939=CARTESIAN_POINT('Ctrl Pts',(22.2031746532106,4.12233664408237,12.));
#214940=CARTESIAN_POINT('Ctrl Pts',(22.1987479618246,4.12128598183533,0.));
#214941=CARTESIAN_POINT('Ctrl Pts',(22.1987479618246,4.12128598183533,12.));
#214942=CARTESIAN_POINT('Ctrl Pts',(22.1946440958098,4.12032932637738,0.));
#214943=CARTESIAN_POINT('Ctrl Pts',(22.1946440958098,4.12032932637738,12.));
#214944=CARTESIAN_POINT('Ctrl Pts',(22.1908725908525,4.11946626228623,0.));
#214945=CARTESIAN_POINT('Ctrl Pts',(22.1908725908525,4.11946626228623,12.));
#214946=CARTESIAN_POINT('Ctrl Pts',(22.1874419861496,4.11869641271752,0.));
#214947=CARTESIAN_POINT('Ctrl Pts',(22.1874419861496,4.11869641271752,12.));
#214948=CARTESIAN_POINT('Ctrl Pts',(22.1843613164855,4.11801938107464,0.));
#214949=CARTESIAN_POINT('Ctrl Pts',(22.1843613164855,4.11801938107464,12.));
#214950=CARTESIAN_POINT('Ctrl Pts',(22.1816414985788,4.11743469691765,0.));
#214951=CARTESIAN_POINT('Ctrl Pts',(22.1816414985788,4.11743469691765,12.));
#214952=CARTESIAN_POINT('Ctrl Pts',(22.179297473024,4.11694173195041,0.));
#214953=CARTESIAN_POINT('Ctrl Pts',(22.179297473024,4.11694173195041,12.));
#214954=CARTESIAN_POINT('Ctrl Pts',(22.177347426894,4.11653973150558,0.));
#214955=CARTESIAN_POINT('Ctrl Pts',(22.177347426894,4.11653973150558,12.));
#214956=CARTESIAN_POINT('Ctrl Pts',(22.1758088296598,4.11622797217066,0.));
#214957=CARTESIAN_POINT('Ctrl Pts',(22.1758088296598,4.11622797217066,12.));
#214958=CARTESIAN_POINT('Ctrl Pts',(22.1746949858773,4.11600589882768,0.));
#214959=CARTESIAN_POINT('Ctrl Pts',(22.1746949858773,4.11600589882768,12.));
#214960=CARTESIAN_POINT('Ctrl Pts',(22.174148802123,4.11589976826061,0.));
#214961=CARTESIAN_POINT('Ctrl Pts',(22.174148802123,4.11589976826061,12.));
#214962=CARTESIAN_POINT('Ctrl Pts',(22.1739341411684,4.1158603587821,0.));
#214963=CARTESIAN_POINT('Ctrl Pts',(22.1739341411684,4.1158603587821,12.));
#214964=CARTESIAN_POINT('Ctrl Pts',(22.1738776823239,4.11585194677412,0.));
#214965=CARTESIAN_POINT('Ctrl Pts',(22.1738776823239,4.11585194677412,12.));
#214966=CARTESIAN_POINT('Ctrl Pts',(22.1738711152697,4.11585220600461,0.));
#214967=CARTESIAN_POINT('Ctrl Pts',(22.1738711152697,4.11585220600461,12.));
#214968=CARTESIAN_POINT('Ctrl Pts',(22.4835757167854,1.76341220531179,0.));
#214969=CARTESIAN_POINT('Ctrl Pts',(22.4835757167854,1.76341220531179,12.));
#214970=CARTESIAN_POINT('Ctrl Pts',(22.483581992979,1.76341415538764,0.));
#214971=CARTESIAN_POINT('Ctrl Pts',(22.483581992979,1.76341415538764,12.));
#214972=CARTESIAN_POINT('Ctrl Pts',(22.4836387052232,1.7634206426357,0.));
#214973=CARTESIAN_POINT('Ctrl Pts',(22.4836387052232,1.7634206426357,12.));
#214974=CARTESIAN_POINT('Ctrl Pts',(22.4838562517069,1.76343813434565,0.));
#214975=CARTESIAN_POINT('Ctrl Pts',(22.4838562517069,1.76343813434565,12.));
#214976=CARTESIAN_POINT('Ctrl Pts',(22.4844112933129,1.76347698284792,0.));
#214977=CARTESIAN_POINT('Ctrl Pts',(22.4844112933129,1.76347698284792,12.));
#214978=CARTESIAN_POINT('Ctrl Pts',(22.4855446605991,1.76355076045546,0.));
#214979=CARTESIAN_POINT('Ctrl Pts',(22.4855446605991,1.76355076045546,12.));
#214980=CARTESIAN_POINT('Ctrl Pts',(22.4871115206571,1.76364784232963,0.));
#214981=CARTESIAN_POINT('Ctrl Pts',(22.4871115206571,1.76364784232963,12.));
#214982=CARTESIAN_POINT('Ctrl Pts',(22.4890991659478,1.76376424879505,0.));
#214983=CARTESIAN_POINT('Ctrl Pts',(22.4890991659478,1.76376424879505,12.));
#214984=CARTESIAN_POINT('Ctrl Pts',(22.4914909094908,1.76389475965724,0.));
#214985=CARTESIAN_POINT('Ctrl Pts',(22.4914909094908,1.76389475965724,12.));
#214986=CARTESIAN_POINT('Ctrl Pts',(22.4942693792449,1.76403393880301,0.));
#214987=CARTESIAN_POINT('Ctrl Pts',(22.4942693792449,1.76403393880301,12.));
#214988=CARTESIAN_POINT('Ctrl Pts',(22.4974203063191,1.76417731243462,0.));
#214989=CARTESIAN_POINT('Ctrl Pts',(22.4974203063191,1.76417731243462,12.));
#214990=CARTESIAN_POINT('Ctrl Pts',(22.5009332677316,1.76432160068726,0.));
#214991=CARTESIAN_POINT('Ctrl Pts',(22.5009332677316,1.76432160068726,12.));
#214992=CARTESIAN_POINT('Ctrl Pts',(22.5047996391978,1.76446408210366,0.));
#214993=CARTESIAN_POINT('Ctrl Pts',(22.5047996391978,1.76446408210366,12.));
#214994=CARTESIAN_POINT('Ctrl Pts',(22.5090112700212,1.76460218257323,0.));
#214995=CARTESIAN_POINT('Ctrl Pts',(22.5090112700212,1.76460218257323,12.));
#214996=CARTESIAN_POINT('Ctrl Pts',(22.5135590569554,1.76473303281159,0.));
#214997=CARTESIAN_POINT('Ctrl Pts',(22.5135590569554,1.76473303281159,12.));
#214998=CARTESIAN_POINT('Ctrl Pts',(22.5184336670207,1.76485369319896,0.));
#214999=CARTESIAN_POINT('Ctrl Pts',(22.5184336670207,1.76485369319896,12.));
#215000=CARTESIAN_POINT('Ctrl Pts',(22.5236259635515,1.76496128643369,0.));
#215001=CARTESIAN_POINT('Ctrl Pts',(22.5236259635515,1.76496128643369,12.));
#215002=CARTESIAN_POINT('Ctrl Pts',(22.529127665298,1.76505320262752,0.));
#215003=CARTESIAN_POINT('Ctrl Pts',(22.529127665298,1.76505320262752,12.));
#215004=CARTESIAN_POINT('Ctrl Pts',(22.5349313983571,1.7651271156325,0.));
#215005=CARTESIAN_POINT('Ctrl Pts',(22.5349313983571,1.7651271156325,12.));
#215006=CARTESIAN_POINT('Ctrl Pts',(22.5410303590891,1.76518087841493,0.));
#215007=CARTESIAN_POINT('Ctrl Pts',(22.5410303590891,1.76518087841493,12.));
#215008=CARTESIAN_POINT('Ctrl Pts',(22.5474180954006,1.76521245524047,0.));
#215009=CARTESIAN_POINT('Ctrl Pts',(22.5474180954006,1.76521245524047,12.));
#215010=CARTESIAN_POINT('Ctrl Pts',(22.5540882235837,1.76521983384063,0.));
#215011=CARTESIAN_POINT('Ctrl Pts',(22.5540882235837,1.76521983384063,12.));
#215012=CARTESIAN_POINT('Ctrl Pts',(22.5610344912501,1.7652010450045,0.));
#215013=CARTESIAN_POINT('Ctrl Pts',(22.5610344912501,1.7652010450045,12.));
#215014=CARTESIAN_POINT('Ctrl Pts',(22.5682508499873,1.76515418518829,0.));
#215015=CARTESIAN_POINT('Ctrl Pts',(22.5682508499873,1.76515418518829,12.));
#215016=CARTESIAN_POINT('Ctrl Pts',(22.5757315316355,1.76507744026747,0.));
#215017=CARTESIAN_POINT('Ctrl Pts',(22.5757315316355,1.76507744026747,12.));
#215018=CARTESIAN_POINT('Ctrl Pts',(22.5834711038024,1.76496910283089,0.));
#215019=CARTESIAN_POINT('Ctrl Pts',(22.5834711038024,1.76496910283089,12.));
#215020=CARTESIAN_POINT('Ctrl Pts',(22.5914644078106,1.76482755288411,0.));
#215021=CARTESIAN_POINT('Ctrl Pts',(22.5914644078106,1.76482755288411,12.));
#215022=CARTESIAN_POINT('Ctrl Pts',(22.5997065145638,1.76465124413556,0.));
#215023=CARTESIAN_POINT('Ctrl Pts',(22.5997065145638,1.76465124413556,12.));
#215024=CARTESIAN_POINT('Ctrl Pts',(22.6081926681342,1.76443868648015,0.));
#215025=CARTESIAN_POINT('Ctrl Pts',(22.6081926681342,1.76443868648015,12.));
#215026=CARTESIAN_POINT('Ctrl Pts',(22.6169182517693,1.76418843543739,0.));
#215027=CARTESIAN_POINT('Ctrl Pts',(22.6169182517693,1.76418843543739,12.));
#215028=CARTESIAN_POINT('Ctrl Pts',(22.6258787994847,1.76389909571402,0.));
#215029=CARTESIAN_POINT('Ctrl Pts',(22.6258787994847,1.76389909571402,12.));
#215030=CARTESIAN_POINT('Ctrl Pts',(22.635069997936,1.76356932176272,0.));
#215031=CARTESIAN_POINT('Ctrl Pts',(22.635069997936,1.76356932176272,12.));
#215032=CARTESIAN_POINT('Ctrl Pts',(22.6444876940425,1.76319782013914,0.));
#215033=CARTESIAN_POINT('Ctrl Pts',(22.6444876940425,1.76319782013914,12.));
#215034=CARTESIAN_POINT('Ctrl Pts',(22.6541278938413,1.76278334912559,0.));
#215035=CARTESIAN_POINT('Ctrl Pts',(22.6541278938413,1.76278334912559,12.));
#215036=CARTESIAN_POINT('Ctrl Pts',(22.6639867471756,1.76232471392568,0.));
#215037=CARTESIAN_POINT('Ctrl Pts',(22.6639867471756,1.76232471392568,12.));
#215038=CARTESIAN_POINT('Ctrl Pts',(22.6740605356699,1.76182076289525,0.));
#215039=CARTESIAN_POINT('Ctrl Pts',(22.6740605356699,1.76182076289525,12.));
#215040=CARTESIAN_POINT('Ctrl Pts',(22.6843456585245,1.76127038310613,0.));
#215041=CARTESIAN_POINT('Ctrl Pts',(22.6843456585245,1.76127038310613,12.));
#215042=CARTESIAN_POINT('Ctrl Pts',(22.6948386219843,1.76067249704884,0.));
#215043=CARTESIAN_POINT('Ctrl Pts',(22.6948386219843,1.76067249704884,12.));
#215044=CARTESIAN_POINT('Ctrl Pts',(22.7055360375481,1.76002606202399,0.));
#215045=CARTESIAN_POINT('Ctrl Pts',(22.7055360375481,1.76002606202399,12.));
#215046=CARTESIAN_POINT('Ctrl Pts',(22.7164346186007,1.75933006905924,0.));
#215047=CARTESIAN_POINT('Ctrl Pts',(22.7164346186007,1.75933006905924,12.));
#215048=CARTESIAN_POINT('Ctrl Pts',(22.7275311777305,1.75858354204635,0.));
#215049=CARTESIAN_POINT('Ctrl Pts',(22.7275311777305,1.75858354204635,12.));
#215050=CARTESIAN_POINT('Ctrl Pts',(22.7388226235565,1.75778553673249,0.));
#215051=CARTESIAN_POINT('Ctrl Pts',(22.7388226235565,1.75778553673249,12.));
#215052=CARTESIAN_POINT('Ctrl Pts',(22.7503059556455,1.75693513908911,0.));
#215053=CARTESIAN_POINT('Ctrl Pts',(22.7503059556455,1.75693513908911,12.));
#215054=CARTESIAN_POINT('Ctrl Pts',(22.7619782595013,1.75603146371641,0.));
#215055=CARTESIAN_POINT('Ctrl Pts',(22.7619782595013,1.75603146371641,12.));
#215056=CARTESIAN_POINT('Ctrl Pts',(22.7738367016115,1.75507365227127,0.));
#215057=CARTESIAN_POINT('Ctrl Pts',(22.7738367016115,1.75507365227127,12.));
#215058=CARTESIAN_POINT('Ctrl Pts',(22.7858785242358,1.7540608718293,0.));
#215059=CARTESIAN_POINT('Ctrl Pts',(22.7858785242358,1.7540608718293,12.));
#215060=CARTESIAN_POINT('Ctrl Pts',(22.7981010424312,1.75299231391461,0.));
#215061=CARTESIAN_POINT('Ctrl Pts',(22.7981010424312,1.75299231391461,12.));
#215062=CARTESIAN_POINT('Ctrl Pts',(22.8105016414712,1.7518671936559,0.));
#215063=CARTESIAN_POINT('Ctrl Pts',(22.8105016414712,1.7518671936559,12.));
#215064=CARTESIAN_POINT('Ctrl Pts',(22.8230777741285,1.75068474890884,0.));
#215065=CARTESIAN_POINT('Ctrl Pts',(22.8230777741285,1.75068474890884,12.));
#215066=CARTESIAN_POINT('Ctrl Pts',(22.8358269579854,1.74944423940117,0.));
#215067=CARTESIAN_POINT('Ctrl Pts',(22.8358269579854,1.74944423940117,12.));
#215068=CARTESIAN_POINT('Ctrl Pts',(22.8487467728075,1.74814494588492,0.));
#215069=CARTESIAN_POINT('Ctrl Pts',(22.8487467728075,1.74814494588492,12.));
#215070=CARTESIAN_POINT('Ctrl Pts',(22.8618348580234,1.74678616930663,0.));
#215071=CARTESIAN_POINT('Ctrl Pts',(22.8618348580234,1.74678616930663,12.));
#215072=CARTESIAN_POINT('Ctrl Pts',(22.8750889101696,1.745367229982,0.));
#215073=CARTESIAN_POINT('Ctrl Pts',(22.8750889101696,1.745367229982,12.));
#215074=CARTESIAN_POINT('Ctrl Pts',(22.8885066803351,1.74388746677702,0.));
#215075=CARTESIAN_POINT('Ctrl Pts',(22.8885066803351,1.74388746677702,12.));
#215076=CARTESIAN_POINT('Ctrl Pts',(22.9020859716144,1.74234623630079,0.));
#215077=CARTESIAN_POINT('Ctrl Pts',(22.9020859716144,1.74234623630079,12.));
#215078=CARTESIAN_POINT('Ctrl Pts',(22.9158246373365,1.74074291231057,0.));
#215079=CARTESIAN_POINT('Ctrl Pts',(22.9158246373365,1.74074291231057,12.));
#215080=CARTESIAN_POINT('Ctrl Pts',(22.9297205792587,1.73907688511665,0.));
#215081=CARTESIAN_POINT('Ctrl Pts',(22.9297205792587,1.73907688511665,12.));
#215082=CARTESIAN_POINT('Ctrl Pts',(22.9437717457825,1.73734756100038,0.));
#215083=CARTESIAN_POINT('Ctrl Pts',(22.9437717457825,1.73734756100038,12.));
#215084=CARTESIAN_POINT('Ctrl Pts',(22.9579761301062,1.73555436162771,0.));
#215085=CARTESIAN_POINT('Ctrl Pts',(22.9579761301062,1.73555436162771,12.));
#215086=CARTESIAN_POINT('Ctrl Pts',(22.9723317685688,1.73369672350818,0.));
#215087=CARTESIAN_POINT('Ctrl Pts',(22.9723317685688,1.73369672350818,12.));
#215088=CARTESIAN_POINT('Ctrl Pts',(22.9868367391978,1.73177409750194,0.));
#215089=CARTESIAN_POINT('Ctrl Pts',(22.9868367391978,1.73177409750194,12.));
#215090=CARTESIAN_POINT('Ctrl Pts',(23.0014891601891,1.72978594832137,0.));
#215091=CARTESIAN_POINT('Ctrl Pts',(23.0014891601891,1.72978594832137,12.));
#215092=CARTESIAN_POINT('Ctrl Pts',(23.0162871884167,1.72773175404703,0.));
#215093=CARTESIAN_POINT('Ctrl Pts',(23.0162871884167,1.72773175404703,12.));
#215094=CARTESIAN_POINT('Ctrl Pts',(23.031229017888,1.72561100564033,0.));
#215095=CARTESIAN_POINT('Ctrl Pts',(23.031229017888,1.72561100564033,12.));
#215096=CARTESIAN_POINT('Ctrl Pts',(23.0463128785528,1.72342320653731,0.));
#215097=CARTESIAN_POINT('Ctrl Pts',(23.0463128785528,1.72342320653731,12.));
#215098=CARTESIAN_POINT('Ctrl Pts',(23.0615370351559,1.72116787225981,0.));
#215099=CARTESIAN_POINT('Ctrl Pts',(23.0615370351559,1.72116787225981,12.));
#215100=CARTESIAN_POINT('Ctrl Pts',(23.0768997860709,1.71884453003027,0.));
#215101=CARTESIAN_POINT('Ctrl Pts',(23.0768997860709,1.71884453003027,12.));
#215102=CARTESIAN_POINT('Ctrl Pts',(23.0923994621216,1.71645271839311,0.));
#215103=CARTESIAN_POINT('Ctrl Pts',(23.0923994621216,1.71645271839311,12.));
#215104=CARTESIAN_POINT('Ctrl Pts',(23.1080344254291,1.71399198684725,0.));
#215105=CARTESIAN_POINT('Ctrl Pts',(23.1080344254291,1.71399198684725,12.));
#215106=CARTESIAN_POINT('Ctrl Pts',(23.1238030684929,1.71146189552192,0.));
#215107=CARTESIAN_POINT('Ctrl Pts',(23.1238030684929,1.71146189552192,12.));
#215108=CARTESIAN_POINT('Ctrl Pts',(23.1397038132358,1.7088620148546,0.));
#215109=CARTESIAN_POINT('Ctrl Pts',(23.1397038132358,1.7088620148546,12.));
#215110=CARTESIAN_POINT('Ctrl Pts',(23.1557351100613,1.70619192527847,0.));
#215111=CARTESIAN_POINT('Ctrl Pts',(23.1557351100613,1.70619192527847,12.));
#215112=CARTESIAN_POINT('Ctrl Pts',(23.1718954368749,1.70345121691259,0.));
#215113=CARTESIAN_POINT('Ctrl Pts',(23.1718954368749,1.70345121691259,12.));
#215114=CARTESIAN_POINT('Ctrl Pts',(23.1881832981848,1.70063948926988,0.));
#215115=CARTESIAN_POINT('Ctrl Pts',(23.1881832981848,1.70063948926988,12.));
#215116=CARTESIAN_POINT('Ctrl Pts',(23.2045972243765,1.69775635099425,0.));
#215117=CARTESIAN_POINT('Ctrl Pts',(23.2045972243765,1.69775635099425,12.));
#215118=CARTESIAN_POINT('Ctrl Pts',(23.2211357709374,1.69480141959946,0.));
#215119=CARTESIAN_POINT('Ctrl Pts',(23.2211357709374,1.69480141959946,12.));
#215120=CARTESIAN_POINT('Ctrl Pts',(23.2377975177014,1.69177432121716,0.));
#215121=CARTESIAN_POINT('Ctrl Pts',(23.2377975177014,1.69177432121716,12.));
#215122=CARTESIAN_POINT('Ctrl Pts',(23.2545810680536,1.6886746903491,0.));
#215123=CARTESIAN_POINT('Ctrl Pts',(23.2545810680536,1.6886746903491,12.));
#215124=CARTESIAN_POINT('Ctrl Pts',(23.2714850482245,1.68550216963275,0.));
#215125=CARTESIAN_POINT('Ctrl Pts',(23.2714850482245,1.68550216963275,12.));
#215126=CARTESIAN_POINT('Ctrl Pts',(23.2885081066949,1.68225640962181,0.));
#215127=CARTESIAN_POINT('Ctrl Pts',(23.2885081066949,1.68225640962181,12.));
#215128=CARTESIAN_POINT('Ctrl Pts',(23.3056489135611,1.67893706857123,0.));
#215129=CARTESIAN_POINT('Ctrl Pts',(23.3056489135611,1.67893706857123,12.));
#215130=CARTESIAN_POINT('Ctrl Pts',(23.3229061599145,1.67554381222988,0.));
#215131=CARTESIAN_POINT('Ctrl Pts',(23.3229061599145,1.67554381222988,12.));
#215132=CARTESIAN_POINT('Ctrl Pts',(23.3402785571866,1.67207631363905,0.));
#215133=CARTESIAN_POINT('Ctrl Pts',(23.3402785571866,1.67207631363905,12.));
#215134=CARTESIAN_POINT('Ctrl Pts',(23.3577648365747,1.66853425293978,0.));
#215135=CARTESIAN_POINT('Ctrl Pts',(23.3577648365747,1.66853425293978,12.));
#215136=CARTESIAN_POINT('Ctrl Pts',(23.375363748555,1.66491731718864,0.));
#215137=CARTESIAN_POINT('Ctrl Pts',(23.375363748555,1.66491731718864,12.));
#215138=CARTESIAN_POINT('Ctrl Pts',(23.3930740623622,1.66122520018008,0.));
#215139=CARTESIAN_POINT('Ctrl Pts',(23.3930740623622,1.66122520018008,12.));
#215140=CARTESIAN_POINT('Ctrl Pts',(23.4108945654803,1.65745760227507,0.));
#215141=CARTESIAN_POINT('Ctrl Pts',(23.4108945654803,1.65745760227507,12.));
#215142=CARTESIAN_POINT('Ctrl Pts',(23.4288240631034,1.6536142302373,0.));
#215143=CARTESIAN_POINT('Ctrl Pts',(23.4288240631034,1.6536142302373,12.));
#215144=CARTESIAN_POINT('Ctrl Pts',(23.446861377656,1.6496947970734,0.));
#215145=CARTESIAN_POINT('Ctrl Pts',(23.446861377656,1.6496947970734,12.));
#215146=CARTESIAN_POINT('Ctrl Pts',(23.4650053483919,1.64569902187608,0.));
#215147=CARTESIAN_POINT('Ctrl Pts',(23.4650053483919,1.64569902187608,12.));
#215148=CARTESIAN_POINT('Ctrl Pts',(23.4832548309638,1.64162662967525,0.));
#215149=CARTESIAN_POINT('Ctrl Pts',(23.4832548309638,1.64162662967525,12.));
#215150=CARTESIAN_POINT('Ctrl Pts',(23.5016086970006,1.63747735129474,0.));
#215151=CARTESIAN_POINT('Ctrl Pts',(23.5016086970006,1.63747735129474,12.));
#215152=CARTESIAN_POINT('Ctrl Pts',(23.5200658336624,1.63325092321731,0.));
#215153=CARTESIAN_POINT('Ctrl Pts',(23.5200658336624,1.63325092321731,12.));
#215154=CARTESIAN_POINT('Ctrl Pts',(23.5386251432278,1.62894708745231,0.));
#215155=CARTESIAN_POINT('Ctrl Pts',(23.5386251432278,1.62894708745231,12.));
#215156=CARTESIAN_POINT('Ctrl Pts',(23.5572855427617,1.62456559140072,0.));
#215157=CARTESIAN_POINT('Ctrl Pts',(23.5572855427617,1.62456559140072,12.));
#215158=CARTESIAN_POINT('Ctrl Pts',(23.5760459637608,1.62010618772869,0.));
#215159=CARTESIAN_POINT('Ctrl Pts',(23.5760459637608,1.62010618772869,12.));
#215160=CARTESIAN_POINT('Ctrl Pts',(23.5949053517996,1.61556863424697,0.));
#215161=CARTESIAN_POINT('Ctrl Pts',(23.5949053517996,1.61556863424697,12.));
#215162=CARTESIAN_POINT('Ctrl Pts',(23.6138626661644,1.61095269379773,0.));
#215163=CARTESIAN_POINT('Ctrl Pts',(23.6138626661644,1.61095269379773,12.));
#215164=CARTESIAN_POINT('Ctrl Pts',(23.6329168794916,1.60625813414666,0.));
#215165=CARTESIAN_POINT('Ctrl Pts',(23.6329168794916,1.60625813414666,12.));
#215166=CARTESIAN_POINT('Ctrl Pts',(23.6520669774863,1.60148472786588,0.));
#215167=CARTESIAN_POINT('Ctrl Pts',(23.6520669774863,1.60148472786588,12.));
#215168=CARTESIAN_POINT('Ctrl Pts',(23.6713119586302,1.59663225222459,0.));
#215169=CARTESIAN_POINT('Ctrl Pts',(23.6713119586302,1.59663225222459,12.));
#215170=CARTESIAN_POINT('Ctrl Pts',(23.6906508338832,1.59170048908631,0.));
#215171=CARTESIAN_POINT('Ctrl Pts',(23.6906508338832,1.59170048908631,12.));
#215172=CARTESIAN_POINT('Ctrl Pts',(23.7100826263835,1.58668922481222,0.));
#215173=CARTESIAN_POINT('Ctrl Pts',(23.7100826263835,1.58668922481222,12.));
#215174=CARTESIAN_POINT('Ctrl Pts',(23.7296063711308,1.58159825017362,0.));
#215175=CARTESIAN_POINT('Ctrl Pts',(23.7296063711308,1.58159825017362,12.));
#215176=CARTESIAN_POINT('Ctrl Pts',(23.7492211147369,1.57642736025251,0.));
#215177=CARTESIAN_POINT('Ctrl Pts',(23.7492211147369,1.57642736025251,12.));
#215178=CARTESIAN_POINT('Ctrl Pts',(23.7689259151869,1.57117635434412,0.));
#215179=CARTESIAN_POINT('Ctrl Pts',(23.7689259151869,1.57117635434412,12.));
#215180=CARTESIAN_POINT('Ctrl Pts',(23.788719841588,1.56584503586844,0.));
#215181=CARTESIAN_POINT('Ctrl Pts',(23.788719841588,1.56584503586844,12.));
#215182=CARTESIAN_POINT('Ctrl Pts',(23.8086019739192,1.56043321228631,0.));
#215183=CARTESIAN_POINT('Ctrl Pts',(23.8086019739192,1.56043321228631,12.));
#215184=CARTESIAN_POINT('Ctrl Pts',(23.8285714027631,1.55494069502628,0.));
#215185=CARTESIAN_POINT('Ctrl Pts',(23.8285714027631,1.55494069502628,12.));
#215186=CARTESIAN_POINT('Ctrl Pts',(23.8486272290698,1.5493672994053,0.));
#215187=CARTESIAN_POINT('Ctrl Pts',(23.8486272290698,1.5493672994053,12.));
#215188=CARTESIAN_POINT('Ctrl Pts',(23.8687685639635,1.54371284453978,0.));
#215189=CARTESIAN_POINT('Ctrl Pts',(23.8687685639635,1.54371284453978,12.));
#215190=CARTESIAN_POINT('Ctrl Pts',(23.8889945285313,1.53797715326748,0.));
#215191=CARTESIAN_POINT('Ctrl Pts',(23.8889945285313,1.53797715326748,12.));
#215192=CARTESIAN_POINT('Ctrl Pts',(23.9093042536119,1.53216005207462,0.));
#215193=CARTESIAN_POINT('Ctrl Pts',(23.9093042536119,1.53216005207462,12.));
#215194=CARTESIAN_POINT('Ctrl Pts',(23.9296968795761,1.5262613710304,0.));
#215195=CARTESIAN_POINT('Ctrl Pts',(23.9296968795761,1.5262613710304,12.));
#215196=CARTESIAN_POINT('Ctrl Pts',(23.9501715561038,1.52028094372806,0.));
#215197=CARTESIAN_POINT('Ctrl Pts',(23.9501715561038,1.52028094372806,12.));
#215198=CARTESIAN_POINT('Ctrl Pts',(23.9707274420145,1.51421860720628,0.));
#215199=CARTESIAN_POINT('Ctrl Pts',(23.9707274420145,1.51421860720628,12.));
#215200=CARTESIAN_POINT('Ctrl Pts',(23.991363705093,1.50807420187703,0.));
#215201=CARTESIAN_POINT('Ctrl Pts',(23.991363705093,1.50807420187703,12.));
#215202=CARTESIAN_POINT('Ctrl Pts',(24.0120795219086,1.50184757146099,0.));
#215203=CARTESIAN_POINT('Ctrl Pts',(24.0120795219086,1.50184757146099,12.));
#215204=CARTESIAN_POINT('Ctrl Pts',(24.0328740776331,1.49553856292798,0.));
#215205=CARTESIAN_POINT('Ctrl Pts',(24.0328740776331,1.49553856292798,12.));
#215206=CARTESIAN_POINT('Ctrl Pts',(24.053746565843,1.48914702644883,0.));
#215207=CARTESIAN_POINT('Ctrl Pts',(24.053746565843,1.48914702644883,12.));
#215208=CARTESIAN_POINT('Ctrl Pts',(24.074696188353,1.4826728153368,0.));
#215209=CARTESIAN_POINT('Ctrl Pts',(24.074696188353,1.4826728153368,12.));
#215210=CARTESIAN_POINT('Ctrl Pts',(24.0957221550782,1.47611578597742,0.));
#215211=CARTESIAN_POINT('Ctrl Pts',(24.0957221550782,1.47611578597742,12.));
#215212=CARTESIAN_POINT('Ctrl Pts',(24.1168236838827,1.46947579776992,0.));
#215213=CARTESIAN_POINT('Ctrl Pts',(24.1168236838827,1.46947579776992,12.));
#215214=CARTESIAN_POINT('Ctrl Pts',(24.1380000004272,1.46275271307398,0.));
#215215=CARTESIAN_POINT('Ctrl Pts',(24.1380000004272,1.46275271307398,12.));
#215216=CARTESIAN_POINT('Ctrl Pts',(24.1592503380105,1.45594639716314,0.));
#215217=CARTESIAN_POINT('Ctrl Pts',(24.1592503380105,1.45594639716314,12.));
#215218=CARTESIAN_POINT('Ctrl Pts',(24.1805739374033,1.44905671818721,0.));
#215219=CARTESIAN_POINT('Ctrl Pts',(24.1805739374033,1.44905671818721,12.));
#215220=CARTESIAN_POINT('Ctrl Pts',(24.2019700467214,1.44208354711074,0.));
#215221=CARTESIAN_POINT('Ctrl Pts',(24.2019700467214,1.44208354711074,12.));
#215222=CARTESIAN_POINT('Ctrl Pts',(24.2234379212978,1.43502675765502,0.));
#215223=CARTESIAN_POINT('Ctrl Pts',(24.2234379212978,1.43502675765502,12.));
#215224=CARTESIAN_POINT('Ctrl Pts',(24.2449768235485,1.42788622624851,0.));
#215225=CARTESIAN_POINT('Ctrl Pts',(24.2449768235485,1.42788622624851,12.));
#215226=CARTESIAN_POINT('Ctrl Pts',(24.2665860228357,1.42066183198252,0.));
#215227=CARTESIAN_POINT('Ctrl Pts',(24.2665860228357,1.42066183198252,12.));
#215228=CARTESIAN_POINT('Ctrl Pts',(24.2882647953214,1.41335345657685,0.));
#215229=CARTESIAN_POINT('Ctrl Pts',(24.2882647953214,1.41335345657685,12.));
#215230=CARTESIAN_POINT('Ctrl Pts',(24.3100124238316,1.40596098434341,0.));
#215231=CARTESIAN_POINT('Ctrl Pts',(24.3100124238316,1.40596098434341,12.));
#215232=CARTESIAN_POINT('Ctrl Pts',(24.3318281977647,1.3984843021281,0.));
#215233=CARTESIAN_POINT('Ctrl Pts',(24.3318281977647,1.3984843021281,12.));
#215234=CARTESIAN_POINT('Ctrl Pts',(24.3537114129877,1.3909232992639,0.));
#215235=CARTESIAN_POINT('Ctrl Pts',(24.3537114129877,1.3909232992639,12.));
#215236=CARTESIAN_POINT('Ctrl Pts',(24.37566137173,1.38327786752998,0.));
#215237=CARTESIAN_POINT('Ctrl Pts',(24.37566137173,1.38327786752998,12.));
#215238=CARTESIAN_POINT('Ctrl Pts',(24.3976773824731,1.37554790111608,0.));
#215239=CARTESIAN_POINT('Ctrl Pts',(24.3976773824731,1.37554790111608,12.));
#215240=CARTESIAN_POINT('Ctrl Pts',(24.4197587598337,1.36773329659954,0.));
#215241=CARTESIAN_POINT('Ctrl Pts',(24.4197587598337,1.36773329659954,12.));
#215242=CARTESIAN_POINT('Ctrl Pts',(24.4419048244524,1.35983395290624,0.));
#215243=CARTESIAN_POINT('Ctrl Pts',(24.4419048244524,1.35983395290624,12.));
#215244=CARTESIAN_POINT('Ctrl Pts',(24.4641149028894,1.35184977125645,0.));
#215245=CARTESIAN_POINT('Ctrl Pts',(24.4641149028894,1.35184977125645,12.));
#215246=CARTESIAN_POINT('Ctrl Pts',(24.4863883275135,1.34378065512335,0.));
#215247=CARTESIAN_POINT('Ctrl Pts',(24.4863883275135,1.34378065512335,12.));
#215248=CARTESIAN_POINT('Ctrl Pts',(24.5087244363856,1.33562651019684,0.));
#215249=CARTESIAN_POINT('Ctrl Pts',(24.5087244363856,1.33562651019684,12.));
#215250=CARTESIAN_POINT('Ctrl Pts',(24.5311225731434,1.32738724435326,0.));
#215251=CARTESIAN_POINT('Ctrl Pts',(24.5311225731434,1.32738724435326,12.));
#215252=CARTESIAN_POINT('Ctrl Pts',(24.5535820868671,1.31906276763669,0.));
#215253=CARTESIAN_POINT('Ctrl Pts',(24.5535820868671,1.31906276763669,12.));
#215254=CARTESIAN_POINT('Ctrl Pts',(24.576102332018,1.31065299222023,0.));
#215255=CARTESIAN_POINT('Ctrl Pts',(24.576102332018,1.31065299222023,12.));
#215256=CARTESIAN_POINT('Ctrl Pts',(24.5986826684025,1.30215783236364,0.));
#215257=CARTESIAN_POINT('Ctrl Pts',(24.5986826684025,1.30215783236364,12.));
#215258=CARTESIAN_POINT('Ctrl Pts',(24.6213224611228,1.29357720438108,0.));
#215259=CARTESIAN_POINT('Ctrl Pts',(24.6213224611228,1.29357720438108,12.));
#215260=CARTESIAN_POINT('Ctrl Pts',(24.6440210805278,1.28491102661514,0.));
#215261=CARTESIAN_POINT('Ctrl Pts',(24.6440210805278,1.28491102661514,12.));
#215262=CARTESIAN_POINT('Ctrl Pts',(24.666777902156,1.2761592194164,0.));
#215263=CARTESIAN_POINT('Ctrl Pts',(24.666777902156,1.2761592194164,12.));
#215264=CARTESIAN_POINT('Ctrl Pts',(24.6895923066837,1.26732170513497,0.));
#215265=CARTESIAN_POINT('Ctrl Pts',(24.6895923066837,1.26732170513497,12.));
#215266=CARTESIAN_POINT('Ctrl Pts',(24.7124636797895,1.25839840807415,0.));
#215267=CARTESIAN_POINT('Ctrl Pts',(24.7124636797895,1.25839840807415,12.));
#215268=CARTESIAN_POINT('Ctrl Pts',(24.7353914120012,1.24938925444324,0.));
#215269=CARTESIAN_POINT('Ctrl Pts',(24.7353914120012,1.24938925444324,12.));
#215270=CARTESIAN_POINT('Ctrl Pts',(24.7583748985439,1.24029417231988,0.));
#215271=CARTESIAN_POINT('Ctrl Pts',(24.7583748985439,1.24029417231988,12.));
#215272=CARTESIAN_POINT('Ctrl Pts',(24.78141353918,1.23111309161843,0.));
#215273=CARTESIAN_POINT('Ctrl Pts',(24.78141353918,1.23111309161843,12.));
#215274=CARTESIAN_POINT('Ctrl Pts',(24.8045067380536,1.22184594406527,0.));
#215275=CARTESIAN_POINT('Ctrl Pts',(24.8045067380536,1.22184594406527,12.));
#215276=CARTESIAN_POINT('Ctrl Pts',(24.8276539035092,1.21249266318205,0.));
#215277=CARTESIAN_POINT('Ctrl Pts',(24.8276539035092,1.21249266318205,12.));
#215278=CARTESIAN_POINT('Ctrl Pts',(24.8508544481973,1.20305318426016,0.));
#215279=CARTESIAN_POINT('Ctrl Pts',(24.8508544481973,1.20305318426016,12.));
#215280=CARTESIAN_POINT('Ctrl Pts',(24.8741077892074,1.19352744434059,0.));
#215281=CARTESIAN_POINT('Ctrl Pts',(24.8741077892074,1.19352744434059,12.));
#215282=CARTESIAN_POINT('Ctrl Pts',(24.8974133481829,1.18391538220098,0.));
#215283=CARTESIAN_POINT('Ctrl Pts',(24.8974133481829,1.18391538220098,12.));
#215284=CARTESIAN_POINT('Ctrl Pts',(24.9207705514449,1.1742169383504,0.));
#215285=CARTESIAN_POINT('Ctrl Pts',(24.9207705514449,1.1742169383504,12.));
#215286=CARTESIAN_POINT('Ctrl Pts',(24.9441788300932,1.16443205502852,0.));
#215287=CARTESIAN_POINT('Ctrl Pts',(24.9441788300932,1.16443205502852,12.));
#215288=CARTESIAN_POINT('Ctrl Pts',(24.9676376201501,1.15456067621894,0.));
#215289=CARTESIAN_POINT('Ctrl Pts',(24.9676376201501,1.15456067621894,12.));
#215290=CARTESIAN_POINT('Ctrl Pts',(24.9911463621431,1.14460274758206,0.));
#215291=CARTESIAN_POINT('Ctrl Pts',(24.9911463621431,1.14460274758206,12.));
#215292=CARTESIAN_POINT('Ctrl Pts',(25.0147045006193,1.13455821638536,0.));
#215293=CARTESIAN_POINT('Ctrl Pts',(25.0147045006193,1.13455821638536,12.));
#215294=CARTESIAN_POINT('Ctrl Pts',(25.0383114836898,1.12442703144455,0.));
#215295=CARTESIAN_POINT('Ctrl Pts',(25.0383114836898,1.12442703144455,12.));
#215296=CARTESIAN_POINT('Ctrl Pts',(25.0619667625336,1.1142091430689,0.));
#215297=CARTESIAN_POINT('Ctrl Pts',(25.0619667625336,1.1142091430689,12.));
#215298=CARTESIAN_POINT('Ctrl Pts',(25.085669790968,1.10390450301741,0.));
#215299=CARTESIAN_POINT('Ctrl Pts',(25.085669790968,1.10390450301741,12.));
#215300=CARTESIAN_POINT('Ctrl Pts',(25.1094200248448,1.09351306445299,0.));
#215301=CARTESIAN_POINT('Ctrl Pts',(25.1094200248448,1.09351306445299,12.));
#215302=CARTESIAN_POINT('Ctrl Pts',(25.1332169227415,1.08303478197174,0.));
#215303=CARTESIAN_POINT('Ctrl Pts',(25.1332169227415,1.08303478197174,12.));
#215304=CARTESIAN_POINT('Ctrl Pts',(25.1570599469311,1.0724696116546,0.));
#215305=CARTESIAN_POINT('Ctrl Pts',(25.1570599469311,1.0724696116546,12.));
#215306=CARTESIAN_POINT('Ctrl Pts',(25.1809485642191,1.06181751111754,0.));
#215307=CARTESIAN_POINT('Ctrl Pts',(25.1809485642191,1.06181751111754,12.));
#215308=CARTESIAN_POINT('Ctrl Pts',(25.2048822469027,1.05107843957926,0.));
#215309=CARTESIAN_POINT('Ctrl Pts',(25.2048822469027,1.05107843957926,12.));
#215310=CARTESIAN_POINT('Ctrl Pts',(25.2288604735087,1.04025235791515,0.));
#215311=CARTESIAN_POINT('Ctrl Pts',(25.2288604735087,1.04025235791515,12.));
#215312=CARTESIAN_POINT('Ctrl Pts',(25.2528827300427,1.0293392287683,0.));
#215313=CARTESIAN_POINT('Ctrl Pts',(25.2528827300427,1.0293392287683,12.));
#215314=CARTESIAN_POINT('Ctrl Pts',(25.2769485087268,1.01833901642273,0.));
#215315=CARTESIAN_POINT('Ctrl Pts',(25.2769485087268,1.01833901642273,12.));
#215316=CARTESIAN_POINT('Ctrl Pts',(25.3010573055557,1.00725168656934,0.));
#215317=CARTESIAN_POINT('Ctrl Pts',(25.3010573055557,1.00725168656934,12.));
#215318=CARTESIAN_POINT('Ctrl Pts',(25.3252086182976,0.996077206120921,
0.));
#215319=CARTESIAN_POINT('Ctrl Pts',(25.3252086182976,0.996077206120921,
12.));
#215320=CARTESIAN_POINT('Ctrl Pts',(25.3494019441444,0.984815543004091,
0.));
#215321=CARTESIAN_POINT('Ctrl Pts',(25.3494019441444,0.984815543004091,
12.));
#215322=CARTESIAN_POINT('Ctrl Pts',(25.3736367778842,0.97346666600005,0.));
#215323=CARTESIAN_POINT('Ctrl Pts',(25.3736367778842,0.97346666600005,12.));
#215324=CARTESIAN_POINT('Ctrl Pts',(25.3979126089155,0.962030544502806,
0.));
#215325=CARTESIAN_POINT('Ctrl Pts',(25.3979126089155,0.962030544502806,
12.));
#215326=CARTESIAN_POINT('Ctrl Pts',(25.4222289223155,0.950507148596971,
0.));
#215327=CARTESIAN_POINT('Ctrl Pts',(25.4222289223155,0.950507148596971,
12.));
#215328=CARTESIAN_POINT('Ctrl Pts',(25.4465852044835,0.938896449495636,
0.));
#215329=CARTESIAN_POINT('Ctrl Pts',(25.4465852044835,0.938896449495636,
12.));
#215330=CARTESIAN_POINT('Ctrl Pts',(25.4709809474996,0.927198419885607,
0.));
#215331=CARTESIAN_POINT('Ctrl Pts',(25.4709809474996,0.927198419885607,
12.));
#215332=CARTESIAN_POINT('Ctrl Pts',(25.4954156541787,0.915413034335334,
0.));
#215333=CARTESIAN_POINT('Ctrl Pts',(25.4954156541787,0.915413034335334,
12.));
#215334=CARTESIAN_POINT('Ctrl Pts',(25.5198888424195,0.903540269651155,
0.));
#215335=CARTESIAN_POINT('Ctrl Pts',(25.5198888424195,0.903540269651155,
12.));
#215336=CARTESIAN_POINT('Ctrl Pts',(25.5444000508223,0.891580105349469,
0.));
#215337=CARTESIAN_POINT('Ctrl Pts',(25.5444000508223,0.891580105349469,
12.));
#215338=CARTESIAN_POINT('Ctrl Pts',(25.568948840818,0.879532523835094,0.));
#215339=CARTESIAN_POINT('Ctrl Pts',(25.568948840818,0.879532523835094,12.));
#215340=CARTESIAN_POINT('Ctrl Pts',(25.5935347843616,0.867397509339473,
0.));
#215341=CARTESIAN_POINT('Ctrl Pts',(25.5935347843616,0.867397509339473,
12.));
#215342=CARTESIAN_POINT('Ctrl Pts',(25.618157453608,0.855175047037618,0.));
#215343=CARTESIAN_POINT('Ctrl Pts',(25.618157453608,0.855175047037618,12.));
#215344=CARTESIAN_POINT('Ctrl Pts',(25.6428164100078,0.842865122121547,
0.));
#215345=CARTESIAN_POINT('Ctrl Pts',(25.6428164100078,0.842865122121547,
12.));
#215346=CARTESIAN_POINT('Ctrl Pts',(25.6675111931957,0.83046771886437,0.));
#215347=CARTESIAN_POINT('Ctrl Pts',(25.6675111931957,0.83046771886437,12.));
#215348=CARTESIAN_POINT('Ctrl Pts',(25.6922413110172,0.817982819786722,
0.));
#215349=CARTESIAN_POINT('Ctrl Pts',(25.6922413110172,0.817982819786722,
12.));
#215350=CARTESIAN_POINT('Ctrl Pts',(25.7170062262474,0.805410404552597,
0.));
#215351=CARTESIAN_POINT('Ctrl Pts',(25.7170062262474,0.805410404552597,
12.));
#215352=CARTESIAN_POINT('Ctrl Pts',(25.7418053757671,0.792750451613538,
0.));
#215353=CARTESIAN_POINT('Ctrl Pts',(25.7418053757671,0.792750451613538,
12.));
#215354=CARTESIAN_POINT('Ctrl Pts',(25.7666381946871,0.780002940289028,
0.));
#215355=CARTESIAN_POINT('Ctrl Pts',(25.7666381946871,0.780002940289028,
12.));
#215356=CARTESIAN_POINT('Ctrl Pts',(25.7915041383304,0.767167852648643,
0.));
#215357=CARTESIAN_POINT('Ctrl Pts',(25.7915041383304,0.767167852648643,
12.));
#215358=CARTESIAN_POINT('Ctrl Pts',(25.816402705995,0.754245175608291,0.));
#215359=CARTESIAN_POINT('Ctrl Pts',(25.816402705995,0.754245175608291,12.));
#215360=CARTESIAN_POINT('Ctrl Pts',(25.841333461908,0.741234902664698,0.));
#215361=CARTESIAN_POINT('Ctrl Pts',(25.841333461908,0.741234902664698,12.));
#215362=CARTESIAN_POINT('Ctrl Pts',(25.8662960624285,0.728137036485881,
0.));
#215363=CARTESIAN_POINT('Ctrl Pts',(25.8662960624285,0.728137036485881,
12.));
#215364=CARTESIAN_POINT('Ctrl Pts',(25.8912902615141,0.714951588533756,
0.));
#215365=CARTESIAN_POINT('Ctrl Pts',(25.8912902615141,0.714951588533756,
12.));
#215366=CARTESIAN_POINT('Ctrl Pts',(25.9163158909645,0.701678575236605,
0.));
#215367=CARTESIAN_POINT('Ctrl Pts',(25.9163158909645,0.701678575236605,
12.));
#215368=CARTESIAN_POINT('Ctrl Pts',(25.941372847213,0.68831801506568,0.));
#215369=CARTESIAN_POINT('Ctrl Pts',(25.941372847213,0.68831801506568,12.));
#215370=CARTESIAN_POINT('Ctrl Pts',(25.9614434298092,0.677559543215907,
0.));
#215371=CARTESIAN_POINT('Ctrl Pts',(25.9614434298092,0.677559543215907,
12.));
#215372=CARTESIAN_POINT('Ctrl Pts',(25.9765104298171,0.669451306784419,
0.));
#215373=CARTESIAN_POINT('Ctrl Pts',(25.9765104298171,0.669451306784419,
12.));
#215374=CARTESIAN_POINT('Ctrl Pts',(25.9865613464809,0.664028313188916,
0.));
#215375=CARTESIAN_POINT('Ctrl Pts',(25.9865613464809,0.664028313188916,
12.));
#215376=CARTESIAN_POINT('Ctrl Pts',(25.991588367311,0.661312440730894,0.));
#215377=CARTESIAN_POINT('Ctrl Pts',(25.991588367311,0.661312440730894,12.));
#215378=CARTESIAN_POINT('',(25.991588367311,0.661312440730894,0.));
#215379=CARTESIAN_POINT('Origin',(0.,0.,0.));
#215380=CARTESIAN_POINT('',(0.,0.,0.));
#215381=CARTESIAN_POINT('Origin',(21.88788407408,-2.2182269405164,0.));
#215382=CARTESIAN_POINT('',(21.3904321633055,-2.1678126918683,0.));
#215383=CARTESIAN_POINT('',(21.9269795755927,-1.71975774210843,0.));
#215384=CARTESIAN_POINT('Origin',(21.88788407408,-2.2182269405164,0.));
#215385=CARTESIAN_POINT('',(21.9269795755927,-1.71975774210843,12.));
#215386=CARTESIAN_POINT('',(21.9269795755927,-1.71975774210843,0.));
#215387=CARTESIAN_POINT('',(21.3904321633055,-2.1678126918683,12.));
#215388=CARTESIAN_POINT('Origin',(21.88788407408,-2.2182269405164,12.));
#215389=CARTESIAN_POINT('',(21.3904321633055,-2.1678126918683,0.));
#215390=CARTESIAN_POINT('Origin',(22.4835757167854,-1.76341220531181,0.));
#215391=CARTESIAN_POINT('',(22.4835757167854,-1.76341220531181,0.));
#215392=CARTESIAN_POINT('',(11.2417878583927,-0.881706102655892,0.));
#215393=CARTESIAN_POINT('',(22.4835757167854,-1.76341220531181,12.));
#215394=CARTESIAN_POINT('',(22.4835757167854,-1.76341220531181,0.));
#215395=CARTESIAN_POINT('',(11.2417878583927,-0.881706102655892,12.));
#215396=CARTESIAN_POINT('Origin',(21.7161918885402,-3.52235856495314,0.));
#215397=CARTESIAN_POINT('',(21.624941921198,-4.0139614976743,0.));
#215398=CARTESIAN_POINT('',(21.2226420728916,-3.4423049612042,0.));
#215399=CARTESIAN_POINT('Origin',(21.7161918885402,-3.52235856495314,0.));
#215400=CARTESIAN_POINT('',(21.2226420728916,-3.4423049612042,12.));
#215401=CARTESIAN_POINT('',(21.2226420728916,-3.4423049612042,0.));
#215402=CARTESIAN_POINT('',(21.624941921198,-4.0139614976743,12.));
#215403=CARTESIAN_POINT('Origin',(21.7161918885402,-3.52235856495314,12.));
#215404=CARTESIAN_POINT('',(21.624941921198,-4.0139614976743,0.));
#215405=CARTESIAN_POINT('Origin',(7.6920903736728E-13,-1.31973449697531E-13,
0.));
#215406=CARTESIAN_POINT('Origin',(7.6920903736728E-13,-1.31973449697531E-13,
12.));
#215407=CARTESIAN_POINT('Origin',(7.6920903736728E-13,-1.31973449697531E-13,
0.));
#215408=CARTESIAN_POINT('Origin',(20.56795313141,-7.80764394578304,0.));
#215409=CARTESIAN_POINT('',(20.1004996511507,-7.63019749246979,0.));
#215410=CARTESIAN_POINT('',(20.7347298079577,-7.33627833380047,0.));
#215411=CARTESIAN_POINT('Origin',(20.56795313141,-7.80764394578304,0.));
#215412=CARTESIAN_POINT('',(20.7347298079577,-7.33627833380047,12.));
#215413=CARTESIAN_POINT('',(20.7347298079577,-7.33627833380047,0.));
#215414=CARTESIAN_POINT('',(20.1004996511507,-7.63019749246979,12.));
#215415=CARTESIAN_POINT('Origin',(20.56795313141,-7.80764394578304,12.));
#215416=CARTESIAN_POINT('',(20.1004996511507,-7.63019749246979,0.));
#215417=CARTESIAN_POINT('Origin',(21.2610617890679,-7.52250298901266,0.));
#215418=CARTESIAN_POINT('',(21.2610617890679,-7.52250298901266,0.));
#215419=CARTESIAN_POINT('',(10.6305308945339,-3.76125149450632,0.));
#215420=CARTESIAN_POINT('',(21.2610617890679,-7.52250298901266,12.));
#215421=CARTESIAN_POINT('',(21.2610617890679,-7.52250298901266,0.));
#215422=CARTESIAN_POINT('',(10.6305308945339,-3.76125149450632,12.));
#215423=CARTESIAN_POINT('Origin',(20.0645771135003,-9.02290115519382,0.));
#215424=CARTESIAN_POINT('',(19.84920021178,-9.47413589477549,0.));
#215425=CARTESIAN_POINT('',(19.6085639972844,-8.81783521984851,0.));
#215426=CARTESIAN_POINT('Origin',(20.0645771135003,-9.02290115519382,0.));
#215427=CARTESIAN_POINT('',(19.6085639972844,-8.81783521984851,12.));
#215428=CARTESIAN_POINT('',(19.6085639972844,-8.81783521984851,0.));
#215429=CARTESIAN_POINT('',(19.84920021178,-9.47413589477549,12.));
#215430=CARTESIAN_POINT('Origin',(20.0645771135003,-9.02290115519382,12.));
#215431=CARTESIAN_POINT('',(19.84920021178,-9.47413589477549,0.));
#215432=CARTESIAN_POINT('Origin',(7.08841632778409E-13,-3.26562511982935E-13,
0.));
#215433=CARTESIAN_POINT('Origin',(7.08841632778409E-13,-3.26562511982935E-13,
12.));
#215434=CARTESIAN_POINT('Origin',(7.08841632778409E-13,-3.26562511982935E-13,
0.));
#215435=CARTESIAN_POINT('Origin',(17.846350172984,-12.8649829188862,0.));
#215436=CARTESIAN_POINT('',(17.4407513054162,-12.572596943457,0.));
#215437=CARTESIAN_POINT('',(18.1294424696716,-12.4528436808172,0.));
#215438=CARTESIAN_POINT('Origin',(17.846350172984,-12.8649829188862,0.));
#215439=CARTESIAN_POINT('',(18.1294424696716,-12.4528436808172,12.));
#215440=CARTESIAN_POINT('',(18.1294424696716,-12.4528436808172,0.));
#215441=CARTESIAN_POINT('',(17.4407513054162,-12.572596943457,12.));
#215442=CARTESIAN_POINT('Origin',(17.846350172984,-12.8649829188862,12.));
#215443=CARTESIAN_POINT('',(17.4407513054162,-12.572596943457,0.));
#215444=CARTESIAN_POINT('Origin',(18.5896416359912,-12.7689476255363,0.));
#215445=CARTESIAN_POINT('',(18.5896416359912,-12.7689476255363,0.));
#215446=CARTESIAN_POINT('',(9.29482081799561,-6.38447381276812,0.));
#215447=CARTESIAN_POINT('',(18.5896416359912,-12.7689476255363,12.));
#215448=CARTESIAN_POINT('',(18.5896416359912,-12.7689476255363,0.));
#215449=CARTESIAN_POINT('',(9.29482081799561,-6.38447381276812,12.));
#215450=CARTESIAN_POINT('Origin',(17.0455945664569,-13.9085479427572,0.));
#215451=CARTESIAN_POINT('',(16.7207683102834,-14.2886635873976,0.));
#215452=CARTESIAN_POINT('',(16.6581946899465,-13.5924445804218,0.));
#215453=CARTESIAN_POINT('Origin',(17.0455945664569,-13.9085479427572,0.));
#215454=CARTESIAN_POINT('',(16.6581946899465,-13.5924445804218,12.));
#215455=CARTESIAN_POINT('',(16.6581946899465,-13.5924445804218,0.));
#215456=CARTESIAN_POINT('',(16.7207683102834,-14.2886635873976,12.));
#215457=CARTESIAN_POINT('Origin',(17.0455945664569,-13.9085479427572,12.));
#215458=CARTESIAN_POINT('',(16.7207683102834,-14.2886635873976,0.));
#215459=CARTESIAN_POINT('Origin',(6.00167842331873E-13,-4.9889687874677E-13,
0.));
#215460=CARTESIAN_POINT('Origin',(6.00167842331873E-13,-4.9889687874677E-13,
12.));
#215461=CARTESIAN_POINT('Origin',(6.00167842331873E-13,-4.9889687874677E-13,
0.));
#215462=CARTESIAN_POINT('Origin',(13.9085479427572,-17.0455945664569,0.));
#215463=CARTESIAN_POINT('',(13.5924445804218,-16.6581946899465,0.));
#215464=CARTESIAN_POINT('',(14.2886635873976,-16.7207683102834,0.));
#215465=CARTESIAN_POINT('Origin',(13.9085479427572,-17.0455945664569,0.));
#215466=CARTESIAN_POINT('',(14.2886635873976,-16.7207683102834,12.));
#215467=CARTESIAN_POINT('',(14.2886635873976,-16.7207683102834,0.));
#215468=CARTESIAN_POINT('',(13.5924445804218,-16.6581946899465,12.));
#215469=CARTESIAN_POINT('Origin',(13.9085479427572,-17.0455945664569,12.));
#215470=CARTESIAN_POINT('',(13.5924445804218,-16.6581946899465,0.));
#215471=CARTESIAN_POINT('Origin',(14.6513681262571,-17.1452095830633,0.));
#215472=CARTESIAN_POINT('',(14.6513681262571,-17.1452095830633,0.));
#215473=CARTESIAN_POINT('',(7.32568406312854,-8.57260479153162,0.));
#215474=CARTESIAN_POINT('',(14.6513681262571,-17.1452095830633,12.));
#215475=CARTESIAN_POINT('',(14.6513681262571,-17.1452095830633,0.));
#215476=CARTESIAN_POINT('',(7.32568406312854,-8.57260479153162,12.));
#215477=CARTESIAN_POINT('Origin',(12.8649829188862,-17.846350172984,0.));
#215478=CARTESIAN_POINT('',(12.4528436808172,-18.1294424696716,0.));
#215479=CARTESIAN_POINT('',(12.572596943457,-17.4407513054162,0.));
#215480=CARTESIAN_POINT('Origin',(12.8649829188862,-17.846350172984,0.));
#215481=CARTESIAN_POINT('',(12.572596943457,-17.4407513054162,12.));
#215482=CARTESIAN_POINT('',(12.572596943457,-17.4407513054162,0.));
#215483=CARTESIAN_POINT('',(12.4528436808172,-18.1294424696716,12.));
#215484=CARTESIAN_POINT('Origin',(12.8649829188862,-17.846350172984,12.));
#215485=CARTESIAN_POINT('',(12.4528436808172,-18.1294424696716,0.));
#215486=CARTESIAN_POINT('Origin',(4.50593605254674E-13,-6.37232247690087E-13,
0.));
#215487=CARTESIAN_POINT('Origin',(4.50593605254674E-13,-6.37232247690087E-13,
12.));
#215488=CARTESIAN_POINT('Origin',(4.50593605254674E-13,-6.37232247690087E-13,
0.));
#215489=CARTESIAN_POINT('Origin',(9.02290115519381,-20.0645771135004,0.));
#215490=CARTESIAN_POINT('',(8.81783521984849,-19.6085639972844,0.));
#215491=CARTESIAN_POINT('',(9.47413589477548,-19.84920021178,0.));
#215492=CARTESIAN_POINT('Origin',(9.02290115519381,-20.0645771135004,0.));
#215493=CARTESIAN_POINT('',(9.47413589477548,-19.84920021178,12.));
#215494=CARTESIAN_POINT('',(9.47413589477547,-19.84920021178,0.));
#215495=CARTESIAN_POINT('',(8.81783521984849,-19.6085639972844,12.));
#215496=CARTESIAN_POINT('Origin',(9.02290115519381,-20.0645771135004,12.));
#215497=CARTESIAN_POINT('',(8.81783521984849,-19.6085639972844,0.));
#215498=CARTESIAN_POINT('Origin',(9.71462809124915,-20.353053841303,0.));
#215499=CARTESIAN_POINT('',(9.71462809124915,-20.353053841303,0.));
#215500=CARTESIAN_POINT('',(4.85731404562459,-10.1765269206515,0.));
#215501=CARTESIAN_POINT('',(9.71462809124915,-20.353053841303,12.));
#215502=CARTESIAN_POINT('',(9.71462809124915,-20.353053841303,0.));
#215503=CARTESIAN_POINT('',(4.85731404562459,-10.1765269206515,12.));
#215504=CARTESIAN_POINT('Origin',(7.80764394578302,-20.56795313141,0.));
#215505=CARTESIAN_POINT('',(7.33627833380045,-20.7347298079577,0.));
#215506=CARTESIAN_POINT('',(7.63019749246977,-20.1004996511507,0.));
#215507=CARTESIAN_POINT('Origin',(7.80764394578302,-20.56795313141,0.));
#215508=CARTESIAN_POINT('',(7.63019749246977,-20.1004996511507,12.));
#215509=CARTESIAN_POINT('',(7.63019749246977,-20.1004996511507,0.));
#215510=CARTESIAN_POINT('',(7.33627833380045,-20.7347298079577,12.));
#215511=CARTESIAN_POINT('Origin',(7.80764394578302,-20.56795313141,12.));
#215512=CARTESIAN_POINT('',(7.33627833380045,-20.7347298079577,0.));
#215513=CARTESIAN_POINT('Origin',(2.70312158620511E-13,-7.32141292029404E-13,
0.));
#215514=CARTESIAN_POINT('Origin',(2.70312158620511E-13,-7.32141292029404E-13,
12.));
#215515=CARTESIAN_POINT('Origin',(2.70312158620511E-13,-7.32141292029404E-13,
0.));
#215516=CARTESIAN_POINT('Origin',(3.52235856495312,-21.7161918885403,0.));
#215517=CARTESIAN_POINT('',(3.44230496120418,-21.2226420728916,0.));
#215518=CARTESIAN_POINT('',(4.01396149767428,-21.624941921198,0.));
#215519=CARTESIAN_POINT('Origin',(3.52235856495312,-21.7161918885403,0.));
#215520=CARTESIAN_POINT('',(4.01396149767428,-21.624941921198,12.));
#215521=CARTESIAN_POINT('',(4.01396149767428,-21.624941921198,0.));
#215522=CARTESIAN_POINT('',(3.44230496120418,-21.2226420728916,12.));
#215523=CARTESIAN_POINT('Origin',(3.52235856495312,-21.7161918885403,12.));
#215524=CARTESIAN_POINT('',(3.44230496120418,-21.2226420728916,0.));
#215525=CARTESIAN_POINT('Origin',(4.11585220600461,-22.1738711152697,0.));
#215526=CARTESIAN_POINT('',(4.11585220600461,-22.1738711152697,0.));
#215527=CARTESIAN_POINT('',(2.05792610300232,-11.0869355576349,0.));
#215528=CARTESIAN_POINT('',(4.11585220600461,-22.1738711152697,12.));
#215529=CARTESIAN_POINT('',(4.11585220600461,-22.1738711152697,0.));
#215530=CARTESIAN_POINT('',(2.05792610300232,-11.0869355576349,12.));
#215531=CARTESIAN_POINT('Origin',(2.21822694051637,-21.8878840740801,0.));
#215532=CARTESIAN_POINT('',(1.71975774210841,-21.9269795755927,0.));
#215533=CARTESIAN_POINT('',(2.16781269186827,-21.3904321633055,0.));
#215534=CARTESIAN_POINT('Origin',(2.21822694051637,-21.8878840740801,0.));
#215535=CARTESIAN_POINT('',(2.16781269186827,-21.3904321633055,12.));
#215536=CARTESIAN_POINT('',(2.16781269186827,-21.3904321633055,0.));
#215537=CARTESIAN_POINT('',(1.71975774210841,-21.9269795755927,12.));
#215538=CARTESIAN_POINT('Origin',(2.21822694051637,-21.8878840740801,12.));
#215539=CARTESIAN_POINT('',(1.71975774210841,-21.9269795755927,0.));
#215540=CARTESIAN_POINT('Origin',(7.16093850883225E-14,-7.7715611723761E-13,
0.));
#215541=CARTESIAN_POINT('Origin',(7.16093850883225E-14,-7.7715611723761E-13,
12.));
#215542=CARTESIAN_POINT('Origin',(7.16093850883225E-14,-7.7715611723761E-13,
0.));
#215543=CARTESIAN_POINT('Origin',(-2.21822694051639,-21.88788407408,0.));
#215544=CARTESIAN_POINT('',(-2.16781269186829,-21.3904321633055,0.));
#215545=CARTESIAN_POINT('',(-1.71975774210843,-21.9269795755927,0.));
#215546=CARTESIAN_POINT('Origin',(-2.21822694051639,-21.88788407408,0.));
#215547=CARTESIAN_POINT('',(-1.71975774210843,-21.9269795755927,12.));
#215548=CARTESIAN_POINT('',(-1.71975774210843,-21.9269795755927,0.));
#215549=CARTESIAN_POINT('',(-2.16781269186829,-21.3904321633055,12.));
#215550=CARTESIAN_POINT('Origin',(-2.21822694051639,-21.88788407408,12.));
#215551=CARTESIAN_POINT('',(-2.16781269186829,-21.3904321633055,0.));
#215552=CARTESIAN_POINT('Origin',(-1.76341220531181,-22.4835757167854,0.));
#215553=CARTESIAN_POINT('',(-1.76341220531181,-22.4835757167854,0.));
#215554=CARTESIAN_POINT('',(-0.881706102655891,-11.2417878583927,0.));
#215555=CARTESIAN_POINT('',(-1.76341220531181,-22.4835757167854,12.));
#215556=CARTESIAN_POINT('',(-1.76341220531181,-22.4835757167854,0.));
#215557=CARTESIAN_POINT('',(-0.881706102655891,-11.2417878583927,12.));
#215558=CARTESIAN_POINT('Origin',(-3.52235856495314,-21.7161918885402,0.));
#215559=CARTESIAN_POINT('',(-4.0139614976743,-21.624941921198,0.));
#215560=CARTESIAN_POINT('',(-3.4423049612042,-21.2226420728916,0.));
#215561=CARTESIAN_POINT('Origin',(-3.52235856495314,-21.7161918885402,0.));
#215562=CARTESIAN_POINT('',(-3.4423049612042,-21.2226420728916,12.));
#215563=CARTESIAN_POINT('',(-3.4423049612042,-21.2226420728916,0.));
#215564=CARTESIAN_POINT('',(-4.0139614976743,-21.624941921198,12.));
#215565=CARTESIAN_POINT('Origin',(-3.52235856495314,-21.7161918885402,12.));
#215566=CARTESIAN_POINT('',(-4.0139614976743,-21.624941921198,0.));
#215567=CARTESIAN_POINT('Origin',(-1.31973449697531E-13,-7.6920903736728E-13,
0.));
#215568=CARTESIAN_POINT('Origin',(-1.31973449697531E-13,-7.6920903736728E-13,
12.));
#215569=CARTESIAN_POINT('Origin',(-1.31973449697531E-13,-7.6920903736728E-13,
0.));
#215570=CARTESIAN_POINT('Origin',(-7.80764394578304,-20.56795313141,0.));
#215571=CARTESIAN_POINT('',(-7.63019749246979,-20.1004996511507,0.));
#215572=CARTESIAN_POINT('',(-7.33627833380047,-20.7347298079577,0.));
#215573=CARTESIAN_POINT('Origin',(-7.80764394578304,-20.56795313141,0.));
#215574=CARTESIAN_POINT('',(-7.33627833380047,-20.7347298079577,12.));
#215575=CARTESIAN_POINT('',(-7.33627833380047,-20.7347298079577,0.));
#215576=CARTESIAN_POINT('',(-7.63019749246979,-20.1004996511507,12.));
#215577=CARTESIAN_POINT('Origin',(-7.80764394578304,-20.56795313141,12.));
#215578=CARTESIAN_POINT('',(-7.63019749246979,-20.1004996511507,0.));
#215579=CARTESIAN_POINT('Origin',(-7.52250298901266,-21.2610617890679,0.));
#215580=CARTESIAN_POINT('',(-7.52250298901266,-21.2610617890679,0.));
#215581=CARTESIAN_POINT('',(-3.76125149450632,-10.6305308945339,0.));
#215582=CARTESIAN_POINT('',(-7.52250298901266,-21.2610617890679,12.));
#215583=CARTESIAN_POINT('',(-7.52250298901266,-21.2610617890679,0.));
#215584=CARTESIAN_POINT('',(-3.76125149450632,-10.6305308945339,12.));
#215585=CARTESIAN_POINT('Origin',(-9.02290115519382,-20.0645771135003,0.));
#215586=CARTESIAN_POINT('',(-9.47413589477549,-19.84920021178,0.));
#215587=CARTESIAN_POINT('',(-8.81783521984851,-19.6085639972844,0.));
#215588=CARTESIAN_POINT('Origin',(-9.02290115519382,-20.0645771135003,0.));
#215589=CARTESIAN_POINT('',(-8.81783521984851,-19.6085639972844,12.));
#215590=CARTESIAN_POINT('',(-8.81783521984851,-19.6085639972844,0.));
#215591=CARTESIAN_POINT('',(-9.47413589477549,-19.84920021178,12.));
#215592=CARTESIAN_POINT('Origin',(-9.02290115519382,-20.0645771135003,12.));
#215593=CARTESIAN_POINT('',(-9.47413589477549,-19.84920021178,0.));
#215594=CARTESIAN_POINT('Origin',(-3.26562511982935E-13,-7.08841632778409E-13,
0.));
#215595=CARTESIAN_POINT('Origin',(-3.26562511982935E-13,-7.08841632778409E-13,
12.));
#215596=CARTESIAN_POINT('Origin',(-3.26562511982935E-13,-7.08841632778409E-13,
0.));
#215597=CARTESIAN_POINT('Origin',(-12.8649829188863,-17.846350172984,0.));
#215598=CARTESIAN_POINT('',(-12.572596943457,-17.4407513054161,0.));
#215599=CARTESIAN_POINT('',(-12.4528436808172,-18.1294424696716,0.));
#215600=CARTESIAN_POINT('Origin',(-12.8649829188863,-17.846350172984,0.));
#215601=CARTESIAN_POINT('',(-12.4528436808172,-18.1294424696716,12.));
#215602=CARTESIAN_POINT('',(-12.4528436808172,-18.1294424696716,0.));
#215603=CARTESIAN_POINT('',(-12.572596943457,-17.4407513054161,12.));
#215604=CARTESIAN_POINT('Origin',(-12.8649829188863,-17.846350172984,12.));
#215605=CARTESIAN_POINT('',(-12.572596943457,-17.4407513054161,0.));
#215606=CARTESIAN_POINT('Origin',(-12.7689476255363,-18.5896416359912,0.));
#215607=CARTESIAN_POINT('',(-12.7689476255363,-18.5896416359912,0.));
#215608=CARTESIAN_POINT('',(-6.38447381276812,-9.29482081799561,0.));
#215609=CARTESIAN_POINT('',(-12.7689476255363,-18.5896416359912,12.));
#215610=CARTESIAN_POINT('',(-12.7689476255363,-18.5896416359912,0.));
#215611=CARTESIAN_POINT('',(-6.38447381276812,-9.29482081799561,12.));
#215612=CARTESIAN_POINT('Origin',(-13.9085479427572,-17.0455945664569,0.));
#215613=CARTESIAN_POINT('',(-14.2886635873976,-16.7207683102834,0.));
#215614=CARTESIAN_POINT('',(-13.5924445804218,-16.6581946899465,0.));
#215615=CARTESIAN_POINT('Origin',(-13.9085479427572,-17.0455945664569,0.));
#215616=CARTESIAN_POINT('',(-13.5924445804218,-16.6581946899465,12.));
#215617=CARTESIAN_POINT('',(-13.5924445804218,-16.6581946899465,0.));
#215618=CARTESIAN_POINT('',(-14.2886635873976,-16.7207683102834,12.));
#215619=CARTESIAN_POINT('Origin',(-13.9085479427572,-17.0455945664569,12.));
#215620=CARTESIAN_POINT('',(-14.2886635873976,-16.7207683102834,0.));
#215621=CARTESIAN_POINT('Origin',(-4.9889687874677E-13,-6.00167842331873E-13,
0.));
#215622=CARTESIAN_POINT('Origin',(-4.9889687874677E-13,-6.00167842331873E-13,
12.));
#215623=CARTESIAN_POINT('Origin',(-4.9889687874677E-13,-6.00167842331873E-13,
0.));
#215624=CARTESIAN_POINT('Origin',(-17.0455945664569,-13.9085479427572,0.));
#215625=CARTESIAN_POINT('',(-16.6581946899465,-13.5924445804218,0.));
#215626=CARTESIAN_POINT('',(-16.7207683102834,-14.2886635873976,0.));
#215627=CARTESIAN_POINT('Origin',(-17.0455945664569,-13.9085479427572,0.));
#215628=CARTESIAN_POINT('',(-16.7207683102834,-14.2886635873976,12.));
#215629=CARTESIAN_POINT('',(-16.7207683102834,-14.2886635873976,0.));
#215630=CARTESIAN_POINT('',(-16.6581946899465,-13.5924445804218,12.));
#215631=CARTESIAN_POINT('Origin',(-17.0455945664569,-13.9085479427572,12.));
#215632=CARTESIAN_POINT('',(-16.6581946899465,-13.5924445804218,0.));
#215633=CARTESIAN_POINT('Origin',(-17.1452095830633,-14.6513681262571,0.));
#215634=CARTESIAN_POINT('',(-17.1452095830633,-14.6513681262571,0.));
#215635=CARTESIAN_POINT('',(-8.57260479153162,-7.32568406312855,0.));
#215636=CARTESIAN_POINT('',(-17.1452095830633,-14.6513681262571,12.));
#215637=CARTESIAN_POINT('',(-17.1452095830633,-14.6513681262571,0.));
#215638=CARTESIAN_POINT('',(-8.57260479153162,-7.32568406312855,12.));
#215639=CARTESIAN_POINT('Origin',(-17.846350172984,-12.8649829188862,0.));
#215640=CARTESIAN_POINT('',(-18.1294424696716,-12.4528436808172,0.));
#215641=CARTESIAN_POINT('',(-17.4407513054162,-12.572596943457,0.));
#215642=CARTESIAN_POINT('Origin',(-17.846350172984,-12.8649829188862,0.));
#215643=CARTESIAN_POINT('',(-17.4407513054162,-12.572596943457,12.));
#215644=CARTESIAN_POINT('',(-17.4407513054162,-12.572596943457,0.));
#215645=CARTESIAN_POINT('',(-18.1294424696716,-12.4528436808172,12.));
#215646=CARTESIAN_POINT('Origin',(-17.846350172984,-12.8649829188862,12.));
#215647=CARTESIAN_POINT('',(-18.1294424696716,-12.4528436808172,0.));
#215648=CARTESIAN_POINT('Origin',(-6.37232247690086E-13,-4.50593605254675E-13,
0.));
#215649=CARTESIAN_POINT('Origin',(-6.37232247690086E-13,-4.50593605254675E-13,
12.));
#215650=CARTESIAN_POINT('Origin',(-6.37232247690086E-13,-4.50593605254675E-13,
0.));
#215651=CARTESIAN_POINT('Origin',(-20.0645771135004,-9.0229011551938,0.));
#215652=CARTESIAN_POINT('',(-19.6085639972844,-8.81783521984849,0.));
#215653=CARTESIAN_POINT('',(-19.84920021178,-9.47413589477548,0.));
#215654=CARTESIAN_POINT('Origin',(-20.0645771135004,-9.0229011551938,0.));
#215655=CARTESIAN_POINT('',(-19.84920021178,-9.47413589477548,12.));
#215656=CARTESIAN_POINT('',(-19.84920021178,-9.47413589477547,0.));
#215657=CARTESIAN_POINT('',(-19.6085639972844,-8.81783521984849,12.));
#215658=CARTESIAN_POINT('Origin',(-20.0645771135004,-9.0229011551938,12.));
#215659=CARTESIAN_POINT('',(-19.6085639972844,-8.81783521984849,0.));
#215660=CARTESIAN_POINT('Origin',(-20.353053841303,-9.71462809124915,0.));
#215661=CARTESIAN_POINT('',(-20.353053841303,-9.71462809124915,0.));
#215662=CARTESIAN_POINT('',(-10.1765269206515,-4.85731404562459,0.));
#215663=CARTESIAN_POINT('',(-20.353053841303,-9.71462809124915,12.));
#215664=CARTESIAN_POINT('',(-20.353053841303,-9.71462809124915,0.));
#215665=CARTESIAN_POINT('',(-10.1765269206515,-4.85731404562459,12.));
#215666=CARTESIAN_POINT('Origin',(-20.56795313141,-7.80764394578302,0.));
#215667=CARTESIAN_POINT('',(-20.7347298079577,-7.33627833380045,0.));
#215668=CARTESIAN_POINT('',(-20.1004996511507,-7.63019749246977,0.));
#215669=CARTESIAN_POINT('Origin',(-20.56795313141,-7.80764394578302,0.));
#215670=CARTESIAN_POINT('',(-20.1004996511507,-7.63019749246977,12.));
#215671=CARTESIAN_POINT('',(-20.1004996511507,-7.63019749246977,0.));
#215672=CARTESIAN_POINT('',(-20.7347298079577,-7.33627833380045,12.));
#215673=CARTESIAN_POINT('Origin',(-20.56795313141,-7.80764394578302,12.));
#215674=CARTESIAN_POINT('',(-20.7347298079577,-7.33627833380045,0.));
#215675=CARTESIAN_POINT('Origin',(-7.32141292029404E-13,-2.70312158620511E-13,
0.));
#215676=CARTESIAN_POINT('Origin',(-7.32141292029404E-13,-2.70312158620511E-13,
12.));
#215677=CARTESIAN_POINT('Origin',(-7.32141292029404E-13,-2.70312158620511E-13,
0.));
#215678=CARTESIAN_POINT('Origin',(-21.7161918885403,-3.52235856495312,0.));
#215679=CARTESIAN_POINT('',(-21.2226420728916,-3.44230496120418,0.));
#215680=CARTESIAN_POINT('',(-21.624941921198,-4.01396149767428,0.));
#215681=CARTESIAN_POINT('Origin',(-21.7161918885403,-3.52235856495312,0.));
#215682=CARTESIAN_POINT('',(-21.624941921198,-4.01396149767428,12.));
#215683=CARTESIAN_POINT('',(-21.624941921198,-4.01396149767428,0.));
#215684=CARTESIAN_POINT('',(-21.2226420728916,-3.44230496120418,12.));
#215685=CARTESIAN_POINT('Origin',(-21.7161918885403,-3.52235856495312,12.));
#215686=CARTESIAN_POINT('',(-21.2226420728916,-3.44230496120418,0.));
#215687=CARTESIAN_POINT('Origin',(-22.1738711152697,-4.11585220600461,0.));
#215688=CARTESIAN_POINT('',(-22.1738711152697,-4.11585220600461,0.));
#215689=CARTESIAN_POINT('',(-11.0869355576349,-2.05792610300232,0.));
#215690=CARTESIAN_POINT('',(-22.1738711152697,-4.11585220600461,12.));
#215691=CARTESIAN_POINT('',(-22.1738711152697,-4.11585220600461,0.));
#215692=CARTESIAN_POINT('',(-11.0869355576349,-2.05792610300232,12.));
#215693=CARTESIAN_POINT('Origin',(-21.8878840740801,-2.21822694051637,0.));
#215694=CARTESIAN_POINT('',(-21.9269795755927,-1.71975774210841,0.));
#215695=CARTESIAN_POINT('',(-21.3904321633055,-2.16781269186828,0.));
#215696=CARTESIAN_POINT('Origin',(-21.8878840740801,-2.21822694051637,0.));
#215697=CARTESIAN_POINT('',(-21.3904321633055,-2.16781269186828,12.));
#215698=CARTESIAN_POINT('',(-21.3904321633055,-2.16781269186827,0.));
#215699=CARTESIAN_POINT('',(-21.9269795755927,-1.71975774210841,12.));
#215700=CARTESIAN_POINT('Origin',(-21.8878840740801,-2.21822694051637,12.));
#215701=CARTESIAN_POINT('',(-21.9269795755927,-1.71975774210841,0.));
#215702=CARTESIAN_POINT('Origin',(-7.7715611723761E-13,-7.16093850883225E-14,
0.));
#215703=CARTESIAN_POINT('Origin',(-7.7715611723761E-13,-7.16093850883225E-14,
12.));
#215704=CARTESIAN_POINT('Origin',(-7.7715611723761E-13,-7.16093850883225E-14,
0.));
#215705=CARTESIAN_POINT('Origin',(-21.8878840740801,2.21822694051638,0.));
#215706=CARTESIAN_POINT('',(-21.3904321633055,2.16781269186828,0.));
#215707=CARTESIAN_POINT('',(-21.9269795755927,1.71975774210842,0.));
#215708=CARTESIAN_POINT('Origin',(-21.8878840740801,2.21822694051638,0.));
#215709=CARTESIAN_POINT('',(-21.9269795755927,1.71975774210842,12.));
#215710=CARTESIAN_POINT('',(-21.9269795755927,1.71975774210842,0.));
#215711=CARTESIAN_POINT('',(-21.3904321633055,2.16781269186828,12.));
#215712=CARTESIAN_POINT('Origin',(-21.8878840740801,2.21822694051638,12.));
#215713=CARTESIAN_POINT('',(-21.3904321633055,2.16781269186828,0.));
#215714=CARTESIAN_POINT('Origin',(-22.4835757167854,1.7634122053118,0.));
#215715=CARTESIAN_POINT('',(-22.4835757167854,1.7634122053118,0.));
#215716=CARTESIAN_POINT('',(-11.2417878583927,0.881706102655883,0.));
#215717=CARTESIAN_POINT('',(-22.4835757167854,1.7634122053118,12.));
#215718=CARTESIAN_POINT('',(-22.4835757167854,1.7634122053118,0.));
#215719=CARTESIAN_POINT('',(-11.2417878583927,0.881706102655883,12.));
#215720=CARTESIAN_POINT('Origin',(-21.7161918885402,3.52235856495312,0.));
#215721=CARTESIAN_POINT('',(-21.624941921198,4.01396149767429,0.));
#215722=CARTESIAN_POINT('',(-21.2226420728916,3.44230496120419,0.));
#215723=CARTESIAN_POINT('Origin',(-21.7161918885402,3.52235856495312,0.));
#215724=CARTESIAN_POINT('',(-21.2226420728916,3.44230496120419,12.));
#215725=CARTESIAN_POINT('',(-21.2226420728916,3.44230496120419,0.));
#215726=CARTESIAN_POINT('',(-21.624941921198,4.01396149767429,12.));
#215727=CARTESIAN_POINT('Origin',(-21.7161918885402,3.52235856495312,12.));
#215728=CARTESIAN_POINT('',(-21.624941921198,4.01396149767429,0.));
#215729=CARTESIAN_POINT('Origin',(-7.6920903736728E-13,1.31973449697531E-13,
0.));
#215730=CARTESIAN_POINT('Origin',(-7.6920903736728E-13,1.31973449697531E-13,
12.));
#215731=CARTESIAN_POINT('Origin',(-7.6920903736728E-13,1.31973449697531E-13,
0.));
#215732=CARTESIAN_POINT('Origin',(-20.56795313141,7.80764394578303,0.));
#215733=CARTESIAN_POINT('',(-20.1004996511507,7.63019749246978,0.));
#215734=CARTESIAN_POINT('',(-20.7347298079577,7.33627833380047,0.));
#215735=CARTESIAN_POINT('Origin',(-20.56795313141,7.80764394578303,0.));
#215736=CARTESIAN_POINT('',(-20.7347298079577,7.33627833380047,12.));
#215737=CARTESIAN_POINT('',(-20.7347298079577,7.33627833380047,0.));
#215738=CARTESIAN_POINT('',(-20.1004996511507,7.63019749246978,12.));
#215739=CARTESIAN_POINT('Origin',(-20.56795313141,7.80764394578303,12.));
#215740=CARTESIAN_POINT('',(-20.1004996511507,7.63019749246978,0.));
#215741=CARTESIAN_POINT('Origin',(-21.2610617890679,7.52250298901265,0.));
#215742=CARTESIAN_POINT('',(-21.2610617890679,7.52250298901265,0.));
#215743=CARTESIAN_POINT('',(-10.6305308945339,3.76125149450631,0.));
#215744=CARTESIAN_POINT('',(-21.2610617890679,7.52250298901265,12.));
#215745=CARTESIAN_POINT('',(-21.2610617890679,7.52250298901265,0.));
#215746=CARTESIAN_POINT('',(-10.6305308945339,3.76125149450631,12.));
#215747=CARTESIAN_POINT('Origin',(-20.0645771135003,9.02290115519382,0.));
#215748=CARTESIAN_POINT('',(-19.84920021178,9.47413589477549,0.));
#215749=CARTESIAN_POINT('',(-19.6085639972844,8.81783521984851,0.));
#215750=CARTESIAN_POINT('Origin',(-20.0645771135003,9.02290115519382,0.));
#215751=CARTESIAN_POINT('',(-19.6085639972844,8.81783521984851,12.));
#215752=CARTESIAN_POINT('',(-19.6085639972844,8.81783521984851,0.));
#215753=CARTESIAN_POINT('',(-19.84920021178,9.47413589477549,12.));
#215754=CARTESIAN_POINT('Origin',(-20.0645771135003,9.02290115519382,12.));
#215755=CARTESIAN_POINT('',(-19.84920021178,9.47413589477549,0.));
#215756=CARTESIAN_POINT('Origin',(-7.08841632778408E-13,3.26562511982935E-13,
0.));
#215757=CARTESIAN_POINT('Origin',(-7.08841632778408E-13,3.26562511982935E-13,
12.));
#215758=CARTESIAN_POINT('Origin',(-7.08841632778408E-13,3.26562511982935E-13,
0.));
#215759=CARTESIAN_POINT('Origin',(-17.846350172984,12.8649829188862,0.));
#215760=CARTESIAN_POINT('',(-17.4407513054162,12.572596943457,0.));
#215761=CARTESIAN_POINT('',(-18.1294424696716,12.4528436808172,0.));
#215762=CARTESIAN_POINT('Origin',(-17.846350172984,12.8649829188862,0.));
#215763=CARTESIAN_POINT('',(-18.1294424696716,12.4528436808172,12.));
#215764=CARTESIAN_POINT('',(-18.1294424696716,12.4528436808172,0.));
#215765=CARTESIAN_POINT('',(-17.4407513054162,12.572596943457,12.));
#215766=CARTESIAN_POINT('Origin',(-17.846350172984,12.8649829188862,12.));
#215767=CARTESIAN_POINT('',(-17.4407513054162,12.572596943457,0.));
#215768=CARTESIAN_POINT('Origin',(-18.5896416359912,12.7689476255363,0.));
#215769=CARTESIAN_POINT('',(-18.5896416359912,12.7689476255363,0.));
#215770=CARTESIAN_POINT('',(-9.29482081799561,6.38447381276812,0.));
#215771=CARTESIAN_POINT('',(-18.5896416359912,12.7689476255363,12.));
#215772=CARTESIAN_POINT('',(-18.5896416359912,12.7689476255363,0.));
#215773=CARTESIAN_POINT('',(-9.29482081799561,6.38447381276812,12.));
#215774=CARTESIAN_POINT('Origin',(-17.0455945664569,13.9085479427572,0.));
#215775=CARTESIAN_POINT('',(-16.7207683102834,14.2886635873976,0.));
#215776=CARTESIAN_POINT('',(-16.6581946899465,13.5924445804218,0.));
#215777=CARTESIAN_POINT('Origin',(-17.0455945664569,13.9085479427572,0.));
#215778=CARTESIAN_POINT('',(-16.6581946899465,13.5924445804218,12.));
#215779=CARTESIAN_POINT('',(-16.6581946899465,13.5924445804218,0.));
#215780=CARTESIAN_POINT('',(-16.7207683102834,14.2886635873976,12.));
#215781=CARTESIAN_POINT('Origin',(-17.0455945664569,13.9085479427572,12.));
#215782=CARTESIAN_POINT('',(-16.7207683102834,14.2886635873976,0.));
#215783=CARTESIAN_POINT('Origin',(-6.00167842331873E-13,4.9889687874677E-13,
0.));
#215784=CARTESIAN_POINT('Origin',(-6.00167842331873E-13,4.9889687874677E-13,
12.));
#215785=CARTESIAN_POINT('Origin',(-6.00167842331873E-13,4.9889687874677E-13,
0.));
#215786=CARTESIAN_POINT('Origin',(-13.9085479427572,17.0455945664569,0.));
#215787=CARTESIAN_POINT('',(-13.5924445804218,16.6581946899465,0.));
#215788=CARTESIAN_POINT('',(-14.2886635873976,16.7207683102834,0.));
#215789=CARTESIAN_POINT('Origin',(-13.9085479427572,17.0455945664569,0.));
#215790=CARTESIAN_POINT('',(-14.2886635873976,16.7207683102834,12.));
#215791=CARTESIAN_POINT('',(-14.2886635873976,16.7207683102834,0.));
#215792=CARTESIAN_POINT('',(-13.5924445804218,16.6581946899465,12.));
#215793=CARTESIAN_POINT('Origin',(-13.9085479427572,17.0455945664569,12.));
#215794=CARTESIAN_POINT('',(-13.5924445804218,16.6581946899465,0.));
#215795=CARTESIAN_POINT('Origin',(-14.6513681262571,17.1452095830633,0.));
#215796=CARTESIAN_POINT('',(-14.6513681262571,17.1452095830633,0.));
#215797=CARTESIAN_POINT('',(-7.32568406312854,8.57260479153162,0.));
#215798=CARTESIAN_POINT('',(-14.6513681262571,17.1452095830633,12.));
#215799=CARTESIAN_POINT('',(-14.6513681262571,17.1452095830633,0.));
#215800=CARTESIAN_POINT('',(-7.32568406312854,8.57260479153162,12.));
#215801=CARTESIAN_POINT('Origin',(-12.8649829188862,17.846350172984,0.));
#215802=CARTESIAN_POINT('',(-12.4528436808172,18.1294424696716,0.));
#215803=CARTESIAN_POINT('',(-12.572596943457,17.4407513054162,0.));
#215804=CARTESIAN_POINT('Origin',(-12.8649829188862,17.846350172984,0.));
#215805=CARTESIAN_POINT('',(-12.572596943457,17.4407513054162,12.));
#215806=CARTESIAN_POINT('',(-12.572596943457,17.4407513054162,0.));
#215807=CARTESIAN_POINT('',(-12.4528436808172,18.1294424696716,12.));
#215808=CARTESIAN_POINT('Origin',(-12.8649829188862,17.846350172984,12.));
#215809=CARTESIAN_POINT('',(-12.4528436808172,18.1294424696716,0.));
#215810=CARTESIAN_POINT('Origin',(-4.50593605254675E-13,6.37232247690086E-13,
0.));
#215811=CARTESIAN_POINT('Origin',(-4.50593605254675E-13,6.37232247690086E-13,
12.));
#215812=CARTESIAN_POINT('Origin',(-4.50593605254675E-13,6.37232247690086E-13,
0.));
#215813=CARTESIAN_POINT('Origin',(-9.02290115519381,20.0645771135003,0.));
#215814=CARTESIAN_POINT('',(-8.8178352198485,19.6085639972844,0.));
#215815=CARTESIAN_POINT('',(-9.47413589477548,19.84920021178,0.));
#215816=CARTESIAN_POINT('Origin',(-9.02290115519381,20.0645771135003,0.));
#215817=CARTESIAN_POINT('',(-9.47413589477548,19.84920021178,12.));
#215818=CARTESIAN_POINT('',(-9.47413589477548,19.84920021178,0.));
#215819=CARTESIAN_POINT('',(-8.8178352198485,19.6085639972844,12.));
#215820=CARTESIAN_POINT('Origin',(-9.02290115519381,20.0645771135003,12.));
#215821=CARTESIAN_POINT('',(-8.8178352198485,19.6085639972844,0.));
#215822=CARTESIAN_POINT('Origin',(-9.71462809124916,20.353053841303,0.));
#215823=CARTESIAN_POINT('',(-9.71462809124916,20.353053841303,0.));
#215824=CARTESIAN_POINT('',(-4.85731404562459,10.1765269206515,0.));
#215825=CARTESIAN_POINT('',(-9.71462809124916,20.353053841303,12.));
#215826=CARTESIAN_POINT('',(-9.71462809124916,20.353053841303,0.));
#215827=CARTESIAN_POINT('',(-4.85731404562459,10.1765269206515,12.));
#215828=CARTESIAN_POINT('Origin',(-7.80764394578302,20.56795313141,0.));
#215829=CARTESIAN_POINT('',(-7.33627833380046,20.7347298079577,0.));
#215830=CARTESIAN_POINT('',(-7.63019749246977,20.1004996511507,0.));
#215831=CARTESIAN_POINT('Origin',(-7.80764394578302,20.56795313141,0.));
#215832=CARTESIAN_POINT('',(-7.63019749246977,20.1004996511507,12.));
#215833=CARTESIAN_POINT('',(-7.63019749246977,20.1004996511507,0.));
#215834=CARTESIAN_POINT('',(-7.33627833380046,20.7347298079577,12.));
#215835=CARTESIAN_POINT('Origin',(-7.80764394578302,20.56795313141,12.));
#215836=CARTESIAN_POINT('',(-7.33627833380046,20.7347298079577,0.));
#215837=CARTESIAN_POINT('Origin',(-2.70312158620511E-13,7.32141292029404E-13,
0.));
#215838=CARTESIAN_POINT('Origin',(-2.70312158620511E-13,7.32141292029404E-13,
12.));
#215839=CARTESIAN_POINT('Origin',(-2.70312158620511E-13,7.32141292029404E-13,
0.));
#215840=CARTESIAN_POINT('Origin',(-3.52235856495312,21.7161918885402,0.));
#215841=CARTESIAN_POINT('',(-3.44230496120418,21.2226420728916,0.));
#215842=CARTESIAN_POINT('',(-4.01396149767428,21.624941921198,0.));
#215843=CARTESIAN_POINT('Origin',(-3.52235856495312,21.7161918885402,0.));
#215844=CARTESIAN_POINT('',(-4.01396149767428,21.624941921198,12.));
#215845=CARTESIAN_POINT('',(-4.01396149767428,21.624941921198,0.));
#215846=CARTESIAN_POINT('',(-3.44230496120418,21.2226420728916,12.));
#215847=CARTESIAN_POINT('Origin',(-3.52235856495312,21.7161918885402,12.));
#215848=CARTESIAN_POINT('',(-3.44230496120418,21.2226420728916,0.));
#215849=CARTESIAN_POINT('Origin',(-4.11585220600461,22.1738711152697,0.));
#215850=CARTESIAN_POINT('',(-4.11585220600461,22.1738711152697,0.));
#215851=CARTESIAN_POINT('',(-2.05792610300232,11.0869355576349,0.));
#215852=CARTESIAN_POINT('',(-4.11585220600461,22.1738711152697,12.));
#215853=CARTESIAN_POINT('',(-4.11585220600461,22.1738711152697,0.));
#215854=CARTESIAN_POINT('',(-2.05792610300232,11.0869355576349,12.));
#215855=CARTESIAN_POINT('Origin',(-2.21822694051637,21.8878840740801,0.));
#215856=CARTESIAN_POINT('',(-1.71975774210841,21.9269795755927,0.));
#215857=CARTESIAN_POINT('',(-2.16781269186828,21.3904321633055,0.));
#215858=CARTESIAN_POINT('Origin',(-2.21822694051637,21.8878840740801,0.));
#215859=CARTESIAN_POINT('',(-2.16781269186828,21.3904321633055,12.));
#215860=CARTESIAN_POINT('',(-2.16781269186828,21.3904321633055,0.));
#215861=CARTESIAN_POINT('',(-1.71975774210841,21.9269795755927,12.));
#215862=CARTESIAN_POINT('Origin',(-2.21822694051637,21.8878840740801,12.));
#215863=CARTESIAN_POINT('',(-1.71975774210841,21.9269795755927,0.));
#215864=CARTESIAN_POINT('Origin',(-7.16093850883226E-14,7.7715611723761E-13,
0.));
#215865=CARTESIAN_POINT('Origin',(-7.16093850883226E-14,7.7715611723761E-13,
12.));
#215866=CARTESIAN_POINT('Origin',(-7.16093850883226E-14,7.7715611723761E-13,
0.));
#215867=CARTESIAN_POINT('Origin',(2.21822694051638,21.8878840740801,0.));
#215868=CARTESIAN_POINT('',(2.16781269186828,21.3904321633055,0.));
#215869=CARTESIAN_POINT('',(1.71975774210842,21.9269795755927,0.));
#215870=CARTESIAN_POINT('Origin',(2.21822694051638,21.8878840740801,0.));
#215871=CARTESIAN_POINT('',(1.71975774210842,21.9269795755927,12.));
#215872=CARTESIAN_POINT('',(1.71975774210842,21.9269795755927,0.));
#215873=CARTESIAN_POINT('',(2.16781269186828,21.3904321633055,12.));
#215874=CARTESIAN_POINT('Origin',(2.21822694051638,21.8878840740801,12.));
#215875=CARTESIAN_POINT('',(2.16781269186828,21.3904321633055,0.));
#215876=CARTESIAN_POINT('Origin',(1.7634122053118,22.4835757167854,0.));
#215877=CARTESIAN_POINT('',(1.7634122053118,22.4835757167854,0.));
#215878=CARTESIAN_POINT('',(0.881706102655883,11.2417878583927,0.));
#215879=CARTESIAN_POINT('',(1.7634122053118,22.4835757167854,12.));
#215880=CARTESIAN_POINT('',(1.7634122053118,22.4835757167854,0.));
#215881=CARTESIAN_POINT('',(0.881706102655883,11.2417878583927,12.));
#215882=CARTESIAN_POINT('Origin',(3.52235856495312,21.7161918885402,0.));
#215883=CARTESIAN_POINT('',(4.01396149767429,21.624941921198,0.));
#215884=CARTESIAN_POINT('',(3.44230496120419,21.2226420728916,0.));
#215885=CARTESIAN_POINT('Origin',(3.52235856495312,21.7161918885402,0.));
#215886=CARTESIAN_POINT('',(3.44230496120419,21.2226420728916,12.));
#215887=CARTESIAN_POINT('',(3.44230496120419,21.2226420728916,0.));
#215888=CARTESIAN_POINT('',(4.01396149767429,21.624941921198,12.));
#215889=CARTESIAN_POINT('Origin',(3.52235856495312,21.7161918885402,12.));
#215890=CARTESIAN_POINT('',(4.01396149767429,21.624941921198,0.));
#215891=CARTESIAN_POINT('Origin',(1.31973449697531E-13,7.6920903736728E-13,
0.));
#215892=CARTESIAN_POINT('Origin',(1.31973449697531E-13,7.6920903736728E-13,
12.));
#215893=CARTESIAN_POINT('Origin',(1.31973449697531E-13,7.6920903736728E-13,
0.));
#215894=CARTESIAN_POINT('Origin',(7.80764394578303,20.56795313141,0.));
#215895=CARTESIAN_POINT('',(7.63019749246978,20.1004996511507,0.));
#215896=CARTESIAN_POINT('',(7.33627833380047,20.7347298079577,0.));
#215897=CARTESIAN_POINT('Origin',(7.80764394578303,20.56795313141,0.));
#215898=CARTESIAN_POINT('',(7.33627833380047,20.7347298079577,12.));
#215899=CARTESIAN_POINT('',(7.33627833380046,20.7347298079577,0.));
#215900=CARTESIAN_POINT('',(7.63019749246978,20.1004996511507,12.));
#215901=CARTESIAN_POINT('Origin',(7.80764394578303,20.56795313141,12.));
#215902=CARTESIAN_POINT('',(7.63019749246978,20.1004996511507,0.));
#215903=CARTESIAN_POINT('Origin',(7.52250298901265,21.2610617890679,0.));
#215904=CARTESIAN_POINT('',(7.52250298901265,21.2610617890679,0.));
#215905=CARTESIAN_POINT('',(3.76125149450631,10.6305308945339,0.));
#215906=CARTESIAN_POINT('',(7.52250298901265,21.2610617890679,12.));
#215907=CARTESIAN_POINT('',(7.52250298901265,21.2610617890679,0.));
#215908=CARTESIAN_POINT('',(3.76125149450631,10.6305308945339,12.));
#215909=CARTESIAN_POINT('Origin',(9.02290115519382,20.0645771135003,0.));
#215910=CARTESIAN_POINT('',(9.47413589477549,19.84920021178,0.));
#215911=CARTESIAN_POINT('',(8.8178352198485,19.6085639972844,0.));
#215912=CARTESIAN_POINT('Origin',(9.02290115519382,20.0645771135003,0.));
#215913=CARTESIAN_POINT('',(8.8178352198485,19.6085639972844,12.));
#215914=CARTESIAN_POINT('',(8.8178352198485,19.6085639972844,0.));
#215915=CARTESIAN_POINT('',(9.47413589477549,19.84920021178,12.));
#215916=CARTESIAN_POINT('Origin',(9.02290115519382,20.0645771135003,12.));
#215917=CARTESIAN_POINT('',(9.47413589477549,19.84920021178,0.));
#215918=CARTESIAN_POINT('Origin',(3.26562511982935E-13,7.08841632778409E-13,
0.));
#215919=CARTESIAN_POINT('Origin',(3.26562511982935E-13,7.08841632778409E-13,
12.));
#215920=CARTESIAN_POINT('Origin',(3.26562511982935E-13,7.08841632778409E-13,
0.));
#215921=CARTESIAN_POINT('Origin',(12.8649829188862,17.846350172984,0.));
#215922=CARTESIAN_POINT('',(12.572596943457,17.4407513054162,0.));
#215923=CARTESIAN_POINT('',(12.4528436808172,18.1294424696716,0.));
#215924=CARTESIAN_POINT('Origin',(12.8649829188862,17.846350172984,0.));
#215925=CARTESIAN_POINT('',(12.4528436808172,18.1294424696716,12.));
#215926=CARTESIAN_POINT('',(12.4528436808172,18.1294424696716,0.));
#215927=CARTESIAN_POINT('',(12.572596943457,17.4407513054162,12.));
#215928=CARTESIAN_POINT('Origin',(12.8649829188862,17.846350172984,12.));
#215929=CARTESIAN_POINT('',(12.572596943457,17.4407513054162,0.));
#215930=CARTESIAN_POINT('Origin',(12.7689476255363,18.5896416359912,0.));
#215931=CARTESIAN_POINT('',(12.7689476255363,18.5896416359912,0.));
#215932=CARTESIAN_POINT('',(6.38447381276812,9.29482081799561,0.));
#215933=CARTESIAN_POINT('',(12.7689476255363,18.5896416359912,12.));
#215934=CARTESIAN_POINT('',(12.7689476255363,18.5896416359912,0.));
#215935=CARTESIAN_POINT('',(6.38447381276812,9.29482081799561,12.));
#215936=CARTESIAN_POINT('Origin',(13.9085479427572,17.0455945664569,0.));
#215937=CARTESIAN_POINT('',(14.2886635873976,16.7207683102834,0.));
#215938=CARTESIAN_POINT('',(13.5924445804218,16.6581946899465,0.));
#215939=CARTESIAN_POINT('Origin',(13.9085479427572,17.0455945664569,0.));
#215940=CARTESIAN_POINT('',(13.5924445804218,16.6581946899465,12.));
#215941=CARTESIAN_POINT('',(13.5924445804218,16.6581946899465,0.));
#215942=CARTESIAN_POINT('',(14.2886635873976,16.7207683102834,12.));
#215943=CARTESIAN_POINT('Origin',(13.9085479427572,17.0455945664569,12.));
#215944=CARTESIAN_POINT('',(14.2886635873976,16.7207683102834,0.));
#215945=CARTESIAN_POINT('Origin',(4.9889687874677E-13,6.00167842331873E-13,
0.));
#215946=CARTESIAN_POINT('Origin',(4.9889687874677E-13,6.00167842331873E-13,
12.));
#215947=CARTESIAN_POINT('Origin',(4.9889687874677E-13,6.00167842331873E-13,
0.));
#215948=CARTESIAN_POINT('Origin',(17.0455945664569,13.9085479427572,0.));
#215949=CARTESIAN_POINT('',(16.6581946899465,13.5924445804218,0.));
#215950=CARTESIAN_POINT('',(16.7207683102834,14.2886635873976,0.));
#215951=CARTESIAN_POINT('Origin',(17.0455945664569,13.9085479427572,0.));
#215952=CARTESIAN_POINT('',(16.7207683102834,14.2886635873976,12.));
#215953=CARTESIAN_POINT('',(16.7207683102834,14.2886635873976,0.));
#215954=CARTESIAN_POINT('',(16.6581946899465,13.5924445804218,12.));
#215955=CARTESIAN_POINT('Origin',(17.0455945664569,13.9085479427572,12.));
#215956=CARTESIAN_POINT('',(16.6581946899465,13.5924445804218,0.));
#215957=CARTESIAN_POINT('Origin',(17.1452095830633,14.6513681262571,0.));
#215958=CARTESIAN_POINT('',(17.1452095830633,14.6513681262571,0.));
#215959=CARTESIAN_POINT('',(8.57260479153162,7.32568406312855,0.));
#215960=CARTESIAN_POINT('',(17.1452095830633,14.6513681262571,12.));
#215961=CARTESIAN_POINT('',(17.1452095830633,14.6513681262571,0.));
#215962=CARTESIAN_POINT('',(8.57260479153162,7.32568406312855,12.));
#215963=CARTESIAN_POINT('Origin',(17.846350172984,12.8649829188862,0.));
#215964=CARTESIAN_POINT('',(18.1294424696716,12.4528436808172,0.));
#215965=CARTESIAN_POINT('',(17.4407513054162,12.572596943457,0.));
#215966=CARTESIAN_POINT('Origin',(17.846350172984,12.8649829188862,0.));
#215967=CARTESIAN_POINT('',(17.4407513054162,12.572596943457,12.));
#215968=CARTESIAN_POINT('',(17.4407513054162,12.572596943457,0.));
#215969=CARTESIAN_POINT('',(18.1294424696716,12.4528436808172,12.));
#215970=CARTESIAN_POINT('Origin',(17.846350172984,12.8649829188862,12.));
#215971=CARTESIAN_POINT('',(18.1294424696716,12.4528436808172,0.));
#215972=CARTESIAN_POINT('Origin',(6.37232247690086E-13,4.50593605254675E-13,
0.));
#215973=CARTESIAN_POINT('Origin',(6.37232247690086E-13,4.50593605254675E-13,
12.));
#215974=CARTESIAN_POINT('Origin',(6.37232247690086E-13,4.50593605254675E-13,
0.));
#215975=CARTESIAN_POINT('Origin',(20.0645771135003,9.02290115519381,0.));
#215976=CARTESIAN_POINT('',(19.6085639972844,8.8178352198485,0.));
#215977=CARTESIAN_POINT('',(19.84920021178,9.47413589477548,0.));
#215978=CARTESIAN_POINT('Origin',(20.0645771135003,9.02290115519381,0.));
#215979=CARTESIAN_POINT('',(19.84920021178,9.47413589477548,12.));
#215980=CARTESIAN_POINT('',(19.84920021178,9.47413589477548,0.));
#215981=CARTESIAN_POINT('',(19.6085639972844,8.8178352198485,12.));
#215982=CARTESIAN_POINT('Origin',(20.0645771135003,9.02290115519381,12.));
#215983=CARTESIAN_POINT('',(19.6085639972844,8.8178352198485,0.));
#215984=CARTESIAN_POINT('Origin',(20.353053841303,9.71462809124916,0.));
#215985=CARTESIAN_POINT('',(20.353053841303,9.71462809124916,0.));
#215986=CARTESIAN_POINT('',(10.1765269206515,4.85731404562459,0.));
#215987=CARTESIAN_POINT('',(20.353053841303,9.71462809124916,12.));
#215988=CARTESIAN_POINT('',(20.353053841303,9.71462809124916,0.));
#215989=CARTESIAN_POINT('',(10.1765269206515,4.85731404562459,12.));
#215990=CARTESIAN_POINT('Origin',(20.56795313141,7.80764394578302,0.));
#215991=CARTESIAN_POINT('',(20.7347298079577,7.33627833380046,0.));
#215992=CARTESIAN_POINT('',(20.1004996511507,7.63019749246977,0.));
#215993=CARTESIAN_POINT('Origin',(20.56795313141,7.80764394578302,0.));
#215994=CARTESIAN_POINT('',(20.1004996511507,7.63019749246977,12.));
#215995=CARTESIAN_POINT('',(20.1004996511507,7.63019749246977,0.));
#215996=CARTESIAN_POINT('',(20.7347298079577,7.33627833380046,12.));
#215997=CARTESIAN_POINT('Origin',(20.56795313141,7.80764394578302,12.));
#215998=CARTESIAN_POINT('',(20.7347298079577,7.33627833380046,0.));
#215999=CARTESIAN_POINT('Origin',(7.32141292029404E-13,2.70312158620511E-13,
0.));
#216000=CARTESIAN_POINT('Origin',(7.32141292029404E-13,2.70312158620511E-13,
12.));
#216001=CARTESIAN_POINT('Origin',(7.32141292029404E-13,2.70312158620511E-13,
0.));
#216002=CARTESIAN_POINT('Origin',(21.1389261070099,-3.92374859571502,0.));
#216003=CARTESIAN_POINT('',(22.1738711152697,-4.11585220600463,12.));
#216004=CARTESIAN_POINT('',(10.5694630535049,-1.96187429785751,12.));
#216005=CARTESIAN_POINT('',(22.1738711152697,-4.11585220600463,0.));
#216006=CARTESIAN_POINT('',(22.1738711152697,-4.11585220600463,0.));
#216007=CARTESIAN_POINT('',(10.5694630535049,-1.96187429785751,0.));
#216008=CARTESIAN_POINT('Ctrl Pts',(25.991588367311,-0.661312440730916,
0.));
#216009=CARTESIAN_POINT('Ctrl Pts',(25.991588367311,-0.661312440730916,
12.));
#216010=CARTESIAN_POINT('Ctrl Pts',(25.9865613464773,-0.66402831318764,
0.));
#216011=CARTESIAN_POINT('Ctrl Pts',(25.9865613464773,-0.66402831318764,
12.));
#216012=CARTESIAN_POINT('Ctrl Pts',(25.9765104298071,-0.669451306780839,
0.));
#216013=CARTESIAN_POINT('Ctrl Pts',(25.9765104298071,-0.669451306780839,
12.));
#216014=CARTESIAN_POINT('Ctrl Pts',(25.9614434297919,-0.67755954320974,
0.));
#216015=CARTESIAN_POINT('Ctrl Pts',(25.9614434297919,-0.67755954320974,
12.));
#216016=CARTESIAN_POINT('Ctrl Pts',(25.9413728471909,-0.688318015057744,
0.));
#216017=CARTESIAN_POINT('Ctrl Pts',(25.9413728471909,-0.688318015057744,
12.));
#216018=CARTESIAN_POINT('Ctrl Pts',(25.9163158909426,-0.701678575228769,
0.));
#216019=CARTESIAN_POINT('Ctrl Pts',(25.9163158909426,-0.701678575228769,
12.));
#216020=CARTESIAN_POINT('Ctrl Pts',(25.8912902614969,-0.714951588527653,
0.));
#216021=CARTESIAN_POINT('Ctrl Pts',(25.8912902614969,-0.714951588527653,
12.));
#216022=CARTESIAN_POINT('Ctrl Pts',(25.8662960624185,-0.728137036482349,
0.));
#216023=CARTESIAN_POINT('Ctrl Pts',(25.8662960624185,-0.728137036482349,
12.));
#216024=CARTESIAN_POINT('Ctrl Pts',(25.8413334619054,-0.74123490266382,
0.));
#216025=CARTESIAN_POINT('Ctrl Pts',(25.8413334619054,-0.74123490266382,
12.));
#216026=CARTESIAN_POINT('Ctrl Pts',(25.8164027059984,-0.754245175609537,
0.));
#216027=CARTESIAN_POINT('Ctrl Pts',(25.8164027059984,-0.754245175609537,
12.));
#216028=CARTESIAN_POINT('Ctrl Pts',(25.7915041383376,-0.767167852651183,
0.));
#216029=CARTESIAN_POINT('Ctrl Pts',(25.7915041383376,-0.767167852651183,
12.));
#216030=CARTESIAN_POINT('Ctrl Pts',(25.7666381946955,-0.780002940291977,
0.));
#216031=CARTESIAN_POINT('Ctrl Pts',(25.7666381946955,-0.780002940291977,
12.));
#216032=CARTESIAN_POINT('Ctrl Pts',(25.7418053757746,-0.79275045161614,
0.));
#216033=CARTESIAN_POINT('Ctrl Pts',(25.7418053757746,-0.79275045161614,
12.));
#216034=CARTESIAN_POINT('Ctrl Pts',(25.7170062262525,-0.805410404554366,
0.));
#216035=CARTESIAN_POINT('Ctrl Pts',(25.7170062262525,-0.805410404554366,
12.));
#216036=CARTESIAN_POINT('Ctrl Pts',(25.6922413110194,-0.817982819787478,
0.));
#216037=CARTESIAN_POINT('Ctrl Pts',(25.6922413110194,-0.817982819787478,
12.));
#216038=CARTESIAN_POINT('Ctrl Pts',(25.6675111931952,-0.830467718864221,
0.));
#216039=CARTESIAN_POINT('Ctrl Pts',(25.6675111931952,-0.830467718864221,
12.));
#216040=CARTESIAN_POINT('Ctrl Pts',(25.6428164100055,-0.842865122120773,
0.));
#216041=CARTESIAN_POINT('Ctrl Pts',(25.6428164100055,-0.842865122120773,
12.));
#216042=CARTESIAN_POINT('Ctrl Pts',(25.6181574536049,-0.855175047036563,
0.));
#216043=CARTESIAN_POINT('Ctrl Pts',(25.6181574536049,-0.855175047036563,
12.));
#216044=CARTESIAN_POINT('Ctrl Pts',(25.5935347843585,-0.867397509338443,
0.));
#216045=CARTESIAN_POINT('Ctrl Pts',(25.5935347843585,-0.867397509338443,
12.));
#216046=CARTESIAN_POINT('Ctrl Pts',(25.5689488408156,-0.879532523834308,
0.));
#216047=CARTESIAN_POINT('Ctrl Pts',(25.5689488408156,-0.879532523834308,
12.));
#216048=CARTESIAN_POINT('Ctrl Pts',(25.5444000508211,-0.891580105349052,
0.));
#216049=CARTESIAN_POINT('Ctrl Pts',(25.5444000508211,-0.891580105349052,
12.));
#216050=CARTESIAN_POINT('Ctrl Pts',(25.5198888424194,-0.903540269651121,
0.));
#216051=CARTESIAN_POINT('Ctrl Pts',(25.5198888424194,-0.903540269651121,
12.));
#216052=CARTESIAN_POINT('Ctrl Pts',(25.4954156541795,-0.915413034335626,
0.));
#216053=CARTESIAN_POINT('Ctrl Pts',(25.4954156541795,-0.915413034335626,
12.));
#216054=CARTESIAN_POINT('Ctrl Pts',(25.4709809475009,-0.927198419886108,
0.));
#216055=CARTESIAN_POINT('Ctrl Pts',(25.4709809475009,-0.927198419886108,
12.));
#216056=CARTESIAN_POINT('Ctrl Pts',(25.4465852044849,-0.938896449496205,
0.));
#216057=CARTESIAN_POINT('Ctrl Pts',(25.4465852044849,-0.938896449496205,
12.));
#216058=CARTESIAN_POINT('Ctrl Pts',(25.4222289223167,-0.950507148597483,
0.));
#216059=CARTESIAN_POINT('Ctrl Pts',(25.4222289223167,-0.950507148597483,
12.));
#216060=CARTESIAN_POINT('Ctrl Pts',(25.3979126089163,-0.962030544503156,
0.));
#216061=CARTESIAN_POINT('Ctrl Pts',(25.3979126089163,-0.962030544503156,
12.));
#216062=CARTESIAN_POINT('Ctrl Pts',(25.3736367778845,-0.973466666000178,
0.));
#216063=CARTESIAN_POINT('Ctrl Pts',(25.3736367778845,-0.973466666000178,
12.));
#216064=CARTESIAN_POINT('Ctrl Pts',(25.3494019441441,-0.984815543003986,
0.));
#216065=CARTESIAN_POINT('Ctrl Pts',(25.3494019441441,-0.984815543003986,
12.));
#216066=CARTESIAN_POINT('Ctrl Pts',(25.3252086182968,-0.996077206120637,
0.));
#216067=CARTESIAN_POINT('Ctrl Pts',(25.3252086182968,-0.996077206120637,
12.));
#216068=CARTESIAN_POINT('Ctrl Pts',(25.3010573055547,-1.00725168656897,
0.));
#216069=CARTESIAN_POINT('Ctrl Pts',(25.3010573055547,-1.00725168656897,
12.));
#216070=CARTESIAN_POINT('Ctrl Pts',(25.276948508726,-1.01833901642238,0.));
#216071=CARTESIAN_POINT('Ctrl Pts',(25.276948508726,-1.01833901642238,12.));
#216072=CARTESIAN_POINT('Ctrl Pts',(25.2528827300422,-1.02933922876807,
0.));
#216073=CARTESIAN_POINT('Ctrl Pts',(25.2528827300422,-1.02933922876807,
12.));
#216074=CARTESIAN_POINT('Ctrl Pts',(25.2288604735086,-1.04025235791508,
0.));
#216075=CARTESIAN_POINT('Ctrl Pts',(25.2288604735086,-1.04025235791508,
12.));
#216076=CARTESIAN_POINT('Ctrl Pts',(25.2048822469028,-1.05107843957933,
0.));
#216077=CARTESIAN_POINT('Ctrl Pts',(25.2048822469028,-1.05107843957933,
12.));
#216078=CARTESIAN_POINT('Ctrl Pts',(25.1809485642192,-1.06181751111769,
0.));
#216079=CARTESIAN_POINT('Ctrl Pts',(25.1809485642192,-1.06181751111769,
12.));
#216080=CARTESIAN_POINT('Ctrl Pts',(25.157059946931,-1.07246961165477,0.));
#216081=CARTESIAN_POINT('Ctrl Pts',(25.157059946931,-1.07246961165477,12.));
#216082=CARTESIAN_POINT('Ctrl Pts',(25.1332169227413,-1.08303478197189,
0.));
#216083=CARTESIAN_POINT('Ctrl Pts',(25.1332169227413,-1.08303478197189,
12.));
#216084=CARTESIAN_POINT('Ctrl Pts',(25.1094200248446,-1.09351306445309,
0.));
#216085=CARTESIAN_POINT('Ctrl Pts',(25.1094200248446,-1.09351306445309,
12.));
#216086=CARTESIAN_POINT('Ctrl Pts',(25.0856697909679,-1.10390450301747,
0.));
#216087=CARTESIAN_POINT('Ctrl Pts',(25.0856697909679,-1.10390450301747,
12.));
#216088=CARTESIAN_POINT('Ctrl Pts',(25.0619667625336,-1.11420914306891,
0.));
#216089=CARTESIAN_POINT('Ctrl Pts',(25.0619667625336,-1.11420914306891,
12.));
#216090=CARTESIAN_POINT('Ctrl Pts',(25.0383114836899,-1.12442703144453,
0.));
#216091=CARTESIAN_POINT('Ctrl Pts',(25.0383114836899,-1.12442703144453,
12.));
#216092=CARTESIAN_POINT('Ctrl Pts',(25.0147045006195,-1.13455821638531,
0.));
#216093=CARTESIAN_POINT('Ctrl Pts',(25.0147045006195,-1.13455821638531,
12.));
#216094=CARTESIAN_POINT('Ctrl Pts',(24.9911463621433,-1.14460274758202,
0.));
#216095=CARTESIAN_POINT('Ctrl Pts',(24.9911463621433,-1.14460274758202,
12.));
#216096=CARTESIAN_POINT('Ctrl Pts',(24.9676376201502,-1.15456067621891,
0.));
#216097=CARTESIAN_POINT('Ctrl Pts',(24.9676376201502,-1.15456067621891,
12.));
#216098=CARTESIAN_POINT('Ctrl Pts',(24.9441788300932,-1.16443205502851,
0.));
#216099=CARTESIAN_POINT('Ctrl Pts',(24.9441788300932,-1.16443205502851,
12.));
#216100=CARTESIAN_POINT('Ctrl Pts',(24.9207705514448,-1.17421693835042,
0.));
#216101=CARTESIAN_POINT('Ctrl Pts',(24.9207705514448,-1.17421693835042,
12.));
#216102=CARTESIAN_POINT('Ctrl Pts',(24.8974133481829,-1.18391538220104,
0.));
#216103=CARTESIAN_POINT('Ctrl Pts',(24.8974133481829,-1.18391538220104,
12.));
#216104=CARTESIAN_POINT('Ctrl Pts',(24.8741077892075,-1.19352744434066,
0.));
#216105=CARTESIAN_POINT('Ctrl Pts',(24.8741077892075,-1.19352744434066,
12.));
#216106=CARTESIAN_POINT('Ctrl Pts',(24.8508544481974,-1.20305318426021,
0.));
#216107=CARTESIAN_POINT('Ctrl Pts',(24.8508544481974,-1.20305318426021,
12.));
#216108=CARTESIAN_POINT('Ctrl Pts',(24.8276539035092,-1.21249266318209,
0.));
#216109=CARTESIAN_POINT('Ctrl Pts',(24.8276539035092,-1.21249266318209,
12.));
#216110=CARTESIAN_POINT('Ctrl Pts',(24.8045067380536,-1.22184594406529,
0.));
#216111=CARTESIAN_POINT('Ctrl Pts',(24.8045067380536,-1.22184594406529,
12.));
#216112=CARTESIAN_POINT('Ctrl Pts',(24.7814135391799,-1.23111309161845,
0.));
#216113=CARTESIAN_POINT('Ctrl Pts',(24.7814135391799,-1.23111309161845,
12.));
#216114=CARTESIAN_POINT('Ctrl Pts',(24.7583748985438,-1.2402941723199,0.));
#216115=CARTESIAN_POINT('Ctrl Pts',(24.7583748985438,-1.2402941723199,12.));
#216116=CARTESIAN_POINT('Ctrl Pts',(24.7353914120011,-1.24938925444327,
0.));
#216117=CARTESIAN_POINT('Ctrl Pts',(24.7353914120011,-1.24938925444327,
12.));
#216118=CARTESIAN_POINT('Ctrl Pts',(24.7124636797894,-1.25839840807419,
0.));
#216119=CARTESIAN_POINT('Ctrl Pts',(24.7124636797894,-1.25839840807419,
12.));
#216120=CARTESIAN_POINT('Ctrl Pts',(24.6895923066836,-1.26732170513501,
0.));
#216121=CARTESIAN_POINT('Ctrl Pts',(24.6895923066836,-1.26732170513501,
12.));
#216122=CARTESIAN_POINT('Ctrl Pts',(24.6667779021559,-1.27615921941643,
0.));
#216123=CARTESIAN_POINT('Ctrl Pts',(24.6667779021559,-1.27615921941643,
12.));
#216124=CARTESIAN_POINT('Ctrl Pts',(24.6440210805278,-1.28491102661515,
0.));
#216125=CARTESIAN_POINT('Ctrl Pts',(24.6440210805278,-1.28491102661515,
12.));
#216126=CARTESIAN_POINT('Ctrl Pts',(24.6213224611229,-1.29357720438108,
0.));
#216127=CARTESIAN_POINT('Ctrl Pts',(24.6213224611229,-1.29357720438108,
12.));
#216128=CARTESIAN_POINT('Ctrl Pts',(24.5986826684027,-1.30215783236363,
0.));
#216129=CARTESIAN_POINT('Ctrl Pts',(24.5986826684027,-1.30215783236363,
12.));
#216130=CARTESIAN_POINT('Ctrl Pts',(24.5761023320183,-1.31065299222023,
0.));
#216131=CARTESIAN_POINT('Ctrl Pts',(24.5761023320183,-1.31065299222023,
12.));
#216132=CARTESIAN_POINT('Ctrl Pts',(24.5535820868674,-1.31906276763669,
0.));
#216133=CARTESIAN_POINT('Ctrl Pts',(24.5535820868674,-1.31906276763669,
12.));
#216134=CARTESIAN_POINT('Ctrl Pts',(24.5311225731435,-1.32738724435327,
0.));
#216135=CARTESIAN_POINT('Ctrl Pts',(24.5311225731435,-1.32738724435327,
12.));
#216136=CARTESIAN_POINT('Ctrl Pts',(24.5087244363856,-1.33562651019687,
0.));
#216137=CARTESIAN_POINT('Ctrl Pts',(24.5087244363856,-1.33562651019687,
12.));
#216138=CARTESIAN_POINT('Ctrl Pts',(24.4863883275134,-1.34378065512339,
0.));
#216139=CARTESIAN_POINT('Ctrl Pts',(24.4863883275134,-1.34378065512339,
12.));
#216140=CARTESIAN_POINT('Ctrl Pts',(24.4641149028892,-1.35184977125649,
0.));
#216141=CARTESIAN_POINT('Ctrl Pts',(24.4641149028892,-1.35184977125649,
12.));
#216142=CARTESIAN_POINT('Ctrl Pts',(24.4419048244523,-1.35983395290629,
0.));
#216143=CARTESIAN_POINT('Ctrl Pts',(24.4419048244523,-1.35983395290629,
12.));
#216144=CARTESIAN_POINT('Ctrl Pts',(24.4197587598337,-1.36773329659958,
0.));
#216145=CARTESIAN_POINT('Ctrl Pts',(24.4197587598337,-1.36773329659958,
12.));
#216146=CARTESIAN_POINT('Ctrl Pts',(24.3976773824732,-1.37554790111611,
0.));
#216147=CARTESIAN_POINT('Ctrl Pts',(24.3976773824732,-1.37554790111611,
12.));
#216148=CARTESIAN_POINT('Ctrl Pts',(24.3756613717299,-1.38327786753,0.));
#216149=CARTESIAN_POINT('Ctrl Pts',(24.3756613717299,-1.38327786753,12.));
#216150=CARTESIAN_POINT('Ctrl Pts',(24.3537114129875,-1.3909232992639,0.));
#216151=CARTESIAN_POINT('Ctrl Pts',(24.3537114129875,-1.3909232992639,12.));
#216152=CARTESIAN_POINT('Ctrl Pts',(24.3318281977643,-1.39848430212808,
0.));
#216153=CARTESIAN_POINT('Ctrl Pts',(24.3318281977643,-1.39848430212808,
12.));
#216154=CARTESIAN_POINT('Ctrl Pts',(24.3100124238311,-1.40596098434339,
0.));
#216155=CARTESIAN_POINT('Ctrl Pts',(24.3100124238311,-1.40596098434339,
12.));
#216156=CARTESIAN_POINT('Ctrl Pts',(24.288264795321,-1.41335345657684,0.));
#216157=CARTESIAN_POINT('Ctrl Pts',(24.288264795321,-1.41335345657684,12.));
#216158=CARTESIAN_POINT('Ctrl Pts',(24.2665860228356,-1.42066183198254,
0.));
#216159=CARTESIAN_POINT('Ctrl Pts',(24.2665860228356,-1.42066183198254,
12.));
#216160=CARTESIAN_POINT('Ctrl Pts',(24.2449768235488,-1.42788622624855,
0.));
#216161=CARTESIAN_POINT('Ctrl Pts',(24.2449768235488,-1.42788622624855,
12.));
#216162=CARTESIAN_POINT('Ctrl Pts',(24.2234379212984,-1.4350267576551,0.));
#216163=CARTESIAN_POINT('Ctrl Pts',(24.2234379212984,-1.4350267576551,12.));
#216164=CARTESIAN_POINT('Ctrl Pts',(24.201970046722,-1.44208354711083,0.));
#216165=CARTESIAN_POINT('Ctrl Pts',(24.201970046722,-1.44208354711083,12.));
#216166=CARTESIAN_POINT('Ctrl Pts',(24.1805739374038,-1.44905671818729,
0.));
#216167=CARTESIAN_POINT('Ctrl Pts',(24.1805739374038,-1.44905671818729,
12.));
#216168=CARTESIAN_POINT('Ctrl Pts',(24.1592503380107,-1.45594639716319,
0.));
#216169=CARTESIAN_POINT('Ctrl Pts',(24.1592503380107,-1.45594639716319,
12.));
#216170=CARTESIAN_POINT('Ctrl Pts',(24.1380000004272,-1.46275271307399,
0.));
#216171=CARTESIAN_POINT('Ctrl Pts',(24.1380000004272,-1.46275271307399,
12.));
#216172=CARTESIAN_POINT('Ctrl Pts',(24.1168236838824,-1.46947579776993,
0.));
#216173=CARTESIAN_POINT('Ctrl Pts',(24.1168236838824,-1.46947579776993,
12.));
#216174=CARTESIAN_POINT('Ctrl Pts',(24.0957221550778,-1.47611578597743,
0.));
#216175=CARTESIAN_POINT('Ctrl Pts',(24.0957221550778,-1.47611578597743,
12.));
#216176=CARTESIAN_POINT('Ctrl Pts',(24.0746961883528,-1.48267281533684,
0.));
#216177=CARTESIAN_POINT('Ctrl Pts',(24.0746961883528,-1.48267281533684,
12.));
#216178=CARTESIAN_POINT('Ctrl Pts',(24.0537465658429,-1.48914702644889,
0.));
#216179=CARTESIAN_POINT('Ctrl Pts',(24.0537465658429,-1.48914702644889,
12.));
#216180=CARTESIAN_POINT('Ctrl Pts',(24.0328740776331,-1.49553856292802,
0.));
#216181=CARTESIAN_POINT('Ctrl Pts',(24.0328740776331,-1.49553856292802,
12.));
#216182=CARTESIAN_POINT('Ctrl Pts',(24.0120795219086,-1.501847571461,0.));
#216183=CARTESIAN_POINT('Ctrl Pts',(24.0120795219086,-1.501847571461,12.));
#216184=CARTESIAN_POINT('Ctrl Pts',(23.9913637050927,-1.50807420187695,
0.));
#216185=CARTESIAN_POINT('Ctrl Pts',(23.9913637050927,-1.50807420187695,
12.));
#216186=CARTESIAN_POINT('Ctrl Pts',(23.970727442014,-1.51421860720616,0.));
#216187=CARTESIAN_POINT('Ctrl Pts',(23.970727442014,-1.51421860720616,12.));
#216188=CARTESIAN_POINT('Ctrl Pts',(23.9501715561033,-1.52028094372793,
0.));
#216189=CARTESIAN_POINT('Ctrl Pts',(23.9501715561033,-1.52028094372793,
12.));
#216190=CARTESIAN_POINT('Ctrl Pts',(23.9296968795757,-1.52626137103033,
0.));
#216191=CARTESIAN_POINT('Ctrl Pts',(23.9296968795757,-1.52626137103033,
12.));
#216192=CARTESIAN_POINT('Ctrl Pts',(23.9093042536119,-1.53216005207464,
0.));
#216193=CARTESIAN_POINT('Ctrl Pts',(23.9093042536119,-1.53216005207464,
12.));
#216194=CARTESIAN_POINT('Ctrl Pts',(23.8889945285318,-1.53797715326759,
0.));
#216195=CARTESIAN_POINT('Ctrl Pts',(23.8889945285318,-1.53797715326759,
12.));
#216196=CARTESIAN_POINT('Ctrl Pts',(23.8687685639642,-1.54371284453992,
0.));
#216197=CARTESIAN_POINT('Ctrl Pts',(23.8687685639642,-1.54371284453992,
12.));
#216198=CARTESIAN_POINT('Ctrl Pts',(23.8486272290705,-1.54936729940542,
0.));
#216199=CARTESIAN_POINT('Ctrl Pts',(23.8486272290705,-1.54936729940542,
12.));
#216200=CARTESIAN_POINT('Ctrl Pts',(23.8285714027636,-1.55494069502636,
0.));
#216201=CARTESIAN_POINT('Ctrl Pts',(23.8285714027636,-1.55494069502636,
12.));
#216202=CARTESIAN_POINT('Ctrl Pts',(23.8086019739194,-1.56043321228635,
0.));
#216203=CARTESIAN_POINT('Ctrl Pts',(23.8086019739194,-1.56043321228635,
12.));
#216204=CARTESIAN_POINT('Ctrl Pts',(23.7887198415878,-1.56584503586844,
0.));
#216205=CARTESIAN_POINT('Ctrl Pts',(23.7887198415878,-1.56584503586844,
12.));
#216206=CARTESIAN_POINT('Ctrl Pts',(23.7689259151862,-1.57117635434409,
0.));
#216207=CARTESIAN_POINT('Ctrl Pts',(23.7689259151862,-1.57117635434409,
12.));
#216208=CARTESIAN_POINT('Ctrl Pts',(23.749221114736,-1.57642736025247,0.));
#216209=CARTESIAN_POINT('Ctrl Pts',(23.749221114736,-1.57642736025247,12.));
#216210=CARTESIAN_POINT('Ctrl Pts',(23.72960637113,-1.58159825017359,0.));
#216211=CARTESIAN_POINT('Ctrl Pts',(23.72960637113,-1.58159825017359,12.));
#216212=CARTESIAN_POINT('Ctrl Pts',(23.710082626383,-1.58668922481222,0.));
#216213=CARTESIAN_POINT('Ctrl Pts',(23.710082626383,-1.58668922481222,12.));
#216214=CARTESIAN_POINT('Ctrl Pts',(23.6906508338833,-1.59170048908634,
0.));
#216215=CARTESIAN_POINT('Ctrl Pts',(23.6906508338833,-1.59170048908634,
12.));
#216216=CARTESIAN_POINT('Ctrl Pts',(23.671311958631,-1.59663225222464,0.));
#216217=CARTESIAN_POINT('Ctrl Pts',(23.671311958631,-1.59663225222464,12.));
#216218=CARTESIAN_POINT('Ctrl Pts',(23.6520669774876,-1.60148472786596,
0.));
#216219=CARTESIAN_POINT('Ctrl Pts',(23.6520669774876,-1.60148472786596,
12.));
#216220=CARTESIAN_POINT('Ctrl Pts',(23.6329168794929,-1.60625813414674,
0.));
#216221=CARTESIAN_POINT('Ctrl Pts',(23.6329168794929,-1.60625813414674,
12.));
#216222=CARTESIAN_POINT('Ctrl Pts',(23.6138626661653,-1.61095269379779,
0.));
#216223=CARTESIAN_POINT('Ctrl Pts',(23.6138626661653,-1.61095269379779,
12.));
#216224=CARTESIAN_POINT('Ctrl Pts',(23.5949053517997,-1.61556863424699,
0.));
#216225=CARTESIAN_POINT('Ctrl Pts',(23.5949053517997,-1.61556863424699,
12.));
#216226=CARTESIAN_POINT('Ctrl Pts',(23.57604596376,-1.62010618772867,0.));
#216227=CARTESIAN_POINT('Ctrl Pts',(23.57604596376,-1.62010618772867,12.));
#216228=CARTESIAN_POINT('Ctrl Pts',(23.5572855427601,-1.62456559140066,
0.));
#216229=CARTESIAN_POINT('Ctrl Pts',(23.5572855427601,-1.62456559140066,
12.));
#216230=CARTESIAN_POINT('Ctrl Pts',(23.538625143226,-1.62894708745224,0.));
#216231=CARTESIAN_POINT('Ctrl Pts',(23.538625143226,-1.62894708745224,12.));
#216232=CARTESIAN_POINT('Ctrl Pts',(23.5200658336612,-1.63325092321727,
0.));
#216233=CARTESIAN_POINT('Ctrl Pts',(23.5200658336612,-1.63325092321727,
12.));
#216234=CARTESIAN_POINT('Ctrl Pts',(23.5016086970003,-1.63747735129475,
0.));
#216235=CARTESIAN_POINT('Ctrl Pts',(23.5016086970003,-1.63747735129475,
12.));
#216236=CARTESIAN_POINT('Ctrl Pts',(23.4832548309645,-1.64162662967529,
0.));
#216237=CARTESIAN_POINT('Ctrl Pts',(23.4832548309645,-1.64162662967529,
12.));
#216238=CARTESIAN_POINT('Ctrl Pts',(23.4650053483932,-1.64569902187612,
0.));
#216239=CARTESIAN_POINT('Ctrl Pts',(23.4650053483932,-1.64569902187612,
12.));
#216240=CARTESIAN_POINT('Ctrl Pts',(23.4468613776574,-1.64969479707341,
0.));
#216241=CARTESIAN_POINT('Ctrl Pts',(23.4468613776574,-1.64969479707341,
12.));
#216242=CARTESIAN_POINT('Ctrl Pts',(23.4288240631043,-1.6536142302373,0.));
#216243=CARTESIAN_POINT('Ctrl Pts',(23.4288240631043,-1.6536142302373,12.));
#216244=CARTESIAN_POINT('Ctrl Pts',(23.4108945654805,-1.65745760227506,
0.));
#216245=CARTESIAN_POINT('Ctrl Pts',(23.4108945654805,-1.65745760227506,
12.));
#216246=CARTESIAN_POINT('Ctrl Pts',(23.3930740623619,-1.66122520018012,
0.));
#216247=CARTESIAN_POINT('Ctrl Pts',(23.3930740623619,-1.66122520018012,
12.));
#216248=CARTESIAN_POINT('Ctrl Pts',(23.3753637485545,-1.66491731718878,
0.));
#216249=CARTESIAN_POINT('Ctrl Pts',(23.3753637485545,-1.66491731718878,
12.));
#216250=CARTESIAN_POINT('Ctrl Pts',(23.3577648365744,-1.66853425293997,
0.));
#216251=CARTESIAN_POINT('Ctrl Pts',(23.3577648365744,-1.66853425293997,
12.));
#216252=CARTESIAN_POINT('Ctrl Pts',(23.3402785571865,-1.67207631363923,
0.));
#216253=CARTESIAN_POINT('Ctrl Pts',(23.3402785571865,-1.67207631363923,
12.));
#216254=CARTESIAN_POINT('Ctrl Pts',(23.3229061599144,-1.67554381222995,
0.));
#216255=CARTESIAN_POINT('Ctrl Pts',(23.3229061599144,-1.67554381222995,
12.));
#216256=CARTESIAN_POINT('Ctrl Pts',(23.3056489135611,-1.67893706857118,
0.));
#216257=CARTESIAN_POINT('Ctrl Pts',(23.3056489135611,-1.67893706857118,
12.));
#216258=CARTESIAN_POINT('Ctrl Pts',(23.2885081066951,-1.68225640962169,
0.));
#216259=CARTESIAN_POINT('Ctrl Pts',(23.2885081066951,-1.68225640962169,
12.));
#216260=CARTESIAN_POINT('Ctrl Pts',(23.2714850482246,-1.68550216963259,
0.));
#216261=CARTESIAN_POINT('Ctrl Pts',(23.2714850482246,-1.68550216963259,
12.));
#216262=CARTESIAN_POINT('Ctrl Pts',(23.2545810680537,-1.68867469034897,
0.));
#216263=CARTESIAN_POINT('Ctrl Pts',(23.2545810680537,-1.68867469034897,
12.));
#216264=CARTESIAN_POINT('Ctrl Pts',(23.2377975177013,-1.69177432121712,
0.));
#216265=CARTESIAN_POINT('Ctrl Pts',(23.2377975177013,-1.69177432121712,
12.));
#216266=CARTESIAN_POINT('Ctrl Pts',(23.2211357709374,-1.69480141959954,
0.));
#216267=CARTESIAN_POINT('Ctrl Pts',(23.2211357709374,-1.69480141959954,
12.));
#216268=CARTESIAN_POINT('Ctrl Pts',(23.2045972243767,-1.69775635099444,
0.));
#216269=CARTESIAN_POINT('Ctrl Pts',(23.2045972243767,-1.69775635099444,
12.));
#216270=CARTESIAN_POINT('Ctrl Pts',(23.1881832981851,-1.70063948927011,
0.));
#216271=CARTESIAN_POINT('Ctrl Pts',(23.1881832981851,-1.70063948927011,
12.));
#216272=CARTESIAN_POINT('Ctrl Pts',(23.1718954368751,-1.70345121691278,
0.));
#216273=CARTESIAN_POINT('Ctrl Pts',(23.1718954368751,-1.70345121691278,
12.));
#216274=CARTESIAN_POINT('Ctrl Pts',(23.1557351100614,-1.70619192527853,
0.));
#216275=CARTESIAN_POINT('Ctrl Pts',(23.1557351100614,-1.70619192527853,
12.));
#216276=CARTESIAN_POINT('Ctrl Pts',(23.1397038132356,-1.70886201485453,
0.));
#216277=CARTESIAN_POINT('Ctrl Pts',(23.1397038132356,-1.70886201485453,
12.));
#216278=CARTESIAN_POINT('Ctrl Pts',(23.1238030684925,-1.71146189552175,
0.));
#216279=CARTESIAN_POINT('Ctrl Pts',(23.1238030684925,-1.71146189552175,
12.));
#216280=CARTESIAN_POINT('Ctrl Pts',(23.1080344254286,-1.71399198684705,
0.));
#216281=CARTESIAN_POINT('Ctrl Pts',(23.1080344254286,-1.71399198684705,
12.));
#216282=CARTESIAN_POINT('Ctrl Pts',(23.0923994621213,-1.71645271839298,
0.));
#216283=CARTESIAN_POINT('Ctrl Pts',(23.0923994621213,-1.71645271839298,
12.));
#216284=CARTESIAN_POINT('Ctrl Pts',(23.0768997860708,-1.71884453003028,
0.));
#216285=CARTESIAN_POINT('Ctrl Pts',(23.0768997860708,-1.71884453003028,
12.));
#216286=CARTESIAN_POINT('Ctrl Pts',(23.0615370351562,-1.72116787225993,
0.));
#216287=CARTESIAN_POINT('Ctrl Pts',(23.0615370351562,-1.72116787225993,
12.));
#216288=CARTESIAN_POINT('Ctrl Pts',(23.0463128785531,-1.72342320653748,
0.));
#216289=CARTESIAN_POINT('Ctrl Pts',(23.0463128785531,-1.72342320653748,
12.));
#216290=CARTESIAN_POINT('Ctrl Pts',(23.0312290178883,-1.72561100564047,
0.));
#216291=CARTESIAN_POINT('Ctrl Pts',(23.0312290178883,-1.72561100564047,
12.));
#216292=CARTESIAN_POINT('Ctrl Pts',(23.0162871884168,-1.7277317540471,0.));
#216293=CARTESIAN_POINT('Ctrl Pts',(23.0162871884168,-1.7277317540471,12.));
#216294=CARTESIAN_POINT('Ctrl Pts',(23.001489160189,-1.72978594832137,0.));
#216295=CARTESIAN_POINT('Ctrl Pts',(23.001489160189,-1.72978594832137,12.));
#216296=CARTESIAN_POINT('Ctrl Pts',(22.9868367391978,-1.73177409750192,
0.));
#216297=CARTESIAN_POINT('Ctrl Pts',(22.9868367391978,-1.73177409750192,
12.));
#216298=CARTESIAN_POINT('Ctrl Pts',(22.9723317685688,-1.73369672350816,
0.));
#216299=CARTESIAN_POINT('Ctrl Pts',(22.9723317685688,-1.73369672350816,
12.));
#216300=CARTESIAN_POINT('Ctrl Pts',(22.9579761301063,-1.73555436162771,
0.));
#216301=CARTESIAN_POINT('Ctrl Pts',(22.9579761301063,-1.73555436162771,
12.));
#216302=CARTESIAN_POINT('Ctrl Pts',(22.9437717457826,-1.7373475610004,0.));
#216303=CARTESIAN_POINT('Ctrl Pts',(22.9437717457826,-1.7373475610004,12.));
#216304=CARTESIAN_POINT('Ctrl Pts',(22.9297205792586,-1.73907688511667,
0.));
#216305=CARTESIAN_POINT('Ctrl Pts',(22.9297205792586,-1.73907688511667,
12.));
#216306=CARTESIAN_POINT('Ctrl Pts',(22.9158246373363,-1.7407429123106,0.));
#216307=CARTESIAN_POINT('Ctrl Pts',(22.9158246373363,-1.7407429123106,12.));
#216308=CARTESIAN_POINT('Ctrl Pts',(22.9020859716141,-1.74234623630081,
0.));
#216309=CARTESIAN_POINT('Ctrl Pts',(22.9020859716141,-1.74234623630081,
12.));
#216310=CARTESIAN_POINT('Ctrl Pts',(22.888506680335,-1.74388746677704,0.));
#216311=CARTESIAN_POINT('Ctrl Pts',(22.888506680335,-1.74388746677704,12.));
#216312=CARTESIAN_POINT('Ctrl Pts',(22.8750889101696,-1.74536722998202,
0.));
#216313=CARTESIAN_POINT('Ctrl Pts',(22.8750889101696,-1.74536722998202,
12.));
#216314=CARTESIAN_POINT('Ctrl Pts',(22.8618348580235,-1.74678616930666,
0.));
#216315=CARTESIAN_POINT('Ctrl Pts',(22.8618348580235,-1.74678616930666,
12.));
#216316=CARTESIAN_POINT('Ctrl Pts',(22.8487467728076,-1.74814494588494,
0.));
#216317=CARTESIAN_POINT('Ctrl Pts',(22.8487467728076,-1.74814494588494,
12.));
#216318=CARTESIAN_POINT('Ctrl Pts',(22.8358269579853,-1.74944423940117,
0.));
#216319=CARTESIAN_POINT('Ctrl Pts',(22.8358269579853,-1.74944423940117,
12.));
#216320=CARTESIAN_POINT('Ctrl Pts',(22.8230777741284,-1.75068474890884,
0.));
#216321=CARTESIAN_POINT('Ctrl Pts',(22.8230777741284,-1.75068474890884,
12.));
#216322=CARTESIAN_POINT('Ctrl Pts',(22.8105016414713,-1.75186719365593,
0.));
#216323=CARTESIAN_POINT('Ctrl Pts',(22.8105016414713,-1.75186719365593,
12.));
#216324=CARTESIAN_POINT('Ctrl Pts',(22.7981010424314,-1.75299231391468,
0.));
#216325=CARTESIAN_POINT('Ctrl Pts',(22.7981010424314,-1.75299231391468,
12.));
#216326=CARTESIAN_POINT('Ctrl Pts',(22.7858785242361,-1.75406087182937,
0.));
#216327=CARTESIAN_POINT('Ctrl Pts',(22.7858785242361,-1.75406087182937,
12.));
#216328=CARTESIAN_POINT('Ctrl Pts',(22.7738367016118,-1.75507365227133,
0.));
#216329=CARTESIAN_POINT('Ctrl Pts',(22.7738367016118,-1.75507365227133,
12.));
#216330=CARTESIAN_POINT('Ctrl Pts',(22.7619782595013,-1.75603146371642,
0.));
#216331=CARTESIAN_POINT('Ctrl Pts',(22.7619782595013,-1.75603146371642,
12.));
#216332=CARTESIAN_POINT('Ctrl Pts',(22.750305955645,-1.75693513908908,0.));
#216333=CARTESIAN_POINT('Ctrl Pts',(22.750305955645,-1.75693513908908,12.));
#216334=CARTESIAN_POINT('Ctrl Pts',(22.7388226235559,-1.75778553673245,
0.));
#216335=CARTESIAN_POINT('Ctrl Pts',(22.7388226235559,-1.75778553673245,
12.));
#216336=CARTESIAN_POINT('Ctrl Pts',(22.72753117773,-1.75858354204634,0.));
#216337=CARTESIAN_POINT('Ctrl Pts',(22.72753117773,-1.75858354204634,12.));
#216338=CARTESIAN_POINT('Ctrl Pts',(22.7164346186006,-1.75933006905926,
0.));
#216339=CARTESIAN_POINT('Ctrl Pts',(22.7164346186006,-1.75933006905926,
12.));
#216340=CARTESIAN_POINT('Ctrl Pts',(22.7055360375485,-1.76002606202402,
0.));
#216341=CARTESIAN_POINT('Ctrl Pts',(22.7055360375485,-1.76002606202402,
12.));
#216342=CARTESIAN_POINT('Ctrl Pts',(22.6948386219851,-1.76067249704888,
0.));
#216343=CARTESIAN_POINT('Ctrl Pts',(22.6948386219851,-1.76067249704888,
12.));
#216344=CARTESIAN_POINT('Ctrl Pts',(22.684345658525,-1.76127038310615,0.));
#216345=CARTESIAN_POINT('Ctrl Pts',(22.684345658525,-1.76127038310615,12.));
#216346=CARTESIAN_POINT('Ctrl Pts',(22.67406053567,-1.76182076289527,0.));
#216347=CARTESIAN_POINT('Ctrl Pts',(22.67406053567,-1.76182076289527,12.));
#216348=CARTESIAN_POINT('Ctrl Pts',(22.6639867471753,-1.7623247139257,0.));
#216349=CARTESIAN_POINT('Ctrl Pts',(22.6639867471753,-1.7623247139257,12.));
#216350=CARTESIAN_POINT('Ctrl Pts',(22.6541278938409,-1.76278334912562,
0.));
#216351=CARTESIAN_POINT('Ctrl Pts',(22.6541278938409,-1.76278334912562,
12.));
#216352=CARTESIAN_POINT('Ctrl Pts',(22.6444876940423,-1.76319782013917,
0.));
#216353=CARTESIAN_POINT('Ctrl Pts',(22.6444876940423,-1.76319782013917,
12.));
#216354=CARTESIAN_POINT('Ctrl Pts',(22.6350699979359,-1.76356932176274,
0.));
#216355=CARTESIAN_POINT('Ctrl Pts',(22.6350699979359,-1.76356932176274,
12.));
#216356=CARTESIAN_POINT('Ctrl Pts',(22.6258787994848,-1.76389909571404,
0.));
#216357=CARTESIAN_POINT('Ctrl Pts',(22.6258787994848,-1.76389909571404,
12.));
#216358=CARTESIAN_POINT('Ctrl Pts',(22.6169182517694,-1.76418843543741,
0.));
#216359=CARTESIAN_POINT('Ctrl Pts',(22.6169182517694,-1.76418843543741,
12.));
#216360=CARTESIAN_POINT('Ctrl Pts',(22.6081926681343,-1.76443868648017,
0.));
#216361=CARTESIAN_POINT('Ctrl Pts',(22.6081926681343,-1.76443868648017,
12.));
#216362=CARTESIAN_POINT('Ctrl Pts',(22.5997065145638,-1.76465124413558,
0.));
#216363=CARTESIAN_POINT('Ctrl Pts',(22.5997065145638,-1.76465124413558,
12.));
#216364=CARTESIAN_POINT('Ctrl Pts',(22.5914644078105,-1.76482755288412,
0.));
#216365=CARTESIAN_POINT('Ctrl Pts',(22.5914644078105,-1.76482755288412,
12.));
#216366=CARTESIAN_POINT('Ctrl Pts',(22.5834711038022,-1.76496910283089,
0.));
#216367=CARTESIAN_POINT('Ctrl Pts',(22.5834711038022,-1.76496910283089,
12.));
#216368=CARTESIAN_POINT('Ctrl Pts',(22.5757315316353,-1.76507744026747,
0.));
#216369=CARTESIAN_POINT('Ctrl Pts',(22.5757315316353,-1.76507744026747,
12.));
#216370=CARTESIAN_POINT('Ctrl Pts',(22.5682508499873,-1.76515418518832,
0.));
#216371=CARTESIAN_POINT('Ctrl Pts',(22.5682508499873,-1.76515418518832,
12.));
#216372=CARTESIAN_POINT('Ctrl Pts',(22.5610344912501,-1.76520104500451,
0.));
#216373=CARTESIAN_POINT('Ctrl Pts',(22.5610344912501,-1.76520104500451,
12.));
#216374=CARTESIAN_POINT('Ctrl Pts',(22.5540882235837,-1.76521983384064,
0.));
#216375=CARTESIAN_POINT('Ctrl Pts',(22.5540882235837,-1.76521983384064,
12.));
#216376=CARTESIAN_POINT('Ctrl Pts',(22.5474180954006,-1.76521245524048,
0.));
#216377=CARTESIAN_POINT('Ctrl Pts',(22.5474180954006,-1.76521245524048,
12.));
#216378=CARTESIAN_POINT('Ctrl Pts',(22.5410303590892,-1.76518087841494,
0.));
#216379=CARTESIAN_POINT('Ctrl Pts',(22.5410303590892,-1.76518087841494,
12.));
#216380=CARTESIAN_POINT('Ctrl Pts',(22.5349313983571,-1.76512711563255,
0.));
#216381=CARTESIAN_POINT('Ctrl Pts',(22.5349313983571,-1.76512711563255,
12.));
#216382=CARTESIAN_POINT('Ctrl Pts',(22.529127665298,-1.7650532026276,0.));
#216383=CARTESIAN_POINT('Ctrl Pts',(22.529127665298,-1.7650532026276,12.));
#216384=CARTESIAN_POINT('Ctrl Pts',(22.5236259635515,-1.76496128643376,
0.));
#216385=CARTESIAN_POINT('Ctrl Pts',(22.5236259635515,-1.76496128643376,
12.));
#216386=CARTESIAN_POINT('Ctrl Pts',(22.5184336670207,-1.76485369319896,
0.));
#216387=CARTESIAN_POINT('Ctrl Pts',(22.5184336670207,-1.76485369319896,
12.));
#216388=CARTESIAN_POINT('Ctrl Pts',(22.5135590569554,-1.7647330328115,0.));
#216389=CARTESIAN_POINT('Ctrl Pts',(22.5135590569554,-1.7647330328115,12.));
#216390=CARTESIAN_POINT('Ctrl Pts',(22.5090112700212,-1.76460218257314,
0.));
#216391=CARTESIAN_POINT('Ctrl Pts',(22.5090112700212,-1.76460218257314,
12.));
#216392=CARTESIAN_POINT('Ctrl Pts',(22.5047996391978,-1.76446408210366,
0.));
#216393=CARTESIAN_POINT('Ctrl Pts',(22.5047996391978,-1.76446408210366,
12.));
#216394=CARTESIAN_POINT('Ctrl Pts',(22.5009332677316,-1.76432160068739,
0.));
#216395=CARTESIAN_POINT('Ctrl Pts',(22.5009332677316,-1.76432160068739,
12.));
#216396=CARTESIAN_POINT('Ctrl Pts',(22.4974203063191,-1.76417731243484,
0.));
#216397=CARTESIAN_POINT('Ctrl Pts',(22.4974203063191,-1.76417731243484,
12.));
#216398=CARTESIAN_POINT('Ctrl Pts',(22.4942693792449,-1.76403393880317,
0.));
#216399=CARTESIAN_POINT('Ctrl Pts',(22.4942693792449,-1.76403393880317,
12.));
#216400=CARTESIAN_POINT('Ctrl Pts',(22.4914909094908,-1.76389475965715,
0.));
#216401=CARTESIAN_POINT('Ctrl Pts',(22.4914909094908,-1.76389475965715,
12.));
#216402=CARTESIAN_POINT('Ctrl Pts',(22.4890991659479,-1.76376424879469,
0.));
#216403=CARTESIAN_POINT('Ctrl Pts',(22.4890991659479,-1.76376424879469,
12.));
#216404=CARTESIAN_POINT('Ctrl Pts',(22.4871115206572,-1.76364784232927,
0.));
#216405=CARTESIAN_POINT('Ctrl Pts',(22.4871115206572,-1.76364784232927,
12.));
#216406=CARTESIAN_POINT('Ctrl Pts',(22.4855446605991,-1.7635507604555,0.));
#216407=CARTESIAN_POINT('Ctrl Pts',(22.4855446605991,-1.7635507604555,12.));
#216408=CARTESIAN_POINT('Ctrl Pts',(22.4844112933125,-1.76347698284863,
0.));
#216409=CARTESIAN_POINT('Ctrl Pts',(22.4844112933125,-1.76347698284863,
12.));
#216410=CARTESIAN_POINT('Ctrl Pts',(22.4838562517064,-1.7634381343466,0.));
#216411=CARTESIAN_POINT('Ctrl Pts',(22.4838562517064,-1.7634381343466,12.));
#216412=CARTESIAN_POINT('Ctrl Pts',(22.4836387052228,-1.76342064263638,
0.));
#216413=CARTESIAN_POINT('Ctrl Pts',(22.4836387052228,-1.76342064263638,
12.));
#216414=CARTESIAN_POINT('Ctrl Pts',(22.4835819929788,-1.76341415538792,
0.));
#216415=CARTESIAN_POINT('Ctrl Pts',(22.4835819929788,-1.76341415538792,
12.));
#216416=CARTESIAN_POINT('Ctrl Pts',(22.4835757167854,-1.76341220531181,
0.));
#216417=CARTESIAN_POINT('Ctrl Pts',(22.4835757167854,-1.76341220531181,
12.));
#216418=CARTESIAN_POINT('',(25.991588367311,-0.661312440730916,0.));
#216419=CARTESIAN_POINT('Ctrl Pts',(25.991588367311,-0.661312440730916,
0.));
#216420=CARTESIAN_POINT('Ctrl Pts',(25.9865613464773,-0.66402831318764,
0.));
#216421=CARTESIAN_POINT('Ctrl Pts',(25.9765104298071,-0.669451306780839,
0.));
#216422=CARTESIAN_POINT('Ctrl Pts',(25.9614434297919,-0.67755954320974,
0.));
#216423=CARTESIAN_POINT('Ctrl Pts',(25.9413728471909,-0.688318015057744,
0.));
#216424=CARTESIAN_POINT('Ctrl Pts',(25.9163158909426,-0.701678575228769,
0.));
#216425=CARTESIAN_POINT('Ctrl Pts',(25.8912902614969,-0.714951588527653,
0.));
#216426=CARTESIAN_POINT('Ctrl Pts',(25.8662960624185,-0.728137036482349,
0.));
#216427=CARTESIAN_POINT('Ctrl Pts',(25.8413334619054,-0.74123490266382,
0.));
#216428=CARTESIAN_POINT('Ctrl Pts',(25.8164027059984,-0.754245175609537,
0.));
#216429=CARTESIAN_POINT('Ctrl Pts',(25.7915041383376,-0.767167852651183,
0.));
#216430=CARTESIAN_POINT('Ctrl Pts',(25.7666381946955,-0.780002940291977,
0.));
#216431=CARTESIAN_POINT('Ctrl Pts',(25.7418053757746,-0.79275045161614,
0.));
#216432=CARTESIAN_POINT('Ctrl Pts',(25.7170062262525,-0.805410404554366,
0.));
#216433=CARTESIAN_POINT('Ctrl Pts',(25.6922413110194,-0.817982819787478,
0.));
#216434=CARTESIAN_POINT('Ctrl Pts',(25.6675111931952,-0.830467718864221,
0.));
#216435=CARTESIAN_POINT('Ctrl Pts',(25.6428164100055,-0.842865122120773,
0.));
#216436=CARTESIAN_POINT('Ctrl Pts',(25.6181574536049,-0.855175047036563,
0.));
#216437=CARTESIAN_POINT('Ctrl Pts',(25.5935347843585,-0.867397509338443,
0.));
#216438=CARTESIAN_POINT('Ctrl Pts',(25.5689488408156,-0.879532523834308,
0.));
#216439=CARTESIAN_POINT('Ctrl Pts',(25.5444000508211,-0.891580105349052,
0.));
#216440=CARTESIAN_POINT('Ctrl Pts',(25.5198888424194,-0.903540269651121,
0.));
#216441=CARTESIAN_POINT('Ctrl Pts',(25.4954156541795,-0.915413034335626,
0.));
#216442=CARTESIAN_POINT('Ctrl Pts',(25.4709809475009,-0.927198419886108,
0.));
#216443=CARTESIAN_POINT('Ctrl Pts',(25.4465852044849,-0.938896449496205,
0.));
#216444=CARTESIAN_POINT('Ctrl Pts',(25.4222289223167,-0.950507148597483,
0.));
#216445=CARTESIAN_POINT('Ctrl Pts',(25.3979126089163,-0.962030544503156,
0.));
#216446=CARTESIAN_POINT('Ctrl Pts',(25.3736367778845,-0.973466666000178,
0.));
#216447=CARTESIAN_POINT('Ctrl Pts',(25.3494019441441,-0.984815543003986,
0.));
#216448=CARTESIAN_POINT('Ctrl Pts',(25.3252086182968,-0.996077206120637,
0.));
#216449=CARTESIAN_POINT('Ctrl Pts',(25.3010573055547,-1.00725168656897,
0.));
#216450=CARTESIAN_POINT('Ctrl Pts',(25.276948508726,-1.01833901642238,0.));
#216451=CARTESIAN_POINT('Ctrl Pts',(25.2528827300422,-1.02933922876807,
0.));
#216452=CARTESIAN_POINT('Ctrl Pts',(25.2288604735086,-1.04025235791508,
0.));
#216453=CARTESIAN_POINT('Ctrl Pts',(25.2048822469028,-1.05107843957933,
0.));
#216454=CARTESIAN_POINT('Ctrl Pts',(25.1809485642192,-1.06181751111769,
0.));
#216455=CARTESIAN_POINT('Ctrl Pts',(25.157059946931,-1.07246961165477,0.));
#216456=CARTESIAN_POINT('Ctrl Pts',(25.1332169227413,-1.08303478197189,
0.));
#216457=CARTESIAN_POINT('Ctrl Pts',(25.1094200248446,-1.09351306445309,
0.));
#216458=CARTESIAN_POINT('Ctrl Pts',(25.0856697909679,-1.10390450301747,
0.));
#216459=CARTESIAN_POINT('Ctrl Pts',(25.0619667625336,-1.11420914306891,
0.));
#216460=CARTESIAN_POINT('Ctrl Pts',(25.0383114836899,-1.12442703144453,
0.));
#216461=CARTESIAN_POINT('Ctrl Pts',(25.0147045006195,-1.13455821638531,
0.));
#216462=CARTESIAN_POINT('Ctrl Pts',(24.9911463621433,-1.14460274758202,
0.));
#216463=CARTESIAN_POINT('Ctrl Pts',(24.9676376201502,-1.15456067621891,
0.));
#216464=CARTESIAN_POINT('Ctrl Pts',(24.9441788300932,-1.16443205502851,
0.));
#216465=CARTESIAN_POINT('Ctrl Pts',(24.9207705514448,-1.17421693835042,
0.));
#216466=CARTESIAN_POINT('Ctrl Pts',(24.8974133481829,-1.18391538220104,
0.));
#216467=CARTESIAN_POINT('Ctrl Pts',(24.8741077892075,-1.19352744434066,
0.));
#216468=CARTESIAN_POINT('Ctrl Pts',(24.8508544481974,-1.20305318426021,
0.));
#216469=CARTESIAN_POINT('Ctrl Pts',(24.8276539035092,-1.21249266318209,
0.));
#216470=CARTESIAN_POINT('Ctrl Pts',(24.8045067380536,-1.22184594406529,
0.));
#216471=CARTESIAN_POINT('Ctrl Pts',(24.7814135391799,-1.23111309161845,
0.));
#216472=CARTESIAN_POINT('Ctrl Pts',(24.7583748985438,-1.2402941723199,0.));
#216473=CARTESIAN_POINT('Ctrl Pts',(24.7353914120011,-1.24938925444327,
0.));
#216474=CARTESIAN_POINT('Ctrl Pts',(24.7124636797894,-1.25839840807419,
0.));
#216475=CARTESIAN_POINT('Ctrl Pts',(24.6895923066836,-1.26732170513501,
0.));
#216476=CARTESIAN_POINT('Ctrl Pts',(24.6667779021559,-1.27615921941643,
0.));
#216477=CARTESIAN_POINT('Ctrl Pts',(24.6440210805278,-1.28491102661515,
0.));
#216478=CARTESIAN_POINT('Ctrl Pts',(24.6213224611229,-1.29357720438108,
0.));
#216479=CARTESIAN_POINT('Ctrl Pts',(24.5986826684027,-1.30215783236363,
0.));
#216480=CARTESIAN_POINT('Ctrl Pts',(24.5761023320183,-1.31065299222023,
0.));
#216481=CARTESIAN_POINT('Ctrl Pts',(24.5535820868674,-1.31906276763669,
0.));
#216482=CARTESIAN_POINT('Ctrl Pts',(24.5311225731435,-1.32738724435327,
0.));
#216483=CARTESIAN_POINT('Ctrl Pts',(24.5087244363856,-1.33562651019687,
0.));
#216484=CARTESIAN_POINT('Ctrl Pts',(24.4863883275134,-1.34378065512339,
0.));
#216485=CARTESIAN_POINT('Ctrl Pts',(24.4641149028892,-1.35184977125649,
0.));
#216486=CARTESIAN_POINT('Ctrl Pts',(24.4419048244523,-1.35983395290629,
0.));
#216487=CARTESIAN_POINT('Ctrl Pts',(24.4197587598337,-1.36773329659958,
0.));
#216488=CARTESIAN_POINT('Ctrl Pts',(24.3976773824732,-1.37554790111611,
0.));
#216489=CARTESIAN_POINT('Ctrl Pts',(24.3756613717299,-1.38327786753,0.));
#216490=CARTESIAN_POINT('Ctrl Pts',(24.3537114129875,-1.3909232992639,0.));
#216491=CARTESIAN_POINT('Ctrl Pts',(24.3318281977643,-1.39848430212808,
0.));
#216492=CARTESIAN_POINT('Ctrl Pts',(24.3100124238311,-1.40596098434339,
0.));
#216493=CARTESIAN_POINT('Ctrl Pts',(24.288264795321,-1.41335345657684,0.));
#216494=CARTESIAN_POINT('Ctrl Pts',(24.2665860228356,-1.42066183198254,
0.));
#216495=CARTESIAN_POINT('Ctrl Pts',(24.2449768235488,-1.42788622624855,
0.));
#216496=CARTESIAN_POINT('Ctrl Pts',(24.2234379212984,-1.4350267576551,0.));
#216497=CARTESIAN_POINT('Ctrl Pts',(24.201970046722,-1.44208354711083,0.));
#216498=CARTESIAN_POINT('Ctrl Pts',(24.1805739374038,-1.44905671818729,
0.));
#216499=CARTESIAN_POINT('Ctrl Pts',(24.1592503380107,-1.45594639716319,
0.));
#216500=CARTESIAN_POINT('Ctrl Pts',(24.1380000004272,-1.46275271307399,
0.));
#216501=CARTESIAN_POINT('Ctrl Pts',(24.1168236838824,-1.46947579776993,
0.));
#216502=CARTESIAN_POINT('Ctrl Pts',(24.0957221550778,-1.47611578597743,
0.));
#216503=CARTESIAN_POINT('Ctrl Pts',(24.0746961883528,-1.48267281533684,
0.));
#216504=CARTESIAN_POINT('Ctrl Pts',(24.0537465658429,-1.48914702644889,
0.));
#216505=CARTESIAN_POINT('Ctrl Pts',(24.0328740776331,-1.49553856292802,
0.));
#216506=CARTESIAN_POINT('Ctrl Pts',(24.0120795219086,-1.501847571461,0.));
#216507=CARTESIAN_POINT('Ctrl Pts',(23.9913637050927,-1.50807420187695,
0.));
#216508=CARTESIAN_POINT('Ctrl Pts',(23.970727442014,-1.51421860720616,0.));
#216509=CARTESIAN_POINT('Ctrl Pts',(23.9501715561033,-1.52028094372793,
0.));
#216510=CARTESIAN_POINT('Ctrl Pts',(23.9296968795757,-1.52626137103033,
0.));
#216511=CARTESIAN_POINT('Ctrl Pts',(23.9093042536119,-1.53216005207464,
0.));
#216512=CARTESIAN_POINT('Ctrl Pts',(23.8889945285318,-1.53797715326759,
0.));
#216513=CARTESIAN_POINT('Ctrl Pts',(23.8687685639642,-1.54371284453992,
0.));
#216514=CARTESIAN_POINT('Ctrl Pts',(23.8486272290705,-1.54936729940542,
0.));
#216515=CARTESIAN_POINT('Ctrl Pts',(23.8285714027636,-1.55494069502636,
0.));
#216516=CARTESIAN_POINT('Ctrl Pts',(23.8086019739194,-1.56043321228635,
0.));
#216517=CARTESIAN_POINT('Ctrl Pts',(23.7887198415878,-1.56584503586844,
0.));
#216518=CARTESIAN_POINT('Ctrl Pts',(23.7689259151862,-1.57117635434409,
0.));
#216519=CARTESIAN_POINT('Ctrl Pts',(23.749221114736,-1.57642736025247,0.));
#216520=CARTESIAN_POINT('Ctrl Pts',(23.72960637113,-1.58159825017359,0.));
#216521=CARTESIAN_POINT('Ctrl Pts',(23.710082626383,-1.58668922481222,0.));
#216522=CARTESIAN_POINT('Ctrl Pts',(23.6906508338833,-1.59170048908634,
0.));
#216523=CARTESIAN_POINT('Ctrl Pts',(23.671311958631,-1.59663225222464,0.));
#216524=CARTESIAN_POINT('Ctrl Pts',(23.6520669774876,-1.60148472786596,
0.));
#216525=CARTESIAN_POINT('Ctrl Pts',(23.6329168794929,-1.60625813414674,
0.));
#216526=CARTESIAN_POINT('Ctrl Pts',(23.6138626661653,-1.61095269379779,
0.));
#216527=CARTESIAN_POINT('Ctrl Pts',(23.5949053517997,-1.61556863424699,
0.));
#216528=CARTESIAN_POINT('Ctrl Pts',(23.57604596376,-1.62010618772867,0.));
#216529=CARTESIAN_POINT('Ctrl Pts',(23.5572855427601,-1.62456559140066,
0.));
#216530=CARTESIAN_POINT('Ctrl Pts',(23.538625143226,-1.62894708745224,0.));
#216531=CARTESIAN_POINT('Ctrl Pts',(23.5200658336612,-1.63325092321727,
0.));
#216532=CARTESIAN_POINT('Ctrl Pts',(23.5016086970003,-1.63747735129475,
0.));
#216533=CARTESIAN_POINT('Ctrl Pts',(23.4832548309645,-1.64162662967529,
0.));
#216534=CARTESIAN_POINT('Ctrl Pts',(23.4650053483932,-1.64569902187612,
0.));
#216535=CARTESIAN_POINT('Ctrl Pts',(23.4468613776574,-1.64969479707341,
0.));
#216536=CARTESIAN_POINT('Ctrl Pts',(23.4288240631043,-1.6536142302373,0.));
#216537=CARTESIAN_POINT('Ctrl Pts',(23.4108945654805,-1.65745760227506,
0.));
#216538=CARTESIAN_POINT('Ctrl Pts',(23.3930740623619,-1.66122520018012,
0.));
#216539=CARTESIAN_POINT('Ctrl Pts',(23.3753637485545,-1.66491731718878,
0.));
#216540=CARTESIAN_POINT('Ctrl Pts',(23.3577648365744,-1.66853425293997,
0.));
#216541=CARTESIAN_POINT('Ctrl Pts',(23.3402785571865,-1.67207631363923,
0.));
#216542=CARTESIAN_POINT('Ctrl Pts',(23.3229061599144,-1.67554381222995,
0.));
#216543=CARTESIAN_POINT('Ctrl Pts',(23.3056489135611,-1.67893706857118,
0.));
#216544=CARTESIAN_POINT('Ctrl Pts',(23.2885081066951,-1.68225640962169,
0.));
#216545=CARTESIAN_POINT('Ctrl Pts',(23.2714850482246,-1.68550216963259,
0.));
#216546=CARTESIAN_POINT('Ctrl Pts',(23.2545810680537,-1.68867469034897,
0.));
#216547=CARTESIAN_POINT('Ctrl Pts',(23.2377975177013,-1.69177432121712,
0.));
#216548=CARTESIAN_POINT('Ctrl Pts',(23.2211357709374,-1.69480141959954,
0.));
#216549=CARTESIAN_POINT('Ctrl Pts',(23.2045972243767,-1.69775635099444,
0.));
#216550=CARTESIAN_POINT('Ctrl Pts',(23.1881832981851,-1.70063948927011,
0.));
#216551=CARTESIAN_POINT('Ctrl Pts',(23.1718954368751,-1.70345121691278,
0.));
#216552=CARTESIAN_POINT('Ctrl Pts',(23.1557351100614,-1.70619192527853,
0.));
#216553=CARTESIAN_POINT('Ctrl Pts',(23.1397038132356,-1.70886201485453,
0.));
#216554=CARTESIAN_POINT('Ctrl Pts',(23.1238030684925,-1.71146189552175,
0.));
#216555=CARTESIAN_POINT('Ctrl Pts',(23.1080344254286,-1.71399198684705,
0.));
#216556=CARTESIAN_POINT('Ctrl Pts',(23.0923994621213,-1.71645271839298,
0.));
#216557=CARTESIAN_POINT('Ctrl Pts',(23.0768997860708,-1.71884453003028,
0.));
#216558=CARTESIAN_POINT('Ctrl Pts',(23.0615370351562,-1.72116787225993,
0.));
#216559=CARTESIAN_POINT('Ctrl Pts',(23.0463128785531,-1.72342320653748,
0.));
#216560=CARTESIAN_POINT('Ctrl Pts',(23.0312290178883,-1.72561100564047,
0.));
#216561=CARTESIAN_POINT('Ctrl Pts',(23.0162871884168,-1.7277317540471,0.));
#216562=CARTESIAN_POINT('Ctrl Pts',(23.001489160189,-1.72978594832137,0.));
#216563=CARTESIAN_POINT('Ctrl Pts',(22.9868367391978,-1.73177409750192,
0.));
#216564=CARTESIAN_POINT('Ctrl Pts',(22.9723317685688,-1.73369672350816,
0.));
#216565=CARTESIAN_POINT('Ctrl Pts',(22.9579761301063,-1.73555436162771,
0.));
#216566=CARTESIAN_POINT('Ctrl Pts',(22.9437717457826,-1.7373475610004,0.));
#216567=CARTESIAN_POINT('Ctrl Pts',(22.9297205792586,-1.73907688511667,
0.));
#216568=CARTESIAN_POINT('Ctrl Pts',(22.9158246373363,-1.7407429123106,0.));
#216569=CARTESIAN_POINT('Ctrl Pts',(22.9020859716141,-1.74234623630081,
0.));
#216570=CARTESIAN_POINT('Ctrl Pts',(22.888506680335,-1.74388746677704,0.));
#216571=CARTESIAN_POINT('Ctrl Pts',(22.8750889101696,-1.74536722998202,
0.));
#216572=CARTESIAN_POINT('Ctrl Pts',(22.8618348580235,-1.74678616930666,
0.));
#216573=CARTESIAN_POINT('Ctrl Pts',(22.8487467728076,-1.74814494588494,
0.));
#216574=CARTESIAN_POINT('Ctrl Pts',(22.8358269579853,-1.74944423940117,
0.));
#216575=CARTESIAN_POINT('Ctrl Pts',(22.8230777741284,-1.75068474890884,
0.));
#216576=CARTESIAN_POINT('Ctrl Pts',(22.8105016414713,-1.75186719365593,
0.));
#216577=CARTESIAN_POINT('Ctrl Pts',(22.7981010424314,-1.75299231391468,
0.));
#216578=CARTESIAN_POINT('Ctrl Pts',(22.7858785242361,-1.75406087182937,
0.));
#216579=CARTESIAN_POINT('Ctrl Pts',(22.7738367016118,-1.75507365227133,
0.));
#216580=CARTESIAN_POINT('Ctrl Pts',(22.7619782595013,-1.75603146371642,
0.));
#216581=CARTESIAN_POINT('Ctrl Pts',(22.750305955645,-1.75693513908908,0.));
#216582=CARTESIAN_POINT('Ctrl Pts',(22.7388226235559,-1.75778553673245,
0.));
#216583=CARTESIAN_POINT('Ctrl Pts',(22.72753117773,-1.75858354204634,0.));
#216584=CARTESIAN_POINT('Ctrl Pts',(22.7164346186006,-1.75933006905926,
0.));
#216585=CARTESIAN_POINT('Ctrl Pts',(22.7055360375485,-1.76002606202402,
0.));
#216586=CARTESIAN_POINT('Ctrl Pts',(22.6948386219851,-1.76067249704888,
0.));
#216587=CARTESIAN_POINT('Ctrl Pts',(22.684345658525,-1.76127038310615,0.));
#216588=CARTESIAN_POINT('Ctrl Pts',(22.67406053567,-1.76182076289527,0.));
#216589=CARTESIAN_POINT('Ctrl Pts',(22.6639867471753,-1.7623247139257,0.));
#216590=CARTESIAN_POINT('Ctrl Pts',(22.6541278938409,-1.76278334912562,
0.));
#216591=CARTESIAN_POINT('Ctrl Pts',(22.6444876940423,-1.76319782013917,
0.));
#216592=CARTESIAN_POINT('Ctrl Pts',(22.6350699979359,-1.76356932176274,
0.));
#216593=CARTESIAN_POINT('Ctrl Pts',(22.6258787994848,-1.76389909571404,
0.));
#216594=CARTESIAN_POINT('Ctrl Pts',(22.6169182517694,-1.76418843543741,
0.));
#216595=CARTESIAN_POINT('Ctrl Pts',(22.6081926681343,-1.76443868648017,
0.));
#216596=CARTESIAN_POINT('Ctrl Pts',(22.5997065145638,-1.76465124413558,
0.));
#216597=CARTESIAN_POINT('Ctrl Pts',(22.5914644078105,-1.76482755288412,
0.));
#216598=CARTESIAN_POINT('Ctrl Pts',(22.5834711038022,-1.76496910283089,
0.));
#216599=CARTESIAN_POINT('Ctrl Pts',(22.5757315316353,-1.76507744026747,
0.));
#216600=CARTESIAN_POINT('Ctrl Pts',(22.5682508499873,-1.76515418518832,
0.));
#216601=CARTESIAN_POINT('Ctrl Pts',(22.5610344912501,-1.76520104500451,
0.));
#216602=CARTESIAN_POINT('Ctrl Pts',(22.5540882235837,-1.76521983384064,
0.));
#216603=CARTESIAN_POINT('Ctrl Pts',(22.5474180954006,-1.76521245524048,
0.));
#216604=CARTESIAN_POINT('Ctrl Pts',(22.5410303590892,-1.76518087841494,
0.));
#216605=CARTESIAN_POINT('Ctrl Pts',(22.5349313983571,-1.76512711563255,
0.));
#216606=CARTESIAN_POINT('Ctrl Pts',(22.529127665298,-1.7650532026276,0.));
#216607=CARTESIAN_POINT('Ctrl Pts',(22.5236259635515,-1.76496128643376,
0.));
#216608=CARTESIAN_POINT('Ctrl Pts',(22.5184336670207,-1.76485369319896,
0.));
#216609=CARTESIAN_POINT('Ctrl Pts',(22.5135590569554,-1.7647330328115,0.));
#216610=CARTESIAN_POINT('Ctrl Pts',(22.5090112700212,-1.76460218257314,
0.));
#216611=CARTESIAN_POINT('Ctrl Pts',(22.5047996391978,-1.76446408210366,
0.));
#216612=CARTESIAN_POINT('Ctrl Pts',(22.5009332677316,-1.76432160068739,
0.));
#216613=CARTESIAN_POINT('Ctrl Pts',(22.4974203063191,-1.76417731243484,
0.));
#216614=CARTESIAN_POINT('Ctrl Pts',(22.4942693792449,-1.76403393880317,
0.));
#216615=CARTESIAN_POINT('Ctrl Pts',(22.4914909094908,-1.76389475965715,
0.));
#216616=CARTESIAN_POINT('Ctrl Pts',(22.4890991659479,-1.76376424879469,
0.));
#216617=CARTESIAN_POINT('Ctrl Pts',(22.4871115206572,-1.76364784232927,
0.));
#216618=CARTESIAN_POINT('Ctrl Pts',(22.4855446605991,-1.7635507604555,0.));
#216619=CARTESIAN_POINT('Ctrl Pts',(22.4844112933125,-1.76347698284863,
0.));
#216620=CARTESIAN_POINT('Ctrl Pts',(22.4838562517064,-1.7634381343466,0.));
#216621=CARTESIAN_POINT('Ctrl Pts',(22.4836387052228,-1.76342064263638,
0.));
#216622=CARTESIAN_POINT('Ctrl Pts',(22.4835819929788,-1.76341415538792,
0.));
#216623=CARTESIAN_POINT('Ctrl Pts',(22.4835757167854,-1.76341220531181,
0.));
#216624=CARTESIAN_POINT('',(25.991588367311,-0.661312440730916,12.));
#216625=CARTESIAN_POINT('',(25.991588367311,-0.661312440730916,0.));
#216626=CARTESIAN_POINT('Ctrl Pts',(22.4835757167854,-1.76341220531181,
12.));
#216627=CARTESIAN_POINT('Ctrl Pts',(22.4835819929788,-1.76341415538792,
12.));
#216628=CARTESIAN_POINT('Ctrl Pts',(22.4836387052228,-1.76342064263638,
12.));
#216629=CARTESIAN_POINT('Ctrl Pts',(22.4838562517064,-1.7634381343466,12.));
#216630=CARTESIAN_POINT('Ctrl Pts',(22.4844112933125,-1.76347698284863,
12.));
#216631=CARTESIAN_POINT('Ctrl Pts',(22.4855446605991,-1.7635507604555,12.));
#216632=CARTESIAN_POINT('Ctrl Pts',(22.4871115206572,-1.76364784232927,
12.));
#216633=CARTESIAN_POINT('Ctrl Pts',(22.4890991659479,-1.76376424879469,
12.));
#216634=CARTESIAN_POINT('Ctrl Pts',(22.4914909094908,-1.76389475965715,
12.));
#216635=CARTESIAN_POINT('Ctrl Pts',(22.4942693792449,-1.76403393880317,
12.));
#216636=CARTESIAN_POINT('Ctrl Pts',(22.4974203063191,-1.76417731243484,
12.));
#216637=CARTESIAN_POINT('Ctrl Pts',(22.5009332677316,-1.76432160068739,
12.));
#216638=CARTESIAN_POINT('Ctrl Pts',(22.5047996391978,-1.76446408210366,
12.));
#216639=CARTESIAN_POINT('Ctrl Pts',(22.5090112700212,-1.76460218257314,
12.));
#216640=CARTESIAN_POINT('Ctrl Pts',(22.5135590569554,-1.7647330328115,12.));
#216641=CARTESIAN_POINT('Ctrl Pts',(22.5184336670207,-1.76485369319896,
12.));
#216642=CARTESIAN_POINT('Ctrl Pts',(22.5236259635515,-1.76496128643376,
12.));
#216643=CARTESIAN_POINT('Ctrl Pts',(22.529127665298,-1.7650532026276,12.));
#216644=CARTESIAN_POINT('Ctrl Pts',(22.5349313983571,-1.76512711563255,
12.));
#216645=CARTESIAN_POINT('Ctrl Pts',(22.5410303590892,-1.76518087841494,
12.));
#216646=CARTESIAN_POINT('Ctrl Pts',(22.5474180954006,-1.76521245524048,
12.));
#216647=CARTESIAN_POINT('Ctrl Pts',(22.5540882235837,-1.76521983384064,
12.));
#216648=CARTESIAN_POINT('Ctrl Pts',(22.5610344912501,-1.76520104500451,
12.));
#216649=CARTESIAN_POINT('Ctrl Pts',(22.5682508499873,-1.76515418518832,
12.));
#216650=CARTESIAN_POINT('Ctrl Pts',(22.5757315316353,-1.76507744026747,
12.));
#216651=CARTESIAN_POINT('Ctrl Pts',(22.5834711038022,-1.76496910283089,
12.));
#216652=CARTESIAN_POINT('Ctrl Pts',(22.5914644078105,-1.76482755288412,
12.));
#216653=CARTESIAN_POINT('Ctrl Pts',(22.5997065145638,-1.76465124413558,
12.));
#216654=CARTESIAN_POINT('Ctrl Pts',(22.6081926681343,-1.76443868648017,
12.));
#216655=CARTESIAN_POINT('Ctrl Pts',(22.6169182517694,-1.76418843543741,
12.));
#216656=CARTESIAN_POINT('Ctrl Pts',(22.6258787994848,-1.76389909571404,
12.));
#216657=CARTESIAN_POINT('Ctrl Pts',(22.6350699979359,-1.76356932176274,
12.));
#216658=CARTESIAN_POINT('Ctrl Pts',(22.6444876940423,-1.76319782013917,
12.));
#216659=CARTESIAN_POINT('Ctrl Pts',(22.6541278938409,-1.76278334912562,
12.));
#216660=CARTESIAN_POINT('Ctrl Pts',(22.6639867471753,-1.7623247139257,12.));
#216661=CARTESIAN_POINT('Ctrl Pts',(22.67406053567,-1.76182076289527,12.));
#216662=CARTESIAN_POINT('Ctrl Pts',(22.684345658525,-1.76127038310615,12.));
#216663=CARTESIAN_POINT('Ctrl Pts',(22.6948386219851,-1.76067249704888,
12.));
#216664=CARTESIAN_POINT('Ctrl Pts',(22.7055360375485,-1.76002606202402,
12.));
#216665=CARTESIAN_POINT('Ctrl Pts',(22.7164346186006,-1.75933006905926,
12.));
#216666=CARTESIAN_POINT('Ctrl Pts',(22.72753117773,-1.75858354204634,12.));
#216667=CARTESIAN_POINT('Ctrl Pts',(22.7388226235559,-1.75778553673245,
12.));
#216668=CARTESIAN_POINT('Ctrl Pts',(22.750305955645,-1.75693513908908,12.));
#216669=CARTESIAN_POINT('Ctrl Pts',(22.7619782595013,-1.75603146371642,
12.));
#216670=CARTESIAN_POINT('Ctrl Pts',(22.7738367016118,-1.75507365227133,
12.));
#216671=CARTESIAN_POINT('Ctrl Pts',(22.7858785242361,-1.75406087182937,
12.));
#216672=CARTESIAN_POINT('Ctrl Pts',(22.7981010424314,-1.75299231391468,
12.));
#216673=CARTESIAN_POINT('Ctrl Pts',(22.8105016414713,-1.75186719365593,
12.));
#216674=CARTESIAN_POINT('Ctrl Pts',(22.8230777741284,-1.75068474890884,
12.));
#216675=CARTESIAN_POINT('Ctrl Pts',(22.8358269579853,-1.74944423940117,
12.));
#216676=CARTESIAN_POINT('Ctrl Pts',(22.8487467728076,-1.74814494588494,
12.));
#216677=CARTESIAN_POINT('Ctrl Pts',(22.8618348580235,-1.74678616930666,
12.));
#216678=CARTESIAN_POINT('Ctrl Pts',(22.8750889101696,-1.74536722998202,
12.));
#216679=CARTESIAN_POINT('Ctrl Pts',(22.888506680335,-1.74388746677704,12.));
#216680=CARTESIAN_POINT('Ctrl Pts',(22.9020859716141,-1.74234623630081,
12.));
#216681=CARTESIAN_POINT('Ctrl Pts',(22.9158246373363,-1.7407429123106,12.));
#216682=CARTESIAN_POINT('Ctrl Pts',(22.9297205792586,-1.73907688511667,
12.));
#216683=CARTESIAN_POINT('Ctrl Pts',(22.9437717457826,-1.7373475610004,12.));
#216684=CARTESIAN_POINT('Ctrl Pts',(22.9579761301063,-1.73555436162771,
12.));
#216685=CARTESIAN_POINT('Ctrl Pts',(22.9723317685688,-1.73369672350816,
12.));
#216686=CARTESIAN_POINT('Ctrl Pts',(22.9868367391978,-1.73177409750192,
12.));
#216687=CARTESIAN_POINT('Ctrl Pts',(23.001489160189,-1.72978594832137,12.));
#216688=CARTESIAN_POINT('Ctrl Pts',(23.0162871884168,-1.7277317540471,12.));
#216689=CARTESIAN_POINT('Ctrl Pts',(23.0312290178883,-1.72561100564047,
12.));
#216690=CARTESIAN_POINT('Ctrl Pts',(23.0463128785531,-1.72342320653748,
12.));
#216691=CARTESIAN_POINT('Ctrl Pts',(23.0615370351562,-1.72116787225993,
12.));
#216692=CARTESIAN_POINT('Ctrl Pts',(23.0768997860708,-1.71884453003028,
12.));
#216693=CARTESIAN_POINT('Ctrl Pts',(23.0923994621213,-1.71645271839298,
12.));
#216694=CARTESIAN_POINT('Ctrl Pts',(23.1080344254286,-1.71399198684705,
12.));
#216695=CARTESIAN_POINT('Ctrl Pts',(23.1238030684925,-1.71146189552175,
12.));
#216696=CARTESIAN_POINT('Ctrl Pts',(23.1397038132356,-1.70886201485453,
12.));
#216697=CARTESIAN_POINT('Ctrl Pts',(23.1557351100614,-1.70619192527853,
12.));
#216698=CARTESIAN_POINT('Ctrl Pts',(23.1718954368751,-1.70345121691278,
12.));
#216699=CARTESIAN_POINT('Ctrl Pts',(23.1881832981851,-1.70063948927011,
12.));
#216700=CARTESIAN_POINT('Ctrl Pts',(23.2045972243767,-1.69775635099444,
12.));
#216701=CARTESIAN_POINT('Ctrl Pts',(23.2211357709374,-1.69480141959954,
12.));
#216702=CARTESIAN_POINT('Ctrl Pts',(23.2377975177013,-1.69177432121712,
12.));
#216703=CARTESIAN_POINT('Ctrl Pts',(23.2545810680537,-1.68867469034897,
12.));
#216704=CARTESIAN_POINT('Ctrl Pts',(23.2714850482246,-1.68550216963259,
12.));
#216705=CARTESIAN_POINT('Ctrl Pts',(23.2885081066951,-1.68225640962169,
12.));
#216706=CARTESIAN_POINT('Ctrl Pts',(23.3056489135611,-1.67893706857118,
12.));
#216707=CARTESIAN_POINT('Ctrl Pts',(23.3229061599144,-1.67554381222995,
12.));
#216708=CARTESIAN_POINT('Ctrl Pts',(23.3402785571865,-1.67207631363923,
12.));
#216709=CARTESIAN_POINT('Ctrl Pts',(23.3577648365744,-1.66853425293997,
12.));
#216710=CARTESIAN_POINT('Ctrl Pts',(23.3753637485545,-1.66491731718878,
12.));
#216711=CARTESIAN_POINT('Ctrl Pts',(23.3930740623619,-1.66122520018012,
12.));
#216712=CARTESIAN_POINT('Ctrl Pts',(23.4108945654805,-1.65745760227506,
12.));
#216713=CARTESIAN_POINT('Ctrl Pts',(23.4288240631043,-1.6536142302373,12.));
#216714=CARTESIAN_POINT('Ctrl Pts',(23.4468613776574,-1.64969479707341,
12.));
#216715=CARTESIAN_POINT('Ctrl Pts',(23.4650053483932,-1.64569902187612,
12.));
#216716=CARTESIAN_POINT('Ctrl Pts',(23.4832548309645,-1.64162662967529,
12.));
#216717=CARTESIAN_POINT('Ctrl Pts',(23.5016086970003,-1.63747735129475,
12.));
#216718=CARTESIAN_POINT('Ctrl Pts',(23.5200658336612,-1.63325092321727,
12.));
#216719=CARTESIAN_POINT('Ctrl Pts',(23.538625143226,-1.62894708745224,12.));
#216720=CARTESIAN_POINT('Ctrl Pts',(23.5572855427601,-1.62456559140066,
12.));
#216721=CARTESIAN_POINT('Ctrl Pts',(23.57604596376,-1.62010618772867,12.));
#216722=CARTESIAN_POINT('Ctrl Pts',(23.5949053517997,-1.61556863424699,
12.));
#216723=CARTESIAN_POINT('Ctrl Pts',(23.6138626661653,-1.61095269379779,
12.));
#216724=CARTESIAN_POINT('Ctrl Pts',(23.6329168794929,-1.60625813414674,
12.));
#216725=CARTESIAN_POINT('Ctrl Pts',(23.6520669774876,-1.60148472786596,
12.));
#216726=CARTESIAN_POINT('Ctrl Pts',(23.671311958631,-1.59663225222464,12.));
#216727=CARTESIAN_POINT('Ctrl Pts',(23.6906508338833,-1.59170048908634,
12.));
#216728=CARTESIAN_POINT('Ctrl Pts',(23.710082626383,-1.58668922481222,12.));
#216729=CARTESIAN_POINT('Ctrl Pts',(23.72960637113,-1.58159825017359,12.));
#216730=CARTESIAN_POINT('Ctrl Pts',(23.749221114736,-1.57642736025247,12.));
#216731=CARTESIAN_POINT('Ctrl Pts',(23.7689259151862,-1.57117635434409,
12.));
#216732=CARTESIAN_POINT('Ctrl Pts',(23.7887198415878,-1.56584503586844,
12.));
#216733=CARTESIAN_POINT('Ctrl Pts',(23.8086019739194,-1.56043321228635,
12.));
#216734=CARTESIAN_POINT('Ctrl Pts',(23.8285714027636,-1.55494069502636,
12.));
#216735=CARTESIAN_POINT('Ctrl Pts',(23.8486272290705,-1.54936729940542,
12.));
#216736=CARTESIAN_POINT('Ctrl Pts',(23.8687685639642,-1.54371284453992,
12.));
#216737=CARTESIAN_POINT('Ctrl Pts',(23.8889945285318,-1.53797715326759,
12.));
#216738=CARTESIAN_POINT('Ctrl Pts',(23.9093042536119,-1.53216005207464,
12.));
#216739=CARTESIAN_POINT('Ctrl Pts',(23.9296968795757,-1.52626137103033,
12.));
#216740=CARTESIAN_POINT('Ctrl Pts',(23.9501715561033,-1.52028094372793,
12.));
#216741=CARTESIAN_POINT('Ctrl Pts',(23.970727442014,-1.51421860720616,12.));
#216742=CARTESIAN_POINT('Ctrl Pts',(23.9913637050927,-1.50807420187695,
12.));
#216743=CARTESIAN_POINT('Ctrl Pts',(24.0120795219086,-1.501847571461,12.));
#216744=CARTESIAN_POINT('Ctrl Pts',(24.0328740776331,-1.49553856292802,
12.));
#216745=CARTESIAN_POINT('Ctrl Pts',(24.0537465658429,-1.48914702644889,
12.));
#216746=CARTESIAN_POINT('Ctrl Pts',(24.0746961883528,-1.48267281533684,
12.));
#216747=CARTESIAN_POINT('Ctrl Pts',(24.0957221550778,-1.47611578597743,
12.));
#216748=CARTESIAN_POINT('Ctrl Pts',(24.1168236838824,-1.46947579776993,
12.));
#216749=CARTESIAN_POINT('Ctrl Pts',(24.1380000004272,-1.46275271307399,
12.));
#216750=CARTESIAN_POINT('Ctrl Pts',(24.1592503380107,-1.45594639716319,
12.));
#216751=CARTESIAN_POINT('Ctrl Pts',(24.1805739374038,-1.44905671818729,
12.));
#216752=CARTESIAN_POINT('Ctrl Pts',(24.201970046722,-1.44208354711083,12.));
#216753=CARTESIAN_POINT('Ctrl Pts',(24.2234379212984,-1.4350267576551,12.));
#216754=CARTESIAN_POINT('Ctrl Pts',(24.2449768235488,-1.42788622624855,
12.));
#216755=CARTESIAN_POINT('Ctrl Pts',(24.2665860228356,-1.42066183198254,
12.));
#216756=CARTESIAN_POINT('Ctrl Pts',(24.288264795321,-1.41335345657684,12.));
#216757=CARTESIAN_POINT('Ctrl Pts',(24.3100124238311,-1.40596098434339,
12.));
#216758=CARTESIAN_POINT('Ctrl Pts',(24.3318281977643,-1.39848430212808,
12.));
#216759=CARTESIAN_POINT('Ctrl Pts',(24.3537114129875,-1.3909232992639,12.));
#216760=CARTESIAN_POINT('Ctrl Pts',(24.3756613717299,-1.38327786753,12.));
#216761=CARTESIAN_POINT('Ctrl Pts',(24.3976773824732,-1.37554790111611,
12.));
#216762=CARTESIAN_POINT('Ctrl Pts',(24.4197587598337,-1.36773329659958,
12.));
#216763=CARTESIAN_POINT('Ctrl Pts',(24.4419048244523,-1.35983395290629,
12.));
#216764=CARTESIAN_POINT('Ctrl Pts',(24.4641149028892,-1.35184977125649,
12.));
#216765=CARTESIAN_POINT('Ctrl Pts',(24.4863883275134,-1.34378065512339,
12.));
#216766=CARTESIAN_POINT('Ctrl Pts',(24.5087244363856,-1.33562651019687,
12.));
#216767=CARTESIAN_POINT('Ctrl Pts',(24.5311225731435,-1.32738724435327,
12.));
#216768=CARTESIAN_POINT('Ctrl Pts',(24.5535820868674,-1.31906276763669,
12.));
#216769=CARTESIAN_POINT('Ctrl Pts',(24.5761023320183,-1.31065299222023,
12.));
#216770=CARTESIAN_POINT('Ctrl Pts',(24.5986826684027,-1.30215783236363,
12.));
#216771=CARTESIAN_POINT('Ctrl Pts',(24.6213224611229,-1.29357720438108,
12.));
#216772=CARTESIAN_POINT('Ctrl Pts',(24.6440210805278,-1.28491102661515,
12.));
#216773=CARTESIAN_POINT('Ctrl Pts',(24.6667779021559,-1.27615921941643,
12.));
#216774=CARTESIAN_POINT('Ctrl Pts',(24.6895923066836,-1.26732170513501,
12.));
#216775=CARTESIAN_POINT('Ctrl Pts',(24.7124636797894,-1.25839840807419,
12.));
#216776=CARTESIAN_POINT('Ctrl Pts',(24.7353914120011,-1.24938925444327,
12.));
#216777=CARTESIAN_POINT('Ctrl Pts',(24.7583748985438,-1.2402941723199,12.));
#216778=CARTESIAN_POINT('Ctrl Pts',(24.7814135391799,-1.23111309161845,
12.));
#216779=CARTESIAN_POINT('Ctrl Pts',(24.8045067380536,-1.22184594406529,
12.));
#216780=CARTESIAN_POINT('Ctrl Pts',(24.8276539035092,-1.21249266318209,
12.));
#216781=CARTESIAN_POINT('Ctrl Pts',(24.8508544481974,-1.20305318426021,
12.));
#216782=CARTESIAN_POINT('Ctrl Pts',(24.8741077892075,-1.19352744434066,
12.));
#216783=CARTESIAN_POINT('Ctrl Pts',(24.8974133481829,-1.18391538220104,
12.));
#216784=CARTESIAN_POINT('Ctrl Pts',(24.9207705514448,-1.17421693835042,
12.));
#216785=CARTESIAN_POINT('Ctrl Pts',(24.9441788300932,-1.16443205502851,
12.));
#216786=CARTESIAN_POINT('Ctrl Pts',(24.9676376201502,-1.15456067621891,
12.));
#216787=CARTESIAN_POINT('Ctrl Pts',(24.9911463621433,-1.14460274758202,
12.));
#216788=CARTESIAN_POINT('Ctrl Pts',(25.0147045006195,-1.13455821638531,
12.));
#216789=CARTESIAN_POINT('Ctrl Pts',(25.0383114836899,-1.12442703144453,
12.));
#216790=CARTESIAN_POINT('Ctrl Pts',(25.0619667625336,-1.11420914306891,
12.));
#216791=CARTESIAN_POINT('Ctrl Pts',(25.0856697909679,-1.10390450301747,
12.));
#216792=CARTESIAN_POINT('Ctrl Pts',(25.1094200248446,-1.09351306445309,
12.));
#216793=CARTESIAN_POINT('Ctrl Pts',(25.1332169227413,-1.08303478197189,
12.));
#216794=CARTESIAN_POINT('Ctrl Pts',(25.157059946931,-1.07246961165477,12.));
#216795=CARTESIAN_POINT('Ctrl Pts',(25.1809485642192,-1.06181751111769,
12.));
#216796=CARTESIAN_POINT('Ctrl Pts',(25.2048822469028,-1.05107843957933,
12.));
#216797=CARTESIAN_POINT('Ctrl Pts',(25.2288604735086,-1.04025235791508,
12.));
#216798=CARTESIAN_POINT('Ctrl Pts',(25.2528827300422,-1.02933922876807,
12.));
#216799=CARTESIAN_POINT('Ctrl Pts',(25.276948508726,-1.01833901642238,12.));
#216800=CARTESIAN_POINT('Ctrl Pts',(25.3010573055547,-1.00725168656897,
12.));
#216801=CARTESIAN_POINT('Ctrl Pts',(25.3252086182968,-0.996077206120637,
12.));
#216802=CARTESIAN_POINT('Ctrl Pts',(25.3494019441441,-0.984815543003986,
12.));
#216803=CARTESIAN_POINT('Ctrl Pts',(25.3736367778845,-0.973466666000178,
12.));
#216804=CARTESIAN_POINT('Ctrl Pts',(25.3979126089163,-0.962030544503156,
12.));
#216805=CARTESIAN_POINT('Ctrl Pts',(25.4222289223167,-0.950507148597483,
12.));
#216806=CARTESIAN_POINT('Ctrl Pts',(25.4465852044849,-0.938896449496205,
12.));
#216807=CARTESIAN_POINT('Ctrl Pts',(25.4709809475009,-0.927198419886108,
12.));
#216808=CARTESIAN_POINT('Ctrl Pts',(25.4954156541795,-0.915413034335626,
12.));
#216809=CARTESIAN_POINT('Ctrl Pts',(25.5198888424194,-0.903540269651121,
12.));
#216810=CARTESIAN_POINT('Ctrl Pts',(25.5444000508211,-0.891580105349052,
12.));
#216811=CARTESIAN_POINT('Ctrl Pts',(25.5689488408156,-0.879532523834308,
12.));
#216812=CARTESIAN_POINT('Ctrl Pts',(25.5935347843585,-0.867397509338443,
12.));
#216813=CARTESIAN_POINT('Ctrl Pts',(25.6181574536049,-0.855175047036563,
12.));
#216814=CARTESIAN_POINT('Ctrl Pts',(25.6428164100055,-0.842865122120773,
12.));
#216815=CARTESIAN_POINT('Ctrl Pts',(25.6675111931952,-0.830467718864221,
12.));
#216816=CARTESIAN_POINT('Ctrl Pts',(25.6922413110194,-0.817982819787478,
12.));
#216817=CARTESIAN_POINT('Ctrl Pts',(25.7170062262525,-0.805410404554366,
12.));
#216818=CARTESIAN_POINT('Ctrl Pts',(25.7418053757746,-0.79275045161614,
12.));
#216819=CARTESIAN_POINT('Ctrl Pts',(25.7666381946955,-0.780002940291977,
12.));
#216820=CARTESIAN_POINT('Ctrl Pts',(25.7915041383376,-0.767167852651183,
12.));
#216821=CARTESIAN_POINT('Ctrl Pts',(25.8164027059984,-0.754245175609537,
12.));
#216822=CARTESIAN_POINT('Ctrl Pts',(25.8413334619054,-0.74123490266382,
12.));
#216823=CARTESIAN_POINT('Ctrl Pts',(25.8662960624185,-0.728137036482349,
12.));
#216824=CARTESIAN_POINT('Ctrl Pts',(25.8912902614969,-0.714951588527653,
12.));
#216825=CARTESIAN_POINT('Ctrl Pts',(25.9163158909426,-0.701678575228769,
12.));
#216826=CARTESIAN_POINT('Ctrl Pts',(25.9413728471909,-0.688318015057744,
12.));
#216827=CARTESIAN_POINT('Ctrl Pts',(25.9614434297919,-0.67755954320974,
12.));
#216828=CARTESIAN_POINT('Ctrl Pts',(25.9765104298071,-0.669451306780839,
12.));
#216829=CARTESIAN_POINT('Ctrl Pts',(25.9865613464773,-0.66402831318764,
12.));
#216830=CARTESIAN_POINT('Ctrl Pts',(25.991588367311,-0.661312440730916,
12.));
#216831=CARTESIAN_POINT('Ctrl Pts',(22.1738711152697,-4.11585220600463,
0.));
#216832=CARTESIAN_POINT('Ctrl Pts',(22.1738711152697,-4.11585220600463,
12.));
#216833=CARTESIAN_POINT('Ctrl Pts',(22.173877682324,-4.11585194677443,0.));
#216834=CARTESIAN_POINT('Ctrl Pts',(22.173877682324,-4.11585194677443,12.));
#216835=CARTESIAN_POINT('Ctrl Pts',(22.1739341411687,-4.11586035878288,
0.));
#216836=CARTESIAN_POINT('Ctrl Pts',(22.1739341411687,-4.11586035878288,
12.));
#216837=CARTESIAN_POINT('Ctrl Pts',(22.1741488021234,-4.11589976826168,
0.));
#216838=CARTESIAN_POINT('Ctrl Pts',(22.1741488021234,-4.11589976826168,
12.));
#216839=CARTESIAN_POINT('Ctrl Pts',(22.1746949858775,-4.11600589882846,
0.));
#216840=CARTESIAN_POINT('Ctrl Pts',(22.1746949858775,-4.11600589882846,
12.));
#216841=CARTESIAN_POINT('Ctrl Pts',(22.1758088296598,-4.1162279721707,0.));
#216842=CARTESIAN_POINT('Ctrl Pts',(22.1758088296598,-4.1162279721707,12.));
#216843=CARTESIAN_POINT('Ctrl Pts',(22.177347426894,-4.11653973150519,0.));
#216844=CARTESIAN_POINT('Ctrl Pts',(22.177347426894,-4.11653973150519,12.));
#216845=CARTESIAN_POINT('Ctrl Pts',(22.179297473024,-4.11694173195005,0.));
#216846=CARTESIAN_POINT('Ctrl Pts',(22.179297473024,-4.11694173195005,12.));
#216847=CARTESIAN_POINT('Ctrl Pts',(22.1816414985788,-4.11743469691757,
0.));
#216848=CARTESIAN_POINT('Ctrl Pts',(22.1816414985788,-4.11743469691757,
12.));
#216849=CARTESIAN_POINT('Ctrl Pts',(22.1843613164855,-4.11801938107481,
0.));
#216850=CARTESIAN_POINT('Ctrl Pts',(22.1843613164855,-4.11801938107481,
12.));
#216851=CARTESIAN_POINT('Ctrl Pts',(22.1874419861496,-4.11869641271775,
0.));
#216852=CARTESIAN_POINT('Ctrl Pts',(22.1874419861496,-4.11869641271775,
12.));
#216853=CARTESIAN_POINT('Ctrl Pts',(22.1908725908525,-4.11946626228637,
0.));
#216854=CARTESIAN_POINT('Ctrl Pts',(22.1908725908525,-4.11946626228637,
12.));
#216855=CARTESIAN_POINT('Ctrl Pts',(22.1946440958098,-4.12032932637738,
0.));
#216856=CARTESIAN_POINT('Ctrl Pts',(22.1946440958098,-4.12032932637738,
12.));
#216857=CARTESIAN_POINT('Ctrl Pts',(22.1987479618246,-4.12128598183523,
0.));
#216858=CARTESIAN_POINT('Ctrl Pts',(22.1987479618246,-4.12128598183523,
12.));
#216859=CARTESIAN_POINT('Ctrl Pts',(22.2031746532106,-4.12233664408228,
0.));
#216860=CARTESIAN_POINT('Ctrl Pts',(22.2031746532106,-4.12233664408228,
12.));
#216861=CARTESIAN_POINT('Ctrl Pts',(22.2079143941719,-4.12348173702024,
0.));
#216862=CARTESIAN_POINT('Ctrl Pts',(22.2079143941719,-4.12348173702024,
12.));
#216863=CARTESIAN_POINT('Ctrl Pts',(22.2129576146671,-4.12472167516608,
0.));
#216864=CARTESIAN_POINT('Ctrl Pts',(22.2129576146671,-4.12472167516608,
12.));
#216865=CARTESIAN_POINT('Ctrl Pts',(22.2182956401341,-4.12605683613308,
0.));
#216866=CARTESIAN_POINT('Ctrl Pts',(22.2182956401341,-4.12605683613308,
12.));
#216867=CARTESIAN_POINT('Ctrl Pts',(22.2239207458781,-4.12748755830105,
0.));
#216868=CARTESIAN_POINT('Ctrl Pts',(22.2239207458781,-4.12748755830105,
12.));
#216869=CARTESIAN_POINT('Ctrl Pts',(22.2298258043947,-4.1290141546338,0.));
#216870=CARTESIAN_POINT('Ctrl Pts',(22.2298258043947,-4.1290141546338,12.));
#216871=CARTESIAN_POINT('Ctrl Pts',(22.2360040565533,-4.13063692157499,
0.));
#216872=CARTESIAN_POINT('Ctrl Pts',(22.2360040565533,-4.13063692157499,
12.));
#216873=CARTESIAN_POINT('Ctrl Pts',(22.2424488153523,-4.13235615060161,
0.));
#216874=CARTESIAN_POINT('Ctrl Pts',(22.2424488153523,-4.13235615060161,
12.));
#216875=CARTESIAN_POINT('Ctrl Pts',(22.249153531779,-4.13417212558811,0.));
#216876=CARTESIAN_POINT('Ctrl Pts',(22.249153531779,-4.13417212558811,12.));
#216877=CARTESIAN_POINT('Ctrl Pts',(22.2561118708421,-4.13608511977227,
0.));
#216878=CARTESIAN_POINT('Ctrl Pts',(22.2561118708421,-4.13608511977227,
12.));
#216879=CARTESIAN_POINT('Ctrl Pts',(22.2633177913972,-4.13809539255423,
0.));
#216880=CARTESIAN_POINT('Ctrl Pts',(22.2633177913972,-4.13809539255423,
12.));
#216881=CARTESIAN_POINT('Ctrl Pts',(22.2707656042457,-4.14020318715992,
0.));
#216882=CARTESIAN_POINT('Ctrl Pts',(22.2707656042457,-4.14020318715992,
12.));
#216883=CARTESIAN_POINT('Ctrl Pts',(22.2784499072027,-4.14240873321985,
0.));
#216884=CARTESIAN_POINT('Ctrl Pts',(22.2784499072027,-4.14240873321985,
12.));
#216885=CARTESIAN_POINT('Ctrl Pts',(22.2863655389166,-4.14471224859297,
0.));
#216886=CARTESIAN_POINT('Ctrl Pts',(22.2863655389166,-4.14471224859297,
12.));
#216887=CARTESIAN_POINT('Ctrl Pts',(22.2945075198467,-4.14711394168557,
0.));
#216888=CARTESIAN_POINT('Ctrl Pts',(22.2945075198467,-4.14711394168557,
12.));
#216889=CARTESIAN_POINT('Ctrl Pts',(22.3028710166933,-4.14961401285523,
0.));
#216890=CARTESIAN_POINT('Ctrl Pts',(22.3028710166933,-4.14961401285523,
12.));
#216891=CARTESIAN_POINT('Ctrl Pts',(22.3114513545185,-4.15221265396991,
0.));
#216892=CARTESIAN_POINT('Ctrl Pts',(22.3114513545185,-4.15221265396991,
12.));
#216893=CARTESIAN_POINT('Ctrl Pts',(22.3202440186979,-4.15491004835282,
0.));
#216894=CARTESIAN_POINT('Ctrl Pts',(22.3202440186979,-4.15491004835282,
12.));
#216895=CARTESIAN_POINT('Ctrl Pts',(22.3292446628959,-4.15770637047891,
0.));
#216896=CARTESIAN_POINT('Ctrl Pts',(22.3292446628959,-4.15770637047891,
12.));
#216897=CARTESIAN_POINT('Ctrl Pts',(22.3384491078602,-4.16060178604165,
0.));
#216898=CARTESIAN_POINT('Ctrl Pts',(22.3384491078602,-4.16060178604165,
12.));
#216899=CARTESIAN_POINT('Ctrl Pts',(22.3478533253889,-4.16359645263189,
0.));
#216900=CARTESIAN_POINT('Ctrl Pts',(22.3478533253889,-4.16359645263189,
12.));
#216901=CARTESIAN_POINT('Ctrl Pts',(22.3574534257396,-4.16669052026601,
0.));
#216902=CARTESIAN_POINT('Ctrl Pts',(22.3574534257396,-4.16669052026601,
12.));
#216903=CARTESIAN_POINT('Ctrl Pts',(22.3672456427599,-4.16988413199458,
0.));
#216904=CARTESIAN_POINT('Ctrl Pts',(22.3672456427599,-4.16988413199458,
12.));
#216905=CARTESIAN_POINT('Ctrl Pts',(22.3772263228617,-4.17317742436146,
0.));
#216906=CARTESIAN_POINT('Ctrl Pts',(22.3772263228617,-4.17317742436146,
12.));
#216907=CARTESIAN_POINT('Ctrl Pts',(22.3873919231334,-4.17657052752826,
0.));
#216908=CARTESIAN_POINT('Ctrl Pts',(22.3873919231334,-4.17657052752826,
12.));
#216909=CARTESIAN_POINT('Ctrl Pts',(22.3977390078075,-4.18006356544883,
0.));
#216910=CARTESIAN_POINT('Ctrl Pts',(22.3977390078075,-4.18006356544883,
12.));
#216911=CARTESIAN_POINT('Ctrl Pts',(22.4082642454453,-4.18365665600852,
0.));
#216912=CARTESIAN_POINT('Ctrl Pts',(22.4082642454453,-4.18365665600852,
12.));
#216913=CARTESIAN_POINT('Ctrl Pts',(22.4189644056115,-4.18734991117722,
0.));
#216914=CARTESIAN_POINT('Ctrl Pts',(22.4189644056115,-4.18734991117722,
12.));
#216915=CARTESIAN_POINT('Ctrl Pts',(22.4298363535421,-4.19114343726943,
0.));
#216916=CARTESIAN_POINT('Ctrl Pts',(22.4298363535421,-4.19114343726943,
12.));
#216917=CARTESIAN_POINT('Ctrl Pts',(22.4408770448917,-4.19503733518862,
0.));
#216918=CARTESIAN_POINT('Ctrl Pts',(22.4408770448917,-4.19503733518862,
12.));
#216919=CARTESIAN_POINT('Ctrl Pts',(22.4520835205419,-4.19903170066356,
0.));
#216920=CARTESIAN_POINT('Ctrl Pts',(22.4520835205419,-4.19903170066356,
12.));
#216921=CARTESIAN_POINT('Ctrl Pts',(22.4634529011433,-4.20312662448172,
0.));
#216922=CARTESIAN_POINT('Ctrl Pts',(22.4634529011433,-4.20312662448172,
12.));
#216923=CARTESIAN_POINT('Ctrl Pts',(22.4749823839915,-4.20732219265649,
0.));
#216924=CARTESIAN_POINT('Ctrl Pts',(22.4749823839915,-4.20732219265649,
12.));
#216925=CARTESIAN_POINT('Ctrl Pts',(22.4866692403147,-4.21161848657429,
0.));
#216926=CARTESIAN_POINT('Ctrl Pts',(22.4866692403147,-4.21161848657429,
12.));
#216927=CARTESIAN_POINT('Ctrl Pts',(22.4985108124229,-4.21601558313909,
0.));
#216928=CARTESIAN_POINT('Ctrl Pts',(22.4985108124229,-4.21601558313909,
12.));
#216929=CARTESIAN_POINT('Ctrl Pts',(22.5105045108882,-4.22051355490198,
0.));
#216930=CARTESIAN_POINT('Ctrl Pts',(22.5105045108882,-4.22051355490198,
12.));
#216931=CARTESIAN_POINT('Ctrl Pts',(22.5226478117885,-4.22511247020041,
0.));
#216932=CARTESIAN_POINT('Ctrl Pts',(22.5226478117885,-4.22511247020041,
12.));
#216933=CARTESIAN_POINT('Ctrl Pts',(22.5349382540587,-4.22981239330733,
0.));
#216934=CARTESIAN_POINT('Ctrl Pts',(22.5349382540587,-4.22981239330733,
12.));
#216935=CARTESIAN_POINT('Ctrl Pts',(22.5473734368086,-4.23461338456714,
0.));
#216936=CARTESIAN_POINT('Ctrl Pts',(22.5473734368086,-4.23461338456714,
12.));
#216937=CARTESIAN_POINT('Ctrl Pts',(22.559951016643,-4.23951550052527,0.));
#216938=CARTESIAN_POINT('Ctrl Pts',(22.559951016643,-4.23951550052527,12.));
#216939=CARTESIAN_POINT('Ctrl Pts',(22.5726687049922,-4.2445187940486,0.));
#216940=CARTESIAN_POINT('Ctrl Pts',(22.5726687049922,-4.2445187940486,12.));
#216941=CARTESIAN_POINT('Ctrl Pts',(22.5855242662479,-4.24962331444186,
0.));
#216942=CARTESIAN_POINT('Ctrl Pts',(22.5855242662479,-4.24962331444186,
12.));
#216943=CARTESIAN_POINT('Ctrl Pts',(22.5985155158637,-4.25482910755486,
0.));
#216944=CARTESIAN_POINT('Ctrl Pts',(22.5985155158637,-4.25482910755486,
12.));
#216945=CARTESIAN_POINT('Ctrl Pts',(22.611640318482,-4.26013621588304,0.));
#216946=CARTESIAN_POINT('Ctrl Pts',(22.611640318482,-4.26013621588304,12.));
#216947=CARTESIAN_POINT('Ctrl Pts',(22.6248965859975,-4.26554467865572,
0.));
#216948=CARTESIAN_POINT('Ctrl Pts',(22.6248965859975,-4.26554467865572,
12.));
#216949=CARTESIAN_POINT('Ctrl Pts',(22.6382822758171,-4.27105453193,0.));
#216950=CARTESIAN_POINT('Ctrl Pts',(22.6382822758171,-4.27105453193,12.));
#216951=CARTESIAN_POINT('Ctrl Pts',(22.6517953893303,-4.27666580869118,
0.));
#216952=CARTESIAN_POINT('Ctrl Pts',(22.6517953893303,-4.27666580869118,
12.));
#216953=CARTESIAN_POINT('Ctrl Pts',(22.665433970311,-4.2823785389406,0.));
#216954=CARTESIAN_POINT('Ctrl Pts',(22.665433970311,-4.2823785389406,12.));
#216955=CARTESIAN_POINT('Ctrl Pts',(22.6791961033536,-4.28819274977767,
0.));
#216956=CARTESIAN_POINT('Ctrl Pts',(22.6791961033536,-4.28819274977767,
12.));
#216957=CARTESIAN_POINT('Ctrl Pts',(22.6930799122545,-4.29410846547062,
0.));
#216958=CARTESIAN_POINT('Ctrl Pts',(22.6930799122545,-4.29410846547062,
12.));
#216959=CARTESIAN_POINT('Ctrl Pts',(22.707083558756,-4.30012570754067,0.));
#216960=CARTESIAN_POINT('Ctrl Pts',(22.707083558756,-4.30012570754067,12.));
#216961=CARTESIAN_POINT('Ctrl Pts',(22.7212052413384,-4.30624449484075,
0.));
#216962=CARTESIAN_POINT('Ctrl Pts',(22.7212052413384,-4.30624449484075,
12.));
#216963=CARTESIAN_POINT('Ctrl Pts',(22.7354431939926,-4.31246484362551,
0.));
#216964=CARTESIAN_POINT('Ctrl Pts',(22.7354431939926,-4.31246484362551,
12.));
#216965=CARTESIAN_POINT('Ctrl Pts',(22.7497956849852,-4.31878676761231,
0.));
#216966=CARTESIAN_POINT('Ctrl Pts',(22.7497956849852,-4.31878676761231,
12.));
#216967=CARTESIAN_POINT('Ctrl Pts',(22.764261015648,-4.32521027803748,0.));
#216968=CARTESIAN_POINT('Ctrl Pts',(22.764261015648,-4.32521027803748,12.));
#216969=CARTESIAN_POINT('Ctrl Pts',(22.7788375194081,-4.33173538373183,
0.));
#216970=CARTESIAN_POINT('Ctrl Pts',(22.7788375194081,-4.33173538373183,
12.));
#216971=CARTESIAN_POINT('Ctrl Pts',(22.7935235607807,-4.33836209118444,
0.));
#216972=CARTESIAN_POINT('Ctrl Pts',(22.7935235607807,-4.33836209118444,
12.));
#216973=CARTESIAN_POINT('Ctrl Pts',(22.808317534379,-4.34509040460066,0.));
#216974=CARTESIAN_POINT('Ctrl Pts',(22.808317534379,-4.34509040460066,12.));
#216975=CARTESIAN_POINT('Ctrl Pts',(22.8232178638873,-4.35192032594802,
0.));
#216976=CARTESIAN_POINT('Ctrl Pts',(22.8232178638873,-4.35192032594802,
12.));
#216977=CARTESIAN_POINT('Ctrl Pts',(22.838223001118,-4.3588518550056,0.));
#216978=CARTESIAN_POINT('Ctrl Pts',(22.838223001118,-4.3588518550056,12.));
#216979=CARTESIAN_POINT('Ctrl Pts',(22.8533314252419,-4.36588498943011,
0.));
#216980=CARTESIAN_POINT('Ctrl Pts',(22.8533314252419,-4.36588498943011,
12.));
#216981=CARTESIAN_POINT('Ctrl Pts',(22.8685416419725,-4.37301972480753,
0.));
#216982=CARTESIAN_POINT('Ctrl Pts',(22.8685416419725,-4.37301972480753,
12.));
#216983=CARTESIAN_POINT('Ctrl Pts',(22.8838521827702,-4.38025605470091,
0.));
#216984=CARTESIAN_POINT('Ctrl Pts',(22.8838521827702,-4.38025605470091,
12.));
#216985=CARTESIAN_POINT('Ctrl Pts',(22.8992616040108,-4.38759397068393,
0.));
#216986=CARTESIAN_POINT('Ctrl Pts',(22.8992616040108,-4.38759397068393,
12.));
#216987=CARTESIAN_POINT('Ctrl Pts',(22.9147684862425,-4.39503346238455,
0.));
#216988=CARTESIAN_POINT('Ctrl Pts',(22.9147684862425,-4.39503346238455,
12.));
#216989=CARTESIAN_POINT('Ctrl Pts',(22.9303714335549,-4.40257451754309,
0.));
#216990=CARTESIAN_POINT('Ctrl Pts',(22.9303714335549,-4.40257451754309,
12.));
#216991=CARTESIAN_POINT('Ctrl Pts',(22.9460690729092,-4.41021712205549,
0.));
#216992=CARTESIAN_POINT('Ctrl Pts',(22.9460690729092,-4.41021712205549,
12.));
#216993=CARTESIAN_POINT('Ctrl Pts',(22.9618600534866,-4.41796126001311,
0.));
#216994=CARTESIAN_POINT('Ctrl Pts',(22.9618600534866,-4.41796126001311,
12.));
#216995=CARTESIAN_POINT('Ctrl Pts',(22.9777430460021,-4.42580691372772,
0.));
#216996=CARTESIAN_POINT('Ctrl Pts',(22.9777430460021,-4.42580691372772,
12.));
#216997=CARTESIAN_POINT('Ctrl Pts',(22.9937167421009,-4.43375406376906,
0.));
#216998=CARTESIAN_POINT('Ctrl Pts',(22.9937167421009,-4.43375406376906,
12.));
#216999=CARTESIAN_POINT('Ctrl Pts',(23.0097798538399,-4.44180268901667,
0.));
#217000=CARTESIAN_POINT('Ctrl Pts',(23.0097798538399,-4.44180268901667,
12.));
#217001=CARTESIAN_POINT('Ctrl Pts',(23.0259311131395,-4.44995276669699,
0.));
#217002=CARTESIAN_POINT('Ctrl Pts',(23.0259311131395,-4.44995276669699,
12.));
#217003=CARTESIAN_POINT('Ctrl Pts',(23.0421692712466,-4.45820427241678,
0.));
#217004=CARTESIAN_POINT('Ctrl Pts',(23.0421692712466,-4.45820427241678,
12.));
#217005=CARTESIAN_POINT('Ctrl Pts',(23.0584930981723,-4.46655718018206,
0.));
#217006=CARTESIAN_POINT('Ctrl Pts',(23.0584930981723,-4.46655718018206,
12.));
#217007=CARTESIAN_POINT('Ctrl Pts',(23.0749013821867,-4.47501146242822,
0.));
#217008=CARTESIAN_POINT('Ctrl Pts',(23.0749013821867,-4.47501146242822,
12.));
#217009=CARTESIAN_POINT('Ctrl Pts',(23.0913929293909,-4.48356709006757,
0.));
#217010=CARTESIAN_POINT('Ctrl Pts',(23.0913929293909,-4.48356709006757,
12.));
#217011=CARTESIAN_POINT('Ctrl Pts',(23.1079665632629,-4.49222403252202,
0.));
#217012=CARTESIAN_POINT('Ctrl Pts',(23.1079665632629,-4.49222403252202,
12.));
#217013=CARTESIAN_POINT('Ctrl Pts',(23.1246211242117,-4.5009822577518,0.));
#217014=CARTESIAN_POINT('Ctrl Pts',(23.1246211242117,-4.5009822577518,12.));
#217015=CARTESIAN_POINT('Ctrl Pts',(23.1413554691136,-4.50984173227088,
0.));
#217016=CARTESIAN_POINT('Ctrl Pts',(23.1413554691136,-4.50984173227088,
12.));
#217017=CARTESIAN_POINT('Ctrl Pts',(23.1581684708778,-4.51880242116786,
0.));
#217018=CARTESIAN_POINT('Ctrl Pts',(23.1581684708778,-4.51880242116786,
12.));
#217019=CARTESIAN_POINT('Ctrl Pts',(23.1750590180923,-4.52786428815049,
0.));
#217020=CARTESIAN_POINT('Ctrl Pts',(23.1750590180923,-4.52786428815049,
12.));
#217021=CARTESIAN_POINT('Ctrl Pts',(23.1920260146474,-4.53702729557586,
0.));
#217022=CARTESIAN_POINT('Ctrl Pts',(23.1920260146474,-4.53702729557586,
12.));
#217023=CARTESIAN_POINT('Ctrl Pts',(23.2090683793627,-4.54629140447543,
0.));
#217024=CARTESIAN_POINT('Ctrl Pts',(23.2090683793627,-4.54629140447543,
12.));
#217025=CARTESIAN_POINT('Ctrl Pts',(23.2261850456054,-4.55565657456957,
0.));
#217026=CARTESIAN_POINT('Ctrl Pts',(23.2261850456054,-4.55565657456957,
12.));
#217027=CARTESIAN_POINT('Ctrl Pts',(23.2433749609117,-4.56512276427812,
0.));
#217028=CARTESIAN_POINT('Ctrl Pts',(23.2433749609117,-4.56512276427812,
12.));
#217029=CARTESIAN_POINT('Ctrl Pts',(23.2606370866853,-4.57468993076071,
0.));
#217030=CARTESIAN_POINT('Ctrl Pts',(23.2606370866853,-4.57468993076071,
12.));
#217031=CARTESIAN_POINT('Ctrl Pts',(23.2779703978868,-4.58435802994675,
0.));
#217032=CARTESIAN_POINT('Ctrl Pts',(23.2779703978868,-4.58435802994675,
12.));
#217033=CARTESIAN_POINT('Ctrl Pts',(23.295373882719,-4.59412701655751,0.));
#217034=CARTESIAN_POINT('Ctrl Pts',(23.295373882719,-4.59412701655751,12.));
#217035=CARTESIAN_POINT('Ctrl Pts',(23.3128465423119,-4.60399684412176,
0.));
#217036=CARTESIAN_POINT('Ctrl Pts',(23.3128465423119,-4.60399684412176,
12.));
#217037=CARTESIAN_POINT('Ctrl Pts',(23.3303873903947,-4.6139674649785,0.));
#217038=CARTESIAN_POINT('Ctrl Pts',(23.3303873903947,-4.6139674649785,12.));
#217039=CARTESIAN_POINT('Ctrl Pts',(23.3479954530281,-4.62403883030825,
0.));
#217040=CARTESIAN_POINT('Ctrl Pts',(23.3479954530281,-4.62403883030825,
12.));
#217041=CARTESIAN_POINT('Ctrl Pts',(23.3656697683496,-4.63421089016556,
0.));
#217042=CARTESIAN_POINT('Ctrl Pts',(23.3656697683496,-4.63421089016556,
12.));
#217043=CARTESIAN_POINT('Ctrl Pts',(23.383409386307,-4.64448359349936,0.));
#217044=CARTESIAN_POINT('Ctrl Pts',(23.383409386307,-4.64448359349936,12.));
#217045=CARTESIAN_POINT('Ctrl Pts',(23.4012133683957,-4.65485688816923,
0.));
#217046=CARTESIAN_POINT('Ctrl Pts',(23.4012133683957,-4.65485688816923,
12.));
#217047=CARTESIAN_POINT('Ctrl Pts',(23.4190807873798,-4.66533072094664,
0.));
#217048=CARTESIAN_POINT('Ctrl Pts',(23.4190807873798,-4.66533072094664,
12.));
#217049=CARTESIAN_POINT('Ctrl Pts',(23.4370107270444,-4.67590503753051,
0.));
#217050=CARTESIAN_POINT('Ctrl Pts',(23.4370107270444,-4.67590503753051,
12.));
#217051=CARTESIAN_POINT('Ctrl Pts',(23.4550022819852,-4.68657978258298,
0.));
#217052=CARTESIAN_POINT('Ctrl Pts',(23.4550022819852,-4.68657978258298,
12.));
#217053=CARTESIAN_POINT('Ctrl Pts',(23.4730545573849,-4.69735489975024,
0.));
#217054=CARTESIAN_POINT('Ctrl Pts',(23.4730545573849,-4.69735489975024,
12.));
#217055=CARTESIAN_POINT('Ctrl Pts',(23.491166668789,-4.70823033167821,0.));
#217056=CARTESIAN_POINT('Ctrl Pts',(23.491166668789,-4.70823033167821,12.));
#217057=CARTESIAN_POINT('Ctrl Pts',(23.5093377418784,-4.71920602001905,
0.));
#217058=CARTESIAN_POINT('Ctrl Pts',(23.5093377418784,-4.71920602001905,
12.));
#217059=CARTESIAN_POINT('Ctrl Pts',(23.5275669122378,-4.73028190543032,
0.));
#217060=CARTESIAN_POINT('Ctrl Pts',(23.5275669122378,-4.73028190543032,
12.));
#217061=CARTESIAN_POINT('Ctrl Pts',(23.5458533251715,-4.74145792760699,
0.));
#217062=CARTESIAN_POINT('Ctrl Pts',(23.5458533251715,-4.74145792760699,
12.));
#217063=CARTESIAN_POINT('Ctrl Pts',(23.564196135517,-4.75273402530616,0.));
#217064=CARTESIAN_POINT('Ctrl Pts',(23.564196135517,-4.75273402530616,12.));
#217065=CARTESIAN_POINT('Ctrl Pts',(23.5825945074535,-4.76411013636252,
0.));
#217066=CARTESIAN_POINT('Ctrl Pts',(23.5825945074535,-4.76411013636252,
12.));
#217067=CARTESIAN_POINT('Ctrl Pts',(23.6010476143099,-4.77558619769876,
0.));
#217068=CARTESIAN_POINT('Ctrl Pts',(23.6010476143099,-4.77558619769876,
12.));
#217069=CARTESIAN_POINT('Ctrl Pts',(23.6195546383625,-4.78716214532105,
0.));
#217070=CARTESIAN_POINT('Ctrl Pts',(23.6195546383625,-4.78716214532105,
12.));
#217071=CARTESIAN_POINT('Ctrl Pts',(23.6381147706581,-4.79883791433231,
0.));
#217072=CARTESIAN_POINT('Ctrl Pts',(23.6381147706581,-4.79883791433231,
12.));
#217073=CARTESIAN_POINT('Ctrl Pts',(23.6567272108631,-4.81061343896443,
0.));
#217074=CARTESIAN_POINT('Ctrl Pts',(23.6567272108631,-4.81061343896443,
12.));
#217075=CARTESIAN_POINT('Ctrl Pts',(23.6753911671023,-4.82248865259571,
0.));
#217076=CARTESIAN_POINT('Ctrl Pts',(23.6753911671023,-4.82248865259571,
12.));
#217077=CARTESIAN_POINT('Ctrl Pts',(23.6941058557971,-4.83446348776268,
0.));
#217078=CARTESIAN_POINT('Ctrl Pts',(23.6941058557971,-4.83446348776268,
12.));
#217079=CARTESIAN_POINT('Ctrl Pts',(23.7128705015014,-4.84653787616424,
0.));
#217080=CARTESIAN_POINT('Ctrl Pts',(23.7128705015014,-4.84653787616424,
12.));
#217081=CARTESIAN_POINT('Ctrl Pts',(23.7316843367308,-4.85871174865493,
0.));
#217082=CARTESIAN_POINT('Ctrl Pts',(23.7316843367308,-4.85871174865493,
12.));
#217083=CARTESIAN_POINT('Ctrl Pts',(23.7505466018239,-4.87098503527144,
0.));
#217084=CARTESIAN_POINT('Ctrl Pts',(23.7505466018239,-4.87098503527144,
12.));
#217085=CARTESIAN_POINT('Ctrl Pts',(23.7694565448044,-4.88335766525566,
0.));
#217086=CARTESIAN_POINT('Ctrl Pts',(23.7694565448044,-4.88335766525566,
12.));
#217087=CARTESIAN_POINT('Ctrl Pts',(23.7884134212381,-4.89582956706772,
0.));
#217088=CARTESIAN_POINT('Ctrl Pts',(23.7884134212381,-4.89582956706772,
12.));
#217089=CARTESIAN_POINT('Ctrl Pts',(23.8074164940897,-4.90840066839348,
0.));
#217090=CARTESIAN_POINT('Ctrl Pts',(23.8074164940897,-4.90840066839348,
12.));
#217091=CARTESIAN_POINT('Ctrl Pts',(23.8264650335721,-4.92107089613978,
0.));
#217092=CARTESIAN_POINT('Ctrl Pts',(23.8264650335721,-4.92107089613978,
12.));
#217093=CARTESIAN_POINT('Ctrl Pts',(23.8455583170062,-4.93384017643443,
0.));
#217094=CARTESIAN_POINT('Ctrl Pts',(23.8455583170062,-4.93384017643443,
12.));
#217095=CARTESIAN_POINT('Ctrl Pts',(23.8646956287172,-4.94670843465869,
0.));
#217096=CARTESIAN_POINT('Ctrl Pts',(23.8646956287172,-4.94670843465869,
12.));
#217097=CARTESIAN_POINT('Ctrl Pts',(23.883876259922,-4.95967559546566,0.));
#217098=CARTESIAN_POINT('Ctrl Pts',(23.883876259922,-4.95967559546566,12.));
#217099=CARTESIAN_POINT('Ctrl Pts',(23.9030995086164,-4.9727415827923,0.));
#217100=CARTESIAN_POINT('Ctrl Pts',(23.9030995086164,-4.9727415827923,12.));
#217101=CARTESIAN_POINT('Ctrl Pts',(23.9223646794591,-4.98590631986534,
0.));
#217102=CARTESIAN_POINT('Ctrl Pts',(23.9223646794591,-4.98590631986534,
12.));
#217103=CARTESIAN_POINT('Ctrl Pts',(23.9416710836528,-4.9991697291931,0.));
#217104=CARTESIAN_POINT('Ctrl Pts',(23.9416710836528,-4.9991697291931,12.));
#217105=CARTESIAN_POINT('Ctrl Pts',(23.9610180388271,-5.01253173257459,
0.));
#217106=CARTESIAN_POINT('Ctrl Pts',(23.9610180388271,-5.01253173257459,
12.));
#217107=CARTESIAN_POINT('Ctrl Pts',(23.9804048689228,-5.02599225112462,
0.));
#217108=CARTESIAN_POINT('Ctrl Pts',(23.9804048689228,-5.02599225112462,
12.));
#217109=CARTESIAN_POINT('Ctrl Pts',(23.9998309040747,-5.03955120528528,
0.));
#217110=CARTESIAN_POINT('Ctrl Pts',(23.9998309040747,-5.03955120528528,
12.));
#217111=CARTESIAN_POINT('Ctrl Pts',(24.0192954804896,-5.05320851483069,
0.));
#217112=CARTESIAN_POINT('Ctrl Pts',(24.0192954804896,-5.05320851483069,
12.));
#217113=CARTESIAN_POINT('Ctrl Pts',(24.0387979403268,-5.0669640988664,0.));
#217114=CARTESIAN_POINT('Ctrl Pts',(24.0387979403268,-5.0669640988664,12.));
#217115=CARTESIAN_POINT('Ctrl Pts',(24.0583376315636,-5.08081787581271,
0.));
#217116=CARTESIAN_POINT('Ctrl Pts',(24.0583376315636,-5.08081787581271,
12.));
#217117=CARTESIAN_POINT('Ctrl Pts',(24.0779139079264,-5.09476976342618,
0.));
#217118=CARTESIAN_POINT('Ctrl Pts',(24.0779139079264,-5.09476976342618,
12.));
#217119=CARTESIAN_POINT('Ctrl Pts',(24.0975261288444,-5.10881967883126,
0.));
#217120=CARTESIAN_POINT('Ctrl Pts',(24.0975261288444,-5.10881967883126,
12.));
#217121=CARTESIAN_POINT('Ctrl Pts',(24.117173659394,-5.12296753853858,0.));
#217122=CARTESIAN_POINT('Ctrl Pts',(24.117173659394,-5.12296753853858,12.));
#217123=CARTESIAN_POINT('Ctrl Pts',(24.1368558702443,-5.13721325845746,
0.));
#217124=CARTESIAN_POINT('Ctrl Pts',(24.1368558702443,-5.13721325845746,
12.));
#217125=CARTESIAN_POINT('Ctrl Pts',(24.1565721375971,-5.1515567539008,0.));
#217126=CARTESIAN_POINT('Ctrl Pts',(24.1565721375971,-5.1515567539008,12.));
#217127=CARTESIAN_POINT('Ctrl Pts',(24.1763218431344,-5.16599793957987,
0.));
#217128=CARTESIAN_POINT('Ctrl Pts',(24.1763218431344,-5.16599793957987,
12.));
#217129=CARTESIAN_POINT('Ctrl Pts',(24.1961043738755,-5.180536729614,0.));
#217130=CARTESIAN_POINT('Ctrl Pts',(24.1961043738755,-5.180536729614,12.));
#217131=CARTESIAN_POINT('Ctrl Pts',(24.2159191220171,-5.19517303753648,
0.));
#217132=CARTESIAN_POINT('Ctrl Pts',(24.2159191220171,-5.19517303753648,
12.));
#217133=CARTESIAN_POINT('Ctrl Pts',(24.2357654847766,-5.20990677629177,
0.));
#217134=CARTESIAN_POINT('Ctrl Pts',(24.2357654847766,-5.20990677629177,
12.));
#217135=CARTESIAN_POINT('Ctrl Pts',(24.2556428642294,-5.22473785822443,
0.));
#217136=CARTESIAN_POINT('Ctrl Pts',(24.2556428642294,-5.22473785822443,
12.));
#217137=CARTESIAN_POINT('Ctrl Pts',(24.2755506671525,-5.2396661950629,0.));
#217138=CARTESIAN_POINT('Ctrl Pts',(24.2755506671525,-5.2396661950629,12.));
#217139=CARTESIAN_POINT('Ctrl Pts',(24.2954883048447,-5.25469169788858,
0.));
#217140=CARTESIAN_POINT('Ctrl Pts',(24.2954883048447,-5.25469169788858,
12.));
#217141=CARTESIAN_POINT('Ctrl Pts',(24.3154551932221,-5.269814277188,0.));
#217142=CARTESIAN_POINT('Ctrl Pts',(24.3154551932221,-5.269814277188,12.));
#217143=CARTESIAN_POINT('Ctrl Pts',(24.3354507529414,-5.28503384290649,
0.));
#217144=CARTESIAN_POINT('Ctrl Pts',(24.3354507529414,-5.28503384290649,
12.));
#217145=CARTESIAN_POINT('Ctrl Pts',(24.3554744095075,-5.30035030449065,
0.));
#217146=CARTESIAN_POINT('Ctrl Pts',(24.3554744095075,-5.30035030449065,
12.));
#217147=CARTESIAN_POINT('Ctrl Pts',(24.3755255933917,-5.31576357092527,
0.));
#217148=CARTESIAN_POINT('Ctrl Pts',(24.3755255933917,-5.31576357092527,
12.));
#217149=CARTESIAN_POINT('Ctrl Pts',(24.3956037401293,-5.33127355076035,
0.));
#217150=CARTESIAN_POINT('Ctrl Pts',(24.3956037401293,-5.33127355076035,
12.));
#217151=CARTESIAN_POINT('Ctrl Pts',(24.4157082904614,-5.34688015213538,
0.));
#217152=CARTESIAN_POINT('Ctrl Pts',(24.4157082904614,-5.34688015213538,
12.));
#217153=CARTESIAN_POINT('Ctrl Pts',(24.435838689915,-5.36258328273628,0.));
#217154=CARTESIAN_POINT('Ctrl Pts',(24.435838689915,-5.36258328273628,12.));
#217155=CARTESIAN_POINT('Ctrl Pts',(24.4559943883157,-5.37838284973696,
0.));
#217156=CARTESIAN_POINT('Ctrl Pts',(24.4559943883157,-5.37838284973696,
12.));
#217157=CARTESIAN_POINT('Ctrl Pts',(24.4761748393321,-5.39427875973825,
0.));
#217158=CARTESIAN_POINT('Ctrl Pts',(24.4761748393321,-5.39427875973825,
12.));
#217159=CARTESIAN_POINT('Ctrl Pts',(24.496379499983,-5.41027091869242,0.));
#217160=CARTESIAN_POINT('Ctrl Pts',(24.496379499983,-5.41027091869242,12.));
#217161=CARTESIAN_POINT('Ctrl Pts',(24.5166078302108,-5.4263592318342,0.));
#217162=CARTESIAN_POINT('Ctrl Pts',(24.5166078302108,-5.4263592318342,12.));
#217163=CARTESIAN_POINT('Ctrl Pts',(24.5368592922863,-5.44254360356881,
0.));
#217164=CARTESIAN_POINT('Ctrl Pts',(24.5368592922863,-5.44254360356881,
12.));
#217165=CARTESIAN_POINT('Ctrl Pts',(24.5571333514842,-5.45882393762263,
0.));
#217166=CARTESIAN_POINT('Ctrl Pts',(24.5571333514842,-5.45882393762263,
12.));
#217167=CARTESIAN_POINT('Ctrl Pts',(24.5774294770329,-5.4752001372442,0.));
#217168=CARTESIAN_POINT('Ctrl Pts',(24.5774294770329,-5.4752001372442,12.));
#217169=CARTESIAN_POINT('Ctrl Pts',(24.5977471429364,-5.49167210537248,
0.));
#217170=CARTESIAN_POINT('Ctrl Pts',(24.5977471429364,-5.49167210537248,
12.));
#217171=CARTESIAN_POINT('Ctrl Pts',(24.6180858289179,-5.50823974481963,
0.));
#217172=CARTESIAN_POINT('Ctrl Pts',(24.6180858289179,-5.50823974481963,
12.));
#217173=CARTESIAN_POINT('Ctrl Pts',(24.6384450211467,-5.52490295840993,
0.));
#217174=CARTESIAN_POINT('Ctrl Pts',(24.6384450211467,-5.52490295840993,
12.));
#217175=CARTESIAN_POINT('Ctrl Pts',(24.6588242134738,-5.54166164919584,
0.));
#217176=CARTESIAN_POINT('Ctrl Pts',(24.6588242134738,-5.54166164919584,
12.));
#217177=CARTESIAN_POINT('Ctrl Pts',(24.6792229061794,-5.55851572025377,
0.));
#217178=CARTESIAN_POINT('Ctrl Pts',(24.6792229061794,-5.55851572025377,
12.));
#217179=CARTESIAN_POINT('Ctrl Pts',(24.6996406035517,-5.57546507427756,
0.));
#217180=CARTESIAN_POINT('Ctrl Pts',(24.6996406035517,-5.57546507427756,
12.));
#217181=CARTESIAN_POINT('Ctrl Pts',(24.7200768119088,-5.59250961323988,
0.));
#217182=CARTESIAN_POINT('Ctrl Pts',(24.7200768119088,-5.59250961323988,
12.));
#217183=CARTESIAN_POINT('Ctrl Pts',(24.7405310372739,-5.60964923798492,
0.));
#217184=CARTESIAN_POINT('Ctrl Pts',(24.7405310372739,-5.60964923798492,
12.));
#217185=CARTESIAN_POINT('Ctrl Pts',(24.7610027835697,-5.62688384790924,
0.));
#217186=CARTESIAN_POINT('Ctrl Pts',(24.7610027835697,-5.62688384790924,
12.));
#217187=CARTESIAN_POINT('Ctrl Pts',(24.781491549672,-5.64421334042262,0.));
#217188=CARTESIAN_POINT('Ctrl Pts',(24.781491549672,-5.64421334042262,12.));
#217189=CARTESIAN_POINT('Ctrl Pts',(24.8019968304605,-5.66163761114922,
0.));
#217190=CARTESIAN_POINT('Ctrl Pts',(24.8019968304605,-5.66163761114922,
12.));
#217191=CARTESIAN_POINT('Ctrl Pts',(24.8225181223845,-5.67915655496543,
0.));
#217192=CARTESIAN_POINT('Ctrl Pts',(24.8225181223845,-5.67915655496543,
12.));
#217193=CARTESIAN_POINT('Ctrl Pts',(24.8430549277621,-5.69677006679445,
0.));
#217194=CARTESIAN_POINT('Ctrl Pts',(24.8430549277621,-5.69677006679445,
12.));
#217195=CARTESIAN_POINT('Ctrl Pts',(24.8636067597669,-5.71447804252028,
0.));
#217196=CARTESIAN_POINT('Ctrl Pts',(24.8636067597669,-5.71447804252028,
12.));
#217197=CARTESIAN_POINT('Ctrl Pts',(24.884173146722,-5.73228037976928,0.));
#217198=CARTESIAN_POINT('Ctrl Pts',(24.884173146722,-5.73228037976928,12.));
#217199=CARTESIAN_POINT('Ctrl Pts',(24.904753637648,-5.75017697890805,0.));
#217200=CARTESIAN_POINT('Ctrl Pts',(24.904753637648,-5.75017697890805,12.));
#217201=CARTESIAN_POINT('Ctrl Pts',(24.9253478043656,-5.76816774342221,
0.));
#217202=CARTESIAN_POINT('Ctrl Pts',(24.9253478043656,-5.76816774342221,
12.));
#217203=CARTESIAN_POINT('Ctrl Pts',(24.945955229334,-5.78625257775682,0.));
#217204=CARTESIAN_POINT('Ctrl Pts',(24.945955229334,-5.78625257775682,12.));
#217205=CARTESIAN_POINT('Ctrl Pts',(24.9665754954496,-5.80443138549727,
0.));
#217206=CARTESIAN_POINT('Ctrl Pts',(24.9665754954496,-5.80443138549727,
12.));
#217207=CARTESIAN_POINT('Ctrl Pts',(24.9872081752734,-5.822704067442,0.));
#217208=CARTESIAN_POINT('Ctrl Pts',(24.9872081752734,-5.822704067442,12.));
#217209=CARTESIAN_POINT('Ctrl Pts',(25.0078528200564,-5.84107051963072,
0.));
#217210=CARTESIAN_POINT('Ctrl Pts',(25.0078528200564,-5.84107051963072,
12.));
#217211=CARTESIAN_POINT('Ctrl Pts',(25.0285089498899,-5.85953063156827,
0.));
#217212=CARTESIAN_POINT('Ctrl Pts',(25.0285089498899,-5.85953063156827,
12.));
#217213=CARTESIAN_POINT('Ctrl Pts',(25.049176040591,-5.87808428385367,0.));
#217214=CARTESIAN_POINT('Ctrl Pts',(25.049176040591,-5.87808428385367,12.));
#217215=CARTESIAN_POINT('Ctrl Pts',(25.0698535426514,-5.89673135155515,
0.));
#217216=CARTESIAN_POINT('Ctrl Pts',(25.0698535426514,-5.89673135155515,
12.));
#217217=CARTESIAN_POINT('Ctrl Pts',(25.0905409050773,-5.91547170844448,
0.));
#217218=CARTESIAN_POINT('Ctrl Pts',(25.0905409050773,-5.91547170844448,
12.));
#217219=CARTESIAN_POINT('Ctrl Pts',(25.1112375971106,-5.93430523086836,
0.));
#217220=CARTESIAN_POINT('Ctrl Pts',(25.1112375971106,-5.93430523086836,
12.));
#217221=CARTESIAN_POINT('Ctrl Pts',(25.1319431317237,-5.95323180187379,
0.));
#217222=CARTESIAN_POINT('Ctrl Pts',(25.1319431317237,-5.95323180187379,
12.));
#217223=CARTESIAN_POINT('Ctrl Pts',(25.1526570863092,-5.97225131495618,
0.));
#217224=CARTESIAN_POINT('Ctrl Pts',(25.1526570863092,-5.97225131495618,
12.));
#217225=CARTESIAN_POINT('Ctrl Pts',(25.1733791296259,-5.99136367859755,
0.));
#217226=CARTESIAN_POINT('Ctrl Pts',(25.1733791296259,-5.99136367859755,
12.));
#217227=CARTESIAN_POINT('Ctrl Pts',(25.1941090269819,-6.01056881804614,
0.));
#217228=CARTESIAN_POINT('Ctrl Pts',(25.1941090269819,-6.01056881804614,
12.));
#217229=CARTESIAN_POINT('Ctrl Pts',(25.21484662016,-6.02986667389998,0.));
#217230=CARTESIAN_POINT('Ctrl Pts',(25.21484662016,-6.02986667389998,12.));
#217231=CARTESIAN_POINT('Ctrl Pts',(25.2355918139032,-6.04925720151219,
0.));
#217232=CARTESIAN_POINT('Ctrl Pts',(25.2355918139032,-6.04925720151219,
12.));
#217233=CARTESIAN_POINT('Ctrl Pts',(25.2521940105705,-6.06484373634547,
0.));
#217234=CARTESIAN_POINT('Ctrl Pts',(25.2521940105705,-6.06484373634547,
12.));
#217235=CARTESIAN_POINT('Ctrl Pts',(25.2646490489922,-6.07657531787491,
0.));
#217236=CARTESIAN_POINT('Ctrl Pts',(25.2646490489922,-6.07657531787491,
12.));
#217237=CARTESIAN_POINT('Ctrl Pts',(25.2729539149517,-6.08441489609794,
0.));
#217238=CARTESIAN_POINT('Ctrl Pts',(25.2729539149517,-6.08441489609794,
12.));
#217239=CARTESIAN_POINT('Ctrl Pts',(25.2771067246846,-6.088339316177,0.));
#217240=CARTESIAN_POINT('Ctrl Pts',(25.2771067246846,-6.088339316177,12.));
#217241=CARTESIAN_POINT('',(25.2771067246846,-6.088339316177,0.));
#217242=CARTESIAN_POINT('Ctrl Pts',(22.1738711152697,-4.11585220600463,
0.));
#217243=CARTESIAN_POINT('Ctrl Pts',(22.173877682324,-4.11585194677443,0.));
#217244=CARTESIAN_POINT('Ctrl Pts',(22.1739341411687,-4.11586035878288,
0.));
#217245=CARTESIAN_POINT('Ctrl Pts',(22.1741488021234,-4.11589976826168,
0.));
#217246=CARTESIAN_POINT('Ctrl Pts',(22.1746949858775,-4.11600589882846,
0.));
#217247=CARTESIAN_POINT('Ctrl Pts',(22.1758088296598,-4.1162279721707,0.));
#217248=CARTESIAN_POINT('Ctrl Pts',(22.177347426894,-4.11653973150519,0.));
#217249=CARTESIAN_POINT('Ctrl Pts',(22.179297473024,-4.11694173195005,0.));
#217250=CARTESIAN_POINT('Ctrl Pts',(22.1816414985788,-4.11743469691757,
0.));
#217251=CARTESIAN_POINT('Ctrl Pts',(22.1843613164855,-4.11801938107481,
0.));
#217252=CARTESIAN_POINT('Ctrl Pts',(22.1874419861496,-4.11869641271775,
0.));
#217253=CARTESIAN_POINT('Ctrl Pts',(22.1908725908525,-4.11946626228637,
0.));
#217254=CARTESIAN_POINT('Ctrl Pts',(22.1946440958098,-4.12032932637738,
0.));
#217255=CARTESIAN_POINT('Ctrl Pts',(22.1987479618246,-4.12128598183523,
0.));
#217256=CARTESIAN_POINT('Ctrl Pts',(22.2031746532106,-4.12233664408228,
0.));
#217257=CARTESIAN_POINT('Ctrl Pts',(22.2079143941719,-4.12348173702024,
0.));
#217258=CARTESIAN_POINT('Ctrl Pts',(22.2129576146671,-4.12472167516608,
0.));
#217259=CARTESIAN_POINT('Ctrl Pts',(22.2182956401341,-4.12605683613308,
0.));
#217260=CARTESIAN_POINT('Ctrl Pts',(22.2239207458781,-4.12748755830105,
0.));
#217261=CARTESIAN_POINT('Ctrl Pts',(22.2298258043947,-4.1290141546338,0.));
#217262=CARTESIAN_POINT('Ctrl Pts',(22.2360040565533,-4.13063692157499,
0.));
#217263=CARTESIAN_POINT('Ctrl Pts',(22.2424488153523,-4.13235615060161,
0.));
#217264=CARTESIAN_POINT('Ctrl Pts',(22.249153531779,-4.13417212558811,0.));
#217265=CARTESIAN_POINT('Ctrl Pts',(22.2561118708421,-4.13608511977227,
0.));
#217266=CARTESIAN_POINT('Ctrl Pts',(22.2633177913972,-4.13809539255423,
0.));
#217267=CARTESIAN_POINT('Ctrl Pts',(22.2707656042457,-4.14020318715992,
0.));
#217268=CARTESIAN_POINT('Ctrl Pts',(22.2784499072027,-4.14240873321985,
0.));
#217269=CARTESIAN_POINT('Ctrl Pts',(22.2863655389166,-4.14471224859297,
0.));
#217270=CARTESIAN_POINT('Ctrl Pts',(22.2945075198467,-4.14711394168557,
0.));
#217271=CARTESIAN_POINT('Ctrl Pts',(22.3028710166933,-4.14961401285523,
0.));
#217272=CARTESIAN_POINT('Ctrl Pts',(22.3114513545185,-4.15221265396991,
0.));
#217273=CARTESIAN_POINT('Ctrl Pts',(22.3202440186979,-4.15491004835282,
0.));
#217274=CARTESIAN_POINT('Ctrl Pts',(22.3292446628959,-4.15770637047891,
0.));
#217275=CARTESIAN_POINT('Ctrl Pts',(22.3384491078602,-4.16060178604165,
0.));
#217276=CARTESIAN_POINT('Ctrl Pts',(22.3478533253889,-4.16359645263189,
0.));
#217277=CARTESIAN_POINT('Ctrl Pts',(22.3574534257396,-4.16669052026601,
0.));
#217278=CARTESIAN_POINT('Ctrl Pts',(22.3672456427599,-4.16988413199458,
0.));
#217279=CARTESIAN_POINT('Ctrl Pts',(22.3772263228617,-4.17317742436146,
0.));
#217280=CARTESIAN_POINT('Ctrl Pts',(22.3873919231334,-4.17657052752826,
0.));
#217281=CARTESIAN_POINT('Ctrl Pts',(22.3977390078075,-4.18006356544883,
0.));
#217282=CARTESIAN_POINT('Ctrl Pts',(22.4082642454453,-4.18365665600852,
0.));
#217283=CARTESIAN_POINT('Ctrl Pts',(22.4189644056115,-4.18734991117722,
0.));
#217284=CARTESIAN_POINT('Ctrl Pts',(22.4298363535421,-4.19114343726943,
0.));
#217285=CARTESIAN_POINT('Ctrl Pts',(22.4408770448917,-4.19503733518862,
0.));
#217286=CARTESIAN_POINT('Ctrl Pts',(22.4520835205419,-4.19903170066356,
0.));
#217287=CARTESIAN_POINT('Ctrl Pts',(22.4634529011433,-4.20312662448172,
0.));
#217288=CARTESIAN_POINT('Ctrl Pts',(22.4749823839915,-4.20732219265649,
0.));
#217289=CARTESIAN_POINT('Ctrl Pts',(22.4866692403147,-4.21161848657429,
0.));
#217290=CARTESIAN_POINT('Ctrl Pts',(22.4985108124229,-4.21601558313909,
0.));
#217291=CARTESIAN_POINT('Ctrl Pts',(22.5105045108882,-4.22051355490198,
0.));
#217292=CARTESIAN_POINT('Ctrl Pts',(22.5226478117885,-4.22511247020041,
0.));
#217293=CARTESIAN_POINT('Ctrl Pts',(22.5349382540587,-4.22981239330733,
0.));
#217294=CARTESIAN_POINT('Ctrl Pts',(22.5473734368086,-4.23461338456714,
0.));
#217295=CARTESIAN_POINT('Ctrl Pts',(22.559951016643,-4.23951550052527,0.));
#217296=CARTESIAN_POINT('Ctrl Pts',(22.5726687049922,-4.2445187940486,0.));
#217297=CARTESIAN_POINT('Ctrl Pts',(22.5855242662479,-4.24962331444186,
0.));
#217298=CARTESIAN_POINT('Ctrl Pts',(22.5985155158637,-4.25482910755486,
0.));
#217299=CARTESIAN_POINT('Ctrl Pts',(22.611640318482,-4.26013621588304,0.));
#217300=CARTESIAN_POINT('Ctrl Pts',(22.6248965859975,-4.26554467865572,
0.));
#217301=CARTESIAN_POINT('Ctrl Pts',(22.6382822758171,-4.27105453193,0.));
#217302=CARTESIAN_POINT('Ctrl Pts',(22.6517953893303,-4.27666580869118,
0.));
#217303=CARTESIAN_POINT('Ctrl Pts',(22.665433970311,-4.2823785389406,0.));
#217304=CARTESIAN_POINT('Ctrl Pts',(22.6791961033536,-4.28819274977767,
0.));
#217305=CARTESIAN_POINT('Ctrl Pts',(22.6930799122545,-4.29410846547062,
0.));
#217306=CARTESIAN_POINT('Ctrl Pts',(22.707083558756,-4.30012570754067,0.));
#217307=CARTESIAN_POINT('Ctrl Pts',(22.7212052413384,-4.30624449484075,
0.));
#217308=CARTESIAN_POINT('Ctrl Pts',(22.7354431939926,-4.31246484362551,
0.));
#217309=CARTESIAN_POINT('Ctrl Pts',(22.7497956849852,-4.31878676761231,
0.));
#217310=CARTESIAN_POINT('Ctrl Pts',(22.764261015648,-4.32521027803748,0.));
#217311=CARTESIAN_POINT('Ctrl Pts',(22.7788375194081,-4.33173538373183,
0.));
#217312=CARTESIAN_POINT('Ctrl Pts',(22.7935235607807,-4.33836209118444,
0.));
#217313=CARTESIAN_POINT('Ctrl Pts',(22.808317534379,-4.34509040460066,0.));
#217314=CARTESIAN_POINT('Ctrl Pts',(22.8232178638873,-4.35192032594802,
0.));
#217315=CARTESIAN_POINT('Ctrl Pts',(22.838223001118,-4.3588518550056,0.));
#217316=CARTESIAN_POINT('Ctrl Pts',(22.8533314252419,-4.36588498943011,
0.));
#217317=CARTESIAN_POINT('Ctrl Pts',(22.8685416419725,-4.37301972480753,
0.));
#217318=CARTESIAN_POINT('Ctrl Pts',(22.8838521827702,-4.38025605470091,
0.));
#217319=CARTESIAN_POINT('Ctrl Pts',(22.8992616040108,-4.38759397068393,
0.));
#217320=CARTESIAN_POINT('Ctrl Pts',(22.9147684862425,-4.39503346238455,
0.));
#217321=CARTESIAN_POINT('Ctrl Pts',(22.9303714335549,-4.40257451754309,
0.));
#217322=CARTESIAN_POINT('Ctrl Pts',(22.9460690729092,-4.41021712205549,
0.));
#217323=CARTESIAN_POINT('Ctrl Pts',(22.9618600534866,-4.41796126001311,
0.));
#217324=CARTESIAN_POINT('Ctrl Pts',(22.9777430460021,-4.42580691372772,
0.));
#217325=CARTESIAN_POINT('Ctrl Pts',(22.9937167421009,-4.43375406376906,
0.));
#217326=CARTESIAN_POINT('Ctrl Pts',(23.0097798538399,-4.44180268901667,
0.));
#217327=CARTESIAN_POINT('Ctrl Pts',(23.0259311131395,-4.44995276669699,
0.));
#217328=CARTESIAN_POINT('Ctrl Pts',(23.0421692712466,-4.45820427241678,
0.));
#217329=CARTESIAN_POINT('Ctrl Pts',(23.0584930981723,-4.46655718018206,
0.));
#217330=CARTESIAN_POINT('Ctrl Pts',(23.0749013821867,-4.47501146242822,
0.));
#217331=CARTESIAN_POINT('Ctrl Pts',(23.0913929293909,-4.48356709006757,
0.));
#217332=CARTESIAN_POINT('Ctrl Pts',(23.1079665632629,-4.49222403252202,
0.));
#217333=CARTESIAN_POINT('Ctrl Pts',(23.1246211242117,-4.5009822577518,0.));
#217334=CARTESIAN_POINT('Ctrl Pts',(23.1413554691136,-4.50984173227088,
0.));
#217335=CARTESIAN_POINT('Ctrl Pts',(23.1581684708778,-4.51880242116786,
0.));
#217336=CARTESIAN_POINT('Ctrl Pts',(23.1750590180923,-4.52786428815049,
0.));
#217337=CARTESIAN_POINT('Ctrl Pts',(23.1920260146474,-4.53702729557586,
0.));
#217338=CARTESIAN_POINT('Ctrl Pts',(23.2090683793627,-4.54629140447543,
0.));
#217339=CARTESIAN_POINT('Ctrl Pts',(23.2261850456054,-4.55565657456957,
0.));
#217340=CARTESIAN_POINT('Ctrl Pts',(23.2433749609117,-4.56512276427812,
0.));
#217341=CARTESIAN_POINT('Ctrl Pts',(23.2606370866853,-4.57468993076071,
0.));
#217342=CARTESIAN_POINT('Ctrl Pts',(23.2779703978868,-4.58435802994675,
0.));
#217343=CARTESIAN_POINT('Ctrl Pts',(23.295373882719,-4.59412701655751,0.));
#217344=CARTESIAN_POINT('Ctrl Pts',(23.3128465423119,-4.60399684412176,
0.));
#217345=CARTESIAN_POINT('Ctrl Pts',(23.3303873903947,-4.6139674649785,0.));
#217346=CARTESIAN_POINT('Ctrl Pts',(23.3479954530281,-4.62403883030825,
0.));
#217347=CARTESIAN_POINT('Ctrl Pts',(23.3656697683496,-4.63421089016556,
0.));
#217348=CARTESIAN_POINT('Ctrl Pts',(23.383409386307,-4.64448359349936,0.));
#217349=CARTESIAN_POINT('Ctrl Pts',(23.4012133683957,-4.65485688816923,
0.));
#217350=CARTESIAN_POINT('Ctrl Pts',(23.4190807873798,-4.66533072094664,
0.));
#217351=CARTESIAN_POINT('Ctrl Pts',(23.4370107270444,-4.67590503753051,
0.));
#217352=CARTESIAN_POINT('Ctrl Pts',(23.4550022819852,-4.68657978258298,
0.));
#217353=CARTESIAN_POINT('Ctrl Pts',(23.4730545573849,-4.69735489975024,
0.));
#217354=CARTESIAN_POINT('Ctrl Pts',(23.491166668789,-4.70823033167821,0.));
#217355=CARTESIAN_POINT('Ctrl Pts',(23.5093377418784,-4.71920602001905,
0.));
#217356=CARTESIAN_POINT('Ctrl Pts',(23.5275669122378,-4.73028190543032,
0.));
#217357=CARTESIAN_POINT('Ctrl Pts',(23.5458533251715,-4.74145792760699,
0.));
#217358=CARTESIAN_POINT('Ctrl Pts',(23.564196135517,-4.75273402530616,0.));
#217359=CARTESIAN_POINT('Ctrl Pts',(23.5825945074535,-4.76411013636252,
0.));
#217360=CARTESIAN_POINT('Ctrl Pts',(23.6010476143099,-4.77558619769876,
0.));
#217361=CARTESIAN_POINT('Ctrl Pts',(23.6195546383625,-4.78716214532105,
0.));
#217362=CARTESIAN_POINT('Ctrl Pts',(23.6381147706581,-4.79883791433231,
0.));
#217363=CARTESIAN_POINT('Ctrl Pts',(23.6567272108631,-4.81061343896443,
0.));
#217364=CARTESIAN_POINT('Ctrl Pts',(23.6753911671023,-4.82248865259571,
0.));
#217365=CARTESIAN_POINT('Ctrl Pts',(23.6941058557971,-4.83446348776268,
0.));
#217366=CARTESIAN_POINT('Ctrl Pts',(23.7128705015014,-4.84653787616424,
0.));
#217367=CARTESIAN_POINT('Ctrl Pts',(23.7316843367308,-4.85871174865493,
0.));
#217368=CARTESIAN_POINT('Ctrl Pts',(23.7505466018239,-4.87098503527144,
0.));
#217369=CARTESIAN_POINT('Ctrl Pts',(23.7694565448044,-4.88335766525566,
0.));
#217370=CARTESIAN_POINT('Ctrl Pts',(23.7884134212381,-4.89582956706772,
0.));
#217371=CARTESIAN_POINT('Ctrl Pts',(23.8074164940897,-4.90840066839348,
0.));
#217372=CARTESIAN_POINT('Ctrl Pts',(23.8264650335721,-4.92107089613978,
0.));
#217373=CARTESIAN_POINT('Ctrl Pts',(23.8455583170062,-4.93384017643443,
0.));
#217374=CARTESIAN_POINT('Ctrl Pts',(23.8646956287172,-4.94670843465869,
0.));
#217375=CARTESIAN_POINT('Ctrl Pts',(23.883876259922,-4.95967559546566,0.));
#217376=CARTESIAN_POINT('Ctrl Pts',(23.9030995086164,-4.9727415827923,0.));
#217377=CARTESIAN_POINT('Ctrl Pts',(23.9223646794591,-4.98590631986534,
0.));
#217378=CARTESIAN_POINT('Ctrl Pts',(23.9416710836528,-4.9991697291931,0.));
#217379=CARTESIAN_POINT('Ctrl Pts',(23.9610180388271,-5.01253173257459,
0.));
#217380=CARTESIAN_POINT('Ctrl Pts',(23.9804048689228,-5.02599225112462,
0.));
#217381=CARTESIAN_POINT('Ctrl Pts',(23.9998309040747,-5.03955120528528,
0.));
#217382=CARTESIAN_POINT('Ctrl Pts',(24.0192954804896,-5.05320851483069,
0.));
#217383=CARTESIAN_POINT('Ctrl Pts',(24.0387979403268,-5.0669640988664,0.));
#217384=CARTESIAN_POINT('Ctrl Pts',(24.0583376315636,-5.08081787581271,
0.));
#217385=CARTESIAN_POINT('Ctrl Pts',(24.0779139079264,-5.09476976342618,
0.));
#217386=CARTESIAN_POINT('Ctrl Pts',(24.0975261288444,-5.10881967883126,
0.));
#217387=CARTESIAN_POINT('Ctrl Pts',(24.117173659394,-5.12296753853858,0.));
#217388=CARTESIAN_POINT('Ctrl Pts',(24.1368558702443,-5.13721325845746,
0.));
#217389=CARTESIAN_POINT('Ctrl Pts',(24.1565721375971,-5.1515567539008,0.));
#217390=CARTESIAN_POINT('Ctrl Pts',(24.1763218431344,-5.16599793957987,
0.));
#217391=CARTESIAN_POINT('Ctrl Pts',(24.1961043738755,-5.180536729614,0.));
#217392=CARTESIAN_POINT('Ctrl Pts',(24.2159191220171,-5.19517303753648,
0.));
#217393=CARTESIAN_POINT('Ctrl Pts',(24.2357654847766,-5.20990677629177,
0.));
#217394=CARTESIAN_POINT('Ctrl Pts',(24.2556428642294,-5.22473785822443,
0.));
#217395=CARTESIAN_POINT('Ctrl Pts',(24.2755506671525,-5.2396661950629,0.));
#217396=CARTESIAN_POINT('Ctrl Pts',(24.2954883048447,-5.25469169788858,
0.));
#217397=CARTESIAN_POINT('Ctrl Pts',(24.3154551932221,-5.269814277188,0.));
#217398=CARTESIAN_POINT('Ctrl Pts',(24.3354507529414,-5.28503384290649,
0.));
#217399=CARTESIAN_POINT('Ctrl Pts',(24.3554744095075,-5.30035030449065,
0.));
#217400=CARTESIAN_POINT('Ctrl Pts',(24.3755255933917,-5.31576357092527,
0.));
#217401=CARTESIAN_POINT('Ctrl Pts',(24.3956037401293,-5.33127355076035,
0.));
#217402=CARTESIAN_POINT('Ctrl Pts',(24.4157082904614,-5.34688015213538,
0.));
#217403=CARTESIAN_POINT('Ctrl Pts',(24.435838689915,-5.36258328273628,0.));
#217404=CARTESIAN_POINT('Ctrl Pts',(24.4559943883157,-5.37838284973696,
0.));
#217405=CARTESIAN_POINT('Ctrl Pts',(24.4761748393321,-5.39427875973825,
0.));
#217406=CARTESIAN_POINT('Ctrl Pts',(24.496379499983,-5.41027091869242,0.));
#217407=CARTESIAN_POINT('Ctrl Pts',(24.5166078302108,-5.4263592318342,0.));
#217408=CARTESIAN_POINT('Ctrl Pts',(24.5368592922863,-5.44254360356881,
0.));
#217409=CARTESIAN_POINT('Ctrl Pts',(24.5571333514842,-5.45882393762263,
0.));
#217410=CARTESIAN_POINT('Ctrl Pts',(24.5774294770329,-5.4752001372442,0.));
#217411=CARTESIAN_POINT('Ctrl Pts',(24.5977471429364,-5.49167210537248,
0.));
#217412=CARTESIAN_POINT('Ctrl Pts',(24.6180858289179,-5.50823974481963,
0.));
#217413=CARTESIAN_POINT('Ctrl Pts',(24.6384450211467,-5.52490295840993,
0.));
#217414=CARTESIAN_POINT('Ctrl Pts',(24.6588242134738,-5.54166164919584,
0.));
#217415=CARTESIAN_POINT('Ctrl Pts',(24.6792229061794,-5.55851572025377,
0.));
#217416=CARTESIAN_POINT('Ctrl Pts',(24.6996406035517,-5.57546507427756,
0.));
#217417=CARTESIAN_POINT('Ctrl Pts',(24.7200768119088,-5.59250961323988,
0.));
#217418=CARTESIAN_POINT('Ctrl Pts',(24.7405310372739,-5.60964923798492,
0.));
#217419=CARTESIAN_POINT('Ctrl Pts',(24.7610027835697,-5.62688384790924,
0.));
#217420=CARTESIAN_POINT('Ctrl Pts',(24.781491549672,-5.64421334042262,0.));
#217421=CARTESIAN_POINT('Ctrl Pts',(24.8019968304605,-5.66163761114922,
0.));
#217422=CARTESIAN_POINT('Ctrl Pts',(24.8225181223845,-5.67915655496543,
0.));
#217423=CARTESIAN_POINT('Ctrl Pts',(24.8430549277621,-5.69677006679445,
0.));
#217424=CARTESIAN_POINT('Ctrl Pts',(24.8636067597669,-5.71447804252028,
0.));
#217425=CARTESIAN_POINT('Ctrl Pts',(24.884173146722,-5.73228037976928,0.));
#217426=CARTESIAN_POINT('Ctrl Pts',(24.904753637648,-5.75017697890805,0.));
#217427=CARTESIAN_POINT('Ctrl Pts',(24.9253478043656,-5.76816774342221,
0.));
#217428=CARTESIAN_POINT('Ctrl Pts',(24.945955229334,-5.78625257775682,0.));
#217429=CARTESIAN_POINT('Ctrl Pts',(24.9665754954496,-5.80443138549727,
0.));
#217430=CARTESIAN_POINT('Ctrl Pts',(24.9872081752734,-5.822704067442,0.));
#217431=CARTESIAN_POINT('Ctrl Pts',(25.0078528200564,-5.84107051963072,
0.));
#217432=CARTESIAN_POINT('Ctrl Pts',(25.0285089498899,-5.85953063156827,
0.));
#217433=CARTESIAN_POINT('Ctrl Pts',(25.049176040591,-5.87808428385367,0.));
#217434=CARTESIAN_POINT('Ctrl Pts',(25.0698535426514,-5.89673135155515,
0.));
#217435=CARTESIAN_POINT('Ctrl Pts',(25.0905409050773,-5.91547170844448,
0.));
#217436=CARTESIAN_POINT('Ctrl Pts',(25.1112375971106,-5.93430523086836,
0.));
#217437=CARTESIAN_POINT('Ctrl Pts',(25.1319431317237,-5.95323180187379,
0.));
#217438=CARTESIAN_POINT('Ctrl Pts',(25.1526570863092,-5.97225131495618,
0.));
#217439=CARTESIAN_POINT('Ctrl Pts',(25.1733791296259,-5.99136367859755,
0.));
#217440=CARTESIAN_POINT('Ctrl Pts',(25.1941090269819,-6.01056881804614,
0.));
#217441=CARTESIAN_POINT('Ctrl Pts',(25.21484662016,-6.02986667389998,0.));
#217442=CARTESIAN_POINT('Ctrl Pts',(25.2355918139032,-6.04925720151219,
0.));
#217443=CARTESIAN_POINT('Ctrl Pts',(25.2521940105705,-6.06484373634547,
0.));
#217444=CARTESIAN_POINT('Ctrl Pts',(25.2646490489922,-6.07657531787491,
0.));
#217445=CARTESIAN_POINT('Ctrl Pts',(25.2729539149517,-6.08441489609794,
0.));
#217446=CARTESIAN_POINT('Ctrl Pts',(25.2771067246846,-6.088339316177,0.));
#217447=CARTESIAN_POINT('',(25.2771067246846,-6.088339316177,12.));
#217448=CARTESIAN_POINT('Ctrl Pts',(25.2771067246846,-6.088339316177,12.));
#217449=CARTESIAN_POINT('Ctrl Pts',(25.2729539149517,-6.08441489609794,
12.));
#217450=CARTESIAN_POINT('Ctrl Pts',(25.2646490489922,-6.07657531787491,
12.));
#217451=CARTESIAN_POINT('Ctrl Pts',(25.2521940105705,-6.06484373634547,
12.));
#217452=CARTESIAN_POINT('Ctrl Pts',(25.2355918139032,-6.04925720151219,
12.));
#217453=CARTESIAN_POINT('Ctrl Pts',(25.21484662016,-6.02986667389998,12.));
#217454=CARTESIAN_POINT('Ctrl Pts',(25.1941090269819,-6.01056881804614,
12.));
#217455=CARTESIAN_POINT('Ctrl Pts',(25.1733791296259,-5.99136367859755,
12.));
#217456=CARTESIAN_POINT('Ctrl Pts',(25.1526570863092,-5.97225131495618,
12.));
#217457=CARTESIAN_POINT('Ctrl Pts',(25.1319431317237,-5.95323180187379,
12.));
#217458=CARTESIAN_POINT('Ctrl Pts',(25.1112375971106,-5.93430523086836,
12.));
#217459=CARTESIAN_POINT('Ctrl Pts',(25.0905409050773,-5.91547170844448,
12.));
#217460=CARTESIAN_POINT('Ctrl Pts',(25.0698535426514,-5.89673135155515,
12.));
#217461=CARTESIAN_POINT('Ctrl Pts',(25.049176040591,-5.87808428385367,12.));
#217462=CARTESIAN_POINT('Ctrl Pts',(25.0285089498899,-5.85953063156827,
12.));
#217463=CARTESIAN_POINT('Ctrl Pts',(25.0078528200564,-5.84107051963072,
12.));
#217464=CARTESIAN_POINT('Ctrl Pts',(24.9872081752734,-5.822704067442,12.));
#217465=CARTESIAN_POINT('Ctrl Pts',(24.9665754954496,-5.80443138549727,
12.));
#217466=CARTESIAN_POINT('Ctrl Pts',(24.945955229334,-5.78625257775682,12.));
#217467=CARTESIAN_POINT('Ctrl Pts',(24.9253478043656,-5.76816774342221,
12.));
#217468=CARTESIAN_POINT('Ctrl Pts',(24.904753637648,-5.75017697890805,12.));
#217469=CARTESIAN_POINT('Ctrl Pts',(24.884173146722,-5.73228037976928,12.));
#217470=CARTESIAN_POINT('Ctrl Pts',(24.8636067597669,-5.71447804252028,
12.));
#217471=CARTESIAN_POINT('Ctrl Pts',(24.8430549277621,-5.69677006679445,
12.));
#217472=CARTESIAN_POINT('Ctrl Pts',(24.8225181223845,-5.67915655496543,
12.));
#217473=CARTESIAN_POINT('Ctrl Pts',(24.8019968304605,-5.66163761114922,
12.));
#217474=CARTESIAN_POINT('Ctrl Pts',(24.781491549672,-5.64421334042262,12.));
#217475=CARTESIAN_POINT('Ctrl Pts',(24.7610027835697,-5.62688384790924,
12.));
#217476=CARTESIAN_POINT('Ctrl Pts',(24.7405310372739,-5.60964923798492,
12.));
#217477=CARTESIAN_POINT('Ctrl Pts',(24.7200768119088,-5.59250961323988,
12.));
#217478=CARTESIAN_POINT('Ctrl Pts',(24.6996406035517,-5.57546507427756,
12.));
#217479=CARTESIAN_POINT('Ctrl Pts',(24.6792229061794,-5.55851572025377,
12.));
#217480=CARTESIAN_POINT('Ctrl Pts',(24.6588242134738,-5.54166164919584,
12.));
#217481=CARTESIAN_POINT('Ctrl Pts',(24.6384450211467,-5.52490295840993,
12.));
#217482=CARTESIAN_POINT('Ctrl Pts',(24.6180858289179,-5.50823974481963,
12.));
#217483=CARTESIAN_POINT('Ctrl Pts',(24.5977471429364,-5.49167210537248,
12.));
#217484=CARTESIAN_POINT('Ctrl Pts',(24.5774294770329,-5.4752001372442,12.));
#217485=CARTESIAN_POINT('Ctrl Pts',(24.5571333514842,-5.45882393762263,
12.));
#217486=CARTESIAN_POINT('Ctrl Pts',(24.5368592922863,-5.44254360356881,
12.));
#217487=CARTESIAN_POINT('Ctrl Pts',(24.5166078302108,-5.4263592318342,12.));
#217488=CARTESIAN_POINT('Ctrl Pts',(24.496379499983,-5.41027091869242,12.));
#217489=CARTESIAN_POINT('Ctrl Pts',(24.4761748393321,-5.39427875973825,
12.));
#217490=CARTESIAN_POINT('Ctrl Pts',(24.4559943883157,-5.37838284973696,
12.));
#217491=CARTESIAN_POINT('Ctrl Pts',(24.435838689915,-5.36258328273628,12.));
#217492=CARTESIAN_POINT('Ctrl Pts',(24.4157082904614,-5.34688015213538,
12.));
#217493=CARTESIAN_POINT('Ctrl Pts',(24.3956037401293,-5.33127355076035,
12.));
#217494=CARTESIAN_POINT('Ctrl Pts',(24.3755255933917,-5.31576357092527,
12.));
#217495=CARTESIAN_POINT('Ctrl Pts',(24.3554744095075,-5.30035030449065,
12.));
#217496=CARTESIAN_POINT('Ctrl Pts',(24.3354507529414,-5.28503384290649,
12.));
#217497=CARTESIAN_POINT('Ctrl Pts',(24.3154551932221,-5.269814277188,12.));
#217498=CARTESIAN_POINT('Ctrl Pts',(24.2954883048447,-5.25469169788858,
12.));
#217499=CARTESIAN_POINT('Ctrl Pts',(24.2755506671525,-5.2396661950629,12.));
#217500=CARTESIAN_POINT('Ctrl Pts',(24.2556428642294,-5.22473785822443,
12.));
#217501=CARTESIAN_POINT('Ctrl Pts',(24.2357654847766,-5.20990677629177,
12.));
#217502=CARTESIAN_POINT('Ctrl Pts',(24.2159191220171,-5.19517303753648,
12.));
#217503=CARTESIAN_POINT('Ctrl Pts',(24.1961043738755,-5.180536729614,12.));
#217504=CARTESIAN_POINT('Ctrl Pts',(24.1763218431344,-5.16599793957987,
12.));
#217505=CARTESIAN_POINT('Ctrl Pts',(24.1565721375971,-5.1515567539008,12.));
#217506=CARTESIAN_POINT('Ctrl Pts',(24.1368558702443,-5.13721325845746,
12.));
#217507=CARTESIAN_POINT('Ctrl Pts',(24.117173659394,-5.12296753853858,12.));
#217508=CARTESIAN_POINT('Ctrl Pts',(24.0975261288444,-5.10881967883126,
12.));
#217509=CARTESIAN_POINT('Ctrl Pts',(24.0779139079264,-5.09476976342618,
12.));
#217510=CARTESIAN_POINT('Ctrl Pts',(24.0583376315636,-5.08081787581271,
12.));
#217511=CARTESIAN_POINT('Ctrl Pts',(24.0387979403268,-5.0669640988664,12.));
#217512=CARTESIAN_POINT('Ctrl Pts',(24.0192954804896,-5.05320851483069,
12.));
#217513=CARTESIAN_POINT('Ctrl Pts',(23.9998309040747,-5.03955120528528,
12.));
#217514=CARTESIAN_POINT('Ctrl Pts',(23.9804048689228,-5.02599225112462,
12.));
#217515=CARTESIAN_POINT('Ctrl Pts',(23.9610180388271,-5.01253173257459,
12.));
#217516=CARTESIAN_POINT('Ctrl Pts',(23.9416710836528,-4.9991697291931,12.));
#217517=CARTESIAN_POINT('Ctrl Pts',(23.9223646794591,-4.98590631986534,
12.));
#217518=CARTESIAN_POINT('Ctrl Pts',(23.9030995086164,-4.9727415827923,12.));
#217519=CARTESIAN_POINT('Ctrl Pts',(23.883876259922,-4.95967559546566,12.));
#217520=CARTESIAN_POINT('Ctrl Pts',(23.8646956287172,-4.94670843465869,
12.));
#217521=CARTESIAN_POINT('Ctrl Pts',(23.8455583170062,-4.93384017643443,
12.));
#217522=CARTESIAN_POINT('Ctrl Pts',(23.8264650335721,-4.92107089613978,
12.));
#217523=CARTESIAN_POINT('Ctrl Pts',(23.8074164940897,-4.90840066839348,
12.));
#217524=CARTESIAN_POINT('Ctrl Pts',(23.7884134212381,-4.89582956706772,
12.));
#217525=CARTESIAN_POINT('Ctrl Pts',(23.7694565448044,-4.88335766525566,
12.));
#217526=CARTESIAN_POINT('Ctrl Pts',(23.7505466018239,-4.87098503527144,
12.));
#217527=CARTESIAN_POINT('Ctrl Pts',(23.7316843367308,-4.85871174865493,
12.));
#217528=CARTESIAN_POINT('Ctrl Pts',(23.7128705015014,-4.84653787616424,
12.));
#217529=CARTESIAN_POINT('Ctrl Pts',(23.6941058557971,-4.83446348776268,
12.));
#217530=CARTESIAN_POINT('Ctrl Pts',(23.6753911671023,-4.82248865259571,
12.));
#217531=CARTESIAN_POINT('Ctrl Pts',(23.6567272108631,-4.81061343896443,
12.));
#217532=CARTESIAN_POINT('Ctrl Pts',(23.6381147706581,-4.79883791433231,
12.));
#217533=CARTESIAN_POINT('Ctrl Pts',(23.6195546383625,-4.78716214532105,
12.));
#217534=CARTESIAN_POINT('Ctrl Pts',(23.6010476143099,-4.77558619769876,
12.));
#217535=CARTESIAN_POINT('Ctrl Pts',(23.5825945074535,-4.76411013636252,
12.));
#217536=CARTESIAN_POINT('Ctrl Pts',(23.564196135517,-4.75273402530616,12.));
#217537=CARTESIAN_POINT('Ctrl Pts',(23.5458533251715,-4.74145792760699,
12.));
#217538=CARTESIAN_POINT('Ctrl Pts',(23.5275669122378,-4.73028190543032,
12.));
#217539=CARTESIAN_POINT('Ctrl Pts',(23.5093377418784,-4.71920602001905,
12.));
#217540=CARTESIAN_POINT('Ctrl Pts',(23.491166668789,-4.70823033167821,12.));
#217541=CARTESIAN_POINT('Ctrl Pts',(23.4730545573849,-4.69735489975024,
12.));
#217542=CARTESIAN_POINT('Ctrl Pts',(23.4550022819852,-4.68657978258298,
12.));
#217543=CARTESIAN_POINT('Ctrl Pts',(23.4370107270444,-4.67590503753051,
12.));
#217544=CARTESIAN_POINT('Ctrl Pts',(23.4190807873798,-4.66533072094664,
12.));
#217545=CARTESIAN_POINT('Ctrl Pts',(23.4012133683957,-4.65485688816923,
12.));
#217546=CARTESIAN_POINT('Ctrl Pts',(23.383409386307,-4.64448359349936,12.));
#217547=CARTESIAN_POINT('Ctrl Pts',(23.3656697683496,-4.63421089016556,
12.));
#217548=CARTESIAN_POINT('Ctrl Pts',(23.3479954530281,-4.62403883030825,
12.));
#217549=CARTESIAN_POINT('Ctrl Pts',(23.3303873903947,-4.6139674649785,12.));
#217550=CARTESIAN_POINT('Ctrl Pts',(23.3128465423119,-4.60399684412176,
12.));
#217551=CARTESIAN_POINT('Ctrl Pts',(23.295373882719,-4.59412701655751,12.));
#217552=CARTESIAN_POINT('Ctrl Pts',(23.2779703978868,-4.58435802994675,
12.));
#217553=CARTESIAN_POINT('Ctrl Pts',(23.2606370866853,-4.57468993076071,
12.));
#217554=CARTESIAN_POINT('Ctrl Pts',(23.2433749609117,-4.56512276427812,
12.));
#217555=CARTESIAN_POINT('Ctrl Pts',(23.2261850456054,-4.55565657456957,
12.));
#217556=CARTESIAN_POINT('Ctrl Pts',(23.2090683793627,-4.54629140447543,
12.));
#217557=CARTESIAN_POINT('Ctrl Pts',(23.1920260146474,-4.53702729557586,
12.));
#217558=CARTESIAN_POINT('Ctrl Pts',(23.1750590180923,-4.52786428815049,
12.));
#217559=CARTESIAN_POINT('Ctrl Pts',(23.1581684708778,-4.51880242116786,
12.));
#217560=CARTESIAN_POINT('Ctrl Pts',(23.1413554691136,-4.50984173227088,
12.));
#217561=CARTESIAN_POINT('Ctrl Pts',(23.1246211242117,-4.5009822577518,12.));
#217562=CARTESIAN_POINT('Ctrl Pts',(23.1079665632629,-4.49222403252202,
12.));
#217563=CARTESIAN_POINT('Ctrl Pts',(23.0913929293909,-4.48356709006757,
12.));
#217564=CARTESIAN_POINT('Ctrl Pts',(23.0749013821867,-4.47501146242822,
12.));
#217565=CARTESIAN_POINT('Ctrl Pts',(23.0584930981723,-4.46655718018206,
12.));
#217566=CARTESIAN_POINT('Ctrl Pts',(23.0421692712466,-4.45820427241678,
12.));
#217567=CARTESIAN_POINT('Ctrl Pts',(23.0259311131395,-4.44995276669699,
12.));
#217568=CARTESIAN_POINT('Ctrl Pts',(23.0097798538399,-4.44180268901667,
12.));
#217569=CARTESIAN_POINT('Ctrl Pts',(22.9937167421009,-4.43375406376906,
12.));
#217570=CARTESIAN_POINT('Ctrl Pts',(22.9777430460021,-4.42580691372772,
12.));
#217571=CARTESIAN_POINT('Ctrl Pts',(22.9618600534866,-4.41796126001311,
12.));
#217572=CARTESIAN_POINT('Ctrl Pts',(22.9460690729092,-4.41021712205549,
12.));
#217573=CARTESIAN_POINT('Ctrl Pts',(22.9303714335549,-4.40257451754309,
12.));
#217574=CARTESIAN_POINT('Ctrl Pts',(22.9147684862425,-4.39503346238455,
12.));
#217575=CARTESIAN_POINT('Ctrl Pts',(22.8992616040108,-4.38759397068393,
12.));
#217576=CARTESIAN_POINT('Ctrl Pts',(22.8838521827702,-4.38025605470091,
12.));
#217577=CARTESIAN_POINT('Ctrl Pts',(22.8685416419725,-4.37301972480753,
12.));
#217578=CARTESIAN_POINT('Ctrl Pts',(22.8533314252419,-4.36588498943011,
12.));
#217579=CARTESIAN_POINT('Ctrl Pts',(22.838223001118,-4.3588518550056,12.));
#217580=CARTESIAN_POINT('Ctrl Pts',(22.8232178638873,-4.35192032594802,
12.));
#217581=CARTESIAN_POINT('Ctrl Pts',(22.808317534379,-4.34509040460066,12.));
#217582=CARTESIAN_POINT('Ctrl Pts',(22.7935235607807,-4.33836209118444,
12.));
#217583=CARTESIAN_POINT('Ctrl Pts',(22.7788375194081,-4.33173538373183,
12.));
#217584=CARTESIAN_POINT('Ctrl Pts',(22.764261015648,-4.32521027803748,12.));
#217585=CARTESIAN_POINT('Ctrl Pts',(22.7497956849852,-4.31878676761231,
12.));
#217586=CARTESIAN_POINT('Ctrl Pts',(22.7354431939926,-4.31246484362551,
12.));
#217587=CARTESIAN_POINT('Ctrl Pts',(22.7212052413384,-4.30624449484075,
12.));
#217588=CARTESIAN_POINT('Ctrl Pts',(22.707083558756,-4.30012570754067,12.));
#217589=CARTESIAN_POINT('Ctrl Pts',(22.6930799122545,-4.29410846547062,
12.));
#217590=CARTESIAN_POINT('Ctrl Pts',(22.6791961033536,-4.28819274977767,
12.));
#217591=CARTESIAN_POINT('Ctrl Pts',(22.665433970311,-4.2823785389406,12.));
#217592=CARTESIAN_POINT('Ctrl Pts',(22.6517953893303,-4.27666580869118,
12.));
#217593=CARTESIAN_POINT('Ctrl Pts',(22.6382822758171,-4.27105453193,12.));
#217594=CARTESIAN_POINT('Ctrl Pts',(22.6248965859975,-4.26554467865572,
12.));
#217595=CARTESIAN_POINT('Ctrl Pts',(22.611640318482,-4.26013621588304,12.));
#217596=CARTESIAN_POINT('Ctrl Pts',(22.5985155158637,-4.25482910755486,
12.));
#217597=CARTESIAN_POINT('Ctrl Pts',(22.5855242662479,-4.24962331444186,
12.));
#217598=CARTESIAN_POINT('Ctrl Pts',(22.5726687049922,-4.2445187940486,12.));
#217599=CARTESIAN_POINT('Ctrl Pts',(22.559951016643,-4.23951550052527,12.));
#217600=CARTESIAN_POINT('Ctrl Pts',(22.5473734368086,-4.23461338456714,
12.));
#217601=CARTESIAN_POINT('Ctrl Pts',(22.5349382540587,-4.22981239330733,
12.));
#217602=CARTESIAN_POINT('Ctrl Pts',(22.5226478117885,-4.22511247020041,
12.));
#217603=CARTESIAN_POINT('Ctrl Pts',(22.5105045108882,-4.22051355490198,
12.));
#217604=CARTESIAN_POINT('Ctrl Pts',(22.4985108124229,-4.21601558313909,
12.));
#217605=CARTESIAN_POINT('Ctrl Pts',(22.4866692403147,-4.21161848657429,
12.));
#217606=CARTESIAN_POINT('Ctrl Pts',(22.4749823839915,-4.20732219265649,
12.));
#217607=CARTESIAN_POINT('Ctrl Pts',(22.4634529011433,-4.20312662448172,
12.));
#217608=CARTESIAN_POINT('Ctrl Pts',(22.4520835205419,-4.19903170066356,
12.));
#217609=CARTESIAN_POINT('Ctrl Pts',(22.4408770448917,-4.19503733518862,
12.));
#217610=CARTESIAN_POINT('Ctrl Pts',(22.4298363535421,-4.19114343726943,
12.));
#217611=CARTESIAN_POINT('Ctrl Pts',(22.4189644056115,-4.18734991117722,
12.));
#217612=CARTESIAN_POINT('Ctrl Pts',(22.4082642454453,-4.18365665600852,
12.));
#217613=CARTESIAN_POINT('Ctrl Pts',(22.3977390078075,-4.18006356544883,
12.));
#217614=CARTESIAN_POINT('Ctrl Pts',(22.3873919231334,-4.17657052752826,
12.));
#217615=CARTESIAN_POINT('Ctrl Pts',(22.3772263228617,-4.17317742436146,
12.));
#217616=CARTESIAN_POINT('Ctrl Pts',(22.3672456427599,-4.16988413199458,
12.));
#217617=CARTESIAN_POINT('Ctrl Pts',(22.3574534257396,-4.16669052026601,
12.));
#217618=CARTESIAN_POINT('Ctrl Pts',(22.3478533253889,-4.16359645263189,
12.));
#217619=CARTESIAN_POINT('Ctrl Pts',(22.3384491078602,-4.16060178604165,
12.));
#217620=CARTESIAN_POINT('Ctrl Pts',(22.3292446628959,-4.15770637047891,
12.));
#217621=CARTESIAN_POINT('Ctrl Pts',(22.3202440186979,-4.15491004835282,
12.));
#217622=CARTESIAN_POINT('Ctrl Pts',(22.3114513545185,-4.15221265396991,
12.));
#217623=CARTESIAN_POINT('Ctrl Pts',(22.3028710166933,-4.14961401285523,
12.));
#217624=CARTESIAN_POINT('Ctrl Pts',(22.2945075198467,-4.14711394168557,
12.));
#217625=CARTESIAN_POINT('Ctrl Pts',(22.2863655389166,-4.14471224859297,
12.));
#217626=CARTESIAN_POINT('Ctrl Pts',(22.2784499072027,-4.14240873321985,
12.));
#217627=CARTESIAN_POINT('Ctrl Pts',(22.2707656042457,-4.14020318715992,
12.));
#217628=CARTESIAN_POINT('Ctrl Pts',(22.2633177913972,-4.13809539255423,
12.));
#217629=CARTESIAN_POINT('Ctrl Pts',(22.2561118708421,-4.13608511977227,
12.));
#217630=CARTESIAN_POINT('Ctrl Pts',(22.249153531779,-4.13417212558811,12.));
#217631=CARTESIAN_POINT('Ctrl Pts',(22.2424488153523,-4.13235615060161,
12.));
#217632=CARTESIAN_POINT('Ctrl Pts',(22.2360040565533,-4.13063692157499,
12.));
#217633=CARTESIAN_POINT('Ctrl Pts',(22.2298258043947,-4.1290141546338,12.));
#217634=CARTESIAN_POINT('Ctrl Pts',(22.2239207458781,-4.12748755830105,
12.));
#217635=CARTESIAN_POINT('Ctrl Pts',(22.2182956401341,-4.12605683613308,
12.));
#217636=CARTESIAN_POINT('Ctrl Pts',(22.2129576146671,-4.12472167516608,
12.));
#217637=CARTESIAN_POINT('Ctrl Pts',(22.2079143941719,-4.12348173702024,
12.));
#217638=CARTESIAN_POINT('Ctrl Pts',(22.2031746532106,-4.12233664408228,
12.));
#217639=CARTESIAN_POINT('Ctrl Pts',(22.1987479618246,-4.12128598183523,
12.));
#217640=CARTESIAN_POINT('Ctrl Pts',(22.1946440958098,-4.12032932637738,
12.));
#217641=CARTESIAN_POINT('Ctrl Pts',(22.1908725908525,-4.11946626228637,
12.));
#217642=CARTESIAN_POINT('Ctrl Pts',(22.1874419861496,-4.11869641271775,
12.));
#217643=CARTESIAN_POINT('Ctrl Pts',(22.1843613164855,-4.11801938107481,
12.));
#217644=CARTESIAN_POINT('Ctrl Pts',(22.1816414985788,-4.11743469691757,
12.));
#217645=CARTESIAN_POINT('Ctrl Pts',(22.179297473024,-4.11694173195005,12.));
#217646=CARTESIAN_POINT('Ctrl Pts',(22.177347426894,-4.11653973150519,12.));
#217647=CARTESIAN_POINT('Ctrl Pts',(22.1758088296598,-4.1162279721707,12.));
#217648=CARTESIAN_POINT('Ctrl Pts',(22.1746949858775,-4.11600589882846,
12.));
#217649=CARTESIAN_POINT('Ctrl Pts',(22.1741488021234,-4.11589976826168,
12.));
#217650=CARTESIAN_POINT('Ctrl Pts',(22.1739341411687,-4.11586035878288,
12.));
#217651=CARTESIAN_POINT('Ctrl Pts',(22.173877682324,-4.11585194677443,12.));
#217652=CARTESIAN_POINT('Ctrl Pts',(22.1738711152697,-4.11585220600463,
12.));
#217653=CARTESIAN_POINT('',(25.2771067246846,-6.088339316177,0.));
#217654=CARTESIAN_POINT('Origin',(19.4030938020118,-9.26120677397565,0.));
#217655=CARTESIAN_POINT('',(20.353053841303,-9.71462809124917,12.));
#217656=CARTESIAN_POINT('',(9.70154690100589,-4.63060338698782,12.));
#217657=CARTESIAN_POINT('',(20.353053841303,-9.71462809124917,0.));
#217658=CARTESIAN_POINT('',(20.353053841303,-9.71462809124917,0.));
#217659=CARTESIAN_POINT('',(9.70154690100589,-4.63060338698782,0.));
#217660=CARTESIAN_POINT('Ctrl Pts',(24.9347862158358,-7.36589684767345,
0.));
#217661=CARTESIAN_POINT('Ctrl Pts',(24.9347862158358,-7.36589684767345,
12.));
#217662=CARTESIAN_POINT('Ctrl Pts',(24.9292275670674,-7.36721909028843,
0.));
#217663=CARTESIAN_POINT('Ctrl Pts',(24.9292275670674,-7.36721909028843,
12.));
#217664=CARTESIAN_POINT('Ctrl Pts',(24.9181155530543,-7.36985593120091,
0.));
#217665=CARTESIAN_POINT('Ctrl Pts',(24.9181155530543,-7.36985593120091,
12.));
#217666=CARTESIAN_POINT('Ctrl Pts',(24.901463382605,-7.37378825961676,0.));
#217667=CARTESIAN_POINT('Ctrl Pts',(24.901463382605,-7.37378825961676,12.));
#217668=CARTESIAN_POINT('Ctrl Pts',(24.8792921911115,-7.3789854964027,0.));
#217669=CARTESIAN_POINT('Ctrl Pts',(24.8792921911115,-7.3789854964027,12.));
#217670=CARTESIAN_POINT('Ctrl Pts',(24.8516310625176,-7.38540558903621,
0.));
#217671=CARTESIAN_POINT('Ctrl Pts',(24.8516310625176,-7.38540558903621,
12.));
#217672=CARTESIAN_POINT('Ctrl Pts',(24.8240228520893,-7.39174922585809,
0.));
#217673=CARTESIAN_POINT('Ctrl Pts',(24.8240228520893,-7.39174922585809,
12.));
#217674=CARTESIAN_POINT('Ctrl Pts',(24.7964676646431,-7.39801641583013,
0.));
#217675=CARTESIAN_POINT('Ctrl Pts',(24.7964676646431,-7.39801641583013,
12.));
#217676=CARTESIAN_POINT('Ctrl Pts',(24.7689656668983,-7.40420718661603,
0.));
#217677=CARTESIAN_POINT('Ctrl Pts',(24.7689656668983,-7.40420718661603,
12.));
#217678=CARTESIAN_POINT('Ctrl Pts',(24.7415170994784,-7.41032159082382,
0.));
#217679=CARTESIAN_POINT('Ctrl Pts',(24.7415170994784,-7.41032159082382,
12.));
#217680=CARTESIAN_POINT('Ctrl Pts',(24.7141222950051,-7.41635971481674,
0.));
#217681=CARTESIAN_POINT('Ctrl Pts',(24.7141222950051,-7.41635971481674,
12.));
#217682=CARTESIAN_POINT('Ctrl Pts',(24.6867816727192,-7.42232167766266,
0.));
#217683=CARTESIAN_POINT('Ctrl Pts',(24.6867816727192,-7.42232167766266,
12.));
#217684=CARTESIAN_POINT('Ctrl Pts',(24.6594957128756,-7.42820762159126,
0.));
#217685=CARTESIAN_POINT('Ctrl Pts',(24.6594957128756,-7.42820762159126,
12.));
#217686=CARTESIAN_POINT('Ctrl Pts',(24.6322649369517,-7.43401770489524,
0.));
#217687=CARTESIAN_POINT('Ctrl Pts',(24.6322649369517,-7.43401770489524,
12.));
#217688=CARTESIAN_POINT('Ctrl Pts',(24.6050898852368,-7.43975209375504,
0.));
#217689=CARTESIAN_POINT('Ctrl Pts',(24.6050898852368,-7.43975209375504,
12.));
#217690=CARTESIAN_POINT('Ctrl Pts',(24.577971096086,-7.44541095473135,0.));
#217691=CARTESIAN_POINT('Ctrl Pts',(24.577971096086,-7.44541095473135,12.));
#217692=CARTESIAN_POINT('Ctrl Pts',(24.5509090831559,-7.4509944465116,0.));
#217693=CARTESIAN_POINT('Ctrl Pts',(24.5509090831559,-7.4509944465116,12.));
#217694=CARTESIAN_POINT('Ctrl Pts',(24.5239043173072,-7.45650271335862,
0.));
#217695=CARTESIAN_POINT('Ctrl Pts',(24.5239043173072,-7.45650271335862,
12.));
#217696=CARTESIAN_POINT('Ctrl Pts',(24.4969572391483,-7.46193588961464,
0.));
#217697=CARTESIAN_POINT('Ctrl Pts',(24.4969572391483,-7.46193588961464,
12.));
#217698=CARTESIAN_POINT('Ctrl Pts',(24.4700682684524,-7.46729410308787,
0.));
#217699=CARTESIAN_POINT('Ctrl Pts',(24.4700682684524,-7.46729410308787,
12.));
#217700=CARTESIAN_POINT('Ctrl Pts',(24.443237814649,-7.47257747883246,0.));
#217701=CARTESIAN_POINT('Ctrl Pts',(24.443237814649,-7.47257747883246,12.));
#217702=CARTESIAN_POINT('Ctrl Pts',(24.4164662871163,-7.47778614286565,
0.));
#217703=CARTESIAN_POINT('Ctrl Pts',(24.4164662871163,-7.47778614286565,
12.));
#217704=CARTESIAN_POINT('Ctrl Pts',(24.3897541049254,-7.48292022569301,
0.));
#217705=CARTESIAN_POINT('Ctrl Pts',(24.3897541049254,-7.48292022569301,
12.));
#217706=CARTESIAN_POINT('Ctrl Pts',(24.3631017084524,-7.48797986651909,
0.));
#217707=CARTESIAN_POINT('Ctrl Pts',(24.3631017084524,-7.48797986651909,
12.));
#217708=CARTESIAN_POINT('Ctrl Pts',(24.3365095573685,-7.49296521252421,
0.));
#217709=CARTESIAN_POINT('Ctrl Pts',(24.3365095573685,-7.49296521252421,
12.));
#217710=CARTESIAN_POINT('Ctrl Pts',(24.3099781253355,-7.49787641695439,
0.));
#217711=CARTESIAN_POINT('Ctrl Pts',(24.3099781253355,-7.49787641695439,
12.));
#217712=CARTESIAN_POINT('Ctrl Pts',(24.2835078958973,-7.50271363765152,
0.));
#217713=CARTESIAN_POINT('Ctrl Pts',(24.2835078958973,-7.50271363765152,
12.));
#217714=CARTESIAN_POINT('Ctrl Pts',(24.2570993577034,-7.50747703535134,
0.));
#217715=CARTESIAN_POINT('Ctrl Pts',(24.2570993577034,-7.50747703535134,
12.));
#217716=CARTESIAN_POINT('Ctrl Pts',(24.2307530003887,-7.51216677222181,
0.));
#217717=CARTESIAN_POINT('Ctrl Pts',(24.2307530003887,-7.51216677222181,
12.));
#217718=CARTESIAN_POINT('Ctrl Pts',(24.2044693092349,-7.51678300997949,
0.));
#217719=CARTESIAN_POINT('Ctrl Pts',(24.2044693092349,-7.51678300997949,
12.));
#217720=CARTESIAN_POINT('Ctrl Pts',(24.1782487641594,-7.52132590953802,
0.));
#217721=CARTESIAN_POINT('Ctrl Pts',(24.1782487641594,-7.52132590953802,
12.));
#217722=CARTESIAN_POINT('Ctrl Pts',(24.1520918425364,-7.52579563201424,
0.));
#217723=CARTESIAN_POINT('Ctrl Pts',(24.1520918425364,-7.52579563201424,
12.));
#217724=CARTESIAN_POINT('Ctrl Pts',(24.1259990209207,-7.53019233935502,
0.));
#217725=CARTESIAN_POINT('Ctrl Pts',(24.1259990209207,-7.53019233935502,
12.));
#217726=CARTESIAN_POINT('Ctrl Pts',(24.0999707772642,-7.53451619514649,
0.));
#217727=CARTESIAN_POINT('Ctrl Pts',(24.0999707772642,-7.53451619514649,
12.));
#217728=CARTESIAN_POINT('Ctrl Pts',(24.0740075927985,-7.53876736531014,
0.));
#217729=CARTESIAN_POINT('Ctrl Pts',(24.0740075927985,-7.53876736531014,
12.));
#217730=CARTESIAN_POINT('Ctrl Pts',(24.0481099543353,-7.54294601896145,
0.));
#217731=CARTESIAN_POINT('Ctrl Pts',(24.0481099543353,-7.54294601896145,
12.));
#217732=CARTESIAN_POINT('Ctrl Pts',(24.022278355453,-7.5470523288591,0.));
#217733=CARTESIAN_POINT('Ctrl Pts',(24.022278355453,-7.5470523288591,12.));
#217734=CARTESIAN_POINT('Ctrl Pts',(23.9965132953185,-7.55108647097441,
0.));
#217735=CARTESIAN_POINT('Ctrl Pts',(23.9965132953185,-7.55108647097441,
12.));
#217736=CARTESIAN_POINT('Ctrl Pts',(23.9708152779884,-7.55504862424812,
0.));
#217737=CARTESIAN_POINT('Ctrl Pts',(23.9708152779884,-7.55504862424812,
12.));
#217738=CARTESIAN_POINT('Ctrl Pts',(23.9451848115,-7.55893897027683,0.));
#217739=CARTESIAN_POINT('Ctrl Pts',(23.9451848115,-7.55893897027683,12.));
#217740=CARTESIAN_POINT('Ctrl Pts',(23.9196224070759,-7.56275769304773,
0.));
#217741=CARTESIAN_POINT('Ctrl Pts',(23.9196224070759,-7.56275769304773,
12.));
#217742=CARTESIAN_POINT('Ctrl Pts',(23.8941285782003,-7.56650497863792,
0.));
#217743=CARTESIAN_POINT('Ctrl Pts',(23.8941285782003,-7.56650497863792,
12.));
#217744=CARTESIAN_POINT('Ctrl Pts',(23.8687038399597,-7.57018101500711,
0.));
#217745=CARTESIAN_POINT('Ctrl Pts',(23.8687038399597,-7.57018101500711,
12.));
#217746=CARTESIAN_POINT('Ctrl Pts',(23.8433487096134,-7.57378599219817,
0.));
#217747=CARTESIAN_POINT('Ctrl Pts',(23.8433487096134,-7.57378599219817,
12.));
#217748=CARTESIAN_POINT('Ctrl Pts',(23.8180637069977,-7.57732010249066,
0.));
#217749=CARTESIAN_POINT('Ctrl Pts',(23.8180637069977,-7.57732010249066,
12.));
#217750=CARTESIAN_POINT('Ctrl Pts',(23.7928493549908,-7.58078354058212,
0.));
#217751=CARTESIAN_POINT('Ctrl Pts',(23.7928493549908,-7.58078354058212,
12.));
#217752=CARTESIAN_POINT('Ctrl Pts',(23.7677061799376,-7.58417650376272,
0.));
#217753=CARTESIAN_POINT('Ctrl Pts',(23.7677061799376,-7.58417650376272,
12.));
#217754=CARTESIAN_POINT('Ctrl Pts',(23.7426347121006,-7.58749919210832,
0.));
#217755=CARTESIAN_POINT('Ctrl Pts',(23.7426347121006,-7.58749919210832,
12.));
#217756=CARTESIAN_POINT('Ctrl Pts',(23.7176354860457,-7.59075180865327,
0.));
#217757=CARTESIAN_POINT('Ctrl Pts',(23.7176354860457,-7.59075180865327,
12.));
#217758=CARTESIAN_POINT('Ctrl Pts',(23.6927090405067,-7.59393455934042,
0.));
#217759=CARTESIAN_POINT('Ctrl Pts',(23.6927090405067,-7.59393455934042,
12.));
#217760=CARTESIAN_POINT('Ctrl Pts',(23.6678559182876,-7.59704765299572,
0.));
#217761=CARTESIAN_POINT('Ctrl Pts',(23.6678559182876,-7.59704765299572,
12.));
#217762=CARTESIAN_POINT('Ctrl Pts',(23.6430766661419,-7.6000913013013,0.));
#217763=CARTESIAN_POINT('Ctrl Pts',(23.6430766661419,-7.6000913013013,12.));
#217764=CARTESIAN_POINT('Ctrl Pts',(23.6183718346576,-7.60306571877806,
0.));
#217765=CARTESIAN_POINT('Ctrl Pts',(23.6183718346576,-7.60306571877806,
12.));
#217766=CARTESIAN_POINT('Ctrl Pts',(23.5937419781244,-7.60597112277094,
0.));
#217767=CARTESIAN_POINT('Ctrl Pts',(23.5937419781244,-7.60597112277094,
12.));
#217768=CARTESIAN_POINT('Ctrl Pts',(23.5691876544243,-7.608807733446,0.));
#217769=CARTESIAN_POINT('Ctrl Pts',(23.5691876544243,-7.608807733446,12.));
#217770=CARTESIAN_POINT('Ctrl Pts',(23.5447094252028,-7.61157577385372,
0.));
#217771=CARTESIAN_POINT('Ctrl Pts',(23.5447094252028,-7.61157577385372,
12.));
#217772=CARTESIAN_POINT('Ctrl Pts',(23.5203078560128,-7.61427546999299,
0.));
#217773=CARTESIAN_POINT('Ctrl Pts',(23.5203078560128,-7.61427546999299,
12.));
#217774=CARTESIAN_POINT('Ctrl Pts',(23.4959835164608,-7.61690705088319,
0.));
#217775=CARTESIAN_POINT('Ctrl Pts',(23.4959835164608,-7.61690705088319,
12.));
#217776=CARTESIAN_POINT('Ctrl Pts',(23.4717369803438,-7.61947074863978,
0.));
#217777=CARTESIAN_POINT('Ctrl Pts',(23.4717369803438,-7.61947074863978,
12.));
#217778=CARTESIAN_POINT('Ctrl Pts',(23.4475688257854,-7.62196679855957,
0.));
#217779=CARTESIAN_POINT('Ctrl Pts',(23.4475688257854,-7.62196679855957,
12.));
#217780=CARTESIAN_POINT('Ctrl Pts',(23.4234796353544,-7.62439543920055,
0.));
#217781=CARTESIAN_POINT('Ctrl Pts',(23.4234796353544,-7.62439543920055,
12.));
#217782=CARTESIAN_POINT('Ctrl Pts',(23.3994699961122,-7.62675691240335,
0.));
#217783=CARTESIAN_POINT('Ctrl Pts',(23.3994699961122,-7.62675691240335,
12.));
#217784=CARTESIAN_POINT('Ctrl Pts',(23.3755404996638,-7.62905146332598,
0.));
#217785=CARTESIAN_POINT('Ctrl Pts',(23.3755404996638,-7.62905146332598,
12.));
#217786=CARTESIAN_POINT('Ctrl Pts',(23.3516917421973,-7.63127934048139,
0.));
#217787=CARTESIAN_POINT('Ctrl Pts',(23.3516917421973,-7.63127934048139,
12.));
#217788=CARTESIAN_POINT('Ctrl Pts',(23.3279243245241,-7.63344079578163,
0.));
#217789=CARTESIAN_POINT('Ctrl Pts',(23.3279243245241,-7.63344079578163,
12.));
#217790=CARTESIAN_POINT('Ctrl Pts',(23.3042388521021,-7.63553608458784,
0.));
#217791=CARTESIAN_POINT('Ctrl Pts',(23.3042388521021,-7.63553608458784,
12.));
#217792=CARTESIAN_POINT('Ctrl Pts',(23.2806359350853,-7.63756546576375,
0.));
#217793=CARTESIAN_POINT('Ctrl Pts',(23.2806359350853,-7.63756546576375,
12.));
#217794=CARTESIAN_POINT('Ctrl Pts',(23.2571161884487,-7.63952920172837,
0.));
#217795=CARTESIAN_POINT('Ctrl Pts',(23.2571161884487,-7.63952920172837,
12.));
#217796=CARTESIAN_POINT('Ctrl Pts',(23.2336802320912,-7.64142755851508,
0.));
#217797=CARTESIAN_POINT('Ctrl Pts',(23.2336802320912,-7.64142755851508,
12.));
#217798=CARTESIAN_POINT('Ctrl Pts',(23.2103286909399,-7.64326080583684,
0.));
#217799=CARTESIAN_POINT('Ctrl Pts',(23.2103286909399,-7.64326080583684,
12.));
#217800=CARTESIAN_POINT('Ctrl Pts',(23.1870621950452,-7.64502921715483,
0.));
#217801=CARTESIAN_POINT('Ctrl Pts',(23.1870621950452,-7.64502921715483,
12.));
#217802=CARTESIAN_POINT('Ctrl Pts',(23.1638813796691,-7.64673306975797,
0.));
#217803=CARTESIAN_POINT('Ctrl Pts',(23.1638813796691,-7.64673306975797,
12.));
#217804=CARTESIAN_POINT('Ctrl Pts',(23.1407868853815,-7.64837264482929,
0.));
#217805=CARTESIAN_POINT('Ctrl Pts',(23.1407868853815,-7.64837264482929,
12.));
#217806=CARTESIAN_POINT('Ctrl Pts',(23.1177793581674,-7.64994822749845,
0.));
#217807=CARTESIAN_POINT('Ctrl Pts',(23.1177793581674,-7.64994822749845,
12.));
#217808=CARTESIAN_POINT('Ctrl Pts',(23.0948594495246,-7.65146010690465,
0.));
#217809=CARTESIAN_POINT('Ctrl Pts',(23.0948594495246,-7.65146010690465,
12.));
#217810=CARTESIAN_POINT('Ctrl Pts',(23.072027816555,-7.65290857626357,0.));
#217811=CARTESIAN_POINT('Ctrl Pts',(23.072027816555,-7.65290857626357,12.));
#217812=CARTESIAN_POINT('Ctrl Pts',(23.049285122053,-7.65429393293955,0.));
#217813=CARTESIAN_POINT('Ctrl Pts',(23.049285122053,-7.65429393293955,12.));
#217814=CARTESIAN_POINT('Ctrl Pts',(23.0266320345792,-7.65561647852555,
0.));
#217815=CARTESIAN_POINT('Ctrl Pts',(23.0266320345792,-7.65561647852555,
12.));
#217816=CARTESIAN_POINT('Ctrl Pts',(23.004069228582,-7.6568765189133,0.));
#217817=CARTESIAN_POINT('Ctrl Pts',(23.004069228582,-7.6568765189133,12.));
#217818=CARTESIAN_POINT('Ctrl Pts',(22.9815973845301,-7.65807436436453,
0.));
#217819=CARTESIAN_POINT('Ctrl Pts',(22.9815973845301,-7.65807436436453,
12.));
#217820=CARTESIAN_POINT('Ctrl Pts',(22.9592171890332,-7.65921032958912,
0.));
#217821=CARTESIAN_POINT('Ctrl Pts',(22.9592171890332,-7.65921032958912,
12.));
#217822=CARTESIAN_POINT('Ctrl Pts',(22.9369293349592,-7.66028473382777,
0.));
#217823=CARTESIAN_POINT('Ctrl Pts',(22.9369293349592,-7.66028473382777,
12.));
#217824=CARTESIAN_POINT('Ctrl Pts',(22.9147345215418,-7.661297900941,0.));
#217825=CARTESIAN_POINT('Ctrl Pts',(22.9147345215418,-7.661297900941,12.));
#217826=CARTESIAN_POINT('Ctrl Pts',(22.8926334544879,-7.66225015950148,
0.));
#217827=CARTESIAN_POINT('Ctrl Pts',(22.8926334544879,-7.66225015950148,
12.));
#217828=CARTESIAN_POINT('Ctrl Pts',(22.870626846128,-7.66314184287334,0.));
#217829=CARTESIAN_POINT('Ctrl Pts',(22.870626846128,-7.66314184287334,12.));
#217830=CARTESIAN_POINT('Ctrl Pts',(22.8487154155569,-7.66397328929805,
0.));
#217831=CARTESIAN_POINT('Ctrl Pts',(22.8487154155569,-7.66397328929805,
12.));
#217832=CARTESIAN_POINT('Ctrl Pts',(22.8268998887678,-7.66474484198553,
0.));
#217833=CARTESIAN_POINT('Ctrl Pts',(22.8268998887678,-7.66474484198553,
12.));
#217834=CARTESIAN_POINT('Ctrl Pts',(22.8051809987833,-7.66545684920988,
0.));
#217835=CARTESIAN_POINT('Ctrl Pts',(22.8051809987833,-7.66545684920988,
12.));
#217836=CARTESIAN_POINT('Ctrl Pts',(22.7835594857697,-7.66610966441259,
0.));
#217837=CARTESIAN_POINT('Ctrl Pts',(22.7835594857697,-7.66610966441259,
12.));
#217838=CARTESIAN_POINT('Ctrl Pts',(22.7620360971839,-7.66670364630273,
0.));
#217839=CARTESIAN_POINT('Ctrl Pts',(22.7620360971839,-7.66670364630273,
12.));
#217840=CARTESIAN_POINT('Ctrl Pts',(22.7406115879508,-7.66723915895413,
0.));
#217841=CARTESIAN_POINT('Ctrl Pts',(22.7406115879508,-7.66723915895413,
12.));
#217842=CARTESIAN_POINT('Ctrl Pts',(22.7192867206242,-7.6677165719101,0.));
#217843=CARTESIAN_POINT('Ctrl Pts',(22.7192867206242,-7.6677165719101,12.));
#217844=CARTESIAN_POINT('Ctrl Pts',(22.6980622655446,-7.66813626029277,
0.));
#217845=CARTESIAN_POINT('Ctrl Pts',(22.6980622655446,-7.66813626029277,
12.));
#217846=CARTESIAN_POINT('Ctrl Pts',(22.6769390009889,-7.66849860491763,
0.));
#217847=CARTESIAN_POINT('Ctrl Pts',(22.6769390009889,-7.66849860491763,
12.));
#217848=CARTESIAN_POINT('Ctrl Pts',(22.6559177133133,-7.66880399241354,
0.));
#217849=CARTESIAN_POINT('Ctrl Pts',(22.6559177133133,-7.66880399241354,
12.));
#217850=CARTESIAN_POINT('Ctrl Pts',(22.6349991971547,-7.66905281533745,
0.));
#217851=CARTESIAN_POINT('Ctrl Pts',(22.6349991971547,-7.66905281533745,
12.));
#217852=CARTESIAN_POINT('Ctrl Pts',(22.6141842556248,-7.66924547229435,
0.));
#217853=CARTESIAN_POINT('Ctrl Pts',(22.6141842556248,-7.66924547229435,
12.));
#217854=CARTESIAN_POINT('Ctrl Pts',(22.5934737004955,-7.66938236806241,
0.));
#217855=CARTESIAN_POINT('Ctrl Pts',(22.5934737004955,-7.66938236806241,
12.));
#217856=CARTESIAN_POINT('Ctrl Pts',(22.5728683523828,-7.66946391372299,
0.));
#217857=CARTESIAN_POINT('Ctrl Pts',(22.5728683523828,-7.66946391372299,
12.));
#217858=CARTESIAN_POINT('Ctrl Pts',(22.5523690409109,-7.66949052679672,
0.));
#217859=CARTESIAN_POINT('Ctrl Pts',(22.5523690409109,-7.66949052679672,
12.));
#217860=CARTESIAN_POINT('Ctrl Pts',(22.5319766049191,-7.66946263138116,
0.));
#217861=CARTESIAN_POINT('Ctrl Pts',(22.5319766049191,-7.66946263138116,
12.));
#217862=CARTESIAN_POINT('Ctrl Pts',(22.5116918927023,-7.66938065829083,
0.));
#217863=CARTESIAN_POINT('Ctrl Pts',(22.5116918927023,-7.66938065829083,
12.));
#217864=CARTESIAN_POINT('Ctrl Pts',(22.4915157622308,-7.66924504520302,
0.));
#217865=CARTESIAN_POINT('Ctrl Pts',(22.4915157622308,-7.66924504520302,
12.));
#217866=CARTESIAN_POINT('Ctrl Pts',(22.47144908137,-7.66905623680836,0.));
#217867=CARTESIAN_POINT('Ctrl Pts',(22.47144908137,-7.66905623680836,12.));
#217868=CARTESIAN_POINT('Ctrl Pts',(22.4514927280862,-7.6688146849666,0.));
#217869=CARTESIAN_POINT('Ctrl Pts',(22.4514927280862,-7.6688146849666,12.));
#217870=CARTESIAN_POINT('Ctrl Pts',(22.4316475906616,-7.66852084886746,
0.));
#217871=CARTESIAN_POINT('Ctrl Pts',(22.4316475906616,-7.66852084886746,
12.));
#217872=CARTESIAN_POINT('Ctrl Pts',(22.411914567977,-7.66817519519682,0.));
#217873=CARTESIAN_POINT('Ctrl Pts',(22.411914567977,-7.66817519519682,12.));
#217874=CARTESIAN_POINT('Ctrl Pts',(22.3922945697782,-7.6677781983082,0.));
#217875=CARTESIAN_POINT('Ctrl Pts',(22.3922945697782,-7.6677781983082,12.));
#217876=CARTESIAN_POINT('Ctrl Pts',(22.3727885169361,-7.66733034039887,
0.));
#217877=CARTESIAN_POINT('Ctrl Pts',(22.3727885169361,-7.66733034039887,
12.));
#217878=CARTESIAN_POINT('Ctrl Pts',(22.3533973417013,-7.66683211169134,
0.));
#217879=CARTESIAN_POINT('Ctrl Pts',(22.3533973417013,-7.66683211169134,
12.));
#217880=CARTESIAN_POINT('Ctrl Pts',(22.3341219879454,-7.66628401061906,
0.));
#217881=CARTESIAN_POINT('Ctrl Pts',(22.3341219879454,-7.66628401061906,
12.));
#217882=CARTESIAN_POINT('Ctrl Pts',(22.3149634114823,-7.66568654402442,
0.));
#217883=CARTESIAN_POINT('Ctrl Pts',(22.3149634114823,-7.66568654402442,
12.));
#217884=CARTESIAN_POINT('Ctrl Pts',(22.2959225803925,-7.66504022736263,
0.));
#217885=CARTESIAN_POINT('Ctrl Pts',(22.2959225803925,-7.66504022736263,
12.));
#217886=CARTESIAN_POINT('Ctrl Pts',(22.2770004753332,-7.66434558490973,
0.));
#217887=CARTESIAN_POINT('Ctrl Pts',(22.2770004753332,-7.66434558490973,
12.));
#217888=CARTESIAN_POINT('Ctrl Pts',(22.2581980898487,-7.66360314997662,
0.));
#217889=CARTESIAN_POINT('Ctrl Pts',(22.2581980898487,-7.66360314997662,
12.));
#217890=CARTESIAN_POINT('Ctrl Pts',(22.239516430656,-7.66281346512546,0.));
#217891=CARTESIAN_POINT('Ctrl Pts',(22.239516430656,-7.66281346512546,12.));
#217892=CARTESIAN_POINT('Ctrl Pts',(22.2209565180098,-7.66197708240436,
0.));
#217893=CARTESIAN_POINT('Ctrl Pts',(22.2209565180098,-7.66197708240436,
12.));
#217894=CARTESIAN_POINT('Ctrl Pts',(22.2025193860972,-7.66109456359292,
0.));
#217895=CARTESIAN_POINT('Ctrl Pts',(22.2025193860972,-7.66109456359292,
12.));
#217896=CARTESIAN_POINT('Ctrl Pts',(22.1842060834092,-7.66016648045008,
0.));
#217897=CARTESIAN_POINT('Ctrl Pts',(22.1842060834092,-7.66016648045008,
12.));
#217898=CARTESIAN_POINT('Ctrl Pts',(22.1660176731174,-7.65919341496926,
0.));
#217899=CARTESIAN_POINT('Ctrl Pts',(22.1660176731174,-7.65919341496926,
12.));
#217900=CARTESIAN_POINT('Ctrl Pts',(22.1479552334206,-7.65817595963351,
0.));
#217901=CARTESIAN_POINT('Ctrl Pts',(22.1479552334206,-7.65817595963351,
12.));
#217902=CARTESIAN_POINT('Ctrl Pts',(22.1300198579671,-7.65711471769407,
0.));
#217903=CARTESIAN_POINT('Ctrl Pts',(22.1300198579671,-7.65711471769407,
12.));
#217904=CARTESIAN_POINT('Ctrl Pts',(22.1122126563327,-7.65601030346819,
0.));
#217905=CARTESIAN_POINT('Ctrl Pts',(22.1122126563327,-7.65601030346819,
12.));
#217906=CARTESIAN_POINT('Ctrl Pts',(22.094534754469,-7.65486334263651,0.));
#217907=CARTESIAN_POINT('Ctrl Pts',(22.094534754469,-7.65486334263651,12.));
#217908=CARTESIAN_POINT('Ctrl Pts',(22.0769872951596,-7.65367447254945,
0.));
#217909=CARTESIAN_POINT('Ctrl Pts',(22.0769872951596,-7.65367447254945,
12.));
#217910=CARTESIAN_POINT('Ctrl Pts',(22.0595714384432,-7.65244434253104,
0.));
#217911=CARTESIAN_POINT('Ctrl Pts',(22.0595714384432,-7.65244434253104,
12.));
#217912=CARTESIAN_POINT('Ctrl Pts',(22.0422883621176,-7.65117361421347,
0.));
#217913=CARTESIAN_POINT('Ctrl Pts',(22.0422883621176,-7.65117361421347,
12.));
#217914=CARTESIAN_POINT('Ctrl Pts',(22.0251392623209,-7.64986296190157,
0.));
#217915=CARTESIAN_POINT('Ctrl Pts',(22.0251392623209,-7.64986296190157,
12.));
#217916=CARTESIAN_POINT('Ctrl Pts',(22.0081253540773,-7.64851307293346,
0.));
#217917=CARTESIAN_POINT('Ctrl Pts',(22.0081253540773,-7.64851307293346,
12.));
#217918=CARTESIAN_POINT('Ctrl Pts',(21.9912478718542,-7.64712464805258,
0.));
#217919=CARTESIAN_POINT('Ctrl Pts',(21.9912478718542,-7.64712464805258,
12.));
#217920=CARTESIAN_POINT('Ctrl Pts',(21.97450807008,-7.64569840177359,0.));
#217921=CARTESIAN_POINT('Ctrl Pts',(21.97450807008,-7.64569840177359,12.));
#217922=CARTESIAN_POINT('Ctrl Pts',(21.9579072237653,-7.64423506279154,
0.));
#217923=CARTESIAN_POINT('Ctrl Pts',(21.9579072237653,-7.64423506279154,
12.));
#217924=CARTESIAN_POINT('Ctrl Pts',(21.9414466292074,-7.64273537442707,
0.));
#217925=CARTESIAN_POINT('Ctrl Pts',(21.9414466292074,-7.64273537442707,
12.));
#217926=CARTESIAN_POINT('Ctrl Pts',(21.9251276046546,-7.6412000950654,0.));
#217927=CARTESIAN_POINT('Ctrl Pts',(21.9251276046546,-7.6412000950654,12.));
#217928=CARTESIAN_POINT('Ctrl Pts',(21.9089514909873,-7.63962999860917,
0.));
#217929=CARTESIAN_POINT('Ctrl Pts',(21.9089514909873,-7.63962999860917,
12.));
#217930=CARTESIAN_POINT('Ctrl Pts',(21.8929196523511,-7.63802587492008,
0.));
#217931=CARTESIAN_POINT('Ctrl Pts',(21.8929196523511,-7.63802587492008,
12.));
#217932=CARTESIAN_POINT('Ctrl Pts',(21.8770334769492,-7.63638853033368,
0.));
#217933=CARTESIAN_POINT('Ctrl Pts',(21.8770334769492,-7.63638853033368,
12.));
#217934=CARTESIAN_POINT('Ctrl Pts',(21.8612943779086,-7.63471878821204,
0.));
#217935=CARTESIAN_POINT('Ctrl Pts',(21.8612943779086,-7.63471878821204,
12.));
#217936=CARTESIAN_POINT('Ctrl Pts',(21.8457037941084,-7.63301748948936,
0.));
#217937=CARTESIAN_POINT('Ctrl Pts',(21.8457037941084,-7.63301748948936,
12.));
#217938=CARTESIAN_POINT('Ctrl Pts',(21.8302631910197,-7.6312854932304,0.));
#217939=CARTESIAN_POINT('Ctrl Pts',(21.8302631910197,-7.6312854932304,12.));
#217940=CARTESIAN_POINT('Ctrl Pts',(21.8149740615093,-7.62952367718151,
0.));
#217941=CARTESIAN_POINT('Ctrl Pts',(21.8149740615093,-7.62952367718151,
12.));
#217942=CARTESIAN_POINT('Ctrl Pts',(21.7998379268583,-7.62773293842409,
0.));
#217943=CARTESIAN_POINT('Ctrl Pts',(21.7998379268583,-7.62773293842409,
12.));
#217944=CARTESIAN_POINT('Ctrl Pts',(21.7848563378022,-7.62591419404521,
0.));
#217945=CARTESIAN_POINT('Ctrl Pts',(21.7848563378022,-7.62591419404521,
12.));
#217946=CARTESIAN_POINT('Ctrl Pts',(21.7700308755583,-7.62406838181164,
0.));
#217947=CARTESIAN_POINT('Ctrl Pts',(21.7700308755583,-7.62406838181164,
12.));
#217948=CARTESIAN_POINT('Ctrl Pts',(21.7553631528329,-7.62219646084226,
0.));
#217949=CARTESIAN_POINT('Ctrl Pts',(21.7553631528329,-7.62219646084226,
12.));
#217950=CARTESIAN_POINT('Ctrl Pts',(21.7408548148657,-7.62029941230855,
0.));
#217951=CARTESIAN_POINT('Ctrl Pts',(21.7408548148657,-7.62029941230855,
12.));
#217952=CARTESIAN_POINT('Ctrl Pts',(21.7265075407977,-7.61837824030542,
0.));
#217953=CARTESIAN_POINT('Ctrl Pts',(21.7265075407977,-7.61837824030542,
12.));
#217954=CARTESIAN_POINT('Ctrl Pts',(21.7123230449835,-7.61643397270425,
0.));
#217955=CARTESIAN_POINT('Ctrl Pts',(21.7123230449835,-7.61643397270425,
12.));
#217956=CARTESIAN_POINT('Ctrl Pts',(21.6983030783321,-7.61446766202787,
0.));
#217957=CARTESIAN_POINT('Ctrl Pts',(21.6983030783321,-7.61446766202787,
12.));
#217958=CARTESIAN_POINT('Ctrl Pts',(21.6844494295813,-7.61248038630265,
0.));
#217959=CARTESIAN_POINT('Ctrl Pts',(21.6844494295813,-7.61248038630265,
12.));
#217960=CARTESIAN_POINT('Ctrl Pts',(21.6707639267573,-7.6104732500095,0.));
#217961=CARTESIAN_POINT('Ctrl Pts',(21.6707639267573,-7.6104732500095,12.));
#217962=CARTESIAN_POINT('Ctrl Pts',(21.6572484388079,-7.60844738512872,
0.));
#217963=CARTESIAN_POINT('Ctrl Pts',(21.6572484388079,-7.60844738512872,
12.));
#217964=CARTESIAN_POINT('Ctrl Pts',(21.6439048771743,-7.60640395216359,
0.));
#217965=CARTESIAN_POINT('Ctrl Pts',(21.6439048771743,-7.60640395216359,
12.));
#217966=CARTESIAN_POINT('Ctrl Pts',(21.6307351973823,-7.604344141183,0.));
#217967=CARTESIAN_POINT('Ctrl Pts',(21.6307351973823,-7.604344141183,12.));
#217968=CARTESIAN_POINT('Ctrl Pts',(21.6177414005991,-7.60226917285432,
0.));
#217969=CARTESIAN_POINT('Ctrl Pts',(21.6177414005991,-7.60226917285432,
12.));
#217970=CARTESIAN_POINT('Ctrl Pts',(21.6049255358842,-7.60018029988238,
0.));
#217971=CARTESIAN_POINT('Ctrl Pts',(21.6049255358842,-7.60018029988238,
12.));
#217972=CARTESIAN_POINT('Ctrl Pts',(21.5922897024466,-7.59807880846193,
0.));
#217973=CARTESIAN_POINT('Ctrl Pts',(21.5922897024466,-7.59807880846193,
12.));
#217974=CARTESIAN_POINT('Ctrl Pts',(21.5798360518978,-7.59596601973589,
0.));
#217975=CARTESIAN_POINT('Ctrl Pts',(21.5798360518978,-7.59596601973589,
12.));
#217976=CARTESIAN_POINT('Ctrl Pts',(21.5675667904728,-7.5938432912493,0.));
#217977=CARTESIAN_POINT('Ctrl Pts',(21.5675667904728,-7.5938432912493,12.));
#217978=CARTESIAN_POINT('Ctrl Pts',(21.5554841813465,-7.59171201844793,
0.));
#217979=CARTESIAN_POINT('Ctrl Pts',(21.5554841813465,-7.59171201844793,
12.));
#217980=CARTESIAN_POINT('Ctrl Pts',(21.5435905470113,-7.58957363620026,
0.));
#217981=CARTESIAN_POINT('Ctrl Pts',(21.5435905470113,-7.58957363620026,
12.));
#217982=CARTESIAN_POINT('Ctrl Pts',(21.5318882716735,-7.58742962034834,
0.));
#217983=CARTESIAN_POINT('Ctrl Pts',(21.5318882716735,-7.58742962034834,
12.));
#217984=CARTESIAN_POINT('Ctrl Pts',(21.5203798035294,-7.58528148919114,
0.));
#217985=CARTESIAN_POINT('Ctrl Pts',(21.5203798035294,-7.58528148919114,
12.));
#217986=CARTESIAN_POINT('Ctrl Pts',(21.5090676573866,-7.58313080519159,
0.));
#217987=CARTESIAN_POINT('Ctrl Pts',(21.5090676573866,-7.58313080519159,
12.));
#217988=CARTESIAN_POINT('Ctrl Pts',(21.4979544192739,-7.5809791779073,0.));
#217989=CARTESIAN_POINT('Ctrl Pts',(21.4979544192739,-7.5809791779073,12.));
#217990=CARTESIAN_POINT('Ctrl Pts',(21.4870427508193,-7.57882826679131,
0.));
#217991=CARTESIAN_POINT('Ctrl Pts',(21.4870427508193,-7.57882826679131,
12.));
#217992=CARTESIAN_POINT('Ctrl Pts',(21.4763353936766,-7.57667978403003,
0.));
#217993=CARTESIAN_POINT('Ctrl Pts',(21.4763353936766,-7.57667978403003,
12.));
#217994=CARTESIAN_POINT('Ctrl Pts',(21.4658351740135,-7.57453549743435,
0.));
#217995=CARTESIAN_POINT('Ctrl Pts',(21.4658351740135,-7.57453549743435,
12.));
#217996=CARTESIAN_POINT('Ctrl Pts',(21.4555450053147,-7.57239723223521,
0.));
#217997=CARTESIAN_POINT('Ctrl Pts',(21.4555450053147,-7.57239723223521,
12.));
#217998=CARTESIAN_POINT('Ctrl Pts',(21.445467890751,-7.5702668726117,0.));
#217999=CARTESIAN_POINT('Ctrl Pts',(21.445467890751,-7.5702668726117,12.));
#218000=CARTESIAN_POINT('Ctrl Pts',(21.435606926151,-7.56814636360842,0.));
#218001=CARTESIAN_POINT('Ctrl Pts',(21.435606926151,-7.56814636360842,12.));
#218002=CARTESIAN_POINT('Ctrl Pts',(21.4259653015732,-7.56603771218706,
0.));
#218003=CARTESIAN_POINT('Ctrl Pts',(21.4259653015732,-7.56603771218706,
12.));
#218004=CARTESIAN_POINT('Ctrl Pts',(21.4165463106252,-7.56394299313683,
0.));
#218005=CARTESIAN_POINT('Ctrl Pts',(21.4165463106252,-7.56394299313683,
12.));
#218006=CARTESIAN_POINT('Ctrl Pts',(21.4073533630364,-7.56186435703622,
0.));
#218007=CARTESIAN_POINT('Ctrl Pts',(21.4073533630364,-7.56186435703622,
12.));
#218008=CARTESIAN_POINT('Ctrl Pts',(21.3983899952988,-7.55980403700615,
0.));
#218009=CARTESIAN_POINT('Ctrl Pts',(21.3983899952988,-7.55980403700615,
12.));
#218010=CARTESIAN_POINT('Ctrl Pts',(21.3896598842119,-7.55776435731422,
0.));
#218011=CARTESIAN_POINT('Ctrl Pts',(21.3896598842119,-7.55776435731422,
12.));
#218012=CARTESIAN_POINT('Ctrl Pts',(21.3811668478933,-7.55574773403508,
0.));
#218013=CARTESIAN_POINT('Ctrl Pts',(21.3811668478933,-7.55574773403508,
12.));
#218014=CARTESIAN_POINT('Ctrl Pts',(21.3729148390244,-7.55375667080032,
0.));
#218015=CARTESIAN_POINT('Ctrl Pts',(21.3729148390244,-7.55375667080032,
12.));
#218016=CARTESIAN_POINT('Ctrl Pts',(21.3649079431864,-7.55179375777442,
0.));
#218017=CARTESIAN_POINT('Ctrl Pts',(21.3649079431864,-7.55179375777442,
12.));
#218018=CARTESIAN_POINT('Ctrl Pts',(21.3571503685853,-7.54986166521307,
0.));
#218019=CARTESIAN_POINT('Ctrl Pts',(21.3571503685853,-7.54986166521307,
12.));
#218020=CARTESIAN_POINT('Ctrl Pts',(21.349646476153,-7.54796316246327,0.));
#218021=CARTESIAN_POINT('Ctrl Pts',(21.349646476153,-7.54796316246327,12.));
#218022=CARTESIAN_POINT('Ctrl Pts',(21.3424008295038,-7.54610114948351,
0.));
#218023=CARTESIAN_POINT('Ctrl Pts',(21.3424008295038,-7.54610114948351,
12.));
#218024=CARTESIAN_POINT('Ctrl Pts',(21.3354182340149,-7.54427868151269,
0.));
#218025=CARTESIAN_POINT('Ctrl Pts',(21.3354182340149,-7.54427868151269,
12.));
#218026=CARTESIAN_POINT('Ctrl Pts',(21.328703791771,-7.54249900377032,0.));
#218027=CARTESIAN_POINT('Ctrl Pts',(21.328703791771,-7.54249900377032,12.));
#218028=CARTESIAN_POINT('Ctrl Pts',(21.3222628524165,-7.5407655203828,0.));
#218029=CARTESIAN_POINT('Ctrl Pts',(21.3222628524165,-7.5407655203828,12.));
#218030=CARTESIAN_POINT('Ctrl Pts',(21.3161009456256,-7.53908175169899,
0.));
#218031=CARTESIAN_POINT('Ctrl Pts',(21.3161009456256,-7.53908175169899,
12.));
#218032=CARTESIAN_POINT('Ctrl Pts',(21.3102237167729,-7.5374512936462,0.));
#218033=CARTESIAN_POINT('Ctrl Pts',(21.3102237167729,-7.5374512936462,12.));
#218034=CARTESIAN_POINT('Ctrl Pts',(21.3046368712156,-7.53587778251743,
0.));
#218035=CARTESIAN_POINT('Ctrl Pts',(21.3046368712156,-7.53587778251743,
12.));
#218036=CARTESIAN_POINT('Ctrl Pts',(21.2993464250717,-7.53436505309949,
0.));
#218037=CARTESIAN_POINT('Ctrl Pts',(21.2993464250717,-7.53436505309949,
12.));
#218038=CARTESIAN_POINT('Ctrl Pts',(21.2943588989331,-7.53291726078527,
0.));
#218039=CARTESIAN_POINT('Ctrl Pts',(21.2943588989331,-7.53291726078527,
12.));
#218040=CARTESIAN_POINT('Ctrl Pts',(21.2896816163843,-7.53153906987847,
0.));
#218041=CARTESIAN_POINT('Ctrl Pts',(21.2896816163843,-7.53153906987847,
12.));
#218042=CARTESIAN_POINT('Ctrl Pts',(21.2853226580658,-7.53023562438221,
0.));
#218043=CARTESIAN_POINT('Ctrl Pts',(21.2853226580658,-7.53023562438221,
12.));
#218044=CARTESIAN_POINT('Ctrl Pts',(21.2812902781143,-7.52901217930407,
0.));
#218045=CARTESIAN_POINT('Ctrl Pts',(21.2812902781143,-7.52901217930407,
12.));
#218046=CARTESIAN_POINT('Ctrl Pts',(21.2775925269651,-7.52787386225344,
0.));
#218047=CARTESIAN_POINT('Ctrl Pts',(21.2775925269651,-7.52787386225344,
12.));
#218048=CARTESIAN_POINT('Ctrl Pts',(21.2742366113578,-7.52682526918561,
0.));
#218049=CARTESIAN_POINT('Ctrl Pts',(21.2742366113578,-7.52682526918561,
12.));
#218050=CARTESIAN_POINT('Ctrl Pts',(21.2712301573465,-7.52587126095544,
0.));
#218051=CARTESIAN_POINT('Ctrl Pts',(21.2712301573465,-7.52587126095544,
12.));
#218052=CARTESIAN_POINT('Ctrl Pts',(21.2685823838672,-7.52501770333522,
0.));
#218053=CARTESIAN_POINT('Ctrl Pts',(21.2685823838672,-7.52501770333522,
12.));
#218054=CARTESIAN_POINT('Ctrl Pts',(21.266305915706,-7.52427261074264,0.));
#218055=CARTESIAN_POINT('Ctrl Pts',(21.266305915706,-7.52427261074264,12.));
#218056=CARTESIAN_POINT('Ctrl Pts',(21.2644161259965,-7.52364573027521,
0.));
#218057=CARTESIAN_POINT('Ctrl Pts',(21.2644161259965,-7.52364573027521,
12.));
#218058=CARTESIAN_POINT('Ctrl Pts',(21.262927782038,-7.52314642316203,0.));
#218059=CARTESIAN_POINT('Ctrl Pts',(21.262927782038,-7.52314642316203,12.));
#218060=CARTESIAN_POINT('Ctrl Pts',(21.261852128355,-7.52278182242728,0.));
#218061=CARTESIAN_POINT('Ctrl Pts',(21.261852128355,-7.52278182242728,12.));
#218062=CARTESIAN_POINT('Ctrl Pts',(21.2613260540651,-7.52260064231736,
0.));
#218063=CARTESIAN_POINT('Ctrl Pts',(21.2613260540651,-7.52260064231736,
12.));
#218064=CARTESIAN_POINT('Ctrl Pts',(21.261120447486,-7.52252744144958,0.));
#218065=CARTESIAN_POINT('Ctrl Pts',(21.261120447486,-7.52252744144958,12.));
#218066=CARTESIAN_POINT('Ctrl Pts',(21.2610673466883,-7.52250649703992,
0.));
#218067=CARTESIAN_POINT('Ctrl Pts',(21.2610673466883,-7.52250649703992,
12.));
#218068=CARTESIAN_POINT('Ctrl Pts',(21.2610617890679,-7.52250298901266,
0.));
#218069=CARTESIAN_POINT('Ctrl Pts',(21.2610617890679,-7.52250298901266,
12.));
#218070=CARTESIAN_POINT('',(24.9347862158358,-7.36589684767345,0.));
#218071=CARTESIAN_POINT('Ctrl Pts',(24.9347862158358,-7.36589684767345,
0.));
#218072=CARTESIAN_POINT('Ctrl Pts',(24.9292275670674,-7.36721909028843,
0.));
#218073=CARTESIAN_POINT('Ctrl Pts',(24.9181155530543,-7.36985593120091,
0.));
#218074=CARTESIAN_POINT('Ctrl Pts',(24.901463382605,-7.37378825961676,0.));
#218075=CARTESIAN_POINT('Ctrl Pts',(24.8792921911115,-7.3789854964027,0.));
#218076=CARTESIAN_POINT('Ctrl Pts',(24.8516310625176,-7.38540558903621,
0.));
#218077=CARTESIAN_POINT('Ctrl Pts',(24.8240228520893,-7.39174922585809,
0.));
#218078=CARTESIAN_POINT('Ctrl Pts',(24.7964676646431,-7.39801641583013,
0.));
#218079=CARTESIAN_POINT('Ctrl Pts',(24.7689656668983,-7.40420718661603,
0.));
#218080=CARTESIAN_POINT('Ctrl Pts',(24.7415170994784,-7.41032159082382,
0.));
#218081=CARTESIAN_POINT('Ctrl Pts',(24.7141222950051,-7.41635971481674,
0.));
#218082=CARTESIAN_POINT('Ctrl Pts',(24.6867816727192,-7.42232167766266,
0.));
#218083=CARTESIAN_POINT('Ctrl Pts',(24.6594957128756,-7.42820762159126,
0.));
#218084=CARTESIAN_POINT('Ctrl Pts',(24.6322649369517,-7.43401770489524,
0.));
#218085=CARTESIAN_POINT('Ctrl Pts',(24.6050898852368,-7.43975209375504,
0.));
#218086=CARTESIAN_POINT('Ctrl Pts',(24.577971096086,-7.44541095473135,0.));
#218087=CARTESIAN_POINT('Ctrl Pts',(24.5509090831559,-7.4509944465116,0.));
#218088=CARTESIAN_POINT('Ctrl Pts',(24.5239043173072,-7.45650271335862,
0.));
#218089=CARTESIAN_POINT('Ctrl Pts',(24.4969572391483,-7.46193588961464,
0.));
#218090=CARTESIAN_POINT('Ctrl Pts',(24.4700682684524,-7.46729410308787,
0.));
#218091=CARTESIAN_POINT('Ctrl Pts',(24.443237814649,-7.47257747883246,0.));
#218092=CARTESIAN_POINT('Ctrl Pts',(24.4164662871163,-7.47778614286565,
0.));
#218093=CARTESIAN_POINT('Ctrl Pts',(24.3897541049254,-7.48292022569301,
0.));
#218094=CARTESIAN_POINT('Ctrl Pts',(24.3631017084524,-7.48797986651909,
0.));
#218095=CARTESIAN_POINT('Ctrl Pts',(24.3365095573685,-7.49296521252421,
0.));
#218096=CARTESIAN_POINT('Ctrl Pts',(24.3099781253355,-7.49787641695439,
0.));
#218097=CARTESIAN_POINT('Ctrl Pts',(24.2835078958973,-7.50271363765152,
0.));
#218098=CARTESIAN_POINT('Ctrl Pts',(24.2570993577034,-7.50747703535134,
0.));
#218099=CARTESIAN_POINT('Ctrl Pts',(24.2307530003887,-7.51216677222181,
0.));
#218100=CARTESIAN_POINT('Ctrl Pts',(24.2044693092349,-7.51678300997949,
0.));
#218101=CARTESIAN_POINT('Ctrl Pts',(24.1782487641594,-7.52132590953802,
0.));
#218102=CARTESIAN_POINT('Ctrl Pts',(24.1520918425364,-7.52579563201424,
0.));
#218103=CARTESIAN_POINT('Ctrl Pts',(24.1259990209207,-7.53019233935502,
0.));
#218104=CARTESIAN_POINT('Ctrl Pts',(24.0999707772642,-7.53451619514649,
0.));
#218105=CARTESIAN_POINT('Ctrl Pts',(24.0740075927985,-7.53876736531014,
0.));
#218106=CARTESIAN_POINT('Ctrl Pts',(24.0481099543353,-7.54294601896145,
0.));
#218107=CARTESIAN_POINT('Ctrl Pts',(24.022278355453,-7.5470523288591,0.));
#218108=CARTESIAN_POINT('Ctrl Pts',(23.9965132953185,-7.55108647097441,
0.));
#218109=CARTESIAN_POINT('Ctrl Pts',(23.9708152779884,-7.55504862424812,
0.));
#218110=CARTESIAN_POINT('Ctrl Pts',(23.9451848115,-7.55893897027683,0.));
#218111=CARTESIAN_POINT('Ctrl Pts',(23.9196224070759,-7.56275769304773,
0.));
#218112=CARTESIAN_POINT('Ctrl Pts',(23.8941285782003,-7.56650497863792,
0.));
#218113=CARTESIAN_POINT('Ctrl Pts',(23.8687038399597,-7.57018101500711,
0.));
#218114=CARTESIAN_POINT('Ctrl Pts',(23.8433487096134,-7.57378599219817,
0.));
#218115=CARTESIAN_POINT('Ctrl Pts',(23.8180637069977,-7.57732010249066,
0.));
#218116=CARTESIAN_POINT('Ctrl Pts',(23.7928493549908,-7.58078354058212,
0.));
#218117=CARTESIAN_POINT('Ctrl Pts',(23.7677061799376,-7.58417650376272,
0.));
#218118=CARTESIAN_POINT('Ctrl Pts',(23.7426347121006,-7.58749919210832,
0.));
#218119=CARTESIAN_POINT('Ctrl Pts',(23.7176354860457,-7.59075180865327,
0.));
#218120=CARTESIAN_POINT('Ctrl Pts',(23.6927090405067,-7.59393455934042,
0.));
#218121=CARTESIAN_POINT('Ctrl Pts',(23.6678559182876,-7.59704765299572,
0.));
#218122=CARTESIAN_POINT('Ctrl Pts',(23.6430766661419,-7.6000913013013,0.));
#218123=CARTESIAN_POINT('Ctrl Pts',(23.6183718346576,-7.60306571877806,
0.));
#218124=CARTESIAN_POINT('Ctrl Pts',(23.5937419781244,-7.60597112277094,
0.));
#218125=CARTESIAN_POINT('Ctrl Pts',(23.5691876544243,-7.608807733446,0.));
#218126=CARTESIAN_POINT('Ctrl Pts',(23.5447094252028,-7.61157577385372,
0.));
#218127=CARTESIAN_POINT('Ctrl Pts',(23.5203078560128,-7.61427546999299,
0.));
#218128=CARTESIAN_POINT('Ctrl Pts',(23.4959835164608,-7.61690705088319,
0.));
#218129=CARTESIAN_POINT('Ctrl Pts',(23.4717369803438,-7.61947074863978,
0.));
#218130=CARTESIAN_POINT('Ctrl Pts',(23.4475688257854,-7.62196679855957,
0.));
#218131=CARTESIAN_POINT('Ctrl Pts',(23.4234796353544,-7.62439543920055,
0.));
#218132=CARTESIAN_POINT('Ctrl Pts',(23.3994699961122,-7.62675691240335,
0.));
#218133=CARTESIAN_POINT('Ctrl Pts',(23.3755404996638,-7.62905146332598,
0.));
#218134=CARTESIAN_POINT('Ctrl Pts',(23.3516917421973,-7.63127934048139,
0.));
#218135=CARTESIAN_POINT('Ctrl Pts',(23.3279243245241,-7.63344079578163,
0.));
#218136=CARTESIAN_POINT('Ctrl Pts',(23.3042388521021,-7.63553608458784,
0.));
#218137=CARTESIAN_POINT('Ctrl Pts',(23.2806359350853,-7.63756546576375,
0.));
#218138=CARTESIAN_POINT('Ctrl Pts',(23.2571161884487,-7.63952920172837,
0.));
#218139=CARTESIAN_POINT('Ctrl Pts',(23.2336802320912,-7.64142755851508,
0.));
#218140=CARTESIAN_POINT('Ctrl Pts',(23.2103286909399,-7.64326080583684,
0.));
#218141=CARTESIAN_POINT('Ctrl Pts',(23.1870621950452,-7.64502921715483,
0.));
#218142=CARTESIAN_POINT('Ctrl Pts',(23.1638813796691,-7.64673306975797,
0.));
#218143=CARTESIAN_POINT('Ctrl Pts',(23.1407868853815,-7.64837264482929,
0.));
#218144=CARTESIAN_POINT('Ctrl Pts',(23.1177793581674,-7.64994822749845,
0.));
#218145=CARTESIAN_POINT('Ctrl Pts',(23.0948594495246,-7.65146010690465,
0.));
#218146=CARTESIAN_POINT('Ctrl Pts',(23.072027816555,-7.65290857626357,0.));
#218147=CARTESIAN_POINT('Ctrl Pts',(23.049285122053,-7.65429393293955,0.));
#218148=CARTESIAN_POINT('Ctrl Pts',(23.0266320345792,-7.65561647852555,
0.));
#218149=CARTESIAN_POINT('Ctrl Pts',(23.004069228582,-7.6568765189133,0.));
#218150=CARTESIAN_POINT('Ctrl Pts',(22.9815973845301,-7.65807436436453,
0.));
#218151=CARTESIAN_POINT('Ctrl Pts',(22.9592171890332,-7.65921032958912,
0.));
#218152=CARTESIAN_POINT('Ctrl Pts',(22.9369293349592,-7.66028473382777,
0.));
#218153=CARTESIAN_POINT('Ctrl Pts',(22.9147345215418,-7.661297900941,0.));
#218154=CARTESIAN_POINT('Ctrl Pts',(22.8926334544879,-7.66225015950148,
0.));
#218155=CARTESIAN_POINT('Ctrl Pts',(22.870626846128,-7.66314184287334,0.));
#218156=CARTESIAN_POINT('Ctrl Pts',(22.8487154155569,-7.66397328929805,
0.));
#218157=CARTESIAN_POINT('Ctrl Pts',(22.8268998887678,-7.66474484198553,
0.));
#218158=CARTESIAN_POINT('Ctrl Pts',(22.8051809987833,-7.66545684920988,
0.));
#218159=CARTESIAN_POINT('Ctrl Pts',(22.7835594857697,-7.66610966441259,
0.));
#218160=CARTESIAN_POINT('Ctrl Pts',(22.7620360971839,-7.66670364630273,
0.));
#218161=CARTESIAN_POINT('Ctrl Pts',(22.7406115879508,-7.66723915895413,
0.));
#218162=CARTESIAN_POINT('Ctrl Pts',(22.7192867206242,-7.6677165719101,0.));
#218163=CARTESIAN_POINT('Ctrl Pts',(22.6980622655446,-7.66813626029277,
0.));
#218164=CARTESIAN_POINT('Ctrl Pts',(22.6769390009889,-7.66849860491763,
0.));
#218165=CARTESIAN_POINT('Ctrl Pts',(22.6559177133133,-7.66880399241354,
0.));
#218166=CARTESIAN_POINT('Ctrl Pts',(22.6349991971547,-7.66905281533745,
0.));
#218167=CARTESIAN_POINT('Ctrl Pts',(22.6141842556248,-7.66924547229435,
0.));
#218168=CARTESIAN_POINT('Ctrl Pts',(22.5934737004955,-7.66938236806241,
0.));
#218169=CARTESIAN_POINT('Ctrl Pts',(22.5728683523828,-7.66946391372299,
0.));
#218170=CARTESIAN_POINT('Ctrl Pts',(22.5523690409109,-7.66949052679672,
0.));
#218171=CARTESIAN_POINT('Ctrl Pts',(22.5319766049191,-7.66946263138116,
0.));
#218172=CARTESIAN_POINT('Ctrl Pts',(22.5116918927023,-7.66938065829083,
0.));
#218173=CARTESIAN_POINT('Ctrl Pts',(22.4915157622308,-7.66924504520302,
0.));
#218174=CARTESIAN_POINT('Ctrl Pts',(22.47144908137,-7.66905623680836,0.));
#218175=CARTESIAN_POINT('Ctrl Pts',(22.4514927280862,-7.6688146849666,0.));
#218176=CARTESIAN_POINT('Ctrl Pts',(22.4316475906616,-7.66852084886746,
0.));
#218177=CARTESIAN_POINT('Ctrl Pts',(22.411914567977,-7.66817519519682,0.));
#218178=CARTESIAN_POINT('Ctrl Pts',(22.3922945697782,-7.6677781983082,0.));
#218179=CARTESIAN_POINT('Ctrl Pts',(22.3727885169361,-7.66733034039887,
0.));
#218180=CARTESIAN_POINT('Ctrl Pts',(22.3533973417013,-7.66683211169134,
0.));
#218181=CARTESIAN_POINT('Ctrl Pts',(22.3341219879454,-7.66628401061906,
0.));
#218182=CARTESIAN_POINT('Ctrl Pts',(22.3149634114823,-7.66568654402442,
0.));
#218183=CARTESIAN_POINT('Ctrl Pts',(22.2959225803925,-7.66504022736263,
0.));
#218184=CARTESIAN_POINT('Ctrl Pts',(22.2770004753332,-7.66434558490973,
0.));
#218185=CARTESIAN_POINT('Ctrl Pts',(22.2581980898487,-7.66360314997662,
0.));
#218186=CARTESIAN_POINT('Ctrl Pts',(22.239516430656,-7.66281346512546,0.));
#218187=CARTESIAN_POINT('Ctrl Pts',(22.2209565180098,-7.66197708240436,
0.));
#218188=CARTESIAN_POINT('Ctrl Pts',(22.2025193860972,-7.66109456359292,
0.));
#218189=CARTESIAN_POINT('Ctrl Pts',(22.1842060834092,-7.66016648045008,
0.));
#218190=CARTESIAN_POINT('Ctrl Pts',(22.1660176731174,-7.65919341496926,
0.));
#218191=CARTESIAN_POINT('Ctrl Pts',(22.1479552334206,-7.65817595963351,
0.));
#218192=CARTESIAN_POINT('Ctrl Pts',(22.1300198579671,-7.65711471769407,
0.));
#218193=CARTESIAN_POINT('Ctrl Pts',(22.1122126563327,-7.65601030346819,
0.));
#218194=CARTESIAN_POINT('Ctrl Pts',(22.094534754469,-7.65486334263651,0.));
#218195=CARTESIAN_POINT('Ctrl Pts',(22.0769872951596,-7.65367447254945,
0.));
#218196=CARTESIAN_POINT('Ctrl Pts',(22.0595714384432,-7.65244434253104,
0.));
#218197=CARTESIAN_POINT('Ctrl Pts',(22.0422883621176,-7.65117361421347,
0.));
#218198=CARTESIAN_POINT('Ctrl Pts',(22.0251392623209,-7.64986296190157,
0.));
#218199=CARTESIAN_POINT('Ctrl Pts',(22.0081253540773,-7.64851307293346,
0.));
#218200=CARTESIAN_POINT('Ctrl Pts',(21.9912478718542,-7.64712464805258,
0.));
#218201=CARTESIAN_POINT('Ctrl Pts',(21.97450807008,-7.64569840177359,0.));
#218202=CARTESIAN_POINT('Ctrl Pts',(21.9579072237653,-7.64423506279154,
0.));
#218203=CARTESIAN_POINT('Ctrl Pts',(21.9414466292074,-7.64273537442707,
0.));
#218204=CARTESIAN_POINT('Ctrl Pts',(21.9251276046546,-7.6412000950654,0.));
#218205=CARTESIAN_POINT('Ctrl Pts',(21.9089514909873,-7.63962999860917,
0.));
#218206=CARTESIAN_POINT('Ctrl Pts',(21.8929196523511,-7.63802587492008,
0.));
#218207=CARTESIAN_POINT('Ctrl Pts',(21.8770334769492,-7.63638853033368,
0.));
#218208=CARTESIAN_POINT('Ctrl Pts',(21.8612943779086,-7.63471878821204,
0.));
#218209=CARTESIAN_POINT('Ctrl Pts',(21.8457037941084,-7.63301748948936,
0.));
#218210=CARTESIAN_POINT('Ctrl Pts',(21.8302631910197,-7.6312854932304,0.));
#218211=CARTESIAN_POINT('Ctrl Pts',(21.8149740615093,-7.62952367718151,
0.));
#218212=CARTESIAN_POINT('Ctrl Pts',(21.7998379268583,-7.62773293842409,
0.));
#218213=CARTESIAN_POINT('Ctrl Pts',(21.7848563378022,-7.62591419404521,
0.));
#218214=CARTESIAN_POINT('Ctrl Pts',(21.7700308755583,-7.62406838181164,
0.));
#218215=CARTESIAN_POINT('Ctrl Pts',(21.7553631528329,-7.62219646084226,
0.));
#218216=CARTESIAN_POINT('Ctrl Pts',(21.7408548148657,-7.62029941230855,
0.));
#218217=CARTESIAN_POINT('Ctrl Pts',(21.7265075407977,-7.61837824030542,
0.));
#218218=CARTESIAN_POINT('Ctrl Pts',(21.7123230449835,-7.61643397270425,
0.));
#218219=CARTESIAN_POINT('Ctrl Pts',(21.6983030783321,-7.61446766202787,
0.));
#218220=CARTESIAN_POINT('Ctrl Pts',(21.6844494295813,-7.61248038630265,
0.));
#218221=CARTESIAN_POINT('Ctrl Pts',(21.6707639267573,-7.6104732500095,0.));
#218222=CARTESIAN_POINT('Ctrl Pts',(21.6572484388079,-7.60844738512872,
0.));
#218223=CARTESIAN_POINT('Ctrl Pts',(21.6439048771743,-7.60640395216359,
0.));
#218224=CARTESIAN_POINT('Ctrl Pts',(21.6307351973823,-7.604344141183,0.));
#218225=CARTESIAN_POINT('Ctrl Pts',(21.6177414005991,-7.60226917285432,
0.));
#218226=CARTESIAN_POINT('Ctrl Pts',(21.6049255358842,-7.60018029988238,
0.));
#218227=CARTESIAN_POINT('Ctrl Pts',(21.5922897024466,-7.59807880846193,
0.));
#218228=CARTESIAN_POINT('Ctrl Pts',(21.5798360518978,-7.59596601973589,
0.));
#218229=CARTESIAN_POINT('Ctrl Pts',(21.5675667904728,-7.5938432912493,0.));
#218230=CARTESIAN_POINT('Ctrl Pts',(21.5554841813465,-7.59171201844793,
0.));
#218231=CARTESIAN_POINT('Ctrl Pts',(21.5435905470113,-7.58957363620026,
0.));
#218232=CARTESIAN_POINT('Ctrl Pts',(21.5318882716735,-7.58742962034834,
0.));
#218233=CARTESIAN_POINT('Ctrl Pts',(21.5203798035294,-7.58528148919114,
0.));
#218234=CARTESIAN_POINT('Ctrl Pts',(21.5090676573866,-7.58313080519159,
0.));
#218235=CARTESIAN_POINT('Ctrl Pts',(21.4979544192739,-7.5809791779073,0.));
#218236=CARTESIAN_POINT('Ctrl Pts',(21.4870427508193,-7.57882826679131,
0.));
#218237=CARTESIAN_POINT('Ctrl Pts',(21.4763353936766,-7.57667978403003,
0.));
#218238=CARTESIAN_POINT('Ctrl Pts',(21.4658351740135,-7.57453549743435,
0.));
#218239=CARTESIAN_POINT('Ctrl Pts',(21.4555450053147,-7.57239723223521,
0.));
#218240=CARTESIAN_POINT('Ctrl Pts',(21.445467890751,-7.5702668726117,0.));
#218241=CARTESIAN_POINT('Ctrl Pts',(21.435606926151,-7.56814636360842,0.));
#218242=CARTESIAN_POINT('Ctrl Pts',(21.4259653015732,-7.56603771218706,
0.));
#218243=CARTESIAN_POINT('Ctrl Pts',(21.4165463106252,-7.56394299313683,
0.));
#218244=CARTESIAN_POINT('Ctrl Pts',(21.4073533630364,-7.56186435703622,
0.));
#218245=CARTESIAN_POINT('Ctrl Pts',(21.3983899952988,-7.55980403700615,
0.));
#218246=CARTESIAN_POINT('Ctrl Pts',(21.3896598842119,-7.55776435731422,
0.));
#218247=CARTESIAN_POINT('Ctrl Pts',(21.3811668478933,-7.55574773403508,
0.));
#218248=CARTESIAN_POINT('Ctrl Pts',(21.3729148390244,-7.55375667080032,
0.));
#218249=CARTESIAN_POINT('Ctrl Pts',(21.3649079431864,-7.55179375777442,
0.));
#218250=CARTESIAN_POINT('Ctrl Pts',(21.3571503685853,-7.54986166521307,
0.));
#218251=CARTESIAN_POINT('Ctrl Pts',(21.349646476153,-7.54796316246327,0.));
#218252=CARTESIAN_POINT('Ctrl Pts',(21.3424008295038,-7.54610114948351,
0.));
#218253=CARTESIAN_POINT('Ctrl Pts',(21.3354182340149,-7.54427868151269,
0.));
#218254=CARTESIAN_POINT('Ctrl Pts',(21.328703791771,-7.54249900377032,0.));
#218255=CARTESIAN_POINT('Ctrl Pts',(21.3222628524165,-7.5407655203828,0.));
#218256=CARTESIAN_POINT('Ctrl Pts',(21.3161009456256,-7.53908175169899,
0.));
#218257=CARTESIAN_POINT('Ctrl Pts',(21.3102237167729,-7.5374512936462,0.));
#218258=CARTESIAN_POINT('Ctrl Pts',(21.3046368712156,-7.53587778251743,
0.));
#218259=CARTESIAN_POINT('Ctrl Pts',(21.2993464250717,-7.53436505309949,
0.));
#218260=CARTESIAN_POINT('Ctrl Pts',(21.2943588989331,-7.53291726078527,
0.));
#218261=CARTESIAN_POINT('Ctrl Pts',(21.2896816163843,-7.53153906987847,
0.));
#218262=CARTESIAN_POINT('Ctrl Pts',(21.2853226580658,-7.53023562438221,
0.));
#218263=CARTESIAN_POINT('Ctrl Pts',(21.2812902781143,-7.52901217930407,
0.));
#218264=CARTESIAN_POINT('Ctrl Pts',(21.2775925269651,-7.52787386225344,
0.));
#218265=CARTESIAN_POINT('Ctrl Pts',(21.2742366113578,-7.52682526918561,
0.));
#218266=CARTESIAN_POINT('Ctrl Pts',(21.2712301573465,-7.52587126095544,
0.));
#218267=CARTESIAN_POINT('Ctrl Pts',(21.2685823838672,-7.52501770333522,
0.));
#218268=CARTESIAN_POINT('Ctrl Pts',(21.266305915706,-7.52427261074264,0.));
#218269=CARTESIAN_POINT('Ctrl Pts',(21.2644161259965,-7.52364573027521,
0.));
#218270=CARTESIAN_POINT('Ctrl Pts',(21.262927782038,-7.52314642316203,0.));
#218271=CARTESIAN_POINT('Ctrl Pts',(21.261852128355,-7.52278182242728,0.));
#218272=CARTESIAN_POINT('Ctrl Pts',(21.2613260540651,-7.52260064231736,
0.));
#218273=CARTESIAN_POINT('Ctrl Pts',(21.261120447486,-7.52252744144958,0.));
#218274=CARTESIAN_POINT('Ctrl Pts',(21.2610673466883,-7.52250649703992,
0.));
#218275=CARTESIAN_POINT('Ctrl Pts',(21.2610617890679,-7.52250298901266,
0.));
#218276=CARTESIAN_POINT('',(24.9347862158358,-7.36589684767345,12.));
#218277=CARTESIAN_POINT('',(24.9347862158358,-7.36589684767345,0.));
#218278=CARTESIAN_POINT('Ctrl Pts',(21.2610617890679,-7.52250298901266,
12.));
#218279=CARTESIAN_POINT('Ctrl Pts',(21.2610673466883,-7.52250649703992,
12.));
#218280=CARTESIAN_POINT('Ctrl Pts',(21.261120447486,-7.52252744144958,12.));
#218281=CARTESIAN_POINT('Ctrl Pts',(21.2613260540651,-7.52260064231736,
12.));
#218282=CARTESIAN_POINT('Ctrl Pts',(21.261852128355,-7.52278182242728,12.));
#218283=CARTESIAN_POINT('Ctrl Pts',(21.262927782038,-7.52314642316203,12.));
#218284=CARTESIAN_POINT('Ctrl Pts',(21.2644161259965,-7.52364573027521,
12.));
#218285=CARTESIAN_POINT('Ctrl Pts',(21.266305915706,-7.52427261074264,12.));
#218286=CARTESIAN_POINT('Ctrl Pts',(21.2685823838672,-7.52501770333522,
12.));
#218287=CARTESIAN_POINT('Ctrl Pts',(21.2712301573465,-7.52587126095544,
12.));
#218288=CARTESIAN_POINT('Ctrl Pts',(21.2742366113578,-7.52682526918561,
12.));
#218289=CARTESIAN_POINT('Ctrl Pts',(21.2775925269651,-7.52787386225344,
12.));
#218290=CARTESIAN_POINT('Ctrl Pts',(21.2812902781143,-7.52901217930407,
12.));
#218291=CARTESIAN_POINT('Ctrl Pts',(21.2853226580658,-7.53023562438221,
12.));
#218292=CARTESIAN_POINT('Ctrl Pts',(21.2896816163843,-7.53153906987847,
12.));
#218293=CARTESIAN_POINT('Ctrl Pts',(21.2943588989331,-7.53291726078527,
12.));
#218294=CARTESIAN_POINT('Ctrl Pts',(21.2993464250717,-7.53436505309949,
12.));
#218295=CARTESIAN_POINT('Ctrl Pts',(21.3046368712156,-7.53587778251743,
12.));
#218296=CARTESIAN_POINT('Ctrl Pts',(21.3102237167729,-7.5374512936462,12.));
#218297=CARTESIAN_POINT('Ctrl Pts',(21.3161009456256,-7.53908175169899,
12.));
#218298=CARTESIAN_POINT('Ctrl Pts',(21.3222628524165,-7.5407655203828,12.));
#218299=CARTESIAN_POINT('Ctrl Pts',(21.328703791771,-7.54249900377032,12.));
#218300=CARTESIAN_POINT('Ctrl Pts',(21.3354182340149,-7.54427868151269,
12.));
#218301=CARTESIAN_POINT('Ctrl Pts',(21.3424008295038,-7.54610114948351,
12.));
#218302=CARTESIAN_POINT('Ctrl Pts',(21.349646476153,-7.54796316246327,12.));
#218303=CARTESIAN_POINT('Ctrl Pts',(21.3571503685853,-7.54986166521307,
12.));
#218304=CARTESIAN_POINT('Ctrl Pts',(21.3649079431864,-7.55179375777442,
12.));
#218305=CARTESIAN_POINT('Ctrl Pts',(21.3729148390244,-7.55375667080032,
12.));
#218306=CARTESIAN_POINT('Ctrl Pts',(21.3811668478933,-7.55574773403508,
12.));
#218307=CARTESIAN_POINT('Ctrl Pts',(21.3896598842119,-7.55776435731422,
12.));
#218308=CARTESIAN_POINT('Ctrl Pts',(21.3983899952988,-7.55980403700615,
12.));
#218309=CARTESIAN_POINT('Ctrl Pts',(21.4073533630364,-7.56186435703622,
12.));
#218310=CARTESIAN_POINT('Ctrl Pts',(21.4165463106252,-7.56394299313683,
12.));
#218311=CARTESIAN_POINT('Ctrl Pts',(21.4259653015732,-7.56603771218706,
12.));
#218312=CARTESIAN_POINT('Ctrl Pts',(21.435606926151,-7.56814636360842,12.));
#218313=CARTESIAN_POINT('Ctrl Pts',(21.445467890751,-7.5702668726117,12.));
#218314=CARTESIAN_POINT('Ctrl Pts',(21.4555450053147,-7.57239723223521,
12.));
#218315=CARTESIAN_POINT('Ctrl Pts',(21.4658351740135,-7.57453549743435,
12.));
#218316=CARTESIAN_POINT('Ctrl Pts',(21.4763353936766,-7.57667978403003,
12.));
#218317=CARTESIAN_POINT('Ctrl Pts',(21.4870427508193,-7.57882826679131,
12.));
#218318=CARTESIAN_POINT('Ctrl Pts',(21.4979544192739,-7.5809791779073,12.));
#218319=CARTESIAN_POINT('Ctrl Pts',(21.5090676573866,-7.58313080519159,
12.));
#218320=CARTESIAN_POINT('Ctrl Pts',(21.5203798035294,-7.58528148919114,
12.));
#218321=CARTESIAN_POINT('Ctrl Pts',(21.5318882716735,-7.58742962034834,
12.));
#218322=CARTESIAN_POINT('Ctrl Pts',(21.5435905470113,-7.58957363620026,
12.));
#218323=CARTESIAN_POINT('Ctrl Pts',(21.5554841813465,-7.59171201844793,
12.));
#218324=CARTESIAN_POINT('Ctrl Pts',(21.5675667904728,-7.5938432912493,12.));
#218325=CARTESIAN_POINT('Ctrl Pts',(21.5798360518978,-7.59596601973589,
12.));
#218326=CARTESIAN_POINT('Ctrl Pts',(21.5922897024466,-7.59807880846193,
12.));
#218327=CARTESIAN_POINT('Ctrl Pts',(21.6049255358842,-7.60018029988238,
12.));
#218328=CARTESIAN_POINT('Ctrl Pts',(21.6177414005991,-7.60226917285432,
12.));
#218329=CARTESIAN_POINT('Ctrl Pts',(21.6307351973823,-7.604344141183,12.));
#218330=CARTESIAN_POINT('Ctrl Pts',(21.6439048771743,-7.60640395216359,
12.));
#218331=CARTESIAN_POINT('Ctrl Pts',(21.6572484388079,-7.60844738512872,
12.));
#218332=CARTESIAN_POINT('Ctrl Pts',(21.6707639267573,-7.6104732500095,12.));
#218333=CARTESIAN_POINT('Ctrl Pts',(21.6844494295813,-7.61248038630265,
12.));
#218334=CARTESIAN_POINT('Ctrl Pts',(21.6983030783321,-7.61446766202787,
12.));
#218335=CARTESIAN_POINT('Ctrl Pts',(21.7123230449835,-7.61643397270425,
12.));
#218336=CARTESIAN_POINT('Ctrl Pts',(21.7265075407977,-7.61837824030542,
12.));
#218337=CARTESIAN_POINT('Ctrl Pts',(21.7408548148657,-7.62029941230855,
12.));
#218338=CARTESIAN_POINT('Ctrl Pts',(21.7553631528329,-7.62219646084226,
12.));
#218339=CARTESIAN_POINT('Ctrl Pts',(21.7700308755583,-7.62406838181164,
12.));
#218340=CARTESIAN_POINT('Ctrl Pts',(21.7848563378022,-7.62591419404521,
12.));
#218341=CARTESIAN_POINT('Ctrl Pts',(21.7998379268583,-7.62773293842409,
12.));
#218342=CARTESIAN_POINT('Ctrl Pts',(21.8149740615093,-7.62952367718151,
12.));
#218343=CARTESIAN_POINT('Ctrl Pts',(21.8302631910197,-7.6312854932304,12.));
#218344=CARTESIAN_POINT('Ctrl Pts',(21.8457037941084,-7.63301748948936,
12.));
#218345=CARTESIAN_POINT('Ctrl Pts',(21.8612943779086,-7.63471878821204,
12.));
#218346=CARTESIAN_POINT('Ctrl Pts',(21.8770334769492,-7.63638853033368,
12.));
#218347=CARTESIAN_POINT('Ctrl Pts',(21.8929196523511,-7.63802587492008,
12.));
#218348=CARTESIAN_POINT('Ctrl Pts',(21.9089514909873,-7.63962999860917,
12.));
#218349=CARTESIAN_POINT('Ctrl Pts',(21.9251276046546,-7.6412000950654,12.));
#218350=CARTESIAN_POINT('Ctrl Pts',(21.9414466292074,-7.64273537442707,
12.));
#218351=CARTESIAN_POINT('Ctrl Pts',(21.9579072237653,-7.64423506279154,
12.));
#218352=CARTESIAN_POINT('Ctrl Pts',(21.97450807008,-7.64569840177359,12.));
#218353=CARTESIAN_POINT('Ctrl Pts',(21.9912478718542,-7.64712464805258,
12.));
#218354=CARTESIAN_POINT('Ctrl Pts',(22.0081253540773,-7.64851307293346,
12.));
#218355=CARTESIAN_POINT('Ctrl Pts',(22.0251392623209,-7.64986296190157,
12.));
#218356=CARTESIAN_POINT('Ctrl Pts',(22.0422883621176,-7.65117361421347,
12.));
#218357=CARTESIAN_POINT('Ctrl Pts',(22.0595714384432,-7.65244434253104,
12.));
#218358=CARTESIAN_POINT('Ctrl Pts',(22.0769872951596,-7.65367447254945,
12.));
#218359=CARTESIAN_POINT('Ctrl Pts',(22.094534754469,-7.65486334263651,12.));
#218360=CARTESIAN_POINT('Ctrl Pts',(22.1122126563327,-7.65601030346819,
12.));
#218361=CARTESIAN_POINT('Ctrl Pts',(22.1300198579671,-7.65711471769407,
12.));
#218362=CARTESIAN_POINT('Ctrl Pts',(22.1479552334206,-7.65817595963351,
12.));
#218363=CARTESIAN_POINT('Ctrl Pts',(22.1660176731174,-7.65919341496926,
12.));
#218364=CARTESIAN_POINT('Ctrl Pts',(22.1842060834092,-7.66016648045008,
12.));
#218365=CARTESIAN_POINT('Ctrl Pts',(22.2025193860972,-7.66109456359292,
12.));
#218366=CARTESIAN_POINT('Ctrl Pts',(22.2209565180098,-7.66197708240436,
12.));
#218367=CARTESIAN_POINT('Ctrl Pts',(22.239516430656,-7.66281346512546,12.));
#218368=CARTESIAN_POINT('Ctrl Pts',(22.2581980898487,-7.66360314997662,
12.));
#218369=CARTESIAN_POINT('Ctrl Pts',(22.2770004753332,-7.66434558490973,
12.));
#218370=CARTESIAN_POINT('Ctrl Pts',(22.2959225803925,-7.66504022736263,
12.));
#218371=CARTESIAN_POINT('Ctrl Pts',(22.3149634114823,-7.66568654402442,
12.));
#218372=CARTESIAN_POINT('Ctrl Pts',(22.3341219879454,-7.66628401061906,
12.));
#218373=CARTESIAN_POINT('Ctrl Pts',(22.3533973417013,-7.66683211169134,
12.));
#218374=CARTESIAN_POINT('Ctrl Pts',(22.3727885169361,-7.66733034039887,
12.));
#218375=CARTESIAN_POINT('Ctrl Pts',(22.3922945697782,-7.6677781983082,12.));
#218376=CARTESIAN_POINT('Ctrl Pts',(22.411914567977,-7.66817519519682,12.));
#218377=CARTESIAN_POINT('Ctrl Pts',(22.4316475906616,-7.66852084886746,
12.));
#218378=CARTESIAN_POINT('Ctrl Pts',(22.4514927280862,-7.6688146849666,12.));
#218379=CARTESIAN_POINT('Ctrl Pts',(22.47144908137,-7.66905623680836,12.));
#218380=CARTESIAN_POINT('Ctrl Pts',(22.4915157622308,-7.66924504520302,
12.));
#218381=CARTESIAN_POINT('Ctrl Pts',(22.5116918927023,-7.66938065829083,
12.));
#218382=CARTESIAN_POINT('Ctrl Pts',(22.5319766049191,-7.66946263138116,
12.));
#218383=CARTESIAN_POINT('Ctrl Pts',(22.5523690409109,-7.66949052679672,
12.));
#218384=CARTESIAN_POINT('Ctrl Pts',(22.5728683523828,-7.66946391372299,
12.));
#218385=CARTESIAN_POINT('Ctrl Pts',(22.5934737004955,-7.66938236806241,
12.));
#218386=CARTESIAN_POINT('Ctrl Pts',(22.6141842556248,-7.66924547229435,
12.));
#218387=CARTESIAN_POINT('Ctrl Pts',(22.6349991971547,-7.66905281533745,
12.));
#218388=CARTESIAN_POINT('Ctrl Pts',(22.6559177133133,-7.66880399241354,
12.));
#218389=CARTESIAN_POINT('Ctrl Pts',(22.6769390009889,-7.66849860491763,
12.));
#218390=CARTESIAN_POINT('Ctrl Pts',(22.6980622655446,-7.66813626029277,
12.));
#218391=CARTESIAN_POINT('Ctrl Pts',(22.7192867206242,-7.6677165719101,12.));
#218392=CARTESIAN_POINT('Ctrl Pts',(22.7406115879508,-7.66723915895413,
12.));
#218393=CARTESIAN_POINT('Ctrl Pts',(22.7620360971839,-7.66670364630273,
12.));
#218394=CARTESIAN_POINT('Ctrl Pts',(22.7835594857697,-7.66610966441259,
12.));
#218395=CARTESIAN_POINT('Ctrl Pts',(22.8051809987833,-7.66545684920988,
12.));
#218396=CARTESIAN_POINT('Ctrl Pts',(22.8268998887678,-7.66474484198553,
12.));
#218397=CARTESIAN_POINT('Ctrl Pts',(22.8487154155569,-7.66397328929805,
12.));
#218398=CARTESIAN_POINT('Ctrl Pts',(22.870626846128,-7.66314184287334,12.));
#218399=CARTESIAN_POINT('Ctrl Pts',(22.8926334544879,-7.66225015950148,
12.));
#218400=CARTESIAN_POINT('Ctrl Pts',(22.9147345215418,-7.661297900941,12.));
#218401=CARTESIAN_POINT('Ctrl Pts',(22.9369293349592,-7.66028473382777,
12.));
#218402=CARTESIAN_POINT('Ctrl Pts',(22.9592171890332,-7.65921032958912,
12.));
#218403=CARTESIAN_POINT('Ctrl Pts',(22.9815973845301,-7.65807436436453,
12.));
#218404=CARTESIAN_POINT('Ctrl Pts',(23.004069228582,-7.6568765189133,12.));
#218405=CARTESIAN_POINT('Ctrl Pts',(23.0266320345792,-7.65561647852555,
12.));
#218406=CARTESIAN_POINT('Ctrl Pts',(23.049285122053,-7.65429393293955,12.));
#218407=CARTESIAN_POINT('Ctrl Pts',(23.072027816555,-7.65290857626357,12.));
#218408=CARTESIAN_POINT('Ctrl Pts',(23.0948594495246,-7.65146010690465,
12.));
#218409=CARTESIAN_POINT('Ctrl Pts',(23.1177793581674,-7.64994822749845,
12.));
#218410=CARTESIAN_POINT('Ctrl Pts',(23.1407868853815,-7.64837264482929,
12.));
#218411=CARTESIAN_POINT('Ctrl Pts',(23.1638813796691,-7.64673306975797,
12.));
#218412=CARTESIAN_POINT('Ctrl Pts',(23.1870621950452,-7.64502921715483,
12.));
#218413=CARTESIAN_POINT('Ctrl Pts',(23.2103286909399,-7.64326080583684,
12.));
#218414=CARTESIAN_POINT('Ctrl Pts',(23.2336802320912,-7.64142755851508,
12.));
#218415=CARTESIAN_POINT('Ctrl Pts',(23.2571161884487,-7.63952920172837,
12.));
#218416=CARTESIAN_POINT('Ctrl Pts',(23.2806359350853,-7.63756546576375,
12.));
#218417=CARTESIAN_POINT('Ctrl Pts',(23.3042388521021,-7.63553608458784,
12.));
#218418=CARTESIAN_POINT('Ctrl Pts',(23.3279243245241,-7.63344079578163,
12.));
#218419=CARTESIAN_POINT('Ctrl Pts',(23.3516917421973,-7.63127934048139,
12.));
#218420=CARTESIAN_POINT('Ctrl Pts',(23.3755404996638,-7.62905146332598,
12.));
#218421=CARTESIAN_POINT('Ctrl Pts',(23.3994699961122,-7.62675691240335,
12.));
#218422=CARTESIAN_POINT('Ctrl Pts',(23.4234796353544,-7.62439543920055,
12.));
#218423=CARTESIAN_POINT('Ctrl Pts',(23.4475688257854,-7.62196679855957,
12.));
#218424=CARTESIAN_POINT('Ctrl Pts',(23.4717369803438,-7.61947074863978,
12.));
#218425=CARTESIAN_POINT('Ctrl Pts',(23.4959835164608,-7.61690705088319,
12.));
#218426=CARTESIAN_POINT('Ctrl Pts',(23.5203078560128,-7.61427546999299,
12.));
#218427=CARTESIAN_POINT('Ctrl Pts',(23.5447094252028,-7.61157577385372,
12.));
#218428=CARTESIAN_POINT('Ctrl Pts',(23.5691876544243,-7.608807733446,12.));
#218429=CARTESIAN_POINT('Ctrl Pts',(23.5937419781244,-7.60597112277094,
12.));
#218430=CARTESIAN_POINT('Ctrl Pts',(23.6183718346576,-7.60306571877806,
12.));
#218431=CARTESIAN_POINT('Ctrl Pts',(23.6430766661419,-7.6000913013013,12.));
#218432=CARTESIAN_POINT('Ctrl Pts',(23.6678559182876,-7.59704765299572,
12.));
#218433=CARTESIAN_POINT('Ctrl Pts',(23.6927090405067,-7.59393455934042,
12.));
#218434=CARTESIAN_POINT('Ctrl Pts',(23.7176354860457,-7.59075180865327,
12.));
#218435=CARTESIAN_POINT('Ctrl Pts',(23.7426347121006,-7.58749919210832,
12.));
#218436=CARTESIAN_POINT('Ctrl Pts',(23.7677061799376,-7.58417650376272,
12.));
#218437=CARTESIAN_POINT('Ctrl Pts',(23.7928493549908,-7.58078354058212,
12.));
#218438=CARTESIAN_POINT('Ctrl Pts',(23.8180637069977,-7.57732010249066,
12.));
#218439=CARTESIAN_POINT('Ctrl Pts',(23.8433487096134,-7.57378599219817,
12.));
#218440=CARTESIAN_POINT('Ctrl Pts',(23.8687038399597,-7.57018101500711,
12.));
#218441=CARTESIAN_POINT('Ctrl Pts',(23.8941285782003,-7.56650497863792,
12.));
#218442=CARTESIAN_POINT('Ctrl Pts',(23.9196224070759,-7.56275769304773,
12.));
#218443=CARTESIAN_POINT('Ctrl Pts',(23.9451848115,-7.55893897027683,12.));
#218444=CARTESIAN_POINT('Ctrl Pts',(23.9708152779884,-7.55504862424812,
12.));
#218445=CARTESIAN_POINT('Ctrl Pts',(23.9965132953185,-7.55108647097441,
12.));
#218446=CARTESIAN_POINT('Ctrl Pts',(24.022278355453,-7.5470523288591,12.));
#218447=CARTESIAN_POINT('Ctrl Pts',(24.0481099543353,-7.54294601896145,
12.));
#218448=CARTESIAN_POINT('Ctrl Pts',(24.0740075927985,-7.53876736531014,
12.));
#218449=CARTESIAN_POINT('Ctrl Pts',(24.0999707772642,-7.53451619514649,
12.));
#218450=CARTESIAN_POINT('Ctrl Pts',(24.1259990209207,-7.53019233935502,
12.));
#218451=CARTESIAN_POINT('Ctrl Pts',(24.1520918425364,-7.52579563201424,
12.));
#218452=CARTESIAN_POINT('Ctrl Pts',(24.1782487641594,-7.52132590953802,
12.));
#218453=CARTESIAN_POINT('Ctrl Pts',(24.2044693092349,-7.51678300997949,
12.));
#218454=CARTESIAN_POINT('Ctrl Pts',(24.2307530003887,-7.51216677222181,
12.));
#218455=CARTESIAN_POINT('Ctrl Pts',(24.2570993577034,-7.50747703535134,
12.));
#218456=CARTESIAN_POINT('Ctrl Pts',(24.2835078958973,-7.50271363765152,
12.));
#218457=CARTESIAN_POINT('Ctrl Pts',(24.3099781253355,-7.49787641695439,
12.));
#218458=CARTESIAN_POINT('Ctrl Pts',(24.3365095573685,-7.49296521252421,
12.));
#218459=CARTESIAN_POINT('Ctrl Pts',(24.3631017084524,-7.48797986651909,
12.));
#218460=CARTESIAN_POINT('Ctrl Pts',(24.3897541049254,-7.48292022569301,
12.));
#218461=CARTESIAN_POINT('Ctrl Pts',(24.4164662871163,-7.47778614286565,
12.));
#218462=CARTESIAN_POINT('Ctrl Pts',(24.443237814649,-7.47257747883246,12.));
#218463=CARTESIAN_POINT('Ctrl Pts',(24.4700682684524,-7.46729410308787,
12.));
#218464=CARTESIAN_POINT('Ctrl Pts',(24.4969572391483,-7.46193588961464,
12.));
#218465=CARTESIAN_POINT('Ctrl Pts',(24.5239043173072,-7.45650271335862,
12.));
#218466=CARTESIAN_POINT('Ctrl Pts',(24.5509090831559,-7.4509944465116,12.));
#218467=CARTESIAN_POINT('Ctrl Pts',(24.577971096086,-7.44541095473135,12.));
#218468=CARTESIAN_POINT('Ctrl Pts',(24.6050898852368,-7.43975209375504,
12.));
#218469=CARTESIAN_POINT('Ctrl Pts',(24.6322649369517,-7.43401770489524,
12.));
#218470=CARTESIAN_POINT('Ctrl Pts',(24.6594957128756,-7.42820762159126,
12.));
#218471=CARTESIAN_POINT('Ctrl Pts',(24.6867816727192,-7.42232167766266,
12.));
#218472=CARTESIAN_POINT('Ctrl Pts',(24.7141222950051,-7.41635971481674,
12.));
#218473=CARTESIAN_POINT('Ctrl Pts',(24.7415170994784,-7.41032159082382,
12.));
#218474=CARTESIAN_POINT('Ctrl Pts',(24.7689656668983,-7.40420718661603,
12.));
#218475=CARTESIAN_POINT('Ctrl Pts',(24.7964676646431,-7.39801641583013,
12.));
#218476=CARTESIAN_POINT('Ctrl Pts',(24.8240228520893,-7.39174922585809,
12.));
#218477=CARTESIAN_POINT('Ctrl Pts',(24.8516310625176,-7.38540558903621,
12.));
#218478=CARTESIAN_POINT('Ctrl Pts',(24.8792921911115,-7.3789854964027,12.));
#218479=CARTESIAN_POINT('Ctrl Pts',(24.901463382605,-7.37378825961676,12.));
#218480=CARTESIAN_POINT('Ctrl Pts',(24.9181155530543,-7.36985593120091,
12.));
#218481=CARTESIAN_POINT('Ctrl Pts',(24.9292275670674,-7.36721909028843,
12.));
#218482=CARTESIAN_POINT('Ctrl Pts',(24.9347862158358,-7.36589684767345,
12.));
#218483=CARTESIAN_POINT('Ctrl Pts',(20.353053841303,-9.71462809124917,0.));
#218484=CARTESIAN_POINT('Ctrl Pts',(20.353053841303,-9.71462809124917,12.));
#218485=CARTESIAN_POINT('Ctrl Pts',(20.353060251684,-9.71462954053074,0.));
#218486=CARTESIAN_POINT('Ctrl Pts',(20.353060251684,-9.71462954053074,12.));
#218487=CARTESIAN_POINT('Ctrl Pts',(20.3531126095522,-9.71465227853122,
0.));
#218488=CARTESIAN_POINT('Ctrl Pts',(20.3531126095522,-9.71465227853122,
12.));
#218489=CARTESIAN_POINT('Ctrl Pts',(20.3533097561886,-9.71474590350792,
0.));
#218490=CARTESIAN_POINT('Ctrl Pts',(20.3533097561886,-9.71474590350792,
12.));
#218491=CARTESIAN_POINT('Ctrl Pts',(20.3538098605706,-9.71498978052101,
0.));
#218492=CARTESIAN_POINT('Ctrl Pts',(20.3538098605706,-9.71498978052101,
12.));
#218493=CARTESIAN_POINT('Ctrl Pts',(20.3548282742361,-9.71549257088175,
0.));
#218494=CARTESIAN_POINT('Ctrl Pts',(20.3548282742361,-9.71549257088175,
12.));
#218495=CARTESIAN_POINT('Ctrl Pts',(20.3562337557875,-9.71619192554147,
0.));
#218496=CARTESIAN_POINT('Ctrl Pts',(20.3562337557875,-9.71619192554147,
12.));
#218497=CARTESIAN_POINT('Ctrl Pts',(20.3580133103357,-9.71708493723062,
0.));
#218498=CARTESIAN_POINT('Ctrl Pts',(20.3580133103357,-9.71708493723062,
12.));
#218499=CARTESIAN_POINT('Ctrl Pts',(20.3601498764344,-9.71816778327999,
0.));
#218500=CARTESIAN_POINT('Ctrl Pts',(20.3601498764344,-9.71816778327999,
12.));
#218501=CARTESIAN_POINT('Ctrl Pts',(20.362625691398,-9.71943648548115,0.));
#218502=CARTESIAN_POINT('Ctrl Pts',(20.362625691398,-9.71943648548115,12.));
#218503=CARTESIAN_POINT('Ctrl Pts',(20.3654261611055,-9.72088778381102,
0.));
#218504=CARTESIAN_POINT('Ctrl Pts',(20.3654261611055,-9.72088778381102,
12.));
#218505=CARTESIAN_POINT('Ctrl Pts',(20.3685406190576,-9.72251930722504,
0.));
#218506=CARTESIAN_POINT('Ctrl Pts',(20.3685406190576,-9.72251930722504,
12.));
#218507=CARTESIAN_POINT('Ctrl Pts',(20.371960235676,-9.72432910043193,0.));
#218508=CARTESIAN_POINT('Ctrl Pts',(20.371960235676,-9.72432910043193,12.));
#218509=CARTESIAN_POINT('Ctrl Pts',(20.3756766651952,-9.72631531732871,
0.));
#218510=CARTESIAN_POINT('Ctrl Pts',(20.3756766651952,-9.72631531732871,
12.));
#218511=CARTESIAN_POINT('Ctrl Pts',(20.3796805893304,-9.72847589116533,
0.));
#218512=CARTESIAN_POINT('Ctrl Pts',(20.3796805893304,-9.72847589116533,
12.));
#218513=CARTESIAN_POINT('Ctrl Pts',(20.3839624556742,-9.73080870123726,
0.));
#218514=CARTESIAN_POINT('Ctrl Pts',(20.3839624556742,-9.73080870123726,
12.));
#218515=CARTESIAN_POINT('Ctrl Pts',(20.3885129129912,-9.73331167102812,
0.));
#218516=CARTESIAN_POINT('Ctrl Pts',(20.3885129129912,-9.73331167102812,
12.));
#218517=CARTESIAN_POINT('Ctrl Pts',(20.3933234845646,-9.7359829201425,0.));
#218518=CARTESIAN_POINT('Ctrl Pts',(20.3933234845646,-9.7359829201425,12.));
#218519=CARTESIAN_POINT('Ctrl Pts',(20.3983866213331,-9.73882077613206,
0.));
#218520=CARTESIAN_POINT('Ctrl Pts',(20.3983866213331,-9.73882077613206,
12.));
#218521=CARTESIAN_POINT('Ctrl Pts',(20.4036953576549,-9.74182369656273,
0.));
#218522=CARTESIAN_POINT('Ctrl Pts',(20.4036953576549,-9.74182369656273,
12.));
#218523=CARTESIAN_POINT('Ctrl Pts',(20.4092430879861,-9.74499021838537,
0.));
#218524=CARTESIAN_POINT('Ctrl Pts',(20.4092430879861,-9.74499021838537,
12.));
#218525=CARTESIAN_POINT('Ctrl Pts',(20.4150232777393,-9.74831889242175,
0.));
#218526=CARTESIAN_POINT('Ctrl Pts',(20.4150232777393,-9.74831889242175,
12.));
#218527=CARTESIAN_POINT('Ctrl Pts',(20.4210295275818,-9.75180829786433,
0.));
#218528=CARTESIAN_POINT('Ctrl Pts',(20.4210295275818,-9.75180829786433,
12.));
#218529=CARTESIAN_POINT('Ctrl Pts',(20.4272556476629,-9.75545705902416,
0.));
#218530=CARTESIAN_POINT('Ctrl Pts',(20.4272556476629,-9.75545705902416,
12.));
#218531=CARTESIAN_POINT('Ctrl Pts',(20.4336957355474,-9.7592638628993,0.));
#218532=CARTESIAN_POINT('Ctrl Pts',(20.4336957355474,-9.7592638628993,12.));
#218533=CARTESIAN_POINT('Ctrl Pts',(20.4403442329401,-9.76322747195502,
0.));
#218534=CARTESIAN_POINT('Ctrl Pts',(20.4403442329401,-9.76322747195502,
12.));
#218535=CARTESIAN_POINT('Ctrl Pts',(20.447195862298,-9.76734670980897,0.));
#218536=CARTESIAN_POINT('Ctrl Pts',(20.447195862298,-9.76734670980897,12.));
#218537=CARTESIAN_POINT('Ctrl Pts',(20.4542455817527,-9.7716204510407,0.));
#218538=CARTESIAN_POINT('Ctrl Pts',(20.4542455817527,-9.7716204510407,12.));
#218539=CARTESIAN_POINT('Ctrl Pts',(20.4614885274973,-9.77604760815523,
0.));
#218540=CARTESIAN_POINT('Ctrl Pts',(20.4614885274973,-9.77604760815523,
12.));
#218541=CARTESIAN_POINT('Ctrl Pts',(20.4689199790668,-9.78062712373313,
0.));
#218542=CARTESIAN_POINT('Ctrl Pts',(20.4689199790668,-9.78062712373313,
12.));
#218543=CARTESIAN_POINT('Ctrl Pts',(20.4765353711585,-9.78535797314162,
0.));
#218544=CARTESIAN_POINT('Ctrl Pts',(20.4765353711585,-9.78535797314162,
12.));
#218545=CARTESIAN_POINT('Ctrl Pts',(20.4843302955329,-9.7902391649866,0.));
#218546=CARTESIAN_POINT('Ctrl Pts',(20.4843302955329,-9.7902391649866,12.));
#218547=CARTESIAN_POINT('Ctrl Pts',(20.4923005087945,-9.79526974288344,
0.));
#218548=CARTESIAN_POINT('Ctrl Pts',(20.4923005087945,-9.79526974288344,
12.));
#218549=CARTESIAN_POINT('Ctrl Pts',(20.500441931211,-9.80044878520968,0.));
#218550=CARTESIAN_POINT('Ctrl Pts',(20.500441931211,-9.80044878520968,12.));
#218551=CARTESIAN_POINT('Ctrl Pts',(20.5087506310507,-9.80577540161103,
0.));
#218552=CARTESIAN_POINT('Ctrl Pts',(20.5087506310507,-9.80577540161103,
12.));
#218553=CARTESIAN_POINT('Ctrl Pts',(20.5172228122839,-9.81124873025278,
0.));
#218554=CARTESIAN_POINT('Ctrl Pts',(20.5172228122839,-9.81124873025278,
12.));
#218555=CARTESIAN_POINT('Ctrl Pts',(20.5258548000625,-9.81686793455918,
0.));
#218556=CARTESIAN_POINT('Ctrl Pts',(20.5258548000625,-9.81686793455918,
12.));
#218557=CARTESIAN_POINT('Ctrl Pts',(20.534643029951,-9.82263220080328,0.));
#218558=CARTESIAN_POINT('Ctrl Pts',(20.534643029951,-9.82263220080328,12.));
#218559=CARTESIAN_POINT('Ctrl Pts',(20.5435840460717,-9.82854073773858,
0.));
#218560=CARTESIAN_POINT('Ctrl Pts',(20.5435840460717,-9.82854073773858,
12.));
#218561=CARTESIAN_POINT('Ctrl Pts',(20.5526744976461,-9.83459277585321,
0.));
#218562=CARTESIAN_POINT('Ctrl Pts',(20.5526744976461,-9.83459277585321,
12.));
#218563=CARTESIAN_POINT('Ctrl Pts',(20.5619111362406,-9.84078756677589,
0.));
#218564=CARTESIAN_POINT('Ctrl Pts',(20.5619111362406,-9.84078756677589,
12.));
#218565=CARTESIAN_POINT('Ctrl Pts',(20.5712908125145,-9.84712438256308,
0.));
#218566=CARTESIAN_POINT('Ctrl Pts',(20.5712908125145,-9.84712438256308,
12.));
#218567=CARTESIAN_POINT('Ctrl Pts',(20.580810471002,-9.85360251457004,0.));
#218568=CARTESIAN_POINT('Ctrl Pts',(20.580810471002,-9.85360251457004,12.));
#218569=CARTESIAN_POINT('Ctrl Pts',(20.5904671449754,-9.8602212723275,0.));
#218570=CARTESIAN_POINT('Ctrl Pts',(20.5904671449754,-9.8602212723275,12.));
#218571=CARTESIAN_POINT('Ctrl Pts',(20.6002579513696,-9.86697998242612,
0.));
#218572=CARTESIAN_POINT('Ctrl Pts',(20.6002579513696,-9.86697998242612,
12.));
#218573=CARTESIAN_POINT('Ctrl Pts',(20.6101800854491,-9.87387798732944,
0.));
#218574=CARTESIAN_POINT('Ctrl Pts',(20.6101800854491,-9.87387798732944,
12.));
#218575=CARTESIAN_POINT('Ctrl Pts',(20.6202308177472,-9.88091464472669,
0.));
#218576=CARTESIAN_POINT('Ctrl Pts',(20.6202308177472,-9.88091464472669,
12.));
#218577=CARTESIAN_POINT('Ctrl Pts',(20.6304074914086,-9.88808932697305,
0.));
#218578=CARTESIAN_POINT('Ctrl Pts',(20.6304074914086,-9.88808932697305,
12.));
#218579=CARTESIAN_POINT('Ctrl Pts',(20.6407075193977,-9.89540142049124,
0.));
#218580=CARTESIAN_POINT('Ctrl Pts',(20.6407075193977,-9.89540142049124,
12.));
#218581=CARTESIAN_POINT('Ctrl Pts',(20.6511283817415,-9.90285032516696,
0.));
#218582=CARTESIAN_POINT('Ctrl Pts',(20.6511283817415,-9.90285032516696,
12.));
#218583=CARTESIAN_POINT('Ctrl Pts',(20.6616676228315,-9.91043545377005,
0.));
#218584=CARTESIAN_POINT('Ctrl Pts',(20.6616676228315,-9.91043545377005,
12.));
#218585=CARTESIAN_POINT('Ctrl Pts',(20.6723228488261,-9.91815623141285,
0.));
#218586=CARTESIAN_POINT('Ctrl Pts',(20.6723228488261,-9.91815623141285,
12.));
#218587=CARTESIAN_POINT('Ctrl Pts',(20.6830917250255,-9.92601209498751,
0.));
#218588=CARTESIAN_POINT('Ctrl Pts',(20.6830917250255,-9.92601209498751,
12.));
#218589=CARTESIAN_POINT('Ctrl Pts',(20.6939719732485,-9.93400249259737,
0.));
#218590=CARTESIAN_POINT('Ctrl Pts',(20.6939719732485,-9.93400249259737,
12.));
#218591=CARTESIAN_POINT('Ctrl Pts',(20.7049613692237,-9.94212688298251,
0.));
#218592=CARTESIAN_POINT('Ctrl Pts',(20.7049613692237,-9.94212688298251,
12.));
#218593=CARTESIAN_POINT('Ctrl Pts',(20.716057740758,-9.95038473514962,0.));
#218594=CARTESIAN_POINT('Ctrl Pts',(20.716057740758,-9.95038473514962,12.));
#218595=CARTESIAN_POINT('Ctrl Pts',(20.7272589658752,-9.95877552798403,
0.));
#218596=CARTESIAN_POINT('Ctrl Pts',(20.7272589658752,-9.95877552798403,
12.));
#218597=CARTESIAN_POINT('Ctrl Pts',(20.7385629709795,-9.96729874986199,
0.));
#218598=CARTESIAN_POINT('Ctrl Pts',(20.7385629709795,-9.96729874986199,
12.));
#218599=CARTESIAN_POINT('Ctrl Pts',(20.7499677289625,-9.97595389823461,
0.));
#218600=CARTESIAN_POINT('Ctrl Pts',(20.7499677289625,-9.97595389823461,
12.));
#218601=CARTESIAN_POINT('Ctrl Pts',(20.7614712574989,-9.98474047926846,
0.));
#218602=CARTESIAN_POINT('Ctrl Pts',(20.7614712574989,-9.98474047926846,
12.));
#218603=CARTESIAN_POINT('Ctrl Pts',(20.7730716175417,-9.99365800754638,
0.));
#218604=CARTESIAN_POINT('Ctrl Pts',(20.7730716175417,-9.99365800754638,
12.));
#218605=CARTESIAN_POINT('Ctrl Pts',(20.7847669117568,-10.0027060057389,
0.));
#218606=CARTESIAN_POINT('Ctrl Pts',(20.7847669117568,-10.0027060057389,
12.));
#218607=CARTESIAN_POINT('Ctrl Pts',(20.7965552829907,-10.0118840042786,
0.));
#218608=CARTESIAN_POINT('Ctrl Pts',(20.7965552829907,-10.0118840042786,
12.));
#218609=CARTESIAN_POINT('Ctrl Pts',(20.8084349126885,-10.0211915410095,
0.));
#218610=CARTESIAN_POINT('Ctrl Pts',(20.8084349126885,-10.0211915410095,
12.));
#218611=CARTESIAN_POINT('Ctrl Pts',(20.8204040196599,-10.0306281609435,
0.));
#218612=CARTESIAN_POINT('Ctrl Pts',(20.8204040196599,-10.0306281609435,
12.));
#218613=CARTESIAN_POINT('Ctrl Pts',(20.8324608588906,-10.0401934160234,
0.));
#218614=CARTESIAN_POINT('Ctrl Pts',(20.8324608588906,-10.0401934160234,
12.));
#218615=CARTESIAN_POINT('Ctrl Pts',(20.8446037203402,-10.0498868648733,
0.));
#218616=CARTESIAN_POINT('Ctrl Pts',(20.8446037203402,-10.0498868648733,
12.));
#218617=CARTESIAN_POINT('Ctrl Pts',(20.856830927732,-10.0597080725375,0.));
#218618=CARTESIAN_POINT('Ctrl Pts',(20.856830927732,-10.0597080725375,12.));
#218619=CARTESIAN_POINT('Ctrl Pts',(20.8691408373705,-10.0696566102219,
0.));
#218620=CARTESIAN_POINT('Ctrl Pts',(20.8691408373705,-10.0696566102219,
12.));
#218621=CARTESIAN_POINT('Ctrl Pts',(20.8815318371844,-10.0797320551154,
0.));
#218622=CARTESIAN_POINT('Ctrl Pts',(20.8815318371844,-10.0797320551154,
12.));
#218623=CARTESIAN_POINT('Ctrl Pts',(20.8940023457371,-10.0899339901916,
0.));
#218624=CARTESIAN_POINT('Ctrl Pts',(20.8940023457371,-10.0899339901916,
12.));
#218625=CARTESIAN_POINT('Ctrl Pts',(20.9065508112556,-10.1002620040076,
0.));
#218626=CARTESIAN_POINT('Ctrl Pts',(20.9065508112556,-10.1002620040076,
12.));
#218627=CARTESIAN_POINT('Ctrl Pts',(20.9191757106266,-10.1107156904836,
0.));
#218628=CARTESIAN_POINT('Ctrl Pts',(20.9191757106266,-10.1107156904836,
12.));
#218629=CARTESIAN_POINT('Ctrl Pts',(20.931875548473,-10.1212946487057,0.));
#218630=CARTESIAN_POINT('Ctrl Pts',(20.931875548473,-10.1212946487057,12.));
#218631=CARTESIAN_POINT('Ctrl Pts',(20.944648856393,-10.1319984827909,0.));
#218632=CARTESIAN_POINT('Ctrl Pts',(20.944648856393,-10.1319984827909,12.));
#218633=CARTESIAN_POINT('Ctrl Pts',(20.9574941921591,-10.1428268017257,
0.));
#218634=CARTESIAN_POINT('Ctrl Pts',(20.9574941921591,-10.1428268017257,
12.));
#218635=CARTESIAN_POINT('Ctrl Pts',(20.970410138937,-10.1537792192065,0.));
#218636=CARTESIAN_POINT('Ctrl Pts',(20.970410138937,-10.1537792192065,12.));
#218637=CARTESIAN_POINT('Ctrl Pts',(20.9833953044736,-10.1648553534567,
0.));
#218638=CARTESIAN_POINT('Ctrl Pts',(20.9833953044736,-10.1648553534567,
12.));
#218639=CARTESIAN_POINT('Ctrl Pts',(20.9964483203685,-10.1760548270765,
0.));
#218640=CARTESIAN_POINT('Ctrl Pts',(20.9964483203685,-10.1760548270765,
12.));
#218641=CARTESIAN_POINT('Ctrl Pts',(21.0095678414486,-10.1873772669358,
0.));
#218642=CARTESIAN_POINT('Ctrl Pts',(21.0095678414486,-10.1873772669358,
12.));
#218643=CARTESIAN_POINT('Ctrl Pts',(21.0227525451107,-10.1988223040425,
0.));
#218644=CARTESIAN_POINT('Ctrl Pts',(21.0227525451107,-10.1988223040425,
12.));
#218645=CARTESIAN_POINT('Ctrl Pts',(21.0360011306814,-10.2103895734124,
0.));
#218646=CARTESIAN_POINT('Ctrl Pts',(21.0360011306814,-10.2103895734124,
12.));
#218647=CARTESIAN_POINT('Ctrl Pts',(21.0493123187483,-10.2220787139157,
0.));
#218648=CARTESIAN_POINT('Ctrl Pts',(21.0493123187483,-10.2220787139157,
12.));
#218649=CARTESIAN_POINT('Ctrl Pts',(21.0626848505665,-10.233889368157,0.));
#218650=CARTESIAN_POINT('Ctrl Pts',(21.0626848505665,-10.233889368157,12.));
#218651=CARTESIAN_POINT('Ctrl Pts',(21.0761174875448,-10.2458211823915,
0.));
#218652=CARTESIAN_POINT('Ctrl Pts',(21.0761174875448,-10.2458211823915,
12.));
#218653=CARTESIAN_POINT('Ctrl Pts',(21.0896090107066,-10.2578738064183,
0.));
#218654=CARTESIAN_POINT('Ctrl Pts',(21.0896090107066,-10.2578738064183,
12.));
#218655=CARTESIAN_POINT('Ctrl Pts',(21.1031582201625,-10.2700468934743,
0.));
#218656=CARTESIAN_POINT('Ctrl Pts',(21.1031582201625,-10.2700468934743,
12.));
#218657=CARTESIAN_POINT('Ctrl Pts',(21.1167639345623,-10.2823401001067,
0.));
#218658=CARTESIAN_POINT('Ctrl Pts',(21.1167639345623,-10.2823401001067,
12.));
#218659=CARTESIAN_POINT('Ctrl Pts',(21.130424990599,-10.2947530860714,0.));
#218660=CARTESIAN_POINT('Ctrl Pts',(21.130424990599,-10.2947530860714,12.));
#218661=CARTESIAN_POINT('Ctrl Pts',(21.1441402425831,-10.307285514268,0.));
#218662=CARTESIAN_POINT('Ctrl Pts',(21.1441402425831,-10.307285514268,12.));
#218663=CARTESIAN_POINT('Ctrl Pts',(21.1579085619959,-10.3199370506541,
0.));
#218664=CARTESIAN_POINT('Ctrl Pts',(21.1579085619959,-10.3199370506541,
12.));
#218665=CARTESIAN_POINT('Ctrl Pts',(21.1717288370512,-10.3327073641574,
0.));
#218666=CARTESIAN_POINT('Ctrl Pts',(21.1717288370512,-10.3327073641574,
12.));
#218667=CARTESIAN_POINT('Ctrl Pts',(21.1855999722427,-10.3455961265706,
0.));
#218668=CARTESIAN_POINT('Ctrl Pts',(21.1855999722427,-10.3455961265706,
12.));
#218669=CARTESIAN_POINT('Ctrl Pts',(21.1995208879205,-10.3586030124595,
0.));
#218670=CARTESIAN_POINT('Ctrl Pts',(21.1995208879205,-10.3586030124595,
12.));
#218671=CARTESIAN_POINT('Ctrl Pts',(21.2134905199359,-10.3717276991137,
0.));
#218672=CARTESIAN_POINT('Ctrl Pts',(21.2134905199359,-10.3717276991137,
12.));
#218673=CARTESIAN_POINT('Ctrl Pts',(21.2275078192708,-10.384969866479,0.));
#218674=CARTESIAN_POINT('Ctrl Pts',(21.2275078192708,-10.384969866479,12.));
#218675=CARTESIAN_POINT('Ctrl Pts',(21.2415717516713,-10.3983291970846,
0.));
#218676=CARTESIAN_POINT('Ctrl Pts',(21.2415717516713,-10.3983291970846,
12.));
#218677=CARTESIAN_POINT('Ctrl Pts',(21.2556812972741,-10.4118053759584,
0.));
#218678=CARTESIAN_POINT('Ctrl Pts',(21.2556812972741,-10.4118053759584,
12.));
#218679=CARTESIAN_POINT('Ctrl Pts',(21.2698354502391,-10.4253980905394,
0.));
#218680=CARTESIAN_POINT('Ctrl Pts',(21.2698354502391,-10.4253980905394,
12.));
#218681=CARTESIAN_POINT('Ctrl Pts',(21.2840332184471,-10.4391070306385,
0.));
#218682=CARTESIAN_POINT('Ctrl Pts',(21.2840332184471,-10.4391070306385,
12.));
#218683=CARTESIAN_POINT('Ctrl Pts',(21.2982736231924,-10.452931888387,0.));
#218684=CARTESIAN_POINT('Ctrl Pts',(21.2982736231924,-10.452931888387,12.));
#218685=CARTESIAN_POINT('Ctrl Pts',(21.312555698873,-10.4668723581768,0.));
#218686=CARTESIAN_POINT('Ctrl Pts',(21.312555698873,-10.4668723581768,12.));
#218687=CARTESIAN_POINT('Ctrl Pts',(21.3268784926823,-10.4809281365933,
0.));
#218688=CARTESIAN_POINT('Ctrl Pts',(21.3268784926823,-10.4809281365933,
12.));
#218689=CARTESIAN_POINT('Ctrl Pts',(21.3412410642912,-10.4950989223341,
0.));
#218690=CARTESIAN_POINT('Ctrl Pts',(21.3412410642912,-10.4950989223341,
12.));
#218691=CARTESIAN_POINT('Ctrl Pts',(21.3556424855822,-10.509384416169,0.));
#218692=CARTESIAN_POINT('Ctrl Pts',(21.3556424855822,-10.509384416169,12.));
#218693=CARTESIAN_POINT('Ctrl Pts',(21.3700818403942,-10.523784320906,0.));
#218694=CARTESIAN_POINT('Ctrl Pts',(21.3700818403942,-10.523784320906,12.));
#218695=CARTESIAN_POINT('Ctrl Pts',(21.3845582242604,-10.5382983413422,
0.));
#218696=CARTESIAN_POINT('Ctrl Pts',(21.3845582242604,-10.5382983413422,
12.));
#218697=CARTESIAN_POINT('Ctrl Pts',(21.3990707441495,-10.5529261842107,
0.));
#218698=CARTESIAN_POINT('Ctrl Pts',(21.3990707441495,-10.5529261842107,
12.));
#218699=CARTESIAN_POINT('Ctrl Pts',(21.4136185181974,-10.5676675581106,
0.));
#218700=CARTESIAN_POINT('Ctrl Pts',(21.4136185181974,-10.5676675581106,
12.));
#218701=CARTESIAN_POINT('Ctrl Pts',(21.4282006754624,-10.582522173457,0.));
#218702=CARTESIAN_POINT('Ctrl Pts',(21.4282006754624,-10.582522173457,12.));
#218703=CARTESIAN_POINT('Ctrl Pts',(21.4428163557137,-10.597489742462,0.));
#218704=CARTESIAN_POINT('Ctrl Pts',(21.4428163557137,-10.597489742462,12.));
#218705=CARTESIAN_POINT('Ctrl Pts',(21.4574647092093,-10.612569979096,0.));
#218706=CARTESIAN_POINT('Ctrl Pts',(21.4574647092093,-10.612569979096,12.));
#218707=CARTESIAN_POINT('Ctrl Pts',(21.4721448964766,-10.6277625990457,
0.));
#218708=CARTESIAN_POINT('Ctrl Pts',(21.4721448964766,-10.6277625990457,
12.));
#218709=CARTESIAN_POINT('Ctrl Pts',(21.4868560880893,-10.6430673196609,
0.));
#218710=CARTESIAN_POINT('Ctrl Pts',(21.4868560880893,-10.6430673196609,
12.));
#218711=CARTESIAN_POINT('Ctrl Pts',(21.5015974644454,-10.6584838598941,
0.));
#218712=CARTESIAN_POINT('Ctrl Pts',(21.5015974644454,-10.6584838598941,
12.));
#218713=CARTESIAN_POINT('Ctrl Pts',(21.5163682155805,-10.6740119402835,
0.));
#218714=CARTESIAN_POINT('Ctrl Pts',(21.5163682155805,-10.6740119402835,
12.));
#218715=CARTESIAN_POINT('Ctrl Pts',(21.531167540981,-10.689651282929,0.));
#218716=CARTESIAN_POINT('Ctrl Pts',(21.531167540981,-10.689651282929,12.));
#218717=CARTESIAN_POINT('Ctrl Pts',(21.5459946493955,-10.7054016114571,
0.));
#218718=CARTESIAN_POINT('Ctrl Pts',(21.5459946493955,-10.7054016114571,
12.));
#218719=CARTESIAN_POINT('Ctrl Pts',(21.5608487586467,-10.7212626509816,
0.));
#218720=CARTESIAN_POINT('Ctrl Pts',(21.5608487586467,-10.7212626509816,
12.));
#218721=CARTESIAN_POINT('Ctrl Pts',(21.5757290954372,-10.7372341280468,
0.));
#218722=CARTESIAN_POINT('Ctrl Pts',(21.5757290954372,-10.7372341280468,
12.));
#218723=CARTESIAN_POINT('Ctrl Pts',(21.5906348951745,-10.7533157705943,
0.));
#218724=CARTESIAN_POINT('Ctrl Pts',(21.5906348951745,-10.7533157705943,
12.));
#218725=CARTESIAN_POINT('Ctrl Pts',(21.6055654018179,-10.7695073079554,
0.));
#218726=CARTESIAN_POINT('Ctrl Pts',(21.6055654018179,-10.7695073079554,
12.));
#218727=CARTESIAN_POINT('Ctrl Pts',(21.6205198677176,-10.7858084708262,
0.));
#218728=CARTESIAN_POINT('Ctrl Pts',(21.6205198677176,-10.7858084708262,
12.));
#218729=CARTESIAN_POINT('Ctrl Pts',(21.6354975534557,-10.802218991237,0.));
#218730=CARTESIAN_POINT('Ctrl Pts',(21.6354975534557,-10.802218991237,12.));
#218731=CARTESIAN_POINT('Ctrl Pts',(21.6504977276864,-10.8187386025135,
0.));
#218732=CARTESIAN_POINT('Ctrl Pts',(21.6504977276864,-10.8187386025135,
12.));
#218733=CARTESIAN_POINT('Ctrl Pts',(21.6655196669727,-10.835367039227,0.));
#218734=CARTESIAN_POINT('Ctrl Pts',(21.6655196669727,-10.835367039227,12.));
#218735=CARTESIAN_POINT('Ctrl Pts',(21.6805626556461,-10.8521040371832,
0.));
#218736=CARTESIAN_POINT('Ctrl Pts',(21.6805626556461,-10.8521040371832,
12.));
#218737=CARTESIAN_POINT('Ctrl Pts',(21.6956259856667,-10.8689493334093,
0.));
#218738=CARTESIAN_POINT('Ctrl Pts',(21.6956259856667,-10.8689493334093,
12.));
#218739=CARTESIAN_POINT('Ctrl Pts',(21.7107089564822,-10.8859026661292,
0.));
#218740=CARTESIAN_POINT('Ctrl Pts',(21.7107089564822,-10.8859026661292,
12.));
#218741=CARTESIAN_POINT('Ctrl Pts',(21.7258108748874,-10.9029637747341,
0.));
#218742=CARTESIAN_POINT('Ctrl Pts',(21.7258108748874,-10.9029637747341,
12.));
#218743=CARTESIAN_POINT('Ctrl Pts',(21.74093105488,-10.9201323997386,0.));
#218744=CARTESIAN_POINT('Ctrl Pts',(21.74093105488,-10.9201323997386,12.));
#218745=CARTESIAN_POINT('Ctrl Pts',(21.7560688175252,-10.9374082827446,
0.));
#218746=CARTESIAN_POINT('Ctrl Pts',(21.7560688175252,-10.9374082827446,
12.));
#218747=CARTESIAN_POINT('Ctrl Pts',(21.7712234908468,-10.9547911664457,
0.));
#218748=CARTESIAN_POINT('Ctrl Pts',(21.7712234908468,-10.9547911664457,
12.));
#218749=CARTESIAN_POINT('Ctrl Pts',(21.7863944097143,-10.9722807946157,
0.));
#218750=CARTESIAN_POINT('Ctrl Pts',(21.7863944097143,-10.9722807946157,
12.));
#218751=CARTESIAN_POINT('Ctrl Pts',(21.8015809157302,-10.9898769120913,
0.));
#218752=CARTESIAN_POINT('Ctrl Pts',(21.8015809157302,-10.9898769120913,
12.));
#218753=CARTESIAN_POINT('Ctrl Pts',(21.8167823571168,-11.0075792647477,
0.));
#218754=CARTESIAN_POINT('Ctrl Pts',(21.8167823571168,-11.0075792647477,
12.));
#218755=CARTESIAN_POINT('Ctrl Pts',(21.8319980886033,-11.0253875994598,
0.));
#218756=CARTESIAN_POINT('Ctrl Pts',(21.8319980886033,-11.0253875994598,
12.));
#218757=CARTESIAN_POINT('Ctrl Pts',(21.8472274713103,-11.0433016640808,
0.));
#218758=CARTESIAN_POINT('Ctrl Pts',(21.8472274713103,-11.0433016640808,
12.));
#218759=CARTESIAN_POINT('Ctrl Pts',(21.8624698726319,-11.0613212074364,
0.));
#218760=CARTESIAN_POINT('Ctrl Pts',(21.8624698726319,-11.0613212074364,
12.));
#218761=CARTESIAN_POINT('Ctrl Pts',(21.8777246661191,-11.0794459793058,
0.));
#218762=CARTESIAN_POINT('Ctrl Pts',(21.8777246661191,-11.0794459793058,
12.));
#218763=CARTESIAN_POINT('Ctrl Pts',(21.8929912313608,-11.0976757303944,
0.));
#218764=CARTESIAN_POINT('Ctrl Pts',(21.8929912313608,-11.0976757303944,
12.));
#218765=CARTESIAN_POINT('Ctrl Pts',(21.9082689538687,-11.1160102123024,
0.));
#218766=CARTESIAN_POINT('Ctrl Pts',(21.9082689538687,-11.1160102123024,
12.));
#218767=CARTESIAN_POINT('Ctrl Pts',(21.9235572249518,-11.134449177474,0.));
#218768=CARTESIAN_POINT('Ctrl Pts',(21.9235572249518,-11.134449177474,12.));
#218769=CARTESIAN_POINT('Ctrl Pts',(21.9388554416437,-11.1529923792002,
0.));
#218770=CARTESIAN_POINT('Ctrl Pts',(21.9388554416437,-11.1529923792002,
12.));
#218771=CARTESIAN_POINT('Ctrl Pts',(21.9541630066504,-11.1716395716375,
0.));
#218772=CARTESIAN_POINT('Ctrl Pts',(21.9541630066504,-11.1716395716375,
12.));
#218773=CARTESIAN_POINT('Ctrl Pts',(21.9694793282913,-11.190390509811,0.));
#218774=CARTESIAN_POINT('Ctrl Pts',(21.9694793282913,-11.190390509811,12.));
#218775=CARTESIAN_POINT('Ctrl Pts',(21.9848038204439,-11.2092449496125,
0.));
#218776=CARTESIAN_POINT('Ctrl Pts',(21.9848038204439,-11.2092449496125,
12.));
#218777=CARTESIAN_POINT('Ctrl Pts',(22.0001359024839,-11.2282026477897,
0.));
#218778=CARTESIAN_POINT('Ctrl Pts',(22.0001359024839,-11.2282026477897,
12.));
#218779=CARTESIAN_POINT('Ctrl Pts',(22.0154749992364,-11.2472633619276,
0.));
#218780=CARTESIAN_POINT('Ctrl Pts',(22.0154749992364,-11.2472633619276,
12.));
#218781=CARTESIAN_POINT('Ctrl Pts',(22.0308205408351,-11.2664268504207,
0.));
#218782=CARTESIAN_POINT('Ctrl Pts',(22.0308205408351,-11.2664268504207,
12.));
#218783=CARTESIAN_POINT('Ctrl Pts',(22.046171962566,-11.2856928724374,0.));
#218784=CARTESIAN_POINT('Ctrl Pts',(22.046171962566,-11.2856928724374,12.));
#218785=CARTESIAN_POINT('Ctrl Pts',(22.0615287047179,-11.3050611878771,
0.));
#218786=CARTESIAN_POINT('Ctrl Pts',(22.0615287047179,-11.3050611878771,
12.));
#218787=CARTESIAN_POINT('Ctrl Pts',(22.0768902124267,-11.3245315573168,
0.));
#218788=CARTESIAN_POINT('Ctrl Pts',(22.0768902124267,-11.3245315573168,
12.));
#218789=CARTESIAN_POINT('Ctrl Pts',(22.0922559355293,-11.3441037419553,
0.));
#218790=CARTESIAN_POINT('Ctrl Pts',(22.0922559355293,-11.3441037419553,
12.));
#218791=CARTESIAN_POINT('Ctrl Pts',(22.1076253283978,-11.3637775035367,
0.));
#218792=CARTESIAN_POINT('Ctrl Pts',(22.1076253283978,-11.3637775035367,
12.));
#218793=CARTESIAN_POINT('Ctrl Pts',(22.1229978500185,-11.3835526044256,
0.));
#218794=CARTESIAN_POINT('Ctrl Pts',(22.1229978500185,-11.3835526044256,
12.));
#218795=CARTESIAN_POINT('Ctrl Pts',(22.1383729640963,-11.4034288076909,
0.));
#218796=CARTESIAN_POINT('Ctrl Pts',(22.1383729640963,-11.4034288076909,
12.));
#218797=CARTESIAN_POINT('Ctrl Pts',(22.1537501391486,-11.4234058771742,
0.));
#218798=CARTESIAN_POINT('Ctrl Pts',(22.1537501391486,-11.4234058771742,
12.));
#218799=CARTESIAN_POINT('Ctrl Pts',(22.1691288486096,-11.443483577557,0.));
#218800=CARTESIAN_POINT('Ctrl Pts',(22.1691288486096,-11.443483577557,12.));
#218801=CARTESIAN_POINT('Ctrl Pts',(22.1845085709169,-11.463661674411,0.));
#218802=CARTESIAN_POINT('Ctrl Pts',(22.1845085709169,-11.463661674411,12.));
#218803=CARTESIAN_POINT('Ctrl Pts',(22.1998887896435,-11.4839399342589,
0.));
#218804=CARTESIAN_POINT('Ctrl Pts',(22.1998887896435,-11.4839399342589,
12.));
#218805=CARTESIAN_POINT('Ctrl Pts',(22.215268993102,-11.504318124424,0.));
#218806=CARTESIAN_POINT('Ctrl Pts',(22.215268993102,-11.504318124424,12.));
#218807=CARTESIAN_POINT('Ctrl Pts',(22.2306486738899,-11.5247960128476,
0.));
#218808=CARTESIAN_POINT('Ctrl Pts',(22.2306486738899,-11.5247960128476,
12.));
#218809=CARTESIAN_POINT('Ctrl Pts',(22.2460273284653,-11.545373367912,0.));
#218810=CARTESIAN_POINT('Ctrl Pts',(22.2460273284653,-11.545373367912,12.));
#218811=CARTESIAN_POINT('Ctrl Pts',(22.2614044566898,-11.5660499582403,
0.));
#218812=CARTESIAN_POINT('Ctrl Pts',(22.2614044566898,-11.5660499582403,
12.));
#218813=CARTESIAN_POINT('Ctrl Pts',(22.2767795614349,-11.5868255525189,
0.));
#218814=CARTESIAN_POINT('Ctrl Pts',(22.2767795614349,-11.5868255525189,
12.));
#218815=CARTESIAN_POINT('Ctrl Pts',(22.2921521480357,-11.6076999192359,
0.));
#218816=CARTESIAN_POINT('Ctrl Pts',(22.2921521480357,-11.6076999192359,
12.));
#218817=CARTESIAN_POINT('Ctrl Pts',(22.3075217249049,-11.6286728270011,
0.));
#218818=CARTESIAN_POINT('Ctrl Pts',(22.3075217249049,-11.6286728270011,
12.));
#218819=CARTESIAN_POINT('Ctrl Pts',(22.3228878043976,-11.6497440449858,
0.));
#218820=CARTESIAN_POINT('Ctrl Pts',(22.3228878043976,-11.6497440449858,
12.));
#218821=CARTESIAN_POINT('Ctrl Pts',(22.3382499035618,-11.6709133432986,
0.));
#218822=CARTESIAN_POINT('Ctrl Pts',(22.3382499035618,-11.6709133432986,
12.));
#218823=CARTESIAN_POINT('Ctrl Pts',(22.3536075450028,-11.6921804934056,
0.));
#218824=CARTESIAN_POINT('Ctrl Pts',(22.3536075450028,-11.6921804934056,
12.));
#218825=CARTESIAN_POINT('Ctrl Pts',(22.3689602575492,-11.7135452684532,
0.));
#218826=CARTESIAN_POINT('Ctrl Pts',(22.3689602575492,-11.7135452684532,
12.));
#218827=CARTESIAN_POINT('Ctrl Pts',(22.3843075773905,-11.7350074437961,
0.));
#218828=CARTESIAN_POINT('Ctrl Pts',(22.3843075773905,-11.7350074437961,
12.));
#218829=CARTESIAN_POINT('Ctrl Pts',(22.39964904692,-11.7565667964765,0.));
#218830=CARTESIAN_POINT('Ctrl Pts',(22.39964904692,-11.7565667964765,12.));
#218831=CARTESIAN_POINT('Ctrl Pts',(22.4149842125018,-11.7782231042041,
0.));
#218832=CARTESIAN_POINT('Ctrl Pts',(22.4149842125018,-11.7782231042041,
12.));
#218833=CARTESIAN_POINT('Ctrl Pts',(22.4303126226468,-11.7999761445175,
0.));
#218834=CARTESIAN_POINT('Ctrl Pts',(22.4303126226468,-11.7999761445175,
12.));
#218835=CARTESIAN_POINT('Ctrl Pts',(22.4456338258738,-11.8218256937889,
0.));
#218836=CARTESIAN_POINT('Ctrl Pts',(22.4456338258738,-11.8218256937889,
12.));
#218837=CARTESIAN_POINT('Ctrl Pts',(22.4609473690469,-11.8437715264487,
0.));
#218838=CARTESIAN_POINT('Ctrl Pts',(22.4609473690469,-11.8437715264487,
12.));
#218839=CARTESIAN_POINT('Ctrl Pts',(22.4762527946694,-11.8658134137018,
0.));
#218840=CARTESIAN_POINT('Ctrl Pts',(22.4762527946694,-11.8658134137018,
12.));
#218841=CARTESIAN_POINT('Ctrl Pts',(22.4915496418472,-11.8879511239941,
0.));
#218842=CARTESIAN_POINT('Ctrl Pts',(22.4915496418472,-11.8879511239941,
12.));
#218843=CARTESIAN_POINT('Ctrl Pts',(22.5068374513958,-11.9101844254555,
0.));
#218844=CARTESIAN_POINT('Ctrl Pts',(22.5068374513958,-11.9101844254555,
12.));
#218845=CARTESIAN_POINT('Ctrl Pts',(22.5221157697869,-11.9325130877801,
0.));
#218846=CARTESIAN_POINT('Ctrl Pts',(22.5221157697869,-11.9325130877801,
12.));
#218847=CARTESIAN_POINT('Ctrl Pts',(22.5373841537299,-11.9549368843996,
0.));
#218848=CARTESIAN_POINT('Ctrl Pts',(22.5373841537299,-11.9549368843996,
12.));
#218849=CARTESIAN_POINT('Ctrl Pts',(22.5526421741159,-11.9774555943496,
0.));
#218850=CARTESIAN_POINT('Ctrl Pts',(22.5526421741159,-11.9774555943496,
12.));
#218851=CARTESIAN_POINT('Ctrl Pts',(22.5678894211194,-12.0000690046697,
0.));
#218852=CARTESIAN_POINT('Ctrl Pts',(22.5678894211194,-12.0000690046697,
12.));
#218853=CARTESIAN_POINT('Ctrl Pts',(22.5831255061306,-12.0227769113132,
0.));
#218854=CARTESIAN_POINT('Ctrl Pts',(22.5831255061306,-12.0227769113132,
12.));
#218855=CARTESIAN_POINT('Ctrl Pts',(22.5983500505675,-12.0455791139135,
0.));
#218856=CARTESIAN_POINT('Ctrl Pts',(22.5983500505675,-12.0455791139135,
12.));
#218857=CARTESIAN_POINT('Ctrl Pts',(22.613562676493,-12.0684754113869,0.));
#218858=CARTESIAN_POINT('Ctrl Pts',(22.613562676493,-12.0684754113869,12.));
#218859=CARTESIAN_POINT('Ctrl Pts',(22.628762996708,-12.0914655972828,0.));
#218860=CARTESIAN_POINT('Ctrl Pts',(22.628762996708,-12.0914655972828,12.));
#218861=CARTESIAN_POINT('Ctrl Pts',(22.6439506046611,-12.1145494550384,
0.));
#218862=CARTESIAN_POINT('Ctrl Pts',(22.6439506046611,-12.1145494550384,
12.));
#218863=CARTESIAN_POINT('Ctrl Pts',(22.6591250653942,-12.1377267537141,
0.));
#218864=CARTESIAN_POINT('Ctrl Pts',(22.6591250653942,-12.1377267537141,
12.));
#218865=CARTESIAN_POINT('Ctrl Pts',(22.6742859034891,-12.1609972423089,
0.));
#218866=CARTESIAN_POINT('Ctrl Pts',(22.6742859034891,-12.1609972423089,
12.));
#218867=CARTESIAN_POINT('Ctrl Pts',(22.6894326204959,-12.1843606579246,
0.));
#218868=CARTESIAN_POINT('Ctrl Pts',(22.6894326204959,-12.1843606579246,
12.));
#218869=CARTESIAN_POINT('Ctrl Pts',(22.7045647168659,-12.2078167360267,
0.));
#218870=CARTESIAN_POINT('Ctrl Pts',(22.7045647168659,-12.2078167360267,
12.));
#218871=CARTESIAN_POINT('Ctrl Pts',(22.7196817119299,-12.2313652198047,
0.));
#218872=CARTESIAN_POINT('Ctrl Pts',(22.7196817119299,-12.2313652198047,
12.));
#218873=CARTESIAN_POINT('Ctrl Pts',(22.7347831655251,-12.2550058702389,
0.));
#218874=CARTESIAN_POINT('Ctrl Pts',(22.7347831655251,-12.2550058702389,
12.));
#218875=CARTESIAN_POINT('Ctrl Pts',(22.7498686970096,-12.2787384750747,
0.));
#218876=CARTESIAN_POINT('Ctrl Pts',(22.7498686970096,-12.2787384750747,
12.));
#218877=CARTESIAN_POINT('Ctrl Pts',(22.7649380101154,-12.3025628601812,
0.));
#218878=CARTESIAN_POINT('Ctrl Pts',(22.7649380101154,-12.3025628601812,
12.));
#218879=CARTESIAN_POINT('Ctrl Pts',(22.7799908974947,-12.3264788926108,
0.));
#218880=CARTESIAN_POINT('Ctrl Pts',(22.7799908974947,-12.3264788926108,
12.));
#218881=CARTESIAN_POINT('Ctrl Pts',(22.7950272216959,-12.3504864740361,
0.));
#218882=CARTESIAN_POINT('Ctrl Pts',(22.7950272216959,-12.3504864740361,
12.));
#218883=CARTESIAN_POINT('Ctrl Pts',(22.8100469022632,-12.3745855366772,
0.));
#218884=CARTESIAN_POINT('Ctrl Pts',(22.8100469022632,-12.3745855366772,
12.));
#218885=CARTESIAN_POINT('Ctrl Pts',(22.8220493007353,-12.393937937903,0.));
#218886=CARTESIAN_POINT('Ctrl Pts',(22.8220493007353,-12.393937937903,12.));
#218887=CARTESIAN_POINT('Ctrl Pts',(22.8310435872852,-12.4084933766366,
0.));
#218888=CARTESIAN_POINT('Ctrl Pts',(22.8310435872852,-12.4084933766366,
12.));
#218889=CARTESIAN_POINT('Ctrl Pts',(22.8370364396497,-12.4182152851867,
0.));
#218890=CARTESIAN_POINT('Ctrl Pts',(22.8370364396497,-12.4182152851867,
12.));
#218891=CARTESIAN_POINT('Ctrl Pts',(22.8400320311648,-12.4230808101438,
0.));
#218892=CARTESIAN_POINT('Ctrl Pts',(22.8400320311648,-12.4230808101438,
12.));
#218893=CARTESIAN_POINT('',(22.8400320311648,-12.4230808101438,0.));
#218894=CARTESIAN_POINT('Ctrl Pts',(20.353053841303,-9.71462809124917,0.));
#218895=CARTESIAN_POINT('Ctrl Pts',(20.353060251684,-9.71462954053074,0.));
#218896=CARTESIAN_POINT('Ctrl Pts',(20.3531126095522,-9.71465227853122,
0.));
#218897=CARTESIAN_POINT('Ctrl Pts',(20.3533097561886,-9.71474590350792,
0.));
#218898=CARTESIAN_POINT('Ctrl Pts',(20.3538098605706,-9.71498978052101,
0.));
#218899=CARTESIAN_POINT('Ctrl Pts',(20.3548282742361,-9.71549257088175,
0.));
#218900=CARTESIAN_POINT('Ctrl Pts',(20.3562337557875,-9.71619192554147,
0.));
#218901=CARTESIAN_POINT('Ctrl Pts',(20.3580133103357,-9.71708493723062,
0.));
#218902=CARTESIAN_POINT('Ctrl Pts',(20.3601498764344,-9.71816778327999,
0.));
#218903=CARTESIAN_POINT('Ctrl Pts',(20.362625691398,-9.71943648548115,0.));
#218904=CARTESIAN_POINT('Ctrl Pts',(20.3654261611055,-9.72088778381102,
0.));
#218905=CARTESIAN_POINT('Ctrl Pts',(20.3685406190576,-9.72251930722504,
0.));
#218906=CARTESIAN_POINT('Ctrl Pts',(20.371960235676,-9.72432910043193,0.));
#218907=CARTESIAN_POINT('Ctrl Pts',(20.3756766651952,-9.72631531732871,
0.));
#218908=CARTESIAN_POINT('Ctrl Pts',(20.3796805893304,-9.72847589116533,
0.));
#218909=CARTESIAN_POINT('Ctrl Pts',(20.3839624556742,-9.73080870123726,
0.));
#218910=CARTESIAN_POINT('Ctrl Pts',(20.3885129129912,-9.73331167102812,
0.));
#218911=CARTESIAN_POINT('Ctrl Pts',(20.3933234845646,-9.7359829201425,0.));
#218912=CARTESIAN_POINT('Ctrl Pts',(20.3983866213331,-9.73882077613206,
0.));
#218913=CARTESIAN_POINT('Ctrl Pts',(20.4036953576549,-9.74182369656273,
0.));
#218914=CARTESIAN_POINT('Ctrl Pts',(20.4092430879861,-9.74499021838537,
0.));
#218915=CARTESIAN_POINT('Ctrl Pts',(20.4150232777393,-9.74831889242175,
0.));
#218916=CARTESIAN_POINT('Ctrl Pts',(20.4210295275818,-9.75180829786433,
0.));
#218917=CARTESIAN_POINT('Ctrl Pts',(20.4272556476629,-9.75545705902416,
0.));
#218918=CARTESIAN_POINT('Ctrl Pts',(20.4336957355474,-9.7592638628993,0.));
#218919=CARTESIAN_POINT('Ctrl Pts',(20.4403442329401,-9.76322747195502,
0.));
#218920=CARTESIAN_POINT('Ctrl Pts',(20.447195862298,-9.76734670980897,0.));
#218921=CARTESIAN_POINT('Ctrl Pts',(20.4542455817527,-9.7716204510407,0.));
#218922=CARTESIAN_POINT('Ctrl Pts',(20.4614885274973,-9.77604760815523,
0.));
#218923=CARTESIAN_POINT('Ctrl Pts',(20.4689199790668,-9.78062712373313,
0.));
#218924=CARTESIAN_POINT('Ctrl Pts',(20.4765353711585,-9.78535797314162,
0.));
#218925=CARTESIAN_POINT('Ctrl Pts',(20.4843302955329,-9.7902391649866,0.));
#218926=CARTESIAN_POINT('Ctrl Pts',(20.4923005087945,-9.79526974288344,
0.));
#218927=CARTESIAN_POINT('Ctrl Pts',(20.500441931211,-9.80044878520968,0.));
#218928=CARTESIAN_POINT('Ctrl Pts',(20.5087506310507,-9.80577540161103,
0.));
#218929=CARTESIAN_POINT('Ctrl Pts',(20.5172228122839,-9.81124873025278,
0.));
#218930=CARTESIAN_POINT('Ctrl Pts',(20.5258548000625,-9.81686793455918,
0.));
#218931=CARTESIAN_POINT('Ctrl Pts',(20.534643029951,-9.82263220080328,0.));
#218932=CARTESIAN_POINT('Ctrl Pts',(20.5435840460717,-9.82854073773858,
0.));
#218933=CARTESIAN_POINT('Ctrl Pts',(20.5526744976461,-9.83459277585321,
0.));
#218934=CARTESIAN_POINT('Ctrl Pts',(20.5619111362406,-9.84078756677589,
0.));
#218935=CARTESIAN_POINT('Ctrl Pts',(20.5712908125145,-9.84712438256308,
0.));
#218936=CARTESIAN_POINT('Ctrl Pts',(20.580810471002,-9.85360251457004,0.));
#218937=CARTESIAN_POINT('Ctrl Pts',(20.5904671449754,-9.8602212723275,0.));
#218938=CARTESIAN_POINT('Ctrl Pts',(20.6002579513696,-9.86697998242612,
0.));
#218939=CARTESIAN_POINT('Ctrl Pts',(20.6101800854491,-9.87387798732944,
0.));
#218940=CARTESIAN_POINT('Ctrl Pts',(20.6202308177472,-9.88091464472669,
0.));
#218941=CARTESIAN_POINT('Ctrl Pts',(20.6304074914086,-9.88808932697305,
0.));
#218942=CARTESIAN_POINT('Ctrl Pts',(20.6407075193977,-9.89540142049124,
0.));
#218943=CARTESIAN_POINT('Ctrl Pts',(20.6511283817415,-9.90285032516696,
0.));
#218944=CARTESIAN_POINT('Ctrl Pts',(20.6616676228315,-9.91043545377005,
0.));
#218945=CARTESIAN_POINT('Ctrl Pts',(20.6723228488261,-9.91815623141285,
0.));
#218946=CARTESIAN_POINT('Ctrl Pts',(20.6830917250255,-9.92601209498751,
0.));
#218947=CARTESIAN_POINT('Ctrl Pts',(20.6939719732485,-9.93400249259737,
0.));
#218948=CARTESIAN_POINT('Ctrl Pts',(20.7049613692237,-9.94212688298251,
0.));
#218949=CARTESIAN_POINT('Ctrl Pts',(20.716057740758,-9.95038473514962,0.));
#218950=CARTESIAN_POINT('Ctrl Pts',(20.7272589658752,-9.95877552798403,
0.));
#218951=CARTESIAN_POINT('Ctrl Pts',(20.7385629709795,-9.96729874986199,
0.));
#218952=CARTESIAN_POINT('Ctrl Pts',(20.7499677289625,-9.97595389823461,
0.));
#218953=CARTESIAN_POINT('Ctrl Pts',(20.7614712574989,-9.98474047926846,
0.));
#218954=CARTESIAN_POINT('Ctrl Pts',(20.7730716175417,-9.99365800754638,
0.));
#218955=CARTESIAN_POINT('Ctrl Pts',(20.7847669117568,-10.0027060057389,
0.));
#218956=CARTESIAN_POINT('Ctrl Pts',(20.7965552829907,-10.0118840042786,
0.));
#218957=CARTESIAN_POINT('Ctrl Pts',(20.8084349126885,-10.0211915410095,
0.));
#218958=CARTESIAN_POINT('Ctrl Pts',(20.8204040196599,-10.0306281609435,
0.));
#218959=CARTESIAN_POINT('Ctrl Pts',(20.8324608588906,-10.0401934160234,
0.));
#218960=CARTESIAN_POINT('Ctrl Pts',(20.8446037203402,-10.0498868648733,
0.));
#218961=CARTESIAN_POINT('Ctrl Pts',(20.856830927732,-10.0597080725375,0.));
#218962=CARTESIAN_POINT('Ctrl Pts',(20.8691408373705,-10.0696566102219,
0.));
#218963=CARTESIAN_POINT('Ctrl Pts',(20.8815318371844,-10.0797320551154,
0.));
#218964=CARTESIAN_POINT('Ctrl Pts',(20.8940023457371,-10.0899339901916,
0.));
#218965=CARTESIAN_POINT('Ctrl Pts',(20.9065508112556,-10.1002620040076,
0.));
#218966=CARTESIAN_POINT('Ctrl Pts',(20.9191757106266,-10.1107156904836,
0.));
#218967=CARTESIAN_POINT('Ctrl Pts',(20.931875548473,-10.1212946487057,0.));
#218968=CARTESIAN_POINT('Ctrl Pts',(20.944648856393,-10.1319984827909,0.));
#218969=CARTESIAN_POINT('Ctrl Pts',(20.9574941921591,-10.1428268017257,
0.));
#218970=CARTESIAN_POINT('Ctrl Pts',(20.970410138937,-10.1537792192065,0.));
#218971=CARTESIAN_POINT('Ctrl Pts',(20.9833953044736,-10.1648553534567,
0.));
#218972=CARTESIAN_POINT('Ctrl Pts',(20.9964483203685,-10.1760548270765,
0.));
#218973=CARTESIAN_POINT('Ctrl Pts',(21.0095678414486,-10.1873772669358,
0.));
#218974=CARTESIAN_POINT('Ctrl Pts',(21.0227525451107,-10.1988223040425,
0.));
#218975=CARTESIAN_POINT('Ctrl Pts',(21.0360011306814,-10.2103895734124,
0.));
#218976=CARTESIAN_POINT('Ctrl Pts',(21.0493123187483,-10.2220787139157,
0.));
#218977=CARTESIAN_POINT('Ctrl Pts',(21.0626848505665,-10.233889368157,0.));
#218978=CARTESIAN_POINT('Ctrl Pts',(21.0761174875448,-10.2458211823915,
0.));
#218979=CARTESIAN_POINT('Ctrl Pts',(21.0896090107066,-10.2578738064183,
0.));
#218980=CARTESIAN_POINT('Ctrl Pts',(21.1031582201625,-10.2700468934743,
0.));
#218981=CARTESIAN_POINT('Ctrl Pts',(21.1167639345623,-10.2823401001067,
0.));
#218982=CARTESIAN_POINT('Ctrl Pts',(21.130424990599,-10.2947530860714,0.));
#218983=CARTESIAN_POINT('Ctrl Pts',(21.1441402425831,-10.307285514268,0.));
#218984=CARTESIAN_POINT('Ctrl Pts',(21.1579085619959,-10.3199370506541,
0.));
#218985=CARTESIAN_POINT('Ctrl Pts',(21.1717288370512,-10.3327073641574,
0.));
#218986=CARTESIAN_POINT('Ctrl Pts',(21.1855999722427,-10.3455961265706,
0.));
#218987=CARTESIAN_POINT('Ctrl Pts',(21.1995208879205,-10.3586030124595,
0.));
#218988=CARTESIAN_POINT('Ctrl Pts',(21.2134905199359,-10.3717276991137,
0.));
#218989=CARTESIAN_POINT('Ctrl Pts',(21.2275078192708,-10.384969866479,0.));
#218990=CARTESIAN_POINT('Ctrl Pts',(21.2415717516713,-10.3983291970846,
0.));
#218991=CARTESIAN_POINT('Ctrl Pts',(21.2556812972741,-10.4118053759584,
0.));
#218992=CARTESIAN_POINT('Ctrl Pts',(21.2698354502391,-10.4253980905394,
0.));
#218993=CARTESIAN_POINT('Ctrl Pts',(21.2840332184471,-10.4391070306385,
0.));
#218994=CARTESIAN_POINT('Ctrl Pts',(21.2982736231924,-10.452931888387,0.));
#218995=CARTESIAN_POINT('Ctrl Pts',(21.312555698873,-10.4668723581768,0.));
#218996=CARTESIAN_POINT('Ctrl Pts',(21.3268784926823,-10.4809281365933,
0.));
#218997=CARTESIAN_POINT('Ctrl Pts',(21.3412410642912,-10.4950989223341,
0.));
#218998=CARTESIAN_POINT('Ctrl Pts',(21.3556424855822,-10.509384416169,0.));
#218999=CARTESIAN_POINT('Ctrl Pts',(21.3700818403942,-10.523784320906,0.));
#219000=CARTESIAN_POINT('Ctrl Pts',(21.3845582242604,-10.5382983413422,
0.));
#219001=CARTESIAN_POINT('Ctrl Pts',(21.3990707441495,-10.5529261842107,
0.));
#219002=CARTESIAN_POINT('Ctrl Pts',(21.4136185181974,-10.5676675581106,
0.));
#219003=CARTESIAN_POINT('Ctrl Pts',(21.4282006754624,-10.582522173457,0.));
#219004=CARTESIAN_POINT('Ctrl Pts',(21.4428163557137,-10.597489742462,0.));
#219005=CARTESIAN_POINT('Ctrl Pts',(21.4574647092093,-10.612569979096,0.));
#219006=CARTESIAN_POINT('Ctrl Pts',(21.4721448964766,-10.6277625990457,
0.));
#219007=CARTESIAN_POINT('Ctrl Pts',(21.4868560880893,-10.6430673196609,
0.));
#219008=CARTESIAN_POINT('Ctrl Pts',(21.5015974644454,-10.6584838598941,
0.));
#219009=CARTESIAN_POINT('Ctrl Pts',(21.5163682155805,-10.6740119402835,
0.));
#219010=CARTESIAN_POINT('Ctrl Pts',(21.531167540981,-10.689651282929,0.));
#219011=CARTESIAN_POINT('Ctrl Pts',(21.5459946493955,-10.7054016114571,
0.));
#219012=CARTESIAN_POINT('Ctrl Pts',(21.5608487586467,-10.7212626509816,
0.));
#219013=CARTESIAN_POINT('Ctrl Pts',(21.5757290954372,-10.7372341280468,
0.));
#219014=CARTESIAN_POINT('Ctrl Pts',(21.5906348951745,-10.7533157705943,
0.));
#219015=CARTESIAN_POINT('Ctrl Pts',(21.6055654018179,-10.7695073079554,
0.));
#219016=CARTESIAN_POINT('Ctrl Pts',(21.6205198677176,-10.7858084708262,
0.));
#219017=CARTESIAN_POINT('Ctrl Pts',(21.6354975534557,-10.802218991237,0.));
#219018=CARTESIAN_POINT('Ctrl Pts',(21.6504977276864,-10.8187386025135,
0.));
#219019=CARTESIAN_POINT('Ctrl Pts',(21.6655196669727,-10.835367039227,0.));
#219020=CARTESIAN_POINT('Ctrl Pts',(21.6805626556461,-10.8521040371832,
0.));
#219021=CARTESIAN_POINT('Ctrl Pts',(21.6956259856667,-10.8689493334093,
0.));
#219022=CARTESIAN_POINT('Ctrl Pts',(21.7107089564822,-10.8859026661292,
0.));
#219023=CARTESIAN_POINT('Ctrl Pts',(21.7258108748874,-10.9029637747341,
0.));
#219024=CARTESIAN_POINT('Ctrl Pts',(21.74093105488,-10.9201323997386,0.));
#219025=CARTESIAN_POINT('Ctrl Pts',(21.7560688175252,-10.9374082827446,
0.));
#219026=CARTESIAN_POINT('Ctrl Pts',(21.7712234908468,-10.9547911664457,
0.));
#219027=CARTESIAN_POINT('Ctrl Pts',(21.7863944097143,-10.9722807946157,
0.));
#219028=CARTESIAN_POINT('Ctrl Pts',(21.8015809157302,-10.9898769120913,
0.));
#219029=CARTESIAN_POINT('Ctrl Pts',(21.8167823571168,-11.0075792647477,
0.));
#219030=CARTESIAN_POINT('Ctrl Pts',(21.8319980886033,-11.0253875994598,
0.));
#219031=CARTESIAN_POINT('Ctrl Pts',(21.8472274713103,-11.0433016640808,
0.));
#219032=CARTESIAN_POINT('Ctrl Pts',(21.8624698726319,-11.0613212074364,
0.));
#219033=CARTESIAN_POINT('Ctrl Pts',(21.8777246661191,-11.0794459793058,
0.));
#219034=CARTESIAN_POINT('Ctrl Pts',(21.8929912313608,-11.0976757303944,
0.));
#219035=CARTESIAN_POINT('Ctrl Pts',(21.9082689538687,-11.1160102123024,
0.));
#219036=CARTESIAN_POINT('Ctrl Pts',(21.9235572249518,-11.134449177474,0.));
#219037=CARTESIAN_POINT('Ctrl Pts',(21.9388554416437,-11.1529923792002,
0.));
#219038=CARTESIAN_POINT('Ctrl Pts',(21.9541630066504,-11.1716395716375,
0.));
#219039=CARTESIAN_POINT('Ctrl Pts',(21.9694793282913,-11.190390509811,0.));
#219040=CARTESIAN_POINT('Ctrl Pts',(21.9848038204439,-11.2092449496125,
0.));
#219041=CARTESIAN_POINT('Ctrl Pts',(22.0001359024839,-11.2282026477897,
0.));
#219042=CARTESIAN_POINT('Ctrl Pts',(22.0154749992364,-11.2472633619276,
0.));
#219043=CARTESIAN_POINT('Ctrl Pts',(22.0308205408351,-11.2664268504207,
0.));
#219044=CARTESIAN_POINT('Ctrl Pts',(22.046171962566,-11.2856928724374,0.));
#219045=CARTESIAN_POINT('Ctrl Pts',(22.0615287047179,-11.3050611878771,
0.));
#219046=CARTESIAN_POINT('Ctrl Pts',(22.0768902124267,-11.3245315573168,
0.));
#219047=CARTESIAN_POINT('Ctrl Pts',(22.0922559355293,-11.3441037419553,
0.));
#219048=CARTESIAN_POINT('Ctrl Pts',(22.1076253283978,-11.3637775035367,
0.));
#219049=CARTESIAN_POINT('Ctrl Pts',(22.1229978500185,-11.3835526044256,
0.));
#219050=CARTESIAN_POINT('Ctrl Pts',(22.1383729640963,-11.4034288076909,
0.));
#219051=CARTESIAN_POINT('Ctrl Pts',(22.1537501391486,-11.4234058771742,
0.));
#219052=CARTESIAN_POINT('Ctrl Pts',(22.1691288486096,-11.443483577557,0.));
#219053=CARTESIAN_POINT('Ctrl Pts',(22.1845085709169,-11.463661674411,0.));
#219054=CARTESIAN_POINT('Ctrl Pts',(22.1998887896435,-11.4839399342589,
0.));
#219055=CARTESIAN_POINT('Ctrl Pts',(22.215268993102,-11.504318124424,0.));
#219056=CARTESIAN_POINT('Ctrl Pts',(22.2306486738899,-11.5247960128476,
0.));
#219057=CARTESIAN_POINT('Ctrl Pts',(22.2460273284653,-11.545373367912,0.));
#219058=CARTESIAN_POINT('Ctrl Pts',(22.2614044566898,-11.5660499582403,
0.));
#219059=CARTESIAN_POINT('Ctrl Pts',(22.2767795614349,-11.5868255525189,
0.));
#219060=CARTESIAN_POINT('Ctrl Pts',(22.2921521480357,-11.6076999192359,
0.));
#219061=CARTESIAN_POINT('Ctrl Pts',(22.3075217249049,-11.6286728270011,
0.));
#219062=CARTESIAN_POINT('Ctrl Pts',(22.3228878043976,-11.6497440449858,
0.));
#219063=CARTESIAN_POINT('Ctrl Pts',(22.3382499035618,-11.6709133432986,
0.));
#219064=CARTESIAN_POINT('Ctrl Pts',(22.3536075450028,-11.6921804934056,
0.));
#219065=CARTESIAN_POINT('Ctrl Pts',(22.3689602575492,-11.7135452684532,
0.));
#219066=CARTESIAN_POINT('Ctrl Pts',(22.3843075773905,-11.7350074437961,
0.));
#219067=CARTESIAN_POINT('Ctrl Pts',(22.39964904692,-11.7565667964765,0.));
#219068=CARTESIAN_POINT('Ctrl Pts',(22.4149842125018,-11.7782231042041,
0.));
#219069=CARTESIAN_POINT('Ctrl Pts',(22.4303126226468,-11.7999761445175,
0.));
#219070=CARTESIAN_POINT('Ctrl Pts',(22.4456338258738,-11.8218256937889,
0.));
#219071=CARTESIAN_POINT('Ctrl Pts',(22.4609473690469,-11.8437715264487,
0.));
#219072=CARTESIAN_POINT('Ctrl Pts',(22.4762527946694,-11.8658134137018,
0.));
#219073=CARTESIAN_POINT('Ctrl Pts',(22.4915496418472,-11.8879511239941,
0.));
#219074=CARTESIAN_POINT('Ctrl Pts',(22.5068374513958,-11.9101844254555,
0.));
#219075=CARTESIAN_POINT('Ctrl Pts',(22.5221157697869,-11.9325130877801,
0.));
#219076=CARTESIAN_POINT('Ctrl Pts',(22.5373841537299,-11.9549368843996,
0.));
#219077=CARTESIAN_POINT('Ctrl Pts',(22.5526421741159,-11.9774555943496,
0.));
#219078=CARTESIAN_POINT('Ctrl Pts',(22.5678894211194,-12.0000690046697,
0.));
#219079=CARTESIAN_POINT('Ctrl Pts',(22.5831255061306,-12.0227769113132,
0.));
#219080=CARTESIAN_POINT('Ctrl Pts',(22.5983500505675,-12.0455791139135,
0.));
#219081=CARTESIAN_POINT('Ctrl Pts',(22.613562676493,-12.0684754113869,0.));
#219082=CARTESIAN_POINT('Ctrl Pts',(22.628762996708,-12.0914655972828,0.));
#219083=CARTESIAN_POINT('Ctrl Pts',(22.6439506046611,-12.1145494550384,
0.));
#219084=CARTESIAN_POINT('Ctrl Pts',(22.6591250653942,-12.1377267537141,
0.));
#219085=CARTESIAN_POINT('Ctrl Pts',(22.6742859034891,-12.1609972423089,
0.));
#219086=CARTESIAN_POINT('Ctrl Pts',(22.6894326204959,-12.1843606579246,
0.));
#219087=CARTESIAN_POINT('Ctrl Pts',(22.7045647168659,-12.2078167360267,
0.));
#219088=CARTESIAN_POINT('Ctrl Pts',(22.7196817119299,-12.2313652198047,
0.));
#219089=CARTESIAN_POINT('Ctrl Pts',(22.7347831655251,-12.2550058702389,
0.));
#219090=CARTESIAN_POINT('Ctrl Pts',(22.7498686970096,-12.2787384750747,
0.));
#219091=CARTESIAN_POINT('Ctrl Pts',(22.7649380101154,-12.3025628601812,
0.));
#219092=CARTESIAN_POINT('Ctrl Pts',(22.7799908974947,-12.3264788926108,
0.));
#219093=CARTESIAN_POINT('Ctrl Pts',(22.7950272216959,-12.3504864740361,
0.));
#219094=CARTESIAN_POINT('Ctrl Pts',(22.8100469022632,-12.3745855366772,
0.));
#219095=CARTESIAN_POINT('Ctrl Pts',(22.8220493007353,-12.393937937903,0.));
#219096=CARTESIAN_POINT('Ctrl Pts',(22.8310435872852,-12.4084933766366,
0.));
#219097=CARTESIAN_POINT('Ctrl Pts',(22.8370364396497,-12.4182152851867,
0.));
#219098=CARTESIAN_POINT('Ctrl Pts',(22.8400320311648,-12.4230808101438,
0.));
#219099=CARTESIAN_POINT('',(22.8400320311648,-12.4230808101438,12.));
#219100=CARTESIAN_POINT('Ctrl Pts',(22.8400320311648,-12.4230808101438,
12.));
#219101=CARTESIAN_POINT('Ctrl Pts',(22.8370364396497,-12.4182152851867,
12.));
#219102=CARTESIAN_POINT('Ctrl Pts',(22.8310435872852,-12.4084933766366,
12.));
#219103=CARTESIAN_POINT('Ctrl Pts',(22.8220493007353,-12.393937937903,12.));
#219104=CARTESIAN_POINT('Ctrl Pts',(22.8100469022632,-12.3745855366772,
12.));
#219105=CARTESIAN_POINT('Ctrl Pts',(22.7950272216959,-12.3504864740361,
12.));
#219106=CARTESIAN_POINT('Ctrl Pts',(22.7799908974947,-12.3264788926108,
12.));
#219107=CARTESIAN_POINT('Ctrl Pts',(22.7649380101154,-12.3025628601812,
12.));
#219108=CARTESIAN_POINT('Ctrl Pts',(22.7498686970096,-12.2787384750747,
12.));
#219109=CARTESIAN_POINT('Ctrl Pts',(22.7347831655251,-12.2550058702389,
12.));
#219110=CARTESIAN_POINT('Ctrl Pts',(22.7196817119299,-12.2313652198047,
12.));
#219111=CARTESIAN_POINT('Ctrl Pts',(22.7045647168659,-12.2078167360267,
12.));
#219112=CARTESIAN_POINT('Ctrl Pts',(22.6894326204959,-12.1843606579246,
12.));
#219113=CARTESIAN_POINT('Ctrl Pts',(22.6742859034891,-12.1609972423089,
12.));
#219114=CARTESIAN_POINT('Ctrl Pts',(22.6591250653942,-12.1377267537141,
12.));
#219115=CARTESIAN_POINT('Ctrl Pts',(22.6439506046611,-12.1145494550384,
12.));
#219116=CARTESIAN_POINT('Ctrl Pts',(22.628762996708,-12.0914655972828,12.));
#219117=CARTESIAN_POINT('Ctrl Pts',(22.613562676493,-12.0684754113869,12.));
#219118=CARTESIAN_POINT('Ctrl Pts',(22.5983500505675,-12.0455791139135,
12.));
#219119=CARTESIAN_POINT('Ctrl Pts',(22.5831255061306,-12.0227769113132,
12.));
#219120=CARTESIAN_POINT('Ctrl Pts',(22.5678894211194,-12.0000690046697,
12.));
#219121=CARTESIAN_POINT('Ctrl Pts',(22.5526421741159,-11.9774555943496,
12.));
#219122=CARTESIAN_POINT('Ctrl Pts',(22.5373841537299,-11.9549368843996,
12.));
#219123=CARTESIAN_POINT('Ctrl Pts',(22.5221157697869,-11.9325130877801,
12.));
#219124=CARTESIAN_POINT('Ctrl Pts',(22.5068374513958,-11.9101844254555,
12.));
#219125=CARTESIAN_POINT('Ctrl Pts',(22.4915496418472,-11.8879511239941,
12.));
#219126=CARTESIAN_POINT('Ctrl Pts',(22.4762527946694,-11.8658134137018,
12.));
#219127=CARTESIAN_POINT('Ctrl Pts',(22.4609473690469,-11.8437715264487,
12.));
#219128=CARTESIAN_POINT('Ctrl Pts',(22.4456338258738,-11.8218256937889,
12.));
#219129=CARTESIAN_POINT('Ctrl Pts',(22.4303126226468,-11.7999761445175,
12.));
#219130=CARTESIAN_POINT('Ctrl Pts',(22.4149842125018,-11.7782231042041,
12.));
#219131=CARTESIAN_POINT('Ctrl Pts',(22.39964904692,-11.7565667964765,12.));
#219132=CARTESIAN_POINT('Ctrl Pts',(22.3843075773905,-11.7350074437961,
12.));
#219133=CARTESIAN_POINT('Ctrl Pts',(22.3689602575492,-11.7135452684532,
12.));
#219134=CARTESIAN_POINT('Ctrl Pts',(22.3536075450028,-11.6921804934056,
12.));
#219135=CARTESIAN_POINT('Ctrl Pts',(22.3382499035618,-11.6709133432986,
12.));
#219136=CARTESIAN_POINT('Ctrl Pts',(22.3228878043976,-11.6497440449858,
12.));
#219137=CARTESIAN_POINT('Ctrl Pts',(22.3075217249049,-11.6286728270011,
12.));
#219138=CARTESIAN_POINT('Ctrl Pts',(22.2921521480357,-11.6076999192359,
12.));
#219139=CARTESIAN_POINT('Ctrl Pts',(22.2767795614349,-11.5868255525189,
12.));
#219140=CARTESIAN_POINT('Ctrl Pts',(22.2614044566898,-11.5660499582403,
12.));
#219141=CARTESIAN_POINT('Ctrl Pts',(22.2460273284653,-11.545373367912,12.));
#219142=CARTESIAN_POINT('Ctrl Pts',(22.2306486738899,-11.5247960128476,
12.));
#219143=CARTESIAN_POINT('Ctrl Pts',(22.215268993102,-11.504318124424,12.));
#219144=CARTESIAN_POINT('Ctrl Pts',(22.1998887896435,-11.4839399342589,
12.));
#219145=CARTESIAN_POINT('Ctrl Pts',(22.1845085709169,-11.463661674411,12.));
#219146=CARTESIAN_POINT('Ctrl Pts',(22.1691288486096,-11.443483577557,12.));
#219147=CARTESIAN_POINT('Ctrl Pts',(22.1537501391486,-11.4234058771742,
12.));
#219148=CARTESIAN_POINT('Ctrl Pts',(22.1383729640963,-11.4034288076909,
12.));
#219149=CARTESIAN_POINT('Ctrl Pts',(22.1229978500185,-11.3835526044256,
12.));
#219150=CARTESIAN_POINT('Ctrl Pts',(22.1076253283978,-11.3637775035367,
12.));
#219151=CARTESIAN_POINT('Ctrl Pts',(22.0922559355293,-11.3441037419553,
12.));
#219152=CARTESIAN_POINT('Ctrl Pts',(22.0768902124267,-11.3245315573168,
12.));
#219153=CARTESIAN_POINT('Ctrl Pts',(22.0615287047179,-11.3050611878771,
12.));
#219154=CARTESIAN_POINT('Ctrl Pts',(22.046171962566,-11.2856928724374,12.));
#219155=CARTESIAN_POINT('Ctrl Pts',(22.0308205408351,-11.2664268504207,
12.));
#219156=CARTESIAN_POINT('Ctrl Pts',(22.0154749992364,-11.2472633619276,
12.));
#219157=CARTESIAN_POINT('Ctrl Pts',(22.0001359024839,-11.2282026477897,
12.));
#219158=CARTESIAN_POINT('Ctrl Pts',(21.9848038204439,-11.2092449496125,
12.));
#219159=CARTESIAN_POINT('Ctrl Pts',(21.9694793282913,-11.190390509811,12.));
#219160=CARTESIAN_POINT('Ctrl Pts',(21.9541630066504,-11.1716395716375,
12.));
#219161=CARTESIAN_POINT('Ctrl Pts',(21.9388554416437,-11.1529923792002,
12.));
#219162=CARTESIAN_POINT('Ctrl Pts',(21.9235572249518,-11.134449177474,12.));
#219163=CARTESIAN_POINT('Ctrl Pts',(21.9082689538687,-11.1160102123024,
12.));
#219164=CARTESIAN_POINT('Ctrl Pts',(21.8929912313608,-11.0976757303944,
12.));
#219165=CARTESIAN_POINT('Ctrl Pts',(21.8777246661191,-11.0794459793058,
12.));
#219166=CARTESIAN_POINT('Ctrl Pts',(21.8624698726319,-11.0613212074364,
12.));
#219167=CARTESIAN_POINT('Ctrl Pts',(21.8472274713103,-11.0433016640808,
12.));
#219168=CARTESIAN_POINT('Ctrl Pts',(21.8319980886033,-11.0253875994598,
12.));
#219169=CARTESIAN_POINT('Ctrl Pts',(21.8167823571168,-11.0075792647477,
12.));
#219170=CARTESIAN_POINT('Ctrl Pts',(21.8015809157302,-10.9898769120913,
12.));
#219171=CARTESIAN_POINT('Ctrl Pts',(21.7863944097143,-10.9722807946157,
12.));
#219172=CARTESIAN_POINT('Ctrl Pts',(21.7712234908468,-10.9547911664457,
12.));
#219173=CARTESIAN_POINT('Ctrl Pts',(21.7560688175252,-10.9374082827446,
12.));
#219174=CARTESIAN_POINT('Ctrl Pts',(21.74093105488,-10.9201323997386,12.));
#219175=CARTESIAN_POINT('Ctrl Pts',(21.7258108748874,-10.9029637747341,
12.));
#219176=CARTESIAN_POINT('Ctrl Pts',(21.7107089564822,-10.8859026661292,
12.));
#219177=CARTESIAN_POINT('Ctrl Pts',(21.6956259856667,-10.8689493334093,
12.));
#219178=CARTESIAN_POINT('Ctrl Pts',(21.6805626556461,-10.8521040371832,
12.));
#219179=CARTESIAN_POINT('Ctrl Pts',(21.6655196669727,-10.835367039227,12.));
#219180=CARTESIAN_POINT('Ctrl Pts',(21.6504977276864,-10.8187386025135,
12.));
#219181=CARTESIAN_POINT('Ctrl Pts',(21.6354975534557,-10.802218991237,12.));
#219182=CARTESIAN_POINT('Ctrl Pts',(21.6205198677176,-10.7858084708262,
12.));
#219183=CARTESIAN_POINT('Ctrl Pts',(21.6055654018179,-10.7695073079554,
12.));
#219184=CARTESIAN_POINT('Ctrl Pts',(21.5906348951745,-10.7533157705943,
12.));
#219185=CARTESIAN_POINT('Ctrl Pts',(21.5757290954372,-10.7372341280468,
12.));
#219186=CARTESIAN_POINT('Ctrl Pts',(21.5608487586467,-10.7212626509816,
12.));
#219187=CARTESIAN_POINT('Ctrl Pts',(21.5459946493955,-10.7054016114571,
12.));
#219188=CARTESIAN_POINT('Ctrl Pts',(21.531167540981,-10.689651282929,12.));
#219189=CARTESIAN_POINT('Ctrl Pts',(21.5163682155805,-10.6740119402835,
12.));
#219190=CARTESIAN_POINT('Ctrl Pts',(21.5015974644454,-10.6584838598941,
12.));
#219191=CARTESIAN_POINT('Ctrl Pts',(21.4868560880893,-10.6430673196609,
12.));
#219192=CARTESIAN_POINT('Ctrl Pts',(21.4721448964766,-10.6277625990457,
12.));
#219193=CARTESIAN_POINT('Ctrl Pts',(21.4574647092093,-10.612569979096,12.));
#219194=CARTESIAN_POINT('Ctrl Pts',(21.4428163557137,-10.597489742462,12.));
#219195=CARTESIAN_POINT('Ctrl Pts',(21.4282006754624,-10.582522173457,12.));
#219196=CARTESIAN_POINT('Ctrl Pts',(21.4136185181974,-10.5676675581106,
12.));
#219197=CARTESIAN_POINT('Ctrl Pts',(21.3990707441495,-10.5529261842107,
12.));
#219198=CARTESIAN_POINT('Ctrl Pts',(21.3845582242604,-10.5382983413422,
12.));
#219199=CARTESIAN_POINT('Ctrl Pts',(21.3700818403942,-10.523784320906,12.));
#219200=CARTESIAN_POINT('Ctrl Pts',(21.3556424855822,-10.509384416169,12.));
#219201=CARTESIAN_POINT('Ctrl Pts',(21.3412410642912,-10.4950989223341,
12.));
#219202=CARTESIAN_POINT('Ctrl Pts',(21.3268784926823,-10.4809281365933,
12.));
#219203=CARTESIAN_POINT('Ctrl Pts',(21.312555698873,-10.4668723581768,12.));
#219204=CARTESIAN_POINT('Ctrl Pts',(21.2982736231924,-10.452931888387,12.));
#219205=CARTESIAN_POINT('Ctrl Pts',(21.2840332184471,-10.4391070306385,
12.));
#219206=CARTESIAN_POINT('Ctrl Pts',(21.2698354502391,-10.4253980905394,
12.));
#219207=CARTESIAN_POINT('Ctrl Pts',(21.2556812972741,-10.4118053759584,
12.));
#219208=CARTESIAN_POINT('Ctrl Pts',(21.2415717516713,-10.3983291970846,
12.));
#219209=CARTESIAN_POINT('Ctrl Pts',(21.2275078192708,-10.384969866479,12.));
#219210=CARTESIAN_POINT('Ctrl Pts',(21.2134905199359,-10.3717276991137,
12.));
#219211=CARTESIAN_POINT('Ctrl Pts',(21.1995208879205,-10.3586030124595,
12.));
#219212=CARTESIAN_POINT('Ctrl Pts',(21.1855999722427,-10.3455961265706,
12.));
#219213=CARTESIAN_POINT('Ctrl Pts',(21.1717288370512,-10.3327073641574,
12.));
#219214=CARTESIAN_POINT('Ctrl Pts',(21.1579085619959,-10.3199370506541,
12.));
#219215=CARTESIAN_POINT('Ctrl Pts',(21.1441402425831,-10.307285514268,12.));
#219216=CARTESIAN_POINT('Ctrl Pts',(21.130424990599,-10.2947530860714,12.));
#219217=CARTESIAN_POINT('Ctrl Pts',(21.1167639345623,-10.2823401001067,
12.));
#219218=CARTESIAN_POINT('Ctrl Pts',(21.1031582201625,-10.2700468934743,
12.));
#219219=CARTESIAN_POINT('Ctrl Pts',(21.0896090107066,-10.2578738064183,
12.));
#219220=CARTESIAN_POINT('Ctrl Pts',(21.0761174875448,-10.2458211823915,
12.));
#219221=CARTESIAN_POINT('Ctrl Pts',(21.0626848505665,-10.233889368157,12.));
#219222=CARTESIAN_POINT('Ctrl Pts',(21.0493123187483,-10.2220787139157,
12.));
#219223=CARTESIAN_POINT('Ctrl Pts',(21.0360011306814,-10.2103895734124,
12.));
#219224=CARTESIAN_POINT('Ctrl Pts',(21.0227525451107,-10.1988223040425,
12.));
#219225=CARTESIAN_POINT('Ctrl Pts',(21.0095678414486,-10.1873772669358,
12.));
#219226=CARTESIAN_POINT('Ctrl Pts',(20.9964483203685,-10.1760548270765,
12.));
#219227=CARTESIAN_POINT('Ctrl Pts',(20.9833953044736,-10.1648553534567,
12.));
#219228=CARTESIAN_POINT('Ctrl Pts',(20.970410138937,-10.1537792192065,12.));
#219229=CARTESIAN_POINT('Ctrl Pts',(20.9574941921591,-10.1428268017257,
12.));
#219230=CARTESIAN_POINT('Ctrl Pts',(20.944648856393,-10.1319984827909,12.));
#219231=CARTESIAN_POINT('Ctrl Pts',(20.931875548473,-10.1212946487057,12.));
#219232=CARTESIAN_POINT('Ctrl Pts',(20.9191757106266,-10.1107156904836,
12.));
#219233=CARTESIAN_POINT('Ctrl Pts',(20.9065508112556,-10.1002620040076,
12.));
#219234=CARTESIAN_POINT('Ctrl Pts',(20.8940023457371,-10.0899339901916,
12.));
#219235=CARTESIAN_POINT('Ctrl Pts',(20.8815318371844,-10.0797320551154,
12.));
#219236=CARTESIAN_POINT('Ctrl Pts',(20.8691408373705,-10.0696566102219,
12.));
#219237=CARTESIAN_POINT('Ctrl Pts',(20.856830927732,-10.0597080725375,12.));
#219238=CARTESIAN_POINT('Ctrl Pts',(20.8446037203402,-10.0498868648733,
12.));
#219239=CARTESIAN_POINT('Ctrl Pts',(20.8324608588906,-10.0401934160234,
12.));
#219240=CARTESIAN_POINT('Ctrl Pts',(20.8204040196599,-10.0306281609435,
12.));
#219241=CARTESIAN_POINT('Ctrl Pts',(20.8084349126885,-10.0211915410095,
12.));
#219242=CARTESIAN_POINT('Ctrl Pts',(20.7965552829907,-10.0118840042786,
12.));
#219243=CARTESIAN_POINT('Ctrl Pts',(20.7847669117568,-10.0027060057389,
12.));
#219244=CARTESIAN_POINT('Ctrl Pts',(20.7730716175417,-9.99365800754638,
12.));
#219245=CARTESIAN_POINT('Ctrl Pts',(20.7614712574989,-9.98474047926846,
12.));
#219246=CARTESIAN_POINT('Ctrl Pts',(20.7499677289625,-9.97595389823461,
12.));
#219247=CARTESIAN_POINT('Ctrl Pts',(20.7385629709795,-9.96729874986199,
12.));
#219248=CARTESIAN_POINT('Ctrl Pts',(20.7272589658752,-9.95877552798403,
12.));
#219249=CARTESIAN_POINT('Ctrl Pts',(20.716057740758,-9.95038473514962,12.));
#219250=CARTESIAN_POINT('Ctrl Pts',(20.7049613692237,-9.94212688298251,
12.));
#219251=CARTESIAN_POINT('Ctrl Pts',(20.6939719732485,-9.93400249259737,
12.));
#219252=CARTESIAN_POINT('Ctrl Pts',(20.6830917250255,-9.92601209498751,
12.));
#219253=CARTESIAN_POINT('Ctrl Pts',(20.6723228488261,-9.91815623141285,
12.));
#219254=CARTESIAN_POINT('Ctrl Pts',(20.6616676228315,-9.91043545377005,
12.));
#219255=CARTESIAN_POINT('Ctrl Pts',(20.6511283817415,-9.90285032516696,
12.));
#219256=CARTESIAN_POINT('Ctrl Pts',(20.6407075193977,-9.89540142049124,
12.));
#219257=CARTESIAN_POINT('Ctrl Pts',(20.6304074914086,-9.88808932697305,
12.));
#219258=CARTESIAN_POINT('Ctrl Pts',(20.6202308177472,-9.88091464472669,
12.));
#219259=CARTESIAN_POINT('Ctrl Pts',(20.6101800854491,-9.87387798732944,
12.));
#219260=CARTESIAN_POINT('Ctrl Pts',(20.6002579513696,-9.86697998242612,
12.));
#219261=CARTESIAN_POINT('Ctrl Pts',(20.5904671449754,-9.8602212723275,12.));
#219262=CARTESIAN_POINT('Ctrl Pts',(20.580810471002,-9.85360251457004,12.));
#219263=CARTESIAN_POINT('Ctrl Pts',(20.5712908125145,-9.84712438256308,
12.));
#219264=CARTESIAN_POINT('Ctrl Pts',(20.5619111362406,-9.84078756677589,
12.));
#219265=CARTESIAN_POINT('Ctrl Pts',(20.5526744976461,-9.83459277585321,
12.));
#219266=CARTESIAN_POINT('Ctrl Pts',(20.5435840460717,-9.82854073773858,
12.));
#219267=CARTESIAN_POINT('Ctrl Pts',(20.534643029951,-9.82263220080328,12.));
#219268=CARTESIAN_POINT('Ctrl Pts',(20.5258548000625,-9.81686793455918,
12.));
#219269=CARTESIAN_POINT('Ctrl Pts',(20.5172228122839,-9.81124873025278,
12.));
#219270=CARTESIAN_POINT('Ctrl Pts',(20.5087506310507,-9.80577540161103,
12.));
#219271=CARTESIAN_POINT('Ctrl Pts',(20.500441931211,-9.80044878520968,12.));
#219272=CARTESIAN_POINT('Ctrl Pts',(20.4923005087945,-9.79526974288344,
12.));
#219273=CARTESIAN_POINT('Ctrl Pts',(20.4843302955329,-9.7902391649866,12.));
#219274=CARTESIAN_POINT('Ctrl Pts',(20.4765353711585,-9.78535797314162,
12.));
#219275=CARTESIAN_POINT('Ctrl Pts',(20.4689199790668,-9.78062712373313,
12.));
#219276=CARTESIAN_POINT('Ctrl Pts',(20.4614885274973,-9.77604760815523,
12.));
#219277=CARTESIAN_POINT('Ctrl Pts',(20.4542455817527,-9.7716204510407,12.));
#219278=CARTESIAN_POINT('Ctrl Pts',(20.447195862298,-9.76734670980897,12.));
#219279=CARTESIAN_POINT('Ctrl Pts',(20.4403442329401,-9.76322747195502,
12.));
#219280=CARTESIAN_POINT('Ctrl Pts',(20.4336957355474,-9.7592638628993,12.));
#219281=CARTESIAN_POINT('Ctrl Pts',(20.4272556476629,-9.75545705902416,
12.));
#219282=CARTESIAN_POINT('Ctrl Pts',(20.4210295275818,-9.75180829786433,
12.));
#219283=CARTESIAN_POINT('Ctrl Pts',(20.4150232777393,-9.74831889242175,
12.));
#219284=CARTESIAN_POINT('Ctrl Pts',(20.4092430879861,-9.74499021838537,
12.));
#219285=CARTESIAN_POINT('Ctrl Pts',(20.4036953576549,-9.74182369656273,
12.));
#219286=CARTESIAN_POINT('Ctrl Pts',(20.3983866213331,-9.73882077613206,
12.));
#219287=CARTESIAN_POINT('Ctrl Pts',(20.3933234845646,-9.7359829201425,12.));
#219288=CARTESIAN_POINT('Ctrl Pts',(20.3885129129912,-9.73331167102812,
12.));
#219289=CARTESIAN_POINT('Ctrl Pts',(20.3839624556742,-9.73080870123726,
12.));
#219290=CARTESIAN_POINT('Ctrl Pts',(20.3796805893304,-9.72847589116533,
12.));
#219291=CARTESIAN_POINT('Ctrl Pts',(20.3756766651952,-9.72631531732871,
12.));
#219292=CARTESIAN_POINT('Ctrl Pts',(20.371960235676,-9.72432910043193,12.));
#219293=CARTESIAN_POINT('Ctrl Pts',(20.3685406190576,-9.72251930722504,
12.));
#219294=CARTESIAN_POINT('Ctrl Pts',(20.3654261611055,-9.72088778381102,
12.));
#219295=CARTESIAN_POINT('Ctrl Pts',(20.362625691398,-9.71943648548115,12.));
#219296=CARTESIAN_POINT('Ctrl Pts',(20.3601498764344,-9.71816778327999,
12.));
#219297=CARTESIAN_POINT('Ctrl Pts',(20.3580133103357,-9.71708493723062,
12.));
#219298=CARTESIAN_POINT('Ctrl Pts',(20.3562337557875,-9.71619192554147,
12.));
#219299=CARTESIAN_POINT('Ctrl Pts',(20.3548282742361,-9.71549257088175,
12.));
#219300=CARTESIAN_POINT('Ctrl Pts',(20.3538098605706,-9.71498978052101,
12.));
#219301=CARTESIAN_POINT('Ctrl Pts',(20.3533097561886,-9.71474590350792,
12.));
#219302=CARTESIAN_POINT('Ctrl Pts',(20.3531126095522,-9.71465227853122,
12.));
#219303=CARTESIAN_POINT('Ctrl Pts',(20.353060251684,-9.71462954053074,12.));
#219304=CARTESIAN_POINT('Ctrl Pts',(20.353053841303,-9.71462809124917,12.));
#219305=CARTESIAN_POINT('',(22.8400320311648,-12.4230808101438,0.));
#219306=CARTESIAN_POINT('Origin',(16.3449727195351,-13.9675290154577,0.));
#219307=CARTESIAN_POINT('',(17.1452095830632,-14.6513681262571,12.));
#219308=CARTESIAN_POINT('',(8.17248635976757,-6.98376450772884,12.));
#219309=CARTESIAN_POINT('',(17.1452095830632,-14.6513681262571,0.));
#219310=CARTESIAN_POINT('',(17.1452095830632,-14.6513681262571,0.));
#219311=CARTESIAN_POINT('',(8.17248635976757,-6.98376450772884,0.));
#219312=CARTESIAN_POINT('Ctrl Pts',(22.1787195904339,-13.5685075571671,
0.));
#219313=CARTESIAN_POINT('Ctrl Pts',(22.1787195904339,-13.5685075571671,
12.));
#219314=CARTESIAN_POINT('Ctrl Pts',(22.1730081264583,-13.5683460612913,
0.));
#219315=CARTESIAN_POINT('Ctrl Pts',(22.1730081264583,-13.5683460612913,
12.));
#219316=CARTESIAN_POINT('Ctrl Pts',(22.1615922804939,-13.5680170531724,
0.));
#219317=CARTESIAN_POINT('Ctrl Pts',(22.1615922804939,-13.5680170531724,
12.));
#219318=CARTESIAN_POINT('Ctrl Pts',(22.1444897575076,-13.5675054918922,
0.));
#219319=CARTESIAN_POINT('Ctrl Pts',(22.1444897575076,-13.5675054918922,
12.));
#219320=CARTESIAN_POINT('Ctrl Pts',(22.1217288871823,-13.5667873105179,
0.));
#219321=CARTESIAN_POINT('Ctrl Pts',(22.1217288871823,-13.5667873105179,
12.));
#219322=CARTESIAN_POINT('Ctrl Pts',(22.0933486464442,-13.5658294169106,
0.));
#219323=CARTESIAN_POINT('Ctrl Pts',(22.0933486464442,-13.5658294169106,
12.));
#219324=CARTESIAN_POINT('Ctrl Pts',(22.0650393089492,-13.5648113688895,
0.));
#219325=CARTESIAN_POINT('Ctrl Pts',(22.0650393089492,-13.5648113688895,
12.));
#219326=CARTESIAN_POINT('Ctrl Pts',(22.0368009736227,-13.5637332022393,
0.));
#219327=CARTESIAN_POINT('Ctrl Pts',(22.0368009736227,-13.5637332022393,
12.));
#219328=CARTESIAN_POINT('Ctrl Pts',(22.0086337943431,-13.5625949868313,
0.));
#219329=CARTESIAN_POINT('Ctrl Pts',(22.0086337943431,-13.5625949868313,
12.));
#219330=CARTESIAN_POINT('Ctrl Pts',(21.9805379899192,-13.5613968357589,
0.));
#219331=CARTESIAN_POINT('Ctrl Pts',(21.9805379899192,-13.5613968357589,
12.));
#219332=CARTESIAN_POINT('Ctrl Pts',(21.9525138592862,-13.5601389185315,
0.));
#219333=CARTESIAN_POINT('Ctrl Pts',(21.9525138592862,-13.5601389185315,
12.));
#219334=CARTESIAN_POINT('Ctrl Pts',(21.9245617765827,-13.5588214586672,
0.));
#219335=CARTESIAN_POINT('Ctrl Pts',(21.9245617765827,-13.5588214586672,
12.));
#219336=CARTESIAN_POINT('Ctrl Pts',(21.8966821688876,-13.5574447178485,
0.));
#219337=CARTESIAN_POINT('Ctrl Pts',(21.8966821688876,-13.5574447178485,
12.));
#219338=CARTESIAN_POINT('Ctrl Pts',(21.8688754989401,-13.5560089839426,
0.));
#219339=CARTESIAN_POINT('Ctrl Pts',(21.8688754989401,-13.5560089839426,
12.));
#219340=CARTESIAN_POINT('Ctrl Pts',(21.841142245609,-13.5545145573048,0.));
#219341=CARTESIAN_POINT('Ctrl Pts',(21.841142245609,-13.5545145573048,12.));
#219342=CARTESIAN_POINT('Ctrl Pts',(21.8134828857963,-13.5529617381569,
0.));
#219343=CARTESIAN_POINT('Ctrl Pts',(21.8134828857963,-13.5529617381569,
12.));
#219344=CARTESIAN_POINT('Ctrl Pts',(21.7858978745848,-13.5513508127232,
0.));
#219345=CARTESIAN_POINT('Ctrl Pts',(21.7858978745848,-13.5513508127232,
12.));
#219346=CARTESIAN_POINT('Ctrl Pts',(21.7583876294532,-13.5496820422186,
0.));
#219347=CARTESIAN_POINT('Ctrl Pts',(21.7583876294532,-13.5496820422186,
12.));
#219348=CARTESIAN_POINT('Ctrl Pts',(21.730952541226,-13.5479556704457,0.));
#219349=CARTESIAN_POINT('Ctrl Pts',(21.730952541226,-13.5479556704457,12.));
#219350=CARTESIAN_POINT('Ctrl Pts',(21.7035929822939,-13.546171929503,0.));
#219351=CARTESIAN_POINT('Ctrl Pts',(21.7035929822939,-13.546171929503,12.));
#219352=CARTESIAN_POINT('Ctrl Pts',(21.676309315769,-13.5443310461516,0.));
#219353=CARTESIAN_POINT('Ctrl Pts',(21.676309315769,-13.5443310461516,12.));
#219354=CARTESIAN_POINT('Ctrl Pts',(21.6491019044647,-13.5424332480698,
0.));
#219355=CARTESIAN_POINT('Ctrl Pts',(21.6491019044647,-13.5424332480698,
12.));
#219356=CARTESIAN_POINT('Ctrl Pts',(21.6219711193951,-13.5404787697798,
0.));
#219357=CARTESIAN_POINT('Ctrl Pts',(21.6219711193951,-13.5404787697798,
12.));
#219358=CARTESIAN_POINT('Ctrl Pts',(21.5949173499022,-13.5384678597206,
0.));
#219359=CARTESIAN_POINT('Ctrl Pts',(21.5949173499022,-13.5384678597206,
12.));
#219360=CARTESIAN_POINT('Ctrl Pts',(21.5679410019011,-13.5364007790292,
0.));
#219361=CARTESIAN_POINT('Ctrl Pts',(21.5679410019011,-13.5364007790292,
12.));
#219362=CARTESIAN_POINT('Ctrl Pts',(21.5410424932511,-13.5342777983225,
0.));
#219363=CARTESIAN_POINT('Ctrl Pts',(21.5410424932511,-13.5342777983225,
12.));
#219364=CARTESIAN_POINT('Ctrl Pts',(21.5142222501671,-13.5320991952145,
0.));
#219365=CARTESIAN_POINT('Ctrl Pts',(21.5142222501671,-13.5320991952145,
12.));
#219366=CARTESIAN_POINT('Ctrl Pts',(21.487480703047,-13.5298652514357,0.));
#219367=CARTESIAN_POINT('Ctrl Pts',(21.487480703047,-13.5298652514357,12.));
#219368=CARTESIAN_POINT('Ctrl Pts',(21.4608182828695,-13.5275762503553,
0.));
#219369=CARTESIAN_POINT('Ctrl Pts',(21.4608182828695,-13.5275762503553,
12.));
#219370=CARTESIAN_POINT('Ctrl Pts',(21.4342354165254,-13.5252324737795,
0.));
#219371=CARTESIAN_POINT('Ctrl Pts',(21.4342354165254,-13.5252324737795,
12.));
#219372=CARTESIAN_POINT('Ctrl Pts',(21.4077325259318,-13.5228342013508,
0.));
#219373=CARTESIAN_POINT('Ctrl Pts',(21.4077325259318,-13.5228342013508,
12.));
#219374=CARTESIAN_POINT('Ctrl Pts',(21.3813100304967,-13.5203817122497,
0.));
#219375=CARTESIAN_POINT('Ctrl Pts',(21.3813100304967,-13.5203817122497,
12.));
#219376=CARTESIAN_POINT('Ctrl Pts',(21.3549683486219,-13.5178752862461,
0.));
#219377=CARTESIAN_POINT('Ctrl Pts',(21.3549683486219,-13.5178752862461,
12.));
#219378=CARTESIAN_POINT('Ctrl Pts',(21.328707899634,-13.5153152050554,0.));
#219379=CARTESIAN_POINT('Ctrl Pts',(21.328707899634,-13.5153152050554,12.));
#219380=CARTESIAN_POINT('Ctrl Pts',(21.3025291054236,-13.5127017534972,
0.));
#219381=CARTESIAN_POINT('Ctrl Pts',(21.3025291054236,-13.5127017534972,
12.));
#219382=CARTESIAN_POINT('Ctrl Pts',(21.2764323924442,-13.5100352209207,
0.));
#219383=CARTESIAN_POINT('Ctrl Pts',(21.2764323924442,-13.5100352209207,
12.));
#219384=CARTESIAN_POINT('Ctrl Pts',(21.2504181927429,-13.5073159019454,
0.));
#219385=CARTESIAN_POINT('Ctrl Pts',(21.2504181927429,-13.5073159019454,
12.));
#219386=CARTESIAN_POINT('Ctrl Pts',(21.224486942933,-13.5045440957404,0.));
#219387=CARTESIAN_POINT('Ctrl Pts',(21.224486942933,-13.5045440957404,12.));
#219388=CARTESIAN_POINT('Ctrl Pts',(21.1986390835825,-13.5017201056088,
0.));
#219389=CARTESIAN_POINT('Ctrl Pts',(21.1986390835825,-13.5017201056088,
12.));
#219390=CARTESIAN_POINT('Ctrl Pts',(21.1728750584173,-13.4988442384491,
0.));
#219391=CARTESIAN_POINT('Ctrl Pts',(21.1728750584173,-13.4988442384491,
12.));
#219392=CARTESIAN_POINT('Ctrl Pts',(21.1471953136209,-13.4959168042934,
0.));
#219393=CARTESIAN_POINT('Ctrl Pts',(21.1471953136209,-13.4959168042934,
12.));
#219394=CARTESIAN_POINT('Ctrl Pts',(21.1216002970209,-13.4929381157778,
0.));
#219395=CARTESIAN_POINT('Ctrl Pts',(21.1216002970209,-13.4929381157778,
12.));
#219396=CARTESIAN_POINT('Ctrl Pts',(21.0960904575048,-13.4899084877718,
0.));
#219397=CARTESIAN_POINT('Ctrl Pts',(21.0960904575048,-13.4899084877718,
12.));
#219398=CARTESIAN_POINT('Ctrl Pts',(21.0706662455202,-13.4868282377192,
0.));
#219399=CARTESIAN_POINT('Ctrl Pts',(21.0706662455202,-13.4868282377192,
12.));
#219400=CARTESIAN_POINT('Ctrl Pts',(21.0453281134247,-13.4836976858912,
0.));
#219401=CARTESIAN_POINT('Ctrl Pts',(21.0453281134247,-13.4836976858912,
12.));
#219402=CARTESIAN_POINT('Ctrl Pts',(21.0200765158885,-13.4805171556822,
0.));
#219403=CARTESIAN_POINT('Ctrl Pts',(21.0200765158885,-13.4805171556822,
12.));
#219404=CARTESIAN_POINT('Ctrl Pts',(20.9949119102592,-13.4772869738879,
0.));
#219405=CARTESIAN_POINT('Ctrl Pts',(20.9949119102592,-13.4772869738879,
12.));
#219406=CARTESIAN_POINT('Ctrl Pts',(20.9698347569476,-13.4740074710087,
0.));
#219407=CARTESIAN_POINT('Ctrl Pts',(20.9698347569476,-13.4740074710087,
12.));
#219408=CARTESIAN_POINT('Ctrl Pts',(20.9448455197557,-13.4706789815166,
0.));
#219409=CARTESIAN_POINT('Ctrl Pts',(20.9448455197557,-13.4706789815166,
12.));
#219410=CARTESIAN_POINT('Ctrl Pts',(20.9199446657584,-13.4673018437718,
0.));
#219411=CARTESIAN_POINT('Ctrl Pts',(20.9199446657584,-13.4673018437718,
12.));
#219412=CARTESIAN_POINT('Ctrl Pts',(20.8951326652158,-13.4638763999725,
0.));
#219413=CARTESIAN_POINT('Ctrl Pts',(20.8951326652158,-13.4638763999725,
12.));
#219414=CARTESIAN_POINT('Ctrl Pts',(20.8704099914641,-13.4604029960983,
0.));
#219415=CARTESIAN_POINT('Ctrl Pts',(20.8704099914641,-13.4604029960983,
12.));
#219416=CARTESIAN_POINT('Ctrl Pts',(20.8457771208082,-13.4568819818631,
0.));
#219417=CARTESIAN_POINT('Ctrl Pts',(20.8457771208082,-13.4568819818631,
12.));
#219418=CARTESIAN_POINT('Ctrl Pts',(20.821234532398,-13.4533137106667,0.));
#219419=CARTESIAN_POINT('Ctrl Pts',(20.821234532398,-13.4533137106667,12.));
#219420=CARTESIAN_POINT('Ctrl Pts',(20.7967827081227,-13.4496985395637,
0.));
#219421=CARTESIAN_POINT('Ctrl Pts',(20.7967827081227,-13.4496985395637,
12.));
#219422=CARTESIAN_POINT('Ctrl Pts',(20.7724221327608,-13.4460368293688,
0.));
#219423=CARTESIAN_POINT('Ctrl Pts',(20.7724221327608,-13.4460368293688,
12.));
#219424=CARTESIAN_POINT('Ctrl Pts',(20.7481532941013,-13.4423289447561,
0.));
#219425=CARTESIAN_POINT('Ctrl Pts',(20.7481532941013,-13.4423289447561,
12.));
#219426=CARTESIAN_POINT('Ctrl Pts',(20.7239766830675,-13.4385752543663,
0.));
#219427=CARTESIAN_POINT('Ctrl Pts',(20.7239766830675,-13.4385752543663,
12.));
#219428=CARTESIAN_POINT('Ctrl Pts',(20.6998927938288,-13.4347761309154,
0.));
#219429=CARTESIAN_POINT('Ctrl Pts',(20.6998927938288,-13.4347761309154,
12.));
#219430=CARTESIAN_POINT('Ctrl Pts',(20.6759021239103,-13.4309319513119,
0.));
#219431=CARTESIAN_POINT('Ctrl Pts',(20.6759021239103,-13.4309319513119,
12.));
#219432=CARTESIAN_POINT('Ctrl Pts',(20.6520051742869,-13.4270430967651,
0.));
#219433=CARTESIAN_POINT('Ctrl Pts',(20.6520051742869,-13.4270430967651,
12.));
#219434=CARTESIAN_POINT('Ctrl Pts',(20.6282024494237,-13.4231099528179,
0.));
#219435=CARTESIAN_POINT('Ctrl Pts',(20.6282024494237,-13.4231099528179,
12.));
#219436=CARTESIAN_POINT('Ctrl Pts',(20.6044944573153,-13.4191329093933,
0.));
#219437=CARTESIAN_POINT('Ctrl Pts',(20.6044944573153,-13.4191329093933,
12.));
#219438=CARTESIAN_POINT('Ctrl Pts',(20.5808817095155,-13.4151123608411,
0.));
#219439=CARTESIAN_POINT('Ctrl Pts',(20.5808817095155,-13.4151123608411,
12.));
#219440=CARTESIAN_POINT('Ctrl Pts',(20.5573647211639,-13.4110487059912,
0.));
#219441=CARTESIAN_POINT('Ctrl Pts',(20.5573647211639,-13.4110487059912,
12.));
#219442=CARTESIAN_POINT('Ctrl Pts',(20.5339440109956,-13.4069423482076,
0.));
#219443=CARTESIAN_POINT('Ctrl Pts',(20.5339440109956,-13.4069423482076,
12.));
#219444=CARTESIAN_POINT('Ctrl Pts',(20.5106201013753,-13.4027936954529,
0.));
#219445=CARTESIAN_POINT('Ctrl Pts',(20.5106201013753,-13.4027936954529,
12.));
#219446=CARTESIAN_POINT('Ctrl Pts',(20.487393518404,-13.3986031603716,0.));
#219447=CARTESIAN_POINT('Ctrl Pts',(20.487393518404,-13.3986031603716,12.));
#219448=CARTESIAN_POINT('Ctrl Pts',(20.4642647920038,-13.3943711603739,
0.));
#219449=CARTESIAN_POINT('Ctrl Pts',(20.4642647920038,-13.3943711603739,
12.));
#219450=CARTESIAN_POINT('Ctrl Pts',(20.4412344560008,-13.3900981177255,
0.));
#219451=CARTESIAN_POINT('Ctrl Pts',(20.4412344560008,-13.3900981177255,
12.));
#219452=CARTESIAN_POINT('Ctrl Pts',(20.4183030482002,-13.3857844596387,
0.));
#219453=CARTESIAN_POINT('Ctrl Pts',(20.4183030482002,-13.3857844596387,
12.));
#219454=CARTESIAN_POINT('Ctrl Pts',(20.3954711104502,-13.3814306183719,
0.));
#219455=CARTESIAN_POINT('Ctrl Pts',(20.3954711104502,-13.3814306183719,
12.));
#219456=CARTESIAN_POINT('Ctrl Pts',(20.3727391887184,-13.3770370313188,
0.));
#219457=CARTESIAN_POINT('Ctrl Pts',(20.3727391887184,-13.3770370313188,
12.));
#219458=CARTESIAN_POINT('Ctrl Pts',(20.3501078331814,-13.3726041410867,
0.));
#219459=CARTESIAN_POINT('Ctrl Pts',(20.3501078331814,-13.3726041410867,
12.));
#219460=CARTESIAN_POINT('Ctrl Pts',(20.3275775983029,-13.3681323955826,
0.));
#219461=CARTESIAN_POINT('Ctrl Pts',(20.3275775983029,-13.3681323955826,
12.));
#219462=CARTESIAN_POINT('Ctrl Pts',(20.3051490429048,-13.3636222481016,
0.));
#219463=CARTESIAN_POINT('Ctrl Pts',(20.3051490429048,-13.3636222481016,
12.));
#219464=CARTESIAN_POINT('Ctrl Pts',(20.2828227302339,-13.3590741574195,
0.));
#219465=CARTESIAN_POINT('Ctrl Pts',(20.2828227302339,-13.3590741574195,
12.));
#219466=CARTESIAN_POINT('Ctrl Pts',(20.2605992280122,-13.3544885878889,
0.));
#219467=CARTESIAN_POINT('Ctrl Pts',(20.2605992280122,-13.3544885878889,
12.));
#219468=CARTESIAN_POINT('Ctrl Pts',(20.2384791085359,-13.3498660095386,
0.));
#219469=CARTESIAN_POINT('Ctrl Pts',(20.2384791085359,-13.3498660095386,
12.));
#219470=CARTESIAN_POINT('Ctrl Pts',(20.216462948786,-13.3452068981766,0.));
#219471=CARTESIAN_POINT('Ctrl Pts',(20.216462948786,-13.3452068981766,12.));
#219472=CARTESIAN_POINT('Ctrl Pts',(20.1945513305235,-13.3405117354971,
0.));
#219473=CARTESIAN_POINT('Ctrl Pts',(20.1945513305235,-13.3405117354971,
12.));
#219474=CARTESIAN_POINT('Ctrl Pts',(20.1727448403817,-13.3357810091903,
0.));
#219475=CARTESIAN_POINT('Ctrl Pts',(20.1727448403817,-13.3357810091903,
12.));
#219476=CARTESIAN_POINT('Ctrl Pts',(20.1510440699474,-13.3310152130564,
0.));
#219477=CARTESIAN_POINT('Ctrl Pts',(20.1510440699474,-13.3310152130564,
12.));
#219478=CARTESIAN_POINT('Ctrl Pts',(20.1294496158402,-13.3262148471226,
0.));
#219479=CARTESIAN_POINT('Ctrl Pts',(20.1294496158402,-13.3262148471226,
12.));
#219480=CARTESIAN_POINT('Ctrl Pts',(20.1079620798375,-13.3213804177587,
0.));
#219481=CARTESIAN_POINT('Ctrl Pts',(20.1079620798375,-13.3213804177587,
12.));
#219482=CARTESIAN_POINT('Ctrl Pts',(20.0865820689882,-13.3165124377963,
0.));
#219483=CARTESIAN_POINT('Ctrl Pts',(20.0865820689882,-13.3165124377963,
12.));
#219484=CARTESIAN_POINT('Ctrl Pts',(20.0653101957188,-13.3116114266515,
0.));
#219485=CARTESIAN_POINT('Ctrl Pts',(20.0653101957188,-13.3116114266515,
12.));
#219486=CARTESIAN_POINT('Ctrl Pts',(20.0441470779345,-13.3066779104515,
0.));
#219487=CARTESIAN_POINT('Ctrl Pts',(20.0441470779345,-13.3066779104515,
12.));
#219488=CARTESIAN_POINT('Ctrl Pts',(20.0230933391038,-13.3017124221637,
0.));
#219489=CARTESIAN_POINT('Ctrl Pts',(20.0230933391038,-13.3017124221637,
12.));
#219490=CARTESIAN_POINT('Ctrl Pts',(20.0021496083738,-13.2967155017306,
0.));
#219491=CARTESIAN_POINT('Ctrl Pts',(20.0021496083738,-13.2967155017306,
12.));
#219492=CARTESIAN_POINT('Ctrl Pts',(19.981316520717,-13.2916876962094,0.));
#219493=CARTESIAN_POINT('Ctrl Pts',(19.981316520717,-13.2916876962094,12.));
#219494=CARTESIAN_POINT('Ctrl Pts',(19.9605947170586,-13.286629559915,0.));
#219495=CARTESIAN_POINT('Ctrl Pts',(19.9605947170586,-13.286629559915,12.));
#219496=CARTESIAN_POINT('Ctrl Pts',(19.9399848444019,-13.2815416545663,
0.));
#219497=CARTESIAN_POINT('Ctrl Pts',(19.9399848444019,-13.2815416545663,
12.));
#219498=CARTESIAN_POINT('Ctrl Pts',(19.9194875559422,-13.2764245494357,
0.));
#219499=CARTESIAN_POINT('Ctrl Pts',(19.9194875559422,-13.2764245494357,
12.));
#219500=CARTESIAN_POINT('Ctrl Pts',(19.8991035111745,-13.271278821502,0.));
#219501=CARTESIAN_POINT('Ctrl Pts',(19.8991035111745,-13.271278821502,12.));
#219502=CARTESIAN_POINT('Ctrl Pts',(19.8788333760577,-13.2661050556132,
0.));
#219503=CARTESIAN_POINT('Ctrl Pts',(19.8788333760577,-13.2661050556132,
12.));
#219504=CARTESIAN_POINT('Ctrl Pts',(19.8586778231715,-13.2609038446529,
0.));
#219505=CARTESIAN_POINT('Ctrl Pts',(19.8586778231715,-13.2609038446529,
12.));
#219506=CARTESIAN_POINT('Ctrl Pts',(19.8386375318634,-13.2556757897086,
0.));
#219507=CARTESIAN_POINT('Ctrl Pts',(19.8386375318634,-13.2556757897086,
12.));
#219508=CARTESIAN_POINT('Ctrl Pts',(19.8187131883917,-13.2504215002457,
0.));
#219509=CARTESIAN_POINT('Ctrl Pts',(19.8187131883917,-13.2504215002457,
12.));
#219510=CARTESIAN_POINT('Ctrl Pts',(19.7989054860495,-13.2451415942805,
0.));
#219511=CARTESIAN_POINT('Ctrl Pts',(19.7989054860495,-13.2451415942805,
12.));
#219512=CARTESIAN_POINT('Ctrl Pts',(19.7792151253289,-13.2398366985675,
0.));
#219513=CARTESIAN_POINT('Ctrl Pts',(19.7792151253289,-13.2398366985675,
12.));
#219514=CARTESIAN_POINT('Ctrl Pts',(19.7596428141168,-13.2345074487963,
0.));
#219515=CARTESIAN_POINT('Ctrl Pts',(19.7596428141168,-13.2345074487963,
12.));
#219516=CARTESIAN_POINT('Ctrl Pts',(19.7401892678697,-13.2291544897899,
0.));
#219517=CARTESIAN_POINT('Ctrl Pts',(19.7401892678697,-13.2291544897899,
12.));
#219518=CARTESIAN_POINT('Ctrl Pts',(19.7208552097868,-13.2237784757065,
0.));
#219519=CARTESIAN_POINT('Ctrl Pts',(19.7208552097868,-13.2237784757065,
12.));
#219520=CARTESIAN_POINT('Ctrl Pts',(19.7016413709685,-13.2183800702436,
0.));
#219521=CARTESIAN_POINT('Ctrl Pts',(19.7016413709685,-13.2183800702436,
12.));
#219522=CARTESIAN_POINT('Ctrl Pts',(19.6825484905823,-13.2129599468485,
0.));
#219523=CARTESIAN_POINT('Ctrl Pts',(19.6825484905823,-13.2129599468485,
12.));
#219524=CARTESIAN_POINT('Ctrl Pts',(19.6635773160936,-13.2075187889529,
0.));
#219525=CARTESIAN_POINT('Ctrl Pts',(19.6635773160936,-13.2075187889529,
12.));
#219526=CARTESIAN_POINT('Ctrl Pts',(19.6447286034772,-13.2020572902065,
0.));
#219527=CARTESIAN_POINT('Ctrl Pts',(19.6447286034772,-13.2020572902065,
12.));
#219528=CARTESIAN_POINT('Ctrl Pts',(19.6260031174244,-13.1965761547151,
0.));
#219529=CARTESIAN_POINT('Ctrl Pts',(19.6260031174244,-13.1965761547151,
12.));
#219530=CARTESIAN_POINT('Ctrl Pts',(19.6074016315414,-13.1910760972814,
0.));
#219531=CARTESIAN_POINT('Ctrl Pts',(19.6074016315414,-13.1910760972814,
12.));
#219532=CARTESIAN_POINT('Ctrl Pts',(19.5889249285338,-13.1855578436471,
0.));
#219533=CARTESIAN_POINT('Ctrl Pts',(19.5889249285338,-13.1855578436471,
12.));
#219534=CARTESIAN_POINT('Ctrl Pts',(19.5705738004667,-13.1800221307673,
0.));
#219535=CARTESIAN_POINT('Ctrl Pts',(19.5705738004667,-13.1800221307673,
12.));
#219536=CARTESIAN_POINT('Ctrl Pts',(19.5523490490244,-13.1744697070911,
0.));
#219537=CARTESIAN_POINT('Ctrl Pts',(19.5523490490244,-13.1744697070911,
12.));
#219538=CARTESIAN_POINT('Ctrl Pts',(19.5342514857562,-13.168901332843,0.));
#219539=CARTESIAN_POINT('Ctrl Pts',(19.5342514857562,-13.168901332843,12.));
#219540=CARTESIAN_POINT('Ctrl Pts',(19.5162819323213,-13.1633177803101,
0.));
#219541=CARTESIAN_POINT('Ctrl Pts',(19.5162819323213,-13.1633177803101,
12.));
#219542=CARTESIAN_POINT('Ctrl Pts',(19.4984412207082,-13.1577198341245,
0.));
#219543=CARTESIAN_POINT('Ctrl Pts',(19.4984412207082,-13.1577198341245,
12.));
#219544=CARTESIAN_POINT('Ctrl Pts',(19.4807301935268,-13.1521082915853,
0.));
#219545=CARTESIAN_POINT('Ctrl Pts',(19.4807301935268,-13.1521082915853,
12.));
#219546=CARTESIAN_POINT('Ctrl Pts',(19.4631497043258,-13.1464839629971,
0.));
#219547=CARTESIAN_POINT('Ctrl Pts',(19.4631497043258,-13.1464839629971,
12.));
#219548=CARTESIAN_POINT('Ctrl Pts',(19.4457006178876,-13.1408476720061,
0.));
#219549=CARTESIAN_POINT('Ctrl Pts',(19.4457006178876,-13.1408476720061,
12.));
#219550=CARTESIAN_POINT('Ctrl Pts',(19.4283838105262,-13.1352002559438,
0.));
#219551=CARTESIAN_POINT('Ctrl Pts',(19.4283838105262,-13.1352002559438,
12.));
#219552=CARTESIAN_POINT('Ctrl Pts',(19.4112001703557,-13.1295425661634,
0.));
#219553=CARTESIAN_POINT('Ctrl Pts',(19.4112001703557,-13.1295425661634,
12.));
#219554=CARTESIAN_POINT('Ctrl Pts',(19.3941505976263,-13.1238754684177,
0.));
#219555=CARTESIAN_POINT('Ctrl Pts',(19.3941505976263,-13.1238754684177,
12.));
#219556=CARTESIAN_POINT('Ctrl Pts',(19.3772360051091,-13.118199843271,0.));
#219557=CARTESIAN_POINT('Ctrl Pts',(19.3772360051091,-13.118199843271,12.));
#219558=CARTESIAN_POINT('Ctrl Pts',(19.3604573184515,-13.1125165865022,
0.));
#219559=CARTESIAN_POINT('Ctrl Pts',(19.3604573184515,-13.1125165865022,
12.));
#219560=CARTESIAN_POINT('Ctrl Pts',(19.3438154765395,-13.1068266095186,
0.));
#219561=CARTESIAN_POINT('Ctrl Pts',(19.3438154765395,-13.1068266095186,
12.));
#219562=CARTESIAN_POINT('Ctrl Pts',(19.3273114318269,-13.1011308397591,
0.));
#219563=CARTESIAN_POINT('Ctrl Pts',(19.3273114318269,-13.1011308397591,
12.));
#219564=CARTESIAN_POINT('Ctrl Pts',(19.310946150736,-13.0954302211479,0.));
#219565=CARTESIAN_POINT('Ctrl Pts',(19.310946150736,-13.0954302211479,12.));
#219566=CARTESIAN_POINT('Ctrl Pts',(19.2947206141247,-13.0897257145969,
0.));
#219567=CARTESIAN_POINT('Ctrl Pts',(19.2947206141247,-13.0897257145969,
12.));
#219568=CARTESIAN_POINT('Ctrl Pts',(19.2786358177198,-13.0840182984949,
0.));
#219569=CARTESIAN_POINT('Ctrl Pts',(19.2786358177198,-13.0840182984949,
12.));
#219570=CARTESIAN_POINT('Ctrl Pts',(19.2626927725596,-13.0783089692118,
0.));
#219571=CARTESIAN_POINT('Ctrl Pts',(19.2626927725596,-13.0783089692118,
12.));
#219572=CARTESIAN_POINT('Ctrl Pts',(19.2468925053989,-13.0725987415859,
0.));
#219573=CARTESIAN_POINT('Ctrl Pts',(19.2468925053989,-13.0725987415859,
12.));
#219574=CARTESIAN_POINT('Ctrl Pts',(19.2312360592033,-13.0668886494795,
0.));
#219575=CARTESIAN_POINT('Ctrl Pts',(19.2312360592033,-13.0668886494795,
12.));
#219576=CARTESIAN_POINT('Ctrl Pts',(19.2157244937142,-13.0611797463915,
0.));
#219577=CARTESIAN_POINT('Ctrl Pts',(19.2157244937142,-13.0611797463915,
12.));
#219578=CARTESIAN_POINT('Ctrl Pts',(19.2003588859772,-13.0554731060538,
0.));
#219579=CARTESIAN_POINT('Ctrl Pts',(19.2003588859772,-13.0554731060538,
12.));
#219580=CARTESIAN_POINT('Ctrl Pts',(19.1851403308825,-13.0497698230441,
0.));
#219581=CARTESIAN_POINT('Ctrl Pts',(19.1851403308825,-13.0497698230441,
12.));
#219582=CARTESIAN_POINT('Ctrl Pts',(19.1700699416622,-13.0440710133772,
0.));
#219583=CARTESIAN_POINT('Ctrl Pts',(19.1700699416622,-13.0440710133772,
12.));
#219584=CARTESIAN_POINT('Ctrl Pts',(19.155148850523,-13.0383778152068,0.));
#219585=CARTESIAN_POINT('Ctrl Pts',(19.155148850523,-13.0383778152068,12.));
#219586=CARTESIAN_POINT('Ctrl Pts',(19.1403782093386,-13.0326913895838,
0.));
#219587=CARTESIAN_POINT('Ctrl Pts',(19.1403782093386,-13.0326913895838,
12.));
#219588=CARTESIAN_POINT('Ctrl Pts',(19.1257591903099,-13.0270129211976,
0.));
#219589=CARTESIAN_POINT('Ctrl Pts',(19.1257591903099,-13.0270129211976,
12.));
#219590=CARTESIAN_POINT('Ctrl Pts',(19.111292986631,-13.0213436191328,0.));
#219591=CARTESIAN_POINT('Ctrl Pts',(19.111292986631,-13.0213436191328,12.));
#219592=CARTESIAN_POINT('Ctrl Pts',(19.0969808131228,-13.0156847176097,
0.));
#219593=CARTESIAN_POINT('Ctrl Pts',(19.0969808131228,-13.0156847176097,
12.));
#219594=CARTESIAN_POINT('Ctrl Pts',(19.0828239070484,-13.0100374768788,
0.));
#219595=CARTESIAN_POINT('Ctrl Pts',(19.0828239070484,-13.0100374768788,
12.));
#219596=CARTESIAN_POINT('Ctrl Pts',(19.0688235289437,-13.0044031841382,
0.));
#219597=CARTESIAN_POINT('Ctrl Pts',(19.0688235289437,-13.0044031841382,
12.));
#219598=CARTESIAN_POINT('Ctrl Pts',(19.0549809634354,-12.9987831544502,
0.));
#219599=CARTESIAN_POINT('Ctrl Pts',(19.0549809634354,-12.9987831544502,
12.));
#219600=CARTESIAN_POINT('Ctrl Pts',(19.0412975200398,-12.9931787316514,
0.));
#219601=CARTESIAN_POINT('Ctrl Pts',(19.0412975200398,-12.9931787316514,
12.));
#219602=CARTESIAN_POINT('Ctrl Pts',(19.0277745339908,-12.9875912893003,
0.));
#219603=CARTESIAN_POINT('Ctrl Pts',(19.0277745339908,-12.9875912893003,
12.));
#219604=CARTESIAN_POINT('Ctrl Pts',(19.014413367335,-12.9820222318716,0.));
#219605=CARTESIAN_POINT('Ctrl Pts',(19.014413367335,-12.9820222318716,12.));
#219606=CARTESIAN_POINT('Ctrl Pts',(19.0012154099792,-12.9764729959206,
0.));
#219607=CARTESIAN_POINT('Ctrl Pts',(19.0012154099792,-12.9764729959206,
12.));
#219608=CARTESIAN_POINT('Ctrl Pts',(18.9881820807585,-12.9709450512747,
0.));
#219609=CARTESIAN_POINT('Ctrl Pts',(18.9881820807585,-12.9709450512747,
12.));
#219610=CARTESIAN_POINT('Ctrl Pts',(18.9753148284473,-12.9654399021868,
0.));
#219611=CARTESIAN_POINT('Ctrl Pts',(18.9753148284473,-12.9654399021868,
12.));
#219612=CARTESIAN_POINT('Ctrl Pts',(18.9626151329226,-12.9599590886318,
0.));
#219613=CARTESIAN_POINT('Ctrl Pts',(18.9626151329226,-12.9599590886318,
12.));
#219614=CARTESIAN_POINT('Ctrl Pts',(18.9500845064714,-12.9545041877377,
0.));
#219615=CARTESIAN_POINT('Ctrl Pts',(18.9500845064714,-12.9545041877377,
12.));
#219616=CARTESIAN_POINT('Ctrl Pts',(18.9377244950435,-12.9490768151821,
0.));
#219617=CARTESIAN_POINT('Ctrl Pts',(18.9377244950435,-12.9490768151821,
12.));
#219618=CARTESIAN_POINT('Ctrl Pts',(18.9255366795196,-12.9436786266106,
0.));
#219619=CARTESIAN_POINT('Ctrl Pts',(18.9255366795196,-12.9436786266106,
12.));
#219620=CARTESIAN_POINT('Ctrl Pts',(18.9135226769466,-12.9383113190375,
0.));
#219621=CARTESIAN_POINT('Ctrl Pts',(18.9135226769466,-12.9383113190375,
12.));
#219622=CARTESIAN_POINT('Ctrl Pts',(18.9016841423402,-12.9329766328184,
0.));
#219623=CARTESIAN_POINT('Ctrl Pts',(18.9016841423402,-12.9329766328184,
12.));
#219624=CARTESIAN_POINT('Ctrl Pts',(18.8900227704888,-12.9276763536372,
0.));
#219625=CARTESIAN_POINT('Ctrl Pts',(18.8900227704888,-12.9276763536372,
12.));
#219626=CARTESIAN_POINT('Ctrl Pts',(18.8785402977528,-12.9224123144982,
0.));
#219627=CARTESIAN_POINT('Ctrl Pts',(18.8785402977528,-12.9224123144982,
12.));
#219628=CARTESIAN_POINT('Ctrl Pts',(18.8672385038328,-12.9171863977047,
0.));
#219629=CARTESIAN_POINT('Ctrl Pts',(18.8672385038328,-12.9171863977047,
12.));
#219630=CARTESIAN_POINT('Ctrl Pts',(18.8561192136201,-12.9120005369066,
0.));
#219631=CARTESIAN_POINT('Ctrl Pts',(18.8561192136201,-12.9120005369066,
12.));
#219632=CARTESIAN_POINT('Ctrl Pts',(18.8451842990986,-12.9068567191856,
0.));
#219633=CARTESIAN_POINT('Ctrl Pts',(18.8451842990986,-12.9068567191856,
12.));
#219634=CARTESIAN_POINT('Ctrl Pts',(18.834435681259,-12.9017569871738,0.));
#219635=CARTESIAN_POINT('Ctrl Pts',(18.834435681259,-12.9017569871738,12.));
#219636=CARTESIAN_POINT('Ctrl Pts',(18.8238753319124,-12.8967034410752,
0.));
#219637=CARTESIAN_POINT('Ctrl Pts',(18.8238753319124,-12.8967034410752,
12.));
#219638=CARTESIAN_POINT('Ctrl Pts',(18.8135052757815,-12.8916982409931,
0.));
#219639=CARTESIAN_POINT('Ctrl Pts',(18.8135052757815,-12.8916982409931,
12.));
#219640=CARTESIAN_POINT('Ctrl Pts',(18.8033275941939,-12.8867436109543,
0.));
#219641=CARTESIAN_POINT('Ctrl Pts',(18.8033275941939,-12.8867436109543,
12.));
#219642=CARTESIAN_POINT('Ctrl Pts',(18.7933444285867,-12.8818418427474,
0.));
#219643=CARTESIAN_POINT('Ctrl Pts',(18.7933444285867,-12.8818418427474,
12.));
#219644=CARTESIAN_POINT('Ctrl Pts',(18.7835579840481,-12.8769952998097,
0.));
#219645=CARTESIAN_POINT('Ctrl Pts',(18.7835579840481,-12.8769952998097,
12.));
#219646=CARTESIAN_POINT('Ctrl Pts',(18.7739705329028,-12.8722064211814,
0.));
#219647=CARTESIAN_POINT('Ctrl Pts',(18.7739705329028,-12.8722064211814,
12.));
#219648=CARTESIAN_POINT('Ctrl Pts',(18.7645844169568,-12.8674777239656,
0.));
#219649=CARTESIAN_POINT('Ctrl Pts',(18.7645844169568,-12.8674777239656,
12.));
#219650=CARTESIAN_POINT('Ctrl Pts',(18.7554020493888,-12.8628118054172,
0.));
#219651=CARTESIAN_POINT('Ctrl Pts',(18.7554020493888,-12.8628118054172,
12.));
#219652=CARTESIAN_POINT('Ctrl Pts',(18.7464259171248,-12.8582113455644,
0.));
#219653=CARTESIAN_POINT('Ctrl Pts',(18.7464259171248,-12.8582113455644,
12.));
#219654=CARTESIAN_POINT('Ctrl Pts',(18.7376585820851,-12.8536791086315,
0.));
#219655=CARTESIAN_POINT('Ctrl Pts',(18.7376585820851,-12.8536791086315,
12.));
#219656=CARTESIAN_POINT('Ctrl Pts',(18.7291026886552,-12.849217951159,0.));
#219657=CARTESIAN_POINT('Ctrl Pts',(18.7291026886552,-12.849217951159,12.));
#219658=CARTESIAN_POINT('Ctrl Pts',(18.7207609737701,-12.8448308329494,
0.));
#219659=CARTESIAN_POINT('Ctrl Pts',(18.7207609737701,-12.8448308329494,
12.));
#219660=CARTESIAN_POINT('Ctrl Pts',(18.7126362754446,-12.8405208263432,
0.));
#219661=CARTESIAN_POINT('Ctrl Pts',(18.7126362754446,-12.8405208263432,
12.));
#219662=CARTESIAN_POINT('Ctrl Pts',(18.7047315436296,-12.8362911280362,
0.));
#219663=CARTESIAN_POINT('Ctrl Pts',(18.7047315436296,-12.8362911280362,
12.));
#219664=CARTESIAN_POINT('Ctrl Pts',(18.6970498410173,-12.832145059979,0.));
#219665=CARTESIAN_POINT('Ctrl Pts',(18.6970498410173,-12.832145059979,12.));
#219666=CARTESIAN_POINT('Ctrl Pts',(18.6895943376172,-12.8280860635231,
0.));
#219667=CARTESIAN_POINT('Ctrl Pts',(18.6895943376172,-12.8280860635231,
12.));
#219668=CARTESIAN_POINT('Ctrl Pts',(18.6823683094139,-12.8241176980016,
0.));
#219669=CARTESIAN_POINT('Ctrl Pts',(18.6823683094139,-12.8241176980016,
12.));
#219670=CARTESIAN_POINT('Ctrl Pts',(18.6753751301091,-12.8202436318473,
0.));
#219671=CARTESIAN_POINT('Ctrl Pts',(18.6753751301091,-12.8202436318473,
12.));
#219672=CARTESIAN_POINT('Ctrl Pts',(18.6686182952798,-12.8164676687361,
0.));
#219673=CARTESIAN_POINT('Ctrl Pts',(18.6686182952798,-12.8164676687361,
12.));
#219674=CARTESIAN_POINT('Ctrl Pts',(18.6621014624746,-12.8127937909632,
0.));
#219675=CARTESIAN_POINT('Ctrl Pts',(18.6621014624746,-12.8127937909632,
12.));
#219676=CARTESIAN_POINT('Ctrl Pts',(18.6558284825772,-12.8092261933858,
0.));
#219677=CARTESIAN_POINT('Ctrl Pts',(18.6558284825772,-12.8092261933858,
12.));
#219678=CARTESIAN_POINT('Ctrl Pts',(18.6498034438986,-12.805769331162,0.));
#219679=CARTESIAN_POINT('Ctrl Pts',(18.6498034438986,-12.805769331162,12.));
#219680=CARTESIAN_POINT('Ctrl Pts',(18.6440306327457,-12.8024278770153,
0.));
#219681=CARTESIAN_POINT('Ctrl Pts',(18.6440306327457,-12.8024278770153,
12.));
#219682=CARTESIAN_POINT('Ctrl Pts',(18.63851447924,-12.7992066625264,0.));
#219683=CARTESIAN_POINT('Ctrl Pts',(18.63851447924,-12.7992066625264,12.));
#219684=CARTESIAN_POINT('Ctrl Pts',(18.6332595057005,-12.7961106222251,
0.));
#219685=CARTESIAN_POINT('Ctrl Pts',(18.6332595057005,-12.7961106222251,
12.));
#219686=CARTESIAN_POINT('Ctrl Pts',(18.6282702819371,-12.7931447451556,
0.));
#219687=CARTESIAN_POINT('Ctrl Pts',(18.6282702819371,-12.7931447451556,
12.));
#219688=CARTESIAN_POINT('Ctrl Pts',(18.6235516265575,-12.7903142925234,
0.));
#219689=CARTESIAN_POINT('Ctrl Pts',(18.6235516265575,-12.7903142925234,
12.));
#219690=CARTESIAN_POINT('Ctrl Pts',(18.6191087624752,-12.7876249657834,
0.));
#219691=CARTESIAN_POINT('Ctrl Pts',(18.6191087624752,-12.7876249657834,
12.));
#219692=CARTESIAN_POINT('Ctrl Pts',(18.6149475565189,-12.78508316579,0.));
#219693=CARTESIAN_POINT('Ctrl Pts',(18.6149475565189,-12.78508316579,12.));
#219694=CARTESIAN_POINT('Ctrl Pts',(18.611074482622,-12.7826959526924,0.));
#219695=CARTESIAN_POINT('Ctrl Pts',(18.611074482622,-12.7826959526924,12.));
#219696=CARTESIAN_POINT('Ctrl Pts',(18.6074961535723,-12.7804705387658,
0.));
#219697=CARTESIAN_POINT('Ctrl Pts',(18.6074961535723,-12.7804705387658,
12.));
#219698=CARTESIAN_POINT('Ctrl Pts',(18.6042190183703,-12.7784139605067,
0.));
#219699=CARTESIAN_POINT('Ctrl Pts',(18.6042190183703,-12.7784139605067,
12.));
#219700=CARTESIAN_POINT('Ctrl Pts',(18.6012488486708,-12.7765325225082,
0.));
#219701=CARTESIAN_POINT('Ctrl Pts',(18.6012488486708,-12.7765325225082,
12.));
#219702=CARTESIAN_POINT('Ctrl Pts',(18.5985917525949,-12.7748328937639,
0.));
#219703=CARTESIAN_POINT('Ctrl Pts',(18.5985917525949,-12.7748328937639,
12.));
#219704=CARTESIAN_POINT('Ctrl Pts',(18.5962551167772,-12.7733231262107,
0.));
#219705=CARTESIAN_POINT('Ctrl Pts',(18.5962551167772,-12.7733231262107,
12.));
#219706=CARTESIAN_POINT('Ctrl Pts',(18.5942490615409,-12.7720142287169,
0.));
#219707=CARTESIAN_POINT('Ctrl Pts',(18.5942490615409,-12.7720142287169,
12.));
#219708=CARTESIAN_POINT('Ctrl Pts',(18.5925859134582,-12.7709195951153,
0.));
#219709=CARTESIAN_POINT('Ctrl Pts',(18.5925859134582,-12.7709195951153,
12.));
#219710=CARTESIAN_POINT('Ctrl Pts',(18.5912775137806,-12.7700520897174,
0.));
#219711=CARTESIAN_POINT('Ctrl Pts',(18.5912775137806,-12.7700520897174,
12.));
#219712=CARTESIAN_POINT('Ctrl Pts',(18.590332877722,-12.7694215127923,0.));
#219713=CARTESIAN_POINT('Ctrl Pts',(18.590332877722,-12.7694215127923,12.));
#219714=CARTESIAN_POINT('Ctrl Pts',(18.589871621842,-12.7691103481996,0.));
#219715=CARTESIAN_POINT('Ctrl Pts',(18.589871621842,-12.7691103481996,12.));
#219716=CARTESIAN_POINT('Ctrl Pts',(18.5896919669158,-12.7689864266924,
0.));
#219717=CARTESIAN_POINT('Ctrl Pts',(18.5896919669158,-12.7689864266924,
12.));
#219718=CARTESIAN_POINT('Ctrl Pts',(18.5896460962961,-12.7689524524484,
0.));
#219719=CARTESIAN_POINT('Ctrl Pts',(18.5896460962961,-12.7689524524484,
12.));
#219720=CARTESIAN_POINT('Ctrl Pts',(18.5896416359912,-12.7689476255363,
0.));
#219721=CARTESIAN_POINT('Ctrl Pts',(18.5896416359912,-12.7689476255363,
12.));
#219722=CARTESIAN_POINT('',(22.1787195904339,-13.5685075571671,0.));
#219723=CARTESIAN_POINT('Ctrl Pts',(22.1787195904339,-13.5685075571671,
0.));
#219724=CARTESIAN_POINT('Ctrl Pts',(22.1730081264583,-13.5683460612913,
0.));
#219725=CARTESIAN_POINT('Ctrl Pts',(22.1615922804939,-13.5680170531724,
0.));
#219726=CARTESIAN_POINT('Ctrl Pts',(22.1444897575076,-13.5675054918922,
0.));
#219727=CARTESIAN_POINT('Ctrl Pts',(22.1217288871823,-13.5667873105179,
0.));
#219728=CARTESIAN_POINT('Ctrl Pts',(22.0933486464442,-13.5658294169106,
0.));
#219729=CARTESIAN_POINT('Ctrl Pts',(22.0650393089492,-13.5648113688895,
0.));
#219730=CARTESIAN_POINT('Ctrl Pts',(22.0368009736227,-13.5637332022393,
0.));
#219731=CARTESIAN_POINT('Ctrl Pts',(22.0086337943431,-13.5625949868313,
0.));
#219732=CARTESIAN_POINT('Ctrl Pts',(21.9805379899192,-13.5613968357589,
0.));
#219733=CARTESIAN_POINT('Ctrl Pts',(21.9525138592862,-13.5601389185315,
0.));
#219734=CARTESIAN_POINT('Ctrl Pts',(21.9245617765827,-13.5588214586672,
0.));
#219735=CARTESIAN_POINT('Ctrl Pts',(21.8966821688876,-13.5574447178485,
0.));
#219736=CARTESIAN_POINT('Ctrl Pts',(21.8688754989401,-13.5560089839426,
0.));
#219737=CARTESIAN_POINT('Ctrl Pts',(21.841142245609,-13.5545145573048,0.));
#219738=CARTESIAN_POINT('Ctrl Pts',(21.8134828857963,-13.5529617381569,
0.));
#219739=CARTESIAN_POINT('Ctrl Pts',(21.7858978745848,-13.5513508127232,
0.));
#219740=CARTESIAN_POINT('Ctrl Pts',(21.7583876294532,-13.5496820422186,
0.));
#219741=CARTESIAN_POINT('Ctrl Pts',(21.730952541226,-13.5479556704457,0.));
#219742=CARTESIAN_POINT('Ctrl Pts',(21.7035929822939,-13.546171929503,0.));
#219743=CARTESIAN_POINT('Ctrl Pts',(21.676309315769,-13.5443310461516,0.));
#219744=CARTESIAN_POINT('Ctrl Pts',(21.6491019044647,-13.5424332480698,
0.));
#219745=CARTESIAN_POINT('Ctrl Pts',(21.6219711193951,-13.5404787697798,
0.));
#219746=CARTESIAN_POINT('Ctrl Pts',(21.5949173499022,-13.5384678597206,
0.));
#219747=CARTESIAN_POINT('Ctrl Pts',(21.5679410019011,-13.5364007790292,
0.));
#219748=CARTESIAN_POINT('Ctrl Pts',(21.5410424932511,-13.5342777983225,
0.));
#219749=CARTESIAN_POINT('Ctrl Pts',(21.5142222501671,-13.5320991952145,
0.));
#219750=CARTESIAN_POINT('Ctrl Pts',(21.487480703047,-13.5298652514357,0.));
#219751=CARTESIAN_POINT('Ctrl Pts',(21.4608182828695,-13.5275762503553,
0.));
#219752=CARTESIAN_POINT('Ctrl Pts',(21.4342354165254,-13.5252324737795,
0.));
#219753=CARTESIAN_POINT('Ctrl Pts',(21.4077325259318,-13.5228342013508,
0.));
#219754=CARTESIAN_POINT('Ctrl Pts',(21.3813100304967,-13.5203817122497,
0.));
#219755=CARTESIAN_POINT('Ctrl Pts',(21.3549683486219,-13.5178752862461,
0.));
#219756=CARTESIAN_POINT('Ctrl Pts',(21.328707899634,-13.5153152050554,0.));
#219757=CARTESIAN_POINT('Ctrl Pts',(21.3025291054236,-13.5127017534972,
0.));
#219758=CARTESIAN_POINT('Ctrl Pts',(21.2764323924442,-13.5100352209207,
0.));
#219759=CARTESIAN_POINT('Ctrl Pts',(21.2504181927429,-13.5073159019454,
0.));
#219760=CARTESIAN_POINT('Ctrl Pts',(21.224486942933,-13.5045440957404,0.));
#219761=CARTESIAN_POINT('Ctrl Pts',(21.1986390835825,-13.5017201056088,
0.));
#219762=CARTESIAN_POINT('Ctrl Pts',(21.1728750584173,-13.4988442384491,
0.));
#219763=CARTESIAN_POINT('Ctrl Pts',(21.1471953136209,-13.4959168042934,
0.));
#219764=CARTESIAN_POINT('Ctrl Pts',(21.1216002970209,-13.4929381157778,
0.));
#219765=CARTESIAN_POINT('Ctrl Pts',(21.0960904575048,-13.4899084877718,
0.));
#219766=CARTESIAN_POINT('Ctrl Pts',(21.0706662455202,-13.4868282377192,
0.));
#219767=CARTESIAN_POINT('Ctrl Pts',(21.0453281134247,-13.4836976858912,
0.));
#219768=CARTESIAN_POINT('Ctrl Pts',(21.0200765158885,-13.4805171556822,
0.));
#219769=CARTESIAN_POINT('Ctrl Pts',(20.9949119102592,-13.4772869738879,
0.));
#219770=CARTESIAN_POINT('Ctrl Pts',(20.9698347569476,-13.4740074710087,
0.));
#219771=CARTESIAN_POINT('Ctrl Pts',(20.9448455197557,-13.4706789815166,
0.));
#219772=CARTESIAN_POINT('Ctrl Pts',(20.9199446657584,-13.4673018437718,
0.));
#219773=CARTESIAN_POINT('Ctrl Pts',(20.8951326652158,-13.4638763999725,
0.));
#219774=CARTESIAN_POINT('Ctrl Pts',(20.8704099914641,-13.4604029960983,
0.));
#219775=CARTESIAN_POINT('Ctrl Pts',(20.8457771208082,-13.4568819818631,
0.));
#219776=CARTESIAN_POINT('Ctrl Pts',(20.821234532398,-13.4533137106667,0.));
#219777=CARTESIAN_POINT('Ctrl Pts',(20.7967827081227,-13.4496985395637,
0.));
#219778=CARTESIAN_POINT('Ctrl Pts',(20.7724221327608,-13.4460368293688,
0.));
#219779=CARTESIAN_POINT('Ctrl Pts',(20.7481532941013,-13.4423289447561,
0.));
#219780=CARTESIAN_POINT('Ctrl Pts',(20.7239766830675,-13.4385752543663,
0.));
#219781=CARTESIAN_POINT('Ctrl Pts',(20.6998927938288,-13.4347761309154,
0.));
#219782=CARTESIAN_POINT('Ctrl Pts',(20.6759021239103,-13.4309319513119,
0.));
#219783=CARTESIAN_POINT('Ctrl Pts',(20.6520051742869,-13.4270430967651,
0.));
#219784=CARTESIAN_POINT('Ctrl Pts',(20.6282024494237,-13.4231099528179,
0.));
#219785=CARTESIAN_POINT('Ctrl Pts',(20.6044944573153,-13.4191329093933,
0.));
#219786=CARTESIAN_POINT('Ctrl Pts',(20.5808817095155,-13.4151123608411,
0.));
#219787=CARTESIAN_POINT('Ctrl Pts',(20.5573647211639,-13.4110487059912,
0.));
#219788=CARTESIAN_POINT('Ctrl Pts',(20.5339440109956,-13.4069423482076,
0.));
#219789=CARTESIAN_POINT('Ctrl Pts',(20.5106201013753,-13.4027936954529,
0.));
#219790=CARTESIAN_POINT('Ctrl Pts',(20.487393518404,-13.3986031603716,0.));
#219791=CARTESIAN_POINT('Ctrl Pts',(20.4642647920038,-13.3943711603739,
0.));
#219792=CARTESIAN_POINT('Ctrl Pts',(20.4412344560008,-13.3900981177255,
0.));
#219793=CARTESIAN_POINT('Ctrl Pts',(20.4183030482002,-13.3857844596387,
0.));
#219794=CARTESIAN_POINT('Ctrl Pts',(20.3954711104502,-13.3814306183719,
0.));
#219795=CARTESIAN_POINT('Ctrl Pts',(20.3727391887184,-13.3770370313188,
0.));
#219796=CARTESIAN_POINT('Ctrl Pts',(20.3501078331814,-13.3726041410867,
0.));
#219797=CARTESIAN_POINT('Ctrl Pts',(20.3275775983029,-13.3681323955826,
0.));
#219798=CARTESIAN_POINT('Ctrl Pts',(20.3051490429048,-13.3636222481016,
0.));
#219799=CARTESIAN_POINT('Ctrl Pts',(20.2828227302339,-13.3590741574195,
0.));
#219800=CARTESIAN_POINT('Ctrl Pts',(20.2605992280122,-13.3544885878889,
0.));
#219801=CARTESIAN_POINT('Ctrl Pts',(20.2384791085359,-13.3498660095386,
0.));
#219802=CARTESIAN_POINT('Ctrl Pts',(20.216462948786,-13.3452068981766,0.));
#219803=CARTESIAN_POINT('Ctrl Pts',(20.1945513305235,-13.3405117354971,
0.));
#219804=CARTESIAN_POINT('Ctrl Pts',(20.1727448403817,-13.3357810091903,
0.));
#219805=CARTESIAN_POINT('Ctrl Pts',(20.1510440699474,-13.3310152130564,
0.));
#219806=CARTESIAN_POINT('Ctrl Pts',(20.1294496158402,-13.3262148471226,
0.));
#219807=CARTESIAN_POINT('Ctrl Pts',(20.1079620798375,-13.3213804177587,
0.));
#219808=CARTESIAN_POINT('Ctrl Pts',(20.0865820689882,-13.3165124377963,
0.));
#219809=CARTESIAN_POINT('Ctrl Pts',(20.0653101957188,-13.3116114266515,
0.));
#219810=CARTESIAN_POINT('Ctrl Pts',(20.0441470779345,-13.3066779104515,
0.));
#219811=CARTESIAN_POINT('Ctrl Pts',(20.0230933391038,-13.3017124221637,
0.));
#219812=CARTESIAN_POINT('Ctrl Pts',(20.0021496083738,-13.2967155017306,
0.));
#219813=CARTESIAN_POINT('Ctrl Pts',(19.981316520717,-13.2916876962094,0.));
#219814=CARTESIAN_POINT('Ctrl Pts',(19.9605947170586,-13.286629559915,0.));
#219815=CARTESIAN_POINT('Ctrl Pts',(19.9399848444019,-13.2815416545663,
0.));
#219816=CARTESIAN_POINT('Ctrl Pts',(19.9194875559422,-13.2764245494357,
0.));
#219817=CARTESIAN_POINT('Ctrl Pts',(19.8991035111745,-13.271278821502,0.));
#219818=CARTESIAN_POINT('Ctrl Pts',(19.8788333760577,-13.2661050556132,
0.));
#219819=CARTESIAN_POINT('Ctrl Pts',(19.8586778231715,-13.2609038446529,
0.));
#219820=CARTESIAN_POINT('Ctrl Pts',(19.8386375318634,-13.2556757897086,
0.));
#219821=CARTESIAN_POINT('Ctrl Pts',(19.8187131883917,-13.2504215002457,
0.));
#219822=CARTESIAN_POINT('Ctrl Pts',(19.7989054860495,-13.2451415942805,
0.));
#219823=CARTESIAN_POINT('Ctrl Pts',(19.7792151253289,-13.2398366985675,
0.));
#219824=CARTESIAN_POINT('Ctrl Pts',(19.7596428141168,-13.2345074487963,
0.));
#219825=CARTESIAN_POINT('Ctrl Pts',(19.7401892678697,-13.2291544897899,
0.));
#219826=CARTESIAN_POINT('Ctrl Pts',(19.7208552097868,-13.2237784757065,
0.));
#219827=CARTESIAN_POINT('Ctrl Pts',(19.7016413709685,-13.2183800702436,
0.));
#219828=CARTESIAN_POINT('Ctrl Pts',(19.6825484905823,-13.2129599468485,
0.));
#219829=CARTESIAN_POINT('Ctrl Pts',(19.6635773160936,-13.2075187889529,
0.));
#219830=CARTESIAN_POINT('Ctrl Pts',(19.6447286034772,-13.2020572902065,
0.));
#219831=CARTESIAN_POINT('Ctrl Pts',(19.6260031174244,-13.1965761547151,
0.));
#219832=CARTESIAN_POINT('Ctrl Pts',(19.6074016315414,-13.1910760972814,
0.));
#219833=CARTESIAN_POINT('Ctrl Pts',(19.5889249285338,-13.1855578436471,
0.));
#219834=CARTESIAN_POINT('Ctrl Pts',(19.5705738004667,-13.1800221307673,
0.));
#219835=CARTESIAN_POINT('Ctrl Pts',(19.5523490490244,-13.1744697070911,
0.));
#219836=CARTESIAN_POINT('Ctrl Pts',(19.5342514857562,-13.168901332843,0.));
#219837=CARTESIAN_POINT('Ctrl Pts',(19.5162819323213,-13.1633177803101,
0.));
#219838=CARTESIAN_POINT('Ctrl Pts',(19.4984412207082,-13.1577198341245,
0.));
#219839=CARTESIAN_POINT('Ctrl Pts',(19.4807301935268,-13.1521082915853,
0.));
#219840=CARTESIAN_POINT('Ctrl Pts',(19.4631497043258,-13.1464839629971,
0.));
#219841=CARTESIAN_POINT('Ctrl Pts',(19.4457006178876,-13.1408476720061,
0.));
#219842=CARTESIAN_POINT('Ctrl Pts',(19.4283838105262,-13.1352002559438,
0.));
#219843=CARTESIAN_POINT('Ctrl Pts',(19.4112001703557,-13.1295425661634,
0.));
#219844=CARTESIAN_POINT('Ctrl Pts',(19.3941505976263,-13.1238754684177,
0.));
#219845=CARTESIAN_POINT('Ctrl Pts',(19.3772360051091,-13.118199843271,0.));
#219846=CARTESIAN_POINT('Ctrl Pts',(19.3604573184515,-13.1125165865022,
0.));
#219847=CARTESIAN_POINT('Ctrl Pts',(19.3438154765395,-13.1068266095186,
0.));
#219848=CARTESIAN_POINT('Ctrl Pts',(19.3273114318269,-13.1011308397591,
0.));
#219849=CARTESIAN_POINT('Ctrl Pts',(19.310946150736,-13.0954302211479,0.));
#219850=CARTESIAN_POINT('Ctrl Pts',(19.2947206141247,-13.0897257145969,
0.));
#219851=CARTESIAN_POINT('Ctrl Pts',(19.2786358177198,-13.0840182984949,
0.));
#219852=CARTESIAN_POINT('Ctrl Pts',(19.2626927725596,-13.0783089692118,
0.));
#219853=CARTESIAN_POINT('Ctrl Pts',(19.2468925053989,-13.0725987415859,
0.));
#219854=CARTESIAN_POINT('Ctrl Pts',(19.2312360592033,-13.0668886494795,
0.));
#219855=CARTESIAN_POINT('Ctrl Pts',(19.2157244937142,-13.0611797463915,
0.));
#219856=CARTESIAN_POINT('Ctrl Pts',(19.2003588859772,-13.0554731060538,
0.));
#219857=CARTESIAN_POINT('Ctrl Pts',(19.1851403308825,-13.0497698230441,
0.));
#219858=CARTESIAN_POINT('Ctrl Pts',(19.1700699416622,-13.0440710133772,
0.));
#219859=CARTESIAN_POINT('Ctrl Pts',(19.155148850523,-13.0383778152068,0.));
#219860=CARTESIAN_POINT('Ctrl Pts',(19.1403782093386,-13.0326913895838,
0.));
#219861=CARTESIAN_POINT('Ctrl Pts',(19.1257591903099,-13.0270129211976,
0.));
#219862=CARTESIAN_POINT('Ctrl Pts',(19.111292986631,-13.0213436191328,0.));
#219863=CARTESIAN_POINT('Ctrl Pts',(19.0969808131228,-13.0156847176097,
0.));
#219864=CARTESIAN_POINT('Ctrl Pts',(19.0828239070484,-13.0100374768788,
0.));
#219865=CARTESIAN_POINT('Ctrl Pts',(19.0688235289437,-13.0044031841382,
0.));
#219866=CARTESIAN_POINT('Ctrl Pts',(19.0549809634354,-12.9987831544502,
0.));
#219867=CARTESIAN_POINT('Ctrl Pts',(19.0412975200398,-12.9931787316514,
0.));
#219868=CARTESIAN_POINT('Ctrl Pts',(19.0277745339908,-12.9875912893003,
0.));
#219869=CARTESIAN_POINT('Ctrl Pts',(19.014413367335,-12.9820222318716,0.));
#219870=CARTESIAN_POINT('Ctrl Pts',(19.0012154099792,-12.9764729959206,
0.));
#219871=CARTESIAN_POINT('Ctrl Pts',(18.9881820807585,-12.9709450512747,
0.));
#219872=CARTESIAN_POINT('Ctrl Pts',(18.9753148284473,-12.9654399021868,
0.));
#219873=CARTESIAN_POINT('Ctrl Pts',(18.9626151329226,-12.9599590886318,
0.));
#219874=CARTESIAN_POINT('Ctrl Pts',(18.9500845064714,-12.9545041877377,
0.));
#219875=CARTESIAN_POINT('Ctrl Pts',(18.9377244950435,-12.9490768151821,
0.));
#219876=CARTESIAN_POINT('Ctrl Pts',(18.9255366795196,-12.9436786266106,
0.));
#219877=CARTESIAN_POINT('Ctrl Pts',(18.9135226769466,-12.9383113190375,
0.));
#219878=CARTESIAN_POINT('Ctrl Pts',(18.9016841423402,-12.9329766328184,
0.));
#219879=CARTESIAN_POINT('Ctrl Pts',(18.8900227704888,-12.9276763536372,
0.));
#219880=CARTESIAN_POINT('Ctrl Pts',(18.8785402977528,-12.9224123144982,
0.));
#219881=CARTESIAN_POINT('Ctrl Pts',(18.8672385038328,-12.9171863977047,
0.));
#219882=CARTESIAN_POINT('Ctrl Pts',(18.8561192136201,-12.9120005369066,
0.));
#219883=CARTESIAN_POINT('Ctrl Pts',(18.8451842990986,-12.9068567191856,
0.));
#219884=CARTESIAN_POINT('Ctrl Pts',(18.834435681259,-12.9017569871738,0.));
#219885=CARTESIAN_POINT('Ctrl Pts',(18.8238753319124,-12.8967034410752,
0.));
#219886=CARTESIAN_POINT('Ctrl Pts',(18.8135052757815,-12.8916982409931,
0.));
#219887=CARTESIAN_POINT('Ctrl Pts',(18.8033275941939,-12.8867436109543,
0.));
#219888=CARTESIAN_POINT('Ctrl Pts',(18.7933444285867,-12.8818418427474,
0.));
#219889=CARTESIAN_POINT('Ctrl Pts',(18.7835579840481,-12.8769952998097,
0.));
#219890=CARTESIAN_POINT('Ctrl Pts',(18.7739705329028,-12.8722064211814,
0.));
#219891=CARTESIAN_POINT('Ctrl Pts',(18.7645844169568,-12.8674777239656,
0.));
#219892=CARTESIAN_POINT('Ctrl Pts',(18.7554020493888,-12.8628118054172,
0.));
#219893=CARTESIAN_POINT('Ctrl Pts',(18.7464259171248,-12.8582113455644,
0.));
#219894=CARTESIAN_POINT('Ctrl Pts',(18.7376585820851,-12.8536791086315,
0.));
#219895=CARTESIAN_POINT('Ctrl Pts',(18.7291026886552,-12.849217951159,0.));
#219896=CARTESIAN_POINT('Ctrl Pts',(18.7207609737701,-12.8448308329494,
0.));
#219897=CARTESIAN_POINT('Ctrl Pts',(18.7126362754446,-12.8405208263432,
0.));
#219898=CARTESIAN_POINT('Ctrl Pts',(18.7047315436296,-12.8362911280362,
0.));
#219899=CARTESIAN_POINT('Ctrl Pts',(18.6970498410173,-12.832145059979,0.));
#219900=CARTESIAN_POINT('Ctrl Pts',(18.6895943376172,-12.8280860635231,
0.));
#219901=CARTESIAN_POINT('Ctrl Pts',(18.6823683094139,-12.8241176980016,
0.));
#219902=CARTESIAN_POINT('Ctrl Pts',(18.6753751301091,-12.8202436318473,
0.));
#219903=CARTESIAN_POINT('Ctrl Pts',(18.6686182952798,-12.8164676687361,
0.));
#219904=CARTESIAN_POINT('Ctrl Pts',(18.6621014624746,-12.8127937909632,
0.));
#219905=CARTESIAN_POINT('Ctrl Pts',(18.6558284825772,-12.8092261933858,
0.));
#219906=CARTESIAN_POINT('Ctrl Pts',(18.6498034438986,-12.805769331162,0.));
#219907=CARTESIAN_POINT('Ctrl Pts',(18.6440306327457,-12.8024278770153,
0.));
#219908=CARTESIAN_POINT('Ctrl Pts',(18.63851447924,-12.7992066625264,0.));
#219909=CARTESIAN_POINT('Ctrl Pts',(18.6332595057005,-12.7961106222251,
0.));
#219910=CARTESIAN_POINT('Ctrl Pts',(18.6282702819371,-12.7931447451556,
0.));
#219911=CARTESIAN_POINT('Ctrl Pts',(18.6235516265575,-12.7903142925234,
0.));
#219912=CARTESIAN_POINT('Ctrl Pts',(18.6191087624752,-12.7876249657834,
0.));
#219913=CARTESIAN_POINT('Ctrl Pts',(18.6149475565189,-12.78508316579,0.));
#219914=CARTESIAN_POINT('Ctrl Pts',(18.611074482622,-12.7826959526924,0.));
#219915=CARTESIAN_POINT('Ctrl Pts',(18.6074961535723,-12.7804705387658,
0.));
#219916=CARTESIAN_POINT('Ctrl Pts',(18.6042190183703,-12.7784139605067,
0.));
#219917=CARTESIAN_POINT('Ctrl Pts',(18.6012488486708,-12.7765325225082,
0.));
#219918=CARTESIAN_POINT('Ctrl Pts',(18.5985917525949,-12.7748328937639,
0.));
#219919=CARTESIAN_POINT('Ctrl Pts',(18.5962551167772,-12.7733231262107,
0.));
#219920=CARTESIAN_POINT('Ctrl Pts',(18.5942490615409,-12.7720142287169,
0.));
#219921=CARTESIAN_POINT('Ctrl Pts',(18.5925859134582,-12.7709195951153,
0.));
#219922=CARTESIAN_POINT('Ctrl Pts',(18.5912775137806,-12.7700520897174,
0.));
#219923=CARTESIAN_POINT('Ctrl Pts',(18.590332877722,-12.7694215127923,0.));
#219924=CARTESIAN_POINT('Ctrl Pts',(18.589871621842,-12.7691103481996,0.));
#219925=CARTESIAN_POINT('Ctrl Pts',(18.5896919669158,-12.7689864266924,
0.));
#219926=CARTESIAN_POINT('Ctrl Pts',(18.5896460962961,-12.7689524524484,
0.));
#219927=CARTESIAN_POINT('Ctrl Pts',(18.5896416359912,-12.7689476255363,
0.));
#219928=CARTESIAN_POINT('',(22.1787195904339,-13.5685075571671,12.));
#219929=CARTESIAN_POINT('',(22.1787195904339,-13.5685075571671,0.));
#219930=CARTESIAN_POINT('Ctrl Pts',(18.5896416359912,-12.7689476255363,
12.));
#219931=CARTESIAN_POINT('Ctrl Pts',(18.5896460962961,-12.7689524524484,
12.));
#219932=CARTESIAN_POINT('Ctrl Pts',(18.5896919669158,-12.7689864266924,
12.));
#219933=CARTESIAN_POINT('Ctrl Pts',(18.589871621842,-12.7691103481996,12.));
#219934=CARTESIAN_POINT('Ctrl Pts',(18.590332877722,-12.7694215127923,12.));
#219935=CARTESIAN_POINT('Ctrl Pts',(18.5912775137806,-12.7700520897174,
12.));
#219936=CARTESIAN_POINT('Ctrl Pts',(18.5925859134582,-12.7709195951153,
12.));
#219937=CARTESIAN_POINT('Ctrl Pts',(18.5942490615409,-12.7720142287169,
12.));
#219938=CARTESIAN_POINT('Ctrl Pts',(18.5962551167772,-12.7733231262107,
12.));
#219939=CARTESIAN_POINT('Ctrl Pts',(18.5985917525949,-12.7748328937639,
12.));
#219940=CARTESIAN_POINT('Ctrl Pts',(18.6012488486708,-12.7765325225082,
12.));
#219941=CARTESIAN_POINT('Ctrl Pts',(18.6042190183703,-12.7784139605067,
12.));
#219942=CARTESIAN_POINT('Ctrl Pts',(18.6074961535723,-12.7804705387658,
12.));
#219943=CARTESIAN_POINT('Ctrl Pts',(18.611074482622,-12.7826959526924,12.));
#219944=CARTESIAN_POINT('Ctrl Pts',(18.6149475565189,-12.78508316579,12.));
#219945=CARTESIAN_POINT('Ctrl Pts',(18.6191087624752,-12.7876249657834,
12.));
#219946=CARTESIAN_POINT('Ctrl Pts',(18.6235516265575,-12.7903142925234,
12.));
#219947=CARTESIAN_POINT('Ctrl Pts',(18.6282702819371,-12.7931447451556,
12.));
#219948=CARTESIAN_POINT('Ctrl Pts',(18.6332595057005,-12.7961106222251,
12.));
#219949=CARTESIAN_POINT('Ctrl Pts',(18.63851447924,-12.7992066625264,12.));
#219950=CARTESIAN_POINT('Ctrl Pts',(18.6440306327457,-12.8024278770153,
12.));
#219951=CARTESIAN_POINT('Ctrl Pts',(18.6498034438986,-12.805769331162,12.));
#219952=CARTESIAN_POINT('Ctrl Pts',(18.6558284825772,-12.8092261933858,
12.));
#219953=CARTESIAN_POINT('Ctrl Pts',(18.6621014624746,-12.8127937909632,
12.));
#219954=CARTESIAN_POINT('Ctrl Pts',(18.6686182952798,-12.8164676687361,
12.));
#219955=CARTESIAN_POINT('Ctrl Pts',(18.6753751301091,-12.8202436318473,
12.));
#219956=CARTESIAN_POINT('Ctrl Pts',(18.6823683094139,-12.8241176980016,
12.));
#219957=CARTESIAN_POINT('Ctrl Pts',(18.6895943376172,-12.8280860635231,
12.));
#219958=CARTESIAN_POINT('Ctrl Pts',(18.6970498410173,-12.832145059979,12.));
#219959=CARTESIAN_POINT('Ctrl Pts',(18.7047315436296,-12.8362911280362,
12.));
#219960=CARTESIAN_POINT('Ctrl Pts',(18.7126362754446,-12.8405208263432,
12.));
#219961=CARTESIAN_POINT('Ctrl Pts',(18.7207609737701,-12.8448308329494,
12.));
#219962=CARTESIAN_POINT('Ctrl Pts',(18.7291026886552,-12.849217951159,12.));
#219963=CARTESIAN_POINT('Ctrl Pts',(18.7376585820851,-12.8536791086315,
12.));
#219964=CARTESIAN_POINT('Ctrl Pts',(18.7464259171248,-12.8582113455644,
12.));
#219965=CARTESIAN_POINT('Ctrl Pts',(18.7554020493888,-12.8628118054172,
12.));
#219966=CARTESIAN_POINT('Ctrl Pts',(18.7645844169568,-12.8674777239656,
12.));
#219967=CARTESIAN_POINT('Ctrl Pts',(18.7739705329028,-12.8722064211814,
12.));
#219968=CARTESIAN_POINT('Ctrl Pts',(18.7835579840481,-12.8769952998097,
12.));
#219969=CARTESIAN_POINT('Ctrl Pts',(18.7933444285867,-12.8818418427474,
12.));
#219970=CARTESIAN_POINT('Ctrl Pts',(18.8033275941939,-12.8867436109543,
12.));
#219971=CARTESIAN_POINT('Ctrl Pts',(18.8135052757815,-12.8916982409931,
12.));
#219972=CARTESIAN_POINT('Ctrl Pts',(18.8238753319124,-12.8967034410752,
12.));
#219973=CARTESIAN_POINT('Ctrl Pts',(18.834435681259,-12.9017569871738,12.));
#219974=CARTESIAN_POINT('Ctrl Pts',(18.8451842990986,-12.9068567191856,
12.));
#219975=CARTESIAN_POINT('Ctrl Pts',(18.8561192136201,-12.9120005369066,
12.));
#219976=CARTESIAN_POINT('Ctrl Pts',(18.8672385038328,-12.9171863977047,
12.));
#219977=CARTESIAN_POINT('Ctrl Pts',(18.8785402977528,-12.9224123144982,
12.));
#219978=CARTESIAN_POINT('Ctrl Pts',(18.8900227704888,-12.9276763536372,
12.));
#219979=CARTESIAN_POINT('Ctrl Pts',(18.9016841423402,-12.9329766328184,
12.));
#219980=CARTESIAN_POINT('Ctrl Pts',(18.9135226769466,-12.9383113190375,
12.));
#219981=CARTESIAN_POINT('Ctrl Pts',(18.9255366795196,-12.9436786266106,
12.));
#219982=CARTESIAN_POINT('Ctrl Pts',(18.9377244950435,-12.9490768151821,
12.));
#219983=CARTESIAN_POINT('Ctrl Pts',(18.9500845064714,-12.9545041877377,
12.));
#219984=CARTESIAN_POINT('Ctrl Pts',(18.9626151329226,-12.9599590886318,
12.));
#219985=CARTESIAN_POINT('Ctrl Pts',(18.9753148284473,-12.9654399021868,
12.));
#219986=CARTESIAN_POINT('Ctrl Pts',(18.9881820807585,-12.9709450512747,
12.));
#219987=CARTESIAN_POINT('Ctrl Pts',(19.0012154099792,-12.9764729959206,
12.));
#219988=CARTESIAN_POINT('Ctrl Pts',(19.014413367335,-12.9820222318716,12.));
#219989=CARTESIAN_POINT('Ctrl Pts',(19.0277745339908,-12.9875912893003,
12.));
#219990=CARTESIAN_POINT('Ctrl Pts',(19.0412975200398,-12.9931787316514,
12.));
#219991=CARTESIAN_POINT('Ctrl Pts',(19.0549809634354,-12.9987831544502,
12.));
#219992=CARTESIAN_POINT('Ctrl Pts',(19.0688235289437,-13.0044031841382,
12.));
#219993=CARTESIAN_POINT('Ctrl Pts',(19.0828239070484,-13.0100374768788,
12.));
#219994=CARTESIAN_POINT('Ctrl Pts',(19.0969808131228,-13.0156847176097,
12.));
#219995=CARTESIAN_POINT('Ctrl Pts',(19.111292986631,-13.0213436191328,12.));
#219996=CARTESIAN_POINT('Ctrl Pts',(19.1257591903099,-13.0270129211976,
12.));
#219997=CARTESIAN_POINT('Ctrl Pts',(19.1403782093386,-13.0326913895838,
12.));
#219998=CARTESIAN_POINT('Ctrl Pts',(19.155148850523,-13.0383778152068,12.));
#219999=CARTESIAN_POINT('Ctrl Pts',(19.1700699416622,-13.0440710133772,
12.));
#220000=CARTESIAN_POINT('Ctrl Pts',(19.1851403308825,-13.0497698230441,
12.));
#220001=CARTESIAN_POINT('Ctrl Pts',(19.2003588859772,-13.0554731060538,
12.));
#220002=CARTESIAN_POINT('Ctrl Pts',(19.2157244937142,-13.0611797463915,
12.));
#220003=CARTESIAN_POINT('Ctrl Pts',(19.2312360592033,-13.0668886494795,
12.));
#220004=CARTESIAN_POINT('Ctrl Pts',(19.2468925053989,-13.0725987415859,
12.));
#220005=CARTESIAN_POINT('Ctrl Pts',(19.2626927725596,-13.0783089692118,
12.));
#220006=CARTESIAN_POINT('Ctrl Pts',(19.2786358177198,-13.0840182984949,
12.));
#220007=CARTESIAN_POINT('Ctrl Pts',(19.2947206141247,-13.0897257145969,
12.));
#220008=CARTESIAN_POINT('Ctrl Pts',(19.310946150736,-13.0954302211479,12.));
#220009=CARTESIAN_POINT('Ctrl Pts',(19.3273114318269,-13.1011308397591,
12.));
#220010=CARTESIAN_POINT('Ctrl Pts',(19.3438154765395,-13.1068266095186,
12.));
#220011=CARTESIAN_POINT('Ctrl Pts',(19.3604573184515,-13.1125165865022,
12.));
#220012=CARTESIAN_POINT('Ctrl Pts',(19.3772360051091,-13.118199843271,12.));
#220013=CARTESIAN_POINT('Ctrl Pts',(19.3941505976263,-13.1238754684177,
12.));
#220014=CARTESIAN_POINT('Ctrl Pts',(19.4112001703557,-13.1295425661634,
12.));
#220015=CARTESIAN_POINT('Ctrl Pts',(19.4283838105262,-13.1352002559438,
12.));
#220016=CARTESIAN_POINT('Ctrl Pts',(19.4457006178876,-13.1408476720061,
12.));
#220017=CARTESIAN_POINT('Ctrl Pts',(19.4631497043258,-13.1464839629971,
12.));
#220018=CARTESIAN_POINT('Ctrl Pts',(19.4807301935268,-13.1521082915853,
12.));
#220019=CARTESIAN_POINT('Ctrl Pts',(19.4984412207082,-13.1577198341245,
12.));
#220020=CARTESIAN_POINT('Ctrl Pts',(19.5162819323213,-13.1633177803101,
12.));
#220021=CARTESIAN_POINT('Ctrl Pts',(19.5342514857562,-13.168901332843,12.));
#220022=CARTESIAN_POINT('Ctrl Pts',(19.5523490490244,-13.1744697070911,
12.));
#220023=CARTESIAN_POINT('Ctrl Pts',(19.5705738004667,-13.1800221307673,
12.));
#220024=CARTESIAN_POINT('Ctrl Pts',(19.5889249285338,-13.1855578436471,
12.));
#220025=CARTESIAN_POINT('Ctrl Pts',(19.6074016315414,-13.1910760972814,
12.));
#220026=CARTESIAN_POINT('Ctrl Pts',(19.6260031174244,-13.1965761547151,
12.));
#220027=CARTESIAN_POINT('Ctrl Pts',(19.6447286034772,-13.2020572902065,
12.));
#220028=CARTESIAN_POINT('Ctrl Pts',(19.6635773160936,-13.2075187889529,
12.));
#220029=CARTESIAN_POINT('Ctrl Pts',(19.6825484905823,-13.2129599468485,
12.));
#220030=CARTESIAN_POINT('Ctrl Pts',(19.7016413709685,-13.2183800702436,
12.));
#220031=CARTESIAN_POINT('Ctrl Pts',(19.7208552097868,-13.2237784757065,
12.));
#220032=CARTESIAN_POINT('Ctrl Pts',(19.7401892678697,-13.2291544897899,
12.));
#220033=CARTESIAN_POINT('Ctrl Pts',(19.7596428141168,-13.2345074487963,
12.));
#220034=CARTESIAN_POINT('Ctrl Pts',(19.7792151253289,-13.2398366985675,
12.));
#220035=CARTESIAN_POINT('Ctrl Pts',(19.7989054860495,-13.2451415942805,
12.));
#220036=CARTESIAN_POINT('Ctrl Pts',(19.8187131883917,-13.2504215002457,
12.));
#220037=CARTESIAN_POINT('Ctrl Pts',(19.8386375318634,-13.2556757897086,
12.));
#220038=CARTESIAN_POINT('Ctrl Pts',(19.8586778231715,-13.2609038446529,
12.));
#220039=CARTESIAN_POINT('Ctrl Pts',(19.8788333760577,-13.2661050556132,
12.));
#220040=CARTESIAN_POINT('Ctrl Pts',(19.8991035111745,-13.271278821502,12.));
#220041=CARTESIAN_POINT('Ctrl Pts',(19.9194875559422,-13.2764245494357,
12.));
#220042=CARTESIAN_POINT('Ctrl Pts',(19.9399848444019,-13.2815416545663,
12.));
#220043=CARTESIAN_POINT('Ctrl Pts',(19.9605947170586,-13.286629559915,12.));
#220044=CARTESIAN_POINT('Ctrl Pts',(19.981316520717,-13.2916876962094,12.));
#220045=CARTESIAN_POINT('Ctrl Pts',(20.0021496083738,-13.2967155017306,
12.));
#220046=CARTESIAN_POINT('Ctrl Pts',(20.0230933391038,-13.3017124221637,
12.));
#220047=CARTESIAN_POINT('Ctrl Pts',(20.0441470779345,-13.3066779104515,
12.));
#220048=CARTESIAN_POINT('Ctrl Pts',(20.0653101957188,-13.3116114266515,
12.));
#220049=CARTESIAN_POINT('Ctrl Pts',(20.0865820689882,-13.3165124377963,
12.));
#220050=CARTESIAN_POINT('Ctrl Pts',(20.1079620798375,-13.3213804177587,
12.));
#220051=CARTESIAN_POINT('Ctrl Pts',(20.1294496158402,-13.3262148471226,
12.));
#220052=CARTESIAN_POINT('Ctrl Pts',(20.1510440699474,-13.3310152130564,
12.));
#220053=CARTESIAN_POINT('Ctrl Pts',(20.1727448403817,-13.3357810091903,
12.));
#220054=CARTESIAN_POINT('Ctrl Pts',(20.1945513305235,-13.3405117354971,
12.));
#220055=CARTESIAN_POINT('Ctrl Pts',(20.216462948786,-13.3452068981766,12.));
#220056=CARTESIAN_POINT('Ctrl Pts',(20.2384791085359,-13.3498660095386,
12.));
#220057=CARTESIAN_POINT('Ctrl Pts',(20.2605992280122,-13.3544885878889,
12.));
#220058=CARTESIAN_POINT('Ctrl Pts',(20.2828227302339,-13.3590741574195,
12.));
#220059=CARTESIAN_POINT('Ctrl Pts',(20.3051490429048,-13.3636222481016,
12.));
#220060=CARTESIAN_POINT('Ctrl Pts',(20.3275775983029,-13.3681323955826,
12.));
#220061=CARTESIAN_POINT('Ctrl Pts',(20.3501078331814,-13.3726041410867,
12.));
#220062=CARTESIAN_POINT('Ctrl Pts',(20.3727391887184,-13.3770370313188,
12.));
#220063=CARTESIAN_POINT('Ctrl Pts',(20.3954711104502,-13.3814306183719,
12.));
#220064=CARTESIAN_POINT('Ctrl Pts',(20.4183030482002,-13.3857844596387,
12.));
#220065=CARTESIAN_POINT('Ctrl Pts',(20.4412344560008,-13.3900981177255,
12.));
#220066=CARTESIAN_POINT('Ctrl Pts',(20.4642647920038,-13.3943711603739,
12.));
#220067=CARTESIAN_POINT('Ctrl Pts',(20.487393518404,-13.3986031603716,12.));
#220068=CARTESIAN_POINT('Ctrl Pts',(20.5106201013753,-13.4027936954529,
12.));
#220069=CARTESIAN_POINT('Ctrl Pts',(20.5339440109956,-13.4069423482076,
12.));
#220070=CARTESIAN_POINT('Ctrl Pts',(20.5573647211639,-13.4110487059912,
12.));
#220071=CARTESIAN_POINT('Ctrl Pts',(20.5808817095155,-13.4151123608411,
12.));
#220072=CARTESIAN_POINT('Ctrl Pts',(20.6044944573153,-13.4191329093933,
12.));
#220073=CARTESIAN_POINT('Ctrl Pts',(20.6282024494237,-13.4231099528179,
12.));
#220074=CARTESIAN_POINT('Ctrl Pts',(20.6520051742869,-13.4270430967651,
12.));
#220075=CARTESIAN_POINT('Ctrl Pts',(20.6759021239103,-13.4309319513119,
12.));
#220076=CARTESIAN_POINT('Ctrl Pts',(20.6998927938288,-13.4347761309154,
12.));
#220077=CARTESIAN_POINT('Ctrl Pts',(20.7239766830675,-13.4385752543663,
12.));
#220078=CARTESIAN_POINT('Ctrl Pts',(20.7481532941013,-13.4423289447561,
12.));
#220079=CARTESIAN_POINT('Ctrl Pts',(20.7724221327608,-13.4460368293688,
12.));
#220080=CARTESIAN_POINT('Ctrl Pts',(20.7967827081227,-13.4496985395637,
12.));
#220081=CARTESIAN_POINT('Ctrl Pts',(20.821234532398,-13.4533137106667,12.));
#220082=CARTESIAN_POINT('Ctrl Pts',(20.8457771208082,-13.4568819818631,
12.));
#220083=CARTESIAN_POINT('Ctrl Pts',(20.8704099914641,-13.4604029960983,
12.));
#220084=CARTESIAN_POINT('Ctrl Pts',(20.8951326652158,-13.4638763999725,
12.));
#220085=CARTESIAN_POINT('Ctrl Pts',(20.9199446657584,-13.4673018437718,
12.));
#220086=CARTESIAN_POINT('Ctrl Pts',(20.9448455197557,-13.4706789815166,
12.));
#220087=CARTESIAN_POINT('Ctrl Pts',(20.9698347569476,-13.4740074710087,
12.));
#220088=CARTESIAN_POINT('Ctrl Pts',(20.9949119102592,-13.4772869738879,
12.));
#220089=CARTESIAN_POINT('Ctrl Pts',(21.0200765158885,-13.4805171556822,
12.));
#220090=CARTESIAN_POINT('Ctrl Pts',(21.0453281134247,-13.4836976858912,
12.));
#220091=CARTESIAN_POINT('Ctrl Pts',(21.0706662455202,-13.4868282377192,
12.));
#220092=CARTESIAN_POINT('Ctrl Pts',(21.0960904575048,-13.4899084877718,
12.));
#220093=CARTESIAN_POINT('Ctrl Pts',(21.1216002970209,-13.4929381157778,
12.));
#220094=CARTESIAN_POINT('Ctrl Pts',(21.1471953136209,-13.4959168042934,
12.));
#220095=CARTESIAN_POINT('Ctrl Pts',(21.1728750584173,-13.4988442384491,
12.));
#220096=CARTESIAN_POINT('Ctrl Pts',(21.1986390835825,-13.5017201056088,
12.));
#220097=CARTESIAN_POINT('Ctrl Pts',(21.224486942933,-13.5045440957404,12.));
#220098=CARTESIAN_POINT('Ctrl Pts',(21.2504181927429,-13.5073159019454,
12.));
#220099=CARTESIAN_POINT('Ctrl Pts',(21.2764323924442,-13.5100352209207,
12.));
#220100=CARTESIAN_POINT('Ctrl Pts',(21.3025291054236,-13.5127017534972,
12.));
#220101=CARTESIAN_POINT('Ctrl Pts',(21.328707899634,-13.5153152050554,12.));
#220102=CARTESIAN_POINT('Ctrl Pts',(21.3549683486219,-13.5178752862461,
12.));
#220103=CARTESIAN_POINT('Ctrl Pts',(21.3813100304967,-13.5203817122497,
12.));
#220104=CARTESIAN_POINT('Ctrl Pts',(21.4077325259318,-13.5228342013508,
12.));
#220105=CARTESIAN_POINT('Ctrl Pts',(21.4342354165254,-13.5252324737795,
12.));
#220106=CARTESIAN_POINT('Ctrl Pts',(21.4608182828695,-13.5275762503553,
12.));
#220107=CARTESIAN_POINT('Ctrl Pts',(21.487480703047,-13.5298652514357,12.));
#220108=CARTESIAN_POINT('Ctrl Pts',(21.5142222501671,-13.5320991952145,
12.));
#220109=CARTESIAN_POINT('Ctrl Pts',(21.5410424932511,-13.5342777983225,
12.));
#220110=CARTESIAN_POINT('Ctrl Pts',(21.5679410019011,-13.5364007790292,
12.));
#220111=CARTESIAN_POINT('Ctrl Pts',(21.5949173499022,-13.5384678597206,
12.));
#220112=CARTESIAN_POINT('Ctrl Pts',(21.6219711193951,-13.5404787697798,
12.));
#220113=CARTESIAN_POINT('Ctrl Pts',(21.6491019044647,-13.5424332480698,
12.));
#220114=CARTESIAN_POINT('Ctrl Pts',(21.676309315769,-13.5443310461516,12.));
#220115=CARTESIAN_POINT('Ctrl Pts',(21.7035929822939,-13.546171929503,12.));
#220116=CARTESIAN_POINT('Ctrl Pts',(21.730952541226,-13.5479556704457,12.));
#220117=CARTESIAN_POINT('Ctrl Pts',(21.7583876294532,-13.5496820422186,
12.));
#220118=CARTESIAN_POINT('Ctrl Pts',(21.7858978745848,-13.5513508127232,
12.));
#220119=CARTESIAN_POINT('Ctrl Pts',(21.8134828857963,-13.5529617381569,
12.));
#220120=CARTESIAN_POINT('Ctrl Pts',(21.841142245609,-13.5545145573048,12.));
#220121=CARTESIAN_POINT('Ctrl Pts',(21.8688754989401,-13.5560089839426,
12.));
#220122=CARTESIAN_POINT('Ctrl Pts',(21.8966821688876,-13.5574447178485,
12.));
#220123=CARTESIAN_POINT('Ctrl Pts',(21.9245617765827,-13.5588214586672,
12.));
#220124=CARTESIAN_POINT('Ctrl Pts',(21.9525138592862,-13.5601389185315,
12.));
#220125=CARTESIAN_POINT('Ctrl Pts',(21.9805379899192,-13.5613968357589,
12.));
#220126=CARTESIAN_POINT('Ctrl Pts',(22.0086337943431,-13.5625949868313,
12.));
#220127=CARTESIAN_POINT('Ctrl Pts',(22.0368009736227,-13.5637332022393,
12.));
#220128=CARTESIAN_POINT('Ctrl Pts',(22.0650393089492,-13.5648113688895,
12.));
#220129=CARTESIAN_POINT('Ctrl Pts',(22.0933486464442,-13.5658294169106,
12.));
#220130=CARTESIAN_POINT('Ctrl Pts',(22.1217288871823,-13.5667873105179,
12.));
#220131=CARTESIAN_POINT('Ctrl Pts',(22.1444897575076,-13.5675054918922,
12.));
#220132=CARTESIAN_POINT('Ctrl Pts',(22.1615922804939,-13.5680170531724,
12.));
#220133=CARTESIAN_POINT('Ctrl Pts',(22.1730081264583,-13.5683460612913,
12.));
#220134=CARTESIAN_POINT('Ctrl Pts',(22.1787195904339,-13.5685075571671,
12.));
#220135=CARTESIAN_POINT('Ctrl Pts',(17.1452095830632,-14.6513681262571,
0.));
#220136=CARTESIAN_POINT('Ctrl Pts',(17.1452095830632,-14.6513681262571,
12.));
#220137=CARTESIAN_POINT('Ctrl Pts',(17.1452153999142,-14.6513711852843,
0.));
#220138=CARTESIAN_POINT('Ctrl Pts',(17.1452153999142,-14.6513711852843,
12.));
#220139=CARTESIAN_POINT('Ctrl Pts',(17.1452600887037,-14.6514066997196,
0.));
#220140=CARTESIAN_POINT('Ctrl Pts',(17.1452600887037,-14.6514066997196,
12.));
#220141=CARTESIAN_POINT('Ctrl Pts',(17.1454262858043,-14.6515481598068,
0.));
#220142=CARTESIAN_POINT('Ctrl Pts',(17.1454262858043,-14.6515481598068,
12.));
#220143=CARTESIAN_POINT('Ctrl Pts',(17.1458462295271,-14.6519131634508,
0.));
#220144=CARTESIAN_POINT('Ctrl Pts',(17.1458462295271,-14.6519131634508,
12.));
#220145=CARTESIAN_POINT('Ctrl Pts',(17.1466998098673,-14.6526624064978,
0.));
#220146=CARTESIAN_POINT('Ctrl Pts',(17.1466998098673,-14.6526624064978,
12.));
#220147=CARTESIAN_POINT('Ctrl Pts',(17.147876394491,-14.6537016966184,0.));
#220148=CARTESIAN_POINT('Ctrl Pts',(17.147876394491,-14.6537016966184,12.));
#220149=CARTESIAN_POINT('Ctrl Pts',(17.1493641837558,-14.655024862281,0.));
#220150=CARTESIAN_POINT('Ctrl Pts',(17.1493641837558,-14.655024862281,12.));
#220151=CARTESIAN_POINT('Ctrl Pts',(17.1511476869496,-14.6566237952435,
0.));
#220152=CARTESIAN_POINT('Ctrl Pts',(17.1511476869496,-14.6566237952435,
12.));
#220153=CARTESIAN_POINT('Ctrl Pts',(17.1532107762718,-14.6584900555302,
0.));
#220154=CARTESIAN_POINT('Ctrl Pts',(17.1532107762718,-14.6584900555302,
12.));
#220155=CARTESIAN_POINT('Ctrl Pts',(17.1555401986401,-14.6606167169642,
0.));
#220156=CARTESIAN_POINT('Ctrl Pts',(17.1555401986401,-14.6606167169642,
12.));
#220157=CARTESIAN_POINT('Ctrl Pts',(17.1581262646789,-14.6629987285992,
0.));
#220158=CARTESIAN_POINT('Ctrl Pts',(17.1581262646789,-14.6629987285992,
12.));
#220159=CARTESIAN_POINT('Ctrl Pts',(17.1609609517369,-14.6656319165057,
0.));
#220160=CARTESIAN_POINT('Ctrl Pts',(17.1609609517369,-14.6656319165057,
12.));
#220161=CARTESIAN_POINT('Ctrl Pts',(17.1640366762305,-14.6685123374423,
0.));
#220162=CARTESIAN_POINT('Ctrl Pts',(17.1640366762305,-14.6685123374423,
12.));
#220163=CARTESIAN_POINT('Ctrl Pts',(17.167344972302,-14.671635583332,0.));
#220164=CARTESIAN_POINT('Ctrl Pts',(17.167344972302,-14.671635583332,12.));
#220165=CARTESIAN_POINT('Ctrl Pts',(17.1708771619129,-14.6749971333867,
0.));
#220166=CARTESIAN_POINT('Ctrl Pts',(17.1708771619129,-14.6749971333867,
12.));
#220167=CARTESIAN_POINT('Ctrl Pts',(17.1746247499057,-14.6785925615677,
0.));
#220168=CARTESIAN_POINT('Ctrl Pts',(17.1746247499057,-14.6785925615677,
12.));
#220169=CARTESIAN_POINT('Ctrl Pts',(17.1785800350826,-14.6824178576167,
0.));
#220170=CARTESIAN_POINT('Ctrl Pts',(17.1785800350826,-14.6824178576167,
12.));
#220171=CARTESIAN_POINT('Ctrl Pts',(17.182736158472,-14.686469452232,0.));
#220172=CARTESIAN_POINT('Ctrl Pts',(17.182736158472,-14.686469452232,12.));
#220173=CARTESIAN_POINT('Ctrl Pts',(17.1870867909918,-14.6907440526958,
0.));
#220174=CARTESIAN_POINT('Ctrl Pts',(17.1870867909918,-14.6907440526958,
12.));
#220175=CARTESIAN_POINT('Ctrl Pts',(17.1916259308415,-14.6952385361706,
0.));
#220176=CARTESIAN_POINT('Ctrl Pts',(17.1916259308415,-14.6952385361706,
12.));
#220177=CARTESIAN_POINT('Ctrl Pts',(17.1963476411694,-14.699949811582,0.));
#220178=CARTESIAN_POINT('Ctrl Pts',(17.1963476411694,-14.699949811582,12.));
#220179=CARTESIAN_POINT('Ctrl Pts',(17.2012461084268,-14.7048748502663,
0.));
#220180=CARTESIAN_POINT('Ctrl Pts',(17.2012461084268,-14.7048748502663,
12.));
#220181=CARTESIAN_POINT('Ctrl Pts',(17.2063157097315,-14.7100107213586,
0.));
#220182=CARTESIAN_POINT('Ctrl Pts',(17.2063157097315,-14.7100107213586,
12.));
#220183=CARTESIAN_POINT('Ctrl Pts',(17.2115510835989,-14.7153546289339,
0.));
#220184=CARTESIAN_POINT('Ctrl Pts',(17.2115510835989,-14.7153546289339,
12.));
#220185=CARTESIAN_POINT('Ctrl Pts',(17.2169471814256,-14.7209039390327,
0.));
#220186=CARTESIAN_POINT('Ctrl Pts',(17.2169471814256,-14.7209039390327,
12.));
#220187=CARTESIAN_POINT('Ctrl Pts',(17.2224992099667,-14.7266561494282,
0.));
#220188=CARTESIAN_POINT('Ctrl Pts',(17.2224992099667,-14.7266561494282,
12.));
#220189=CARTESIAN_POINT('Ctrl Pts',(17.2282025904314,-14.7326088681163,
0.));
#220190=CARTESIAN_POINT('Ctrl Pts',(17.2282025904314,-14.7326088681163,
12.));
#220191=CARTESIAN_POINT('Ctrl Pts',(17.2340529062076,-14.7387597858117,
0.));
#220192=CARTESIAN_POINT('Ctrl Pts',(17.2340529062076,-14.7387597858117,
12.));
#220193=CARTESIAN_POINT('Ctrl Pts',(17.2400458713565,-14.7451066593792,
0.));
#220194=CARTESIAN_POINT('Ctrl Pts',(17.2400458713565,-14.7451066593792,
12.));
#220195=CARTESIAN_POINT('Ctrl Pts',(17.2461773413288,-14.7516473175124,
0.));
#220196=CARTESIAN_POINT('Ctrl Pts',(17.2461773413288,-14.7516473175124,
12.));
#220197=CARTESIAN_POINT('Ctrl Pts',(17.2524433146837,-14.7583796616617,
0.));
#220198=CARTESIAN_POINT('Ctrl Pts',(17.2524433146837,-14.7583796616617,
12.));
#220199=CARTESIAN_POINT('Ctrl Pts',(17.2588399401465,-14.7653016697591,
0.));
#220200=CARTESIAN_POINT('Ctrl Pts',(17.2588399401465,-14.7653016697591,
12.));
#220201=CARTESIAN_POINT('Ctrl Pts',(17.2653635155319,-14.7724113956731,
0.));
#220202=CARTESIAN_POINT('Ctrl Pts',(17.2653635155319,-14.7724113956731,
12.));
#220203=CARTESIAN_POINT('Ctrl Pts',(17.2720104735194,-14.7797069617804,
0.));
#220204=CARTESIAN_POINT('Ctrl Pts',(17.2720104735194,-14.7797069617804,
12.));
#220205=CARTESIAN_POINT('Ctrl Pts',(17.2787773704849,-14.787186553128,0.));
#220206=CARTESIAN_POINT('Ctrl Pts',(17.2787773704849,-14.787186553128,12.));
#220207=CARTESIAN_POINT('Ctrl Pts',(17.2856608733196,-14.7948484105249,
0.));
#220208=CARTESIAN_POINT('Ctrl Pts',(17.2856608733196,-14.7948484105249,
12.));
#220209=CARTESIAN_POINT('Ctrl Pts',(17.2926577496513,-14.8026908254276,
0.));
#220210=CARTESIAN_POINT('Ctrl Pts',(17.2926577496513,-14.8026908254276,
12.));
#220211=CARTESIAN_POINT('Ctrl Pts',(17.299764866148,-14.8107121391035,0.));
#220212=CARTESIAN_POINT('Ctrl Pts',(17.299764866148,-14.8107121391035,12.));
#220213=CARTESIAN_POINT('Ctrl Pts',(17.3069791853706,-14.8189107410162,
0.));
#220214=CARTESIAN_POINT('Ctrl Pts',(17.3069791853706,-14.8189107410162,
12.));
#220215=CARTESIAN_POINT('Ctrl Pts',(17.3142977632659,-14.8272850675379,
0.));
#220216=CARTESIAN_POINT('Ctrl Pts',(17.3142977632659,-14.8272850675379,
12.));
#220217=CARTESIAN_POINT('Ctrl Pts',(17.3217177462101,-14.8358336004197,
0.));
#220218=CARTESIAN_POINT('Ctrl Pts',(17.3217177462101,-14.8358336004197,
12.));
#220219=CARTESIAN_POINT('Ctrl Pts',(17.3292363662605,-14.8445548643508,
0.));
#220220=CARTESIAN_POINT('Ctrl Pts',(17.3292363662605,-14.8445548643508,
12.));
#220221=CARTESIAN_POINT('Ctrl Pts',(17.336850936485,-14.8534474245434,0.));
#220222=CARTESIAN_POINT('Ctrl Pts',(17.336850936485,-14.8534474245434,12.));
#220223=CARTESIAN_POINT('Ctrl Pts',(17.3445588463474,-14.8625098843417,
0.));
#220224=CARTESIAN_POINT('Ctrl Pts',(17.3445588463474,-14.8625098843417,
12.));
#220225=CARTESIAN_POINT('Ctrl Pts',(17.3523575568645,-14.8717408826956,
0.));
#220226=CARTESIAN_POINT('Ctrl Pts',(17.3523575568645,-14.8717408826956,
12.));
#220227=CARTESIAN_POINT('Ctrl Pts',(17.3602445978161,-14.8811390927423,
0.));
#220228=CARTESIAN_POINT('Ctrl Pts',(17.3602445978161,-14.8811390927423,
12.));
#220229=CARTESIAN_POINT('Ctrl Pts',(17.3682175653235,-14.8907032205788,
0.));
#220230=CARTESIAN_POINT('Ctrl Pts',(17.3682175653235,-14.8907032205788,
12.));
#220231=CARTESIAN_POINT('Ctrl Pts',(17.3762741193076,-14.900432003961,0.));
#220232=CARTESIAN_POINT('Ctrl Pts',(17.3762741193076,-14.900432003961,12.));
#220233=CARTESIAN_POINT('Ctrl Pts',(17.3844119809824,-14.9103242110057,
0.));
#220234=CARTESIAN_POINT('Ctrl Pts',(17.3844119809824,-14.9103242110057,
12.));
#220235=CARTESIAN_POINT('Ctrl Pts',(17.3926289303986,-14.9203786389342,
0.));
#220236=CARTESIAN_POINT('Ctrl Pts',(17.3926289303986,-14.9203786389342,
12.));
#220237=CARTESIAN_POINT('Ctrl Pts',(17.4009228040749,-14.9305941128757,
0.));
#220238=CARTESIAN_POINT('Ctrl Pts',(17.4009228040749,-14.9305941128757,
12.));
#220239=CARTESIAN_POINT('Ctrl Pts',(17.4092914926071,-14.940969484645,0.));
#220240=CARTESIAN_POINT('Ctrl Pts',(17.4092914926071,-14.940969484645,12.));
#220241=CARTESIAN_POINT('Ctrl Pts',(17.4177329382828,-14.9515036315143,
0.));
#220242=CARTESIAN_POINT('Ctrl Pts',(17.4177329382828,-14.9515036315143,
12.));
#220243=CARTESIAN_POINT('Ctrl Pts',(17.426245132709,-14.9621954549827,0.));
#220244=CARTESIAN_POINT('Ctrl Pts',(17.426245132709,-14.9621954549827,12.));
#220245=CARTESIAN_POINT('Ctrl Pts',(17.4348261151396,-14.9730438799452,
0.));
#220246=CARTESIAN_POINT('Ctrl Pts',(17.4348261151396,-14.9730438799452,
12.));
#220247=CARTESIAN_POINT('Ctrl Pts',(17.4434739707773,-14.9840478538358,
0.));
#220248=CARTESIAN_POINT('Ctrl Pts',(17.4434739707773,-14.9840478538358,
12.));
#220249=CARTESIAN_POINT('Ctrl Pts',(17.4521868291004,-14.9952063457778,
0.));
#220250=CARTESIAN_POINT('Ctrl Pts',(17.4521868291004,-14.9952063457778,
12.));
#220251=CARTESIAN_POINT('Ctrl Pts',(17.4609628621418,-15.0065183456921,
0.));
#220252=CARTESIAN_POINT('Ctrl Pts',(17.4609628621418,-15.0065183456921,
12.));
#220253=CARTESIAN_POINT('Ctrl Pts',(17.4698002829357,-15.0179828635086,
0.));
#220254=CARTESIAN_POINT('Ctrl Pts',(17.4698002829357,-15.0179828635086,
12.));
#220255=CARTESIAN_POINT('Ctrl Pts',(17.4786973441417,-15.029598928488,0.));
#220256=CARTESIAN_POINT('Ctrl Pts',(17.4786973441417,-15.029598928488,12.));
#220257=CARTESIAN_POINT('Ctrl Pts',(17.4876523366178,-15.0413655884993,
0.));
#220258=CARTESIAN_POINT('Ctrl Pts',(17.4876523366178,-15.0413655884993,
12.));
#220259=CARTESIAN_POINT('Ctrl Pts',(17.4966635880245,-15.0532819093085,
0.));
#220260=CARTESIAN_POINT('Ctrl Pts',(17.4966635880245,-15.0532819093085,
12.));
#220261=CARTESIAN_POINT('Ctrl Pts',(17.5057294613874,-15.0653469738306,
0.));
#220262=CARTESIAN_POINT('Ctrl Pts',(17.5057294613874,-15.0653469738306,
12.));
#220263=CARTESIAN_POINT('Ctrl Pts',(17.5148483539683,-15.0775598815748,
0.));
#220264=CARTESIAN_POINT('Ctrl Pts',(17.5148483539683,-15.0775598815748,
12.));
#220265=CARTESIAN_POINT('Ctrl Pts',(17.5240186961788,-15.0899197481082,
0.));
#220266=CARTESIAN_POINT('Ctrl Pts',(17.5240186961788,-15.0899197481082,
12.));
#220267=CARTESIAN_POINT('Ctrl Pts',(17.5332389504829,-15.1024257045033,
0.));
#220268=CARTESIAN_POINT('Ctrl Pts',(17.5332389504829,-15.1024257045033,
12.));
#220269=CARTESIAN_POINT('Ctrl Pts',(17.5425076102966,-15.1150768967729,
0.));
#220270=CARTESIAN_POINT('Ctrl Pts',(17.5425076102966,-15.1150768967729,
12.));
#220271=CARTESIAN_POINT('Ctrl Pts',(17.5518231989122,-15.127872485314,0.));
#220272=CARTESIAN_POINT('Ctrl Pts',(17.5518231989122,-15.127872485314,12.));
#220273=CARTESIAN_POINT('Ctrl Pts',(17.5611842686196,-15.1408116444877,
0.));
#220274=CARTESIAN_POINT('Ctrl Pts',(17.5611842686196,-15.1408116444877,
12.));
#220275=CARTESIAN_POINT('Ctrl Pts',(17.570589399803,-15.1538935621715,0.));
#220276=CARTESIAN_POINT('Ctrl Pts',(17.570589399803,-15.1538935621715,12.));
#220277=CARTESIAN_POINT('Ctrl Pts',(17.5800372000539,-15.1671174393136,
0.));
#220278=CARTESIAN_POINT('Ctrl Pts',(17.5800372000539,-15.1671174393136,
12.));
#220279=CARTESIAN_POINT('Ctrl Pts',(17.5895263032592,-15.1804824894605,
0.));
#220280=CARTESIAN_POINT('Ctrl Pts',(17.5895263032592,-15.1804824894605,
12.));
#220281=CARTESIAN_POINT('Ctrl Pts',(17.5990553687595,-15.1939879383268,
0.));
#220282=CARTESIAN_POINT('Ctrl Pts',(17.5990553687595,-15.1939879383268,
12.));
#220283=CARTESIAN_POINT('Ctrl Pts',(17.6086230806497,-15.2076330234686,
0.));
#220284=CARTESIAN_POINT('Ctrl Pts',(17.6086230806497,-15.2076330234686,
12.));
#220285=CARTESIAN_POINT('Ctrl Pts',(17.6182281470467,-15.22141699392,0.));
#220286=CARTESIAN_POINT('Ctrl Pts',(17.6182281470467,-15.22141699392,12.));
#220287=CARTESIAN_POINT('Ctrl Pts',(17.6278692993765,-15.2353391098367,
0.));
#220288=CARTESIAN_POINT('Ctrl Pts',(17.6278692993765,-15.2353391098367,
12.));
#220289=CARTESIAN_POINT('Ctrl Pts',(17.637545291637,-15.2493986421091,0.));
#220290=CARTESIAN_POINT('Ctrl Pts',(17.637545291637,-15.2493986421091,12.));
#220291=CARTESIAN_POINT('Ctrl Pts',(17.6472548997329,-15.263594872029,0.));
#220292=CARTESIAN_POINT('Ctrl Pts',(17.6472548997329,-15.263594872029,12.));
#220293=CARTESIAN_POINT('Ctrl Pts',(17.6569969209,-15.2779270910238,0.));
#220294=CARTESIAN_POINT('Ctrl Pts',(17.6569969209,-15.2779270910238,12.));
#220295=CARTESIAN_POINT('Ctrl Pts',(17.6667701731041,-15.2923946003598,
0.));
#220296=CARTESIAN_POINT('Ctrl Pts',(17.6667701731041,-15.2923946003598,
12.));
#220297=CARTESIAN_POINT('Ctrl Pts',(17.6765734944559,-15.3069967108501,
0.));
#220298=CARTESIAN_POINT('Ctrl Pts',(17.6765734944559,-15.3069967108501,
12.));
#220299=CARTESIAN_POINT('Ctrl Pts',(17.6864057426052,-15.3217327425341,
0.));
#220300=CARTESIAN_POINT('Ctrl Pts',(17.6864057426052,-15.3217327425341,
12.));
#220301=CARTESIAN_POINT('Ctrl Pts',(17.6962657941984,-15.3366020244069,
0.));
#220302=CARTESIAN_POINT('Ctrl Pts',(17.6962657941984,-15.3366020244069,
12.));
#220303=CARTESIAN_POINT('Ctrl Pts',(17.7061525444044,-15.3516038942064,
0.));
#220304=CARTESIAN_POINT('Ctrl Pts',(17.7061525444044,-15.3516038942064,
12.));
#220305=CARTESIAN_POINT('Ctrl Pts',(17.7160649064208,-15.3667376981702,
0.));
#220306=CARTESIAN_POINT('Ctrl Pts',(17.7160649064208,-15.3667376981702,
12.));
#220307=CARTESIAN_POINT('Ctrl Pts',(17.7260018109923,-15.3820027907965,
0.));
#220308=CARTESIAN_POINT('Ctrl Pts',(17.7260018109923,-15.3820027907965,
12.));
#220309=CARTESIAN_POINT('Ctrl Pts',(17.7359622059143,-15.3973985345796,
0.));
#220310=CARTESIAN_POINT('Ctrl Pts',(17.7359622059143,-15.3973985345796,
12.));
#220311=CARTESIAN_POINT('Ctrl Pts',(17.7459450555803,-15.4129242997828,
0.));
#220312=CARTESIAN_POINT('Ctrl Pts',(17.7459450555803,-15.4129242997828,
12.));
#220313=CARTESIAN_POINT('Ctrl Pts',(17.7559493405871,-15.4285794642658,
0.));
#220314=CARTESIAN_POINT('Ctrl Pts',(17.7559493405871,-15.4285794642658,
12.));
#220315=CARTESIAN_POINT('Ctrl Pts',(17.765974057326,-15.4443634132865,0.));
#220316=CARTESIAN_POINT('Ctrl Pts',(17.765974057326,-15.4443634132865,12.));
#220317=CARTESIAN_POINT('Ctrl Pts',(17.7760182175817,-15.4602755393019,
0.));
#220318=CARTESIAN_POINT('Ctrl Pts',(17.7760182175817,-15.4602755393019,
12.));
#220319=CARTESIAN_POINT('Ctrl Pts',(17.7860808481229,-15.4763152417506,
0.));
#220320=CARTESIAN_POINT('Ctrl Pts',(17.7860808481229,-15.4763152417506,
12.));
#220321=CARTESIAN_POINT('Ctrl Pts',(17.7961609903161,-15.4924819268529,
0.));
#220322=CARTESIAN_POINT('Ctrl Pts',(17.7961609903161,-15.4924819268529,
12.));
#220323=CARTESIAN_POINT('Ctrl Pts',(17.8062576997964,-15.5087750074728,
0.));
#220324=CARTESIAN_POINT('Ctrl Pts',(17.8062576997964,-15.5087750074728,
12.));
#220325=CARTESIAN_POINT('Ctrl Pts',(17.8163700461263,-15.5251939029558,
0.));
#220326=CARTESIAN_POINT('Ctrl Pts',(17.8163700461263,-15.5251939029558,
12.));
#220327=CARTESIAN_POINT('Ctrl Pts',(17.8264971124606,-15.5417380389639,
0.));
#220328=CARTESIAN_POINT('Ctrl Pts',(17.8264971124606,-15.5417380389639,
12.));
#220329=CARTESIAN_POINT('Ctrl Pts',(17.8366379952078,-15.5584068472976,
0.));
#220330=CARTESIAN_POINT('Ctrl Pts',(17.8366379952078,-15.5584068472976,
12.));
#220331=CARTESIAN_POINT('Ctrl Pts',(17.8467918036976,-15.5751997657153,
0.));
#220332=CARTESIAN_POINT('Ctrl Pts',(17.8467918036976,-15.5751997657153,
12.));
#220333=CARTESIAN_POINT('Ctrl Pts',(17.8569576598996,-15.5921162378183,
0.));
#220334=CARTESIAN_POINT('Ctrl Pts',(17.8569576598996,-15.5921162378183,
12.));
#220335=CARTESIAN_POINT('Ctrl Pts',(17.8671346981388,-15.6091557129205,
0.));
#220336=CARTESIAN_POINT('Ctrl Pts',(17.8671346981388,-15.6091557129205,
12.));
#220337=CARTESIAN_POINT('Ctrl Pts',(17.8773220648125,-15.6263176459107,
0.));
#220338=CARTESIAN_POINT('Ctrl Pts',(17.8773220648125,-15.6263176459107,
12.));
#220339=CARTESIAN_POINT('Ctrl Pts',(17.8875189181095,-15.6436014971088,
0.));
#220340=CARTESIAN_POINT('Ctrl Pts',(17.8875189181095,-15.6436014971088,
12.));
#220341=CARTESIAN_POINT('Ctrl Pts',(17.8977244277247,-15.6610067321036,
0.));
#220342=CARTESIAN_POINT('Ctrl Pts',(17.8977244277247,-15.6610067321036,
12.));
#220343=CARTESIAN_POINT('Ctrl Pts',(17.9079377746118,-15.6785328216467,
0.));
#220344=CARTESIAN_POINT('Ctrl Pts',(17.9079377746118,-15.6785328216467,
12.));
#220345=CARTESIAN_POINT('Ctrl Pts',(17.918158150746,-15.6961792415526,0.));
#220346=CARTESIAN_POINT('Ctrl Pts',(17.918158150746,-15.6961792415526,12.));
#220347=CARTESIAN_POINT('Ctrl Pts',(17.9283847588837,-15.713945472584,0.));
#220348=CARTESIAN_POINT('Ctrl Pts',(17.9283847588837,-15.713945472584,12.));
#220349=CARTESIAN_POINT('Ctrl Pts',(17.9386168123261,-15.7318310003334,
0.));
#220350=CARTESIAN_POINT('Ctrl Pts',(17.9386168123261,-15.7318310003334,
12.));
#220351=CARTESIAN_POINT('Ctrl Pts',(17.9488535346776,-15.7498353150856,
0.));
#220352=CARTESIAN_POINT('Ctrl Pts',(17.9488535346776,-15.7498353150856,
12.));
#220353=CARTESIAN_POINT('Ctrl Pts',(17.9590941596236,-15.7679579117072,
0.));
#220354=CARTESIAN_POINT('Ctrl Pts',(17.9590941596236,-15.7679579117072,
12.));
#220355=CARTESIAN_POINT('Ctrl Pts',(17.9693379307297,-15.786198289572,0.));
#220356=CARTESIAN_POINT('Ctrl Pts',(17.9693379307297,-15.786198289572,12.));
#220357=CARTESIAN_POINT('Ctrl Pts',(17.9795841012383,-15.8045559524674,
0.));
#220358=CARTESIAN_POINT('Ctrl Pts',(17.9795841012383,-15.8045559524674,
12.));
#220359=CARTESIAN_POINT('Ctrl Pts',(17.9898319338664,-15.8230304084963,
0.));
#220360=CARTESIAN_POINT('Ctrl Pts',(17.9898319338664,-15.8230304084963,
12.));
#220361=CARTESIAN_POINT('Ctrl Pts',(18.0000807006055,-15.8416211699682,
0.));
#220362=CARTESIAN_POINT('Ctrl Pts',(18.0000807006055,-15.8416211699682,
12.));
#220363=CARTESIAN_POINT('Ctrl Pts',(18.010329682521,-15.8603277532834,0.));
#220364=CARTESIAN_POINT('Ctrl Pts',(18.010329682521,-15.8603277532834,12.));
#220365=CARTESIAN_POINT('Ctrl Pts',(18.0205781695773,-15.8791496788685,
0.));
#220366=CARTESIAN_POINT('Ctrl Pts',(18.0205781695773,-15.8791496788685,
12.));
#220367=CARTESIAN_POINT('Ctrl Pts',(18.0308254604638,-15.8980864711043,
0.));
#220368=CARTESIAN_POINT('Ctrl Pts',(18.0308254604638,-15.8980864711043,
12.));
#220369=CARTESIAN_POINT('Ctrl Pts',(18.0410708624208,-15.9171376582436,
0.));
#220370=CARTESIAN_POINT('Ctrl Pts',(18.0410708624208,-15.9171376582436,
12.));
#220371=CARTESIAN_POINT('Ctrl Pts',(18.0513136910691,-15.9363027723244,
0.));
#220372=CARTESIAN_POINT('Ctrl Pts',(18.0513136910691,-15.9363027723244,
12.));
#220373=CARTESIAN_POINT('Ctrl Pts',(18.061553270236,-15.9555813490645,0.));
#220374=CARTESIAN_POINT('Ctrl Pts',(18.061553270236,-15.9555813490645,12.));
#220375=CARTESIAN_POINT('Ctrl Pts',(18.071788931796,-15.9749729277848,0.));
#220376=CARTESIAN_POINT('Ctrl Pts',(18.071788931796,-15.9749729277848,12.));
#220377=CARTESIAN_POINT('Ctrl Pts',(18.0820200155239,-15.9944770513616,
0.));
#220378=CARTESIAN_POINT('Ctrl Pts',(18.0820200155239,-15.9944770513616,
12.));
#220379=CARTESIAN_POINT('Ctrl Pts',(18.0922458689464,-16.0140932661612,
0.));
#220380=CARTESIAN_POINT('Ctrl Pts',(18.0922458689464,-16.0140932661612,
12.));
#220381=CARTESIAN_POINT('Ctrl Pts',(18.1024658471966,-16.0338211219694,
0.));
#220382=CARTESIAN_POINT('Ctrl Pts',(18.1024658471966,-16.0338211219694,
12.));
#220383=CARTESIAN_POINT('Ctrl Pts',(18.1126793128688,-16.0536601719124,
0.));
#220384=CARTESIAN_POINT('Ctrl Pts',(18.1126793128688,-16.0536601719124,
12.));
#220385=CARTESIAN_POINT('Ctrl Pts',(18.1228856358746,-16.0736099723664,
0.));
#220386=CARTESIAN_POINT('Ctrl Pts',(18.1228856358746,-16.0736099723664,
12.));
#220387=CARTESIAN_POINT('Ctrl Pts',(18.1330841933099,-16.0936700829108,
0.));
#220388=CARTESIAN_POINT('Ctrl Pts',(18.1330841933099,-16.0936700829108,
12.));
#220389=CARTESIAN_POINT('Ctrl Pts',(18.1432743693231,-16.113840066279,0.));
#220390=CARTESIAN_POINT('Ctrl Pts',(18.1432743693231,-16.113840066279,12.));
#220391=CARTESIAN_POINT('Ctrl Pts',(18.153455554985,-16.1341194882987,0.));
#220392=CARTESIAN_POINT('Ctrl Pts',(18.153455554985,-16.1341194882987,12.));
#220393=CARTESIAN_POINT('Ctrl Pts',(18.1636271481616,-16.1545079178261,
0.));
#220394=CARTESIAN_POINT('Ctrl Pts',(18.1636271481616,-16.1545079178261,
12.));
#220395=CARTESIAN_POINT('Ctrl Pts',(18.1737885533852,-16.1750049266673,
0.));
#220396=CARTESIAN_POINT('Ctrl Pts',(18.1737885533852,-16.1750049266673,
12.));
#220397=CARTESIAN_POINT('Ctrl Pts',(18.1839391817335,-16.1956100895076,
0.));
#220398=CARTESIAN_POINT('Ctrl Pts',(18.1839391817335,-16.1956100895076,
12.));
#220399=CARTESIAN_POINT('Ctrl Pts',(18.1940784507232,-16.2163229838878,
0.));
#220400=CARTESIAN_POINT('Ctrl Pts',(18.1940784507232,-16.2163229838878,
12.));
#220401=CARTESIAN_POINT('Ctrl Pts',(18.2042057842037,-16.237143190164,0.));
#220402=CARTESIAN_POINT('Ctrl Pts',(18.2042057842037,-16.237143190164,12.));
#220403=CARTESIAN_POINT('Ctrl Pts',(18.214320612253,-16.2580702914615,0.));
#220404=CARTESIAN_POINT('Ctrl Pts',(18.214320612253,-16.2580702914615,12.));
#220405=CARTESIAN_POINT('Ctrl Pts',(18.2244223710745,-16.2791038736223,
0.));
#220406=CARTESIAN_POINT('Ctrl Pts',(18.2244223710745,-16.2791038736223,
12.));
#220407=CARTESIAN_POINT('Ctrl Pts',(18.2345105028981,-16.3002435251378,
0.));
#220408=CARTESIAN_POINT('Ctrl Pts',(18.2345105028981,-16.3002435251378,
12.));
#220409=CARTESIAN_POINT('Ctrl Pts',(18.2445844558742,-16.3214888370988,
0.));
#220410=CARTESIAN_POINT('Ctrl Pts',(18.2445844558742,-16.3214888370988,
12.));
#220411=CARTESIAN_POINT('Ctrl Pts',(18.2546436839609,-16.342839403159,0.));
#220412=CARTESIAN_POINT('Ctrl Pts',(18.2546436839609,-16.342839403159,12.));
#220413=CARTESIAN_POINT('Ctrl Pts',(18.2646876468169,-16.3642948194869,
0.));
#220414=CARTESIAN_POINT('Ctrl Pts',(18.2646876468169,-16.3642948194869,
12.));
#220415=CARTESIAN_POINT('Ctrl Pts',(18.2747158096934,-16.385854684708,0.));
#220416=CARTESIAN_POINT('Ctrl Pts',(18.2747158096934,-16.385854684708,12.));
#220417=CARTESIAN_POINT('Ctrl Pts',(18.2847276433308,-16.4075185998454,
0.));
#220418=CARTESIAN_POINT('Ctrl Pts',(18.2847276433308,-16.4075185998454,
12.));
#220419=CARTESIAN_POINT('Ctrl Pts',(18.2947226238509,-16.4292861682377,
0.));
#220420=CARTESIAN_POINT('Ctrl Pts',(18.2947226238509,-16.4292861682377,
12.));
#220421=CARTESIAN_POINT('Ctrl Pts',(18.3047002326858,-16.4511569955231,
0.));
#220422=CARTESIAN_POINT('Ctrl Pts',(18.3047002326858,-16.4511569955231,
12.));
#220423=CARTESIAN_POINT('Ctrl Pts',(18.3146599565229,-16.4731306896439,
0.));
#220424=CARTESIAN_POINT('Ctrl Pts',(18.3146599565229,-16.4731306896439,
12.));
#220425=CARTESIAN_POINT('Ctrl Pts',(18.3246012872468,-16.4952068608344,
0.));
#220426=CARTESIAN_POINT('Ctrl Pts',(18.3246012872468,-16.4952068608344,
12.));
#220427=CARTESIAN_POINT('Ctrl Pts',(18.3345237218864,-16.5173851216045,
0.));
#220428=CARTESIAN_POINT('Ctrl Pts',(18.3345237218864,-16.5173851216045,
12.));
#220429=CARTESIAN_POINT('Ctrl Pts',(18.3444267625601,-16.5396650867139,
0.));
#220430=CARTESIAN_POINT('Ctrl Pts',(18.3444267625601,-16.5396650867139,
12.));
#220431=CARTESIAN_POINT('Ctrl Pts',(18.3543099164331,-16.5620463731414,
0.));
#220432=CARTESIAN_POINT('Ctrl Pts',(18.3543099164331,-16.5620463731414,
12.));
#220433=CARTESIAN_POINT('Ctrl Pts',(18.364172695589,-16.5845286000218,0.));
#220434=CARTESIAN_POINT('Ctrl Pts',(18.364172695589,-16.5845286000218,12.));
#220435=CARTESIAN_POINT('Ctrl Pts',(18.3740146168879,-16.6071113885711,
0.));
#220436=CARTESIAN_POINT('Ctrl Pts',(18.3740146168879,-16.6071113885711,
12.));
#220437=CARTESIAN_POINT('Ctrl Pts',(18.3838352018327,-16.6297943620056,
0.));
#220438=CARTESIAN_POINT('Ctrl Pts',(18.3838352018327,-16.6297943620056,
12.));
#220439=CARTESIAN_POINT('Ctrl Pts',(18.3936339764332,-16.6525771454513,
0.));
#220440=CARTESIAN_POINT('Ctrl Pts',(18.3936339764332,-16.6525771454513,
12.));
#220441=CARTESIAN_POINT('Ctrl Pts',(18.4034104710789,-16.6754593658513,
0.));
#220442=CARTESIAN_POINT('Ctrl Pts',(18.4034104710789,-16.6754593658513,
12.));
#220443=CARTESIAN_POINT('Ctrl Pts',(18.4131642203989,-16.698440651849,0.));
#220444=CARTESIAN_POINT('Ctrl Pts',(18.4131642203989,-16.698440651849,12.));
#220445=CARTESIAN_POINT('Ctrl Pts',(18.4228947633186,-16.7215206338818,
0.));
#220446=CARTESIAN_POINT('Ctrl Pts',(18.4228947633186,-16.7215206338818,
12.));
#220447=CARTESIAN_POINT('Ctrl Pts',(18.4326016431392,-16.7446989442882,
0.));
#220448=CARTESIAN_POINT('Ctrl Pts',(18.4326016431392,-16.7446989442882,
12.));
#220449=CARTESIAN_POINT('Ctrl Pts',(18.4422844076099,-16.7679752173992,
0.));
#220450=CARTESIAN_POINT('Ctrl Pts',(18.4422844076099,-16.7679752173992,
12.));
#220451=CARTESIAN_POINT('Ctrl Pts',(18.4519426090124,-16.791349089629,0.));
#220452=CARTESIAN_POINT('Ctrl Pts',(18.4519426090124,-16.791349089629,12.));
#220453=CARTESIAN_POINT('Ctrl Pts',(18.4615758042305,-16.8148201995472,
0.));
#220454=CARTESIAN_POINT('Ctrl Pts',(18.4615758042305,-16.8148201995472,
12.));
#220455=CARTESIAN_POINT('Ctrl Pts',(18.4711835548622,-16.8383881879707,
0.));
#220456=CARTESIAN_POINT('Ctrl Pts',(18.4711835548622,-16.8383881879707,
12.));
#220457=CARTESIAN_POINT('Ctrl Pts',(18.4807654268769,-16.8620526977169,
0.));
#220458=CARTESIAN_POINT('Ctrl Pts',(18.4807654268769,-16.8620526977169,
12.));
#220459=CARTESIAN_POINT('Ctrl Pts',(18.4903209902226,-16.8858133733086,
0.));
#220460=CARTESIAN_POINT('Ctrl Pts',(18.4903209902226,-16.8858133733086,
12.));
#220461=CARTESIAN_POINT('Ctrl Pts',(18.4998498184619,-16.9096698606942,
0.));
#220462=CARTESIAN_POINT('Ctrl Pts',(18.4998498184619,-16.9096698606942,
12.));
#220463=CARTESIAN_POINT('Ctrl Pts',(18.5093514883835,-16.9336218069353,
0.));
#220464=CARTESIAN_POINT('Ctrl Pts',(18.5093514883835,-16.9336218069353,
12.));
#220465=CARTESIAN_POINT('Ctrl Pts',(18.518825579666,-16.957668859934,0.));
#220466=CARTESIAN_POINT('Ctrl Pts',(18.518825579666,-16.957668859934,12.));
#220467=CARTESIAN_POINT('Ctrl Pts',(18.5282716744198,-16.9818106680382,
0.));
#220468=CARTESIAN_POINT('Ctrl Pts',(18.5282716744198,-16.9818106680382,
12.));
#220469=CARTESIAN_POINT('Ctrl Pts',(18.5376893576961,-17.0060468805099,
0.));
#220470=CARTESIAN_POINT('Ctrl Pts',(18.5376893576961,-17.0060468805099,
12.));
#220471=CARTESIAN_POINT('Ctrl Pts',(18.5470782182089,-17.030377148174,0.));
#220472=CARTESIAN_POINT('Ctrl Pts',(18.5470782182089,-17.030377148174,12.));
#220473=CARTESIAN_POINT('Ctrl Pts',(18.5564378489628,-17.0548011239751,
0.));
#220474=CARTESIAN_POINT('Ctrl Pts',(18.5564378489628,-17.0548011239751,
12.));
#220475=CARTESIAN_POINT('Ctrl Pts',(18.5657678479788,-17.0793184636079,
0.));
#220476=CARTESIAN_POINT('Ctrl Pts',(18.5657678479788,-17.0793184636079,
12.));
#220477=CARTESIAN_POINT('Ctrl Pts',(18.5750678188543,-17.1039288260002,
0.));
#220478=CARTESIAN_POINT('Ctrl Pts',(18.5750678188543,-17.1039288260002,
12.));
#220479=CARTESIAN_POINT('Ctrl Pts',(18.5843373717253,-17.1286318741185,
0.));
#220480=CARTESIAN_POINT('Ctrl Pts',(18.5843373717253,-17.1286318741185,
12.));
#220481=CARTESIAN_POINT('Ctrl Pts',(18.5935761222833,-17.1534272741646,
0.));
#220482=CARTESIAN_POINT('Ctrl Pts',(18.5935761222833,-17.1534272741646,
12.));
#220483=CARTESIAN_POINT('Ctrl Pts',(18.6027836898826,-17.1783146940131,
0.));
#220484=CARTESIAN_POINT('Ctrl Pts',(18.6027836898826,-17.1783146940131,
12.));
#220485=CARTESIAN_POINT('Ctrl Pts',(18.6119596959957,-17.2032938019288,
0.));
#220486=CARTESIAN_POINT('Ctrl Pts',(18.6119596959957,-17.2032938019288,
12.));
#220487=CARTESIAN_POINT('Ctrl Pts',(18.6211037624041,-17.2283642650519,
0.));
#220488=CARTESIAN_POINT('Ctrl Pts',(18.6211037624041,-17.2283642650519,
12.));
#220489=CARTESIAN_POINT('Ctrl Pts',(18.630215509794,-17.2535257482186,0.));
#220490=CARTESIAN_POINT('Ctrl Pts',(18.630215509794,-17.2535257482186,12.));
#220491=CARTESIAN_POINT('Ctrl Pts',(18.639294555474,-17.278777912021,0.));
#220492=CARTESIAN_POINT('Ctrl Pts',(18.639294555474,-17.278777912021,12.));
#220493=CARTESIAN_POINT('Ctrl Pts',(18.6483405141853,-17.3041204135069,
0.));
#220494=CARTESIAN_POINT('Ctrl Pts',(18.6483405141853,-17.3041204135069,
12.));
#220495=CARTESIAN_POINT('Ctrl Pts',(18.6573530024019,-17.3295529098612,
0.));
#220496=CARTESIAN_POINT('Ctrl Pts',(18.6573530024019,-17.3295529098612,
12.));
#220497=CARTESIAN_POINT('Ctrl Pts',(18.6663316416569,-17.3550750612438,
0.));
#220498=CARTESIAN_POINT('Ctrl Pts',(18.6663316416569,-17.3550750612438,
12.));
#220499=CARTESIAN_POINT('Ctrl Pts',(18.6752760624045,-17.3806865340744,
0.));
#220500=CARTESIAN_POINT('Ctrl Pts',(18.6752760624045,-17.3806865340744,
12.));
#220501=CARTESIAN_POINT('Ctrl Pts',(18.6841859073472,-17.4063870038563,
0.));
#220502=CARTESIAN_POINT('Ctrl Pts',(18.6841859073472,-17.4063870038563,
12.));
#220503=CARTESIAN_POINT('Ctrl Pts',(18.6930608357421,-17.4321761588148,
0.));
#220504=CARTESIAN_POINT('Ctrl Pts',(18.6930608357421,-17.4321761588148,
12.));
#220505=CARTESIAN_POINT('Ctrl Pts',(18.7019005250322,-17.4580537012764,
0.));
#220506=CARTESIAN_POINT('Ctrl Pts',(18.7019005250322,-17.4580537012764,
12.));
#220507=CARTESIAN_POINT('Ctrl Pts',(18.7107046613941,-17.4840193397176,
0.));
#220508=CARTESIAN_POINT('Ctrl Pts',(18.7107046613941,-17.4840193397176,
12.));
#220509=CARTESIAN_POINT('Ctrl Pts',(18.7194729318127,-17.5100727820891,
0.));
#220510=CARTESIAN_POINT('Ctrl Pts',(18.7194729318127,-17.5100727820891,
12.));
#220511=CARTESIAN_POINT('Ctrl Pts',(18.728205015716,-17.5362137287604,0.));
#220512=CARTESIAN_POINT('Ctrl Pts',(18.728205015716,-17.5362137287604,12.));
#220513=CARTESIAN_POINT('Ctrl Pts',(18.7369005764558,-17.5624418653248,
0.));
#220514=CARTESIAN_POINT('Ctrl Pts',(18.7369005764558,-17.5624418653248,
12.));
#220515=CARTESIAN_POINT('Ctrl Pts',(18.7455592536667,-17.5887568561361,
0.));
#220516=CARTESIAN_POINT('Ctrl Pts',(18.7455592536667,-17.5887568561361,
12.));
#220517=CARTESIAN_POINT('Ctrl Pts',(18.7541806530935,-17.6151583356989,
0.));
#220518=CARTESIAN_POINT('Ctrl Pts',(18.7541806530935,-17.6151583356989,
12.));
#220519=CARTESIAN_POINT('Ctrl Pts',(18.7627643613139,-17.6416459210646,
0.));
#220520=CARTESIAN_POINT('Ctrl Pts',(18.7627643613139,-17.6416459210646,
12.));
#220521=CARTESIAN_POINT('Ctrl Pts',(18.7713099642673,-17.6682192274197,
0.));
#220522=CARTESIAN_POINT('Ctrl Pts',(18.7713099642673,-17.6682192274197,
12.));
#220523=CARTESIAN_POINT('Ctrl Pts',(18.7798170641305,-17.6948778822982,
0.));
#220524=CARTESIAN_POINT('Ctrl Pts',(18.7798170641305,-17.6948778822982,
12.));
#220525=CARTESIAN_POINT('Ctrl Pts',(18.7882852976016,-17.7216215409019,
0.));
#220526=CARTESIAN_POINT('Ctrl Pts',(18.7882852976016,-17.7216215409019,
12.));
#220527=CARTESIAN_POINT('Ctrl Pts',(18.7967143519444,-17.7484498996916,
0.));
#220528=CARTESIAN_POINT('Ctrl Pts',(18.7967143519444,-17.7484498996916,
12.));
#220529=CARTESIAN_POINT('Ctrl Pts',(18.8051039860543,-17.7753627137898,
0.));
#220530=CARTESIAN_POINT('Ctrl Pts',(18.8051039860543,-17.7753627137898,
12.));
#220531=CARTESIAN_POINT('Ctrl Pts',(18.8134540340581,-17.8023598011135,
0.));
#220532=CARTESIAN_POINT('Ctrl Pts',(18.8134540340581,-17.8023598011135,
12.));
#220533=CARTESIAN_POINT('Ctrl Pts',(18.8217643886368,-17.8294410311105,
0.));
#220534=CARTESIAN_POINT('Ctrl Pts',(18.8217643886368,-17.8294410311105,
12.));
#220535=CARTESIAN_POINT('Ctrl Pts',(18.8300349896187,-17.8566063174871,
0.));
#220536=CARTESIAN_POINT('Ctrl Pts',(18.8300349896187,-17.8566063174871,
12.));
#220537=CARTESIAN_POINT('Ctrl Pts',(18.8366196462746,-17.8784057509434,
0.));
#220538=CARTESIAN_POINT('Ctrl Pts',(18.8366196462746,-17.8784057509434,
12.));
#220539=CARTESIAN_POINT('Ctrl Pts',(18.8415402351882,-17.8947931177853,
0.));
#220540=CARTESIAN_POINT('Ctrl Pts',(18.8415402351882,-17.8947931177853,
12.));
#220541=CARTESIAN_POINT('Ctrl Pts',(18.8448126709726,-17.9057348246611,
0.));
#220542=CARTESIAN_POINT('Ctrl Pts',(18.8448126709726,-17.9057348246611,
12.));
#220543=CARTESIAN_POINT('Ctrl Pts',(18.8464468996588,-17.9112098770111,
0.));
#220544=CARTESIAN_POINT('Ctrl Pts',(18.8464468996588,-17.9112098770111,
12.));
#220545=CARTESIAN_POINT('',(18.8464468996588,-17.9112098770111,0.));
#220546=CARTESIAN_POINT('Ctrl Pts',(17.1452095830632,-14.6513681262571,
0.));
#220547=CARTESIAN_POINT('Ctrl Pts',(17.1452153999142,-14.6513711852843,
0.));
#220548=CARTESIAN_POINT('Ctrl Pts',(17.1452600887037,-14.6514066997196,
0.));
#220549=CARTESIAN_POINT('Ctrl Pts',(17.1454262858043,-14.6515481598068,
0.));
#220550=CARTESIAN_POINT('Ctrl Pts',(17.1458462295271,-14.6519131634508,
0.));
#220551=CARTESIAN_POINT('Ctrl Pts',(17.1466998098673,-14.6526624064978,
0.));
#220552=CARTESIAN_POINT('Ctrl Pts',(17.147876394491,-14.6537016966184,0.));
#220553=CARTESIAN_POINT('Ctrl Pts',(17.1493641837558,-14.655024862281,0.));
#220554=CARTESIAN_POINT('Ctrl Pts',(17.1511476869496,-14.6566237952435,
0.));
#220555=CARTESIAN_POINT('Ctrl Pts',(17.1532107762718,-14.6584900555302,
0.));
#220556=CARTESIAN_POINT('Ctrl Pts',(17.1555401986401,-14.6606167169642,
0.));
#220557=CARTESIAN_POINT('Ctrl Pts',(17.1581262646789,-14.6629987285992,
0.));
#220558=CARTESIAN_POINT('Ctrl Pts',(17.1609609517369,-14.6656319165057,
0.));
#220559=CARTESIAN_POINT('Ctrl Pts',(17.1640366762305,-14.6685123374423,
0.));
#220560=CARTESIAN_POINT('Ctrl Pts',(17.167344972302,-14.671635583332,0.));
#220561=CARTESIAN_POINT('Ctrl Pts',(17.1708771619129,-14.6749971333867,
0.));
#220562=CARTESIAN_POINT('Ctrl Pts',(17.1746247499057,-14.6785925615677,
0.));
#220563=CARTESIAN_POINT('Ctrl Pts',(17.1785800350826,-14.6824178576167,
0.));
#220564=CARTESIAN_POINT('Ctrl Pts',(17.182736158472,-14.686469452232,0.));
#220565=CARTESIAN_POINT('Ctrl Pts',(17.1870867909918,-14.6907440526958,
0.));
#220566=CARTESIAN_POINT('Ctrl Pts',(17.1916259308415,-14.6952385361706,
0.));
#220567=CARTESIAN_POINT('Ctrl Pts',(17.1963476411694,-14.699949811582,0.));
#220568=CARTESIAN_POINT('Ctrl Pts',(17.2012461084268,-14.7048748502663,
0.));
#220569=CARTESIAN_POINT('Ctrl Pts',(17.2063157097315,-14.7100107213586,
0.));
#220570=CARTESIAN_POINT('Ctrl Pts',(17.2115510835989,-14.7153546289339,
0.));
#220571=CARTESIAN_POINT('Ctrl Pts',(17.2169471814256,-14.7209039390327,
0.));
#220572=CARTESIAN_POINT('Ctrl Pts',(17.2224992099667,-14.7266561494282,
0.));
#220573=CARTESIAN_POINT('Ctrl Pts',(17.2282025904314,-14.7326088681163,
0.));
#220574=CARTESIAN_POINT('Ctrl Pts',(17.2340529062076,-14.7387597858117,
0.));
#220575=CARTESIAN_POINT('Ctrl Pts',(17.2400458713565,-14.7451066593792,
0.));
#220576=CARTESIAN_POINT('Ctrl Pts',(17.2461773413288,-14.7516473175124,
0.));
#220577=CARTESIAN_POINT('Ctrl Pts',(17.2524433146837,-14.7583796616617,
0.));
#220578=CARTESIAN_POINT('Ctrl Pts',(17.2588399401465,-14.7653016697591,
0.));
#220579=CARTESIAN_POINT('Ctrl Pts',(17.2653635155319,-14.7724113956731,
0.));
#220580=CARTESIAN_POINT('Ctrl Pts',(17.2720104735194,-14.7797069617804,
0.));
#220581=CARTESIAN_POINT('Ctrl Pts',(17.2787773704849,-14.787186553128,0.));
#220582=CARTESIAN_POINT('Ctrl Pts',(17.2856608733196,-14.7948484105249,
0.));
#220583=CARTESIAN_POINT('Ctrl Pts',(17.2926577496513,-14.8026908254276,
0.));
#220584=CARTESIAN_POINT('Ctrl Pts',(17.299764866148,-14.8107121391035,0.));
#220585=CARTESIAN_POINT('Ctrl Pts',(17.3069791853706,-14.8189107410162,
0.));
#220586=CARTESIAN_POINT('Ctrl Pts',(17.3142977632659,-14.8272850675379,
0.));
#220587=CARTESIAN_POINT('Ctrl Pts',(17.3217177462101,-14.8358336004197,
0.));
#220588=CARTESIAN_POINT('Ctrl Pts',(17.3292363662605,-14.8445548643508,
0.));
#220589=CARTESIAN_POINT('Ctrl Pts',(17.336850936485,-14.8534474245434,0.));
#220590=CARTESIAN_POINT('Ctrl Pts',(17.3445588463474,-14.8625098843417,
0.));
#220591=CARTESIAN_POINT('Ctrl Pts',(17.3523575568645,-14.8717408826956,
0.));
#220592=CARTESIAN_POINT('Ctrl Pts',(17.3602445978161,-14.8811390927423,
0.));
#220593=CARTESIAN_POINT('Ctrl Pts',(17.3682175653235,-14.8907032205788,
0.));
#220594=CARTESIAN_POINT('Ctrl Pts',(17.3762741193076,-14.900432003961,0.));
#220595=CARTESIAN_POINT('Ctrl Pts',(17.3844119809824,-14.9103242110057,
0.));
#220596=CARTESIAN_POINT('Ctrl Pts',(17.3926289303986,-14.9203786389342,
0.));
#220597=CARTESIAN_POINT('Ctrl Pts',(17.4009228040749,-14.9305941128757,
0.));
#220598=CARTESIAN_POINT('Ctrl Pts',(17.4092914926071,-14.940969484645,0.));
#220599=CARTESIAN_POINT('Ctrl Pts',(17.4177329382828,-14.9515036315143,
0.));
#220600=CARTESIAN_POINT('Ctrl Pts',(17.426245132709,-14.9621954549827,0.));
#220601=CARTESIAN_POINT('Ctrl Pts',(17.4348261151396,-14.9730438799452,
0.));
#220602=CARTESIAN_POINT('Ctrl Pts',(17.4434739707773,-14.9840478538358,
0.));
#220603=CARTESIAN_POINT('Ctrl Pts',(17.4521868291004,-14.9952063457778,
0.));
#220604=CARTESIAN_POINT('Ctrl Pts',(17.4609628621418,-15.0065183456921,
0.));
#220605=CARTESIAN_POINT('Ctrl Pts',(17.4698002829357,-15.0179828635086,
0.));
#220606=CARTESIAN_POINT('Ctrl Pts',(17.4786973441417,-15.029598928488,0.));
#220607=CARTESIAN_POINT('Ctrl Pts',(17.4876523366178,-15.0413655884993,
0.));
#220608=CARTESIAN_POINT('Ctrl Pts',(17.4966635880245,-15.0532819093085,
0.));
#220609=CARTESIAN_POINT('Ctrl Pts',(17.5057294613874,-15.0653469738306,
0.));
#220610=CARTESIAN_POINT('Ctrl Pts',(17.5148483539683,-15.0775598815748,
0.));
#220611=CARTESIAN_POINT('Ctrl Pts',(17.5240186961788,-15.0899197481082,
0.));
#220612=CARTESIAN_POINT('Ctrl Pts',(17.5332389504829,-15.1024257045033,
0.));
#220613=CARTESIAN_POINT('Ctrl Pts',(17.5425076102966,-15.1150768967729,
0.));
#220614=CARTESIAN_POINT('Ctrl Pts',(17.5518231989122,-15.127872485314,0.));
#220615=CARTESIAN_POINT('Ctrl Pts',(17.5611842686196,-15.1408116444877,
0.));
#220616=CARTESIAN_POINT('Ctrl Pts',(17.570589399803,-15.1538935621715,0.));
#220617=CARTESIAN_POINT('Ctrl Pts',(17.5800372000539,-15.1671174393136,
0.));
#220618=CARTESIAN_POINT('Ctrl Pts',(17.5895263032592,-15.1804824894605,
0.));
#220619=CARTESIAN_POINT('Ctrl Pts',(17.5990553687595,-15.1939879383268,
0.));
#220620=CARTESIAN_POINT('Ctrl Pts',(17.6086230806497,-15.2076330234686,
0.));
#220621=CARTESIAN_POINT('Ctrl Pts',(17.6182281470467,-15.22141699392,0.));
#220622=CARTESIAN_POINT('Ctrl Pts',(17.6278692993765,-15.2353391098367,
0.));
#220623=CARTESIAN_POINT('Ctrl Pts',(17.637545291637,-15.2493986421091,0.));
#220624=CARTESIAN_POINT('Ctrl Pts',(17.6472548997329,-15.263594872029,0.));
#220625=CARTESIAN_POINT('Ctrl Pts',(17.6569969209,-15.2779270910238,0.));
#220626=CARTESIAN_POINT('Ctrl Pts',(17.6667701731041,-15.2923946003598,
0.));
#220627=CARTESIAN_POINT('Ctrl Pts',(17.6765734944559,-15.3069967108501,
0.));
#220628=CARTESIAN_POINT('Ctrl Pts',(17.6864057426052,-15.3217327425341,
0.));
#220629=CARTESIAN_POINT('Ctrl Pts',(17.6962657941984,-15.3366020244069,
0.));
#220630=CARTESIAN_POINT('Ctrl Pts',(17.7061525444044,-15.3516038942064,
0.));
#220631=CARTESIAN_POINT('Ctrl Pts',(17.7160649064208,-15.3667376981702,
0.));
#220632=CARTESIAN_POINT('Ctrl Pts',(17.7260018109923,-15.3820027907965,
0.));
#220633=CARTESIAN_POINT('Ctrl Pts',(17.7359622059143,-15.3973985345796,
0.));
#220634=CARTESIAN_POINT('Ctrl Pts',(17.7459450555803,-15.4129242997828,
0.));
#220635=CARTESIAN_POINT('Ctrl Pts',(17.7559493405871,-15.4285794642658,
0.));
#220636=CARTESIAN_POINT('Ctrl Pts',(17.765974057326,-15.4443634132865,0.));
#220637=CARTESIAN_POINT('Ctrl Pts',(17.7760182175817,-15.4602755393019,
0.));
#220638=CARTESIAN_POINT('Ctrl Pts',(17.7860808481229,-15.4763152417506,
0.));
#220639=CARTESIAN_POINT('Ctrl Pts',(17.7961609903161,-15.4924819268529,
0.));
#220640=CARTESIAN_POINT('Ctrl Pts',(17.8062576997964,-15.5087750074728,
0.));
#220641=CARTESIAN_POINT('Ctrl Pts',(17.8163700461263,-15.5251939029558,
0.));
#220642=CARTESIAN_POINT('Ctrl Pts',(17.8264971124606,-15.5417380389639,
0.));
#220643=CARTESIAN_POINT('Ctrl Pts',(17.8366379952078,-15.5584068472976,
0.));
#220644=CARTESIAN_POINT('Ctrl Pts',(17.8467918036976,-15.5751997657153,
0.));
#220645=CARTESIAN_POINT('Ctrl Pts',(17.8569576598996,-15.5921162378183,
0.));
#220646=CARTESIAN_POINT('Ctrl Pts',(17.8671346981388,-15.6091557129205,
0.));
#220647=CARTESIAN_POINT('Ctrl Pts',(17.8773220648125,-15.6263176459107,
0.));
#220648=CARTESIAN_POINT('Ctrl Pts',(17.8875189181095,-15.6436014971088,
0.));
#220649=CARTESIAN_POINT('Ctrl Pts',(17.8977244277247,-15.6610067321036,
0.));
#220650=CARTESIAN_POINT('Ctrl Pts',(17.9079377746118,-15.6785328216467,
0.));
#220651=CARTESIAN_POINT('Ctrl Pts',(17.918158150746,-15.6961792415526,0.));
#220652=CARTESIAN_POINT('Ctrl Pts',(17.9283847588837,-15.713945472584,0.));
#220653=CARTESIAN_POINT('Ctrl Pts',(17.9386168123261,-15.7318310003334,
0.));
#220654=CARTESIAN_POINT('Ctrl Pts',(17.9488535346776,-15.7498353150856,
0.));
#220655=CARTESIAN_POINT('Ctrl Pts',(17.9590941596236,-15.7679579117072,
0.));
#220656=CARTESIAN_POINT('Ctrl Pts',(17.9693379307297,-15.786198289572,0.));
#220657=CARTESIAN_POINT('Ctrl Pts',(17.9795841012383,-15.8045559524674,
0.));
#220658=CARTESIAN_POINT('Ctrl Pts',(17.9898319338664,-15.8230304084963,
0.));
#220659=CARTESIAN_POINT('Ctrl Pts',(18.0000807006055,-15.8416211699682,
0.));
#220660=CARTESIAN_POINT('Ctrl Pts',(18.010329682521,-15.8603277532834,0.));
#220661=CARTESIAN_POINT('Ctrl Pts',(18.0205781695773,-15.8791496788685,
0.));
#220662=CARTESIAN_POINT('Ctrl Pts',(18.0308254604638,-15.8980864711043,
0.));
#220663=CARTESIAN_POINT('Ctrl Pts',(18.0410708624208,-15.9171376582436,
0.));
#220664=CARTESIAN_POINT('Ctrl Pts',(18.0513136910691,-15.9363027723244,
0.));
#220665=CARTESIAN_POINT('Ctrl Pts',(18.061553270236,-15.9555813490645,0.));
#220666=CARTESIAN_POINT('Ctrl Pts',(18.071788931796,-15.9749729277848,0.));
#220667=CARTESIAN_POINT('Ctrl Pts',(18.0820200155239,-15.9944770513616,
0.));
#220668=CARTESIAN_POINT('Ctrl Pts',(18.0922458689464,-16.0140932661612,
0.));
#220669=CARTESIAN_POINT('Ctrl Pts',(18.1024658471966,-16.0338211219694,
0.));
#220670=CARTESIAN_POINT('Ctrl Pts',(18.1126793128688,-16.0536601719124,
0.));
#220671=CARTESIAN_POINT('Ctrl Pts',(18.1228856358746,-16.0736099723664,
0.));
#220672=CARTESIAN_POINT('Ctrl Pts',(18.1330841933099,-16.0936700829108,
0.));
#220673=CARTESIAN_POINT('Ctrl Pts',(18.1432743693231,-16.113840066279,0.));
#220674=CARTESIAN_POINT('Ctrl Pts',(18.153455554985,-16.1341194882987,0.));
#220675=CARTESIAN_POINT('Ctrl Pts',(18.1636271481616,-16.1545079178261,
0.));
#220676=CARTESIAN_POINT('Ctrl Pts',(18.1737885533852,-16.1750049266673,
0.));
#220677=CARTESIAN_POINT('Ctrl Pts',(18.1839391817335,-16.1956100895076,
0.));
#220678=CARTESIAN_POINT('Ctrl Pts',(18.1940784507232,-16.2163229838878,
0.));
#220679=CARTESIAN_POINT('Ctrl Pts',(18.2042057842037,-16.237143190164,0.));
#220680=CARTESIAN_POINT('Ctrl Pts',(18.214320612253,-16.2580702914615,0.));
#220681=CARTESIAN_POINT('Ctrl Pts',(18.2244223710745,-16.2791038736223,
0.));
#220682=CARTESIAN_POINT('Ctrl Pts',(18.2345105028981,-16.3002435251378,
0.));
#220683=CARTESIAN_POINT('Ctrl Pts',(18.2445844558742,-16.3214888370988,
0.));
#220684=CARTESIAN_POINT('Ctrl Pts',(18.2546436839609,-16.342839403159,0.));
#220685=CARTESIAN_POINT('Ctrl Pts',(18.2646876468169,-16.3642948194869,
0.));
#220686=CARTESIAN_POINT('Ctrl Pts',(18.2747158096934,-16.385854684708,0.));
#220687=CARTESIAN_POINT('Ctrl Pts',(18.2847276433308,-16.4075185998454,
0.));
#220688=CARTESIAN_POINT('Ctrl Pts',(18.2947226238509,-16.4292861682377,
0.));
#220689=CARTESIAN_POINT('Ctrl Pts',(18.3047002326858,-16.4511569955231,
0.));
#220690=CARTESIAN_POINT('Ctrl Pts',(18.3146599565229,-16.4731306896439,
0.));
#220691=CARTESIAN_POINT('Ctrl Pts',(18.3246012872468,-16.4952068608344,
0.));
#220692=CARTESIAN_POINT('Ctrl Pts',(18.3345237218864,-16.5173851216045,
0.));
#220693=CARTESIAN_POINT('Ctrl Pts',(18.3444267625601,-16.5396650867139,
0.));
#220694=CARTESIAN_POINT('Ctrl Pts',(18.3543099164331,-16.5620463731414,
0.));
#220695=CARTESIAN_POINT('Ctrl Pts',(18.364172695589,-16.5845286000218,0.));
#220696=CARTESIAN_POINT('Ctrl Pts',(18.3740146168879,-16.6071113885711,
0.));
#220697=CARTESIAN_POINT('Ctrl Pts',(18.3838352018327,-16.6297943620056,
0.));
#220698=CARTESIAN_POINT('Ctrl Pts',(18.3936339764332,-16.6525771454513,
0.));
#220699=CARTESIAN_POINT('Ctrl Pts',(18.4034104710789,-16.6754593658513,
0.));
#220700=CARTESIAN_POINT('Ctrl Pts',(18.4131642203989,-16.698440651849,0.));
#220701=CARTESIAN_POINT('Ctrl Pts',(18.4228947633186,-16.7215206338818,
0.));
#220702=CARTESIAN_POINT('Ctrl Pts',(18.4326016431392,-16.7446989442882,
0.));
#220703=CARTESIAN_POINT('Ctrl Pts',(18.4422844076099,-16.7679752173992,
0.));
#220704=CARTESIAN_POINT('Ctrl Pts',(18.4519426090124,-16.791349089629,0.));
#220705=CARTESIAN_POINT('Ctrl Pts',(18.4615758042305,-16.8148201995472,
0.));
#220706=CARTESIAN_POINT('Ctrl Pts',(18.4711835548622,-16.8383881879707,
0.));
#220707=CARTESIAN_POINT('Ctrl Pts',(18.4807654268769,-16.8620526977169,
0.));
#220708=CARTESIAN_POINT('Ctrl Pts',(18.4903209902226,-16.8858133733086,
0.));
#220709=CARTESIAN_POINT('Ctrl Pts',(18.4998498184619,-16.9096698606942,
0.));
#220710=CARTESIAN_POINT('Ctrl Pts',(18.5093514883835,-16.9336218069353,
0.));
#220711=CARTESIAN_POINT('Ctrl Pts',(18.518825579666,-16.957668859934,0.));
#220712=CARTESIAN_POINT('Ctrl Pts',(18.5282716744198,-16.9818106680382,
0.));
#220713=CARTESIAN_POINT('Ctrl Pts',(18.5376893576961,-17.0060468805099,
0.));
#220714=CARTESIAN_POINT('Ctrl Pts',(18.5470782182089,-17.030377148174,0.));
#220715=CARTESIAN_POINT('Ctrl Pts',(18.5564378489628,-17.0548011239751,
0.));
#220716=CARTESIAN_POINT('Ctrl Pts',(18.5657678479788,-17.0793184636079,
0.));
#220717=CARTESIAN_POINT('Ctrl Pts',(18.5750678188543,-17.1039288260002,
0.));
#220718=CARTESIAN_POINT('Ctrl Pts',(18.5843373717253,-17.1286318741185,
0.));
#220719=CARTESIAN_POINT('Ctrl Pts',(18.5935761222833,-17.1534272741646,
0.));
#220720=CARTESIAN_POINT('Ctrl Pts',(18.6027836898826,-17.1783146940131,
0.));
#220721=CARTESIAN_POINT('Ctrl Pts',(18.6119596959957,-17.2032938019288,
0.));
#220722=CARTESIAN_POINT('Ctrl Pts',(18.6211037624041,-17.2283642650519,
0.));
#220723=CARTESIAN_POINT('Ctrl Pts',(18.630215509794,-17.2535257482186,0.));
#220724=CARTESIAN_POINT('Ctrl Pts',(18.639294555474,-17.278777912021,0.));
#220725=CARTESIAN_POINT('Ctrl Pts',(18.6483405141853,-17.3041204135069,
0.));
#220726=CARTESIAN_POINT('Ctrl Pts',(18.6573530024019,-17.3295529098612,
0.));
#220727=CARTESIAN_POINT('Ctrl Pts',(18.6663316416569,-17.3550750612438,
0.));
#220728=CARTESIAN_POINT('Ctrl Pts',(18.6752760624045,-17.3806865340744,
0.));
#220729=CARTESIAN_POINT('Ctrl Pts',(18.6841859073472,-17.4063870038563,
0.));
#220730=CARTESIAN_POINT('Ctrl Pts',(18.6930608357421,-17.4321761588148,
0.));
#220731=CARTESIAN_POINT('Ctrl Pts',(18.7019005250322,-17.4580537012764,
0.));
#220732=CARTESIAN_POINT('Ctrl Pts',(18.7107046613941,-17.4840193397176,
0.));
#220733=CARTESIAN_POINT('Ctrl Pts',(18.7194729318127,-17.5100727820891,
0.));
#220734=CARTESIAN_POINT('Ctrl Pts',(18.728205015716,-17.5362137287604,0.));
#220735=CARTESIAN_POINT('Ctrl Pts',(18.7369005764558,-17.5624418653248,
0.));
#220736=CARTESIAN_POINT('Ctrl Pts',(18.7455592536667,-17.5887568561361,
0.));
#220737=CARTESIAN_POINT('Ctrl Pts',(18.7541806530935,-17.6151583356989,
0.));
#220738=CARTESIAN_POINT('Ctrl Pts',(18.7627643613139,-17.6416459210646,
0.));
#220739=CARTESIAN_POINT('Ctrl Pts',(18.7713099642673,-17.6682192274197,
0.));
#220740=CARTESIAN_POINT('Ctrl Pts',(18.7798170641305,-17.6948778822982,
0.));
#220741=CARTESIAN_POINT('Ctrl Pts',(18.7882852976016,-17.7216215409019,
0.));
#220742=CARTESIAN_POINT('Ctrl Pts',(18.7967143519444,-17.7484498996916,
0.));
#220743=CARTESIAN_POINT('Ctrl Pts',(18.8051039860543,-17.7753627137898,
0.));
#220744=CARTESIAN_POINT('Ctrl Pts',(18.8134540340581,-17.8023598011135,
0.));
#220745=CARTESIAN_POINT('Ctrl Pts',(18.8217643886368,-17.8294410311105,
0.));
#220746=CARTESIAN_POINT('Ctrl Pts',(18.8300349896187,-17.8566063174871,
0.));
#220747=CARTESIAN_POINT('Ctrl Pts',(18.8366196462746,-17.8784057509434,
0.));
#220748=CARTESIAN_POINT('Ctrl Pts',(18.8415402351882,-17.8947931177853,
0.));
#220749=CARTESIAN_POINT('Ctrl Pts',(18.8448126709726,-17.9057348246611,
0.));
#220750=CARTESIAN_POINT('Ctrl Pts',(18.8464468996588,-17.9112098770111,
0.));
#220751=CARTESIAN_POINT('',(18.8464468996588,-17.9112098770111,12.));
#220752=CARTESIAN_POINT('Ctrl Pts',(18.8464468996588,-17.9112098770111,
12.));
#220753=CARTESIAN_POINT('Ctrl Pts',(18.8448126709726,-17.9057348246611,
12.));
#220754=CARTESIAN_POINT('Ctrl Pts',(18.8415402351882,-17.8947931177853,
12.));
#220755=CARTESIAN_POINT('Ctrl Pts',(18.8366196462746,-17.8784057509434,
12.));
#220756=CARTESIAN_POINT('Ctrl Pts',(18.8300349896187,-17.8566063174871,
12.));
#220757=CARTESIAN_POINT('Ctrl Pts',(18.8217643886368,-17.8294410311105,
12.));
#220758=CARTESIAN_POINT('Ctrl Pts',(18.8134540340581,-17.8023598011135,
12.));
#220759=CARTESIAN_POINT('Ctrl Pts',(18.8051039860543,-17.7753627137898,
12.));
#220760=CARTESIAN_POINT('Ctrl Pts',(18.7967143519444,-17.7484498996916,
12.));
#220761=CARTESIAN_POINT('Ctrl Pts',(18.7882852976016,-17.7216215409019,
12.));
#220762=CARTESIAN_POINT('Ctrl Pts',(18.7798170641305,-17.6948778822982,
12.));
#220763=CARTESIAN_POINT('Ctrl Pts',(18.7713099642673,-17.6682192274197,
12.));
#220764=CARTESIAN_POINT('Ctrl Pts',(18.7627643613139,-17.6416459210646,
12.));
#220765=CARTESIAN_POINT('Ctrl Pts',(18.7541806530935,-17.6151583356989,
12.));
#220766=CARTESIAN_POINT('Ctrl Pts',(18.7455592536667,-17.5887568561361,
12.));
#220767=CARTESIAN_POINT('Ctrl Pts',(18.7369005764558,-17.5624418653248,
12.));
#220768=CARTESIAN_POINT('Ctrl Pts',(18.728205015716,-17.5362137287604,12.));
#220769=CARTESIAN_POINT('Ctrl Pts',(18.7194729318127,-17.5100727820891,
12.));
#220770=CARTESIAN_POINT('Ctrl Pts',(18.7107046613941,-17.4840193397176,
12.));
#220771=CARTESIAN_POINT('Ctrl Pts',(18.7019005250322,-17.4580537012764,
12.));
#220772=CARTESIAN_POINT('Ctrl Pts',(18.6930608357421,-17.4321761588148,
12.));
#220773=CARTESIAN_POINT('Ctrl Pts',(18.6841859073472,-17.4063870038563,
12.));
#220774=CARTESIAN_POINT('Ctrl Pts',(18.6752760624045,-17.3806865340744,
12.));
#220775=CARTESIAN_POINT('Ctrl Pts',(18.6663316416569,-17.3550750612438,
12.));
#220776=CARTESIAN_POINT('Ctrl Pts',(18.6573530024019,-17.3295529098612,
12.));
#220777=CARTESIAN_POINT('Ctrl Pts',(18.6483405141853,-17.3041204135069,
12.));
#220778=CARTESIAN_POINT('Ctrl Pts',(18.639294555474,-17.278777912021,12.));
#220779=CARTESIAN_POINT('Ctrl Pts',(18.630215509794,-17.2535257482186,12.));
#220780=CARTESIAN_POINT('Ctrl Pts',(18.6211037624041,-17.2283642650519,
12.));
#220781=CARTESIAN_POINT('Ctrl Pts',(18.6119596959957,-17.2032938019288,
12.));
#220782=CARTESIAN_POINT('Ctrl Pts',(18.6027836898826,-17.1783146940131,
12.));
#220783=CARTESIAN_POINT('Ctrl Pts',(18.5935761222833,-17.1534272741646,
12.));
#220784=CARTESIAN_POINT('Ctrl Pts',(18.5843373717253,-17.1286318741185,
12.));
#220785=CARTESIAN_POINT('Ctrl Pts',(18.5750678188543,-17.1039288260002,
12.));
#220786=CARTESIAN_POINT('Ctrl Pts',(18.5657678479788,-17.0793184636079,
12.));
#220787=CARTESIAN_POINT('Ctrl Pts',(18.5564378489628,-17.0548011239751,
12.));
#220788=CARTESIAN_POINT('Ctrl Pts',(18.5470782182089,-17.030377148174,12.));
#220789=CARTESIAN_POINT('Ctrl Pts',(18.5376893576961,-17.0060468805099,
12.));
#220790=CARTESIAN_POINT('Ctrl Pts',(18.5282716744198,-16.9818106680382,
12.));
#220791=CARTESIAN_POINT('Ctrl Pts',(18.518825579666,-16.957668859934,12.));
#220792=CARTESIAN_POINT('Ctrl Pts',(18.5093514883835,-16.9336218069353,
12.));
#220793=CARTESIAN_POINT('Ctrl Pts',(18.4998498184619,-16.9096698606942,
12.));
#220794=CARTESIAN_POINT('Ctrl Pts',(18.4903209902226,-16.8858133733086,
12.));
#220795=CARTESIAN_POINT('Ctrl Pts',(18.4807654268769,-16.8620526977169,
12.));
#220796=CARTESIAN_POINT('Ctrl Pts',(18.4711835548622,-16.8383881879707,
12.));
#220797=CARTESIAN_POINT('Ctrl Pts',(18.4615758042305,-16.8148201995472,
12.));
#220798=CARTESIAN_POINT('Ctrl Pts',(18.4519426090124,-16.791349089629,12.));
#220799=CARTESIAN_POINT('Ctrl Pts',(18.4422844076099,-16.7679752173992,
12.));
#220800=CARTESIAN_POINT('Ctrl Pts',(18.4326016431392,-16.7446989442882,
12.));
#220801=CARTESIAN_POINT('Ctrl Pts',(18.4228947633186,-16.7215206338818,
12.));
#220802=CARTESIAN_POINT('Ctrl Pts',(18.4131642203989,-16.698440651849,12.));
#220803=CARTESIAN_POINT('Ctrl Pts',(18.4034104710789,-16.6754593658513,
12.));
#220804=CARTESIAN_POINT('Ctrl Pts',(18.3936339764332,-16.6525771454513,
12.));
#220805=CARTESIAN_POINT('Ctrl Pts',(18.3838352018327,-16.6297943620056,
12.));
#220806=CARTESIAN_POINT('Ctrl Pts',(18.3740146168879,-16.6071113885711,
12.));
#220807=CARTESIAN_POINT('Ctrl Pts',(18.364172695589,-16.5845286000218,12.));
#220808=CARTESIAN_POINT('Ctrl Pts',(18.3543099164331,-16.5620463731414,
12.));
#220809=CARTESIAN_POINT('Ctrl Pts',(18.3444267625601,-16.5396650867139,
12.));
#220810=CARTESIAN_POINT('Ctrl Pts',(18.3345237218864,-16.5173851216045,
12.));
#220811=CARTESIAN_POINT('Ctrl Pts',(18.3246012872468,-16.4952068608344,
12.));
#220812=CARTESIAN_POINT('Ctrl Pts',(18.3146599565229,-16.4731306896439,
12.));
#220813=CARTESIAN_POINT('Ctrl Pts',(18.3047002326858,-16.4511569955231,
12.));
#220814=CARTESIAN_POINT('Ctrl Pts',(18.2947226238509,-16.4292861682377,
12.));
#220815=CARTESIAN_POINT('Ctrl Pts',(18.2847276433308,-16.4075185998454,
12.));
#220816=CARTESIAN_POINT('Ctrl Pts',(18.2747158096934,-16.385854684708,12.));
#220817=CARTESIAN_POINT('Ctrl Pts',(18.2646876468169,-16.3642948194869,
12.));
#220818=CARTESIAN_POINT('Ctrl Pts',(18.2546436839609,-16.342839403159,12.));
#220819=CARTESIAN_POINT('Ctrl Pts',(18.2445844558742,-16.3214888370988,
12.));
#220820=CARTESIAN_POINT('Ctrl Pts',(18.2345105028981,-16.3002435251378,
12.));
#220821=CARTESIAN_POINT('Ctrl Pts',(18.2244223710745,-16.2791038736223,
12.));
#220822=CARTESIAN_POINT('Ctrl Pts',(18.214320612253,-16.2580702914615,12.));
#220823=CARTESIAN_POINT('Ctrl Pts',(18.2042057842037,-16.237143190164,12.));
#220824=CARTESIAN_POINT('Ctrl Pts',(18.1940784507232,-16.2163229838878,
12.));
#220825=CARTESIAN_POINT('Ctrl Pts',(18.1839391817335,-16.1956100895076,
12.));
#220826=CARTESIAN_POINT('Ctrl Pts',(18.1737885533852,-16.1750049266673,
12.));
#220827=CARTESIAN_POINT('Ctrl Pts',(18.1636271481616,-16.1545079178261,
12.));
#220828=CARTESIAN_POINT('Ctrl Pts',(18.153455554985,-16.1341194882987,12.));
#220829=CARTESIAN_POINT('Ctrl Pts',(18.1432743693231,-16.113840066279,12.));
#220830=CARTESIAN_POINT('Ctrl Pts',(18.1330841933099,-16.0936700829108,
12.));
#220831=CARTESIAN_POINT('Ctrl Pts',(18.1228856358746,-16.0736099723664,
12.));
#220832=CARTESIAN_POINT('Ctrl Pts',(18.1126793128688,-16.0536601719124,
12.));
#220833=CARTESIAN_POINT('Ctrl Pts',(18.1024658471966,-16.0338211219694,
12.));
#220834=CARTESIAN_POINT('Ctrl Pts',(18.0922458689464,-16.0140932661612,
12.));
#220835=CARTESIAN_POINT('Ctrl Pts',(18.0820200155239,-15.9944770513616,
12.));
#220836=CARTESIAN_POINT('Ctrl Pts',(18.071788931796,-15.9749729277848,12.));
#220837=CARTESIAN_POINT('Ctrl Pts',(18.061553270236,-15.9555813490645,12.));
#220838=CARTESIAN_POINT('Ctrl Pts',(18.0513136910691,-15.9363027723244,
12.));
#220839=CARTESIAN_POINT('Ctrl Pts',(18.0410708624208,-15.9171376582436,
12.));
#220840=CARTESIAN_POINT('Ctrl Pts',(18.0308254604638,-15.8980864711043,
12.));
#220841=CARTESIAN_POINT('Ctrl Pts',(18.0205781695773,-15.8791496788685,
12.));
#220842=CARTESIAN_POINT('Ctrl Pts',(18.010329682521,-15.8603277532834,12.));
#220843=CARTESIAN_POINT('Ctrl Pts',(18.0000807006055,-15.8416211699682,
12.));
#220844=CARTESIAN_POINT('Ctrl Pts',(17.9898319338664,-15.8230304084963,
12.));
#220845=CARTESIAN_POINT('Ctrl Pts',(17.9795841012383,-15.8045559524674,
12.));
#220846=CARTESIAN_POINT('Ctrl Pts',(17.9693379307297,-15.786198289572,12.));
#220847=CARTESIAN_POINT('Ctrl Pts',(17.9590941596236,-15.7679579117072,
12.));
#220848=CARTESIAN_POINT('Ctrl Pts',(17.9488535346776,-15.7498353150856,
12.));
#220849=CARTESIAN_POINT('Ctrl Pts',(17.9386168123261,-15.7318310003334,
12.));
#220850=CARTESIAN_POINT('Ctrl Pts',(17.9283847588837,-15.713945472584,12.));
#220851=CARTESIAN_POINT('Ctrl Pts',(17.918158150746,-15.6961792415526,12.));
#220852=CARTESIAN_POINT('Ctrl Pts',(17.9079377746118,-15.6785328216467,
12.));
#220853=CARTESIAN_POINT('Ctrl Pts',(17.8977244277247,-15.6610067321036,
12.));
#220854=CARTESIAN_POINT('Ctrl Pts',(17.8875189181095,-15.6436014971088,
12.));
#220855=CARTESIAN_POINT('Ctrl Pts',(17.8773220648125,-15.6263176459107,
12.));
#220856=CARTESIAN_POINT('Ctrl Pts',(17.8671346981388,-15.6091557129205,
12.));
#220857=CARTESIAN_POINT('Ctrl Pts',(17.8569576598996,-15.5921162378183,
12.));
#220858=CARTESIAN_POINT('Ctrl Pts',(17.8467918036976,-15.5751997657153,
12.));
#220859=CARTESIAN_POINT('Ctrl Pts',(17.8366379952078,-15.5584068472976,
12.));
#220860=CARTESIAN_POINT('Ctrl Pts',(17.8264971124606,-15.5417380389639,
12.));
#220861=CARTESIAN_POINT('Ctrl Pts',(17.8163700461263,-15.5251939029558,
12.));
#220862=CARTESIAN_POINT('Ctrl Pts',(17.8062576997964,-15.5087750074728,
12.));
#220863=CARTESIAN_POINT('Ctrl Pts',(17.7961609903161,-15.4924819268529,
12.));
#220864=CARTESIAN_POINT('Ctrl Pts',(17.7860808481229,-15.4763152417506,
12.));
#220865=CARTESIAN_POINT('Ctrl Pts',(17.7760182175817,-15.4602755393019,
12.));
#220866=CARTESIAN_POINT('Ctrl Pts',(17.765974057326,-15.4443634132865,12.));
#220867=CARTESIAN_POINT('Ctrl Pts',(17.7559493405871,-15.4285794642658,
12.));
#220868=CARTESIAN_POINT('Ctrl Pts',(17.7459450555803,-15.4129242997828,
12.));
#220869=CARTESIAN_POINT('Ctrl Pts',(17.7359622059143,-15.3973985345796,
12.));
#220870=CARTESIAN_POINT('Ctrl Pts',(17.7260018109923,-15.3820027907965,
12.));
#220871=CARTESIAN_POINT('Ctrl Pts',(17.7160649064208,-15.3667376981702,
12.));
#220872=CARTESIAN_POINT('Ctrl Pts',(17.7061525444044,-15.3516038942064,
12.));
#220873=CARTESIAN_POINT('Ctrl Pts',(17.6962657941984,-15.3366020244069,
12.));
#220874=CARTESIAN_POINT('Ctrl Pts',(17.6864057426052,-15.3217327425341,
12.));
#220875=CARTESIAN_POINT('Ctrl Pts',(17.6765734944559,-15.3069967108501,
12.));
#220876=CARTESIAN_POINT('Ctrl Pts',(17.6667701731041,-15.2923946003598,
12.));
#220877=CARTESIAN_POINT('Ctrl Pts',(17.6569969209,-15.2779270910238,12.));
#220878=CARTESIAN_POINT('Ctrl Pts',(17.6472548997329,-15.263594872029,12.));
#220879=CARTESIAN_POINT('Ctrl Pts',(17.637545291637,-15.2493986421091,12.));
#220880=CARTESIAN_POINT('Ctrl Pts',(17.6278692993765,-15.2353391098367,
12.));
#220881=CARTESIAN_POINT('Ctrl Pts',(17.6182281470467,-15.22141699392,12.));
#220882=CARTESIAN_POINT('Ctrl Pts',(17.6086230806497,-15.2076330234686,
12.));
#220883=CARTESIAN_POINT('Ctrl Pts',(17.5990553687595,-15.1939879383268,
12.));
#220884=CARTESIAN_POINT('Ctrl Pts',(17.5895263032592,-15.1804824894605,
12.));
#220885=CARTESIAN_POINT('Ctrl Pts',(17.5800372000539,-15.1671174393136,
12.));
#220886=CARTESIAN_POINT('Ctrl Pts',(17.570589399803,-15.1538935621715,12.));
#220887=CARTESIAN_POINT('Ctrl Pts',(17.5611842686196,-15.1408116444877,
12.));
#220888=CARTESIAN_POINT('Ctrl Pts',(17.5518231989122,-15.127872485314,12.));
#220889=CARTESIAN_POINT('Ctrl Pts',(17.5425076102966,-15.1150768967729,
12.));
#220890=CARTESIAN_POINT('Ctrl Pts',(17.5332389504829,-15.1024257045033,
12.));
#220891=CARTESIAN_POINT('Ctrl Pts',(17.5240186961788,-15.0899197481082,
12.));
#220892=CARTESIAN_POINT('Ctrl Pts',(17.5148483539683,-15.0775598815748,
12.));
#220893=CARTESIAN_POINT('Ctrl Pts',(17.5057294613874,-15.0653469738306,
12.));
#220894=CARTESIAN_POINT('Ctrl Pts',(17.4966635880245,-15.0532819093085,
12.));
#220895=CARTESIAN_POINT('Ctrl Pts',(17.4876523366178,-15.0413655884993,
12.));
#220896=CARTESIAN_POINT('Ctrl Pts',(17.4786973441417,-15.029598928488,12.));
#220897=CARTESIAN_POINT('Ctrl Pts',(17.4698002829357,-15.0179828635086,
12.));
#220898=CARTESIAN_POINT('Ctrl Pts',(17.4609628621418,-15.0065183456921,
12.));
#220899=CARTESIAN_POINT('Ctrl Pts',(17.4521868291004,-14.9952063457778,
12.));
#220900=CARTESIAN_POINT('Ctrl Pts',(17.4434739707773,-14.9840478538358,
12.));
#220901=CARTESIAN_POINT('Ctrl Pts',(17.4348261151396,-14.9730438799452,
12.));
#220902=CARTESIAN_POINT('Ctrl Pts',(17.426245132709,-14.9621954549827,12.));
#220903=CARTESIAN_POINT('Ctrl Pts',(17.4177329382828,-14.9515036315143,
12.));
#220904=CARTESIAN_POINT('Ctrl Pts',(17.4092914926071,-14.940969484645,12.));
#220905=CARTESIAN_POINT('Ctrl Pts',(17.4009228040749,-14.9305941128757,
12.));
#220906=CARTESIAN_POINT('Ctrl Pts',(17.3926289303986,-14.9203786389342,
12.));
#220907=CARTESIAN_POINT('Ctrl Pts',(17.3844119809824,-14.9103242110057,
12.));
#220908=CARTESIAN_POINT('Ctrl Pts',(17.3762741193076,-14.900432003961,12.));
#220909=CARTESIAN_POINT('Ctrl Pts',(17.3682175653235,-14.8907032205788,
12.));
#220910=CARTESIAN_POINT('Ctrl Pts',(17.3602445978161,-14.8811390927423,
12.));
#220911=CARTESIAN_POINT('Ctrl Pts',(17.3523575568645,-14.8717408826956,
12.));
#220912=CARTESIAN_POINT('Ctrl Pts',(17.3445588463474,-14.8625098843417,
12.));
#220913=CARTESIAN_POINT('Ctrl Pts',(17.336850936485,-14.8534474245434,12.));
#220914=CARTESIAN_POINT('Ctrl Pts',(17.3292363662605,-14.8445548643508,
12.));
#220915=CARTESIAN_POINT('Ctrl Pts',(17.3217177462101,-14.8358336004197,
12.));
#220916=CARTESIAN_POINT('Ctrl Pts',(17.3142977632659,-14.8272850675379,
12.));
#220917=CARTESIAN_POINT('Ctrl Pts',(17.3069791853706,-14.8189107410162,
12.));
#220918=CARTESIAN_POINT('Ctrl Pts',(17.299764866148,-14.8107121391035,12.));
#220919=CARTESIAN_POINT('Ctrl Pts',(17.2926577496513,-14.8026908254276,
12.));
#220920=CARTESIAN_POINT('Ctrl Pts',(17.2856608733196,-14.7948484105249,
12.));
#220921=CARTESIAN_POINT('Ctrl Pts',(17.2787773704849,-14.787186553128,12.));
#220922=CARTESIAN_POINT('Ctrl Pts',(17.2720104735194,-14.7797069617804,
12.));
#220923=CARTESIAN_POINT('Ctrl Pts',(17.2653635155319,-14.7724113956731,
12.));
#220924=CARTESIAN_POINT('Ctrl Pts',(17.2588399401465,-14.7653016697591,
12.));
#220925=CARTESIAN_POINT('Ctrl Pts',(17.2524433146837,-14.7583796616617,
12.));
#220926=CARTESIAN_POINT('Ctrl Pts',(17.2461773413288,-14.7516473175124,
12.));
#220927=CARTESIAN_POINT('Ctrl Pts',(17.2400458713565,-14.7451066593792,
12.));
#220928=CARTESIAN_POINT('Ctrl Pts',(17.2340529062076,-14.7387597858117,
12.));
#220929=CARTESIAN_POINT('Ctrl Pts',(17.2282025904314,-14.7326088681163,
12.));
#220930=CARTESIAN_POINT('Ctrl Pts',(17.2224992099667,-14.7266561494282,
12.));
#220931=CARTESIAN_POINT('Ctrl Pts',(17.2169471814256,-14.7209039390327,
12.));
#220932=CARTESIAN_POINT('Ctrl Pts',(17.2115510835989,-14.7153546289339,
12.));
#220933=CARTESIAN_POINT('Ctrl Pts',(17.2063157097315,-14.7100107213586,
12.));
#220934=CARTESIAN_POINT('Ctrl Pts',(17.2012461084268,-14.7048748502663,
12.));
#220935=CARTESIAN_POINT('Ctrl Pts',(17.1963476411694,-14.699949811582,12.));
#220936=CARTESIAN_POINT('Ctrl Pts',(17.1916259308415,-14.6952385361706,
12.));
#220937=CARTESIAN_POINT('Ctrl Pts',(17.1870867909918,-14.6907440526958,
12.));
#220938=CARTESIAN_POINT('Ctrl Pts',(17.182736158472,-14.686469452232,12.));
#220939=CARTESIAN_POINT('Ctrl Pts',(17.1785800350826,-14.6824178576167,
12.));
#220940=CARTESIAN_POINT('Ctrl Pts',(17.1746247499057,-14.6785925615677,
12.));
#220941=CARTESIAN_POINT('Ctrl Pts',(17.1708771619129,-14.6749971333867,
12.));
#220942=CARTESIAN_POINT('Ctrl Pts',(17.167344972302,-14.671635583332,12.));
#220943=CARTESIAN_POINT('Ctrl Pts',(17.1640366762305,-14.6685123374423,
12.));
#220944=CARTESIAN_POINT('Ctrl Pts',(17.1609609517369,-14.6656319165057,
12.));
#220945=CARTESIAN_POINT('Ctrl Pts',(17.1581262646789,-14.6629987285992,
12.));
#220946=CARTESIAN_POINT('Ctrl Pts',(17.1555401986401,-14.6606167169642,
12.));
#220947=CARTESIAN_POINT('Ctrl Pts',(17.1532107762718,-14.6584900555302,
12.));
#220948=CARTESIAN_POINT('Ctrl Pts',(17.1511476869496,-14.6566237952435,
12.));
#220949=CARTESIAN_POINT('Ctrl Pts',(17.1493641837558,-14.655024862281,12.));
#220950=CARTESIAN_POINT('Ctrl Pts',(17.147876394491,-14.6537016966184,12.));
#220951=CARTESIAN_POINT('Ctrl Pts',(17.1466998098673,-14.6526624064978,
12.));
#220952=CARTESIAN_POINT('Ctrl Pts',(17.1458462295271,-14.6519131634508,
12.));
#220953=CARTESIAN_POINT('Ctrl Pts',(17.1454262858043,-14.6515481598068,
12.));
#220954=CARTESIAN_POINT('Ctrl Pts',(17.1452600887037,-14.6514066997196,
12.));
#220955=CARTESIAN_POINT('Ctrl Pts',(17.1452153999142,-14.6513711852843,
12.));
#220956=CARTESIAN_POINT('Ctrl Pts',(17.1452095830632,-14.6513681262571,
12.));
#220957=CARTESIAN_POINT('',(18.8464468996588,-17.9112098770111,0.));
#220958=CARTESIAN_POINT('Origin',(12.1729687575668,-17.7219872369693,0.));
#220959=CARTESIAN_POINT('',(12.7689476255362,-18.5896416359912,12.));
#220960=CARTESIAN_POINT('',(6.08648437878337,-8.86099361848466,12.));
#220961=CARTESIAN_POINT('',(12.7689476255362,-18.5896416359912,0.));
#220962=CARTESIAN_POINT('',(12.7689476255362,-18.5896416359912,0.));
#220963=CARTESIAN_POINT('',(6.08648437878337,-8.86099361848466,0.));
#220964=CARTESIAN_POINT('Ctrl Pts',(17.9112098770111,-18.8464468996588,
0.));
#220965=CARTESIAN_POINT('Ctrl Pts',(17.9112098770111,-18.8464468996588,
12.));
#220966=CARTESIAN_POINT('Ctrl Pts',(17.9057348246595,-18.8448126709692,
0.));
#220967=CARTESIAN_POINT('Ctrl Pts',(17.9057348246595,-18.8448126709692,
12.));
#220968=CARTESIAN_POINT('Ctrl Pts',(17.8947931177807,-18.8415402351786,
0.));
#220969=CARTESIAN_POINT('Ctrl Pts',(17.8947931177807,-18.8415402351786,
12.));
#220970=CARTESIAN_POINT('Ctrl Pts',(17.8784057509355,-18.8366196462581,
0.));
#220971=CARTESIAN_POINT('Ctrl Pts',(17.8784057509355,-18.8366196462581,
12.));
#220972=CARTESIAN_POINT('Ctrl Pts',(17.856606317477,-18.8300349895974,0.));
#220973=CARTESIAN_POINT('Ctrl Pts',(17.856606317477,-18.8300349895974,12.));
#220974=CARTESIAN_POINT('Ctrl Pts',(17.8294410311006,-18.8217643886157,
0.));
#220975=CARTESIAN_POINT('Ctrl Pts',(17.8294410311006,-18.8217643886157,
12.));
#220976=CARTESIAN_POINT('Ctrl Pts',(17.8023598011057,-18.8134540340417,
0.));
#220977=CARTESIAN_POINT('Ctrl Pts',(17.8023598011057,-18.8134540340417,
12.));
#220978=CARTESIAN_POINT('Ctrl Pts',(17.7753627137853,-18.8051039860448,
0.));
#220979=CARTESIAN_POINT('Ctrl Pts',(17.7753627137853,-18.8051039860448,
12.));
#220980=CARTESIAN_POINT('Ctrl Pts',(17.7484498996905,-18.7967143519419,
0.));
#220981=CARTESIAN_POINT('Ctrl Pts',(17.7484498996905,-18.7967143519419,
12.));
#220982=CARTESIAN_POINT('Ctrl Pts',(17.7216215409035,-18.788285297605,0.));
#220983=CARTESIAN_POINT('Ctrl Pts',(17.7216215409035,-18.788285297605,12.));
#220984=CARTESIAN_POINT('Ctrl Pts',(17.6948778823014,-18.7798170641374,
0.));
#220985=CARTESIAN_POINT('Ctrl Pts',(17.6948778823014,-18.7798170641374,
12.));
#220986=CARTESIAN_POINT('Ctrl Pts',(17.6682192274236,-18.7713099642754,
0.));
#220987=CARTESIAN_POINT('Ctrl Pts',(17.6682192274236,-18.7713099642754,
12.));
#220988=CARTESIAN_POINT('Ctrl Pts',(17.6416459210681,-18.762764361321,0.));
#220989=CARTESIAN_POINT('Ctrl Pts',(17.6416459210681,-18.762764361321,12.));
#220990=CARTESIAN_POINT('Ctrl Pts',(17.6151583357012,-18.7541806530984,
0.));
#220991=CARTESIAN_POINT('Ctrl Pts',(17.6151583357012,-18.7541806530984,
12.));
#220992=CARTESIAN_POINT('Ctrl Pts',(17.5887568561371,-18.7455592536688,
0.));
#220993=CARTESIAN_POINT('Ctrl Pts',(17.5887568561371,-18.7455592536688,
12.));
#220994=CARTESIAN_POINT('Ctrl Pts',(17.5624418653245,-18.7369005764553,
0.));
#220995=CARTESIAN_POINT('Ctrl Pts',(17.5624418653245,-18.7369005764553,
12.));
#220996=CARTESIAN_POINT('Ctrl Pts',(17.5362137287593,-18.7282050157138,
0.));
#220997=CARTESIAN_POINT('Ctrl Pts',(17.5362137287593,-18.7282050157138,
12.));
#220998=CARTESIAN_POINT('Ctrl Pts',(17.5100727820876,-18.7194729318098,
0.));
#220999=CARTESIAN_POINT('Ctrl Pts',(17.5100727820876,-18.7194729318098,
12.));
#221000=CARTESIAN_POINT('Ctrl Pts',(17.4840193397162,-18.7107046613912,
0.));
#221001=CARTESIAN_POINT('Ctrl Pts',(17.4840193397162,-18.7107046613912,
12.));
#221002=CARTESIAN_POINT('Ctrl Pts',(17.4580537012753,-18.70190052503,0.));
#221003=CARTESIAN_POINT('Ctrl Pts',(17.4580537012753,-18.70190052503,12.));
#221004=CARTESIAN_POINT('Ctrl Pts',(17.4321761588142,-18.6930608357409,
0.));
#221005=CARTESIAN_POINT('Ctrl Pts',(17.4321761588142,-18.6930608357409,
12.));
#221006=CARTESIAN_POINT('Ctrl Pts',(17.4063870038562,-18.6841859073471,
0.));
#221007=CARTESIAN_POINT('Ctrl Pts',(17.4063870038562,-18.6841859073471,
12.));
#221008=CARTESIAN_POINT('Ctrl Pts',(17.3806865340747,-18.6752760624052,
0.));
#221009=CARTESIAN_POINT('Ctrl Pts',(17.3806865340747,-18.6752760624052,
12.));
#221010=CARTESIAN_POINT('Ctrl Pts',(17.3550750612443,-18.6663316416582,
0.));
#221011=CARTESIAN_POINT('Ctrl Pts',(17.3550750612443,-18.6663316416582,
12.));
#221012=CARTESIAN_POINT('Ctrl Pts',(17.3295529098618,-18.6573530024033,
0.));
#221013=CARTESIAN_POINT('Ctrl Pts',(17.3295529098618,-18.6573530024033,
12.));
#221014=CARTESIAN_POINT('Ctrl Pts',(17.3041204135074,-18.6483405141865,
0.));
#221015=CARTESIAN_POINT('Ctrl Pts',(17.3041204135074,-18.6483405141865,
12.));
#221016=CARTESIAN_POINT('Ctrl Pts',(17.2787779120213,-18.6392945554748,
0.));
#221017=CARTESIAN_POINT('Ctrl Pts',(17.2787779120213,-18.6392945554748,
12.));
#221018=CARTESIAN_POINT('Ctrl Pts',(17.2535257482187,-18.6302155097943,
0.));
#221019=CARTESIAN_POINT('Ctrl Pts',(17.2535257482187,-18.6302155097943,
12.));
#221020=CARTESIAN_POINT('Ctrl Pts',(17.2283642650517,-18.6211037624038,
0.));
#221021=CARTESIAN_POINT('Ctrl Pts',(17.2283642650517,-18.6211037624038,
12.));
#221022=CARTESIAN_POINT('Ctrl Pts',(17.2032938019284,-18.6119596959949,
0.));
#221023=CARTESIAN_POINT('Ctrl Pts',(17.2032938019284,-18.6119596959949,
12.));
#221024=CARTESIAN_POINT('Ctrl Pts',(17.1783146940127,-18.6027836898817,
0.));
#221025=CARTESIAN_POINT('Ctrl Pts',(17.1783146940127,-18.6027836898817,
12.));
#221026=CARTESIAN_POINT('Ctrl Pts',(17.1534272741643,-18.5935761222825,
0.));
#221027=CARTESIAN_POINT('Ctrl Pts',(17.1534272741643,-18.5935761222825,
12.));
#221028=CARTESIAN_POINT('Ctrl Pts',(17.1286318741183,-18.5843373717247,
0.));
#221029=CARTESIAN_POINT('Ctrl Pts',(17.1286318741183,-18.5843373717247,
12.));
#221030=CARTESIAN_POINT('Ctrl Pts',(17.1039288260001,-18.5750678188542,
0.));
#221031=CARTESIAN_POINT('Ctrl Pts',(17.1039288260001,-18.5750678188542,
12.));
#221032=CARTESIAN_POINT('Ctrl Pts',(17.0793184636079,-18.5657678479789,
0.));
#221033=CARTESIAN_POINT('Ctrl Pts',(17.0793184636079,-18.5657678479789,
12.));
#221034=CARTESIAN_POINT('Ctrl Pts',(17.0548011239751,-18.556437848963,0.));
#221035=CARTESIAN_POINT('Ctrl Pts',(17.0548011239751,-18.556437848963,12.));
#221036=CARTESIAN_POINT('Ctrl Pts',(17.0303771481738,-18.547078218209,0.));
#221037=CARTESIAN_POINT('Ctrl Pts',(17.0303771481738,-18.547078218209,12.));
#221038=CARTESIAN_POINT('Ctrl Pts',(17.0060468805097,-18.5376893576961,
0.));
#221039=CARTESIAN_POINT('Ctrl Pts',(17.0060468805097,-18.5376893576961,
12.));
#221040=CARTESIAN_POINT('Ctrl Pts',(16.981810668038,-18.5282716744197,0.));
#221041=CARTESIAN_POINT('Ctrl Pts',(16.981810668038,-18.5282716744197,12.));
#221042=CARTESIAN_POINT('Ctrl Pts',(16.9576688599339,-18.5188255796659,
0.));
#221043=CARTESIAN_POINT('Ctrl Pts',(16.9576688599339,-18.5188255796659,
12.));
#221044=CARTESIAN_POINT('Ctrl Pts',(16.9336218069353,-18.5093514883835,
0.));
#221045=CARTESIAN_POINT('Ctrl Pts',(16.9336218069353,-18.5093514883835,
12.));
#221046=CARTESIAN_POINT('Ctrl Pts',(16.9096698606943,-18.499849818462,0.));
#221047=CARTESIAN_POINT('Ctrl Pts',(16.9096698606943,-18.499849818462,12.));
#221048=CARTESIAN_POINT('Ctrl Pts',(16.8858133733088,-18.4903209902227,
0.));
#221049=CARTESIAN_POINT('Ctrl Pts',(16.8858133733088,-18.4903209902227,
12.));
#221050=CARTESIAN_POINT('Ctrl Pts',(16.8620526977171,-18.4807654268771,
0.));
#221051=CARTESIAN_POINT('Ctrl Pts',(16.8620526977171,-18.4807654268771,
12.));
#221052=CARTESIAN_POINT('Ctrl Pts',(16.8383881879709,-18.4711835548623,
0.));
#221053=CARTESIAN_POINT('Ctrl Pts',(16.8383881879709,-18.4711835548623,
12.));
#221054=CARTESIAN_POINT('Ctrl Pts',(16.8148201995472,-18.4615758042305,
0.));
#221055=CARTESIAN_POINT('Ctrl Pts',(16.8148201995472,-18.4615758042305,
12.));
#221056=CARTESIAN_POINT('Ctrl Pts',(16.791349089629,-18.4519426090124,0.));
#221057=CARTESIAN_POINT('Ctrl Pts',(16.791349089629,-18.4519426090124,12.));
#221058=CARTESIAN_POINT('Ctrl Pts',(16.7679752173992,-18.44228440761,0.));
#221059=CARTESIAN_POINT('Ctrl Pts',(16.7679752173992,-18.44228440761,12.));
#221060=CARTESIAN_POINT('Ctrl Pts',(16.7446989442882,-18.4326016431392,
0.));
#221061=CARTESIAN_POINT('Ctrl Pts',(16.7446989442882,-18.4326016431392,
12.));
#221062=CARTESIAN_POINT('Ctrl Pts',(16.7215206338818,-18.4228947633187,
0.));
#221063=CARTESIAN_POINT('Ctrl Pts',(16.7215206338818,-18.4228947633187,
12.));
#221064=CARTESIAN_POINT('Ctrl Pts',(16.698440651849,-18.413164220399,0.));
#221065=CARTESIAN_POINT('Ctrl Pts',(16.698440651849,-18.413164220399,12.));
#221066=CARTESIAN_POINT('Ctrl Pts',(16.6754593658513,-18.403410471079,0.));
#221067=CARTESIAN_POINT('Ctrl Pts',(16.6754593658513,-18.403410471079,12.));
#221068=CARTESIAN_POINT('Ctrl Pts',(16.6525771454513,-18.3936339764332,
0.));
#221069=CARTESIAN_POINT('Ctrl Pts',(16.6525771454513,-18.3936339764332,
12.));
#221070=CARTESIAN_POINT('Ctrl Pts',(16.6297943620056,-18.3838352018327,
0.));
#221071=CARTESIAN_POINT('Ctrl Pts',(16.6297943620056,-18.3838352018327,
12.));
#221072=CARTESIAN_POINT('Ctrl Pts',(16.607111388571,-18.3740146168879,0.));
#221073=CARTESIAN_POINT('Ctrl Pts',(16.607111388571,-18.3740146168879,12.));
#221074=CARTESIAN_POINT('Ctrl Pts',(16.5845286000217,-18.3641726955889,
0.));
#221075=CARTESIAN_POINT('Ctrl Pts',(16.5845286000217,-18.3641726955889,
12.));
#221076=CARTESIAN_POINT('Ctrl Pts',(16.5620463731413,-18.354309916433,0.));
#221077=CARTESIAN_POINT('Ctrl Pts',(16.5620463731413,-18.354309916433,12.));
#221078=CARTESIAN_POINT('Ctrl Pts',(16.5396650867139,-18.34442676256,0.));
#221079=CARTESIAN_POINT('Ctrl Pts',(16.5396650867139,-18.34442676256,12.));
#221080=CARTESIAN_POINT('Ctrl Pts',(16.5173851216045,-18.3345237218864,
0.));
#221081=CARTESIAN_POINT('Ctrl Pts',(16.5173851216045,-18.3345237218864,
12.));
#221082=CARTESIAN_POINT('Ctrl Pts',(16.4952068608345,-18.3246012872469,
0.));
#221083=CARTESIAN_POINT('Ctrl Pts',(16.4952068608345,-18.3246012872469,
12.));
#221084=CARTESIAN_POINT('Ctrl Pts',(16.4731306896441,-18.3146599565231,
0.));
#221085=CARTESIAN_POINT('Ctrl Pts',(16.4731306896441,-18.3146599565231,
12.));
#221086=CARTESIAN_POINT('Ctrl Pts',(16.4511569955233,-18.304700232686,0.));
#221087=CARTESIAN_POINT('Ctrl Pts',(16.4511569955233,-18.304700232686,12.));
#221088=CARTESIAN_POINT('Ctrl Pts',(16.4292861682378,-18.294722623851,0.));
#221089=CARTESIAN_POINT('Ctrl Pts',(16.4292861682378,-18.294722623851,12.));
#221090=CARTESIAN_POINT('Ctrl Pts',(16.4075185998454,-18.2847276433309,
0.));
#221091=CARTESIAN_POINT('Ctrl Pts',(16.4075185998454,-18.2847276433309,
12.));
#221092=CARTESIAN_POINT('Ctrl Pts',(16.385854684708,-18.2747158096934,0.));
#221093=CARTESIAN_POINT('Ctrl Pts',(16.385854684708,-18.2747158096934,12.));
#221094=CARTESIAN_POINT('Ctrl Pts',(16.3642948194868,-18.2646876468169,
0.));
#221095=CARTESIAN_POINT('Ctrl Pts',(16.3642948194868,-18.2646876468169,
12.));
#221096=CARTESIAN_POINT('Ctrl Pts',(16.3428394031589,-18.2546436839608,
0.));
#221097=CARTESIAN_POINT('Ctrl Pts',(16.3428394031589,-18.2546436839608,
12.));
#221098=CARTESIAN_POINT('Ctrl Pts',(16.3214888370987,-18.2445844558742,
0.));
#221099=CARTESIAN_POINT('Ctrl Pts',(16.3214888370987,-18.2445844558742,
12.));
#221100=CARTESIAN_POINT('Ctrl Pts',(16.3002435251378,-18.2345105028982,
0.));
#221101=CARTESIAN_POINT('Ctrl Pts',(16.3002435251378,-18.2345105028982,
12.));
#221102=CARTESIAN_POINT('Ctrl Pts',(16.2791038736223,-18.2244223710746,
0.));
#221103=CARTESIAN_POINT('Ctrl Pts',(16.2791038736223,-18.2244223710746,
12.));
#221104=CARTESIAN_POINT('Ctrl Pts',(16.2580702914615,-18.2143206122529,
0.));
#221105=CARTESIAN_POINT('Ctrl Pts',(16.2580702914615,-18.2143206122529,
12.));
#221106=CARTESIAN_POINT('Ctrl Pts',(16.2371431901638,-18.2042057842035,
0.));
#221107=CARTESIAN_POINT('Ctrl Pts',(16.2371431901638,-18.2042057842035,
12.));
#221108=CARTESIAN_POINT('Ctrl Pts',(16.2163229838875,-18.1940784507229,
0.));
#221109=CARTESIAN_POINT('Ctrl Pts',(16.2163229838875,-18.1940784507229,
12.));
#221110=CARTESIAN_POINT('Ctrl Pts',(16.1956100895073,-18.1839391817331,
0.));
#221111=CARTESIAN_POINT('Ctrl Pts',(16.1956100895073,-18.1839391817331,
12.));
#221112=CARTESIAN_POINT('Ctrl Pts',(16.1750049266671,-18.1737885533849,
0.));
#221113=CARTESIAN_POINT('Ctrl Pts',(16.1750049266671,-18.1737885533849,
12.));
#221114=CARTESIAN_POINT('Ctrl Pts',(16.154507917826,-18.1636271481615,0.));
#221115=CARTESIAN_POINT('Ctrl Pts',(16.154507917826,-18.1636271481615,12.));
#221116=CARTESIAN_POINT('Ctrl Pts',(16.1341194882988,-18.1534555549853,
0.));
#221117=CARTESIAN_POINT('Ctrl Pts',(16.1341194882988,-18.1534555549853,
12.));
#221118=CARTESIAN_POINT('Ctrl Pts',(16.1138400662794,-18.1432743693235,
0.));
#221119=CARTESIAN_POINT('Ctrl Pts',(16.1138400662794,-18.1432743693235,
12.));
#221120=CARTESIAN_POINT('Ctrl Pts',(16.0936700829112,-18.1330841933105,
0.));
#221121=CARTESIAN_POINT('Ctrl Pts',(16.0936700829112,-18.1330841933105,
12.));
#221122=CARTESIAN_POINT('Ctrl Pts',(16.0736099723668,-18.1228856358751,
0.));
#221123=CARTESIAN_POINT('Ctrl Pts',(16.0736099723668,-18.1228856358751,
12.));
#221124=CARTESIAN_POINT('Ctrl Pts',(16.0536601719125,-18.112679312869,0.));
#221125=CARTESIAN_POINT('Ctrl Pts',(16.0536601719125,-18.112679312869,12.));
#221126=CARTESIAN_POINT('Ctrl Pts',(16.0338211219693,-18.1024658471966,
0.));
#221127=CARTESIAN_POINT('Ctrl Pts',(16.0338211219693,-18.1024658471966,
12.));
#221128=CARTESIAN_POINT('Ctrl Pts',(16.014093266161,-18.0922458689462,0.));
#221129=CARTESIAN_POINT('Ctrl Pts',(16.014093266161,-18.0922458689462,12.));
#221130=CARTESIAN_POINT('Ctrl Pts',(15.9944770513613,-18.0820200155236,
0.));
#221131=CARTESIAN_POINT('Ctrl Pts',(15.9944770513613,-18.0820200155236,
12.));
#221132=CARTESIAN_POINT('Ctrl Pts',(15.9749729277846,-18.0717889317958,
0.));
#221133=CARTESIAN_POINT('Ctrl Pts',(15.9749729277846,-18.0717889317958,
12.));
#221134=CARTESIAN_POINT('Ctrl Pts',(15.9555813490644,-18.061553270236,0.));
#221135=CARTESIAN_POINT('Ctrl Pts',(15.9555813490644,-18.061553270236,12.));
#221136=CARTESIAN_POINT('Ctrl Pts',(15.9363027723244,-18.0513136910691,
0.));
#221137=CARTESIAN_POINT('Ctrl Pts',(15.9363027723244,-18.0513136910691,
12.));
#221138=CARTESIAN_POINT('Ctrl Pts',(15.9171376582436,-18.0410708624209,
0.));
#221139=CARTESIAN_POINT('Ctrl Pts',(15.9171376582436,-18.0410708624209,
12.));
#221140=CARTESIAN_POINT('Ctrl Pts',(15.8980864711042,-18.0308254604636,
0.));
#221141=CARTESIAN_POINT('Ctrl Pts',(15.8980864711042,-18.0308254604636,
12.));
#221142=CARTESIAN_POINT('Ctrl Pts',(15.8791496788682,-18.0205781695769,
0.));
#221143=CARTESIAN_POINT('Ctrl Pts',(15.8791496788682,-18.0205781695769,
12.));
#221144=CARTESIAN_POINT('Ctrl Pts',(15.8603277532831,-18.0103296825205,
0.));
#221145=CARTESIAN_POINT('Ctrl Pts',(15.8603277532831,-18.0103296825205,
12.));
#221146=CARTESIAN_POINT('Ctrl Pts',(15.8416211699679,-18.0000807006052,
0.));
#221147=CARTESIAN_POINT('Ctrl Pts',(15.8416211699679,-18.0000807006052,
12.));
#221148=CARTESIAN_POINT('Ctrl Pts',(15.8230304084962,-17.9898319338665,
0.));
#221149=CARTESIAN_POINT('Ctrl Pts',(15.8230304084962,-17.9898319338665,
12.));
#221150=CARTESIAN_POINT('Ctrl Pts',(15.8045559524676,-17.9795841012386,
0.));
#221151=CARTESIAN_POINT('Ctrl Pts',(15.8045559524676,-17.9795841012386,
12.));
#221152=CARTESIAN_POINT('Ctrl Pts',(15.7861982895724,-17.9693379307303,
0.));
#221153=CARTESIAN_POINT('Ctrl Pts',(15.7861982895724,-17.9693379307303,
12.));
#221154=CARTESIAN_POINT('Ctrl Pts',(15.7679579117077,-17.9590941596242,
0.));
#221155=CARTESIAN_POINT('Ctrl Pts',(15.7679579117077,-17.9590941596242,
12.));
#221156=CARTESIAN_POINT('Ctrl Pts',(15.749835315086,-17.9488535346781,0.));
#221157=CARTESIAN_POINT('Ctrl Pts',(15.749835315086,-17.9488535346781,12.));
#221158=CARTESIAN_POINT('Ctrl Pts',(15.7318310003335,-17.9386168123262,
0.));
#221159=CARTESIAN_POINT('Ctrl Pts',(15.7318310003335,-17.9386168123262,
12.));
#221160=CARTESIAN_POINT('Ctrl Pts',(15.7139454725838,-17.9283847588836,
0.));
#221161=CARTESIAN_POINT('Ctrl Pts',(15.7139454725838,-17.9283847588836,
12.));
#221162=CARTESIAN_POINT('Ctrl Pts',(15.6961792415522,-17.9181581507455,
0.));
#221163=CARTESIAN_POINT('Ctrl Pts',(15.6961792415522,-17.9181581507455,
12.));
#221164=CARTESIAN_POINT('Ctrl Pts',(15.678532821646,-17.9079377746111,0.));
#221165=CARTESIAN_POINT('Ctrl Pts',(15.678532821646,-17.9079377746111,12.));
#221166=CARTESIAN_POINT('Ctrl Pts',(15.661006732103,-17.897724427724,0.));
#221167=CARTESIAN_POINT('Ctrl Pts',(15.661006732103,-17.897724427724,12.));
#221168=CARTESIAN_POINT('Ctrl Pts',(15.6436014971084,-17.8875189181091,
0.));
#221169=CARTESIAN_POINT('Ctrl Pts',(15.6436014971084,-17.8875189181091,
12.));
#221170=CARTESIAN_POINT('Ctrl Pts',(15.6263176459108,-17.8773220648125,
0.));
#221171=CARTESIAN_POINT('Ctrl Pts',(15.6263176459108,-17.8773220648125,
12.));
#221172=CARTESIAN_POINT('Ctrl Pts',(15.609155712921,-17.8671346981394,0.));
#221173=CARTESIAN_POINT('Ctrl Pts',(15.609155712921,-17.8671346981394,12.));
#221174=CARTESIAN_POINT('Ctrl Pts',(15.5921162378192,-17.8569576599006,
0.));
#221175=CARTESIAN_POINT('Ctrl Pts',(15.5921162378192,-17.8569576599006,
12.));
#221176=CARTESIAN_POINT('Ctrl Pts',(15.5751997657162,-17.8467918036987,
0.));
#221177=CARTESIAN_POINT('Ctrl Pts',(15.5751997657162,-17.8467918036987,
12.));
#221178=CARTESIAN_POINT('Ctrl Pts',(15.5584068472982,-17.8366379952085,
0.));
#221179=CARTESIAN_POINT('Ctrl Pts',(15.5584068472982,-17.8366379952085,
12.));
#221180=CARTESIAN_POINT('Ctrl Pts',(15.541738038964,-17.8264971124607,0.));
#221181=CARTESIAN_POINT('Ctrl Pts',(15.541738038964,-17.8264971124607,12.));
#221182=CARTESIAN_POINT('Ctrl Pts',(15.5251939029552,-17.8163700461256,
0.));
#221183=CARTESIAN_POINT('Ctrl Pts',(15.5251939029552,-17.8163700461256,
12.));
#221184=CARTESIAN_POINT('Ctrl Pts',(15.5087750074718,-17.8062576997952,
0.));
#221185=CARTESIAN_POINT('Ctrl Pts',(15.5087750074718,-17.8062576997952,
12.));
#221186=CARTESIAN_POINT('Ctrl Pts',(15.4924819268517,-17.7961609903148,
0.));
#221187=CARTESIAN_POINT('Ctrl Pts',(15.4924819268517,-17.7961609903148,
12.));
#221188=CARTESIAN_POINT('Ctrl Pts',(15.4763152417497,-17.786080848122,0.));
#221189=CARTESIAN_POINT('Ctrl Pts',(15.4763152417497,-17.786080848122,12.));
#221190=CARTESIAN_POINT('Ctrl Pts',(15.4602755393017,-17.7760182175815,
0.));
#221191=CARTESIAN_POINT('Ctrl Pts',(15.4602755393017,-17.7760182175815,
12.));
#221192=CARTESIAN_POINT('Ctrl Pts',(15.4443634132869,-17.7659740573265,
0.));
#221193=CARTESIAN_POINT('Ctrl Pts',(15.4443634132869,-17.7659740573265,
12.));
#221194=CARTESIAN_POINT('Ctrl Pts',(15.4285794642667,-17.7559493405881,
0.));
#221195=CARTESIAN_POINT('Ctrl Pts',(15.4285794642667,-17.7559493405881,
12.));
#221196=CARTESIAN_POINT('Ctrl Pts',(15.4129242997837,-17.7459450555813,
0.));
#221197=CARTESIAN_POINT('Ctrl Pts',(15.4129242997837,-17.7459450555813,
12.));
#221198=CARTESIAN_POINT('Ctrl Pts',(15.3973985345802,-17.735962205915,0.));
#221199=CARTESIAN_POINT('Ctrl Pts',(15.3973985345802,-17.735962205915,12.));
#221200=CARTESIAN_POINT('Ctrl Pts',(15.3820027907966,-17.7260018109924,
0.));
#221201=CARTESIAN_POINT('Ctrl Pts',(15.3820027907966,-17.7260018109924,
12.));
#221202=CARTESIAN_POINT('Ctrl Pts',(15.3667376981699,-17.7160649064206,
0.));
#221203=CARTESIAN_POINT('Ctrl Pts',(15.3667376981699,-17.7160649064206,
12.));
#221204=CARTESIAN_POINT('Ctrl Pts',(15.351603894206,-17.7061525444042,0.));
#221205=CARTESIAN_POINT('Ctrl Pts',(15.351603894206,-17.7061525444042,12.));
#221206=CARTESIAN_POINT('Ctrl Pts',(15.3366020244066,-17.6962657941983,
0.));
#221207=CARTESIAN_POINT('Ctrl Pts',(15.3366020244066,-17.6962657941983,
12.));
#221208=CARTESIAN_POINT('Ctrl Pts',(15.3217327425338,-17.6864057426052,
0.));
#221209=CARTESIAN_POINT('Ctrl Pts',(15.3217327425338,-17.6864057426052,
12.));
#221210=CARTESIAN_POINT('Ctrl Pts',(15.30699671085,-17.676573494456,0.));
#221211=CARTESIAN_POINT('Ctrl Pts',(15.30699671085,-17.676573494456,12.));
#221212=CARTESIAN_POINT('Ctrl Pts',(15.2923946003598,-17.6667701731041,
0.));
#221213=CARTESIAN_POINT('Ctrl Pts',(15.2923946003598,-17.6667701731041,
12.));
#221214=CARTESIAN_POINT('Ctrl Pts',(15.2779270910239,-17.6569969209,0.));
#221215=CARTESIAN_POINT('Ctrl Pts',(15.2779270910239,-17.6569969209,12.));
#221216=CARTESIAN_POINT('Ctrl Pts',(15.2635948720292,-17.6472548997328,
0.));
#221217=CARTESIAN_POINT('Ctrl Pts',(15.2635948720292,-17.6472548997328,
12.));
#221218=CARTESIAN_POINT('Ctrl Pts',(15.2493986421092,-17.6375452916369,
0.));
#221219=CARTESIAN_POINT('Ctrl Pts',(15.2493986421092,-17.6375452916369,
12.));
#221220=CARTESIAN_POINT('Ctrl Pts',(15.2353391098366,-17.6278692993764,
0.));
#221221=CARTESIAN_POINT('Ctrl Pts',(15.2353391098366,-17.6278692993764,
12.));
#221222=CARTESIAN_POINT('Ctrl Pts',(15.2214169939199,-17.6182281470468,
0.));
#221223=CARTESIAN_POINT('Ctrl Pts',(15.2214169939199,-17.6182281470468,
12.));
#221224=CARTESIAN_POINT('Ctrl Pts',(15.2076330234686,-17.60862308065,0.));
#221225=CARTESIAN_POINT('Ctrl Pts',(15.2076330234686,-17.60862308065,12.));
#221226=CARTESIAN_POINT('Ctrl Pts',(15.1939879383268,-17.5990553687599,
0.));
#221227=CARTESIAN_POINT('Ctrl Pts',(15.1939879383268,-17.5990553687599,
12.));
#221228=CARTESIAN_POINT('Ctrl Pts',(15.1804824894605,-17.5895263032595,
0.));
#221229=CARTESIAN_POINT('Ctrl Pts',(15.1804824894605,-17.5895263032595,
12.));
#221230=CARTESIAN_POINT('Ctrl Pts',(15.1671174393137,-17.580037200054,0.));
#221231=CARTESIAN_POINT('Ctrl Pts',(15.1671174393137,-17.580037200054,12.));
#221232=CARTESIAN_POINT('Ctrl Pts',(15.1538935621714,-17.5705893998029,
0.));
#221233=CARTESIAN_POINT('Ctrl Pts',(15.1538935621714,-17.5705893998029,
12.));
#221234=CARTESIAN_POINT('Ctrl Pts',(15.1408116444876,-17.5611842686192,
0.));
#221235=CARTESIAN_POINT('Ctrl Pts',(15.1408116444876,-17.5611842686192,
12.));
#221236=CARTESIAN_POINT('Ctrl Pts',(15.1278724853138,-17.5518231989117,
0.));
#221237=CARTESIAN_POINT('Ctrl Pts',(15.1278724853138,-17.5518231989117,
12.));
#221238=CARTESIAN_POINT('Ctrl Pts',(15.1150768967728,-17.5425076102963,
0.));
#221239=CARTESIAN_POINT('Ctrl Pts',(15.1150768967728,-17.5425076102963,
12.));
#221240=CARTESIAN_POINT('Ctrl Pts',(15.1024257045033,-17.5332389504829,
0.));
#221241=CARTESIAN_POINT('Ctrl Pts',(15.1024257045033,-17.5332389504829,
12.));
#221242=CARTESIAN_POINT('Ctrl Pts',(15.0899197481082,-17.5240186961791,
0.));
#221243=CARTESIAN_POINT('Ctrl Pts',(15.0899197481082,-17.5240186961791,
12.));
#221244=CARTESIAN_POINT('Ctrl Pts',(15.0775598815749,-17.5148483539687,
0.));
#221245=CARTESIAN_POINT('Ctrl Pts',(15.0775598815749,-17.5148483539687,
12.));
#221246=CARTESIAN_POINT('Ctrl Pts',(15.0653469738307,-17.5057294613877,
0.));
#221247=CARTESIAN_POINT('Ctrl Pts',(15.0653469738307,-17.5057294613877,
12.));
#221248=CARTESIAN_POINT('Ctrl Pts',(15.0532819093085,-17.4966635880246,
0.));
#221249=CARTESIAN_POINT('Ctrl Pts',(15.0532819093085,-17.4966635880246,
12.));
#221250=CARTESIAN_POINT('Ctrl Pts',(15.0413655884993,-17.4876523366178,
0.));
#221251=CARTESIAN_POINT('Ctrl Pts',(15.0413655884993,-17.4876523366178,
12.));
#221252=CARTESIAN_POINT('Ctrl Pts',(15.029598928488,-17.4786973441417,0.));
#221253=CARTESIAN_POINT('Ctrl Pts',(15.029598928488,-17.4786973441417,12.));
#221254=CARTESIAN_POINT('Ctrl Pts',(15.0179828635087,-17.4698002829357,
0.));
#221255=CARTESIAN_POINT('Ctrl Pts',(15.0179828635087,-17.4698002829357,
12.));
#221256=CARTESIAN_POINT('Ctrl Pts',(15.0065183456922,-17.4609628621419,
0.));
#221257=CARTESIAN_POINT('Ctrl Pts',(15.0065183456922,-17.4609628621419,
12.));
#221258=CARTESIAN_POINT('Ctrl Pts',(14.9952063457779,-17.4521868291005,
0.));
#221259=CARTESIAN_POINT('Ctrl Pts',(14.9952063457779,-17.4521868291005,
12.));
#221260=CARTESIAN_POINT('Ctrl Pts',(14.9840478538357,-17.4434739707773,
0.));
#221261=CARTESIAN_POINT('Ctrl Pts',(14.9840478538357,-17.4434739707773,
12.));
#221262=CARTESIAN_POINT('Ctrl Pts',(14.973043879945,-17.4348261151395,0.));
#221263=CARTESIAN_POINT('Ctrl Pts',(14.973043879945,-17.4348261151395,12.));
#221264=CARTESIAN_POINT('Ctrl Pts',(14.9621954549825,-17.4262451327088,
0.));
#221265=CARTESIAN_POINT('Ctrl Pts',(14.9621954549825,-17.4262451327088,
12.));
#221266=CARTESIAN_POINT('Ctrl Pts',(14.9515036315142,-17.4177329382827,
0.));
#221267=CARTESIAN_POINT('Ctrl Pts',(14.9515036315142,-17.4177329382827,
12.));
#221268=CARTESIAN_POINT('Ctrl Pts',(14.940969484645,-17.4092914926072,0.));
#221269=CARTESIAN_POINT('Ctrl Pts',(14.940969484645,-17.4092914926072,12.));
#221270=CARTESIAN_POINT('Ctrl Pts',(14.9305941128758,-17.400922804075,0.));
#221271=CARTESIAN_POINT('Ctrl Pts',(14.9305941128758,-17.400922804075,12.));
#221272=CARTESIAN_POINT('Ctrl Pts',(14.9203786389343,-17.3926289303987,
0.));
#221273=CARTESIAN_POINT('Ctrl Pts',(14.9203786389343,-17.3926289303987,
12.));
#221274=CARTESIAN_POINT('Ctrl Pts',(14.9103242110057,-17.3844119809823,
0.));
#221275=CARTESIAN_POINT('Ctrl Pts',(14.9103242110057,-17.3844119809823,
12.));
#221276=CARTESIAN_POINT('Ctrl Pts',(14.9004320039609,-17.3762741193075,
0.));
#221277=CARTESIAN_POINT('Ctrl Pts',(14.9004320039609,-17.3762741193075,
12.));
#221278=CARTESIAN_POINT('Ctrl Pts',(14.8907032205789,-17.3682175653236,
0.));
#221279=CARTESIAN_POINT('Ctrl Pts',(14.8907032205789,-17.3682175653236,
12.));
#221280=CARTESIAN_POINT('Ctrl Pts',(14.8811390927424,-17.3602445978163,
0.));
#221281=CARTESIAN_POINT('Ctrl Pts',(14.8811390927424,-17.3602445978163,
12.));
#221282=CARTESIAN_POINT('Ctrl Pts',(14.8717408826957,-17.3523575568648,
0.));
#221283=CARTESIAN_POINT('Ctrl Pts',(14.8717408826957,-17.3523575568648,
12.));
#221284=CARTESIAN_POINT('Ctrl Pts',(14.8625098843419,-17.3445588463477,
0.));
#221285=CARTESIAN_POINT('Ctrl Pts',(14.8625098843419,-17.3445588463477,
12.));
#221286=CARTESIAN_POINT('Ctrl Pts',(14.8534474245433,-17.336850936485,0.));
#221287=CARTESIAN_POINT('Ctrl Pts',(14.8534474245433,-17.336850936485,12.));
#221288=CARTESIAN_POINT('Ctrl Pts',(14.8445548643504,-17.3292363662601,
0.));
#221289=CARTESIAN_POINT('Ctrl Pts',(14.8445548643504,-17.3292363662601,
12.));
#221290=CARTESIAN_POINT('Ctrl Pts',(14.8358336004193,-17.3217177462096,
0.));
#221291=CARTESIAN_POINT('Ctrl Pts',(14.8358336004193,-17.3217177462096,
12.));
#221292=CARTESIAN_POINT('Ctrl Pts',(14.8272850675375,-17.3142977632656,
0.));
#221293=CARTESIAN_POINT('Ctrl Pts',(14.8272850675375,-17.3142977632656,
12.));
#221294=CARTESIAN_POINT('Ctrl Pts',(14.8189107410161,-17.3069791853705,
0.));
#221295=CARTESIAN_POINT('Ctrl Pts',(14.8189107410161,-17.3069791853705,
12.));
#221296=CARTESIAN_POINT('Ctrl Pts',(14.8107121391038,-17.2997648661483,
0.));
#221297=CARTESIAN_POINT('Ctrl Pts',(14.8107121391038,-17.2997648661483,
12.));
#221298=CARTESIAN_POINT('Ctrl Pts',(14.8026908254281,-17.2926577496519,
0.));
#221299=CARTESIAN_POINT('Ctrl Pts',(14.8026908254281,-17.2926577496519,
12.));
#221300=CARTESIAN_POINT('Ctrl Pts',(14.7948484105252,-17.28566087332,0.));
#221301=CARTESIAN_POINT('Ctrl Pts',(14.7948484105252,-17.28566087332,12.));
#221302=CARTESIAN_POINT('Ctrl Pts',(14.787186553128,-17.278777370485,0.));
#221303=CARTESIAN_POINT('Ctrl Pts',(14.787186553128,-17.278777370485,12.));
#221304=CARTESIAN_POINT('Ctrl Pts',(14.7797069617802,-17.2720104735192,
0.));
#221305=CARTESIAN_POINT('Ctrl Pts',(14.7797069617802,-17.2720104735192,
12.));
#221306=CARTESIAN_POINT('Ctrl Pts',(14.7724113956728,-17.2653635155317,
0.));
#221307=CARTESIAN_POINT('Ctrl Pts',(14.7724113956728,-17.2653635155317,
12.));
#221308=CARTESIAN_POINT('Ctrl Pts',(14.7653016697589,-17.2588399401464,
0.));
#221309=CARTESIAN_POINT('Ctrl Pts',(14.7653016697589,-17.2588399401464,
12.));
#221310=CARTESIAN_POINT('Ctrl Pts',(14.7583796616617,-17.2524433146837,
0.));
#221311=CARTESIAN_POINT('Ctrl Pts',(14.7583796616617,-17.2524433146837,
12.));
#221312=CARTESIAN_POINT('Ctrl Pts',(14.7516473175124,-17.2461773413289,
0.));
#221313=CARTESIAN_POINT('Ctrl Pts',(14.7516473175124,-17.2461773413289,
12.));
#221314=CARTESIAN_POINT('Ctrl Pts',(14.7451066593793,-17.2400458713566,
0.));
#221315=CARTESIAN_POINT('Ctrl Pts',(14.7451066593793,-17.2400458713566,
12.));
#221316=CARTESIAN_POINT('Ctrl Pts',(14.7387597858117,-17.2340529062078,
0.));
#221317=CARTESIAN_POINT('Ctrl Pts',(14.7387597858117,-17.2340529062078,
12.));
#221318=CARTESIAN_POINT('Ctrl Pts',(14.7326088681163,-17.2282025904314,
0.));
#221319=CARTESIAN_POINT('Ctrl Pts',(14.7326088681163,-17.2282025904314,
12.));
#221320=CARTESIAN_POINT('Ctrl Pts',(14.7266561494282,-17.2224992099666,
0.));
#221321=CARTESIAN_POINT('Ctrl Pts',(14.7266561494282,-17.2224992099666,
12.));
#221322=CARTESIAN_POINT('Ctrl Pts',(14.7209039390325,-17.2169471814255,
0.));
#221323=CARTESIAN_POINT('Ctrl Pts',(14.7209039390325,-17.2169471814255,
12.));
#221324=CARTESIAN_POINT('Ctrl Pts',(14.7153546289338,-17.2115510835988,
0.));
#221325=CARTESIAN_POINT('Ctrl Pts',(14.7153546289338,-17.2115510835988,
12.));
#221326=CARTESIAN_POINT('Ctrl Pts',(14.7100107213586,-17.2063157097316,
0.));
#221327=CARTESIAN_POINT('Ctrl Pts',(14.7100107213586,-17.2063157097316,
12.));
#221328=CARTESIAN_POINT('Ctrl Pts',(14.7048748502662,-17.2012461084268,
0.));
#221329=CARTESIAN_POINT('Ctrl Pts',(14.7048748502662,-17.2012461084268,
12.));
#221330=CARTESIAN_POINT('Ctrl Pts',(14.699949811582,-17.1963476411694,0.));
#221331=CARTESIAN_POINT('Ctrl Pts',(14.699949811582,-17.1963476411694,12.));
#221332=CARTESIAN_POINT('Ctrl Pts',(14.6952385361706,-17.1916259308416,
0.));
#221333=CARTESIAN_POINT('Ctrl Pts',(14.6952385361706,-17.1916259308416,
12.));
#221334=CARTESIAN_POINT('Ctrl Pts',(14.6907440526957,-17.1870867909918,
0.));
#221335=CARTESIAN_POINT('Ctrl Pts',(14.6907440526957,-17.1870867909918,
12.));
#221336=CARTESIAN_POINT('Ctrl Pts',(14.6864694522319,-17.182736158472,0.));
#221337=CARTESIAN_POINT('Ctrl Pts',(14.6864694522319,-17.182736158472,12.));
#221338=CARTESIAN_POINT('Ctrl Pts',(14.6824178576166,-17.1785800350827,
0.));
#221339=CARTESIAN_POINT('Ctrl Pts',(14.6824178576166,-17.1785800350827,
12.));
#221340=CARTESIAN_POINT('Ctrl Pts',(14.6785925615676,-17.1746247499057,
0.));
#221341=CARTESIAN_POINT('Ctrl Pts',(14.6785925615676,-17.1746247499057,
12.));
#221342=CARTESIAN_POINT('Ctrl Pts',(14.6749971333867,-17.1708771619129,
0.));
#221343=CARTESIAN_POINT('Ctrl Pts',(14.6749971333867,-17.1708771619129,
12.));
#221344=CARTESIAN_POINT('Ctrl Pts',(14.6716355833321,-17.1673449723019,
0.));
#221345=CARTESIAN_POINT('Ctrl Pts',(14.6716355833321,-17.1673449723019,
12.));
#221346=CARTESIAN_POINT('Ctrl Pts',(14.6685123374424,-17.1640366762304,
0.));
#221347=CARTESIAN_POINT('Ctrl Pts',(14.6685123374424,-17.1640366762304,
12.));
#221348=CARTESIAN_POINT('Ctrl Pts',(14.6656319165057,-17.1609609517369,
0.));
#221349=CARTESIAN_POINT('Ctrl Pts',(14.6656319165057,-17.1609609517369,
12.));
#221350=CARTESIAN_POINT('Ctrl Pts',(14.662998728599,-17.1581262646789,0.));
#221351=CARTESIAN_POINT('Ctrl Pts',(14.662998728599,-17.1581262646789,12.));
#221352=CARTESIAN_POINT('Ctrl Pts',(14.660616716964,-17.1555401986403,0.));
#221353=CARTESIAN_POINT('Ctrl Pts',(14.660616716964,-17.1555401986403,12.));
#221354=CARTESIAN_POINT('Ctrl Pts',(14.65849005553,-17.1532107762719,0.));
#221355=CARTESIAN_POINT('Ctrl Pts',(14.65849005553,-17.1532107762719,12.));
#221356=CARTESIAN_POINT('Ctrl Pts',(14.6566237952435,-17.1511476869495,
0.));
#221357=CARTESIAN_POINT('Ctrl Pts',(14.6566237952435,-17.1511476869495,
12.));
#221358=CARTESIAN_POINT('Ctrl Pts',(14.6550248622813,-17.1493641837556,
0.));
#221359=CARTESIAN_POINT('Ctrl Pts',(14.6550248622813,-17.1493641837556,
12.));
#221360=CARTESIAN_POINT('Ctrl Pts',(14.6537016966188,-17.1478763944909,
0.));
#221361=CARTESIAN_POINT('Ctrl Pts',(14.6537016966188,-17.1478763944909,
12.));
#221362=CARTESIAN_POINT('Ctrl Pts',(14.6526624064978,-17.1466998098673,
0.));
#221363=CARTESIAN_POINT('Ctrl Pts',(14.6526624064978,-17.1466998098673,
12.));
#221364=CARTESIAN_POINT('Ctrl Pts',(14.65191316345,-17.1458462295273,0.));
#221365=CARTESIAN_POINT('Ctrl Pts',(14.65191316345,-17.1458462295273,12.));
#221366=CARTESIAN_POINT('Ctrl Pts',(14.6515481598057,-17.1454262858045,
0.));
#221367=CARTESIAN_POINT('Ctrl Pts',(14.6515481598057,-17.1454262858045,
12.));
#221368=CARTESIAN_POINT('Ctrl Pts',(14.6514066997188,-17.1452600887039,
0.));
#221369=CARTESIAN_POINT('Ctrl Pts',(14.6514066997188,-17.1452600887039,
12.));
#221370=CARTESIAN_POINT('Ctrl Pts',(14.6513711852839,-17.1452153999142,
0.));
#221371=CARTESIAN_POINT('Ctrl Pts',(14.6513711852839,-17.1452153999142,
12.));
#221372=CARTESIAN_POINT('Ctrl Pts',(14.6513681262571,-17.1452095830633,
0.));
#221373=CARTESIAN_POINT('Ctrl Pts',(14.6513681262571,-17.1452095830633,
12.));
#221374=CARTESIAN_POINT('',(17.9112098770111,-18.8464468996588,0.));
#221375=CARTESIAN_POINT('Ctrl Pts',(17.9112098770111,-18.8464468996588,
0.));
#221376=CARTESIAN_POINT('Ctrl Pts',(17.9057348246595,-18.8448126709692,
0.));
#221377=CARTESIAN_POINT('Ctrl Pts',(17.8947931177807,-18.8415402351786,
0.));
#221378=CARTESIAN_POINT('Ctrl Pts',(17.8784057509355,-18.8366196462581,
0.));
#221379=CARTESIAN_POINT('Ctrl Pts',(17.856606317477,-18.8300349895974,0.));
#221380=CARTESIAN_POINT('Ctrl Pts',(17.8294410311006,-18.8217643886157,
0.));
#221381=CARTESIAN_POINT('Ctrl Pts',(17.8023598011057,-18.8134540340417,
0.));
#221382=CARTESIAN_POINT('Ctrl Pts',(17.7753627137853,-18.8051039860448,
0.));
#221383=CARTESIAN_POINT('Ctrl Pts',(17.7484498996905,-18.7967143519419,
0.));
#221384=CARTESIAN_POINT('Ctrl Pts',(17.7216215409035,-18.788285297605,0.));
#221385=CARTESIAN_POINT('Ctrl Pts',(17.6948778823014,-18.7798170641374,
0.));
#221386=CARTESIAN_POINT('Ctrl Pts',(17.6682192274236,-18.7713099642754,
0.));
#221387=CARTESIAN_POINT('Ctrl Pts',(17.6416459210681,-18.762764361321,0.));
#221388=CARTESIAN_POINT('Ctrl Pts',(17.6151583357012,-18.7541806530984,
0.));
#221389=CARTESIAN_POINT('Ctrl Pts',(17.5887568561371,-18.7455592536688,
0.));
#221390=CARTESIAN_POINT('Ctrl Pts',(17.5624418653245,-18.7369005764553,
0.));
#221391=CARTESIAN_POINT('Ctrl Pts',(17.5362137287593,-18.7282050157138,
0.));
#221392=CARTESIAN_POINT('Ctrl Pts',(17.5100727820876,-18.7194729318098,
0.));
#221393=CARTESIAN_POINT('Ctrl Pts',(17.4840193397162,-18.7107046613912,
0.));
#221394=CARTESIAN_POINT('Ctrl Pts',(17.4580537012753,-18.70190052503,0.));
#221395=CARTESIAN_POINT('Ctrl Pts',(17.4321761588142,-18.6930608357409,
0.));
#221396=CARTESIAN_POINT('Ctrl Pts',(17.4063870038562,-18.6841859073471,
0.));
#221397=CARTESIAN_POINT('Ctrl Pts',(17.3806865340747,-18.6752760624052,
0.));
#221398=CARTESIAN_POINT('Ctrl Pts',(17.3550750612443,-18.6663316416582,
0.));
#221399=CARTESIAN_POINT('Ctrl Pts',(17.3295529098618,-18.6573530024033,
0.));
#221400=CARTESIAN_POINT('Ctrl Pts',(17.3041204135074,-18.6483405141865,
0.));
#221401=CARTESIAN_POINT('Ctrl Pts',(17.2787779120213,-18.6392945554748,
0.));
#221402=CARTESIAN_POINT('Ctrl Pts',(17.2535257482187,-18.6302155097943,
0.));
#221403=CARTESIAN_POINT('Ctrl Pts',(17.2283642650517,-18.6211037624038,
0.));
#221404=CARTESIAN_POINT('Ctrl Pts',(17.2032938019284,-18.6119596959949,
0.));
#221405=CARTESIAN_POINT('Ctrl Pts',(17.1783146940127,-18.6027836898817,
0.));
#221406=CARTESIAN_POINT('Ctrl Pts',(17.1534272741643,-18.5935761222825,
0.));
#221407=CARTESIAN_POINT('Ctrl Pts',(17.1286318741183,-18.5843373717247,
0.));
#221408=CARTESIAN_POINT('Ctrl Pts',(17.1039288260001,-18.5750678188542,
0.));
#221409=CARTESIAN_POINT('Ctrl Pts',(17.0793184636079,-18.5657678479789,
0.));
#221410=CARTESIAN_POINT('Ctrl Pts',(17.0548011239751,-18.556437848963,0.));
#221411=CARTESIAN_POINT('Ctrl Pts',(17.0303771481738,-18.547078218209,0.));
#221412=CARTESIAN_POINT('Ctrl Pts',(17.0060468805097,-18.5376893576961,
0.));
#221413=CARTESIAN_POINT('Ctrl Pts',(16.981810668038,-18.5282716744197,0.));
#221414=CARTESIAN_POINT('Ctrl Pts',(16.9576688599339,-18.5188255796659,
0.));
#221415=CARTESIAN_POINT('Ctrl Pts',(16.9336218069353,-18.5093514883835,
0.));
#221416=CARTESIAN_POINT('Ctrl Pts',(16.9096698606943,-18.499849818462,0.));
#221417=CARTESIAN_POINT('Ctrl Pts',(16.8858133733088,-18.4903209902227,
0.));
#221418=CARTESIAN_POINT('Ctrl Pts',(16.8620526977171,-18.4807654268771,
0.));
#221419=CARTESIAN_POINT('Ctrl Pts',(16.8383881879709,-18.4711835548623,
0.));
#221420=CARTESIAN_POINT('Ctrl Pts',(16.8148201995472,-18.4615758042305,
0.));
#221421=CARTESIAN_POINT('Ctrl Pts',(16.791349089629,-18.4519426090124,0.));
#221422=CARTESIAN_POINT('Ctrl Pts',(16.7679752173992,-18.44228440761,0.));
#221423=CARTESIAN_POINT('Ctrl Pts',(16.7446989442882,-18.4326016431392,
0.));
#221424=CARTESIAN_POINT('Ctrl Pts',(16.7215206338818,-18.4228947633187,
0.));
#221425=CARTESIAN_POINT('Ctrl Pts',(16.698440651849,-18.413164220399,0.));
#221426=CARTESIAN_POINT('Ctrl Pts',(16.6754593658513,-18.403410471079,0.));
#221427=CARTESIAN_POINT('Ctrl Pts',(16.6525771454513,-18.3936339764332,
0.));
#221428=CARTESIAN_POINT('Ctrl Pts',(16.6297943620056,-18.3838352018327,
0.));
#221429=CARTESIAN_POINT('Ctrl Pts',(16.607111388571,-18.3740146168879,0.));
#221430=CARTESIAN_POINT('Ctrl Pts',(16.5845286000217,-18.3641726955889,
0.));
#221431=CARTESIAN_POINT('Ctrl Pts',(16.5620463731413,-18.354309916433,0.));
#221432=CARTESIAN_POINT('Ctrl Pts',(16.5396650867139,-18.34442676256,0.));
#221433=CARTESIAN_POINT('Ctrl Pts',(16.5173851216045,-18.3345237218864,
0.));
#221434=CARTESIAN_POINT('Ctrl Pts',(16.4952068608345,-18.3246012872469,
0.));
#221435=CARTESIAN_POINT('Ctrl Pts',(16.4731306896441,-18.3146599565231,
0.));
#221436=CARTESIAN_POINT('Ctrl Pts',(16.4511569955233,-18.304700232686,0.));
#221437=CARTESIAN_POINT('Ctrl Pts',(16.4292861682378,-18.294722623851,0.));
#221438=CARTESIAN_POINT('Ctrl Pts',(16.4075185998454,-18.2847276433309,
0.));
#221439=CARTESIAN_POINT('Ctrl Pts',(16.385854684708,-18.2747158096934,0.));
#221440=CARTESIAN_POINT('Ctrl Pts',(16.3642948194868,-18.2646876468169,
0.));
#221441=CARTESIAN_POINT('Ctrl Pts',(16.3428394031589,-18.2546436839608,
0.));
#221442=CARTESIAN_POINT('Ctrl Pts',(16.3214888370987,-18.2445844558742,
0.));
#221443=CARTESIAN_POINT('Ctrl Pts',(16.3002435251378,-18.2345105028982,
0.));
#221444=CARTESIAN_POINT('Ctrl Pts',(16.2791038736223,-18.2244223710746,
0.));
#221445=CARTESIAN_POINT('Ctrl Pts',(16.2580702914615,-18.2143206122529,
0.));
#221446=CARTESIAN_POINT('Ctrl Pts',(16.2371431901638,-18.2042057842035,
0.));
#221447=CARTESIAN_POINT('Ctrl Pts',(16.2163229838875,-18.1940784507229,
0.));
#221448=CARTESIAN_POINT('Ctrl Pts',(16.1956100895073,-18.1839391817331,
0.));
#221449=CARTESIAN_POINT('Ctrl Pts',(16.1750049266671,-18.1737885533849,
0.));
#221450=CARTESIAN_POINT('Ctrl Pts',(16.154507917826,-18.1636271481615,0.));
#221451=CARTESIAN_POINT('Ctrl Pts',(16.1341194882988,-18.1534555549853,
0.));
#221452=CARTESIAN_POINT('Ctrl Pts',(16.1138400662794,-18.1432743693235,
0.));
#221453=CARTESIAN_POINT('Ctrl Pts',(16.0936700829112,-18.1330841933105,
0.));
#221454=CARTESIAN_POINT('Ctrl Pts',(16.0736099723668,-18.1228856358751,
0.));
#221455=CARTESIAN_POINT('Ctrl Pts',(16.0536601719125,-18.112679312869,0.));
#221456=CARTESIAN_POINT('Ctrl Pts',(16.0338211219693,-18.1024658471966,
0.));
#221457=CARTESIAN_POINT('Ctrl Pts',(16.014093266161,-18.0922458689462,0.));
#221458=CARTESIAN_POINT('Ctrl Pts',(15.9944770513613,-18.0820200155236,
0.));
#221459=CARTESIAN_POINT('Ctrl Pts',(15.9749729277846,-18.0717889317958,
0.));
#221460=CARTESIAN_POINT('Ctrl Pts',(15.9555813490644,-18.061553270236,0.));
#221461=CARTESIAN_POINT('Ctrl Pts',(15.9363027723244,-18.0513136910691,
0.));
#221462=CARTESIAN_POINT('Ctrl Pts',(15.9171376582436,-18.0410708624209,
0.));
#221463=CARTESIAN_POINT('Ctrl Pts',(15.8980864711042,-18.0308254604636,
0.));
#221464=CARTESIAN_POINT('Ctrl Pts',(15.8791496788682,-18.0205781695769,
0.));
#221465=CARTESIAN_POINT('Ctrl Pts',(15.8603277532831,-18.0103296825205,
0.));
#221466=CARTESIAN_POINT('Ctrl Pts',(15.8416211699679,-18.0000807006052,
0.));
#221467=CARTESIAN_POINT('Ctrl Pts',(15.8230304084962,-17.9898319338665,
0.));
#221468=CARTESIAN_POINT('Ctrl Pts',(15.8045559524676,-17.9795841012386,
0.));
#221469=CARTESIAN_POINT('Ctrl Pts',(15.7861982895724,-17.9693379307303,
0.));
#221470=CARTESIAN_POINT('Ctrl Pts',(15.7679579117077,-17.9590941596242,
0.));
#221471=CARTESIAN_POINT('Ctrl Pts',(15.749835315086,-17.9488535346781,0.));
#221472=CARTESIAN_POINT('Ctrl Pts',(15.7318310003335,-17.9386168123262,
0.));
#221473=CARTESIAN_POINT('Ctrl Pts',(15.7139454725838,-17.9283847588836,
0.));
#221474=CARTESIAN_POINT('Ctrl Pts',(15.6961792415522,-17.9181581507455,
0.));
#221475=CARTESIAN_POINT('Ctrl Pts',(15.678532821646,-17.9079377746111,0.));
#221476=CARTESIAN_POINT('Ctrl Pts',(15.661006732103,-17.897724427724,0.));
#221477=CARTESIAN_POINT('Ctrl Pts',(15.6436014971084,-17.8875189181091,
0.));
#221478=CARTESIAN_POINT('Ctrl Pts',(15.6263176459108,-17.8773220648125,
0.));
#221479=CARTESIAN_POINT('Ctrl Pts',(15.609155712921,-17.8671346981394,0.));
#221480=CARTESIAN_POINT('Ctrl Pts',(15.5921162378192,-17.8569576599006,
0.));
#221481=CARTESIAN_POINT('Ctrl Pts',(15.5751997657162,-17.8467918036987,
0.));
#221482=CARTESIAN_POINT('Ctrl Pts',(15.5584068472982,-17.8366379952085,
0.));
#221483=CARTESIAN_POINT('Ctrl Pts',(15.541738038964,-17.8264971124607,0.));
#221484=CARTESIAN_POINT('Ctrl Pts',(15.5251939029552,-17.8163700461256,
0.));
#221485=CARTESIAN_POINT('Ctrl Pts',(15.5087750074718,-17.8062576997952,
0.));
#221486=CARTESIAN_POINT('Ctrl Pts',(15.4924819268517,-17.7961609903148,
0.));
#221487=CARTESIAN_POINT('Ctrl Pts',(15.4763152417497,-17.786080848122,0.));
#221488=CARTESIAN_POINT('Ctrl Pts',(15.4602755393017,-17.7760182175815,
0.));
#221489=CARTESIAN_POINT('Ctrl Pts',(15.4443634132869,-17.7659740573265,
0.));
#221490=CARTESIAN_POINT('Ctrl Pts',(15.4285794642667,-17.7559493405881,
0.));
#221491=CARTESIAN_POINT('Ctrl Pts',(15.4129242997837,-17.7459450555813,
0.));
#221492=CARTESIAN_POINT('Ctrl Pts',(15.3973985345802,-17.735962205915,0.));
#221493=CARTESIAN_POINT('Ctrl Pts',(15.3820027907966,-17.7260018109924,
0.));
#221494=CARTESIAN_POINT('Ctrl Pts',(15.3667376981699,-17.7160649064206,
0.));
#221495=CARTESIAN_POINT('Ctrl Pts',(15.351603894206,-17.7061525444042,0.));
#221496=CARTESIAN_POINT('Ctrl Pts',(15.3366020244066,-17.6962657941983,
0.));
#221497=CARTESIAN_POINT('Ctrl Pts',(15.3217327425338,-17.6864057426052,
0.));
#221498=CARTESIAN_POINT('Ctrl Pts',(15.30699671085,-17.676573494456,0.));
#221499=CARTESIAN_POINT('Ctrl Pts',(15.2923946003598,-17.6667701731041,
0.));
#221500=CARTESIAN_POINT('Ctrl Pts',(15.2779270910239,-17.6569969209,0.));
#221501=CARTESIAN_POINT('Ctrl Pts',(15.2635948720292,-17.6472548997328,
0.));
#221502=CARTESIAN_POINT('Ctrl Pts',(15.2493986421092,-17.6375452916369,
0.));
#221503=CARTESIAN_POINT('Ctrl Pts',(15.2353391098366,-17.6278692993764,
0.));
#221504=CARTESIAN_POINT('Ctrl Pts',(15.2214169939199,-17.6182281470468,
0.));
#221505=CARTESIAN_POINT('Ctrl Pts',(15.2076330234686,-17.60862308065,0.));
#221506=CARTESIAN_POINT('Ctrl Pts',(15.1939879383268,-17.5990553687599,
0.));
#221507=CARTESIAN_POINT('Ctrl Pts',(15.1804824894605,-17.5895263032595,
0.));
#221508=CARTESIAN_POINT('Ctrl Pts',(15.1671174393137,-17.580037200054,0.));
#221509=CARTESIAN_POINT('Ctrl Pts',(15.1538935621714,-17.5705893998029,
0.));
#221510=CARTESIAN_POINT('Ctrl Pts',(15.1408116444876,-17.5611842686192,
0.));
#221511=CARTESIAN_POINT('Ctrl Pts',(15.1278724853138,-17.5518231989117,
0.));
#221512=CARTESIAN_POINT('Ctrl Pts',(15.1150768967728,-17.5425076102963,
0.));
#221513=CARTESIAN_POINT('Ctrl Pts',(15.1024257045033,-17.5332389504829,
0.));
#221514=CARTESIAN_POINT('Ctrl Pts',(15.0899197481082,-17.5240186961791,
0.));
#221515=CARTESIAN_POINT('Ctrl Pts',(15.0775598815749,-17.5148483539687,
0.));
#221516=CARTESIAN_POINT('Ctrl Pts',(15.0653469738307,-17.5057294613877,
0.));
#221517=CARTESIAN_POINT('Ctrl Pts',(15.0532819093085,-17.4966635880246,
0.));
#221518=CARTESIAN_POINT('Ctrl Pts',(15.0413655884993,-17.4876523366178,
0.));
#221519=CARTESIAN_POINT('Ctrl Pts',(15.029598928488,-17.4786973441417,0.));
#221520=CARTESIAN_POINT('Ctrl Pts',(15.0179828635087,-17.4698002829357,
0.));
#221521=CARTESIAN_POINT('Ctrl Pts',(15.0065183456922,-17.4609628621419,
0.));
#221522=CARTESIAN_POINT('Ctrl Pts',(14.9952063457779,-17.4521868291005,
0.));
#221523=CARTESIAN_POINT('Ctrl Pts',(14.9840478538357,-17.4434739707773,
0.));
#221524=CARTESIAN_POINT('Ctrl Pts',(14.973043879945,-17.4348261151395,0.));
#221525=CARTESIAN_POINT('Ctrl Pts',(14.9621954549825,-17.4262451327088,
0.));
#221526=CARTESIAN_POINT('Ctrl Pts',(14.9515036315142,-17.4177329382827,
0.));
#221527=CARTESIAN_POINT('Ctrl Pts',(14.940969484645,-17.4092914926072,0.));
#221528=CARTESIAN_POINT('Ctrl Pts',(14.9305941128758,-17.400922804075,0.));
#221529=CARTESIAN_POINT('Ctrl Pts',(14.9203786389343,-17.3926289303987,
0.));
#221530=CARTESIAN_POINT('Ctrl Pts',(14.9103242110057,-17.3844119809823,
0.));
#221531=CARTESIAN_POINT('Ctrl Pts',(14.9004320039609,-17.3762741193075,
0.));
#221532=CARTESIAN_POINT('Ctrl Pts',(14.8907032205789,-17.3682175653236,
0.));
#221533=CARTESIAN_POINT('Ctrl Pts',(14.8811390927424,-17.3602445978163,
0.));
#221534=CARTESIAN_POINT('Ctrl Pts',(14.8717408826957,-17.3523575568648,
0.));
#221535=CARTESIAN_POINT('Ctrl Pts',(14.8625098843419,-17.3445588463477,
0.));
#221536=CARTESIAN_POINT('Ctrl Pts',(14.8534474245433,-17.336850936485,0.));
#221537=CARTESIAN_POINT('Ctrl Pts',(14.8445548643504,-17.3292363662601,
0.));
#221538=CARTESIAN_POINT('Ctrl Pts',(14.8358336004193,-17.3217177462096,
0.));
#221539=CARTESIAN_POINT('Ctrl Pts',(14.8272850675375,-17.3142977632656,
0.));
#221540=CARTESIAN_POINT('Ctrl Pts',(14.8189107410161,-17.3069791853705,
0.));
#221541=CARTESIAN_POINT('Ctrl Pts',(14.8107121391038,-17.2997648661483,
0.));
#221542=CARTESIAN_POINT('Ctrl Pts',(14.8026908254281,-17.2926577496519,
0.));
#221543=CARTESIAN_POINT('Ctrl Pts',(14.7948484105252,-17.28566087332,0.));
#221544=CARTESIAN_POINT('Ctrl Pts',(14.787186553128,-17.278777370485,0.));
#221545=CARTESIAN_POINT('Ctrl Pts',(14.7797069617802,-17.2720104735192,
0.));
#221546=CARTESIAN_POINT('Ctrl Pts',(14.7724113956728,-17.2653635155317,
0.));
#221547=CARTESIAN_POINT('Ctrl Pts',(14.7653016697589,-17.2588399401464,
0.));
#221548=CARTESIAN_POINT('Ctrl Pts',(14.7583796616617,-17.2524433146837,
0.));
#221549=CARTESIAN_POINT('Ctrl Pts',(14.7516473175124,-17.2461773413289,
0.));
#221550=CARTESIAN_POINT('Ctrl Pts',(14.7451066593793,-17.2400458713566,
0.));
#221551=CARTESIAN_POINT('Ctrl Pts',(14.7387597858117,-17.2340529062078,
0.));
#221552=CARTESIAN_POINT('Ctrl Pts',(14.7326088681163,-17.2282025904314,
0.));
#221553=CARTESIAN_POINT('Ctrl Pts',(14.7266561494282,-17.2224992099666,
0.));
#221554=CARTESIAN_POINT('Ctrl Pts',(14.7209039390325,-17.2169471814255,
0.));
#221555=CARTESIAN_POINT('Ctrl Pts',(14.7153546289338,-17.2115510835988,
0.));
#221556=CARTESIAN_POINT('Ctrl Pts',(14.7100107213586,-17.2063157097316,
0.));
#221557=CARTESIAN_POINT('Ctrl Pts',(14.7048748502662,-17.2012461084268,
0.));
#221558=CARTESIAN_POINT('Ctrl Pts',(14.699949811582,-17.1963476411694,0.));
#221559=CARTESIAN_POINT('Ctrl Pts',(14.6952385361706,-17.1916259308416,
0.));
#221560=CARTESIAN_POINT('Ctrl Pts',(14.6907440526957,-17.1870867909918,
0.));
#221561=CARTESIAN_POINT('Ctrl Pts',(14.6864694522319,-17.182736158472,0.));
#221562=CARTESIAN_POINT('Ctrl Pts',(14.6824178576166,-17.1785800350827,
0.));
#221563=CARTESIAN_POINT('Ctrl Pts',(14.6785925615676,-17.1746247499057,
0.));
#221564=CARTESIAN_POINT('Ctrl Pts',(14.6749971333867,-17.1708771619129,
0.));
#221565=CARTESIAN_POINT('Ctrl Pts',(14.6716355833321,-17.1673449723019,
0.));
#221566=CARTESIAN_POINT('Ctrl Pts',(14.6685123374424,-17.1640366762304,
0.));
#221567=CARTESIAN_POINT('Ctrl Pts',(14.6656319165057,-17.1609609517369,
0.));
#221568=CARTESIAN_POINT('Ctrl Pts',(14.662998728599,-17.1581262646789,0.));
#221569=CARTESIAN_POINT('Ctrl Pts',(14.660616716964,-17.1555401986403,0.));
#221570=CARTESIAN_POINT('Ctrl Pts',(14.65849005553,-17.1532107762719,0.));
#221571=CARTESIAN_POINT('Ctrl Pts',(14.6566237952435,-17.1511476869495,
0.));
#221572=CARTESIAN_POINT('Ctrl Pts',(14.6550248622813,-17.1493641837556,
0.));
#221573=CARTESIAN_POINT('Ctrl Pts',(14.6537016966188,-17.1478763944909,
0.));
#221574=CARTESIAN_POINT('Ctrl Pts',(14.6526624064978,-17.1466998098673,
0.));
#221575=CARTESIAN_POINT('Ctrl Pts',(14.65191316345,-17.1458462295273,0.));
#221576=CARTESIAN_POINT('Ctrl Pts',(14.6515481598057,-17.1454262858045,
0.));
#221577=CARTESIAN_POINT('Ctrl Pts',(14.6514066997188,-17.1452600887039,
0.));
#221578=CARTESIAN_POINT('Ctrl Pts',(14.6513711852839,-17.1452153999142,
0.));
#221579=CARTESIAN_POINT('Ctrl Pts',(14.6513681262571,-17.1452095830633,
0.));
#221580=CARTESIAN_POINT('',(17.9112098770111,-18.8464468996588,12.));
#221581=CARTESIAN_POINT('',(17.9112098770111,-18.8464468996588,0.));
#221582=CARTESIAN_POINT('Ctrl Pts',(14.6513681262571,-17.1452095830633,
12.));
#221583=CARTESIAN_POINT('Ctrl Pts',(14.6513711852839,-17.1452153999142,
12.));
#221584=CARTESIAN_POINT('Ctrl Pts',(14.6514066997188,-17.1452600887039,
12.));
#221585=CARTESIAN_POINT('Ctrl Pts',(14.6515481598057,-17.1454262858045,
12.));
#221586=CARTESIAN_POINT('Ctrl Pts',(14.65191316345,-17.1458462295273,12.));
#221587=CARTESIAN_POINT('Ctrl Pts',(14.6526624064978,-17.1466998098673,
12.));
#221588=CARTESIAN_POINT('Ctrl Pts',(14.6537016966188,-17.1478763944909,
12.));
#221589=CARTESIAN_POINT('Ctrl Pts',(14.6550248622813,-17.1493641837556,
12.));
#221590=CARTESIAN_POINT('Ctrl Pts',(14.6566237952435,-17.1511476869495,
12.));
#221591=CARTESIAN_POINT('Ctrl Pts',(14.65849005553,-17.1532107762719,12.));
#221592=CARTESIAN_POINT('Ctrl Pts',(14.660616716964,-17.1555401986403,12.));
#221593=CARTESIAN_POINT('Ctrl Pts',(14.662998728599,-17.1581262646789,12.));
#221594=CARTESIAN_POINT('Ctrl Pts',(14.6656319165057,-17.1609609517369,
12.));
#221595=CARTESIAN_POINT('Ctrl Pts',(14.6685123374424,-17.1640366762304,
12.));
#221596=CARTESIAN_POINT('Ctrl Pts',(14.6716355833321,-17.1673449723019,
12.));
#221597=CARTESIAN_POINT('Ctrl Pts',(14.6749971333867,-17.1708771619129,
12.));
#221598=CARTESIAN_POINT('Ctrl Pts',(14.6785925615676,-17.1746247499057,
12.));
#221599=CARTESIAN_POINT('Ctrl Pts',(14.6824178576166,-17.1785800350827,
12.));
#221600=CARTESIAN_POINT('Ctrl Pts',(14.6864694522319,-17.182736158472,12.));
#221601=CARTESIAN_POINT('Ctrl Pts',(14.6907440526957,-17.1870867909918,
12.));
#221602=CARTESIAN_POINT('Ctrl Pts',(14.6952385361706,-17.1916259308416,
12.));
#221603=CARTESIAN_POINT('Ctrl Pts',(14.699949811582,-17.1963476411694,12.));
#221604=CARTESIAN_POINT('Ctrl Pts',(14.7048748502662,-17.2012461084268,
12.));
#221605=CARTESIAN_POINT('Ctrl Pts',(14.7100107213586,-17.2063157097316,
12.));
#221606=CARTESIAN_POINT('Ctrl Pts',(14.7153546289338,-17.2115510835988,
12.));
#221607=CARTESIAN_POINT('Ctrl Pts',(14.7209039390325,-17.2169471814255,
12.));
#221608=CARTESIAN_POINT('Ctrl Pts',(14.7266561494282,-17.2224992099666,
12.));
#221609=CARTESIAN_POINT('Ctrl Pts',(14.7326088681163,-17.2282025904314,
12.));
#221610=CARTESIAN_POINT('Ctrl Pts',(14.7387597858117,-17.2340529062078,
12.));
#221611=CARTESIAN_POINT('Ctrl Pts',(14.7451066593793,-17.2400458713566,
12.));
#221612=CARTESIAN_POINT('Ctrl Pts',(14.7516473175124,-17.2461773413289,
12.));
#221613=CARTESIAN_POINT('Ctrl Pts',(14.7583796616617,-17.2524433146837,
12.));
#221614=CARTESIAN_POINT('Ctrl Pts',(14.7653016697589,-17.2588399401464,
12.));
#221615=CARTESIAN_POINT('Ctrl Pts',(14.7724113956728,-17.2653635155317,
12.));
#221616=CARTESIAN_POINT('Ctrl Pts',(14.7797069617802,-17.2720104735192,
12.));
#221617=CARTESIAN_POINT('Ctrl Pts',(14.787186553128,-17.278777370485,12.));
#221618=CARTESIAN_POINT('Ctrl Pts',(14.7948484105252,-17.28566087332,12.));
#221619=CARTESIAN_POINT('Ctrl Pts',(14.8026908254281,-17.2926577496519,
12.));
#221620=CARTESIAN_POINT('Ctrl Pts',(14.8107121391038,-17.2997648661483,
12.));
#221621=CARTESIAN_POINT('Ctrl Pts',(14.8189107410161,-17.3069791853705,
12.));
#221622=CARTESIAN_POINT('Ctrl Pts',(14.8272850675375,-17.3142977632656,
12.));
#221623=CARTESIAN_POINT('Ctrl Pts',(14.8358336004193,-17.3217177462096,
12.));
#221624=CARTESIAN_POINT('Ctrl Pts',(14.8445548643504,-17.3292363662601,
12.));
#221625=CARTESIAN_POINT('Ctrl Pts',(14.8534474245433,-17.336850936485,12.));
#221626=CARTESIAN_POINT('Ctrl Pts',(14.8625098843419,-17.3445588463477,
12.));
#221627=CARTESIAN_POINT('Ctrl Pts',(14.8717408826957,-17.3523575568648,
12.));
#221628=CARTESIAN_POINT('Ctrl Pts',(14.8811390927424,-17.3602445978163,
12.));
#221629=CARTESIAN_POINT('Ctrl Pts',(14.8907032205789,-17.3682175653236,
12.));
#221630=CARTESIAN_POINT('Ctrl Pts',(14.9004320039609,-17.3762741193075,
12.));
#221631=CARTESIAN_POINT('Ctrl Pts',(14.9103242110057,-17.3844119809823,
12.));
#221632=CARTESIAN_POINT('Ctrl Pts',(14.9203786389343,-17.3926289303987,
12.));
#221633=CARTESIAN_POINT('Ctrl Pts',(14.9305941128758,-17.400922804075,12.));
#221634=CARTESIAN_POINT('Ctrl Pts',(14.940969484645,-17.4092914926072,12.));
#221635=CARTESIAN_POINT('Ctrl Pts',(14.9515036315142,-17.4177329382827,
12.));
#221636=CARTESIAN_POINT('Ctrl Pts',(14.9621954549825,-17.4262451327088,
12.));
#221637=CARTESIAN_POINT('Ctrl Pts',(14.973043879945,-17.4348261151395,12.));
#221638=CARTESIAN_POINT('Ctrl Pts',(14.9840478538357,-17.4434739707773,
12.));
#221639=CARTESIAN_POINT('Ctrl Pts',(14.9952063457779,-17.4521868291005,
12.));
#221640=CARTESIAN_POINT('Ctrl Pts',(15.0065183456922,-17.4609628621419,
12.));
#221641=CARTESIAN_POINT('Ctrl Pts',(15.0179828635087,-17.4698002829357,
12.));
#221642=CARTESIAN_POINT('Ctrl Pts',(15.029598928488,-17.4786973441417,12.));
#221643=CARTESIAN_POINT('Ctrl Pts',(15.0413655884993,-17.4876523366178,
12.));
#221644=CARTESIAN_POINT('Ctrl Pts',(15.0532819093085,-17.4966635880246,
12.));
#221645=CARTESIAN_POINT('Ctrl Pts',(15.0653469738307,-17.5057294613877,
12.));
#221646=CARTESIAN_POINT('Ctrl Pts',(15.0775598815749,-17.5148483539687,
12.));
#221647=CARTESIAN_POINT('Ctrl Pts',(15.0899197481082,-17.5240186961791,
12.));
#221648=CARTESIAN_POINT('Ctrl Pts',(15.1024257045033,-17.5332389504829,
12.));
#221649=CARTESIAN_POINT('Ctrl Pts',(15.1150768967728,-17.5425076102963,
12.));
#221650=CARTESIAN_POINT('Ctrl Pts',(15.1278724853138,-17.5518231989117,
12.));
#221651=CARTESIAN_POINT('Ctrl Pts',(15.1408116444876,-17.5611842686192,
12.));
#221652=CARTESIAN_POINT('Ctrl Pts',(15.1538935621714,-17.5705893998029,
12.));
#221653=CARTESIAN_POINT('Ctrl Pts',(15.1671174393137,-17.580037200054,12.));
#221654=CARTESIAN_POINT('Ctrl Pts',(15.1804824894605,-17.5895263032595,
12.));
#221655=CARTESIAN_POINT('Ctrl Pts',(15.1939879383268,-17.5990553687599,
12.));
#221656=CARTESIAN_POINT('Ctrl Pts',(15.2076330234686,-17.60862308065,12.));
#221657=CARTESIAN_POINT('Ctrl Pts',(15.2214169939199,-17.6182281470468,
12.));
#221658=CARTESIAN_POINT('Ctrl Pts',(15.2353391098366,-17.6278692993764,
12.));
#221659=CARTESIAN_POINT('Ctrl Pts',(15.2493986421092,-17.6375452916369,
12.));
#221660=CARTESIAN_POINT('Ctrl Pts',(15.2635948720292,-17.6472548997328,
12.));
#221661=CARTESIAN_POINT('Ctrl Pts',(15.2779270910239,-17.6569969209,12.));
#221662=CARTESIAN_POINT('Ctrl Pts',(15.2923946003598,-17.6667701731041,
12.));
#221663=CARTESIAN_POINT('Ctrl Pts',(15.30699671085,-17.676573494456,12.));
#221664=CARTESIAN_POINT('Ctrl Pts',(15.3217327425338,-17.6864057426052,
12.));
#221665=CARTESIAN_POINT('Ctrl Pts',(15.3366020244066,-17.6962657941983,
12.));
#221666=CARTESIAN_POINT('Ctrl Pts',(15.351603894206,-17.7061525444042,12.));
#221667=CARTESIAN_POINT('Ctrl Pts',(15.3667376981699,-17.7160649064206,
12.));
#221668=CARTESIAN_POINT('Ctrl Pts',(15.3820027907966,-17.7260018109924,
12.));
#221669=CARTESIAN_POINT('Ctrl Pts',(15.3973985345802,-17.735962205915,12.));
#221670=CARTESIAN_POINT('Ctrl Pts',(15.4129242997837,-17.7459450555813,
12.));
#221671=CARTESIAN_POINT('Ctrl Pts',(15.4285794642667,-17.7559493405881,
12.));
#221672=CARTESIAN_POINT('Ctrl Pts',(15.4443634132869,-17.7659740573265,
12.));
#221673=CARTESIAN_POINT('Ctrl Pts',(15.4602755393017,-17.7760182175815,
12.));
#221674=CARTESIAN_POINT('Ctrl Pts',(15.4763152417497,-17.786080848122,12.));
#221675=CARTESIAN_POINT('Ctrl Pts',(15.4924819268517,-17.7961609903148,
12.));
#221676=CARTESIAN_POINT('Ctrl Pts',(15.5087750074718,-17.8062576997952,
12.));
#221677=CARTESIAN_POINT('Ctrl Pts',(15.5251939029552,-17.8163700461256,
12.));
#221678=CARTESIAN_POINT('Ctrl Pts',(15.541738038964,-17.8264971124607,12.));
#221679=CARTESIAN_POINT('Ctrl Pts',(15.5584068472982,-17.8366379952085,
12.));
#221680=CARTESIAN_POINT('Ctrl Pts',(15.5751997657162,-17.8467918036987,
12.));
#221681=CARTESIAN_POINT('Ctrl Pts',(15.5921162378192,-17.8569576599006,
12.));
#221682=CARTESIAN_POINT('Ctrl Pts',(15.609155712921,-17.8671346981394,12.));
#221683=CARTESIAN_POINT('Ctrl Pts',(15.6263176459108,-17.8773220648125,
12.));
#221684=CARTESIAN_POINT('Ctrl Pts',(15.6436014971084,-17.8875189181091,
12.));
#221685=CARTESIAN_POINT('Ctrl Pts',(15.661006732103,-17.897724427724,12.));
#221686=CARTESIAN_POINT('Ctrl Pts',(15.678532821646,-17.9079377746111,12.));
#221687=CARTESIAN_POINT('Ctrl Pts',(15.6961792415522,-17.9181581507455,
12.));
#221688=CARTESIAN_POINT('Ctrl Pts',(15.7139454725838,-17.9283847588836,
12.));
#221689=CARTESIAN_POINT('Ctrl Pts',(15.7318310003335,-17.9386168123262,
12.));
#221690=CARTESIAN_POINT('Ctrl Pts',(15.749835315086,-17.9488535346781,12.));
#221691=CARTESIAN_POINT('Ctrl Pts',(15.7679579117077,-17.9590941596242,
12.));
#221692=CARTESIAN_POINT('Ctrl Pts',(15.7861982895724,-17.9693379307303,
12.));
#221693=CARTESIAN_POINT('Ctrl Pts',(15.8045559524676,-17.9795841012386,
12.));
#221694=CARTESIAN_POINT('Ctrl Pts',(15.8230304084962,-17.9898319338665,
12.));
#221695=CARTESIAN_POINT('Ctrl Pts',(15.8416211699679,-18.0000807006052,
12.));
#221696=CARTESIAN_POINT('Ctrl Pts',(15.8603277532831,-18.0103296825205,
12.));
#221697=CARTESIAN_POINT('Ctrl Pts',(15.8791496788682,-18.0205781695769,
12.));
#221698=CARTESIAN_POINT('Ctrl Pts',(15.8980864711042,-18.0308254604636,
12.));
#221699=CARTESIAN_POINT('Ctrl Pts',(15.9171376582436,-18.0410708624209,
12.));
#221700=CARTESIAN_POINT('Ctrl Pts',(15.9363027723244,-18.0513136910691,
12.));
#221701=CARTESIAN_POINT('Ctrl Pts',(15.9555813490644,-18.061553270236,12.));
#221702=CARTESIAN_POINT('Ctrl Pts',(15.9749729277846,-18.0717889317958,
12.));
#221703=CARTESIAN_POINT('Ctrl Pts',(15.9944770513613,-18.0820200155236,
12.));
#221704=CARTESIAN_POINT('Ctrl Pts',(16.014093266161,-18.0922458689462,12.));
#221705=CARTESIAN_POINT('Ctrl Pts',(16.0338211219693,-18.1024658471966,
12.));
#221706=CARTESIAN_POINT('Ctrl Pts',(16.0536601719125,-18.112679312869,12.));
#221707=CARTESIAN_POINT('Ctrl Pts',(16.0736099723668,-18.1228856358751,
12.));
#221708=CARTESIAN_POINT('Ctrl Pts',(16.0936700829112,-18.1330841933105,
12.));
#221709=CARTESIAN_POINT('Ctrl Pts',(16.1138400662794,-18.1432743693235,
12.));
#221710=CARTESIAN_POINT('Ctrl Pts',(16.1341194882988,-18.1534555549853,
12.));
#221711=CARTESIAN_POINT('Ctrl Pts',(16.154507917826,-18.1636271481615,12.));
#221712=CARTESIAN_POINT('Ctrl Pts',(16.1750049266671,-18.1737885533849,
12.));
#221713=CARTESIAN_POINT('Ctrl Pts',(16.1956100895073,-18.1839391817331,
12.));
#221714=CARTESIAN_POINT('Ctrl Pts',(16.2163229838875,-18.1940784507229,
12.));
#221715=CARTESIAN_POINT('Ctrl Pts',(16.2371431901638,-18.2042057842035,
12.));
#221716=CARTESIAN_POINT('Ctrl Pts',(16.2580702914615,-18.2143206122529,
12.));
#221717=CARTESIAN_POINT('Ctrl Pts',(16.2791038736223,-18.2244223710746,
12.));
#221718=CARTESIAN_POINT('Ctrl Pts',(16.3002435251378,-18.2345105028982,
12.));
#221719=CARTESIAN_POINT('Ctrl Pts',(16.3214888370987,-18.2445844558742,
12.));
#221720=CARTESIAN_POINT('Ctrl Pts',(16.3428394031589,-18.2546436839608,
12.));
#221721=CARTESIAN_POINT('Ctrl Pts',(16.3642948194868,-18.2646876468169,
12.));
#221722=CARTESIAN_POINT('Ctrl Pts',(16.385854684708,-18.2747158096934,12.));
#221723=CARTESIAN_POINT('Ctrl Pts',(16.4075185998454,-18.2847276433309,
12.));
#221724=CARTESIAN_POINT('Ctrl Pts',(16.4292861682378,-18.294722623851,12.));
#221725=CARTESIAN_POINT('Ctrl Pts',(16.4511569955233,-18.304700232686,12.));
#221726=CARTESIAN_POINT('Ctrl Pts',(16.4731306896441,-18.3146599565231,
12.));
#221727=CARTESIAN_POINT('Ctrl Pts',(16.4952068608345,-18.3246012872469,
12.));
#221728=CARTESIAN_POINT('Ctrl Pts',(16.5173851216045,-18.3345237218864,
12.));
#221729=CARTESIAN_POINT('Ctrl Pts',(16.5396650867139,-18.34442676256,12.));
#221730=CARTESIAN_POINT('Ctrl Pts',(16.5620463731413,-18.354309916433,12.));
#221731=CARTESIAN_POINT('Ctrl Pts',(16.5845286000217,-18.3641726955889,
12.));
#221732=CARTESIAN_POINT('Ctrl Pts',(16.607111388571,-18.3740146168879,12.));
#221733=CARTESIAN_POINT('Ctrl Pts',(16.6297943620056,-18.3838352018327,
12.));
#221734=CARTESIAN_POINT('Ctrl Pts',(16.6525771454513,-18.3936339764332,
12.));
#221735=CARTESIAN_POINT('Ctrl Pts',(16.6754593658513,-18.403410471079,12.));
#221736=CARTESIAN_POINT('Ctrl Pts',(16.698440651849,-18.413164220399,12.));
#221737=CARTESIAN_POINT('Ctrl Pts',(16.7215206338818,-18.4228947633187,
12.));
#221738=CARTESIAN_POINT('Ctrl Pts',(16.7446989442882,-18.4326016431392,
12.));
#221739=CARTESIAN_POINT('Ctrl Pts',(16.7679752173992,-18.44228440761,12.));
#221740=CARTESIAN_POINT('Ctrl Pts',(16.791349089629,-18.4519426090124,12.));
#221741=CARTESIAN_POINT('Ctrl Pts',(16.8148201995472,-18.4615758042305,
12.));
#221742=CARTESIAN_POINT('Ctrl Pts',(16.8383881879709,-18.4711835548623,
12.));
#221743=CARTESIAN_POINT('Ctrl Pts',(16.8620526977171,-18.4807654268771,
12.));
#221744=CARTESIAN_POINT('Ctrl Pts',(16.8858133733088,-18.4903209902227,
12.));
#221745=CARTESIAN_POINT('Ctrl Pts',(16.9096698606943,-18.499849818462,12.));
#221746=CARTESIAN_POINT('Ctrl Pts',(16.9336218069353,-18.5093514883835,
12.));
#221747=CARTESIAN_POINT('Ctrl Pts',(16.9576688599339,-18.5188255796659,
12.));
#221748=CARTESIAN_POINT('Ctrl Pts',(16.981810668038,-18.5282716744197,12.));
#221749=CARTESIAN_POINT('Ctrl Pts',(17.0060468805097,-18.5376893576961,
12.));
#221750=CARTESIAN_POINT('Ctrl Pts',(17.0303771481738,-18.547078218209,12.));
#221751=CARTESIAN_POINT('Ctrl Pts',(17.0548011239751,-18.556437848963,12.));
#221752=CARTESIAN_POINT('Ctrl Pts',(17.0793184636079,-18.5657678479789,
12.));
#221753=CARTESIAN_POINT('Ctrl Pts',(17.1039288260001,-18.5750678188542,
12.));
#221754=CARTESIAN_POINT('Ctrl Pts',(17.1286318741183,-18.5843373717247,
12.));
#221755=CARTESIAN_POINT('Ctrl Pts',(17.1534272741643,-18.5935761222825,
12.));
#221756=CARTESIAN_POINT('Ctrl Pts',(17.1783146940127,-18.6027836898817,
12.));
#221757=CARTESIAN_POINT('Ctrl Pts',(17.2032938019284,-18.6119596959949,
12.));
#221758=CARTESIAN_POINT('Ctrl Pts',(17.2283642650517,-18.6211037624038,
12.));
#221759=CARTESIAN_POINT('Ctrl Pts',(17.2535257482187,-18.6302155097943,
12.));
#221760=CARTESIAN_POINT('Ctrl Pts',(17.2787779120213,-18.6392945554748,
12.));
#221761=CARTESIAN_POINT('Ctrl Pts',(17.3041204135074,-18.6483405141865,
12.));
#221762=CARTESIAN_POINT('Ctrl Pts',(17.3295529098618,-18.6573530024033,
12.));
#221763=CARTESIAN_POINT('Ctrl Pts',(17.3550750612443,-18.6663316416582,
12.));
#221764=CARTESIAN_POINT('Ctrl Pts',(17.3806865340747,-18.6752760624052,
12.));
#221765=CARTESIAN_POINT('Ctrl Pts',(17.4063870038562,-18.6841859073471,
12.));
#221766=CARTESIAN_POINT('Ctrl Pts',(17.4321761588142,-18.6930608357409,
12.));
#221767=CARTESIAN_POINT('Ctrl Pts',(17.4580537012753,-18.70190052503,12.));
#221768=CARTESIAN_POINT('Ctrl Pts',(17.4840193397162,-18.7107046613912,
12.));
#221769=CARTESIAN_POINT('Ctrl Pts',(17.5100727820876,-18.7194729318098,
12.));
#221770=CARTESIAN_POINT('Ctrl Pts',(17.5362137287593,-18.7282050157138,
12.));
#221771=CARTESIAN_POINT('Ctrl Pts',(17.5624418653245,-18.7369005764553,
12.));
#221772=CARTESIAN_POINT('Ctrl Pts',(17.5887568561371,-18.7455592536688,
12.));
#221773=CARTESIAN_POINT('Ctrl Pts',(17.6151583357012,-18.7541806530984,
12.));
#221774=CARTESIAN_POINT('Ctrl Pts',(17.6416459210681,-18.762764361321,12.));
#221775=CARTESIAN_POINT('Ctrl Pts',(17.6682192274236,-18.7713099642754,
12.));
#221776=CARTESIAN_POINT('Ctrl Pts',(17.6948778823014,-18.7798170641374,
12.));
#221777=CARTESIAN_POINT('Ctrl Pts',(17.7216215409035,-18.788285297605,12.));
#221778=CARTESIAN_POINT('Ctrl Pts',(17.7484498996905,-18.7967143519419,
12.));
#221779=CARTESIAN_POINT('Ctrl Pts',(17.7753627137853,-18.8051039860448,
12.));
#221780=CARTESIAN_POINT('Ctrl Pts',(17.8023598011057,-18.8134540340417,
12.));
#221781=CARTESIAN_POINT('Ctrl Pts',(17.8294410311006,-18.8217643886157,
12.));
#221782=CARTESIAN_POINT('Ctrl Pts',(17.856606317477,-18.8300349895974,12.));
#221783=CARTESIAN_POINT('Ctrl Pts',(17.8784057509355,-18.8366196462581,
12.));
#221784=CARTESIAN_POINT('Ctrl Pts',(17.8947931177807,-18.8415402351786,
12.));
#221785=CARTESIAN_POINT('Ctrl Pts',(17.9057348246595,-18.8448126709692,
12.));
#221786=CARTESIAN_POINT('Ctrl Pts',(17.9112098770111,-18.8464468996588,
12.));
#221787=CARTESIAN_POINT('Ctrl Pts',(12.7689476255362,-18.5896416359912,
0.));
#221788=CARTESIAN_POINT('Ctrl Pts',(12.7689476255362,-18.5896416359912,
12.));
#221789=CARTESIAN_POINT('Ctrl Pts',(12.7689524524483,-18.5896460962964,
0.));
#221790=CARTESIAN_POINT('Ctrl Pts',(12.7689524524483,-18.5896460962964,
12.));
#221791=CARTESIAN_POINT('Ctrl Pts',(12.768986426692,-18.5896919669165,0.));
#221792=CARTESIAN_POINT('Ctrl Pts',(12.768986426692,-18.5896919669165,12.));
#221793=CARTESIAN_POINT('Ctrl Pts',(12.769110348199,-18.589871621843,0.));
#221794=CARTESIAN_POINT('Ctrl Pts',(12.769110348199,-18.589871621843,12.));
#221795=CARTESIAN_POINT('Ctrl Pts',(12.7694215127918,-18.5903328777227,
0.));
#221796=CARTESIAN_POINT('Ctrl Pts',(12.7694215127918,-18.5903328777227,
12.));
#221797=CARTESIAN_POINT('Ctrl Pts',(12.7700520897173,-18.5912775137806,
0.));
#221798=CARTESIAN_POINT('Ctrl Pts',(12.7700520897173,-18.5912775137806,
12.));
#221799=CARTESIAN_POINT('Ctrl Pts',(12.7709195951156,-18.5925859134579,
0.));
#221800=CARTESIAN_POINT('Ctrl Pts',(12.7709195951156,-18.5925859134579,
12.));
#221801=CARTESIAN_POINT('Ctrl Pts',(12.7720142287172,-18.5942490615407,
0.));
#221802=CARTESIAN_POINT('Ctrl Pts',(12.7720142287172,-18.5942490615407,
12.));
#221803=CARTESIAN_POINT('Ctrl Pts',(12.7733231262108,-18.5962551167772,
0.));
#221804=CARTESIAN_POINT('Ctrl Pts',(12.7733231262108,-18.5962551167772,
12.));
#221805=CARTESIAN_POINT('Ctrl Pts',(12.7748328937638,-18.598591752595,0.));
#221806=CARTESIAN_POINT('Ctrl Pts',(12.7748328937638,-18.598591752595,12.));
#221807=CARTESIAN_POINT('Ctrl Pts',(12.7765325225081,-18.6012488486709,
0.));
#221808=CARTESIAN_POINT('Ctrl Pts',(12.7765325225081,-18.6012488486709,
12.));
#221809=CARTESIAN_POINT('Ctrl Pts',(12.7784139605066,-18.6042190183704,
0.));
#221810=CARTESIAN_POINT('Ctrl Pts',(12.7784139605066,-18.6042190183704,
12.));
#221811=CARTESIAN_POINT('Ctrl Pts',(12.7804705387658,-18.6074961535723,
0.));
#221812=CARTESIAN_POINT('Ctrl Pts',(12.7804705387658,-18.6074961535723,
12.));
#221813=CARTESIAN_POINT('Ctrl Pts',(12.7826959526924,-18.611074482622,0.));
#221814=CARTESIAN_POINT('Ctrl Pts',(12.7826959526924,-18.611074482622,12.));
#221815=CARTESIAN_POINT('Ctrl Pts',(12.7850831657901,-18.6149475565188,
0.));
#221816=CARTESIAN_POINT('Ctrl Pts',(12.7850831657901,-18.6149475565188,
12.));
#221817=CARTESIAN_POINT('Ctrl Pts',(12.7876249657834,-18.6191087624752,
0.));
#221818=CARTESIAN_POINT('Ctrl Pts',(12.7876249657834,-18.6191087624752,
12.));
#221819=CARTESIAN_POINT('Ctrl Pts',(12.7903142925234,-18.6235516265575,
0.));
#221820=CARTESIAN_POINT('Ctrl Pts',(12.7903142925234,-18.6235516265575,
12.));
#221821=CARTESIAN_POINT('Ctrl Pts',(12.7931447451555,-18.6282702819371,
0.));
#221822=CARTESIAN_POINT('Ctrl Pts',(12.7931447451555,-18.6282702819371,
12.));
#221823=CARTESIAN_POINT('Ctrl Pts',(12.796110622225,-18.6332595057006,0.));
#221824=CARTESIAN_POINT('Ctrl Pts',(12.796110622225,-18.6332595057006,12.));
#221825=CARTESIAN_POINT('Ctrl Pts',(12.7992066625264,-18.63851447924,0.));
#221826=CARTESIAN_POINT('Ctrl Pts',(12.7992066625264,-18.63851447924,12.));
#221827=CARTESIAN_POINT('Ctrl Pts',(12.8024278770152,-18.6440306327456,
0.));
#221828=CARTESIAN_POINT('Ctrl Pts',(12.8024278770152,-18.6440306327456,
12.));
#221829=CARTESIAN_POINT('Ctrl Pts',(12.805769331162,-18.6498034438987,0.));
#221830=CARTESIAN_POINT('Ctrl Pts',(12.805769331162,-18.6498034438987,12.));
#221831=CARTESIAN_POINT('Ctrl Pts',(12.8092261933858,-18.6558284825773,
0.));
#221832=CARTESIAN_POINT('Ctrl Pts',(12.8092261933858,-18.6558284825773,
12.));
#221833=CARTESIAN_POINT('Ctrl Pts',(12.8127937909631,-18.6621014624746,
0.));
#221834=CARTESIAN_POINT('Ctrl Pts',(12.8127937909631,-18.6621014624746,
12.));
#221835=CARTESIAN_POINT('Ctrl Pts',(12.8164676687362,-18.66861829528,0.));
#221836=CARTESIAN_POINT('Ctrl Pts',(12.8164676687362,-18.66861829528,12.));
#221837=CARTESIAN_POINT('Ctrl Pts',(12.8202436318474,-18.6753751301092,
0.));
#221838=CARTESIAN_POINT('Ctrl Pts',(12.8202436318474,-18.6753751301092,
12.));
#221839=CARTESIAN_POINT('Ctrl Pts',(12.8241176980017,-18.6823683094139,
0.));
#221840=CARTESIAN_POINT('Ctrl Pts',(12.8241176980017,-18.6823683094139,
12.));
#221841=CARTESIAN_POINT('Ctrl Pts',(12.8280860635231,-18.6895943376172,
0.));
#221842=CARTESIAN_POINT('Ctrl Pts',(12.8280860635231,-18.6895943376172,
12.));
#221843=CARTESIAN_POINT('Ctrl Pts',(12.8321450599789,-18.6970498410172,
0.));
#221844=CARTESIAN_POINT('Ctrl Pts',(12.8321450599789,-18.6970498410172,
12.));
#221845=CARTESIAN_POINT('Ctrl Pts',(12.8362911280361,-18.7047315436294,
0.));
#221846=CARTESIAN_POINT('Ctrl Pts',(12.8362911280361,-18.7047315436294,
12.));
#221847=CARTESIAN_POINT('Ctrl Pts',(12.8405208263431,-18.7126362754445,
0.));
#221848=CARTESIAN_POINT('Ctrl Pts',(12.8405208263431,-18.7126362754445,
12.));
#221849=CARTESIAN_POINT('Ctrl Pts',(12.8448308329494,-18.7207609737702,
0.));
#221850=CARTESIAN_POINT('Ctrl Pts',(12.8448308329494,-18.7207609737702,
12.));
#221851=CARTESIAN_POINT('Ctrl Pts',(12.8492179511591,-18.7291026886554,
0.));
#221852=CARTESIAN_POINT('Ctrl Pts',(12.8492179511591,-18.7291026886554,
12.));
#221853=CARTESIAN_POINT('Ctrl Pts',(12.8536791086316,-18.7376585820854,
0.));
#221854=CARTESIAN_POINT('Ctrl Pts',(12.8536791086316,-18.7376585820854,
12.));
#221855=CARTESIAN_POINT('Ctrl Pts',(12.8582113455646,-18.7464259171251,
0.));
#221856=CARTESIAN_POINT('Ctrl Pts',(12.8582113455646,-18.7464259171251,
12.));
#221857=CARTESIAN_POINT('Ctrl Pts',(12.8628118054171,-18.7554020493887,
0.));
#221858=CARTESIAN_POINT('Ctrl Pts',(12.8628118054171,-18.7554020493887,
12.));
#221859=CARTESIAN_POINT('Ctrl Pts',(12.8674777239653,-18.7645844169564,
0.));
#221860=CARTESIAN_POINT('Ctrl Pts',(12.8674777239653,-18.7645844169564,
12.));
#221861=CARTESIAN_POINT('Ctrl Pts',(12.872206421181,-18.7739705329022,0.));
#221862=CARTESIAN_POINT('Ctrl Pts',(12.872206421181,-18.7739705329022,12.));
#221863=CARTESIAN_POINT('Ctrl Pts',(12.8769952998095,-18.7835579840477,
0.));
#221864=CARTESIAN_POINT('Ctrl Pts',(12.8769952998095,-18.7835579840477,
12.));
#221865=CARTESIAN_POINT('Ctrl Pts',(12.8818418427475,-18.7933444285868,
0.));
#221866=CARTESIAN_POINT('Ctrl Pts',(12.8818418427475,-18.7933444285868,
12.));
#221867=CARTESIAN_POINT('Ctrl Pts',(12.8867436109546,-18.8033275941943,
0.));
#221868=CARTESIAN_POINT('Ctrl Pts',(12.8867436109546,-18.8033275941943,
12.));
#221869=CARTESIAN_POINT('Ctrl Pts',(12.8916982409935,-18.813505275782,0.));
#221870=CARTESIAN_POINT('Ctrl Pts',(12.8916982409935,-18.813505275782,12.));
#221871=CARTESIAN_POINT('Ctrl Pts',(12.8967034410754,-18.8238753319129,
0.));
#221872=CARTESIAN_POINT('Ctrl Pts',(12.8967034410754,-18.8238753319129,
12.));
#221873=CARTESIAN_POINT('Ctrl Pts',(12.9017569871738,-18.8344356812591,
0.));
#221874=CARTESIAN_POINT('Ctrl Pts',(12.9017569871738,-18.8344356812591,
12.));
#221875=CARTESIAN_POINT('Ctrl Pts',(12.9068567191854,-18.8451842990984,
0.));
#221876=CARTESIAN_POINT('Ctrl Pts',(12.9068567191854,-18.8451842990984,
12.));
#221877=CARTESIAN_POINT('Ctrl Pts',(12.9120005369063,-18.8561192136198,
0.));
#221878=CARTESIAN_POINT('Ctrl Pts',(12.9120005369063,-18.8561192136198,
12.));
#221879=CARTESIAN_POINT('Ctrl Pts',(12.9171863977045,-18.8672385038326,
0.));
#221880=CARTESIAN_POINT('Ctrl Pts',(12.9171863977045,-18.8672385038326,
12.));
#221881=CARTESIAN_POINT('Ctrl Pts',(12.9224123144981,-18.8785402977528,
0.));
#221882=CARTESIAN_POINT('Ctrl Pts',(12.9224123144981,-18.8785402977528,
12.));
#221883=CARTESIAN_POINT('Ctrl Pts',(12.9276763536373,-18.8900227704889,
0.));
#221884=CARTESIAN_POINT('Ctrl Pts',(12.9276763536373,-18.8900227704889,
12.));
#221885=CARTESIAN_POINT('Ctrl Pts',(12.9329766328184,-18.9016841423403,
0.));
#221886=CARTESIAN_POINT('Ctrl Pts',(12.9329766328184,-18.9016841423403,
12.));
#221887=CARTESIAN_POINT('Ctrl Pts',(12.9383113190374,-18.9135226769466,
0.));
#221888=CARTESIAN_POINT('Ctrl Pts',(12.9383113190374,-18.9135226769466,
12.));
#221889=CARTESIAN_POINT('Ctrl Pts',(12.9436786266105,-18.9255366795195,
0.));
#221890=CARTESIAN_POINT('Ctrl Pts',(12.9436786266105,-18.9255366795195,
12.));
#221891=CARTESIAN_POINT('Ctrl Pts',(12.9490768151821,-18.9377244950435,
0.));
#221892=CARTESIAN_POINT('Ctrl Pts',(12.9490768151821,-18.9377244950435,
12.));
#221893=CARTESIAN_POINT('Ctrl Pts',(12.9545041877377,-18.9500845064715,
0.));
#221894=CARTESIAN_POINT('Ctrl Pts',(12.9545041877377,-18.9500845064715,
12.));
#221895=CARTESIAN_POINT('Ctrl Pts',(12.9599590886319,-18.9626151329229,
0.));
#221896=CARTESIAN_POINT('Ctrl Pts',(12.9599590886319,-18.9626151329229,
12.));
#221897=CARTESIAN_POINT('Ctrl Pts',(12.9654399021869,-18.9753148284475,
0.));
#221898=CARTESIAN_POINT('Ctrl Pts',(12.9654399021869,-18.9753148284475,
12.));
#221899=CARTESIAN_POINT('Ctrl Pts',(12.9709450512747,-18.9881820807586,
0.));
#221900=CARTESIAN_POINT('Ctrl Pts',(12.9709450512747,-18.9881820807586,
12.));
#221901=CARTESIAN_POINT('Ctrl Pts',(12.9764729959205,-19.0012154099791,
0.));
#221902=CARTESIAN_POINT('Ctrl Pts',(12.9764729959205,-19.0012154099791,
12.));
#221903=CARTESIAN_POINT('Ctrl Pts',(12.9820222318715,-19.0144133673348,
0.));
#221904=CARTESIAN_POINT('Ctrl Pts',(12.9820222318715,-19.0144133673348,
12.));
#221905=CARTESIAN_POINT('Ctrl Pts',(12.9875912893003,-19.0277745339908,
0.));
#221906=CARTESIAN_POINT('Ctrl Pts',(12.9875912893003,-19.0277745339908,
12.));
#221907=CARTESIAN_POINT('Ctrl Pts',(12.9931787316514,-19.0412975200398,
0.));
#221908=CARTESIAN_POINT('Ctrl Pts',(12.9931787316514,-19.0412975200398,
12.));
#221909=CARTESIAN_POINT('Ctrl Pts',(12.9987831544502,-19.0549809634355,
0.));
#221910=CARTESIAN_POINT('Ctrl Pts',(12.9987831544502,-19.0549809634355,
12.));
#221911=CARTESIAN_POINT('Ctrl Pts',(13.0044031841381,-19.0688235289437,
0.));
#221912=CARTESIAN_POINT('Ctrl Pts',(13.0044031841381,-19.0688235289437,
12.));
#221913=CARTESIAN_POINT('Ctrl Pts',(13.0100374768785,-19.0828239070482,
0.));
#221914=CARTESIAN_POINT('Ctrl Pts',(13.0100374768785,-19.0828239070482,
12.));
#221915=CARTESIAN_POINT('Ctrl Pts',(13.0156847176093,-19.0969808131226,
0.));
#221916=CARTESIAN_POINT('Ctrl Pts',(13.0156847176093,-19.0969808131226,
12.));
#221917=CARTESIAN_POINT('Ctrl Pts',(13.0213436191326,-19.1112929866308,
0.));
#221918=CARTESIAN_POINT('Ctrl Pts',(13.0213436191326,-19.1112929866308,
12.));
#221919=CARTESIAN_POINT('Ctrl Pts',(13.0270129211976,-19.1257591903099,
0.));
#221920=CARTESIAN_POINT('Ctrl Pts',(13.0270129211976,-19.1257591903099,
12.));
#221921=CARTESIAN_POINT('Ctrl Pts',(13.0326913895841,-19.1403782093389,
0.));
#221922=CARTESIAN_POINT('Ctrl Pts',(13.0326913895841,-19.1403782093389,
12.));
#221923=CARTESIAN_POINT('Ctrl Pts',(13.0383778152072,-19.1551488505233,
0.));
#221924=CARTESIAN_POINT('Ctrl Pts',(13.0383778152072,-19.1551488505233,
12.));
#221925=CARTESIAN_POINT('Ctrl Pts',(13.0440710133775,-19.1700699416625,
0.));
#221926=CARTESIAN_POINT('Ctrl Pts',(13.0440710133775,-19.1700699416625,
12.));
#221927=CARTESIAN_POINT('Ctrl Pts',(13.0497698230442,-19.1851403308826,
0.));
#221928=CARTESIAN_POINT('Ctrl Pts',(13.0497698230442,-19.1851403308826,
12.));
#221929=CARTESIAN_POINT('Ctrl Pts',(13.0554731060537,-19.2003588859771,
0.));
#221930=CARTESIAN_POINT('Ctrl Pts',(13.0554731060537,-19.2003588859771,
12.));
#221931=CARTESIAN_POINT('Ctrl Pts',(13.0611797463912,-19.2157244937141,
0.));
#221932=CARTESIAN_POINT('Ctrl Pts',(13.0611797463912,-19.2157244937141,
12.));
#221933=CARTESIAN_POINT('Ctrl Pts',(13.0668886494791,-19.2312360592031,
0.));
#221934=CARTESIAN_POINT('Ctrl Pts',(13.0668886494791,-19.2312360592031,
12.));
#221935=CARTESIAN_POINT('Ctrl Pts',(13.0725987415856,-19.2468925053988,
0.));
#221936=CARTESIAN_POINT('Ctrl Pts',(13.0725987415856,-19.2468925053988,
12.));
#221937=CARTESIAN_POINT('Ctrl Pts',(13.0783089692117,-19.2626927725596,
0.));
#221938=CARTESIAN_POINT('Ctrl Pts',(13.0783089692117,-19.2626927725596,
12.));
#221939=CARTESIAN_POINT('Ctrl Pts',(13.0840182984949,-19.2786358177198,
0.));
#221940=CARTESIAN_POINT('Ctrl Pts',(13.0840182984949,-19.2786358177198,
12.));
#221941=CARTESIAN_POINT('Ctrl Pts',(13.0897257145969,-19.2947206141246,
0.));
#221942=CARTESIAN_POINT('Ctrl Pts',(13.0897257145969,-19.2947206141246,
12.));
#221943=CARTESIAN_POINT('Ctrl Pts',(13.095430221148,-19.3109461507358,0.));
#221944=CARTESIAN_POINT('Ctrl Pts',(13.095430221148,-19.3109461507358,12.));
#221945=CARTESIAN_POINT('Ctrl Pts',(13.1011308397591,-19.3273114318268,
0.));
#221946=CARTESIAN_POINT('Ctrl Pts',(13.1011308397591,-19.3273114318268,
12.));
#221947=CARTESIAN_POINT('Ctrl Pts',(13.1068266095186,-19.3438154765395,
0.));
#221948=CARTESIAN_POINT('Ctrl Pts',(13.1068266095186,-19.3438154765395,
12.));
#221949=CARTESIAN_POINT('Ctrl Pts',(13.1125165865021,-19.3604573184516,
0.));
#221950=CARTESIAN_POINT('Ctrl Pts',(13.1125165865021,-19.3604573184516,
12.));
#221951=CARTESIAN_POINT('Ctrl Pts',(13.118199843271,-19.3772360051093,0.));
#221952=CARTESIAN_POINT('Ctrl Pts',(13.118199843271,-19.3772360051093,12.));
#221953=CARTESIAN_POINT('Ctrl Pts',(13.1238754684177,-19.3941505976267,
0.));
#221954=CARTESIAN_POINT('Ctrl Pts',(13.1238754684177,-19.3941505976267,
12.));
#221955=CARTESIAN_POINT('Ctrl Pts',(13.1295425661635,-19.4112001703561,
0.));
#221956=CARTESIAN_POINT('Ctrl Pts',(13.1295425661635,-19.4112001703561,
12.));
#221957=CARTESIAN_POINT('Ctrl Pts',(13.1352002559439,-19.4283838105265,
0.));
#221958=CARTESIAN_POINT('Ctrl Pts',(13.1352002559439,-19.4283838105265,
12.));
#221959=CARTESIAN_POINT('Ctrl Pts',(13.140847672006,-19.4457006178875,0.));
#221960=CARTESIAN_POINT('Ctrl Pts',(13.140847672006,-19.4457006178875,12.));
#221961=CARTESIAN_POINT('Ctrl Pts',(13.1464839629966,-19.463149704325,0.));
#221962=CARTESIAN_POINT('Ctrl Pts',(13.1464839629966,-19.463149704325,12.));
#221963=CARTESIAN_POINT('Ctrl Pts',(13.1521082915846,-19.4807301935256,
0.));
#221964=CARTESIAN_POINT('Ctrl Pts',(13.1521082915846,-19.4807301935256,
12.));
#221965=CARTESIAN_POINT('Ctrl Pts',(13.1577198341238,-19.498441220707,0.));
#221966=CARTESIAN_POINT('Ctrl Pts',(13.1577198341238,-19.498441220707,12.));
#221967=CARTESIAN_POINT('Ctrl Pts',(13.1633177803097,-19.5162819323207,
0.));
#221968=CARTESIAN_POINT('Ctrl Pts',(13.1633177803097,-19.5162819323207,
12.));
#221969=CARTESIAN_POINT('Ctrl Pts',(13.1689013328432,-19.5342514857564,
0.));
#221970=CARTESIAN_POINT('Ctrl Pts',(13.1689013328432,-19.5342514857564,
12.));
#221971=CARTESIAN_POINT('Ctrl Pts',(13.1744697070918,-19.5523490490254,
0.));
#221972=CARTESIAN_POINT('Ctrl Pts',(13.1744697070918,-19.5523490490254,
12.));
#221973=CARTESIAN_POINT('Ctrl Pts',(13.1800221307682,-19.5705738004682,
0.));
#221974=CARTESIAN_POINT('Ctrl Pts',(13.1800221307682,-19.5705738004682,
12.));
#221975=CARTESIAN_POINT('Ctrl Pts',(13.1855578436479,-19.5889249285352,
0.));
#221976=CARTESIAN_POINT('Ctrl Pts',(13.1855578436479,-19.5889249285352,
12.));
#221977=CARTESIAN_POINT('Ctrl Pts',(13.1910760972818,-19.6074016315421,
0.));
#221978=CARTESIAN_POINT('Ctrl Pts',(13.1910760972818,-19.6074016315421,
12.));
#221979=CARTESIAN_POINT('Ctrl Pts',(13.196576154715,-19.6260031174244,0.));
#221980=CARTESIAN_POINT('Ctrl Pts',(13.196576154715,-19.6260031174244,12.));
#221981=CARTESIAN_POINT('Ctrl Pts',(13.202057290206,-19.6447286034764,0.));
#221982=CARTESIAN_POINT('Ctrl Pts',(13.202057290206,-19.6447286034764,12.));
#221983=CARTESIAN_POINT('Ctrl Pts',(13.2075187889522,-19.6635773160924,
0.));
#221984=CARTESIAN_POINT('Ctrl Pts',(13.2075187889522,-19.6635773160924,
12.));
#221985=CARTESIAN_POINT('Ctrl Pts',(13.2129599468478,-19.6825484905812,
0.));
#221986=CARTESIAN_POINT('Ctrl Pts',(13.2129599468478,-19.6825484905812,
12.));
#221987=CARTESIAN_POINT('Ctrl Pts',(13.2183800702431,-19.7016413709678,
0.));
#221988=CARTESIAN_POINT('Ctrl Pts',(13.2183800702431,-19.7016413709678,
12.));
#221989=CARTESIAN_POINT('Ctrl Pts',(13.2237784757065,-19.7208552097867,
0.));
#221990=CARTESIAN_POINT('Ctrl Pts',(13.2237784757065,-19.7208552097867,
12.));
#221991=CARTESIAN_POINT('Ctrl Pts',(13.2291544897902,-19.7401892678701,
0.));
#221992=CARTESIAN_POINT('Ctrl Pts',(13.2291544897902,-19.7401892678701,
12.));
#221993=CARTESIAN_POINT('Ctrl Pts',(13.2345074487968,-19.7596428141176,
0.));
#221994=CARTESIAN_POINT('Ctrl Pts',(13.2345074487968,-19.7596428141176,
12.));
#221995=CARTESIAN_POINT('Ctrl Pts',(13.239836698568,-19.7792151253297,0.));
#221996=CARTESIAN_POINT('Ctrl Pts',(13.239836698568,-19.7792151253297,12.));
#221997=CARTESIAN_POINT('Ctrl Pts',(13.2451415942809,-19.7989054860501,
0.));
#221998=CARTESIAN_POINT('Ctrl Pts',(13.2451415942809,-19.7989054860501,
12.));
#221999=CARTESIAN_POINT('Ctrl Pts',(13.2504215002458,-19.8187131883919,
0.));
#222000=CARTESIAN_POINT('Ctrl Pts',(13.2504215002458,-19.8187131883919,
12.));
#222001=CARTESIAN_POINT('Ctrl Pts',(13.2556757897085,-19.8386375318632,
0.));
#222002=CARTESIAN_POINT('Ctrl Pts',(13.2556757897085,-19.8386375318632,
12.));
#222003=CARTESIAN_POINT('Ctrl Pts',(13.2609038446525,-19.8586778231711,
0.));
#222004=CARTESIAN_POINT('Ctrl Pts',(13.2609038446525,-19.8586778231711,
12.));
#222005=CARTESIAN_POINT('Ctrl Pts',(13.2661050556128,-19.8788333760571,
0.));
#222006=CARTESIAN_POINT('Ctrl Pts',(13.2661050556128,-19.8788333760571,
12.));
#222007=CARTESIAN_POINT('Ctrl Pts',(13.2712788215015,-19.8991035111739,
0.));
#222008=CARTESIAN_POINT('Ctrl Pts',(13.2712788215015,-19.8991035111739,
12.));
#222009=CARTESIAN_POINT('Ctrl Pts',(13.2764245494354,-19.9194875559419,
0.));
#222010=CARTESIAN_POINT('Ctrl Pts',(13.2764245494354,-19.9194875559419,
12.));
#222011=CARTESIAN_POINT('Ctrl Pts',(13.2815416545662,-19.939984844402,0.));
#222012=CARTESIAN_POINT('Ctrl Pts',(13.2815416545662,-19.939984844402,12.));
#222013=CARTESIAN_POINT('Ctrl Pts',(13.2866295599152,-19.9605947170589,
0.));
#222014=CARTESIAN_POINT('Ctrl Pts',(13.2866295599152,-19.9605947170589,
12.));
#222015=CARTESIAN_POINT('Ctrl Pts',(13.2916876962098,-19.9813165207174,
0.));
#222016=CARTESIAN_POINT('Ctrl Pts',(13.2916876962098,-19.9813165207174,
12.));
#222017=CARTESIAN_POINT('Ctrl Pts',(13.296715501731,-20.0021496083742,0.));
#222018=CARTESIAN_POINT('Ctrl Pts',(13.296715501731,-20.0021496083742,12.));
#222019=CARTESIAN_POINT('Ctrl Pts',(13.3017124221639,-20.023093339104,0.));
#222020=CARTESIAN_POINT('Ctrl Pts',(13.3017124221639,-20.023093339104,12.));
#222021=CARTESIAN_POINT('Ctrl Pts',(13.3066779104515,-20.0441470779345,
0.));
#222022=CARTESIAN_POINT('Ctrl Pts',(13.3066779104515,-20.0441470779345,
12.));
#222023=CARTESIAN_POINT('Ctrl Pts',(13.3116114266514,-20.0653101957188,
0.));
#222024=CARTESIAN_POINT('Ctrl Pts',(13.3116114266514,-20.0653101957188,
12.));
#222025=CARTESIAN_POINT('Ctrl Pts',(13.3165124377962,-20.0865820689884,
0.));
#222026=CARTESIAN_POINT('Ctrl Pts',(13.3165124377962,-20.0865820689884,
12.));
#222027=CARTESIAN_POINT('Ctrl Pts',(13.3213804177588,-20.1079620798377,
0.));
#222028=CARTESIAN_POINT('Ctrl Pts',(13.3213804177588,-20.1079620798377,
12.));
#222029=CARTESIAN_POINT('Ctrl Pts',(13.3262148471228,-20.1294496158405,
0.));
#222030=CARTESIAN_POINT('Ctrl Pts',(13.3262148471228,-20.1294496158405,
12.));
#222031=CARTESIAN_POINT('Ctrl Pts',(13.3310152130565,-20.1510440699477,
0.));
#222032=CARTESIAN_POINT('Ctrl Pts',(13.3310152130565,-20.1510440699477,
12.));
#222033=CARTESIAN_POINT('Ctrl Pts',(13.3357810091903,-20.1727448403818,
0.));
#222034=CARTESIAN_POINT('Ctrl Pts',(13.3357810091903,-20.1727448403818,
12.));
#222035=CARTESIAN_POINT('Ctrl Pts',(13.3405117354969,-20.1945513305233,
0.));
#222036=CARTESIAN_POINT('Ctrl Pts',(13.3405117354969,-20.1945513305233,
12.));
#222037=CARTESIAN_POINT('Ctrl Pts',(13.3452068981762,-20.2164629487855,
0.));
#222038=CARTESIAN_POINT('Ctrl Pts',(13.3452068981762,-20.2164629487855,
12.));
#222039=CARTESIAN_POINT('Ctrl Pts',(13.3498660095381,-20.2384791085354,
0.));
#222040=CARTESIAN_POINT('Ctrl Pts',(13.3498660095381,-20.2384791085354,
12.));
#222041=CARTESIAN_POINT('Ctrl Pts',(13.3544885878886,-20.2605992280117,
0.));
#222042=CARTESIAN_POINT('Ctrl Pts',(13.3544885878886,-20.2605992280117,
12.));
#222043=CARTESIAN_POINT('Ctrl Pts',(13.3590741574194,-20.2828227302337,
0.));
#222044=CARTESIAN_POINT('Ctrl Pts',(13.3590741574194,-20.2828227302337,
12.));
#222045=CARTESIAN_POINT('Ctrl Pts',(13.3636222481016,-20.3051490429049,
0.));
#222046=CARTESIAN_POINT('Ctrl Pts',(13.3636222481016,-20.3051490429049,
12.));
#222047=CARTESIAN_POINT('Ctrl Pts',(13.3681323955828,-20.3275775983032,
0.));
#222048=CARTESIAN_POINT('Ctrl Pts',(13.3681323955828,-20.3275775983032,
12.));
#222049=CARTESIAN_POINT('Ctrl Pts',(13.3726041410869,-20.3501078331818,
0.));
#222050=CARTESIAN_POINT('Ctrl Pts',(13.3726041410869,-20.3501078331818,
12.));
#222051=CARTESIAN_POINT('Ctrl Pts',(13.377037031319,-20.3727391887187,0.));
#222052=CARTESIAN_POINT('Ctrl Pts',(13.377037031319,-20.3727391887187,12.));
#222053=CARTESIAN_POINT('Ctrl Pts',(13.3814306183721,-20.3954711104505,
0.));
#222054=CARTESIAN_POINT('Ctrl Pts',(13.3814306183721,-20.3954711104505,
12.));
#222055=CARTESIAN_POINT('Ctrl Pts',(13.3857844596387,-20.4183030482002,
0.));
#222056=CARTESIAN_POINT('Ctrl Pts',(13.3857844596387,-20.4183030482002,
12.));
#222057=CARTESIAN_POINT('Ctrl Pts',(13.3900981177254,-20.4412344560007,
0.));
#222058=CARTESIAN_POINT('Ctrl Pts',(13.3900981177254,-20.4412344560007,
12.));
#222059=CARTESIAN_POINT('Ctrl Pts',(13.3943711603739,-20.4642647920038,
0.));
#222060=CARTESIAN_POINT('Ctrl Pts',(13.3943711603739,-20.4642647920038,
12.));
#222061=CARTESIAN_POINT('Ctrl Pts',(13.3986031603716,-20.4873935184041,
0.));
#222062=CARTESIAN_POINT('Ctrl Pts',(13.3986031603716,-20.4873935184041,
12.));
#222063=CARTESIAN_POINT('Ctrl Pts',(13.4027936954529,-20.5106201013755,
0.));
#222064=CARTESIAN_POINT('Ctrl Pts',(13.4027936954529,-20.5106201013755,
12.));
#222065=CARTESIAN_POINT('Ctrl Pts',(13.4069423482076,-20.5339440109958,
0.));
#222066=CARTESIAN_POINT('Ctrl Pts',(13.4069423482076,-20.5339440109958,
12.));
#222067=CARTESIAN_POINT('Ctrl Pts',(13.4110487059912,-20.557364721164,0.));
#222068=CARTESIAN_POINT('Ctrl Pts',(13.4110487059912,-20.557364721164,12.));
#222069=CARTESIAN_POINT('Ctrl Pts',(13.415112360841,-20.5808817095155,0.));
#222070=CARTESIAN_POINT('Ctrl Pts',(13.415112360841,-20.5808817095155,12.));
#222071=CARTESIAN_POINT('Ctrl Pts',(13.4191329093931,-20.6044944573151,
0.));
#222072=CARTESIAN_POINT('Ctrl Pts',(13.4191329093931,-20.6044944573151,
12.));
#222073=CARTESIAN_POINT('Ctrl Pts',(13.4231099528178,-20.6282024494234,
0.));
#222074=CARTESIAN_POINT('Ctrl Pts',(13.4231099528178,-20.6282024494234,
12.));
#222075=CARTESIAN_POINT('Ctrl Pts',(13.427043096765,-20.6520051742868,0.));
#222076=CARTESIAN_POINT('Ctrl Pts',(13.427043096765,-20.6520051742868,12.));
#222077=CARTESIAN_POINT('Ctrl Pts',(13.4309319513119,-20.6759021239102,
0.));
#222078=CARTESIAN_POINT('Ctrl Pts',(13.4309319513119,-20.6759021239102,
12.));
#222079=CARTESIAN_POINT('Ctrl Pts',(13.4347761309154,-20.6998927938288,
0.));
#222080=CARTESIAN_POINT('Ctrl Pts',(13.4347761309154,-20.6998927938288,
12.));
#222081=CARTESIAN_POINT('Ctrl Pts',(13.4385752543663,-20.7239766830676,
0.));
#222082=CARTESIAN_POINT('Ctrl Pts',(13.4385752543663,-20.7239766830676,
12.));
#222083=CARTESIAN_POINT('Ctrl Pts',(13.4423289447561,-20.7481532941014,
0.));
#222084=CARTESIAN_POINT('Ctrl Pts',(13.4423289447561,-20.7481532941014,
12.));
#222085=CARTESIAN_POINT('Ctrl Pts',(13.4460368293689,-20.7724221327609,
0.));
#222086=CARTESIAN_POINT('Ctrl Pts',(13.4460368293689,-20.7724221327609,
12.));
#222087=CARTESIAN_POINT('Ctrl Pts',(13.4496985395637,-20.7967827081228,
0.));
#222088=CARTESIAN_POINT('Ctrl Pts',(13.4496985395637,-20.7967827081228,
12.));
#222089=CARTESIAN_POINT('Ctrl Pts',(13.4533137106667,-20.821234532398,0.));
#222090=CARTESIAN_POINT('Ctrl Pts',(13.4533137106667,-20.821234532398,12.));
#222091=CARTESIAN_POINT('Ctrl Pts',(13.4568819818631,-20.8457771208083,
0.));
#222092=CARTESIAN_POINT('Ctrl Pts',(13.4568819818631,-20.8457771208083,
12.));
#222093=CARTESIAN_POINT('Ctrl Pts',(13.4604029960983,-20.8704099914641,
0.));
#222094=CARTESIAN_POINT('Ctrl Pts',(13.4604029960983,-20.8704099914641,
12.));
#222095=CARTESIAN_POINT('Ctrl Pts',(13.4638763999725,-20.8951326652158,
0.));
#222096=CARTESIAN_POINT('Ctrl Pts',(13.4638763999725,-20.8951326652158,
12.));
#222097=CARTESIAN_POINT('Ctrl Pts',(13.4673018437717,-20.9199446657583,
0.));
#222098=CARTESIAN_POINT('Ctrl Pts',(13.4673018437717,-20.9199446657583,
12.));
#222099=CARTESIAN_POINT('Ctrl Pts',(13.4706789815166,-20.9448455197557,
0.));
#222100=CARTESIAN_POINT('Ctrl Pts',(13.4706789815166,-20.9448455197557,
12.));
#222101=CARTESIAN_POINT('Ctrl Pts',(13.4740074710086,-20.9698347569477,
0.));
#222102=CARTESIAN_POINT('Ctrl Pts',(13.4740074710086,-20.9698347569477,
12.));
#222103=CARTESIAN_POINT('Ctrl Pts',(13.4772869738878,-20.9949119102592,
0.));
#222104=CARTESIAN_POINT('Ctrl Pts',(13.4772869738878,-20.9949119102592,
12.));
#222105=CARTESIAN_POINT('Ctrl Pts',(13.4805171556822,-21.0200765158884,
0.));
#222106=CARTESIAN_POINT('Ctrl Pts',(13.4805171556822,-21.0200765158884,
12.));
#222107=CARTESIAN_POINT('Ctrl Pts',(13.4836976858912,-21.0453281134245,
0.));
#222108=CARTESIAN_POINT('Ctrl Pts',(13.4836976858912,-21.0453281134245,
12.));
#222109=CARTESIAN_POINT('Ctrl Pts',(13.4868282377191,-21.0706662455199,
0.));
#222110=CARTESIAN_POINT('Ctrl Pts',(13.4868282377191,-21.0706662455199,
12.));
#222111=CARTESIAN_POINT('Ctrl Pts',(13.4899084877717,-21.0960904575046,
0.));
#222112=CARTESIAN_POINT('Ctrl Pts',(13.4899084877717,-21.0960904575046,
12.));
#222113=CARTESIAN_POINT('Ctrl Pts',(13.4929381157778,-21.1216002970207,
0.));
#222114=CARTESIAN_POINT('Ctrl Pts',(13.4929381157778,-21.1216002970207,
12.));
#222115=CARTESIAN_POINT('Ctrl Pts',(13.4959168042934,-21.1471953136209,
0.));
#222116=CARTESIAN_POINT('Ctrl Pts',(13.4959168042934,-21.1471953136209,
12.));
#222117=CARTESIAN_POINT('Ctrl Pts',(13.4988442384491,-21.1728750584175,
0.));
#222118=CARTESIAN_POINT('Ctrl Pts',(13.4988442384491,-21.1728750584175,
12.));
#222119=CARTESIAN_POINT('Ctrl Pts',(13.5017201056088,-21.1986390835828,
0.));
#222120=CARTESIAN_POINT('Ctrl Pts',(13.5017201056088,-21.1986390835828,
12.));
#222121=CARTESIAN_POINT('Ctrl Pts',(13.5045440957404,-21.2244869429332,
0.));
#222122=CARTESIAN_POINT('Ctrl Pts',(13.5045440957404,-21.2244869429332,
12.));
#222123=CARTESIAN_POINT('Ctrl Pts',(13.5073159019452,-21.250418192743,0.));
#222124=CARTESIAN_POINT('Ctrl Pts',(13.5073159019452,-21.250418192743,12.));
#222125=CARTESIAN_POINT('Ctrl Pts',(13.5100352209205,-21.2764323924442,
0.));
#222126=CARTESIAN_POINT('Ctrl Pts',(13.5100352209205,-21.2764323924442,
12.));
#222127=CARTESIAN_POINT('Ctrl Pts',(13.5127017534971,-21.3025291054235,
0.));
#222128=CARTESIAN_POINT('Ctrl Pts',(13.5127017534971,-21.3025291054235,
12.));
#222129=CARTESIAN_POINT('Ctrl Pts',(13.5153152050555,-21.3287078996341,
0.));
#222130=CARTESIAN_POINT('Ctrl Pts',(13.5153152050555,-21.3287078996341,
12.));
#222131=CARTESIAN_POINT('Ctrl Pts',(13.5178752862466,-21.3549683486222,
0.));
#222132=CARTESIAN_POINT('Ctrl Pts',(13.5178752862466,-21.3549683486222,
12.));
#222133=CARTESIAN_POINT('Ctrl Pts',(13.5203817122503,-21.3813100304973,
0.));
#222134=CARTESIAN_POINT('Ctrl Pts',(13.5203817122503,-21.3813100304973,
12.));
#222135=CARTESIAN_POINT('Ctrl Pts',(13.5228342013516,-21.4077325259324,
0.));
#222136=CARTESIAN_POINT('Ctrl Pts',(13.5228342013516,-21.4077325259324,
12.));
#222137=CARTESIAN_POINT('Ctrl Pts',(13.5252324737801,-21.4342354165259,
0.));
#222138=CARTESIAN_POINT('Ctrl Pts',(13.5252324737801,-21.4342354165259,
12.));
#222139=CARTESIAN_POINT('Ctrl Pts',(13.5275762503555,-21.4608182828697,
0.));
#222140=CARTESIAN_POINT('Ctrl Pts',(13.5275762503555,-21.4608182828697,
12.));
#222141=CARTESIAN_POINT('Ctrl Pts',(13.5298652514355,-21.4874807030468,
0.));
#222142=CARTESIAN_POINT('Ctrl Pts',(13.5298652514355,-21.4874807030468,
12.));
#222143=CARTESIAN_POINT('Ctrl Pts',(13.5320991952138,-21.5142222501666,
0.));
#222144=CARTESIAN_POINT('Ctrl Pts',(13.5320991952138,-21.5142222501666,
12.));
#222145=CARTESIAN_POINT('Ctrl Pts',(13.5342777983214,-21.5410424932503,
0.));
#222146=CARTESIAN_POINT('Ctrl Pts',(13.5342777983214,-21.5410424932503,
12.));
#222147=CARTESIAN_POINT('Ctrl Pts',(13.536400779028,-21.5679410019002,0.));
#222148=CARTESIAN_POINT('Ctrl Pts',(13.536400779028,-21.5679410019002,12.));
#222149=CARTESIAN_POINT('Ctrl Pts',(13.5384678597195,-21.5949173499013,
0.));
#222150=CARTESIAN_POINT('Ctrl Pts',(13.5384678597195,-21.5949173499013,
12.));
#222151=CARTESIAN_POINT('Ctrl Pts',(13.5404787697791,-21.6219711193946,
0.));
#222152=CARTESIAN_POINT('Ctrl Pts',(13.5404787697791,-21.6219711193946,
12.));
#222153=CARTESIAN_POINT('Ctrl Pts',(13.5424332480699,-21.6491019044648,
0.));
#222154=CARTESIAN_POINT('Ctrl Pts',(13.5424332480699,-21.6491019044648,
12.));
#222155=CARTESIAN_POINT('Ctrl Pts',(13.5443310461526,-21.6763093157699,
0.));
#222156=CARTESIAN_POINT('Ctrl Pts',(13.5443310461526,-21.6763093157699,
12.));
#222157=CARTESIAN_POINT('Ctrl Pts',(13.5461719295048,-21.7035929822955,
0.));
#222158=CARTESIAN_POINT('Ctrl Pts',(13.5461719295048,-21.7035929822955,
12.));
#222159=CARTESIAN_POINT('Ctrl Pts',(13.5479556704481,-21.7309525412281,
0.));
#222160=CARTESIAN_POINT('Ctrl Pts',(13.5479556704481,-21.7309525412281,
12.));
#222161=CARTESIAN_POINT('Ctrl Pts',(13.5496820422211,-21.7583876294554,
0.));
#222162=CARTESIAN_POINT('Ctrl Pts',(13.5496820422211,-21.7583876294554,
12.));
#222163=CARTESIAN_POINT('Ctrl Pts',(13.551350812725,-21.7858978745865,0.));
#222164=CARTESIAN_POINT('Ctrl Pts',(13.551350812725,-21.7858978745865,12.));
#222165=CARTESIAN_POINT('Ctrl Pts',(13.5529617381573,-21.8134828857967,
0.));
#222166=CARTESIAN_POINT('Ctrl Pts',(13.5529617381573,-21.8134828857967,
12.));
#222167=CARTESIAN_POINT('Ctrl Pts',(13.5545145573031,-21.8411422456075,
0.));
#222168=CARTESIAN_POINT('Ctrl Pts',(13.5545145573031,-21.8411422456075,
12.));
#222169=CARTESIAN_POINT('Ctrl Pts',(13.5560089839385,-21.8688754989365,
0.));
#222170=CARTESIAN_POINT('Ctrl Pts',(13.5560089839385,-21.8688754989365,
12.));
#222171=CARTESIAN_POINT('Ctrl Pts',(13.5574447178424,-21.8966821688824,
0.));
#222172=CARTESIAN_POINT('Ctrl Pts',(13.5574447178424,-21.8966821688824,
12.));
#222173=CARTESIAN_POINT('Ctrl Pts',(13.5588214586604,-21.9245617765769,
0.));
#222174=CARTESIAN_POINT('Ctrl Pts',(13.5588214586604,-21.9245617765769,
12.));
#222175=CARTESIAN_POINT('Ctrl Pts',(13.5601389185257,-21.9525138592813,
0.));
#222176=CARTESIAN_POINT('Ctrl Pts',(13.5601389185257,-21.9525138592813,
12.));
#222177=CARTESIAN_POINT('Ctrl Pts',(13.5613968357561,-21.9805379899168,
0.));
#222178=CARTESIAN_POINT('Ctrl Pts',(13.5613968357561,-21.9805379899168,
12.));
#222179=CARTESIAN_POINT('Ctrl Pts',(13.5625949868333,-22.0086337943449,
0.));
#222180=CARTESIAN_POINT('Ctrl Pts',(13.5625949868333,-22.0086337943449,
12.));
#222181=CARTESIAN_POINT('Ctrl Pts',(13.5637332022473,-22.0368009736295,
0.));
#222182=CARTESIAN_POINT('Ctrl Pts',(13.5637332022473,-22.0368009736295,
12.));
#222183=CARTESIAN_POINT('Ctrl Pts',(13.5648113689033,-22.065039308961,0.));
#222184=CARTESIAN_POINT('Ctrl Pts',(13.5648113689033,-22.065039308961,12.));
#222185=CARTESIAN_POINT('Ctrl Pts',(13.5658294169284,-22.0933486464593,
0.));
#222186=CARTESIAN_POINT('Ctrl Pts',(13.5658294169284,-22.0933486464593,
12.));
#222187=CARTESIAN_POINT('Ctrl Pts',(13.5667873105359,-22.1217288871975,
0.));
#222188=CARTESIAN_POINT('Ctrl Pts',(13.5667873105359,-22.1217288871975,
12.));
#222189=CARTESIAN_POINT('Ctrl Pts',(13.5675054919061,-22.1444897575194,
0.));
#222190=CARTESIAN_POINT('Ctrl Pts',(13.5675054919061,-22.1444897575194,
12.));
#222191=CARTESIAN_POINT('Ctrl Pts',(13.5680170531805,-22.1615922805008,
0.));
#222192=CARTESIAN_POINT('Ctrl Pts',(13.5680170531805,-22.1615922805008,
12.));
#222193=CARTESIAN_POINT('Ctrl Pts',(13.5683460612942,-22.1730081264608,
0.));
#222194=CARTESIAN_POINT('Ctrl Pts',(13.5683460612942,-22.1730081264608,
12.));
#222195=CARTESIAN_POINT('Ctrl Pts',(13.5685075571671,-22.178719590434,0.));
#222196=CARTESIAN_POINT('Ctrl Pts',(13.5685075571671,-22.178719590434,12.));
#222197=CARTESIAN_POINT('',(13.5685075571671,-22.178719590434,0.));
#222198=CARTESIAN_POINT('Ctrl Pts',(12.7689476255362,-18.5896416359912,
0.));
#222199=CARTESIAN_POINT('Ctrl Pts',(12.7689524524483,-18.5896460962964,
0.));
#222200=CARTESIAN_POINT('Ctrl Pts',(12.768986426692,-18.5896919669165,0.));
#222201=CARTESIAN_POINT('Ctrl Pts',(12.769110348199,-18.589871621843,0.));
#222202=CARTESIAN_POINT('Ctrl Pts',(12.7694215127918,-18.5903328777227,
0.));
#222203=CARTESIAN_POINT('Ctrl Pts',(12.7700520897173,-18.5912775137806,
0.));
#222204=CARTESIAN_POINT('Ctrl Pts',(12.7709195951156,-18.5925859134579,
0.));
#222205=CARTESIAN_POINT('Ctrl Pts',(12.7720142287172,-18.5942490615407,
0.));
#222206=CARTESIAN_POINT('Ctrl Pts',(12.7733231262108,-18.5962551167772,
0.));
#222207=CARTESIAN_POINT('Ctrl Pts',(12.7748328937638,-18.598591752595,0.));
#222208=CARTESIAN_POINT('Ctrl Pts',(12.7765325225081,-18.6012488486709,
0.));
#222209=CARTESIAN_POINT('Ctrl Pts',(12.7784139605066,-18.6042190183704,
0.));
#222210=CARTESIAN_POINT('Ctrl Pts',(12.7804705387658,-18.6074961535723,
0.));
#222211=CARTESIAN_POINT('Ctrl Pts',(12.7826959526924,-18.611074482622,0.));
#222212=CARTESIAN_POINT('Ctrl Pts',(12.7850831657901,-18.6149475565188,
0.));
#222213=CARTESIAN_POINT('Ctrl Pts',(12.7876249657834,-18.6191087624752,
0.));
#222214=CARTESIAN_POINT('Ctrl Pts',(12.7903142925234,-18.6235516265575,
0.));
#222215=CARTESIAN_POINT('Ctrl Pts',(12.7931447451555,-18.6282702819371,
0.));
#222216=CARTESIAN_POINT('Ctrl Pts',(12.796110622225,-18.6332595057006,0.));
#222217=CARTESIAN_POINT('Ctrl Pts',(12.7992066625264,-18.63851447924,0.));
#222218=CARTESIAN_POINT('Ctrl Pts',(12.8024278770152,-18.6440306327456,
0.));
#222219=CARTESIAN_POINT('Ctrl Pts',(12.805769331162,-18.6498034438987,0.));
#222220=CARTESIAN_POINT('Ctrl Pts',(12.8092261933858,-18.6558284825773,
0.));
#222221=CARTESIAN_POINT('Ctrl Pts',(12.8127937909631,-18.6621014624746,
0.));
#222222=CARTESIAN_POINT('Ctrl Pts',(12.8164676687362,-18.66861829528,0.));
#222223=CARTESIAN_POINT('Ctrl Pts',(12.8202436318474,-18.6753751301092,
0.));
#222224=CARTESIAN_POINT('Ctrl Pts',(12.8241176980017,-18.6823683094139,
0.));
#222225=CARTESIAN_POINT('Ctrl Pts',(12.8280860635231,-18.6895943376172,
0.));
#222226=CARTESIAN_POINT('Ctrl Pts',(12.8321450599789,-18.6970498410172,
0.));
#222227=CARTESIAN_POINT('Ctrl Pts',(12.8362911280361,-18.7047315436294,
0.));
#222228=CARTESIAN_POINT('Ctrl Pts',(12.8405208263431,-18.7126362754445,
0.));
#222229=CARTESIAN_POINT('Ctrl Pts',(12.8448308329494,-18.7207609737702,
0.));
#222230=CARTESIAN_POINT('Ctrl Pts',(12.8492179511591,-18.7291026886554,
0.));
#222231=CARTESIAN_POINT('Ctrl Pts',(12.8536791086316,-18.7376585820854,
0.));
#222232=CARTESIAN_POINT('Ctrl Pts',(12.8582113455646,-18.7464259171251,
0.));
#222233=CARTESIAN_POINT('Ctrl Pts',(12.8628118054171,-18.7554020493887,
0.));
#222234=CARTESIAN_POINT('Ctrl Pts',(12.8674777239653,-18.7645844169564,
0.));
#222235=CARTESIAN_POINT('Ctrl Pts',(12.872206421181,-18.7739705329022,0.));
#222236=CARTESIAN_POINT('Ctrl Pts',(12.8769952998095,-18.7835579840477,
0.));
#222237=CARTESIAN_POINT('Ctrl Pts',(12.8818418427475,-18.7933444285868,
0.));
#222238=CARTESIAN_POINT('Ctrl Pts',(12.8867436109546,-18.8033275941943,
0.));
#222239=CARTESIAN_POINT('Ctrl Pts',(12.8916982409935,-18.813505275782,0.));
#222240=CARTESIAN_POINT('Ctrl Pts',(12.8967034410754,-18.8238753319129,
0.));
#222241=CARTESIAN_POINT('Ctrl Pts',(12.9017569871738,-18.8344356812591,
0.));
#222242=CARTESIAN_POINT('Ctrl Pts',(12.9068567191854,-18.8451842990984,
0.));
#222243=CARTESIAN_POINT('Ctrl Pts',(12.9120005369063,-18.8561192136198,
0.));
#222244=CARTESIAN_POINT('Ctrl Pts',(12.9171863977045,-18.8672385038326,
0.));
#222245=CARTESIAN_POINT('Ctrl Pts',(12.9224123144981,-18.8785402977528,
0.));
#222246=CARTESIAN_POINT('Ctrl Pts',(12.9276763536373,-18.8900227704889,
0.));
#222247=CARTESIAN_POINT('Ctrl Pts',(12.9329766328184,-18.9016841423403,
0.));
#222248=CARTESIAN_POINT('Ctrl Pts',(12.9383113190374,-18.9135226769466,
0.));
#222249=CARTESIAN_POINT('Ctrl Pts',(12.9436786266105,-18.9255366795195,
0.));
#222250=CARTESIAN_POINT('Ctrl Pts',(12.9490768151821,-18.9377244950435,
0.));
#222251=CARTESIAN_POINT('Ctrl Pts',(12.9545041877377,-18.9500845064715,
0.));
#222252=CARTESIAN_POINT('Ctrl Pts',(12.9599590886319,-18.9626151329229,
0.));
#222253=CARTESIAN_POINT('Ctrl Pts',(12.9654399021869,-18.9753148284475,
0.));
#222254=CARTESIAN_POINT('Ctrl Pts',(12.9709450512747,-18.9881820807586,
0.));
#222255=CARTESIAN_POINT('Ctrl Pts',(12.9764729959205,-19.0012154099791,
0.));
#222256=CARTESIAN_POINT('Ctrl Pts',(12.9820222318715,-19.0144133673348,
0.));
#222257=CARTESIAN_POINT('Ctrl Pts',(12.9875912893003,-19.0277745339908,
0.));
#222258=CARTESIAN_POINT('Ctrl Pts',(12.9931787316514,-19.0412975200398,
0.));
#222259=CARTESIAN_POINT('Ctrl Pts',(12.9987831544502,-19.0549809634355,
0.));
#222260=CARTESIAN_POINT('Ctrl Pts',(13.0044031841381,-19.0688235289437,
0.));
#222261=CARTESIAN_POINT('Ctrl Pts',(13.0100374768785,-19.0828239070482,
0.));
#222262=CARTESIAN_POINT('Ctrl Pts',(13.0156847176093,-19.0969808131226,
0.));
#222263=CARTESIAN_POINT('Ctrl Pts',(13.0213436191326,-19.1112929866308,
0.));
#222264=CARTESIAN_POINT('Ctrl Pts',(13.0270129211976,-19.1257591903099,
0.));
#222265=CARTESIAN_POINT('Ctrl Pts',(13.0326913895841,-19.1403782093389,
0.));
#222266=CARTESIAN_POINT('Ctrl Pts',(13.0383778152072,-19.1551488505233,
0.));
#222267=CARTESIAN_POINT('Ctrl Pts',(13.0440710133775,-19.1700699416625,
0.));
#222268=CARTESIAN_POINT('Ctrl Pts',(13.0497698230442,-19.1851403308826,
0.));
#222269=CARTESIAN_POINT('Ctrl Pts',(13.0554731060537,-19.2003588859771,
0.));
#222270=CARTESIAN_POINT('Ctrl Pts',(13.0611797463912,-19.2157244937141,
0.));
#222271=CARTESIAN_POINT('Ctrl Pts',(13.0668886494791,-19.2312360592031,
0.));
#222272=CARTESIAN_POINT('Ctrl Pts',(13.0725987415856,-19.2468925053988,
0.));
#222273=CARTESIAN_POINT('Ctrl Pts',(13.0783089692117,-19.2626927725596,
0.));
#222274=CARTESIAN_POINT('Ctrl Pts',(13.0840182984949,-19.2786358177198,
0.));
#222275=CARTESIAN_POINT('Ctrl Pts',(13.0897257145969,-19.2947206141246,
0.));
#222276=CARTESIAN_POINT('Ctrl Pts',(13.095430221148,-19.3109461507358,0.));
#222277=CARTESIAN_POINT('Ctrl Pts',(13.1011308397591,-19.3273114318268,
0.));
#222278=CARTESIAN_POINT('Ctrl Pts',(13.1068266095186,-19.3438154765395,
0.));
#222279=CARTESIAN_POINT('Ctrl Pts',(13.1125165865021,-19.3604573184516,
0.));
#222280=CARTESIAN_POINT('Ctrl Pts',(13.118199843271,-19.3772360051093,0.));
#222281=CARTESIAN_POINT('Ctrl Pts',(13.1238754684177,-19.3941505976267,
0.));
#222282=CARTESIAN_POINT('Ctrl Pts',(13.1295425661635,-19.4112001703561,
0.));
#222283=CARTESIAN_POINT('Ctrl Pts',(13.1352002559439,-19.4283838105265,
0.));
#222284=CARTESIAN_POINT('Ctrl Pts',(13.140847672006,-19.4457006178875,0.));
#222285=CARTESIAN_POINT('Ctrl Pts',(13.1464839629966,-19.463149704325,0.));
#222286=CARTESIAN_POINT('Ctrl Pts',(13.1521082915846,-19.4807301935256,
0.));
#222287=CARTESIAN_POINT('Ctrl Pts',(13.1577198341238,-19.498441220707,0.));
#222288=CARTESIAN_POINT('Ctrl Pts',(13.1633177803097,-19.5162819323207,
0.));
#222289=CARTESIAN_POINT('Ctrl Pts',(13.1689013328432,-19.5342514857564,
0.));
#222290=CARTESIAN_POINT('Ctrl Pts',(13.1744697070918,-19.5523490490254,
0.));
#222291=CARTESIAN_POINT('Ctrl Pts',(13.1800221307682,-19.5705738004682,
0.));
#222292=CARTESIAN_POINT('Ctrl Pts',(13.1855578436479,-19.5889249285352,
0.));
#222293=CARTESIAN_POINT('Ctrl Pts',(13.1910760972818,-19.6074016315421,
0.));
#222294=CARTESIAN_POINT('Ctrl Pts',(13.196576154715,-19.6260031174244,0.));
#222295=CARTESIAN_POINT('Ctrl Pts',(13.202057290206,-19.6447286034764,0.));
#222296=CARTESIAN_POINT('Ctrl Pts',(13.2075187889522,-19.6635773160924,
0.));
#222297=CARTESIAN_POINT('Ctrl Pts',(13.2129599468478,-19.6825484905812,
0.));
#222298=CARTESIAN_POINT('Ctrl Pts',(13.2183800702431,-19.7016413709678,
0.));
#222299=CARTESIAN_POINT('Ctrl Pts',(13.2237784757065,-19.7208552097867,
0.));
#222300=CARTESIAN_POINT('Ctrl Pts',(13.2291544897902,-19.7401892678701,
0.));
#222301=CARTESIAN_POINT('Ctrl Pts',(13.2345074487968,-19.7596428141176,
0.));
#222302=CARTESIAN_POINT('Ctrl Pts',(13.239836698568,-19.7792151253297,0.));
#222303=CARTESIAN_POINT('Ctrl Pts',(13.2451415942809,-19.7989054860501,
0.));
#222304=CARTESIAN_POINT('Ctrl Pts',(13.2504215002458,-19.8187131883919,
0.));
#222305=CARTESIAN_POINT('Ctrl Pts',(13.2556757897085,-19.8386375318632,
0.));
#222306=CARTESIAN_POINT('Ctrl Pts',(13.2609038446525,-19.8586778231711,
0.));
#222307=CARTESIAN_POINT('Ctrl Pts',(13.2661050556128,-19.8788333760571,
0.));
#222308=CARTESIAN_POINT('Ctrl Pts',(13.2712788215015,-19.8991035111739,
0.));
#222309=CARTESIAN_POINT('Ctrl Pts',(13.2764245494354,-19.9194875559419,
0.));
#222310=CARTESIAN_POINT('Ctrl Pts',(13.2815416545662,-19.939984844402,0.));
#222311=CARTESIAN_POINT('Ctrl Pts',(13.2866295599152,-19.9605947170589,
0.));
#222312=CARTESIAN_POINT('Ctrl Pts',(13.2916876962098,-19.9813165207174,
0.));
#222313=CARTESIAN_POINT('Ctrl Pts',(13.296715501731,-20.0021496083742,0.));
#222314=CARTESIAN_POINT('Ctrl Pts',(13.3017124221639,-20.023093339104,0.));
#222315=CARTESIAN_POINT('Ctrl Pts',(13.3066779104515,-20.0441470779345,
0.));
#222316=CARTESIAN_POINT('Ctrl Pts',(13.3116114266514,-20.0653101957188,
0.));
#222317=CARTESIAN_POINT('Ctrl Pts',(13.3165124377962,-20.0865820689884,
0.));
#222318=CARTESIAN_POINT('Ctrl Pts',(13.3213804177588,-20.1079620798377,
0.));
#222319=CARTESIAN_POINT('Ctrl Pts',(13.3262148471228,-20.1294496158405,
0.));
#222320=CARTESIAN_POINT('Ctrl Pts',(13.3310152130565,-20.1510440699477,
0.));
#222321=CARTESIAN_POINT('Ctrl Pts',(13.3357810091903,-20.1727448403818,
0.));
#222322=CARTESIAN_POINT('Ctrl Pts',(13.3405117354969,-20.1945513305233,
0.));
#222323=CARTESIAN_POINT('Ctrl Pts',(13.3452068981762,-20.2164629487855,
0.));
#222324=CARTESIAN_POINT('Ctrl Pts',(13.3498660095381,-20.2384791085354,
0.));
#222325=CARTESIAN_POINT('Ctrl Pts',(13.3544885878886,-20.2605992280117,
0.));
#222326=CARTESIAN_POINT('Ctrl Pts',(13.3590741574194,-20.2828227302337,
0.));
#222327=CARTESIAN_POINT('Ctrl Pts',(13.3636222481016,-20.3051490429049,
0.));
#222328=CARTESIAN_POINT('Ctrl Pts',(13.3681323955828,-20.3275775983032,
0.));
#222329=CARTESIAN_POINT('Ctrl Pts',(13.3726041410869,-20.3501078331818,
0.));
#222330=CARTESIAN_POINT('Ctrl Pts',(13.377037031319,-20.3727391887187,0.));
#222331=CARTESIAN_POINT('Ctrl Pts',(13.3814306183721,-20.3954711104505,
0.));
#222332=CARTESIAN_POINT('Ctrl Pts',(13.3857844596387,-20.4183030482002,
0.));
#222333=CARTESIAN_POINT('Ctrl Pts',(13.3900981177254,-20.4412344560007,
0.));
#222334=CARTESIAN_POINT('Ctrl Pts',(13.3943711603739,-20.4642647920038,
0.));
#222335=CARTESIAN_POINT('Ctrl Pts',(13.3986031603716,-20.4873935184041,
0.));
#222336=CARTESIAN_POINT('Ctrl Pts',(13.4027936954529,-20.5106201013755,
0.));
#222337=CARTESIAN_POINT('Ctrl Pts',(13.4069423482076,-20.5339440109958,
0.));
#222338=CARTESIAN_POINT('Ctrl Pts',(13.4110487059912,-20.557364721164,0.));
#222339=CARTESIAN_POINT('Ctrl Pts',(13.415112360841,-20.5808817095155,0.));
#222340=CARTESIAN_POINT('Ctrl Pts',(13.4191329093931,-20.6044944573151,
0.));
#222341=CARTESIAN_POINT('Ctrl Pts',(13.4231099528178,-20.6282024494234,
0.));
#222342=CARTESIAN_POINT('Ctrl Pts',(13.427043096765,-20.6520051742868,0.));
#222343=CARTESIAN_POINT('Ctrl Pts',(13.4309319513119,-20.6759021239102,
0.));
#222344=CARTESIAN_POINT('Ctrl Pts',(13.4347761309154,-20.6998927938288,
0.));
#222345=CARTESIAN_POINT('Ctrl Pts',(13.4385752543663,-20.7239766830676,
0.));
#222346=CARTESIAN_POINT('Ctrl Pts',(13.4423289447561,-20.7481532941014,
0.));
#222347=CARTESIAN_POINT('Ctrl Pts',(13.4460368293689,-20.7724221327609,
0.));
#222348=CARTESIAN_POINT('Ctrl Pts',(13.4496985395637,-20.7967827081228,
0.));
#222349=CARTESIAN_POINT('Ctrl Pts',(13.4533137106667,-20.821234532398,0.));
#222350=CARTESIAN_POINT('Ctrl Pts',(13.4568819818631,-20.8457771208083,
0.));
#222351=CARTESIAN_POINT('Ctrl Pts',(13.4604029960983,-20.8704099914641,
0.));
#222352=CARTESIAN_POINT('Ctrl Pts',(13.4638763999725,-20.8951326652158,
0.));
#222353=CARTESIAN_POINT('Ctrl Pts',(13.4673018437717,-20.9199446657583,
0.));
#222354=CARTESIAN_POINT('Ctrl Pts',(13.4706789815166,-20.9448455197557,
0.));
#222355=CARTESIAN_POINT('Ctrl Pts',(13.4740074710086,-20.9698347569477,
0.));
#222356=CARTESIAN_POINT('Ctrl Pts',(13.4772869738878,-20.9949119102592,
0.));
#222357=CARTESIAN_POINT('Ctrl Pts',(13.4805171556822,-21.0200765158884,
0.));
#222358=CARTESIAN_POINT('Ctrl Pts',(13.4836976858912,-21.0453281134245,
0.));
#222359=CARTESIAN_POINT('Ctrl Pts',(13.4868282377191,-21.0706662455199,
0.));
#222360=CARTESIAN_POINT('Ctrl Pts',(13.4899084877717,-21.0960904575046,
0.));
#222361=CARTESIAN_POINT('Ctrl Pts',(13.4929381157778,-21.1216002970207,
0.));
#222362=CARTESIAN_POINT('Ctrl Pts',(13.4959168042934,-21.1471953136209,
0.));
#222363=CARTESIAN_POINT('Ctrl Pts',(13.4988442384491,-21.1728750584175,
0.));
#222364=CARTESIAN_POINT('Ctrl Pts',(13.5017201056088,-21.1986390835828,
0.));
#222365=CARTESIAN_POINT('Ctrl Pts',(13.5045440957404,-21.2244869429332,
0.));
#222366=CARTESIAN_POINT('Ctrl Pts',(13.5073159019452,-21.250418192743,0.));
#222367=CARTESIAN_POINT('Ctrl Pts',(13.5100352209205,-21.2764323924442,
0.));
#222368=CARTESIAN_POINT('Ctrl Pts',(13.5127017534971,-21.3025291054235,
0.));
#222369=CARTESIAN_POINT('Ctrl Pts',(13.5153152050555,-21.3287078996341,
0.));
#222370=CARTESIAN_POINT('Ctrl Pts',(13.5178752862466,-21.3549683486222,
0.));
#222371=CARTESIAN_POINT('Ctrl Pts',(13.5203817122503,-21.3813100304973,
0.));
#222372=CARTESIAN_POINT('Ctrl Pts',(13.5228342013516,-21.4077325259324,
0.));
#222373=CARTESIAN_POINT('Ctrl Pts',(13.5252324737801,-21.4342354165259,
0.));
#222374=CARTESIAN_POINT('Ctrl Pts',(13.5275762503555,-21.4608182828697,
0.));
#222375=CARTESIAN_POINT('Ctrl Pts',(13.5298652514355,-21.4874807030468,
0.));
#222376=CARTESIAN_POINT('Ctrl Pts',(13.5320991952138,-21.5142222501666,
0.));
#222377=CARTESIAN_POINT('Ctrl Pts',(13.5342777983214,-21.5410424932503,
0.));
#222378=CARTESIAN_POINT('Ctrl Pts',(13.536400779028,-21.5679410019002,0.));
#222379=CARTESIAN_POINT('Ctrl Pts',(13.5384678597195,-21.5949173499013,
0.));
#222380=CARTESIAN_POINT('Ctrl Pts',(13.5404787697791,-21.6219711193946,
0.));
#222381=CARTESIAN_POINT('Ctrl Pts',(13.5424332480699,-21.6491019044648,
0.));
#222382=CARTESIAN_POINT('Ctrl Pts',(13.5443310461526,-21.6763093157699,
0.));
#222383=CARTESIAN_POINT('Ctrl Pts',(13.5461719295048,-21.7035929822955,
0.));
#222384=CARTESIAN_POINT('Ctrl Pts',(13.5479556704481,-21.7309525412281,
0.));
#222385=CARTESIAN_POINT('Ctrl Pts',(13.5496820422211,-21.7583876294554,
0.));
#222386=CARTESIAN_POINT('Ctrl Pts',(13.551350812725,-21.7858978745865,0.));
#222387=CARTESIAN_POINT('Ctrl Pts',(13.5529617381573,-21.8134828857967,
0.));
#222388=CARTESIAN_POINT('Ctrl Pts',(13.5545145573031,-21.8411422456075,
0.));
#222389=CARTESIAN_POINT('Ctrl Pts',(13.5560089839385,-21.8688754989365,
0.));
#222390=CARTESIAN_POINT('Ctrl Pts',(13.5574447178424,-21.8966821688824,
0.));
#222391=CARTESIAN_POINT('Ctrl Pts',(13.5588214586604,-21.9245617765769,
0.));
#222392=CARTESIAN_POINT('Ctrl Pts',(13.5601389185257,-21.9525138592813,
0.));
#222393=CARTESIAN_POINT('Ctrl Pts',(13.5613968357561,-21.9805379899168,
0.));
#222394=CARTESIAN_POINT('Ctrl Pts',(13.5625949868333,-22.0086337943449,
0.));
#222395=CARTESIAN_POINT('Ctrl Pts',(13.5637332022473,-22.0368009736295,
0.));
#222396=CARTESIAN_POINT('Ctrl Pts',(13.5648113689033,-22.065039308961,0.));
#222397=CARTESIAN_POINT('Ctrl Pts',(13.5658294169284,-22.0933486464593,
0.));
#222398=CARTESIAN_POINT('Ctrl Pts',(13.5667873105359,-22.1217288871975,
0.));
#222399=CARTESIAN_POINT('Ctrl Pts',(13.5675054919061,-22.1444897575194,
0.));
#222400=CARTESIAN_POINT('Ctrl Pts',(13.5680170531805,-22.1615922805008,
0.));
#222401=CARTESIAN_POINT('Ctrl Pts',(13.5683460612942,-22.1730081264608,
0.));
#222402=CARTESIAN_POINT('Ctrl Pts',(13.5685075571671,-22.178719590434,0.));
#222403=CARTESIAN_POINT('',(13.5685075571671,-22.178719590434,12.));
#222404=CARTESIAN_POINT('Ctrl Pts',(13.5685075571671,-22.178719590434,12.));
#222405=CARTESIAN_POINT('Ctrl Pts',(13.5683460612942,-22.1730081264608,
12.));
#222406=CARTESIAN_POINT('Ctrl Pts',(13.5680170531805,-22.1615922805008,
12.));
#222407=CARTESIAN_POINT('Ctrl Pts',(13.5675054919061,-22.1444897575194,
12.));
#222408=CARTESIAN_POINT('Ctrl Pts',(13.5667873105359,-22.1217288871975,
12.));
#222409=CARTESIAN_POINT('Ctrl Pts',(13.5658294169284,-22.0933486464593,
12.));
#222410=CARTESIAN_POINT('Ctrl Pts',(13.5648113689033,-22.065039308961,12.));
#222411=CARTESIAN_POINT('Ctrl Pts',(13.5637332022473,-22.0368009736295,
12.));
#222412=CARTESIAN_POINT('Ctrl Pts',(13.5625949868333,-22.0086337943449,
12.));
#222413=CARTESIAN_POINT('Ctrl Pts',(13.5613968357561,-21.9805379899168,
12.));
#222414=CARTESIAN_POINT('Ctrl Pts',(13.5601389185257,-21.9525138592813,
12.));
#222415=CARTESIAN_POINT('Ctrl Pts',(13.5588214586604,-21.9245617765769,
12.));
#222416=CARTESIAN_POINT('Ctrl Pts',(13.5574447178424,-21.8966821688824,
12.));
#222417=CARTESIAN_POINT('Ctrl Pts',(13.5560089839385,-21.8688754989365,
12.));
#222418=CARTESIAN_POINT('Ctrl Pts',(13.5545145573031,-21.8411422456075,
12.));
#222419=CARTESIAN_POINT('Ctrl Pts',(13.5529617381573,-21.8134828857967,
12.));
#222420=CARTESIAN_POINT('Ctrl Pts',(13.551350812725,-21.7858978745865,12.));
#222421=CARTESIAN_POINT('Ctrl Pts',(13.5496820422211,-21.7583876294554,
12.));
#222422=CARTESIAN_POINT('Ctrl Pts',(13.5479556704481,-21.7309525412281,
12.));
#222423=CARTESIAN_POINT('Ctrl Pts',(13.5461719295048,-21.7035929822955,
12.));
#222424=CARTESIAN_POINT('Ctrl Pts',(13.5443310461526,-21.6763093157699,
12.));
#222425=CARTESIAN_POINT('Ctrl Pts',(13.5424332480699,-21.6491019044648,
12.));
#222426=CARTESIAN_POINT('Ctrl Pts',(13.5404787697791,-21.6219711193946,
12.));
#222427=CARTESIAN_POINT('Ctrl Pts',(13.5384678597195,-21.5949173499013,
12.));
#222428=CARTESIAN_POINT('Ctrl Pts',(13.536400779028,-21.5679410019002,12.));
#222429=CARTESIAN_POINT('Ctrl Pts',(13.5342777983214,-21.5410424932503,
12.));
#222430=CARTESIAN_POINT('Ctrl Pts',(13.5320991952138,-21.5142222501666,
12.));
#222431=CARTESIAN_POINT('Ctrl Pts',(13.5298652514355,-21.4874807030468,
12.));
#222432=CARTESIAN_POINT('Ctrl Pts',(13.5275762503555,-21.4608182828697,
12.));
#222433=CARTESIAN_POINT('Ctrl Pts',(13.5252324737801,-21.4342354165259,
12.));
#222434=CARTESIAN_POINT('Ctrl Pts',(13.5228342013516,-21.4077325259324,
12.));
#222435=CARTESIAN_POINT('Ctrl Pts',(13.5203817122503,-21.3813100304973,
12.));
#222436=CARTESIAN_POINT('Ctrl Pts',(13.5178752862466,-21.3549683486222,
12.));
#222437=CARTESIAN_POINT('Ctrl Pts',(13.5153152050555,-21.3287078996341,
12.));
#222438=CARTESIAN_POINT('Ctrl Pts',(13.5127017534971,-21.3025291054235,
12.));
#222439=CARTESIAN_POINT('Ctrl Pts',(13.5100352209205,-21.2764323924442,
12.));
#222440=CARTESIAN_POINT('Ctrl Pts',(13.5073159019452,-21.250418192743,12.));
#222441=CARTESIAN_POINT('Ctrl Pts',(13.5045440957404,-21.2244869429332,
12.));
#222442=CARTESIAN_POINT('Ctrl Pts',(13.5017201056088,-21.1986390835828,
12.));
#222443=CARTESIAN_POINT('Ctrl Pts',(13.4988442384491,-21.1728750584175,
12.));
#222444=CARTESIAN_POINT('Ctrl Pts',(13.4959168042934,-21.1471953136209,
12.));
#222445=CARTESIAN_POINT('Ctrl Pts',(13.4929381157778,-21.1216002970207,
12.));
#222446=CARTESIAN_POINT('Ctrl Pts',(13.4899084877717,-21.0960904575046,
12.));
#222447=CARTESIAN_POINT('Ctrl Pts',(13.4868282377191,-21.0706662455199,
12.));
#222448=CARTESIAN_POINT('Ctrl Pts',(13.4836976858912,-21.0453281134245,
12.));
#222449=CARTESIAN_POINT('Ctrl Pts',(13.4805171556822,-21.0200765158884,
12.));
#222450=CARTESIAN_POINT('Ctrl Pts',(13.4772869738878,-20.9949119102592,
12.));
#222451=CARTESIAN_POINT('Ctrl Pts',(13.4740074710086,-20.9698347569477,
12.));
#222452=CARTESIAN_POINT('Ctrl Pts',(13.4706789815166,-20.9448455197557,
12.));
#222453=CARTESIAN_POINT('Ctrl Pts',(13.4673018437717,-20.9199446657583,
12.));
#222454=CARTESIAN_POINT('Ctrl Pts',(13.4638763999725,-20.8951326652158,
12.));
#222455=CARTESIAN_POINT('Ctrl Pts',(13.4604029960983,-20.8704099914641,
12.));
#222456=CARTESIAN_POINT('Ctrl Pts',(13.4568819818631,-20.8457771208083,
12.));
#222457=CARTESIAN_POINT('Ctrl Pts',(13.4533137106667,-20.821234532398,12.));
#222458=CARTESIAN_POINT('Ctrl Pts',(13.4496985395637,-20.7967827081228,
12.));
#222459=CARTESIAN_POINT('Ctrl Pts',(13.4460368293689,-20.7724221327609,
12.));
#222460=CARTESIAN_POINT('Ctrl Pts',(13.4423289447561,-20.7481532941014,
12.));
#222461=CARTESIAN_POINT('Ctrl Pts',(13.4385752543663,-20.7239766830676,
12.));
#222462=CARTESIAN_POINT('Ctrl Pts',(13.4347761309154,-20.6998927938288,
12.));
#222463=CARTESIAN_POINT('Ctrl Pts',(13.4309319513119,-20.6759021239102,
12.));
#222464=CARTESIAN_POINT('Ctrl Pts',(13.427043096765,-20.6520051742868,12.));
#222465=CARTESIAN_POINT('Ctrl Pts',(13.4231099528178,-20.6282024494234,
12.));
#222466=CARTESIAN_POINT('Ctrl Pts',(13.4191329093931,-20.6044944573151,
12.));
#222467=CARTESIAN_POINT('Ctrl Pts',(13.415112360841,-20.5808817095155,12.));
#222468=CARTESIAN_POINT('Ctrl Pts',(13.4110487059912,-20.557364721164,12.));
#222469=CARTESIAN_POINT('Ctrl Pts',(13.4069423482076,-20.5339440109958,
12.));
#222470=CARTESIAN_POINT('Ctrl Pts',(13.4027936954529,-20.5106201013755,
12.));
#222471=CARTESIAN_POINT('Ctrl Pts',(13.3986031603716,-20.4873935184041,
12.));
#222472=CARTESIAN_POINT('Ctrl Pts',(13.3943711603739,-20.4642647920038,
12.));
#222473=CARTESIAN_POINT('Ctrl Pts',(13.3900981177254,-20.4412344560007,
12.));
#222474=CARTESIAN_POINT('Ctrl Pts',(13.3857844596387,-20.4183030482002,
12.));
#222475=CARTESIAN_POINT('Ctrl Pts',(13.3814306183721,-20.3954711104505,
12.));
#222476=CARTESIAN_POINT('Ctrl Pts',(13.377037031319,-20.3727391887187,12.));
#222477=CARTESIAN_POINT('Ctrl Pts',(13.3726041410869,-20.3501078331818,
12.));
#222478=CARTESIAN_POINT('Ctrl Pts',(13.3681323955828,-20.3275775983032,
12.));
#222479=CARTESIAN_POINT('Ctrl Pts',(13.3636222481016,-20.3051490429049,
12.));
#222480=CARTESIAN_POINT('Ctrl Pts',(13.3590741574194,-20.2828227302337,
12.));
#222481=CARTESIAN_POINT('Ctrl Pts',(13.3544885878886,-20.2605992280117,
12.));
#222482=CARTESIAN_POINT('Ctrl Pts',(13.3498660095381,-20.2384791085354,
12.));
#222483=CARTESIAN_POINT('Ctrl Pts',(13.3452068981762,-20.2164629487855,
12.));
#222484=CARTESIAN_POINT('Ctrl Pts',(13.3405117354969,-20.1945513305233,
12.));
#222485=CARTESIAN_POINT('Ctrl Pts',(13.3357810091903,-20.1727448403818,
12.));
#222486=CARTESIAN_POINT('Ctrl Pts',(13.3310152130565,-20.1510440699477,
12.));
#222487=CARTESIAN_POINT('Ctrl Pts',(13.3262148471228,-20.1294496158405,
12.));
#222488=CARTESIAN_POINT('Ctrl Pts',(13.3213804177588,-20.1079620798377,
12.));
#222489=CARTESIAN_POINT('Ctrl Pts',(13.3165124377962,-20.0865820689884,
12.));
#222490=CARTESIAN_POINT('Ctrl Pts',(13.3116114266514,-20.0653101957188,
12.));
#222491=CARTESIAN_POINT('Ctrl Pts',(13.3066779104515,-20.0441470779345,
12.));
#222492=CARTESIAN_POINT('Ctrl Pts',(13.3017124221639,-20.023093339104,12.));
#222493=CARTESIAN_POINT('Ctrl Pts',(13.296715501731,-20.0021496083742,12.));
#222494=CARTESIAN_POINT('Ctrl Pts',(13.2916876962098,-19.9813165207174,
12.));
#222495=CARTESIAN_POINT('Ctrl Pts',(13.2866295599152,-19.9605947170589,
12.));
#222496=CARTESIAN_POINT('Ctrl Pts',(13.2815416545662,-19.939984844402,12.));
#222497=CARTESIAN_POINT('Ctrl Pts',(13.2764245494354,-19.9194875559419,
12.));
#222498=CARTESIAN_POINT('Ctrl Pts',(13.2712788215015,-19.8991035111739,
12.));
#222499=CARTESIAN_POINT('Ctrl Pts',(13.2661050556128,-19.8788333760571,
12.));
#222500=CARTESIAN_POINT('Ctrl Pts',(13.2609038446525,-19.8586778231711,
12.));
#222501=CARTESIAN_POINT('Ctrl Pts',(13.2556757897085,-19.8386375318632,
12.));
#222502=CARTESIAN_POINT('Ctrl Pts',(13.2504215002458,-19.8187131883919,
12.));
#222503=CARTESIAN_POINT('Ctrl Pts',(13.2451415942809,-19.7989054860501,
12.));
#222504=CARTESIAN_POINT('Ctrl Pts',(13.239836698568,-19.7792151253297,12.));
#222505=CARTESIAN_POINT('Ctrl Pts',(13.2345074487968,-19.7596428141176,
12.));
#222506=CARTESIAN_POINT('Ctrl Pts',(13.2291544897902,-19.7401892678701,
12.));
#222507=CARTESIAN_POINT('Ctrl Pts',(13.2237784757065,-19.7208552097867,
12.));
#222508=CARTESIAN_POINT('Ctrl Pts',(13.2183800702431,-19.7016413709678,
12.));
#222509=CARTESIAN_POINT('Ctrl Pts',(13.2129599468478,-19.6825484905812,
12.));
#222510=CARTESIAN_POINT('Ctrl Pts',(13.2075187889522,-19.6635773160924,
12.));
#222511=CARTESIAN_POINT('Ctrl Pts',(13.202057290206,-19.6447286034764,12.));
#222512=CARTESIAN_POINT('Ctrl Pts',(13.196576154715,-19.6260031174244,12.));
#222513=CARTESIAN_POINT('Ctrl Pts',(13.1910760972818,-19.6074016315421,
12.));
#222514=CARTESIAN_POINT('Ctrl Pts',(13.1855578436479,-19.5889249285352,
12.));
#222515=CARTESIAN_POINT('Ctrl Pts',(13.1800221307682,-19.5705738004682,
12.));
#222516=CARTESIAN_POINT('Ctrl Pts',(13.1744697070918,-19.5523490490254,
12.));
#222517=CARTESIAN_POINT('Ctrl Pts',(13.1689013328432,-19.5342514857564,
12.));
#222518=CARTESIAN_POINT('Ctrl Pts',(13.1633177803097,-19.5162819323207,
12.));
#222519=CARTESIAN_POINT('Ctrl Pts',(13.1577198341238,-19.498441220707,12.));
#222520=CARTESIAN_POINT('Ctrl Pts',(13.1521082915846,-19.4807301935256,
12.));
#222521=CARTESIAN_POINT('Ctrl Pts',(13.1464839629966,-19.463149704325,12.));
#222522=CARTESIAN_POINT('Ctrl Pts',(13.140847672006,-19.4457006178875,12.));
#222523=CARTESIAN_POINT('Ctrl Pts',(13.1352002559439,-19.4283838105265,
12.));
#222524=CARTESIAN_POINT('Ctrl Pts',(13.1295425661635,-19.4112001703561,
12.));
#222525=CARTESIAN_POINT('Ctrl Pts',(13.1238754684177,-19.3941505976267,
12.));
#222526=CARTESIAN_POINT('Ctrl Pts',(13.118199843271,-19.3772360051093,12.));
#222527=CARTESIAN_POINT('Ctrl Pts',(13.1125165865021,-19.3604573184516,
12.));
#222528=CARTESIAN_POINT('Ctrl Pts',(13.1068266095186,-19.3438154765395,
12.));
#222529=CARTESIAN_POINT('Ctrl Pts',(13.1011308397591,-19.3273114318268,
12.));
#222530=CARTESIAN_POINT('Ctrl Pts',(13.095430221148,-19.3109461507358,12.));
#222531=CARTESIAN_POINT('Ctrl Pts',(13.0897257145969,-19.2947206141246,
12.));
#222532=CARTESIAN_POINT('Ctrl Pts',(13.0840182984949,-19.2786358177198,
12.));
#222533=CARTESIAN_POINT('Ctrl Pts',(13.0783089692117,-19.2626927725596,
12.));
#222534=CARTESIAN_POINT('Ctrl Pts',(13.0725987415856,-19.2468925053988,
12.));
#222535=CARTESIAN_POINT('Ctrl Pts',(13.0668886494791,-19.2312360592031,
12.));
#222536=CARTESIAN_POINT('Ctrl Pts',(13.0611797463912,-19.2157244937141,
12.));
#222537=CARTESIAN_POINT('Ctrl Pts',(13.0554731060537,-19.2003588859771,
12.));
#222538=CARTESIAN_POINT('Ctrl Pts',(13.0497698230442,-19.1851403308826,
12.));
#222539=CARTESIAN_POINT('Ctrl Pts',(13.0440710133775,-19.1700699416625,
12.));
#222540=CARTESIAN_POINT('Ctrl Pts',(13.0383778152072,-19.1551488505233,
12.));
#222541=CARTESIAN_POINT('Ctrl Pts',(13.0326913895841,-19.1403782093389,
12.));
#222542=CARTESIAN_POINT('Ctrl Pts',(13.0270129211976,-19.1257591903099,
12.));
#222543=CARTESIAN_POINT('Ctrl Pts',(13.0213436191326,-19.1112929866308,
12.));
#222544=CARTESIAN_POINT('Ctrl Pts',(13.0156847176093,-19.0969808131226,
12.));
#222545=CARTESIAN_POINT('Ctrl Pts',(13.0100374768785,-19.0828239070482,
12.));
#222546=CARTESIAN_POINT('Ctrl Pts',(13.0044031841381,-19.0688235289437,
12.));
#222547=CARTESIAN_POINT('Ctrl Pts',(12.9987831544502,-19.0549809634355,
12.));
#222548=CARTESIAN_POINT('Ctrl Pts',(12.9931787316514,-19.0412975200398,
12.));
#222549=CARTESIAN_POINT('Ctrl Pts',(12.9875912893003,-19.0277745339908,
12.));
#222550=CARTESIAN_POINT('Ctrl Pts',(12.9820222318715,-19.0144133673348,
12.));
#222551=CARTESIAN_POINT('Ctrl Pts',(12.9764729959205,-19.0012154099791,
12.));
#222552=CARTESIAN_POINT('Ctrl Pts',(12.9709450512747,-18.9881820807586,
12.));
#222553=CARTESIAN_POINT('Ctrl Pts',(12.9654399021869,-18.9753148284475,
12.));
#222554=CARTESIAN_POINT('Ctrl Pts',(12.9599590886319,-18.9626151329229,
12.));
#222555=CARTESIAN_POINT('Ctrl Pts',(12.9545041877377,-18.9500845064715,
12.));
#222556=CARTESIAN_POINT('Ctrl Pts',(12.9490768151821,-18.9377244950435,
12.));
#222557=CARTESIAN_POINT('Ctrl Pts',(12.9436786266105,-18.9255366795195,
12.));
#222558=CARTESIAN_POINT('Ctrl Pts',(12.9383113190374,-18.9135226769466,
12.));
#222559=CARTESIAN_POINT('Ctrl Pts',(12.9329766328184,-18.9016841423403,
12.));
#222560=CARTESIAN_POINT('Ctrl Pts',(12.9276763536373,-18.8900227704889,
12.));
#222561=CARTESIAN_POINT('Ctrl Pts',(12.9224123144981,-18.8785402977528,
12.));
#222562=CARTESIAN_POINT('Ctrl Pts',(12.9171863977045,-18.8672385038326,
12.));
#222563=CARTESIAN_POINT('Ctrl Pts',(12.9120005369063,-18.8561192136198,
12.));
#222564=CARTESIAN_POINT('Ctrl Pts',(12.9068567191854,-18.8451842990984,
12.));
#222565=CARTESIAN_POINT('Ctrl Pts',(12.9017569871738,-18.8344356812591,
12.));
#222566=CARTESIAN_POINT('Ctrl Pts',(12.8967034410754,-18.8238753319129,
12.));
#222567=CARTESIAN_POINT('Ctrl Pts',(12.8916982409935,-18.813505275782,12.));
#222568=CARTESIAN_POINT('Ctrl Pts',(12.8867436109546,-18.8033275941943,
12.));
#222569=CARTESIAN_POINT('Ctrl Pts',(12.8818418427475,-18.7933444285868,
12.));
#222570=CARTESIAN_POINT('Ctrl Pts',(12.8769952998095,-18.7835579840477,
12.));
#222571=CARTESIAN_POINT('Ctrl Pts',(12.872206421181,-18.7739705329022,12.));
#222572=CARTESIAN_POINT('Ctrl Pts',(12.8674777239653,-18.7645844169564,
12.));
#222573=CARTESIAN_POINT('Ctrl Pts',(12.8628118054171,-18.7554020493887,
12.));
#222574=CARTESIAN_POINT('Ctrl Pts',(12.8582113455646,-18.7464259171251,
12.));
#222575=CARTESIAN_POINT('Ctrl Pts',(12.8536791086316,-18.7376585820854,
12.));
#222576=CARTESIAN_POINT('Ctrl Pts',(12.8492179511591,-18.7291026886554,
12.));
#222577=CARTESIAN_POINT('Ctrl Pts',(12.8448308329494,-18.7207609737702,
12.));
#222578=CARTESIAN_POINT('Ctrl Pts',(12.8405208263431,-18.7126362754445,
12.));
#222579=CARTESIAN_POINT('Ctrl Pts',(12.8362911280361,-18.7047315436294,
12.));
#222580=CARTESIAN_POINT('Ctrl Pts',(12.8321450599789,-18.6970498410172,
12.));
#222581=CARTESIAN_POINT('Ctrl Pts',(12.8280860635231,-18.6895943376172,
12.));
#222582=CARTESIAN_POINT('Ctrl Pts',(12.8241176980017,-18.6823683094139,
12.));
#222583=CARTESIAN_POINT('Ctrl Pts',(12.8202436318474,-18.6753751301092,
12.));
#222584=CARTESIAN_POINT('Ctrl Pts',(12.8164676687362,-18.66861829528,12.));
#222585=CARTESIAN_POINT('Ctrl Pts',(12.8127937909631,-18.6621014624746,
12.));
#222586=CARTESIAN_POINT('Ctrl Pts',(12.8092261933858,-18.6558284825773,
12.));
#222587=CARTESIAN_POINT('Ctrl Pts',(12.805769331162,-18.6498034438987,12.));
#222588=CARTESIAN_POINT('Ctrl Pts',(12.8024278770152,-18.6440306327456,
12.));
#222589=CARTESIAN_POINT('Ctrl Pts',(12.7992066625264,-18.63851447924,12.));
#222590=CARTESIAN_POINT('Ctrl Pts',(12.796110622225,-18.6332595057006,12.));
#222591=CARTESIAN_POINT('Ctrl Pts',(12.7931447451555,-18.6282702819371,
12.));
#222592=CARTESIAN_POINT('Ctrl Pts',(12.7903142925234,-18.6235516265575,
12.));
#222593=CARTESIAN_POINT('Ctrl Pts',(12.7876249657834,-18.6191087624752,
12.));
#222594=CARTESIAN_POINT('Ctrl Pts',(12.7850831657901,-18.6149475565188,
12.));
#222595=CARTESIAN_POINT('Ctrl Pts',(12.7826959526924,-18.611074482622,12.));
#222596=CARTESIAN_POINT('Ctrl Pts',(12.7804705387658,-18.6074961535723,
12.));
#222597=CARTESIAN_POINT('Ctrl Pts',(12.7784139605066,-18.6042190183704,
12.));
#222598=CARTESIAN_POINT('Ctrl Pts',(12.7765325225081,-18.6012488486709,
12.));
#222599=CARTESIAN_POINT('Ctrl Pts',(12.7748328937638,-18.598591752595,12.));
#222600=CARTESIAN_POINT('Ctrl Pts',(12.7733231262108,-18.5962551167772,
12.));
#222601=CARTESIAN_POINT('Ctrl Pts',(12.7720142287172,-18.5942490615407,
12.));
#222602=CARTESIAN_POINT('Ctrl Pts',(12.7709195951156,-18.5925859134579,
12.));
#222603=CARTESIAN_POINT('Ctrl Pts',(12.7700520897173,-18.5912775137806,
12.));
#222604=CARTESIAN_POINT('Ctrl Pts',(12.7694215127918,-18.5903328777227,
12.));
#222605=CARTESIAN_POINT('Ctrl Pts',(12.769110348199,-18.589871621843,12.));
#222606=CARTESIAN_POINT('Ctrl Pts',(12.768986426692,-18.5896919669165,12.));
#222607=CARTESIAN_POINT('Ctrl Pts',(12.7689524524483,-18.5896460962964,
12.));
#222608=CARTESIAN_POINT('Ctrl Pts',(12.7689476255362,-18.5896416359912,
12.));
#222609=CARTESIAN_POINT('',(13.5685075571671,-22.178719590434,0.));
#222610=CARTESIAN_POINT('Origin',(7.17139709155223,-20.2687213152502,0.));
#222611=CARTESIAN_POINT('',(7.52250298901263,-21.2610617890679,12.));
#222612=CARTESIAN_POINT('',(3.58569854577611,-10.1343606576251,12.));
#222613=CARTESIAN_POINT('',(7.52250298901263,-21.2610617890679,0.));
#222614=CARTESIAN_POINT('',(7.52250298901263,-21.2610617890679,0.));
#222615=CARTESIAN_POINT('',(3.58569854577611,-10.1343606576251,0.));
#222616=CARTESIAN_POINT('Ctrl Pts',(12.4230808101438,-22.8400320311649,
0.));
#222617=CARTESIAN_POINT('Ctrl Pts',(12.4230808101438,-22.8400320311649,
12.));
#222618=CARTESIAN_POINT('Ctrl Pts',(12.418215285186,-22.8370364396459,0.));
#222619=CARTESIAN_POINT('Ctrl Pts',(12.418215285186,-22.8370364396459,12.));
#222620=CARTESIAN_POINT('Ctrl Pts',(12.4084933766346,-22.8310435872748,
0.));
#222621=CARTESIAN_POINT('Ctrl Pts',(12.4084933766346,-22.8310435872748,
12.));
#222622=CARTESIAN_POINT('Ctrl Pts',(12.3939379378998,-22.8220493007173,
0.));
#222623=CARTESIAN_POINT('Ctrl Pts',(12.3939379378998,-22.8220493007173,
12.));
#222624=CARTESIAN_POINT('Ctrl Pts',(12.374585536673,-22.81004690224,0.));
#222625=CARTESIAN_POINT('Ctrl Pts',(12.374585536673,-22.81004690224,12.));
#222626=CARTESIAN_POINT('Ctrl Pts',(12.3504864740319,-22.795027221673,0.));
#222627=CARTESIAN_POINT('Ctrl Pts',(12.3504864740319,-22.795027221673,12.));
#222628=CARTESIAN_POINT('Ctrl Pts',(12.3264788926075,-22.7799908974768,
0.));
#222629=CARTESIAN_POINT('Ctrl Pts',(12.3264788926075,-22.7799908974768,
12.));
#222630=CARTESIAN_POINT('Ctrl Pts',(12.3025628601792,-22.764938010105,0.));
#222631=CARTESIAN_POINT('Ctrl Pts',(12.3025628601792,-22.764938010105,12.));
#222632=CARTESIAN_POINT('Ctrl Pts',(12.2787384750742,-22.7498686970069,
0.));
#222633=CARTESIAN_POINT('Ctrl Pts',(12.2787384750742,-22.7498686970069,
12.));
#222634=CARTESIAN_POINT('Ctrl Pts',(12.2550058702395,-22.7347831655287,
0.));
#222635=CARTESIAN_POINT('Ctrl Pts',(12.2550058702395,-22.7347831655287,
12.));
#222636=CARTESIAN_POINT('Ctrl Pts',(12.2313652198061,-22.7196817119374,
0.));
#222637=CARTESIAN_POINT('Ctrl Pts',(12.2313652198061,-22.7196817119374,
12.));
#222638=CARTESIAN_POINT('Ctrl Pts',(12.2078167360284,-22.7045647168747,
0.));
#222639=CARTESIAN_POINT('Ctrl Pts',(12.2078167360284,-22.7045647168747,
12.));
#222640=CARTESIAN_POINT('Ctrl Pts',(12.1843606579261,-22.6894326205037,
0.));
#222641=CARTESIAN_POINT('Ctrl Pts',(12.1843606579261,-22.6894326205037,
12.));
#222642=CARTESIAN_POINT('Ctrl Pts',(12.1609972423099,-22.6742859034944,
0.));
#222643=CARTESIAN_POINT('Ctrl Pts',(12.1609972423099,-22.6742859034944,
12.));
#222644=CARTESIAN_POINT('Ctrl Pts',(12.1377267537145,-22.6591250653965,
0.));
#222645=CARTESIAN_POINT('Ctrl Pts',(12.1377267537145,-22.6591250653965,
12.));
#222646=CARTESIAN_POINT('Ctrl Pts',(12.1145494550383,-22.6439506046605,
0.));
#222647=CARTESIAN_POINT('Ctrl Pts',(12.1145494550383,-22.6439506046605,
12.));
#222648=CARTESIAN_POINT('Ctrl Pts',(12.0914655972823,-22.6287629967056,
0.));
#222649=CARTESIAN_POINT('Ctrl Pts',(12.0914655972823,-22.6287629967056,
12.));
#222650=CARTESIAN_POINT('Ctrl Pts',(12.0684754113862,-22.6135626764898,
0.));
#222651=CARTESIAN_POINT('Ctrl Pts',(12.0684754113862,-22.6135626764898,
12.));
#222652=CARTESIAN_POINT('Ctrl Pts',(12.0455791139128,-22.5983500505644,
0.));
#222653=CARTESIAN_POINT('Ctrl Pts',(12.0455791139128,-22.5983500505644,
12.));
#222654=CARTESIAN_POINT('Ctrl Pts',(12.0227769113127,-22.5831255061282,
0.));
#222655=CARTESIAN_POINT('Ctrl Pts',(12.0227769113127,-22.5831255061282,
12.));
#222656=CARTESIAN_POINT('Ctrl Pts',(12.0000690046694,-22.5678894211181,
0.));
#222657=CARTESIAN_POINT('Ctrl Pts',(12.0000690046694,-22.5678894211181,
12.));
#222658=CARTESIAN_POINT('Ctrl Pts',(11.9774555943496,-22.5526421741158,
0.));
#222659=CARTESIAN_POINT('Ctrl Pts',(11.9774555943496,-22.5526421741158,
12.));
#222660=CARTESIAN_POINT('Ctrl Pts',(11.9549368843997,-22.5373841537307,
0.));
#222661=CARTESIAN_POINT('Ctrl Pts',(11.9549368843997,-22.5373841537307,
12.));
#222662=CARTESIAN_POINT('Ctrl Pts',(11.9325130877803,-22.5221157697883,
0.));
#222663=CARTESIAN_POINT('Ctrl Pts',(11.9325130877803,-22.5221157697883,
12.));
#222664=CARTESIAN_POINT('Ctrl Pts',(11.9101844254557,-22.5068374513973,
0.));
#222665=CARTESIAN_POINT('Ctrl Pts',(11.9101844254557,-22.5068374513973,
12.));
#222666=CARTESIAN_POINT('Ctrl Pts',(11.8879511239942,-22.4915496418485,
0.));
#222667=CARTESIAN_POINT('Ctrl Pts',(11.8879511239942,-22.4915496418485,
12.));
#222668=CARTESIAN_POINT('Ctrl Pts',(11.8658134137019,-22.4762527946702,
0.));
#222669=CARTESIAN_POINT('Ctrl Pts',(11.8658134137019,-22.4762527946702,
12.));
#222670=CARTESIAN_POINT('Ctrl Pts',(11.8437715264487,-22.4609473690472,
0.));
#222671=CARTESIAN_POINT('Ctrl Pts',(11.8437715264487,-22.4609473690472,
12.));
#222672=CARTESIAN_POINT('Ctrl Pts',(11.8218256937889,-22.4456338258735,
0.));
#222673=CARTESIAN_POINT('Ctrl Pts',(11.8218256937889,-22.4456338258735,
12.));
#222674=CARTESIAN_POINT('Ctrl Pts',(11.7999761445173,-22.430312622646,0.));
#222675=CARTESIAN_POINT('Ctrl Pts',(11.7999761445173,-22.430312622646,12.));
#222676=CARTESIAN_POINT('Ctrl Pts',(11.7782231042039,-22.4149842125008,
0.));
#222677=CARTESIAN_POINT('Ctrl Pts',(11.7782231042039,-22.4149842125008,
12.));
#222678=CARTESIAN_POINT('Ctrl Pts',(11.7565667964764,-22.3996490469191,
0.));
#222679=CARTESIAN_POINT('Ctrl Pts',(11.7565667964764,-22.3996490469191,
12.));
#222680=CARTESIAN_POINT('Ctrl Pts',(11.7350074437961,-22.3843075773899,
0.));
#222681=CARTESIAN_POINT('Ctrl Pts',(11.7350074437961,-22.3843075773899,
12.));
#222682=CARTESIAN_POINT('Ctrl Pts',(11.7135452684532,-22.3689602575491,
0.));
#222683=CARTESIAN_POINT('Ctrl Pts',(11.7135452684532,-22.3689602575491,
12.));
#222684=CARTESIAN_POINT('Ctrl Pts',(11.6921804934056,-22.3536075450029,
0.));
#222685=CARTESIAN_POINT('Ctrl Pts',(11.6921804934056,-22.3536075450029,
12.));
#222686=CARTESIAN_POINT('Ctrl Pts',(11.6709133432985,-22.3382499035619,
0.));
#222687=CARTESIAN_POINT('Ctrl Pts',(11.6709133432985,-22.3382499035619,
12.));
#222688=CARTESIAN_POINT('Ctrl Pts',(11.6497440449857,-22.3228878043976,
0.));
#222689=CARTESIAN_POINT('Ctrl Pts',(11.6497440449857,-22.3228878043976,
12.));
#222690=CARTESIAN_POINT('Ctrl Pts',(11.6286728270009,-22.3075217249049,
0.));
#222691=CARTESIAN_POINT('Ctrl Pts',(11.6286728270009,-22.3075217249049,
12.));
#222692=CARTESIAN_POINT('Ctrl Pts',(11.6076999192357,-22.2921521480356,
0.));
#222693=CARTESIAN_POINT('Ctrl Pts',(11.6076999192357,-22.2921521480356,
12.));
#222694=CARTESIAN_POINT('Ctrl Pts',(11.5868255525188,-22.2767795614348,
0.));
#222695=CARTESIAN_POINT('Ctrl Pts',(11.5868255525188,-22.2767795614348,
12.));
#222696=CARTESIAN_POINT('Ctrl Pts',(11.5660499582403,-22.2614044566898,
0.));
#222697=CARTESIAN_POINT('Ctrl Pts',(11.5660499582403,-22.2614044566898,
12.));
#222698=CARTESIAN_POINT('Ctrl Pts',(11.5453733679121,-22.2460273284654,
0.));
#222699=CARTESIAN_POINT('Ctrl Pts',(11.5453733679121,-22.2460273284654,
12.));
#222700=CARTESIAN_POINT('Ctrl Pts',(11.5247960128477,-22.2306486738901,
0.));
#222701=CARTESIAN_POINT('Ctrl Pts',(11.5247960128477,-22.2306486738901,
12.));
#222702=CARTESIAN_POINT('Ctrl Pts',(11.5043181244242,-22.2152689931022,
0.));
#222703=CARTESIAN_POINT('Ctrl Pts',(11.5043181244242,-22.2152689931022,
12.));
#222704=CARTESIAN_POINT('Ctrl Pts',(11.483939934259,-22.1998887896436,0.));
#222705=CARTESIAN_POINT('Ctrl Pts',(11.483939934259,-22.1998887896436,12.));
#222706=CARTESIAN_POINT('Ctrl Pts',(11.463661674411,-22.184508570917,0.));
#222707=CARTESIAN_POINT('Ctrl Pts',(11.463661674411,-22.184508570917,12.));
#222708=CARTESIAN_POINT('Ctrl Pts',(11.443483577557,-22.1691288486096,0.));
#222709=CARTESIAN_POINT('Ctrl Pts',(11.443483577557,-22.1691288486096,12.));
#222710=CARTESIAN_POINT('Ctrl Pts',(11.4234058771742,-22.1537501391487,
0.));
#222711=CARTESIAN_POINT('Ctrl Pts',(11.4234058771742,-22.1537501391487,
12.));
#222712=CARTESIAN_POINT('Ctrl Pts',(11.4034288076908,-22.1383729640964,
0.));
#222713=CARTESIAN_POINT('Ctrl Pts',(11.4034288076908,-22.1383729640964,
12.));
#222714=CARTESIAN_POINT('Ctrl Pts',(11.3835526044256,-22.1229978500186,
0.));
#222715=CARTESIAN_POINT('Ctrl Pts',(11.3835526044256,-22.1229978500186,
12.));
#222716=CARTESIAN_POINT('Ctrl Pts',(11.3637775035367,-22.1076253283979,
0.));
#222717=CARTESIAN_POINT('Ctrl Pts',(11.3637775035367,-22.1076253283979,
12.));
#222718=CARTESIAN_POINT('Ctrl Pts',(11.3441037419553,-22.0922559355294,
0.));
#222719=CARTESIAN_POINT('Ctrl Pts',(11.3441037419553,-22.0922559355294,
12.));
#222720=CARTESIAN_POINT('Ctrl Pts',(11.3245315573168,-22.0768902124267,
0.));
#222721=CARTESIAN_POINT('Ctrl Pts',(11.3245315573168,-22.0768902124267,
12.));
#222722=CARTESIAN_POINT('Ctrl Pts',(11.3050611878771,-22.0615287047179,
0.));
#222723=CARTESIAN_POINT('Ctrl Pts',(11.3050611878771,-22.0615287047179,
12.));
#222724=CARTESIAN_POINT('Ctrl Pts',(11.2856928724374,-22.046171962566,0.));
#222725=CARTESIAN_POINT('Ctrl Pts',(11.2856928724374,-22.046171962566,12.));
#222726=CARTESIAN_POINT('Ctrl Pts',(11.2664268504206,-22.030820540835,0.));
#222727=CARTESIAN_POINT('Ctrl Pts',(11.2664268504206,-22.030820540835,12.));
#222728=CARTESIAN_POINT('Ctrl Pts',(11.2472633619275,-22.0154749992363,
0.));
#222729=CARTESIAN_POINT('Ctrl Pts',(11.2472633619275,-22.0154749992363,
12.));
#222730=CARTESIAN_POINT('Ctrl Pts',(11.2282026477896,-22.0001359024839,
0.));
#222731=CARTESIAN_POINT('Ctrl Pts',(11.2282026477896,-22.0001359024839,
12.));
#222732=CARTESIAN_POINT('Ctrl Pts',(11.2092449496125,-21.9848038204439,
0.));
#222733=CARTESIAN_POINT('Ctrl Pts',(11.2092449496125,-21.9848038204439,
12.));
#222734=CARTESIAN_POINT('Ctrl Pts',(11.190390509811,-21.9694793282914,0.));
#222735=CARTESIAN_POINT('Ctrl Pts',(11.190390509811,-21.9694793282914,12.));
#222736=CARTESIAN_POINT('Ctrl Pts',(11.1716395716376,-21.9541630066506,
0.));
#222737=CARTESIAN_POINT('Ctrl Pts',(11.1716395716376,-21.9541630066506,
12.));
#222738=CARTESIAN_POINT('Ctrl Pts',(11.1529923792003,-21.9388554416439,
0.));
#222739=CARTESIAN_POINT('Ctrl Pts',(11.1529923792003,-21.9388554416439,
12.));
#222740=CARTESIAN_POINT('Ctrl Pts',(11.1344491774741,-21.923557224952,0.));
#222741=CARTESIAN_POINT('Ctrl Pts',(11.1344491774741,-21.923557224952,12.));
#222742=CARTESIAN_POINT('Ctrl Pts',(11.1160102123024,-21.9082689538688,
0.));
#222743=CARTESIAN_POINT('Ctrl Pts',(11.1160102123024,-21.9082689538688,
12.));
#222744=CARTESIAN_POINT('Ctrl Pts',(11.0976757303944,-21.8929912313608,
0.));
#222745=CARTESIAN_POINT('Ctrl Pts',(11.0976757303944,-21.8929912313608,
12.));
#222746=CARTESIAN_POINT('Ctrl Pts',(11.0794459793057,-21.877724666119,0.));
#222747=CARTESIAN_POINT('Ctrl Pts',(11.0794459793057,-21.877724666119,12.));
#222748=CARTESIAN_POINT('Ctrl Pts',(11.0613212074363,-21.8624698726318,
0.));
#222749=CARTESIAN_POINT('Ctrl Pts',(11.0613212074363,-21.8624698726318,
12.));
#222750=CARTESIAN_POINT('Ctrl Pts',(11.0433016640807,-21.8472274713103,
0.));
#222751=CARTESIAN_POINT('Ctrl Pts',(11.0433016640807,-21.8472274713103,
12.));
#222752=CARTESIAN_POINT('Ctrl Pts',(11.0253875994598,-21.8319980886033,
0.));
#222753=CARTESIAN_POINT('Ctrl Pts',(11.0253875994598,-21.8319980886033,
12.));
#222754=CARTESIAN_POINT('Ctrl Pts',(11.0075792647477,-21.8167823571168,
0.));
#222755=CARTESIAN_POINT('Ctrl Pts',(11.0075792647477,-21.8167823571168,
12.));
#222756=CARTESIAN_POINT('Ctrl Pts',(10.9898769120912,-21.8015809157301,
0.));
#222757=CARTESIAN_POINT('Ctrl Pts',(10.9898769120912,-21.8015809157301,
12.));
#222758=CARTESIAN_POINT('Ctrl Pts',(10.9722807946155,-21.7863944097141,
0.));
#222759=CARTESIAN_POINT('Ctrl Pts',(10.9722807946155,-21.7863944097141,
12.));
#222760=CARTESIAN_POINT('Ctrl Pts',(10.9547911664455,-21.7712234908464,
0.));
#222761=CARTESIAN_POINT('Ctrl Pts',(10.9547911664455,-21.7712234908464,
12.));
#222762=CARTESIAN_POINT('Ctrl Pts',(10.9374082827444,-21.7560688175247,
0.));
#222763=CARTESIAN_POINT('Ctrl Pts',(10.9374082827444,-21.7560688175247,
12.));
#222764=CARTESIAN_POINT('Ctrl Pts',(10.9201323997384,-21.7409310548797,
0.));
#222765=CARTESIAN_POINT('Ctrl Pts',(10.9201323997384,-21.7409310548797,
12.));
#222766=CARTESIAN_POINT('Ctrl Pts',(10.902963774734,-21.7258108748873,0.));
#222767=CARTESIAN_POINT('Ctrl Pts',(10.902963774734,-21.7258108748873,12.));
#222768=CARTESIAN_POINT('Ctrl Pts',(10.8859026661293,-21.7107089564825,
0.));
#222769=CARTESIAN_POINT('Ctrl Pts',(10.8859026661293,-21.7107089564825,
12.));
#222770=CARTESIAN_POINT('Ctrl Pts',(10.8689493334095,-21.6956259856672,
0.));
#222771=CARTESIAN_POINT('Ctrl Pts',(10.8689493334095,-21.6956259856672,
12.));
#222772=CARTESIAN_POINT('Ctrl Pts',(10.8521040371835,-21.6805626556467,
0.));
#222773=CARTESIAN_POINT('Ctrl Pts',(10.8521040371835,-21.6805626556467,
12.));
#222774=CARTESIAN_POINT('Ctrl Pts',(10.8353670392272,-21.6655196669732,
0.));
#222775=CARTESIAN_POINT('Ctrl Pts',(10.8353670392272,-21.6655196669732,
12.));
#222776=CARTESIAN_POINT('Ctrl Pts',(10.8187386025136,-21.6504977276866,
0.));
#222777=CARTESIAN_POINT('Ctrl Pts',(10.8187386025136,-21.6504977276866,
12.));
#222778=CARTESIAN_POINT('Ctrl Pts',(10.8022189912369,-21.6354975534557,
0.));
#222779=CARTESIAN_POINT('Ctrl Pts',(10.8022189912369,-21.6354975534557,
12.));
#222780=CARTESIAN_POINT('Ctrl Pts',(10.7858084708261,-21.6205198677173,
0.));
#222781=CARTESIAN_POINT('Ctrl Pts',(10.7858084708261,-21.6205198677173,
12.));
#222782=CARTESIAN_POINT('Ctrl Pts',(10.7695073079552,-21.6055654018176,
0.));
#222783=CARTESIAN_POINT('Ctrl Pts',(10.7695073079552,-21.6055654018176,
12.));
#222784=CARTESIAN_POINT('Ctrl Pts',(10.7533157705941,-21.5906348951743,
0.));
#222785=CARTESIAN_POINT('Ctrl Pts',(10.7533157705941,-21.5906348951743,
12.));
#222786=CARTESIAN_POINT('Ctrl Pts',(10.7372341280467,-21.5757290954371,
0.));
#222787=CARTESIAN_POINT('Ctrl Pts',(10.7372341280467,-21.5757290954371,
12.));
#222788=CARTESIAN_POINT('Ctrl Pts',(10.7212626509816,-21.5608487586468,
0.));
#222789=CARTESIAN_POINT('Ctrl Pts',(10.7212626509816,-21.5608487586468,
12.));
#222790=CARTESIAN_POINT('Ctrl Pts',(10.7054016114571,-21.5459946493955,
0.));
#222791=CARTESIAN_POINT('Ctrl Pts',(10.7054016114571,-21.5459946493955,
12.));
#222792=CARTESIAN_POINT('Ctrl Pts',(10.689651282929,-21.5311675409807,0.));
#222793=CARTESIAN_POINT('Ctrl Pts',(10.689651282929,-21.5311675409807,12.));
#222794=CARTESIAN_POINT('Ctrl Pts',(10.6740119402834,-21.51636821558,0.));
#222795=CARTESIAN_POINT('Ctrl Pts',(10.6740119402834,-21.51636821558,12.));
#222796=CARTESIAN_POINT('Ctrl Pts',(10.6584838598939,-21.5015974644449,
0.));
#222797=CARTESIAN_POINT('Ctrl Pts',(10.6584838598939,-21.5015974644449,
12.));
#222798=CARTESIAN_POINT('Ctrl Pts',(10.6430673196607,-21.4868560880889,
0.));
#222799=CARTESIAN_POINT('Ctrl Pts',(10.6430673196607,-21.4868560880889,
12.));
#222800=CARTESIAN_POINT('Ctrl Pts',(10.6277625990456,-21.4721448964766,
0.));
#222801=CARTESIAN_POINT('Ctrl Pts',(10.6277625990456,-21.4721448964766,
12.));
#222802=CARTESIAN_POINT('Ctrl Pts',(10.6125699790961,-21.4574647092097,
0.));
#222803=CARTESIAN_POINT('Ctrl Pts',(10.6125699790961,-21.4574647092097,
12.));
#222804=CARTESIAN_POINT('Ctrl Pts',(10.5974897424622,-21.4428163557144,
0.));
#222805=CARTESIAN_POINT('Ctrl Pts',(10.5974897424622,-21.4428163557144,
12.));
#222806=CARTESIAN_POINT('Ctrl Pts',(10.5825221734573,-21.4282006754631,
0.));
#222807=CARTESIAN_POINT('Ctrl Pts',(10.5825221734573,-21.4282006754631,
12.));
#222808=CARTESIAN_POINT('Ctrl Pts',(10.5676675581108,-21.4136185181979,
0.));
#222809=CARTESIAN_POINT('Ctrl Pts',(10.5676675581108,-21.4136185181979,
12.));
#222810=CARTESIAN_POINT('Ctrl Pts',(10.5529261842108,-21.3990707441497,
0.));
#222811=CARTESIAN_POINT('Ctrl Pts',(10.5529261842108,-21.3990707441497,
12.));
#222812=CARTESIAN_POINT('Ctrl Pts',(10.5382983413421,-21.3845582242602,
0.));
#222813=CARTESIAN_POINT('Ctrl Pts',(10.5382983413421,-21.3845582242602,
12.));
#222814=CARTESIAN_POINT('Ctrl Pts',(10.5237843209057,-21.3700818403936,
0.));
#222815=CARTESIAN_POINT('Ctrl Pts',(10.5237843209057,-21.3700818403936,
12.));
#222816=CARTESIAN_POINT('Ctrl Pts',(10.5093844161685,-21.3556424855814,
0.));
#222817=CARTESIAN_POINT('Ctrl Pts',(10.5093844161685,-21.3556424855814,
12.));
#222818=CARTESIAN_POINT('Ctrl Pts',(10.4950989223336,-21.3412410642904,
0.));
#222819=CARTESIAN_POINT('Ctrl Pts',(10.4950989223336,-21.3412410642904,
12.));
#222820=CARTESIAN_POINT('Ctrl Pts',(10.4809281365931,-21.3268784926819,
0.));
#222821=CARTESIAN_POINT('Ctrl Pts',(10.4809281365931,-21.3268784926819,
12.));
#222822=CARTESIAN_POINT('Ctrl Pts',(10.4668723581768,-21.3125556988731,
0.));
#222823=CARTESIAN_POINT('Ctrl Pts',(10.4668723581768,-21.3125556988731,
12.));
#222824=CARTESIAN_POINT('Ctrl Pts',(10.4529318883874,-21.2982736231931,
0.));
#222825=CARTESIAN_POINT('Ctrl Pts',(10.4529318883874,-21.2982736231931,
12.));
#222826=CARTESIAN_POINT('Ctrl Pts',(10.4391070306391,-21.2840332184483,
0.));
#222827=CARTESIAN_POINT('Ctrl Pts',(10.4391070306391,-21.2840332184483,
12.));
#222828=CARTESIAN_POINT('Ctrl Pts',(10.42539809054,-21.2698354502403,0.));
#222829=CARTESIAN_POINT('Ctrl Pts',(10.42539809054,-21.2698354502403,12.));
#222830=CARTESIAN_POINT('Ctrl Pts',(10.4118053759588,-21.255681297275,0.));
#222831=CARTESIAN_POINT('Ctrl Pts',(10.4118053759588,-21.255681297275,12.));
#222832=CARTESIAN_POINT('Ctrl Pts',(10.3983291970846,-21.2415717516714,
0.));
#222833=CARTESIAN_POINT('Ctrl Pts',(10.3983291970846,-21.2415717516714,
12.));
#222834=CARTESIAN_POINT('Ctrl Pts',(10.3849698664786,-21.22750781927,0.));
#222835=CARTESIAN_POINT('Ctrl Pts',(10.3849698664786,-21.22750781927,12.));
#222836=CARTESIAN_POINT('Ctrl Pts',(10.371727699113,-21.2134905199345,0.));
#222837=CARTESIAN_POINT('Ctrl Pts',(10.371727699113,-21.2134905199345,12.));
#222838=CARTESIAN_POINT('Ctrl Pts',(10.3586030124587,-21.199520887919,0.));
#222839=CARTESIAN_POINT('Ctrl Pts',(10.3586030124587,-21.199520887919,12.));
#222840=CARTESIAN_POINT('Ctrl Pts',(10.34559612657,-21.1855999722416,0.));
#222841=CARTESIAN_POINT('Ctrl Pts',(10.34559612657,-21.1855999722416,12.));
#222842=CARTESIAN_POINT('Ctrl Pts',(10.3327073641572,-21.1717288370509,
0.));
#222843=CARTESIAN_POINT('Ctrl Pts',(10.3327073641572,-21.1717288370509,
12.));
#222844=CARTESIAN_POINT('Ctrl Pts',(10.3199370506544,-21.1579085619965,
0.));
#222845=CARTESIAN_POINT('Ctrl Pts',(10.3199370506544,-21.1579085619965,
12.));
#222846=CARTESIAN_POINT('Ctrl Pts',(10.3072855142687,-21.1441402425843,
0.));
#222847=CARTESIAN_POINT('Ctrl Pts',(10.3072855142687,-21.1441402425843,
12.));
#222848=CARTESIAN_POINT('Ctrl Pts',(10.2947530860721,-21.1304249906002,
0.));
#222849=CARTESIAN_POINT('Ctrl Pts',(10.2947530860721,-21.1304249906002,
12.));
#222850=CARTESIAN_POINT('Ctrl Pts',(10.2823401001072,-21.1167639345631,
0.));
#222851=CARTESIAN_POINT('Ctrl Pts',(10.2823401001072,-21.1167639345631,
12.));
#222852=CARTESIAN_POINT('Ctrl Pts',(10.2700468934744,-21.1031582201627,
0.));
#222853=CARTESIAN_POINT('Ctrl Pts',(10.2700468934744,-21.1031582201627,
12.));
#222854=CARTESIAN_POINT('Ctrl Pts',(10.2578738064181,-21.0896090107063,
0.));
#222855=CARTESIAN_POINT('Ctrl Pts',(10.2578738064181,-21.0896090107063,
12.));
#222856=CARTESIAN_POINT('Ctrl Pts',(10.2458211823912,-21.0761174875445,
0.));
#222857=CARTESIAN_POINT('Ctrl Pts',(10.2458211823912,-21.0761174875445,
12.));
#222858=CARTESIAN_POINT('Ctrl Pts',(10.2338893681567,-21.0626848505663,
0.));
#222859=CARTESIAN_POINT('Ctrl Pts',(10.2338893681567,-21.0626848505663,
12.));
#222860=CARTESIAN_POINT('Ctrl Pts',(10.2220787139154,-21.0493123187483,
0.));
#222861=CARTESIAN_POINT('Ctrl Pts',(10.2220787139154,-21.0493123187483,
12.));
#222862=CARTESIAN_POINT('Ctrl Pts',(10.2103895734123,-21.0360011306815,
0.));
#222863=CARTESIAN_POINT('Ctrl Pts',(10.2103895734123,-21.0360011306815,
12.));
#222864=CARTESIAN_POINT('Ctrl Pts',(10.1988223040425,-21.0227525451107,
0.));
#222865=CARTESIAN_POINT('Ctrl Pts',(10.1988223040425,-21.0227525451107,
12.));
#222866=CARTESIAN_POINT('Ctrl Pts',(10.187377266936,-21.0095678414486,0.));
#222867=CARTESIAN_POINT('Ctrl Pts',(10.187377266936,-21.0095678414486,12.));
#222868=CARTESIAN_POINT('Ctrl Pts',(10.1760548270767,-20.9964483203686,
0.));
#222869=CARTESIAN_POINT('Ctrl Pts',(10.1760548270767,-20.9964483203686,
12.));
#222870=CARTESIAN_POINT('Ctrl Pts',(10.1648553534568,-20.9833953044736,
0.));
#222871=CARTESIAN_POINT('Ctrl Pts',(10.1648553534568,-20.9833953044736,
12.));
#222872=CARTESIAN_POINT('Ctrl Pts',(10.1537792192065,-20.9704101389369,
0.));
#222873=CARTESIAN_POINT('Ctrl Pts',(10.1537792192065,-20.9704101389369,
12.));
#222874=CARTESIAN_POINT('Ctrl Pts',(10.1428268017256,-20.9574941921591,
0.));
#222875=CARTESIAN_POINT('Ctrl Pts',(10.1428268017256,-20.9574941921591,
12.));
#222876=CARTESIAN_POINT('Ctrl Pts',(10.1319984827908,-20.9446488563933,
0.));
#222877=CARTESIAN_POINT('Ctrl Pts',(10.1319984827908,-20.9446488563933,
12.));
#222878=CARTESIAN_POINT('Ctrl Pts',(10.1212946487057,-20.9318755484734,
0.));
#222879=CARTESIAN_POINT('Ctrl Pts',(10.1212946487057,-20.9318755484734,
12.));
#222880=CARTESIAN_POINT('Ctrl Pts',(10.1107156904836,-20.919175710627,0.));
#222881=CARTESIAN_POINT('Ctrl Pts',(10.1107156904836,-20.919175710627,12.));
#222882=CARTESIAN_POINT('Ctrl Pts',(10.1002620040076,-20.9065508112557,
0.));
#222883=CARTESIAN_POINT('Ctrl Pts',(10.1002620040076,-20.9065508112557,
12.));
#222884=CARTESIAN_POINT('Ctrl Pts',(10.0899339901915,-20.894002345737,0.));
#222885=CARTESIAN_POINT('Ctrl Pts',(10.0899339901915,-20.894002345737,12.));
#222886=CARTESIAN_POINT('Ctrl Pts',(10.0797320551154,-20.881531837184,0.));
#222887=CARTESIAN_POINT('Ctrl Pts',(10.0797320551154,-20.881531837184,12.));
#222888=CARTESIAN_POINT('Ctrl Pts',(10.0696566102218,-20.86914083737,0.));
#222889=CARTESIAN_POINT('Ctrl Pts',(10.0696566102218,-20.86914083737,12.));
#222890=CARTESIAN_POINT('Ctrl Pts',(10.0597080725375,-20.8568309277316,
0.));
#222891=CARTESIAN_POINT('Ctrl Pts',(10.0597080725375,-20.8568309277316,
12.));
#222892=CARTESIAN_POINT('Ctrl Pts',(10.0498868648733,-20.8446037203402,
0.));
#222893=CARTESIAN_POINT('Ctrl Pts',(10.0498868648733,-20.8446037203402,
12.));
#222894=CARTESIAN_POINT('Ctrl Pts',(10.0401934160234,-20.8324608588909,
0.));
#222895=CARTESIAN_POINT('Ctrl Pts',(10.0401934160234,-20.8324608588909,
12.));
#222896=CARTESIAN_POINT('Ctrl Pts',(10.0306281609435,-20.8204040196602,
0.));
#222897=CARTESIAN_POINT('Ctrl Pts',(10.0306281609435,-20.8204040196602,
12.));
#222898=CARTESIAN_POINT('Ctrl Pts',(10.0211915410095,-20.8084349126888,
0.));
#222899=CARTESIAN_POINT('Ctrl Pts',(10.0211915410095,-20.8084349126888,
12.));
#222900=CARTESIAN_POINT('Ctrl Pts',(10.0118840042786,-20.7965552829908,
0.));
#222901=CARTESIAN_POINT('Ctrl Pts',(10.0118840042786,-20.7965552829908,
12.));
#222902=CARTESIAN_POINT('Ctrl Pts',(10.0027060057389,-20.7847669117568,
0.));
#222903=CARTESIAN_POINT('Ctrl Pts',(10.0027060057389,-20.7847669117568,
12.));
#222904=CARTESIAN_POINT('Ctrl Pts',(9.9936580075464,-20.7730716175417,0.));
#222905=CARTESIAN_POINT('Ctrl Pts',(9.9936580075464,-20.7730716175417,12.));
#222906=CARTESIAN_POINT('Ctrl Pts',(9.98474047926852,-20.761471257499,0.));
#222907=CARTESIAN_POINT('Ctrl Pts',(9.98474047926852,-20.761471257499,12.));
#222908=CARTESIAN_POINT('Ctrl Pts',(9.97595389823469,-20.7499677289627,
0.));
#222909=CARTESIAN_POINT('Ctrl Pts',(9.97595389823469,-20.7499677289627,
12.));
#222910=CARTESIAN_POINT('Ctrl Pts',(9.96729874986201,-20.7385629709795,
0.));
#222911=CARTESIAN_POINT('Ctrl Pts',(9.96729874986201,-20.7385629709795,
12.));
#222912=CARTESIAN_POINT('Ctrl Pts',(9.95877552798397,-20.7272589658751,
0.));
#222913=CARTESIAN_POINT('Ctrl Pts',(9.95877552798397,-20.7272589658751,
12.));
#222914=CARTESIAN_POINT('Ctrl Pts',(9.95038473514948,-20.7160577407579,
0.));
#222915=CARTESIAN_POINT('Ctrl Pts',(9.95038473514948,-20.7160577407579,
12.));
#222916=CARTESIAN_POINT('Ctrl Pts',(9.94212688298236,-20.7049613692234,
0.));
#222917=CARTESIAN_POINT('Ctrl Pts',(9.94212688298236,-20.7049613692234,
12.));
#222918=CARTESIAN_POINT('Ctrl Pts',(9.93400249259729,-20.6939719732484,
0.));
#222919=CARTESIAN_POINT('Ctrl Pts',(9.93400249259729,-20.6939719732484,
12.));
#222920=CARTESIAN_POINT('Ctrl Pts',(9.92601209498748,-20.6830917250255,
0.));
#222921=CARTESIAN_POINT('Ctrl Pts',(9.92601209498748,-20.6830917250255,
12.));
#222922=CARTESIAN_POINT('Ctrl Pts',(9.91815623141288,-20.6723228488263,
0.));
#222923=CARTESIAN_POINT('Ctrl Pts',(9.91815623141288,-20.6723228488263,
12.));
#222924=CARTESIAN_POINT('Ctrl Pts',(9.91043545377007,-20.6616676228315,
0.));
#222925=CARTESIAN_POINT('Ctrl Pts',(9.91043545377007,-20.6616676228315,
12.));
#222926=CARTESIAN_POINT('Ctrl Pts',(9.90285032516692,-20.6511283817414,
0.));
#222927=CARTESIAN_POINT('Ctrl Pts',(9.90285032516692,-20.6511283817414,
12.));
#222928=CARTESIAN_POINT('Ctrl Pts',(9.89540142049119,-20.6407075193976,
0.));
#222929=CARTESIAN_POINT('Ctrl Pts',(9.89540142049119,-20.6407075193976,
12.));
#222930=CARTESIAN_POINT('Ctrl Pts',(9.88808932697305,-20.6304074914087,
0.));
#222931=CARTESIAN_POINT('Ctrl Pts',(9.88808932697305,-20.6304074914087,
12.));
#222932=CARTESIAN_POINT('Ctrl Pts',(9.88091464472675,-20.6202308177475,
0.));
#222933=CARTESIAN_POINT('Ctrl Pts',(9.88091464472675,-20.6202308177475,
12.));
#222934=CARTESIAN_POINT('Ctrl Pts',(9.87387798732955,-20.6101800854494,
0.));
#222935=CARTESIAN_POINT('Ctrl Pts',(9.87387798732955,-20.6101800854494,
12.));
#222936=CARTESIAN_POINT('Ctrl Pts',(9.86697998242622,-20.6002579513699,
0.));
#222937=CARTESIAN_POINT('Ctrl Pts',(9.86697998242622,-20.6002579513699,
12.));
#222938=CARTESIAN_POINT('Ctrl Pts',(9.86022127232747,-20.5904671449754,
0.));
#222939=CARTESIAN_POINT('Ctrl Pts',(9.86022127232747,-20.5904671449754,
12.));
#222940=CARTESIAN_POINT('Ctrl Pts',(9.8536025145698,-20.5808104710015,0.));
#222941=CARTESIAN_POINT('Ctrl Pts',(9.8536025145698,-20.5808104710015,12.));
#222942=CARTESIAN_POINT('Ctrl Pts',(9.84712438256277,-20.5712908125139,
0.));
#222943=CARTESIAN_POINT('Ctrl Pts',(9.84712438256277,-20.5712908125139,
12.));
#222944=CARTESIAN_POINT('Ctrl Pts',(9.84078756677565,-20.5619111362402,
0.));
#222945=CARTESIAN_POINT('Ctrl Pts',(9.84078756677565,-20.5619111362402,
12.));
#222946=CARTESIAN_POINT('Ctrl Pts',(9.83459277585315,-20.552674497646,0.));
#222947=CARTESIAN_POINT('Ctrl Pts',(9.83459277585315,-20.552674497646,12.));
#222948=CARTESIAN_POINT('Ctrl Pts',(9.82854073773876,-20.5435840460721,
0.));
#222949=CARTESIAN_POINT('Ctrl Pts',(9.82854073773876,-20.5435840460721,
12.));
#222950=CARTESIAN_POINT('Ctrl Pts',(9.82263220080362,-20.5346430299517,
0.));
#222951=CARTESIAN_POINT('Ctrl Pts',(9.82263220080362,-20.5346430299517,
12.));
#222952=CARTESIAN_POINT('Ctrl Pts',(9.81686793455942,-20.5258548000629,
0.));
#222953=CARTESIAN_POINT('Ctrl Pts',(9.81686793455942,-20.5258548000629,
12.));
#222954=CARTESIAN_POINT('Ctrl Pts',(9.81124873025281,-20.517222812284,0.));
#222955=CARTESIAN_POINT('Ctrl Pts',(9.81124873025281,-20.517222812284,12.));
#222956=CARTESIAN_POINT('Ctrl Pts',(9.80577540161087,-20.5087506310505,
0.));
#222957=CARTESIAN_POINT('Ctrl Pts',(9.80577540161087,-20.5087506310505,
12.));
#222958=CARTESIAN_POINT('Ctrl Pts',(9.80044878520948,-20.5004419312107,
0.));
#222959=CARTESIAN_POINT('Ctrl Pts',(9.80044878520948,-20.5004419312107,
12.));
#222960=CARTESIAN_POINT('Ctrl Pts',(9.7952697428833,-20.4923005087943,0.));
#222961=CARTESIAN_POINT('Ctrl Pts',(9.7952697428833,-20.4923005087943,12.));
#222962=CARTESIAN_POINT('Ctrl Pts',(9.79023916498655,-20.4843302955329,
0.));
#222963=CARTESIAN_POINT('Ctrl Pts',(9.79023916498655,-20.4843302955329,
12.));
#222964=CARTESIAN_POINT('Ctrl Pts',(9.78535797314166,-20.4765353711586,
0.));
#222965=CARTESIAN_POINT('Ctrl Pts',(9.78535797314166,-20.4765353711586,
12.));
#222966=CARTESIAN_POINT('Ctrl Pts',(9.7806271237332,-20.4689199790669,0.));
#222967=CARTESIAN_POINT('Ctrl Pts',(9.7806271237332,-20.4689199790669,12.));
#222968=CARTESIAN_POINT('Ctrl Pts',(9.77604760815528,-20.4614885274975,
0.));
#222969=CARTESIAN_POINT('Ctrl Pts',(9.77604760815528,-20.4614885274975,
12.));
#222970=CARTESIAN_POINT('Ctrl Pts',(9.77162045104069,-20.4542455817527,
0.));
#222971=CARTESIAN_POINT('Ctrl Pts',(9.77162045104069,-20.4542455817527,
12.));
#222972=CARTESIAN_POINT('Ctrl Pts',(9.76734670980891,-20.447195862298,0.));
#222973=CARTESIAN_POINT('Ctrl Pts',(9.76734670980891,-20.447195862298,12.));
#222974=CARTESIAN_POINT('Ctrl Pts',(9.76322747195494,-20.44034423294,0.));
#222975=CARTESIAN_POINT('Ctrl Pts',(9.76322747195494,-20.44034423294,12.));
#222976=CARTESIAN_POINT('Ctrl Pts',(9.75926386289922,-20.4336957355473,
0.));
#222977=CARTESIAN_POINT('Ctrl Pts',(9.75926386289922,-20.4336957355473,
12.));
#222978=CARTESIAN_POINT('Ctrl Pts',(9.75545705902417,-20.4272556476629,
0.));
#222979=CARTESIAN_POINT('Ctrl Pts',(9.75545705902417,-20.4272556476629,
12.));
#222980=CARTESIAN_POINT('Ctrl Pts',(9.75180829786429,-20.4210295275817,
0.));
#222981=CARTESIAN_POINT('Ctrl Pts',(9.75180829786429,-20.4210295275817,
12.));
#222982=CARTESIAN_POINT('Ctrl Pts',(9.74831889242173,-20.4150232777393,
0.));
#222983=CARTESIAN_POINT('Ctrl Pts',(9.74831889242173,-20.4150232777393,
12.));
#222984=CARTESIAN_POINT('Ctrl Pts',(9.74499021838537,-20.4092430879861,
0.));
#222985=CARTESIAN_POINT('Ctrl Pts',(9.74499021838537,-20.4092430879861,
12.));
#222986=CARTESIAN_POINT('Ctrl Pts',(9.74182369656271,-20.4036953576549,
0.));
#222987=CARTESIAN_POINT('Ctrl Pts',(9.74182369656271,-20.4036953576549,
12.));
#222988=CARTESIAN_POINT('Ctrl Pts',(9.738820776132,-20.3983866213331,0.));
#222989=CARTESIAN_POINT('Ctrl Pts',(9.738820776132,-20.3983866213331,12.));
#222990=CARTESIAN_POINT('Ctrl Pts',(9.73598292014242,-20.3933234845647,
0.));
#222991=CARTESIAN_POINT('Ctrl Pts',(9.73598292014242,-20.3933234845647,
12.));
#222992=CARTESIAN_POINT('Ctrl Pts',(9.73331167102807,-20.3885129129912,
0.));
#222993=CARTESIAN_POINT('Ctrl Pts',(9.73331167102807,-20.3885129129912,
12.));
#222994=CARTESIAN_POINT('Ctrl Pts',(9.73080870123726,-20.3839624556742,
0.));
#222995=CARTESIAN_POINT('Ctrl Pts',(9.73080870123726,-20.3839624556742,
12.));
#222996=CARTESIAN_POINT('Ctrl Pts',(9.72847589116541,-20.3796805893304,
0.));
#222997=CARTESIAN_POINT('Ctrl Pts',(9.72847589116541,-20.3796805893304,
12.));
#222998=CARTESIAN_POINT('Ctrl Pts',(9.7263153173288,-20.3756766651951,0.));
#222999=CARTESIAN_POINT('Ctrl Pts',(9.7263153173288,-20.3756766651951,12.));
#223000=CARTESIAN_POINT('Ctrl Pts',(9.72432910043194,-20.371960235676,0.));
#223001=CARTESIAN_POINT('Ctrl Pts',(9.72432910043194,-20.371960235676,12.));
#223002=CARTESIAN_POINT('Ctrl Pts',(9.72251930722489,-20.3685406190576,
0.));
#223003=CARTESIAN_POINT('Ctrl Pts',(9.72251930722489,-20.3685406190576,
12.));
#223004=CARTESIAN_POINT('Ctrl Pts',(9.7208877838108,-20.3654261611056,0.));
#223005=CARTESIAN_POINT('Ctrl Pts',(9.7208877838108,-20.3654261611056,12.));
#223006=CARTESIAN_POINT('Ctrl Pts',(9.71943648548099,-20.3626256913981,
0.));
#223007=CARTESIAN_POINT('Ctrl Pts',(9.71943648548099,-20.3626256913981,
12.));
#223008=CARTESIAN_POINT('Ctrl Pts',(9.71816778328006,-20.3601498764344,
0.));
#223009=CARTESIAN_POINT('Ctrl Pts',(9.71816778328006,-20.3601498764344,
12.));
#223010=CARTESIAN_POINT('Ctrl Pts',(9.71708493723096,-20.3580133103356,
0.));
#223011=CARTESIAN_POINT('Ctrl Pts',(9.71708493723096,-20.3580133103356,
12.));
#223012=CARTESIAN_POINT('Ctrl Pts',(9.71619192554185,-20.3562337557875,
0.));
#223013=CARTESIAN_POINT('Ctrl Pts',(9.71619192554185,-20.3562337557875,
12.));
#223014=CARTESIAN_POINT('Ctrl Pts',(9.71549257088172,-20.3548282742361,
0.));
#223015=CARTESIAN_POINT('Ctrl Pts',(9.71549257088172,-20.3548282742361,
12.));
#223016=CARTESIAN_POINT('Ctrl Pts',(9.7149897805202,-20.3538098605706,0.));
#223017=CARTESIAN_POINT('Ctrl Pts',(9.7149897805202,-20.3538098605706,12.));
#223018=CARTESIAN_POINT('Ctrl Pts',(9.7147459035068,-20.3533097561886,0.));
#223019=CARTESIAN_POINT('Ctrl Pts',(9.7147459035068,-20.3533097561886,12.));
#223020=CARTESIAN_POINT('Ctrl Pts',(9.71465227853041,-20.3531126095522,
0.));
#223021=CARTESIAN_POINT('Ctrl Pts',(9.71465227853041,-20.3531126095522,
12.));
#223022=CARTESIAN_POINT('Ctrl Pts',(9.71462954053041,-20.353060251684,0.));
#223023=CARTESIAN_POINT('Ctrl Pts',(9.71462954053041,-20.353060251684,12.));
#223024=CARTESIAN_POINT('Ctrl Pts',(9.71462809124915,-20.353053841303,0.));
#223025=CARTESIAN_POINT('Ctrl Pts',(9.71462809124915,-20.353053841303,12.));
#223026=CARTESIAN_POINT('',(12.4230808101438,-22.8400320311649,0.));
#223027=CARTESIAN_POINT('Ctrl Pts',(12.4230808101438,-22.8400320311649,
0.));
#223028=CARTESIAN_POINT('Ctrl Pts',(12.418215285186,-22.8370364396459,0.));
#223029=CARTESIAN_POINT('Ctrl Pts',(12.4084933766346,-22.8310435872748,
0.));
#223030=CARTESIAN_POINT('Ctrl Pts',(12.3939379378998,-22.8220493007173,
0.));
#223031=CARTESIAN_POINT('Ctrl Pts',(12.374585536673,-22.81004690224,0.));
#223032=CARTESIAN_POINT('Ctrl Pts',(12.3504864740319,-22.795027221673,0.));
#223033=CARTESIAN_POINT('Ctrl Pts',(12.3264788926075,-22.7799908974768,
0.));
#223034=CARTESIAN_POINT('Ctrl Pts',(12.3025628601792,-22.764938010105,0.));
#223035=CARTESIAN_POINT('Ctrl Pts',(12.2787384750742,-22.7498686970069,
0.));
#223036=CARTESIAN_POINT('Ctrl Pts',(12.2550058702395,-22.7347831655287,
0.));
#223037=CARTESIAN_POINT('Ctrl Pts',(12.2313652198061,-22.7196817119374,
0.));
#223038=CARTESIAN_POINT('Ctrl Pts',(12.2078167360284,-22.7045647168747,
0.));
#223039=CARTESIAN_POINT('Ctrl Pts',(12.1843606579261,-22.6894326205037,
0.));
#223040=CARTESIAN_POINT('Ctrl Pts',(12.1609972423099,-22.6742859034944,
0.));
#223041=CARTESIAN_POINT('Ctrl Pts',(12.1377267537145,-22.6591250653965,
0.));
#223042=CARTESIAN_POINT('Ctrl Pts',(12.1145494550383,-22.6439506046605,
0.));
#223043=CARTESIAN_POINT('Ctrl Pts',(12.0914655972823,-22.6287629967056,
0.));
#223044=CARTESIAN_POINT('Ctrl Pts',(12.0684754113862,-22.6135626764898,
0.));
#223045=CARTESIAN_POINT('Ctrl Pts',(12.0455791139128,-22.5983500505644,
0.));
#223046=CARTESIAN_POINT('Ctrl Pts',(12.0227769113127,-22.5831255061282,
0.));
#223047=CARTESIAN_POINT('Ctrl Pts',(12.0000690046694,-22.5678894211181,
0.));
#223048=CARTESIAN_POINT('Ctrl Pts',(11.9774555943496,-22.5526421741158,
0.));
#223049=CARTESIAN_POINT('Ctrl Pts',(11.9549368843997,-22.5373841537307,
0.));
#223050=CARTESIAN_POINT('Ctrl Pts',(11.9325130877803,-22.5221157697883,
0.));
#223051=CARTESIAN_POINT('Ctrl Pts',(11.9101844254557,-22.5068374513973,
0.));
#223052=CARTESIAN_POINT('Ctrl Pts',(11.8879511239942,-22.4915496418485,
0.));
#223053=CARTESIAN_POINT('Ctrl Pts',(11.8658134137019,-22.4762527946702,
0.));
#223054=CARTESIAN_POINT('Ctrl Pts',(11.8437715264487,-22.4609473690472,
0.));
#223055=CARTESIAN_POINT('Ctrl Pts',(11.8218256937889,-22.4456338258735,
0.));
#223056=CARTESIAN_POINT('Ctrl Pts',(11.7999761445173,-22.430312622646,0.));
#223057=CARTESIAN_POINT('Ctrl Pts',(11.7782231042039,-22.4149842125008,
0.));
#223058=CARTESIAN_POINT('Ctrl Pts',(11.7565667964764,-22.3996490469191,
0.));
#223059=CARTESIAN_POINT('Ctrl Pts',(11.7350074437961,-22.3843075773899,
0.));
#223060=CARTESIAN_POINT('Ctrl Pts',(11.7135452684532,-22.3689602575491,
0.));
#223061=CARTESIAN_POINT('Ctrl Pts',(11.6921804934056,-22.3536075450029,
0.));
#223062=CARTESIAN_POINT('Ctrl Pts',(11.6709133432985,-22.3382499035619,
0.));
#223063=CARTESIAN_POINT('Ctrl Pts',(11.6497440449857,-22.3228878043976,
0.));
#223064=CARTESIAN_POINT('Ctrl Pts',(11.6286728270009,-22.3075217249049,
0.));
#223065=CARTESIAN_POINT('Ctrl Pts',(11.6076999192357,-22.2921521480356,
0.));
#223066=CARTESIAN_POINT('Ctrl Pts',(11.5868255525188,-22.2767795614348,
0.));
#223067=CARTESIAN_POINT('Ctrl Pts',(11.5660499582403,-22.2614044566898,
0.));
#223068=CARTESIAN_POINT('Ctrl Pts',(11.5453733679121,-22.2460273284654,
0.));
#223069=CARTESIAN_POINT('Ctrl Pts',(11.5247960128477,-22.2306486738901,
0.));
#223070=CARTESIAN_POINT('Ctrl Pts',(11.5043181244242,-22.2152689931022,
0.));
#223071=CARTESIAN_POINT('Ctrl Pts',(11.483939934259,-22.1998887896436,0.));
#223072=CARTESIAN_POINT('Ctrl Pts',(11.463661674411,-22.184508570917,0.));
#223073=CARTESIAN_POINT('Ctrl Pts',(11.443483577557,-22.1691288486096,0.));
#223074=CARTESIAN_POINT('Ctrl Pts',(11.4234058771742,-22.1537501391487,
0.));
#223075=CARTESIAN_POINT('Ctrl Pts',(11.4034288076908,-22.1383729640964,
0.));
#223076=CARTESIAN_POINT('Ctrl Pts',(11.3835526044256,-22.1229978500186,
0.));
#223077=CARTESIAN_POINT('Ctrl Pts',(11.3637775035367,-22.1076253283979,
0.));
#223078=CARTESIAN_POINT('Ctrl Pts',(11.3441037419553,-22.0922559355294,
0.));
#223079=CARTESIAN_POINT('Ctrl Pts',(11.3245315573168,-22.0768902124267,
0.));
#223080=CARTESIAN_POINT('Ctrl Pts',(11.3050611878771,-22.0615287047179,
0.));
#223081=CARTESIAN_POINT('Ctrl Pts',(11.2856928724374,-22.046171962566,0.));
#223082=CARTESIAN_POINT('Ctrl Pts',(11.2664268504206,-22.030820540835,0.));
#223083=CARTESIAN_POINT('Ctrl Pts',(11.2472633619275,-22.0154749992363,
0.));
#223084=CARTESIAN_POINT('Ctrl Pts',(11.2282026477896,-22.0001359024839,
0.));
#223085=CARTESIAN_POINT('Ctrl Pts',(11.2092449496125,-21.9848038204439,
0.));
#223086=CARTESIAN_POINT('Ctrl Pts',(11.190390509811,-21.9694793282914,0.));
#223087=CARTESIAN_POINT('Ctrl Pts',(11.1716395716376,-21.9541630066506,
0.));
#223088=CARTESIAN_POINT('Ctrl Pts',(11.1529923792003,-21.9388554416439,
0.));
#223089=CARTESIAN_POINT('Ctrl Pts',(11.1344491774741,-21.923557224952,0.));
#223090=CARTESIAN_POINT('Ctrl Pts',(11.1160102123024,-21.9082689538688,
0.));
#223091=CARTESIAN_POINT('Ctrl Pts',(11.0976757303944,-21.8929912313608,
0.));
#223092=CARTESIAN_POINT('Ctrl Pts',(11.0794459793057,-21.877724666119,0.));
#223093=CARTESIAN_POINT('Ctrl Pts',(11.0613212074363,-21.8624698726318,
0.));
#223094=CARTESIAN_POINT('Ctrl Pts',(11.0433016640807,-21.8472274713103,
0.));
#223095=CARTESIAN_POINT('Ctrl Pts',(11.0253875994598,-21.8319980886033,
0.));
#223096=CARTESIAN_POINT('Ctrl Pts',(11.0075792647477,-21.8167823571168,
0.));
#223097=CARTESIAN_POINT('Ctrl Pts',(10.9898769120912,-21.8015809157301,
0.));
#223098=CARTESIAN_POINT('Ctrl Pts',(10.9722807946155,-21.7863944097141,
0.));
#223099=CARTESIAN_POINT('Ctrl Pts',(10.9547911664455,-21.7712234908464,
0.));
#223100=CARTESIAN_POINT('Ctrl Pts',(10.9374082827444,-21.7560688175247,
0.));
#223101=CARTESIAN_POINT('Ctrl Pts',(10.9201323997384,-21.7409310548797,
0.));
#223102=CARTESIAN_POINT('Ctrl Pts',(10.902963774734,-21.7258108748873,0.));
#223103=CARTESIAN_POINT('Ctrl Pts',(10.8859026661293,-21.7107089564825,
0.));
#223104=CARTESIAN_POINT('Ctrl Pts',(10.8689493334095,-21.6956259856672,
0.));
#223105=CARTESIAN_POINT('Ctrl Pts',(10.8521040371835,-21.6805626556467,
0.));
#223106=CARTESIAN_POINT('Ctrl Pts',(10.8353670392272,-21.6655196669732,
0.));
#223107=CARTESIAN_POINT('Ctrl Pts',(10.8187386025136,-21.6504977276866,
0.));
#223108=CARTESIAN_POINT('Ctrl Pts',(10.8022189912369,-21.6354975534557,
0.));
#223109=CARTESIAN_POINT('Ctrl Pts',(10.7858084708261,-21.6205198677173,
0.));
#223110=CARTESIAN_POINT('Ctrl Pts',(10.7695073079552,-21.6055654018176,
0.));
#223111=CARTESIAN_POINT('Ctrl Pts',(10.7533157705941,-21.5906348951743,
0.));
#223112=CARTESIAN_POINT('Ctrl Pts',(10.7372341280467,-21.5757290954371,
0.));
#223113=CARTESIAN_POINT('Ctrl Pts',(10.7212626509816,-21.5608487586468,
0.));
#223114=CARTESIAN_POINT('Ctrl Pts',(10.7054016114571,-21.5459946493955,
0.));
#223115=CARTESIAN_POINT('Ctrl Pts',(10.689651282929,-21.5311675409807,0.));
#223116=CARTESIAN_POINT('Ctrl Pts',(10.6740119402834,-21.51636821558,0.));
#223117=CARTESIAN_POINT('Ctrl Pts',(10.6584838598939,-21.5015974644449,
0.));
#223118=CARTESIAN_POINT('Ctrl Pts',(10.6430673196607,-21.4868560880889,
0.));
#223119=CARTESIAN_POINT('Ctrl Pts',(10.6277625990456,-21.4721448964766,
0.));
#223120=CARTESIAN_POINT('Ctrl Pts',(10.6125699790961,-21.4574647092097,
0.));
#223121=CARTESIAN_POINT('Ctrl Pts',(10.5974897424622,-21.4428163557144,
0.));
#223122=CARTESIAN_POINT('Ctrl Pts',(10.5825221734573,-21.4282006754631,
0.));
#223123=CARTESIAN_POINT('Ctrl Pts',(10.5676675581108,-21.4136185181979,
0.));
#223124=CARTESIAN_POINT('Ctrl Pts',(10.5529261842108,-21.3990707441497,
0.));
#223125=CARTESIAN_POINT('Ctrl Pts',(10.5382983413421,-21.3845582242602,
0.));
#223126=CARTESIAN_POINT('Ctrl Pts',(10.5237843209057,-21.3700818403936,
0.));
#223127=CARTESIAN_POINT('Ctrl Pts',(10.5093844161685,-21.3556424855814,
0.));
#223128=CARTESIAN_POINT('Ctrl Pts',(10.4950989223336,-21.3412410642904,
0.));
#223129=CARTESIAN_POINT('Ctrl Pts',(10.4809281365931,-21.3268784926819,
0.));
#223130=CARTESIAN_POINT('Ctrl Pts',(10.4668723581768,-21.3125556988731,
0.));
#223131=CARTESIAN_POINT('Ctrl Pts',(10.4529318883874,-21.2982736231931,
0.));
#223132=CARTESIAN_POINT('Ctrl Pts',(10.4391070306391,-21.2840332184483,
0.));
#223133=CARTESIAN_POINT('Ctrl Pts',(10.42539809054,-21.2698354502403,0.));
#223134=CARTESIAN_POINT('Ctrl Pts',(10.4118053759588,-21.255681297275,0.));
#223135=CARTESIAN_POINT('Ctrl Pts',(10.3983291970846,-21.2415717516714,
0.));
#223136=CARTESIAN_POINT('Ctrl Pts',(10.3849698664786,-21.22750781927,0.));
#223137=CARTESIAN_POINT('Ctrl Pts',(10.371727699113,-21.2134905199345,0.));
#223138=CARTESIAN_POINT('Ctrl Pts',(10.3586030124587,-21.199520887919,0.));
#223139=CARTESIAN_POINT('Ctrl Pts',(10.34559612657,-21.1855999722416,0.));
#223140=CARTESIAN_POINT('Ctrl Pts',(10.3327073641572,-21.1717288370509,
0.));
#223141=CARTESIAN_POINT('Ctrl Pts',(10.3199370506544,-21.1579085619965,
0.));
#223142=CARTESIAN_POINT('Ctrl Pts',(10.3072855142687,-21.1441402425843,
0.));
#223143=CARTESIAN_POINT('Ctrl Pts',(10.2947530860721,-21.1304249906002,
0.));
#223144=CARTESIAN_POINT('Ctrl Pts',(10.2823401001072,-21.1167639345631,
0.));
#223145=CARTESIAN_POINT('Ctrl Pts',(10.2700468934744,-21.1031582201627,
0.));
#223146=CARTESIAN_POINT('Ctrl Pts',(10.2578738064181,-21.0896090107063,
0.));
#223147=CARTESIAN_POINT('Ctrl Pts',(10.2458211823912,-21.0761174875445,
0.));
#223148=CARTESIAN_POINT('Ctrl Pts',(10.2338893681567,-21.0626848505663,
0.));
#223149=CARTESIAN_POINT('Ctrl Pts',(10.2220787139154,-21.0493123187483,
0.));
#223150=CARTESIAN_POINT('Ctrl Pts',(10.2103895734123,-21.0360011306815,
0.));
#223151=CARTESIAN_POINT('Ctrl Pts',(10.1988223040425,-21.0227525451107,
0.));
#223152=CARTESIAN_POINT('Ctrl Pts',(10.187377266936,-21.0095678414486,0.));
#223153=CARTESIAN_POINT('Ctrl Pts',(10.1760548270767,-20.9964483203686,
0.));
#223154=CARTESIAN_POINT('Ctrl Pts',(10.1648553534568,-20.9833953044736,
0.));
#223155=CARTESIAN_POINT('Ctrl Pts',(10.1537792192065,-20.9704101389369,
0.));
#223156=CARTESIAN_POINT('Ctrl Pts',(10.1428268017256,-20.9574941921591,
0.));
#223157=CARTESIAN_POINT('Ctrl Pts',(10.1319984827908,-20.9446488563933,
0.));
#223158=CARTESIAN_POINT('Ctrl Pts',(10.1212946487057,-20.9318755484734,
0.));
#223159=CARTESIAN_POINT('Ctrl Pts',(10.1107156904836,-20.919175710627,0.));
#223160=CARTESIAN_POINT('Ctrl Pts',(10.1002620040076,-20.9065508112557,
0.));
#223161=CARTESIAN_POINT('Ctrl Pts',(10.0899339901915,-20.894002345737,0.));
#223162=CARTESIAN_POINT('Ctrl Pts',(10.0797320551154,-20.881531837184,0.));
#223163=CARTESIAN_POINT('Ctrl Pts',(10.0696566102218,-20.86914083737,0.));
#223164=CARTESIAN_POINT('Ctrl Pts',(10.0597080725375,-20.8568309277316,
0.));
#223165=CARTESIAN_POINT('Ctrl Pts',(10.0498868648733,-20.8446037203402,
0.));
#223166=CARTESIAN_POINT('Ctrl Pts',(10.0401934160234,-20.8324608588909,
0.));
#223167=CARTESIAN_POINT('Ctrl Pts',(10.0306281609435,-20.8204040196602,
0.));
#223168=CARTESIAN_POINT('Ctrl Pts',(10.0211915410095,-20.8084349126888,
0.));
#223169=CARTESIAN_POINT('Ctrl Pts',(10.0118840042786,-20.7965552829908,
0.));
#223170=CARTESIAN_POINT('Ctrl Pts',(10.0027060057389,-20.7847669117568,
0.));
#223171=CARTESIAN_POINT('Ctrl Pts',(9.9936580075464,-20.7730716175417,0.));
#223172=CARTESIAN_POINT('Ctrl Pts',(9.98474047926852,-20.761471257499,0.));
#223173=CARTESIAN_POINT('Ctrl Pts',(9.97595389823469,-20.7499677289627,
0.));
#223174=CARTESIAN_POINT('Ctrl Pts',(9.96729874986201,-20.7385629709795,
0.));
#223175=CARTESIAN_POINT('Ctrl Pts',(9.95877552798397,-20.7272589658751,
0.));
#223176=CARTESIAN_POINT('Ctrl Pts',(9.95038473514948,-20.7160577407579,
0.));
#223177=CARTESIAN_POINT('Ctrl Pts',(9.94212688298236,-20.7049613692234,
0.));
#223178=CARTESIAN_POINT('Ctrl Pts',(9.93400249259729,-20.6939719732484,
0.));
#223179=CARTESIAN_POINT('Ctrl Pts',(9.92601209498748,-20.6830917250255,
0.));
#223180=CARTESIAN_POINT('Ctrl Pts',(9.91815623141288,-20.6723228488263,
0.));
#223181=CARTESIAN_POINT('Ctrl Pts',(9.91043545377007,-20.6616676228315,
0.));
#223182=CARTESIAN_POINT('Ctrl Pts',(9.90285032516692,-20.6511283817414,
0.));
#223183=CARTESIAN_POINT('Ctrl Pts',(9.89540142049119,-20.6407075193976,
0.));
#223184=CARTESIAN_POINT('Ctrl Pts',(9.88808932697305,-20.6304074914087,
0.));
#223185=CARTESIAN_POINT('Ctrl Pts',(9.88091464472675,-20.6202308177475,
0.));
#223186=CARTESIAN_POINT('Ctrl Pts',(9.87387798732955,-20.6101800854494,
0.));
#223187=CARTESIAN_POINT('Ctrl Pts',(9.86697998242622,-20.6002579513699,
0.));
#223188=CARTESIAN_POINT('Ctrl Pts',(9.86022127232747,-20.5904671449754,
0.));
#223189=CARTESIAN_POINT('Ctrl Pts',(9.8536025145698,-20.5808104710015,0.));
#223190=CARTESIAN_POINT('Ctrl Pts',(9.84712438256277,-20.5712908125139,
0.));
#223191=CARTESIAN_POINT('Ctrl Pts',(9.84078756677565,-20.5619111362402,
0.));
#223192=CARTESIAN_POINT('Ctrl Pts',(9.83459277585315,-20.552674497646,0.));
#223193=CARTESIAN_POINT('Ctrl Pts',(9.82854073773876,-20.5435840460721,
0.));
#223194=CARTESIAN_POINT('Ctrl Pts',(9.82263220080362,-20.5346430299517,
0.));
#223195=CARTESIAN_POINT('Ctrl Pts',(9.81686793455942,-20.5258548000629,
0.));
#223196=CARTESIAN_POINT('Ctrl Pts',(9.81124873025281,-20.517222812284,0.));
#223197=CARTESIAN_POINT('Ctrl Pts',(9.80577540161087,-20.5087506310505,
0.));
#223198=CARTESIAN_POINT('Ctrl Pts',(9.80044878520948,-20.5004419312107,
0.));
#223199=CARTESIAN_POINT('Ctrl Pts',(9.7952697428833,-20.4923005087943,0.));
#223200=CARTESIAN_POINT('Ctrl Pts',(9.79023916498655,-20.4843302955329,
0.));
#223201=CARTESIAN_POINT('Ctrl Pts',(9.78535797314166,-20.4765353711586,
0.));
#223202=CARTESIAN_POINT('Ctrl Pts',(9.7806271237332,-20.4689199790669,0.));
#223203=CARTESIAN_POINT('Ctrl Pts',(9.77604760815528,-20.4614885274975,
0.));
#223204=CARTESIAN_POINT('Ctrl Pts',(9.77162045104069,-20.4542455817527,
0.));
#223205=CARTESIAN_POINT('Ctrl Pts',(9.76734670980891,-20.447195862298,0.));
#223206=CARTESIAN_POINT('Ctrl Pts',(9.76322747195494,-20.44034423294,0.));
#223207=CARTESIAN_POINT('Ctrl Pts',(9.75926386289922,-20.4336957355473,
0.));
#223208=CARTESIAN_POINT('Ctrl Pts',(9.75545705902417,-20.4272556476629,
0.));
#223209=CARTESIAN_POINT('Ctrl Pts',(9.75180829786429,-20.4210295275817,
0.));
#223210=CARTESIAN_POINT('Ctrl Pts',(9.74831889242173,-20.4150232777393,
0.));
#223211=CARTESIAN_POINT('Ctrl Pts',(9.74499021838537,-20.4092430879861,
0.));
#223212=CARTESIAN_POINT('Ctrl Pts',(9.74182369656271,-20.4036953576549,
0.));
#223213=CARTESIAN_POINT('Ctrl Pts',(9.738820776132,-20.3983866213331,0.));
#223214=CARTESIAN_POINT('Ctrl Pts',(9.73598292014242,-20.3933234845647,
0.));
#223215=CARTESIAN_POINT('Ctrl Pts',(9.73331167102807,-20.3885129129912,
0.));
#223216=CARTESIAN_POINT('Ctrl Pts',(9.73080870123726,-20.3839624556742,
0.));
#223217=CARTESIAN_POINT('Ctrl Pts',(9.72847589116541,-20.3796805893304,
0.));
#223218=CARTESIAN_POINT('Ctrl Pts',(9.7263153173288,-20.3756766651951,0.));
#223219=CARTESIAN_POINT('Ctrl Pts',(9.72432910043194,-20.371960235676,0.));
#223220=CARTESIAN_POINT('Ctrl Pts',(9.72251930722489,-20.3685406190576,
0.));
#223221=CARTESIAN_POINT('Ctrl Pts',(9.7208877838108,-20.3654261611056,0.));
#223222=CARTESIAN_POINT('Ctrl Pts',(9.71943648548099,-20.3626256913981,
0.));
#223223=CARTESIAN_POINT('Ctrl Pts',(9.71816778328006,-20.3601498764344,
0.));
#223224=CARTESIAN_POINT('Ctrl Pts',(9.71708493723096,-20.3580133103356,
0.));
#223225=CARTESIAN_POINT('Ctrl Pts',(9.71619192554185,-20.3562337557875,
0.));
#223226=CARTESIAN_POINT('Ctrl Pts',(9.71549257088172,-20.3548282742361,
0.));
#223227=CARTESIAN_POINT('Ctrl Pts',(9.7149897805202,-20.3538098605706,0.));
#223228=CARTESIAN_POINT('Ctrl Pts',(9.7147459035068,-20.3533097561886,0.));
#223229=CARTESIAN_POINT('Ctrl Pts',(9.71465227853041,-20.3531126095522,
0.));
#223230=CARTESIAN_POINT('Ctrl Pts',(9.71462954053041,-20.353060251684,0.));
#223231=CARTESIAN_POINT('Ctrl Pts',(9.71462809124915,-20.353053841303,0.));
#223232=CARTESIAN_POINT('',(12.4230808101438,-22.8400320311649,12.));
#223233=CARTESIAN_POINT('',(12.4230808101438,-22.8400320311649,0.));
#223234=CARTESIAN_POINT('Ctrl Pts',(9.71462809124915,-20.353053841303,12.));
#223235=CARTESIAN_POINT('Ctrl Pts',(9.71462954053041,-20.353060251684,12.));
#223236=CARTESIAN_POINT('Ctrl Pts',(9.71465227853041,-20.3531126095522,
12.));
#223237=CARTESIAN_POINT('Ctrl Pts',(9.7147459035068,-20.3533097561886,12.));
#223238=CARTESIAN_POINT('Ctrl Pts',(9.7149897805202,-20.3538098605706,12.));
#223239=CARTESIAN_POINT('Ctrl Pts',(9.71549257088172,-20.3548282742361,
12.));
#223240=CARTESIAN_POINT('Ctrl Pts',(9.71619192554185,-20.3562337557875,
12.));
#223241=CARTESIAN_POINT('Ctrl Pts',(9.71708493723096,-20.3580133103356,
12.));
#223242=CARTESIAN_POINT('Ctrl Pts',(9.71816778328006,-20.3601498764344,
12.));
#223243=CARTESIAN_POINT('Ctrl Pts',(9.71943648548099,-20.3626256913981,
12.));
#223244=CARTESIAN_POINT('Ctrl Pts',(9.7208877838108,-20.3654261611056,12.));
#223245=CARTESIAN_POINT('Ctrl Pts',(9.72251930722489,-20.3685406190576,
12.));
#223246=CARTESIAN_POINT('Ctrl Pts',(9.72432910043194,-20.371960235676,12.));
#223247=CARTESIAN_POINT('Ctrl Pts',(9.7263153173288,-20.3756766651951,12.));
#223248=CARTESIAN_POINT('Ctrl Pts',(9.72847589116541,-20.3796805893304,
12.));
#223249=CARTESIAN_POINT('Ctrl Pts',(9.73080870123726,-20.3839624556742,
12.));
#223250=CARTESIAN_POINT('Ctrl Pts',(9.73331167102807,-20.3885129129912,
12.));
#223251=CARTESIAN_POINT('Ctrl Pts',(9.73598292014242,-20.3933234845647,
12.));
#223252=CARTESIAN_POINT('Ctrl Pts',(9.738820776132,-20.3983866213331,12.));
#223253=CARTESIAN_POINT('Ctrl Pts',(9.74182369656271,-20.4036953576549,
12.));
#223254=CARTESIAN_POINT('Ctrl Pts',(9.74499021838537,-20.4092430879861,
12.));
#223255=CARTESIAN_POINT('Ctrl Pts',(9.74831889242173,-20.4150232777393,
12.));
#223256=CARTESIAN_POINT('Ctrl Pts',(9.75180829786429,-20.4210295275817,
12.));
#223257=CARTESIAN_POINT('Ctrl Pts',(9.75545705902417,-20.4272556476629,
12.));
#223258=CARTESIAN_POINT('Ctrl Pts',(9.75926386289922,-20.4336957355473,
12.));
#223259=CARTESIAN_POINT('Ctrl Pts',(9.76322747195494,-20.44034423294,12.));
#223260=CARTESIAN_POINT('Ctrl Pts',(9.76734670980891,-20.447195862298,12.));
#223261=CARTESIAN_POINT('Ctrl Pts',(9.77162045104069,-20.4542455817527,
12.));
#223262=CARTESIAN_POINT('Ctrl Pts',(9.77604760815528,-20.4614885274975,
12.));
#223263=CARTESIAN_POINT('Ctrl Pts',(9.7806271237332,-20.4689199790669,12.));
#223264=CARTESIAN_POINT('Ctrl Pts',(9.78535797314166,-20.4765353711586,
12.));
#223265=CARTESIAN_POINT('Ctrl Pts',(9.79023916498655,-20.4843302955329,
12.));
#223266=CARTESIAN_POINT('Ctrl Pts',(9.7952697428833,-20.4923005087943,12.));
#223267=CARTESIAN_POINT('Ctrl Pts',(9.80044878520948,-20.5004419312107,
12.));
#223268=CARTESIAN_POINT('Ctrl Pts',(9.80577540161087,-20.5087506310505,
12.));
#223269=CARTESIAN_POINT('Ctrl Pts',(9.81124873025281,-20.517222812284,12.));
#223270=CARTESIAN_POINT('Ctrl Pts',(9.81686793455942,-20.5258548000629,
12.));
#223271=CARTESIAN_POINT('Ctrl Pts',(9.82263220080362,-20.5346430299517,
12.));
#223272=CARTESIAN_POINT('Ctrl Pts',(9.82854073773876,-20.5435840460721,
12.));
#223273=CARTESIAN_POINT('Ctrl Pts',(9.83459277585315,-20.552674497646,12.));
#223274=CARTESIAN_POINT('Ctrl Pts',(9.84078756677565,-20.5619111362402,
12.));
#223275=CARTESIAN_POINT('Ctrl Pts',(9.84712438256277,-20.5712908125139,
12.));
#223276=CARTESIAN_POINT('Ctrl Pts',(9.8536025145698,-20.5808104710015,12.));
#223277=CARTESIAN_POINT('Ctrl Pts',(9.86022127232747,-20.5904671449754,
12.));
#223278=CARTESIAN_POINT('Ctrl Pts',(9.86697998242622,-20.6002579513699,
12.));
#223279=CARTESIAN_POINT('Ctrl Pts',(9.87387798732955,-20.6101800854494,
12.));
#223280=CARTESIAN_POINT('Ctrl Pts',(9.88091464472675,-20.6202308177475,
12.));
#223281=CARTESIAN_POINT('Ctrl Pts',(9.88808932697305,-20.6304074914087,
12.));
#223282=CARTESIAN_POINT('Ctrl Pts',(9.89540142049119,-20.6407075193976,
12.));
#223283=CARTESIAN_POINT('Ctrl Pts',(9.90285032516692,-20.6511283817414,
12.));
#223284=CARTESIAN_POINT('Ctrl Pts',(9.91043545377007,-20.6616676228315,
12.));
#223285=CARTESIAN_POINT('Ctrl Pts',(9.91815623141288,-20.6723228488263,
12.));
#223286=CARTESIAN_POINT('Ctrl Pts',(9.92601209498748,-20.6830917250255,
12.));
#223287=CARTESIAN_POINT('Ctrl Pts',(9.93400249259729,-20.6939719732484,
12.));
#223288=CARTESIAN_POINT('Ctrl Pts',(9.94212688298236,-20.7049613692234,
12.));
#223289=CARTESIAN_POINT('Ctrl Pts',(9.95038473514948,-20.7160577407579,
12.));
#223290=CARTESIAN_POINT('Ctrl Pts',(9.95877552798397,-20.7272589658751,
12.));
#223291=CARTESIAN_POINT('Ctrl Pts',(9.96729874986201,-20.7385629709795,
12.));
#223292=CARTESIAN_POINT('Ctrl Pts',(9.97595389823469,-20.7499677289627,
12.));
#223293=CARTESIAN_POINT('Ctrl Pts',(9.98474047926852,-20.761471257499,12.));
#223294=CARTESIAN_POINT('Ctrl Pts',(9.9936580075464,-20.7730716175417,12.));
#223295=CARTESIAN_POINT('Ctrl Pts',(10.0027060057389,-20.7847669117568,
12.));
#223296=CARTESIAN_POINT('Ctrl Pts',(10.0118840042786,-20.7965552829908,
12.));
#223297=CARTESIAN_POINT('Ctrl Pts',(10.0211915410095,-20.8084349126888,
12.));
#223298=CARTESIAN_POINT('Ctrl Pts',(10.0306281609435,-20.8204040196602,
12.));
#223299=CARTESIAN_POINT('Ctrl Pts',(10.0401934160234,-20.8324608588909,
12.));
#223300=CARTESIAN_POINT('Ctrl Pts',(10.0498868648733,-20.8446037203402,
12.));
#223301=CARTESIAN_POINT('Ctrl Pts',(10.0597080725375,-20.8568309277316,
12.));
#223302=CARTESIAN_POINT('Ctrl Pts',(10.0696566102218,-20.86914083737,12.));
#223303=CARTESIAN_POINT('Ctrl Pts',(10.0797320551154,-20.881531837184,12.));
#223304=CARTESIAN_POINT('Ctrl Pts',(10.0899339901915,-20.894002345737,12.));
#223305=CARTESIAN_POINT('Ctrl Pts',(10.1002620040076,-20.9065508112557,
12.));
#223306=CARTESIAN_POINT('Ctrl Pts',(10.1107156904836,-20.919175710627,12.));
#223307=CARTESIAN_POINT('Ctrl Pts',(10.1212946487057,-20.9318755484734,
12.));
#223308=CARTESIAN_POINT('Ctrl Pts',(10.1319984827908,-20.9446488563933,
12.));
#223309=CARTESIAN_POINT('Ctrl Pts',(10.1428268017256,-20.9574941921591,
12.));
#223310=CARTESIAN_POINT('Ctrl Pts',(10.1537792192065,-20.9704101389369,
12.));
#223311=CARTESIAN_POINT('Ctrl Pts',(10.1648553534568,-20.9833953044736,
12.));
#223312=CARTESIAN_POINT('Ctrl Pts',(10.1760548270767,-20.9964483203686,
12.));
#223313=CARTESIAN_POINT('Ctrl Pts',(10.187377266936,-21.0095678414486,12.));
#223314=CARTESIAN_POINT('Ctrl Pts',(10.1988223040425,-21.0227525451107,
12.));
#223315=CARTESIAN_POINT('Ctrl Pts',(10.2103895734123,-21.0360011306815,
12.));
#223316=CARTESIAN_POINT('Ctrl Pts',(10.2220787139154,-21.0493123187483,
12.));
#223317=CARTESIAN_POINT('Ctrl Pts',(10.2338893681567,-21.0626848505663,
12.));
#223318=CARTESIAN_POINT('Ctrl Pts',(10.2458211823912,-21.0761174875445,
12.));
#223319=CARTESIAN_POINT('Ctrl Pts',(10.2578738064181,-21.0896090107063,
12.));
#223320=CARTESIAN_POINT('Ctrl Pts',(10.2700468934744,-21.1031582201627,
12.));
#223321=CARTESIAN_POINT('Ctrl Pts',(10.2823401001072,-21.1167639345631,
12.));
#223322=CARTESIAN_POINT('Ctrl Pts',(10.2947530860721,-21.1304249906002,
12.));
#223323=CARTESIAN_POINT('Ctrl Pts',(10.3072855142687,-21.1441402425843,
12.));
#223324=CARTESIAN_POINT('Ctrl Pts',(10.3199370506544,-21.1579085619965,
12.));
#223325=CARTESIAN_POINT('Ctrl Pts',(10.3327073641572,-21.1717288370509,
12.));
#223326=CARTESIAN_POINT('Ctrl Pts',(10.34559612657,-21.1855999722416,12.));
#223327=CARTESIAN_POINT('Ctrl Pts',(10.3586030124587,-21.199520887919,12.));
#223328=CARTESIAN_POINT('Ctrl Pts',(10.371727699113,-21.2134905199345,12.));
#223329=CARTESIAN_POINT('Ctrl Pts',(10.3849698664786,-21.22750781927,12.));
#223330=CARTESIAN_POINT('Ctrl Pts',(10.3983291970846,-21.2415717516714,
12.));
#223331=CARTESIAN_POINT('Ctrl Pts',(10.4118053759588,-21.255681297275,12.));
#223332=CARTESIAN_POINT('Ctrl Pts',(10.42539809054,-21.2698354502403,12.));
#223333=CARTESIAN_POINT('Ctrl Pts',(10.4391070306391,-21.2840332184483,
12.));
#223334=CARTESIAN_POINT('Ctrl Pts',(10.4529318883874,-21.2982736231931,
12.));
#223335=CARTESIAN_POINT('Ctrl Pts',(10.4668723581768,-21.3125556988731,
12.));
#223336=CARTESIAN_POINT('Ctrl Pts',(10.4809281365931,-21.3268784926819,
12.));
#223337=CARTESIAN_POINT('Ctrl Pts',(10.4950989223336,-21.3412410642904,
12.));
#223338=CARTESIAN_POINT('Ctrl Pts',(10.5093844161685,-21.3556424855814,
12.));
#223339=CARTESIAN_POINT('Ctrl Pts',(10.5237843209057,-21.3700818403936,
12.));
#223340=CARTESIAN_POINT('Ctrl Pts',(10.5382983413421,-21.3845582242602,
12.));
#223341=CARTESIAN_POINT('Ctrl Pts',(10.5529261842108,-21.3990707441497,
12.));
#223342=CARTESIAN_POINT('Ctrl Pts',(10.5676675581108,-21.4136185181979,
12.));
#223343=CARTESIAN_POINT('Ctrl Pts',(10.5825221734573,-21.4282006754631,
12.));
#223344=CARTESIAN_POINT('Ctrl Pts',(10.5974897424622,-21.4428163557144,
12.));
#223345=CARTESIAN_POINT('Ctrl Pts',(10.6125699790961,-21.4574647092097,
12.));
#223346=CARTESIAN_POINT('Ctrl Pts',(10.6277625990456,-21.4721448964766,
12.));
#223347=CARTESIAN_POINT('Ctrl Pts',(10.6430673196607,-21.4868560880889,
12.));
#223348=CARTESIAN_POINT('Ctrl Pts',(10.6584838598939,-21.5015974644449,
12.));
#223349=CARTESIAN_POINT('Ctrl Pts',(10.6740119402834,-21.51636821558,12.));
#223350=CARTESIAN_POINT('Ctrl Pts',(10.689651282929,-21.5311675409807,12.));
#223351=CARTESIAN_POINT('Ctrl Pts',(10.7054016114571,-21.5459946493955,
12.));
#223352=CARTESIAN_POINT('Ctrl Pts',(10.7212626509816,-21.5608487586468,
12.));
#223353=CARTESIAN_POINT('Ctrl Pts',(10.7372341280467,-21.5757290954371,
12.));
#223354=CARTESIAN_POINT('Ctrl Pts',(10.7533157705941,-21.5906348951743,
12.));
#223355=CARTESIAN_POINT('Ctrl Pts',(10.7695073079552,-21.6055654018176,
12.));
#223356=CARTESIAN_POINT('Ctrl Pts',(10.7858084708261,-21.6205198677173,
12.));
#223357=CARTESIAN_POINT('Ctrl Pts',(10.8022189912369,-21.6354975534557,
12.));
#223358=CARTESIAN_POINT('Ctrl Pts',(10.8187386025136,-21.6504977276866,
12.));
#223359=CARTESIAN_POINT('Ctrl Pts',(10.8353670392272,-21.6655196669732,
12.));
#223360=CARTESIAN_POINT('Ctrl Pts',(10.8521040371835,-21.6805626556467,
12.));
#223361=CARTESIAN_POINT('Ctrl Pts',(10.8689493334095,-21.6956259856672,
12.));
#223362=CARTESIAN_POINT('Ctrl Pts',(10.8859026661293,-21.7107089564825,
12.));
#223363=CARTESIAN_POINT('Ctrl Pts',(10.902963774734,-21.7258108748873,12.));
#223364=CARTESIAN_POINT('Ctrl Pts',(10.9201323997384,-21.7409310548797,
12.));
#223365=CARTESIAN_POINT('Ctrl Pts',(10.9374082827444,-21.7560688175247,
12.));
#223366=CARTESIAN_POINT('Ctrl Pts',(10.9547911664455,-21.7712234908464,
12.));
#223367=CARTESIAN_POINT('Ctrl Pts',(10.9722807946155,-21.7863944097141,
12.));
#223368=CARTESIAN_POINT('Ctrl Pts',(10.9898769120912,-21.8015809157301,
12.));
#223369=CARTESIAN_POINT('Ctrl Pts',(11.0075792647477,-21.8167823571168,
12.));
#223370=CARTESIAN_POINT('Ctrl Pts',(11.0253875994598,-21.8319980886033,
12.));
#223371=CARTESIAN_POINT('Ctrl Pts',(11.0433016640807,-21.8472274713103,
12.));
#223372=CARTESIAN_POINT('Ctrl Pts',(11.0613212074363,-21.8624698726318,
12.));
#223373=CARTESIAN_POINT('Ctrl Pts',(11.0794459793057,-21.877724666119,12.));
#223374=CARTESIAN_POINT('Ctrl Pts',(11.0976757303944,-21.8929912313608,
12.));
#223375=CARTESIAN_POINT('Ctrl Pts',(11.1160102123024,-21.9082689538688,
12.));
#223376=CARTESIAN_POINT('Ctrl Pts',(11.1344491774741,-21.923557224952,12.));
#223377=CARTESIAN_POINT('Ctrl Pts',(11.1529923792003,-21.9388554416439,
12.));
#223378=CARTESIAN_POINT('Ctrl Pts',(11.1716395716376,-21.9541630066506,
12.));
#223379=CARTESIAN_POINT('Ctrl Pts',(11.190390509811,-21.9694793282914,12.));
#223380=CARTESIAN_POINT('Ctrl Pts',(11.2092449496125,-21.9848038204439,
12.));
#223381=CARTESIAN_POINT('Ctrl Pts',(11.2282026477896,-22.0001359024839,
12.));
#223382=CARTESIAN_POINT('Ctrl Pts',(11.2472633619275,-22.0154749992363,
12.));
#223383=CARTESIAN_POINT('Ctrl Pts',(11.2664268504206,-22.030820540835,12.));
#223384=CARTESIAN_POINT('Ctrl Pts',(11.2856928724374,-22.046171962566,12.));
#223385=CARTESIAN_POINT('Ctrl Pts',(11.3050611878771,-22.0615287047179,
12.));
#223386=CARTESIAN_POINT('Ctrl Pts',(11.3245315573168,-22.0768902124267,
12.));
#223387=CARTESIAN_POINT('Ctrl Pts',(11.3441037419553,-22.0922559355294,
12.));
#223388=CARTESIAN_POINT('Ctrl Pts',(11.3637775035367,-22.1076253283979,
12.));
#223389=CARTESIAN_POINT('Ctrl Pts',(11.3835526044256,-22.1229978500186,
12.));
#223390=CARTESIAN_POINT('Ctrl Pts',(11.4034288076908,-22.1383729640964,
12.));
#223391=CARTESIAN_POINT('Ctrl Pts',(11.4234058771742,-22.1537501391487,
12.));
#223392=CARTESIAN_POINT('Ctrl Pts',(11.443483577557,-22.1691288486096,12.));
#223393=CARTESIAN_POINT('Ctrl Pts',(11.463661674411,-22.184508570917,12.));
#223394=CARTESIAN_POINT('Ctrl Pts',(11.483939934259,-22.1998887896436,12.));
#223395=CARTESIAN_POINT('Ctrl Pts',(11.5043181244242,-22.2152689931022,
12.));
#223396=CARTESIAN_POINT('Ctrl Pts',(11.5247960128477,-22.2306486738901,
12.));
#223397=CARTESIAN_POINT('Ctrl Pts',(11.5453733679121,-22.2460273284654,
12.));
#223398=CARTESIAN_POINT('Ctrl Pts',(11.5660499582403,-22.2614044566898,
12.));
#223399=CARTESIAN_POINT('Ctrl Pts',(11.5868255525188,-22.2767795614348,
12.));
#223400=CARTESIAN_POINT('Ctrl Pts',(11.6076999192357,-22.2921521480356,
12.));
#223401=CARTESIAN_POINT('Ctrl Pts',(11.6286728270009,-22.3075217249049,
12.));
#223402=CARTESIAN_POINT('Ctrl Pts',(11.6497440449857,-22.3228878043976,
12.));
#223403=CARTESIAN_POINT('Ctrl Pts',(11.6709133432985,-22.3382499035619,
12.));
#223404=CARTESIAN_POINT('Ctrl Pts',(11.6921804934056,-22.3536075450029,
12.));
#223405=CARTESIAN_POINT('Ctrl Pts',(11.7135452684532,-22.3689602575491,
12.));
#223406=CARTESIAN_POINT('Ctrl Pts',(11.7350074437961,-22.3843075773899,
12.));
#223407=CARTESIAN_POINT('Ctrl Pts',(11.7565667964764,-22.3996490469191,
12.));
#223408=CARTESIAN_POINT('Ctrl Pts',(11.7782231042039,-22.4149842125008,
12.));
#223409=CARTESIAN_POINT('Ctrl Pts',(11.7999761445173,-22.430312622646,12.));
#223410=CARTESIAN_POINT('Ctrl Pts',(11.8218256937889,-22.4456338258735,
12.));
#223411=CARTESIAN_POINT('Ctrl Pts',(11.8437715264487,-22.4609473690472,
12.));
#223412=CARTESIAN_POINT('Ctrl Pts',(11.8658134137019,-22.4762527946702,
12.));
#223413=CARTESIAN_POINT('Ctrl Pts',(11.8879511239942,-22.4915496418485,
12.));
#223414=CARTESIAN_POINT('Ctrl Pts',(11.9101844254557,-22.5068374513973,
12.));
#223415=CARTESIAN_POINT('Ctrl Pts',(11.9325130877803,-22.5221157697883,
12.));
#223416=CARTESIAN_POINT('Ctrl Pts',(11.9549368843997,-22.5373841537307,
12.));
#223417=CARTESIAN_POINT('Ctrl Pts',(11.9774555943496,-22.5526421741158,
12.));
#223418=CARTESIAN_POINT('Ctrl Pts',(12.0000690046694,-22.5678894211181,
12.));
#223419=CARTESIAN_POINT('Ctrl Pts',(12.0227769113127,-22.5831255061282,
12.));
#223420=CARTESIAN_POINT('Ctrl Pts',(12.0455791139128,-22.5983500505644,
12.));
#223421=CARTESIAN_POINT('Ctrl Pts',(12.0684754113862,-22.6135626764898,
12.));
#223422=CARTESIAN_POINT('Ctrl Pts',(12.0914655972823,-22.6287629967056,
12.));
#223423=CARTESIAN_POINT('Ctrl Pts',(12.1145494550383,-22.6439506046605,
12.));
#223424=CARTESIAN_POINT('Ctrl Pts',(12.1377267537145,-22.6591250653965,
12.));
#223425=CARTESIAN_POINT('Ctrl Pts',(12.1609972423099,-22.6742859034944,
12.));
#223426=CARTESIAN_POINT('Ctrl Pts',(12.1843606579261,-22.6894326205037,
12.));
#223427=CARTESIAN_POINT('Ctrl Pts',(12.2078167360284,-22.7045647168747,
12.));
#223428=CARTESIAN_POINT('Ctrl Pts',(12.2313652198061,-22.7196817119374,
12.));
#223429=CARTESIAN_POINT('Ctrl Pts',(12.2550058702395,-22.7347831655287,
12.));
#223430=CARTESIAN_POINT('Ctrl Pts',(12.2787384750742,-22.7498686970069,
12.));
#223431=CARTESIAN_POINT('Ctrl Pts',(12.3025628601792,-22.764938010105,12.));
#223432=CARTESIAN_POINT('Ctrl Pts',(12.3264788926075,-22.7799908974768,
12.));
#223433=CARTESIAN_POINT('Ctrl Pts',(12.3504864740319,-22.795027221673,12.));
#223434=CARTESIAN_POINT('Ctrl Pts',(12.374585536673,-22.81004690224,12.));
#223435=CARTESIAN_POINT('Ctrl Pts',(12.3939379378998,-22.8220493007173,
12.));
#223436=CARTESIAN_POINT('Ctrl Pts',(12.4084933766346,-22.8310435872748,
12.));
#223437=CARTESIAN_POINT('Ctrl Pts',(12.418215285186,-22.8370364396459,12.));
#223438=CARTESIAN_POINT('Ctrl Pts',(12.4230808101438,-22.8400320311649,
12.));
#223439=CARTESIAN_POINT('Ctrl Pts',(7.52250298901263,-21.2610617890679,
0.));
#223440=CARTESIAN_POINT('Ctrl Pts',(7.52250298901263,-21.2610617890679,
12.));
#223441=CARTESIAN_POINT('Ctrl Pts',(7.52250649703969,-21.2610673466886,
0.));
#223442=CARTESIAN_POINT('Ctrl Pts',(7.52250649703969,-21.2610673466886,
12.));
#223443=CARTESIAN_POINT('Ctrl Pts',(7.52252744144903,-21.2611204474866,
0.));
#223444=CARTESIAN_POINT('Ctrl Pts',(7.52252744144903,-21.2611204474866,
12.));
#223445=CARTESIAN_POINT('Ctrl Pts',(7.5226006423166,-21.261326054066,0.));
#223446=CARTESIAN_POINT('Ctrl Pts',(7.5226006423166,-21.261326054066,12.));
#223447=CARTESIAN_POINT('Ctrl Pts',(7.52278182242669,-21.2618521283555,
0.));
#223448=CARTESIAN_POINT('Ctrl Pts',(7.52278182242669,-21.2618521283555,
12.));
#223449=CARTESIAN_POINT('Ctrl Pts',(7.52314642316199,-21.262927782038,0.));
#223450=CARTESIAN_POINT('Ctrl Pts',(7.52314642316199,-21.262927782038,12.));
#223451=CARTESIAN_POINT('Ctrl Pts',(7.52364573027552,-21.2644161259962,
0.));
#223452=CARTESIAN_POINT('Ctrl Pts',(7.52364573027552,-21.2644161259962,
12.));
#223453=CARTESIAN_POINT('Ctrl Pts',(7.52427261074297,-21.2663059157058,
0.));
#223454=CARTESIAN_POINT('Ctrl Pts',(7.52427261074297,-21.2663059157058,
12.));
#223455=CARTESIAN_POINT('Ctrl Pts',(7.5250177033353,-21.2685823838671,0.));
#223456=CARTESIAN_POINT('Ctrl Pts',(7.5250177033353,-21.2685823838671,12.));
#223457=CARTESIAN_POINT('Ctrl Pts',(7.52587126095529,-21.2712301573466,
0.));
#223458=CARTESIAN_POINT('Ctrl Pts',(7.52587126095529,-21.2712301573466,
12.));
#223459=CARTESIAN_POINT('Ctrl Pts',(7.5268252691854,-21.2742366113579,0.));
#223460=CARTESIAN_POINT('Ctrl Pts',(7.5268252691854,-21.2742366113579,12.));
#223461=CARTESIAN_POINT('Ctrl Pts',(7.52787386225332,-21.2775925269652,
0.));
#223462=CARTESIAN_POINT('Ctrl Pts',(7.52787386225332,-21.2775925269652,
12.));
#223463=CARTESIAN_POINT('Ctrl Pts',(7.52901217930407,-21.2812902781143,
0.));
#223464=CARTESIAN_POINT('Ctrl Pts',(7.52901217930407,-21.2812902781143,
12.));
#223465=CARTESIAN_POINT('Ctrl Pts',(7.53023562438229,-21.2853226580657,
0.));
#223466=CARTESIAN_POINT('Ctrl Pts',(7.53023562438229,-21.2853226580657,
12.));
#223467=CARTESIAN_POINT('Ctrl Pts',(7.53153906987855,-21.2896816163842,
0.));
#223468=CARTESIAN_POINT('Ctrl Pts',(7.53153906987855,-21.2896816163842,
12.));
#223469=CARTESIAN_POINT('Ctrl Pts',(7.53291726078526,-21.2943588989331,
0.));
#223470=CARTESIAN_POINT('Ctrl Pts',(7.53291726078526,-21.2943588989331,
12.));
#223471=CARTESIAN_POINT('Ctrl Pts',(7.53436505309942,-21.2993464250717,
0.));
#223472=CARTESIAN_POINT('Ctrl Pts',(7.53436505309942,-21.2993464250717,
12.));
#223473=CARTESIAN_POINT('Ctrl Pts',(7.53587778251735,-21.3046368712157,
0.));
#223474=CARTESIAN_POINT('Ctrl Pts',(7.53587778251735,-21.3046368712157,
12.));
#223475=CARTESIAN_POINT('Ctrl Pts',(7.53745129364615,-21.310223716773,0.));
#223476=CARTESIAN_POINT('Ctrl Pts',(7.53745129364615,-21.310223716773,12.));
#223477=CARTESIAN_POINT('Ctrl Pts',(7.53908175169898,-21.3161009456256,
0.));
#223478=CARTESIAN_POINT('Ctrl Pts',(7.53908175169898,-21.3161009456256,
12.));
#223479=CARTESIAN_POINT('Ctrl Pts',(7.54076552038278,-21.3222628524165,
0.));
#223480=CARTESIAN_POINT('Ctrl Pts',(7.54076552038278,-21.3222628524165,
12.));
#223481=CARTESIAN_POINT('Ctrl Pts',(7.5424990037703,-21.328703791771,0.));
#223482=CARTESIAN_POINT('Ctrl Pts',(7.5424990037703,-21.328703791771,12.));
#223483=CARTESIAN_POINT('Ctrl Pts',(7.54427868151267,-21.3354182340149,
0.));
#223484=CARTESIAN_POINT('Ctrl Pts',(7.54427868151267,-21.3354182340149,
12.));
#223485=CARTESIAN_POINT('Ctrl Pts',(7.54610114948346,-21.3424008295038,
0.));
#223486=CARTESIAN_POINT('Ctrl Pts',(7.54610114948346,-21.3424008295038,
12.));
#223487=CARTESIAN_POINT('Ctrl Pts',(7.5479631624633,-21.3496464761531,0.));
#223488=CARTESIAN_POINT('Ctrl Pts',(7.5479631624633,-21.3496464761531,12.));
#223489=CARTESIAN_POINT('Ctrl Pts',(7.54986166521309,-21.3571503685855,
0.));
#223490=CARTESIAN_POINT('Ctrl Pts',(7.54986166521309,-21.3571503685855,
12.));
#223491=CARTESIAN_POINT('Ctrl Pts',(7.55179375777443,-21.3649079431865,
0.));
#223492=CARTESIAN_POINT('Ctrl Pts',(7.55179375777443,-21.3649079431865,
12.));
#223493=CARTESIAN_POINT('Ctrl Pts',(7.55375667080028,-21.3729148390243,
0.));
#223494=CARTESIAN_POINT('Ctrl Pts',(7.55375667080028,-21.3729148390243,
12.));
#223495=CARTESIAN_POINT('Ctrl Pts',(7.55574773403502,-21.3811668478932,
0.));
#223496=CARTESIAN_POINT('Ctrl Pts',(7.55574773403502,-21.3811668478932,
12.));
#223497=CARTESIAN_POINT('Ctrl Pts',(7.55776435731416,-21.3896598842117,
0.));
#223498=CARTESIAN_POINT('Ctrl Pts',(7.55776435731416,-21.3896598842117,
12.));
#223499=CARTESIAN_POINT('Ctrl Pts',(7.5598040370061,-21.3983899952987,0.));
#223500=CARTESIAN_POINT('Ctrl Pts',(7.5598040370061,-21.3983899952987,12.));
#223501=CARTESIAN_POINT('Ctrl Pts',(7.56186435703621,-21.4073533630365,
0.));
#223502=CARTESIAN_POINT('Ctrl Pts',(7.56186435703621,-21.4073533630365,
12.));
#223503=CARTESIAN_POINT('Ctrl Pts',(7.56394299313684,-21.4165463106254,
0.));
#223504=CARTESIAN_POINT('Ctrl Pts',(7.56394299313684,-21.4165463106254,
12.));
#223505=CARTESIAN_POINT('Ctrl Pts',(7.56603771218711,-21.4259653015736,
0.));
#223506=CARTESIAN_POINT('Ctrl Pts',(7.56603771218711,-21.4259653015736,
12.));
#223507=CARTESIAN_POINT('Ctrl Pts',(7.56814636360847,-21.4356069261513,
0.));
#223508=CARTESIAN_POINT('Ctrl Pts',(7.56814636360847,-21.4356069261513,
12.));
#223509=CARTESIAN_POINT('Ctrl Pts',(7.57026687261165,-21.4454678907509,
0.));
#223510=CARTESIAN_POINT('Ctrl Pts',(7.57026687261165,-21.4454678907509,
12.));
#223511=CARTESIAN_POINT('Ctrl Pts',(7.57239723223505,-21.4555450053142,
0.));
#223512=CARTESIAN_POINT('Ctrl Pts',(7.57239723223505,-21.4555450053142,
12.));
#223513=CARTESIAN_POINT('Ctrl Pts',(7.57453549743411,-21.4658351740128,
0.));
#223514=CARTESIAN_POINT('Ctrl Pts',(7.57453549743411,-21.4658351740128,
12.));
#223515=CARTESIAN_POINT('Ctrl Pts',(7.57667978402986,-21.4763353936762,
0.));
#223516=CARTESIAN_POINT('Ctrl Pts',(7.57667978402986,-21.4763353936762,
12.));
#223517=CARTESIAN_POINT('Ctrl Pts',(7.57882826679131,-21.4870427508194,
0.));
#223518=CARTESIAN_POINT('Ctrl Pts',(7.57882826679131,-21.4870427508194,
12.));
#223519=CARTESIAN_POINT('Ctrl Pts',(7.58097917790743,-21.4979544192744,
0.));
#223520=CARTESIAN_POINT('Ctrl Pts',(7.58097917790743,-21.4979544192744,
12.));
#223521=CARTESIAN_POINT('Ctrl Pts',(7.58313080519179,-21.5090676573873,
0.));
#223522=CARTESIAN_POINT('Ctrl Pts',(7.58313080519179,-21.5090676573873,
12.));
#223523=CARTESIAN_POINT('Ctrl Pts',(7.58528148919129,-21.5203798035299,
0.));
#223524=CARTESIAN_POINT('Ctrl Pts',(7.58528148919129,-21.5203798035299,
12.));
#223525=CARTESIAN_POINT('Ctrl Pts',(7.58742962034833,-21.5318882716736,
0.));
#223526=CARTESIAN_POINT('Ctrl Pts',(7.58742962034833,-21.5318882716736,
12.));
#223527=CARTESIAN_POINT('Ctrl Pts',(7.58957363620013,-21.543590547011,0.));
#223528=CARTESIAN_POINT('Ctrl Pts',(7.58957363620013,-21.543590547011,12.));
#223529=CARTESIAN_POINT('Ctrl Pts',(7.59171201844776,-21.5554841813462,
0.));
#223530=CARTESIAN_POINT('Ctrl Pts',(7.59171201844776,-21.5554841813462,
12.));
#223531=CARTESIAN_POINT('Ctrl Pts',(7.59384329124918,-21.5675667904726,
0.));
#223532=CARTESIAN_POINT('Ctrl Pts',(7.59384329124918,-21.5675667904726,
12.));
#223533=CARTESIAN_POINT('Ctrl Pts',(7.59596601973583,-21.5798360518978,
0.));
#223534=CARTESIAN_POINT('Ctrl Pts',(7.59596601973583,-21.5798360518978,
12.));
#223535=CARTESIAN_POINT('Ctrl Pts',(7.59807880846194,-21.5922897024466,
0.));
#223536=CARTESIAN_POINT('Ctrl Pts',(7.59807880846194,-21.5922897024466,
12.));
#223537=CARTESIAN_POINT('Ctrl Pts',(7.6001802998824,-21.6049255358843,0.));
#223538=CARTESIAN_POINT('Ctrl Pts',(7.6001802998824,-21.6049255358843,12.));
#223539=CARTESIAN_POINT('Ctrl Pts',(7.60226917285428,-21.617741400599,0.));
#223540=CARTESIAN_POINT('Ctrl Pts',(7.60226917285428,-21.617741400599,12.));
#223541=CARTESIAN_POINT('Ctrl Pts',(7.60434414118295,-21.6307351973822,
0.));
#223542=CARTESIAN_POINT('Ctrl Pts',(7.60434414118295,-21.6307351973822,
12.));
#223543=CARTESIAN_POINT('Ctrl Pts',(7.60640395216356,-21.6439048771743,
0.));
#223544=CARTESIAN_POINT('Ctrl Pts',(7.60640395216356,-21.6439048771743,
12.));
#223545=CARTESIAN_POINT('Ctrl Pts',(7.60844738512873,-21.6572484388081,
0.));
#223546=CARTESIAN_POINT('Ctrl Pts',(7.60844738512873,-21.6572484388081,
12.));
#223547=CARTESIAN_POINT('Ctrl Pts',(7.61047325000955,-21.6707639267576,
0.));
#223548=CARTESIAN_POINT('Ctrl Pts',(7.61047325000955,-21.6707639267576,
12.));
#223549=CARTESIAN_POINT('Ctrl Pts',(7.61248038630268,-21.6844494295815,
0.));
#223550=CARTESIAN_POINT('Ctrl Pts',(7.61248038630268,-21.6844494295815,
12.));
#223551=CARTESIAN_POINT('Ctrl Pts',(7.61446766202786,-21.6983030783322,
0.));
#223552=CARTESIAN_POINT('Ctrl Pts',(7.61446766202786,-21.6983030783322,
12.));
#223553=CARTESIAN_POINT('Ctrl Pts',(7.6164339727042,-21.7123230449834,0.));
#223554=CARTESIAN_POINT('Ctrl Pts',(7.6164339727042,-21.7123230449834,12.));
#223555=CARTESIAN_POINT('Ctrl Pts',(7.61837824030537,-21.7265075407975,
0.));
#223556=CARTESIAN_POINT('Ctrl Pts',(7.61837824030537,-21.7265075407975,
12.));
#223557=CARTESIAN_POINT('Ctrl Pts',(7.62029941230854,-21.7408548148656,
0.));
#223558=CARTESIAN_POINT('Ctrl Pts',(7.62029941230854,-21.7408548148656,
12.));
#223559=CARTESIAN_POINT('Ctrl Pts',(7.62219646084228,-21.7553631528328,
0.));
#223560=CARTESIAN_POINT('Ctrl Pts',(7.62219646084228,-21.7553631528328,
12.));
#223561=CARTESIAN_POINT('Ctrl Pts',(7.62406838181165,-21.7700308755584,
0.));
#223562=CARTESIAN_POINT('Ctrl Pts',(7.62406838181165,-21.7700308755584,
12.));
#223563=CARTESIAN_POINT('Ctrl Pts',(7.62591419404512,-21.7848563378021,
0.));
#223564=CARTESIAN_POINT('Ctrl Pts',(7.62591419404512,-21.7848563378021,
12.));
#223565=CARTESIAN_POINT('Ctrl Pts',(7.62773293842388,-21.799837926858,0.));
#223566=CARTESIAN_POINT('Ctrl Pts',(7.62773293842388,-21.799837926858,12.));
#223567=CARTESIAN_POINT('Ctrl Pts',(7.62952367718126,-21.814974061509,0.));
#223568=CARTESIAN_POINT('Ctrl Pts',(7.62952367718126,-21.814974061509,12.));
#223569=CARTESIAN_POINT('Ctrl Pts',(7.63128549323022,-21.8302631910195,
0.));
#223570=CARTESIAN_POINT('Ctrl Pts',(7.63128549323022,-21.8302631910195,
12.));
#223571=CARTESIAN_POINT('Ctrl Pts',(7.63301748948935,-21.8457037941084,
0.));
#223572=CARTESIAN_POINT('Ctrl Pts',(7.63301748948935,-21.8457037941084,
12.));
#223573=CARTESIAN_POINT('Ctrl Pts',(7.63471878821225,-21.8612943779089,
0.));
#223574=CARTESIAN_POINT('Ctrl Pts',(7.63471878821225,-21.8612943779089,
12.));
#223575=CARTESIAN_POINT('Ctrl Pts',(7.63638853033399,-21.8770334769496,
0.));
#223576=CARTESIAN_POINT('Ctrl Pts',(7.63638853033399,-21.8770334769496,
12.));
#223577=CARTESIAN_POINT('Ctrl Pts',(7.63802587492034,-21.8929196523514,
0.));
#223578=CARTESIAN_POINT('Ctrl Pts',(7.63802587492034,-21.8929196523514,
12.));
#223579=CARTESIAN_POINT('Ctrl Pts',(7.63962999860926,-21.9089514909874,
0.));
#223580=CARTESIAN_POINT('Ctrl Pts',(7.63962999860926,-21.9089514909874,
12.));
#223581=CARTESIAN_POINT('Ctrl Pts',(7.64120009506531,-21.9251276046546,
0.));
#223582=CARTESIAN_POINT('Ctrl Pts',(7.64120009506531,-21.9251276046546,
12.));
#223583=CARTESIAN_POINT('Ctrl Pts',(7.64273537442681,-21.9414466292072,
0.));
#223584=CARTESIAN_POINT('Ctrl Pts',(7.64273537442681,-21.9414466292072,
12.));
#223585=CARTESIAN_POINT('Ctrl Pts',(7.64423506279122,-21.9579072237651,
0.));
#223586=CARTESIAN_POINT('Ctrl Pts',(7.64423506279122,-21.9579072237651,
12.));
#223587=CARTESIAN_POINT('Ctrl Pts',(7.64569840177335,-21.9745080700798,
0.));
#223588=CARTESIAN_POINT('Ctrl Pts',(7.64569840177335,-21.9745080700798,
12.));
#223589=CARTESIAN_POINT('Ctrl Pts',(7.64712464805249,-21.9912478718542,
0.));
#223590=CARTESIAN_POINT('Ctrl Pts',(7.64712464805249,-21.9912478718542,
12.));
#223591=CARTESIAN_POINT('Ctrl Pts',(7.64851307293351,-22.0081253540774,
0.));
#223592=CARTESIAN_POINT('Ctrl Pts',(7.64851307293351,-22.0081253540774,
12.));
#223593=CARTESIAN_POINT('Ctrl Pts',(7.64986296190168,-22.0251392623209,
0.));
#223594=CARTESIAN_POINT('Ctrl Pts',(7.64986296190168,-22.0251392623209,
12.));
#223595=CARTESIAN_POINT('Ctrl Pts',(7.65117361421358,-22.0422883621174,
0.));
#223596=CARTESIAN_POINT('Ctrl Pts',(7.65117361421358,-22.0422883621174,
12.));
#223597=CARTESIAN_POINT('Ctrl Pts',(7.65244434253112,-22.0595714384431,
0.));
#223598=CARTESIAN_POINT('Ctrl Pts',(7.65244434253112,-22.0595714384431,
12.));
#223599=CARTESIAN_POINT('Ctrl Pts',(7.65367447254949,-22.0769872951596,
0.));
#223600=CARTESIAN_POINT('Ctrl Pts',(7.65367447254949,-22.0769872951596,
12.));
#223601=CARTESIAN_POINT('Ctrl Pts',(7.65486334263643,-22.094534754469,0.));
#223602=CARTESIAN_POINT('Ctrl Pts',(7.65486334263643,-22.094534754469,12.));
#223603=CARTESIAN_POINT('Ctrl Pts',(7.65601030346806,-22.1122126563329,
0.));
#223604=CARTESIAN_POINT('Ctrl Pts',(7.65601030346806,-22.1122126563329,
12.));
#223605=CARTESIAN_POINT('Ctrl Pts',(7.65711471769396,-22.1300198579675,
0.));
#223606=CARTESIAN_POINT('Ctrl Pts',(7.65711471769396,-22.1300198579675,
12.));
#223607=CARTESIAN_POINT('Ctrl Pts',(7.65817595963348,-22.1479552334211,
0.));
#223608=CARTESIAN_POINT('Ctrl Pts',(7.65817595963348,-22.1479552334211,
12.));
#223609=CARTESIAN_POINT('Ctrl Pts',(7.6591934149693,-22.1660176731178,0.));
#223610=CARTESIAN_POINT('Ctrl Pts',(7.6591934149693,-22.1660176731178,12.));
#223611=CARTESIAN_POINT('Ctrl Pts',(7.66016648045004,-22.1842060834091,
0.));
#223612=CARTESIAN_POINT('Ctrl Pts',(7.66016648045004,-22.1842060834091,
12.));
#223613=CARTESIAN_POINT('Ctrl Pts',(7.6610945635927,-22.2025193860964,0.));
#223614=CARTESIAN_POINT('Ctrl Pts',(7.6610945635927,-22.2025193860964,12.));
#223615=CARTESIAN_POINT('Ctrl Pts',(7.66197708240399,-22.2209565180085,
0.));
#223616=CARTESIAN_POINT('Ctrl Pts',(7.66197708240399,-22.2209565180085,
12.));
#223617=CARTESIAN_POINT('Ctrl Pts',(7.66281346512508,-22.2395164306547,
0.));
#223618=CARTESIAN_POINT('Ctrl Pts',(7.66281346512508,-22.2395164306547,
12.));
#223619=CARTESIAN_POINT('Ctrl Pts',(7.6636031499764,-22.258198089848,0.));
#223620=CARTESIAN_POINT('Ctrl Pts',(7.6636031499764,-22.258198089848,12.));
#223621=CARTESIAN_POINT('Ctrl Pts',(7.66434558490978,-22.2770004753335,
0.));
#223622=CARTESIAN_POINT('Ctrl Pts',(7.66434558490978,-22.2770004753335,
12.));
#223623=CARTESIAN_POINT('Ctrl Pts',(7.66504022736298,-22.2959225803937,
0.));
#223624=CARTESIAN_POINT('Ctrl Pts',(7.66504022736298,-22.2959225803937,
12.));
#223625=CARTESIAN_POINT('Ctrl Pts',(7.66568654402493,-22.314963411484,0.));
#223626=CARTESIAN_POINT('Ctrl Pts',(7.66568654402493,-22.314963411484,12.));
#223627=CARTESIAN_POINT('Ctrl Pts',(7.66628401061951,-22.3341219879469,
0.));
#223628=CARTESIAN_POINT('Ctrl Pts',(7.66628401061951,-22.3341219879469,
12.));
#223629=CARTESIAN_POINT('Ctrl Pts',(7.66683211169157,-22.3533973417021,
0.));
#223630=CARTESIAN_POINT('Ctrl Pts',(7.66683211169157,-22.3533973417021,
12.));
#223631=CARTESIAN_POINT('Ctrl Pts',(7.66733034039882,-22.372788516936,0.));
#223632=CARTESIAN_POINT('Ctrl Pts',(7.66733034039882,-22.372788516936,12.));
#223633=CARTESIAN_POINT('Ctrl Pts',(7.66777819830789,-22.3922945697773,
0.));
#223634=CARTESIAN_POINT('Ctrl Pts',(7.66777819830789,-22.3922945697773,
12.));
#223635=CARTESIAN_POINT('Ctrl Pts',(7.66817519519639,-22.4119145679758,
0.));
#223636=CARTESIAN_POINT('Ctrl Pts',(7.66817519519639,-22.4119145679758,
12.));
#223637=CARTESIAN_POINT('Ctrl Pts',(7.66852084886703,-22.4316475906603,
0.));
#223638=CARTESIAN_POINT('Ctrl Pts',(7.66852084886703,-22.4316475906603,
12.));
#223639=CARTESIAN_POINT('Ctrl Pts',(7.66881468496634,-22.4514927280855,
0.));
#223640=CARTESIAN_POINT('Ctrl Pts',(7.66881468496634,-22.4514927280855,
12.));
#223641=CARTESIAN_POINT('Ctrl Pts',(7.6690562368083,-22.47144908137,0.));
#223642=CARTESIAN_POINT('Ctrl Pts',(7.6690562368083,-22.47144908137,12.));
#223643=CARTESIAN_POINT('Ctrl Pts',(7.66924504520314,-22.4915157622312,
0.));
#223644=CARTESIAN_POINT('Ctrl Pts',(7.66924504520314,-22.4915157622312,
12.));
#223645=CARTESIAN_POINT('Ctrl Pts',(7.66938065829107,-22.5116918927032,
0.));
#223646=CARTESIAN_POINT('Ctrl Pts',(7.66938065829107,-22.5116918927032,
12.));
#223647=CARTESIAN_POINT('Ctrl Pts',(7.66946263138143,-22.53197660492,0.));
#223648=CARTESIAN_POINT('Ctrl Pts',(7.66946263138143,-22.53197660492,12.));
#223649=CARTESIAN_POINT('Ctrl Pts',(7.66949052679692,-22.5523690409116,
0.));
#223650=CARTESIAN_POINT('Ctrl Pts',(7.66949052679692,-22.5523690409116,
12.));
#223651=CARTESIAN_POINT('Ctrl Pts',(7.66946391372305,-22.5728683523831,
0.));
#223652=CARTESIAN_POINT('Ctrl Pts',(7.66946391372305,-22.5728683523831,
12.));
#223653=CARTESIAN_POINT('Ctrl Pts',(7.66938236806232,-22.5934737004953,
0.));
#223654=CARTESIAN_POINT('Ctrl Pts',(7.66938236806232,-22.5934737004953,
12.));
#223655=CARTESIAN_POINT('Ctrl Pts',(7.66924547229413,-22.6141842556243,
0.));
#223656=CARTESIAN_POINT('Ctrl Pts',(7.66924547229413,-22.6141842556243,
12.));
#223657=CARTESIAN_POINT('Ctrl Pts',(7.66905281533714,-22.6349991971541,
0.));
#223658=CARTESIAN_POINT('Ctrl Pts',(7.66905281533714,-22.6349991971541,
12.));
#223659=CARTESIAN_POINT('Ctrl Pts',(7.66880399241322,-22.6559177133127,
0.));
#223660=CARTESIAN_POINT('Ctrl Pts',(7.66880399241322,-22.6559177133127,
12.));
#223661=CARTESIAN_POINT('Ctrl Pts',(7.66849860491742,-22.6769390009885,
0.));
#223662=CARTESIAN_POINT('Ctrl Pts',(7.66849860491742,-22.6769390009885,
12.));
#223663=CARTESIAN_POINT('Ctrl Pts',(7.66813626029274,-22.6980622655446,
0.));
#223664=CARTESIAN_POINT('Ctrl Pts',(7.66813626029274,-22.6980622655446,
12.));
#223665=CARTESIAN_POINT('Ctrl Pts',(7.66771657191027,-22.7192867206245,
0.));
#223666=CARTESIAN_POINT('Ctrl Pts',(7.66771657191027,-22.7192867206245,
12.));
#223667=CARTESIAN_POINT('Ctrl Pts',(7.66723915895439,-22.7406115879513,
0.));
#223668=CARTESIAN_POINT('Ctrl Pts',(7.66723915895439,-22.7406115879513,
12.));
#223669=CARTESIAN_POINT('Ctrl Pts',(7.66670364630298,-22.7620360971843,
0.));
#223670=CARTESIAN_POINT('Ctrl Pts',(7.66670364630298,-22.7620360971843,
12.));
#223671=CARTESIAN_POINT('Ctrl Pts',(7.66610966441272,-22.7835594857699,
0.));
#223672=CARTESIAN_POINT('Ctrl Pts',(7.66610966441272,-22.7835594857699,
12.));
#223673=CARTESIAN_POINT('Ctrl Pts',(7.66545684920986,-22.8051809987833,
0.));
#223674=CARTESIAN_POINT('Ctrl Pts',(7.66545684920986,-22.8051809987833,
12.));
#223675=CARTESIAN_POINT('Ctrl Pts',(7.66474484198548,-22.8268998887678,
0.));
#223676=CARTESIAN_POINT('Ctrl Pts',(7.66474484198548,-22.8268998887678,
12.));
#223677=CARTESIAN_POINT('Ctrl Pts',(7.66397328929802,-22.848715415557,0.));
#223678=CARTESIAN_POINT('Ctrl Pts',(7.66397328929802,-22.848715415557,12.));
#223679=CARTESIAN_POINT('Ctrl Pts',(7.66314184287336,-22.8706268461283,
0.));
#223680=CARTESIAN_POINT('Ctrl Pts',(7.66314184287336,-22.8706268461283,
12.));
#223681=CARTESIAN_POINT('Ctrl Pts',(7.66225015950155,-22.8926334544883,
0.));
#223682=CARTESIAN_POINT('Ctrl Pts',(7.66225015950155,-22.8926334544883,
12.));
#223683=CARTESIAN_POINT('Ctrl Pts',(7.66129790094107,-22.9147345215421,
0.));
#223684=CARTESIAN_POINT('Ctrl Pts',(7.66129790094107,-22.9147345215421,
12.));
#223685=CARTESIAN_POINT('Ctrl Pts',(7.66028473382777,-22.9369293349593,
0.));
#223686=CARTESIAN_POINT('Ctrl Pts',(7.66028473382777,-22.9369293349593,
12.));
#223687=CARTESIAN_POINT('Ctrl Pts',(7.65921032958901,-22.959217189033,0.));
#223688=CARTESIAN_POINT('Ctrl Pts',(7.65921032958901,-22.959217189033,12.));
#223689=CARTESIAN_POINT('Ctrl Pts',(7.65807436436431,-22.9815973845296,
0.));
#223690=CARTESIAN_POINT('Ctrl Pts',(7.65807436436431,-22.9815973845296,
12.));
#223691=CARTESIAN_POINT('Ctrl Pts',(7.65687651891303,-23.0040692285814,
0.));
#223692=CARTESIAN_POINT('Ctrl Pts',(7.65687651891303,-23.0040692285814,
12.));
#223693=CARTESIAN_POINT('Ctrl Pts',(7.65561647852533,-23.0266320345787,
0.));
#223694=CARTESIAN_POINT('Ctrl Pts',(7.65561647852533,-23.0266320345787,
12.));
#223695=CARTESIAN_POINT('Ctrl Pts',(7.65429393293945,-23.0492851220528,
0.));
#223696=CARTESIAN_POINT('Ctrl Pts',(7.65429393293945,-23.0492851220528,
12.));
#223697=CARTESIAN_POINT('Ctrl Pts',(7.65290857626357,-23.072027816555,0.));
#223698=CARTESIAN_POINT('Ctrl Pts',(7.65290857626357,-23.072027816555,12.));
#223699=CARTESIAN_POINT('Ctrl Pts',(7.65146010690475,-23.094859449525,0.));
#223700=CARTESIAN_POINT('Ctrl Pts',(7.65146010690475,-23.094859449525,12.));
#223701=CARTESIAN_POINT('Ctrl Pts',(7.64994822749859,-23.1177793581679,
0.));
#223702=CARTESIAN_POINT('Ctrl Pts',(7.64994822749859,-23.1177793581679,
12.));
#223703=CARTESIAN_POINT('Ctrl Pts',(7.64837264482942,-23.1407868853819,
0.));
#223704=CARTESIAN_POINT('Ctrl Pts',(7.64837264482942,-23.1407868853819,
12.));
#223705=CARTESIAN_POINT('Ctrl Pts',(7.64673306975804,-23.1638813796694,
0.));
#223706=CARTESIAN_POINT('Ctrl Pts',(7.64673306975804,-23.1638813796694,
12.));
#223707=CARTESIAN_POINT('Ctrl Pts',(7.64502921715482,-23.1870621950452,
0.));
#223708=CARTESIAN_POINT('Ctrl Pts',(7.64502921715482,-23.1870621950452,
12.));
#223709=CARTESIAN_POINT('Ctrl Pts',(7.64326080583679,-23.2103286909398,
0.));
#223710=CARTESIAN_POINT('Ctrl Pts',(7.64326080583679,-23.2103286909398,
12.));
#223711=CARTESIAN_POINT('Ctrl Pts',(7.64142755851504,-23.2336802320912,
0.));
#223712=CARTESIAN_POINT('Ctrl Pts',(7.64142755851504,-23.2336802320912,
12.));
#223713=CARTESIAN_POINT('Ctrl Pts',(7.63952920172834,-23.2571161884488,
0.));
#223714=CARTESIAN_POINT('Ctrl Pts',(7.63952920172834,-23.2571161884488,
12.));
#223715=CARTESIAN_POINT('Ctrl Pts',(7.63756546576373,-23.2806359350855,
0.));
#223716=CARTESIAN_POINT('Ctrl Pts',(7.63756546576373,-23.2806359350855,
12.));
#223717=CARTESIAN_POINT('Ctrl Pts',(7.63553608458782,-23.3042388521022,
0.));
#223718=CARTESIAN_POINT('Ctrl Pts',(7.63553608458782,-23.3042388521022,
12.));
#223719=CARTESIAN_POINT('Ctrl Pts',(7.63344079578161,-23.3279243245241,
0.));
#223720=CARTESIAN_POINT('Ctrl Pts',(7.63344079578161,-23.3279243245241,
12.));
#223721=CARTESIAN_POINT('Ctrl Pts',(7.63127934048136,-23.3516917421972,
0.));
#223722=CARTESIAN_POINT('Ctrl Pts',(7.63127934048136,-23.3516917421972,
12.));
#223723=CARTESIAN_POINT('Ctrl Pts',(7.62905146332592,-23.3755404996636,
0.));
#223724=CARTESIAN_POINT('Ctrl Pts',(7.62905146332592,-23.3755404996636,
12.));
#223725=CARTESIAN_POINT('Ctrl Pts',(7.62675691240328,-23.399469996112,0.));
#223726=CARTESIAN_POINT('Ctrl Pts',(7.62675691240328,-23.399469996112,12.));
#223727=CARTESIAN_POINT('Ctrl Pts',(7.62439543920049,-23.4234796353542,
0.));
#223728=CARTESIAN_POINT('Ctrl Pts',(7.62439543920049,-23.4234796353542,
12.));
#223729=CARTESIAN_POINT('Ctrl Pts',(7.62196679855954,-23.4475688257854,
0.));
#223730=CARTESIAN_POINT('Ctrl Pts',(7.62196679855954,-23.4475688257854,
12.));
#223731=CARTESIAN_POINT('Ctrl Pts',(7.61947074863976,-23.4717369803438,
0.));
#223732=CARTESIAN_POINT('Ctrl Pts',(7.61947074863976,-23.4717369803438,
12.));
#223733=CARTESIAN_POINT('Ctrl Pts',(7.61690705088318,-23.4959835164609,
0.));
#223734=CARTESIAN_POINT('Ctrl Pts',(7.61690705088318,-23.4959835164609,
12.));
#223735=CARTESIAN_POINT('Ctrl Pts',(7.61427546999297,-23.5203078560129,
0.));
#223736=CARTESIAN_POINT('Ctrl Pts',(7.61427546999297,-23.5203078560129,
12.));
#223737=CARTESIAN_POINT('Ctrl Pts',(7.61157577385371,-23.544709425203,0.));
#223738=CARTESIAN_POINT('Ctrl Pts',(7.61157577385371,-23.544709425203,12.));
#223739=CARTESIAN_POINT('Ctrl Pts',(7.60880773344599,-23.5691876544244,
0.));
#223740=CARTESIAN_POINT('Ctrl Pts',(7.60880773344599,-23.5691876544244,
12.));
#223741=CARTESIAN_POINT('Ctrl Pts',(7.60597112277093,-23.5937419781245,
0.));
#223742=CARTESIAN_POINT('Ctrl Pts',(7.60597112277093,-23.5937419781245,
12.));
#223743=CARTESIAN_POINT('Ctrl Pts',(7.60306571877805,-23.6183718346576,
0.));
#223744=CARTESIAN_POINT('Ctrl Pts',(7.60306571877805,-23.6183718346576,
12.));
#223745=CARTESIAN_POINT('Ctrl Pts',(7.60009130130125,-23.6430766661418,
0.));
#223746=CARTESIAN_POINT('Ctrl Pts',(7.60009130130125,-23.6430766661418,
12.));
#223747=CARTESIAN_POINT('Ctrl Pts',(7.59704765299566,-23.6678559182875,
0.));
#223748=CARTESIAN_POINT('Ctrl Pts',(7.59704765299566,-23.6678559182875,
12.));
#223749=CARTESIAN_POINT('Ctrl Pts',(7.59393455934034,-23.6927090405066,
0.));
#223750=CARTESIAN_POINT('Ctrl Pts',(7.59393455934034,-23.6927090405066,
12.));
#223751=CARTESIAN_POINT('Ctrl Pts',(7.5907518086532,-23.7176354860457,0.));
#223752=CARTESIAN_POINT('Ctrl Pts',(7.5907518086532,-23.7176354860457,12.));
#223753=CARTESIAN_POINT('Ctrl Pts',(7.58749919210825,-23.7426347121006,
0.));
#223754=CARTESIAN_POINT('Ctrl Pts',(7.58749919210825,-23.7426347121006,
12.));
#223755=CARTESIAN_POINT('Ctrl Pts',(7.5841765037627,-23.7677061799376,0.));
#223756=CARTESIAN_POINT('Ctrl Pts',(7.5841765037627,-23.7677061799376,12.));
#223757=CARTESIAN_POINT('Ctrl Pts',(7.58078354058212,-23.7928493549908,
0.));
#223758=CARTESIAN_POINT('Ctrl Pts',(7.58078354058212,-23.7928493549908,
12.));
#223759=CARTESIAN_POINT('Ctrl Pts',(7.57732010249065,-23.8180637069976,
0.));
#223760=CARTESIAN_POINT('Ctrl Pts',(7.57732010249065,-23.8180637069976,
12.));
#223761=CARTESIAN_POINT('Ctrl Pts',(7.57378599219813,-23.8433487096132,
0.));
#223762=CARTESIAN_POINT('Ctrl Pts',(7.57378599219813,-23.8433487096132,
12.));
#223763=CARTESIAN_POINT('Ctrl Pts',(7.57018101500708,-23.8687038399595,
0.));
#223764=CARTESIAN_POINT('Ctrl Pts',(7.57018101500708,-23.8687038399595,
12.));
#223765=CARTESIAN_POINT('Ctrl Pts',(7.5665049786379,-23.8941285782002,0.));
#223766=CARTESIAN_POINT('Ctrl Pts',(7.5665049786379,-23.8941285782002,12.));
#223767=CARTESIAN_POINT('Ctrl Pts',(7.56275769304772,-23.9196224070759,
0.));
#223768=CARTESIAN_POINT('Ctrl Pts',(7.56275769304772,-23.9196224070759,
12.));
#223769=CARTESIAN_POINT('Ctrl Pts',(7.55893897027679,-23.9451848115002,
0.));
#223770=CARTESIAN_POINT('Ctrl Pts',(7.55893897027679,-23.9451848115002,
12.));
#223771=CARTESIAN_POINT('Ctrl Pts',(7.55504862424807,-23.9708152779886,
0.));
#223772=CARTESIAN_POINT('Ctrl Pts',(7.55504862424807,-23.9708152779886,
12.));
#223773=CARTESIAN_POINT('Ctrl Pts',(7.55108647097431,-23.9965132953187,
0.));
#223774=CARTESIAN_POINT('Ctrl Pts',(7.55108647097431,-23.9965132953187,
12.));
#223775=CARTESIAN_POINT('Ctrl Pts',(7.54705232885894,-24.0222783554531,
0.));
#223776=CARTESIAN_POINT('Ctrl Pts',(7.54705232885894,-24.0222783554531,
12.));
#223777=CARTESIAN_POINT('Ctrl Pts',(7.54294601896127,-24.0481099543353,
0.));
#223778=CARTESIAN_POINT('Ctrl Pts',(7.54294601896127,-24.0481099543353,
12.));
#223779=CARTESIAN_POINT('Ctrl Pts',(7.53876736531004,-24.0740075927984,
0.));
#223780=CARTESIAN_POINT('Ctrl Pts',(7.53876736531004,-24.0740075927984,
12.));
#223781=CARTESIAN_POINT('Ctrl Pts',(7.53451619514658,-24.0999707772643,
0.));
#223782=CARTESIAN_POINT('Ctrl Pts',(7.53451619514658,-24.0999707772643,
12.));
#223783=CARTESIAN_POINT('Ctrl Pts',(7.53019233935536,-24.1259990209211,
0.));
#223784=CARTESIAN_POINT('Ctrl Pts',(7.53019233935536,-24.1259990209211,
12.));
#223785=CARTESIAN_POINT('Ctrl Pts',(7.52579563201478,-24.152091842537,0.));
#223786=CARTESIAN_POINT('Ctrl Pts',(7.52579563201478,-24.152091842537,12.));
#223787=CARTESIAN_POINT('Ctrl Pts',(7.52132590953862,-24.1782487641602,
0.));
#223788=CARTESIAN_POINT('Ctrl Pts',(7.52132590953862,-24.1782487641602,
12.));
#223789=CARTESIAN_POINT('Ctrl Pts',(7.51678300997997,-24.2044693092356,
0.));
#223790=CARTESIAN_POINT('Ctrl Pts',(7.51678300997997,-24.2044693092356,
12.));
#223791=CARTESIAN_POINT('Ctrl Pts',(7.51216677222198,-24.230753000389,0.));
#223792=CARTESIAN_POINT('Ctrl Pts',(7.51216677222198,-24.230753000389,12.));
#223793=CARTESIAN_POINT('Ctrl Pts',(7.50747703535114,-24.2570993577032,
0.));
#223794=CARTESIAN_POINT('Ctrl Pts',(7.50747703535114,-24.2570993577032,
12.));
#223795=CARTESIAN_POINT('Ctrl Pts',(7.50271363765098,-24.2835078958966,
0.));
#223796=CARTESIAN_POINT('Ctrl Pts',(7.50271363765098,-24.2835078958966,
12.));
#223797=CARTESIAN_POINT('Ctrl Pts',(7.49787641695358,-24.3099781253345,
0.));
#223798=CARTESIAN_POINT('Ctrl Pts',(7.49787641695358,-24.3099781253345,
12.));
#223799=CARTESIAN_POINT('Ctrl Pts',(7.49296521252329,-24.3365095573673,
0.));
#223800=CARTESIAN_POINT('Ctrl Pts',(7.49296521252329,-24.3365095573673,
12.));
#223801=CARTESIAN_POINT('Ctrl Pts',(7.48797986651827,-24.3631017084513,
0.));
#223802=CARTESIAN_POINT('Ctrl Pts',(7.48797986651827,-24.3631017084513,
12.));
#223803=CARTESIAN_POINT('Ctrl Pts',(7.48292022569253,-24.3897541049248,
0.));
#223804=CARTESIAN_POINT('Ctrl Pts',(7.48292022569253,-24.3897541049248,
12.));
#223805=CARTESIAN_POINT('Ctrl Pts',(7.47778614286572,-24.4164662871165,
0.));
#223806=CARTESIAN_POINT('Ctrl Pts',(7.47778614286572,-24.4164662871165,
12.));
#223807=CARTESIAN_POINT('Ctrl Pts',(7.47257747883318,-24.4432378146501,
0.));
#223808=CARTESIAN_POINT('Ctrl Pts',(7.47257747883318,-24.4432378146501,
12.));
#223809=CARTESIAN_POINT('Ctrl Pts',(7.46729410308922,-24.4700682684544,
0.));
#223810=CARTESIAN_POINT('Ctrl Pts',(7.46729410308922,-24.4700682684544,
12.));
#223811=CARTESIAN_POINT('Ctrl Pts',(7.46193588961641,-24.4969572391509,
0.));
#223812=CARTESIAN_POINT('Ctrl Pts',(7.46193588961641,-24.4969572391509,
12.));
#223813=CARTESIAN_POINT('Ctrl Pts',(7.45650271336044,-24.52390431731,0.));
#223814=CARTESIAN_POINT('Ctrl Pts',(7.45650271336044,-24.52390431731,12.));
#223815=CARTESIAN_POINT('Ctrl Pts',(7.45099444651295,-24.550909083158,0.));
#223816=CARTESIAN_POINT('Ctrl Pts',(7.45099444651295,-24.550909083158,12.));
#223817=CARTESIAN_POINT('Ctrl Pts',(7.44541095473162,-24.5779710960865,
0.));
#223818=CARTESIAN_POINT('Ctrl Pts',(7.44541095473162,-24.5779710960865,
12.));
#223819=CARTESIAN_POINT('Ctrl Pts',(7.43975209375374,-24.6050898852349,
0.));
#223820=CARTESIAN_POINT('Ctrl Pts',(7.43975209375374,-24.6050898852349,
12.));
#223821=CARTESIAN_POINT('Ctrl Pts',(7.4340177048922,-24.6322649369472,0.));
#223822=CARTESIAN_POINT('Ctrl Pts',(7.4340177048922,-24.6322649369472,12.));
#223823=CARTESIAN_POINT('Ctrl Pts',(7.4282076215868,-24.659495712869,0.));
#223824=CARTESIAN_POINT('Ctrl Pts',(7.4282076215868,-24.659495712869,12.));
#223825=CARTESIAN_POINT('Ctrl Pts',(7.42232167765762,-24.6867816727118,
0.));
#223826=CARTESIAN_POINT('Ctrl Pts',(7.42232167765762,-24.6867816727118,
12.));
#223827=CARTESIAN_POINT('Ctrl Pts',(7.41635971481242,-24.7141222949988,
0.));
#223828=CARTESIAN_POINT('Ctrl Pts',(7.41635971481242,-24.7141222949988,
12.));
#223829=CARTESIAN_POINT('Ctrl Pts',(7.41032159082172,-24.7415170994754,
0.));
#223830=CARTESIAN_POINT('Ctrl Pts',(7.41032159082172,-24.7415170994754,
12.));
#223831=CARTESIAN_POINT('Ctrl Pts',(7.40420718661754,-24.7689656669005,
0.));
#223832=CARTESIAN_POINT('Ctrl Pts',(7.40420718661754,-24.7689656669005,
12.));
#223833=CARTESIAN_POINT('Ctrl Pts',(7.39801641583612,-24.7964676646518,
0.));
#223834=CARTESIAN_POINT('Ctrl Pts',(7.39801641583612,-24.7964676646518,
12.));
#223835=CARTESIAN_POINT('Ctrl Pts',(7.3917492258684,-24.8240228521042,0.));
#223836=CARTESIAN_POINT('Ctrl Pts',(7.3917492258684,-24.8240228521042,12.));
#223837=CARTESIAN_POINT('Ctrl Pts',(7.38540558904945,-24.8516310625367,
0.));
#223838=CARTESIAN_POINT('Ctrl Pts',(7.38540558904945,-24.8516310625367,
12.));
#223839=CARTESIAN_POINT('Ctrl Pts',(7.37898549641609,-24.8792921911309,
0.));
#223840=CARTESIAN_POINT('Ctrl Pts',(7.37898549641609,-24.8792921911309,
12.));
#223841=CARTESIAN_POINT('Ctrl Pts',(7.37378825962717,-24.9014633826201,
0.));
#223842=CARTESIAN_POINT('Ctrl Pts',(7.37378825962717,-24.9014633826201,
12.));
#223843=CARTESIAN_POINT('Ctrl Pts',(7.36985593120695,-24.9181155530631,
0.));
#223844=CARTESIAN_POINT('Ctrl Pts',(7.36985593120695,-24.9181155530631,
12.));
#223845=CARTESIAN_POINT('Ctrl Pts',(7.36721909029059,-24.9292275670705,
0.));
#223846=CARTESIAN_POINT('Ctrl Pts',(7.36721909029059,-24.9292275670705,
12.));
#223847=CARTESIAN_POINT('Ctrl Pts',(7.36589684767343,-24.9347862158358,
0.));
#223848=CARTESIAN_POINT('Ctrl Pts',(7.36589684767343,-24.9347862158358,
12.));
#223849=CARTESIAN_POINT('',(7.36589684767343,-24.9347862158358,0.));
#223850=CARTESIAN_POINT('Ctrl Pts',(7.52250298901263,-21.2610617890679,
0.));
#223851=CARTESIAN_POINT('Ctrl Pts',(7.52250649703969,-21.2610673466886,
0.));
#223852=CARTESIAN_POINT('Ctrl Pts',(7.52252744144903,-21.2611204474866,
0.));
#223853=CARTESIAN_POINT('Ctrl Pts',(7.5226006423166,-21.261326054066,0.));
#223854=CARTESIAN_POINT('Ctrl Pts',(7.52278182242669,-21.2618521283555,
0.));
#223855=CARTESIAN_POINT('Ctrl Pts',(7.52314642316199,-21.262927782038,0.));
#223856=CARTESIAN_POINT('Ctrl Pts',(7.52364573027552,-21.2644161259962,
0.));
#223857=CARTESIAN_POINT('Ctrl Pts',(7.52427261074297,-21.2663059157058,
0.));
#223858=CARTESIAN_POINT('Ctrl Pts',(7.5250177033353,-21.2685823838671,0.));
#223859=CARTESIAN_POINT('Ctrl Pts',(7.52587126095529,-21.2712301573466,
0.));
#223860=CARTESIAN_POINT('Ctrl Pts',(7.5268252691854,-21.2742366113579,0.));
#223861=CARTESIAN_POINT('Ctrl Pts',(7.52787386225332,-21.2775925269652,
0.));
#223862=CARTESIAN_POINT('Ctrl Pts',(7.52901217930407,-21.2812902781143,
0.));
#223863=CARTESIAN_POINT('Ctrl Pts',(7.53023562438229,-21.2853226580657,
0.));
#223864=CARTESIAN_POINT('Ctrl Pts',(7.53153906987855,-21.2896816163842,
0.));
#223865=CARTESIAN_POINT('Ctrl Pts',(7.53291726078526,-21.2943588989331,
0.));
#223866=CARTESIAN_POINT('Ctrl Pts',(7.53436505309942,-21.2993464250717,
0.));
#223867=CARTESIAN_POINT('Ctrl Pts',(7.53587778251735,-21.3046368712157,
0.));
#223868=CARTESIAN_POINT('Ctrl Pts',(7.53745129364615,-21.310223716773,0.));
#223869=CARTESIAN_POINT('Ctrl Pts',(7.53908175169898,-21.3161009456256,
0.));
#223870=CARTESIAN_POINT('Ctrl Pts',(7.54076552038278,-21.3222628524165,
0.));
#223871=CARTESIAN_POINT('Ctrl Pts',(7.5424990037703,-21.328703791771,0.));
#223872=CARTESIAN_POINT('Ctrl Pts',(7.54427868151267,-21.3354182340149,
0.));
#223873=CARTESIAN_POINT('Ctrl Pts',(7.54610114948346,-21.3424008295038,
0.));
#223874=CARTESIAN_POINT('Ctrl Pts',(7.5479631624633,-21.3496464761531,0.));
#223875=CARTESIAN_POINT('Ctrl Pts',(7.54986166521309,-21.3571503685855,
0.));
#223876=CARTESIAN_POINT('Ctrl Pts',(7.55179375777443,-21.3649079431865,
0.));
#223877=CARTESIAN_POINT('Ctrl Pts',(7.55375667080028,-21.3729148390243,
0.));
#223878=CARTESIAN_POINT('Ctrl Pts',(7.55574773403502,-21.3811668478932,
0.));
#223879=CARTESIAN_POINT('Ctrl Pts',(7.55776435731416,-21.3896598842117,
0.));
#223880=CARTESIAN_POINT('Ctrl Pts',(7.5598040370061,-21.3983899952987,0.));
#223881=CARTESIAN_POINT('Ctrl Pts',(7.56186435703621,-21.4073533630365,
0.));
#223882=CARTESIAN_POINT('Ctrl Pts',(7.56394299313684,-21.4165463106254,
0.));
#223883=CARTESIAN_POINT('Ctrl Pts',(7.56603771218711,-21.4259653015736,
0.));
#223884=CARTESIAN_POINT('Ctrl Pts',(7.56814636360847,-21.4356069261513,
0.));
#223885=CARTESIAN_POINT('Ctrl Pts',(7.57026687261165,-21.4454678907509,
0.));
#223886=CARTESIAN_POINT('Ctrl Pts',(7.57239723223505,-21.4555450053142,
0.));
#223887=CARTESIAN_POINT('Ctrl Pts',(7.57453549743411,-21.4658351740128,
0.));
#223888=CARTESIAN_POINT('Ctrl Pts',(7.57667978402986,-21.4763353936762,
0.));
#223889=CARTESIAN_POINT('Ctrl Pts',(7.57882826679131,-21.4870427508194,
0.));
#223890=CARTESIAN_POINT('Ctrl Pts',(7.58097917790743,-21.4979544192744,
0.));
#223891=CARTESIAN_POINT('Ctrl Pts',(7.58313080519179,-21.5090676573873,
0.));
#223892=CARTESIAN_POINT('Ctrl Pts',(7.58528148919129,-21.5203798035299,
0.));
#223893=CARTESIAN_POINT('Ctrl Pts',(7.58742962034833,-21.5318882716736,
0.));
#223894=CARTESIAN_POINT('Ctrl Pts',(7.58957363620013,-21.543590547011,0.));
#223895=CARTESIAN_POINT('Ctrl Pts',(7.59171201844776,-21.5554841813462,
0.));
#223896=CARTESIAN_POINT('Ctrl Pts',(7.59384329124918,-21.5675667904726,
0.));
#223897=CARTESIAN_POINT('Ctrl Pts',(7.59596601973583,-21.5798360518978,
0.));
#223898=CARTESIAN_POINT('Ctrl Pts',(7.59807880846194,-21.5922897024466,
0.));
#223899=CARTESIAN_POINT('Ctrl Pts',(7.6001802998824,-21.6049255358843,0.));
#223900=CARTESIAN_POINT('Ctrl Pts',(7.60226917285428,-21.617741400599,0.));
#223901=CARTESIAN_POINT('Ctrl Pts',(7.60434414118295,-21.6307351973822,
0.));
#223902=CARTESIAN_POINT('Ctrl Pts',(7.60640395216356,-21.6439048771743,
0.));
#223903=CARTESIAN_POINT('Ctrl Pts',(7.60844738512873,-21.6572484388081,
0.));
#223904=CARTESIAN_POINT('Ctrl Pts',(7.61047325000955,-21.6707639267576,
0.));
#223905=CARTESIAN_POINT('Ctrl Pts',(7.61248038630268,-21.6844494295815,
0.));
#223906=CARTESIAN_POINT('Ctrl Pts',(7.61446766202786,-21.6983030783322,
0.));
#223907=CARTESIAN_POINT('Ctrl Pts',(7.6164339727042,-21.7123230449834,0.));
#223908=CARTESIAN_POINT('Ctrl Pts',(7.61837824030537,-21.7265075407975,
0.));
#223909=CARTESIAN_POINT('Ctrl Pts',(7.62029941230854,-21.7408548148656,
0.));
#223910=CARTESIAN_POINT('Ctrl Pts',(7.62219646084228,-21.7553631528328,
0.));
#223911=CARTESIAN_POINT('Ctrl Pts',(7.62406838181165,-21.7700308755584,
0.));
#223912=CARTESIAN_POINT('Ctrl Pts',(7.62591419404512,-21.7848563378021,
0.));
#223913=CARTESIAN_POINT('Ctrl Pts',(7.62773293842388,-21.799837926858,0.));
#223914=CARTESIAN_POINT('Ctrl Pts',(7.62952367718126,-21.814974061509,0.));
#223915=CARTESIAN_POINT('Ctrl Pts',(7.63128549323022,-21.8302631910195,
0.));
#223916=CARTESIAN_POINT('Ctrl Pts',(7.63301748948935,-21.8457037941084,
0.));
#223917=CARTESIAN_POINT('Ctrl Pts',(7.63471878821225,-21.8612943779089,
0.));
#223918=CARTESIAN_POINT('Ctrl Pts',(7.63638853033399,-21.8770334769496,
0.));
#223919=CARTESIAN_POINT('Ctrl Pts',(7.63802587492034,-21.8929196523514,
0.));
#223920=CARTESIAN_POINT('Ctrl Pts',(7.63962999860926,-21.9089514909874,
0.));
#223921=CARTESIAN_POINT('Ctrl Pts',(7.64120009506531,-21.9251276046546,
0.));
#223922=CARTESIAN_POINT('Ctrl Pts',(7.64273537442681,-21.9414466292072,
0.));
#223923=CARTESIAN_POINT('Ctrl Pts',(7.64423506279122,-21.9579072237651,
0.));
#223924=CARTESIAN_POINT('Ctrl Pts',(7.64569840177335,-21.9745080700798,
0.));
#223925=CARTESIAN_POINT('Ctrl Pts',(7.64712464805249,-21.9912478718542,
0.));
#223926=CARTESIAN_POINT('Ctrl Pts',(7.64851307293351,-22.0081253540774,
0.));
#223927=CARTESIAN_POINT('Ctrl Pts',(7.64986296190168,-22.0251392623209,
0.));
#223928=CARTESIAN_POINT('Ctrl Pts',(7.65117361421358,-22.0422883621174,
0.));
#223929=CARTESIAN_POINT('Ctrl Pts',(7.65244434253112,-22.0595714384431,
0.));
#223930=CARTESIAN_POINT('Ctrl Pts',(7.65367447254949,-22.0769872951596,
0.));
#223931=CARTESIAN_POINT('Ctrl Pts',(7.65486334263643,-22.094534754469,0.));
#223932=CARTESIAN_POINT('Ctrl Pts',(7.65601030346806,-22.1122126563329,
0.));
#223933=CARTESIAN_POINT('Ctrl Pts',(7.65711471769396,-22.1300198579675,
0.));
#223934=CARTESIAN_POINT('Ctrl Pts',(7.65817595963348,-22.1479552334211,
0.));
#223935=CARTESIAN_POINT('Ctrl Pts',(7.6591934149693,-22.1660176731178,0.));
#223936=CARTESIAN_POINT('Ctrl Pts',(7.66016648045004,-22.1842060834091,
0.));
#223937=CARTESIAN_POINT('Ctrl Pts',(7.6610945635927,-22.2025193860964,0.));
#223938=CARTESIAN_POINT('Ctrl Pts',(7.66197708240399,-22.2209565180085,
0.));
#223939=CARTESIAN_POINT('Ctrl Pts',(7.66281346512508,-22.2395164306547,
0.));
#223940=CARTESIAN_POINT('Ctrl Pts',(7.6636031499764,-22.258198089848,0.));
#223941=CARTESIAN_POINT('Ctrl Pts',(7.66434558490978,-22.2770004753335,
0.));
#223942=CARTESIAN_POINT('Ctrl Pts',(7.66504022736298,-22.2959225803937,
0.));
#223943=CARTESIAN_POINT('Ctrl Pts',(7.66568654402493,-22.314963411484,0.));
#223944=CARTESIAN_POINT('Ctrl Pts',(7.66628401061951,-22.3341219879469,
0.));
#223945=CARTESIAN_POINT('Ctrl Pts',(7.66683211169157,-22.3533973417021,
0.));
#223946=CARTESIAN_POINT('Ctrl Pts',(7.66733034039882,-22.372788516936,0.));
#223947=CARTESIAN_POINT('Ctrl Pts',(7.66777819830789,-22.3922945697773,
0.));
#223948=CARTESIAN_POINT('Ctrl Pts',(7.66817519519639,-22.4119145679758,
0.));
#223949=CARTESIAN_POINT('Ctrl Pts',(7.66852084886703,-22.4316475906603,
0.));
#223950=CARTESIAN_POINT('Ctrl Pts',(7.66881468496634,-22.4514927280855,
0.));
#223951=CARTESIAN_POINT('Ctrl Pts',(7.6690562368083,-22.47144908137,0.));
#223952=CARTESIAN_POINT('Ctrl Pts',(7.66924504520314,-22.4915157622312,
0.));
#223953=CARTESIAN_POINT('Ctrl Pts',(7.66938065829107,-22.5116918927032,
0.));
#223954=CARTESIAN_POINT('Ctrl Pts',(7.66946263138143,-22.53197660492,0.));
#223955=CARTESIAN_POINT('Ctrl Pts',(7.66949052679692,-22.5523690409116,
0.));
#223956=CARTESIAN_POINT('Ctrl Pts',(7.66946391372305,-22.5728683523831,
0.));
#223957=CARTESIAN_POINT('Ctrl Pts',(7.66938236806232,-22.5934737004953,
0.));
#223958=CARTESIAN_POINT('Ctrl Pts',(7.66924547229413,-22.6141842556243,
0.));
#223959=CARTESIAN_POINT('Ctrl Pts',(7.66905281533714,-22.6349991971541,
0.));
#223960=CARTESIAN_POINT('Ctrl Pts',(7.66880399241322,-22.6559177133127,
0.));
#223961=CARTESIAN_POINT('Ctrl Pts',(7.66849860491742,-22.6769390009885,
0.));
#223962=CARTESIAN_POINT('Ctrl Pts',(7.66813626029274,-22.6980622655446,
0.));
#223963=CARTESIAN_POINT('Ctrl Pts',(7.66771657191027,-22.7192867206245,
0.));
#223964=CARTESIAN_POINT('Ctrl Pts',(7.66723915895439,-22.7406115879513,
0.));
#223965=CARTESIAN_POINT('Ctrl Pts',(7.66670364630298,-22.7620360971843,
0.));
#223966=CARTESIAN_POINT('Ctrl Pts',(7.66610966441272,-22.7835594857699,
0.));
#223967=CARTESIAN_POINT('Ctrl Pts',(7.66545684920986,-22.8051809987833,
0.));
#223968=CARTESIAN_POINT('Ctrl Pts',(7.66474484198548,-22.8268998887678,
0.));
#223969=CARTESIAN_POINT('Ctrl Pts',(7.66397328929802,-22.848715415557,0.));
#223970=CARTESIAN_POINT('Ctrl Pts',(7.66314184287336,-22.8706268461283,
0.));
#223971=CARTESIAN_POINT('Ctrl Pts',(7.66225015950155,-22.8926334544883,
0.));
#223972=CARTESIAN_POINT('Ctrl Pts',(7.66129790094107,-22.9147345215421,
0.));
#223973=CARTESIAN_POINT('Ctrl Pts',(7.66028473382777,-22.9369293349593,
0.));
#223974=CARTESIAN_POINT('Ctrl Pts',(7.65921032958901,-22.959217189033,0.));
#223975=CARTESIAN_POINT('Ctrl Pts',(7.65807436436431,-22.9815973845296,
0.));
#223976=CARTESIAN_POINT('Ctrl Pts',(7.65687651891303,-23.0040692285814,
0.));
#223977=CARTESIAN_POINT('Ctrl Pts',(7.65561647852533,-23.0266320345787,
0.));
#223978=CARTESIAN_POINT('Ctrl Pts',(7.65429393293945,-23.0492851220528,
0.));
#223979=CARTESIAN_POINT('Ctrl Pts',(7.65290857626357,-23.072027816555,0.));
#223980=CARTESIAN_POINT('Ctrl Pts',(7.65146010690475,-23.094859449525,0.));
#223981=CARTESIAN_POINT('Ctrl Pts',(7.64994822749859,-23.1177793581679,
0.));
#223982=CARTESIAN_POINT('Ctrl Pts',(7.64837264482942,-23.1407868853819,
0.));
#223983=CARTESIAN_POINT('Ctrl Pts',(7.64673306975804,-23.1638813796694,
0.));
#223984=CARTESIAN_POINT('Ctrl Pts',(7.64502921715482,-23.1870621950452,
0.));
#223985=CARTESIAN_POINT('Ctrl Pts',(7.64326080583679,-23.2103286909398,
0.));
#223986=CARTESIAN_POINT('Ctrl Pts',(7.64142755851504,-23.2336802320912,
0.));
#223987=CARTESIAN_POINT('Ctrl Pts',(7.63952920172834,-23.2571161884488,
0.));
#223988=CARTESIAN_POINT('Ctrl Pts',(7.63756546576373,-23.2806359350855,
0.));
#223989=CARTESIAN_POINT('Ctrl Pts',(7.63553608458782,-23.3042388521022,
0.));
#223990=CARTESIAN_POINT('Ctrl Pts',(7.63344079578161,-23.3279243245241,
0.));
#223991=CARTESIAN_POINT('Ctrl Pts',(7.63127934048136,-23.3516917421972,
0.));
#223992=CARTESIAN_POINT('Ctrl Pts',(7.62905146332592,-23.3755404996636,
0.));
#223993=CARTESIAN_POINT('Ctrl Pts',(7.62675691240328,-23.399469996112,0.));
#223994=CARTESIAN_POINT('Ctrl Pts',(7.62439543920049,-23.4234796353542,
0.));
#223995=CARTESIAN_POINT('Ctrl Pts',(7.62196679855954,-23.4475688257854,
0.));
#223996=CARTESIAN_POINT('Ctrl Pts',(7.61947074863976,-23.4717369803438,
0.));
#223997=CARTESIAN_POINT('Ctrl Pts',(7.61690705088318,-23.4959835164609,
0.));
#223998=CARTESIAN_POINT('Ctrl Pts',(7.61427546999297,-23.5203078560129,
0.));
#223999=CARTESIAN_POINT('Ctrl Pts',(7.61157577385371,-23.544709425203,0.));
#224000=CARTESIAN_POINT('Ctrl Pts',(7.60880773344599,-23.5691876544244,
0.));
#224001=CARTESIAN_POINT('Ctrl Pts',(7.60597112277093,-23.5937419781245,
0.));
#224002=CARTESIAN_POINT('Ctrl Pts',(7.60306571877805,-23.6183718346576,
0.));
#224003=CARTESIAN_POINT('Ctrl Pts',(7.60009130130125,-23.6430766661418,
0.));
#224004=CARTESIAN_POINT('Ctrl Pts',(7.59704765299566,-23.6678559182875,
0.));
#224005=CARTESIAN_POINT('Ctrl Pts',(7.59393455934034,-23.6927090405066,
0.));
#224006=CARTESIAN_POINT('Ctrl Pts',(7.5907518086532,-23.7176354860457,0.));
#224007=CARTESIAN_POINT('Ctrl Pts',(7.58749919210825,-23.7426347121006,
0.));
#224008=CARTESIAN_POINT('Ctrl Pts',(7.5841765037627,-23.7677061799376,0.));
#224009=CARTESIAN_POINT('Ctrl Pts',(7.58078354058212,-23.7928493549908,
0.));
#224010=CARTESIAN_POINT('Ctrl Pts',(7.57732010249065,-23.8180637069976,
0.));
#224011=CARTESIAN_POINT('Ctrl Pts',(7.57378599219813,-23.8433487096132,
0.));
#224012=CARTESIAN_POINT('Ctrl Pts',(7.57018101500708,-23.8687038399595,
0.));
#224013=CARTESIAN_POINT('Ctrl Pts',(7.5665049786379,-23.8941285782002,0.));
#224014=CARTESIAN_POINT('Ctrl Pts',(7.56275769304772,-23.9196224070759,
0.));
#224015=CARTESIAN_POINT('Ctrl Pts',(7.55893897027679,-23.9451848115002,
0.));
#224016=CARTESIAN_POINT('Ctrl Pts',(7.55504862424807,-23.9708152779886,
0.));
#224017=CARTESIAN_POINT('Ctrl Pts',(7.55108647097431,-23.9965132953187,
0.));
#224018=CARTESIAN_POINT('Ctrl Pts',(7.54705232885894,-24.0222783554531,
0.));
#224019=CARTESIAN_POINT('Ctrl Pts',(7.54294601896127,-24.0481099543353,
0.));
#224020=CARTESIAN_POINT('Ctrl Pts',(7.53876736531004,-24.0740075927984,
0.));
#224021=CARTESIAN_POINT('Ctrl Pts',(7.53451619514658,-24.0999707772643,
0.));
#224022=CARTESIAN_POINT('Ctrl Pts',(7.53019233935536,-24.1259990209211,
0.));
#224023=CARTESIAN_POINT('Ctrl Pts',(7.52579563201478,-24.152091842537,0.));
#224024=CARTESIAN_POINT('Ctrl Pts',(7.52132590953862,-24.1782487641602,
0.));
#224025=CARTESIAN_POINT('Ctrl Pts',(7.51678300997997,-24.2044693092356,
0.));
#224026=CARTESIAN_POINT('Ctrl Pts',(7.51216677222198,-24.230753000389,0.));
#224027=CARTESIAN_POINT('Ctrl Pts',(7.50747703535114,-24.2570993577032,
0.));
#224028=CARTESIAN_POINT('Ctrl Pts',(7.50271363765098,-24.2835078958966,
0.));
#224029=CARTESIAN_POINT('Ctrl Pts',(7.49787641695358,-24.3099781253345,
0.));
#224030=CARTESIAN_POINT('Ctrl Pts',(7.49296521252329,-24.3365095573673,
0.));
#224031=CARTESIAN_POINT('Ctrl Pts',(7.48797986651827,-24.3631017084513,
0.));
#224032=CARTESIAN_POINT('Ctrl Pts',(7.48292022569253,-24.3897541049248,
0.));
#224033=CARTESIAN_POINT('Ctrl Pts',(7.47778614286572,-24.4164662871165,
0.));
#224034=CARTESIAN_POINT('Ctrl Pts',(7.47257747883318,-24.4432378146501,
0.));
#224035=CARTESIAN_POINT('Ctrl Pts',(7.46729410308922,-24.4700682684544,
0.));
#224036=CARTESIAN_POINT('Ctrl Pts',(7.46193588961641,-24.4969572391509,
0.));
#224037=CARTESIAN_POINT('Ctrl Pts',(7.45650271336044,-24.52390431731,0.));
#224038=CARTESIAN_POINT('Ctrl Pts',(7.45099444651295,-24.550909083158,0.));
#224039=CARTESIAN_POINT('Ctrl Pts',(7.44541095473162,-24.5779710960865,
0.));
#224040=CARTESIAN_POINT('Ctrl Pts',(7.43975209375374,-24.6050898852349,
0.));
#224041=CARTESIAN_POINT('Ctrl Pts',(7.4340177048922,-24.6322649369472,0.));
#224042=CARTESIAN_POINT('Ctrl Pts',(7.4282076215868,-24.659495712869,0.));
#224043=CARTESIAN_POINT('Ctrl Pts',(7.42232167765762,-24.6867816727118,
0.));
#224044=CARTESIAN_POINT('Ctrl Pts',(7.41635971481242,-24.7141222949988,
0.));
#224045=CARTESIAN_POINT('Ctrl Pts',(7.41032159082172,-24.7415170994754,
0.));
#224046=CARTESIAN_POINT('Ctrl Pts',(7.40420718661754,-24.7689656669005,
0.));
#224047=CARTESIAN_POINT('Ctrl Pts',(7.39801641583612,-24.7964676646518,
0.));
#224048=CARTESIAN_POINT('Ctrl Pts',(7.3917492258684,-24.8240228521042,0.));
#224049=CARTESIAN_POINT('Ctrl Pts',(7.38540558904945,-24.8516310625367,
0.));
#224050=CARTESIAN_POINT('Ctrl Pts',(7.37898549641609,-24.8792921911309,
0.));
#224051=CARTESIAN_POINT('Ctrl Pts',(7.37378825962717,-24.9014633826201,
0.));
#224052=CARTESIAN_POINT('Ctrl Pts',(7.36985593120695,-24.9181155530631,
0.));
#224053=CARTESIAN_POINT('Ctrl Pts',(7.36721909029059,-24.9292275670705,
0.));
#224054=CARTESIAN_POINT('Ctrl Pts',(7.36589684767343,-24.9347862158358,
0.));
#224055=CARTESIAN_POINT('',(7.36589684767343,-24.9347862158358,12.));
#224056=CARTESIAN_POINT('Ctrl Pts',(7.36589684767343,-24.9347862158358,
12.));
#224057=CARTESIAN_POINT('Ctrl Pts',(7.36721909029059,-24.9292275670705,
12.));
#224058=CARTESIAN_POINT('Ctrl Pts',(7.36985593120695,-24.9181155530631,
12.));
#224059=CARTESIAN_POINT('Ctrl Pts',(7.37378825962717,-24.9014633826201,
12.));
#224060=CARTESIAN_POINT('Ctrl Pts',(7.37898549641609,-24.8792921911309,
12.));
#224061=CARTESIAN_POINT('Ctrl Pts',(7.38540558904945,-24.8516310625367,
12.));
#224062=CARTESIAN_POINT('Ctrl Pts',(7.3917492258684,-24.8240228521042,12.));
#224063=CARTESIAN_POINT('Ctrl Pts',(7.39801641583612,-24.7964676646518,
12.));
#224064=CARTESIAN_POINT('Ctrl Pts',(7.40420718661754,-24.7689656669005,
12.));
#224065=CARTESIAN_POINT('Ctrl Pts',(7.41032159082172,-24.7415170994754,
12.));
#224066=CARTESIAN_POINT('Ctrl Pts',(7.41635971481242,-24.7141222949988,
12.));
#224067=CARTESIAN_POINT('Ctrl Pts',(7.42232167765762,-24.6867816727118,
12.));
#224068=CARTESIAN_POINT('Ctrl Pts',(7.4282076215868,-24.659495712869,12.));
#224069=CARTESIAN_POINT('Ctrl Pts',(7.4340177048922,-24.6322649369472,12.));
#224070=CARTESIAN_POINT('Ctrl Pts',(7.43975209375374,-24.6050898852349,
12.));
#224071=CARTESIAN_POINT('Ctrl Pts',(7.44541095473162,-24.5779710960865,
12.));
#224072=CARTESIAN_POINT('Ctrl Pts',(7.45099444651295,-24.550909083158,12.));
#224073=CARTESIAN_POINT('Ctrl Pts',(7.45650271336044,-24.52390431731,12.));
#224074=CARTESIAN_POINT('Ctrl Pts',(7.46193588961641,-24.4969572391509,
12.));
#224075=CARTESIAN_POINT('Ctrl Pts',(7.46729410308922,-24.4700682684544,
12.));
#224076=CARTESIAN_POINT('Ctrl Pts',(7.47257747883318,-24.4432378146501,
12.));
#224077=CARTESIAN_POINT('Ctrl Pts',(7.47778614286572,-24.4164662871165,
12.));
#224078=CARTESIAN_POINT('Ctrl Pts',(7.48292022569253,-24.3897541049248,
12.));
#224079=CARTESIAN_POINT('Ctrl Pts',(7.48797986651827,-24.3631017084513,
12.));
#224080=CARTESIAN_POINT('Ctrl Pts',(7.49296521252329,-24.3365095573673,
12.));
#224081=CARTESIAN_POINT('Ctrl Pts',(7.49787641695358,-24.3099781253345,
12.));
#224082=CARTESIAN_POINT('Ctrl Pts',(7.50271363765098,-24.2835078958966,
12.));
#224083=CARTESIAN_POINT('Ctrl Pts',(7.50747703535114,-24.2570993577032,
12.));
#224084=CARTESIAN_POINT('Ctrl Pts',(7.51216677222198,-24.230753000389,12.));
#224085=CARTESIAN_POINT('Ctrl Pts',(7.51678300997997,-24.2044693092356,
12.));
#224086=CARTESIAN_POINT('Ctrl Pts',(7.52132590953862,-24.1782487641602,
12.));
#224087=CARTESIAN_POINT('Ctrl Pts',(7.52579563201478,-24.152091842537,12.));
#224088=CARTESIAN_POINT('Ctrl Pts',(7.53019233935536,-24.1259990209211,
12.));
#224089=CARTESIAN_POINT('Ctrl Pts',(7.53451619514658,-24.0999707772643,
12.));
#224090=CARTESIAN_POINT('Ctrl Pts',(7.53876736531004,-24.0740075927984,
12.));
#224091=CARTESIAN_POINT('Ctrl Pts',(7.54294601896127,-24.0481099543353,
12.));
#224092=CARTESIAN_POINT('Ctrl Pts',(7.54705232885894,-24.0222783554531,
12.));
#224093=CARTESIAN_POINT('Ctrl Pts',(7.55108647097431,-23.9965132953187,
12.));
#224094=CARTESIAN_POINT('Ctrl Pts',(7.55504862424807,-23.9708152779886,
12.));
#224095=CARTESIAN_POINT('Ctrl Pts',(7.55893897027679,-23.9451848115002,
12.));
#224096=CARTESIAN_POINT('Ctrl Pts',(7.56275769304772,-23.9196224070759,
12.));
#224097=CARTESIAN_POINT('Ctrl Pts',(7.5665049786379,-23.8941285782002,12.));
#224098=CARTESIAN_POINT('Ctrl Pts',(7.57018101500708,-23.8687038399595,
12.));
#224099=CARTESIAN_POINT('Ctrl Pts',(7.57378599219813,-23.8433487096132,
12.));
#224100=CARTESIAN_POINT('Ctrl Pts',(7.57732010249065,-23.8180637069976,
12.));
#224101=CARTESIAN_POINT('Ctrl Pts',(7.58078354058212,-23.7928493549908,
12.));
#224102=CARTESIAN_POINT('Ctrl Pts',(7.5841765037627,-23.7677061799376,12.));
#224103=CARTESIAN_POINT('Ctrl Pts',(7.58749919210825,-23.7426347121006,
12.));
#224104=CARTESIAN_POINT('Ctrl Pts',(7.5907518086532,-23.7176354860457,12.));
#224105=CARTESIAN_POINT('Ctrl Pts',(7.59393455934034,-23.6927090405066,
12.));
#224106=CARTESIAN_POINT('Ctrl Pts',(7.59704765299566,-23.6678559182875,
12.));
#224107=CARTESIAN_POINT('Ctrl Pts',(7.60009130130125,-23.6430766661418,
12.));
#224108=CARTESIAN_POINT('Ctrl Pts',(7.60306571877805,-23.6183718346576,
12.));
#224109=CARTESIAN_POINT('Ctrl Pts',(7.60597112277093,-23.5937419781245,
12.));
#224110=CARTESIAN_POINT('Ctrl Pts',(7.60880773344599,-23.5691876544244,
12.));
#224111=CARTESIAN_POINT('Ctrl Pts',(7.61157577385371,-23.544709425203,12.));
#224112=CARTESIAN_POINT('Ctrl Pts',(7.61427546999297,-23.5203078560129,
12.));
#224113=CARTESIAN_POINT('Ctrl Pts',(7.61690705088318,-23.4959835164609,
12.));
#224114=CARTESIAN_POINT('Ctrl Pts',(7.61947074863976,-23.4717369803438,
12.));
#224115=CARTESIAN_POINT('Ctrl Pts',(7.62196679855954,-23.4475688257854,
12.));
#224116=CARTESIAN_POINT('Ctrl Pts',(7.62439543920049,-23.4234796353542,
12.));
#224117=CARTESIAN_POINT('Ctrl Pts',(7.62675691240328,-23.399469996112,12.));
#224118=CARTESIAN_POINT('Ctrl Pts',(7.62905146332592,-23.3755404996636,
12.));
#224119=CARTESIAN_POINT('Ctrl Pts',(7.63127934048136,-23.3516917421972,
12.));
#224120=CARTESIAN_POINT('Ctrl Pts',(7.63344079578161,-23.3279243245241,
12.));
#224121=CARTESIAN_POINT('Ctrl Pts',(7.63553608458782,-23.3042388521022,
12.));
#224122=CARTESIAN_POINT('Ctrl Pts',(7.63756546576373,-23.2806359350855,
12.));
#224123=CARTESIAN_POINT('Ctrl Pts',(7.63952920172834,-23.2571161884488,
12.));
#224124=CARTESIAN_POINT('Ctrl Pts',(7.64142755851504,-23.2336802320912,
12.));
#224125=CARTESIAN_POINT('Ctrl Pts',(7.64326080583679,-23.2103286909398,
12.));
#224126=CARTESIAN_POINT('Ctrl Pts',(7.64502921715482,-23.1870621950452,
12.));
#224127=CARTESIAN_POINT('Ctrl Pts',(7.64673306975804,-23.1638813796694,
12.));
#224128=CARTESIAN_POINT('Ctrl Pts',(7.64837264482942,-23.1407868853819,
12.));
#224129=CARTESIAN_POINT('Ctrl Pts',(7.64994822749859,-23.1177793581679,
12.));
#224130=CARTESIAN_POINT('Ctrl Pts',(7.65146010690475,-23.094859449525,12.));
#224131=CARTESIAN_POINT('Ctrl Pts',(7.65290857626357,-23.072027816555,12.));
#224132=CARTESIAN_POINT('Ctrl Pts',(7.65429393293945,-23.0492851220528,
12.));
#224133=CARTESIAN_POINT('Ctrl Pts',(7.65561647852533,-23.0266320345787,
12.));
#224134=CARTESIAN_POINT('Ctrl Pts',(7.65687651891303,-23.0040692285814,
12.));
#224135=CARTESIAN_POINT('Ctrl Pts',(7.65807436436431,-22.9815973845296,
12.));
#224136=CARTESIAN_POINT('Ctrl Pts',(7.65921032958901,-22.959217189033,12.));
#224137=CARTESIAN_POINT('Ctrl Pts',(7.66028473382777,-22.9369293349593,
12.));
#224138=CARTESIAN_POINT('Ctrl Pts',(7.66129790094107,-22.9147345215421,
12.));
#224139=CARTESIAN_POINT('Ctrl Pts',(7.66225015950155,-22.8926334544883,
12.));
#224140=CARTESIAN_POINT('Ctrl Pts',(7.66314184287336,-22.8706268461283,
12.));
#224141=CARTESIAN_POINT('Ctrl Pts',(7.66397328929802,-22.848715415557,12.));
#224142=CARTESIAN_POINT('Ctrl Pts',(7.66474484198548,-22.8268998887678,
12.));
#224143=CARTESIAN_POINT('Ctrl Pts',(7.66545684920986,-22.8051809987833,
12.));
#224144=CARTESIAN_POINT('Ctrl Pts',(7.66610966441272,-22.7835594857699,
12.));
#224145=CARTESIAN_POINT('Ctrl Pts',(7.66670364630298,-22.7620360971843,
12.));
#224146=CARTESIAN_POINT('Ctrl Pts',(7.66723915895439,-22.7406115879513,
12.));
#224147=CARTESIAN_POINT('Ctrl Pts',(7.66771657191027,-22.7192867206245,
12.));
#224148=CARTESIAN_POINT('Ctrl Pts',(7.66813626029274,-22.6980622655446,
12.));
#224149=CARTESIAN_POINT('Ctrl Pts',(7.66849860491742,-22.6769390009885,
12.));
#224150=CARTESIAN_POINT('Ctrl Pts',(7.66880399241322,-22.6559177133127,
12.));
#224151=CARTESIAN_POINT('Ctrl Pts',(7.66905281533714,-22.6349991971541,
12.));
#224152=CARTESIAN_POINT('Ctrl Pts',(7.66924547229413,-22.6141842556243,
12.));
#224153=CARTESIAN_POINT('Ctrl Pts',(7.66938236806232,-22.5934737004953,
12.));
#224154=CARTESIAN_POINT('Ctrl Pts',(7.66946391372305,-22.5728683523831,
12.));
#224155=CARTESIAN_POINT('Ctrl Pts',(7.66949052679692,-22.5523690409116,
12.));
#224156=CARTESIAN_POINT('Ctrl Pts',(7.66946263138143,-22.53197660492,12.));
#224157=CARTESIAN_POINT('Ctrl Pts',(7.66938065829107,-22.5116918927032,
12.));
#224158=CARTESIAN_POINT('Ctrl Pts',(7.66924504520314,-22.4915157622312,
12.));
#224159=CARTESIAN_POINT('Ctrl Pts',(7.6690562368083,-22.47144908137,12.));
#224160=CARTESIAN_POINT('Ctrl Pts',(7.66881468496634,-22.4514927280855,
12.));
#224161=CARTESIAN_POINT('Ctrl Pts',(7.66852084886703,-22.4316475906603,
12.));
#224162=CARTESIAN_POINT('Ctrl Pts',(7.66817519519639,-22.4119145679758,
12.));
#224163=CARTESIAN_POINT('Ctrl Pts',(7.66777819830789,-22.3922945697773,
12.));
#224164=CARTESIAN_POINT('Ctrl Pts',(7.66733034039882,-22.372788516936,12.));
#224165=CARTESIAN_POINT('Ctrl Pts',(7.66683211169157,-22.3533973417021,
12.));
#224166=CARTESIAN_POINT('Ctrl Pts',(7.66628401061951,-22.3341219879469,
12.));
#224167=CARTESIAN_POINT('Ctrl Pts',(7.66568654402493,-22.314963411484,12.));
#224168=CARTESIAN_POINT('Ctrl Pts',(7.66504022736298,-22.2959225803937,
12.));
#224169=CARTESIAN_POINT('Ctrl Pts',(7.66434558490978,-22.2770004753335,
12.));
#224170=CARTESIAN_POINT('Ctrl Pts',(7.6636031499764,-22.258198089848,12.));
#224171=CARTESIAN_POINT('Ctrl Pts',(7.66281346512508,-22.2395164306547,
12.));
#224172=CARTESIAN_POINT('Ctrl Pts',(7.66197708240399,-22.2209565180085,
12.));
#224173=CARTESIAN_POINT('Ctrl Pts',(7.6610945635927,-22.2025193860964,12.));
#224174=CARTESIAN_POINT('Ctrl Pts',(7.66016648045004,-22.1842060834091,
12.));
#224175=CARTESIAN_POINT('Ctrl Pts',(7.6591934149693,-22.1660176731178,12.));
#224176=CARTESIAN_POINT('Ctrl Pts',(7.65817595963348,-22.1479552334211,
12.));
#224177=CARTESIAN_POINT('Ctrl Pts',(7.65711471769396,-22.1300198579675,
12.));
#224178=CARTESIAN_POINT('Ctrl Pts',(7.65601030346806,-22.1122126563329,
12.));
#224179=CARTESIAN_POINT('Ctrl Pts',(7.65486334263643,-22.094534754469,12.));
#224180=CARTESIAN_POINT('Ctrl Pts',(7.65367447254949,-22.0769872951596,
12.));
#224181=CARTESIAN_POINT('Ctrl Pts',(7.65244434253112,-22.0595714384431,
12.));
#224182=CARTESIAN_POINT('Ctrl Pts',(7.65117361421358,-22.0422883621174,
12.));
#224183=CARTESIAN_POINT('Ctrl Pts',(7.64986296190168,-22.0251392623209,
12.));
#224184=CARTESIAN_POINT('Ctrl Pts',(7.64851307293351,-22.0081253540774,
12.));
#224185=CARTESIAN_POINT('Ctrl Pts',(7.64712464805249,-21.9912478718542,
12.));
#224186=CARTESIAN_POINT('Ctrl Pts',(7.64569840177335,-21.9745080700798,
12.));
#224187=CARTESIAN_POINT('Ctrl Pts',(7.64423506279122,-21.9579072237651,
12.));
#224188=CARTESIAN_POINT('Ctrl Pts',(7.64273537442681,-21.9414466292072,
12.));
#224189=CARTESIAN_POINT('Ctrl Pts',(7.64120009506531,-21.9251276046546,
12.));
#224190=CARTESIAN_POINT('Ctrl Pts',(7.63962999860926,-21.9089514909874,
12.));
#224191=CARTESIAN_POINT('Ctrl Pts',(7.63802587492034,-21.8929196523514,
12.));
#224192=CARTESIAN_POINT('Ctrl Pts',(7.63638853033399,-21.8770334769496,
12.));
#224193=CARTESIAN_POINT('Ctrl Pts',(7.63471878821225,-21.8612943779089,
12.));
#224194=CARTESIAN_POINT('Ctrl Pts',(7.63301748948935,-21.8457037941084,
12.));
#224195=CARTESIAN_POINT('Ctrl Pts',(7.63128549323022,-21.8302631910195,
12.));
#224196=CARTESIAN_POINT('Ctrl Pts',(7.62952367718126,-21.814974061509,12.));
#224197=CARTESIAN_POINT('Ctrl Pts',(7.62773293842388,-21.799837926858,12.));
#224198=CARTESIAN_POINT('Ctrl Pts',(7.62591419404512,-21.7848563378021,
12.));
#224199=CARTESIAN_POINT('Ctrl Pts',(7.62406838181165,-21.7700308755584,
12.));
#224200=CARTESIAN_POINT('Ctrl Pts',(7.62219646084228,-21.7553631528328,
12.));
#224201=CARTESIAN_POINT('Ctrl Pts',(7.62029941230854,-21.7408548148656,
12.));
#224202=CARTESIAN_POINT('Ctrl Pts',(7.61837824030537,-21.7265075407975,
12.));
#224203=CARTESIAN_POINT('Ctrl Pts',(7.6164339727042,-21.7123230449834,12.));
#224204=CARTESIAN_POINT('Ctrl Pts',(7.61446766202786,-21.6983030783322,
12.));
#224205=CARTESIAN_POINT('Ctrl Pts',(7.61248038630268,-21.6844494295815,
12.));
#224206=CARTESIAN_POINT('Ctrl Pts',(7.61047325000955,-21.6707639267576,
12.));
#224207=CARTESIAN_POINT('Ctrl Pts',(7.60844738512873,-21.6572484388081,
12.));
#224208=CARTESIAN_POINT('Ctrl Pts',(7.60640395216356,-21.6439048771743,
12.));
#224209=CARTESIAN_POINT('Ctrl Pts',(7.60434414118295,-21.6307351973822,
12.));
#224210=CARTESIAN_POINT('Ctrl Pts',(7.60226917285428,-21.617741400599,12.));
#224211=CARTESIAN_POINT('Ctrl Pts',(7.6001802998824,-21.6049255358843,12.));
#224212=CARTESIAN_POINT('Ctrl Pts',(7.59807880846194,-21.5922897024466,
12.));
#224213=CARTESIAN_POINT('Ctrl Pts',(7.59596601973583,-21.5798360518978,
12.));
#224214=CARTESIAN_POINT('Ctrl Pts',(7.59384329124918,-21.5675667904726,
12.));
#224215=CARTESIAN_POINT('Ctrl Pts',(7.59171201844776,-21.5554841813462,
12.));
#224216=CARTESIAN_POINT('Ctrl Pts',(7.58957363620013,-21.543590547011,12.));
#224217=CARTESIAN_POINT('Ctrl Pts',(7.58742962034833,-21.5318882716736,
12.));
#224218=CARTESIAN_POINT('Ctrl Pts',(7.58528148919129,-21.5203798035299,
12.));
#224219=CARTESIAN_POINT('Ctrl Pts',(7.58313080519179,-21.5090676573873,
12.));
#224220=CARTESIAN_POINT('Ctrl Pts',(7.58097917790743,-21.4979544192744,
12.));
#224221=CARTESIAN_POINT('Ctrl Pts',(7.57882826679131,-21.4870427508194,
12.));
#224222=CARTESIAN_POINT('Ctrl Pts',(7.57667978402986,-21.4763353936762,
12.));
#224223=CARTESIAN_POINT('Ctrl Pts',(7.57453549743411,-21.4658351740128,
12.));
#224224=CARTESIAN_POINT('Ctrl Pts',(7.57239723223505,-21.4555450053142,
12.));
#224225=CARTESIAN_POINT('Ctrl Pts',(7.57026687261165,-21.4454678907509,
12.));
#224226=CARTESIAN_POINT('Ctrl Pts',(7.56814636360847,-21.4356069261513,
12.));
#224227=CARTESIAN_POINT('Ctrl Pts',(7.56603771218711,-21.4259653015736,
12.));
#224228=CARTESIAN_POINT('Ctrl Pts',(7.56394299313684,-21.4165463106254,
12.));
#224229=CARTESIAN_POINT('Ctrl Pts',(7.56186435703621,-21.4073533630365,
12.));
#224230=CARTESIAN_POINT('Ctrl Pts',(7.5598040370061,-21.3983899952987,12.));
#224231=CARTESIAN_POINT('Ctrl Pts',(7.55776435731416,-21.3896598842117,
12.));
#224232=CARTESIAN_POINT('Ctrl Pts',(7.55574773403502,-21.3811668478932,
12.));
#224233=CARTESIAN_POINT('Ctrl Pts',(7.55375667080028,-21.3729148390243,
12.));
#224234=CARTESIAN_POINT('Ctrl Pts',(7.55179375777443,-21.3649079431865,
12.));
#224235=CARTESIAN_POINT('Ctrl Pts',(7.54986166521309,-21.3571503685855,
12.));
#224236=CARTESIAN_POINT('Ctrl Pts',(7.5479631624633,-21.3496464761531,12.));
#224237=CARTESIAN_POINT('Ctrl Pts',(7.54610114948346,-21.3424008295038,
12.));
#224238=CARTESIAN_POINT('Ctrl Pts',(7.54427868151267,-21.3354182340149,
12.));
#224239=CARTESIAN_POINT('Ctrl Pts',(7.5424990037703,-21.328703791771,12.));
#224240=CARTESIAN_POINT('Ctrl Pts',(7.54076552038278,-21.3222628524165,
12.));
#224241=CARTESIAN_POINT('Ctrl Pts',(7.53908175169898,-21.3161009456256,
12.));
#224242=CARTESIAN_POINT('Ctrl Pts',(7.53745129364615,-21.310223716773,12.));
#224243=CARTESIAN_POINT('Ctrl Pts',(7.53587778251735,-21.3046368712157,
12.));
#224244=CARTESIAN_POINT('Ctrl Pts',(7.53436505309942,-21.2993464250717,
12.));
#224245=CARTESIAN_POINT('Ctrl Pts',(7.53291726078526,-21.2943588989331,
12.));
#224246=CARTESIAN_POINT('Ctrl Pts',(7.53153906987855,-21.2896816163842,
12.));
#224247=CARTESIAN_POINT('Ctrl Pts',(7.53023562438229,-21.2853226580657,
12.));
#224248=CARTESIAN_POINT('Ctrl Pts',(7.52901217930407,-21.2812902781143,
12.));
#224249=CARTESIAN_POINT('Ctrl Pts',(7.52787386225332,-21.2775925269652,
12.));
#224250=CARTESIAN_POINT('Ctrl Pts',(7.5268252691854,-21.2742366113579,12.));
#224251=CARTESIAN_POINT('Ctrl Pts',(7.52587126095529,-21.2712301573466,
12.));
#224252=CARTESIAN_POINT('Ctrl Pts',(7.5250177033353,-21.2685823838671,12.));
#224253=CARTESIAN_POINT('Ctrl Pts',(7.52427261074297,-21.2663059157058,
12.));
#224254=CARTESIAN_POINT('Ctrl Pts',(7.52364573027552,-21.2644161259962,
12.));
#224255=CARTESIAN_POINT('Ctrl Pts',(7.52314642316199,-21.262927782038,12.));
#224256=CARTESIAN_POINT('Ctrl Pts',(7.52278182242669,-21.2618521283555,
12.));
#224257=CARTESIAN_POINT('Ctrl Pts',(7.5226006423166,-21.261326054066,12.));
#224258=CARTESIAN_POINT('Ctrl Pts',(7.52252744144903,-21.2611204474866,
12.));
#224259=CARTESIAN_POINT('Ctrl Pts',(7.52250649703969,-21.2610673466886,
12.));
#224260=CARTESIAN_POINT('Ctrl Pts',(7.52250298901263,-21.2610617890679,
12.));
#224261=CARTESIAN_POINT('',(7.36589684767343,-24.9347862158358,0.));
#224262=CARTESIAN_POINT('Origin',(1.68110656504246,-21.4341755315424,0.));
#224263=CARTESIAN_POINT('',(1.76341220531179,-22.4835757167854,12.));
#224264=CARTESIAN_POINT('',(0.840553282521226,-10.7170877657712,12.));
#224265=CARTESIAN_POINT('',(1.76341220531179,-22.4835757167854,0.));
#224266=CARTESIAN_POINT('',(1.76341220531179,-22.4835757167854,0.));
#224267=CARTESIAN_POINT('',(0.840553282521226,-10.7170877657712,0.));
#224268=CARTESIAN_POINT('Ctrl Pts',(6.08833931617698,-25.2771067246846,
0.));
#224269=CARTESIAN_POINT('Ctrl Pts',(6.08833931617698,-25.2771067246846,
12.));
#224270=CARTESIAN_POINT('Ctrl Pts',(6.08441489609824,-25.2729539149479,
0.));
#224271=CARTESIAN_POINT('Ctrl Pts',(6.08441489609824,-25.2729539149479,
12.));
#224272=CARTESIAN_POINT('Ctrl Pts',(6.07657531787577,-25.2646490489816,
0.));
#224273=CARTESIAN_POINT('Ctrl Pts',(6.07657531787577,-25.2646490489816,
12.));
#224274=CARTESIAN_POINT('Ctrl Pts',(6.06484373634696,-25.2521940105523,
0.));
#224275=CARTESIAN_POINT('Ctrl Pts',(6.06484373634696,-25.2521940105523,
12.));
#224276=CARTESIAN_POINT('Ctrl Pts',(6.04925720151412,-25.2355918138798,
0.));
#224277=CARTESIAN_POINT('Ctrl Pts',(6.04925720151412,-25.2355918138798,
12.));
#224278=CARTESIAN_POINT('Ctrl Pts',(6.02986667390187,-25.2148466201368,
0.));
#224279=CARTESIAN_POINT('Ctrl Pts',(6.02986667390187,-25.2148466201368,
12.));
#224280=CARTESIAN_POINT('Ctrl Pts',(6.0105688180476,-25.1941090269638,0.));
#224281=CARTESIAN_POINT('Ctrl Pts',(6.0105688180476,-25.1941090269638,12.));
#224282=CARTESIAN_POINT('Ctrl Pts',(5.99136367859838,-25.1733791296154,
0.));
#224283=CARTESIAN_POINT('Ctrl Pts',(5.99136367859838,-25.1733791296154,
12.));
#224284=CARTESIAN_POINT('Ctrl Pts',(5.97225131495636,-25.1526570863065,
0.));
#224285=CARTESIAN_POINT('Ctrl Pts',(5.97225131495636,-25.1526570863065,
12.));
#224286=CARTESIAN_POINT('Ctrl Pts',(5.95323180187347,-25.1319431317273,
0.));
#224287=CARTESIAN_POINT('Ctrl Pts',(5.95323180187347,-25.1319431317273,
12.));
#224288=CARTESIAN_POINT('Ctrl Pts',(5.93430523086776,-25.1112375971182,
0.));
#224289=CARTESIAN_POINT('Ctrl Pts',(5.93430523086776,-25.1112375971182,
12.));
#224290=CARTESIAN_POINT('Ctrl Pts',(5.91547170844382,-25.0905409050863,
0.));
#224291=CARTESIAN_POINT('Ctrl Pts',(5.91547170844382,-25.0905409050863,
12.));
#224292=CARTESIAN_POINT('Ctrl Pts',(5.89673135155458,-25.0698535426593,
0.));
#224293=CARTESIAN_POINT('Ctrl Pts',(5.89673135155458,-25.0698535426593,
12.));
#224294=CARTESIAN_POINT('Ctrl Pts',(5.87808428385329,-25.0491760405965,
0.));
#224295=CARTESIAN_POINT('Ctrl Pts',(5.87808428385329,-25.0491760405965,
12.));
#224296=CARTESIAN_POINT('Ctrl Pts',(5.8595306315681,-25.0285089498922,0.));
#224297=CARTESIAN_POINT('Ctrl Pts',(5.8595306315681,-25.0285089498922,12.));
#224298=CARTESIAN_POINT('Ctrl Pts',(5.84107051963073,-25.0078528200558,
0.));
#224299=CARTESIAN_POINT('Ctrl Pts',(5.84107051963073,-25.0078528200558,
12.));
#224300=CARTESIAN_POINT('Ctrl Pts',(5.82270406744213,-24.9872081752709,
0.));
#224301=CARTESIAN_POINT('Ctrl Pts',(5.82270406744213,-24.9872081752709,
12.));
#224302=CARTESIAN_POINT('Ctrl Pts',(5.80443138549747,-24.9665754954463,
0.));
#224303=CARTESIAN_POINT('Ctrl Pts',(5.80443138549747,-24.9665754954463,
12.));
#224304=CARTESIAN_POINT('Ctrl Pts',(5.78625257775702,-24.9459552293308,
0.));
#224305=CARTESIAN_POINT('Ctrl Pts',(5.78625257775702,-24.9459552293308,
12.));
#224306=CARTESIAN_POINT('Ctrl Pts',(5.76816774342236,-24.9253478043632,
0.));
#224307=CARTESIAN_POINT('Ctrl Pts',(5.76816774342236,-24.9253478043632,
12.));
#224308=CARTESIAN_POINT('Ctrl Pts',(5.75017697890812,-24.9047536376467,
0.));
#224309=CARTESIAN_POINT('Ctrl Pts',(5.75017697890812,-24.9047536376467,
12.));
#224310=CARTESIAN_POINT('Ctrl Pts',(5.73228037976926,-24.8841731467219,
0.));
#224311=CARTESIAN_POINT('Ctrl Pts',(5.73228037976926,-24.8841731467219,
12.));
#224312=CARTESIAN_POINT('Ctrl Pts',(5.71447804252019,-24.8636067597677,
0.));
#224313=CARTESIAN_POINT('Ctrl Pts',(5.71447804252019,-24.8636067597677,
12.));
#224314=CARTESIAN_POINT('Ctrl Pts',(5.69677006679429,-24.8430549277634,
0.));
#224315=CARTESIAN_POINT('Ctrl Pts',(5.69677006679429,-24.8430549277634,
12.));
#224316=CARTESIAN_POINT('Ctrl Pts',(5.67915655496524,-24.822518122386,0.));
#224317=CARTESIAN_POINT('Ctrl Pts',(5.67915655496524,-24.822518122386,12.));
#224318=CARTESIAN_POINT('Ctrl Pts',(5.66163761114903,-24.8019968304618,
0.));
#224319=CARTESIAN_POINT('Ctrl Pts',(5.66163761114903,-24.8019968304618,
12.));
#224320=CARTESIAN_POINT('Ctrl Pts',(5.64421334042247,-24.7814915496728,
0.));
#224321=CARTESIAN_POINT('Ctrl Pts',(5.64421334042247,-24.7814915496728,
12.));
#224322=CARTESIAN_POINT('Ctrl Pts',(5.62688384790918,-24.76100278357,0.));
#224323=CARTESIAN_POINT('Ctrl Pts',(5.62688384790918,-24.76100278357,12.));
#224324=CARTESIAN_POINT('Ctrl Pts',(5.60964923798494,-24.7405310372736,
0.));
#224325=CARTESIAN_POINT('Ctrl Pts',(5.60964923798494,-24.7405310372736,
12.));
#224326=CARTESIAN_POINT('Ctrl Pts',(5.59250961323995,-24.7200768119079,
0.));
#224327=CARTESIAN_POINT('Ctrl Pts',(5.59250961323995,-24.7200768119079,
12.));
#224328=CARTESIAN_POINT('Ctrl Pts',(5.57546507427766,-24.6996406035507,
0.));
#224329=CARTESIAN_POINT('Ctrl Pts',(5.57546507427766,-24.6996406035507,
12.));
#224330=CARTESIAN_POINT('Ctrl Pts',(5.55851572025389,-24.6792229061785,
0.));
#224331=CARTESIAN_POINT('Ctrl Pts',(5.55851572025389,-24.6792229061785,
12.));
#224332=CARTESIAN_POINT('Ctrl Pts',(5.54166164919592,-24.6588242134733,
0.));
#224333=CARTESIAN_POINT('Ctrl Pts',(5.54166164919592,-24.6588242134733,
12.));
#224334=CARTESIAN_POINT('Ctrl Pts',(5.52490295840996,-24.6384450211466,
0.));
#224335=CARTESIAN_POINT('Ctrl Pts',(5.52490295840996,-24.6384450211466,
12.));
#224336=CARTESIAN_POINT('Ctrl Pts',(5.50823974481959,-24.618085828918,0.));
#224337=CARTESIAN_POINT('Ctrl Pts',(5.50823974481959,-24.618085828918,12.));
#224338=CARTESIAN_POINT('Ctrl Pts',(5.49167210537235,-24.5977471429365,
0.));
#224339=CARTESIAN_POINT('Ctrl Pts',(5.49167210537235,-24.5977471429365,
12.));
#224340=CARTESIAN_POINT('Ctrl Pts',(5.47520013724403,-24.5774294770329,
0.));
#224341=CARTESIAN_POINT('Ctrl Pts',(5.47520013724403,-24.5774294770329,
12.));
#224342=CARTESIAN_POINT('Ctrl Pts',(5.45882393762244,-24.5571333514841,
0.));
#224343=CARTESIAN_POINT('Ctrl Pts',(5.45882393762244,-24.5571333514841,
12.));
#224344=CARTESIAN_POINT('Ctrl Pts',(5.44254360356865,-24.5368592922861,
0.));
#224345=CARTESIAN_POINT('Ctrl Pts',(5.44254360356865,-24.5368592922861,
12.));
#224346=CARTESIAN_POINT('Ctrl Pts',(5.42635923183411,-24.5166078302107,
0.));
#224347=CARTESIAN_POINT('Ctrl Pts',(5.42635923183411,-24.5166078302107,
12.));
#224348=CARTESIAN_POINT('Ctrl Pts',(5.41027091869242,-24.4963794999831,
0.));
#224349=CARTESIAN_POINT('Ctrl Pts',(5.41027091869242,-24.4963794999831,
12.));
#224350=CARTESIAN_POINT('Ctrl Pts',(5.3942787597383,-24.4761748393322,0.));
#224351=CARTESIAN_POINT('Ctrl Pts',(5.3942787597383,-24.4761748393322,12.));
#224352=CARTESIAN_POINT('Ctrl Pts',(5.37838284973706,-24.4559943883159,
0.));
#224353=CARTESIAN_POINT('Ctrl Pts',(5.37838284973706,-24.4559943883159,
12.));
#224354=CARTESIAN_POINT('Ctrl Pts',(5.36258328273639,-24.4358386899152,
0.));
#224355=CARTESIAN_POINT('Ctrl Pts',(5.36258328273639,-24.4358386899152,
12.));
#224356=CARTESIAN_POINT('Ctrl Pts',(5.34688015213546,-24.4157082904615,
0.));
#224357=CARTESIAN_POINT('Ctrl Pts',(5.34688015213546,-24.4157082904615,
12.));
#224358=CARTESIAN_POINT('Ctrl Pts',(5.33127355076036,-24.3956037401293,
0.));
#224359=CARTESIAN_POINT('Ctrl Pts',(5.33127355076036,-24.3956037401293,
12.));
#224360=CARTESIAN_POINT('Ctrl Pts',(5.31576357092524,-24.3755255933917,
0.));
#224361=CARTESIAN_POINT('Ctrl Pts',(5.31576357092524,-24.3755255933917,
12.));
#224362=CARTESIAN_POINT('Ctrl Pts',(5.30035030449058,-24.3554744095075,
0.));
#224363=CARTESIAN_POINT('Ctrl Pts',(5.30035030449058,-24.3554744095075,
12.));
#224364=CARTESIAN_POINT('Ctrl Pts',(5.28503384290644,-24.3354507529415,
0.));
#224365=CARTESIAN_POINT('Ctrl Pts',(5.28503384290644,-24.3354507529415,
12.));
#224366=CARTESIAN_POINT('Ctrl Pts',(5.26981427718796,-24.3154551932222,
0.));
#224367=CARTESIAN_POINT('Ctrl Pts',(5.26981427718796,-24.3154551932222,
12.));
#224368=CARTESIAN_POINT('Ctrl Pts',(5.25469169788855,-24.2954883048448,
0.));
#224369=CARTESIAN_POINT('Ctrl Pts',(5.25469169788855,-24.2954883048448,
12.));
#224370=CARTESIAN_POINT('Ctrl Pts',(5.23966619506289,-24.2755506671526,
0.));
#224371=CARTESIAN_POINT('Ctrl Pts',(5.23966619506289,-24.2755506671526,
12.));
#224372=CARTESIAN_POINT('Ctrl Pts',(5.22473785822441,-24.2556428642294,
0.));
#224373=CARTESIAN_POINT('Ctrl Pts',(5.22473785822441,-24.2556428642294,
12.));
#224374=CARTESIAN_POINT('Ctrl Pts',(5.20990677629173,-24.2357654847765,
0.));
#224375=CARTESIAN_POINT('Ctrl Pts',(5.20990677629173,-24.2357654847765,
12.));
#224376=CARTESIAN_POINT('Ctrl Pts',(5.19517303753642,-24.215919122017,0.));
#224377=CARTESIAN_POINT('Ctrl Pts',(5.19517303753642,-24.215919122017,12.));
#224378=CARTESIAN_POINT('Ctrl Pts',(5.18053672961392,-24.1961043738754,
0.));
#224379=CARTESIAN_POINT('Ctrl Pts',(5.18053672961392,-24.1961043738754,
12.));
#224380=CARTESIAN_POINT('Ctrl Pts',(5.16599793957979,-24.1763218431343,
0.));
#224381=CARTESIAN_POINT('Ctrl Pts',(5.16599793957979,-24.1763218431343,
12.));
#224382=CARTESIAN_POINT('Ctrl Pts',(5.15155675390075,-24.1565721375971,
0.));
#224383=CARTESIAN_POINT('Ctrl Pts',(5.15155675390075,-24.1565721375971,
12.));
#224384=CARTESIAN_POINT('Ctrl Pts',(5.13721325845744,-24.1368558702443,
0.));
#224385=CARTESIAN_POINT('Ctrl Pts',(5.13721325845744,-24.1368558702443,
12.));
#224386=CARTESIAN_POINT('Ctrl Pts',(5.12296753853859,-24.117173659394,0.));
#224387=CARTESIAN_POINT('Ctrl Pts',(5.12296753853859,-24.117173659394,12.));
#224388=CARTESIAN_POINT('Ctrl Pts',(5.10881967883132,-24.0975261288446,
0.));
#224389=CARTESIAN_POINT('Ctrl Pts',(5.10881967883132,-24.0975261288446,
12.));
#224390=CARTESIAN_POINT('Ctrl Pts',(5.09476976342625,-24.0779139079266,
0.));
#224391=CARTESIAN_POINT('Ctrl Pts',(5.09476976342625,-24.0779139079266,
12.));
#224392=CARTESIAN_POINT('Ctrl Pts',(5.08081787581276,-24.0583376315638,
0.));
#224393=CARTESIAN_POINT('Ctrl Pts',(5.08081787581276,-24.0583376315638,
12.));
#224394=CARTESIAN_POINT('Ctrl Pts',(5.06696409886641,-24.0387979403268,
0.));
#224395=CARTESIAN_POINT('Ctrl Pts',(5.06696409886641,-24.0387979403268,
12.));
#224396=CARTESIAN_POINT('Ctrl Pts',(5.05320851483065,-24.0192954804896,
0.));
#224397=CARTESIAN_POINT('Ctrl Pts',(5.05320851483065,-24.0192954804896,
12.));
#224398=CARTESIAN_POINT('Ctrl Pts',(5.03955120528521,-23.9998309040746,
0.));
#224399=CARTESIAN_POINT('Ctrl Pts',(5.03955120528521,-23.9998309040746,
12.));
#224400=CARTESIAN_POINT('Ctrl Pts',(5.02599225112454,-23.9804048689227,
0.));
#224401=CARTESIAN_POINT('Ctrl Pts',(5.02599225112454,-23.9804048689227,
12.));
#224402=CARTESIAN_POINT('Ctrl Pts',(5.01253173257452,-23.9610180388271,
0.));
#224403=CARTESIAN_POINT('Ctrl Pts',(5.01253173257452,-23.9610180388271,
12.));
#224404=CARTESIAN_POINT('Ctrl Pts',(4.99916972919306,-23.9416710836529,
0.));
#224405=CARTESIAN_POINT('Ctrl Pts',(4.99916972919306,-23.9416710836529,
12.));
#224406=CARTESIAN_POINT('Ctrl Pts',(4.98590631986532,-23.9223646794592,
0.));
#224407=CARTESIAN_POINT('Ctrl Pts',(4.98590631986532,-23.9223646794592,
12.));
#224408=CARTESIAN_POINT('Ctrl Pts',(4.97274158279226,-23.9030995086163,
0.));
#224409=CARTESIAN_POINT('Ctrl Pts',(4.97274158279226,-23.9030995086163,
12.));
#224410=CARTESIAN_POINT('Ctrl Pts',(4.9596755954656,-23.8838762599218,0.));
#224411=CARTESIAN_POINT('Ctrl Pts',(4.9596755954656,-23.8838762599218,12.));
#224412=CARTESIAN_POINT('Ctrl Pts',(4.9467084346586,-23.8646956287168,0.));
#224413=CARTESIAN_POINT('Ctrl Pts',(4.9467084346586,-23.8646956287168,12.));
#224414=CARTESIAN_POINT('Ctrl Pts',(4.93384017643432,-23.8455583170057,
0.));
#224415=CARTESIAN_POINT('Ctrl Pts',(4.93384017643432,-23.8455583170057,
12.));
#224416=CARTESIAN_POINT('Ctrl Pts',(4.92107089613968,-23.8264650335717,
0.));
#224417=CARTESIAN_POINT('Ctrl Pts',(4.92107089613968,-23.8264650335717,
12.));
#224418=CARTESIAN_POINT('Ctrl Pts',(4.90840066839344,-23.8074164940896,
0.));
#224419=CARTESIAN_POINT('Ctrl Pts',(4.90840066839344,-23.8074164940896,
12.));
#224420=CARTESIAN_POINT('Ctrl Pts',(4.89582956706775,-23.7884134212384,
0.));
#224421=CARTESIAN_POINT('Ctrl Pts',(4.89582956706775,-23.7884134212384,
12.));
#224422=CARTESIAN_POINT('Ctrl Pts',(4.88335766525573,-23.7694565448049,
0.));
#224423=CARTESIAN_POINT('Ctrl Pts',(4.88335766525573,-23.7694565448049,
12.));
#224424=CARTESIAN_POINT('Ctrl Pts',(4.87098503527152,-23.7505466018245,
0.));
#224425=CARTESIAN_POINT('Ctrl Pts',(4.87098503527152,-23.7505466018245,
12.));
#224426=CARTESIAN_POINT('Ctrl Pts',(4.85871174865499,-23.7316843367313,
0.));
#224427=CARTESIAN_POINT('Ctrl Pts',(4.85871174865499,-23.7316843367313,
12.));
#224428=CARTESIAN_POINT('Ctrl Pts',(4.84653787616425,-23.7128705015017,
0.));
#224429=CARTESIAN_POINT('Ctrl Pts',(4.84653787616425,-23.7128705015017,
12.));
#224430=CARTESIAN_POINT('Ctrl Pts',(4.83446348776265,-23.6941058557971,
0.));
#224431=CARTESIAN_POINT('Ctrl Pts',(4.83446348776265,-23.6941058557971,
12.));
#224432=CARTESIAN_POINT('Ctrl Pts',(4.82248865259562,-23.675391167102,0.));
#224433=CARTESIAN_POINT('Ctrl Pts',(4.82248865259562,-23.675391167102,12.));
#224434=CARTESIAN_POINT('Ctrl Pts',(4.81061343896432,-23.6567272108628,
0.));
#224435=CARTESIAN_POINT('Ctrl Pts',(4.81061343896432,-23.6567272108628,
12.));
#224436=CARTESIAN_POINT('Ctrl Pts',(4.7988379143322,-23.6381147706579,0.));
#224437=CARTESIAN_POINT('Ctrl Pts',(4.7988379143322,-23.6381147706579,12.));
#224438=CARTESIAN_POINT('Ctrl Pts',(4.78716214532097,-23.6195546383624,
0.));
#224439=CARTESIAN_POINT('Ctrl Pts',(4.78716214532097,-23.6195546383624,
12.));
#224440=CARTESIAN_POINT('Ctrl Pts',(4.77558619769872,-23.6010476143099,
0.));
#224441=CARTESIAN_POINT('Ctrl Pts',(4.77558619769872,-23.6010476143099,
12.));
#224442=CARTESIAN_POINT('Ctrl Pts',(4.76411013636251,-23.5825945074535,
0.));
#224443=CARTESIAN_POINT('Ctrl Pts',(4.76411013636251,-23.5825945074535,
12.));
#224444=CARTESIAN_POINT('Ctrl Pts',(4.75273402530617,-23.5641961355168,
0.));
#224445=CARTESIAN_POINT('Ctrl Pts',(4.75273402530617,-23.5641961355168,
12.));
#224446=CARTESIAN_POINT('Ctrl Pts',(4.74145792760698,-23.545853325171,0.));
#224447=CARTESIAN_POINT('Ctrl Pts',(4.74145792760698,-23.545853325171,12.));
#224448=CARTESIAN_POINT('Ctrl Pts',(4.73028190543029,-23.5275669122372,
0.));
#224449=CARTESIAN_POINT('Ctrl Pts',(4.73028190543029,-23.5275669122372,
12.));
#224450=CARTESIAN_POINT('Ctrl Pts',(4.71920602001901,-23.509337741878,0.));
#224451=CARTESIAN_POINT('Ctrl Pts',(4.71920602001901,-23.509337741878,12.));
#224452=CARTESIAN_POINT('Ctrl Pts',(4.70823033167818,-23.491166668789,0.));
#224453=CARTESIAN_POINT('Ctrl Pts',(4.70823033167818,-23.491166668789,12.));
#224454=CARTESIAN_POINT('Ctrl Pts',(4.69735489975024,-23.4730545573853,
0.));
#224455=CARTESIAN_POINT('Ctrl Pts',(4.69735489975024,-23.4730545573853,
12.));
#224456=CARTESIAN_POINT('Ctrl Pts',(4.68657978258303,-23.455002281986,0.));
#224457=CARTESIAN_POINT('Ctrl Pts',(4.68657978258303,-23.455002281986,12.));
#224458=CARTESIAN_POINT('Ctrl Pts',(4.67590503753058,-23.4370107270451,
0.));
#224459=CARTESIAN_POINT('Ctrl Pts',(4.67590503753058,-23.4370107270451,
12.));
#224460=CARTESIAN_POINT('Ctrl Pts',(4.6653307209467,-23.4190807873803,0.));
#224461=CARTESIAN_POINT('Ctrl Pts',(4.6653307209467,-23.4190807873803,12.));
#224462=CARTESIAN_POINT('Ctrl Pts',(4.65485688816924,-23.4012133683959,
0.));
#224463=CARTESIAN_POINT('Ctrl Pts',(4.65485688816924,-23.4012133683959,
12.));
#224464=CARTESIAN_POINT('Ctrl Pts',(4.6444835934993,-23.3834093863068,0.));
#224465=CARTESIAN_POINT('Ctrl Pts',(4.6444835934993,-23.3834093863068,12.));
#224466=CARTESIAN_POINT('Ctrl Pts',(4.63421089016541,-23.3656697683489,
0.));
#224467=CARTESIAN_POINT('Ctrl Pts',(4.63421089016541,-23.3656697683489,
12.));
#224468=CARTESIAN_POINT('Ctrl Pts',(4.62403883030805,-23.3479954530272,
0.));
#224469=CARTESIAN_POINT('Ctrl Pts',(4.62403883030805,-23.3479954530272,
12.));
#224470=CARTESIAN_POINT('Ctrl Pts',(4.6139674649783,-23.3303873903938,0.));
#224471=CARTESIAN_POINT('Ctrl Pts',(4.6139674649783,-23.3303873903938,12.));
#224472=CARTESIAN_POINT('Ctrl Pts',(4.60399684412163,-23.3128465423115,
0.));
#224473=CARTESIAN_POINT('Ctrl Pts',(4.60399684412163,-23.3128465423115,
12.));
#224474=CARTESIAN_POINT('Ctrl Pts',(4.5941270165575,-23.2953738827191,0.));
#224475=CARTESIAN_POINT('Ctrl Pts',(4.5941270165575,-23.2953738827191,12.));
#224476=CARTESIAN_POINT('Ctrl Pts',(4.5843580299469,-23.2779703978876,0.));
#224477=CARTESIAN_POINT('Ctrl Pts',(4.5843580299469,-23.2779703978876,12.));
#224478=CARTESIAN_POINT('Ctrl Pts',(4.57468993076097,-23.2606370866866,
0.));
#224479=CARTESIAN_POINT('Ctrl Pts',(4.57468993076097,-23.2606370866866,
12.));
#224480=CARTESIAN_POINT('Ctrl Pts',(4.56512276427839,-23.2433749609131,
0.));
#224481=CARTESIAN_POINT('Ctrl Pts',(4.56512276427839,-23.2433749609131,
12.));
#224482=CARTESIAN_POINT('Ctrl Pts',(4.55565657456975,-23.2261850456064,
0.));
#224483=CARTESIAN_POINT('Ctrl Pts',(4.55565657456975,-23.2261850456064,
12.));
#224484=CARTESIAN_POINT('Ctrl Pts',(4.54629140447544,-23.2090683793629,
0.));
#224485=CARTESIAN_POINT('Ctrl Pts',(4.54629140447544,-23.2090683793629,
12.));
#224486=CARTESIAN_POINT('Ctrl Pts',(4.53702729557566,-23.1920260146465,
0.));
#224487=CARTESIAN_POINT('Ctrl Pts',(4.53702729557566,-23.1920260146465,
12.));
#224488=CARTESIAN_POINT('Ctrl Pts',(4.52786428815014,-23.1750590180908,
0.));
#224489=CARTESIAN_POINT('Ctrl Pts',(4.52786428815014,-23.1750590180908,
12.));
#224490=CARTESIAN_POINT('Ctrl Pts',(4.51880242116748,-23.1581684708761,
0.));
#224491=CARTESIAN_POINT('Ctrl Pts',(4.51880242116748,-23.1581684708761,
12.));
#224492=CARTESIAN_POINT('Ctrl Pts',(4.5098417322706,-23.1413554691123,0.));
#224493=CARTESIAN_POINT('Ctrl Pts',(4.5098417322706,-23.1413554691123,12.));
#224494=CARTESIAN_POINT('Ctrl Pts',(4.50098225775171,-23.1246211242115,
0.));
#224495=CARTESIAN_POINT('Ctrl Pts',(4.50098225775171,-23.1246211242115,
12.));
#224496=CARTESIAN_POINT('Ctrl Pts',(4.49222403252216,-23.1079665632636,
0.));
#224497=CARTESIAN_POINT('Ctrl Pts',(4.49222403252216,-23.1079665632636,
12.));
#224498=CARTESIAN_POINT('Ctrl Pts',(4.48356709006788,-23.0913929293922,
0.));
#224499=CARTESIAN_POINT('Ctrl Pts',(4.48356709006788,-23.0913929293922,
12.));
#224500=CARTESIAN_POINT('Ctrl Pts',(4.47501146242856,-23.0749013821881,
0.));
#224501=CARTESIAN_POINT('Ctrl Pts',(4.47501146242856,-23.0749013821881,
12.));
#224502=CARTESIAN_POINT('Ctrl Pts',(4.4665571801823,-23.0584930981732,0.));
#224503=CARTESIAN_POINT('Ctrl Pts',(4.4665571801823,-23.0584930981732,12.));
#224504=CARTESIAN_POINT('Ctrl Pts',(4.45820427241683,-23.0421692712467,
0.));
#224505=CARTESIAN_POINT('Ctrl Pts',(4.45820427241683,-23.0421692712467,
12.));
#224506=CARTESIAN_POINT('Ctrl Pts',(4.44995276669686,-23.0259311131392,
0.));
#224507=CARTESIAN_POINT('Ctrl Pts',(4.44995276669686,-23.0259311131392,
12.));
#224508=CARTESIAN_POINT('Ctrl Pts',(4.44180268901643,-23.0097798538395,
0.));
#224509=CARTESIAN_POINT('Ctrl Pts',(4.44180268901643,-23.0097798538395,
12.));
#224510=CARTESIAN_POINT('Ctrl Pts',(4.43375406376879,-22.9937167421006,
0.));
#224511=CARTESIAN_POINT('Ctrl Pts',(4.43375406376879,-22.9937167421006,
12.));
#224512=CARTESIAN_POINT('Ctrl Pts',(4.42580691372751,-22.977743046002,0.));
#224513=CARTESIAN_POINT('Ctrl Pts',(4.42580691372751,-22.977743046002,12.));
#224514=CARTESIAN_POINT('Ctrl Pts',(4.41796126001302,-22.9618600534866,
0.));
#224515=CARTESIAN_POINT('Ctrl Pts',(4.41796126001302,-22.9618600534866,
12.));
#224516=CARTESIAN_POINT('Ctrl Pts',(4.41021712205553,-22.9460690729093,
0.));
#224517=CARTESIAN_POINT('Ctrl Pts',(4.41021712205553,-22.9460690729093,
12.));
#224518=CARTESIAN_POINT('Ctrl Pts',(4.40257451754323,-22.930371433555,0.));
#224519=CARTESIAN_POINT('Ctrl Pts',(4.40257451754323,-22.930371433555,12.));
#224520=CARTESIAN_POINT('Ctrl Pts',(4.39503346238473,-22.9147684862426,
0.));
#224521=CARTESIAN_POINT('Ctrl Pts',(4.39503346238473,-22.9147684862426,
12.));
#224522=CARTESIAN_POINT('Ctrl Pts',(4.38759397068405,-22.8992616040108,
0.));
#224523=CARTESIAN_POINT('Ctrl Pts',(4.38759397068405,-22.8992616040108,
12.));
#224524=CARTESIAN_POINT('Ctrl Pts',(4.38025605470092,-22.8838521827701,
0.));
#224525=CARTESIAN_POINT('Ctrl Pts',(4.38025605470092,-22.8838521827701,
12.));
#224526=CARTESIAN_POINT('Ctrl Pts',(4.37301972480745,-22.8685416419725,
0.));
#224527=CARTESIAN_POINT('Ctrl Pts',(4.37301972480745,-22.8685416419725,
12.));
#224528=CARTESIAN_POINT('Ctrl Pts',(4.36588498942997,-22.8533314252422,
0.));
#224529=CARTESIAN_POINT('Ctrl Pts',(4.36588498942997,-22.8533314252422,
12.));
#224530=CARTESIAN_POINT('Ctrl Pts',(4.35885185500546,-22.8382230011184,
0.));
#224531=CARTESIAN_POINT('Ctrl Pts',(4.35885185500546,-22.8382230011184,
12.));
#224532=CARTESIAN_POINT('Ctrl Pts',(4.3519203259479,-22.8232178638876,0.));
#224533=CARTESIAN_POINT('Ctrl Pts',(4.3519203259479,-22.8232178638876,12.));
#224534=CARTESIAN_POINT('Ctrl Pts',(4.34509040460062,-22.8083175343791,
0.));
#224535=CARTESIAN_POINT('Ctrl Pts',(4.34509040460062,-22.8083175343791,
12.));
#224536=CARTESIAN_POINT('Ctrl Pts',(4.33836209118446,-22.7935235607806,
0.));
#224537=CARTESIAN_POINT('Ctrl Pts',(4.33836209118446,-22.7935235607806,
12.));
#224538=CARTESIAN_POINT('Ctrl Pts',(4.33173538373189,-22.7788375194076,
0.));
#224539=CARTESIAN_POINT('Ctrl Pts',(4.33173538373189,-22.7788375194076,
12.));
#224540=CARTESIAN_POINT('Ctrl Pts',(4.32521027803754,-22.7642610156475,
0.));
#224541=CARTESIAN_POINT('Ctrl Pts',(4.32521027803754,-22.7642610156475,
12.));
#224542=CARTESIAN_POINT('Ctrl Pts',(4.31878676761235,-22.7497956849848,
0.));
#224543=CARTESIAN_POINT('Ctrl Pts',(4.31878676761235,-22.7497956849848,
12.));
#224544=CARTESIAN_POINT('Ctrl Pts',(4.31246484362549,-22.7354431939926,
0.));
#224545=CARTESIAN_POINT('Ctrl Pts',(4.31246484362549,-22.7354431939926,
12.));
#224546=CARTESIAN_POINT('Ctrl Pts',(4.30624449484069,-22.7212052413386,
0.));
#224547=CARTESIAN_POINT('Ctrl Pts',(4.30624449484069,-22.7212052413386,
12.));
#224548=CARTESIAN_POINT('Ctrl Pts',(4.3001257075406,-22.7070835587564,0.));
#224549=CARTESIAN_POINT('Ctrl Pts',(4.3001257075406,-22.7070835587564,12.));
#224550=CARTESIAN_POINT('Ctrl Pts',(4.29410846547056,-22.6930799122548,
0.));
#224551=CARTESIAN_POINT('Ctrl Pts',(4.29410846547056,-22.6930799122548,
12.));
#224552=CARTESIAN_POINT('Ctrl Pts',(4.28819274977763,-22.6791961033538,
0.));
#224553=CARTESIAN_POINT('Ctrl Pts',(4.28819274977763,-22.6791961033538,
12.));
#224554=CARTESIAN_POINT('Ctrl Pts',(4.28237853894058,-22.6654339703109,
0.));
#224555=CARTESIAN_POINT('Ctrl Pts',(4.28237853894058,-22.6654339703109,
12.));
#224556=CARTESIAN_POINT('Ctrl Pts',(4.2766658086912,-22.6517953893303,0.));
#224557=CARTESIAN_POINT('Ctrl Pts',(4.2766658086912,-22.6517953893303,12.));
#224558=CARTESIAN_POINT('Ctrl Pts',(4.27105453193004,-22.6382822758172,
0.));
#224559=CARTESIAN_POINT('Ctrl Pts',(4.27105453193004,-22.6382822758172,
12.));
#224560=CARTESIAN_POINT('Ctrl Pts',(4.26554467865576,-22.6248965859977,
0.));
#224561=CARTESIAN_POINT('Ctrl Pts',(4.26554467865576,-22.6248965859977,
12.));
#224562=CARTESIAN_POINT('Ctrl Pts',(4.26013621588305,-22.6116403184821,
0.));
#224563=CARTESIAN_POINT('Ctrl Pts',(4.26013621588305,-22.6116403184821,
12.));
#224564=CARTESIAN_POINT('Ctrl Pts',(4.25482910755481,-22.5985155158636,
0.));
#224565=CARTESIAN_POINT('Ctrl Pts',(4.25482910755481,-22.5985155158636,
12.));
#224566=CARTESIAN_POINT('Ctrl Pts',(4.24962331444177,-22.5855242662477,
0.));
#224567=CARTESIAN_POINT('Ctrl Pts',(4.24962331444177,-22.5855242662477,
12.));
#224568=CARTESIAN_POINT('Ctrl Pts',(4.24451879404851,-22.572668704992,0.));
#224569=CARTESIAN_POINT('Ctrl Pts',(4.24451879404851,-22.572668704992,12.));
#224570=CARTESIAN_POINT('Ctrl Pts',(4.23951550052522,-22.5599510166429,
0.));
#224571=CARTESIAN_POINT('Ctrl Pts',(4.23951550052522,-22.5599510166429,
12.));
#224572=CARTESIAN_POINT('Ctrl Pts',(4.23461338456712,-22.5473734368086,
0.));
#224573=CARTESIAN_POINT('Ctrl Pts',(4.23461338456712,-22.5473734368086,
12.));
#224574=CARTESIAN_POINT('Ctrl Pts',(4.22981239330733,-22.5349382540588,
0.));
#224575=CARTESIAN_POINT('Ctrl Pts',(4.22981239330733,-22.5349382540588,
12.));
#224576=CARTESIAN_POINT('Ctrl Pts',(4.22511247020041,-22.5226478117886,
0.));
#224577=CARTESIAN_POINT('Ctrl Pts',(4.22511247020041,-22.5226478117886,
12.));
#224578=CARTESIAN_POINT('Ctrl Pts',(4.22051355490196,-22.5105045108881,
0.));
#224579=CARTESIAN_POINT('Ctrl Pts',(4.22051355490196,-22.5105045108881,
12.));
#224580=CARTESIAN_POINT('Ctrl Pts',(4.21601558313906,-22.4985108124228,
0.));
#224581=CARTESIAN_POINT('Ctrl Pts',(4.21601558313906,-22.4985108124228,
12.));
#224582=CARTESIAN_POINT('Ctrl Pts',(4.21161848657428,-22.4866692403147,
0.));
#224583=CARTESIAN_POINT('Ctrl Pts',(4.21161848657428,-22.4866692403147,
12.));
#224584=CARTESIAN_POINT('Ctrl Pts',(4.20732219265648,-22.4749823839917,
0.));
#224585=CARTESIAN_POINT('Ctrl Pts',(4.20732219265648,-22.4749823839917,
12.));
#224586=CARTESIAN_POINT('Ctrl Pts',(4.20312662448174,-22.4634529011437,
0.));
#224587=CARTESIAN_POINT('Ctrl Pts',(4.20312662448174,-22.4634529011437,
12.));
#224588=CARTESIAN_POINT('Ctrl Pts',(4.19903170066358,-22.4520835205422,
0.));
#224589=CARTESIAN_POINT('Ctrl Pts',(4.19903170066358,-22.4520835205422,
12.));
#224590=CARTESIAN_POINT('Ctrl Pts',(4.1950373351886,-22.4408770448917,0.));
#224591=CARTESIAN_POINT('Ctrl Pts',(4.1950373351886,-22.4408770448917,12.));
#224592=CARTESIAN_POINT('Ctrl Pts',(4.19114343726932,-22.4298363535416,
0.));
#224593=CARTESIAN_POINT('Ctrl Pts',(4.19114343726932,-22.4298363535416,
12.));
#224594=CARTESIAN_POINT('Ctrl Pts',(4.18734991117707,-22.4189644056109,
0.));
#224595=CARTESIAN_POINT('Ctrl Pts',(4.18734991117707,-22.4189644056109,
12.));
#224596=CARTESIAN_POINT('Ctrl Pts',(4.18365665600839,-22.4082642454448,
0.));
#224597=CARTESIAN_POINT('Ctrl Pts',(4.18365665600839,-22.4082642454448,
12.));
#224598=CARTESIAN_POINT('Ctrl Pts',(4.18006356544879,-22.3977390078074,
0.));
#224599=CARTESIAN_POINT('Ctrl Pts',(4.18006356544879,-22.3977390078074,
12.));
#224600=CARTESIAN_POINT('Ctrl Pts',(4.17657052752834,-22.3873919231339,
0.));
#224601=CARTESIAN_POINT('Ctrl Pts',(4.17657052752834,-22.3873919231339,
12.));
#224602=CARTESIAN_POINT('Ctrl Pts',(4.17317742436162,-22.3772263228624,
0.));
#224603=CARTESIAN_POINT('Ctrl Pts',(4.17317742436162,-22.3772263228624,
12.));
#224604=CARTESIAN_POINT('Ctrl Pts',(4.16988413199469,-22.3672456427605,
0.));
#224605=CARTESIAN_POINT('Ctrl Pts',(4.16988413199469,-22.3672456427605,
12.));
#224606=CARTESIAN_POINT('Ctrl Pts',(4.16669052026602,-22.3574534257397,
0.));
#224607=CARTESIAN_POINT('Ctrl Pts',(4.16669052026602,-22.3574534257397,
12.));
#224608=CARTESIAN_POINT('Ctrl Pts',(4.1635964526318,-22.3478533253886,0.));
#224609=CARTESIAN_POINT('Ctrl Pts',(4.1635964526318,-22.3478533253886,12.));
#224610=CARTESIAN_POINT('Ctrl Pts',(4.16060178604153,-22.3384491078599,
0.));
#224611=CARTESIAN_POINT('Ctrl Pts',(4.16060178604153,-22.3384491078599,
12.));
#224612=CARTESIAN_POINT('Ctrl Pts',(4.15770637047882,-22.3292446628957,
0.));
#224613=CARTESIAN_POINT('Ctrl Pts',(4.15770637047882,-22.3292446628957,
12.));
#224614=CARTESIAN_POINT('Ctrl Pts',(4.15491004835278,-22.3202440186979,
0.));
#224615=CARTESIAN_POINT('Ctrl Pts',(4.15491004835278,-22.3202440186979,
12.));
#224616=CARTESIAN_POINT('Ctrl Pts',(4.15221265396992,-22.3114513545186,
0.));
#224617=CARTESIAN_POINT('Ctrl Pts',(4.15221265396992,-22.3114513545186,
12.));
#224618=CARTESIAN_POINT('Ctrl Pts',(4.14961401285525,-22.3028710166935,
0.));
#224619=CARTESIAN_POINT('Ctrl Pts',(4.14961401285525,-22.3028710166935,
12.));
#224620=CARTESIAN_POINT('Ctrl Pts',(4.14711394168559,-22.2945075198468,
0.));
#224621=CARTESIAN_POINT('Ctrl Pts',(4.14711394168559,-22.2945075198468,
12.));
#224622=CARTESIAN_POINT('Ctrl Pts',(4.14471224859295,-22.2863655389167,
0.));
#224623=CARTESIAN_POINT('Ctrl Pts',(4.14471224859295,-22.2863655389167,
12.));
#224624=CARTESIAN_POINT('Ctrl Pts',(4.14240873321982,-22.2784499072026,
0.));
#224625=CARTESIAN_POINT('Ctrl Pts',(4.14240873321982,-22.2784499072026,
12.));
#224626=CARTESIAN_POINT('Ctrl Pts',(4.14020318715987,-22.2707656042456,
0.));
#224627=CARTESIAN_POINT('Ctrl Pts',(4.14020318715987,-22.2707656042456,
12.));
#224628=CARTESIAN_POINT('Ctrl Pts',(4.13809539255418,-22.263317791397,0.));
#224629=CARTESIAN_POINT('Ctrl Pts',(4.13809539255418,-22.263317791397,12.));
#224630=CARTESIAN_POINT('Ctrl Pts',(4.13608511977226,-22.2561118708422,
0.));
#224631=CARTESIAN_POINT('Ctrl Pts',(4.13608511977226,-22.2561118708422,
12.));
#224632=CARTESIAN_POINT('Ctrl Pts',(4.13417212558808,-22.2491535317789,
0.));
#224633=CARTESIAN_POINT('Ctrl Pts',(4.13417212558808,-22.2491535317789,
12.));
#224634=CARTESIAN_POINT('Ctrl Pts',(4.1323561506016,-22.2424488153523,0.));
#224635=CARTESIAN_POINT('Ctrl Pts',(4.1323561506016,-22.2424488153523,12.));
#224636=CARTESIAN_POINT('Ctrl Pts',(4.13063692157499,-22.2360040565534,
0.));
#224637=CARTESIAN_POINT('Ctrl Pts',(4.13063692157499,-22.2360040565534,
12.));
#224638=CARTESIAN_POINT('Ctrl Pts',(4.12901415463378,-22.2298258043947,
0.));
#224639=CARTESIAN_POINT('Ctrl Pts',(4.12901415463378,-22.2298258043947,
12.));
#224640=CARTESIAN_POINT('Ctrl Pts',(4.12748755830099,-22.2239207458781,
0.));
#224641=CARTESIAN_POINT('Ctrl Pts',(4.12748755830099,-22.2239207458781,
12.));
#224642=CARTESIAN_POINT('Ctrl Pts',(4.12605683613299,-22.2182956401341,
0.));
#224643=CARTESIAN_POINT('Ctrl Pts',(4.12605683613299,-22.2182956401341,
12.));
#224644=CARTESIAN_POINT('Ctrl Pts',(4.12472167516602,-22.2129576146671,
0.));
#224645=CARTESIAN_POINT('Ctrl Pts',(4.12472167516602,-22.2129576146671,
12.));
#224646=CARTESIAN_POINT('Ctrl Pts',(4.12348173702024,-22.2079143941719,
0.));
#224647=CARTESIAN_POINT('Ctrl Pts',(4.12348173702024,-22.2079143941719,
12.));
#224648=CARTESIAN_POINT('Ctrl Pts',(4.12233664408237,-22.2031746532106,
0.));
#224649=CARTESIAN_POINT('Ctrl Pts',(4.12233664408237,-22.2031746532106,
12.));
#224650=CARTESIAN_POINT('Ctrl Pts',(4.12128598183533,-22.1987479618246,
0.));
#224651=CARTESIAN_POINT('Ctrl Pts',(4.12128598183533,-22.1987479618246,
12.));
#224652=CARTESIAN_POINT('Ctrl Pts',(4.12032932637738,-22.1946440958098,
0.));
#224653=CARTESIAN_POINT('Ctrl Pts',(4.12032932637738,-22.1946440958098,
12.));
#224654=CARTESIAN_POINT('Ctrl Pts',(4.11946626228623,-22.1908725908525,
0.));
#224655=CARTESIAN_POINT('Ctrl Pts',(4.11946626228623,-22.1908725908525,
12.));
#224656=CARTESIAN_POINT('Ctrl Pts',(4.11869641271752,-22.1874419861496,
0.));
#224657=CARTESIAN_POINT('Ctrl Pts',(4.11869641271752,-22.1874419861496,
12.));
#224658=CARTESIAN_POINT('Ctrl Pts',(4.11801938107464,-22.1843613164855,
0.));
#224659=CARTESIAN_POINT('Ctrl Pts',(4.11801938107464,-22.1843613164855,
12.));
#224660=CARTESIAN_POINT('Ctrl Pts',(4.11743469691765,-22.1816414985788,
0.));
#224661=CARTESIAN_POINT('Ctrl Pts',(4.11743469691765,-22.1816414985788,
12.));
#224662=CARTESIAN_POINT('Ctrl Pts',(4.11694173195041,-22.179297473024,0.));
#224663=CARTESIAN_POINT('Ctrl Pts',(4.11694173195041,-22.179297473024,12.));
#224664=CARTESIAN_POINT('Ctrl Pts',(4.11653973150558,-22.177347426894,0.));
#224665=CARTESIAN_POINT('Ctrl Pts',(4.11653973150558,-22.177347426894,12.));
#224666=CARTESIAN_POINT('Ctrl Pts',(4.11622797217066,-22.1758088296598,
0.));
#224667=CARTESIAN_POINT('Ctrl Pts',(4.11622797217066,-22.1758088296598,
12.));
#224668=CARTESIAN_POINT('Ctrl Pts',(4.11600589882767,-22.1746949858773,
0.));
#224669=CARTESIAN_POINT('Ctrl Pts',(4.11600589882767,-22.1746949858773,
12.));
#224670=CARTESIAN_POINT('Ctrl Pts',(4.11589976826061,-22.174148802123,0.));
#224671=CARTESIAN_POINT('Ctrl Pts',(4.11589976826061,-22.174148802123,12.));
#224672=CARTESIAN_POINT('Ctrl Pts',(4.1158603587821,-22.1739341411684,0.));
#224673=CARTESIAN_POINT('Ctrl Pts',(4.1158603587821,-22.1739341411684,12.));
#224674=CARTESIAN_POINT('Ctrl Pts',(4.11585194677412,-22.1738776823239,
0.));
#224675=CARTESIAN_POINT('Ctrl Pts',(4.11585194677412,-22.1738776823239,
12.));
#224676=CARTESIAN_POINT('Ctrl Pts',(4.11585220600461,-22.1738711152697,
0.));
#224677=CARTESIAN_POINT('Ctrl Pts',(4.11585220600461,-22.1738711152697,
12.));
#224678=CARTESIAN_POINT('',(6.08833931617698,-25.2771067246846,0.));
#224679=CARTESIAN_POINT('Ctrl Pts',(6.08833931617698,-25.2771067246846,
0.));
#224680=CARTESIAN_POINT('Ctrl Pts',(6.08441489609824,-25.2729539149479,
0.));
#224681=CARTESIAN_POINT('Ctrl Pts',(6.07657531787577,-25.2646490489816,
0.));
#224682=CARTESIAN_POINT('Ctrl Pts',(6.06484373634696,-25.2521940105523,
0.));
#224683=CARTESIAN_POINT('Ctrl Pts',(6.04925720151412,-25.2355918138798,
0.));
#224684=CARTESIAN_POINT('Ctrl Pts',(6.02986667390187,-25.2148466201368,
0.));
#224685=CARTESIAN_POINT('Ctrl Pts',(6.0105688180476,-25.1941090269638,0.));
#224686=CARTESIAN_POINT('Ctrl Pts',(5.99136367859838,-25.1733791296154,
0.));
#224687=CARTESIAN_POINT('Ctrl Pts',(5.97225131495636,-25.1526570863065,
0.));
#224688=CARTESIAN_POINT('Ctrl Pts',(5.95323180187347,-25.1319431317273,
0.));
#224689=CARTESIAN_POINT('Ctrl Pts',(5.93430523086776,-25.1112375971182,
0.));
#224690=CARTESIAN_POINT('Ctrl Pts',(5.91547170844382,-25.0905409050863,
0.));
#224691=CARTESIAN_POINT('Ctrl Pts',(5.89673135155458,-25.0698535426593,
0.));
#224692=CARTESIAN_POINT('Ctrl Pts',(5.87808428385329,-25.0491760405965,
0.));
#224693=CARTESIAN_POINT('Ctrl Pts',(5.8595306315681,-25.0285089498922,0.));
#224694=CARTESIAN_POINT('Ctrl Pts',(5.84107051963073,-25.0078528200558,
0.));
#224695=CARTESIAN_POINT('Ctrl Pts',(5.82270406744213,-24.9872081752709,
0.));
#224696=CARTESIAN_POINT('Ctrl Pts',(5.80443138549747,-24.9665754954463,
0.));
#224697=CARTESIAN_POINT('Ctrl Pts',(5.78625257775702,-24.9459552293308,
0.));
#224698=CARTESIAN_POINT('Ctrl Pts',(5.76816774342236,-24.9253478043632,
0.));
#224699=CARTESIAN_POINT('Ctrl Pts',(5.75017697890812,-24.9047536376467,
0.));
#224700=CARTESIAN_POINT('Ctrl Pts',(5.73228037976926,-24.8841731467219,
0.));
#224701=CARTESIAN_POINT('Ctrl Pts',(5.71447804252019,-24.8636067597677,
0.));
#224702=CARTESIAN_POINT('Ctrl Pts',(5.69677006679429,-24.8430549277634,
0.));
#224703=CARTESIAN_POINT('Ctrl Pts',(5.67915655496524,-24.822518122386,0.));
#224704=CARTESIAN_POINT('Ctrl Pts',(5.66163761114903,-24.8019968304618,
0.));
#224705=CARTESIAN_POINT('Ctrl Pts',(5.64421334042247,-24.7814915496728,
0.));
#224706=CARTESIAN_POINT('Ctrl Pts',(5.62688384790918,-24.76100278357,0.));
#224707=CARTESIAN_POINT('Ctrl Pts',(5.60964923798494,-24.7405310372736,
0.));
#224708=CARTESIAN_POINT('Ctrl Pts',(5.59250961323995,-24.7200768119079,
0.));
#224709=CARTESIAN_POINT('Ctrl Pts',(5.57546507427766,-24.6996406035507,
0.));
#224710=CARTESIAN_POINT('Ctrl Pts',(5.55851572025389,-24.6792229061785,
0.));
#224711=CARTESIAN_POINT('Ctrl Pts',(5.54166164919592,-24.6588242134733,
0.));
#224712=CARTESIAN_POINT('Ctrl Pts',(5.52490295840996,-24.6384450211466,
0.));
#224713=CARTESIAN_POINT('Ctrl Pts',(5.50823974481959,-24.618085828918,0.));
#224714=CARTESIAN_POINT('Ctrl Pts',(5.49167210537235,-24.5977471429365,
0.));
#224715=CARTESIAN_POINT('Ctrl Pts',(5.47520013724403,-24.5774294770329,
0.));
#224716=CARTESIAN_POINT('Ctrl Pts',(5.45882393762244,-24.5571333514841,
0.));
#224717=CARTESIAN_POINT('Ctrl Pts',(5.44254360356865,-24.5368592922861,
0.));
#224718=CARTESIAN_POINT('Ctrl Pts',(5.42635923183411,-24.5166078302107,
0.));
#224719=CARTESIAN_POINT('Ctrl Pts',(5.41027091869242,-24.4963794999831,
0.));
#224720=CARTESIAN_POINT('Ctrl Pts',(5.3942787597383,-24.4761748393322,0.));
#224721=CARTESIAN_POINT('Ctrl Pts',(5.37838284973706,-24.4559943883159,
0.));
#224722=CARTESIAN_POINT('Ctrl Pts',(5.36258328273639,-24.4358386899152,
0.));
#224723=CARTESIAN_POINT('Ctrl Pts',(5.34688015213546,-24.4157082904615,
0.));
#224724=CARTESIAN_POINT('Ctrl Pts',(5.33127355076036,-24.3956037401293,
0.));
#224725=CARTESIAN_POINT('Ctrl Pts',(5.31576357092524,-24.3755255933917,
0.));
#224726=CARTESIAN_POINT('Ctrl Pts',(5.30035030449058,-24.3554744095075,
0.));
#224727=CARTESIAN_POINT('Ctrl Pts',(5.28503384290644,-24.3354507529415,
0.));
#224728=CARTESIAN_POINT('Ctrl Pts',(5.26981427718796,-24.3154551932222,
0.));
#224729=CARTESIAN_POINT('Ctrl Pts',(5.25469169788855,-24.2954883048448,
0.));
#224730=CARTESIAN_POINT('Ctrl Pts',(5.23966619506289,-24.2755506671526,
0.));
#224731=CARTESIAN_POINT('Ctrl Pts',(5.22473785822441,-24.2556428642294,
0.));
#224732=CARTESIAN_POINT('Ctrl Pts',(5.20990677629173,-24.2357654847765,
0.));
#224733=CARTESIAN_POINT('Ctrl Pts',(5.19517303753642,-24.215919122017,0.));
#224734=CARTESIAN_POINT('Ctrl Pts',(5.18053672961392,-24.1961043738754,
0.));
#224735=CARTESIAN_POINT('Ctrl Pts',(5.16599793957979,-24.1763218431343,
0.));
#224736=CARTESIAN_POINT('Ctrl Pts',(5.15155675390075,-24.1565721375971,
0.));
#224737=CARTESIAN_POINT('Ctrl Pts',(5.13721325845744,-24.1368558702443,
0.));
#224738=CARTESIAN_POINT('Ctrl Pts',(5.12296753853859,-24.117173659394,0.));
#224739=CARTESIAN_POINT('Ctrl Pts',(5.10881967883132,-24.0975261288446,
0.));
#224740=CARTESIAN_POINT('Ctrl Pts',(5.09476976342625,-24.0779139079266,
0.));
#224741=CARTESIAN_POINT('Ctrl Pts',(5.08081787581276,-24.0583376315638,
0.));
#224742=CARTESIAN_POINT('Ctrl Pts',(5.06696409886641,-24.0387979403268,
0.));
#224743=CARTESIAN_POINT('Ctrl Pts',(5.05320851483065,-24.0192954804896,
0.));
#224744=CARTESIAN_POINT('Ctrl Pts',(5.03955120528521,-23.9998309040746,
0.));
#224745=CARTESIAN_POINT('Ctrl Pts',(5.02599225112454,-23.9804048689227,
0.));
#224746=CARTESIAN_POINT('Ctrl Pts',(5.01253173257452,-23.9610180388271,
0.));
#224747=CARTESIAN_POINT('Ctrl Pts',(4.99916972919306,-23.9416710836529,
0.));
#224748=CARTESIAN_POINT('Ctrl Pts',(4.98590631986532,-23.9223646794592,
0.));
#224749=CARTESIAN_POINT('Ctrl Pts',(4.97274158279226,-23.9030995086163,
0.));
#224750=CARTESIAN_POINT('Ctrl Pts',(4.9596755954656,-23.8838762599218,0.));
#224751=CARTESIAN_POINT('Ctrl Pts',(4.9467084346586,-23.8646956287168,0.));
#224752=CARTESIAN_POINT('Ctrl Pts',(4.93384017643432,-23.8455583170057,
0.));
#224753=CARTESIAN_POINT('Ctrl Pts',(4.92107089613968,-23.8264650335717,
0.));
#224754=CARTESIAN_POINT('Ctrl Pts',(4.90840066839344,-23.8074164940896,
0.));
#224755=CARTESIAN_POINT('Ctrl Pts',(4.89582956706775,-23.7884134212384,
0.));
#224756=CARTESIAN_POINT('Ctrl Pts',(4.88335766525573,-23.7694565448049,
0.));
#224757=CARTESIAN_POINT('Ctrl Pts',(4.87098503527152,-23.7505466018245,
0.));
#224758=CARTESIAN_POINT('Ctrl Pts',(4.85871174865499,-23.7316843367313,
0.));
#224759=CARTESIAN_POINT('Ctrl Pts',(4.84653787616425,-23.7128705015017,
0.));
#224760=CARTESIAN_POINT('Ctrl Pts',(4.83446348776265,-23.6941058557971,
0.));
#224761=CARTESIAN_POINT('Ctrl Pts',(4.82248865259562,-23.675391167102,0.));
#224762=CARTESIAN_POINT('Ctrl Pts',(4.81061343896432,-23.6567272108628,
0.));
#224763=CARTESIAN_POINT('Ctrl Pts',(4.7988379143322,-23.6381147706579,0.));
#224764=CARTESIAN_POINT('Ctrl Pts',(4.78716214532097,-23.6195546383624,
0.));
#224765=CARTESIAN_POINT('Ctrl Pts',(4.77558619769872,-23.6010476143099,
0.));
#224766=CARTESIAN_POINT('Ctrl Pts',(4.76411013636251,-23.5825945074535,
0.));
#224767=CARTESIAN_POINT('Ctrl Pts',(4.75273402530617,-23.5641961355168,
0.));
#224768=CARTESIAN_POINT('Ctrl Pts',(4.74145792760698,-23.545853325171,0.));
#224769=CARTESIAN_POINT('Ctrl Pts',(4.73028190543029,-23.5275669122372,
0.));
#224770=CARTESIAN_POINT('Ctrl Pts',(4.71920602001901,-23.509337741878,0.));
#224771=CARTESIAN_POINT('Ctrl Pts',(4.70823033167818,-23.491166668789,0.));
#224772=CARTESIAN_POINT('Ctrl Pts',(4.69735489975024,-23.4730545573853,
0.));
#224773=CARTESIAN_POINT('Ctrl Pts',(4.68657978258303,-23.455002281986,0.));
#224774=CARTESIAN_POINT('Ctrl Pts',(4.67590503753058,-23.4370107270451,
0.));
#224775=CARTESIAN_POINT('Ctrl Pts',(4.6653307209467,-23.4190807873803,0.));
#224776=CARTESIAN_POINT('Ctrl Pts',(4.65485688816924,-23.4012133683959,
0.));
#224777=CARTESIAN_POINT('Ctrl Pts',(4.6444835934993,-23.3834093863068,0.));
#224778=CARTESIAN_POINT('Ctrl Pts',(4.63421089016541,-23.3656697683489,
0.));
#224779=CARTESIAN_POINT('Ctrl Pts',(4.62403883030805,-23.3479954530272,
0.));
#224780=CARTESIAN_POINT('Ctrl Pts',(4.6139674649783,-23.3303873903938,0.));
#224781=CARTESIAN_POINT('Ctrl Pts',(4.60399684412163,-23.3128465423115,
0.));
#224782=CARTESIAN_POINT('Ctrl Pts',(4.5941270165575,-23.2953738827191,0.));
#224783=CARTESIAN_POINT('Ctrl Pts',(4.5843580299469,-23.2779703978876,0.));
#224784=CARTESIAN_POINT('Ctrl Pts',(4.57468993076097,-23.2606370866866,
0.));
#224785=CARTESIAN_POINT('Ctrl Pts',(4.56512276427839,-23.2433749609131,
0.));
#224786=CARTESIAN_POINT('Ctrl Pts',(4.55565657456975,-23.2261850456064,
0.));
#224787=CARTESIAN_POINT('Ctrl Pts',(4.54629140447544,-23.2090683793629,
0.));
#224788=CARTESIAN_POINT('Ctrl Pts',(4.53702729557566,-23.1920260146465,
0.));
#224789=CARTESIAN_POINT('Ctrl Pts',(4.52786428815014,-23.1750590180908,
0.));
#224790=CARTESIAN_POINT('Ctrl Pts',(4.51880242116748,-23.1581684708761,
0.));
#224791=CARTESIAN_POINT('Ctrl Pts',(4.5098417322706,-23.1413554691123,0.));
#224792=CARTESIAN_POINT('Ctrl Pts',(4.50098225775171,-23.1246211242115,
0.));
#224793=CARTESIAN_POINT('Ctrl Pts',(4.49222403252216,-23.1079665632636,
0.));
#224794=CARTESIAN_POINT('Ctrl Pts',(4.48356709006788,-23.0913929293922,
0.));
#224795=CARTESIAN_POINT('Ctrl Pts',(4.47501146242856,-23.0749013821881,
0.));
#224796=CARTESIAN_POINT('Ctrl Pts',(4.4665571801823,-23.0584930981732,0.));
#224797=CARTESIAN_POINT('Ctrl Pts',(4.45820427241683,-23.0421692712467,
0.));
#224798=CARTESIAN_POINT('Ctrl Pts',(4.44995276669686,-23.0259311131392,
0.));
#224799=CARTESIAN_POINT('Ctrl Pts',(4.44180268901643,-23.0097798538395,
0.));
#224800=CARTESIAN_POINT('Ctrl Pts',(4.43375406376879,-22.9937167421006,
0.));
#224801=CARTESIAN_POINT('Ctrl Pts',(4.42580691372751,-22.977743046002,0.));
#224802=CARTESIAN_POINT('Ctrl Pts',(4.41796126001302,-22.9618600534866,
0.));
#224803=CARTESIAN_POINT('Ctrl Pts',(4.41021712205553,-22.9460690729093,
0.));
#224804=CARTESIAN_POINT('Ctrl Pts',(4.40257451754323,-22.930371433555,0.));
#224805=CARTESIAN_POINT('Ctrl Pts',(4.39503346238473,-22.9147684862426,
0.));
#224806=CARTESIAN_POINT('Ctrl Pts',(4.38759397068405,-22.8992616040108,
0.));
#224807=CARTESIAN_POINT('Ctrl Pts',(4.38025605470092,-22.8838521827701,
0.));
#224808=CARTESIAN_POINT('Ctrl Pts',(4.37301972480745,-22.8685416419725,
0.));
#224809=CARTESIAN_POINT('Ctrl Pts',(4.36588498942997,-22.8533314252422,
0.));
#224810=CARTESIAN_POINT('Ctrl Pts',(4.35885185500546,-22.8382230011184,
0.));
#224811=CARTESIAN_POINT('Ctrl Pts',(4.3519203259479,-22.8232178638876,0.));
#224812=CARTESIAN_POINT('Ctrl Pts',(4.34509040460062,-22.8083175343791,
0.));
#224813=CARTESIAN_POINT('Ctrl Pts',(4.33836209118446,-22.7935235607806,
0.));
#224814=CARTESIAN_POINT('Ctrl Pts',(4.33173538373189,-22.7788375194076,
0.));
#224815=CARTESIAN_POINT('Ctrl Pts',(4.32521027803754,-22.7642610156475,
0.));
#224816=CARTESIAN_POINT('Ctrl Pts',(4.31878676761235,-22.7497956849848,
0.));
#224817=CARTESIAN_POINT('Ctrl Pts',(4.31246484362549,-22.7354431939926,
0.));
#224818=CARTESIAN_POINT('Ctrl Pts',(4.30624449484069,-22.7212052413386,
0.));
#224819=CARTESIAN_POINT('Ctrl Pts',(4.3001257075406,-22.7070835587564,0.));
#224820=CARTESIAN_POINT('Ctrl Pts',(4.29410846547056,-22.6930799122548,
0.));
#224821=CARTESIAN_POINT('Ctrl Pts',(4.28819274977763,-22.6791961033538,
0.));
#224822=CARTESIAN_POINT('Ctrl Pts',(4.28237853894058,-22.6654339703109,
0.));
#224823=CARTESIAN_POINT('Ctrl Pts',(4.2766658086912,-22.6517953893303,0.));
#224824=CARTESIAN_POINT('Ctrl Pts',(4.27105453193004,-22.6382822758172,
0.));
#224825=CARTESIAN_POINT('Ctrl Pts',(4.26554467865576,-22.6248965859977,
0.));
#224826=CARTESIAN_POINT('Ctrl Pts',(4.26013621588305,-22.6116403184821,
0.));
#224827=CARTESIAN_POINT('Ctrl Pts',(4.25482910755481,-22.5985155158636,
0.));
#224828=CARTESIAN_POINT('Ctrl Pts',(4.24962331444177,-22.5855242662477,
0.));
#224829=CARTESIAN_POINT('Ctrl Pts',(4.24451879404851,-22.572668704992,0.));
#224830=CARTESIAN_POINT('Ctrl Pts',(4.23951550052522,-22.5599510166429,
0.));
#224831=CARTESIAN_POINT('Ctrl Pts',(4.23461338456712,-22.5473734368086,
0.));
#224832=CARTESIAN_POINT('Ctrl Pts',(4.22981239330733,-22.5349382540588,
0.));
#224833=CARTESIAN_POINT('Ctrl Pts',(4.22511247020041,-22.5226478117886,
0.));
#224834=CARTESIAN_POINT('Ctrl Pts',(4.22051355490196,-22.5105045108881,
0.));
#224835=CARTESIAN_POINT('Ctrl Pts',(4.21601558313906,-22.4985108124228,
0.));
#224836=CARTESIAN_POINT('Ctrl Pts',(4.21161848657428,-22.4866692403147,
0.));
#224837=CARTESIAN_POINT('Ctrl Pts',(4.20732219265648,-22.4749823839917,
0.));
#224838=CARTESIAN_POINT('Ctrl Pts',(4.20312662448174,-22.4634529011437,
0.));
#224839=CARTESIAN_POINT('Ctrl Pts',(4.19903170066358,-22.4520835205422,
0.));
#224840=CARTESIAN_POINT('Ctrl Pts',(4.1950373351886,-22.4408770448917,0.));
#224841=CARTESIAN_POINT('Ctrl Pts',(4.19114343726932,-22.4298363535416,
0.));
#224842=CARTESIAN_POINT('Ctrl Pts',(4.18734991117707,-22.4189644056109,
0.));
#224843=CARTESIAN_POINT('Ctrl Pts',(4.18365665600839,-22.4082642454448,
0.));
#224844=CARTESIAN_POINT('Ctrl Pts',(4.18006356544879,-22.3977390078074,
0.));
#224845=CARTESIAN_POINT('Ctrl Pts',(4.17657052752834,-22.3873919231339,
0.));
#224846=CARTESIAN_POINT('Ctrl Pts',(4.17317742436162,-22.3772263228624,
0.));
#224847=CARTESIAN_POINT('Ctrl Pts',(4.16988413199469,-22.3672456427605,
0.));
#224848=CARTESIAN_POINT('Ctrl Pts',(4.16669052026602,-22.3574534257397,
0.));
#224849=CARTESIAN_POINT('Ctrl Pts',(4.1635964526318,-22.3478533253886,0.));
#224850=CARTESIAN_POINT('Ctrl Pts',(4.16060178604153,-22.3384491078599,
0.));
#224851=CARTESIAN_POINT('Ctrl Pts',(4.15770637047882,-22.3292446628957,
0.));
#224852=CARTESIAN_POINT('Ctrl Pts',(4.15491004835278,-22.3202440186979,
0.));
#224853=CARTESIAN_POINT('Ctrl Pts',(4.15221265396992,-22.3114513545186,
0.));
#224854=CARTESIAN_POINT('Ctrl Pts',(4.14961401285525,-22.3028710166935,
0.));
#224855=CARTESIAN_POINT('Ctrl Pts',(4.14711394168559,-22.2945075198468,
0.));
#224856=CARTESIAN_POINT('Ctrl Pts',(4.14471224859295,-22.2863655389167,
0.));
#224857=CARTESIAN_POINT('Ctrl Pts',(4.14240873321982,-22.2784499072026,
0.));
#224858=CARTESIAN_POINT('Ctrl Pts',(4.14020318715987,-22.2707656042456,
0.));
#224859=CARTESIAN_POINT('Ctrl Pts',(4.13809539255418,-22.263317791397,0.));
#224860=CARTESIAN_POINT('Ctrl Pts',(4.13608511977226,-22.2561118708422,
0.));
#224861=CARTESIAN_POINT('Ctrl Pts',(4.13417212558808,-22.2491535317789,
0.));
#224862=CARTESIAN_POINT('Ctrl Pts',(4.1323561506016,-22.2424488153523,0.));
#224863=CARTESIAN_POINT('Ctrl Pts',(4.13063692157499,-22.2360040565534,
0.));
#224864=CARTESIAN_POINT('Ctrl Pts',(4.12901415463378,-22.2298258043947,
0.));
#224865=CARTESIAN_POINT('Ctrl Pts',(4.12748755830099,-22.2239207458781,
0.));
#224866=CARTESIAN_POINT('Ctrl Pts',(4.12605683613299,-22.2182956401341,
0.));
#224867=CARTESIAN_POINT('Ctrl Pts',(4.12472167516602,-22.2129576146671,
0.));
#224868=CARTESIAN_POINT('Ctrl Pts',(4.12348173702024,-22.2079143941719,
0.));
#224869=CARTESIAN_POINT('Ctrl Pts',(4.12233664408237,-22.2031746532106,
0.));
#224870=CARTESIAN_POINT('Ctrl Pts',(4.12128598183533,-22.1987479618246,
0.));
#224871=CARTESIAN_POINT('Ctrl Pts',(4.12032932637738,-22.1946440958098,
0.));
#224872=CARTESIAN_POINT('Ctrl Pts',(4.11946626228623,-22.1908725908525,
0.));
#224873=CARTESIAN_POINT('Ctrl Pts',(4.11869641271752,-22.1874419861496,
0.));
#224874=CARTESIAN_POINT('Ctrl Pts',(4.11801938107464,-22.1843613164855,
0.));
#224875=CARTESIAN_POINT('Ctrl Pts',(4.11743469691765,-22.1816414985788,
0.));
#224876=CARTESIAN_POINT('Ctrl Pts',(4.11694173195041,-22.179297473024,0.));
#224877=CARTESIAN_POINT('Ctrl Pts',(4.11653973150558,-22.177347426894,0.));
#224878=CARTESIAN_POINT('Ctrl Pts',(4.11622797217066,-22.1758088296598,
0.));
#224879=CARTESIAN_POINT('Ctrl Pts',(4.11600589882767,-22.1746949858773,
0.));
#224880=CARTESIAN_POINT('Ctrl Pts',(4.11589976826061,-22.174148802123,0.));
#224881=CARTESIAN_POINT('Ctrl Pts',(4.1158603587821,-22.1739341411684,0.));
#224882=CARTESIAN_POINT('Ctrl Pts',(4.11585194677412,-22.1738776823239,
0.));
#224883=CARTESIAN_POINT('Ctrl Pts',(4.11585220600461,-22.1738711152697,
0.));
#224884=CARTESIAN_POINT('',(6.08833931617698,-25.2771067246846,12.));
#224885=CARTESIAN_POINT('',(6.08833931617698,-25.2771067246846,0.));
#224886=CARTESIAN_POINT('Ctrl Pts',(4.11585220600461,-22.1738711152697,
12.));
#224887=CARTESIAN_POINT('Ctrl Pts',(4.11585194677412,-22.1738776823239,
12.));
#224888=CARTESIAN_POINT('Ctrl Pts',(4.1158603587821,-22.1739341411684,12.));
#224889=CARTESIAN_POINT('Ctrl Pts',(4.11589976826061,-22.174148802123,12.));
#224890=CARTESIAN_POINT('Ctrl Pts',(4.11600589882767,-22.1746949858773,
12.));
#224891=CARTESIAN_POINT('Ctrl Pts',(4.11622797217066,-22.1758088296598,
12.));
#224892=CARTESIAN_POINT('Ctrl Pts',(4.11653973150558,-22.177347426894,12.));
#224893=CARTESIAN_POINT('Ctrl Pts',(4.11694173195041,-22.179297473024,12.));
#224894=CARTESIAN_POINT('Ctrl Pts',(4.11743469691765,-22.1816414985788,
12.));
#224895=CARTESIAN_POINT('Ctrl Pts',(4.11801938107464,-22.1843613164855,
12.));
#224896=CARTESIAN_POINT('Ctrl Pts',(4.11869641271752,-22.1874419861496,
12.));
#224897=CARTESIAN_POINT('Ctrl Pts',(4.11946626228623,-22.1908725908525,
12.));
#224898=CARTESIAN_POINT('Ctrl Pts',(4.12032932637738,-22.1946440958098,
12.));
#224899=CARTESIAN_POINT('Ctrl Pts',(4.12128598183533,-22.1987479618246,
12.));
#224900=CARTESIAN_POINT('Ctrl Pts',(4.12233664408237,-22.2031746532106,
12.));
#224901=CARTESIAN_POINT('Ctrl Pts',(4.12348173702024,-22.2079143941719,
12.));
#224902=CARTESIAN_POINT('Ctrl Pts',(4.12472167516602,-22.2129576146671,
12.));
#224903=CARTESIAN_POINT('Ctrl Pts',(4.12605683613299,-22.2182956401341,
12.));
#224904=CARTESIAN_POINT('Ctrl Pts',(4.12748755830099,-22.2239207458781,
12.));
#224905=CARTESIAN_POINT('Ctrl Pts',(4.12901415463378,-22.2298258043947,
12.));
#224906=CARTESIAN_POINT('Ctrl Pts',(4.13063692157499,-22.2360040565534,
12.));
#224907=CARTESIAN_POINT('Ctrl Pts',(4.1323561506016,-22.2424488153523,12.));
#224908=CARTESIAN_POINT('Ctrl Pts',(4.13417212558808,-22.2491535317789,
12.));
#224909=CARTESIAN_POINT('Ctrl Pts',(4.13608511977226,-22.2561118708422,
12.));
#224910=CARTESIAN_POINT('Ctrl Pts',(4.13809539255418,-22.263317791397,12.));
#224911=CARTESIAN_POINT('Ctrl Pts',(4.14020318715987,-22.2707656042456,
12.));
#224912=CARTESIAN_POINT('Ctrl Pts',(4.14240873321982,-22.2784499072026,
12.));
#224913=CARTESIAN_POINT('Ctrl Pts',(4.14471224859295,-22.2863655389167,
12.));
#224914=CARTESIAN_POINT('Ctrl Pts',(4.14711394168559,-22.2945075198468,
12.));
#224915=CARTESIAN_POINT('Ctrl Pts',(4.14961401285525,-22.3028710166935,
12.));
#224916=CARTESIAN_POINT('Ctrl Pts',(4.15221265396992,-22.3114513545186,
12.));
#224917=CARTESIAN_POINT('Ctrl Pts',(4.15491004835278,-22.3202440186979,
12.));
#224918=CARTESIAN_POINT('Ctrl Pts',(4.15770637047882,-22.3292446628957,
12.));
#224919=CARTESIAN_POINT('Ctrl Pts',(4.16060178604153,-22.3384491078599,
12.));
#224920=CARTESIAN_POINT('Ctrl Pts',(4.1635964526318,-22.3478533253886,12.));
#224921=CARTESIAN_POINT('Ctrl Pts',(4.16669052026602,-22.3574534257397,
12.));
#224922=CARTESIAN_POINT('Ctrl Pts',(4.16988413199469,-22.3672456427605,
12.));
#224923=CARTESIAN_POINT('Ctrl Pts',(4.17317742436162,-22.3772263228624,
12.));
#224924=CARTESIAN_POINT('Ctrl Pts',(4.17657052752834,-22.3873919231339,
12.));
#224925=CARTESIAN_POINT('Ctrl Pts',(4.18006356544879,-22.3977390078074,
12.));
#224926=CARTESIAN_POINT('Ctrl Pts',(4.18365665600839,-22.4082642454448,
12.));
#224927=CARTESIAN_POINT('Ctrl Pts',(4.18734991117707,-22.4189644056109,
12.));
#224928=CARTESIAN_POINT('Ctrl Pts',(4.19114343726932,-22.4298363535416,
12.));
#224929=CARTESIAN_POINT('Ctrl Pts',(4.1950373351886,-22.4408770448917,12.));
#224930=CARTESIAN_POINT('Ctrl Pts',(4.19903170066358,-22.4520835205422,
12.));
#224931=CARTESIAN_POINT('Ctrl Pts',(4.20312662448174,-22.4634529011437,
12.));
#224932=CARTESIAN_POINT('Ctrl Pts',(4.20732219265648,-22.4749823839917,
12.));
#224933=CARTESIAN_POINT('Ctrl Pts',(4.21161848657428,-22.4866692403147,
12.));
#224934=CARTESIAN_POINT('Ctrl Pts',(4.21601558313906,-22.4985108124228,
12.));
#224935=CARTESIAN_POINT('Ctrl Pts',(4.22051355490196,-22.5105045108881,
12.));
#224936=CARTESIAN_POINT('Ctrl Pts',(4.22511247020041,-22.5226478117886,
12.));
#224937=CARTESIAN_POINT('Ctrl Pts',(4.22981239330733,-22.5349382540588,
12.));
#224938=CARTESIAN_POINT('Ctrl Pts',(4.23461338456712,-22.5473734368086,
12.));
#224939=CARTESIAN_POINT('Ctrl Pts',(4.23951550052522,-22.5599510166429,
12.));
#224940=CARTESIAN_POINT('Ctrl Pts',(4.24451879404851,-22.572668704992,12.));
#224941=CARTESIAN_POINT('Ctrl Pts',(4.24962331444177,-22.5855242662477,
12.));
#224942=CARTESIAN_POINT('Ctrl Pts',(4.25482910755481,-22.5985155158636,
12.));
#224943=CARTESIAN_POINT('Ctrl Pts',(4.26013621588305,-22.6116403184821,
12.));
#224944=CARTESIAN_POINT('Ctrl Pts',(4.26554467865576,-22.6248965859977,
12.));
#224945=CARTESIAN_POINT('Ctrl Pts',(4.27105453193004,-22.6382822758172,
12.));
#224946=CARTESIAN_POINT('Ctrl Pts',(4.2766658086912,-22.6517953893303,12.));
#224947=CARTESIAN_POINT('Ctrl Pts',(4.28237853894058,-22.6654339703109,
12.));
#224948=CARTESIAN_POINT('Ctrl Pts',(4.28819274977763,-22.6791961033538,
12.));
#224949=CARTESIAN_POINT('Ctrl Pts',(4.29410846547056,-22.6930799122548,
12.));
#224950=CARTESIAN_POINT('Ctrl Pts',(4.3001257075406,-22.7070835587564,12.));
#224951=CARTESIAN_POINT('Ctrl Pts',(4.30624449484069,-22.7212052413386,
12.));
#224952=CARTESIAN_POINT('Ctrl Pts',(4.31246484362549,-22.7354431939926,
12.));
#224953=CARTESIAN_POINT('Ctrl Pts',(4.31878676761235,-22.7497956849848,
12.));
#224954=CARTESIAN_POINT('Ctrl Pts',(4.32521027803754,-22.7642610156475,
12.));
#224955=CARTESIAN_POINT('Ctrl Pts',(4.33173538373189,-22.7788375194076,
12.));
#224956=CARTESIAN_POINT('Ctrl Pts',(4.33836209118446,-22.7935235607806,
12.));
#224957=CARTESIAN_POINT('Ctrl Pts',(4.34509040460062,-22.8083175343791,
12.));
#224958=CARTESIAN_POINT('Ctrl Pts',(4.3519203259479,-22.8232178638876,12.));
#224959=CARTESIAN_POINT('Ctrl Pts',(4.35885185500546,-22.8382230011184,
12.));
#224960=CARTESIAN_POINT('Ctrl Pts',(4.36588498942997,-22.8533314252422,
12.));
#224961=CARTESIAN_POINT('Ctrl Pts',(4.37301972480745,-22.8685416419725,
12.));
#224962=CARTESIAN_POINT('Ctrl Pts',(4.38025605470092,-22.8838521827701,
12.));
#224963=CARTESIAN_POINT('Ctrl Pts',(4.38759397068405,-22.8992616040108,
12.));
#224964=CARTESIAN_POINT('Ctrl Pts',(4.39503346238473,-22.9147684862426,
12.));
#224965=CARTESIAN_POINT('Ctrl Pts',(4.40257451754323,-22.930371433555,12.));
#224966=CARTESIAN_POINT('Ctrl Pts',(4.41021712205553,-22.9460690729093,
12.));
#224967=CARTESIAN_POINT('Ctrl Pts',(4.41796126001302,-22.9618600534866,
12.));
#224968=CARTESIAN_POINT('Ctrl Pts',(4.42580691372751,-22.977743046002,12.));
#224969=CARTESIAN_POINT('Ctrl Pts',(4.43375406376879,-22.9937167421006,
12.));
#224970=CARTESIAN_POINT('Ctrl Pts',(4.44180268901643,-23.0097798538395,
12.));
#224971=CARTESIAN_POINT('Ctrl Pts',(4.44995276669686,-23.0259311131392,
12.));
#224972=CARTESIAN_POINT('Ctrl Pts',(4.45820427241683,-23.0421692712467,
12.));
#224973=CARTESIAN_POINT('Ctrl Pts',(4.4665571801823,-23.0584930981732,12.));
#224974=CARTESIAN_POINT('Ctrl Pts',(4.47501146242856,-23.0749013821881,
12.));
#224975=CARTESIAN_POINT('Ctrl Pts',(4.48356709006788,-23.0913929293922,
12.));
#224976=CARTESIAN_POINT('Ctrl Pts',(4.49222403252216,-23.1079665632636,
12.));
#224977=CARTESIAN_POINT('Ctrl Pts',(4.50098225775171,-23.1246211242115,
12.));
#224978=CARTESIAN_POINT('Ctrl Pts',(4.5098417322706,-23.1413554691123,12.));
#224979=CARTESIAN_POINT('Ctrl Pts',(4.51880242116748,-23.1581684708761,
12.));
#224980=CARTESIAN_POINT('Ctrl Pts',(4.52786428815014,-23.1750590180908,
12.));
#224981=CARTESIAN_POINT('Ctrl Pts',(4.53702729557566,-23.1920260146465,
12.));
#224982=CARTESIAN_POINT('Ctrl Pts',(4.54629140447544,-23.2090683793629,
12.));
#224983=CARTESIAN_POINT('Ctrl Pts',(4.55565657456975,-23.2261850456064,
12.));
#224984=CARTESIAN_POINT('Ctrl Pts',(4.56512276427839,-23.2433749609131,
12.));
#224985=CARTESIAN_POINT('Ctrl Pts',(4.57468993076097,-23.2606370866866,
12.));
#224986=CARTESIAN_POINT('Ctrl Pts',(4.5843580299469,-23.2779703978876,12.));
#224987=CARTESIAN_POINT('Ctrl Pts',(4.5941270165575,-23.2953738827191,12.));
#224988=CARTESIAN_POINT('Ctrl Pts',(4.60399684412163,-23.3128465423115,
12.));
#224989=CARTESIAN_POINT('Ctrl Pts',(4.6139674649783,-23.3303873903938,12.));
#224990=CARTESIAN_POINT('Ctrl Pts',(4.62403883030805,-23.3479954530272,
12.));
#224991=CARTESIAN_POINT('Ctrl Pts',(4.63421089016541,-23.3656697683489,
12.));
#224992=CARTESIAN_POINT('Ctrl Pts',(4.6444835934993,-23.3834093863068,12.));
#224993=CARTESIAN_POINT('Ctrl Pts',(4.65485688816924,-23.4012133683959,
12.));
#224994=CARTESIAN_POINT('Ctrl Pts',(4.6653307209467,-23.4190807873803,12.));
#224995=CARTESIAN_POINT('Ctrl Pts',(4.67590503753058,-23.4370107270451,
12.));
#224996=CARTESIAN_POINT('Ctrl Pts',(4.68657978258303,-23.455002281986,12.));
#224997=CARTESIAN_POINT('Ctrl Pts',(4.69735489975024,-23.4730545573853,
12.));
#224998=CARTESIAN_POINT('Ctrl Pts',(4.70823033167818,-23.491166668789,12.));
#224999=CARTESIAN_POINT('Ctrl Pts',(4.71920602001901,-23.509337741878,12.));
#225000=CARTESIAN_POINT('Ctrl Pts',(4.73028190543029,-23.5275669122372,
12.));
#225001=CARTESIAN_POINT('Ctrl Pts',(4.74145792760698,-23.545853325171,12.));
#225002=CARTESIAN_POINT('Ctrl Pts',(4.75273402530617,-23.5641961355168,
12.));
#225003=CARTESIAN_POINT('Ctrl Pts',(4.76411013636251,-23.5825945074535,
12.));
#225004=CARTESIAN_POINT('Ctrl Pts',(4.77558619769872,-23.6010476143099,
12.));
#225005=CARTESIAN_POINT('Ctrl Pts',(4.78716214532097,-23.6195546383624,
12.));
#225006=CARTESIAN_POINT('Ctrl Pts',(4.7988379143322,-23.6381147706579,12.));
#225007=CARTESIAN_POINT('Ctrl Pts',(4.81061343896432,-23.6567272108628,
12.));
#225008=CARTESIAN_POINT('Ctrl Pts',(4.82248865259562,-23.675391167102,12.));
#225009=CARTESIAN_POINT('Ctrl Pts',(4.83446348776265,-23.6941058557971,
12.));
#225010=CARTESIAN_POINT('Ctrl Pts',(4.84653787616425,-23.7128705015017,
12.));
#225011=CARTESIAN_POINT('Ctrl Pts',(4.85871174865499,-23.7316843367313,
12.));
#225012=CARTESIAN_POINT('Ctrl Pts',(4.87098503527152,-23.7505466018245,
12.));
#225013=CARTESIAN_POINT('Ctrl Pts',(4.88335766525573,-23.7694565448049,
12.));
#225014=CARTESIAN_POINT('Ctrl Pts',(4.89582956706775,-23.7884134212384,
12.));
#225015=CARTESIAN_POINT('Ctrl Pts',(4.90840066839344,-23.8074164940896,
12.));
#225016=CARTESIAN_POINT('Ctrl Pts',(4.92107089613968,-23.8264650335717,
12.));
#225017=CARTESIAN_POINT('Ctrl Pts',(4.93384017643432,-23.8455583170057,
12.));
#225018=CARTESIAN_POINT('Ctrl Pts',(4.9467084346586,-23.8646956287168,12.));
#225019=CARTESIAN_POINT('Ctrl Pts',(4.9596755954656,-23.8838762599218,12.));
#225020=CARTESIAN_POINT('Ctrl Pts',(4.97274158279226,-23.9030995086163,
12.));
#225021=CARTESIAN_POINT('Ctrl Pts',(4.98590631986532,-23.9223646794592,
12.));
#225022=CARTESIAN_POINT('Ctrl Pts',(4.99916972919306,-23.9416710836529,
12.));
#225023=CARTESIAN_POINT('Ctrl Pts',(5.01253173257452,-23.9610180388271,
12.));
#225024=CARTESIAN_POINT('Ctrl Pts',(5.02599225112454,-23.9804048689227,
12.));
#225025=CARTESIAN_POINT('Ctrl Pts',(5.03955120528521,-23.9998309040746,
12.));
#225026=CARTESIAN_POINT('Ctrl Pts',(5.05320851483065,-24.0192954804896,
12.));
#225027=CARTESIAN_POINT('Ctrl Pts',(5.06696409886641,-24.0387979403268,
12.));
#225028=CARTESIAN_POINT('Ctrl Pts',(5.08081787581276,-24.0583376315638,
12.));
#225029=CARTESIAN_POINT('Ctrl Pts',(5.09476976342625,-24.0779139079266,
12.));
#225030=CARTESIAN_POINT('Ctrl Pts',(5.10881967883132,-24.0975261288446,
12.));
#225031=CARTESIAN_POINT('Ctrl Pts',(5.12296753853859,-24.117173659394,12.));
#225032=CARTESIAN_POINT('Ctrl Pts',(5.13721325845744,-24.1368558702443,
12.));
#225033=CARTESIAN_POINT('Ctrl Pts',(5.15155675390075,-24.1565721375971,
12.));
#225034=CARTESIAN_POINT('Ctrl Pts',(5.16599793957979,-24.1763218431343,
12.));
#225035=CARTESIAN_POINT('Ctrl Pts',(5.18053672961392,-24.1961043738754,
12.));
#225036=CARTESIAN_POINT('Ctrl Pts',(5.19517303753642,-24.215919122017,12.));
#225037=CARTESIAN_POINT('Ctrl Pts',(5.20990677629173,-24.2357654847765,
12.));
#225038=CARTESIAN_POINT('Ctrl Pts',(5.22473785822441,-24.2556428642294,
12.));
#225039=CARTESIAN_POINT('Ctrl Pts',(5.23966619506289,-24.2755506671526,
12.));
#225040=CARTESIAN_POINT('Ctrl Pts',(5.25469169788855,-24.2954883048448,
12.));
#225041=CARTESIAN_POINT('Ctrl Pts',(5.26981427718796,-24.3154551932222,
12.));
#225042=CARTESIAN_POINT('Ctrl Pts',(5.28503384290644,-24.3354507529415,
12.));
#225043=CARTESIAN_POINT('Ctrl Pts',(5.30035030449058,-24.3554744095075,
12.));
#225044=CARTESIAN_POINT('Ctrl Pts',(5.31576357092524,-24.3755255933917,
12.));
#225045=CARTESIAN_POINT('Ctrl Pts',(5.33127355076036,-24.3956037401293,
12.));
#225046=CARTESIAN_POINT('Ctrl Pts',(5.34688015213546,-24.4157082904615,
12.));
#225047=CARTESIAN_POINT('Ctrl Pts',(5.36258328273639,-24.4358386899152,
12.));
#225048=CARTESIAN_POINT('Ctrl Pts',(5.37838284973706,-24.4559943883159,
12.));
#225049=CARTESIAN_POINT('Ctrl Pts',(5.3942787597383,-24.4761748393322,12.));
#225050=CARTESIAN_POINT('Ctrl Pts',(5.41027091869242,-24.4963794999831,
12.));
#225051=CARTESIAN_POINT('Ctrl Pts',(5.42635923183411,-24.5166078302107,
12.));
#225052=CARTESIAN_POINT('Ctrl Pts',(5.44254360356865,-24.5368592922861,
12.));
#225053=CARTESIAN_POINT('Ctrl Pts',(5.45882393762244,-24.5571333514841,
12.));
#225054=CARTESIAN_POINT('Ctrl Pts',(5.47520013724403,-24.5774294770329,
12.));
#225055=CARTESIAN_POINT('Ctrl Pts',(5.49167210537235,-24.5977471429365,
12.));
#225056=CARTESIAN_POINT('Ctrl Pts',(5.50823974481959,-24.618085828918,12.));
#225057=CARTESIAN_POINT('Ctrl Pts',(5.52490295840996,-24.6384450211466,
12.));
#225058=CARTESIAN_POINT('Ctrl Pts',(5.54166164919592,-24.6588242134733,
12.));
#225059=CARTESIAN_POINT('Ctrl Pts',(5.55851572025389,-24.6792229061785,
12.));
#225060=CARTESIAN_POINT('Ctrl Pts',(5.57546507427766,-24.6996406035507,
12.));
#225061=CARTESIAN_POINT('Ctrl Pts',(5.59250961323995,-24.7200768119079,
12.));
#225062=CARTESIAN_POINT('Ctrl Pts',(5.60964923798494,-24.7405310372736,
12.));
#225063=CARTESIAN_POINT('Ctrl Pts',(5.62688384790918,-24.76100278357,12.));
#225064=CARTESIAN_POINT('Ctrl Pts',(5.64421334042247,-24.7814915496728,
12.));
#225065=CARTESIAN_POINT('Ctrl Pts',(5.66163761114903,-24.8019968304618,
12.));
#225066=CARTESIAN_POINT('Ctrl Pts',(5.67915655496524,-24.822518122386,12.));
#225067=CARTESIAN_POINT('Ctrl Pts',(5.69677006679429,-24.8430549277634,
12.));
#225068=CARTESIAN_POINT('Ctrl Pts',(5.71447804252019,-24.8636067597677,
12.));
#225069=CARTESIAN_POINT('Ctrl Pts',(5.73228037976926,-24.8841731467219,
12.));
#225070=CARTESIAN_POINT('Ctrl Pts',(5.75017697890812,-24.9047536376467,
12.));
#225071=CARTESIAN_POINT('Ctrl Pts',(5.76816774342236,-24.9253478043632,
12.));
#225072=CARTESIAN_POINT('Ctrl Pts',(5.78625257775702,-24.9459552293308,
12.));
#225073=CARTESIAN_POINT('Ctrl Pts',(5.80443138549747,-24.9665754954463,
12.));
#225074=CARTESIAN_POINT('Ctrl Pts',(5.82270406744213,-24.9872081752709,
12.));
#225075=CARTESIAN_POINT('Ctrl Pts',(5.84107051963073,-25.0078528200558,
12.));
#225076=CARTESIAN_POINT('Ctrl Pts',(5.8595306315681,-25.0285089498922,12.));
#225077=CARTESIAN_POINT('Ctrl Pts',(5.87808428385329,-25.0491760405965,
12.));
#225078=CARTESIAN_POINT('Ctrl Pts',(5.89673135155458,-25.0698535426593,
12.));
#225079=CARTESIAN_POINT('Ctrl Pts',(5.91547170844382,-25.0905409050863,
12.));
#225080=CARTESIAN_POINT('Ctrl Pts',(5.93430523086776,-25.1112375971182,
12.));
#225081=CARTESIAN_POINT('Ctrl Pts',(5.95323180187347,-25.1319431317273,
12.));
#225082=CARTESIAN_POINT('Ctrl Pts',(5.97225131495636,-25.1526570863065,
12.));
#225083=CARTESIAN_POINT('Ctrl Pts',(5.99136367859838,-25.1733791296154,
12.));
#225084=CARTESIAN_POINT('Ctrl Pts',(6.0105688180476,-25.1941090269638,12.));
#225085=CARTESIAN_POINT('Ctrl Pts',(6.02986667390187,-25.2148466201368,
12.));
#225086=CARTESIAN_POINT('Ctrl Pts',(6.04925720151412,-25.2355918138798,
12.));
#225087=CARTESIAN_POINT('Ctrl Pts',(6.06484373634696,-25.2521940105523,
12.));
#225088=CARTESIAN_POINT('Ctrl Pts',(6.07657531787577,-25.2646490489816,
12.));
#225089=CARTESIAN_POINT('Ctrl Pts',(6.08441489609824,-25.2729539149479,
12.));
#225090=CARTESIAN_POINT('Ctrl Pts',(6.08833931617698,-25.2771067246846,
12.));
#225091=CARTESIAN_POINT('Ctrl Pts',(1.76341220531179,-22.4835757167854,
0.));
#225092=CARTESIAN_POINT('Ctrl Pts',(1.76341220531179,-22.4835757167854,
12.));
#225093=CARTESIAN_POINT('Ctrl Pts',(1.76341415538764,-22.483581992979,0.));
#225094=CARTESIAN_POINT('Ctrl Pts',(1.76341415538764,-22.483581992979,12.));
#225095=CARTESIAN_POINT('Ctrl Pts',(1.7634206426357,-22.4836387052232,0.));
#225096=CARTESIAN_POINT('Ctrl Pts',(1.7634206426357,-22.4836387052232,12.));
#225097=CARTESIAN_POINT('Ctrl Pts',(1.76343813434565,-22.483856251707,0.));
#225098=CARTESIAN_POINT('Ctrl Pts',(1.76343813434565,-22.483856251707,12.));
#225099=CARTESIAN_POINT('Ctrl Pts',(1.76347698284791,-22.4844112933129,
0.));
#225100=CARTESIAN_POINT('Ctrl Pts',(1.76347698284791,-22.4844112933129,
12.));
#225101=CARTESIAN_POINT('Ctrl Pts',(1.76355076045546,-22.4855446605991,
0.));
#225102=CARTESIAN_POINT('Ctrl Pts',(1.76355076045546,-22.4855446605991,
12.));
#225103=CARTESIAN_POINT('Ctrl Pts',(1.76364784232963,-22.4871115206571,
0.));
#225104=CARTESIAN_POINT('Ctrl Pts',(1.76364784232963,-22.4871115206571,
12.));
#225105=CARTESIAN_POINT('Ctrl Pts',(1.76376424879504,-22.4890991659478,
0.));
#225106=CARTESIAN_POINT('Ctrl Pts',(1.76376424879504,-22.4890991659478,
12.));
#225107=CARTESIAN_POINT('Ctrl Pts',(1.76389475965723,-22.4914909094908,
0.));
#225108=CARTESIAN_POINT('Ctrl Pts',(1.76389475965723,-22.4914909094908,
12.));
#225109=CARTESIAN_POINT('Ctrl Pts',(1.764033938803,-22.4942693792449,0.));
#225110=CARTESIAN_POINT('Ctrl Pts',(1.764033938803,-22.4942693792449,12.));
#225111=CARTESIAN_POINT('Ctrl Pts',(1.76417731243462,-22.4974203063191,
0.));
#225112=CARTESIAN_POINT('Ctrl Pts',(1.76417731243462,-22.4974203063191,
12.));
#225113=CARTESIAN_POINT('Ctrl Pts',(1.76432160068725,-22.5009332677316,
0.));
#225114=CARTESIAN_POINT('Ctrl Pts',(1.76432160068725,-22.5009332677316,
12.));
#225115=CARTESIAN_POINT('Ctrl Pts',(1.76446408210366,-22.5047996391978,
0.));
#225116=CARTESIAN_POINT('Ctrl Pts',(1.76446408210366,-22.5047996391978,
12.));
#225117=CARTESIAN_POINT('Ctrl Pts',(1.76460218257323,-22.5090112700212,
0.));
#225118=CARTESIAN_POINT('Ctrl Pts',(1.76460218257323,-22.5090112700212,
12.));
#225119=CARTESIAN_POINT('Ctrl Pts',(1.76473303281158,-22.5135590569554,
0.));
#225120=CARTESIAN_POINT('Ctrl Pts',(1.76473303281158,-22.5135590569554,
12.));
#225121=CARTESIAN_POINT('Ctrl Pts',(1.76485369319896,-22.5184336670207,
0.));
#225122=CARTESIAN_POINT('Ctrl Pts',(1.76485369319896,-22.5184336670207,
12.));
#225123=CARTESIAN_POINT('Ctrl Pts',(1.76496128643369,-22.5236259635515,
0.));
#225124=CARTESIAN_POINT('Ctrl Pts',(1.76496128643369,-22.5236259635515,
12.));
#225125=CARTESIAN_POINT('Ctrl Pts',(1.76505320262751,-22.529127665298,0.));
#225126=CARTESIAN_POINT('Ctrl Pts',(1.76505320262751,-22.529127665298,12.));
#225127=CARTESIAN_POINT('Ctrl Pts',(1.7651271156325,-22.5349313983571,0.));
#225128=CARTESIAN_POINT('Ctrl Pts',(1.7651271156325,-22.5349313983571,12.));
#225129=CARTESIAN_POINT('Ctrl Pts',(1.76518087841492,-22.5410303590891,
0.));
#225130=CARTESIAN_POINT('Ctrl Pts',(1.76518087841492,-22.5410303590891,
12.));
#225131=CARTESIAN_POINT('Ctrl Pts',(1.76521245524047,-22.5474180954006,
0.));
#225132=CARTESIAN_POINT('Ctrl Pts',(1.76521245524047,-22.5474180954006,
12.));
#225133=CARTESIAN_POINT('Ctrl Pts',(1.76521983384062,-22.5540882235837,
0.));
#225134=CARTESIAN_POINT('Ctrl Pts',(1.76521983384062,-22.5540882235837,
12.));
#225135=CARTESIAN_POINT('Ctrl Pts',(1.76520104500449,-22.5610344912501,
0.));
#225136=CARTESIAN_POINT('Ctrl Pts',(1.76520104500449,-22.5610344912501,
12.));
#225137=CARTESIAN_POINT('Ctrl Pts',(1.76515418518829,-22.5682508499873,
0.));
#225138=CARTESIAN_POINT('Ctrl Pts',(1.76515418518829,-22.5682508499873,
12.));
#225139=CARTESIAN_POINT('Ctrl Pts',(1.76507744026747,-22.5757315316355,
0.));
#225140=CARTESIAN_POINT('Ctrl Pts',(1.76507744026747,-22.5757315316355,
12.));
#225141=CARTESIAN_POINT('Ctrl Pts',(1.76496910283088,-22.5834711038024,
0.));
#225142=CARTESIAN_POINT('Ctrl Pts',(1.76496910283088,-22.5834711038024,
12.));
#225143=CARTESIAN_POINT('Ctrl Pts',(1.76482755288411,-22.5914644078106,
0.));
#225144=CARTESIAN_POINT('Ctrl Pts',(1.76482755288411,-22.5914644078106,
12.));
#225145=CARTESIAN_POINT('Ctrl Pts',(1.76465124413556,-22.5997065145638,
0.));
#225146=CARTESIAN_POINT('Ctrl Pts',(1.76465124413556,-22.5997065145638,
12.));
#225147=CARTESIAN_POINT('Ctrl Pts',(1.76443868648015,-22.6081926681342,
0.));
#225148=CARTESIAN_POINT('Ctrl Pts',(1.76443868648015,-22.6081926681342,
12.));
#225149=CARTESIAN_POINT('Ctrl Pts',(1.76418843543739,-22.6169182517693,
0.));
#225150=CARTESIAN_POINT('Ctrl Pts',(1.76418843543739,-22.6169182517693,
12.));
#225151=CARTESIAN_POINT('Ctrl Pts',(1.76389909571402,-22.6258787994847,
0.));
#225152=CARTESIAN_POINT('Ctrl Pts',(1.76389909571402,-22.6258787994847,
12.));
#225153=CARTESIAN_POINT('Ctrl Pts',(1.76356932176272,-22.635069997936,0.));
#225154=CARTESIAN_POINT('Ctrl Pts',(1.76356932176272,-22.635069997936,12.));
#225155=CARTESIAN_POINT('Ctrl Pts',(1.76319782013913,-22.6444876940425,
0.));
#225156=CARTESIAN_POINT('Ctrl Pts',(1.76319782013913,-22.6444876940425,
12.));
#225157=CARTESIAN_POINT('Ctrl Pts',(1.76278334912559,-22.6541278938413,
0.));
#225158=CARTESIAN_POINT('Ctrl Pts',(1.76278334912559,-22.6541278938413,
12.));
#225159=CARTESIAN_POINT('Ctrl Pts',(1.76232471392567,-22.6639867471756,
0.));
#225160=CARTESIAN_POINT('Ctrl Pts',(1.76232471392567,-22.6639867471756,
12.));
#225161=CARTESIAN_POINT('Ctrl Pts',(1.76182076289525,-22.6740605356699,
0.));
#225162=CARTESIAN_POINT('Ctrl Pts',(1.76182076289525,-22.6740605356699,
12.));
#225163=CARTESIAN_POINT('Ctrl Pts',(1.76127038310612,-22.6843456585245,
0.));
#225164=CARTESIAN_POINT('Ctrl Pts',(1.76127038310612,-22.6843456585245,
12.));
#225165=CARTESIAN_POINT('Ctrl Pts',(1.76067249704884,-22.6948386219843,
0.));
#225166=CARTESIAN_POINT('Ctrl Pts',(1.76067249704884,-22.6948386219843,
12.));
#225167=CARTESIAN_POINT('Ctrl Pts',(1.76002606202398,-22.7055360375481,
0.));
#225168=CARTESIAN_POINT('Ctrl Pts',(1.76002606202398,-22.7055360375481,
12.));
#225169=CARTESIAN_POINT('Ctrl Pts',(1.75933006905924,-22.7164346186007,
0.));
#225170=CARTESIAN_POINT('Ctrl Pts',(1.75933006905924,-22.7164346186007,
12.));
#225171=CARTESIAN_POINT('Ctrl Pts',(1.75858354204634,-22.7275311777305,
0.));
#225172=CARTESIAN_POINT('Ctrl Pts',(1.75858354204634,-22.7275311777305,
12.));
#225173=CARTESIAN_POINT('Ctrl Pts',(1.75778553673249,-22.7388226235565,
0.));
#225174=CARTESIAN_POINT('Ctrl Pts',(1.75778553673249,-22.7388226235565,
12.));
#225175=CARTESIAN_POINT('Ctrl Pts',(1.75693513908911,-22.7503059556455,
0.));
#225176=CARTESIAN_POINT('Ctrl Pts',(1.75693513908911,-22.7503059556455,
12.));
#225177=CARTESIAN_POINT('Ctrl Pts',(1.7560314637164,-22.7619782595013,0.));
#225178=CARTESIAN_POINT('Ctrl Pts',(1.7560314637164,-22.7619782595013,12.));
#225179=CARTESIAN_POINT('Ctrl Pts',(1.75507365227127,-22.7738367016115,
0.));
#225180=CARTESIAN_POINT('Ctrl Pts',(1.75507365227127,-22.7738367016115,
12.));
#225181=CARTESIAN_POINT('Ctrl Pts',(1.75406087182929,-22.7858785242358,
0.));
#225182=CARTESIAN_POINT('Ctrl Pts',(1.75406087182929,-22.7858785242358,
12.));
#225183=CARTESIAN_POINT('Ctrl Pts',(1.75299231391461,-22.7981010424312,
0.));
#225184=CARTESIAN_POINT('Ctrl Pts',(1.75299231391461,-22.7981010424312,
12.));
#225185=CARTESIAN_POINT('Ctrl Pts',(1.75186719365589,-22.8105016414712,
0.));
#225186=CARTESIAN_POINT('Ctrl Pts',(1.75186719365589,-22.8105016414712,
12.));
#225187=CARTESIAN_POINT('Ctrl Pts',(1.75068474890883,-22.8230777741285,
0.));
#225188=CARTESIAN_POINT('Ctrl Pts',(1.75068474890883,-22.8230777741285,
12.));
#225189=CARTESIAN_POINT('Ctrl Pts',(1.74944423940117,-22.8358269579854,
0.));
#225190=CARTESIAN_POINT('Ctrl Pts',(1.74944423940117,-22.8358269579854,
12.));
#225191=CARTESIAN_POINT('Ctrl Pts',(1.74814494588491,-22.8487467728075,
0.));
#225192=CARTESIAN_POINT('Ctrl Pts',(1.74814494588491,-22.8487467728075,
12.));
#225193=CARTESIAN_POINT('Ctrl Pts',(1.74678616930663,-22.8618348580234,
0.));
#225194=CARTESIAN_POINT('Ctrl Pts',(1.74678616930663,-22.8618348580234,
12.));
#225195=CARTESIAN_POINT('Ctrl Pts',(1.74536722998199,-22.8750889101696,
0.));
#225196=CARTESIAN_POINT('Ctrl Pts',(1.74536722998199,-22.8750889101696,
12.));
#225197=CARTESIAN_POINT('Ctrl Pts',(1.74388746677702,-22.8885066803351,
0.));
#225198=CARTESIAN_POINT('Ctrl Pts',(1.74388746677702,-22.8885066803351,
12.));
#225199=CARTESIAN_POINT('Ctrl Pts',(1.74234623630079,-22.9020859716144,
0.));
#225200=CARTESIAN_POINT('Ctrl Pts',(1.74234623630079,-22.9020859716144,
12.));
#225201=CARTESIAN_POINT('Ctrl Pts',(1.74074291231056,-22.9158246373365,
0.));
#225202=CARTESIAN_POINT('Ctrl Pts',(1.74074291231056,-22.9158246373365,
12.));
#225203=CARTESIAN_POINT('Ctrl Pts',(1.73907688511664,-22.9297205792587,
0.));
#225204=CARTESIAN_POINT('Ctrl Pts',(1.73907688511664,-22.9297205792587,
12.));
#225205=CARTESIAN_POINT('Ctrl Pts',(1.73734756100038,-22.9437717457825,
0.));
#225206=CARTESIAN_POINT('Ctrl Pts',(1.73734756100038,-22.9437717457825,
12.));
#225207=CARTESIAN_POINT('Ctrl Pts',(1.73555436162771,-22.9579761301062,
0.));
#225208=CARTESIAN_POINT('Ctrl Pts',(1.73555436162771,-22.9579761301062,
12.));
#225209=CARTESIAN_POINT('Ctrl Pts',(1.73369672350817,-22.9723317685688,
0.));
#225210=CARTESIAN_POINT('Ctrl Pts',(1.73369672350817,-22.9723317685688,
12.));
#225211=CARTESIAN_POINT('Ctrl Pts',(1.73177409750193,-22.9868367391978,
0.));
#225212=CARTESIAN_POINT('Ctrl Pts',(1.73177409750193,-22.9868367391978,
12.));
#225213=CARTESIAN_POINT('Ctrl Pts',(1.72978594832137,-23.0014891601891,
0.));
#225214=CARTESIAN_POINT('Ctrl Pts',(1.72978594832137,-23.0014891601891,
12.));
#225215=CARTESIAN_POINT('Ctrl Pts',(1.72773175404702,-23.0162871884167,
0.));
#225216=CARTESIAN_POINT('Ctrl Pts',(1.72773175404702,-23.0162871884167,
12.));
#225217=CARTESIAN_POINT('Ctrl Pts',(1.72561100564033,-23.031229017888,0.));
#225218=CARTESIAN_POINT('Ctrl Pts',(1.72561100564033,-23.031229017888,12.));
#225219=CARTESIAN_POINT('Ctrl Pts',(1.72342320653731,-23.0463128785528,
0.));
#225220=CARTESIAN_POINT('Ctrl Pts',(1.72342320653731,-23.0463128785528,
12.));
#225221=CARTESIAN_POINT('Ctrl Pts',(1.7211678722598,-23.061537035156,0.));
#225222=CARTESIAN_POINT('Ctrl Pts',(1.7211678722598,-23.061537035156,12.));
#225223=CARTESIAN_POINT('Ctrl Pts',(1.71884453003027,-23.0768997860709,
0.));
#225224=CARTESIAN_POINT('Ctrl Pts',(1.71884453003027,-23.0768997860709,
12.));
#225225=CARTESIAN_POINT('Ctrl Pts',(1.71645271839311,-23.0923994621216,
0.));
#225226=CARTESIAN_POINT('Ctrl Pts',(1.71645271839311,-23.0923994621216,
12.));
#225227=CARTESIAN_POINT('Ctrl Pts',(1.71399198684724,-23.1080344254291,
0.));
#225228=CARTESIAN_POINT('Ctrl Pts',(1.71399198684724,-23.1080344254291,
12.));
#225229=CARTESIAN_POINT('Ctrl Pts',(1.71146189552192,-23.1238030684929,
0.));
#225230=CARTESIAN_POINT('Ctrl Pts',(1.71146189552192,-23.1238030684929,
12.));
#225231=CARTESIAN_POINT('Ctrl Pts',(1.70886201485459,-23.1397038132358,
0.));
#225232=CARTESIAN_POINT('Ctrl Pts',(1.70886201485459,-23.1397038132358,
12.));
#225233=CARTESIAN_POINT('Ctrl Pts',(1.70619192527846,-23.1557351100613,
0.));
#225234=CARTESIAN_POINT('Ctrl Pts',(1.70619192527846,-23.1557351100613,
12.));
#225235=CARTESIAN_POINT('Ctrl Pts',(1.70345121691259,-23.1718954368749,
0.));
#225236=CARTESIAN_POINT('Ctrl Pts',(1.70345121691259,-23.1718954368749,
12.));
#225237=CARTESIAN_POINT('Ctrl Pts',(1.70063948926987,-23.1881832981848,
0.));
#225238=CARTESIAN_POINT('Ctrl Pts',(1.70063948926987,-23.1881832981848,
12.));
#225239=CARTESIAN_POINT('Ctrl Pts',(1.69775635099425,-23.2045972243765,
0.));
#225240=CARTESIAN_POINT('Ctrl Pts',(1.69775635099425,-23.2045972243765,
12.));
#225241=CARTESIAN_POINT('Ctrl Pts',(1.69480141959945,-23.2211357709374,
0.));
#225242=CARTESIAN_POINT('Ctrl Pts',(1.69480141959945,-23.2211357709374,
12.));
#225243=CARTESIAN_POINT('Ctrl Pts',(1.69177432121716,-23.2377975177014,
0.));
#225244=CARTESIAN_POINT('Ctrl Pts',(1.69177432121716,-23.2377975177014,
12.));
#225245=CARTESIAN_POINT('Ctrl Pts',(1.6886746903491,-23.2545810680536,0.));
#225246=CARTESIAN_POINT('Ctrl Pts',(1.6886746903491,-23.2545810680536,12.));
#225247=CARTESIAN_POINT('Ctrl Pts',(1.68550216963274,-23.2714850482245,
0.));
#225248=CARTESIAN_POINT('Ctrl Pts',(1.68550216963274,-23.2714850482245,
12.));
#225249=CARTESIAN_POINT('Ctrl Pts',(1.68225640962181,-23.2885081066949,
0.));
#225250=CARTESIAN_POINT('Ctrl Pts',(1.68225640962181,-23.2885081066949,
12.));
#225251=CARTESIAN_POINT('Ctrl Pts',(1.67893706857123,-23.3056489135611,
0.));
#225252=CARTESIAN_POINT('Ctrl Pts',(1.67893706857123,-23.3056489135611,
12.));
#225253=CARTESIAN_POINT('Ctrl Pts',(1.67554381222987,-23.3229061599145,
0.));
#225254=CARTESIAN_POINT('Ctrl Pts',(1.67554381222987,-23.3229061599145,
12.));
#225255=CARTESIAN_POINT('Ctrl Pts',(1.67207631363905,-23.3402785571866,
0.));
#225256=CARTESIAN_POINT('Ctrl Pts',(1.67207631363905,-23.3402785571866,
12.));
#225257=CARTESIAN_POINT('Ctrl Pts',(1.66853425293977,-23.3577648365747,
0.));
#225258=CARTESIAN_POINT('Ctrl Pts',(1.66853425293977,-23.3577648365747,
12.));
#225259=CARTESIAN_POINT('Ctrl Pts',(1.66491731718864,-23.375363748555,0.));
#225260=CARTESIAN_POINT('Ctrl Pts',(1.66491731718864,-23.375363748555,12.));
#225261=CARTESIAN_POINT('Ctrl Pts',(1.66122520018008,-23.3930740623622,
0.));
#225262=CARTESIAN_POINT('Ctrl Pts',(1.66122520018008,-23.3930740623622,
12.));
#225263=CARTESIAN_POINT('Ctrl Pts',(1.65745760227507,-23.4108945654803,
0.));
#225264=CARTESIAN_POINT('Ctrl Pts',(1.65745760227507,-23.4108945654803,
12.));
#225265=CARTESIAN_POINT('Ctrl Pts',(1.6536142302373,-23.4288240631034,0.));
#225266=CARTESIAN_POINT('Ctrl Pts',(1.6536142302373,-23.4288240631034,12.));
#225267=CARTESIAN_POINT('Ctrl Pts',(1.64969479707339,-23.446861377656,0.));
#225268=CARTESIAN_POINT('Ctrl Pts',(1.64969479707339,-23.446861377656,12.));
#225269=CARTESIAN_POINT('Ctrl Pts',(1.64569902187608,-23.4650053483919,
0.));
#225270=CARTESIAN_POINT('Ctrl Pts',(1.64569902187608,-23.4650053483919,
12.));
#225271=CARTESIAN_POINT('Ctrl Pts',(1.64162662967524,-23.4832548309638,
0.));
#225272=CARTESIAN_POINT('Ctrl Pts',(1.64162662967524,-23.4832548309638,
12.));
#225273=CARTESIAN_POINT('Ctrl Pts',(1.63747735129474,-23.5016086970006,
0.));
#225274=CARTESIAN_POINT('Ctrl Pts',(1.63747735129474,-23.5016086970006,
12.));
#225275=CARTESIAN_POINT('Ctrl Pts',(1.63325092321731,-23.5200658336624,
0.));
#225276=CARTESIAN_POINT('Ctrl Pts',(1.63325092321731,-23.5200658336624,
12.));
#225277=CARTESIAN_POINT('Ctrl Pts',(1.62894708745231,-23.5386251432278,
0.));
#225278=CARTESIAN_POINT('Ctrl Pts',(1.62894708745231,-23.5386251432278,
12.));
#225279=CARTESIAN_POINT('Ctrl Pts',(1.62456559140071,-23.5572855427617,
0.));
#225280=CARTESIAN_POINT('Ctrl Pts',(1.62456559140071,-23.5572855427617,
12.));
#225281=CARTESIAN_POINT('Ctrl Pts',(1.62010618772869,-23.5760459637608,
0.));
#225282=CARTESIAN_POINT('Ctrl Pts',(1.62010618772869,-23.5760459637608,
12.));
#225283=CARTESIAN_POINT('Ctrl Pts',(1.61556863424697,-23.5949053517996,
0.));
#225284=CARTESIAN_POINT('Ctrl Pts',(1.61556863424697,-23.5949053517996,
12.));
#225285=CARTESIAN_POINT('Ctrl Pts',(1.61095269379773,-23.6138626661644,
0.));
#225286=CARTESIAN_POINT('Ctrl Pts',(1.61095269379773,-23.6138626661644,
12.));
#225287=CARTESIAN_POINT('Ctrl Pts',(1.60625813414666,-23.6329168794916,
0.));
#225288=CARTESIAN_POINT('Ctrl Pts',(1.60625813414666,-23.6329168794916,
12.));
#225289=CARTESIAN_POINT('Ctrl Pts',(1.60148472786588,-23.6520669774863,
0.));
#225290=CARTESIAN_POINT('Ctrl Pts',(1.60148472786588,-23.6520669774863,
12.));
#225291=CARTESIAN_POINT('Ctrl Pts',(1.59663225222458,-23.6713119586302,
0.));
#225292=CARTESIAN_POINT('Ctrl Pts',(1.59663225222458,-23.6713119586302,
12.));
#225293=CARTESIAN_POINT('Ctrl Pts',(1.59170048908631,-23.6906508338833,
0.));
#225294=CARTESIAN_POINT('Ctrl Pts',(1.59170048908631,-23.6906508338833,
12.));
#225295=CARTESIAN_POINT('Ctrl Pts',(1.58668922481222,-23.7100826263835,
0.));
#225296=CARTESIAN_POINT('Ctrl Pts',(1.58668922481222,-23.7100826263835,
12.));
#225297=CARTESIAN_POINT('Ctrl Pts',(1.58159825017362,-23.7296063711308,
0.));
#225298=CARTESIAN_POINT('Ctrl Pts',(1.58159825017362,-23.7296063711308,
12.));
#225299=CARTESIAN_POINT('Ctrl Pts',(1.57642736025251,-23.7492211147369,
0.));
#225300=CARTESIAN_POINT('Ctrl Pts',(1.57642736025251,-23.7492211147369,
12.));
#225301=CARTESIAN_POINT('Ctrl Pts',(1.57117635434412,-23.7689259151869,
0.));
#225302=CARTESIAN_POINT('Ctrl Pts',(1.57117635434412,-23.7689259151869,
12.));
#225303=CARTESIAN_POINT('Ctrl Pts',(1.56584503586844,-23.788719841588,0.));
#225304=CARTESIAN_POINT('Ctrl Pts',(1.56584503586844,-23.788719841588,12.));
#225305=CARTESIAN_POINT('Ctrl Pts',(1.56043321228631,-23.8086019739192,
0.));
#225306=CARTESIAN_POINT('Ctrl Pts',(1.56043321228631,-23.8086019739192,
12.));
#225307=CARTESIAN_POINT('Ctrl Pts',(1.55494069502627,-23.8285714027631,
0.));
#225308=CARTESIAN_POINT('Ctrl Pts',(1.55494069502627,-23.8285714027631,
12.));
#225309=CARTESIAN_POINT('Ctrl Pts',(1.5493672994053,-23.8486272290698,0.));
#225310=CARTESIAN_POINT('Ctrl Pts',(1.5493672994053,-23.8486272290698,12.));
#225311=CARTESIAN_POINT('Ctrl Pts',(1.54371284453977,-23.8687685639635,
0.));
#225312=CARTESIAN_POINT('Ctrl Pts',(1.54371284453977,-23.8687685639635,
12.));
#225313=CARTESIAN_POINT('Ctrl Pts',(1.53797715326748,-23.8889945285313,
0.));
#225314=CARTESIAN_POINT('Ctrl Pts',(1.53797715326748,-23.8889945285313,
12.));
#225315=CARTESIAN_POINT('Ctrl Pts',(1.53216005207462,-23.9093042536119,
0.));
#225316=CARTESIAN_POINT('Ctrl Pts',(1.53216005207462,-23.9093042536119,
12.));
#225317=CARTESIAN_POINT('Ctrl Pts',(1.52626137103039,-23.9296968795761,
0.));
#225318=CARTESIAN_POINT('Ctrl Pts',(1.52626137103039,-23.9296968795761,
12.));
#225319=CARTESIAN_POINT('Ctrl Pts',(1.52028094372806,-23.9501715561038,
0.));
#225320=CARTESIAN_POINT('Ctrl Pts',(1.52028094372806,-23.9501715561038,
12.));
#225321=CARTESIAN_POINT('Ctrl Pts',(1.51421860720628,-23.9707274420145,
0.));
#225322=CARTESIAN_POINT('Ctrl Pts',(1.51421860720628,-23.9707274420145,
12.));
#225323=CARTESIAN_POINT('Ctrl Pts',(1.50807420187702,-23.991363705093,0.));
#225324=CARTESIAN_POINT('Ctrl Pts',(1.50807420187702,-23.991363705093,12.));
#225325=CARTESIAN_POINT('Ctrl Pts',(1.50184757146099,-24.0120795219086,
0.));
#225326=CARTESIAN_POINT('Ctrl Pts',(1.50184757146099,-24.0120795219086,
12.));
#225327=CARTESIAN_POINT('Ctrl Pts',(1.49553856292798,-24.0328740776331,
0.));
#225328=CARTESIAN_POINT('Ctrl Pts',(1.49553856292798,-24.0328740776331,
12.));
#225329=CARTESIAN_POINT('Ctrl Pts',(1.48914702644883,-24.053746565843,0.));
#225330=CARTESIAN_POINT('Ctrl Pts',(1.48914702644883,-24.053746565843,12.));
#225331=CARTESIAN_POINT('Ctrl Pts',(1.4826728153368,-24.074696188353,0.));
#225332=CARTESIAN_POINT('Ctrl Pts',(1.4826728153368,-24.074696188353,12.));
#225333=CARTESIAN_POINT('Ctrl Pts',(1.47611578597741,-24.0957221550782,
0.));
#225334=CARTESIAN_POINT('Ctrl Pts',(1.47611578597741,-24.0957221550782,
12.));
#225335=CARTESIAN_POINT('Ctrl Pts',(1.46947579776991,-24.1168236838827,
0.));
#225336=CARTESIAN_POINT('Ctrl Pts',(1.46947579776991,-24.1168236838827,
12.));
#225337=CARTESIAN_POINT('Ctrl Pts',(1.46275271307398,-24.1380000004272,
0.));
#225338=CARTESIAN_POINT('Ctrl Pts',(1.46275271307398,-24.1380000004272,
12.));
#225339=CARTESIAN_POINT('Ctrl Pts',(1.45594639716314,-24.1592503380105,
0.));
#225340=CARTESIAN_POINT('Ctrl Pts',(1.45594639716314,-24.1592503380105,
12.));
#225341=CARTESIAN_POINT('Ctrl Pts',(1.4490567181872,-24.1805739374033,0.));
#225342=CARTESIAN_POINT('Ctrl Pts',(1.4490567181872,-24.1805739374033,12.));
#225343=CARTESIAN_POINT('Ctrl Pts',(1.44208354711074,-24.2019700467214,
0.));
#225344=CARTESIAN_POINT('Ctrl Pts',(1.44208354711074,-24.2019700467214,
12.));
#225345=CARTESIAN_POINT('Ctrl Pts',(1.43502675765502,-24.2234379212978,
0.));
#225346=CARTESIAN_POINT('Ctrl Pts',(1.43502675765502,-24.2234379212978,
12.));
#225347=CARTESIAN_POINT('Ctrl Pts',(1.42788622624851,-24.2449768235485,
0.));
#225348=CARTESIAN_POINT('Ctrl Pts',(1.42788622624851,-24.2449768235485,
12.));
#225349=CARTESIAN_POINT('Ctrl Pts',(1.42066183198252,-24.2665860228357,
0.));
#225350=CARTESIAN_POINT('Ctrl Pts',(1.42066183198252,-24.2665860228357,
12.));
#225351=CARTESIAN_POINT('Ctrl Pts',(1.41335345657684,-24.2882647953214,
0.));
#225352=CARTESIAN_POINT('Ctrl Pts',(1.41335345657684,-24.2882647953214,
12.));
#225353=CARTESIAN_POINT('Ctrl Pts',(1.4059609843434,-24.3100124238316,0.));
#225354=CARTESIAN_POINT('Ctrl Pts',(1.4059609843434,-24.3100124238316,12.));
#225355=CARTESIAN_POINT('Ctrl Pts',(1.3984843021281,-24.3318281977647,0.));
#225356=CARTESIAN_POINT('Ctrl Pts',(1.3984843021281,-24.3318281977647,12.));
#225357=CARTESIAN_POINT('Ctrl Pts',(1.3909232992639,-24.3537114129877,0.));
#225358=CARTESIAN_POINT('Ctrl Pts',(1.3909232992639,-24.3537114129877,12.));
#225359=CARTESIAN_POINT('Ctrl Pts',(1.38327786752998,-24.37566137173,0.));
#225360=CARTESIAN_POINT('Ctrl Pts',(1.38327786752998,-24.37566137173,12.));
#225361=CARTESIAN_POINT('Ctrl Pts',(1.37554790111607,-24.3976773824731,
0.));
#225362=CARTESIAN_POINT('Ctrl Pts',(1.37554790111607,-24.3976773824731,
12.));
#225363=CARTESIAN_POINT('Ctrl Pts',(1.36773329659954,-24.4197587598337,
0.));
#225364=CARTESIAN_POINT('Ctrl Pts',(1.36773329659954,-24.4197587598337,
12.));
#225365=CARTESIAN_POINT('Ctrl Pts',(1.35983395290624,-24.4419048244524,
0.));
#225366=CARTESIAN_POINT('Ctrl Pts',(1.35983395290624,-24.4419048244524,
12.));
#225367=CARTESIAN_POINT('Ctrl Pts',(1.35184977125644,-24.4641149028894,
0.));
#225368=CARTESIAN_POINT('Ctrl Pts',(1.35184977125644,-24.4641149028894,
12.));
#225369=CARTESIAN_POINT('Ctrl Pts',(1.34378065512335,-24.4863883275135,
0.));
#225370=CARTESIAN_POINT('Ctrl Pts',(1.34378065512335,-24.4863883275135,
12.));
#225371=CARTESIAN_POINT('Ctrl Pts',(1.33562651019684,-24.5087244363856,
0.));
#225372=CARTESIAN_POINT('Ctrl Pts',(1.33562651019684,-24.5087244363856,
12.));
#225373=CARTESIAN_POINT('Ctrl Pts',(1.32738724435326,-24.5311225731434,
0.));
#225374=CARTESIAN_POINT('Ctrl Pts',(1.32738724435326,-24.5311225731434,
12.));
#225375=CARTESIAN_POINT('Ctrl Pts',(1.31906276763669,-24.5535820868671,
0.));
#225376=CARTESIAN_POINT('Ctrl Pts',(1.31906276763669,-24.5535820868671,
12.));
#225377=CARTESIAN_POINT('Ctrl Pts',(1.31065299222023,-24.576102332018,0.));
#225378=CARTESIAN_POINT('Ctrl Pts',(1.31065299222023,-24.576102332018,12.));
#225379=CARTESIAN_POINT('Ctrl Pts',(1.30215783236363,-24.5986826684025,
0.));
#225380=CARTESIAN_POINT('Ctrl Pts',(1.30215783236363,-24.5986826684025,
12.));
#225381=CARTESIAN_POINT('Ctrl Pts',(1.29357720438107,-24.6213224611228,
0.));
#225382=CARTESIAN_POINT('Ctrl Pts',(1.29357720438107,-24.6213224611228,
12.));
#225383=CARTESIAN_POINT('Ctrl Pts',(1.28491102661513,-24.6440210805278,
0.));
#225384=CARTESIAN_POINT('Ctrl Pts',(1.28491102661513,-24.6440210805278,
12.));
#225385=CARTESIAN_POINT('Ctrl Pts',(1.2761592194164,-24.666777902156,0.));
#225386=CARTESIAN_POINT('Ctrl Pts',(1.2761592194164,-24.666777902156,12.));
#225387=CARTESIAN_POINT('Ctrl Pts',(1.26732170513497,-24.6895923066837,
0.));
#225388=CARTESIAN_POINT('Ctrl Pts',(1.26732170513497,-24.6895923066837,
12.));
#225389=CARTESIAN_POINT('Ctrl Pts',(1.25839840807414,-24.7124636797895,
0.));
#225390=CARTESIAN_POINT('Ctrl Pts',(1.25839840807414,-24.7124636797895,
12.));
#225391=CARTESIAN_POINT('Ctrl Pts',(1.24938925444323,-24.7353914120012,
0.));
#225392=CARTESIAN_POINT('Ctrl Pts',(1.24938925444323,-24.7353914120012,
12.));
#225393=CARTESIAN_POINT('Ctrl Pts',(1.24029417231987,-24.7583748985439,
0.));
#225394=CARTESIAN_POINT('Ctrl Pts',(1.24029417231987,-24.7583748985439,
12.));
#225395=CARTESIAN_POINT('Ctrl Pts',(1.23111309161843,-24.78141353918,0.));
#225396=CARTESIAN_POINT('Ctrl Pts',(1.23111309161843,-24.78141353918,12.));
#225397=CARTESIAN_POINT('Ctrl Pts',(1.22184594406526,-24.8045067380536,
0.));
#225398=CARTESIAN_POINT('Ctrl Pts',(1.22184594406526,-24.8045067380536,
12.));
#225399=CARTESIAN_POINT('Ctrl Pts',(1.21249266318205,-24.8276539035092,
0.));
#225400=CARTESIAN_POINT('Ctrl Pts',(1.21249266318205,-24.8276539035092,
12.));
#225401=CARTESIAN_POINT('Ctrl Pts',(1.20305318426015,-24.8508544481973,
0.));
#225402=CARTESIAN_POINT('Ctrl Pts',(1.20305318426015,-24.8508544481973,
12.));
#225403=CARTESIAN_POINT('Ctrl Pts',(1.19352744434059,-24.8741077892074,
0.));
#225404=CARTESIAN_POINT('Ctrl Pts',(1.19352744434059,-24.8741077892074,
12.));
#225405=CARTESIAN_POINT('Ctrl Pts',(1.18391538220098,-24.8974133481829,
0.));
#225406=CARTESIAN_POINT('Ctrl Pts',(1.18391538220098,-24.8974133481829,
12.));
#225407=CARTESIAN_POINT('Ctrl Pts',(1.17421693835039,-24.9207705514449,
0.));
#225408=CARTESIAN_POINT('Ctrl Pts',(1.17421693835039,-24.9207705514449,
12.));
#225409=CARTESIAN_POINT('Ctrl Pts',(1.16443205502852,-24.9441788300932,
0.));
#225410=CARTESIAN_POINT('Ctrl Pts',(1.16443205502852,-24.9441788300932,
12.));
#225411=CARTESIAN_POINT('Ctrl Pts',(1.15456067621894,-24.9676376201501,
0.));
#225412=CARTESIAN_POINT('Ctrl Pts',(1.15456067621894,-24.9676376201501,
12.));
#225413=CARTESIAN_POINT('Ctrl Pts',(1.14460274758206,-24.9911463621431,
0.));
#225414=CARTESIAN_POINT('Ctrl Pts',(1.14460274758206,-24.9911463621431,
12.));
#225415=CARTESIAN_POINT('Ctrl Pts',(1.13455821638535,-25.0147045006193,
0.));
#225416=CARTESIAN_POINT('Ctrl Pts',(1.13455821638535,-25.0147045006193,
12.));
#225417=CARTESIAN_POINT('Ctrl Pts',(1.12442703144455,-25.0383114836898,
0.));
#225418=CARTESIAN_POINT('Ctrl Pts',(1.12442703144455,-25.0383114836898,
12.));
#225419=CARTESIAN_POINT('Ctrl Pts',(1.1142091430689,-25.0619667625336,0.));
#225420=CARTESIAN_POINT('Ctrl Pts',(1.1142091430689,-25.0619667625336,12.));
#225421=CARTESIAN_POINT('Ctrl Pts',(1.1039045030174,-25.085669790968,0.));
#225422=CARTESIAN_POINT('Ctrl Pts',(1.1039045030174,-25.085669790968,12.));
#225423=CARTESIAN_POINT('Ctrl Pts',(1.09351306445299,-25.1094200248448,
0.));
#225424=CARTESIAN_POINT('Ctrl Pts',(1.09351306445299,-25.1094200248448,
12.));
#225425=CARTESIAN_POINT('Ctrl Pts',(1.08303478197174,-25.1332169227415,
0.));
#225426=CARTESIAN_POINT('Ctrl Pts',(1.08303478197174,-25.1332169227415,
12.));
#225427=CARTESIAN_POINT('Ctrl Pts',(1.07246961165459,-25.1570599469311,
0.));
#225428=CARTESIAN_POINT('Ctrl Pts',(1.07246961165459,-25.1570599469311,
12.));
#225429=CARTESIAN_POINT('Ctrl Pts',(1.06181751111754,-25.1809485642191,
0.));
#225430=CARTESIAN_POINT('Ctrl Pts',(1.06181751111754,-25.1809485642191,
12.));
#225431=CARTESIAN_POINT('Ctrl Pts',(1.05107843957925,-25.2048822469027,
0.));
#225432=CARTESIAN_POINT('Ctrl Pts',(1.05107843957925,-25.2048822469027,
12.));
#225433=CARTESIAN_POINT('Ctrl Pts',(1.04025235791514,-25.2288604735087,
0.));
#225434=CARTESIAN_POINT('Ctrl Pts',(1.04025235791514,-25.2288604735087,
12.));
#225435=CARTESIAN_POINT('Ctrl Pts',(1.0293392287683,-25.2528827300427,0.));
#225436=CARTESIAN_POINT('Ctrl Pts',(1.0293392287683,-25.2528827300427,12.));
#225437=CARTESIAN_POINT('Ctrl Pts',(1.01833901642272,-25.2769485087268,
0.));
#225438=CARTESIAN_POINT('Ctrl Pts',(1.01833901642272,-25.2769485087268,
12.));
#225439=CARTESIAN_POINT('Ctrl Pts',(1.00725168656933,-25.3010573055557,
0.));
#225440=CARTESIAN_POINT('Ctrl Pts',(1.00725168656933,-25.3010573055557,
12.));
#225441=CARTESIAN_POINT('Ctrl Pts',(0.996077206120918,-25.3252086182976,
0.));
#225442=CARTESIAN_POINT('Ctrl Pts',(0.996077206120918,-25.3252086182976,
12.));
#225443=CARTESIAN_POINT('Ctrl Pts',(0.984815543004088,-25.3494019441444,
0.));
#225444=CARTESIAN_POINT('Ctrl Pts',(0.984815543004088,-25.3494019441444,
12.));
#225445=CARTESIAN_POINT('Ctrl Pts',(0.973466666000047,-25.3736367778842,
0.));
#225446=CARTESIAN_POINT('Ctrl Pts',(0.973466666000047,-25.3736367778842,
12.));
#225447=CARTESIAN_POINT('Ctrl Pts',(0.962030544502801,-25.3979126089155,
0.));
#225448=CARTESIAN_POINT('Ctrl Pts',(0.962030544502801,-25.3979126089155,
12.));
#225449=CARTESIAN_POINT('Ctrl Pts',(0.950507148596967,-25.4222289223155,
0.));
#225450=CARTESIAN_POINT('Ctrl Pts',(0.950507148596967,-25.4222289223155,
12.));
#225451=CARTESIAN_POINT('Ctrl Pts',(0.938896449495631,-25.4465852044835,
0.));
#225452=CARTESIAN_POINT('Ctrl Pts',(0.938896449495631,-25.4465852044835,
12.));
#225453=CARTESIAN_POINT('Ctrl Pts',(0.927198419885603,-25.4709809474996,
0.));
#225454=CARTESIAN_POINT('Ctrl Pts',(0.927198419885603,-25.4709809474996,
12.));
#225455=CARTESIAN_POINT('Ctrl Pts',(0.915413034335331,-25.4954156541787,
0.));
#225456=CARTESIAN_POINT('Ctrl Pts',(0.915413034335331,-25.4954156541787,
12.));
#225457=CARTESIAN_POINT('Ctrl Pts',(0.903540269651152,-25.5198888424195,
0.));
#225458=CARTESIAN_POINT('Ctrl Pts',(0.903540269651152,-25.5198888424195,
12.));
#225459=CARTESIAN_POINT('Ctrl Pts',(0.891580105349464,-25.5444000508223,
0.));
#225460=CARTESIAN_POINT('Ctrl Pts',(0.891580105349464,-25.5444000508223,
12.));
#225461=CARTESIAN_POINT('Ctrl Pts',(0.879532523835088,-25.568948840818,
0.));
#225462=CARTESIAN_POINT('Ctrl Pts',(0.879532523835088,-25.568948840818,
12.));
#225463=CARTESIAN_POINT('Ctrl Pts',(0.867397509339468,-25.5935347843616,
0.));
#225464=CARTESIAN_POINT('Ctrl Pts',(0.867397509339468,-25.5935347843616,
12.));
#225465=CARTESIAN_POINT('Ctrl Pts',(0.855175047037614,-25.618157453608,
0.));
#225466=CARTESIAN_POINT('Ctrl Pts',(0.855175047037614,-25.618157453608,
12.));
#225467=CARTESIAN_POINT('Ctrl Pts',(0.842865122121542,-25.6428164100078,
0.));
#225468=CARTESIAN_POINT('Ctrl Pts',(0.842865122121542,-25.6428164100078,
12.));
#225469=CARTESIAN_POINT('Ctrl Pts',(0.830467718864366,-25.6675111931957,
0.));
#225470=CARTESIAN_POINT('Ctrl Pts',(0.830467718864366,-25.6675111931957,
12.));
#225471=CARTESIAN_POINT('Ctrl Pts',(0.817982819786718,-25.6922413110172,
0.));
#225472=CARTESIAN_POINT('Ctrl Pts',(0.817982819786718,-25.6922413110172,
12.));
#225473=CARTESIAN_POINT('Ctrl Pts',(0.805410404552592,-25.7170062262474,
0.));
#225474=CARTESIAN_POINT('Ctrl Pts',(0.805410404552592,-25.7170062262474,
12.));
#225475=CARTESIAN_POINT('Ctrl Pts',(0.792750451613533,-25.7418053757671,
0.));
#225476=CARTESIAN_POINT('Ctrl Pts',(0.792750451613533,-25.7418053757671,
12.));
#225477=CARTESIAN_POINT('Ctrl Pts',(0.780002940289024,-25.7666381946871,
0.));
#225478=CARTESIAN_POINT('Ctrl Pts',(0.780002940289024,-25.7666381946871,
12.));
#225479=CARTESIAN_POINT('Ctrl Pts',(0.767167852648638,-25.7915041383304,
0.));
#225480=CARTESIAN_POINT('Ctrl Pts',(0.767167852648638,-25.7915041383304,
12.));
#225481=CARTESIAN_POINT('Ctrl Pts',(0.754245175608287,-25.816402705995,
0.));
#225482=CARTESIAN_POINT('Ctrl Pts',(0.754245175608287,-25.816402705995,
12.));
#225483=CARTESIAN_POINT('Ctrl Pts',(0.741234902664695,-25.841333461908,
0.));
#225484=CARTESIAN_POINT('Ctrl Pts',(0.741234902664695,-25.841333461908,
12.));
#225485=CARTESIAN_POINT('Ctrl Pts',(0.728137036485876,-25.8662960624285,
0.));
#225486=CARTESIAN_POINT('Ctrl Pts',(0.728137036485876,-25.8662960624285,
12.));
#225487=CARTESIAN_POINT('Ctrl Pts',(0.714951588533752,-25.8912902615141,
0.));
#225488=CARTESIAN_POINT('Ctrl Pts',(0.714951588533752,-25.8912902615141,
12.));
#225489=CARTESIAN_POINT('Ctrl Pts',(0.701678575236601,-25.9163158909645,
0.));
#225490=CARTESIAN_POINT('Ctrl Pts',(0.701678575236601,-25.9163158909645,
12.));
#225491=CARTESIAN_POINT('Ctrl Pts',(0.688318015065675,-25.941372847213,
0.));
#225492=CARTESIAN_POINT('Ctrl Pts',(0.688318015065675,-25.941372847213,
12.));
#225493=CARTESIAN_POINT('Ctrl Pts',(0.677559543215902,-25.9614434298092,
0.));
#225494=CARTESIAN_POINT('Ctrl Pts',(0.677559543215902,-25.9614434298092,
12.));
#225495=CARTESIAN_POINT('Ctrl Pts',(0.669451306784414,-25.9765104298171,
0.));
#225496=CARTESIAN_POINT('Ctrl Pts',(0.669451306784414,-25.9765104298171,
12.));
#225497=CARTESIAN_POINT('Ctrl Pts',(0.664028313188911,-25.9865613464809,
0.));
#225498=CARTESIAN_POINT('Ctrl Pts',(0.664028313188911,-25.9865613464809,
12.));
#225499=CARTESIAN_POINT('Ctrl Pts',(0.66131244073089,-25.991588367311,0.));
#225500=CARTESIAN_POINT('Ctrl Pts',(0.66131244073089,-25.991588367311,12.));
#225501=CARTESIAN_POINT('',(0.66131244073089,-25.991588367311,0.));
#225502=CARTESIAN_POINT('Ctrl Pts',(1.76341220531179,-22.4835757167854,
0.));
#225503=CARTESIAN_POINT('Ctrl Pts',(1.76341415538764,-22.483581992979,0.));
#225504=CARTESIAN_POINT('Ctrl Pts',(1.7634206426357,-22.4836387052232,0.));
#225505=CARTESIAN_POINT('Ctrl Pts',(1.76343813434565,-22.483856251707,0.));
#225506=CARTESIAN_POINT('Ctrl Pts',(1.76347698284791,-22.4844112933129,
0.));
#225507=CARTESIAN_POINT('Ctrl Pts',(1.76355076045546,-22.4855446605991,
0.));
#225508=CARTESIAN_POINT('Ctrl Pts',(1.76364784232963,-22.4871115206571,
0.));
#225509=CARTESIAN_POINT('Ctrl Pts',(1.76376424879504,-22.4890991659478,
0.));
#225510=CARTESIAN_POINT('Ctrl Pts',(1.76389475965723,-22.4914909094908,
0.));
#225511=CARTESIAN_POINT('Ctrl Pts',(1.764033938803,-22.4942693792449,0.));
#225512=CARTESIAN_POINT('Ctrl Pts',(1.76417731243462,-22.4974203063191,
0.));
#225513=CARTESIAN_POINT('Ctrl Pts',(1.76432160068725,-22.5009332677316,
0.));
#225514=CARTESIAN_POINT('Ctrl Pts',(1.76446408210366,-22.5047996391978,
0.));
#225515=CARTESIAN_POINT('Ctrl Pts',(1.76460218257323,-22.5090112700212,
0.));
#225516=CARTESIAN_POINT('Ctrl Pts',(1.76473303281158,-22.5135590569554,
0.));
#225517=CARTESIAN_POINT('Ctrl Pts',(1.76485369319896,-22.5184336670207,
0.));
#225518=CARTESIAN_POINT('Ctrl Pts',(1.76496128643369,-22.5236259635515,
0.));
#225519=CARTESIAN_POINT('Ctrl Pts',(1.76505320262751,-22.529127665298,0.));
#225520=CARTESIAN_POINT('Ctrl Pts',(1.7651271156325,-22.5349313983571,0.));
#225521=CARTESIAN_POINT('Ctrl Pts',(1.76518087841492,-22.5410303590891,
0.));
#225522=CARTESIAN_POINT('Ctrl Pts',(1.76521245524047,-22.5474180954006,
0.));
#225523=CARTESIAN_POINT('Ctrl Pts',(1.76521983384062,-22.5540882235837,
0.));
#225524=CARTESIAN_POINT('Ctrl Pts',(1.76520104500449,-22.5610344912501,
0.));
#225525=CARTESIAN_POINT('Ctrl Pts',(1.76515418518829,-22.5682508499873,
0.));
#225526=CARTESIAN_POINT('Ctrl Pts',(1.76507744026747,-22.5757315316355,
0.));
#225527=CARTESIAN_POINT('Ctrl Pts',(1.76496910283088,-22.5834711038024,
0.));
#225528=CARTESIAN_POINT('Ctrl Pts',(1.76482755288411,-22.5914644078106,
0.));
#225529=CARTESIAN_POINT('Ctrl Pts',(1.76465124413556,-22.5997065145638,
0.));
#225530=CARTESIAN_POINT('Ctrl Pts',(1.76443868648015,-22.6081926681342,
0.));
#225531=CARTESIAN_POINT('Ctrl Pts',(1.76418843543739,-22.6169182517693,
0.));
#225532=CARTESIAN_POINT('Ctrl Pts',(1.76389909571402,-22.6258787994847,
0.));
#225533=CARTESIAN_POINT('Ctrl Pts',(1.76356932176272,-22.635069997936,0.));
#225534=CARTESIAN_POINT('Ctrl Pts',(1.76319782013913,-22.6444876940425,
0.));
#225535=CARTESIAN_POINT('Ctrl Pts',(1.76278334912559,-22.6541278938413,
0.));
#225536=CARTESIAN_POINT('Ctrl Pts',(1.76232471392567,-22.6639867471756,
0.));
#225537=CARTESIAN_POINT('Ctrl Pts',(1.76182076289525,-22.6740605356699,
0.));
#225538=CARTESIAN_POINT('Ctrl Pts',(1.76127038310612,-22.6843456585245,
0.));
#225539=CARTESIAN_POINT('Ctrl Pts',(1.76067249704884,-22.6948386219843,
0.));
#225540=CARTESIAN_POINT('Ctrl Pts',(1.76002606202398,-22.7055360375481,
0.));
#225541=CARTESIAN_POINT('Ctrl Pts',(1.75933006905924,-22.7164346186007,
0.));
#225542=CARTESIAN_POINT('Ctrl Pts',(1.75858354204634,-22.7275311777305,
0.));
#225543=CARTESIAN_POINT('Ctrl Pts',(1.75778553673249,-22.7388226235565,
0.));
#225544=CARTESIAN_POINT('Ctrl Pts',(1.75693513908911,-22.7503059556455,
0.));
#225545=CARTESIAN_POINT('Ctrl Pts',(1.7560314637164,-22.7619782595013,0.));
#225546=CARTESIAN_POINT('Ctrl Pts',(1.75507365227127,-22.7738367016115,
0.));
#225547=CARTESIAN_POINT('Ctrl Pts',(1.75406087182929,-22.7858785242358,
0.));
#225548=CARTESIAN_POINT('Ctrl Pts',(1.75299231391461,-22.7981010424312,
0.));
#225549=CARTESIAN_POINT('Ctrl Pts',(1.75186719365589,-22.8105016414712,
0.));
#225550=CARTESIAN_POINT('Ctrl Pts',(1.75068474890883,-22.8230777741285,
0.));
#225551=CARTESIAN_POINT('Ctrl Pts',(1.74944423940117,-22.8358269579854,
0.));
#225552=CARTESIAN_POINT('Ctrl Pts',(1.74814494588491,-22.8487467728075,
0.));
#225553=CARTESIAN_POINT('Ctrl Pts',(1.74678616930663,-22.8618348580234,
0.));
#225554=CARTESIAN_POINT('Ctrl Pts',(1.74536722998199,-22.8750889101696,
0.));
#225555=CARTESIAN_POINT('Ctrl Pts',(1.74388746677702,-22.8885066803351,
0.));
#225556=CARTESIAN_POINT('Ctrl Pts',(1.74234623630079,-22.9020859716144,
0.));
#225557=CARTESIAN_POINT('Ctrl Pts',(1.74074291231056,-22.9158246373365,
0.));
#225558=CARTESIAN_POINT('Ctrl Pts',(1.73907688511664,-22.9297205792587,
0.));
#225559=CARTESIAN_POINT('Ctrl Pts',(1.73734756100038,-22.9437717457825,
0.));
#225560=CARTESIAN_POINT('Ctrl Pts',(1.73555436162771,-22.9579761301062,
0.));
#225561=CARTESIAN_POINT('Ctrl Pts',(1.73369672350817,-22.9723317685688,
0.));
#225562=CARTESIAN_POINT('Ctrl Pts',(1.73177409750193,-22.9868367391978,
0.));
#225563=CARTESIAN_POINT('Ctrl Pts',(1.72978594832137,-23.0014891601891,
0.));
#225564=CARTESIAN_POINT('Ctrl Pts',(1.72773175404702,-23.0162871884167,
0.));
#225565=CARTESIAN_POINT('Ctrl Pts',(1.72561100564033,-23.031229017888,0.));
#225566=CARTESIAN_POINT('Ctrl Pts',(1.72342320653731,-23.0463128785528,
0.));
#225567=CARTESIAN_POINT('Ctrl Pts',(1.7211678722598,-23.061537035156,0.));
#225568=CARTESIAN_POINT('Ctrl Pts',(1.71884453003027,-23.0768997860709,
0.));
#225569=CARTESIAN_POINT('Ctrl Pts',(1.71645271839311,-23.0923994621216,
0.));
#225570=CARTESIAN_POINT('Ctrl Pts',(1.71399198684724,-23.1080344254291,
0.));
#225571=CARTESIAN_POINT('Ctrl Pts',(1.71146189552192,-23.1238030684929,
0.));
#225572=CARTESIAN_POINT('Ctrl Pts',(1.70886201485459,-23.1397038132358,
0.));
#225573=CARTESIAN_POINT('Ctrl Pts',(1.70619192527846,-23.1557351100613,
0.));
#225574=CARTESIAN_POINT('Ctrl Pts',(1.70345121691259,-23.1718954368749,
0.));
#225575=CARTESIAN_POINT('Ctrl Pts',(1.70063948926987,-23.1881832981848,
0.));
#225576=CARTESIAN_POINT('Ctrl Pts',(1.69775635099425,-23.2045972243765,
0.));
#225577=CARTESIAN_POINT('Ctrl Pts',(1.69480141959945,-23.2211357709374,
0.));
#225578=CARTESIAN_POINT('Ctrl Pts',(1.69177432121716,-23.2377975177014,
0.));
#225579=CARTESIAN_POINT('Ctrl Pts',(1.6886746903491,-23.2545810680536,0.));
#225580=CARTESIAN_POINT('Ctrl Pts',(1.68550216963274,-23.2714850482245,
0.));
#225581=CARTESIAN_POINT('Ctrl Pts',(1.68225640962181,-23.2885081066949,
0.));
#225582=CARTESIAN_POINT('Ctrl Pts',(1.67893706857123,-23.3056489135611,
0.));
#225583=CARTESIAN_POINT('Ctrl Pts',(1.67554381222987,-23.3229061599145,
0.));
#225584=CARTESIAN_POINT('Ctrl Pts',(1.67207631363905,-23.3402785571866,
0.));
#225585=CARTESIAN_POINT('Ctrl Pts',(1.66853425293977,-23.3577648365747,
0.));
#225586=CARTESIAN_POINT('Ctrl Pts',(1.66491731718864,-23.375363748555,0.));
#225587=CARTESIAN_POINT('Ctrl Pts',(1.66122520018008,-23.3930740623622,
0.));
#225588=CARTESIAN_POINT('Ctrl Pts',(1.65745760227507,-23.4108945654803,
0.));
#225589=CARTESIAN_POINT('Ctrl Pts',(1.6536142302373,-23.4288240631034,0.));
#225590=CARTESIAN_POINT('Ctrl Pts',(1.64969479707339,-23.446861377656,0.));
#225591=CARTESIAN_POINT('Ctrl Pts',(1.64569902187608,-23.4650053483919,
0.));
#225592=CARTESIAN_POINT('Ctrl Pts',(1.64162662967524,-23.4832548309638,
0.));
#225593=CARTESIAN_POINT('Ctrl Pts',(1.63747735129474,-23.5016086970006,
0.));
#225594=CARTESIAN_POINT('Ctrl Pts',(1.63325092321731,-23.5200658336624,
0.));
#225595=CARTESIAN_POINT('Ctrl Pts',(1.62894708745231,-23.5386251432278,
0.));
#225596=CARTESIAN_POINT('Ctrl Pts',(1.62456559140071,-23.5572855427617,
0.));
#225597=CARTESIAN_POINT('Ctrl Pts',(1.62010618772869,-23.5760459637608,
0.));
#225598=CARTESIAN_POINT('Ctrl Pts',(1.61556863424697,-23.5949053517996,
0.));
#225599=CARTESIAN_POINT('Ctrl Pts',(1.61095269379773,-23.6138626661644,
0.));
#225600=CARTESIAN_POINT('Ctrl Pts',(1.60625813414666,-23.6329168794916,
0.));
#225601=CARTESIAN_POINT('Ctrl Pts',(1.60148472786588,-23.6520669774863,
0.));
#225602=CARTESIAN_POINT('Ctrl Pts',(1.59663225222458,-23.6713119586302,
0.));
#225603=CARTESIAN_POINT('Ctrl Pts',(1.59170048908631,-23.6906508338833,
0.));
#225604=CARTESIAN_POINT('Ctrl Pts',(1.58668922481222,-23.7100826263835,
0.));
#225605=CARTESIAN_POINT('Ctrl Pts',(1.58159825017362,-23.7296063711308,
0.));
#225606=CARTESIAN_POINT('Ctrl Pts',(1.57642736025251,-23.7492211147369,
0.));
#225607=CARTESIAN_POINT('Ctrl Pts',(1.57117635434412,-23.7689259151869,
0.));
#225608=CARTESIAN_POINT('Ctrl Pts',(1.56584503586844,-23.788719841588,0.));
#225609=CARTESIAN_POINT('Ctrl Pts',(1.56043321228631,-23.8086019739192,
0.));
#225610=CARTESIAN_POINT('Ctrl Pts',(1.55494069502627,-23.8285714027631,
0.));
#225611=CARTESIAN_POINT('Ctrl Pts',(1.5493672994053,-23.8486272290698,0.));
#225612=CARTESIAN_POINT('Ctrl Pts',(1.54371284453977,-23.8687685639635,
0.));
#225613=CARTESIAN_POINT('Ctrl Pts',(1.53797715326748,-23.8889945285313,
0.));
#225614=CARTESIAN_POINT('Ctrl Pts',(1.53216005207462,-23.9093042536119,
0.));
#225615=CARTESIAN_POINT('Ctrl Pts',(1.52626137103039,-23.9296968795761,
0.));
#225616=CARTESIAN_POINT('Ctrl Pts',(1.52028094372806,-23.9501715561038,
0.));
#225617=CARTESIAN_POINT('Ctrl Pts',(1.51421860720628,-23.9707274420145,
0.));
#225618=CARTESIAN_POINT('Ctrl Pts',(1.50807420187702,-23.991363705093,0.));
#225619=CARTESIAN_POINT('Ctrl Pts',(1.50184757146099,-24.0120795219086,
0.));
#225620=CARTESIAN_POINT('Ctrl Pts',(1.49553856292798,-24.0328740776331,
0.));
#225621=CARTESIAN_POINT('Ctrl Pts',(1.48914702644883,-24.053746565843,0.));
#225622=CARTESIAN_POINT('Ctrl Pts',(1.4826728153368,-24.074696188353,0.));
#225623=CARTESIAN_POINT('Ctrl Pts',(1.47611578597741,-24.0957221550782,
0.));
#225624=CARTESIAN_POINT('Ctrl Pts',(1.46947579776991,-24.1168236838827,
0.));
#225625=CARTESIAN_POINT('Ctrl Pts',(1.46275271307398,-24.1380000004272,
0.));
#225626=CARTESIAN_POINT('Ctrl Pts',(1.45594639716314,-24.1592503380105,
0.));
#225627=CARTESIAN_POINT('Ctrl Pts',(1.4490567181872,-24.1805739374033,0.));
#225628=CARTESIAN_POINT('Ctrl Pts',(1.44208354711074,-24.2019700467214,
0.));
#225629=CARTESIAN_POINT('Ctrl Pts',(1.43502675765502,-24.2234379212978,
0.));
#225630=CARTESIAN_POINT('Ctrl Pts',(1.42788622624851,-24.2449768235485,
0.));
#225631=CARTESIAN_POINT('Ctrl Pts',(1.42066183198252,-24.2665860228357,
0.));
#225632=CARTESIAN_POINT('Ctrl Pts',(1.41335345657684,-24.2882647953214,
0.));
#225633=CARTESIAN_POINT('Ctrl Pts',(1.4059609843434,-24.3100124238316,0.));
#225634=CARTESIAN_POINT('Ctrl Pts',(1.3984843021281,-24.3318281977647,0.));
#225635=CARTESIAN_POINT('Ctrl Pts',(1.3909232992639,-24.3537114129877,0.));
#225636=CARTESIAN_POINT('Ctrl Pts',(1.38327786752998,-24.37566137173,0.));
#225637=CARTESIAN_POINT('Ctrl Pts',(1.37554790111607,-24.3976773824731,
0.));
#225638=CARTESIAN_POINT('Ctrl Pts',(1.36773329659954,-24.4197587598337,
0.));
#225639=CARTESIAN_POINT('Ctrl Pts',(1.35983395290624,-24.4419048244524,
0.));
#225640=CARTESIAN_POINT('Ctrl Pts',(1.35184977125644,-24.4641149028894,
0.));
#225641=CARTESIAN_POINT('Ctrl Pts',(1.34378065512335,-24.4863883275135,
0.));
#225642=CARTESIAN_POINT('Ctrl Pts',(1.33562651019684,-24.5087244363856,
0.));
#225643=CARTESIAN_POINT('Ctrl Pts',(1.32738724435326,-24.5311225731434,
0.));
#225644=CARTESIAN_POINT('Ctrl Pts',(1.31906276763669,-24.5535820868671,
0.));
#225645=CARTESIAN_POINT('Ctrl Pts',(1.31065299222023,-24.576102332018,0.));
#225646=CARTESIAN_POINT('Ctrl Pts',(1.30215783236363,-24.5986826684025,
0.));
#225647=CARTESIAN_POINT('Ctrl Pts',(1.29357720438107,-24.6213224611228,
0.));
#225648=CARTESIAN_POINT('Ctrl Pts',(1.28491102661513,-24.6440210805278,
0.));
#225649=CARTESIAN_POINT('Ctrl Pts',(1.2761592194164,-24.666777902156,0.));
#225650=CARTESIAN_POINT('Ctrl Pts',(1.26732170513497,-24.6895923066837,
0.));
#225651=CARTESIAN_POINT('Ctrl Pts',(1.25839840807414,-24.7124636797895,
0.));
#225652=CARTESIAN_POINT('Ctrl Pts',(1.24938925444323,-24.7353914120012,
0.));
#225653=CARTESIAN_POINT('Ctrl Pts',(1.24029417231987,-24.7583748985439,
0.));
#225654=CARTESIAN_POINT('Ctrl Pts',(1.23111309161843,-24.78141353918,0.));
#225655=CARTESIAN_POINT('Ctrl Pts',(1.22184594406526,-24.8045067380536,
0.));
#225656=CARTESIAN_POINT('Ctrl Pts',(1.21249266318205,-24.8276539035092,
0.));
#225657=CARTESIAN_POINT('Ctrl Pts',(1.20305318426015,-24.8508544481973,
0.));
#225658=CARTESIAN_POINT('Ctrl Pts',(1.19352744434059,-24.8741077892074,
0.));
#225659=CARTESIAN_POINT('Ctrl Pts',(1.18391538220098,-24.8974133481829,
0.));
#225660=CARTESIAN_POINT('Ctrl Pts',(1.17421693835039,-24.9207705514449,
0.));
#225661=CARTESIAN_POINT('Ctrl Pts',(1.16443205502852,-24.9441788300932,
0.));
#225662=CARTESIAN_POINT('Ctrl Pts',(1.15456067621894,-24.9676376201501,
0.));
#225663=CARTESIAN_POINT('Ctrl Pts',(1.14460274758206,-24.9911463621431,
0.));
#225664=CARTESIAN_POINT('Ctrl Pts',(1.13455821638535,-25.0147045006193,
0.));
#225665=CARTESIAN_POINT('Ctrl Pts',(1.12442703144455,-25.0383114836898,
0.));
#225666=CARTESIAN_POINT('Ctrl Pts',(1.1142091430689,-25.0619667625336,0.));
#225667=CARTESIAN_POINT('Ctrl Pts',(1.1039045030174,-25.085669790968,0.));
#225668=CARTESIAN_POINT('Ctrl Pts',(1.09351306445299,-25.1094200248448,
0.));
#225669=CARTESIAN_POINT('Ctrl Pts',(1.08303478197174,-25.1332169227415,
0.));
#225670=CARTESIAN_POINT('Ctrl Pts',(1.07246961165459,-25.1570599469311,
0.));
#225671=CARTESIAN_POINT('Ctrl Pts',(1.06181751111754,-25.1809485642191,
0.));
#225672=CARTESIAN_POINT('Ctrl Pts',(1.05107843957925,-25.2048822469027,
0.));
#225673=CARTESIAN_POINT('Ctrl Pts',(1.04025235791514,-25.2288604735087,
0.));
#225674=CARTESIAN_POINT('Ctrl Pts',(1.0293392287683,-25.2528827300427,0.));
#225675=CARTESIAN_POINT('Ctrl Pts',(1.01833901642272,-25.2769485087268,
0.));
#225676=CARTESIAN_POINT('Ctrl Pts',(1.00725168656933,-25.3010573055557,
0.));
#225677=CARTESIAN_POINT('Ctrl Pts',(0.996077206120918,-25.3252086182976,
0.));
#225678=CARTESIAN_POINT('Ctrl Pts',(0.984815543004088,-25.3494019441444,
0.));
#225679=CARTESIAN_POINT('Ctrl Pts',(0.973466666000047,-25.3736367778842,
0.));
#225680=CARTESIAN_POINT('Ctrl Pts',(0.962030544502801,-25.3979126089155,
0.));
#225681=CARTESIAN_POINT('Ctrl Pts',(0.950507148596967,-25.4222289223155,
0.));
#225682=CARTESIAN_POINT('Ctrl Pts',(0.938896449495631,-25.4465852044835,
0.));
#225683=CARTESIAN_POINT('Ctrl Pts',(0.927198419885603,-25.4709809474996,
0.));
#225684=CARTESIAN_POINT('Ctrl Pts',(0.915413034335331,-25.4954156541787,
0.));
#225685=CARTESIAN_POINT('Ctrl Pts',(0.903540269651152,-25.5198888424195,
0.));
#225686=CARTESIAN_POINT('Ctrl Pts',(0.891580105349464,-25.5444000508223,
0.));
#225687=CARTESIAN_POINT('Ctrl Pts',(0.879532523835088,-25.568948840818,
0.));
#225688=CARTESIAN_POINT('Ctrl Pts',(0.867397509339468,-25.5935347843616,
0.));
#225689=CARTESIAN_POINT('Ctrl Pts',(0.855175047037614,-25.618157453608,
0.));
#225690=CARTESIAN_POINT('Ctrl Pts',(0.842865122121542,-25.6428164100078,
0.));
#225691=CARTESIAN_POINT('Ctrl Pts',(0.830467718864366,-25.6675111931957,
0.));
#225692=CARTESIAN_POINT('Ctrl Pts',(0.817982819786718,-25.6922413110172,
0.));
#225693=CARTESIAN_POINT('Ctrl Pts',(0.805410404552592,-25.7170062262474,
0.));
#225694=CARTESIAN_POINT('Ctrl Pts',(0.792750451613533,-25.7418053757671,
0.));
#225695=CARTESIAN_POINT('Ctrl Pts',(0.780002940289024,-25.7666381946871,
0.));
#225696=CARTESIAN_POINT('Ctrl Pts',(0.767167852648638,-25.7915041383304,
0.));
#225697=CARTESIAN_POINT('Ctrl Pts',(0.754245175608287,-25.816402705995,
0.));
#225698=CARTESIAN_POINT('Ctrl Pts',(0.741234902664695,-25.841333461908,
0.));
#225699=CARTESIAN_POINT('Ctrl Pts',(0.728137036485876,-25.8662960624285,
0.));
#225700=CARTESIAN_POINT('Ctrl Pts',(0.714951588533752,-25.8912902615141,
0.));
#225701=CARTESIAN_POINT('Ctrl Pts',(0.701678575236601,-25.9163158909645,
0.));
#225702=CARTESIAN_POINT('Ctrl Pts',(0.688318015065675,-25.941372847213,
0.));
#225703=CARTESIAN_POINT('Ctrl Pts',(0.677559543215902,-25.9614434298092,
0.));
#225704=CARTESIAN_POINT('Ctrl Pts',(0.669451306784414,-25.9765104298171,
0.));
#225705=CARTESIAN_POINT('Ctrl Pts',(0.664028313188911,-25.9865613464809,
0.));
#225706=CARTESIAN_POINT('Ctrl Pts',(0.66131244073089,-25.991588367311,0.));
#225707=CARTESIAN_POINT('',(0.66131244073089,-25.991588367311,12.));
#225708=CARTESIAN_POINT('Ctrl Pts',(0.66131244073089,-25.991588367311,12.));
#225709=CARTESIAN_POINT('Ctrl Pts',(0.664028313188911,-25.9865613464809,
12.));
#225710=CARTESIAN_POINT('Ctrl Pts',(0.669451306784414,-25.9765104298171,
12.));
#225711=CARTESIAN_POINT('Ctrl Pts',(0.677559543215902,-25.9614434298092,
12.));
#225712=CARTESIAN_POINT('Ctrl Pts',(0.688318015065675,-25.941372847213,
12.));
#225713=CARTESIAN_POINT('Ctrl Pts',(0.701678575236601,-25.9163158909645,
12.));
#225714=CARTESIAN_POINT('Ctrl Pts',(0.714951588533752,-25.8912902615141,
12.));
#225715=CARTESIAN_POINT('Ctrl Pts',(0.728137036485876,-25.8662960624285,
12.));
#225716=CARTESIAN_POINT('Ctrl Pts',(0.741234902664695,-25.841333461908,
12.));
#225717=CARTESIAN_POINT('Ctrl Pts',(0.754245175608287,-25.816402705995,
12.));
#225718=CARTESIAN_POINT('Ctrl Pts',(0.767167852648638,-25.7915041383304,
12.));
#225719=CARTESIAN_POINT('Ctrl Pts',(0.780002940289024,-25.7666381946871,
12.));
#225720=CARTESIAN_POINT('Ctrl Pts',(0.792750451613533,-25.7418053757671,
12.));
#225721=CARTESIAN_POINT('Ctrl Pts',(0.805410404552592,-25.7170062262474,
12.));
#225722=CARTESIAN_POINT('Ctrl Pts',(0.817982819786718,-25.6922413110172,
12.));
#225723=CARTESIAN_POINT('Ctrl Pts',(0.830467718864366,-25.6675111931957,
12.));
#225724=CARTESIAN_POINT('Ctrl Pts',(0.842865122121542,-25.6428164100078,
12.));
#225725=CARTESIAN_POINT('Ctrl Pts',(0.855175047037614,-25.618157453608,
12.));
#225726=CARTESIAN_POINT('Ctrl Pts',(0.867397509339468,-25.5935347843616,
12.));
#225727=CARTESIAN_POINT('Ctrl Pts',(0.879532523835088,-25.568948840818,
12.));
#225728=CARTESIAN_POINT('Ctrl Pts',(0.891580105349464,-25.5444000508223,
12.));
#225729=CARTESIAN_POINT('Ctrl Pts',(0.903540269651152,-25.5198888424195,
12.));
#225730=CARTESIAN_POINT('Ctrl Pts',(0.915413034335331,-25.4954156541787,
12.));
#225731=CARTESIAN_POINT('Ctrl Pts',(0.927198419885603,-25.4709809474996,
12.));
#225732=CARTESIAN_POINT('Ctrl Pts',(0.938896449495631,-25.4465852044835,
12.));
#225733=CARTESIAN_POINT('Ctrl Pts',(0.950507148596967,-25.4222289223155,
12.));
#225734=CARTESIAN_POINT('Ctrl Pts',(0.962030544502801,-25.3979126089155,
12.));
#225735=CARTESIAN_POINT('Ctrl Pts',(0.973466666000047,-25.3736367778842,
12.));
#225736=CARTESIAN_POINT('Ctrl Pts',(0.984815543004088,-25.3494019441444,
12.));
#225737=CARTESIAN_POINT('Ctrl Pts',(0.996077206120918,-25.3252086182976,
12.));
#225738=CARTESIAN_POINT('Ctrl Pts',(1.00725168656933,-25.3010573055557,
12.));
#225739=CARTESIAN_POINT('Ctrl Pts',(1.01833901642272,-25.2769485087268,
12.));
#225740=CARTESIAN_POINT('Ctrl Pts',(1.0293392287683,-25.2528827300427,12.));
#225741=CARTESIAN_POINT('Ctrl Pts',(1.04025235791514,-25.2288604735087,
12.));
#225742=CARTESIAN_POINT('Ctrl Pts',(1.05107843957925,-25.2048822469027,
12.));
#225743=CARTESIAN_POINT('Ctrl Pts',(1.06181751111754,-25.1809485642191,
12.));
#225744=CARTESIAN_POINT('Ctrl Pts',(1.07246961165459,-25.1570599469311,
12.));
#225745=CARTESIAN_POINT('Ctrl Pts',(1.08303478197174,-25.1332169227415,
12.));
#225746=CARTESIAN_POINT('Ctrl Pts',(1.09351306445299,-25.1094200248448,
12.));
#225747=CARTESIAN_POINT('Ctrl Pts',(1.1039045030174,-25.085669790968,12.));
#225748=CARTESIAN_POINT('Ctrl Pts',(1.1142091430689,-25.0619667625336,12.));
#225749=CARTESIAN_POINT('Ctrl Pts',(1.12442703144455,-25.0383114836898,
12.));
#225750=CARTESIAN_POINT('Ctrl Pts',(1.13455821638535,-25.0147045006193,
12.));
#225751=CARTESIAN_POINT('Ctrl Pts',(1.14460274758206,-24.9911463621431,
12.));
#225752=CARTESIAN_POINT('Ctrl Pts',(1.15456067621894,-24.9676376201501,
12.));
#225753=CARTESIAN_POINT('Ctrl Pts',(1.16443205502852,-24.9441788300932,
12.));
#225754=CARTESIAN_POINT('Ctrl Pts',(1.17421693835039,-24.9207705514449,
12.));
#225755=CARTESIAN_POINT('Ctrl Pts',(1.18391538220098,-24.8974133481829,
12.));
#225756=CARTESIAN_POINT('Ctrl Pts',(1.19352744434059,-24.8741077892074,
12.));
#225757=CARTESIAN_POINT('Ctrl Pts',(1.20305318426015,-24.8508544481973,
12.));
#225758=CARTESIAN_POINT('Ctrl Pts',(1.21249266318205,-24.8276539035092,
12.));
#225759=CARTESIAN_POINT('Ctrl Pts',(1.22184594406526,-24.8045067380536,
12.));
#225760=CARTESIAN_POINT('Ctrl Pts',(1.23111309161843,-24.78141353918,12.));
#225761=CARTESIAN_POINT('Ctrl Pts',(1.24029417231987,-24.7583748985439,
12.));
#225762=CARTESIAN_POINT('Ctrl Pts',(1.24938925444323,-24.7353914120012,
12.));
#225763=CARTESIAN_POINT('Ctrl Pts',(1.25839840807414,-24.7124636797895,
12.));
#225764=CARTESIAN_POINT('Ctrl Pts',(1.26732170513497,-24.6895923066837,
12.));
#225765=CARTESIAN_POINT('Ctrl Pts',(1.2761592194164,-24.666777902156,12.));
#225766=CARTESIAN_POINT('Ctrl Pts',(1.28491102661513,-24.6440210805278,
12.));
#225767=CARTESIAN_POINT('Ctrl Pts',(1.29357720438107,-24.6213224611228,
12.));
#225768=CARTESIAN_POINT('Ctrl Pts',(1.30215783236363,-24.5986826684025,
12.));
#225769=CARTESIAN_POINT('Ctrl Pts',(1.31065299222023,-24.576102332018,12.));
#225770=CARTESIAN_POINT('Ctrl Pts',(1.31906276763669,-24.5535820868671,
12.));
#225771=CARTESIAN_POINT('Ctrl Pts',(1.32738724435326,-24.5311225731434,
12.));
#225772=CARTESIAN_POINT('Ctrl Pts',(1.33562651019684,-24.5087244363856,
12.));
#225773=CARTESIAN_POINT('Ctrl Pts',(1.34378065512335,-24.4863883275135,
12.));
#225774=CARTESIAN_POINT('Ctrl Pts',(1.35184977125644,-24.4641149028894,
12.));
#225775=CARTESIAN_POINT('Ctrl Pts',(1.35983395290624,-24.4419048244524,
12.));
#225776=CARTESIAN_POINT('Ctrl Pts',(1.36773329659954,-24.4197587598337,
12.));
#225777=CARTESIAN_POINT('Ctrl Pts',(1.37554790111607,-24.3976773824731,
12.));
#225778=CARTESIAN_POINT('Ctrl Pts',(1.38327786752998,-24.37566137173,12.));
#225779=CARTESIAN_POINT('Ctrl Pts',(1.3909232992639,-24.3537114129877,12.));
#225780=CARTESIAN_POINT('Ctrl Pts',(1.3984843021281,-24.3318281977647,12.));
#225781=CARTESIAN_POINT('Ctrl Pts',(1.4059609843434,-24.3100124238316,12.));
#225782=CARTESIAN_POINT('Ctrl Pts',(1.41335345657684,-24.2882647953214,
12.));
#225783=CARTESIAN_POINT('Ctrl Pts',(1.42066183198252,-24.2665860228357,
12.));
#225784=CARTESIAN_POINT('Ctrl Pts',(1.42788622624851,-24.2449768235485,
12.));
#225785=CARTESIAN_POINT('Ctrl Pts',(1.43502675765502,-24.2234379212978,
12.));
#225786=CARTESIAN_POINT('Ctrl Pts',(1.44208354711074,-24.2019700467214,
12.));
#225787=CARTESIAN_POINT('Ctrl Pts',(1.4490567181872,-24.1805739374033,12.));
#225788=CARTESIAN_POINT('Ctrl Pts',(1.45594639716314,-24.1592503380105,
12.));
#225789=CARTESIAN_POINT('Ctrl Pts',(1.46275271307398,-24.1380000004272,
12.));
#225790=CARTESIAN_POINT('Ctrl Pts',(1.46947579776991,-24.1168236838827,
12.));
#225791=CARTESIAN_POINT('Ctrl Pts',(1.47611578597741,-24.0957221550782,
12.));
#225792=CARTESIAN_POINT('Ctrl Pts',(1.4826728153368,-24.074696188353,12.));
#225793=CARTESIAN_POINT('Ctrl Pts',(1.48914702644883,-24.053746565843,12.));
#225794=CARTESIAN_POINT('Ctrl Pts',(1.49553856292798,-24.0328740776331,
12.));
#225795=CARTESIAN_POINT('Ctrl Pts',(1.50184757146099,-24.0120795219086,
12.));
#225796=CARTESIAN_POINT('Ctrl Pts',(1.50807420187702,-23.991363705093,12.));
#225797=CARTESIAN_POINT('Ctrl Pts',(1.51421860720628,-23.9707274420145,
12.));
#225798=CARTESIAN_POINT('Ctrl Pts',(1.52028094372806,-23.9501715561038,
12.));
#225799=CARTESIAN_POINT('Ctrl Pts',(1.52626137103039,-23.9296968795761,
12.));
#225800=CARTESIAN_POINT('Ctrl Pts',(1.53216005207462,-23.9093042536119,
12.));
#225801=CARTESIAN_POINT('Ctrl Pts',(1.53797715326748,-23.8889945285313,
12.));
#225802=CARTESIAN_POINT('Ctrl Pts',(1.54371284453977,-23.8687685639635,
12.));
#225803=CARTESIAN_POINT('Ctrl Pts',(1.5493672994053,-23.8486272290698,12.));
#225804=CARTESIAN_POINT('Ctrl Pts',(1.55494069502627,-23.8285714027631,
12.));
#225805=CARTESIAN_POINT('Ctrl Pts',(1.56043321228631,-23.8086019739192,
12.));
#225806=CARTESIAN_POINT('Ctrl Pts',(1.56584503586844,-23.788719841588,12.));
#225807=CARTESIAN_POINT('Ctrl Pts',(1.57117635434412,-23.7689259151869,
12.));
#225808=CARTESIAN_POINT('Ctrl Pts',(1.57642736025251,-23.7492211147369,
12.));
#225809=CARTESIAN_POINT('Ctrl Pts',(1.58159825017362,-23.7296063711308,
12.));
#225810=CARTESIAN_POINT('Ctrl Pts',(1.58668922481222,-23.7100826263835,
12.));
#225811=CARTESIAN_POINT('Ctrl Pts',(1.59170048908631,-23.6906508338833,
12.));
#225812=CARTESIAN_POINT('Ctrl Pts',(1.59663225222458,-23.6713119586302,
12.));
#225813=CARTESIAN_POINT('Ctrl Pts',(1.60148472786588,-23.6520669774863,
12.));
#225814=CARTESIAN_POINT('Ctrl Pts',(1.60625813414666,-23.6329168794916,
12.));
#225815=CARTESIAN_POINT('Ctrl Pts',(1.61095269379773,-23.6138626661644,
12.));
#225816=CARTESIAN_POINT('Ctrl Pts',(1.61556863424697,-23.5949053517996,
12.));
#225817=CARTESIAN_POINT('Ctrl Pts',(1.62010618772869,-23.5760459637608,
12.));
#225818=CARTESIAN_POINT('Ctrl Pts',(1.62456559140071,-23.5572855427617,
12.));
#225819=CARTESIAN_POINT('Ctrl Pts',(1.62894708745231,-23.5386251432278,
12.));
#225820=CARTESIAN_POINT('Ctrl Pts',(1.63325092321731,-23.5200658336624,
12.));
#225821=CARTESIAN_POINT('Ctrl Pts',(1.63747735129474,-23.5016086970006,
12.));
#225822=CARTESIAN_POINT('Ctrl Pts',(1.64162662967524,-23.4832548309638,
12.));
#225823=CARTESIAN_POINT('Ctrl Pts',(1.64569902187608,-23.4650053483919,
12.));
#225824=CARTESIAN_POINT('Ctrl Pts',(1.64969479707339,-23.446861377656,12.));
#225825=CARTESIAN_POINT('Ctrl Pts',(1.6536142302373,-23.4288240631034,12.));
#225826=CARTESIAN_POINT('Ctrl Pts',(1.65745760227507,-23.4108945654803,
12.));
#225827=CARTESIAN_POINT('Ctrl Pts',(1.66122520018008,-23.3930740623622,
12.));
#225828=CARTESIAN_POINT('Ctrl Pts',(1.66491731718864,-23.375363748555,12.));
#225829=CARTESIAN_POINT('Ctrl Pts',(1.66853425293977,-23.3577648365747,
12.));
#225830=CARTESIAN_POINT('Ctrl Pts',(1.67207631363905,-23.3402785571866,
12.));
#225831=CARTESIAN_POINT('Ctrl Pts',(1.67554381222987,-23.3229061599145,
12.));
#225832=CARTESIAN_POINT('Ctrl Pts',(1.67893706857123,-23.3056489135611,
12.));
#225833=CARTESIAN_POINT('Ctrl Pts',(1.68225640962181,-23.2885081066949,
12.));
#225834=CARTESIAN_POINT('Ctrl Pts',(1.68550216963274,-23.2714850482245,
12.));
#225835=CARTESIAN_POINT('Ctrl Pts',(1.6886746903491,-23.2545810680536,12.));
#225836=CARTESIAN_POINT('Ctrl Pts',(1.69177432121716,-23.2377975177014,
12.));
#225837=CARTESIAN_POINT('Ctrl Pts',(1.69480141959945,-23.2211357709374,
12.));
#225838=CARTESIAN_POINT('Ctrl Pts',(1.69775635099425,-23.2045972243765,
12.));
#225839=CARTESIAN_POINT('Ctrl Pts',(1.70063948926987,-23.1881832981848,
12.));
#225840=CARTESIAN_POINT('Ctrl Pts',(1.70345121691259,-23.1718954368749,
12.));
#225841=CARTESIAN_POINT('Ctrl Pts',(1.70619192527846,-23.1557351100613,
12.));
#225842=CARTESIAN_POINT('Ctrl Pts',(1.70886201485459,-23.1397038132358,
12.));
#225843=CARTESIAN_POINT('Ctrl Pts',(1.71146189552192,-23.1238030684929,
12.));
#225844=CARTESIAN_POINT('Ctrl Pts',(1.71399198684724,-23.1080344254291,
12.));
#225845=CARTESIAN_POINT('Ctrl Pts',(1.71645271839311,-23.0923994621216,
12.));
#225846=CARTESIAN_POINT('Ctrl Pts',(1.71884453003027,-23.0768997860709,
12.));
#225847=CARTESIAN_POINT('Ctrl Pts',(1.7211678722598,-23.061537035156,12.));
#225848=CARTESIAN_POINT('Ctrl Pts',(1.72342320653731,-23.0463128785528,
12.));
#225849=CARTESIAN_POINT('Ctrl Pts',(1.72561100564033,-23.031229017888,12.));
#225850=CARTESIAN_POINT('Ctrl Pts',(1.72773175404702,-23.0162871884167,
12.));
#225851=CARTESIAN_POINT('Ctrl Pts',(1.72978594832137,-23.0014891601891,
12.));
#225852=CARTESIAN_POINT('Ctrl Pts',(1.73177409750193,-22.9868367391978,
12.));
#225853=CARTESIAN_POINT('Ctrl Pts',(1.73369672350817,-22.9723317685688,
12.));
#225854=CARTESIAN_POINT('Ctrl Pts',(1.73555436162771,-22.9579761301062,
12.));
#225855=CARTESIAN_POINT('Ctrl Pts',(1.73734756100038,-22.9437717457825,
12.));
#225856=CARTESIAN_POINT('Ctrl Pts',(1.73907688511664,-22.9297205792587,
12.));
#225857=CARTESIAN_POINT('Ctrl Pts',(1.74074291231056,-22.9158246373365,
12.));
#225858=CARTESIAN_POINT('Ctrl Pts',(1.74234623630079,-22.9020859716144,
12.));
#225859=CARTESIAN_POINT('Ctrl Pts',(1.74388746677702,-22.8885066803351,
12.));
#225860=CARTESIAN_POINT('Ctrl Pts',(1.74536722998199,-22.8750889101696,
12.));
#225861=CARTESIAN_POINT('Ctrl Pts',(1.74678616930663,-22.8618348580234,
12.));
#225862=CARTESIAN_POINT('Ctrl Pts',(1.74814494588491,-22.8487467728075,
12.));
#225863=CARTESIAN_POINT('Ctrl Pts',(1.74944423940117,-22.8358269579854,
12.));
#225864=CARTESIAN_POINT('Ctrl Pts',(1.75068474890883,-22.8230777741285,
12.));
#225865=CARTESIAN_POINT('Ctrl Pts',(1.75186719365589,-22.8105016414712,
12.));
#225866=CARTESIAN_POINT('Ctrl Pts',(1.75299231391461,-22.7981010424312,
12.));
#225867=CARTESIAN_POINT('Ctrl Pts',(1.75406087182929,-22.7858785242358,
12.));
#225868=CARTESIAN_POINT('Ctrl Pts',(1.75507365227127,-22.7738367016115,
12.));
#225869=CARTESIAN_POINT('Ctrl Pts',(1.7560314637164,-22.7619782595013,12.));
#225870=CARTESIAN_POINT('Ctrl Pts',(1.75693513908911,-22.7503059556455,
12.));
#225871=CARTESIAN_POINT('Ctrl Pts',(1.75778553673249,-22.7388226235565,
12.));
#225872=CARTESIAN_POINT('Ctrl Pts',(1.75858354204634,-22.7275311777305,
12.));
#225873=CARTESIAN_POINT('Ctrl Pts',(1.75933006905924,-22.7164346186007,
12.));
#225874=CARTESIAN_POINT('Ctrl Pts',(1.76002606202398,-22.7055360375481,
12.));
#225875=CARTESIAN_POINT('Ctrl Pts',(1.76067249704884,-22.6948386219843,
12.));
#225876=CARTESIAN_POINT('Ctrl Pts',(1.76127038310612,-22.6843456585245,
12.));
#225877=CARTESIAN_POINT('Ctrl Pts',(1.76182076289525,-22.6740605356699,
12.));
#225878=CARTESIAN_POINT('Ctrl Pts',(1.76232471392567,-22.6639867471756,
12.));
#225879=CARTESIAN_POINT('Ctrl Pts',(1.76278334912559,-22.6541278938413,
12.));
#225880=CARTESIAN_POINT('Ctrl Pts',(1.76319782013913,-22.6444876940425,
12.));
#225881=CARTESIAN_POINT('Ctrl Pts',(1.76356932176272,-22.635069997936,12.));
#225882=CARTESIAN_POINT('Ctrl Pts',(1.76389909571402,-22.6258787994847,
12.));
#225883=CARTESIAN_POINT('Ctrl Pts',(1.76418843543739,-22.6169182517693,
12.));
#225884=CARTESIAN_POINT('Ctrl Pts',(1.76443868648015,-22.6081926681342,
12.));
#225885=CARTESIAN_POINT('Ctrl Pts',(1.76465124413556,-22.5997065145638,
12.));
#225886=CARTESIAN_POINT('Ctrl Pts',(1.76482755288411,-22.5914644078106,
12.));
#225887=CARTESIAN_POINT('Ctrl Pts',(1.76496910283088,-22.5834711038024,
12.));
#225888=CARTESIAN_POINT('Ctrl Pts',(1.76507744026747,-22.5757315316355,
12.));
#225889=CARTESIAN_POINT('Ctrl Pts',(1.76515418518829,-22.5682508499873,
12.));
#225890=CARTESIAN_POINT('Ctrl Pts',(1.76520104500449,-22.5610344912501,
12.));
#225891=CARTESIAN_POINT('Ctrl Pts',(1.76521983384062,-22.5540882235837,
12.));
#225892=CARTESIAN_POINT('Ctrl Pts',(1.76521245524047,-22.5474180954006,
12.));
#225893=CARTESIAN_POINT('Ctrl Pts',(1.76518087841492,-22.5410303590891,
12.));
#225894=CARTESIAN_POINT('Ctrl Pts',(1.7651271156325,-22.5349313983571,12.));
#225895=CARTESIAN_POINT('Ctrl Pts',(1.76505320262751,-22.529127665298,12.));
#225896=CARTESIAN_POINT('Ctrl Pts',(1.76496128643369,-22.5236259635515,
12.));
#225897=CARTESIAN_POINT('Ctrl Pts',(1.76485369319896,-22.5184336670207,
12.));
#225898=CARTESIAN_POINT('Ctrl Pts',(1.76473303281158,-22.5135590569554,
12.));
#225899=CARTESIAN_POINT('Ctrl Pts',(1.76460218257323,-22.5090112700212,
12.));
#225900=CARTESIAN_POINT('Ctrl Pts',(1.76446408210366,-22.5047996391978,
12.));
#225901=CARTESIAN_POINT('Ctrl Pts',(1.76432160068725,-22.5009332677316,
12.));
#225902=CARTESIAN_POINT('Ctrl Pts',(1.76417731243462,-22.4974203063191,
12.));
#225903=CARTESIAN_POINT('Ctrl Pts',(1.764033938803,-22.4942693792449,12.));
#225904=CARTESIAN_POINT('Ctrl Pts',(1.76389475965723,-22.4914909094908,
12.));
#225905=CARTESIAN_POINT('Ctrl Pts',(1.76376424879504,-22.4890991659478,
12.));
#225906=CARTESIAN_POINT('Ctrl Pts',(1.76364784232963,-22.4871115206571,
12.));
#225907=CARTESIAN_POINT('Ctrl Pts',(1.76355076045546,-22.4855446605991,
12.));
#225908=CARTESIAN_POINT('Ctrl Pts',(1.76347698284791,-22.4844112933129,
12.));
#225909=CARTESIAN_POINT('Ctrl Pts',(1.76343813434565,-22.483856251707,12.));
#225910=CARTESIAN_POINT('Ctrl Pts',(1.7634206426357,-22.4836387052232,12.));
#225911=CARTESIAN_POINT('Ctrl Pts',(1.76341415538764,-22.483581992979,12.));
#225912=CARTESIAN_POINT('Ctrl Pts',(1.76341220531179,-22.4835757167854,
12.));
#225913=CARTESIAN_POINT('',(0.66131244073089,-25.991588367311,0.));
#225914=CARTESIAN_POINT('Origin',(-3.92374859571502,-21.1389261070099,0.));
#225915=CARTESIAN_POINT('',(-4.11585220600463,-22.1738711152697,12.));
#225916=CARTESIAN_POINT('',(-1.96187429785751,-10.5694630535049,12.));
#225917=CARTESIAN_POINT('',(-4.11585220600463,-22.1738711152697,0.));
#225918=CARTESIAN_POINT('',(-4.11585220600463,-22.1738711152697,0.));
#225919=CARTESIAN_POINT('',(-1.96187429785751,-10.5694630535049,0.));
#225920=CARTESIAN_POINT('Ctrl Pts',(-0.661312440730913,-25.991588367311,
0.));
#225921=CARTESIAN_POINT('Ctrl Pts',(-0.661312440730913,-25.991588367311,
12.));
#225922=CARTESIAN_POINT('Ctrl Pts',(-0.664028313187638,-25.9865613464773,
0.));
#225923=CARTESIAN_POINT('Ctrl Pts',(-0.664028313187638,-25.9865613464773,
12.));
#225924=CARTESIAN_POINT('Ctrl Pts',(-0.669451306780837,-25.9765104298071,
0.));
#225925=CARTESIAN_POINT('Ctrl Pts',(-0.669451306780837,-25.9765104298071,
12.));
#225926=CARTESIAN_POINT('Ctrl Pts',(-0.677559543209739,-25.9614434297919,
0.));
#225927=CARTESIAN_POINT('Ctrl Pts',(-0.677559543209739,-25.9614434297919,
12.));
#225928=CARTESIAN_POINT('Ctrl Pts',(-0.688318015057743,-25.9413728471909,
0.));
#225929=CARTESIAN_POINT('Ctrl Pts',(-0.688318015057743,-25.9413728471909,
12.));
#225930=CARTESIAN_POINT('Ctrl Pts',(-0.701678575228768,-25.9163158909426,
0.));
#225931=CARTESIAN_POINT('Ctrl Pts',(-0.701678575228768,-25.9163158909426,
12.));
#225932=CARTESIAN_POINT('Ctrl Pts',(-0.714951588527651,-25.891290261497,
0.));
#225933=CARTESIAN_POINT('Ctrl Pts',(-0.714951588527651,-25.891290261497,
12.));
#225934=CARTESIAN_POINT('Ctrl Pts',(-0.728137036482348,-25.8662960624185,
0.));
#225935=CARTESIAN_POINT('Ctrl Pts',(-0.728137036482348,-25.8662960624185,
12.));
#225936=CARTESIAN_POINT('Ctrl Pts',(-0.741234902663818,-25.8413334619055,
0.));
#225937=CARTESIAN_POINT('Ctrl Pts',(-0.741234902663818,-25.8413334619055,
12.));
#225938=CARTESIAN_POINT('Ctrl Pts',(-0.754245175609535,-25.8164027059984,
0.));
#225939=CARTESIAN_POINT('Ctrl Pts',(-0.754245175609535,-25.8164027059984,
12.));
#225940=CARTESIAN_POINT('Ctrl Pts',(-0.76716785265118,-25.7915041383376,
0.));
#225941=CARTESIAN_POINT('Ctrl Pts',(-0.76716785265118,-25.7915041383376,
12.));
#225942=CARTESIAN_POINT('Ctrl Pts',(-0.780002940291976,-25.7666381946955,
0.));
#225943=CARTESIAN_POINT('Ctrl Pts',(-0.780002940291976,-25.7666381946955,
12.));
#225944=CARTESIAN_POINT('Ctrl Pts',(-0.792750451616139,-25.7418053757746,
0.));
#225945=CARTESIAN_POINT('Ctrl Pts',(-0.792750451616139,-25.7418053757746,
12.));
#225946=CARTESIAN_POINT('Ctrl Pts',(-0.805410404554365,-25.7170062262525,
0.));
#225947=CARTESIAN_POINT('Ctrl Pts',(-0.805410404554365,-25.7170062262525,
12.));
#225948=CARTESIAN_POINT('Ctrl Pts',(-0.817982819787476,-25.6922413110194,
0.));
#225949=CARTESIAN_POINT('Ctrl Pts',(-0.817982819787476,-25.6922413110194,
12.));
#225950=CARTESIAN_POINT('Ctrl Pts',(-0.830467718864218,-25.6675111931952,
0.));
#225951=CARTESIAN_POINT('Ctrl Pts',(-0.830467718864218,-25.6675111931952,
12.));
#225952=CARTESIAN_POINT('Ctrl Pts',(-0.842865122120771,-25.6428164100055,
0.));
#225953=CARTESIAN_POINT('Ctrl Pts',(-0.842865122120771,-25.6428164100055,
12.));
#225954=CARTESIAN_POINT('Ctrl Pts',(-0.85517504703656,-25.6181574536049,
0.));
#225955=CARTESIAN_POINT('Ctrl Pts',(-0.85517504703656,-25.6181574536049,
12.));
#225956=CARTESIAN_POINT('Ctrl Pts',(-0.867397509338443,-25.5935347843585,
0.));
#225957=CARTESIAN_POINT('Ctrl Pts',(-0.867397509338443,-25.5935347843585,
12.));
#225958=CARTESIAN_POINT('Ctrl Pts',(-0.879532523834307,-25.5689488408156,
0.));
#225959=CARTESIAN_POINT('Ctrl Pts',(-0.879532523834307,-25.5689488408156,
12.));
#225960=CARTESIAN_POINT('Ctrl Pts',(-0.891580105349052,-25.5444000508211,
0.));
#225961=CARTESIAN_POINT('Ctrl Pts',(-0.891580105349052,-25.5444000508211,
12.));
#225962=CARTESIAN_POINT('Ctrl Pts',(-0.903540269651119,-25.5198888424194,
0.));
#225963=CARTESIAN_POINT('Ctrl Pts',(-0.903540269651119,-25.5198888424194,
12.));
#225964=CARTESIAN_POINT('Ctrl Pts',(-0.915413034335626,-25.4954156541795,
0.));
#225965=CARTESIAN_POINT('Ctrl Pts',(-0.915413034335626,-25.4954156541795,
12.));
#225966=CARTESIAN_POINT('Ctrl Pts',(-0.927198419886107,-25.4709809475009,
0.));
#225967=CARTESIAN_POINT('Ctrl Pts',(-0.927198419886107,-25.4709809475009,
12.));
#225968=CARTESIAN_POINT('Ctrl Pts',(-0.938896449496205,-25.4465852044849,
0.));
#225969=CARTESIAN_POINT('Ctrl Pts',(-0.938896449496205,-25.4465852044849,
12.));
#225970=CARTESIAN_POINT('Ctrl Pts',(-0.950507148597481,-25.4222289223167,
0.));
#225971=CARTESIAN_POINT('Ctrl Pts',(-0.950507148597481,-25.4222289223167,
12.));
#225972=CARTESIAN_POINT('Ctrl Pts',(-0.962030544503155,-25.3979126089163,
0.));
#225973=CARTESIAN_POINT('Ctrl Pts',(-0.962030544503155,-25.3979126089163,
12.));
#225974=CARTESIAN_POINT('Ctrl Pts',(-0.973466666000176,-25.3736367778845,
0.));
#225975=CARTESIAN_POINT('Ctrl Pts',(-0.973466666000176,-25.3736367778845,
12.));
#225976=CARTESIAN_POINT('Ctrl Pts',(-0.984815543003984,-25.3494019441441,
0.));
#225977=CARTESIAN_POINT('Ctrl Pts',(-0.984815543003984,-25.3494019441441,
12.));
#225978=CARTESIAN_POINT('Ctrl Pts',(-0.996077206120636,-25.3252086182968,
0.));
#225979=CARTESIAN_POINT('Ctrl Pts',(-0.996077206120636,-25.3252086182968,
12.));
#225980=CARTESIAN_POINT('Ctrl Pts',(-1.00725168656897,-25.3010573055548,
0.));
#225981=CARTESIAN_POINT('Ctrl Pts',(-1.00725168656897,-25.3010573055548,
12.));
#225982=CARTESIAN_POINT('Ctrl Pts',(-1.01833901642238,-25.276948508726,
0.));
#225983=CARTESIAN_POINT('Ctrl Pts',(-1.01833901642238,-25.276948508726,
12.));
#225984=CARTESIAN_POINT('Ctrl Pts',(-1.02933922876807,-25.2528827300422,
0.));
#225985=CARTESIAN_POINT('Ctrl Pts',(-1.02933922876807,-25.2528827300422,
12.));
#225986=CARTESIAN_POINT('Ctrl Pts',(-1.04025235791508,-25.2288604735086,
0.));
#225987=CARTESIAN_POINT('Ctrl Pts',(-1.04025235791508,-25.2288604735086,
12.));
#225988=CARTESIAN_POINT('Ctrl Pts',(-1.05107843957933,-25.2048822469028,
0.));
#225989=CARTESIAN_POINT('Ctrl Pts',(-1.05107843957933,-25.2048822469028,
12.));
#225990=CARTESIAN_POINT('Ctrl Pts',(-1.06181751111769,-25.1809485642192,
0.));
#225991=CARTESIAN_POINT('Ctrl Pts',(-1.06181751111769,-25.1809485642192,
12.));
#225992=CARTESIAN_POINT('Ctrl Pts',(-1.07246961165477,-25.157059946931,
0.));
#225993=CARTESIAN_POINT('Ctrl Pts',(-1.07246961165477,-25.157059946931,
12.));
#225994=CARTESIAN_POINT('Ctrl Pts',(-1.08303478197189,-25.1332169227413,
0.));
#225995=CARTESIAN_POINT('Ctrl Pts',(-1.08303478197189,-25.1332169227413,
12.));
#225996=CARTESIAN_POINT('Ctrl Pts',(-1.09351306445309,-25.1094200248446,
0.));
#225997=CARTESIAN_POINT('Ctrl Pts',(-1.09351306445309,-25.1094200248446,
12.));
#225998=CARTESIAN_POINT('Ctrl Pts',(-1.10390450301746,-25.0856697909679,
0.));
#225999=CARTESIAN_POINT('Ctrl Pts',(-1.10390450301746,-25.0856697909679,
12.));
#226000=CARTESIAN_POINT('Ctrl Pts',(-1.1142091430689,-25.0619667625336,
0.));
#226001=CARTESIAN_POINT('Ctrl Pts',(-1.1142091430689,-25.0619667625336,
12.));
#226002=CARTESIAN_POINT('Ctrl Pts',(-1.12442703144453,-25.0383114836899,
0.));
#226003=CARTESIAN_POINT('Ctrl Pts',(-1.12442703144453,-25.0383114836899,
12.));
#226004=CARTESIAN_POINT('Ctrl Pts',(-1.13455821638531,-25.0147045006196,
0.));
#226005=CARTESIAN_POINT('Ctrl Pts',(-1.13455821638531,-25.0147045006196,
12.));
#226006=CARTESIAN_POINT('Ctrl Pts',(-1.14460274758202,-24.9911463621433,
0.));
#226007=CARTESIAN_POINT('Ctrl Pts',(-1.14460274758202,-24.9911463621433,
12.));
#226008=CARTESIAN_POINT('Ctrl Pts',(-1.1545606762189,-24.9676376201502,
0.));
#226009=CARTESIAN_POINT('Ctrl Pts',(-1.1545606762189,-24.9676376201502,
12.));
#226010=CARTESIAN_POINT('Ctrl Pts',(-1.16443205502851,-24.9441788300932,
0.));
#226011=CARTESIAN_POINT('Ctrl Pts',(-1.16443205502851,-24.9441788300932,
12.));
#226012=CARTESIAN_POINT('Ctrl Pts',(-1.17421693835042,-24.9207705514448,
0.));
#226013=CARTESIAN_POINT('Ctrl Pts',(-1.17421693835042,-24.9207705514448,
12.));
#226014=CARTESIAN_POINT('Ctrl Pts',(-1.18391538220104,-24.8974133481829,
0.));
#226015=CARTESIAN_POINT('Ctrl Pts',(-1.18391538220104,-24.8974133481829,
12.));
#226016=CARTESIAN_POINT('Ctrl Pts',(-1.19352744434065,-24.8741077892075,
0.));
#226017=CARTESIAN_POINT('Ctrl Pts',(-1.19352744434065,-24.8741077892075,
12.));
#226018=CARTESIAN_POINT('Ctrl Pts',(-1.20305318426021,-24.8508544481974,
0.));
#226019=CARTESIAN_POINT('Ctrl Pts',(-1.20305318426021,-24.8508544481974,
12.));
#226020=CARTESIAN_POINT('Ctrl Pts',(-1.21249266318209,-24.8276539035092,
0.));
#226021=CARTESIAN_POINT('Ctrl Pts',(-1.21249266318209,-24.8276539035092,
12.));
#226022=CARTESIAN_POINT('Ctrl Pts',(-1.22184594406529,-24.8045067380536,
0.));
#226023=CARTESIAN_POINT('Ctrl Pts',(-1.22184594406529,-24.8045067380536,
12.));
#226024=CARTESIAN_POINT('Ctrl Pts',(-1.23111309161845,-24.7814135391799,
0.));
#226025=CARTESIAN_POINT('Ctrl Pts',(-1.23111309161845,-24.7814135391799,
12.));
#226026=CARTESIAN_POINT('Ctrl Pts',(-1.2402941723199,-24.7583748985438,
0.));
#226027=CARTESIAN_POINT('Ctrl Pts',(-1.2402941723199,-24.7583748985438,
12.));
#226028=CARTESIAN_POINT('Ctrl Pts',(-1.24938925444327,-24.7353914120011,
0.));
#226029=CARTESIAN_POINT('Ctrl Pts',(-1.24938925444327,-24.7353914120011,
12.));
#226030=CARTESIAN_POINT('Ctrl Pts',(-1.25839840807419,-24.7124636797894,
0.));
#226031=CARTESIAN_POINT('Ctrl Pts',(-1.25839840807419,-24.7124636797894,
12.));
#226032=CARTESIAN_POINT('Ctrl Pts',(-1.26732170513501,-24.6895923066836,
0.));
#226033=CARTESIAN_POINT('Ctrl Pts',(-1.26732170513501,-24.6895923066836,
12.));
#226034=CARTESIAN_POINT('Ctrl Pts',(-1.27615921941643,-24.6667779021559,
0.));
#226035=CARTESIAN_POINT('Ctrl Pts',(-1.27615921941643,-24.6667779021559,
12.));
#226036=CARTESIAN_POINT('Ctrl Pts',(-1.28491102661515,-24.6440210805278,
0.));
#226037=CARTESIAN_POINT('Ctrl Pts',(-1.28491102661515,-24.6440210805278,
12.));
#226038=CARTESIAN_POINT('Ctrl Pts',(-1.29357720438108,-24.6213224611229,
0.));
#226039=CARTESIAN_POINT('Ctrl Pts',(-1.29357720438108,-24.6213224611229,
12.));
#226040=CARTESIAN_POINT('Ctrl Pts',(-1.30215783236363,-24.5986826684027,
0.));
#226041=CARTESIAN_POINT('Ctrl Pts',(-1.30215783236363,-24.5986826684027,
12.));
#226042=CARTESIAN_POINT('Ctrl Pts',(-1.31065299222023,-24.5761023320183,
0.));
#226043=CARTESIAN_POINT('Ctrl Pts',(-1.31065299222023,-24.5761023320183,
12.));
#226044=CARTESIAN_POINT('Ctrl Pts',(-1.31906276763669,-24.5535820868674,
0.));
#226045=CARTESIAN_POINT('Ctrl Pts',(-1.31906276763669,-24.5535820868674,
12.));
#226046=CARTESIAN_POINT('Ctrl Pts',(-1.32738724435327,-24.5311225731435,
0.));
#226047=CARTESIAN_POINT('Ctrl Pts',(-1.32738724435327,-24.5311225731435,
12.));
#226048=CARTESIAN_POINT('Ctrl Pts',(-1.33562651019687,-24.5087244363856,
0.));
#226049=CARTESIAN_POINT('Ctrl Pts',(-1.33562651019687,-24.5087244363856,
12.));
#226050=CARTESIAN_POINT('Ctrl Pts',(-1.34378065512339,-24.4863883275134,
0.));
#226051=CARTESIAN_POINT('Ctrl Pts',(-1.34378065512339,-24.4863883275134,
12.));
#226052=CARTESIAN_POINT('Ctrl Pts',(-1.35184977125649,-24.4641149028892,
0.));
#226053=CARTESIAN_POINT('Ctrl Pts',(-1.35184977125649,-24.4641149028892,
12.));
#226054=CARTESIAN_POINT('Ctrl Pts',(-1.35983395290628,-24.4419048244523,
0.));
#226055=CARTESIAN_POINT('Ctrl Pts',(-1.35983395290628,-24.4419048244523,
12.));
#226056=CARTESIAN_POINT('Ctrl Pts',(-1.36773329659957,-24.4197587598337,
0.));
#226057=CARTESIAN_POINT('Ctrl Pts',(-1.36773329659957,-24.4197587598337,
12.));
#226058=CARTESIAN_POINT('Ctrl Pts',(-1.3755479011161,-24.3976773824732,
0.));
#226059=CARTESIAN_POINT('Ctrl Pts',(-1.3755479011161,-24.3976773824732,
12.));
#226060=CARTESIAN_POINT('Ctrl Pts',(-1.38327786753,-24.3756613717299,0.));
#226061=CARTESIAN_POINT('Ctrl Pts',(-1.38327786753,-24.3756613717299,12.));
#226062=CARTESIAN_POINT('Ctrl Pts',(-1.39092329926389,-24.3537114129875,
0.));
#226063=CARTESIAN_POINT('Ctrl Pts',(-1.39092329926389,-24.3537114129875,
12.));
#226064=CARTESIAN_POINT('Ctrl Pts',(-1.39848430212808,-24.3318281977643,
0.));
#226065=CARTESIAN_POINT('Ctrl Pts',(-1.39848430212808,-24.3318281977643,
12.));
#226066=CARTESIAN_POINT('Ctrl Pts',(-1.40596098434338,-24.3100124238311,
0.));
#226067=CARTESIAN_POINT('Ctrl Pts',(-1.40596098434338,-24.3100124238311,
12.));
#226068=CARTESIAN_POINT('Ctrl Pts',(-1.41335345657684,-24.288264795321,
0.));
#226069=CARTESIAN_POINT('Ctrl Pts',(-1.41335345657684,-24.288264795321,
12.));
#226070=CARTESIAN_POINT('Ctrl Pts',(-1.42066183198254,-24.2665860228356,
0.));
#226071=CARTESIAN_POINT('Ctrl Pts',(-1.42066183198254,-24.2665860228356,
12.));
#226072=CARTESIAN_POINT('Ctrl Pts',(-1.42788622624855,-24.2449768235488,
0.));
#226073=CARTESIAN_POINT('Ctrl Pts',(-1.42788622624855,-24.2449768235488,
12.));
#226074=CARTESIAN_POINT('Ctrl Pts',(-1.43502675765509,-24.2234379212984,
0.));
#226075=CARTESIAN_POINT('Ctrl Pts',(-1.43502675765509,-24.2234379212984,
12.));
#226076=CARTESIAN_POINT('Ctrl Pts',(-1.44208354711083,-24.201970046722,
0.));
#226077=CARTESIAN_POINT('Ctrl Pts',(-1.44208354711083,-24.201970046722,
12.));
#226078=CARTESIAN_POINT('Ctrl Pts',(-1.44905671818729,-24.1805739374038,
0.));
#226079=CARTESIAN_POINT('Ctrl Pts',(-1.44905671818729,-24.1805739374038,
12.));
#226080=CARTESIAN_POINT('Ctrl Pts',(-1.45594639716319,-24.1592503380107,
0.));
#226081=CARTESIAN_POINT('Ctrl Pts',(-1.45594639716319,-24.1592503380107,
12.));
#226082=CARTESIAN_POINT('Ctrl Pts',(-1.46275271307399,-24.1380000004272,
0.));
#226083=CARTESIAN_POINT('Ctrl Pts',(-1.46275271307399,-24.1380000004272,
12.));
#226084=CARTESIAN_POINT('Ctrl Pts',(-1.46947579776992,-24.1168236838824,
0.));
#226085=CARTESIAN_POINT('Ctrl Pts',(-1.46947579776992,-24.1168236838824,
12.));
#226086=CARTESIAN_POINT('Ctrl Pts',(-1.47611578597743,-24.0957221550778,
0.));
#226087=CARTESIAN_POINT('Ctrl Pts',(-1.47611578597743,-24.0957221550778,
12.));
#226088=CARTESIAN_POINT('Ctrl Pts',(-1.48267281533684,-24.0746961883528,
0.));
#226089=CARTESIAN_POINT('Ctrl Pts',(-1.48267281533684,-24.0746961883528,
12.));
#226090=CARTESIAN_POINT('Ctrl Pts',(-1.48914702644888,-24.0537465658429,
0.));
#226091=CARTESIAN_POINT('Ctrl Pts',(-1.48914702644888,-24.0537465658429,
12.));
#226092=CARTESIAN_POINT('Ctrl Pts',(-1.49553856292802,-24.0328740776331,
0.));
#226093=CARTESIAN_POINT('Ctrl Pts',(-1.49553856292802,-24.0328740776331,
12.));
#226094=CARTESIAN_POINT('Ctrl Pts',(-1.501847571461,-24.0120795219086,0.));
#226095=CARTESIAN_POINT('Ctrl Pts',(-1.501847571461,-24.0120795219086,12.));
#226096=CARTESIAN_POINT('Ctrl Pts',(-1.50807420187695,-23.9913637050927,
0.));
#226097=CARTESIAN_POINT('Ctrl Pts',(-1.50807420187695,-23.9913637050927,
12.));
#226098=CARTESIAN_POINT('Ctrl Pts',(-1.51421860720615,-23.970727442014,
0.));
#226099=CARTESIAN_POINT('Ctrl Pts',(-1.51421860720615,-23.970727442014,
12.));
#226100=CARTESIAN_POINT('Ctrl Pts',(-1.52028094372793,-23.9501715561033,
0.));
#226101=CARTESIAN_POINT('Ctrl Pts',(-1.52028094372793,-23.9501715561033,
12.));
#226102=CARTESIAN_POINT('Ctrl Pts',(-1.52626137103033,-23.9296968795757,
0.));
#226103=CARTESIAN_POINT('Ctrl Pts',(-1.52626137103033,-23.9296968795757,
12.));
#226104=CARTESIAN_POINT('Ctrl Pts',(-1.53216005207464,-23.9093042536119,
0.));
#226105=CARTESIAN_POINT('Ctrl Pts',(-1.53216005207464,-23.9093042536119,
12.));
#226106=CARTESIAN_POINT('Ctrl Pts',(-1.53797715326759,-23.8889945285318,
0.));
#226107=CARTESIAN_POINT('Ctrl Pts',(-1.53797715326759,-23.8889945285318,
12.));
#226108=CARTESIAN_POINT('Ctrl Pts',(-1.54371284453991,-23.8687685639642,
0.));
#226109=CARTESIAN_POINT('Ctrl Pts',(-1.54371284453991,-23.8687685639642,
12.));
#226110=CARTESIAN_POINT('Ctrl Pts',(-1.54936729940542,-23.8486272290705,
0.));
#226111=CARTESIAN_POINT('Ctrl Pts',(-1.54936729940542,-23.8486272290705,
12.));
#226112=CARTESIAN_POINT('Ctrl Pts',(-1.55494069502636,-23.8285714027636,
0.));
#226113=CARTESIAN_POINT('Ctrl Pts',(-1.55494069502636,-23.8285714027636,
12.));
#226114=CARTESIAN_POINT('Ctrl Pts',(-1.56043321228635,-23.8086019739194,
0.));
#226115=CARTESIAN_POINT('Ctrl Pts',(-1.56043321228635,-23.8086019739194,
12.));
#226116=CARTESIAN_POINT('Ctrl Pts',(-1.56584503586844,-23.7887198415878,
0.));
#226117=CARTESIAN_POINT('Ctrl Pts',(-1.56584503586844,-23.7887198415878,
12.));
#226118=CARTESIAN_POINT('Ctrl Pts',(-1.57117635434409,-23.7689259151862,
0.));
#226119=CARTESIAN_POINT('Ctrl Pts',(-1.57117635434409,-23.7689259151862,
12.));
#226120=CARTESIAN_POINT('Ctrl Pts',(-1.57642736025247,-23.749221114736,
0.));
#226121=CARTESIAN_POINT('Ctrl Pts',(-1.57642736025247,-23.749221114736,
12.));
#226122=CARTESIAN_POINT('Ctrl Pts',(-1.58159825017359,-23.72960637113,0.));
#226123=CARTESIAN_POINT('Ctrl Pts',(-1.58159825017359,-23.72960637113,12.));
#226124=CARTESIAN_POINT('Ctrl Pts',(-1.58668922481222,-23.710082626383,
0.));
#226125=CARTESIAN_POINT('Ctrl Pts',(-1.58668922481222,-23.710082626383,
12.));
#226126=CARTESIAN_POINT('Ctrl Pts',(-1.59170048908634,-23.6906508338833,
0.));
#226127=CARTESIAN_POINT('Ctrl Pts',(-1.59170048908634,-23.6906508338833,
12.));
#226128=CARTESIAN_POINT('Ctrl Pts',(-1.59663225222464,-23.671311958631,
0.));
#226129=CARTESIAN_POINT('Ctrl Pts',(-1.59663225222464,-23.671311958631,
12.));
#226130=CARTESIAN_POINT('Ctrl Pts',(-1.60148472786596,-23.6520669774876,
0.));
#226131=CARTESIAN_POINT('Ctrl Pts',(-1.60148472786596,-23.6520669774876,
12.));
#226132=CARTESIAN_POINT('Ctrl Pts',(-1.60625813414674,-23.6329168794929,
0.));
#226133=CARTESIAN_POINT('Ctrl Pts',(-1.60625813414674,-23.6329168794929,
12.));
#226134=CARTESIAN_POINT('Ctrl Pts',(-1.61095269379779,-23.6138626661653,
0.));
#226135=CARTESIAN_POINT('Ctrl Pts',(-1.61095269379779,-23.6138626661653,
12.));
#226136=CARTESIAN_POINT('Ctrl Pts',(-1.61556863424699,-23.5949053517997,
0.));
#226137=CARTESIAN_POINT('Ctrl Pts',(-1.61556863424699,-23.5949053517997,
12.));
#226138=CARTESIAN_POINT('Ctrl Pts',(-1.62010618772867,-23.57604596376,0.));
#226139=CARTESIAN_POINT('Ctrl Pts',(-1.62010618772867,-23.57604596376,12.));
#226140=CARTESIAN_POINT('Ctrl Pts',(-1.62456559140065,-23.5572855427601,
0.));
#226141=CARTESIAN_POINT('Ctrl Pts',(-1.62456559140065,-23.5572855427601,
12.));
#226142=CARTESIAN_POINT('Ctrl Pts',(-1.62894708745224,-23.538625143226,
0.));
#226143=CARTESIAN_POINT('Ctrl Pts',(-1.62894708745224,-23.538625143226,
12.));
#226144=CARTESIAN_POINT('Ctrl Pts',(-1.63325092321727,-23.5200658336612,
0.));
#226145=CARTESIAN_POINT('Ctrl Pts',(-1.63325092321727,-23.5200658336612,
12.));
#226146=CARTESIAN_POINT('Ctrl Pts',(-1.63747735129475,-23.5016086970003,
0.));
#226147=CARTESIAN_POINT('Ctrl Pts',(-1.63747735129475,-23.5016086970003,
12.));
#226148=CARTESIAN_POINT('Ctrl Pts',(-1.64162662967529,-23.4832548309645,
0.));
#226149=CARTESIAN_POINT('Ctrl Pts',(-1.64162662967529,-23.4832548309645,
12.));
#226150=CARTESIAN_POINT('Ctrl Pts',(-1.64569902187612,-23.4650053483932,
0.));
#226151=CARTESIAN_POINT('Ctrl Pts',(-1.64569902187612,-23.4650053483932,
12.));
#226152=CARTESIAN_POINT('Ctrl Pts',(-1.64969479707341,-23.4468613776574,
0.));
#226153=CARTESIAN_POINT('Ctrl Pts',(-1.64969479707341,-23.4468613776574,
12.));
#226154=CARTESIAN_POINT('Ctrl Pts',(-1.65361423023729,-23.4288240631043,
0.));
#226155=CARTESIAN_POINT('Ctrl Pts',(-1.65361423023729,-23.4288240631043,
12.));
#226156=CARTESIAN_POINT('Ctrl Pts',(-1.65745760227506,-23.4108945654805,
0.));
#226157=CARTESIAN_POINT('Ctrl Pts',(-1.65745760227506,-23.4108945654805,
12.));
#226158=CARTESIAN_POINT('Ctrl Pts',(-1.66122520018012,-23.3930740623619,
0.));
#226159=CARTESIAN_POINT('Ctrl Pts',(-1.66122520018012,-23.3930740623619,
12.));
#226160=CARTESIAN_POINT('Ctrl Pts',(-1.66491731718878,-23.3753637485545,
0.));
#226161=CARTESIAN_POINT('Ctrl Pts',(-1.66491731718878,-23.3753637485545,
12.));
#226162=CARTESIAN_POINT('Ctrl Pts',(-1.66853425293997,-23.3577648365744,
0.));
#226163=CARTESIAN_POINT('Ctrl Pts',(-1.66853425293997,-23.3577648365744,
12.));
#226164=CARTESIAN_POINT('Ctrl Pts',(-1.67207631363923,-23.3402785571865,
0.));
#226165=CARTESIAN_POINT('Ctrl Pts',(-1.67207631363923,-23.3402785571865,
12.));
#226166=CARTESIAN_POINT('Ctrl Pts',(-1.67554381222995,-23.3229061599145,
0.));
#226167=CARTESIAN_POINT('Ctrl Pts',(-1.67554381222995,-23.3229061599145,
12.));
#226168=CARTESIAN_POINT('Ctrl Pts',(-1.67893706857118,-23.3056489135611,
0.));
#226169=CARTESIAN_POINT('Ctrl Pts',(-1.67893706857118,-23.3056489135611,
12.));
#226170=CARTESIAN_POINT('Ctrl Pts',(-1.68225640962169,-23.2885081066951,
0.));
#226171=CARTESIAN_POINT('Ctrl Pts',(-1.68225640962169,-23.2885081066951,
12.));
#226172=CARTESIAN_POINT('Ctrl Pts',(-1.68550216963259,-23.2714850482246,
0.));
#226173=CARTESIAN_POINT('Ctrl Pts',(-1.68550216963259,-23.2714850482246,
12.));
#226174=CARTESIAN_POINT('Ctrl Pts',(-1.68867469034897,-23.2545810680537,
0.));
#226175=CARTESIAN_POINT('Ctrl Pts',(-1.68867469034897,-23.2545810680537,
12.));
#226176=CARTESIAN_POINT('Ctrl Pts',(-1.69177432121712,-23.2377975177013,
0.));
#226177=CARTESIAN_POINT('Ctrl Pts',(-1.69177432121712,-23.2377975177013,
12.));
#226178=CARTESIAN_POINT('Ctrl Pts',(-1.69480141959954,-23.2211357709374,
0.));
#226179=CARTESIAN_POINT('Ctrl Pts',(-1.69480141959954,-23.2211357709374,
12.));
#226180=CARTESIAN_POINT('Ctrl Pts',(-1.69775635099444,-23.2045972243767,
0.));
#226181=CARTESIAN_POINT('Ctrl Pts',(-1.69775635099444,-23.2045972243767,
12.));
#226182=CARTESIAN_POINT('Ctrl Pts',(-1.70063948927011,-23.1881832981851,
0.));
#226183=CARTESIAN_POINT('Ctrl Pts',(-1.70063948927011,-23.1881832981851,
12.));
#226184=CARTESIAN_POINT('Ctrl Pts',(-1.70345121691277,-23.1718954368751,
0.));
#226185=CARTESIAN_POINT('Ctrl Pts',(-1.70345121691277,-23.1718954368751,
12.));
#226186=CARTESIAN_POINT('Ctrl Pts',(-1.70619192527853,-23.1557351100614,
0.));
#226187=CARTESIAN_POINT('Ctrl Pts',(-1.70619192527853,-23.1557351100614,
12.));
#226188=CARTESIAN_POINT('Ctrl Pts',(-1.70886201485453,-23.1397038132356,
0.));
#226189=CARTESIAN_POINT('Ctrl Pts',(-1.70886201485453,-23.1397038132356,
12.));
#226190=CARTESIAN_POINT('Ctrl Pts',(-1.71146189552175,-23.1238030684925,
0.));
#226191=CARTESIAN_POINT('Ctrl Pts',(-1.71146189552175,-23.1238030684925,
12.));
#226192=CARTESIAN_POINT('Ctrl Pts',(-1.71399198684705,-23.1080344254286,
0.));
#226193=CARTESIAN_POINT('Ctrl Pts',(-1.71399198684705,-23.1080344254286,
12.));
#226194=CARTESIAN_POINT('Ctrl Pts',(-1.71645271839298,-23.0923994621213,
0.));
#226195=CARTESIAN_POINT('Ctrl Pts',(-1.71645271839298,-23.0923994621213,
12.));
#226196=CARTESIAN_POINT('Ctrl Pts',(-1.71884453003028,-23.0768997860709,
0.));
#226197=CARTESIAN_POINT('Ctrl Pts',(-1.71884453003028,-23.0768997860709,
12.));
#226198=CARTESIAN_POINT('Ctrl Pts',(-1.72116787225993,-23.0615370351562,
0.));
#226199=CARTESIAN_POINT('Ctrl Pts',(-1.72116787225993,-23.0615370351562,
12.));
#226200=CARTESIAN_POINT('Ctrl Pts',(-1.72342320653748,-23.0463128785531,
0.));
#226201=CARTESIAN_POINT('Ctrl Pts',(-1.72342320653748,-23.0463128785531,
12.));
#226202=CARTESIAN_POINT('Ctrl Pts',(-1.72561100564047,-23.0312290178883,
0.));
#226203=CARTESIAN_POINT('Ctrl Pts',(-1.72561100564047,-23.0312290178883,
12.));
#226204=CARTESIAN_POINT('Ctrl Pts',(-1.7277317540471,-23.0162871884168,
0.));
#226205=CARTESIAN_POINT('Ctrl Pts',(-1.7277317540471,-23.0162871884168,
12.));
#226206=CARTESIAN_POINT('Ctrl Pts',(-1.72978594832137,-23.001489160189,
0.));
#226207=CARTESIAN_POINT('Ctrl Pts',(-1.72978594832137,-23.001489160189,
12.));
#226208=CARTESIAN_POINT('Ctrl Pts',(-1.73177409750192,-22.9868367391978,
0.));
#226209=CARTESIAN_POINT('Ctrl Pts',(-1.73177409750192,-22.9868367391978,
12.));
#226210=CARTESIAN_POINT('Ctrl Pts',(-1.73369672350816,-22.9723317685688,
0.));
#226211=CARTESIAN_POINT('Ctrl Pts',(-1.73369672350816,-22.9723317685688,
12.));
#226212=CARTESIAN_POINT('Ctrl Pts',(-1.7355543616277,-22.9579761301063,
0.));
#226213=CARTESIAN_POINT('Ctrl Pts',(-1.7355543616277,-22.9579761301063,
12.));
#226214=CARTESIAN_POINT('Ctrl Pts',(-1.7373475610004,-22.9437717457826,
0.));
#226215=CARTESIAN_POINT('Ctrl Pts',(-1.7373475610004,-22.9437717457826,
12.));
#226216=CARTESIAN_POINT('Ctrl Pts',(-1.73907688511667,-22.9297205792586,
0.));
#226217=CARTESIAN_POINT('Ctrl Pts',(-1.73907688511667,-22.9297205792586,
12.));
#226218=CARTESIAN_POINT('Ctrl Pts',(-1.74074291231059,-22.9158246373363,
0.));
#226219=CARTESIAN_POINT('Ctrl Pts',(-1.74074291231059,-22.9158246373363,
12.));
#226220=CARTESIAN_POINT('Ctrl Pts',(-1.74234623630081,-22.9020859716141,
0.));
#226221=CARTESIAN_POINT('Ctrl Pts',(-1.74234623630081,-22.9020859716141,
12.));
#226222=CARTESIAN_POINT('Ctrl Pts',(-1.74388746677703,-22.888506680335,
0.));
#226223=CARTESIAN_POINT('Ctrl Pts',(-1.74388746677703,-22.888506680335,
12.));
#226224=CARTESIAN_POINT('Ctrl Pts',(-1.74536722998202,-22.8750889101696,
0.));
#226225=CARTESIAN_POINT('Ctrl Pts',(-1.74536722998202,-22.8750889101696,
12.));
#226226=CARTESIAN_POINT('Ctrl Pts',(-1.74678616930666,-22.8618348580235,
0.));
#226227=CARTESIAN_POINT('Ctrl Pts',(-1.74678616930666,-22.8618348580235,
12.));
#226228=CARTESIAN_POINT('Ctrl Pts',(-1.74814494588494,-22.8487467728076,
0.));
#226229=CARTESIAN_POINT('Ctrl Pts',(-1.74814494588494,-22.8487467728076,
12.));
#226230=CARTESIAN_POINT('Ctrl Pts',(-1.74944423940117,-22.8358269579853,
0.));
#226231=CARTESIAN_POINT('Ctrl Pts',(-1.74944423940117,-22.8358269579853,
12.));
#226232=CARTESIAN_POINT('Ctrl Pts',(-1.75068474890884,-22.8230777741284,
0.));
#226233=CARTESIAN_POINT('Ctrl Pts',(-1.75068474890884,-22.8230777741284,
12.));
#226234=CARTESIAN_POINT('Ctrl Pts',(-1.75186719365593,-22.8105016414713,
0.));
#226235=CARTESIAN_POINT('Ctrl Pts',(-1.75186719365593,-22.8105016414713,
12.));
#226236=CARTESIAN_POINT('Ctrl Pts',(-1.75299231391467,-22.7981010424314,
0.));
#226237=CARTESIAN_POINT('Ctrl Pts',(-1.75299231391467,-22.7981010424314,
12.));
#226238=CARTESIAN_POINT('Ctrl Pts',(-1.75406087182937,-22.7858785242361,
0.));
#226239=CARTESIAN_POINT('Ctrl Pts',(-1.75406087182937,-22.7858785242361,
12.));
#226240=CARTESIAN_POINT('Ctrl Pts',(-1.75507365227133,-22.7738367016118,
0.));
#226241=CARTESIAN_POINT('Ctrl Pts',(-1.75507365227133,-22.7738367016118,
12.));
#226242=CARTESIAN_POINT('Ctrl Pts',(-1.75603146371642,-22.7619782595013,
0.));
#226243=CARTESIAN_POINT('Ctrl Pts',(-1.75603146371642,-22.7619782595013,
12.));
#226244=CARTESIAN_POINT('Ctrl Pts',(-1.75693513908908,-22.750305955645,
0.));
#226245=CARTESIAN_POINT('Ctrl Pts',(-1.75693513908908,-22.750305955645,
12.));
#226246=CARTESIAN_POINT('Ctrl Pts',(-1.75778553673245,-22.7388226235559,
0.));
#226247=CARTESIAN_POINT('Ctrl Pts',(-1.75778553673245,-22.7388226235559,
12.));
#226248=CARTESIAN_POINT('Ctrl Pts',(-1.75858354204634,-22.72753117773,0.));
#226249=CARTESIAN_POINT('Ctrl Pts',(-1.75858354204634,-22.72753117773,12.));
#226250=CARTESIAN_POINT('Ctrl Pts',(-1.75933006905926,-22.7164346186006,
0.));
#226251=CARTESIAN_POINT('Ctrl Pts',(-1.75933006905926,-22.7164346186006,
12.));
#226252=CARTESIAN_POINT('Ctrl Pts',(-1.76002606202402,-22.7055360375485,
0.));
#226253=CARTESIAN_POINT('Ctrl Pts',(-1.76002606202402,-22.7055360375485,
12.));
#226254=CARTESIAN_POINT('Ctrl Pts',(-1.76067249704888,-22.6948386219851,
0.));
#226255=CARTESIAN_POINT('Ctrl Pts',(-1.76067249704888,-22.6948386219851,
12.));
#226256=CARTESIAN_POINT('Ctrl Pts',(-1.76127038310615,-22.684345658525,
0.));
#226257=CARTESIAN_POINT('Ctrl Pts',(-1.76127038310615,-22.684345658525,
12.));
#226258=CARTESIAN_POINT('Ctrl Pts',(-1.76182076289527,-22.67406053567,0.));
#226259=CARTESIAN_POINT('Ctrl Pts',(-1.76182076289527,-22.67406053567,12.));
#226260=CARTESIAN_POINT('Ctrl Pts',(-1.7623247139257,-22.6639867471753,
0.));
#226261=CARTESIAN_POINT('Ctrl Pts',(-1.7623247139257,-22.6639867471753,
12.));
#226262=CARTESIAN_POINT('Ctrl Pts',(-1.76278334912562,-22.654127893841,
0.));
#226263=CARTESIAN_POINT('Ctrl Pts',(-1.76278334912562,-22.654127893841,
12.));
#226264=CARTESIAN_POINT('Ctrl Pts',(-1.76319782013917,-22.6444876940423,
0.));
#226265=CARTESIAN_POINT('Ctrl Pts',(-1.76319782013917,-22.6444876940423,
12.));
#226266=CARTESIAN_POINT('Ctrl Pts',(-1.76356932176274,-22.6350699979359,
0.));
#226267=CARTESIAN_POINT('Ctrl Pts',(-1.76356932176274,-22.6350699979359,
12.));
#226268=CARTESIAN_POINT('Ctrl Pts',(-1.76389909571404,-22.6258787994848,
0.));
#226269=CARTESIAN_POINT('Ctrl Pts',(-1.76389909571404,-22.6258787994848,
12.));
#226270=CARTESIAN_POINT('Ctrl Pts',(-1.7641884354374,-22.6169182517694,
0.));
#226271=CARTESIAN_POINT('Ctrl Pts',(-1.7641884354374,-22.6169182517694,
12.));
#226272=CARTESIAN_POINT('Ctrl Pts',(-1.76443868648017,-22.6081926681343,
0.));
#226273=CARTESIAN_POINT('Ctrl Pts',(-1.76443868648017,-22.6081926681343,
12.));
#226274=CARTESIAN_POINT('Ctrl Pts',(-1.76465124413558,-22.5997065145638,
0.));
#226275=CARTESIAN_POINT('Ctrl Pts',(-1.76465124413558,-22.5997065145638,
12.));
#226276=CARTESIAN_POINT('Ctrl Pts',(-1.76482755288412,-22.5914644078106,
0.));
#226277=CARTESIAN_POINT('Ctrl Pts',(-1.76482755288412,-22.5914644078106,
12.));
#226278=CARTESIAN_POINT('Ctrl Pts',(-1.76496910283089,-22.5834711038022,
0.));
#226279=CARTESIAN_POINT('Ctrl Pts',(-1.76496910283089,-22.5834711038022,
12.));
#226280=CARTESIAN_POINT('Ctrl Pts',(-1.76507744026747,-22.5757315316353,
0.));
#226281=CARTESIAN_POINT('Ctrl Pts',(-1.76507744026747,-22.5757315316353,
12.));
#226282=CARTESIAN_POINT('Ctrl Pts',(-1.76515418518832,-22.5682508499874,
0.));
#226283=CARTESIAN_POINT('Ctrl Pts',(-1.76515418518832,-22.5682508499874,
12.));
#226284=CARTESIAN_POINT('Ctrl Pts',(-1.76520104500451,-22.5610344912501,
0.));
#226285=CARTESIAN_POINT('Ctrl Pts',(-1.76520104500451,-22.5610344912501,
12.));
#226286=CARTESIAN_POINT('Ctrl Pts',(-1.76521983384063,-22.5540882235837,
0.));
#226287=CARTESIAN_POINT('Ctrl Pts',(-1.76521983384063,-22.5540882235837,
12.));
#226288=CARTESIAN_POINT('Ctrl Pts',(-1.76521245524048,-22.5474180954006,
0.));
#226289=CARTESIAN_POINT('Ctrl Pts',(-1.76521245524048,-22.5474180954006,
12.));
#226290=CARTESIAN_POINT('Ctrl Pts',(-1.76518087841494,-22.5410303590892,
0.));
#226291=CARTESIAN_POINT('Ctrl Pts',(-1.76518087841494,-22.5410303590892,
12.));
#226292=CARTESIAN_POINT('Ctrl Pts',(-1.76512711563255,-22.5349313983571,
0.));
#226293=CARTESIAN_POINT('Ctrl Pts',(-1.76512711563255,-22.5349313983571,
12.));
#226294=CARTESIAN_POINT('Ctrl Pts',(-1.7650532026276,-22.529127665298,0.));
#226295=CARTESIAN_POINT('Ctrl Pts',(-1.7650532026276,-22.529127665298,12.));
#226296=CARTESIAN_POINT('Ctrl Pts',(-1.76496128643376,-22.5236259635515,
0.));
#226297=CARTESIAN_POINT('Ctrl Pts',(-1.76496128643376,-22.5236259635515,
12.));
#226298=CARTESIAN_POINT('Ctrl Pts',(-1.76485369319896,-22.5184336670207,
0.));
#226299=CARTESIAN_POINT('Ctrl Pts',(-1.76485369319896,-22.5184336670207,
12.));
#226300=CARTESIAN_POINT('Ctrl Pts',(-1.7647330328115,-22.5135590569554,
0.));
#226301=CARTESIAN_POINT('Ctrl Pts',(-1.7647330328115,-22.5135590569554,
12.));
#226302=CARTESIAN_POINT('Ctrl Pts',(-1.76460218257314,-22.5090112700212,
0.));
#226303=CARTESIAN_POINT('Ctrl Pts',(-1.76460218257314,-22.5090112700212,
12.));
#226304=CARTESIAN_POINT('Ctrl Pts',(-1.76446408210366,-22.5047996391978,
0.));
#226305=CARTESIAN_POINT('Ctrl Pts',(-1.76446408210366,-22.5047996391978,
12.));
#226306=CARTESIAN_POINT('Ctrl Pts',(-1.76432160068739,-22.5009332677316,
0.));
#226307=CARTESIAN_POINT('Ctrl Pts',(-1.76432160068739,-22.5009332677316,
12.));
#226308=CARTESIAN_POINT('Ctrl Pts',(-1.76417731243484,-22.4974203063191,
0.));
#226309=CARTESIAN_POINT('Ctrl Pts',(-1.76417731243484,-22.4974203063191,
12.));
#226310=CARTESIAN_POINT('Ctrl Pts',(-1.76403393880317,-22.4942693792449,
0.));
#226311=CARTESIAN_POINT('Ctrl Pts',(-1.76403393880317,-22.4942693792449,
12.));
#226312=CARTESIAN_POINT('Ctrl Pts',(-1.76389475965715,-22.4914909094908,
0.));
#226313=CARTESIAN_POINT('Ctrl Pts',(-1.76389475965715,-22.4914909094908,
12.));
#226314=CARTESIAN_POINT('Ctrl Pts',(-1.76376424879469,-22.4890991659479,
0.));
#226315=CARTESIAN_POINT('Ctrl Pts',(-1.76376424879469,-22.4890991659479,
12.));
#226316=CARTESIAN_POINT('Ctrl Pts',(-1.76364784232926,-22.4871115206572,
0.));
#226317=CARTESIAN_POINT('Ctrl Pts',(-1.76364784232926,-22.4871115206572,
12.));
#226318=CARTESIAN_POINT('Ctrl Pts',(-1.7635507604555,-22.4855446605991,
0.));
#226319=CARTESIAN_POINT('Ctrl Pts',(-1.7635507604555,-22.4855446605991,
12.));
#226320=CARTESIAN_POINT('Ctrl Pts',(-1.76347698284863,-22.4844112933125,
0.));
#226321=CARTESIAN_POINT('Ctrl Pts',(-1.76347698284863,-22.4844112933125,
12.));
#226322=CARTESIAN_POINT('Ctrl Pts',(-1.7634381343466,-22.4838562517064,
0.));
#226323=CARTESIAN_POINT('Ctrl Pts',(-1.7634381343466,-22.4838562517064,
12.));
#226324=CARTESIAN_POINT('Ctrl Pts',(-1.76342064263638,-22.4836387052228,
0.));
#226325=CARTESIAN_POINT('Ctrl Pts',(-1.76342064263638,-22.4836387052228,
12.));
#226326=CARTESIAN_POINT('Ctrl Pts',(-1.76341415538792,-22.4835819929788,
0.));
#226327=CARTESIAN_POINT('Ctrl Pts',(-1.76341415538792,-22.4835819929788,
12.));
#226328=CARTESIAN_POINT('Ctrl Pts',(-1.76341220531181,-22.4835757167854,
0.));
#226329=CARTESIAN_POINT('Ctrl Pts',(-1.76341220531181,-22.4835757167854,
12.));
#226330=CARTESIAN_POINT('',(-0.661312440730913,-25.991588367311,0.));
#226331=CARTESIAN_POINT('Ctrl Pts',(-0.661312440730913,-25.991588367311,
0.));
#226332=CARTESIAN_POINT('Ctrl Pts',(-0.664028313187638,-25.9865613464773,
0.));
#226333=CARTESIAN_POINT('Ctrl Pts',(-0.669451306780837,-25.9765104298071,
0.));
#226334=CARTESIAN_POINT('Ctrl Pts',(-0.677559543209739,-25.9614434297919,
0.));
#226335=CARTESIAN_POINT('Ctrl Pts',(-0.688318015057743,-25.9413728471909,
0.));
#226336=CARTESIAN_POINT('Ctrl Pts',(-0.701678575228768,-25.9163158909426,
0.));
#226337=CARTESIAN_POINT('Ctrl Pts',(-0.714951588527651,-25.891290261497,
0.));
#226338=CARTESIAN_POINT('Ctrl Pts',(-0.728137036482348,-25.8662960624185,
0.));
#226339=CARTESIAN_POINT('Ctrl Pts',(-0.741234902663818,-25.8413334619055,
0.));
#226340=CARTESIAN_POINT('Ctrl Pts',(-0.754245175609535,-25.8164027059984,
0.));
#226341=CARTESIAN_POINT('Ctrl Pts',(-0.76716785265118,-25.7915041383376,
0.));
#226342=CARTESIAN_POINT('Ctrl Pts',(-0.780002940291976,-25.7666381946955,
0.));
#226343=CARTESIAN_POINT('Ctrl Pts',(-0.792750451616139,-25.7418053757746,
0.));
#226344=CARTESIAN_POINT('Ctrl Pts',(-0.805410404554365,-25.7170062262525,
0.));
#226345=CARTESIAN_POINT('Ctrl Pts',(-0.817982819787476,-25.6922413110194,
0.));
#226346=CARTESIAN_POINT('Ctrl Pts',(-0.830467718864218,-25.6675111931952,
0.));
#226347=CARTESIAN_POINT('Ctrl Pts',(-0.842865122120771,-25.6428164100055,
0.));
#226348=CARTESIAN_POINT('Ctrl Pts',(-0.85517504703656,-25.6181574536049,
0.));
#226349=CARTESIAN_POINT('Ctrl Pts',(-0.867397509338443,-25.5935347843585,
0.));
#226350=CARTESIAN_POINT('Ctrl Pts',(-0.879532523834307,-25.5689488408156,
0.));
#226351=CARTESIAN_POINT('Ctrl Pts',(-0.891580105349052,-25.5444000508211,
0.));
#226352=CARTESIAN_POINT('Ctrl Pts',(-0.903540269651119,-25.5198888424194,
0.));
#226353=CARTESIAN_POINT('Ctrl Pts',(-0.915413034335626,-25.4954156541795,
0.));
#226354=CARTESIAN_POINT('Ctrl Pts',(-0.927198419886107,-25.4709809475009,
0.));
#226355=CARTESIAN_POINT('Ctrl Pts',(-0.938896449496205,-25.4465852044849,
0.));
#226356=CARTESIAN_POINT('Ctrl Pts',(-0.950507148597481,-25.4222289223167,
0.));
#226357=CARTESIAN_POINT('Ctrl Pts',(-0.962030544503155,-25.3979126089163,
0.));
#226358=CARTESIAN_POINT('Ctrl Pts',(-0.973466666000176,-25.3736367778845,
0.));
#226359=CARTESIAN_POINT('Ctrl Pts',(-0.984815543003984,-25.3494019441441,
0.));
#226360=CARTESIAN_POINT('Ctrl Pts',(-0.996077206120636,-25.3252086182968,
0.));
#226361=CARTESIAN_POINT('Ctrl Pts',(-1.00725168656897,-25.3010573055548,
0.));
#226362=CARTESIAN_POINT('Ctrl Pts',(-1.01833901642238,-25.276948508726,
0.));
#226363=CARTESIAN_POINT('Ctrl Pts',(-1.02933922876807,-25.2528827300422,
0.));
#226364=CARTESIAN_POINT('Ctrl Pts',(-1.04025235791508,-25.2288604735086,
0.));
#226365=CARTESIAN_POINT('Ctrl Pts',(-1.05107843957933,-25.2048822469028,
0.));
#226366=CARTESIAN_POINT('Ctrl Pts',(-1.06181751111769,-25.1809485642192,
0.));
#226367=CARTESIAN_POINT('Ctrl Pts',(-1.07246961165477,-25.157059946931,
0.));
#226368=CARTESIAN_POINT('Ctrl Pts',(-1.08303478197189,-25.1332169227413,
0.));
#226369=CARTESIAN_POINT('Ctrl Pts',(-1.09351306445309,-25.1094200248446,
0.));
#226370=CARTESIAN_POINT('Ctrl Pts',(-1.10390450301746,-25.0856697909679,
0.));
#226371=CARTESIAN_POINT('Ctrl Pts',(-1.1142091430689,-25.0619667625336,
0.));
#226372=CARTESIAN_POINT('Ctrl Pts',(-1.12442703144453,-25.0383114836899,
0.));
#226373=CARTESIAN_POINT('Ctrl Pts',(-1.13455821638531,-25.0147045006196,
0.));
#226374=CARTESIAN_POINT('Ctrl Pts',(-1.14460274758202,-24.9911463621433,
0.));
#226375=CARTESIAN_POINT('Ctrl Pts',(-1.1545606762189,-24.9676376201502,
0.));
#226376=CARTESIAN_POINT('Ctrl Pts',(-1.16443205502851,-24.9441788300932,
0.));
#226377=CARTESIAN_POINT('Ctrl Pts',(-1.17421693835042,-24.9207705514448,
0.));
#226378=CARTESIAN_POINT('Ctrl Pts',(-1.18391538220104,-24.8974133481829,
0.));
#226379=CARTESIAN_POINT('Ctrl Pts',(-1.19352744434065,-24.8741077892075,
0.));
#226380=CARTESIAN_POINT('Ctrl Pts',(-1.20305318426021,-24.8508544481974,
0.));
#226381=CARTESIAN_POINT('Ctrl Pts',(-1.21249266318209,-24.8276539035092,
0.));
#226382=CARTESIAN_POINT('Ctrl Pts',(-1.22184594406529,-24.8045067380536,
0.));
#226383=CARTESIAN_POINT('Ctrl Pts',(-1.23111309161845,-24.7814135391799,
0.));
#226384=CARTESIAN_POINT('Ctrl Pts',(-1.2402941723199,-24.7583748985438,
0.));
#226385=CARTESIAN_POINT('Ctrl Pts',(-1.24938925444327,-24.7353914120011,
0.));
#226386=CARTESIAN_POINT('Ctrl Pts',(-1.25839840807419,-24.7124636797894,
0.));
#226387=CARTESIAN_POINT('Ctrl Pts',(-1.26732170513501,-24.6895923066836,
0.));
#226388=CARTESIAN_POINT('Ctrl Pts',(-1.27615921941643,-24.6667779021559,
0.));
#226389=CARTESIAN_POINT('Ctrl Pts',(-1.28491102661515,-24.6440210805278,
0.));
#226390=CARTESIAN_POINT('Ctrl Pts',(-1.29357720438108,-24.6213224611229,
0.));
#226391=CARTESIAN_POINT('Ctrl Pts',(-1.30215783236363,-24.5986826684027,
0.));
#226392=CARTESIAN_POINT('Ctrl Pts',(-1.31065299222023,-24.5761023320183,
0.));
#226393=CARTESIAN_POINT('Ctrl Pts',(-1.31906276763669,-24.5535820868674,
0.));
#226394=CARTESIAN_POINT('Ctrl Pts',(-1.32738724435327,-24.5311225731435,
0.));
#226395=CARTESIAN_POINT('Ctrl Pts',(-1.33562651019687,-24.5087244363856,
0.));
#226396=CARTESIAN_POINT('Ctrl Pts',(-1.34378065512339,-24.4863883275134,
0.));
#226397=CARTESIAN_POINT('Ctrl Pts',(-1.35184977125649,-24.4641149028892,
0.));
#226398=CARTESIAN_POINT('Ctrl Pts',(-1.35983395290628,-24.4419048244523,
0.));
#226399=CARTESIAN_POINT('Ctrl Pts',(-1.36773329659957,-24.4197587598337,
0.));
#226400=CARTESIAN_POINT('Ctrl Pts',(-1.3755479011161,-24.3976773824732,
0.));
#226401=CARTESIAN_POINT('Ctrl Pts',(-1.38327786753,-24.3756613717299,0.));
#226402=CARTESIAN_POINT('Ctrl Pts',(-1.39092329926389,-24.3537114129875,
0.));
#226403=CARTESIAN_POINT('Ctrl Pts',(-1.39848430212808,-24.3318281977643,
0.));
#226404=CARTESIAN_POINT('Ctrl Pts',(-1.40596098434338,-24.3100124238311,
0.));
#226405=CARTESIAN_POINT('Ctrl Pts',(-1.41335345657684,-24.288264795321,
0.));
#226406=CARTESIAN_POINT('Ctrl Pts',(-1.42066183198254,-24.2665860228356,
0.));
#226407=CARTESIAN_POINT('Ctrl Pts',(-1.42788622624855,-24.2449768235488,
0.));
#226408=CARTESIAN_POINT('Ctrl Pts',(-1.43502675765509,-24.2234379212984,
0.));
#226409=CARTESIAN_POINT('Ctrl Pts',(-1.44208354711083,-24.201970046722,
0.));
#226410=CARTESIAN_POINT('Ctrl Pts',(-1.44905671818729,-24.1805739374038,
0.));
#226411=CARTESIAN_POINT('Ctrl Pts',(-1.45594639716319,-24.1592503380107,
0.));
#226412=CARTESIAN_POINT('Ctrl Pts',(-1.46275271307399,-24.1380000004272,
0.));
#226413=CARTESIAN_POINT('Ctrl Pts',(-1.46947579776992,-24.1168236838824,
0.));
#226414=CARTESIAN_POINT('Ctrl Pts',(-1.47611578597743,-24.0957221550778,
0.));
#226415=CARTESIAN_POINT('Ctrl Pts',(-1.48267281533684,-24.0746961883528,
0.));
#226416=CARTESIAN_POINT('Ctrl Pts',(-1.48914702644888,-24.0537465658429,
0.));
#226417=CARTESIAN_POINT('Ctrl Pts',(-1.49553856292802,-24.0328740776331,
0.));
#226418=CARTESIAN_POINT('Ctrl Pts',(-1.501847571461,-24.0120795219086,0.));
#226419=CARTESIAN_POINT('Ctrl Pts',(-1.50807420187695,-23.9913637050927,
0.));
#226420=CARTESIAN_POINT('Ctrl Pts',(-1.51421860720615,-23.970727442014,
0.));
#226421=CARTESIAN_POINT('Ctrl Pts',(-1.52028094372793,-23.9501715561033,
0.));
#226422=CARTESIAN_POINT('Ctrl Pts',(-1.52626137103033,-23.9296968795757,
0.));
#226423=CARTESIAN_POINT('Ctrl Pts',(-1.53216005207464,-23.9093042536119,
0.));
#226424=CARTESIAN_POINT('Ctrl Pts',(-1.53797715326759,-23.8889945285318,
0.));
#226425=CARTESIAN_POINT('Ctrl Pts',(-1.54371284453991,-23.8687685639642,
0.));
#226426=CARTESIAN_POINT('Ctrl Pts',(-1.54936729940542,-23.8486272290705,
0.));
#226427=CARTESIAN_POINT('Ctrl Pts',(-1.55494069502636,-23.8285714027636,
0.));
#226428=CARTESIAN_POINT('Ctrl Pts',(-1.56043321228635,-23.8086019739194,
0.));
#226429=CARTESIAN_POINT('Ctrl Pts',(-1.56584503586844,-23.7887198415878,
0.));
#226430=CARTESIAN_POINT('Ctrl Pts',(-1.57117635434409,-23.7689259151862,
0.));
#226431=CARTESIAN_POINT('Ctrl Pts',(-1.57642736025247,-23.749221114736,
0.));
#226432=CARTESIAN_POINT('Ctrl Pts',(-1.58159825017359,-23.72960637113,0.));
#226433=CARTESIAN_POINT('Ctrl Pts',(-1.58668922481222,-23.710082626383,
0.));
#226434=CARTESIAN_POINT('Ctrl Pts',(-1.59170048908634,-23.6906508338833,
0.));
#226435=CARTESIAN_POINT('Ctrl Pts',(-1.59663225222464,-23.671311958631,
0.));
#226436=CARTESIAN_POINT('Ctrl Pts',(-1.60148472786596,-23.6520669774876,
0.));
#226437=CARTESIAN_POINT('Ctrl Pts',(-1.60625813414674,-23.6329168794929,
0.));
#226438=CARTESIAN_POINT('Ctrl Pts',(-1.61095269379779,-23.6138626661653,
0.));
#226439=CARTESIAN_POINT('Ctrl Pts',(-1.61556863424699,-23.5949053517997,
0.));
#226440=CARTESIAN_POINT('Ctrl Pts',(-1.62010618772867,-23.57604596376,0.));
#226441=CARTESIAN_POINT('Ctrl Pts',(-1.62456559140065,-23.5572855427601,
0.));
#226442=CARTESIAN_POINT('Ctrl Pts',(-1.62894708745224,-23.538625143226,
0.));
#226443=CARTESIAN_POINT('Ctrl Pts',(-1.63325092321727,-23.5200658336612,
0.));
#226444=CARTESIAN_POINT('Ctrl Pts',(-1.63747735129475,-23.5016086970003,
0.));
#226445=CARTESIAN_POINT('Ctrl Pts',(-1.64162662967529,-23.4832548309645,
0.));
#226446=CARTESIAN_POINT('Ctrl Pts',(-1.64569902187612,-23.4650053483932,
0.));
#226447=CARTESIAN_POINT('Ctrl Pts',(-1.64969479707341,-23.4468613776574,
0.));
#226448=CARTESIAN_POINT('Ctrl Pts',(-1.65361423023729,-23.4288240631043,
0.));
#226449=CARTESIAN_POINT('Ctrl Pts',(-1.65745760227506,-23.4108945654805,
0.));
#226450=CARTESIAN_POINT('Ctrl Pts',(-1.66122520018012,-23.3930740623619,
0.));
#226451=CARTESIAN_POINT('Ctrl Pts',(-1.66491731718878,-23.3753637485545,
0.));
#226452=CARTESIAN_POINT('Ctrl Pts',(-1.66853425293997,-23.3577648365744,
0.));
#226453=CARTESIAN_POINT('Ctrl Pts',(-1.67207631363923,-23.3402785571865,
0.));
#226454=CARTESIAN_POINT('Ctrl Pts',(-1.67554381222995,-23.3229061599145,
0.));
#226455=CARTESIAN_POINT('Ctrl Pts',(-1.67893706857118,-23.3056489135611,
0.));
#226456=CARTESIAN_POINT('Ctrl Pts',(-1.68225640962169,-23.2885081066951,
0.));
#226457=CARTESIAN_POINT('Ctrl Pts',(-1.68550216963259,-23.2714850482246,
0.));
#226458=CARTESIAN_POINT('Ctrl Pts',(-1.68867469034897,-23.2545810680537,
0.));
#226459=CARTESIAN_POINT('Ctrl Pts',(-1.69177432121712,-23.2377975177013,
0.));
#226460=CARTESIAN_POINT('Ctrl Pts',(-1.69480141959954,-23.2211357709374,
0.));
#226461=CARTESIAN_POINT('Ctrl Pts',(-1.69775635099444,-23.2045972243767,
0.));
#226462=CARTESIAN_POINT('Ctrl Pts',(-1.70063948927011,-23.1881832981851,
0.));
#226463=CARTESIAN_POINT('Ctrl Pts',(-1.70345121691277,-23.1718954368751,
0.));
#226464=CARTESIAN_POINT('Ctrl Pts',(-1.70619192527853,-23.1557351100614,
0.));
#226465=CARTESIAN_POINT('Ctrl Pts',(-1.70886201485453,-23.1397038132356,
0.));
#226466=CARTESIAN_POINT('Ctrl Pts',(-1.71146189552175,-23.1238030684925,
0.));
#226467=CARTESIAN_POINT('Ctrl Pts',(-1.71399198684705,-23.1080344254286,
0.));
#226468=CARTESIAN_POINT('Ctrl Pts',(-1.71645271839298,-23.0923994621213,
0.));
#226469=CARTESIAN_POINT('Ctrl Pts',(-1.71884453003028,-23.0768997860709,
0.));
#226470=CARTESIAN_POINT('Ctrl Pts',(-1.72116787225993,-23.0615370351562,
0.));
#226471=CARTESIAN_POINT('Ctrl Pts',(-1.72342320653748,-23.0463128785531,
0.));
#226472=CARTESIAN_POINT('Ctrl Pts',(-1.72561100564047,-23.0312290178883,
0.));
#226473=CARTESIAN_POINT('Ctrl Pts',(-1.7277317540471,-23.0162871884168,
0.));
#226474=CARTESIAN_POINT('Ctrl Pts',(-1.72978594832137,-23.001489160189,
0.));
#226475=CARTESIAN_POINT('Ctrl Pts',(-1.73177409750192,-22.9868367391978,
0.));
#226476=CARTESIAN_POINT('Ctrl Pts',(-1.73369672350816,-22.9723317685688,
0.));
#226477=CARTESIAN_POINT('Ctrl Pts',(-1.7355543616277,-22.9579761301063,
0.));
#226478=CARTESIAN_POINT('Ctrl Pts',(-1.7373475610004,-22.9437717457826,
0.));
#226479=CARTESIAN_POINT('Ctrl Pts',(-1.73907688511667,-22.9297205792586,
0.));
#226480=CARTESIAN_POINT('Ctrl Pts',(-1.74074291231059,-22.9158246373363,
0.));
#226481=CARTESIAN_POINT('Ctrl Pts',(-1.74234623630081,-22.9020859716141,
0.));
#226482=CARTESIAN_POINT('Ctrl Pts',(-1.74388746677703,-22.888506680335,
0.));
#226483=CARTESIAN_POINT('Ctrl Pts',(-1.74536722998202,-22.8750889101696,
0.));
#226484=CARTESIAN_POINT('Ctrl Pts',(-1.74678616930666,-22.8618348580235,
0.));
#226485=CARTESIAN_POINT('Ctrl Pts',(-1.74814494588494,-22.8487467728076,
0.));
#226486=CARTESIAN_POINT('Ctrl Pts',(-1.74944423940117,-22.8358269579853,
0.));
#226487=CARTESIAN_POINT('Ctrl Pts',(-1.75068474890884,-22.8230777741284,
0.));
#226488=CARTESIAN_POINT('Ctrl Pts',(-1.75186719365593,-22.8105016414713,
0.));
#226489=CARTESIAN_POINT('Ctrl Pts',(-1.75299231391467,-22.7981010424314,
0.));
#226490=CARTESIAN_POINT('Ctrl Pts',(-1.75406087182937,-22.7858785242361,
0.));
#226491=CARTESIAN_POINT('Ctrl Pts',(-1.75507365227133,-22.7738367016118,
0.));
#226492=CARTESIAN_POINT('Ctrl Pts',(-1.75603146371642,-22.7619782595013,
0.));
#226493=CARTESIAN_POINT('Ctrl Pts',(-1.75693513908908,-22.750305955645,
0.));
#226494=CARTESIAN_POINT('Ctrl Pts',(-1.75778553673245,-22.7388226235559,
0.));
#226495=CARTESIAN_POINT('Ctrl Pts',(-1.75858354204634,-22.72753117773,0.));
#226496=CARTESIAN_POINT('Ctrl Pts',(-1.75933006905926,-22.7164346186006,
0.));
#226497=CARTESIAN_POINT('Ctrl Pts',(-1.76002606202402,-22.7055360375485,
0.));
#226498=CARTESIAN_POINT('Ctrl Pts',(-1.76067249704888,-22.6948386219851,
0.));
#226499=CARTESIAN_POINT('Ctrl Pts',(-1.76127038310615,-22.684345658525,
0.));
#226500=CARTESIAN_POINT('Ctrl Pts',(-1.76182076289527,-22.67406053567,0.));
#226501=CARTESIAN_POINT('Ctrl Pts',(-1.7623247139257,-22.6639867471753,
0.));
#226502=CARTESIAN_POINT('Ctrl Pts',(-1.76278334912562,-22.654127893841,
0.));
#226503=CARTESIAN_POINT('Ctrl Pts',(-1.76319782013917,-22.6444876940423,
0.));
#226504=CARTESIAN_POINT('Ctrl Pts',(-1.76356932176274,-22.6350699979359,
0.));
#226505=CARTESIAN_POINT('Ctrl Pts',(-1.76389909571404,-22.6258787994848,
0.));
#226506=CARTESIAN_POINT('Ctrl Pts',(-1.7641884354374,-22.6169182517694,
0.));
#226507=CARTESIAN_POINT('Ctrl Pts',(-1.76443868648017,-22.6081926681343,
0.));
#226508=CARTESIAN_POINT('Ctrl Pts',(-1.76465124413558,-22.5997065145638,
0.));
#226509=CARTESIAN_POINT('Ctrl Pts',(-1.76482755288412,-22.5914644078106,
0.));
#226510=CARTESIAN_POINT('Ctrl Pts',(-1.76496910283089,-22.5834711038022,
0.));
#226511=CARTESIAN_POINT('Ctrl Pts',(-1.76507744026747,-22.5757315316353,
0.));
#226512=CARTESIAN_POINT('Ctrl Pts',(-1.76515418518832,-22.5682508499874,
0.));
#226513=CARTESIAN_POINT('Ctrl Pts',(-1.76520104500451,-22.5610344912501,
0.));
#226514=CARTESIAN_POINT('Ctrl Pts',(-1.76521983384063,-22.5540882235837,
0.));
#226515=CARTESIAN_POINT('Ctrl Pts',(-1.76521245524048,-22.5474180954006,
0.));
#226516=CARTESIAN_POINT('Ctrl Pts',(-1.76518087841494,-22.5410303590892,
0.));
#226517=CARTESIAN_POINT('Ctrl Pts',(-1.76512711563255,-22.5349313983571,
0.));
#226518=CARTESIAN_POINT('Ctrl Pts',(-1.7650532026276,-22.529127665298,0.));
#226519=CARTESIAN_POINT('Ctrl Pts',(-1.76496128643376,-22.5236259635515,
0.));
#226520=CARTESIAN_POINT('Ctrl Pts',(-1.76485369319896,-22.5184336670207,
0.));
#226521=CARTESIAN_POINT('Ctrl Pts',(-1.7647330328115,-22.5135590569554,
0.));
#226522=CARTESIAN_POINT('Ctrl Pts',(-1.76460218257314,-22.5090112700212,
0.));
#226523=CARTESIAN_POINT('Ctrl Pts',(-1.76446408210366,-22.5047996391978,
0.));
#226524=CARTESIAN_POINT('Ctrl Pts',(-1.76432160068739,-22.5009332677316,
0.));
#226525=CARTESIAN_POINT('Ctrl Pts',(-1.76417731243484,-22.4974203063191,
0.));
#226526=CARTESIAN_POINT('Ctrl Pts',(-1.76403393880317,-22.4942693792449,
0.));
#226527=CARTESIAN_POINT('Ctrl Pts',(-1.76389475965715,-22.4914909094908,
0.));
#226528=CARTESIAN_POINT('Ctrl Pts',(-1.76376424879469,-22.4890991659479,
0.));
#226529=CARTESIAN_POINT('Ctrl Pts',(-1.76364784232926,-22.4871115206572,
0.));
#226530=CARTESIAN_POINT('Ctrl Pts',(-1.7635507604555,-22.4855446605991,
0.));
#226531=CARTESIAN_POINT('Ctrl Pts',(-1.76347698284863,-22.4844112933125,
0.));
#226532=CARTESIAN_POINT('Ctrl Pts',(-1.7634381343466,-22.4838562517064,
0.));
#226533=CARTESIAN_POINT('Ctrl Pts',(-1.76342064263638,-22.4836387052228,
0.));
#226534=CARTESIAN_POINT('Ctrl Pts',(-1.76341415538792,-22.4835819929788,
0.));
#226535=CARTESIAN_POINT('Ctrl Pts',(-1.76341220531181,-22.4835757167854,
0.));
#226536=CARTESIAN_POINT('',(-0.661312440730913,-25.991588367311,12.));
#226537=CARTESIAN_POINT('',(-0.661312440730913,-25.991588367311,0.));
#226538=CARTESIAN_POINT('Ctrl Pts',(-1.76341220531181,-22.4835757167854,
12.));
#226539=CARTESIAN_POINT('Ctrl Pts',(-1.76341415538792,-22.4835819929788,
12.));
#226540=CARTESIAN_POINT('Ctrl Pts',(-1.76342064263638,-22.4836387052228,
12.));
#226541=CARTESIAN_POINT('Ctrl Pts',(-1.7634381343466,-22.4838562517064,
12.));
#226542=CARTESIAN_POINT('Ctrl Pts',(-1.76347698284863,-22.4844112933125,
12.));
#226543=CARTESIAN_POINT('Ctrl Pts',(-1.7635507604555,-22.4855446605991,
12.));
#226544=CARTESIAN_POINT('Ctrl Pts',(-1.76364784232926,-22.4871115206572,
12.));
#226545=CARTESIAN_POINT('Ctrl Pts',(-1.76376424879469,-22.4890991659479,
12.));
#226546=CARTESIAN_POINT('Ctrl Pts',(-1.76389475965715,-22.4914909094908,
12.));
#226547=CARTESIAN_POINT('Ctrl Pts',(-1.76403393880317,-22.4942693792449,
12.));
#226548=CARTESIAN_POINT('Ctrl Pts',(-1.76417731243484,-22.4974203063191,
12.));
#226549=CARTESIAN_POINT('Ctrl Pts',(-1.76432160068739,-22.5009332677316,
12.));
#226550=CARTESIAN_POINT('Ctrl Pts',(-1.76446408210366,-22.5047996391978,
12.));
#226551=CARTESIAN_POINT('Ctrl Pts',(-1.76460218257314,-22.5090112700212,
12.));
#226552=CARTESIAN_POINT('Ctrl Pts',(-1.7647330328115,-22.5135590569554,
12.));
#226553=CARTESIAN_POINT('Ctrl Pts',(-1.76485369319896,-22.5184336670207,
12.));
#226554=CARTESIAN_POINT('Ctrl Pts',(-1.76496128643376,-22.5236259635515,
12.));
#226555=CARTESIAN_POINT('Ctrl Pts',(-1.7650532026276,-22.529127665298,12.));
#226556=CARTESIAN_POINT('Ctrl Pts',(-1.76512711563255,-22.5349313983571,
12.));
#226557=CARTESIAN_POINT('Ctrl Pts',(-1.76518087841494,-22.5410303590892,
12.));
#226558=CARTESIAN_POINT('Ctrl Pts',(-1.76521245524048,-22.5474180954006,
12.));
#226559=CARTESIAN_POINT('Ctrl Pts',(-1.76521983384063,-22.5540882235837,
12.));
#226560=CARTESIAN_POINT('Ctrl Pts',(-1.76520104500451,-22.5610344912501,
12.));
#226561=CARTESIAN_POINT('Ctrl Pts',(-1.76515418518832,-22.5682508499874,
12.));
#226562=CARTESIAN_POINT('Ctrl Pts',(-1.76507744026747,-22.5757315316353,
12.));
#226563=CARTESIAN_POINT('Ctrl Pts',(-1.76496910283089,-22.5834711038022,
12.));
#226564=CARTESIAN_POINT('Ctrl Pts',(-1.76482755288412,-22.5914644078106,
12.));
#226565=CARTESIAN_POINT('Ctrl Pts',(-1.76465124413558,-22.5997065145638,
12.));
#226566=CARTESIAN_POINT('Ctrl Pts',(-1.76443868648017,-22.6081926681343,
12.));
#226567=CARTESIAN_POINT('Ctrl Pts',(-1.7641884354374,-22.6169182517694,
12.));
#226568=CARTESIAN_POINT('Ctrl Pts',(-1.76389909571404,-22.6258787994848,
12.));
#226569=CARTESIAN_POINT('Ctrl Pts',(-1.76356932176274,-22.6350699979359,
12.));
#226570=CARTESIAN_POINT('Ctrl Pts',(-1.76319782013917,-22.6444876940423,
12.));
#226571=CARTESIAN_POINT('Ctrl Pts',(-1.76278334912562,-22.654127893841,
12.));
#226572=CARTESIAN_POINT('Ctrl Pts',(-1.7623247139257,-22.6639867471753,
12.));
#226573=CARTESIAN_POINT('Ctrl Pts',(-1.76182076289527,-22.67406053567,12.));
#226574=CARTESIAN_POINT('Ctrl Pts',(-1.76127038310615,-22.684345658525,
12.));
#226575=CARTESIAN_POINT('Ctrl Pts',(-1.76067249704888,-22.6948386219851,
12.));
#226576=CARTESIAN_POINT('Ctrl Pts',(-1.76002606202402,-22.7055360375485,
12.));
#226577=CARTESIAN_POINT('Ctrl Pts',(-1.75933006905926,-22.7164346186006,
12.));
#226578=CARTESIAN_POINT('Ctrl Pts',(-1.75858354204634,-22.72753117773,12.));
#226579=CARTESIAN_POINT('Ctrl Pts',(-1.75778553673245,-22.7388226235559,
12.));
#226580=CARTESIAN_POINT('Ctrl Pts',(-1.75693513908908,-22.750305955645,
12.));
#226581=CARTESIAN_POINT('Ctrl Pts',(-1.75603146371642,-22.7619782595013,
12.));
#226582=CARTESIAN_POINT('Ctrl Pts',(-1.75507365227133,-22.7738367016118,
12.));
#226583=CARTESIAN_POINT('Ctrl Pts',(-1.75406087182937,-22.7858785242361,
12.));
#226584=CARTESIAN_POINT('Ctrl Pts',(-1.75299231391467,-22.7981010424314,
12.));
#226585=CARTESIAN_POINT('Ctrl Pts',(-1.75186719365593,-22.8105016414713,
12.));
#226586=CARTESIAN_POINT('Ctrl Pts',(-1.75068474890884,-22.8230777741284,
12.));
#226587=CARTESIAN_POINT('Ctrl Pts',(-1.74944423940117,-22.8358269579853,
12.));
#226588=CARTESIAN_POINT('Ctrl Pts',(-1.74814494588494,-22.8487467728076,
12.));
#226589=CARTESIAN_POINT('Ctrl Pts',(-1.74678616930666,-22.8618348580235,
12.));
#226590=CARTESIAN_POINT('Ctrl Pts',(-1.74536722998202,-22.8750889101696,
12.));
#226591=CARTESIAN_POINT('Ctrl Pts',(-1.74388746677703,-22.888506680335,
12.));
#226592=CARTESIAN_POINT('Ctrl Pts',(-1.74234623630081,-22.9020859716141,
12.));
#226593=CARTESIAN_POINT('Ctrl Pts',(-1.74074291231059,-22.9158246373363,
12.));
#226594=CARTESIAN_POINT('Ctrl Pts',(-1.73907688511667,-22.9297205792586,
12.));
#226595=CARTESIAN_POINT('Ctrl Pts',(-1.7373475610004,-22.9437717457826,
12.));
#226596=CARTESIAN_POINT('Ctrl Pts',(-1.7355543616277,-22.9579761301063,
12.));
#226597=CARTESIAN_POINT('Ctrl Pts',(-1.73369672350816,-22.9723317685688,
12.));
#226598=CARTESIAN_POINT('Ctrl Pts',(-1.73177409750192,-22.9868367391978,
12.));
#226599=CARTESIAN_POINT('Ctrl Pts',(-1.72978594832137,-23.001489160189,
12.));
#226600=CARTESIAN_POINT('Ctrl Pts',(-1.7277317540471,-23.0162871884168,
12.));
#226601=CARTESIAN_POINT('Ctrl Pts',(-1.72561100564047,-23.0312290178883,
12.));
#226602=CARTESIAN_POINT('Ctrl Pts',(-1.72342320653748,-23.0463128785531,
12.));
#226603=CARTESIAN_POINT('Ctrl Pts',(-1.72116787225993,-23.0615370351562,
12.));
#226604=CARTESIAN_POINT('Ctrl Pts',(-1.71884453003028,-23.0768997860709,
12.));
#226605=CARTESIAN_POINT('Ctrl Pts',(-1.71645271839298,-23.0923994621213,
12.));
#226606=CARTESIAN_POINT('Ctrl Pts',(-1.71399198684705,-23.1080344254286,
12.));
#226607=CARTESIAN_POINT('Ctrl Pts',(-1.71146189552175,-23.1238030684925,
12.));
#226608=CARTESIAN_POINT('Ctrl Pts',(-1.70886201485453,-23.1397038132356,
12.));
#226609=CARTESIAN_POINT('Ctrl Pts',(-1.70619192527853,-23.1557351100614,
12.));
#226610=CARTESIAN_POINT('Ctrl Pts',(-1.70345121691277,-23.1718954368751,
12.));
#226611=CARTESIAN_POINT('Ctrl Pts',(-1.70063948927011,-23.1881832981851,
12.));
#226612=CARTESIAN_POINT('Ctrl Pts',(-1.69775635099444,-23.2045972243767,
12.));
#226613=CARTESIAN_POINT('Ctrl Pts',(-1.69480141959954,-23.2211357709374,
12.));
#226614=CARTESIAN_POINT('Ctrl Pts',(-1.69177432121712,-23.2377975177013,
12.));
#226615=CARTESIAN_POINT('Ctrl Pts',(-1.68867469034897,-23.2545810680537,
12.));
#226616=CARTESIAN_POINT('Ctrl Pts',(-1.68550216963259,-23.2714850482246,
12.));
#226617=CARTESIAN_POINT('Ctrl Pts',(-1.68225640962169,-23.2885081066951,
12.));
#226618=CARTESIAN_POINT('Ctrl Pts',(-1.67893706857118,-23.3056489135611,
12.));
#226619=CARTESIAN_POINT('Ctrl Pts',(-1.67554381222995,-23.3229061599145,
12.));
#226620=CARTESIAN_POINT('Ctrl Pts',(-1.67207631363923,-23.3402785571865,
12.));
#226621=CARTESIAN_POINT('Ctrl Pts',(-1.66853425293997,-23.3577648365744,
12.));
#226622=CARTESIAN_POINT('Ctrl Pts',(-1.66491731718878,-23.3753637485545,
12.));
#226623=CARTESIAN_POINT('Ctrl Pts',(-1.66122520018012,-23.3930740623619,
12.));
#226624=CARTESIAN_POINT('Ctrl Pts',(-1.65745760227506,-23.4108945654805,
12.));
#226625=CARTESIAN_POINT('Ctrl Pts',(-1.65361423023729,-23.4288240631043,
12.));
#226626=CARTESIAN_POINT('Ctrl Pts',(-1.64969479707341,-23.4468613776574,
12.));
#226627=CARTESIAN_POINT('Ctrl Pts',(-1.64569902187612,-23.4650053483932,
12.));
#226628=CARTESIAN_POINT('Ctrl Pts',(-1.64162662967529,-23.4832548309645,
12.));
#226629=CARTESIAN_POINT('Ctrl Pts',(-1.63747735129475,-23.5016086970003,
12.));
#226630=CARTESIAN_POINT('Ctrl Pts',(-1.63325092321727,-23.5200658336612,
12.));
#226631=CARTESIAN_POINT('Ctrl Pts',(-1.62894708745224,-23.538625143226,
12.));
#226632=CARTESIAN_POINT('Ctrl Pts',(-1.62456559140065,-23.5572855427601,
12.));
#226633=CARTESIAN_POINT('Ctrl Pts',(-1.62010618772867,-23.57604596376,12.));
#226634=CARTESIAN_POINT('Ctrl Pts',(-1.61556863424699,-23.5949053517997,
12.));
#226635=CARTESIAN_POINT('Ctrl Pts',(-1.61095269379779,-23.6138626661653,
12.));
#226636=CARTESIAN_POINT('Ctrl Pts',(-1.60625813414674,-23.6329168794929,
12.));
#226637=CARTESIAN_POINT('Ctrl Pts',(-1.60148472786596,-23.6520669774876,
12.));
#226638=CARTESIAN_POINT('Ctrl Pts',(-1.59663225222464,-23.671311958631,
12.));
#226639=CARTESIAN_POINT('Ctrl Pts',(-1.59170048908634,-23.6906508338833,
12.));
#226640=CARTESIAN_POINT('Ctrl Pts',(-1.58668922481222,-23.710082626383,
12.));
#226641=CARTESIAN_POINT('Ctrl Pts',(-1.58159825017359,-23.72960637113,12.));
#226642=CARTESIAN_POINT('Ctrl Pts',(-1.57642736025247,-23.749221114736,
12.));
#226643=CARTESIAN_POINT('Ctrl Pts',(-1.57117635434409,-23.7689259151862,
12.));
#226644=CARTESIAN_POINT('Ctrl Pts',(-1.56584503586844,-23.7887198415878,
12.));
#226645=CARTESIAN_POINT('Ctrl Pts',(-1.56043321228635,-23.8086019739194,
12.));
#226646=CARTESIAN_POINT('Ctrl Pts',(-1.55494069502636,-23.8285714027636,
12.));
#226647=CARTESIAN_POINT('Ctrl Pts',(-1.54936729940542,-23.8486272290705,
12.));
#226648=CARTESIAN_POINT('Ctrl Pts',(-1.54371284453991,-23.8687685639642,
12.));
#226649=CARTESIAN_POINT('Ctrl Pts',(-1.53797715326759,-23.8889945285318,
12.));
#226650=CARTESIAN_POINT('Ctrl Pts',(-1.53216005207464,-23.9093042536119,
12.));
#226651=CARTESIAN_POINT('Ctrl Pts',(-1.52626137103033,-23.9296968795757,
12.));
#226652=CARTESIAN_POINT('Ctrl Pts',(-1.52028094372793,-23.9501715561033,
12.));
#226653=CARTESIAN_POINT('Ctrl Pts',(-1.51421860720615,-23.970727442014,
12.));
#226654=CARTESIAN_POINT('Ctrl Pts',(-1.50807420187695,-23.9913637050927,
12.));
#226655=CARTESIAN_POINT('Ctrl Pts',(-1.501847571461,-24.0120795219086,12.));
#226656=CARTESIAN_POINT('Ctrl Pts',(-1.49553856292802,-24.0328740776331,
12.));
#226657=CARTESIAN_POINT('Ctrl Pts',(-1.48914702644888,-24.0537465658429,
12.));
#226658=CARTESIAN_POINT('Ctrl Pts',(-1.48267281533684,-24.0746961883528,
12.));
#226659=CARTESIAN_POINT('Ctrl Pts',(-1.47611578597743,-24.0957221550778,
12.));
#226660=CARTESIAN_POINT('Ctrl Pts',(-1.46947579776992,-24.1168236838824,
12.));
#226661=CARTESIAN_POINT('Ctrl Pts',(-1.46275271307399,-24.1380000004272,
12.));
#226662=CARTESIAN_POINT('Ctrl Pts',(-1.45594639716319,-24.1592503380107,
12.));
#226663=CARTESIAN_POINT('Ctrl Pts',(-1.44905671818729,-24.1805739374038,
12.));
#226664=CARTESIAN_POINT('Ctrl Pts',(-1.44208354711083,-24.201970046722,
12.));
#226665=CARTESIAN_POINT('Ctrl Pts',(-1.43502675765509,-24.2234379212984,
12.));
#226666=CARTESIAN_POINT('Ctrl Pts',(-1.42788622624855,-24.2449768235488,
12.));
#226667=CARTESIAN_POINT('Ctrl Pts',(-1.42066183198254,-24.2665860228356,
12.));
#226668=CARTESIAN_POINT('Ctrl Pts',(-1.41335345657684,-24.288264795321,
12.));
#226669=CARTESIAN_POINT('Ctrl Pts',(-1.40596098434338,-24.3100124238311,
12.));
#226670=CARTESIAN_POINT('Ctrl Pts',(-1.39848430212808,-24.3318281977643,
12.));
#226671=CARTESIAN_POINT('Ctrl Pts',(-1.39092329926389,-24.3537114129875,
12.));
#226672=CARTESIAN_POINT('Ctrl Pts',(-1.38327786753,-24.3756613717299,12.));
#226673=CARTESIAN_POINT('Ctrl Pts',(-1.3755479011161,-24.3976773824732,
12.));
#226674=CARTESIAN_POINT('Ctrl Pts',(-1.36773329659957,-24.4197587598337,
12.));
#226675=CARTESIAN_POINT('Ctrl Pts',(-1.35983395290628,-24.4419048244523,
12.));
#226676=CARTESIAN_POINT('Ctrl Pts',(-1.35184977125649,-24.4641149028892,
12.));
#226677=CARTESIAN_POINT('Ctrl Pts',(-1.34378065512339,-24.4863883275134,
12.));
#226678=CARTESIAN_POINT('Ctrl Pts',(-1.33562651019687,-24.5087244363856,
12.));
#226679=CARTESIAN_POINT('Ctrl Pts',(-1.32738724435327,-24.5311225731435,
12.));
#226680=CARTESIAN_POINT('Ctrl Pts',(-1.31906276763669,-24.5535820868674,
12.));
#226681=CARTESIAN_POINT('Ctrl Pts',(-1.31065299222023,-24.5761023320183,
12.));
#226682=CARTESIAN_POINT('Ctrl Pts',(-1.30215783236363,-24.5986826684027,
12.));
#226683=CARTESIAN_POINT('Ctrl Pts',(-1.29357720438108,-24.6213224611229,
12.));
#226684=CARTESIAN_POINT('Ctrl Pts',(-1.28491102661515,-24.6440210805278,
12.));
#226685=CARTESIAN_POINT('Ctrl Pts',(-1.27615921941643,-24.6667779021559,
12.));
#226686=CARTESIAN_POINT('Ctrl Pts',(-1.26732170513501,-24.6895923066836,
12.));
#226687=CARTESIAN_POINT('Ctrl Pts',(-1.25839840807419,-24.7124636797894,
12.));
#226688=CARTESIAN_POINT('Ctrl Pts',(-1.24938925444327,-24.7353914120011,
12.));
#226689=CARTESIAN_POINT('Ctrl Pts',(-1.2402941723199,-24.7583748985438,
12.));
#226690=CARTESIAN_POINT('Ctrl Pts',(-1.23111309161845,-24.7814135391799,
12.));
#226691=CARTESIAN_POINT('Ctrl Pts',(-1.22184594406529,-24.8045067380536,
12.));
#226692=CARTESIAN_POINT('Ctrl Pts',(-1.21249266318209,-24.8276539035092,
12.));
#226693=CARTESIAN_POINT('Ctrl Pts',(-1.20305318426021,-24.8508544481974,
12.));
#226694=CARTESIAN_POINT('Ctrl Pts',(-1.19352744434065,-24.8741077892075,
12.));
#226695=CARTESIAN_POINT('Ctrl Pts',(-1.18391538220104,-24.8974133481829,
12.));
#226696=CARTESIAN_POINT('Ctrl Pts',(-1.17421693835042,-24.9207705514448,
12.));
#226697=CARTESIAN_POINT('Ctrl Pts',(-1.16443205502851,-24.9441788300932,
12.));
#226698=CARTESIAN_POINT('Ctrl Pts',(-1.1545606762189,-24.9676376201502,
12.));
#226699=CARTESIAN_POINT('Ctrl Pts',(-1.14460274758202,-24.9911463621433,
12.));
#226700=CARTESIAN_POINT('Ctrl Pts',(-1.13455821638531,-25.0147045006196,
12.));
#226701=CARTESIAN_POINT('Ctrl Pts',(-1.12442703144453,-25.0383114836899,
12.));
#226702=CARTESIAN_POINT('Ctrl Pts',(-1.1142091430689,-25.0619667625336,
12.));
#226703=CARTESIAN_POINT('Ctrl Pts',(-1.10390450301746,-25.0856697909679,
12.));
#226704=CARTESIAN_POINT('Ctrl Pts',(-1.09351306445309,-25.1094200248446,
12.));
#226705=CARTESIAN_POINT('Ctrl Pts',(-1.08303478197189,-25.1332169227413,
12.));
#226706=CARTESIAN_POINT('Ctrl Pts',(-1.07246961165477,-25.157059946931,
12.));
#226707=CARTESIAN_POINT('Ctrl Pts',(-1.06181751111769,-25.1809485642192,
12.));
#226708=CARTESIAN_POINT('Ctrl Pts',(-1.05107843957933,-25.2048822469028,
12.));
#226709=CARTESIAN_POINT('Ctrl Pts',(-1.04025235791508,-25.2288604735086,
12.));
#226710=CARTESIAN_POINT('Ctrl Pts',(-1.02933922876807,-25.2528827300422,
12.));
#226711=CARTESIAN_POINT('Ctrl Pts',(-1.01833901642238,-25.276948508726,
12.));
#226712=CARTESIAN_POINT('Ctrl Pts',(-1.00725168656897,-25.3010573055548,
12.));
#226713=CARTESIAN_POINT('Ctrl Pts',(-0.996077206120636,-25.3252086182968,
12.));
#226714=CARTESIAN_POINT('Ctrl Pts',(-0.984815543003984,-25.3494019441441,
12.));
#226715=CARTESIAN_POINT('Ctrl Pts',(-0.973466666000176,-25.3736367778845,
12.));
#226716=CARTESIAN_POINT('Ctrl Pts',(-0.962030544503155,-25.3979126089163,
12.));
#226717=CARTESIAN_POINT('Ctrl Pts',(-0.950507148597481,-25.4222289223167,
12.));
#226718=CARTESIAN_POINT('Ctrl Pts',(-0.938896449496205,-25.4465852044849,
12.));
#226719=CARTESIAN_POINT('Ctrl Pts',(-0.927198419886107,-25.4709809475009,
12.));
#226720=CARTESIAN_POINT('Ctrl Pts',(-0.915413034335626,-25.4954156541795,
12.));
#226721=CARTESIAN_POINT('Ctrl Pts',(-0.903540269651119,-25.5198888424194,
12.));
#226722=CARTESIAN_POINT('Ctrl Pts',(-0.891580105349052,-25.5444000508211,
12.));
#226723=CARTESIAN_POINT('Ctrl Pts',(-0.879532523834307,-25.5689488408156,
12.));
#226724=CARTESIAN_POINT('Ctrl Pts',(-0.867397509338443,-25.5935347843585,
12.));
#226725=CARTESIAN_POINT('Ctrl Pts',(-0.85517504703656,-25.6181574536049,
12.));
#226726=CARTESIAN_POINT('Ctrl Pts',(-0.842865122120771,-25.6428164100055,
12.));
#226727=CARTESIAN_POINT('Ctrl Pts',(-0.830467718864218,-25.6675111931952,
12.));
#226728=CARTESIAN_POINT('Ctrl Pts',(-0.817982819787476,-25.6922413110194,
12.));
#226729=CARTESIAN_POINT('Ctrl Pts',(-0.805410404554365,-25.7170062262525,
12.));
#226730=CARTESIAN_POINT('Ctrl Pts',(-0.792750451616139,-25.7418053757746,
12.));
#226731=CARTESIAN_POINT('Ctrl Pts',(-0.780002940291976,-25.7666381946955,
12.));
#226732=CARTESIAN_POINT('Ctrl Pts',(-0.76716785265118,-25.7915041383376,
12.));
#226733=CARTESIAN_POINT('Ctrl Pts',(-0.754245175609535,-25.8164027059984,
12.));
#226734=CARTESIAN_POINT('Ctrl Pts',(-0.741234902663818,-25.8413334619055,
12.));
#226735=CARTESIAN_POINT('Ctrl Pts',(-0.728137036482348,-25.8662960624185,
12.));
#226736=CARTESIAN_POINT('Ctrl Pts',(-0.714951588527651,-25.891290261497,
12.));
#226737=CARTESIAN_POINT('Ctrl Pts',(-0.701678575228768,-25.9163158909426,
12.));
#226738=CARTESIAN_POINT('Ctrl Pts',(-0.688318015057743,-25.9413728471909,
12.));
#226739=CARTESIAN_POINT('Ctrl Pts',(-0.677559543209739,-25.9614434297919,
12.));
#226740=CARTESIAN_POINT('Ctrl Pts',(-0.669451306780837,-25.9765104298071,
12.));
#226741=CARTESIAN_POINT('Ctrl Pts',(-0.664028313187638,-25.9865613464773,
12.));
#226742=CARTESIAN_POINT('Ctrl Pts',(-0.661312440730913,-25.991588367311,
12.));
#226743=CARTESIAN_POINT('Ctrl Pts',(-4.11585220600463,-22.1738711152697,
0.));
#226744=CARTESIAN_POINT('Ctrl Pts',(-4.11585220600463,-22.1738711152697,
12.));
#226745=CARTESIAN_POINT('Ctrl Pts',(-4.11585194677443,-22.173877682324,
0.));
#226746=CARTESIAN_POINT('Ctrl Pts',(-4.11585194677443,-22.173877682324,
12.));
#226747=CARTESIAN_POINT('Ctrl Pts',(-4.11586035878288,-22.1739341411687,
0.));
#226748=CARTESIAN_POINT('Ctrl Pts',(-4.11586035878288,-22.1739341411687,
12.));
#226749=CARTESIAN_POINT('Ctrl Pts',(-4.11589976826167,-22.1741488021234,
0.));
#226750=CARTESIAN_POINT('Ctrl Pts',(-4.11589976826167,-22.1741488021234,
12.));
#226751=CARTESIAN_POINT('Ctrl Pts',(-4.11600589882846,-22.1746949858775,
0.));
#226752=CARTESIAN_POINT('Ctrl Pts',(-4.11600589882846,-22.1746949858775,
12.));
#226753=CARTESIAN_POINT('Ctrl Pts',(-4.11622797217069,-22.1758088296598,
0.));
#226754=CARTESIAN_POINT('Ctrl Pts',(-4.11622797217069,-22.1758088296598,
12.));
#226755=CARTESIAN_POINT('Ctrl Pts',(-4.11653973150519,-22.177347426894,
0.));
#226756=CARTESIAN_POINT('Ctrl Pts',(-4.11653973150519,-22.177347426894,
12.));
#226757=CARTESIAN_POINT('Ctrl Pts',(-4.11694173195005,-22.179297473024,
0.));
#226758=CARTESIAN_POINT('Ctrl Pts',(-4.11694173195005,-22.179297473024,
12.));
#226759=CARTESIAN_POINT('Ctrl Pts',(-4.11743469691757,-22.1816414985788,
0.));
#226760=CARTESIAN_POINT('Ctrl Pts',(-4.11743469691757,-22.1816414985788,
12.));
#226761=CARTESIAN_POINT('Ctrl Pts',(-4.11801938107481,-22.1843613164855,
0.));
#226762=CARTESIAN_POINT('Ctrl Pts',(-4.11801938107481,-22.1843613164855,
12.));
#226763=CARTESIAN_POINT('Ctrl Pts',(-4.11869641271774,-22.1874419861496,
0.));
#226764=CARTESIAN_POINT('Ctrl Pts',(-4.11869641271774,-22.1874419861496,
12.));
#226765=CARTESIAN_POINT('Ctrl Pts',(-4.11946626228637,-22.1908725908525,
0.));
#226766=CARTESIAN_POINT('Ctrl Pts',(-4.11946626228637,-22.1908725908525,
12.));
#226767=CARTESIAN_POINT('Ctrl Pts',(-4.12032932637737,-22.1946440958098,
0.));
#226768=CARTESIAN_POINT('Ctrl Pts',(-4.12032932637737,-22.1946440958098,
12.));
#226769=CARTESIAN_POINT('Ctrl Pts',(-4.12128598183523,-22.1987479618246,
0.));
#226770=CARTESIAN_POINT('Ctrl Pts',(-4.12128598183523,-22.1987479618246,
12.));
#226771=CARTESIAN_POINT('Ctrl Pts',(-4.12233664408228,-22.2031746532106,
0.));
#226772=CARTESIAN_POINT('Ctrl Pts',(-4.12233664408228,-22.2031746532106,
12.));
#226773=CARTESIAN_POINT('Ctrl Pts',(-4.12348173702024,-22.2079143941719,
0.));
#226774=CARTESIAN_POINT('Ctrl Pts',(-4.12348173702024,-22.2079143941719,
12.));
#226775=CARTESIAN_POINT('Ctrl Pts',(-4.12472167516608,-22.2129576146671,
0.));
#226776=CARTESIAN_POINT('Ctrl Pts',(-4.12472167516608,-22.2129576146671,
12.));
#226777=CARTESIAN_POINT('Ctrl Pts',(-4.12605683613308,-22.2182956401341,
0.));
#226778=CARTESIAN_POINT('Ctrl Pts',(-4.12605683613308,-22.2182956401341,
12.));
#226779=CARTESIAN_POINT('Ctrl Pts',(-4.12748755830105,-22.2239207458781,
0.));
#226780=CARTESIAN_POINT('Ctrl Pts',(-4.12748755830105,-22.2239207458781,
12.));
#226781=CARTESIAN_POINT('Ctrl Pts',(-4.1290141546338,-22.2298258043947,
0.));
#226782=CARTESIAN_POINT('Ctrl Pts',(-4.1290141546338,-22.2298258043947,
12.));
#226783=CARTESIAN_POINT('Ctrl Pts',(-4.13063692157499,-22.2360040565533,
0.));
#226784=CARTESIAN_POINT('Ctrl Pts',(-4.13063692157499,-22.2360040565533,
12.));
#226785=CARTESIAN_POINT('Ctrl Pts',(-4.13235615060161,-22.2424488153523,
0.));
#226786=CARTESIAN_POINT('Ctrl Pts',(-4.13235615060161,-22.2424488153523,
12.));
#226787=CARTESIAN_POINT('Ctrl Pts',(-4.13417212558811,-22.249153531779,
0.));
#226788=CARTESIAN_POINT('Ctrl Pts',(-4.13417212558811,-22.249153531779,
12.));
#226789=CARTESIAN_POINT('Ctrl Pts',(-4.13608511977226,-22.2561118708421,
0.));
#226790=CARTESIAN_POINT('Ctrl Pts',(-4.13608511977226,-22.2561118708421,
12.));
#226791=CARTESIAN_POINT('Ctrl Pts',(-4.13809539255423,-22.2633177913972,
0.));
#226792=CARTESIAN_POINT('Ctrl Pts',(-4.13809539255423,-22.2633177913972,
12.));
#226793=CARTESIAN_POINT('Ctrl Pts',(-4.14020318715992,-22.2707656042457,
0.));
#226794=CARTESIAN_POINT('Ctrl Pts',(-4.14020318715992,-22.2707656042457,
12.));
#226795=CARTESIAN_POINT('Ctrl Pts',(-4.14240873321985,-22.2784499072027,
0.));
#226796=CARTESIAN_POINT('Ctrl Pts',(-4.14240873321985,-22.2784499072027,
12.));
#226797=CARTESIAN_POINT('Ctrl Pts',(-4.14471224859296,-22.2863655389166,
0.));
#226798=CARTESIAN_POINT('Ctrl Pts',(-4.14471224859296,-22.2863655389166,
12.));
#226799=CARTESIAN_POINT('Ctrl Pts',(-4.14711394168557,-22.2945075198467,
0.));
#226800=CARTESIAN_POINT('Ctrl Pts',(-4.14711394168557,-22.2945075198467,
12.));
#226801=CARTESIAN_POINT('Ctrl Pts',(-4.14961401285523,-22.3028710166933,
0.));
#226802=CARTESIAN_POINT('Ctrl Pts',(-4.14961401285523,-22.3028710166933,
12.));
#226803=CARTESIAN_POINT('Ctrl Pts',(-4.15221265396991,-22.3114513545185,
0.));
#226804=CARTESIAN_POINT('Ctrl Pts',(-4.15221265396991,-22.3114513545185,
12.));
#226805=CARTESIAN_POINT('Ctrl Pts',(-4.15491004835282,-22.320244018698,
0.));
#226806=CARTESIAN_POINT('Ctrl Pts',(-4.15491004835282,-22.320244018698,
12.));
#226807=CARTESIAN_POINT('Ctrl Pts',(-4.15770637047891,-22.3292446628959,
0.));
#226808=CARTESIAN_POINT('Ctrl Pts',(-4.15770637047891,-22.3292446628959,
12.));
#226809=CARTESIAN_POINT('Ctrl Pts',(-4.16060178604165,-22.3384491078602,
0.));
#226810=CARTESIAN_POINT('Ctrl Pts',(-4.16060178604165,-22.3384491078602,
12.));
#226811=CARTESIAN_POINT('Ctrl Pts',(-4.16359645263189,-22.3478533253889,
0.));
#226812=CARTESIAN_POINT('Ctrl Pts',(-4.16359645263189,-22.3478533253889,
12.));
#226813=CARTESIAN_POINT('Ctrl Pts',(-4.16669052026601,-22.3574534257396,
0.));
#226814=CARTESIAN_POINT('Ctrl Pts',(-4.16669052026601,-22.3574534257396,
12.));
#226815=CARTESIAN_POINT('Ctrl Pts',(-4.16988413199458,-22.36724564276,0.));
#226816=CARTESIAN_POINT('Ctrl Pts',(-4.16988413199458,-22.36724564276,12.));
#226817=CARTESIAN_POINT('Ctrl Pts',(-4.17317742436146,-22.3772263228617,
0.));
#226818=CARTESIAN_POINT('Ctrl Pts',(-4.17317742436146,-22.3772263228617,
12.));
#226819=CARTESIAN_POINT('Ctrl Pts',(-4.17657052752826,-22.3873919231334,
0.));
#226820=CARTESIAN_POINT('Ctrl Pts',(-4.17657052752826,-22.3873919231334,
12.));
#226821=CARTESIAN_POINT('Ctrl Pts',(-4.18006356544883,-22.3977390078075,
0.));
#226822=CARTESIAN_POINT('Ctrl Pts',(-4.18006356544883,-22.3977390078075,
12.));
#226823=CARTESIAN_POINT('Ctrl Pts',(-4.18365665600851,-22.4082642454453,
0.));
#226824=CARTESIAN_POINT('Ctrl Pts',(-4.18365665600851,-22.4082642454453,
12.));
#226825=CARTESIAN_POINT('Ctrl Pts',(-4.18734991117722,-22.4189644056115,
0.));
#226826=CARTESIAN_POINT('Ctrl Pts',(-4.18734991117722,-22.4189644056115,
12.));
#226827=CARTESIAN_POINT('Ctrl Pts',(-4.19114343726943,-22.4298363535421,
0.));
#226828=CARTESIAN_POINT('Ctrl Pts',(-4.19114343726943,-22.4298363535421,
12.));
#226829=CARTESIAN_POINT('Ctrl Pts',(-4.19503733518862,-22.4408770448917,
0.));
#226830=CARTESIAN_POINT('Ctrl Pts',(-4.19503733518862,-22.4408770448917,
12.));
#226831=CARTESIAN_POINT('Ctrl Pts',(-4.19903170066356,-22.4520835205419,
0.));
#226832=CARTESIAN_POINT('Ctrl Pts',(-4.19903170066356,-22.4520835205419,
12.));
#226833=CARTESIAN_POINT('Ctrl Pts',(-4.20312662448172,-22.4634529011433,
0.));
#226834=CARTESIAN_POINT('Ctrl Pts',(-4.20312662448172,-22.4634529011433,
12.));
#226835=CARTESIAN_POINT('Ctrl Pts',(-4.20732219265649,-22.4749823839915,
0.));
#226836=CARTESIAN_POINT('Ctrl Pts',(-4.20732219265649,-22.4749823839915,
12.));
#226837=CARTESIAN_POINT('Ctrl Pts',(-4.21161848657429,-22.4866692403147,
0.));
#226838=CARTESIAN_POINT('Ctrl Pts',(-4.21161848657429,-22.4866692403147,
12.));
#226839=CARTESIAN_POINT('Ctrl Pts',(-4.21601558313909,-22.4985108124229,
0.));
#226840=CARTESIAN_POINT('Ctrl Pts',(-4.21601558313909,-22.4985108124229,
12.));
#226841=CARTESIAN_POINT('Ctrl Pts',(-4.22051355490198,-22.5105045108882,
0.));
#226842=CARTESIAN_POINT('Ctrl Pts',(-4.22051355490198,-22.5105045108882,
12.));
#226843=CARTESIAN_POINT('Ctrl Pts',(-4.22511247020041,-22.5226478117885,
0.));
#226844=CARTESIAN_POINT('Ctrl Pts',(-4.22511247020041,-22.5226478117885,
12.));
#226845=CARTESIAN_POINT('Ctrl Pts',(-4.22981239330732,-22.5349382540587,
0.));
#226846=CARTESIAN_POINT('Ctrl Pts',(-4.22981239330732,-22.5349382540587,
12.));
#226847=CARTESIAN_POINT('Ctrl Pts',(-4.23461338456714,-22.5473734368086,
0.));
#226848=CARTESIAN_POINT('Ctrl Pts',(-4.23461338456714,-22.5473734368086,
12.));
#226849=CARTESIAN_POINT('Ctrl Pts',(-4.23951550052527,-22.559951016643,
0.));
#226850=CARTESIAN_POINT('Ctrl Pts',(-4.23951550052527,-22.559951016643,
12.));
#226851=CARTESIAN_POINT('Ctrl Pts',(-4.2445187940486,-22.5726687049922,
0.));
#226852=CARTESIAN_POINT('Ctrl Pts',(-4.2445187940486,-22.5726687049922,
12.));
#226853=CARTESIAN_POINT('Ctrl Pts',(-4.24962331444186,-22.5855242662479,
0.));
#226854=CARTESIAN_POINT('Ctrl Pts',(-4.24962331444186,-22.5855242662479,
12.));
#226855=CARTESIAN_POINT('Ctrl Pts',(-4.25482910755486,-22.5985155158637,
0.));
#226856=CARTESIAN_POINT('Ctrl Pts',(-4.25482910755486,-22.5985155158637,
12.));
#226857=CARTESIAN_POINT('Ctrl Pts',(-4.26013621588304,-22.611640318482,
0.));
#226858=CARTESIAN_POINT('Ctrl Pts',(-4.26013621588304,-22.611640318482,
12.));
#226859=CARTESIAN_POINT('Ctrl Pts',(-4.26554467865572,-22.6248965859975,
0.));
#226860=CARTESIAN_POINT('Ctrl Pts',(-4.26554467865572,-22.6248965859975,
12.));
#226861=CARTESIAN_POINT('Ctrl Pts',(-4.27105453193,-22.6382822758171,0.));
#226862=CARTESIAN_POINT('Ctrl Pts',(-4.27105453193,-22.6382822758171,12.));
#226863=CARTESIAN_POINT('Ctrl Pts',(-4.27666580869118,-22.6517953893303,
0.));
#226864=CARTESIAN_POINT('Ctrl Pts',(-4.27666580869118,-22.6517953893303,
12.));
#226865=CARTESIAN_POINT('Ctrl Pts',(-4.2823785389406,-22.665433970311,0.));
#226866=CARTESIAN_POINT('Ctrl Pts',(-4.2823785389406,-22.665433970311,12.));
#226867=CARTESIAN_POINT('Ctrl Pts',(-4.28819274977767,-22.6791961033536,
0.));
#226868=CARTESIAN_POINT('Ctrl Pts',(-4.28819274977767,-22.6791961033536,
12.));
#226869=CARTESIAN_POINT('Ctrl Pts',(-4.29410846547062,-22.6930799122545,
0.));
#226870=CARTESIAN_POINT('Ctrl Pts',(-4.29410846547062,-22.6930799122545,
12.));
#226871=CARTESIAN_POINT('Ctrl Pts',(-4.30012570754067,-22.707083558756,
0.));
#226872=CARTESIAN_POINT('Ctrl Pts',(-4.30012570754067,-22.707083558756,
12.));
#226873=CARTESIAN_POINT('Ctrl Pts',(-4.30624449484075,-22.7212052413384,
0.));
#226874=CARTESIAN_POINT('Ctrl Pts',(-4.30624449484075,-22.7212052413384,
12.));
#226875=CARTESIAN_POINT('Ctrl Pts',(-4.31246484362551,-22.7354431939926,
0.));
#226876=CARTESIAN_POINT('Ctrl Pts',(-4.31246484362551,-22.7354431939926,
12.));
#226877=CARTESIAN_POINT('Ctrl Pts',(-4.31878676761231,-22.7497956849852,
0.));
#226878=CARTESIAN_POINT('Ctrl Pts',(-4.31878676761231,-22.7497956849852,
12.));
#226879=CARTESIAN_POINT('Ctrl Pts',(-4.32521027803748,-22.764261015648,
0.));
#226880=CARTESIAN_POINT('Ctrl Pts',(-4.32521027803748,-22.764261015648,
12.));
#226881=CARTESIAN_POINT('Ctrl Pts',(-4.33173538373183,-22.7788375194081,
0.));
#226882=CARTESIAN_POINT('Ctrl Pts',(-4.33173538373183,-22.7788375194081,
12.));
#226883=CARTESIAN_POINT('Ctrl Pts',(-4.33836209118444,-22.7935235607807,
0.));
#226884=CARTESIAN_POINT('Ctrl Pts',(-4.33836209118444,-22.7935235607807,
12.));
#226885=CARTESIAN_POINT('Ctrl Pts',(-4.34509040460066,-22.808317534379,
0.));
#226886=CARTESIAN_POINT('Ctrl Pts',(-4.34509040460066,-22.808317534379,
12.));
#226887=CARTESIAN_POINT('Ctrl Pts',(-4.35192032594802,-22.8232178638873,
0.));
#226888=CARTESIAN_POINT('Ctrl Pts',(-4.35192032594802,-22.8232178638873,
12.));
#226889=CARTESIAN_POINT('Ctrl Pts',(-4.3588518550056,-22.838223001118,0.));
#226890=CARTESIAN_POINT('Ctrl Pts',(-4.3588518550056,-22.838223001118,12.));
#226891=CARTESIAN_POINT('Ctrl Pts',(-4.36588498943011,-22.8533314252419,
0.));
#226892=CARTESIAN_POINT('Ctrl Pts',(-4.36588498943011,-22.8533314252419,
12.));
#226893=CARTESIAN_POINT('Ctrl Pts',(-4.37301972480753,-22.8685416419725,
0.));
#226894=CARTESIAN_POINT('Ctrl Pts',(-4.37301972480753,-22.8685416419725,
12.));
#226895=CARTESIAN_POINT('Ctrl Pts',(-4.38025605470091,-22.8838521827702,
0.));
#226896=CARTESIAN_POINT('Ctrl Pts',(-4.38025605470091,-22.8838521827702,
12.));
#226897=CARTESIAN_POINT('Ctrl Pts',(-4.38759397068393,-22.8992616040108,
0.));
#226898=CARTESIAN_POINT('Ctrl Pts',(-4.38759397068393,-22.8992616040108,
12.));
#226899=CARTESIAN_POINT('Ctrl Pts',(-4.39503346238455,-22.9147684862425,
0.));
#226900=CARTESIAN_POINT('Ctrl Pts',(-4.39503346238455,-22.9147684862425,
12.));
#226901=CARTESIAN_POINT('Ctrl Pts',(-4.40257451754308,-22.9303714335549,
0.));
#226902=CARTESIAN_POINT('Ctrl Pts',(-4.40257451754308,-22.9303714335549,
12.));
#226903=CARTESIAN_POINT('Ctrl Pts',(-4.41021712205549,-22.9460690729093,
0.));
#226904=CARTESIAN_POINT('Ctrl Pts',(-4.41021712205549,-22.9460690729093,
12.));
#226905=CARTESIAN_POINT('Ctrl Pts',(-4.41796126001311,-22.9618600534866,
0.));
#226906=CARTESIAN_POINT('Ctrl Pts',(-4.41796126001311,-22.9618600534866,
12.));
#226907=CARTESIAN_POINT('Ctrl Pts',(-4.42580691372772,-22.9777430460021,
0.));
#226908=CARTESIAN_POINT('Ctrl Pts',(-4.42580691372772,-22.9777430460021,
12.));
#226909=CARTESIAN_POINT('Ctrl Pts',(-4.43375406376906,-22.9937167421009,
0.));
#226910=CARTESIAN_POINT('Ctrl Pts',(-4.43375406376906,-22.9937167421009,
12.));
#226911=CARTESIAN_POINT('Ctrl Pts',(-4.44180268901667,-23.0097798538399,
0.));
#226912=CARTESIAN_POINT('Ctrl Pts',(-4.44180268901667,-23.0097798538399,
12.));
#226913=CARTESIAN_POINT('Ctrl Pts',(-4.44995276669699,-23.0259311131395,
0.));
#226914=CARTESIAN_POINT('Ctrl Pts',(-4.44995276669699,-23.0259311131395,
12.));
#226915=CARTESIAN_POINT('Ctrl Pts',(-4.45820427241677,-23.0421692712466,
0.));
#226916=CARTESIAN_POINT('Ctrl Pts',(-4.45820427241677,-23.0421692712466,
12.));
#226917=CARTESIAN_POINT('Ctrl Pts',(-4.46655718018206,-23.0584930981723,
0.));
#226918=CARTESIAN_POINT('Ctrl Pts',(-4.46655718018206,-23.0584930981723,
12.));
#226919=CARTESIAN_POINT('Ctrl Pts',(-4.47501146242822,-23.0749013821867,
0.));
#226920=CARTESIAN_POINT('Ctrl Pts',(-4.47501146242822,-23.0749013821867,
12.));
#226921=CARTESIAN_POINT('Ctrl Pts',(-4.48356709006757,-23.0913929293909,
0.));
#226922=CARTESIAN_POINT('Ctrl Pts',(-4.48356709006757,-23.0913929293909,
12.));
#226923=CARTESIAN_POINT('Ctrl Pts',(-4.49222403252202,-23.1079665632629,
0.));
#226924=CARTESIAN_POINT('Ctrl Pts',(-4.49222403252202,-23.1079665632629,
12.));
#226925=CARTESIAN_POINT('Ctrl Pts',(-4.50098225775179,-23.1246211242117,
0.));
#226926=CARTESIAN_POINT('Ctrl Pts',(-4.50098225775179,-23.1246211242117,
12.));
#226927=CARTESIAN_POINT('Ctrl Pts',(-4.50984173227088,-23.1413554691136,
0.));
#226928=CARTESIAN_POINT('Ctrl Pts',(-4.50984173227088,-23.1413554691136,
12.));
#226929=CARTESIAN_POINT('Ctrl Pts',(-4.51880242116786,-23.1581684708778,
0.));
#226930=CARTESIAN_POINT('Ctrl Pts',(-4.51880242116786,-23.1581684708778,
12.));
#226931=CARTESIAN_POINT('Ctrl Pts',(-4.52786428815049,-23.1750590180923,
0.));
#226932=CARTESIAN_POINT('Ctrl Pts',(-4.52786428815049,-23.1750590180923,
12.));
#226933=CARTESIAN_POINT('Ctrl Pts',(-4.53702729557586,-23.1920260146474,
0.));
#226934=CARTESIAN_POINT('Ctrl Pts',(-4.53702729557586,-23.1920260146474,
12.));
#226935=CARTESIAN_POINT('Ctrl Pts',(-4.54629140447543,-23.2090683793627,
0.));
#226936=CARTESIAN_POINT('Ctrl Pts',(-4.54629140447543,-23.2090683793627,
12.));
#226937=CARTESIAN_POINT('Ctrl Pts',(-4.55565657456957,-23.2261850456055,
0.));
#226938=CARTESIAN_POINT('Ctrl Pts',(-4.55565657456957,-23.2261850456055,
12.));
#226939=CARTESIAN_POINT('Ctrl Pts',(-4.56512276427812,-23.2433749609117,
0.));
#226940=CARTESIAN_POINT('Ctrl Pts',(-4.56512276427812,-23.2433749609117,
12.));
#226941=CARTESIAN_POINT('Ctrl Pts',(-4.57468993076071,-23.2606370866854,
0.));
#226942=CARTESIAN_POINT('Ctrl Pts',(-4.57468993076071,-23.2606370866854,
12.));
#226943=CARTESIAN_POINT('Ctrl Pts',(-4.58435802994675,-23.2779703978868,
0.));
#226944=CARTESIAN_POINT('Ctrl Pts',(-4.58435802994675,-23.2779703978868,
12.));
#226945=CARTESIAN_POINT('Ctrl Pts',(-4.5941270165575,-23.295373882719,0.));
#226946=CARTESIAN_POINT('Ctrl Pts',(-4.5941270165575,-23.295373882719,12.));
#226947=CARTESIAN_POINT('Ctrl Pts',(-4.60399684412176,-23.3128465423119,
0.));
#226948=CARTESIAN_POINT('Ctrl Pts',(-4.60399684412176,-23.3128465423119,
12.));
#226949=CARTESIAN_POINT('Ctrl Pts',(-4.61396746497849,-23.3303873903947,
0.));
#226950=CARTESIAN_POINT('Ctrl Pts',(-4.61396746497849,-23.3303873903947,
12.));
#226951=CARTESIAN_POINT('Ctrl Pts',(-4.62403883030825,-23.3479954530281,
0.));
#226952=CARTESIAN_POINT('Ctrl Pts',(-4.62403883030825,-23.3479954530281,
12.));
#226953=CARTESIAN_POINT('Ctrl Pts',(-4.63421089016555,-23.3656697683496,
0.));
#226954=CARTESIAN_POINT('Ctrl Pts',(-4.63421089016555,-23.3656697683496,
12.));
#226955=CARTESIAN_POINT('Ctrl Pts',(-4.64448359349936,-23.383409386307,
0.));
#226956=CARTESIAN_POINT('Ctrl Pts',(-4.64448359349936,-23.383409386307,
12.));
#226957=CARTESIAN_POINT('Ctrl Pts',(-4.65485688816923,-23.4012133683957,
0.));
#226958=CARTESIAN_POINT('Ctrl Pts',(-4.65485688816923,-23.4012133683957,
12.));
#226959=CARTESIAN_POINT('Ctrl Pts',(-4.66533072094664,-23.4190807873798,
0.));
#226960=CARTESIAN_POINT('Ctrl Pts',(-4.66533072094664,-23.4190807873798,
12.));
#226961=CARTESIAN_POINT('Ctrl Pts',(-4.67590503753051,-23.4370107270444,
0.));
#226962=CARTESIAN_POINT('Ctrl Pts',(-4.67590503753051,-23.4370107270444,
12.));
#226963=CARTESIAN_POINT('Ctrl Pts',(-4.68657978258298,-23.4550022819852,
0.));
#226964=CARTESIAN_POINT('Ctrl Pts',(-4.68657978258298,-23.4550022819852,
12.));
#226965=CARTESIAN_POINT('Ctrl Pts',(-4.69735489975024,-23.4730545573849,
0.));
#226966=CARTESIAN_POINT('Ctrl Pts',(-4.69735489975024,-23.4730545573849,
12.));
#226967=CARTESIAN_POINT('Ctrl Pts',(-4.70823033167821,-23.491166668789,
0.));
#226968=CARTESIAN_POINT('Ctrl Pts',(-4.70823033167821,-23.491166668789,
12.));
#226969=CARTESIAN_POINT('Ctrl Pts',(-4.71920602001905,-23.5093377418784,
0.));
#226970=CARTESIAN_POINT('Ctrl Pts',(-4.71920602001905,-23.5093377418784,
12.));
#226971=CARTESIAN_POINT('Ctrl Pts',(-4.73028190543032,-23.5275669122378,
0.));
#226972=CARTESIAN_POINT('Ctrl Pts',(-4.73028190543032,-23.5275669122378,
12.));
#226973=CARTESIAN_POINT('Ctrl Pts',(-4.74145792760699,-23.5458533251715,
0.));
#226974=CARTESIAN_POINT('Ctrl Pts',(-4.74145792760699,-23.5458533251715,
12.));
#226975=CARTESIAN_POINT('Ctrl Pts',(-4.75273402530616,-23.564196135517,
0.));
#226976=CARTESIAN_POINT('Ctrl Pts',(-4.75273402530616,-23.564196135517,
12.));
#226977=CARTESIAN_POINT('Ctrl Pts',(-4.76411013636252,-23.5825945074535,
0.));
#226978=CARTESIAN_POINT('Ctrl Pts',(-4.76411013636252,-23.5825945074535,
12.));
#226979=CARTESIAN_POINT('Ctrl Pts',(-4.77558619769876,-23.6010476143099,
0.));
#226980=CARTESIAN_POINT('Ctrl Pts',(-4.77558619769876,-23.6010476143099,
12.));
#226981=CARTESIAN_POINT('Ctrl Pts',(-4.78716214532105,-23.6195546383625,
0.));
#226982=CARTESIAN_POINT('Ctrl Pts',(-4.78716214532105,-23.6195546383625,
12.));
#226983=CARTESIAN_POINT('Ctrl Pts',(-4.79883791433231,-23.6381147706581,
0.));
#226984=CARTESIAN_POINT('Ctrl Pts',(-4.79883791433231,-23.6381147706581,
12.));
#226985=CARTESIAN_POINT('Ctrl Pts',(-4.81061343896443,-23.6567272108631,
0.));
#226986=CARTESIAN_POINT('Ctrl Pts',(-4.81061343896443,-23.6567272108631,
12.));
#226987=CARTESIAN_POINT('Ctrl Pts',(-4.82248865259571,-23.6753911671023,
0.));
#226988=CARTESIAN_POINT('Ctrl Pts',(-4.82248865259571,-23.6753911671023,
12.));
#226989=CARTESIAN_POINT('Ctrl Pts',(-4.83446348776268,-23.6941058557971,
0.));
#226990=CARTESIAN_POINT('Ctrl Pts',(-4.83446348776268,-23.6941058557971,
12.));
#226991=CARTESIAN_POINT('Ctrl Pts',(-4.84653787616424,-23.7128705015014,
0.));
#226992=CARTESIAN_POINT('Ctrl Pts',(-4.84653787616424,-23.7128705015014,
12.));
#226993=CARTESIAN_POINT('Ctrl Pts',(-4.85871174865492,-23.7316843367308,
0.));
#226994=CARTESIAN_POINT('Ctrl Pts',(-4.85871174865492,-23.7316843367308,
12.));
#226995=CARTESIAN_POINT('Ctrl Pts',(-4.87098503527144,-23.7505466018239,
0.));
#226996=CARTESIAN_POINT('Ctrl Pts',(-4.87098503527144,-23.7505466018239,
12.));
#226997=CARTESIAN_POINT('Ctrl Pts',(-4.88335766525566,-23.7694565448044,
0.));
#226998=CARTESIAN_POINT('Ctrl Pts',(-4.88335766525566,-23.7694565448044,
12.));
#226999=CARTESIAN_POINT('Ctrl Pts',(-4.89582956706772,-23.7884134212381,
0.));
#227000=CARTESIAN_POINT('Ctrl Pts',(-4.89582956706772,-23.7884134212381,
12.));
#227001=CARTESIAN_POINT('Ctrl Pts',(-4.90840066839348,-23.8074164940897,
0.));
#227002=CARTESIAN_POINT('Ctrl Pts',(-4.90840066839348,-23.8074164940897,
12.));
#227003=CARTESIAN_POINT('Ctrl Pts',(-4.92107089613977,-23.8264650335721,
0.));
#227004=CARTESIAN_POINT('Ctrl Pts',(-4.92107089613977,-23.8264650335721,
12.));
#227005=CARTESIAN_POINT('Ctrl Pts',(-4.93384017643442,-23.8455583170062,
0.));
#227006=CARTESIAN_POINT('Ctrl Pts',(-4.93384017643442,-23.8455583170062,
12.));
#227007=CARTESIAN_POINT('Ctrl Pts',(-4.94670843465869,-23.8646956287172,
0.));
#227008=CARTESIAN_POINT('Ctrl Pts',(-4.94670843465869,-23.8646956287172,
12.));
#227009=CARTESIAN_POINT('Ctrl Pts',(-4.95967559546566,-23.883876259922,
0.));
#227010=CARTESIAN_POINT('Ctrl Pts',(-4.95967559546566,-23.883876259922,
12.));
#227011=CARTESIAN_POINT('Ctrl Pts',(-4.9727415827923,-23.9030995086164,
0.));
#227012=CARTESIAN_POINT('Ctrl Pts',(-4.9727415827923,-23.9030995086164,
12.));
#227013=CARTESIAN_POINT('Ctrl Pts',(-4.98590631986534,-23.9223646794591,
0.));
#227014=CARTESIAN_POINT('Ctrl Pts',(-4.98590631986534,-23.9223646794591,
12.));
#227015=CARTESIAN_POINT('Ctrl Pts',(-4.9991697291931,-23.9416710836529,
0.));
#227016=CARTESIAN_POINT('Ctrl Pts',(-4.9991697291931,-23.9416710836529,
12.));
#227017=CARTESIAN_POINT('Ctrl Pts',(-5.01253173257459,-23.9610180388271,
0.));
#227018=CARTESIAN_POINT('Ctrl Pts',(-5.01253173257459,-23.9610180388271,
12.));
#227019=CARTESIAN_POINT('Ctrl Pts',(-5.02599225112462,-23.9804048689228,
0.));
#227020=CARTESIAN_POINT('Ctrl Pts',(-5.02599225112462,-23.9804048689228,
12.));
#227021=CARTESIAN_POINT('Ctrl Pts',(-5.03955120528528,-23.9998309040747,
0.));
#227022=CARTESIAN_POINT('Ctrl Pts',(-5.03955120528528,-23.9998309040747,
12.));
#227023=CARTESIAN_POINT('Ctrl Pts',(-5.05320851483069,-24.0192954804896,
0.));
#227024=CARTESIAN_POINT('Ctrl Pts',(-5.05320851483069,-24.0192954804896,
12.));
#227025=CARTESIAN_POINT('Ctrl Pts',(-5.0669640988664,-24.0387979403268,
0.));
#227026=CARTESIAN_POINT('Ctrl Pts',(-5.0669640988664,-24.0387979403268,
12.));
#227027=CARTESIAN_POINT('Ctrl Pts',(-5.08081787581271,-24.0583376315636,
0.));
#227028=CARTESIAN_POINT('Ctrl Pts',(-5.08081787581271,-24.0583376315636,
12.));
#227029=CARTESIAN_POINT('Ctrl Pts',(-5.09476976342618,-24.0779139079264,
0.));
#227030=CARTESIAN_POINT('Ctrl Pts',(-5.09476976342618,-24.0779139079264,
12.));
#227031=CARTESIAN_POINT('Ctrl Pts',(-5.10881967883126,-24.0975261288444,
0.));
#227032=CARTESIAN_POINT('Ctrl Pts',(-5.10881967883126,-24.0975261288444,
12.));
#227033=CARTESIAN_POINT('Ctrl Pts',(-5.12296753853858,-24.117173659394,
0.));
#227034=CARTESIAN_POINT('Ctrl Pts',(-5.12296753853858,-24.117173659394,
12.));
#227035=CARTESIAN_POINT('Ctrl Pts',(-5.13721325845746,-24.1368558702443,
0.));
#227036=CARTESIAN_POINT('Ctrl Pts',(-5.13721325845746,-24.1368558702443,
12.));
#227037=CARTESIAN_POINT('Ctrl Pts',(-5.1515567539008,-24.1565721375971,
0.));
#227038=CARTESIAN_POINT('Ctrl Pts',(-5.1515567539008,-24.1565721375971,
12.));
#227039=CARTESIAN_POINT('Ctrl Pts',(-5.16599793957987,-24.1763218431344,
0.));
#227040=CARTESIAN_POINT('Ctrl Pts',(-5.16599793957987,-24.1763218431344,
12.));
#227041=CARTESIAN_POINT('Ctrl Pts',(-5.180536729614,-24.1961043738756,0.));
#227042=CARTESIAN_POINT('Ctrl Pts',(-5.180536729614,-24.1961043738756,12.));
#227043=CARTESIAN_POINT('Ctrl Pts',(-5.19517303753648,-24.2159191220171,
0.));
#227044=CARTESIAN_POINT('Ctrl Pts',(-5.19517303753648,-24.2159191220171,
12.));
#227045=CARTESIAN_POINT('Ctrl Pts',(-5.20990677629177,-24.2357654847766,
0.));
#227046=CARTESIAN_POINT('Ctrl Pts',(-5.20990677629177,-24.2357654847766,
12.));
#227047=CARTESIAN_POINT('Ctrl Pts',(-5.22473785822443,-24.2556428642294,
0.));
#227048=CARTESIAN_POINT('Ctrl Pts',(-5.22473785822443,-24.2556428642294,
12.));
#227049=CARTESIAN_POINT('Ctrl Pts',(-5.2396661950629,-24.2755506671525,
0.));
#227050=CARTESIAN_POINT('Ctrl Pts',(-5.2396661950629,-24.2755506671525,
12.));
#227051=CARTESIAN_POINT('Ctrl Pts',(-5.25469169788857,-24.2954883048447,
0.));
#227052=CARTESIAN_POINT('Ctrl Pts',(-5.25469169788857,-24.2954883048447,
12.));
#227053=CARTESIAN_POINT('Ctrl Pts',(-5.269814277188,-24.3154551932221,0.));
#227054=CARTESIAN_POINT('Ctrl Pts',(-5.269814277188,-24.3154551932221,12.));
#227055=CARTESIAN_POINT('Ctrl Pts',(-5.28503384290649,-24.3354507529414,
0.));
#227056=CARTESIAN_POINT('Ctrl Pts',(-5.28503384290649,-24.3354507529414,
12.));
#227057=CARTESIAN_POINT('Ctrl Pts',(-5.30035030449064,-24.3554744095075,
0.));
#227058=CARTESIAN_POINT('Ctrl Pts',(-5.30035030449064,-24.3554744095075,
12.));
#227059=CARTESIAN_POINT('Ctrl Pts',(-5.31576357092527,-24.3755255933917,
0.));
#227060=CARTESIAN_POINT('Ctrl Pts',(-5.31576357092527,-24.3755255933917,
12.));
#227061=CARTESIAN_POINT('Ctrl Pts',(-5.33127355076035,-24.3956037401293,
0.));
#227062=CARTESIAN_POINT('Ctrl Pts',(-5.33127355076035,-24.3956037401293,
12.));
#227063=CARTESIAN_POINT('Ctrl Pts',(-5.34688015213538,-24.4157082904614,
0.));
#227064=CARTESIAN_POINT('Ctrl Pts',(-5.34688015213538,-24.4157082904614,
12.));
#227065=CARTESIAN_POINT('Ctrl Pts',(-5.36258328273628,-24.435838689915,
0.));
#227066=CARTESIAN_POINT('Ctrl Pts',(-5.36258328273628,-24.435838689915,
12.));
#227067=CARTESIAN_POINT('Ctrl Pts',(-5.37838284973696,-24.4559943883157,
0.));
#227068=CARTESIAN_POINT('Ctrl Pts',(-5.37838284973696,-24.4559943883157,
12.));
#227069=CARTESIAN_POINT('Ctrl Pts',(-5.39427875973825,-24.4761748393321,
0.));
#227070=CARTESIAN_POINT('Ctrl Pts',(-5.39427875973825,-24.4761748393321,
12.));
#227071=CARTESIAN_POINT('Ctrl Pts',(-5.41027091869242,-24.496379499983,
0.));
#227072=CARTESIAN_POINT('Ctrl Pts',(-5.41027091869242,-24.496379499983,
12.));
#227073=CARTESIAN_POINT('Ctrl Pts',(-5.4263592318342,-24.5166078302108,
0.));
#227074=CARTESIAN_POINT('Ctrl Pts',(-5.4263592318342,-24.5166078302108,
12.));
#227075=CARTESIAN_POINT('Ctrl Pts',(-5.44254360356881,-24.5368592922863,
0.));
#227076=CARTESIAN_POINT('Ctrl Pts',(-5.44254360356881,-24.5368592922863,
12.));
#227077=CARTESIAN_POINT('Ctrl Pts',(-5.45882393762262,-24.5571333514842,
0.));
#227078=CARTESIAN_POINT('Ctrl Pts',(-5.45882393762262,-24.5571333514842,
12.));
#227079=CARTESIAN_POINT('Ctrl Pts',(-5.4752001372442,-24.5774294770329,
0.));
#227080=CARTESIAN_POINT('Ctrl Pts',(-5.4752001372442,-24.5774294770329,
12.));
#227081=CARTESIAN_POINT('Ctrl Pts',(-5.49167210537248,-24.5977471429364,
0.));
#227082=CARTESIAN_POINT('Ctrl Pts',(-5.49167210537248,-24.5977471429364,
12.));
#227083=CARTESIAN_POINT('Ctrl Pts',(-5.50823974481963,-24.6180858289179,
0.));
#227084=CARTESIAN_POINT('Ctrl Pts',(-5.50823974481963,-24.6180858289179,
12.));
#227085=CARTESIAN_POINT('Ctrl Pts',(-5.52490295840993,-24.6384450211467,
0.));
#227086=CARTESIAN_POINT('Ctrl Pts',(-5.52490295840993,-24.6384450211467,
12.));
#227087=CARTESIAN_POINT('Ctrl Pts',(-5.54166164919584,-24.6588242134738,
0.));
#227088=CARTESIAN_POINT('Ctrl Pts',(-5.54166164919584,-24.6588242134738,
12.));
#227089=CARTESIAN_POINT('Ctrl Pts',(-5.55851572025377,-24.6792229061794,
0.));
#227090=CARTESIAN_POINT('Ctrl Pts',(-5.55851572025377,-24.6792229061794,
12.));
#227091=CARTESIAN_POINT('Ctrl Pts',(-5.57546507427756,-24.6996406035517,
0.));
#227092=CARTESIAN_POINT('Ctrl Pts',(-5.57546507427756,-24.6996406035517,
12.));
#227093=CARTESIAN_POINT('Ctrl Pts',(-5.59250961323988,-24.7200768119088,
0.));
#227094=CARTESIAN_POINT('Ctrl Pts',(-5.59250961323988,-24.7200768119088,
12.));
#227095=CARTESIAN_POINT('Ctrl Pts',(-5.60964923798492,-24.7405310372739,
0.));
#227096=CARTESIAN_POINT('Ctrl Pts',(-5.60964923798492,-24.7405310372739,
12.));
#227097=CARTESIAN_POINT('Ctrl Pts',(-5.62688384790924,-24.7610027835697,
0.));
#227098=CARTESIAN_POINT('Ctrl Pts',(-5.62688384790924,-24.7610027835697,
12.));
#227099=CARTESIAN_POINT('Ctrl Pts',(-5.64421334042262,-24.781491549672,
0.));
#227100=CARTESIAN_POINT('Ctrl Pts',(-5.64421334042262,-24.781491549672,
12.));
#227101=CARTESIAN_POINT('Ctrl Pts',(-5.66163761114922,-24.8019968304605,
0.));
#227102=CARTESIAN_POINT('Ctrl Pts',(-5.66163761114922,-24.8019968304605,
12.));
#227103=CARTESIAN_POINT('Ctrl Pts',(-5.67915655496543,-24.8225181223845,
0.));
#227104=CARTESIAN_POINT('Ctrl Pts',(-5.67915655496543,-24.8225181223845,
12.));
#227105=CARTESIAN_POINT('Ctrl Pts',(-5.69677006679445,-24.8430549277621,
0.));
#227106=CARTESIAN_POINT('Ctrl Pts',(-5.69677006679445,-24.8430549277621,
12.));
#227107=CARTESIAN_POINT('Ctrl Pts',(-5.71447804252028,-24.8636067597669,
0.));
#227108=CARTESIAN_POINT('Ctrl Pts',(-5.71447804252028,-24.8636067597669,
12.));
#227109=CARTESIAN_POINT('Ctrl Pts',(-5.73228037976928,-24.884173146722,
0.));
#227110=CARTESIAN_POINT('Ctrl Pts',(-5.73228037976928,-24.884173146722,
12.));
#227111=CARTESIAN_POINT('Ctrl Pts',(-5.75017697890805,-24.904753637648,
0.));
#227112=CARTESIAN_POINT('Ctrl Pts',(-5.75017697890805,-24.904753637648,
12.));
#227113=CARTESIAN_POINT('Ctrl Pts',(-5.76816774342221,-24.9253478043656,
0.));
#227114=CARTESIAN_POINT('Ctrl Pts',(-5.76816774342221,-24.9253478043656,
12.));
#227115=CARTESIAN_POINT('Ctrl Pts',(-5.78625257775682,-24.945955229334,
0.));
#227116=CARTESIAN_POINT('Ctrl Pts',(-5.78625257775682,-24.945955229334,
12.));
#227117=CARTESIAN_POINT('Ctrl Pts',(-5.80443138549727,-24.9665754954496,
0.));
#227118=CARTESIAN_POINT('Ctrl Pts',(-5.80443138549727,-24.9665754954496,
12.));
#227119=CARTESIAN_POINT('Ctrl Pts',(-5.822704067442,-24.9872081752734,0.));
#227120=CARTESIAN_POINT('Ctrl Pts',(-5.822704067442,-24.9872081752734,12.));
#227121=CARTESIAN_POINT('Ctrl Pts',(-5.84107051963072,-25.0078528200564,
0.));
#227122=CARTESIAN_POINT('Ctrl Pts',(-5.84107051963072,-25.0078528200564,
12.));
#227123=CARTESIAN_POINT('Ctrl Pts',(-5.85953063156827,-25.0285089498899,
0.));
#227124=CARTESIAN_POINT('Ctrl Pts',(-5.85953063156827,-25.0285089498899,
12.));
#227125=CARTESIAN_POINT('Ctrl Pts',(-5.87808428385367,-25.049176040591,
0.));
#227126=CARTESIAN_POINT('Ctrl Pts',(-5.87808428385367,-25.049176040591,
12.));
#227127=CARTESIAN_POINT('Ctrl Pts',(-5.89673135155515,-25.0698535426514,
0.));
#227128=CARTESIAN_POINT('Ctrl Pts',(-5.89673135155515,-25.0698535426514,
12.));
#227129=CARTESIAN_POINT('Ctrl Pts',(-5.91547170844448,-25.0905409050773,
0.));
#227130=CARTESIAN_POINT('Ctrl Pts',(-5.91547170844448,-25.0905409050773,
12.));
#227131=CARTESIAN_POINT('Ctrl Pts',(-5.93430523086836,-25.1112375971106,
0.));
#227132=CARTESIAN_POINT('Ctrl Pts',(-5.93430523086836,-25.1112375971106,
12.));
#227133=CARTESIAN_POINT('Ctrl Pts',(-5.95323180187379,-25.1319431317237,
0.));
#227134=CARTESIAN_POINT('Ctrl Pts',(-5.95323180187379,-25.1319431317237,
12.));
#227135=CARTESIAN_POINT('Ctrl Pts',(-5.97225131495618,-25.1526570863092,
0.));
#227136=CARTESIAN_POINT('Ctrl Pts',(-5.97225131495618,-25.1526570863092,
12.));
#227137=CARTESIAN_POINT('Ctrl Pts',(-5.99136367859755,-25.1733791296259,
0.));
#227138=CARTESIAN_POINT('Ctrl Pts',(-5.99136367859755,-25.1733791296259,
12.));
#227139=CARTESIAN_POINT('Ctrl Pts',(-6.01056881804614,-25.1941090269819,
0.));
#227140=CARTESIAN_POINT('Ctrl Pts',(-6.01056881804614,-25.1941090269819,
12.));
#227141=CARTESIAN_POINT('Ctrl Pts',(-6.02986667389998,-25.21484662016,0.));
#227142=CARTESIAN_POINT('Ctrl Pts',(-6.02986667389998,-25.21484662016,12.));
#227143=CARTESIAN_POINT('Ctrl Pts',(-6.04925720151219,-25.2355918139032,
0.));
#227144=CARTESIAN_POINT('Ctrl Pts',(-6.04925720151219,-25.2355918139032,
12.));
#227145=CARTESIAN_POINT('Ctrl Pts',(-6.06484373634547,-25.2521940105705,
0.));
#227146=CARTESIAN_POINT('Ctrl Pts',(-6.06484373634547,-25.2521940105705,
12.));
#227147=CARTESIAN_POINT('Ctrl Pts',(-6.07657531787491,-25.2646490489922,
0.));
#227148=CARTESIAN_POINT('Ctrl Pts',(-6.07657531787491,-25.2646490489922,
12.));
#227149=CARTESIAN_POINT('Ctrl Pts',(-6.08441489609794,-25.2729539149517,
0.));
#227150=CARTESIAN_POINT('Ctrl Pts',(-6.08441489609794,-25.2729539149517,
12.));
#227151=CARTESIAN_POINT('Ctrl Pts',(-6.088339316177,-25.2771067246846,0.));
#227152=CARTESIAN_POINT('Ctrl Pts',(-6.088339316177,-25.2771067246846,12.));
#227153=CARTESIAN_POINT('',(-6.088339316177,-25.2771067246846,0.));
#227154=CARTESIAN_POINT('Ctrl Pts',(-4.11585220600463,-22.1738711152697,
0.));
#227155=CARTESIAN_POINT('Ctrl Pts',(-4.11585194677443,-22.173877682324,
0.));
#227156=CARTESIAN_POINT('Ctrl Pts',(-4.11586035878288,-22.1739341411687,
0.));
#227157=CARTESIAN_POINT('Ctrl Pts',(-4.11589976826167,-22.1741488021234,
0.));
#227158=CARTESIAN_POINT('Ctrl Pts',(-4.11600589882846,-22.1746949858775,
0.));
#227159=CARTESIAN_POINT('Ctrl Pts',(-4.11622797217069,-22.1758088296598,
0.));
#227160=CARTESIAN_POINT('Ctrl Pts',(-4.11653973150519,-22.177347426894,
0.));
#227161=CARTESIAN_POINT('Ctrl Pts',(-4.11694173195005,-22.179297473024,
0.));
#227162=CARTESIAN_POINT('Ctrl Pts',(-4.11743469691757,-22.1816414985788,
0.));
#227163=CARTESIAN_POINT('Ctrl Pts',(-4.11801938107481,-22.1843613164855,
0.));
#227164=CARTESIAN_POINT('Ctrl Pts',(-4.11869641271774,-22.1874419861496,
0.));
#227165=CARTESIAN_POINT('Ctrl Pts',(-4.11946626228637,-22.1908725908525,
0.));
#227166=CARTESIAN_POINT('Ctrl Pts',(-4.12032932637737,-22.1946440958098,
0.));
#227167=CARTESIAN_POINT('Ctrl Pts',(-4.12128598183523,-22.1987479618246,
0.));
#227168=CARTESIAN_POINT('Ctrl Pts',(-4.12233664408228,-22.2031746532106,
0.));
#227169=CARTESIAN_POINT('Ctrl Pts',(-4.12348173702024,-22.2079143941719,
0.));
#227170=CARTESIAN_POINT('Ctrl Pts',(-4.12472167516608,-22.2129576146671,
0.));
#227171=CARTESIAN_POINT('Ctrl Pts',(-4.12605683613308,-22.2182956401341,
0.));
#227172=CARTESIAN_POINT('Ctrl Pts',(-4.12748755830105,-22.2239207458781,
0.));
#227173=CARTESIAN_POINT('Ctrl Pts',(-4.1290141546338,-22.2298258043947,
0.));
#227174=CARTESIAN_POINT('Ctrl Pts',(-4.13063692157499,-22.2360040565533,
0.));
#227175=CARTESIAN_POINT('Ctrl Pts',(-4.13235615060161,-22.2424488153523,
0.));
#227176=CARTESIAN_POINT('Ctrl Pts',(-4.13417212558811,-22.249153531779,
0.));
#227177=CARTESIAN_POINT('Ctrl Pts',(-4.13608511977226,-22.2561118708421,
0.));
#227178=CARTESIAN_POINT('Ctrl Pts',(-4.13809539255423,-22.2633177913972,
0.));
#227179=CARTESIAN_POINT('Ctrl Pts',(-4.14020318715992,-22.2707656042457,
0.));
#227180=CARTESIAN_POINT('Ctrl Pts',(-4.14240873321985,-22.2784499072027,
0.));
#227181=CARTESIAN_POINT('Ctrl Pts',(-4.14471224859296,-22.2863655389166,
0.));
#227182=CARTESIAN_POINT('Ctrl Pts',(-4.14711394168557,-22.2945075198467,
0.));
#227183=CARTESIAN_POINT('Ctrl Pts',(-4.14961401285523,-22.3028710166933,
0.));
#227184=CARTESIAN_POINT('Ctrl Pts',(-4.15221265396991,-22.3114513545185,
0.));
#227185=CARTESIAN_POINT('Ctrl Pts',(-4.15491004835282,-22.320244018698,
0.));
#227186=CARTESIAN_POINT('Ctrl Pts',(-4.15770637047891,-22.3292446628959,
0.));
#227187=CARTESIAN_POINT('Ctrl Pts',(-4.16060178604165,-22.3384491078602,
0.));
#227188=CARTESIAN_POINT('Ctrl Pts',(-4.16359645263189,-22.3478533253889,
0.));
#227189=CARTESIAN_POINT('Ctrl Pts',(-4.16669052026601,-22.3574534257396,
0.));
#227190=CARTESIAN_POINT('Ctrl Pts',(-4.16988413199458,-22.36724564276,0.));
#227191=CARTESIAN_POINT('Ctrl Pts',(-4.17317742436146,-22.3772263228617,
0.));
#227192=CARTESIAN_POINT('Ctrl Pts',(-4.17657052752826,-22.3873919231334,
0.));
#227193=CARTESIAN_POINT('Ctrl Pts',(-4.18006356544883,-22.3977390078075,
0.));
#227194=CARTESIAN_POINT('Ctrl Pts',(-4.18365665600851,-22.4082642454453,
0.));
#227195=CARTESIAN_POINT('Ctrl Pts',(-4.18734991117722,-22.4189644056115,
0.));
#227196=CARTESIAN_POINT('Ctrl Pts',(-4.19114343726943,-22.4298363535421,
0.));
#227197=CARTESIAN_POINT('Ctrl Pts',(-4.19503733518862,-22.4408770448917,
0.));
#227198=CARTESIAN_POINT('Ctrl Pts',(-4.19903170066356,-22.4520835205419,
0.));
#227199=CARTESIAN_POINT('Ctrl Pts',(-4.20312662448172,-22.4634529011433,
0.));
#227200=CARTESIAN_POINT('Ctrl Pts',(-4.20732219265649,-22.4749823839915,
0.));
#227201=CARTESIAN_POINT('Ctrl Pts',(-4.21161848657429,-22.4866692403147,
0.));
#227202=CARTESIAN_POINT('Ctrl Pts',(-4.21601558313909,-22.4985108124229,
0.));
#227203=CARTESIAN_POINT('Ctrl Pts',(-4.22051355490198,-22.5105045108882,
0.));
#227204=CARTESIAN_POINT('Ctrl Pts',(-4.22511247020041,-22.5226478117885,
0.));
#227205=CARTESIAN_POINT('Ctrl Pts',(-4.22981239330732,-22.5349382540587,
0.));
#227206=CARTESIAN_POINT('Ctrl Pts',(-4.23461338456714,-22.5473734368086,
0.));
#227207=CARTESIAN_POINT('Ctrl Pts',(-4.23951550052527,-22.559951016643,
0.));
#227208=CARTESIAN_POINT('Ctrl Pts',(-4.2445187940486,-22.5726687049922,
0.));
#227209=CARTESIAN_POINT('Ctrl Pts',(-4.24962331444186,-22.5855242662479,
0.));
#227210=CARTESIAN_POINT('Ctrl Pts',(-4.25482910755486,-22.5985155158637,
0.));
#227211=CARTESIAN_POINT('Ctrl Pts',(-4.26013621588304,-22.611640318482,
0.));
#227212=CARTESIAN_POINT('Ctrl Pts',(-4.26554467865572,-22.6248965859975,
0.));
#227213=CARTESIAN_POINT('Ctrl Pts',(-4.27105453193,-22.6382822758171,0.));
#227214=CARTESIAN_POINT('Ctrl Pts',(-4.27666580869118,-22.6517953893303,
0.));
#227215=CARTESIAN_POINT('Ctrl Pts',(-4.2823785389406,-22.665433970311,0.));
#227216=CARTESIAN_POINT('Ctrl Pts',(-4.28819274977767,-22.6791961033536,
0.));
#227217=CARTESIAN_POINT('Ctrl Pts',(-4.29410846547062,-22.6930799122545,
0.));
#227218=CARTESIAN_POINT('Ctrl Pts',(-4.30012570754067,-22.707083558756,
0.));
#227219=CARTESIAN_POINT('Ctrl Pts',(-4.30624449484075,-22.7212052413384,
0.));
#227220=CARTESIAN_POINT('Ctrl Pts',(-4.31246484362551,-22.7354431939926,
0.));
#227221=CARTESIAN_POINT('Ctrl Pts',(-4.31878676761231,-22.7497956849852,
0.));
#227222=CARTESIAN_POINT('Ctrl Pts',(-4.32521027803748,-22.764261015648,
0.));
#227223=CARTESIAN_POINT('Ctrl Pts',(-4.33173538373183,-22.7788375194081,
0.));
#227224=CARTESIAN_POINT('Ctrl Pts',(-4.33836209118444,-22.7935235607807,
0.));
#227225=CARTESIAN_POINT('Ctrl Pts',(-4.34509040460066,-22.808317534379,
0.));
#227226=CARTESIAN_POINT('Ctrl Pts',(-4.35192032594802,-22.8232178638873,
0.));
#227227=CARTESIAN_POINT('Ctrl Pts',(-4.3588518550056,-22.838223001118,0.));
#227228=CARTESIAN_POINT('Ctrl Pts',(-4.36588498943011,-22.8533314252419,
0.));
#227229=CARTESIAN_POINT('Ctrl Pts',(-4.37301972480753,-22.8685416419725,
0.));
#227230=CARTESIAN_POINT('Ctrl Pts',(-4.38025605470091,-22.8838521827702,
0.));
#227231=CARTESIAN_POINT('Ctrl Pts',(-4.38759397068393,-22.8992616040108,
0.));
#227232=CARTESIAN_POINT('Ctrl Pts',(-4.39503346238455,-22.9147684862425,
0.));
#227233=CARTESIAN_POINT('Ctrl Pts',(-4.40257451754308,-22.9303714335549,
0.));
#227234=CARTESIAN_POINT('Ctrl Pts',(-4.41021712205549,-22.9460690729093,
0.));
#227235=CARTESIAN_POINT('Ctrl Pts',(-4.41796126001311,-22.9618600534866,
0.));
#227236=CARTESIAN_POINT('Ctrl Pts',(-4.42580691372772,-22.9777430460021,
0.));
#227237=CARTESIAN_POINT('Ctrl Pts',(-4.43375406376906,-22.9937167421009,
0.));
#227238=CARTESIAN_POINT('Ctrl Pts',(-4.44180268901667,-23.0097798538399,
0.));
#227239=CARTESIAN_POINT('Ctrl Pts',(-4.44995276669699,-23.0259311131395,
0.));
#227240=CARTESIAN_POINT('Ctrl Pts',(-4.45820427241677,-23.0421692712466,
0.));
#227241=CARTESIAN_POINT('Ctrl Pts',(-4.46655718018206,-23.0584930981723,
0.));
#227242=CARTESIAN_POINT('Ctrl Pts',(-4.47501146242822,-23.0749013821867,
0.));
#227243=CARTESIAN_POINT('Ctrl Pts',(-4.48356709006757,-23.0913929293909,
0.));
#227244=CARTESIAN_POINT('Ctrl Pts',(-4.49222403252202,-23.1079665632629,
0.));
#227245=CARTESIAN_POINT('Ctrl Pts',(-4.50098225775179,-23.1246211242117,
0.));
#227246=CARTESIAN_POINT('Ctrl Pts',(-4.50984173227088,-23.1413554691136,
0.));
#227247=CARTESIAN_POINT('Ctrl Pts',(-4.51880242116786,-23.1581684708778,
0.));
#227248=CARTESIAN_POINT('Ctrl Pts',(-4.52786428815049,-23.1750590180923,
0.));
#227249=CARTESIAN_POINT('Ctrl Pts',(-4.53702729557586,-23.1920260146474,
0.));
#227250=CARTESIAN_POINT('Ctrl Pts',(-4.54629140447543,-23.2090683793627,
0.));
#227251=CARTESIAN_POINT('Ctrl Pts',(-4.55565657456957,-23.2261850456055,
0.));
#227252=CARTESIAN_POINT('Ctrl Pts',(-4.56512276427812,-23.2433749609117,
0.));
#227253=CARTESIAN_POINT('Ctrl Pts',(-4.57468993076071,-23.2606370866854,
0.));
#227254=CARTESIAN_POINT('Ctrl Pts',(-4.58435802994675,-23.2779703978868,
0.));
#227255=CARTESIAN_POINT('Ctrl Pts',(-4.5941270165575,-23.295373882719,0.));
#227256=CARTESIAN_POINT('Ctrl Pts',(-4.60399684412176,-23.3128465423119,
0.));
#227257=CARTESIAN_POINT('Ctrl Pts',(-4.61396746497849,-23.3303873903947,
0.));
#227258=CARTESIAN_POINT('Ctrl Pts',(-4.62403883030825,-23.3479954530281,
0.));
#227259=CARTESIAN_POINT('Ctrl Pts',(-4.63421089016555,-23.3656697683496,
0.));
#227260=CARTESIAN_POINT('Ctrl Pts',(-4.64448359349936,-23.383409386307,
0.));
#227261=CARTESIAN_POINT('Ctrl Pts',(-4.65485688816923,-23.4012133683957,
0.));
#227262=CARTESIAN_POINT('Ctrl Pts',(-4.66533072094664,-23.4190807873798,
0.));
#227263=CARTESIAN_POINT('Ctrl Pts',(-4.67590503753051,-23.4370107270444,
0.));
#227264=CARTESIAN_POINT('Ctrl Pts',(-4.68657978258298,-23.4550022819852,
0.));
#227265=CARTESIAN_POINT('Ctrl Pts',(-4.69735489975024,-23.4730545573849,
0.));
#227266=CARTESIAN_POINT('Ctrl Pts',(-4.70823033167821,-23.491166668789,
0.));
#227267=CARTESIAN_POINT('Ctrl Pts',(-4.71920602001905,-23.5093377418784,
0.));
#227268=CARTESIAN_POINT('Ctrl Pts',(-4.73028190543032,-23.5275669122378,
0.));
#227269=CARTESIAN_POINT('Ctrl Pts',(-4.74145792760699,-23.5458533251715,
0.));
#227270=CARTESIAN_POINT('Ctrl Pts',(-4.75273402530616,-23.564196135517,
0.));
#227271=CARTESIAN_POINT('Ctrl Pts',(-4.76411013636252,-23.5825945074535,
0.));
#227272=CARTESIAN_POINT('Ctrl Pts',(-4.77558619769876,-23.6010476143099,
0.));
#227273=CARTESIAN_POINT('Ctrl Pts',(-4.78716214532105,-23.6195546383625,
0.));
#227274=CARTESIAN_POINT('Ctrl Pts',(-4.79883791433231,-23.6381147706581,
0.));
#227275=CARTESIAN_POINT('Ctrl Pts',(-4.81061343896443,-23.6567272108631,
0.));
#227276=CARTESIAN_POINT('Ctrl Pts',(-4.82248865259571,-23.6753911671023,
0.));
#227277=CARTESIAN_POINT('Ctrl Pts',(-4.83446348776268,-23.6941058557971,
0.));
#227278=CARTESIAN_POINT('Ctrl Pts',(-4.84653787616424,-23.7128705015014,
0.));
#227279=CARTESIAN_POINT('Ctrl Pts',(-4.85871174865492,-23.7316843367308,
0.));
#227280=CARTESIAN_POINT('Ctrl Pts',(-4.87098503527144,-23.7505466018239,
0.));
#227281=CARTESIAN_POINT('Ctrl Pts',(-4.88335766525566,-23.7694565448044,
0.));
#227282=CARTESIAN_POINT('Ctrl Pts',(-4.89582956706772,-23.7884134212381,
0.));
#227283=CARTESIAN_POINT('Ctrl Pts',(-4.90840066839348,-23.8074164940897,
0.));
#227284=CARTESIAN_POINT('Ctrl Pts',(-4.92107089613977,-23.8264650335721,
0.));
#227285=CARTESIAN_POINT('Ctrl Pts',(-4.93384017643442,-23.8455583170062,
0.));
#227286=CARTESIAN_POINT('Ctrl Pts',(-4.94670843465869,-23.8646956287172,
0.));
#227287=CARTESIAN_POINT('Ctrl Pts',(-4.95967559546566,-23.883876259922,
0.));
#227288=CARTESIAN_POINT('Ctrl Pts',(-4.9727415827923,-23.9030995086164,
0.));
#227289=CARTESIAN_POINT('Ctrl Pts',(-4.98590631986534,-23.9223646794591,
0.));
#227290=CARTESIAN_POINT('Ctrl Pts',(-4.9991697291931,-23.9416710836529,
0.));
#227291=CARTESIAN_POINT('Ctrl Pts',(-5.01253173257459,-23.9610180388271,
0.));
#227292=CARTESIAN_POINT('Ctrl Pts',(-5.02599225112462,-23.9804048689228,
0.));
#227293=CARTESIAN_POINT('Ctrl Pts',(-5.03955120528528,-23.9998309040747,
0.));
#227294=CARTESIAN_POINT('Ctrl Pts',(-5.05320851483069,-24.0192954804896,
0.));
#227295=CARTESIAN_POINT('Ctrl Pts',(-5.0669640988664,-24.0387979403268,
0.));
#227296=CARTESIAN_POINT('Ctrl Pts',(-5.08081787581271,-24.0583376315636,
0.));
#227297=CARTESIAN_POINT('Ctrl Pts',(-5.09476976342618,-24.0779139079264,
0.));
#227298=CARTESIAN_POINT('Ctrl Pts',(-5.10881967883126,-24.0975261288444,
0.));
#227299=CARTESIAN_POINT('Ctrl Pts',(-5.12296753853858,-24.117173659394,
0.));
#227300=CARTESIAN_POINT('Ctrl Pts',(-5.13721325845746,-24.1368558702443,
0.));
#227301=CARTESIAN_POINT('Ctrl Pts',(-5.1515567539008,-24.1565721375971,
0.));
#227302=CARTESIAN_POINT('Ctrl Pts',(-5.16599793957987,-24.1763218431344,
0.));
#227303=CARTESIAN_POINT('Ctrl Pts',(-5.180536729614,-24.1961043738756,0.));
#227304=CARTESIAN_POINT('Ctrl Pts',(-5.19517303753648,-24.2159191220171,
0.));
#227305=CARTESIAN_POINT('Ctrl Pts',(-5.20990677629177,-24.2357654847766,
0.));
#227306=CARTESIAN_POINT('Ctrl Pts',(-5.22473785822443,-24.2556428642294,
0.));
#227307=CARTESIAN_POINT('Ctrl Pts',(-5.2396661950629,-24.2755506671525,
0.));
#227308=CARTESIAN_POINT('Ctrl Pts',(-5.25469169788857,-24.2954883048447,
0.));
#227309=CARTESIAN_POINT('Ctrl Pts',(-5.269814277188,-24.3154551932221,0.));
#227310=CARTESIAN_POINT('Ctrl Pts',(-5.28503384290649,-24.3354507529414,
0.));
#227311=CARTESIAN_POINT('Ctrl Pts',(-5.30035030449064,-24.3554744095075,
0.));
#227312=CARTESIAN_POINT('Ctrl Pts',(-5.31576357092527,-24.3755255933917,
0.));
#227313=CARTESIAN_POINT('Ctrl Pts',(-5.33127355076035,-24.3956037401293,
0.));
#227314=CARTESIAN_POINT('Ctrl Pts',(-5.34688015213538,-24.4157082904614,
0.));
#227315=CARTESIAN_POINT('Ctrl Pts',(-5.36258328273628,-24.435838689915,
0.));
#227316=CARTESIAN_POINT('Ctrl Pts',(-5.37838284973696,-24.4559943883157,
0.));
#227317=CARTESIAN_POINT('Ctrl Pts',(-5.39427875973825,-24.4761748393321,
0.));
#227318=CARTESIAN_POINT('Ctrl Pts',(-5.41027091869242,-24.496379499983,
0.));
#227319=CARTESIAN_POINT('Ctrl Pts',(-5.4263592318342,-24.5166078302108,
0.));
#227320=CARTESIAN_POINT('Ctrl Pts',(-5.44254360356881,-24.5368592922863,
0.));
#227321=CARTESIAN_POINT('Ctrl Pts',(-5.45882393762262,-24.5571333514842,
0.));
#227322=CARTESIAN_POINT('Ctrl Pts',(-5.4752001372442,-24.5774294770329,
0.));
#227323=CARTESIAN_POINT('Ctrl Pts',(-5.49167210537248,-24.5977471429364,
0.));
#227324=CARTESIAN_POINT('Ctrl Pts',(-5.50823974481963,-24.6180858289179,
0.));
#227325=CARTESIAN_POINT('Ctrl Pts',(-5.52490295840993,-24.6384450211467,
0.));
#227326=CARTESIAN_POINT('Ctrl Pts',(-5.54166164919584,-24.6588242134738,
0.));
#227327=CARTESIAN_POINT('Ctrl Pts',(-5.55851572025377,-24.6792229061794,
0.));
#227328=CARTESIAN_POINT('Ctrl Pts',(-5.57546507427756,-24.6996406035517,
0.));
#227329=CARTESIAN_POINT('Ctrl Pts',(-5.59250961323988,-24.7200768119088,
0.));
#227330=CARTESIAN_POINT('Ctrl Pts',(-5.60964923798492,-24.7405310372739,
0.));
#227331=CARTESIAN_POINT('Ctrl Pts',(-5.62688384790924,-24.7610027835697,
0.));
#227332=CARTESIAN_POINT('Ctrl Pts',(-5.64421334042262,-24.781491549672,
0.));
#227333=CARTESIAN_POINT('Ctrl Pts',(-5.66163761114922,-24.8019968304605,
0.));
#227334=CARTESIAN_POINT('Ctrl Pts',(-5.67915655496543,-24.8225181223845,
0.));
#227335=CARTESIAN_POINT('Ctrl Pts',(-5.69677006679445,-24.8430549277621,
0.));
#227336=CARTESIAN_POINT('Ctrl Pts',(-5.71447804252028,-24.8636067597669,
0.));
#227337=CARTESIAN_POINT('Ctrl Pts',(-5.73228037976928,-24.884173146722,
0.));
#227338=CARTESIAN_POINT('Ctrl Pts',(-5.75017697890805,-24.904753637648,
0.));
#227339=CARTESIAN_POINT('Ctrl Pts',(-5.76816774342221,-24.9253478043656,
0.));
#227340=CARTESIAN_POINT('Ctrl Pts',(-5.78625257775682,-24.945955229334,
0.));
#227341=CARTESIAN_POINT('Ctrl Pts',(-5.80443138549727,-24.9665754954496,
0.));
#227342=CARTESIAN_POINT('Ctrl Pts',(-5.822704067442,-24.9872081752734,0.));
#227343=CARTESIAN_POINT('Ctrl Pts',(-5.84107051963072,-25.0078528200564,
0.));
#227344=CARTESIAN_POINT('Ctrl Pts',(-5.85953063156827,-25.0285089498899,
0.));
#227345=CARTESIAN_POINT('Ctrl Pts',(-5.87808428385367,-25.049176040591,
0.));
#227346=CARTESIAN_POINT('Ctrl Pts',(-5.89673135155515,-25.0698535426514,
0.));
#227347=CARTESIAN_POINT('Ctrl Pts',(-5.91547170844448,-25.0905409050773,
0.));
#227348=CARTESIAN_POINT('Ctrl Pts',(-5.93430523086836,-25.1112375971106,
0.));
#227349=CARTESIAN_POINT('Ctrl Pts',(-5.95323180187379,-25.1319431317237,
0.));
#227350=CARTESIAN_POINT('Ctrl Pts',(-5.97225131495618,-25.1526570863092,
0.));
#227351=CARTESIAN_POINT('Ctrl Pts',(-5.99136367859755,-25.1733791296259,
0.));
#227352=CARTESIAN_POINT('Ctrl Pts',(-6.01056881804614,-25.1941090269819,
0.));
#227353=CARTESIAN_POINT('Ctrl Pts',(-6.02986667389998,-25.21484662016,0.));
#227354=CARTESIAN_POINT('Ctrl Pts',(-6.04925720151219,-25.2355918139032,
0.));
#227355=CARTESIAN_POINT('Ctrl Pts',(-6.06484373634547,-25.2521940105705,
0.));
#227356=CARTESIAN_POINT('Ctrl Pts',(-6.07657531787491,-25.2646490489922,
0.));
#227357=CARTESIAN_POINT('Ctrl Pts',(-6.08441489609794,-25.2729539149517,
0.));
#227358=CARTESIAN_POINT('Ctrl Pts',(-6.088339316177,-25.2771067246846,0.));
#227359=CARTESIAN_POINT('',(-6.088339316177,-25.2771067246846,12.));
#227360=CARTESIAN_POINT('Ctrl Pts',(-6.088339316177,-25.2771067246846,12.));
#227361=CARTESIAN_POINT('Ctrl Pts',(-6.08441489609794,-25.2729539149517,
12.));
#227362=CARTESIAN_POINT('Ctrl Pts',(-6.07657531787491,-25.2646490489922,
12.));
#227363=CARTESIAN_POINT('Ctrl Pts',(-6.06484373634547,-25.2521940105705,
12.));
#227364=CARTESIAN_POINT('Ctrl Pts',(-6.04925720151219,-25.2355918139032,
12.));
#227365=CARTESIAN_POINT('Ctrl Pts',(-6.02986667389998,-25.21484662016,12.));
#227366=CARTESIAN_POINT('Ctrl Pts',(-6.01056881804614,-25.1941090269819,
12.));
#227367=CARTESIAN_POINT('Ctrl Pts',(-5.99136367859755,-25.1733791296259,
12.));
#227368=CARTESIAN_POINT('Ctrl Pts',(-5.97225131495618,-25.1526570863092,
12.));
#227369=CARTESIAN_POINT('Ctrl Pts',(-5.95323180187379,-25.1319431317237,
12.));
#227370=CARTESIAN_POINT('Ctrl Pts',(-5.93430523086836,-25.1112375971106,
12.));
#227371=CARTESIAN_POINT('Ctrl Pts',(-5.91547170844448,-25.0905409050773,
12.));
#227372=CARTESIAN_POINT('Ctrl Pts',(-5.89673135155515,-25.0698535426514,
12.));
#227373=CARTESIAN_POINT('Ctrl Pts',(-5.87808428385367,-25.049176040591,
12.));
#227374=CARTESIAN_POINT('Ctrl Pts',(-5.85953063156827,-25.0285089498899,
12.));
#227375=CARTESIAN_POINT('Ctrl Pts',(-5.84107051963072,-25.0078528200564,
12.));
#227376=CARTESIAN_POINT('Ctrl Pts',(-5.822704067442,-24.9872081752734,12.));
#227377=CARTESIAN_POINT('Ctrl Pts',(-5.80443138549727,-24.9665754954496,
12.));
#227378=CARTESIAN_POINT('Ctrl Pts',(-5.78625257775682,-24.945955229334,
12.));
#227379=CARTESIAN_POINT('Ctrl Pts',(-5.76816774342221,-24.9253478043656,
12.));
#227380=CARTESIAN_POINT('Ctrl Pts',(-5.75017697890805,-24.904753637648,
12.));
#227381=CARTESIAN_POINT('Ctrl Pts',(-5.73228037976928,-24.884173146722,
12.));
#227382=CARTESIAN_POINT('Ctrl Pts',(-5.71447804252028,-24.8636067597669,
12.));
#227383=CARTESIAN_POINT('Ctrl Pts',(-5.69677006679445,-24.8430549277621,
12.));
#227384=CARTESIAN_POINT('Ctrl Pts',(-5.67915655496543,-24.8225181223845,
12.));
#227385=CARTESIAN_POINT('Ctrl Pts',(-5.66163761114922,-24.8019968304605,
12.));
#227386=CARTESIAN_POINT('Ctrl Pts',(-5.64421334042262,-24.781491549672,
12.));
#227387=CARTESIAN_POINT('Ctrl Pts',(-5.62688384790924,-24.7610027835697,
12.));
#227388=CARTESIAN_POINT('Ctrl Pts',(-5.60964923798492,-24.7405310372739,
12.));
#227389=CARTESIAN_POINT('Ctrl Pts',(-5.59250961323988,-24.7200768119088,
12.));
#227390=CARTESIAN_POINT('Ctrl Pts',(-5.57546507427756,-24.6996406035517,
12.));
#227391=CARTESIAN_POINT('Ctrl Pts',(-5.55851572025377,-24.6792229061794,
12.));
#227392=CARTESIAN_POINT('Ctrl Pts',(-5.54166164919584,-24.6588242134738,
12.));
#227393=CARTESIAN_POINT('Ctrl Pts',(-5.52490295840993,-24.6384450211467,
12.));
#227394=CARTESIAN_POINT('Ctrl Pts',(-5.50823974481963,-24.6180858289179,
12.));
#227395=CARTESIAN_POINT('Ctrl Pts',(-5.49167210537248,-24.5977471429364,
12.));
#227396=CARTESIAN_POINT('Ctrl Pts',(-5.4752001372442,-24.5774294770329,
12.));
#227397=CARTESIAN_POINT('Ctrl Pts',(-5.45882393762262,-24.5571333514842,
12.));
#227398=CARTESIAN_POINT('Ctrl Pts',(-5.44254360356881,-24.5368592922863,
12.));
#227399=CARTESIAN_POINT('Ctrl Pts',(-5.4263592318342,-24.5166078302108,
12.));
#227400=CARTESIAN_POINT('Ctrl Pts',(-5.41027091869242,-24.496379499983,
12.));
#227401=CARTESIAN_POINT('Ctrl Pts',(-5.39427875973825,-24.4761748393321,
12.));
#227402=CARTESIAN_POINT('Ctrl Pts',(-5.37838284973696,-24.4559943883157,
12.));
#227403=CARTESIAN_POINT('Ctrl Pts',(-5.36258328273628,-24.435838689915,
12.));
#227404=CARTESIAN_POINT('Ctrl Pts',(-5.34688015213538,-24.4157082904614,
12.));
#227405=CARTESIAN_POINT('Ctrl Pts',(-5.33127355076035,-24.3956037401293,
12.));
#227406=CARTESIAN_POINT('Ctrl Pts',(-5.31576357092527,-24.3755255933917,
12.));
#227407=CARTESIAN_POINT('Ctrl Pts',(-5.30035030449064,-24.3554744095075,
12.));
#227408=CARTESIAN_POINT('Ctrl Pts',(-5.28503384290649,-24.3354507529414,
12.));
#227409=CARTESIAN_POINT('Ctrl Pts',(-5.269814277188,-24.3154551932221,12.));
#227410=CARTESIAN_POINT('Ctrl Pts',(-5.25469169788857,-24.2954883048447,
12.));
#227411=CARTESIAN_POINT('Ctrl Pts',(-5.2396661950629,-24.2755506671525,
12.));
#227412=CARTESIAN_POINT('Ctrl Pts',(-5.22473785822443,-24.2556428642294,
12.));
#227413=CARTESIAN_POINT('Ctrl Pts',(-5.20990677629177,-24.2357654847766,
12.));
#227414=CARTESIAN_POINT('Ctrl Pts',(-5.19517303753648,-24.2159191220171,
12.));
#227415=CARTESIAN_POINT('Ctrl Pts',(-5.180536729614,-24.1961043738756,12.));
#227416=CARTESIAN_POINT('Ctrl Pts',(-5.16599793957987,-24.1763218431344,
12.));
#227417=CARTESIAN_POINT('Ctrl Pts',(-5.1515567539008,-24.1565721375971,
12.));
#227418=CARTESIAN_POINT('Ctrl Pts',(-5.13721325845746,-24.1368558702443,
12.));
#227419=CARTESIAN_POINT('Ctrl Pts',(-5.12296753853858,-24.117173659394,
12.));
#227420=CARTESIAN_POINT('Ctrl Pts',(-5.10881967883126,-24.0975261288444,
12.));
#227421=CARTESIAN_POINT('Ctrl Pts',(-5.09476976342618,-24.0779139079264,
12.));
#227422=CARTESIAN_POINT('Ctrl Pts',(-5.08081787581271,-24.0583376315636,
12.));
#227423=CARTESIAN_POINT('Ctrl Pts',(-5.0669640988664,-24.0387979403268,
12.));
#227424=CARTESIAN_POINT('Ctrl Pts',(-5.05320851483069,-24.0192954804896,
12.));
#227425=CARTESIAN_POINT('Ctrl Pts',(-5.03955120528528,-23.9998309040747,
12.));
#227426=CARTESIAN_POINT('Ctrl Pts',(-5.02599225112462,-23.9804048689228,
12.));
#227427=CARTESIAN_POINT('Ctrl Pts',(-5.01253173257459,-23.9610180388271,
12.));
#227428=CARTESIAN_POINT('Ctrl Pts',(-4.9991697291931,-23.9416710836529,
12.));
#227429=CARTESIAN_POINT('Ctrl Pts',(-4.98590631986534,-23.9223646794591,
12.));
#227430=CARTESIAN_POINT('Ctrl Pts',(-4.9727415827923,-23.9030995086164,
12.));
#227431=CARTESIAN_POINT('Ctrl Pts',(-4.95967559546566,-23.883876259922,
12.));
#227432=CARTESIAN_POINT('Ctrl Pts',(-4.94670843465869,-23.8646956287172,
12.));
#227433=CARTESIAN_POINT('Ctrl Pts',(-4.93384017643442,-23.8455583170062,
12.));
#227434=CARTESIAN_POINT('Ctrl Pts',(-4.92107089613977,-23.8264650335721,
12.));
#227435=CARTESIAN_POINT('Ctrl Pts',(-4.90840066839348,-23.8074164940897,
12.));
#227436=CARTESIAN_POINT('Ctrl Pts',(-4.89582956706772,-23.7884134212381,
12.));
#227437=CARTESIAN_POINT('Ctrl Pts',(-4.88335766525566,-23.7694565448044,
12.));
#227438=CARTESIAN_POINT('Ctrl Pts',(-4.87098503527144,-23.7505466018239,
12.));
#227439=CARTESIAN_POINT('Ctrl Pts',(-4.85871174865492,-23.7316843367308,
12.));
#227440=CARTESIAN_POINT('Ctrl Pts',(-4.84653787616424,-23.7128705015014,
12.));
#227441=CARTESIAN_POINT('Ctrl Pts',(-4.83446348776268,-23.6941058557971,
12.));
#227442=CARTESIAN_POINT('Ctrl Pts',(-4.82248865259571,-23.6753911671023,
12.));
#227443=CARTESIAN_POINT('Ctrl Pts',(-4.81061343896443,-23.6567272108631,
12.));
#227444=CARTESIAN_POINT('Ctrl Pts',(-4.79883791433231,-23.6381147706581,
12.));
#227445=CARTESIAN_POINT('Ctrl Pts',(-4.78716214532105,-23.6195546383625,
12.));
#227446=CARTESIAN_POINT('Ctrl Pts',(-4.77558619769876,-23.6010476143099,
12.));
#227447=CARTESIAN_POINT('Ctrl Pts',(-4.76411013636252,-23.5825945074535,
12.));
#227448=CARTESIAN_POINT('Ctrl Pts',(-4.75273402530616,-23.564196135517,
12.));
#227449=CARTESIAN_POINT('Ctrl Pts',(-4.74145792760699,-23.5458533251715,
12.));
#227450=CARTESIAN_POINT('Ctrl Pts',(-4.73028190543032,-23.5275669122378,
12.));
#227451=CARTESIAN_POINT('Ctrl Pts',(-4.71920602001905,-23.5093377418784,
12.));
#227452=CARTESIAN_POINT('Ctrl Pts',(-4.70823033167821,-23.491166668789,
12.));
#227453=CARTESIAN_POINT('Ctrl Pts',(-4.69735489975024,-23.4730545573849,
12.));
#227454=CARTESIAN_POINT('Ctrl Pts',(-4.68657978258298,-23.4550022819852,
12.));
#227455=CARTESIAN_POINT('Ctrl Pts',(-4.67590503753051,-23.4370107270444,
12.));
#227456=CARTESIAN_POINT('Ctrl Pts',(-4.66533072094664,-23.4190807873798,
12.));
#227457=CARTESIAN_POINT('Ctrl Pts',(-4.65485688816923,-23.4012133683957,
12.));
#227458=CARTESIAN_POINT('Ctrl Pts',(-4.64448359349936,-23.383409386307,
12.));
#227459=CARTESIAN_POINT('Ctrl Pts',(-4.63421089016555,-23.3656697683496,
12.));
#227460=CARTESIAN_POINT('Ctrl Pts',(-4.62403883030825,-23.3479954530281,
12.));
#227461=CARTESIAN_POINT('Ctrl Pts',(-4.61396746497849,-23.3303873903947,
12.));
#227462=CARTESIAN_POINT('Ctrl Pts',(-4.60399684412176,-23.3128465423119,
12.));
#227463=CARTESIAN_POINT('Ctrl Pts',(-4.5941270165575,-23.295373882719,12.));
#227464=CARTESIAN_POINT('Ctrl Pts',(-4.58435802994675,-23.2779703978868,
12.));
#227465=CARTESIAN_POINT('Ctrl Pts',(-4.57468993076071,-23.2606370866854,
12.));
#227466=CARTESIAN_POINT('Ctrl Pts',(-4.56512276427812,-23.2433749609117,
12.));
#227467=CARTESIAN_POINT('Ctrl Pts',(-4.55565657456957,-23.2261850456055,
12.));
#227468=CARTESIAN_POINT('Ctrl Pts',(-4.54629140447543,-23.2090683793627,
12.));
#227469=CARTESIAN_POINT('Ctrl Pts',(-4.53702729557586,-23.1920260146474,
12.));
#227470=CARTESIAN_POINT('Ctrl Pts',(-4.52786428815049,-23.1750590180923,
12.));
#227471=CARTESIAN_POINT('Ctrl Pts',(-4.51880242116786,-23.1581684708778,
12.));
#227472=CARTESIAN_POINT('Ctrl Pts',(-4.50984173227088,-23.1413554691136,
12.));
#227473=CARTESIAN_POINT('Ctrl Pts',(-4.50098225775179,-23.1246211242117,
12.));
#227474=CARTESIAN_POINT('Ctrl Pts',(-4.49222403252202,-23.1079665632629,
12.));
#227475=CARTESIAN_POINT('Ctrl Pts',(-4.48356709006757,-23.0913929293909,
12.));
#227476=CARTESIAN_POINT('Ctrl Pts',(-4.47501146242822,-23.0749013821867,
12.));
#227477=CARTESIAN_POINT('Ctrl Pts',(-4.46655718018206,-23.0584930981723,
12.));
#227478=CARTESIAN_POINT('Ctrl Pts',(-4.45820427241677,-23.0421692712466,
12.));
#227479=CARTESIAN_POINT('Ctrl Pts',(-4.44995276669699,-23.0259311131395,
12.));
#227480=CARTESIAN_POINT('Ctrl Pts',(-4.44180268901667,-23.0097798538399,
12.));
#227481=CARTESIAN_POINT('Ctrl Pts',(-4.43375406376906,-22.9937167421009,
12.));
#227482=CARTESIAN_POINT('Ctrl Pts',(-4.42580691372772,-22.9777430460021,
12.));
#227483=CARTESIAN_POINT('Ctrl Pts',(-4.41796126001311,-22.9618600534866,
12.));
#227484=CARTESIAN_POINT('Ctrl Pts',(-4.41021712205549,-22.9460690729093,
12.));
#227485=CARTESIAN_POINT('Ctrl Pts',(-4.40257451754308,-22.9303714335549,
12.));
#227486=CARTESIAN_POINT('Ctrl Pts',(-4.39503346238455,-22.9147684862425,
12.));
#227487=CARTESIAN_POINT('Ctrl Pts',(-4.38759397068393,-22.8992616040108,
12.));
#227488=CARTESIAN_POINT('Ctrl Pts',(-4.38025605470091,-22.8838521827702,
12.));
#227489=CARTESIAN_POINT('Ctrl Pts',(-4.37301972480753,-22.8685416419725,
12.));
#227490=CARTESIAN_POINT('Ctrl Pts',(-4.36588498943011,-22.8533314252419,
12.));
#227491=CARTESIAN_POINT('Ctrl Pts',(-4.3588518550056,-22.838223001118,12.));
#227492=CARTESIAN_POINT('Ctrl Pts',(-4.35192032594802,-22.8232178638873,
12.));
#227493=CARTESIAN_POINT('Ctrl Pts',(-4.34509040460066,-22.808317534379,
12.));
#227494=CARTESIAN_POINT('Ctrl Pts',(-4.33836209118444,-22.7935235607807,
12.));
#227495=CARTESIAN_POINT('Ctrl Pts',(-4.33173538373183,-22.7788375194081,
12.));
#227496=CARTESIAN_POINT('Ctrl Pts',(-4.32521027803748,-22.764261015648,
12.));
#227497=CARTESIAN_POINT('Ctrl Pts',(-4.31878676761231,-22.7497956849852,
12.));
#227498=CARTESIAN_POINT('Ctrl Pts',(-4.31246484362551,-22.7354431939926,
12.));
#227499=CARTESIAN_POINT('Ctrl Pts',(-4.30624449484075,-22.7212052413384,
12.));
#227500=CARTESIAN_POINT('Ctrl Pts',(-4.30012570754067,-22.707083558756,
12.));
#227501=CARTESIAN_POINT('Ctrl Pts',(-4.29410846547062,-22.6930799122545,
12.));
#227502=CARTESIAN_POINT('Ctrl Pts',(-4.28819274977767,-22.6791961033536,
12.));
#227503=CARTESIAN_POINT('Ctrl Pts',(-4.2823785389406,-22.665433970311,12.));
#227504=CARTESIAN_POINT('Ctrl Pts',(-4.27666580869118,-22.6517953893303,
12.));
#227505=CARTESIAN_POINT('Ctrl Pts',(-4.27105453193,-22.6382822758171,12.));
#227506=CARTESIAN_POINT('Ctrl Pts',(-4.26554467865572,-22.6248965859975,
12.));
#227507=CARTESIAN_POINT('Ctrl Pts',(-4.26013621588304,-22.611640318482,
12.));
#227508=CARTESIAN_POINT('Ctrl Pts',(-4.25482910755486,-22.5985155158637,
12.));
#227509=CARTESIAN_POINT('Ctrl Pts',(-4.24962331444186,-22.5855242662479,
12.));
#227510=CARTESIAN_POINT('Ctrl Pts',(-4.2445187940486,-22.5726687049922,
12.));
#227511=CARTESIAN_POINT('Ctrl Pts',(-4.23951550052527,-22.559951016643,
12.));
#227512=CARTESIAN_POINT('Ctrl Pts',(-4.23461338456714,-22.5473734368086,
12.));
#227513=CARTESIAN_POINT('Ctrl Pts',(-4.22981239330732,-22.5349382540587,
12.));
#227514=CARTESIAN_POINT('Ctrl Pts',(-4.22511247020041,-22.5226478117885,
12.));
#227515=CARTESIAN_POINT('Ctrl Pts',(-4.22051355490198,-22.5105045108882,
12.));
#227516=CARTESIAN_POINT('Ctrl Pts',(-4.21601558313909,-22.4985108124229,
12.));
#227517=CARTESIAN_POINT('Ctrl Pts',(-4.21161848657429,-22.4866692403147,
12.));
#227518=CARTESIAN_POINT('Ctrl Pts',(-4.20732219265649,-22.4749823839915,
12.));
#227519=CARTESIAN_POINT('Ctrl Pts',(-4.20312662448172,-22.4634529011433,
12.));
#227520=CARTESIAN_POINT('Ctrl Pts',(-4.19903170066356,-22.4520835205419,
12.));
#227521=CARTESIAN_POINT('Ctrl Pts',(-4.19503733518862,-22.4408770448917,
12.));
#227522=CARTESIAN_POINT('Ctrl Pts',(-4.19114343726943,-22.4298363535421,
12.));
#227523=CARTESIAN_POINT('Ctrl Pts',(-4.18734991117722,-22.4189644056115,
12.));
#227524=CARTESIAN_POINT('Ctrl Pts',(-4.18365665600851,-22.4082642454453,
12.));
#227525=CARTESIAN_POINT('Ctrl Pts',(-4.18006356544883,-22.3977390078075,
12.));
#227526=CARTESIAN_POINT('Ctrl Pts',(-4.17657052752826,-22.3873919231334,
12.));
#227527=CARTESIAN_POINT('Ctrl Pts',(-4.17317742436146,-22.3772263228617,
12.));
#227528=CARTESIAN_POINT('Ctrl Pts',(-4.16988413199458,-22.36724564276,12.));
#227529=CARTESIAN_POINT('Ctrl Pts',(-4.16669052026601,-22.3574534257396,
12.));
#227530=CARTESIAN_POINT('Ctrl Pts',(-4.16359645263189,-22.3478533253889,
12.));
#227531=CARTESIAN_POINT('Ctrl Pts',(-4.16060178604165,-22.3384491078602,
12.));
#227532=CARTESIAN_POINT('Ctrl Pts',(-4.15770637047891,-22.3292446628959,
12.));
#227533=CARTESIAN_POINT('Ctrl Pts',(-4.15491004835282,-22.320244018698,
12.));
#227534=CARTESIAN_POINT('Ctrl Pts',(-4.15221265396991,-22.3114513545185,
12.));
#227535=CARTESIAN_POINT('Ctrl Pts',(-4.14961401285523,-22.3028710166933,
12.));
#227536=CARTESIAN_POINT('Ctrl Pts',(-4.14711394168557,-22.2945075198467,
12.));
#227537=CARTESIAN_POINT('Ctrl Pts',(-4.14471224859296,-22.2863655389166,
12.));
#227538=CARTESIAN_POINT('Ctrl Pts',(-4.14240873321985,-22.2784499072027,
12.));
#227539=CARTESIAN_POINT('Ctrl Pts',(-4.14020318715992,-22.2707656042457,
12.));
#227540=CARTESIAN_POINT('Ctrl Pts',(-4.13809539255423,-22.2633177913972,
12.));
#227541=CARTESIAN_POINT('Ctrl Pts',(-4.13608511977226,-22.2561118708421,
12.));
#227542=CARTESIAN_POINT('Ctrl Pts',(-4.13417212558811,-22.249153531779,
12.));
#227543=CARTESIAN_POINT('Ctrl Pts',(-4.13235615060161,-22.2424488153523,
12.));
#227544=CARTESIAN_POINT('Ctrl Pts',(-4.13063692157499,-22.2360040565533,
12.));
#227545=CARTESIAN_POINT('Ctrl Pts',(-4.1290141546338,-22.2298258043947,
12.));
#227546=CARTESIAN_POINT('Ctrl Pts',(-4.12748755830105,-22.2239207458781,
12.));
#227547=CARTESIAN_POINT('Ctrl Pts',(-4.12605683613308,-22.2182956401341,
12.));
#227548=CARTESIAN_POINT('Ctrl Pts',(-4.12472167516608,-22.2129576146671,
12.));
#227549=CARTESIAN_POINT('Ctrl Pts',(-4.12348173702024,-22.2079143941719,
12.));
#227550=CARTESIAN_POINT('Ctrl Pts',(-4.12233664408228,-22.2031746532106,
12.));
#227551=CARTESIAN_POINT('Ctrl Pts',(-4.12128598183523,-22.1987479618246,
12.));
#227552=CARTESIAN_POINT('Ctrl Pts',(-4.12032932637737,-22.1946440958098,
12.));
#227553=CARTESIAN_POINT('Ctrl Pts',(-4.11946626228637,-22.1908725908525,
12.));
#227554=CARTESIAN_POINT('Ctrl Pts',(-4.11869641271774,-22.1874419861496,
12.));
#227555=CARTESIAN_POINT('Ctrl Pts',(-4.11801938107481,-22.1843613164855,
12.));
#227556=CARTESIAN_POINT('Ctrl Pts',(-4.11743469691757,-22.1816414985788,
12.));
#227557=CARTESIAN_POINT('Ctrl Pts',(-4.11694173195005,-22.179297473024,
12.));
#227558=CARTESIAN_POINT('Ctrl Pts',(-4.11653973150519,-22.177347426894,
12.));
#227559=CARTESIAN_POINT('Ctrl Pts',(-4.11622797217069,-22.1758088296598,
12.));
#227560=CARTESIAN_POINT('Ctrl Pts',(-4.11600589882846,-22.1746949858775,
12.));
#227561=CARTESIAN_POINT('Ctrl Pts',(-4.11589976826167,-22.1741488021234,
12.));
#227562=CARTESIAN_POINT('Ctrl Pts',(-4.11586035878288,-22.1739341411687,
12.));
#227563=CARTESIAN_POINT('Ctrl Pts',(-4.11585194677443,-22.173877682324,
12.));
#227564=CARTESIAN_POINT('Ctrl Pts',(-4.11585220600463,-22.1738711152697,
12.));
#227565=CARTESIAN_POINT('',(-6.088339316177,-25.2771067246846,0.));
#227566=CARTESIAN_POINT('Origin',(-9.26120677397565,-19.4030938020118,0.));
#227567=CARTESIAN_POINT('',(-9.71462809124917,-20.353053841303,12.));
#227568=CARTESIAN_POINT('',(-4.63060338698782,-9.70154690100589,12.));
#227569=CARTESIAN_POINT('',(-9.71462809124917,-20.353053841303,0.));
#227570=CARTESIAN_POINT('',(-9.71462809124917,-20.353053841303,0.));
#227571=CARTESIAN_POINT('',(-4.63060338698782,-9.70154690100589,0.));
#227572=CARTESIAN_POINT('Ctrl Pts',(-7.36589684767345,-24.9347862158358,
0.));
#227573=CARTESIAN_POINT('Ctrl Pts',(-7.36589684767345,-24.9347862158358,
12.));
#227574=CARTESIAN_POINT('Ctrl Pts',(-7.36721909028843,-24.9292275670674,
0.));
#227575=CARTESIAN_POINT('Ctrl Pts',(-7.36721909028843,-24.9292275670674,
12.));
#227576=CARTESIAN_POINT('Ctrl Pts',(-7.36985593120091,-24.9181155530543,
0.));
#227577=CARTESIAN_POINT('Ctrl Pts',(-7.36985593120091,-24.9181155530543,
12.));
#227578=CARTESIAN_POINT('Ctrl Pts',(-7.37378825961676,-24.901463382605,
0.));
#227579=CARTESIAN_POINT('Ctrl Pts',(-7.37378825961676,-24.901463382605,
12.));
#227580=CARTESIAN_POINT('Ctrl Pts',(-7.3789854964027,-24.8792921911115,
0.));
#227581=CARTESIAN_POINT('Ctrl Pts',(-7.3789854964027,-24.8792921911115,
12.));
#227582=CARTESIAN_POINT('Ctrl Pts',(-7.38540558903621,-24.8516310625176,
0.));
#227583=CARTESIAN_POINT('Ctrl Pts',(-7.38540558903621,-24.8516310625176,
12.));
#227584=CARTESIAN_POINT('Ctrl Pts',(-7.39174922585809,-24.8240228520893,
0.));
#227585=CARTESIAN_POINT('Ctrl Pts',(-7.39174922585809,-24.8240228520893,
12.));
#227586=CARTESIAN_POINT('Ctrl Pts',(-7.39801641583013,-24.7964676646431,
0.));
#227587=CARTESIAN_POINT('Ctrl Pts',(-7.39801641583013,-24.7964676646431,
12.));
#227588=CARTESIAN_POINT('Ctrl Pts',(-7.40420718661603,-24.7689656668983,
0.));
#227589=CARTESIAN_POINT('Ctrl Pts',(-7.40420718661603,-24.7689656668983,
12.));
#227590=CARTESIAN_POINT('Ctrl Pts',(-7.41032159082382,-24.7415170994784,
0.));
#227591=CARTESIAN_POINT('Ctrl Pts',(-7.41032159082382,-24.7415170994784,
12.));
#227592=CARTESIAN_POINT('Ctrl Pts',(-7.41635971481674,-24.7141222950051,
0.));
#227593=CARTESIAN_POINT('Ctrl Pts',(-7.41635971481674,-24.7141222950051,
12.));
#227594=CARTESIAN_POINT('Ctrl Pts',(-7.42232167766266,-24.6867816727192,
0.));
#227595=CARTESIAN_POINT('Ctrl Pts',(-7.42232167766266,-24.6867816727192,
12.));
#227596=CARTESIAN_POINT('Ctrl Pts',(-7.42820762159126,-24.6594957128756,
0.));
#227597=CARTESIAN_POINT('Ctrl Pts',(-7.42820762159126,-24.6594957128756,
12.));
#227598=CARTESIAN_POINT('Ctrl Pts',(-7.43401770489524,-24.6322649369517,
0.));
#227599=CARTESIAN_POINT('Ctrl Pts',(-7.43401770489524,-24.6322649369517,
12.));
#227600=CARTESIAN_POINT('Ctrl Pts',(-7.43975209375504,-24.6050898852368,
0.));
#227601=CARTESIAN_POINT('Ctrl Pts',(-7.43975209375504,-24.6050898852368,
12.));
#227602=CARTESIAN_POINT('Ctrl Pts',(-7.44541095473135,-24.577971096086,
0.));
#227603=CARTESIAN_POINT('Ctrl Pts',(-7.44541095473135,-24.577971096086,
12.));
#227604=CARTESIAN_POINT('Ctrl Pts',(-7.4509944465116,-24.5509090831559,
0.));
#227605=CARTESIAN_POINT('Ctrl Pts',(-7.4509944465116,-24.5509090831559,
12.));
#227606=CARTESIAN_POINT('Ctrl Pts',(-7.45650271335862,-24.5239043173072,
0.));
#227607=CARTESIAN_POINT('Ctrl Pts',(-7.45650271335862,-24.5239043173072,
12.));
#227608=CARTESIAN_POINT('Ctrl Pts',(-7.46193588961464,-24.4969572391483,
0.));
#227609=CARTESIAN_POINT('Ctrl Pts',(-7.46193588961464,-24.4969572391483,
12.));
#227610=CARTESIAN_POINT('Ctrl Pts',(-7.46729410308787,-24.4700682684524,
0.));
#227611=CARTESIAN_POINT('Ctrl Pts',(-7.46729410308787,-24.4700682684524,
12.));
#227612=CARTESIAN_POINT('Ctrl Pts',(-7.47257747883246,-24.443237814649,
0.));
#227613=CARTESIAN_POINT('Ctrl Pts',(-7.47257747883246,-24.443237814649,
12.));
#227614=CARTESIAN_POINT('Ctrl Pts',(-7.47778614286565,-24.4164662871163,
0.));
#227615=CARTESIAN_POINT('Ctrl Pts',(-7.47778614286565,-24.4164662871163,
12.));
#227616=CARTESIAN_POINT('Ctrl Pts',(-7.48292022569301,-24.3897541049254,
0.));
#227617=CARTESIAN_POINT('Ctrl Pts',(-7.48292022569301,-24.3897541049254,
12.));
#227618=CARTESIAN_POINT('Ctrl Pts',(-7.48797986651909,-24.3631017084524,
0.));
#227619=CARTESIAN_POINT('Ctrl Pts',(-7.48797986651909,-24.3631017084524,
12.));
#227620=CARTESIAN_POINT('Ctrl Pts',(-7.49296521252421,-24.3365095573685,
0.));
#227621=CARTESIAN_POINT('Ctrl Pts',(-7.49296521252421,-24.3365095573685,
12.));
#227622=CARTESIAN_POINT('Ctrl Pts',(-7.49787641695439,-24.3099781253355,
0.));
#227623=CARTESIAN_POINT('Ctrl Pts',(-7.49787641695439,-24.3099781253355,
12.));
#227624=CARTESIAN_POINT('Ctrl Pts',(-7.50271363765152,-24.2835078958973,
0.));
#227625=CARTESIAN_POINT('Ctrl Pts',(-7.50271363765152,-24.2835078958973,
12.));
#227626=CARTESIAN_POINT('Ctrl Pts',(-7.50747703535134,-24.2570993577034,
0.));
#227627=CARTESIAN_POINT('Ctrl Pts',(-7.50747703535134,-24.2570993577034,
12.));
#227628=CARTESIAN_POINT('Ctrl Pts',(-7.51216677222181,-24.2307530003887,
0.));
#227629=CARTESIAN_POINT('Ctrl Pts',(-7.51216677222181,-24.2307530003887,
12.));
#227630=CARTESIAN_POINT('Ctrl Pts',(-7.51678300997949,-24.2044693092349,
0.));
#227631=CARTESIAN_POINT('Ctrl Pts',(-7.51678300997949,-24.2044693092349,
12.));
#227632=CARTESIAN_POINT('Ctrl Pts',(-7.52132590953802,-24.1782487641594,
0.));
#227633=CARTESIAN_POINT('Ctrl Pts',(-7.52132590953802,-24.1782487641594,
12.));
#227634=CARTESIAN_POINT('Ctrl Pts',(-7.52579563201424,-24.1520918425364,
0.));
#227635=CARTESIAN_POINT('Ctrl Pts',(-7.52579563201424,-24.1520918425364,
12.));
#227636=CARTESIAN_POINT('Ctrl Pts',(-7.53019233935502,-24.1259990209207,
0.));
#227637=CARTESIAN_POINT('Ctrl Pts',(-7.53019233935502,-24.1259990209207,
12.));
#227638=CARTESIAN_POINT('Ctrl Pts',(-7.53451619514649,-24.0999707772642,
0.));
#227639=CARTESIAN_POINT('Ctrl Pts',(-7.53451619514649,-24.0999707772642,
12.));
#227640=CARTESIAN_POINT('Ctrl Pts',(-7.53876736531014,-24.0740075927985,
0.));
#227641=CARTESIAN_POINT('Ctrl Pts',(-7.53876736531014,-24.0740075927985,
12.));
#227642=CARTESIAN_POINT('Ctrl Pts',(-7.54294601896145,-24.0481099543353,
0.));
#227643=CARTESIAN_POINT('Ctrl Pts',(-7.54294601896145,-24.0481099543353,
12.));
#227644=CARTESIAN_POINT('Ctrl Pts',(-7.5470523288591,-24.022278355453,0.));
#227645=CARTESIAN_POINT('Ctrl Pts',(-7.5470523288591,-24.022278355453,12.));
#227646=CARTESIAN_POINT('Ctrl Pts',(-7.55108647097441,-23.9965132953185,
0.));
#227647=CARTESIAN_POINT('Ctrl Pts',(-7.55108647097441,-23.9965132953185,
12.));
#227648=CARTESIAN_POINT('Ctrl Pts',(-7.55504862424812,-23.9708152779884,
0.));
#227649=CARTESIAN_POINT('Ctrl Pts',(-7.55504862424812,-23.9708152779884,
12.));
#227650=CARTESIAN_POINT('Ctrl Pts',(-7.55893897027683,-23.9451848115,0.));
#227651=CARTESIAN_POINT('Ctrl Pts',(-7.55893897027683,-23.9451848115,12.));
#227652=CARTESIAN_POINT('Ctrl Pts',(-7.56275769304773,-23.9196224070759,
0.));
#227653=CARTESIAN_POINT('Ctrl Pts',(-7.56275769304773,-23.9196224070759,
12.));
#227654=CARTESIAN_POINT('Ctrl Pts',(-7.56650497863792,-23.8941285782003,
0.));
#227655=CARTESIAN_POINT('Ctrl Pts',(-7.56650497863792,-23.8941285782003,
12.));
#227656=CARTESIAN_POINT('Ctrl Pts',(-7.57018101500711,-23.8687038399597,
0.));
#227657=CARTESIAN_POINT('Ctrl Pts',(-7.57018101500711,-23.8687038399597,
12.));
#227658=CARTESIAN_POINT('Ctrl Pts',(-7.57378599219817,-23.8433487096134,
0.));
#227659=CARTESIAN_POINT('Ctrl Pts',(-7.57378599219817,-23.8433487096134,
12.));
#227660=CARTESIAN_POINT('Ctrl Pts',(-7.57732010249066,-23.8180637069977,
0.));
#227661=CARTESIAN_POINT('Ctrl Pts',(-7.57732010249066,-23.8180637069977,
12.));
#227662=CARTESIAN_POINT('Ctrl Pts',(-7.58078354058212,-23.7928493549908,
0.));
#227663=CARTESIAN_POINT('Ctrl Pts',(-7.58078354058212,-23.7928493549908,
12.));
#227664=CARTESIAN_POINT('Ctrl Pts',(-7.58417650376272,-23.7677061799376,
0.));
#227665=CARTESIAN_POINT('Ctrl Pts',(-7.58417650376272,-23.7677061799376,
12.));
#227666=CARTESIAN_POINT('Ctrl Pts',(-7.58749919210832,-23.7426347121006,
0.));
#227667=CARTESIAN_POINT('Ctrl Pts',(-7.58749919210832,-23.7426347121006,
12.));
#227668=CARTESIAN_POINT('Ctrl Pts',(-7.59075180865327,-23.7176354860457,
0.));
#227669=CARTESIAN_POINT('Ctrl Pts',(-7.59075180865327,-23.7176354860457,
12.));
#227670=CARTESIAN_POINT('Ctrl Pts',(-7.59393455934042,-23.6927090405067,
0.));
#227671=CARTESIAN_POINT('Ctrl Pts',(-7.59393455934042,-23.6927090405067,
12.));
#227672=CARTESIAN_POINT('Ctrl Pts',(-7.59704765299572,-23.6678559182876,
0.));
#227673=CARTESIAN_POINT('Ctrl Pts',(-7.59704765299572,-23.6678559182876,
12.));
#227674=CARTESIAN_POINT('Ctrl Pts',(-7.6000913013013,-23.6430766661419,
0.));
#227675=CARTESIAN_POINT('Ctrl Pts',(-7.6000913013013,-23.6430766661419,
12.));
#227676=CARTESIAN_POINT('Ctrl Pts',(-7.60306571877806,-23.6183718346576,
0.));
#227677=CARTESIAN_POINT('Ctrl Pts',(-7.60306571877806,-23.6183718346576,
12.));
#227678=CARTESIAN_POINT('Ctrl Pts',(-7.60597112277094,-23.5937419781244,
0.));
#227679=CARTESIAN_POINT('Ctrl Pts',(-7.60597112277094,-23.5937419781244,
12.));
#227680=CARTESIAN_POINT('Ctrl Pts',(-7.608807733446,-23.5691876544243,0.));
#227681=CARTESIAN_POINT('Ctrl Pts',(-7.608807733446,-23.5691876544243,12.));
#227682=CARTESIAN_POINT('Ctrl Pts',(-7.61157577385372,-23.5447094252028,
0.));
#227683=CARTESIAN_POINT('Ctrl Pts',(-7.61157577385372,-23.5447094252028,
12.));
#227684=CARTESIAN_POINT('Ctrl Pts',(-7.61427546999299,-23.5203078560128,
0.));
#227685=CARTESIAN_POINT('Ctrl Pts',(-7.61427546999299,-23.5203078560128,
12.));
#227686=CARTESIAN_POINT('Ctrl Pts',(-7.61690705088319,-23.4959835164608,
0.));
#227687=CARTESIAN_POINT('Ctrl Pts',(-7.61690705088319,-23.4959835164608,
12.));
#227688=CARTESIAN_POINT('Ctrl Pts',(-7.61947074863978,-23.4717369803438,
0.));
#227689=CARTESIAN_POINT('Ctrl Pts',(-7.61947074863978,-23.4717369803438,
12.));
#227690=CARTESIAN_POINT('Ctrl Pts',(-7.62196679855957,-23.4475688257854,
0.));
#227691=CARTESIAN_POINT('Ctrl Pts',(-7.62196679855957,-23.4475688257854,
12.));
#227692=CARTESIAN_POINT('Ctrl Pts',(-7.62439543920055,-23.4234796353544,
0.));
#227693=CARTESIAN_POINT('Ctrl Pts',(-7.62439543920055,-23.4234796353544,
12.));
#227694=CARTESIAN_POINT('Ctrl Pts',(-7.62675691240335,-23.3994699961122,
0.));
#227695=CARTESIAN_POINT('Ctrl Pts',(-7.62675691240335,-23.3994699961122,
12.));
#227696=CARTESIAN_POINT('Ctrl Pts',(-7.62905146332598,-23.3755404996638,
0.));
#227697=CARTESIAN_POINT('Ctrl Pts',(-7.62905146332598,-23.3755404996638,
12.));
#227698=CARTESIAN_POINT('Ctrl Pts',(-7.63127934048139,-23.3516917421973,
0.));
#227699=CARTESIAN_POINT('Ctrl Pts',(-7.63127934048139,-23.3516917421973,
12.));
#227700=CARTESIAN_POINT('Ctrl Pts',(-7.63344079578163,-23.3279243245241,
0.));
#227701=CARTESIAN_POINT('Ctrl Pts',(-7.63344079578163,-23.3279243245241,
12.));
#227702=CARTESIAN_POINT('Ctrl Pts',(-7.63553608458784,-23.3042388521021,
0.));
#227703=CARTESIAN_POINT('Ctrl Pts',(-7.63553608458784,-23.3042388521021,
12.));
#227704=CARTESIAN_POINT('Ctrl Pts',(-7.63756546576375,-23.2806359350853,
0.));
#227705=CARTESIAN_POINT('Ctrl Pts',(-7.63756546576375,-23.2806359350853,
12.));
#227706=CARTESIAN_POINT('Ctrl Pts',(-7.63952920172837,-23.2571161884487,
0.));
#227707=CARTESIAN_POINT('Ctrl Pts',(-7.63952920172837,-23.2571161884487,
12.));
#227708=CARTESIAN_POINT('Ctrl Pts',(-7.64142755851508,-23.2336802320912,
0.));
#227709=CARTESIAN_POINT('Ctrl Pts',(-7.64142755851508,-23.2336802320912,
12.));
#227710=CARTESIAN_POINT('Ctrl Pts',(-7.64326080583684,-23.2103286909399,
0.));
#227711=CARTESIAN_POINT('Ctrl Pts',(-7.64326080583684,-23.2103286909399,
12.));
#227712=CARTESIAN_POINT('Ctrl Pts',(-7.64502921715483,-23.1870621950452,
0.));
#227713=CARTESIAN_POINT('Ctrl Pts',(-7.64502921715483,-23.1870621950452,
12.));
#227714=CARTESIAN_POINT('Ctrl Pts',(-7.64673306975797,-23.1638813796691,
0.));
#227715=CARTESIAN_POINT('Ctrl Pts',(-7.64673306975797,-23.1638813796691,
12.));
#227716=CARTESIAN_POINT('Ctrl Pts',(-7.64837264482929,-23.1407868853815,
0.));
#227717=CARTESIAN_POINT('Ctrl Pts',(-7.64837264482929,-23.1407868853815,
12.));
#227718=CARTESIAN_POINT('Ctrl Pts',(-7.64994822749845,-23.1177793581674,
0.));
#227719=CARTESIAN_POINT('Ctrl Pts',(-7.64994822749845,-23.1177793581674,
12.));
#227720=CARTESIAN_POINT('Ctrl Pts',(-7.65146010690465,-23.0948594495246,
0.));
#227721=CARTESIAN_POINT('Ctrl Pts',(-7.65146010690465,-23.0948594495246,
12.));
#227722=CARTESIAN_POINT('Ctrl Pts',(-7.65290857626357,-23.072027816555,
0.));
#227723=CARTESIAN_POINT('Ctrl Pts',(-7.65290857626357,-23.072027816555,
12.));
#227724=CARTESIAN_POINT('Ctrl Pts',(-7.65429393293955,-23.049285122053,
0.));
#227725=CARTESIAN_POINT('Ctrl Pts',(-7.65429393293955,-23.049285122053,
12.));
#227726=CARTESIAN_POINT('Ctrl Pts',(-7.65561647852555,-23.0266320345792,
0.));
#227727=CARTESIAN_POINT('Ctrl Pts',(-7.65561647852555,-23.0266320345792,
12.));
#227728=CARTESIAN_POINT('Ctrl Pts',(-7.6568765189133,-23.004069228582,0.));
#227729=CARTESIAN_POINT('Ctrl Pts',(-7.6568765189133,-23.004069228582,12.));
#227730=CARTESIAN_POINT('Ctrl Pts',(-7.65807436436453,-22.9815973845301,
0.));
#227731=CARTESIAN_POINT('Ctrl Pts',(-7.65807436436453,-22.9815973845301,
12.));
#227732=CARTESIAN_POINT('Ctrl Pts',(-7.65921032958912,-22.9592171890332,
0.));
#227733=CARTESIAN_POINT('Ctrl Pts',(-7.65921032958912,-22.9592171890332,
12.));
#227734=CARTESIAN_POINT('Ctrl Pts',(-7.66028473382777,-22.9369293349592,
0.));
#227735=CARTESIAN_POINT('Ctrl Pts',(-7.66028473382777,-22.9369293349592,
12.));
#227736=CARTESIAN_POINT('Ctrl Pts',(-7.661297900941,-22.9147345215418,0.));
#227737=CARTESIAN_POINT('Ctrl Pts',(-7.661297900941,-22.9147345215418,12.));
#227738=CARTESIAN_POINT('Ctrl Pts',(-7.66225015950148,-22.8926334544879,
0.));
#227739=CARTESIAN_POINT('Ctrl Pts',(-7.66225015950148,-22.8926334544879,
12.));
#227740=CARTESIAN_POINT('Ctrl Pts',(-7.66314184287334,-22.870626846128,
0.));
#227741=CARTESIAN_POINT('Ctrl Pts',(-7.66314184287334,-22.870626846128,
12.));
#227742=CARTESIAN_POINT('Ctrl Pts',(-7.66397328929805,-22.8487154155569,
0.));
#227743=CARTESIAN_POINT('Ctrl Pts',(-7.66397328929805,-22.8487154155569,
12.));
#227744=CARTESIAN_POINT('Ctrl Pts',(-7.66474484198553,-22.8268998887678,
0.));
#227745=CARTESIAN_POINT('Ctrl Pts',(-7.66474484198553,-22.8268998887678,
12.));
#227746=CARTESIAN_POINT('Ctrl Pts',(-7.66545684920988,-22.8051809987833,
0.));
#227747=CARTESIAN_POINT('Ctrl Pts',(-7.66545684920988,-22.8051809987833,
12.));
#227748=CARTESIAN_POINT('Ctrl Pts',(-7.66610966441259,-22.7835594857697,
0.));
#227749=CARTESIAN_POINT('Ctrl Pts',(-7.66610966441259,-22.7835594857697,
12.));
#227750=CARTESIAN_POINT('Ctrl Pts',(-7.66670364630273,-22.7620360971839,
0.));
#227751=CARTESIAN_POINT('Ctrl Pts',(-7.66670364630273,-22.7620360971839,
12.));
#227752=CARTESIAN_POINT('Ctrl Pts',(-7.66723915895413,-22.7406115879508,
0.));
#227753=CARTESIAN_POINT('Ctrl Pts',(-7.66723915895413,-22.7406115879508,
12.));
#227754=CARTESIAN_POINT('Ctrl Pts',(-7.6677165719101,-22.7192867206242,
0.));
#227755=CARTESIAN_POINT('Ctrl Pts',(-7.6677165719101,-22.7192867206242,
12.));
#227756=CARTESIAN_POINT('Ctrl Pts',(-7.66813626029277,-22.6980622655446,
0.));
#227757=CARTESIAN_POINT('Ctrl Pts',(-7.66813626029277,-22.6980622655446,
12.));
#227758=CARTESIAN_POINT('Ctrl Pts',(-7.66849860491763,-22.6769390009889,
0.));
#227759=CARTESIAN_POINT('Ctrl Pts',(-7.66849860491763,-22.6769390009889,
12.));
#227760=CARTESIAN_POINT('Ctrl Pts',(-7.66880399241354,-22.6559177133133,
0.));
#227761=CARTESIAN_POINT('Ctrl Pts',(-7.66880399241354,-22.6559177133133,
12.));
#227762=CARTESIAN_POINT('Ctrl Pts',(-7.66905281533745,-22.6349991971547,
0.));
#227763=CARTESIAN_POINT('Ctrl Pts',(-7.66905281533745,-22.6349991971547,
12.));
#227764=CARTESIAN_POINT('Ctrl Pts',(-7.66924547229435,-22.6141842556248,
0.));
#227765=CARTESIAN_POINT('Ctrl Pts',(-7.66924547229435,-22.6141842556248,
12.));
#227766=CARTESIAN_POINT('Ctrl Pts',(-7.66938236806241,-22.5934737004955,
0.));
#227767=CARTESIAN_POINT('Ctrl Pts',(-7.66938236806241,-22.5934737004955,
12.));
#227768=CARTESIAN_POINT('Ctrl Pts',(-7.66946391372299,-22.5728683523828,
0.));
#227769=CARTESIAN_POINT('Ctrl Pts',(-7.66946391372299,-22.5728683523828,
12.));
#227770=CARTESIAN_POINT('Ctrl Pts',(-7.66949052679672,-22.5523690409109,
0.));
#227771=CARTESIAN_POINT('Ctrl Pts',(-7.66949052679672,-22.5523690409109,
12.));
#227772=CARTESIAN_POINT('Ctrl Pts',(-7.66946263138116,-22.5319766049191,
0.));
#227773=CARTESIAN_POINT('Ctrl Pts',(-7.66946263138116,-22.5319766049191,
12.));
#227774=CARTESIAN_POINT('Ctrl Pts',(-7.66938065829083,-22.5116918927023,
0.));
#227775=CARTESIAN_POINT('Ctrl Pts',(-7.66938065829083,-22.5116918927023,
12.));
#227776=CARTESIAN_POINT('Ctrl Pts',(-7.66924504520302,-22.4915157622308,
0.));
#227777=CARTESIAN_POINT('Ctrl Pts',(-7.66924504520302,-22.4915157622308,
12.));
#227778=CARTESIAN_POINT('Ctrl Pts',(-7.66905623680836,-22.47144908137,0.));
#227779=CARTESIAN_POINT('Ctrl Pts',(-7.66905623680836,-22.47144908137,12.));
#227780=CARTESIAN_POINT('Ctrl Pts',(-7.6688146849666,-22.4514927280862,
0.));
#227781=CARTESIAN_POINT('Ctrl Pts',(-7.6688146849666,-22.4514927280862,
12.));
#227782=CARTESIAN_POINT('Ctrl Pts',(-7.66852084886746,-22.4316475906616,
0.));
#227783=CARTESIAN_POINT('Ctrl Pts',(-7.66852084886746,-22.4316475906616,
12.));
#227784=CARTESIAN_POINT('Ctrl Pts',(-7.66817519519682,-22.411914567977,
0.));
#227785=CARTESIAN_POINT('Ctrl Pts',(-7.66817519519682,-22.411914567977,
12.));
#227786=CARTESIAN_POINT('Ctrl Pts',(-7.6677781983082,-22.3922945697782,
0.));
#227787=CARTESIAN_POINT('Ctrl Pts',(-7.6677781983082,-22.3922945697782,
12.));
#227788=CARTESIAN_POINT('Ctrl Pts',(-7.66733034039887,-22.3727885169361,
0.));
#227789=CARTESIAN_POINT('Ctrl Pts',(-7.66733034039887,-22.3727885169361,
12.));
#227790=CARTESIAN_POINT('Ctrl Pts',(-7.66683211169134,-22.3533973417013,
0.));
#227791=CARTESIAN_POINT('Ctrl Pts',(-7.66683211169134,-22.3533973417013,
12.));
#227792=CARTESIAN_POINT('Ctrl Pts',(-7.66628401061906,-22.3341219879454,
0.));
#227793=CARTESIAN_POINT('Ctrl Pts',(-7.66628401061906,-22.3341219879454,
12.));
#227794=CARTESIAN_POINT('Ctrl Pts',(-7.66568654402442,-22.3149634114823,
0.));
#227795=CARTESIAN_POINT('Ctrl Pts',(-7.66568654402442,-22.3149634114823,
12.));
#227796=CARTESIAN_POINT('Ctrl Pts',(-7.66504022736263,-22.2959225803925,
0.));
#227797=CARTESIAN_POINT('Ctrl Pts',(-7.66504022736263,-22.2959225803925,
12.));
#227798=CARTESIAN_POINT('Ctrl Pts',(-7.66434558490973,-22.2770004753332,
0.));
#227799=CARTESIAN_POINT('Ctrl Pts',(-7.66434558490973,-22.2770004753332,
12.));
#227800=CARTESIAN_POINT('Ctrl Pts',(-7.66360314997662,-22.2581980898487,
0.));
#227801=CARTESIAN_POINT('Ctrl Pts',(-7.66360314997662,-22.2581980898487,
12.));
#227802=CARTESIAN_POINT('Ctrl Pts',(-7.66281346512546,-22.239516430656,
0.));
#227803=CARTESIAN_POINT('Ctrl Pts',(-7.66281346512546,-22.239516430656,
12.));
#227804=CARTESIAN_POINT('Ctrl Pts',(-7.66197708240436,-22.2209565180098,
0.));
#227805=CARTESIAN_POINT('Ctrl Pts',(-7.66197708240436,-22.2209565180098,
12.));
#227806=CARTESIAN_POINT('Ctrl Pts',(-7.66109456359292,-22.2025193860972,
0.));
#227807=CARTESIAN_POINT('Ctrl Pts',(-7.66109456359292,-22.2025193860972,
12.));
#227808=CARTESIAN_POINT('Ctrl Pts',(-7.66016648045008,-22.1842060834092,
0.));
#227809=CARTESIAN_POINT('Ctrl Pts',(-7.66016648045008,-22.1842060834092,
12.));
#227810=CARTESIAN_POINT('Ctrl Pts',(-7.65919341496926,-22.1660176731174,
0.));
#227811=CARTESIAN_POINT('Ctrl Pts',(-7.65919341496926,-22.1660176731174,
12.));
#227812=CARTESIAN_POINT('Ctrl Pts',(-7.65817595963351,-22.1479552334206,
0.));
#227813=CARTESIAN_POINT('Ctrl Pts',(-7.65817595963351,-22.1479552334206,
12.));
#227814=CARTESIAN_POINT('Ctrl Pts',(-7.65711471769407,-22.1300198579671,
0.));
#227815=CARTESIAN_POINT('Ctrl Pts',(-7.65711471769407,-22.1300198579671,
12.));
#227816=CARTESIAN_POINT('Ctrl Pts',(-7.65601030346819,-22.1122126563327,
0.));
#227817=CARTESIAN_POINT('Ctrl Pts',(-7.65601030346819,-22.1122126563327,
12.));
#227818=CARTESIAN_POINT('Ctrl Pts',(-7.65486334263651,-22.094534754469,
0.));
#227819=CARTESIAN_POINT('Ctrl Pts',(-7.65486334263651,-22.094534754469,
12.));
#227820=CARTESIAN_POINT('Ctrl Pts',(-7.65367447254945,-22.0769872951596,
0.));
#227821=CARTESIAN_POINT('Ctrl Pts',(-7.65367447254945,-22.0769872951596,
12.));
#227822=CARTESIAN_POINT('Ctrl Pts',(-7.65244434253104,-22.0595714384432,
0.));
#227823=CARTESIAN_POINT('Ctrl Pts',(-7.65244434253104,-22.0595714384432,
12.));
#227824=CARTESIAN_POINT('Ctrl Pts',(-7.65117361421347,-22.0422883621176,
0.));
#227825=CARTESIAN_POINT('Ctrl Pts',(-7.65117361421347,-22.0422883621176,
12.));
#227826=CARTESIAN_POINT('Ctrl Pts',(-7.64986296190157,-22.0251392623209,
0.));
#227827=CARTESIAN_POINT('Ctrl Pts',(-7.64986296190157,-22.0251392623209,
12.));
#227828=CARTESIAN_POINT('Ctrl Pts',(-7.64851307293346,-22.0081253540773,
0.));
#227829=CARTESIAN_POINT('Ctrl Pts',(-7.64851307293346,-22.0081253540773,
12.));
#227830=CARTESIAN_POINT('Ctrl Pts',(-7.64712464805258,-21.9912478718542,
0.));
#227831=CARTESIAN_POINT('Ctrl Pts',(-7.64712464805258,-21.9912478718542,
12.));
#227832=CARTESIAN_POINT('Ctrl Pts',(-7.64569840177359,-21.97450807008,0.));
#227833=CARTESIAN_POINT('Ctrl Pts',(-7.64569840177359,-21.97450807008,12.));
#227834=CARTESIAN_POINT('Ctrl Pts',(-7.64423506279154,-21.9579072237653,
0.));
#227835=CARTESIAN_POINT('Ctrl Pts',(-7.64423506279154,-21.9579072237653,
12.));
#227836=CARTESIAN_POINT('Ctrl Pts',(-7.64273537442707,-21.9414466292074,
0.));
#227837=CARTESIAN_POINT('Ctrl Pts',(-7.64273537442707,-21.9414466292074,
12.));
#227838=CARTESIAN_POINT('Ctrl Pts',(-7.6412000950654,-21.9251276046546,
0.));
#227839=CARTESIAN_POINT('Ctrl Pts',(-7.6412000950654,-21.9251276046546,
12.));
#227840=CARTESIAN_POINT('Ctrl Pts',(-7.63962999860917,-21.9089514909873,
0.));
#227841=CARTESIAN_POINT('Ctrl Pts',(-7.63962999860917,-21.9089514909873,
12.));
#227842=CARTESIAN_POINT('Ctrl Pts',(-7.63802587492008,-21.8929196523511,
0.));
#227843=CARTESIAN_POINT('Ctrl Pts',(-7.63802587492008,-21.8929196523511,
12.));
#227844=CARTESIAN_POINT('Ctrl Pts',(-7.63638853033368,-21.8770334769492,
0.));
#227845=CARTESIAN_POINT('Ctrl Pts',(-7.63638853033368,-21.8770334769492,
12.));
#227846=CARTESIAN_POINT('Ctrl Pts',(-7.63471878821204,-21.8612943779086,
0.));
#227847=CARTESIAN_POINT('Ctrl Pts',(-7.63471878821204,-21.8612943779086,
12.));
#227848=CARTESIAN_POINT('Ctrl Pts',(-7.63301748948936,-21.8457037941084,
0.));
#227849=CARTESIAN_POINT('Ctrl Pts',(-7.63301748948936,-21.8457037941084,
12.));
#227850=CARTESIAN_POINT('Ctrl Pts',(-7.6312854932304,-21.8302631910197,
0.));
#227851=CARTESIAN_POINT('Ctrl Pts',(-7.6312854932304,-21.8302631910197,
12.));
#227852=CARTESIAN_POINT('Ctrl Pts',(-7.62952367718151,-21.8149740615093,
0.));
#227853=CARTESIAN_POINT('Ctrl Pts',(-7.62952367718151,-21.8149740615093,
12.));
#227854=CARTESIAN_POINT('Ctrl Pts',(-7.62773293842409,-21.7998379268583,
0.));
#227855=CARTESIAN_POINT('Ctrl Pts',(-7.62773293842409,-21.7998379268583,
12.));
#227856=CARTESIAN_POINT('Ctrl Pts',(-7.62591419404521,-21.7848563378022,
0.));
#227857=CARTESIAN_POINT('Ctrl Pts',(-7.62591419404521,-21.7848563378022,
12.));
#227858=CARTESIAN_POINT('Ctrl Pts',(-7.62406838181164,-21.7700308755583,
0.));
#227859=CARTESIAN_POINT('Ctrl Pts',(-7.62406838181164,-21.7700308755583,
12.));
#227860=CARTESIAN_POINT('Ctrl Pts',(-7.62219646084226,-21.7553631528329,
0.));
#227861=CARTESIAN_POINT('Ctrl Pts',(-7.62219646084226,-21.7553631528329,
12.));
#227862=CARTESIAN_POINT('Ctrl Pts',(-7.62029941230855,-21.7408548148657,
0.));
#227863=CARTESIAN_POINT('Ctrl Pts',(-7.62029941230855,-21.7408548148657,
12.));
#227864=CARTESIAN_POINT('Ctrl Pts',(-7.61837824030542,-21.7265075407977,
0.));
#227865=CARTESIAN_POINT('Ctrl Pts',(-7.61837824030542,-21.7265075407977,
12.));
#227866=CARTESIAN_POINT('Ctrl Pts',(-7.61643397270425,-21.7123230449835,
0.));
#227867=CARTESIAN_POINT('Ctrl Pts',(-7.61643397270425,-21.7123230449835,
12.));
#227868=CARTESIAN_POINT('Ctrl Pts',(-7.61446766202787,-21.6983030783321,
0.));
#227869=CARTESIAN_POINT('Ctrl Pts',(-7.61446766202787,-21.6983030783321,
12.));
#227870=CARTESIAN_POINT('Ctrl Pts',(-7.61248038630265,-21.6844494295813,
0.));
#227871=CARTESIAN_POINT('Ctrl Pts',(-7.61248038630265,-21.6844494295813,
12.));
#227872=CARTESIAN_POINT('Ctrl Pts',(-7.6104732500095,-21.6707639267573,
0.));
#227873=CARTESIAN_POINT('Ctrl Pts',(-7.6104732500095,-21.6707639267573,
12.));
#227874=CARTESIAN_POINT('Ctrl Pts',(-7.60844738512872,-21.6572484388079,
0.));
#227875=CARTESIAN_POINT('Ctrl Pts',(-7.60844738512872,-21.6572484388079,
12.));
#227876=CARTESIAN_POINT('Ctrl Pts',(-7.60640395216359,-21.6439048771743,
0.));
#227877=CARTESIAN_POINT('Ctrl Pts',(-7.60640395216359,-21.6439048771743,
12.));
#227878=CARTESIAN_POINT('Ctrl Pts',(-7.604344141183,-21.6307351973823,0.));
#227879=CARTESIAN_POINT('Ctrl Pts',(-7.604344141183,-21.6307351973823,12.));
#227880=CARTESIAN_POINT('Ctrl Pts',(-7.60226917285432,-21.6177414005991,
0.));
#227881=CARTESIAN_POINT('Ctrl Pts',(-7.60226917285432,-21.6177414005991,
12.));
#227882=CARTESIAN_POINT('Ctrl Pts',(-7.60018029988238,-21.6049255358842,
0.));
#227883=CARTESIAN_POINT('Ctrl Pts',(-7.60018029988238,-21.6049255358842,
12.));
#227884=CARTESIAN_POINT('Ctrl Pts',(-7.59807880846193,-21.5922897024466,
0.));
#227885=CARTESIAN_POINT('Ctrl Pts',(-7.59807880846193,-21.5922897024466,
12.));
#227886=CARTESIAN_POINT('Ctrl Pts',(-7.59596601973589,-21.5798360518978,
0.));
#227887=CARTESIAN_POINT('Ctrl Pts',(-7.59596601973589,-21.5798360518978,
12.));
#227888=CARTESIAN_POINT('Ctrl Pts',(-7.5938432912493,-21.5675667904728,
0.));
#227889=CARTESIAN_POINT('Ctrl Pts',(-7.5938432912493,-21.5675667904728,
12.));
#227890=CARTESIAN_POINT('Ctrl Pts',(-7.59171201844793,-21.5554841813465,
0.));
#227891=CARTESIAN_POINT('Ctrl Pts',(-7.59171201844793,-21.5554841813465,
12.));
#227892=CARTESIAN_POINT('Ctrl Pts',(-7.58957363620026,-21.5435905470113,
0.));
#227893=CARTESIAN_POINT('Ctrl Pts',(-7.58957363620026,-21.5435905470113,
12.));
#227894=CARTESIAN_POINT('Ctrl Pts',(-7.58742962034834,-21.5318882716735,
0.));
#227895=CARTESIAN_POINT('Ctrl Pts',(-7.58742962034834,-21.5318882716735,
12.));
#227896=CARTESIAN_POINT('Ctrl Pts',(-7.58528148919114,-21.5203798035294,
0.));
#227897=CARTESIAN_POINT('Ctrl Pts',(-7.58528148919114,-21.5203798035294,
12.));
#227898=CARTESIAN_POINT('Ctrl Pts',(-7.58313080519159,-21.5090676573866,
0.));
#227899=CARTESIAN_POINT('Ctrl Pts',(-7.58313080519159,-21.5090676573866,
12.));
#227900=CARTESIAN_POINT('Ctrl Pts',(-7.5809791779073,-21.4979544192739,
0.));
#227901=CARTESIAN_POINT('Ctrl Pts',(-7.5809791779073,-21.4979544192739,
12.));
#227902=CARTESIAN_POINT('Ctrl Pts',(-7.57882826679131,-21.4870427508193,
0.));
#227903=CARTESIAN_POINT('Ctrl Pts',(-7.57882826679131,-21.4870427508193,
12.));
#227904=CARTESIAN_POINT('Ctrl Pts',(-7.57667978403003,-21.4763353936766,
0.));
#227905=CARTESIAN_POINT('Ctrl Pts',(-7.57667978403003,-21.4763353936766,
12.));
#227906=CARTESIAN_POINT('Ctrl Pts',(-7.57453549743435,-21.4658351740135,
0.));
#227907=CARTESIAN_POINT('Ctrl Pts',(-7.57453549743435,-21.4658351740135,
12.));
#227908=CARTESIAN_POINT('Ctrl Pts',(-7.57239723223521,-21.4555450053147,
0.));
#227909=CARTESIAN_POINT('Ctrl Pts',(-7.57239723223521,-21.4555450053147,
12.));
#227910=CARTESIAN_POINT('Ctrl Pts',(-7.5702668726117,-21.445467890751,0.));
#227911=CARTESIAN_POINT('Ctrl Pts',(-7.5702668726117,-21.445467890751,12.));
#227912=CARTESIAN_POINT('Ctrl Pts',(-7.56814636360842,-21.435606926151,
0.));
#227913=CARTESIAN_POINT('Ctrl Pts',(-7.56814636360842,-21.435606926151,
12.));
#227914=CARTESIAN_POINT('Ctrl Pts',(-7.56603771218706,-21.4259653015732,
0.));
#227915=CARTESIAN_POINT('Ctrl Pts',(-7.56603771218706,-21.4259653015732,
12.));
#227916=CARTESIAN_POINT('Ctrl Pts',(-7.56394299313683,-21.4165463106252,
0.));
#227917=CARTESIAN_POINT('Ctrl Pts',(-7.56394299313683,-21.4165463106252,
12.));
#227918=CARTESIAN_POINT('Ctrl Pts',(-7.56186435703622,-21.4073533630364,
0.));
#227919=CARTESIAN_POINT('Ctrl Pts',(-7.56186435703622,-21.4073533630364,
12.));
#227920=CARTESIAN_POINT('Ctrl Pts',(-7.55980403700615,-21.3983899952988,
0.));
#227921=CARTESIAN_POINT('Ctrl Pts',(-7.55980403700615,-21.3983899952988,
12.));
#227922=CARTESIAN_POINT('Ctrl Pts',(-7.55776435731422,-21.3896598842119,
0.));
#227923=CARTESIAN_POINT('Ctrl Pts',(-7.55776435731422,-21.3896598842119,
12.));
#227924=CARTESIAN_POINT('Ctrl Pts',(-7.55574773403508,-21.3811668478933,
0.));
#227925=CARTESIAN_POINT('Ctrl Pts',(-7.55574773403508,-21.3811668478933,
12.));
#227926=CARTESIAN_POINT('Ctrl Pts',(-7.55375667080032,-21.3729148390244,
0.));
#227927=CARTESIAN_POINT('Ctrl Pts',(-7.55375667080032,-21.3729148390244,
12.));
#227928=CARTESIAN_POINT('Ctrl Pts',(-7.55179375777442,-21.3649079431864,
0.));
#227929=CARTESIAN_POINT('Ctrl Pts',(-7.55179375777442,-21.3649079431864,
12.));
#227930=CARTESIAN_POINT('Ctrl Pts',(-7.54986166521307,-21.3571503685853,
0.));
#227931=CARTESIAN_POINT('Ctrl Pts',(-7.54986166521307,-21.3571503685853,
12.));
#227932=CARTESIAN_POINT('Ctrl Pts',(-7.54796316246327,-21.349646476153,
0.));
#227933=CARTESIAN_POINT('Ctrl Pts',(-7.54796316246327,-21.349646476153,
12.));
#227934=CARTESIAN_POINT('Ctrl Pts',(-7.54610114948351,-21.3424008295038,
0.));
#227935=CARTESIAN_POINT('Ctrl Pts',(-7.54610114948351,-21.3424008295038,
12.));
#227936=CARTESIAN_POINT('Ctrl Pts',(-7.54427868151269,-21.3354182340149,
0.));
#227937=CARTESIAN_POINT('Ctrl Pts',(-7.54427868151269,-21.3354182340149,
12.));
#227938=CARTESIAN_POINT('Ctrl Pts',(-7.54249900377032,-21.328703791771,
0.));
#227939=CARTESIAN_POINT('Ctrl Pts',(-7.54249900377032,-21.328703791771,
12.));
#227940=CARTESIAN_POINT('Ctrl Pts',(-7.5407655203828,-21.3222628524165,
0.));
#227941=CARTESIAN_POINT('Ctrl Pts',(-7.5407655203828,-21.3222628524165,
12.));
#227942=CARTESIAN_POINT('Ctrl Pts',(-7.53908175169899,-21.3161009456256,
0.));
#227943=CARTESIAN_POINT('Ctrl Pts',(-7.53908175169899,-21.3161009456256,
12.));
#227944=CARTESIAN_POINT('Ctrl Pts',(-7.5374512936462,-21.3102237167729,
0.));
#227945=CARTESIAN_POINT('Ctrl Pts',(-7.5374512936462,-21.3102237167729,
12.));
#227946=CARTESIAN_POINT('Ctrl Pts',(-7.53587778251743,-21.3046368712156,
0.));
#227947=CARTESIAN_POINT('Ctrl Pts',(-7.53587778251743,-21.3046368712156,
12.));
#227948=CARTESIAN_POINT('Ctrl Pts',(-7.53436505309949,-21.2993464250717,
0.));
#227949=CARTESIAN_POINT('Ctrl Pts',(-7.53436505309949,-21.2993464250717,
12.));
#227950=CARTESIAN_POINT('Ctrl Pts',(-7.53291726078527,-21.2943588989331,
0.));
#227951=CARTESIAN_POINT('Ctrl Pts',(-7.53291726078527,-21.2943588989331,
12.));
#227952=CARTESIAN_POINT('Ctrl Pts',(-7.53153906987847,-21.2896816163843,
0.));
#227953=CARTESIAN_POINT('Ctrl Pts',(-7.53153906987847,-21.2896816163843,
12.));
#227954=CARTESIAN_POINT('Ctrl Pts',(-7.53023562438221,-21.2853226580658,
0.));
#227955=CARTESIAN_POINT('Ctrl Pts',(-7.53023562438221,-21.2853226580658,
12.));
#227956=CARTESIAN_POINT('Ctrl Pts',(-7.52901217930407,-21.2812902781143,
0.));
#227957=CARTESIAN_POINT('Ctrl Pts',(-7.52901217930407,-21.2812902781143,
12.));
#227958=CARTESIAN_POINT('Ctrl Pts',(-7.52787386225344,-21.2775925269651,
0.));
#227959=CARTESIAN_POINT('Ctrl Pts',(-7.52787386225344,-21.2775925269651,
12.));
#227960=CARTESIAN_POINT('Ctrl Pts',(-7.52682526918561,-21.2742366113578,
0.));
#227961=CARTESIAN_POINT('Ctrl Pts',(-7.52682526918561,-21.2742366113578,
12.));
#227962=CARTESIAN_POINT('Ctrl Pts',(-7.52587126095544,-21.2712301573465,
0.));
#227963=CARTESIAN_POINT('Ctrl Pts',(-7.52587126095544,-21.2712301573465,
12.));
#227964=CARTESIAN_POINT('Ctrl Pts',(-7.52501770333522,-21.2685823838672,
0.));
#227965=CARTESIAN_POINT('Ctrl Pts',(-7.52501770333522,-21.2685823838672,
12.));
#227966=CARTESIAN_POINT('Ctrl Pts',(-7.52427261074264,-21.266305915706,
0.));
#227967=CARTESIAN_POINT('Ctrl Pts',(-7.52427261074264,-21.266305915706,
12.));
#227968=CARTESIAN_POINT('Ctrl Pts',(-7.52364573027521,-21.2644161259965,
0.));
#227969=CARTESIAN_POINT('Ctrl Pts',(-7.52364573027521,-21.2644161259965,
12.));
#227970=CARTESIAN_POINT('Ctrl Pts',(-7.52314642316203,-21.262927782038,
0.));
#227971=CARTESIAN_POINT('Ctrl Pts',(-7.52314642316203,-21.262927782038,
12.));
#227972=CARTESIAN_POINT('Ctrl Pts',(-7.52278182242728,-21.261852128355,
0.));
#227973=CARTESIAN_POINT('Ctrl Pts',(-7.52278182242728,-21.261852128355,
12.));
#227974=CARTESIAN_POINT('Ctrl Pts',(-7.52260064231736,-21.2613260540651,
0.));
#227975=CARTESIAN_POINT('Ctrl Pts',(-7.52260064231736,-21.2613260540651,
12.));
#227976=CARTESIAN_POINT('Ctrl Pts',(-7.52252744144958,-21.261120447486,
0.));
#227977=CARTESIAN_POINT('Ctrl Pts',(-7.52252744144958,-21.261120447486,
12.));
#227978=CARTESIAN_POINT('Ctrl Pts',(-7.52250649703992,-21.2610673466883,
0.));
#227979=CARTESIAN_POINT('Ctrl Pts',(-7.52250649703992,-21.2610673466883,
12.));
#227980=CARTESIAN_POINT('Ctrl Pts',(-7.52250298901266,-21.2610617890679,
0.));
#227981=CARTESIAN_POINT('Ctrl Pts',(-7.52250298901266,-21.2610617890679,
12.));
#227982=CARTESIAN_POINT('',(-7.36589684767345,-24.9347862158358,0.));
#227983=CARTESIAN_POINT('Ctrl Pts',(-7.36589684767345,-24.9347862158358,
0.));
#227984=CARTESIAN_POINT('Ctrl Pts',(-7.36721909028843,-24.9292275670674,
0.));
#227985=CARTESIAN_POINT('Ctrl Pts',(-7.36985593120091,-24.9181155530543,
0.));
#227986=CARTESIAN_POINT('Ctrl Pts',(-7.37378825961676,-24.901463382605,
0.));
#227987=CARTESIAN_POINT('Ctrl Pts',(-7.3789854964027,-24.8792921911115,
0.));
#227988=CARTESIAN_POINT('Ctrl Pts',(-7.38540558903621,-24.8516310625176,
0.));
#227989=CARTESIAN_POINT('Ctrl Pts',(-7.39174922585809,-24.8240228520893,
0.));
#227990=CARTESIAN_POINT('Ctrl Pts',(-7.39801641583013,-24.7964676646431,
0.));
#227991=CARTESIAN_POINT('Ctrl Pts',(-7.40420718661603,-24.7689656668983,
0.));
#227992=CARTESIAN_POINT('Ctrl Pts',(-7.41032159082382,-24.7415170994784,
0.));
#227993=CARTESIAN_POINT('Ctrl Pts',(-7.41635971481674,-24.7141222950051,
0.));
#227994=CARTESIAN_POINT('Ctrl Pts',(-7.42232167766266,-24.6867816727192,
0.));
#227995=CARTESIAN_POINT('Ctrl Pts',(-7.42820762159126,-24.6594957128756,
0.));
#227996=CARTESIAN_POINT('Ctrl Pts',(-7.43401770489524,-24.6322649369517,
0.));
#227997=CARTESIAN_POINT('Ctrl Pts',(-7.43975209375504,-24.6050898852368,
0.));
#227998=CARTESIAN_POINT('Ctrl Pts',(-7.44541095473135,-24.577971096086,
0.));
#227999=CARTESIAN_POINT('Ctrl Pts',(-7.4509944465116,-24.5509090831559,
0.));
#228000=CARTESIAN_POINT('Ctrl Pts',(-7.45650271335862,-24.5239043173072,
0.));
#228001=CARTESIAN_POINT('Ctrl Pts',(-7.46193588961464,-24.4969572391483,
0.));
#228002=CARTESIAN_POINT('Ctrl Pts',(-7.46729410308787,-24.4700682684524,
0.));
#228003=CARTESIAN_POINT('Ctrl Pts',(-7.47257747883246,-24.443237814649,
0.));
#228004=CARTESIAN_POINT('Ctrl Pts',(-7.47778614286565,-24.4164662871163,
0.));
#228005=CARTESIAN_POINT('Ctrl Pts',(-7.48292022569301,-24.3897541049254,
0.));
#228006=CARTESIAN_POINT('Ctrl Pts',(-7.48797986651909,-24.3631017084524,
0.));
#228007=CARTESIAN_POINT('Ctrl Pts',(-7.49296521252421,-24.3365095573685,
0.));
#228008=CARTESIAN_POINT('Ctrl Pts',(-7.49787641695439,-24.3099781253355,
0.));
#228009=CARTESIAN_POINT('Ctrl Pts',(-7.50271363765152,-24.2835078958973,
0.));
#228010=CARTESIAN_POINT('Ctrl Pts',(-7.50747703535134,-24.2570993577034,
0.));
#228011=CARTESIAN_POINT('Ctrl Pts',(-7.51216677222181,-24.2307530003887,
0.));
#228012=CARTESIAN_POINT('Ctrl Pts',(-7.51678300997949,-24.2044693092349,
0.));
#228013=CARTESIAN_POINT('Ctrl Pts',(-7.52132590953802,-24.1782487641594,
0.));
#228014=CARTESIAN_POINT('Ctrl Pts',(-7.52579563201424,-24.1520918425364,
0.));
#228015=CARTESIAN_POINT('Ctrl Pts',(-7.53019233935502,-24.1259990209207,
0.));
#228016=CARTESIAN_POINT('Ctrl Pts',(-7.53451619514649,-24.0999707772642,
0.));
#228017=CARTESIAN_POINT('Ctrl Pts',(-7.53876736531014,-24.0740075927985,
0.));
#228018=CARTESIAN_POINT('Ctrl Pts',(-7.54294601896145,-24.0481099543353,
0.));
#228019=CARTESIAN_POINT('Ctrl Pts',(-7.5470523288591,-24.022278355453,0.));
#228020=CARTESIAN_POINT('Ctrl Pts',(-7.55108647097441,-23.9965132953185,
0.));
#228021=CARTESIAN_POINT('Ctrl Pts',(-7.55504862424812,-23.9708152779884,
0.));
#228022=CARTESIAN_POINT('Ctrl Pts',(-7.55893897027683,-23.9451848115,0.));
#228023=CARTESIAN_POINT('Ctrl Pts',(-7.56275769304773,-23.9196224070759,
0.));
#228024=CARTESIAN_POINT('Ctrl Pts',(-7.56650497863792,-23.8941285782003,
0.));
#228025=CARTESIAN_POINT('Ctrl Pts',(-7.57018101500711,-23.8687038399597,
0.));
#228026=CARTESIAN_POINT('Ctrl Pts',(-7.57378599219817,-23.8433487096134,
0.));
#228027=CARTESIAN_POINT('Ctrl Pts',(-7.57732010249066,-23.8180637069977,
0.));
#228028=CARTESIAN_POINT('Ctrl Pts',(-7.58078354058212,-23.7928493549908,
0.));
#228029=CARTESIAN_POINT('Ctrl Pts',(-7.58417650376272,-23.7677061799376,
0.));
#228030=CARTESIAN_POINT('Ctrl Pts',(-7.58749919210832,-23.7426347121006,
0.));
#228031=CARTESIAN_POINT('Ctrl Pts',(-7.59075180865327,-23.7176354860457,
0.));
#228032=CARTESIAN_POINT('Ctrl Pts',(-7.59393455934042,-23.6927090405067,
0.));
#228033=CARTESIAN_POINT('Ctrl Pts',(-7.59704765299572,-23.6678559182876,
0.));
#228034=CARTESIAN_POINT('Ctrl Pts',(-7.6000913013013,-23.6430766661419,
0.));
#228035=CARTESIAN_POINT('Ctrl Pts',(-7.60306571877806,-23.6183718346576,
0.));
#228036=CARTESIAN_POINT('Ctrl Pts',(-7.60597112277094,-23.5937419781244,
0.));
#228037=CARTESIAN_POINT('Ctrl Pts',(-7.608807733446,-23.5691876544243,0.));
#228038=CARTESIAN_POINT('Ctrl Pts',(-7.61157577385372,-23.5447094252028,
0.));
#228039=CARTESIAN_POINT('Ctrl Pts',(-7.61427546999299,-23.5203078560128,
0.));
#228040=CARTESIAN_POINT('Ctrl Pts',(-7.61690705088319,-23.4959835164608,
0.));
#228041=CARTESIAN_POINT('Ctrl Pts',(-7.61947074863978,-23.4717369803438,
0.));
#228042=CARTESIAN_POINT('Ctrl Pts',(-7.62196679855957,-23.4475688257854,
0.));
#228043=CARTESIAN_POINT('Ctrl Pts',(-7.62439543920055,-23.4234796353544,
0.));
#228044=CARTESIAN_POINT('Ctrl Pts',(-7.62675691240335,-23.3994699961122,
0.));
#228045=CARTESIAN_POINT('Ctrl Pts',(-7.62905146332598,-23.3755404996638,
0.));
#228046=CARTESIAN_POINT('Ctrl Pts',(-7.63127934048139,-23.3516917421973,
0.));
#228047=CARTESIAN_POINT('Ctrl Pts',(-7.63344079578163,-23.3279243245241,
0.));
#228048=CARTESIAN_POINT('Ctrl Pts',(-7.63553608458784,-23.3042388521021,
0.));
#228049=CARTESIAN_POINT('Ctrl Pts',(-7.63756546576375,-23.2806359350853,
0.));
#228050=CARTESIAN_POINT('Ctrl Pts',(-7.63952920172837,-23.2571161884487,
0.));
#228051=CARTESIAN_POINT('Ctrl Pts',(-7.64142755851508,-23.2336802320912,
0.));
#228052=CARTESIAN_POINT('Ctrl Pts',(-7.64326080583684,-23.2103286909399,
0.));
#228053=CARTESIAN_POINT('Ctrl Pts',(-7.64502921715483,-23.1870621950452,
0.));
#228054=CARTESIAN_POINT('Ctrl Pts',(-7.64673306975797,-23.1638813796691,
0.));
#228055=CARTESIAN_POINT('Ctrl Pts',(-7.64837264482929,-23.1407868853815,
0.));
#228056=CARTESIAN_POINT('Ctrl Pts',(-7.64994822749845,-23.1177793581674,
0.));
#228057=CARTESIAN_POINT('Ctrl Pts',(-7.65146010690465,-23.0948594495246,
0.));
#228058=CARTESIAN_POINT('Ctrl Pts',(-7.65290857626357,-23.072027816555,
0.));
#228059=CARTESIAN_POINT('Ctrl Pts',(-7.65429393293955,-23.049285122053,
0.));
#228060=CARTESIAN_POINT('Ctrl Pts',(-7.65561647852555,-23.0266320345792,
0.));
#228061=CARTESIAN_POINT('Ctrl Pts',(-7.6568765189133,-23.004069228582,0.));
#228062=CARTESIAN_POINT('Ctrl Pts',(-7.65807436436453,-22.9815973845301,
0.));
#228063=CARTESIAN_POINT('Ctrl Pts',(-7.65921032958912,-22.9592171890332,
0.));
#228064=CARTESIAN_POINT('Ctrl Pts',(-7.66028473382777,-22.9369293349592,
0.));
#228065=CARTESIAN_POINT('Ctrl Pts',(-7.661297900941,-22.9147345215418,0.));
#228066=CARTESIAN_POINT('Ctrl Pts',(-7.66225015950148,-22.8926334544879,
0.));
#228067=CARTESIAN_POINT('Ctrl Pts',(-7.66314184287334,-22.870626846128,
0.));
#228068=CARTESIAN_POINT('Ctrl Pts',(-7.66397328929805,-22.8487154155569,
0.));
#228069=CARTESIAN_POINT('Ctrl Pts',(-7.66474484198553,-22.8268998887678,
0.));
#228070=CARTESIAN_POINT('Ctrl Pts',(-7.66545684920988,-22.8051809987833,
0.));
#228071=CARTESIAN_POINT('Ctrl Pts',(-7.66610966441259,-22.7835594857697,
0.));
#228072=CARTESIAN_POINT('Ctrl Pts',(-7.66670364630273,-22.7620360971839,
0.));
#228073=CARTESIAN_POINT('Ctrl Pts',(-7.66723915895413,-22.7406115879508,
0.));
#228074=CARTESIAN_POINT('Ctrl Pts',(-7.6677165719101,-22.7192867206242,
0.));
#228075=CARTESIAN_POINT('Ctrl Pts',(-7.66813626029277,-22.6980622655446,
0.));
#228076=CARTESIAN_POINT('Ctrl Pts',(-7.66849860491763,-22.6769390009889,
0.));
#228077=CARTESIAN_POINT('Ctrl Pts',(-7.66880399241354,-22.6559177133133,
0.));
#228078=CARTESIAN_POINT('Ctrl Pts',(-7.66905281533745,-22.6349991971547,
0.));
#228079=CARTESIAN_POINT('Ctrl Pts',(-7.66924547229435,-22.6141842556248,
0.));
#228080=CARTESIAN_POINT('Ctrl Pts',(-7.66938236806241,-22.5934737004955,
0.));
#228081=CARTESIAN_POINT('Ctrl Pts',(-7.66946391372299,-22.5728683523828,
0.));
#228082=CARTESIAN_POINT('Ctrl Pts',(-7.66949052679672,-22.5523690409109,
0.));
#228083=CARTESIAN_POINT('Ctrl Pts',(-7.66946263138116,-22.5319766049191,
0.));
#228084=CARTESIAN_POINT('Ctrl Pts',(-7.66938065829083,-22.5116918927023,
0.));
#228085=CARTESIAN_POINT('Ctrl Pts',(-7.66924504520302,-22.4915157622308,
0.));
#228086=CARTESIAN_POINT('Ctrl Pts',(-7.66905623680836,-22.47144908137,0.));
#228087=CARTESIAN_POINT('Ctrl Pts',(-7.6688146849666,-22.4514927280862,
0.));
#228088=CARTESIAN_POINT('Ctrl Pts',(-7.66852084886746,-22.4316475906616,
0.));
#228089=CARTESIAN_POINT('Ctrl Pts',(-7.66817519519682,-22.411914567977,
0.));
#228090=CARTESIAN_POINT('Ctrl Pts',(-7.6677781983082,-22.3922945697782,
0.));
#228091=CARTESIAN_POINT('Ctrl Pts',(-7.66733034039887,-22.3727885169361,
0.));
#228092=CARTESIAN_POINT('Ctrl Pts',(-7.66683211169134,-22.3533973417013,
0.));
#228093=CARTESIAN_POINT('Ctrl Pts',(-7.66628401061906,-22.3341219879454,
0.));
#228094=CARTESIAN_POINT('Ctrl Pts',(-7.66568654402442,-22.3149634114823,
0.));
#228095=CARTESIAN_POINT('Ctrl Pts',(-7.66504022736263,-22.2959225803925,
0.));
#228096=CARTESIAN_POINT('Ctrl Pts',(-7.66434558490973,-22.2770004753332,
0.));
#228097=CARTESIAN_POINT('Ctrl Pts',(-7.66360314997662,-22.2581980898487,
0.));
#228098=CARTESIAN_POINT('Ctrl Pts',(-7.66281346512546,-22.239516430656,
0.));
#228099=CARTESIAN_POINT('Ctrl Pts',(-7.66197708240436,-22.2209565180098,
0.));
#228100=CARTESIAN_POINT('Ctrl Pts',(-7.66109456359292,-22.2025193860972,
0.));
#228101=CARTESIAN_POINT('Ctrl Pts',(-7.66016648045008,-22.1842060834092,
0.));
#228102=CARTESIAN_POINT('Ctrl Pts',(-7.65919341496926,-22.1660176731174,
0.));
#228103=CARTESIAN_POINT('Ctrl Pts',(-7.65817595963351,-22.1479552334206,
0.));
#228104=CARTESIAN_POINT('Ctrl Pts',(-7.65711471769407,-22.1300198579671,
0.));
#228105=CARTESIAN_POINT('Ctrl Pts',(-7.65601030346819,-22.1122126563327,
0.));
#228106=CARTESIAN_POINT('Ctrl Pts',(-7.65486334263651,-22.094534754469,
0.));
#228107=CARTESIAN_POINT('Ctrl Pts',(-7.65367447254945,-22.0769872951596,
0.));
#228108=CARTESIAN_POINT('Ctrl Pts',(-7.65244434253104,-22.0595714384432,
0.));
#228109=CARTESIAN_POINT('Ctrl Pts',(-7.65117361421347,-22.0422883621176,
0.));
#228110=CARTESIAN_POINT('Ctrl Pts',(-7.64986296190157,-22.0251392623209,
0.));
#228111=CARTESIAN_POINT('Ctrl Pts',(-7.64851307293346,-22.0081253540773,
0.));
#228112=CARTESIAN_POINT('Ctrl Pts',(-7.64712464805258,-21.9912478718542,
0.));
#228113=CARTESIAN_POINT('Ctrl Pts',(-7.64569840177359,-21.97450807008,0.));
#228114=CARTESIAN_POINT('Ctrl Pts',(-7.64423506279154,-21.9579072237653,
0.));
#228115=CARTESIAN_POINT('Ctrl Pts',(-7.64273537442707,-21.9414466292074,
0.));
#228116=CARTESIAN_POINT('Ctrl Pts',(-7.6412000950654,-21.9251276046546,
0.));
#228117=CARTESIAN_POINT('Ctrl Pts',(-7.63962999860917,-21.9089514909873,
0.));
#228118=CARTESIAN_POINT('Ctrl Pts',(-7.63802587492008,-21.8929196523511,
0.));
#228119=CARTESIAN_POINT('Ctrl Pts',(-7.63638853033368,-21.8770334769492,
0.));
#228120=CARTESIAN_POINT('Ctrl Pts',(-7.63471878821204,-21.8612943779086,
0.));
#228121=CARTESIAN_POINT('Ctrl Pts',(-7.63301748948936,-21.8457037941084,
0.));
#228122=CARTESIAN_POINT('Ctrl Pts',(-7.6312854932304,-21.8302631910197,
0.));
#228123=CARTESIAN_POINT('Ctrl Pts',(-7.62952367718151,-21.8149740615093,
0.));
#228124=CARTESIAN_POINT('Ctrl Pts',(-7.62773293842409,-21.7998379268583,
0.));
#228125=CARTESIAN_POINT('Ctrl Pts',(-7.62591419404521,-21.7848563378022,
0.));
#228126=CARTESIAN_POINT('Ctrl Pts',(-7.62406838181164,-21.7700308755583,
0.));
#228127=CARTESIAN_POINT('Ctrl Pts',(-7.62219646084226,-21.7553631528329,
0.));
#228128=CARTESIAN_POINT('Ctrl Pts',(-7.62029941230855,-21.7408548148657,
0.));
#228129=CARTESIAN_POINT('Ctrl Pts',(-7.61837824030542,-21.7265075407977,
0.));
#228130=CARTESIAN_POINT('Ctrl Pts',(-7.61643397270425,-21.7123230449835,
0.));
#228131=CARTESIAN_POINT('Ctrl Pts',(-7.61446766202787,-21.6983030783321,
0.));
#228132=CARTESIAN_POINT('Ctrl Pts',(-7.61248038630265,-21.6844494295813,
0.));
#228133=CARTESIAN_POINT('Ctrl Pts',(-7.6104732500095,-21.6707639267573,
0.));
#228134=CARTESIAN_POINT('Ctrl Pts',(-7.60844738512872,-21.6572484388079,
0.));
#228135=CARTESIAN_POINT('Ctrl Pts',(-7.60640395216359,-21.6439048771743,
0.));
#228136=CARTESIAN_POINT('Ctrl Pts',(-7.604344141183,-21.6307351973823,0.));
#228137=CARTESIAN_POINT('Ctrl Pts',(-7.60226917285432,-21.6177414005991,
0.));
#228138=CARTESIAN_POINT('Ctrl Pts',(-7.60018029988238,-21.6049255358842,
0.));
#228139=CARTESIAN_POINT('Ctrl Pts',(-7.59807880846193,-21.5922897024466,
0.));
#228140=CARTESIAN_POINT('Ctrl Pts',(-7.59596601973589,-21.5798360518978,
0.));
#228141=CARTESIAN_POINT('Ctrl Pts',(-7.5938432912493,-21.5675667904728,
0.));
#228142=CARTESIAN_POINT('Ctrl Pts',(-7.59171201844793,-21.5554841813465,
0.));
#228143=CARTESIAN_POINT('Ctrl Pts',(-7.58957363620026,-21.5435905470113,
0.));
#228144=CARTESIAN_POINT('Ctrl Pts',(-7.58742962034834,-21.5318882716735,
0.));
#228145=CARTESIAN_POINT('Ctrl Pts',(-7.58528148919114,-21.5203798035294,
0.));
#228146=CARTESIAN_POINT('Ctrl Pts',(-7.58313080519159,-21.5090676573866,
0.));
#228147=CARTESIAN_POINT('Ctrl Pts',(-7.5809791779073,-21.4979544192739,
0.));
#228148=CARTESIAN_POINT('Ctrl Pts',(-7.57882826679131,-21.4870427508193,
0.));
#228149=CARTESIAN_POINT('Ctrl Pts',(-7.57667978403003,-21.4763353936766,
0.));
#228150=CARTESIAN_POINT('Ctrl Pts',(-7.57453549743435,-21.4658351740135,
0.));
#228151=CARTESIAN_POINT('Ctrl Pts',(-7.57239723223521,-21.4555450053147,
0.));
#228152=CARTESIAN_POINT('Ctrl Pts',(-7.5702668726117,-21.445467890751,0.));
#228153=CARTESIAN_POINT('Ctrl Pts',(-7.56814636360842,-21.435606926151,
0.));
#228154=CARTESIAN_POINT('Ctrl Pts',(-7.56603771218706,-21.4259653015732,
0.));
#228155=CARTESIAN_POINT('Ctrl Pts',(-7.56394299313683,-21.4165463106252,
0.));
#228156=CARTESIAN_POINT('Ctrl Pts',(-7.56186435703622,-21.4073533630364,
0.));
#228157=CARTESIAN_POINT('Ctrl Pts',(-7.55980403700615,-21.3983899952988,
0.));
#228158=CARTESIAN_POINT('Ctrl Pts',(-7.55776435731422,-21.3896598842119,
0.));
#228159=CARTESIAN_POINT('Ctrl Pts',(-7.55574773403508,-21.3811668478933,
0.));
#228160=CARTESIAN_POINT('Ctrl Pts',(-7.55375667080032,-21.3729148390244,
0.));
#228161=CARTESIAN_POINT('Ctrl Pts',(-7.55179375777442,-21.3649079431864,
0.));
#228162=CARTESIAN_POINT('Ctrl Pts',(-7.54986166521307,-21.3571503685853,
0.));
#228163=CARTESIAN_POINT('Ctrl Pts',(-7.54796316246327,-21.349646476153,
0.));
#228164=CARTESIAN_POINT('Ctrl Pts',(-7.54610114948351,-21.3424008295038,
0.));
#228165=CARTESIAN_POINT('Ctrl Pts',(-7.54427868151269,-21.3354182340149,
0.));
#228166=CARTESIAN_POINT('Ctrl Pts',(-7.54249900377032,-21.328703791771,
0.));
#228167=CARTESIAN_POINT('Ctrl Pts',(-7.5407655203828,-21.3222628524165,
0.));
#228168=CARTESIAN_POINT('Ctrl Pts',(-7.53908175169899,-21.3161009456256,
0.));
#228169=CARTESIAN_POINT('Ctrl Pts',(-7.5374512936462,-21.3102237167729,
0.));
#228170=CARTESIAN_POINT('Ctrl Pts',(-7.53587778251743,-21.3046368712156,
0.));
#228171=CARTESIAN_POINT('Ctrl Pts',(-7.53436505309949,-21.2993464250717,
0.));
#228172=CARTESIAN_POINT('Ctrl Pts',(-7.53291726078527,-21.2943588989331,
0.));
#228173=CARTESIAN_POINT('Ctrl Pts',(-7.53153906987847,-21.2896816163843,
0.));
#228174=CARTESIAN_POINT('Ctrl Pts',(-7.53023562438221,-21.2853226580658,
0.));
#228175=CARTESIAN_POINT('Ctrl Pts',(-7.52901217930407,-21.2812902781143,
0.));
#228176=CARTESIAN_POINT('Ctrl Pts',(-7.52787386225344,-21.2775925269651,
0.));
#228177=CARTESIAN_POINT('Ctrl Pts',(-7.52682526918561,-21.2742366113578,
0.));
#228178=CARTESIAN_POINT('Ctrl Pts',(-7.52587126095544,-21.2712301573465,
0.));
#228179=CARTESIAN_POINT('Ctrl Pts',(-7.52501770333522,-21.2685823838672,
0.));
#228180=CARTESIAN_POINT('Ctrl Pts',(-7.52427261074264,-21.266305915706,
0.));
#228181=CARTESIAN_POINT('Ctrl Pts',(-7.52364573027521,-21.2644161259965,
0.));
#228182=CARTESIAN_POINT('Ctrl Pts',(-7.52314642316203,-21.262927782038,
0.));
#228183=CARTESIAN_POINT('Ctrl Pts',(-7.52278182242728,-21.261852128355,
0.));
#228184=CARTESIAN_POINT('Ctrl Pts',(-7.52260064231736,-21.2613260540651,
0.));
#228185=CARTESIAN_POINT('Ctrl Pts',(-7.52252744144958,-21.261120447486,
0.));
#228186=CARTESIAN_POINT('Ctrl Pts',(-7.52250649703992,-21.2610673466883,
0.));
#228187=CARTESIAN_POINT('Ctrl Pts',(-7.52250298901266,-21.2610617890679,
0.));
#228188=CARTESIAN_POINT('',(-7.36589684767345,-24.9347862158358,12.));
#228189=CARTESIAN_POINT('',(-7.36589684767345,-24.9347862158358,0.));
#228190=CARTESIAN_POINT('Ctrl Pts',(-7.52250298901266,-21.2610617890679,
12.));
#228191=CARTESIAN_POINT('Ctrl Pts',(-7.52250649703992,-21.2610673466883,
12.));
#228192=CARTESIAN_POINT('Ctrl Pts',(-7.52252744144958,-21.261120447486,
12.));
#228193=CARTESIAN_POINT('Ctrl Pts',(-7.52260064231736,-21.2613260540651,
12.));
#228194=CARTESIAN_POINT('Ctrl Pts',(-7.52278182242728,-21.261852128355,
12.));
#228195=CARTESIAN_POINT('Ctrl Pts',(-7.52314642316203,-21.262927782038,
12.));
#228196=CARTESIAN_POINT('Ctrl Pts',(-7.52364573027521,-21.2644161259965,
12.));
#228197=CARTESIAN_POINT('Ctrl Pts',(-7.52427261074264,-21.266305915706,
12.));
#228198=CARTESIAN_POINT('Ctrl Pts',(-7.52501770333522,-21.2685823838672,
12.));
#228199=CARTESIAN_POINT('Ctrl Pts',(-7.52587126095544,-21.2712301573465,
12.));
#228200=CARTESIAN_POINT('Ctrl Pts',(-7.52682526918561,-21.2742366113578,
12.));
#228201=CARTESIAN_POINT('Ctrl Pts',(-7.52787386225344,-21.2775925269651,
12.));
#228202=CARTESIAN_POINT('Ctrl Pts',(-7.52901217930407,-21.2812902781143,
12.));
#228203=CARTESIAN_POINT('Ctrl Pts',(-7.53023562438221,-21.2853226580658,
12.));
#228204=CARTESIAN_POINT('Ctrl Pts',(-7.53153906987847,-21.2896816163843,
12.));
#228205=CARTESIAN_POINT('Ctrl Pts',(-7.53291726078527,-21.2943588989331,
12.));
#228206=CARTESIAN_POINT('Ctrl Pts',(-7.53436505309949,-21.2993464250717,
12.));
#228207=CARTESIAN_POINT('Ctrl Pts',(-7.53587778251743,-21.3046368712156,
12.));
#228208=CARTESIAN_POINT('Ctrl Pts',(-7.5374512936462,-21.3102237167729,
12.));
#228209=CARTESIAN_POINT('Ctrl Pts',(-7.53908175169899,-21.3161009456256,
12.));
#228210=CARTESIAN_POINT('Ctrl Pts',(-7.5407655203828,-21.3222628524165,
12.));
#228211=CARTESIAN_POINT('Ctrl Pts',(-7.54249900377032,-21.328703791771,
12.));
#228212=CARTESIAN_POINT('Ctrl Pts',(-7.54427868151269,-21.3354182340149,
12.));
#228213=CARTESIAN_POINT('Ctrl Pts',(-7.54610114948351,-21.3424008295038,
12.));
#228214=CARTESIAN_POINT('Ctrl Pts',(-7.54796316246327,-21.349646476153,
12.));
#228215=CARTESIAN_POINT('Ctrl Pts',(-7.54986166521307,-21.3571503685853,
12.));
#228216=CARTESIAN_POINT('Ctrl Pts',(-7.55179375777442,-21.3649079431864,
12.));
#228217=CARTESIAN_POINT('Ctrl Pts',(-7.55375667080032,-21.3729148390244,
12.));
#228218=CARTESIAN_POINT('Ctrl Pts',(-7.55574773403508,-21.3811668478933,
12.));
#228219=CARTESIAN_POINT('Ctrl Pts',(-7.55776435731422,-21.3896598842119,
12.));
#228220=CARTESIAN_POINT('Ctrl Pts',(-7.55980403700615,-21.3983899952988,
12.));
#228221=CARTESIAN_POINT('Ctrl Pts',(-7.56186435703622,-21.4073533630364,
12.));
#228222=CARTESIAN_POINT('Ctrl Pts',(-7.56394299313683,-21.4165463106252,
12.));
#228223=CARTESIAN_POINT('Ctrl Pts',(-7.56603771218706,-21.4259653015732,
12.));
#228224=CARTESIAN_POINT('Ctrl Pts',(-7.56814636360842,-21.435606926151,
12.));
#228225=CARTESIAN_POINT('Ctrl Pts',(-7.5702668726117,-21.445467890751,12.));
#228226=CARTESIAN_POINT('Ctrl Pts',(-7.57239723223521,-21.4555450053147,
12.));
#228227=CARTESIAN_POINT('Ctrl Pts',(-7.57453549743435,-21.4658351740135,
12.));
#228228=CARTESIAN_POINT('Ctrl Pts',(-7.57667978403003,-21.4763353936766,
12.));
#228229=CARTESIAN_POINT('Ctrl Pts',(-7.57882826679131,-21.4870427508193,
12.));
#228230=CARTESIAN_POINT('Ctrl Pts',(-7.5809791779073,-21.4979544192739,
12.));
#228231=CARTESIAN_POINT('Ctrl Pts',(-7.58313080519159,-21.5090676573866,
12.));
#228232=CARTESIAN_POINT('Ctrl Pts',(-7.58528148919114,-21.5203798035294,
12.));
#228233=CARTESIAN_POINT('Ctrl Pts',(-7.58742962034834,-21.5318882716735,
12.));
#228234=CARTESIAN_POINT('Ctrl Pts',(-7.58957363620026,-21.5435905470113,
12.));
#228235=CARTESIAN_POINT('Ctrl Pts',(-7.59171201844793,-21.5554841813465,
12.));
#228236=CARTESIAN_POINT('Ctrl Pts',(-7.5938432912493,-21.5675667904728,
12.));
#228237=CARTESIAN_POINT('Ctrl Pts',(-7.59596601973589,-21.5798360518978,
12.));
#228238=CARTESIAN_POINT('Ctrl Pts',(-7.59807880846193,-21.5922897024466,
12.));
#228239=CARTESIAN_POINT('Ctrl Pts',(-7.60018029988238,-21.6049255358842,
12.));
#228240=CARTESIAN_POINT('Ctrl Pts',(-7.60226917285432,-21.6177414005991,
12.));
#228241=CARTESIAN_POINT('Ctrl Pts',(-7.604344141183,-21.6307351973823,12.));
#228242=CARTESIAN_POINT('Ctrl Pts',(-7.60640395216359,-21.6439048771743,
12.));
#228243=CARTESIAN_POINT('Ctrl Pts',(-7.60844738512872,-21.6572484388079,
12.));
#228244=CARTESIAN_POINT('Ctrl Pts',(-7.6104732500095,-21.6707639267573,
12.));
#228245=CARTESIAN_POINT('Ctrl Pts',(-7.61248038630265,-21.6844494295813,
12.));
#228246=CARTESIAN_POINT('Ctrl Pts',(-7.61446766202787,-21.6983030783321,
12.));
#228247=CARTESIAN_POINT('Ctrl Pts',(-7.61643397270425,-21.7123230449835,
12.));
#228248=CARTESIAN_POINT('Ctrl Pts',(-7.61837824030542,-21.7265075407977,
12.));
#228249=CARTESIAN_POINT('Ctrl Pts',(-7.62029941230855,-21.7408548148657,
12.));
#228250=CARTESIAN_POINT('Ctrl Pts',(-7.62219646084226,-21.7553631528329,
12.));
#228251=CARTESIAN_POINT('Ctrl Pts',(-7.62406838181164,-21.7700308755583,
12.));
#228252=CARTESIAN_POINT('Ctrl Pts',(-7.62591419404521,-21.7848563378022,
12.));
#228253=CARTESIAN_POINT('Ctrl Pts',(-7.62773293842409,-21.7998379268583,
12.));
#228254=CARTESIAN_POINT('Ctrl Pts',(-7.62952367718151,-21.8149740615093,
12.));
#228255=CARTESIAN_POINT('Ctrl Pts',(-7.6312854932304,-21.8302631910197,
12.));
#228256=CARTESIAN_POINT('Ctrl Pts',(-7.63301748948936,-21.8457037941084,
12.));
#228257=CARTESIAN_POINT('Ctrl Pts',(-7.63471878821204,-21.8612943779086,
12.));
#228258=CARTESIAN_POINT('Ctrl Pts',(-7.63638853033368,-21.8770334769492,
12.));
#228259=CARTESIAN_POINT('Ctrl Pts',(-7.63802587492008,-21.8929196523511,
12.));
#228260=CARTESIAN_POINT('Ctrl Pts',(-7.63962999860917,-21.9089514909873,
12.));
#228261=CARTESIAN_POINT('Ctrl Pts',(-7.6412000950654,-21.9251276046546,
12.));
#228262=CARTESIAN_POINT('Ctrl Pts',(-7.64273537442707,-21.9414466292074,
12.));
#228263=CARTESIAN_POINT('Ctrl Pts',(-7.64423506279154,-21.9579072237653,
12.));
#228264=CARTESIAN_POINT('Ctrl Pts',(-7.64569840177359,-21.97450807008,12.));
#228265=CARTESIAN_POINT('Ctrl Pts',(-7.64712464805258,-21.9912478718542,
12.));
#228266=CARTESIAN_POINT('Ctrl Pts',(-7.64851307293346,-22.0081253540773,
12.));
#228267=CARTESIAN_POINT('Ctrl Pts',(-7.64986296190157,-22.0251392623209,
12.));
#228268=CARTESIAN_POINT('Ctrl Pts',(-7.65117361421347,-22.0422883621176,
12.));
#228269=CARTESIAN_POINT('Ctrl Pts',(-7.65244434253104,-22.0595714384432,
12.));
#228270=CARTESIAN_POINT('Ctrl Pts',(-7.65367447254945,-22.0769872951596,
12.));
#228271=CARTESIAN_POINT('Ctrl Pts',(-7.65486334263651,-22.094534754469,
12.));
#228272=CARTESIAN_POINT('Ctrl Pts',(-7.65601030346819,-22.1122126563327,
12.));
#228273=CARTESIAN_POINT('Ctrl Pts',(-7.65711471769407,-22.1300198579671,
12.));
#228274=CARTESIAN_POINT('Ctrl Pts',(-7.65817595963351,-22.1479552334206,
12.));
#228275=CARTESIAN_POINT('Ctrl Pts',(-7.65919341496926,-22.1660176731174,
12.));
#228276=CARTESIAN_POINT('Ctrl Pts',(-7.66016648045008,-22.1842060834092,
12.));
#228277=CARTESIAN_POINT('Ctrl Pts',(-7.66109456359292,-22.2025193860972,
12.));
#228278=CARTESIAN_POINT('Ctrl Pts',(-7.66197708240436,-22.2209565180098,
12.));
#228279=CARTESIAN_POINT('Ctrl Pts',(-7.66281346512546,-22.239516430656,
12.));
#228280=CARTESIAN_POINT('Ctrl Pts',(-7.66360314997662,-22.2581980898487,
12.));
#228281=CARTESIAN_POINT('Ctrl Pts',(-7.66434558490973,-22.2770004753332,
12.));
#228282=CARTESIAN_POINT('Ctrl Pts',(-7.66504022736263,-22.2959225803925,
12.));
#228283=CARTESIAN_POINT('Ctrl Pts',(-7.66568654402442,-22.3149634114823,
12.));
#228284=CARTESIAN_POINT('Ctrl Pts',(-7.66628401061906,-22.3341219879454,
12.));
#228285=CARTESIAN_POINT('Ctrl Pts',(-7.66683211169134,-22.3533973417013,
12.));
#228286=CARTESIAN_POINT('Ctrl Pts',(-7.66733034039887,-22.3727885169361,
12.));
#228287=CARTESIAN_POINT('Ctrl Pts',(-7.6677781983082,-22.3922945697782,
12.));
#228288=CARTESIAN_POINT('Ctrl Pts',(-7.66817519519682,-22.411914567977,
12.));
#228289=CARTESIAN_POINT('Ctrl Pts',(-7.66852084886746,-22.4316475906616,
12.));
#228290=CARTESIAN_POINT('Ctrl Pts',(-7.6688146849666,-22.4514927280862,
12.));
#228291=CARTESIAN_POINT('Ctrl Pts',(-7.66905623680836,-22.47144908137,12.));
#228292=CARTESIAN_POINT('Ctrl Pts',(-7.66924504520302,-22.4915157622308,
12.));
#228293=CARTESIAN_POINT('Ctrl Pts',(-7.66938065829083,-22.5116918927023,
12.));
#228294=CARTESIAN_POINT('Ctrl Pts',(-7.66946263138116,-22.5319766049191,
12.));
#228295=CARTESIAN_POINT('Ctrl Pts',(-7.66949052679672,-22.5523690409109,
12.));
#228296=CARTESIAN_POINT('Ctrl Pts',(-7.66946391372299,-22.5728683523828,
12.));
#228297=CARTESIAN_POINT('Ctrl Pts',(-7.66938236806241,-22.5934737004955,
12.));
#228298=CARTESIAN_POINT('Ctrl Pts',(-7.66924547229435,-22.6141842556248,
12.));
#228299=CARTESIAN_POINT('Ctrl Pts',(-7.66905281533745,-22.6349991971547,
12.));
#228300=CARTESIAN_POINT('Ctrl Pts',(-7.66880399241354,-22.6559177133133,
12.));
#228301=CARTESIAN_POINT('Ctrl Pts',(-7.66849860491763,-22.6769390009889,
12.));
#228302=CARTESIAN_POINT('Ctrl Pts',(-7.66813626029277,-22.6980622655446,
12.));
#228303=CARTESIAN_POINT('Ctrl Pts',(-7.6677165719101,-22.7192867206242,
12.));
#228304=CARTESIAN_POINT('Ctrl Pts',(-7.66723915895413,-22.7406115879508,
12.));
#228305=CARTESIAN_POINT('Ctrl Pts',(-7.66670364630273,-22.7620360971839,
12.));
#228306=CARTESIAN_POINT('Ctrl Pts',(-7.66610966441259,-22.7835594857697,
12.));
#228307=CARTESIAN_POINT('Ctrl Pts',(-7.66545684920988,-22.8051809987833,
12.));
#228308=CARTESIAN_POINT('Ctrl Pts',(-7.66474484198553,-22.8268998887678,
12.));
#228309=CARTESIAN_POINT('Ctrl Pts',(-7.66397328929805,-22.8487154155569,
12.));
#228310=CARTESIAN_POINT('Ctrl Pts',(-7.66314184287334,-22.870626846128,
12.));
#228311=CARTESIAN_POINT('Ctrl Pts',(-7.66225015950148,-22.8926334544879,
12.));
#228312=CARTESIAN_POINT('Ctrl Pts',(-7.661297900941,-22.9147345215418,12.));
#228313=CARTESIAN_POINT('Ctrl Pts',(-7.66028473382777,-22.9369293349592,
12.));
#228314=CARTESIAN_POINT('Ctrl Pts',(-7.65921032958912,-22.9592171890332,
12.));
#228315=CARTESIAN_POINT('Ctrl Pts',(-7.65807436436453,-22.9815973845301,
12.));
#228316=CARTESIAN_POINT('Ctrl Pts',(-7.6568765189133,-23.004069228582,12.));
#228317=CARTESIAN_POINT('Ctrl Pts',(-7.65561647852555,-23.0266320345792,
12.));
#228318=CARTESIAN_POINT('Ctrl Pts',(-7.65429393293955,-23.049285122053,
12.));
#228319=CARTESIAN_POINT('Ctrl Pts',(-7.65290857626357,-23.072027816555,
12.));
#228320=CARTESIAN_POINT('Ctrl Pts',(-7.65146010690465,-23.0948594495246,
12.));
#228321=CARTESIAN_POINT('Ctrl Pts',(-7.64994822749845,-23.1177793581674,
12.));
#228322=CARTESIAN_POINT('Ctrl Pts',(-7.64837264482929,-23.1407868853815,
12.));
#228323=CARTESIAN_POINT('Ctrl Pts',(-7.64673306975797,-23.1638813796691,
12.));
#228324=CARTESIAN_POINT('Ctrl Pts',(-7.64502921715483,-23.1870621950452,
12.));
#228325=CARTESIAN_POINT('Ctrl Pts',(-7.64326080583684,-23.2103286909399,
12.));
#228326=CARTESIAN_POINT('Ctrl Pts',(-7.64142755851508,-23.2336802320912,
12.));
#228327=CARTESIAN_POINT('Ctrl Pts',(-7.63952920172837,-23.2571161884487,
12.));
#228328=CARTESIAN_POINT('Ctrl Pts',(-7.63756546576375,-23.2806359350853,
12.));
#228329=CARTESIAN_POINT('Ctrl Pts',(-7.63553608458784,-23.3042388521021,
12.));
#228330=CARTESIAN_POINT('Ctrl Pts',(-7.63344079578163,-23.3279243245241,
12.));
#228331=CARTESIAN_POINT('Ctrl Pts',(-7.63127934048139,-23.3516917421973,
12.));
#228332=CARTESIAN_POINT('Ctrl Pts',(-7.62905146332598,-23.3755404996638,
12.));
#228333=CARTESIAN_POINT('Ctrl Pts',(-7.62675691240335,-23.3994699961122,
12.));
#228334=CARTESIAN_POINT('Ctrl Pts',(-7.62439543920055,-23.4234796353544,
12.));
#228335=CARTESIAN_POINT('Ctrl Pts',(-7.62196679855957,-23.4475688257854,
12.));
#228336=CARTESIAN_POINT('Ctrl Pts',(-7.61947074863978,-23.4717369803438,
12.));
#228337=CARTESIAN_POINT('Ctrl Pts',(-7.61690705088319,-23.4959835164608,
12.));
#228338=CARTESIAN_POINT('Ctrl Pts',(-7.61427546999299,-23.5203078560128,
12.));
#228339=CARTESIAN_POINT('Ctrl Pts',(-7.61157577385372,-23.5447094252028,
12.));
#228340=CARTESIAN_POINT('Ctrl Pts',(-7.608807733446,-23.5691876544243,12.));
#228341=CARTESIAN_POINT('Ctrl Pts',(-7.60597112277094,-23.5937419781244,
12.));
#228342=CARTESIAN_POINT('Ctrl Pts',(-7.60306571877806,-23.6183718346576,
12.));
#228343=CARTESIAN_POINT('Ctrl Pts',(-7.6000913013013,-23.6430766661419,
12.));
#228344=CARTESIAN_POINT('Ctrl Pts',(-7.59704765299572,-23.6678559182876,
12.));
#228345=CARTESIAN_POINT('Ctrl Pts',(-7.59393455934042,-23.6927090405067,
12.));
#228346=CARTESIAN_POINT('Ctrl Pts',(-7.59075180865327,-23.7176354860457,
12.));
#228347=CARTESIAN_POINT('Ctrl Pts',(-7.58749919210832,-23.7426347121006,
12.));
#228348=CARTESIAN_POINT('Ctrl Pts',(-7.58417650376272,-23.7677061799376,
12.));
#228349=CARTESIAN_POINT('Ctrl Pts',(-7.58078354058212,-23.7928493549908,
12.));
#228350=CARTESIAN_POINT('Ctrl Pts',(-7.57732010249066,-23.8180637069977,
12.));
#228351=CARTESIAN_POINT('Ctrl Pts',(-7.57378599219817,-23.8433487096134,
12.));
#228352=CARTESIAN_POINT('Ctrl Pts',(-7.57018101500711,-23.8687038399597,
12.));
#228353=CARTESIAN_POINT('Ctrl Pts',(-7.56650497863792,-23.8941285782003,
12.));
#228354=CARTESIAN_POINT('Ctrl Pts',(-7.56275769304773,-23.9196224070759,
12.));
#228355=CARTESIAN_POINT('Ctrl Pts',(-7.55893897027683,-23.9451848115,12.));
#228356=CARTESIAN_POINT('Ctrl Pts',(-7.55504862424812,-23.9708152779884,
12.));
#228357=CARTESIAN_POINT('Ctrl Pts',(-7.55108647097441,-23.9965132953185,
12.));
#228358=CARTESIAN_POINT('Ctrl Pts',(-7.5470523288591,-24.022278355453,12.));
#228359=CARTESIAN_POINT('Ctrl Pts',(-7.54294601896145,-24.0481099543353,
12.));
#228360=CARTESIAN_POINT('Ctrl Pts',(-7.53876736531014,-24.0740075927985,
12.));
#228361=CARTESIAN_POINT('Ctrl Pts',(-7.53451619514649,-24.0999707772642,
12.));
#228362=CARTESIAN_POINT('Ctrl Pts',(-7.53019233935502,-24.1259990209207,
12.));
#228363=CARTESIAN_POINT('Ctrl Pts',(-7.52579563201424,-24.1520918425364,
12.));
#228364=CARTESIAN_POINT('Ctrl Pts',(-7.52132590953802,-24.1782487641594,
12.));
#228365=CARTESIAN_POINT('Ctrl Pts',(-7.51678300997949,-24.2044693092349,
12.));
#228366=CARTESIAN_POINT('Ctrl Pts',(-7.51216677222181,-24.2307530003887,
12.));
#228367=CARTESIAN_POINT('Ctrl Pts',(-7.50747703535134,-24.2570993577034,
12.));
#228368=CARTESIAN_POINT('Ctrl Pts',(-7.50271363765152,-24.2835078958973,
12.));
#228369=CARTESIAN_POINT('Ctrl Pts',(-7.49787641695439,-24.3099781253355,
12.));
#228370=CARTESIAN_POINT('Ctrl Pts',(-7.49296521252421,-24.3365095573685,
12.));
#228371=CARTESIAN_POINT('Ctrl Pts',(-7.48797986651909,-24.3631017084524,
12.));
#228372=CARTESIAN_POINT('Ctrl Pts',(-7.48292022569301,-24.3897541049254,
12.));
#228373=CARTESIAN_POINT('Ctrl Pts',(-7.47778614286565,-24.4164662871163,
12.));
#228374=CARTESIAN_POINT('Ctrl Pts',(-7.47257747883246,-24.443237814649,
12.));
#228375=CARTESIAN_POINT('Ctrl Pts',(-7.46729410308787,-24.4700682684524,
12.));
#228376=CARTESIAN_POINT('Ctrl Pts',(-7.46193588961464,-24.4969572391483,
12.));
#228377=CARTESIAN_POINT('Ctrl Pts',(-7.45650271335862,-24.5239043173072,
12.));
#228378=CARTESIAN_POINT('Ctrl Pts',(-7.4509944465116,-24.5509090831559,
12.));
#228379=CARTESIAN_POINT('Ctrl Pts',(-7.44541095473135,-24.577971096086,
12.));
#228380=CARTESIAN_POINT('Ctrl Pts',(-7.43975209375504,-24.6050898852368,
12.));
#228381=CARTESIAN_POINT('Ctrl Pts',(-7.43401770489524,-24.6322649369517,
12.));
#228382=CARTESIAN_POINT('Ctrl Pts',(-7.42820762159126,-24.6594957128756,
12.));
#228383=CARTESIAN_POINT('Ctrl Pts',(-7.42232167766266,-24.6867816727192,
12.));
#228384=CARTESIAN_POINT('Ctrl Pts',(-7.41635971481674,-24.7141222950051,
12.));
#228385=CARTESIAN_POINT('Ctrl Pts',(-7.41032159082382,-24.7415170994784,
12.));
#228386=CARTESIAN_POINT('Ctrl Pts',(-7.40420718661603,-24.7689656668983,
12.));
#228387=CARTESIAN_POINT('Ctrl Pts',(-7.39801641583013,-24.7964676646431,
12.));
#228388=CARTESIAN_POINT('Ctrl Pts',(-7.39174922585809,-24.8240228520893,
12.));
#228389=CARTESIAN_POINT('Ctrl Pts',(-7.38540558903621,-24.8516310625176,
12.));
#228390=CARTESIAN_POINT('Ctrl Pts',(-7.3789854964027,-24.8792921911115,
12.));
#228391=CARTESIAN_POINT('Ctrl Pts',(-7.37378825961676,-24.901463382605,
12.));
#228392=CARTESIAN_POINT('Ctrl Pts',(-7.36985593120091,-24.9181155530543,
12.));
#228393=CARTESIAN_POINT('Ctrl Pts',(-7.36721909028843,-24.9292275670674,
12.));
#228394=CARTESIAN_POINT('Ctrl Pts',(-7.36589684767345,-24.9347862158358,
12.));
#228395=CARTESIAN_POINT('Ctrl Pts',(-9.71462809124917,-20.353053841303,
0.));
#228396=CARTESIAN_POINT('Ctrl Pts',(-9.71462809124917,-20.353053841303,
12.));
#228397=CARTESIAN_POINT('Ctrl Pts',(-9.71462954053074,-20.353060251684,
0.));
#228398=CARTESIAN_POINT('Ctrl Pts',(-9.71462954053074,-20.353060251684,
12.));
#228399=CARTESIAN_POINT('Ctrl Pts',(-9.71465227853122,-20.3531126095522,
0.));
#228400=CARTESIAN_POINT('Ctrl Pts',(-9.71465227853122,-20.3531126095522,
12.));
#228401=CARTESIAN_POINT('Ctrl Pts',(-9.71474590350792,-20.3533097561886,
0.));
#228402=CARTESIAN_POINT('Ctrl Pts',(-9.71474590350792,-20.3533097561886,
12.));
#228403=CARTESIAN_POINT('Ctrl Pts',(-9.71498978052101,-20.3538098605706,
0.));
#228404=CARTESIAN_POINT('Ctrl Pts',(-9.71498978052101,-20.3538098605706,
12.));
#228405=CARTESIAN_POINT('Ctrl Pts',(-9.71549257088175,-20.3548282742361,
0.));
#228406=CARTESIAN_POINT('Ctrl Pts',(-9.71549257088175,-20.3548282742361,
12.));
#228407=CARTESIAN_POINT('Ctrl Pts',(-9.71619192554147,-20.3562337557875,
0.));
#228408=CARTESIAN_POINT('Ctrl Pts',(-9.71619192554147,-20.3562337557875,
12.));
#228409=CARTESIAN_POINT('Ctrl Pts',(-9.71708493723062,-20.3580133103357,
0.));
#228410=CARTESIAN_POINT('Ctrl Pts',(-9.71708493723062,-20.3580133103357,
12.));
#228411=CARTESIAN_POINT('Ctrl Pts',(-9.71816778327999,-20.3601498764344,
0.));
#228412=CARTESIAN_POINT('Ctrl Pts',(-9.71816778327999,-20.3601498764344,
12.));
#228413=CARTESIAN_POINT('Ctrl Pts',(-9.71943648548115,-20.362625691398,
0.));
#228414=CARTESIAN_POINT('Ctrl Pts',(-9.71943648548115,-20.362625691398,
12.));
#228415=CARTESIAN_POINT('Ctrl Pts',(-9.72088778381102,-20.3654261611055,
0.));
#228416=CARTESIAN_POINT('Ctrl Pts',(-9.72088778381102,-20.3654261611055,
12.));
#228417=CARTESIAN_POINT('Ctrl Pts',(-9.72251930722504,-20.3685406190576,
0.));
#228418=CARTESIAN_POINT('Ctrl Pts',(-9.72251930722504,-20.3685406190576,
12.));
#228419=CARTESIAN_POINT('Ctrl Pts',(-9.72432910043193,-20.371960235676,
0.));
#228420=CARTESIAN_POINT('Ctrl Pts',(-9.72432910043193,-20.371960235676,
12.));
#228421=CARTESIAN_POINT('Ctrl Pts',(-9.72631531732871,-20.3756766651952,
0.));
#228422=CARTESIAN_POINT('Ctrl Pts',(-9.72631531732871,-20.3756766651952,
12.));
#228423=CARTESIAN_POINT('Ctrl Pts',(-9.72847589116533,-20.3796805893304,
0.));
#228424=CARTESIAN_POINT('Ctrl Pts',(-9.72847589116533,-20.3796805893304,
12.));
#228425=CARTESIAN_POINT('Ctrl Pts',(-9.73080870123726,-20.3839624556742,
0.));
#228426=CARTESIAN_POINT('Ctrl Pts',(-9.73080870123726,-20.3839624556742,
12.));
#228427=CARTESIAN_POINT('Ctrl Pts',(-9.73331167102812,-20.3885129129912,
0.));
#228428=CARTESIAN_POINT('Ctrl Pts',(-9.73331167102812,-20.3885129129912,
12.));
#228429=CARTESIAN_POINT('Ctrl Pts',(-9.7359829201425,-20.3933234845646,
0.));
#228430=CARTESIAN_POINT('Ctrl Pts',(-9.7359829201425,-20.3933234845646,
12.));
#228431=CARTESIAN_POINT('Ctrl Pts',(-9.73882077613206,-20.3983866213331,
0.));
#228432=CARTESIAN_POINT('Ctrl Pts',(-9.73882077613206,-20.3983866213331,
12.));
#228433=CARTESIAN_POINT('Ctrl Pts',(-9.74182369656273,-20.4036953576549,
0.));
#228434=CARTESIAN_POINT('Ctrl Pts',(-9.74182369656273,-20.4036953576549,
12.));
#228435=CARTESIAN_POINT('Ctrl Pts',(-9.74499021838537,-20.4092430879861,
0.));
#228436=CARTESIAN_POINT('Ctrl Pts',(-9.74499021838537,-20.4092430879861,
12.));
#228437=CARTESIAN_POINT('Ctrl Pts',(-9.74831889242175,-20.4150232777393,
0.));
#228438=CARTESIAN_POINT('Ctrl Pts',(-9.74831889242175,-20.4150232777393,
12.));
#228439=CARTESIAN_POINT('Ctrl Pts',(-9.75180829786433,-20.4210295275818,
0.));
#228440=CARTESIAN_POINT('Ctrl Pts',(-9.75180829786433,-20.4210295275818,
12.));
#228441=CARTESIAN_POINT('Ctrl Pts',(-9.75545705902416,-20.4272556476629,
0.));
#228442=CARTESIAN_POINT('Ctrl Pts',(-9.75545705902416,-20.4272556476629,
12.));
#228443=CARTESIAN_POINT('Ctrl Pts',(-9.7592638628993,-20.4336957355474,
0.));
#228444=CARTESIAN_POINT('Ctrl Pts',(-9.7592638628993,-20.4336957355474,
12.));
#228445=CARTESIAN_POINT('Ctrl Pts',(-9.76322747195502,-20.4403442329401,
0.));
#228446=CARTESIAN_POINT('Ctrl Pts',(-9.76322747195502,-20.4403442329401,
12.));
#228447=CARTESIAN_POINT('Ctrl Pts',(-9.76734670980897,-20.447195862298,
0.));
#228448=CARTESIAN_POINT('Ctrl Pts',(-9.76734670980897,-20.447195862298,
12.));
#228449=CARTESIAN_POINT('Ctrl Pts',(-9.7716204510407,-20.4542455817527,
0.));
#228450=CARTESIAN_POINT('Ctrl Pts',(-9.7716204510407,-20.4542455817527,
12.));
#228451=CARTESIAN_POINT('Ctrl Pts',(-9.77604760815523,-20.4614885274973,
0.));
#228452=CARTESIAN_POINT('Ctrl Pts',(-9.77604760815523,-20.4614885274973,
12.));
#228453=CARTESIAN_POINT('Ctrl Pts',(-9.78062712373313,-20.4689199790668,
0.));
#228454=CARTESIAN_POINT('Ctrl Pts',(-9.78062712373313,-20.4689199790668,
12.));
#228455=CARTESIAN_POINT('Ctrl Pts',(-9.78535797314162,-20.4765353711585,
0.));
#228456=CARTESIAN_POINT('Ctrl Pts',(-9.78535797314162,-20.4765353711585,
12.));
#228457=CARTESIAN_POINT('Ctrl Pts',(-9.7902391649866,-20.4843302955329,
0.));
#228458=CARTESIAN_POINT('Ctrl Pts',(-9.7902391649866,-20.4843302955329,
12.));
#228459=CARTESIAN_POINT('Ctrl Pts',(-9.79526974288344,-20.4923005087945,
0.));
#228460=CARTESIAN_POINT('Ctrl Pts',(-9.79526974288344,-20.4923005087945,
12.));
#228461=CARTESIAN_POINT('Ctrl Pts',(-9.80044878520968,-20.500441931211,
0.));
#228462=CARTESIAN_POINT('Ctrl Pts',(-9.80044878520968,-20.500441931211,
12.));
#228463=CARTESIAN_POINT('Ctrl Pts',(-9.80577540161103,-20.5087506310507,
0.));
#228464=CARTESIAN_POINT('Ctrl Pts',(-9.80577540161103,-20.5087506310507,
12.));
#228465=CARTESIAN_POINT('Ctrl Pts',(-9.81124873025278,-20.5172228122839,
0.));
#228466=CARTESIAN_POINT('Ctrl Pts',(-9.81124873025278,-20.5172228122839,
12.));
#228467=CARTESIAN_POINT('Ctrl Pts',(-9.81686793455918,-20.5258548000625,
0.));
#228468=CARTESIAN_POINT('Ctrl Pts',(-9.81686793455918,-20.5258548000625,
12.));
#228469=CARTESIAN_POINT('Ctrl Pts',(-9.82263220080328,-20.534643029951,
0.));
#228470=CARTESIAN_POINT('Ctrl Pts',(-9.82263220080328,-20.534643029951,
12.));
#228471=CARTESIAN_POINT('Ctrl Pts',(-9.82854073773858,-20.5435840460717,
0.));
#228472=CARTESIAN_POINT('Ctrl Pts',(-9.82854073773858,-20.5435840460717,
12.));
#228473=CARTESIAN_POINT('Ctrl Pts',(-9.83459277585321,-20.5526744976461,
0.));
#228474=CARTESIAN_POINT('Ctrl Pts',(-9.83459277585321,-20.5526744976461,
12.));
#228475=CARTESIAN_POINT('Ctrl Pts',(-9.84078756677589,-20.5619111362406,
0.));
#228476=CARTESIAN_POINT('Ctrl Pts',(-9.84078756677589,-20.5619111362406,
12.));
#228477=CARTESIAN_POINT('Ctrl Pts',(-9.84712438256308,-20.5712908125145,
0.));
#228478=CARTESIAN_POINT('Ctrl Pts',(-9.84712438256308,-20.5712908125145,
12.));
#228479=CARTESIAN_POINT('Ctrl Pts',(-9.85360251457004,-20.580810471002,
0.));
#228480=CARTESIAN_POINT('Ctrl Pts',(-9.85360251457004,-20.580810471002,
12.));
#228481=CARTESIAN_POINT('Ctrl Pts',(-9.8602212723275,-20.5904671449754,
0.));
#228482=CARTESIAN_POINT('Ctrl Pts',(-9.8602212723275,-20.5904671449754,
12.));
#228483=CARTESIAN_POINT('Ctrl Pts',(-9.86697998242612,-20.6002579513696,
0.));
#228484=CARTESIAN_POINT('Ctrl Pts',(-9.86697998242612,-20.6002579513696,
12.));
#228485=CARTESIAN_POINT('Ctrl Pts',(-9.87387798732944,-20.6101800854491,
0.));
#228486=CARTESIAN_POINT('Ctrl Pts',(-9.87387798732944,-20.6101800854491,
12.));
#228487=CARTESIAN_POINT('Ctrl Pts',(-9.88091464472669,-20.6202308177472,
0.));
#228488=CARTESIAN_POINT('Ctrl Pts',(-9.88091464472669,-20.6202308177472,
12.));
#228489=CARTESIAN_POINT('Ctrl Pts',(-9.88808932697305,-20.6304074914086,
0.));
#228490=CARTESIAN_POINT('Ctrl Pts',(-9.88808932697305,-20.6304074914086,
12.));
#228491=CARTESIAN_POINT('Ctrl Pts',(-9.89540142049124,-20.6407075193977,
0.));
#228492=CARTESIAN_POINT('Ctrl Pts',(-9.89540142049124,-20.6407075193977,
12.));
#228493=CARTESIAN_POINT('Ctrl Pts',(-9.90285032516696,-20.6511283817415,
0.));
#228494=CARTESIAN_POINT('Ctrl Pts',(-9.90285032516696,-20.6511283817415,
12.));
#228495=CARTESIAN_POINT('Ctrl Pts',(-9.91043545377005,-20.6616676228315,
0.));
#228496=CARTESIAN_POINT('Ctrl Pts',(-9.91043545377005,-20.6616676228315,
12.));
#228497=CARTESIAN_POINT('Ctrl Pts',(-9.91815623141285,-20.6723228488261,
0.));
#228498=CARTESIAN_POINT('Ctrl Pts',(-9.91815623141285,-20.6723228488261,
12.));
#228499=CARTESIAN_POINT('Ctrl Pts',(-9.92601209498751,-20.6830917250255,
0.));
#228500=CARTESIAN_POINT('Ctrl Pts',(-9.92601209498751,-20.6830917250255,
12.));
#228501=CARTESIAN_POINT('Ctrl Pts',(-9.93400249259737,-20.6939719732485,
0.));
#228502=CARTESIAN_POINT('Ctrl Pts',(-9.93400249259737,-20.6939719732485,
12.));
#228503=CARTESIAN_POINT('Ctrl Pts',(-9.94212688298251,-20.7049613692237,
0.));
#228504=CARTESIAN_POINT('Ctrl Pts',(-9.94212688298251,-20.7049613692237,
12.));
#228505=CARTESIAN_POINT('Ctrl Pts',(-9.95038473514962,-20.716057740758,
0.));
#228506=CARTESIAN_POINT('Ctrl Pts',(-9.95038473514962,-20.716057740758,
12.));
#228507=CARTESIAN_POINT('Ctrl Pts',(-9.95877552798403,-20.7272589658752,
0.));
#228508=CARTESIAN_POINT('Ctrl Pts',(-9.95877552798403,-20.7272589658752,
12.));
#228509=CARTESIAN_POINT('Ctrl Pts',(-9.96729874986199,-20.7385629709795,
0.));
#228510=CARTESIAN_POINT('Ctrl Pts',(-9.96729874986199,-20.7385629709795,
12.));
#228511=CARTESIAN_POINT('Ctrl Pts',(-9.97595389823461,-20.7499677289625,
0.));
#228512=CARTESIAN_POINT('Ctrl Pts',(-9.97595389823461,-20.7499677289625,
12.));
#228513=CARTESIAN_POINT('Ctrl Pts',(-9.98474047926846,-20.7614712574989,
0.));
#228514=CARTESIAN_POINT('Ctrl Pts',(-9.98474047926846,-20.7614712574989,
12.));
#228515=CARTESIAN_POINT('Ctrl Pts',(-9.99365800754638,-20.7730716175417,
0.));
#228516=CARTESIAN_POINT('Ctrl Pts',(-9.99365800754638,-20.7730716175417,
12.));
#228517=CARTESIAN_POINT('Ctrl Pts',(-10.0027060057389,-20.7847669117568,
0.));
#228518=CARTESIAN_POINT('Ctrl Pts',(-10.0027060057389,-20.7847669117568,
12.));
#228519=CARTESIAN_POINT('Ctrl Pts',(-10.0118840042786,-20.7965552829907,
0.));
#228520=CARTESIAN_POINT('Ctrl Pts',(-10.0118840042786,-20.7965552829907,
12.));
#228521=CARTESIAN_POINT('Ctrl Pts',(-10.0211915410095,-20.8084349126885,
0.));
#228522=CARTESIAN_POINT('Ctrl Pts',(-10.0211915410095,-20.8084349126885,
12.));
#228523=CARTESIAN_POINT('Ctrl Pts',(-10.0306281609435,-20.8204040196599,
0.));
#228524=CARTESIAN_POINT('Ctrl Pts',(-10.0306281609435,-20.8204040196599,
12.));
#228525=CARTESIAN_POINT('Ctrl Pts',(-10.0401934160234,-20.8324608588906,
0.));
#228526=CARTESIAN_POINT('Ctrl Pts',(-10.0401934160234,-20.8324608588906,
12.));
#228527=CARTESIAN_POINT('Ctrl Pts',(-10.0498868648733,-20.8446037203402,
0.));
#228528=CARTESIAN_POINT('Ctrl Pts',(-10.0498868648733,-20.8446037203402,
12.));
#228529=CARTESIAN_POINT('Ctrl Pts',(-10.0597080725375,-20.856830927732,
0.));
#228530=CARTESIAN_POINT('Ctrl Pts',(-10.0597080725375,-20.856830927732,
12.));
#228531=CARTESIAN_POINT('Ctrl Pts',(-10.0696566102219,-20.8691408373705,
0.));
#228532=CARTESIAN_POINT('Ctrl Pts',(-10.0696566102219,-20.8691408373705,
12.));
#228533=CARTESIAN_POINT('Ctrl Pts',(-10.0797320551154,-20.8815318371844,
0.));
#228534=CARTESIAN_POINT('Ctrl Pts',(-10.0797320551154,-20.8815318371844,
12.));
#228535=CARTESIAN_POINT('Ctrl Pts',(-10.0899339901916,-20.8940023457371,
0.));
#228536=CARTESIAN_POINT('Ctrl Pts',(-10.0899339901916,-20.8940023457371,
12.));
#228537=CARTESIAN_POINT('Ctrl Pts',(-10.1002620040076,-20.9065508112556,
0.));
#228538=CARTESIAN_POINT('Ctrl Pts',(-10.1002620040076,-20.9065508112556,
12.));
#228539=CARTESIAN_POINT('Ctrl Pts',(-10.1107156904836,-20.9191757106266,
0.));
#228540=CARTESIAN_POINT('Ctrl Pts',(-10.1107156904836,-20.9191757106266,
12.));
#228541=CARTESIAN_POINT('Ctrl Pts',(-10.1212946487057,-20.931875548473,
0.));
#228542=CARTESIAN_POINT('Ctrl Pts',(-10.1212946487057,-20.931875548473,
12.));
#228543=CARTESIAN_POINT('Ctrl Pts',(-10.1319984827909,-20.944648856393,
0.));
#228544=CARTESIAN_POINT('Ctrl Pts',(-10.1319984827909,-20.944648856393,
12.));
#228545=CARTESIAN_POINT('Ctrl Pts',(-10.1428268017257,-20.9574941921591,
0.));
#228546=CARTESIAN_POINT('Ctrl Pts',(-10.1428268017257,-20.9574941921591,
12.));
#228547=CARTESIAN_POINT('Ctrl Pts',(-10.1537792192065,-20.970410138937,
0.));
#228548=CARTESIAN_POINT('Ctrl Pts',(-10.1537792192065,-20.970410138937,
12.));
#228549=CARTESIAN_POINT('Ctrl Pts',(-10.1648553534567,-20.9833953044736,
0.));
#228550=CARTESIAN_POINT('Ctrl Pts',(-10.1648553534567,-20.9833953044736,
12.));
#228551=CARTESIAN_POINT('Ctrl Pts',(-10.1760548270765,-20.9964483203685,
0.));
#228552=CARTESIAN_POINT('Ctrl Pts',(-10.1760548270765,-20.9964483203685,
12.));
#228553=CARTESIAN_POINT('Ctrl Pts',(-10.1873772669358,-21.0095678414486,
0.));
#228554=CARTESIAN_POINT('Ctrl Pts',(-10.1873772669358,-21.0095678414486,
12.));
#228555=CARTESIAN_POINT('Ctrl Pts',(-10.1988223040425,-21.0227525451107,
0.));
#228556=CARTESIAN_POINT('Ctrl Pts',(-10.1988223040425,-21.0227525451107,
12.));
#228557=CARTESIAN_POINT('Ctrl Pts',(-10.2103895734124,-21.0360011306814,
0.));
#228558=CARTESIAN_POINT('Ctrl Pts',(-10.2103895734124,-21.0360011306814,
12.));
#228559=CARTESIAN_POINT('Ctrl Pts',(-10.2220787139157,-21.0493123187483,
0.));
#228560=CARTESIAN_POINT('Ctrl Pts',(-10.2220787139157,-21.0493123187483,
12.));
#228561=CARTESIAN_POINT('Ctrl Pts',(-10.233889368157,-21.0626848505665,
0.));
#228562=CARTESIAN_POINT('Ctrl Pts',(-10.233889368157,-21.0626848505665,
12.));
#228563=CARTESIAN_POINT('Ctrl Pts',(-10.2458211823915,-21.0761174875448,
0.));
#228564=CARTESIAN_POINT('Ctrl Pts',(-10.2458211823915,-21.0761174875448,
12.));
#228565=CARTESIAN_POINT('Ctrl Pts',(-10.2578738064183,-21.0896090107066,
0.));
#228566=CARTESIAN_POINT('Ctrl Pts',(-10.2578738064183,-21.0896090107066,
12.));
#228567=CARTESIAN_POINT('Ctrl Pts',(-10.2700468934743,-21.1031582201625,
0.));
#228568=CARTESIAN_POINT('Ctrl Pts',(-10.2700468934743,-21.1031582201625,
12.));
#228569=CARTESIAN_POINT('Ctrl Pts',(-10.2823401001067,-21.1167639345623,
0.));
#228570=CARTESIAN_POINT('Ctrl Pts',(-10.2823401001067,-21.1167639345623,
12.));
#228571=CARTESIAN_POINT('Ctrl Pts',(-10.2947530860714,-21.130424990599,
0.));
#228572=CARTESIAN_POINT('Ctrl Pts',(-10.2947530860714,-21.130424990599,
12.));
#228573=CARTESIAN_POINT('Ctrl Pts',(-10.307285514268,-21.1441402425831,
0.));
#228574=CARTESIAN_POINT('Ctrl Pts',(-10.307285514268,-21.1441402425831,
12.));
#228575=CARTESIAN_POINT('Ctrl Pts',(-10.3199370506541,-21.1579085619959,
0.));
#228576=CARTESIAN_POINT('Ctrl Pts',(-10.3199370506541,-21.1579085619959,
12.));
#228577=CARTESIAN_POINT('Ctrl Pts',(-10.3327073641574,-21.1717288370512,
0.));
#228578=CARTESIAN_POINT('Ctrl Pts',(-10.3327073641574,-21.1717288370512,
12.));
#228579=CARTESIAN_POINT('Ctrl Pts',(-10.3455961265706,-21.1855999722427,
0.));
#228580=CARTESIAN_POINT('Ctrl Pts',(-10.3455961265706,-21.1855999722427,
12.));
#228581=CARTESIAN_POINT('Ctrl Pts',(-10.3586030124595,-21.1995208879205,
0.));
#228582=CARTESIAN_POINT('Ctrl Pts',(-10.3586030124595,-21.1995208879205,
12.));
#228583=CARTESIAN_POINT('Ctrl Pts',(-10.3717276991137,-21.2134905199359,
0.));
#228584=CARTESIAN_POINT('Ctrl Pts',(-10.3717276991137,-21.2134905199359,
12.));
#228585=CARTESIAN_POINT('Ctrl Pts',(-10.384969866479,-21.2275078192708,
0.));
#228586=CARTESIAN_POINT('Ctrl Pts',(-10.384969866479,-21.2275078192708,
12.));
#228587=CARTESIAN_POINT('Ctrl Pts',(-10.3983291970846,-21.2415717516713,
0.));
#228588=CARTESIAN_POINT('Ctrl Pts',(-10.3983291970846,-21.2415717516713,
12.));
#228589=CARTESIAN_POINT('Ctrl Pts',(-10.4118053759584,-21.2556812972741,
0.));
#228590=CARTESIAN_POINT('Ctrl Pts',(-10.4118053759584,-21.2556812972741,
12.));
#228591=CARTESIAN_POINT('Ctrl Pts',(-10.4253980905394,-21.2698354502391,
0.));
#228592=CARTESIAN_POINT('Ctrl Pts',(-10.4253980905394,-21.2698354502391,
12.));
#228593=CARTESIAN_POINT('Ctrl Pts',(-10.4391070306385,-21.2840332184471,
0.));
#228594=CARTESIAN_POINT('Ctrl Pts',(-10.4391070306385,-21.2840332184471,
12.));
#228595=CARTESIAN_POINT('Ctrl Pts',(-10.452931888387,-21.2982736231924,
0.));
#228596=CARTESIAN_POINT('Ctrl Pts',(-10.452931888387,-21.2982736231924,
12.));
#228597=CARTESIAN_POINT('Ctrl Pts',(-10.4668723581768,-21.312555698873,
0.));
#228598=CARTESIAN_POINT('Ctrl Pts',(-10.4668723581768,-21.312555698873,
12.));
#228599=CARTESIAN_POINT('Ctrl Pts',(-10.4809281365933,-21.3268784926823,
0.));
#228600=CARTESIAN_POINT('Ctrl Pts',(-10.4809281365933,-21.3268784926823,
12.));
#228601=CARTESIAN_POINT('Ctrl Pts',(-10.4950989223341,-21.3412410642912,
0.));
#228602=CARTESIAN_POINT('Ctrl Pts',(-10.4950989223341,-21.3412410642912,
12.));
#228603=CARTESIAN_POINT('Ctrl Pts',(-10.509384416169,-21.3556424855822,
0.));
#228604=CARTESIAN_POINT('Ctrl Pts',(-10.509384416169,-21.3556424855822,
12.));
#228605=CARTESIAN_POINT('Ctrl Pts',(-10.523784320906,-21.3700818403942,
0.));
#228606=CARTESIAN_POINT('Ctrl Pts',(-10.523784320906,-21.3700818403942,
12.));
#228607=CARTESIAN_POINT('Ctrl Pts',(-10.5382983413422,-21.3845582242604,
0.));
#228608=CARTESIAN_POINT('Ctrl Pts',(-10.5382983413422,-21.3845582242604,
12.));
#228609=CARTESIAN_POINT('Ctrl Pts',(-10.5529261842107,-21.3990707441495,
0.));
#228610=CARTESIAN_POINT('Ctrl Pts',(-10.5529261842107,-21.3990707441495,
12.));
#228611=CARTESIAN_POINT('Ctrl Pts',(-10.5676675581106,-21.4136185181974,
0.));
#228612=CARTESIAN_POINT('Ctrl Pts',(-10.5676675581106,-21.4136185181974,
12.));
#228613=CARTESIAN_POINT('Ctrl Pts',(-10.582522173457,-21.4282006754624,
0.));
#228614=CARTESIAN_POINT('Ctrl Pts',(-10.582522173457,-21.4282006754624,
12.));
#228615=CARTESIAN_POINT('Ctrl Pts',(-10.597489742462,-21.4428163557137,
0.));
#228616=CARTESIAN_POINT('Ctrl Pts',(-10.597489742462,-21.4428163557137,
12.));
#228617=CARTESIAN_POINT('Ctrl Pts',(-10.612569979096,-21.4574647092093,
0.));
#228618=CARTESIAN_POINT('Ctrl Pts',(-10.612569979096,-21.4574647092093,
12.));
#228619=CARTESIAN_POINT('Ctrl Pts',(-10.6277625990457,-21.4721448964766,
0.));
#228620=CARTESIAN_POINT('Ctrl Pts',(-10.6277625990457,-21.4721448964766,
12.));
#228621=CARTESIAN_POINT('Ctrl Pts',(-10.6430673196609,-21.4868560880893,
0.));
#228622=CARTESIAN_POINT('Ctrl Pts',(-10.6430673196609,-21.4868560880893,
12.));
#228623=CARTESIAN_POINT('Ctrl Pts',(-10.6584838598941,-21.5015974644454,
0.));
#228624=CARTESIAN_POINT('Ctrl Pts',(-10.6584838598941,-21.5015974644454,
12.));
#228625=CARTESIAN_POINT('Ctrl Pts',(-10.6740119402835,-21.5163682155805,
0.));
#228626=CARTESIAN_POINT('Ctrl Pts',(-10.6740119402835,-21.5163682155805,
12.));
#228627=CARTESIAN_POINT('Ctrl Pts',(-10.689651282929,-21.531167540981,0.));
#228628=CARTESIAN_POINT('Ctrl Pts',(-10.689651282929,-21.531167540981,12.));
#228629=CARTESIAN_POINT('Ctrl Pts',(-10.7054016114571,-21.5459946493955,
0.));
#228630=CARTESIAN_POINT('Ctrl Pts',(-10.7054016114571,-21.5459946493955,
12.));
#228631=CARTESIAN_POINT('Ctrl Pts',(-10.7212626509816,-21.5608487586467,
0.));
#228632=CARTESIAN_POINT('Ctrl Pts',(-10.7212626509816,-21.5608487586467,
12.));
#228633=CARTESIAN_POINT('Ctrl Pts',(-10.7372341280468,-21.5757290954372,
0.));
#228634=CARTESIAN_POINT('Ctrl Pts',(-10.7372341280468,-21.5757290954372,
12.));
#228635=CARTESIAN_POINT('Ctrl Pts',(-10.7533157705943,-21.5906348951745,
0.));
#228636=CARTESIAN_POINT('Ctrl Pts',(-10.7533157705943,-21.5906348951745,
12.));
#228637=CARTESIAN_POINT('Ctrl Pts',(-10.7695073079554,-21.6055654018179,
0.));
#228638=CARTESIAN_POINT('Ctrl Pts',(-10.7695073079554,-21.6055654018179,
12.));
#228639=CARTESIAN_POINT('Ctrl Pts',(-10.7858084708262,-21.6205198677176,
0.));
#228640=CARTESIAN_POINT('Ctrl Pts',(-10.7858084708262,-21.6205198677176,
12.));
#228641=CARTESIAN_POINT('Ctrl Pts',(-10.802218991237,-21.6354975534557,
0.));
#228642=CARTESIAN_POINT('Ctrl Pts',(-10.802218991237,-21.6354975534557,
12.));
#228643=CARTESIAN_POINT('Ctrl Pts',(-10.8187386025135,-21.6504977276864,
0.));
#228644=CARTESIAN_POINT('Ctrl Pts',(-10.8187386025135,-21.6504977276864,
12.));
#228645=CARTESIAN_POINT('Ctrl Pts',(-10.835367039227,-21.6655196669727,
0.));
#228646=CARTESIAN_POINT('Ctrl Pts',(-10.835367039227,-21.6655196669727,
12.));
#228647=CARTESIAN_POINT('Ctrl Pts',(-10.8521040371832,-21.6805626556461,
0.));
#228648=CARTESIAN_POINT('Ctrl Pts',(-10.8521040371832,-21.6805626556461,
12.));
#228649=CARTESIAN_POINT('Ctrl Pts',(-10.8689493334093,-21.6956259856667,
0.));
#228650=CARTESIAN_POINT('Ctrl Pts',(-10.8689493334093,-21.6956259856667,
12.));
#228651=CARTESIAN_POINT('Ctrl Pts',(-10.8859026661292,-21.7107089564822,
0.));
#228652=CARTESIAN_POINT('Ctrl Pts',(-10.8859026661292,-21.7107089564822,
12.));
#228653=CARTESIAN_POINT('Ctrl Pts',(-10.9029637747341,-21.7258108748874,
0.));
#228654=CARTESIAN_POINT('Ctrl Pts',(-10.9029637747341,-21.7258108748874,
12.));
#228655=CARTESIAN_POINT('Ctrl Pts',(-10.9201323997386,-21.74093105488,0.));
#228656=CARTESIAN_POINT('Ctrl Pts',(-10.9201323997386,-21.74093105488,12.));
#228657=CARTESIAN_POINT('Ctrl Pts',(-10.9374082827446,-21.7560688175252,
0.));
#228658=CARTESIAN_POINT('Ctrl Pts',(-10.9374082827446,-21.7560688175252,
12.));
#228659=CARTESIAN_POINT('Ctrl Pts',(-10.9547911664457,-21.7712234908468,
0.));
#228660=CARTESIAN_POINT('Ctrl Pts',(-10.9547911664457,-21.7712234908468,
12.));
#228661=CARTESIAN_POINT('Ctrl Pts',(-10.9722807946157,-21.7863944097143,
0.));
#228662=CARTESIAN_POINT('Ctrl Pts',(-10.9722807946157,-21.7863944097143,
12.));
#228663=CARTESIAN_POINT('Ctrl Pts',(-10.9898769120913,-21.8015809157302,
0.));
#228664=CARTESIAN_POINT('Ctrl Pts',(-10.9898769120913,-21.8015809157302,
12.));
#228665=CARTESIAN_POINT('Ctrl Pts',(-11.0075792647477,-21.8167823571168,
0.));
#228666=CARTESIAN_POINT('Ctrl Pts',(-11.0075792647477,-21.8167823571168,
12.));
#228667=CARTESIAN_POINT('Ctrl Pts',(-11.0253875994598,-21.8319980886033,
0.));
#228668=CARTESIAN_POINT('Ctrl Pts',(-11.0253875994598,-21.8319980886033,
12.));
#228669=CARTESIAN_POINT('Ctrl Pts',(-11.0433016640808,-21.8472274713103,
0.));
#228670=CARTESIAN_POINT('Ctrl Pts',(-11.0433016640808,-21.8472274713103,
12.));
#228671=CARTESIAN_POINT('Ctrl Pts',(-11.0613212074364,-21.8624698726319,
0.));
#228672=CARTESIAN_POINT('Ctrl Pts',(-11.0613212074364,-21.8624698726319,
12.));
#228673=CARTESIAN_POINT('Ctrl Pts',(-11.0794459793058,-21.8777246661191,
0.));
#228674=CARTESIAN_POINT('Ctrl Pts',(-11.0794459793058,-21.8777246661191,
12.));
#228675=CARTESIAN_POINT('Ctrl Pts',(-11.0976757303944,-21.8929912313608,
0.));
#228676=CARTESIAN_POINT('Ctrl Pts',(-11.0976757303944,-21.8929912313608,
12.));
#228677=CARTESIAN_POINT('Ctrl Pts',(-11.1160102123024,-21.9082689538687,
0.));
#228678=CARTESIAN_POINT('Ctrl Pts',(-11.1160102123024,-21.9082689538687,
12.));
#228679=CARTESIAN_POINT('Ctrl Pts',(-11.134449177474,-21.9235572249518,
0.));
#228680=CARTESIAN_POINT('Ctrl Pts',(-11.134449177474,-21.9235572249518,
12.));
#228681=CARTESIAN_POINT('Ctrl Pts',(-11.1529923792002,-21.9388554416437,
0.));
#228682=CARTESIAN_POINT('Ctrl Pts',(-11.1529923792002,-21.9388554416437,
12.));
#228683=CARTESIAN_POINT('Ctrl Pts',(-11.1716395716375,-21.9541630066504,
0.));
#228684=CARTESIAN_POINT('Ctrl Pts',(-11.1716395716375,-21.9541630066504,
12.));
#228685=CARTESIAN_POINT('Ctrl Pts',(-11.190390509811,-21.9694793282913,
0.));
#228686=CARTESIAN_POINT('Ctrl Pts',(-11.190390509811,-21.9694793282913,
12.));
#228687=CARTESIAN_POINT('Ctrl Pts',(-11.2092449496125,-21.9848038204439,
0.));
#228688=CARTESIAN_POINT('Ctrl Pts',(-11.2092449496125,-21.9848038204439,
12.));
#228689=CARTESIAN_POINT('Ctrl Pts',(-11.2282026477897,-22.0001359024839,
0.));
#228690=CARTESIAN_POINT('Ctrl Pts',(-11.2282026477897,-22.0001359024839,
12.));
#228691=CARTESIAN_POINT('Ctrl Pts',(-11.2472633619276,-22.0154749992364,
0.));
#228692=CARTESIAN_POINT('Ctrl Pts',(-11.2472633619276,-22.0154749992364,
12.));
#228693=CARTESIAN_POINT('Ctrl Pts',(-11.2664268504207,-22.0308205408351,
0.));
#228694=CARTESIAN_POINT('Ctrl Pts',(-11.2664268504207,-22.0308205408351,
12.));
#228695=CARTESIAN_POINT('Ctrl Pts',(-11.2856928724374,-22.046171962566,
0.));
#228696=CARTESIAN_POINT('Ctrl Pts',(-11.2856928724374,-22.046171962566,
12.));
#228697=CARTESIAN_POINT('Ctrl Pts',(-11.3050611878771,-22.0615287047179,
0.));
#228698=CARTESIAN_POINT('Ctrl Pts',(-11.3050611878771,-22.0615287047179,
12.));
#228699=CARTESIAN_POINT('Ctrl Pts',(-11.3245315573168,-22.0768902124267,
0.));
#228700=CARTESIAN_POINT('Ctrl Pts',(-11.3245315573168,-22.0768902124267,
12.));
#228701=CARTESIAN_POINT('Ctrl Pts',(-11.3441037419553,-22.0922559355293,
0.));
#228702=CARTESIAN_POINT('Ctrl Pts',(-11.3441037419553,-22.0922559355293,
12.));
#228703=CARTESIAN_POINT('Ctrl Pts',(-11.3637775035367,-22.1076253283978,
0.));
#228704=CARTESIAN_POINT('Ctrl Pts',(-11.3637775035367,-22.1076253283978,
12.));
#228705=CARTESIAN_POINT('Ctrl Pts',(-11.3835526044256,-22.1229978500185,
0.));
#228706=CARTESIAN_POINT('Ctrl Pts',(-11.3835526044256,-22.1229978500185,
12.));
#228707=CARTESIAN_POINT('Ctrl Pts',(-11.4034288076909,-22.1383729640963,
0.));
#228708=CARTESIAN_POINT('Ctrl Pts',(-11.4034288076909,-22.1383729640963,
12.));
#228709=CARTESIAN_POINT('Ctrl Pts',(-11.4234058771742,-22.1537501391486,
0.));
#228710=CARTESIAN_POINT('Ctrl Pts',(-11.4234058771742,-22.1537501391486,
12.));
#228711=CARTESIAN_POINT('Ctrl Pts',(-11.443483577557,-22.1691288486096,
0.));
#228712=CARTESIAN_POINT('Ctrl Pts',(-11.443483577557,-22.1691288486096,
12.));
#228713=CARTESIAN_POINT('Ctrl Pts',(-11.463661674411,-22.1845085709169,
0.));
#228714=CARTESIAN_POINT('Ctrl Pts',(-11.463661674411,-22.1845085709169,
12.));
#228715=CARTESIAN_POINT('Ctrl Pts',(-11.4839399342589,-22.1998887896435,
0.));
#228716=CARTESIAN_POINT('Ctrl Pts',(-11.4839399342589,-22.1998887896435,
12.));
#228717=CARTESIAN_POINT('Ctrl Pts',(-11.504318124424,-22.215268993102,0.));
#228718=CARTESIAN_POINT('Ctrl Pts',(-11.504318124424,-22.215268993102,12.));
#228719=CARTESIAN_POINT('Ctrl Pts',(-11.5247960128476,-22.2306486738899,
0.));
#228720=CARTESIAN_POINT('Ctrl Pts',(-11.5247960128476,-22.2306486738899,
12.));
#228721=CARTESIAN_POINT('Ctrl Pts',(-11.545373367912,-22.2460273284653,
0.));
#228722=CARTESIAN_POINT('Ctrl Pts',(-11.545373367912,-22.2460273284653,
12.));
#228723=CARTESIAN_POINT('Ctrl Pts',(-11.5660499582403,-22.2614044566898,
0.));
#228724=CARTESIAN_POINT('Ctrl Pts',(-11.5660499582403,-22.2614044566898,
12.));
#228725=CARTESIAN_POINT('Ctrl Pts',(-11.5868255525189,-22.2767795614349,
0.));
#228726=CARTESIAN_POINT('Ctrl Pts',(-11.5868255525189,-22.2767795614349,
12.));
#228727=CARTESIAN_POINT('Ctrl Pts',(-11.6076999192359,-22.2921521480357,
0.));
#228728=CARTESIAN_POINT('Ctrl Pts',(-11.6076999192359,-22.2921521480357,
12.));
#228729=CARTESIAN_POINT('Ctrl Pts',(-11.6286728270011,-22.3075217249049,
0.));
#228730=CARTESIAN_POINT('Ctrl Pts',(-11.6286728270011,-22.3075217249049,
12.));
#228731=CARTESIAN_POINT('Ctrl Pts',(-11.6497440449858,-22.3228878043976,
0.));
#228732=CARTESIAN_POINT('Ctrl Pts',(-11.6497440449858,-22.3228878043976,
12.));
#228733=CARTESIAN_POINT('Ctrl Pts',(-11.6709133432986,-22.3382499035618,
0.));
#228734=CARTESIAN_POINT('Ctrl Pts',(-11.6709133432986,-22.3382499035618,
12.));
#228735=CARTESIAN_POINT('Ctrl Pts',(-11.6921804934056,-22.3536075450028,
0.));
#228736=CARTESIAN_POINT('Ctrl Pts',(-11.6921804934056,-22.3536075450028,
12.));
#228737=CARTESIAN_POINT('Ctrl Pts',(-11.7135452684532,-22.3689602575492,
0.));
#228738=CARTESIAN_POINT('Ctrl Pts',(-11.7135452684532,-22.3689602575492,
12.));
#228739=CARTESIAN_POINT('Ctrl Pts',(-11.7350074437961,-22.3843075773905,
0.));
#228740=CARTESIAN_POINT('Ctrl Pts',(-11.7350074437961,-22.3843075773905,
12.));
#228741=CARTESIAN_POINT('Ctrl Pts',(-11.7565667964765,-22.39964904692,0.));
#228742=CARTESIAN_POINT('Ctrl Pts',(-11.7565667964765,-22.39964904692,12.));
#228743=CARTESIAN_POINT('Ctrl Pts',(-11.7782231042041,-22.4149842125018,
0.));
#228744=CARTESIAN_POINT('Ctrl Pts',(-11.7782231042041,-22.4149842125018,
12.));
#228745=CARTESIAN_POINT('Ctrl Pts',(-11.7999761445175,-22.4303126226468,
0.));
#228746=CARTESIAN_POINT('Ctrl Pts',(-11.7999761445175,-22.4303126226468,
12.));
#228747=CARTESIAN_POINT('Ctrl Pts',(-11.8218256937889,-22.4456338258738,
0.));
#228748=CARTESIAN_POINT('Ctrl Pts',(-11.8218256937889,-22.4456338258738,
12.));
#228749=CARTESIAN_POINT('Ctrl Pts',(-11.8437715264487,-22.4609473690469,
0.));
#228750=CARTESIAN_POINT('Ctrl Pts',(-11.8437715264487,-22.4609473690469,
12.));
#228751=CARTESIAN_POINT('Ctrl Pts',(-11.8658134137018,-22.4762527946694,
0.));
#228752=CARTESIAN_POINT('Ctrl Pts',(-11.8658134137018,-22.4762527946694,
12.));
#228753=CARTESIAN_POINT('Ctrl Pts',(-11.8879511239941,-22.4915496418472,
0.));
#228754=CARTESIAN_POINT('Ctrl Pts',(-11.8879511239941,-22.4915496418472,
12.));
#228755=CARTESIAN_POINT('Ctrl Pts',(-11.9101844254555,-22.5068374513958,
0.));
#228756=CARTESIAN_POINT('Ctrl Pts',(-11.9101844254555,-22.5068374513958,
12.));
#228757=CARTESIAN_POINT('Ctrl Pts',(-11.9325130877801,-22.5221157697869,
0.));
#228758=CARTESIAN_POINT('Ctrl Pts',(-11.9325130877801,-22.5221157697869,
12.));
#228759=CARTESIAN_POINT('Ctrl Pts',(-11.9549368843996,-22.5373841537299,
0.));
#228760=CARTESIAN_POINT('Ctrl Pts',(-11.9549368843996,-22.5373841537299,
12.));
#228761=CARTESIAN_POINT('Ctrl Pts',(-11.9774555943496,-22.5526421741159,
0.));
#228762=CARTESIAN_POINT('Ctrl Pts',(-11.9774555943496,-22.5526421741159,
12.));
#228763=CARTESIAN_POINT('Ctrl Pts',(-12.0000690046697,-22.5678894211194,
0.));
#228764=CARTESIAN_POINT('Ctrl Pts',(-12.0000690046697,-22.5678894211194,
12.));
#228765=CARTESIAN_POINT('Ctrl Pts',(-12.0227769113132,-22.5831255061306,
0.));
#228766=CARTESIAN_POINT('Ctrl Pts',(-12.0227769113132,-22.5831255061306,
12.));
#228767=CARTESIAN_POINT('Ctrl Pts',(-12.0455791139135,-22.5983500505675,
0.));
#228768=CARTESIAN_POINT('Ctrl Pts',(-12.0455791139135,-22.5983500505675,
12.));
#228769=CARTESIAN_POINT('Ctrl Pts',(-12.0684754113869,-22.613562676493,
0.));
#228770=CARTESIAN_POINT('Ctrl Pts',(-12.0684754113869,-22.613562676493,
12.));
#228771=CARTESIAN_POINT('Ctrl Pts',(-12.0914655972828,-22.628762996708,
0.));
#228772=CARTESIAN_POINT('Ctrl Pts',(-12.0914655972828,-22.628762996708,
12.));
#228773=CARTESIAN_POINT('Ctrl Pts',(-12.1145494550384,-22.6439506046611,
0.));
#228774=CARTESIAN_POINT('Ctrl Pts',(-12.1145494550384,-22.6439506046611,
12.));
#228775=CARTESIAN_POINT('Ctrl Pts',(-12.1377267537141,-22.6591250653942,
0.));
#228776=CARTESIAN_POINT('Ctrl Pts',(-12.1377267537141,-22.6591250653942,
12.));
#228777=CARTESIAN_POINT('Ctrl Pts',(-12.1609972423089,-22.6742859034891,
0.));
#228778=CARTESIAN_POINT('Ctrl Pts',(-12.1609972423089,-22.6742859034891,
12.));
#228779=CARTESIAN_POINT('Ctrl Pts',(-12.1843606579246,-22.6894326204959,
0.));
#228780=CARTESIAN_POINT('Ctrl Pts',(-12.1843606579246,-22.6894326204959,
12.));
#228781=CARTESIAN_POINT('Ctrl Pts',(-12.2078167360267,-22.7045647168659,
0.));
#228782=CARTESIAN_POINT('Ctrl Pts',(-12.2078167360267,-22.7045647168659,
12.));
#228783=CARTESIAN_POINT('Ctrl Pts',(-12.2313652198047,-22.7196817119299,
0.));
#228784=CARTESIAN_POINT('Ctrl Pts',(-12.2313652198047,-22.7196817119299,
12.));
#228785=CARTESIAN_POINT('Ctrl Pts',(-12.2550058702389,-22.7347831655251,
0.));
#228786=CARTESIAN_POINT('Ctrl Pts',(-12.2550058702389,-22.7347831655251,
12.));
#228787=CARTESIAN_POINT('Ctrl Pts',(-12.2787384750747,-22.7498686970096,
0.));
#228788=CARTESIAN_POINT('Ctrl Pts',(-12.2787384750747,-22.7498686970096,
12.));
#228789=CARTESIAN_POINT('Ctrl Pts',(-12.3025628601812,-22.7649380101154,
0.));
#228790=CARTESIAN_POINT('Ctrl Pts',(-12.3025628601812,-22.7649380101154,
12.));
#228791=CARTESIAN_POINT('Ctrl Pts',(-12.3264788926108,-22.7799908974947,
0.));
#228792=CARTESIAN_POINT('Ctrl Pts',(-12.3264788926108,-22.7799908974947,
12.));
#228793=CARTESIAN_POINT('Ctrl Pts',(-12.3504864740361,-22.7950272216959,
0.));
#228794=CARTESIAN_POINT('Ctrl Pts',(-12.3504864740361,-22.7950272216959,
12.));
#228795=CARTESIAN_POINT('Ctrl Pts',(-12.3745855366772,-22.8100469022632,
0.));
#228796=CARTESIAN_POINT('Ctrl Pts',(-12.3745855366772,-22.8100469022632,
12.));
#228797=CARTESIAN_POINT('Ctrl Pts',(-12.393937937903,-22.8220493007353,
0.));
#228798=CARTESIAN_POINT('Ctrl Pts',(-12.393937937903,-22.8220493007353,
12.));
#228799=CARTESIAN_POINT('Ctrl Pts',(-12.4084933766366,-22.8310435872852,
0.));
#228800=CARTESIAN_POINT('Ctrl Pts',(-12.4084933766366,-22.8310435872852,
12.));
#228801=CARTESIAN_POINT('Ctrl Pts',(-12.4182152851867,-22.8370364396497,
0.));
#228802=CARTESIAN_POINT('Ctrl Pts',(-12.4182152851867,-22.8370364396497,
12.));
#228803=CARTESIAN_POINT('Ctrl Pts',(-12.4230808101438,-22.8400320311648,
0.));
#228804=CARTESIAN_POINT('Ctrl Pts',(-12.4230808101438,-22.8400320311648,
12.));
#228805=CARTESIAN_POINT('',(-12.4230808101438,-22.8400320311648,0.));
#228806=CARTESIAN_POINT('Ctrl Pts',(-9.71462809124917,-20.353053841303,
0.));
#228807=CARTESIAN_POINT('Ctrl Pts',(-9.71462954053074,-20.353060251684,
0.));
#228808=CARTESIAN_POINT('Ctrl Pts',(-9.71465227853122,-20.3531126095522,
0.));
#228809=CARTESIAN_POINT('Ctrl Pts',(-9.71474590350792,-20.3533097561886,
0.));
#228810=CARTESIAN_POINT('Ctrl Pts',(-9.71498978052101,-20.3538098605706,
0.));
#228811=CARTESIAN_POINT('Ctrl Pts',(-9.71549257088175,-20.3548282742361,
0.));
#228812=CARTESIAN_POINT('Ctrl Pts',(-9.71619192554147,-20.3562337557875,
0.));
#228813=CARTESIAN_POINT('Ctrl Pts',(-9.71708493723062,-20.3580133103357,
0.));
#228814=CARTESIAN_POINT('Ctrl Pts',(-9.71816778327999,-20.3601498764344,
0.));
#228815=CARTESIAN_POINT('Ctrl Pts',(-9.71943648548115,-20.362625691398,
0.));
#228816=CARTESIAN_POINT('Ctrl Pts',(-9.72088778381102,-20.3654261611055,
0.));
#228817=CARTESIAN_POINT('Ctrl Pts',(-9.72251930722504,-20.3685406190576,
0.));
#228818=CARTESIAN_POINT('Ctrl Pts',(-9.72432910043193,-20.371960235676,
0.));
#228819=CARTESIAN_POINT('Ctrl Pts',(-9.72631531732871,-20.3756766651952,
0.));
#228820=CARTESIAN_POINT('Ctrl Pts',(-9.72847589116533,-20.3796805893304,
0.));
#228821=CARTESIAN_POINT('Ctrl Pts',(-9.73080870123726,-20.3839624556742,
0.));
#228822=CARTESIAN_POINT('Ctrl Pts',(-9.73331167102812,-20.3885129129912,
0.));
#228823=CARTESIAN_POINT('Ctrl Pts',(-9.7359829201425,-20.3933234845646,
0.));
#228824=CARTESIAN_POINT('Ctrl Pts',(-9.73882077613206,-20.3983866213331,
0.));
#228825=CARTESIAN_POINT('Ctrl Pts',(-9.74182369656273,-20.4036953576549,
0.));
#228826=CARTESIAN_POINT('Ctrl Pts',(-9.74499021838537,-20.4092430879861,
0.));
#228827=CARTESIAN_POINT('Ctrl Pts',(-9.74831889242175,-20.4150232777393,
0.));
#228828=CARTESIAN_POINT('Ctrl Pts',(-9.75180829786433,-20.4210295275818,
0.));
#228829=CARTESIAN_POINT('Ctrl Pts',(-9.75545705902416,-20.4272556476629,
0.));
#228830=CARTESIAN_POINT('Ctrl Pts',(-9.7592638628993,-20.4336957355474,
0.));
#228831=CARTESIAN_POINT('Ctrl Pts',(-9.76322747195502,-20.4403442329401,
0.));
#228832=CARTESIAN_POINT('Ctrl Pts',(-9.76734670980897,-20.447195862298,
0.));
#228833=CARTESIAN_POINT('Ctrl Pts',(-9.7716204510407,-20.4542455817527,
0.));
#228834=CARTESIAN_POINT('Ctrl Pts',(-9.77604760815523,-20.4614885274973,
0.));
#228835=CARTESIAN_POINT('Ctrl Pts',(-9.78062712373313,-20.4689199790668,
0.));
#228836=CARTESIAN_POINT('Ctrl Pts',(-9.78535797314162,-20.4765353711585,
0.));
#228837=CARTESIAN_POINT('Ctrl Pts',(-9.7902391649866,-20.4843302955329,
0.));
#228838=CARTESIAN_POINT('Ctrl Pts',(-9.79526974288344,-20.4923005087945,
0.));
#228839=CARTESIAN_POINT('Ctrl Pts',(-9.80044878520968,-20.500441931211,
0.));
#228840=CARTESIAN_POINT('Ctrl Pts',(-9.80577540161103,-20.5087506310507,
0.));
#228841=CARTESIAN_POINT('Ctrl Pts',(-9.81124873025278,-20.5172228122839,
0.));
#228842=CARTESIAN_POINT('Ctrl Pts',(-9.81686793455918,-20.5258548000625,
0.));
#228843=CARTESIAN_POINT('Ctrl Pts',(-9.82263220080328,-20.534643029951,
0.));
#228844=CARTESIAN_POINT('Ctrl Pts',(-9.82854073773858,-20.5435840460717,
0.));
#228845=CARTESIAN_POINT('Ctrl Pts',(-9.83459277585321,-20.5526744976461,
0.));
#228846=CARTESIAN_POINT('Ctrl Pts',(-9.84078756677589,-20.5619111362406,
0.));
#228847=CARTESIAN_POINT('Ctrl Pts',(-9.84712438256308,-20.5712908125145,
0.));
#228848=CARTESIAN_POINT('Ctrl Pts',(-9.85360251457004,-20.580810471002,
0.));
#228849=CARTESIAN_POINT('Ctrl Pts',(-9.8602212723275,-20.5904671449754,
0.));
#228850=CARTESIAN_POINT('Ctrl Pts',(-9.86697998242612,-20.6002579513696,
0.));
#228851=CARTESIAN_POINT('Ctrl Pts',(-9.87387798732944,-20.6101800854491,
0.));
#228852=CARTESIAN_POINT('Ctrl Pts',(-9.88091464472669,-20.6202308177472,
0.));
#228853=CARTESIAN_POINT('Ctrl Pts',(-9.88808932697305,-20.6304074914086,
0.));
#228854=CARTESIAN_POINT('Ctrl Pts',(-9.89540142049124,-20.6407075193977,
0.));
#228855=CARTESIAN_POINT('Ctrl Pts',(-9.90285032516696,-20.6511283817415,
0.));
#228856=CARTESIAN_POINT('Ctrl Pts',(-9.91043545377005,-20.6616676228315,
0.));
#228857=CARTESIAN_POINT('Ctrl Pts',(-9.91815623141285,-20.6723228488261,
0.));
#228858=CARTESIAN_POINT('Ctrl Pts',(-9.92601209498751,-20.6830917250255,
0.));
#228859=CARTESIAN_POINT('Ctrl Pts',(-9.93400249259737,-20.6939719732485,
0.));
#228860=CARTESIAN_POINT('Ctrl Pts',(-9.94212688298251,-20.7049613692237,
0.));
#228861=CARTESIAN_POINT('Ctrl Pts',(-9.95038473514962,-20.716057740758,
0.));
#228862=CARTESIAN_POINT('Ctrl Pts',(-9.95877552798403,-20.7272589658752,
0.));
#228863=CARTESIAN_POINT('Ctrl Pts',(-9.96729874986199,-20.7385629709795,
0.));
#228864=CARTESIAN_POINT('Ctrl Pts',(-9.97595389823461,-20.7499677289625,
0.));
#228865=CARTESIAN_POINT('Ctrl Pts',(-9.98474047926846,-20.7614712574989,
0.));
#228866=CARTESIAN_POINT('Ctrl Pts',(-9.99365800754638,-20.7730716175417,
0.));
#228867=CARTESIAN_POINT('Ctrl Pts',(-10.0027060057389,-20.7847669117568,
0.));
#228868=CARTESIAN_POINT('Ctrl Pts',(-10.0118840042786,-20.7965552829907,
0.));
#228869=CARTESIAN_POINT('Ctrl Pts',(-10.0211915410095,-20.8084349126885,
0.));
#228870=CARTESIAN_POINT('Ctrl Pts',(-10.0306281609435,-20.8204040196599,
0.));
#228871=CARTESIAN_POINT('Ctrl Pts',(-10.0401934160234,-20.8324608588906,
0.));
#228872=CARTESIAN_POINT('Ctrl Pts',(-10.0498868648733,-20.8446037203402,
0.));
#228873=CARTESIAN_POINT('Ctrl Pts',(-10.0597080725375,-20.856830927732,
0.));
#228874=CARTESIAN_POINT('Ctrl Pts',(-10.0696566102219,-20.8691408373705,
0.));
#228875=CARTESIAN_POINT('Ctrl Pts',(-10.0797320551154,-20.8815318371844,
0.));
#228876=CARTESIAN_POINT('Ctrl Pts',(-10.0899339901916,-20.8940023457371,
0.));
#228877=CARTESIAN_POINT('Ctrl Pts',(-10.1002620040076,-20.9065508112556,
0.));
#228878=CARTESIAN_POINT('Ctrl Pts',(-10.1107156904836,-20.9191757106266,
0.));
#228879=CARTESIAN_POINT('Ctrl Pts',(-10.1212946487057,-20.931875548473,
0.));
#228880=CARTESIAN_POINT('Ctrl Pts',(-10.1319984827909,-20.944648856393,
0.));
#228881=CARTESIAN_POINT('Ctrl Pts',(-10.1428268017257,-20.9574941921591,
0.));
#228882=CARTESIAN_POINT('Ctrl Pts',(-10.1537792192065,-20.970410138937,
0.));
#228883=CARTESIAN_POINT('Ctrl Pts',(-10.1648553534567,-20.9833953044736,
0.));
#228884=CARTESIAN_POINT('Ctrl Pts',(-10.1760548270765,-20.9964483203685,
0.));
#228885=CARTESIAN_POINT('Ctrl Pts',(-10.1873772669358,-21.0095678414486,
0.));
#228886=CARTESIAN_POINT('Ctrl Pts',(-10.1988223040425,-21.0227525451107,
0.));
#228887=CARTESIAN_POINT('Ctrl Pts',(-10.2103895734124,-21.0360011306814,
0.));
#228888=CARTESIAN_POINT('Ctrl Pts',(-10.2220787139157,-21.0493123187483,
0.));
#228889=CARTESIAN_POINT('Ctrl Pts',(-10.233889368157,-21.0626848505665,
0.));
#228890=CARTESIAN_POINT('Ctrl Pts',(-10.2458211823915,-21.0761174875448,
0.));
#228891=CARTESIAN_POINT('Ctrl Pts',(-10.2578738064183,-21.0896090107066,
0.));
#228892=CARTESIAN_POINT('Ctrl Pts',(-10.2700468934743,-21.1031582201625,
0.));
#228893=CARTESIAN_POINT('Ctrl Pts',(-10.2823401001067,-21.1167639345623,
0.));
#228894=CARTESIAN_POINT('Ctrl Pts',(-10.2947530860714,-21.130424990599,
0.));
#228895=CARTESIAN_POINT('Ctrl Pts',(-10.307285514268,-21.1441402425831,
0.));
#228896=CARTESIAN_POINT('Ctrl Pts',(-10.3199370506541,-21.1579085619959,
0.));
#228897=CARTESIAN_POINT('Ctrl Pts',(-10.3327073641574,-21.1717288370512,
0.));
#228898=CARTESIAN_POINT('Ctrl Pts',(-10.3455961265706,-21.1855999722427,
0.));
#228899=CARTESIAN_POINT('Ctrl Pts',(-10.3586030124595,-21.1995208879205,
0.));
#228900=CARTESIAN_POINT('Ctrl Pts',(-10.3717276991137,-21.2134905199359,
0.));
#228901=CARTESIAN_POINT('Ctrl Pts',(-10.384969866479,-21.2275078192708,
0.));
#228902=CARTESIAN_POINT('Ctrl Pts',(-10.3983291970846,-21.2415717516713,
0.));
#228903=CARTESIAN_POINT('Ctrl Pts',(-10.4118053759584,-21.2556812972741,
0.));
#228904=CARTESIAN_POINT('Ctrl Pts',(-10.4253980905394,-21.2698354502391,
0.));
#228905=CARTESIAN_POINT('Ctrl Pts',(-10.4391070306385,-21.2840332184471,
0.));
#228906=CARTESIAN_POINT('Ctrl Pts',(-10.452931888387,-21.2982736231924,
0.));
#228907=CARTESIAN_POINT('Ctrl Pts',(-10.4668723581768,-21.312555698873,
0.));
#228908=CARTESIAN_POINT('Ctrl Pts',(-10.4809281365933,-21.3268784926823,
0.));
#228909=CARTESIAN_POINT('Ctrl Pts',(-10.4950989223341,-21.3412410642912,
0.));
#228910=CARTESIAN_POINT('Ctrl Pts',(-10.509384416169,-21.3556424855822,
0.));
#228911=CARTESIAN_POINT('Ctrl Pts',(-10.523784320906,-21.3700818403942,
0.));
#228912=CARTESIAN_POINT('Ctrl Pts',(-10.5382983413422,-21.3845582242604,
0.));
#228913=CARTESIAN_POINT('Ctrl Pts',(-10.5529261842107,-21.3990707441495,
0.));
#228914=CARTESIAN_POINT('Ctrl Pts',(-10.5676675581106,-21.4136185181974,
0.));
#228915=CARTESIAN_POINT('Ctrl Pts',(-10.582522173457,-21.4282006754624,
0.));
#228916=CARTESIAN_POINT('Ctrl Pts',(-10.597489742462,-21.4428163557137,
0.));
#228917=CARTESIAN_POINT('Ctrl Pts',(-10.612569979096,-21.4574647092093,
0.));
#228918=CARTESIAN_POINT('Ctrl Pts',(-10.6277625990457,-21.4721448964766,
0.));
#228919=CARTESIAN_POINT('Ctrl Pts',(-10.6430673196609,-21.4868560880893,
0.));
#228920=CARTESIAN_POINT('Ctrl Pts',(-10.6584838598941,-21.5015974644454,
0.));
#228921=CARTESIAN_POINT('Ctrl Pts',(-10.6740119402835,-21.5163682155805,
0.));
#228922=CARTESIAN_POINT('Ctrl Pts',(-10.689651282929,-21.531167540981,0.));
#228923=CARTESIAN_POINT('Ctrl Pts',(-10.7054016114571,-21.5459946493955,
0.));
#228924=CARTESIAN_POINT('Ctrl Pts',(-10.7212626509816,-21.5608487586467,
0.));
#228925=CARTESIAN_POINT('Ctrl Pts',(-10.7372341280468,-21.5757290954372,
0.));
#228926=CARTESIAN_POINT('Ctrl Pts',(-10.7533157705943,-21.5906348951745,
0.));
#228927=CARTESIAN_POINT('Ctrl Pts',(-10.7695073079554,-21.6055654018179,
0.));
#228928=CARTESIAN_POINT('Ctrl Pts',(-10.7858084708262,-21.6205198677176,
0.));
#228929=CARTESIAN_POINT('Ctrl Pts',(-10.802218991237,-21.6354975534557,
0.));
#228930=CARTESIAN_POINT('Ctrl Pts',(-10.8187386025135,-21.6504977276864,
0.));
#228931=CARTESIAN_POINT('Ctrl Pts',(-10.835367039227,-21.6655196669727,
0.));
#228932=CARTESIAN_POINT('Ctrl Pts',(-10.8521040371832,-21.6805626556461,
0.));
#228933=CARTESIAN_POINT('Ctrl Pts',(-10.8689493334093,-21.6956259856667,
0.));
#228934=CARTESIAN_POINT('Ctrl Pts',(-10.8859026661292,-21.7107089564822,
0.));
#228935=CARTESIAN_POINT('Ctrl Pts',(-10.9029637747341,-21.7258108748874,
0.));
#228936=CARTESIAN_POINT('Ctrl Pts',(-10.9201323997386,-21.74093105488,0.));
#228937=CARTESIAN_POINT('Ctrl Pts',(-10.9374082827446,-21.7560688175252,
0.));
#228938=CARTESIAN_POINT('Ctrl Pts',(-10.9547911664457,-21.7712234908468,
0.));
#228939=CARTESIAN_POINT('Ctrl Pts',(-10.9722807946157,-21.7863944097143,
0.));
#228940=CARTESIAN_POINT('Ctrl Pts',(-10.9898769120913,-21.8015809157302,
0.));
#228941=CARTESIAN_POINT('Ctrl Pts',(-11.0075792647477,-21.8167823571168,
0.));
#228942=CARTESIAN_POINT('Ctrl Pts',(-11.0253875994598,-21.8319980886033,
0.));
#228943=CARTESIAN_POINT('Ctrl Pts',(-11.0433016640808,-21.8472274713103,
0.));
#228944=CARTESIAN_POINT('Ctrl Pts',(-11.0613212074364,-21.8624698726319,
0.));
#228945=CARTESIAN_POINT('Ctrl Pts',(-11.0794459793058,-21.8777246661191,
0.));
#228946=CARTESIAN_POINT('Ctrl Pts',(-11.0976757303944,-21.8929912313608,
0.));
#228947=CARTESIAN_POINT('Ctrl Pts',(-11.1160102123024,-21.9082689538687,
0.));
#228948=CARTESIAN_POINT('Ctrl Pts',(-11.134449177474,-21.9235572249518,
0.));
#228949=CARTESIAN_POINT('Ctrl Pts',(-11.1529923792002,-21.9388554416437,
0.));
#228950=CARTESIAN_POINT('Ctrl Pts',(-11.1716395716375,-21.9541630066504,
0.));
#228951=CARTESIAN_POINT('Ctrl Pts',(-11.190390509811,-21.9694793282913,
0.));
#228952=CARTESIAN_POINT('Ctrl Pts',(-11.2092449496125,-21.9848038204439,
0.));
#228953=CARTESIAN_POINT('Ctrl Pts',(-11.2282026477897,-22.0001359024839,
0.));
#228954=CARTESIAN_POINT('Ctrl Pts',(-11.2472633619276,-22.0154749992364,
0.));
#228955=CARTESIAN_POINT('Ctrl Pts',(-11.2664268504207,-22.0308205408351,
0.));
#228956=CARTESIAN_POINT('Ctrl Pts',(-11.2856928724374,-22.046171962566,
0.));
#228957=CARTESIAN_POINT('Ctrl Pts',(-11.3050611878771,-22.0615287047179,
0.));
#228958=CARTESIAN_POINT('Ctrl Pts',(-11.3245315573168,-22.0768902124267,
0.));
#228959=CARTESIAN_POINT('Ctrl Pts',(-11.3441037419553,-22.0922559355293,
0.));
#228960=CARTESIAN_POINT('Ctrl Pts',(-11.3637775035367,-22.1076253283978,
0.));
#228961=CARTESIAN_POINT('Ctrl Pts',(-11.3835526044256,-22.1229978500185,
0.));
#228962=CARTESIAN_POINT('Ctrl Pts',(-11.4034288076909,-22.1383729640963,
0.));
#228963=CARTESIAN_POINT('Ctrl Pts',(-11.4234058771742,-22.1537501391486,
0.));
#228964=CARTESIAN_POINT('Ctrl Pts',(-11.443483577557,-22.1691288486096,
0.));
#228965=CARTESIAN_POINT('Ctrl Pts',(-11.463661674411,-22.1845085709169,
0.));
#228966=CARTESIAN_POINT('Ctrl Pts',(-11.4839399342589,-22.1998887896435,
0.));
#228967=CARTESIAN_POINT('Ctrl Pts',(-11.504318124424,-22.215268993102,0.));
#228968=CARTESIAN_POINT('Ctrl Pts',(-11.5247960128476,-22.2306486738899,
0.));
#228969=CARTESIAN_POINT('Ctrl Pts',(-11.545373367912,-22.2460273284653,
0.));
#228970=CARTESIAN_POINT('Ctrl Pts',(-11.5660499582403,-22.2614044566898,
0.));
#228971=CARTESIAN_POINT('Ctrl Pts',(-11.5868255525189,-22.2767795614349,
0.));
#228972=CARTESIAN_POINT('Ctrl Pts',(-11.6076999192359,-22.2921521480357,
0.));
#228973=CARTESIAN_POINT('Ctrl Pts',(-11.6286728270011,-22.3075217249049,
0.));
#228974=CARTESIAN_POINT('Ctrl Pts',(-11.6497440449858,-22.3228878043976,
0.));
#228975=CARTESIAN_POINT('Ctrl Pts',(-11.6709133432986,-22.3382499035618,
0.));
#228976=CARTESIAN_POINT('Ctrl Pts',(-11.6921804934056,-22.3536075450028,
0.));
#228977=CARTESIAN_POINT('Ctrl Pts',(-11.7135452684532,-22.3689602575492,
0.));
#228978=CARTESIAN_POINT('Ctrl Pts',(-11.7350074437961,-22.3843075773905,
0.));
#228979=CARTESIAN_POINT('Ctrl Pts',(-11.7565667964765,-22.39964904692,0.));
#228980=CARTESIAN_POINT('Ctrl Pts',(-11.7782231042041,-22.4149842125018,
0.));
#228981=CARTESIAN_POINT('Ctrl Pts',(-11.7999761445175,-22.4303126226468,
0.));
#228982=CARTESIAN_POINT('Ctrl Pts',(-11.8218256937889,-22.4456338258738,
0.));
#228983=CARTESIAN_POINT('Ctrl Pts',(-11.8437715264487,-22.4609473690469,
0.));
#228984=CARTESIAN_POINT('Ctrl Pts',(-11.8658134137018,-22.4762527946694,
0.));
#228985=CARTESIAN_POINT('Ctrl Pts',(-11.8879511239941,-22.4915496418472,
0.));
#228986=CARTESIAN_POINT('Ctrl Pts',(-11.9101844254555,-22.5068374513958,
0.));
#228987=CARTESIAN_POINT('Ctrl Pts',(-11.9325130877801,-22.5221157697869,
0.));
#228988=CARTESIAN_POINT('Ctrl Pts',(-11.9549368843996,-22.5373841537299,
0.));
#228989=CARTESIAN_POINT('Ctrl Pts',(-11.9774555943496,-22.5526421741159,
0.));
#228990=CARTESIAN_POINT('Ctrl Pts',(-12.0000690046697,-22.5678894211194,
0.));
#228991=CARTESIAN_POINT('Ctrl Pts',(-12.0227769113132,-22.5831255061306,
0.));
#228992=CARTESIAN_POINT('Ctrl Pts',(-12.0455791139135,-22.5983500505675,
0.));
#228993=CARTESIAN_POINT('Ctrl Pts',(-12.0684754113869,-22.613562676493,
0.));
#228994=CARTESIAN_POINT('Ctrl Pts',(-12.0914655972828,-22.628762996708,
0.));
#228995=CARTESIAN_POINT('Ctrl Pts',(-12.1145494550384,-22.6439506046611,
0.));
#228996=CARTESIAN_POINT('Ctrl Pts',(-12.1377267537141,-22.6591250653942,
0.));
#228997=CARTESIAN_POINT('Ctrl Pts',(-12.1609972423089,-22.6742859034891,
0.));
#228998=CARTESIAN_POINT('Ctrl Pts',(-12.1843606579246,-22.6894326204959,
0.));
#228999=CARTESIAN_POINT('Ctrl Pts',(-12.2078167360267,-22.7045647168659,
0.));
#229000=CARTESIAN_POINT('Ctrl Pts',(-12.2313652198047,-22.7196817119299,
0.));
#229001=CARTESIAN_POINT('Ctrl Pts',(-12.2550058702389,-22.7347831655251,
0.));
#229002=CARTESIAN_POINT('Ctrl Pts',(-12.2787384750747,-22.7498686970096,
0.));
#229003=CARTESIAN_POINT('Ctrl Pts',(-12.3025628601812,-22.7649380101154,
0.));
#229004=CARTESIAN_POINT('Ctrl Pts',(-12.3264788926108,-22.7799908974947,
0.));
#229005=CARTESIAN_POINT('Ctrl Pts',(-12.3504864740361,-22.7950272216959,
0.));
#229006=CARTESIAN_POINT('Ctrl Pts',(-12.3745855366772,-22.8100469022632,
0.));
#229007=CARTESIAN_POINT('Ctrl Pts',(-12.393937937903,-22.8220493007353,
0.));
#229008=CARTESIAN_POINT('Ctrl Pts',(-12.4084933766366,-22.8310435872852,
0.));
#229009=CARTESIAN_POINT('Ctrl Pts',(-12.4182152851867,-22.8370364396497,
0.));
#229010=CARTESIAN_POINT('Ctrl Pts',(-12.4230808101438,-22.8400320311648,
0.));
#229011=CARTESIAN_POINT('',(-12.4230808101438,-22.8400320311648,12.));
#229012=CARTESIAN_POINT('Ctrl Pts',(-12.4230808101438,-22.8400320311648,
12.));
#229013=CARTESIAN_POINT('Ctrl Pts',(-12.4182152851867,-22.8370364396497,
12.));
#229014=CARTESIAN_POINT('Ctrl Pts',(-12.4084933766366,-22.8310435872852,
12.));
#229015=CARTESIAN_POINT('Ctrl Pts',(-12.393937937903,-22.8220493007353,
12.));
#229016=CARTESIAN_POINT('Ctrl Pts',(-12.3745855366772,-22.8100469022632,
12.));
#229017=CARTESIAN_POINT('Ctrl Pts',(-12.3504864740361,-22.7950272216959,
12.));
#229018=CARTESIAN_POINT('Ctrl Pts',(-12.3264788926108,-22.7799908974947,
12.));
#229019=CARTESIAN_POINT('Ctrl Pts',(-12.3025628601812,-22.7649380101154,
12.));
#229020=CARTESIAN_POINT('Ctrl Pts',(-12.2787384750747,-22.7498686970096,
12.));
#229021=CARTESIAN_POINT('Ctrl Pts',(-12.2550058702389,-22.7347831655251,
12.));
#229022=CARTESIAN_POINT('Ctrl Pts',(-12.2313652198047,-22.7196817119299,
12.));
#229023=CARTESIAN_POINT('Ctrl Pts',(-12.2078167360267,-22.7045647168659,
12.));
#229024=CARTESIAN_POINT('Ctrl Pts',(-12.1843606579246,-22.6894326204959,
12.));
#229025=CARTESIAN_POINT('Ctrl Pts',(-12.1609972423089,-22.6742859034891,
12.));
#229026=CARTESIAN_POINT('Ctrl Pts',(-12.1377267537141,-22.6591250653942,
12.));
#229027=CARTESIAN_POINT('Ctrl Pts',(-12.1145494550384,-22.6439506046611,
12.));
#229028=CARTESIAN_POINT('Ctrl Pts',(-12.0914655972828,-22.628762996708,
12.));
#229029=CARTESIAN_POINT('Ctrl Pts',(-12.0684754113869,-22.613562676493,
12.));
#229030=CARTESIAN_POINT('Ctrl Pts',(-12.0455791139135,-22.5983500505675,
12.));
#229031=CARTESIAN_POINT('Ctrl Pts',(-12.0227769113132,-22.5831255061306,
12.));
#229032=CARTESIAN_POINT('Ctrl Pts',(-12.0000690046697,-22.5678894211194,
12.));
#229033=CARTESIAN_POINT('Ctrl Pts',(-11.9774555943496,-22.5526421741159,
12.));
#229034=CARTESIAN_POINT('Ctrl Pts',(-11.9549368843996,-22.5373841537299,
12.));
#229035=CARTESIAN_POINT('Ctrl Pts',(-11.9325130877801,-22.5221157697869,
12.));
#229036=CARTESIAN_POINT('Ctrl Pts',(-11.9101844254555,-22.5068374513958,
12.));
#229037=CARTESIAN_POINT('Ctrl Pts',(-11.8879511239941,-22.4915496418472,
12.));
#229038=CARTESIAN_POINT('Ctrl Pts',(-11.8658134137018,-22.4762527946694,
12.));
#229039=CARTESIAN_POINT('Ctrl Pts',(-11.8437715264487,-22.4609473690469,
12.));
#229040=CARTESIAN_POINT('Ctrl Pts',(-11.8218256937889,-22.4456338258738,
12.));
#229041=CARTESIAN_POINT('Ctrl Pts',(-11.7999761445175,-22.4303126226468,
12.));
#229042=CARTESIAN_POINT('Ctrl Pts',(-11.7782231042041,-22.4149842125018,
12.));
#229043=CARTESIAN_POINT('Ctrl Pts',(-11.7565667964765,-22.39964904692,12.));
#229044=CARTESIAN_POINT('Ctrl Pts',(-11.7350074437961,-22.3843075773905,
12.));
#229045=CARTESIAN_POINT('Ctrl Pts',(-11.7135452684532,-22.3689602575492,
12.));
#229046=CARTESIAN_POINT('Ctrl Pts',(-11.6921804934056,-22.3536075450028,
12.));
#229047=CARTESIAN_POINT('Ctrl Pts',(-11.6709133432986,-22.3382499035618,
12.));
#229048=CARTESIAN_POINT('Ctrl Pts',(-11.6497440449858,-22.3228878043976,
12.));
#229049=CARTESIAN_POINT('Ctrl Pts',(-11.6286728270011,-22.3075217249049,
12.));
#229050=CARTESIAN_POINT('Ctrl Pts',(-11.6076999192359,-22.2921521480357,
12.));
#229051=CARTESIAN_POINT('Ctrl Pts',(-11.5868255525189,-22.2767795614349,
12.));
#229052=CARTESIAN_POINT('Ctrl Pts',(-11.5660499582403,-22.2614044566898,
12.));
#229053=CARTESIAN_POINT('Ctrl Pts',(-11.545373367912,-22.2460273284653,
12.));
#229054=CARTESIAN_POINT('Ctrl Pts',(-11.5247960128476,-22.2306486738899,
12.));
#229055=CARTESIAN_POINT('Ctrl Pts',(-11.504318124424,-22.215268993102,12.));
#229056=CARTESIAN_POINT('Ctrl Pts',(-11.4839399342589,-22.1998887896435,
12.));
#229057=CARTESIAN_POINT('Ctrl Pts',(-11.463661674411,-22.1845085709169,
12.));
#229058=CARTESIAN_POINT('Ctrl Pts',(-11.443483577557,-22.1691288486096,
12.));
#229059=CARTESIAN_POINT('Ctrl Pts',(-11.4234058771742,-22.1537501391486,
12.));
#229060=CARTESIAN_POINT('Ctrl Pts',(-11.4034288076909,-22.1383729640963,
12.));
#229061=CARTESIAN_POINT('Ctrl Pts',(-11.3835526044256,-22.1229978500185,
12.));
#229062=CARTESIAN_POINT('Ctrl Pts',(-11.3637775035367,-22.1076253283978,
12.));
#229063=CARTESIAN_POINT('Ctrl Pts',(-11.3441037419553,-22.0922559355293,
12.));
#229064=CARTESIAN_POINT('Ctrl Pts',(-11.3245315573168,-22.0768902124267,
12.));
#229065=CARTESIAN_POINT('Ctrl Pts',(-11.3050611878771,-22.0615287047179,
12.));
#229066=CARTESIAN_POINT('Ctrl Pts',(-11.2856928724374,-22.046171962566,
12.));
#229067=CARTESIAN_POINT('Ctrl Pts',(-11.2664268504207,-22.0308205408351,
12.));
#229068=CARTESIAN_POINT('Ctrl Pts',(-11.2472633619276,-22.0154749992364,
12.));
#229069=CARTESIAN_POINT('Ctrl Pts',(-11.2282026477897,-22.0001359024839,
12.));
#229070=CARTESIAN_POINT('Ctrl Pts',(-11.2092449496125,-21.9848038204439,
12.));
#229071=CARTESIAN_POINT('Ctrl Pts',(-11.190390509811,-21.9694793282913,
12.));
#229072=CARTESIAN_POINT('Ctrl Pts',(-11.1716395716375,-21.9541630066504,
12.));
#229073=CARTESIAN_POINT('Ctrl Pts',(-11.1529923792002,-21.9388554416437,
12.));
#229074=CARTESIAN_POINT('Ctrl Pts',(-11.134449177474,-21.9235572249518,
12.));
#229075=CARTESIAN_POINT('Ctrl Pts',(-11.1160102123024,-21.9082689538687,
12.));
#229076=CARTESIAN_POINT('Ctrl Pts',(-11.0976757303944,-21.8929912313608,
12.));
#229077=CARTESIAN_POINT('Ctrl Pts',(-11.0794459793058,-21.8777246661191,
12.));
#229078=CARTESIAN_POINT('Ctrl Pts',(-11.0613212074364,-21.8624698726319,
12.));
#229079=CARTESIAN_POINT('Ctrl Pts',(-11.0433016640808,-21.8472274713103,
12.));
#229080=CARTESIAN_POINT('Ctrl Pts',(-11.0253875994598,-21.8319980886033,
12.));
#229081=CARTESIAN_POINT('Ctrl Pts',(-11.0075792647477,-21.8167823571168,
12.));
#229082=CARTESIAN_POINT('Ctrl Pts',(-10.9898769120913,-21.8015809157302,
12.));
#229083=CARTESIAN_POINT('Ctrl Pts',(-10.9722807946157,-21.7863944097143,
12.));
#229084=CARTESIAN_POINT('Ctrl Pts',(-10.9547911664457,-21.7712234908468,
12.));
#229085=CARTESIAN_POINT('Ctrl Pts',(-10.9374082827446,-21.7560688175252,
12.));
#229086=CARTESIAN_POINT('Ctrl Pts',(-10.9201323997386,-21.74093105488,12.));
#229087=CARTESIAN_POINT('Ctrl Pts',(-10.9029637747341,-21.7258108748874,
12.));
#229088=CARTESIAN_POINT('Ctrl Pts',(-10.8859026661292,-21.7107089564822,
12.));
#229089=CARTESIAN_POINT('Ctrl Pts',(-10.8689493334093,-21.6956259856667,
12.));
#229090=CARTESIAN_POINT('Ctrl Pts',(-10.8521040371832,-21.6805626556461,
12.));
#229091=CARTESIAN_POINT('Ctrl Pts',(-10.835367039227,-21.6655196669727,
12.));
#229092=CARTESIAN_POINT('Ctrl Pts',(-10.8187386025135,-21.6504977276864,
12.));
#229093=CARTESIAN_POINT('Ctrl Pts',(-10.802218991237,-21.6354975534557,
12.));
#229094=CARTESIAN_POINT('Ctrl Pts',(-10.7858084708262,-21.6205198677176,
12.));
#229095=CARTESIAN_POINT('Ctrl Pts',(-10.7695073079554,-21.6055654018179,
12.));
#229096=CARTESIAN_POINT('Ctrl Pts',(-10.7533157705943,-21.5906348951745,
12.));
#229097=CARTESIAN_POINT('Ctrl Pts',(-10.7372341280468,-21.5757290954372,
12.));
#229098=CARTESIAN_POINT('Ctrl Pts',(-10.7212626509816,-21.5608487586467,
12.));
#229099=CARTESIAN_POINT('Ctrl Pts',(-10.7054016114571,-21.5459946493955,
12.));
#229100=CARTESIAN_POINT('Ctrl Pts',(-10.689651282929,-21.531167540981,12.));
#229101=CARTESIAN_POINT('Ctrl Pts',(-10.6740119402835,-21.5163682155805,
12.));
#229102=CARTESIAN_POINT('Ctrl Pts',(-10.6584838598941,-21.5015974644454,
12.));
#229103=CARTESIAN_POINT('Ctrl Pts',(-10.6430673196609,-21.4868560880893,
12.));
#229104=CARTESIAN_POINT('Ctrl Pts',(-10.6277625990457,-21.4721448964766,
12.));
#229105=CARTESIAN_POINT('Ctrl Pts',(-10.612569979096,-21.4574647092093,
12.));
#229106=CARTESIAN_POINT('Ctrl Pts',(-10.597489742462,-21.4428163557137,
12.));
#229107=CARTESIAN_POINT('Ctrl Pts',(-10.582522173457,-21.4282006754624,
12.));
#229108=CARTESIAN_POINT('Ctrl Pts',(-10.5676675581106,-21.4136185181974,
12.));
#229109=CARTESIAN_POINT('Ctrl Pts',(-10.5529261842107,-21.3990707441495,
12.));
#229110=CARTESIAN_POINT('Ctrl Pts',(-10.5382983413422,-21.3845582242604,
12.));
#229111=CARTESIAN_POINT('Ctrl Pts',(-10.523784320906,-21.3700818403942,
12.));
#229112=CARTESIAN_POINT('Ctrl Pts',(-10.509384416169,-21.3556424855822,
12.));
#229113=CARTESIAN_POINT('Ctrl Pts',(-10.4950989223341,-21.3412410642912,
12.));
#229114=CARTESIAN_POINT('Ctrl Pts',(-10.4809281365933,-21.3268784926823,
12.));
#229115=CARTESIAN_POINT('Ctrl Pts',(-10.4668723581768,-21.312555698873,
12.));
#229116=CARTESIAN_POINT('Ctrl Pts',(-10.452931888387,-21.2982736231924,
12.));
#229117=CARTESIAN_POINT('Ctrl Pts',(-10.4391070306385,-21.2840332184471,
12.));
#229118=CARTESIAN_POINT('Ctrl Pts',(-10.4253980905394,-21.2698354502391,
12.));
#229119=CARTESIAN_POINT('Ctrl Pts',(-10.4118053759584,-21.2556812972741,
12.));
#229120=CARTESIAN_POINT('Ctrl Pts',(-10.3983291970846,-21.2415717516713,
12.));
#229121=CARTESIAN_POINT('Ctrl Pts',(-10.384969866479,-21.2275078192708,
12.));
#229122=CARTESIAN_POINT('Ctrl Pts',(-10.3717276991137,-21.2134905199359,
12.));
#229123=CARTESIAN_POINT('Ctrl Pts',(-10.3586030124595,-21.1995208879205,
12.));
#229124=CARTESIAN_POINT('Ctrl Pts',(-10.3455961265706,-21.1855999722427,
12.));
#229125=CARTESIAN_POINT('Ctrl Pts',(-10.3327073641574,-21.1717288370512,
12.));
#229126=CARTESIAN_POINT('Ctrl Pts',(-10.3199370506541,-21.1579085619959,
12.));
#229127=CARTESIAN_POINT('Ctrl Pts',(-10.307285514268,-21.1441402425831,
12.));
#229128=CARTESIAN_POINT('Ctrl Pts',(-10.2947530860714,-21.130424990599,
12.));
#229129=CARTESIAN_POINT('Ctrl Pts',(-10.2823401001067,-21.1167639345623,
12.));
#229130=CARTESIAN_POINT('Ctrl Pts',(-10.2700468934743,-21.1031582201625,
12.));
#229131=CARTESIAN_POINT('Ctrl Pts',(-10.2578738064183,-21.0896090107066,
12.));
#229132=CARTESIAN_POINT('Ctrl Pts',(-10.2458211823915,-21.0761174875448,
12.));
#229133=CARTESIAN_POINT('Ctrl Pts',(-10.233889368157,-21.0626848505665,
12.));
#229134=CARTESIAN_POINT('Ctrl Pts',(-10.2220787139157,-21.0493123187483,
12.));
#229135=CARTESIAN_POINT('Ctrl Pts',(-10.2103895734124,-21.0360011306814,
12.));
#229136=CARTESIAN_POINT('Ctrl Pts',(-10.1988223040425,-21.0227525451107,
12.));
#229137=CARTESIAN_POINT('Ctrl Pts',(-10.1873772669358,-21.0095678414486,
12.));
#229138=CARTESIAN_POINT('Ctrl Pts',(-10.1760548270765,-20.9964483203685,
12.));
#229139=CARTESIAN_POINT('Ctrl Pts',(-10.1648553534567,-20.9833953044736,
12.));
#229140=CARTESIAN_POINT('Ctrl Pts',(-10.1537792192065,-20.970410138937,
12.));
#229141=CARTESIAN_POINT('Ctrl Pts',(-10.1428268017257,-20.9574941921591,
12.));
#229142=CARTESIAN_POINT('Ctrl Pts',(-10.1319984827909,-20.944648856393,
12.));
#229143=CARTESIAN_POINT('Ctrl Pts',(-10.1212946487057,-20.931875548473,
12.));
#229144=CARTESIAN_POINT('Ctrl Pts',(-10.1107156904836,-20.9191757106266,
12.));
#229145=CARTESIAN_POINT('Ctrl Pts',(-10.1002620040076,-20.9065508112556,
12.));
#229146=CARTESIAN_POINT('Ctrl Pts',(-10.0899339901916,-20.8940023457371,
12.));
#229147=CARTESIAN_POINT('Ctrl Pts',(-10.0797320551154,-20.8815318371844,
12.));
#229148=CARTESIAN_POINT('Ctrl Pts',(-10.0696566102219,-20.8691408373705,
12.));
#229149=CARTESIAN_POINT('Ctrl Pts',(-10.0597080725375,-20.856830927732,
12.));
#229150=CARTESIAN_POINT('Ctrl Pts',(-10.0498868648733,-20.8446037203402,
12.));
#229151=CARTESIAN_POINT('Ctrl Pts',(-10.0401934160234,-20.8324608588906,
12.));
#229152=CARTESIAN_POINT('Ctrl Pts',(-10.0306281609435,-20.8204040196599,
12.));
#229153=CARTESIAN_POINT('Ctrl Pts',(-10.0211915410095,-20.8084349126885,
12.));
#229154=CARTESIAN_POINT('Ctrl Pts',(-10.0118840042786,-20.7965552829907,
12.));
#229155=CARTESIAN_POINT('Ctrl Pts',(-10.0027060057389,-20.7847669117568,
12.));
#229156=CARTESIAN_POINT('Ctrl Pts',(-9.99365800754638,-20.7730716175417,
12.));
#229157=CARTESIAN_POINT('Ctrl Pts',(-9.98474047926846,-20.7614712574989,
12.));
#229158=CARTESIAN_POINT('Ctrl Pts',(-9.97595389823461,-20.7499677289625,
12.));
#229159=CARTESIAN_POINT('Ctrl Pts',(-9.96729874986199,-20.7385629709795,
12.));
#229160=CARTESIAN_POINT('Ctrl Pts',(-9.95877552798403,-20.7272589658752,
12.));
#229161=CARTESIAN_POINT('Ctrl Pts',(-9.95038473514962,-20.716057740758,
12.));
#229162=CARTESIAN_POINT('Ctrl Pts',(-9.94212688298251,-20.7049613692237,
12.));
#229163=CARTESIAN_POINT('Ctrl Pts',(-9.93400249259737,-20.6939719732485,
12.));
#229164=CARTESIAN_POINT('Ctrl Pts',(-9.92601209498751,-20.6830917250255,
12.));
#229165=CARTESIAN_POINT('Ctrl Pts',(-9.91815623141285,-20.6723228488261,
12.));
#229166=CARTESIAN_POINT('Ctrl Pts',(-9.91043545377005,-20.6616676228315,
12.));
#229167=CARTESIAN_POINT('Ctrl Pts',(-9.90285032516696,-20.6511283817415,
12.));
#229168=CARTESIAN_POINT('Ctrl Pts',(-9.89540142049124,-20.6407075193977,
12.));
#229169=CARTESIAN_POINT('Ctrl Pts',(-9.88808932697305,-20.6304074914086,
12.));
#229170=CARTESIAN_POINT('Ctrl Pts',(-9.88091464472669,-20.6202308177472,
12.));
#229171=CARTESIAN_POINT('Ctrl Pts',(-9.87387798732944,-20.6101800854491,
12.));
#229172=CARTESIAN_POINT('Ctrl Pts',(-9.86697998242612,-20.6002579513696,
12.));
#229173=CARTESIAN_POINT('Ctrl Pts',(-9.8602212723275,-20.5904671449754,
12.));
#229174=CARTESIAN_POINT('Ctrl Pts',(-9.85360251457004,-20.580810471002,
12.));
#229175=CARTESIAN_POINT('Ctrl Pts',(-9.84712438256308,-20.5712908125145,
12.));
#229176=CARTESIAN_POINT('Ctrl Pts',(-9.84078756677589,-20.5619111362406,
12.));
#229177=CARTESIAN_POINT('Ctrl Pts',(-9.83459277585321,-20.5526744976461,
12.));
#229178=CARTESIAN_POINT('Ctrl Pts',(-9.82854073773858,-20.5435840460717,
12.));
#229179=CARTESIAN_POINT('Ctrl Pts',(-9.82263220080328,-20.534643029951,
12.));
#229180=CARTESIAN_POINT('Ctrl Pts',(-9.81686793455918,-20.5258548000625,
12.));
#229181=CARTESIAN_POINT('Ctrl Pts',(-9.81124873025278,-20.5172228122839,
12.));
#229182=CARTESIAN_POINT('Ctrl Pts',(-9.80577540161103,-20.5087506310507,
12.));
#229183=CARTESIAN_POINT('Ctrl Pts',(-9.80044878520968,-20.500441931211,
12.));
#229184=CARTESIAN_POINT('Ctrl Pts',(-9.79526974288344,-20.4923005087945,
12.));
#229185=CARTESIAN_POINT('Ctrl Pts',(-9.7902391649866,-20.4843302955329,
12.));
#229186=CARTESIAN_POINT('Ctrl Pts',(-9.78535797314162,-20.4765353711585,
12.));
#229187=CARTESIAN_POINT('Ctrl Pts',(-9.78062712373313,-20.4689199790668,
12.));
#229188=CARTESIAN_POINT('Ctrl Pts',(-9.77604760815523,-20.4614885274973,
12.));
#229189=CARTESIAN_POINT('Ctrl Pts',(-9.7716204510407,-20.4542455817527,
12.));
#229190=CARTESIAN_POINT('Ctrl Pts',(-9.76734670980897,-20.447195862298,
12.));
#229191=CARTESIAN_POINT('Ctrl Pts',(-9.76322747195502,-20.4403442329401,
12.));
#229192=CARTESIAN_POINT('Ctrl Pts',(-9.7592638628993,-20.4336957355474,
12.));
#229193=CARTESIAN_POINT('Ctrl Pts',(-9.75545705902416,-20.4272556476629,
12.));
#229194=CARTESIAN_POINT('Ctrl Pts',(-9.75180829786433,-20.4210295275818,
12.));
#229195=CARTESIAN_POINT('Ctrl Pts',(-9.74831889242175,-20.4150232777393,
12.));
#229196=CARTESIAN_POINT('Ctrl Pts',(-9.74499021838537,-20.4092430879861,
12.));
#229197=CARTESIAN_POINT('Ctrl Pts',(-9.74182369656273,-20.4036953576549,
12.));
#229198=CARTESIAN_POINT('Ctrl Pts',(-9.73882077613206,-20.3983866213331,
12.));
#229199=CARTESIAN_POINT('Ctrl Pts',(-9.7359829201425,-20.3933234845646,
12.));
#229200=CARTESIAN_POINT('Ctrl Pts',(-9.73331167102812,-20.3885129129912,
12.));
#229201=CARTESIAN_POINT('Ctrl Pts',(-9.73080870123726,-20.3839624556742,
12.));
#229202=CARTESIAN_POINT('Ctrl Pts',(-9.72847589116533,-20.3796805893304,
12.));
#229203=CARTESIAN_POINT('Ctrl Pts',(-9.72631531732871,-20.3756766651952,
12.));
#229204=CARTESIAN_POINT('Ctrl Pts',(-9.72432910043193,-20.371960235676,
12.));
#229205=CARTESIAN_POINT('Ctrl Pts',(-9.72251930722504,-20.3685406190576,
12.));
#229206=CARTESIAN_POINT('Ctrl Pts',(-9.72088778381102,-20.3654261611055,
12.));
#229207=CARTESIAN_POINT('Ctrl Pts',(-9.71943648548115,-20.362625691398,
12.));
#229208=CARTESIAN_POINT('Ctrl Pts',(-9.71816778327999,-20.3601498764344,
12.));
#229209=CARTESIAN_POINT('Ctrl Pts',(-9.71708493723062,-20.3580133103357,
12.));
#229210=CARTESIAN_POINT('Ctrl Pts',(-9.71619192554147,-20.3562337557875,
12.));
#229211=CARTESIAN_POINT('Ctrl Pts',(-9.71549257088175,-20.3548282742361,
12.));
#229212=CARTESIAN_POINT('Ctrl Pts',(-9.71498978052101,-20.3538098605706,
12.));
#229213=CARTESIAN_POINT('Ctrl Pts',(-9.71474590350792,-20.3533097561886,
12.));
#229214=CARTESIAN_POINT('Ctrl Pts',(-9.71465227853122,-20.3531126095522,
12.));
#229215=CARTESIAN_POINT('Ctrl Pts',(-9.71462954053074,-20.353060251684,
12.));
#229216=CARTESIAN_POINT('Ctrl Pts',(-9.71462809124917,-20.353053841303,
12.));
#229217=CARTESIAN_POINT('',(-12.4230808101438,-22.8400320311648,0.));
#229218=CARTESIAN_POINT('Origin',(-13.9675290154577,-16.3449727195351,0.));
#229219=CARTESIAN_POINT('',(-14.6513681262571,-17.1452095830632,12.));
#229220=CARTESIAN_POINT('',(-6.98376450772884,-8.17248635976757,12.));
#229221=CARTESIAN_POINT('',(-14.6513681262571,-17.1452095830632,0.));
#229222=CARTESIAN_POINT('',(-14.6513681262571,-17.1452095830632,0.));
#229223=CARTESIAN_POINT('',(-6.98376450772884,-8.17248635976757,0.));
#229224=CARTESIAN_POINT('Ctrl Pts',(-13.5685075571671,-22.1787195904339,
0.));
#229225=CARTESIAN_POINT('Ctrl Pts',(-13.5685075571671,-22.1787195904339,
12.));
#229226=CARTESIAN_POINT('Ctrl Pts',(-13.5683460612913,-22.1730081264583,
0.));
#229227=CARTESIAN_POINT('Ctrl Pts',(-13.5683460612913,-22.1730081264583,
12.));
#229228=CARTESIAN_POINT('Ctrl Pts',(-13.5680170531724,-22.1615922804939,
0.));
#229229=CARTESIAN_POINT('Ctrl Pts',(-13.5680170531724,-22.1615922804939,
12.));
#229230=CARTESIAN_POINT('Ctrl Pts',(-13.5675054918922,-22.1444897575076,
0.));
#229231=CARTESIAN_POINT('Ctrl Pts',(-13.5675054918922,-22.1444897575076,
12.));
#229232=CARTESIAN_POINT('Ctrl Pts',(-13.5667873105179,-22.1217288871823,
0.));
#229233=CARTESIAN_POINT('Ctrl Pts',(-13.5667873105179,-22.1217288871823,
12.));
#229234=CARTESIAN_POINT('Ctrl Pts',(-13.5658294169107,-22.0933486464442,
0.));
#229235=CARTESIAN_POINT('Ctrl Pts',(-13.5658294169107,-22.0933486464442,
12.));
#229236=CARTESIAN_POINT('Ctrl Pts',(-13.5648113688895,-22.0650393089492,
0.));
#229237=CARTESIAN_POINT('Ctrl Pts',(-13.5648113688895,-22.0650393089492,
12.));
#229238=CARTESIAN_POINT('Ctrl Pts',(-13.5637332022393,-22.0368009736227,
0.));
#229239=CARTESIAN_POINT('Ctrl Pts',(-13.5637332022393,-22.0368009736227,
12.));
#229240=CARTESIAN_POINT('Ctrl Pts',(-13.5625949868313,-22.0086337943431,
0.));
#229241=CARTESIAN_POINT('Ctrl Pts',(-13.5625949868313,-22.0086337943431,
12.));
#229242=CARTESIAN_POINT('Ctrl Pts',(-13.5613968357589,-21.9805379899192,
0.));
#229243=CARTESIAN_POINT('Ctrl Pts',(-13.5613968357589,-21.9805379899192,
12.));
#229244=CARTESIAN_POINT('Ctrl Pts',(-13.5601389185315,-21.9525138592862,
0.));
#229245=CARTESIAN_POINT('Ctrl Pts',(-13.5601389185315,-21.9525138592862,
12.));
#229246=CARTESIAN_POINT('Ctrl Pts',(-13.5588214586672,-21.9245617765827,
0.));
#229247=CARTESIAN_POINT('Ctrl Pts',(-13.5588214586672,-21.9245617765827,
12.));
#229248=CARTESIAN_POINT('Ctrl Pts',(-13.5574447178485,-21.8966821688876,
0.));
#229249=CARTESIAN_POINT('Ctrl Pts',(-13.5574447178485,-21.8966821688876,
12.));
#229250=CARTESIAN_POINT('Ctrl Pts',(-13.5560089839426,-21.8688754989401,
0.));
#229251=CARTESIAN_POINT('Ctrl Pts',(-13.5560089839426,-21.8688754989401,
12.));
#229252=CARTESIAN_POINT('Ctrl Pts',(-13.5545145573049,-21.841142245609,
0.));
#229253=CARTESIAN_POINT('Ctrl Pts',(-13.5545145573049,-21.841142245609,
12.));
#229254=CARTESIAN_POINT('Ctrl Pts',(-13.5529617381569,-21.8134828857963,
0.));
#229255=CARTESIAN_POINT('Ctrl Pts',(-13.5529617381569,-21.8134828857963,
12.));
#229256=CARTESIAN_POINT('Ctrl Pts',(-13.5513508127232,-21.7858978745848,
0.));
#229257=CARTESIAN_POINT('Ctrl Pts',(-13.5513508127232,-21.7858978745848,
12.));
#229258=CARTESIAN_POINT('Ctrl Pts',(-13.5496820422187,-21.7583876294532,
0.));
#229259=CARTESIAN_POINT('Ctrl Pts',(-13.5496820422187,-21.7583876294532,
12.));
#229260=CARTESIAN_POINT('Ctrl Pts',(-13.5479556704457,-21.730952541226,
0.));
#229261=CARTESIAN_POINT('Ctrl Pts',(-13.5479556704457,-21.730952541226,
12.));
#229262=CARTESIAN_POINT('Ctrl Pts',(-13.546171929503,-21.7035929822939,
0.));
#229263=CARTESIAN_POINT('Ctrl Pts',(-13.546171929503,-21.7035929822939,
12.));
#229264=CARTESIAN_POINT('Ctrl Pts',(-13.5443310461516,-21.676309315769,
0.));
#229265=CARTESIAN_POINT('Ctrl Pts',(-13.5443310461516,-21.676309315769,
12.));
#229266=CARTESIAN_POINT('Ctrl Pts',(-13.5424332480698,-21.6491019044647,
0.));
#229267=CARTESIAN_POINT('Ctrl Pts',(-13.5424332480698,-21.6491019044647,
12.));
#229268=CARTESIAN_POINT('Ctrl Pts',(-13.5404787697798,-21.6219711193951,
0.));
#229269=CARTESIAN_POINT('Ctrl Pts',(-13.5404787697798,-21.6219711193951,
12.));
#229270=CARTESIAN_POINT('Ctrl Pts',(-13.5384678597206,-21.5949173499022,
0.));
#229271=CARTESIAN_POINT('Ctrl Pts',(-13.5384678597206,-21.5949173499022,
12.));
#229272=CARTESIAN_POINT('Ctrl Pts',(-13.5364007790292,-21.5679410019011,
0.));
#229273=CARTESIAN_POINT('Ctrl Pts',(-13.5364007790292,-21.5679410019011,
12.));
#229274=CARTESIAN_POINT('Ctrl Pts',(-13.5342777983225,-21.5410424932511,
0.));
#229275=CARTESIAN_POINT('Ctrl Pts',(-13.5342777983225,-21.5410424932511,
12.));
#229276=CARTESIAN_POINT('Ctrl Pts',(-13.5320991952145,-21.5142222501671,
0.));
#229277=CARTESIAN_POINT('Ctrl Pts',(-13.5320991952145,-21.5142222501671,
12.));
#229278=CARTESIAN_POINT('Ctrl Pts',(-13.5298652514357,-21.487480703047,
0.));
#229279=CARTESIAN_POINT('Ctrl Pts',(-13.5298652514357,-21.487480703047,
12.));
#229280=CARTESIAN_POINT('Ctrl Pts',(-13.5275762503553,-21.4608182828695,
0.));
#229281=CARTESIAN_POINT('Ctrl Pts',(-13.5275762503553,-21.4608182828695,
12.));
#229282=CARTESIAN_POINT('Ctrl Pts',(-13.5252324737795,-21.4342354165253,
0.));
#229283=CARTESIAN_POINT('Ctrl Pts',(-13.5252324737795,-21.4342354165253,
12.));
#229284=CARTESIAN_POINT('Ctrl Pts',(-13.5228342013508,-21.4077325259318,
0.));
#229285=CARTESIAN_POINT('Ctrl Pts',(-13.5228342013508,-21.4077325259318,
12.));
#229286=CARTESIAN_POINT('Ctrl Pts',(-13.5203817122497,-21.3813100304967,
0.));
#229287=CARTESIAN_POINT('Ctrl Pts',(-13.5203817122497,-21.3813100304967,
12.));
#229288=CARTESIAN_POINT('Ctrl Pts',(-13.5178752862461,-21.3549683486219,
0.));
#229289=CARTESIAN_POINT('Ctrl Pts',(-13.5178752862461,-21.3549683486219,
12.));
#229290=CARTESIAN_POINT('Ctrl Pts',(-13.5153152050554,-21.328707899634,
0.));
#229291=CARTESIAN_POINT('Ctrl Pts',(-13.5153152050554,-21.328707899634,
12.));
#229292=CARTESIAN_POINT('Ctrl Pts',(-13.5127017534972,-21.3025291054236,
0.));
#229293=CARTESIAN_POINT('Ctrl Pts',(-13.5127017534972,-21.3025291054236,
12.));
#229294=CARTESIAN_POINT('Ctrl Pts',(-13.5100352209207,-21.2764323924442,
0.));
#229295=CARTESIAN_POINT('Ctrl Pts',(-13.5100352209207,-21.2764323924442,
12.));
#229296=CARTESIAN_POINT('Ctrl Pts',(-13.5073159019454,-21.2504181927429,
0.));
#229297=CARTESIAN_POINT('Ctrl Pts',(-13.5073159019454,-21.2504181927429,
12.));
#229298=CARTESIAN_POINT('Ctrl Pts',(-13.5045440957404,-21.224486942933,
0.));
#229299=CARTESIAN_POINT('Ctrl Pts',(-13.5045440957404,-21.224486942933,
12.));
#229300=CARTESIAN_POINT('Ctrl Pts',(-13.5017201056088,-21.1986390835825,
0.));
#229301=CARTESIAN_POINT('Ctrl Pts',(-13.5017201056088,-21.1986390835825,
12.));
#229302=CARTESIAN_POINT('Ctrl Pts',(-13.4988442384491,-21.1728750584173,
0.));
#229303=CARTESIAN_POINT('Ctrl Pts',(-13.4988442384491,-21.1728750584173,
12.));
#229304=CARTESIAN_POINT('Ctrl Pts',(-13.4959168042934,-21.1471953136209,
0.));
#229305=CARTESIAN_POINT('Ctrl Pts',(-13.4959168042934,-21.1471953136209,
12.));
#229306=CARTESIAN_POINT('Ctrl Pts',(-13.4929381157778,-21.1216002970209,
0.));
#229307=CARTESIAN_POINT('Ctrl Pts',(-13.4929381157778,-21.1216002970209,
12.));
#229308=CARTESIAN_POINT('Ctrl Pts',(-13.4899084877718,-21.0960904575048,
0.));
#229309=CARTESIAN_POINT('Ctrl Pts',(-13.4899084877718,-21.0960904575048,
12.));
#229310=CARTESIAN_POINT('Ctrl Pts',(-13.4868282377192,-21.0706662455202,
0.));
#229311=CARTESIAN_POINT('Ctrl Pts',(-13.4868282377192,-21.0706662455202,
12.));
#229312=CARTESIAN_POINT('Ctrl Pts',(-13.4836976858912,-21.0453281134247,
0.));
#229313=CARTESIAN_POINT('Ctrl Pts',(-13.4836976858912,-21.0453281134247,
12.));
#229314=CARTESIAN_POINT('Ctrl Pts',(-13.4805171556822,-21.0200765158885,
0.));
#229315=CARTESIAN_POINT('Ctrl Pts',(-13.4805171556822,-21.0200765158885,
12.));
#229316=CARTESIAN_POINT('Ctrl Pts',(-13.4772869738879,-20.9949119102592,
0.));
#229317=CARTESIAN_POINT('Ctrl Pts',(-13.4772869738879,-20.9949119102592,
12.));
#229318=CARTESIAN_POINT('Ctrl Pts',(-13.4740074710087,-20.9698347569476,
0.));
#229319=CARTESIAN_POINT('Ctrl Pts',(-13.4740074710087,-20.9698347569476,
12.));
#229320=CARTESIAN_POINT('Ctrl Pts',(-13.4706789815167,-20.9448455197557,
0.));
#229321=CARTESIAN_POINT('Ctrl Pts',(-13.4706789815167,-20.9448455197557,
12.));
#229322=CARTESIAN_POINT('Ctrl Pts',(-13.4673018437718,-20.9199446657584,
0.));
#229323=CARTESIAN_POINT('Ctrl Pts',(-13.4673018437718,-20.9199446657584,
12.));
#229324=CARTESIAN_POINT('Ctrl Pts',(-13.4638763999726,-20.8951326652158,
0.));
#229325=CARTESIAN_POINT('Ctrl Pts',(-13.4638763999726,-20.8951326652158,
12.));
#229326=CARTESIAN_POINT('Ctrl Pts',(-13.4604029960983,-20.8704099914641,
0.));
#229327=CARTESIAN_POINT('Ctrl Pts',(-13.4604029960983,-20.8704099914641,
12.));
#229328=CARTESIAN_POINT('Ctrl Pts',(-13.4568819818631,-20.8457771208082,
0.));
#229329=CARTESIAN_POINT('Ctrl Pts',(-13.4568819818631,-20.8457771208082,
12.));
#229330=CARTESIAN_POINT('Ctrl Pts',(-13.4533137106667,-20.821234532398,
0.));
#229331=CARTESIAN_POINT('Ctrl Pts',(-13.4533137106667,-20.821234532398,
12.));
#229332=CARTESIAN_POINT('Ctrl Pts',(-13.4496985395637,-20.7967827081227,
0.));
#229333=CARTESIAN_POINT('Ctrl Pts',(-13.4496985395637,-20.7967827081227,
12.));
#229334=CARTESIAN_POINT('Ctrl Pts',(-13.4460368293688,-20.7724221327608,
0.));
#229335=CARTESIAN_POINT('Ctrl Pts',(-13.4460368293688,-20.7724221327608,
12.));
#229336=CARTESIAN_POINT('Ctrl Pts',(-13.4423289447561,-20.7481532941013,
0.));
#229337=CARTESIAN_POINT('Ctrl Pts',(-13.4423289447561,-20.7481532941013,
12.));
#229338=CARTESIAN_POINT('Ctrl Pts',(-13.4385752543663,-20.7239766830675,
0.));
#229339=CARTESIAN_POINT('Ctrl Pts',(-13.4385752543663,-20.7239766830675,
12.));
#229340=CARTESIAN_POINT('Ctrl Pts',(-13.4347761309154,-20.6998927938288,
0.));
#229341=CARTESIAN_POINT('Ctrl Pts',(-13.4347761309154,-20.6998927938288,
12.));
#229342=CARTESIAN_POINT('Ctrl Pts',(-13.4309319513119,-20.6759021239103,
0.));
#229343=CARTESIAN_POINT('Ctrl Pts',(-13.4309319513119,-20.6759021239103,
12.));
#229344=CARTESIAN_POINT('Ctrl Pts',(-13.4270430967652,-20.6520051742869,
0.));
#229345=CARTESIAN_POINT('Ctrl Pts',(-13.4270430967652,-20.6520051742869,
12.));
#229346=CARTESIAN_POINT('Ctrl Pts',(-13.4231099528179,-20.6282024494237,
0.));
#229347=CARTESIAN_POINT('Ctrl Pts',(-13.4231099528179,-20.6282024494237,
12.));
#229348=CARTESIAN_POINT('Ctrl Pts',(-13.4191329093933,-20.6044944573153,
0.));
#229349=CARTESIAN_POINT('Ctrl Pts',(-13.4191329093933,-20.6044944573153,
12.));
#229350=CARTESIAN_POINT('Ctrl Pts',(-13.4151123608411,-20.5808817095155,
0.));
#229351=CARTESIAN_POINT('Ctrl Pts',(-13.4151123608411,-20.5808817095155,
12.));
#229352=CARTESIAN_POINT('Ctrl Pts',(-13.4110487059912,-20.5573647211639,
0.));
#229353=CARTESIAN_POINT('Ctrl Pts',(-13.4110487059912,-20.5573647211639,
12.));
#229354=CARTESIAN_POINT('Ctrl Pts',(-13.4069423482076,-20.5339440109956,
0.));
#229355=CARTESIAN_POINT('Ctrl Pts',(-13.4069423482076,-20.5339440109956,
12.));
#229356=CARTESIAN_POINT('Ctrl Pts',(-13.4027936954529,-20.5106201013753,
0.));
#229357=CARTESIAN_POINT('Ctrl Pts',(-13.4027936954529,-20.5106201013753,
12.));
#229358=CARTESIAN_POINT('Ctrl Pts',(-13.3986031603716,-20.487393518404,
0.));
#229359=CARTESIAN_POINT('Ctrl Pts',(-13.3986031603716,-20.487393518404,
12.));
#229360=CARTESIAN_POINT('Ctrl Pts',(-13.3943711603739,-20.4642647920037,
0.));
#229361=CARTESIAN_POINT('Ctrl Pts',(-13.3943711603739,-20.4642647920037,
12.));
#229362=CARTESIAN_POINT('Ctrl Pts',(-13.3900981177255,-20.4412344560007,
0.));
#229363=CARTESIAN_POINT('Ctrl Pts',(-13.3900981177255,-20.4412344560007,
12.));
#229364=CARTESIAN_POINT('Ctrl Pts',(-13.3857844596387,-20.4183030482002,
0.));
#229365=CARTESIAN_POINT('Ctrl Pts',(-13.3857844596387,-20.4183030482002,
12.));
#229366=CARTESIAN_POINT('Ctrl Pts',(-13.3814306183719,-20.3954711104502,
0.));
#229367=CARTESIAN_POINT('Ctrl Pts',(-13.3814306183719,-20.3954711104502,
12.));
#229368=CARTESIAN_POINT('Ctrl Pts',(-13.3770370313188,-20.3727391887184,
0.));
#229369=CARTESIAN_POINT('Ctrl Pts',(-13.3770370313188,-20.3727391887184,
12.));
#229370=CARTESIAN_POINT('Ctrl Pts',(-13.3726041410867,-20.3501078331814,
0.));
#229371=CARTESIAN_POINT('Ctrl Pts',(-13.3726041410867,-20.3501078331814,
12.));
#229372=CARTESIAN_POINT('Ctrl Pts',(-13.3681323955826,-20.3275775983029,
0.));
#229373=CARTESIAN_POINT('Ctrl Pts',(-13.3681323955826,-20.3275775983029,
12.));
#229374=CARTESIAN_POINT('Ctrl Pts',(-13.3636222481016,-20.3051490429048,
0.));
#229375=CARTESIAN_POINT('Ctrl Pts',(-13.3636222481016,-20.3051490429048,
12.));
#229376=CARTESIAN_POINT('Ctrl Pts',(-13.3590741574195,-20.2828227302339,
0.));
#229377=CARTESIAN_POINT('Ctrl Pts',(-13.3590741574195,-20.2828227302339,
12.));
#229378=CARTESIAN_POINT('Ctrl Pts',(-13.3544885878889,-20.2605992280122,
0.));
#229379=CARTESIAN_POINT('Ctrl Pts',(-13.3544885878889,-20.2605992280122,
12.));
#229380=CARTESIAN_POINT('Ctrl Pts',(-13.3498660095386,-20.2384791085359,
0.));
#229381=CARTESIAN_POINT('Ctrl Pts',(-13.3498660095386,-20.2384791085359,
12.));
#229382=CARTESIAN_POINT('Ctrl Pts',(-13.3452068981766,-20.216462948786,
0.));
#229383=CARTESIAN_POINT('Ctrl Pts',(-13.3452068981766,-20.216462948786,
12.));
#229384=CARTESIAN_POINT('Ctrl Pts',(-13.3405117354971,-20.1945513305235,
0.));
#229385=CARTESIAN_POINT('Ctrl Pts',(-13.3405117354971,-20.1945513305235,
12.));
#229386=CARTESIAN_POINT('Ctrl Pts',(-13.3357810091903,-20.1727448403817,
0.));
#229387=CARTESIAN_POINT('Ctrl Pts',(-13.3357810091903,-20.1727448403817,
12.));
#229388=CARTESIAN_POINT('Ctrl Pts',(-13.3310152130564,-20.1510440699474,
0.));
#229389=CARTESIAN_POINT('Ctrl Pts',(-13.3310152130564,-20.1510440699474,
12.));
#229390=CARTESIAN_POINT('Ctrl Pts',(-13.3262148471226,-20.1294496158402,
0.));
#229391=CARTESIAN_POINT('Ctrl Pts',(-13.3262148471226,-20.1294496158402,
12.));
#229392=CARTESIAN_POINT('Ctrl Pts',(-13.3213804177587,-20.1079620798375,
0.));
#229393=CARTESIAN_POINT('Ctrl Pts',(-13.3213804177587,-20.1079620798375,
12.));
#229394=CARTESIAN_POINT('Ctrl Pts',(-13.3165124377963,-20.0865820689882,
0.));
#229395=CARTESIAN_POINT('Ctrl Pts',(-13.3165124377963,-20.0865820689882,
12.));
#229396=CARTESIAN_POINT('Ctrl Pts',(-13.3116114266515,-20.0653101957188,
0.));
#229397=CARTESIAN_POINT('Ctrl Pts',(-13.3116114266515,-20.0653101957188,
12.));
#229398=CARTESIAN_POINT('Ctrl Pts',(-13.3066779104515,-20.0441470779345,
0.));
#229399=CARTESIAN_POINT('Ctrl Pts',(-13.3066779104515,-20.0441470779345,
12.));
#229400=CARTESIAN_POINT('Ctrl Pts',(-13.3017124221637,-20.0230933391038,
0.));
#229401=CARTESIAN_POINT('Ctrl Pts',(-13.3017124221637,-20.0230933391038,
12.));
#229402=CARTESIAN_POINT('Ctrl Pts',(-13.2967155017306,-20.0021496083738,
0.));
#229403=CARTESIAN_POINT('Ctrl Pts',(-13.2967155017306,-20.0021496083738,
12.));
#229404=CARTESIAN_POINT('Ctrl Pts',(-13.2916876962094,-19.981316520717,
0.));
#229405=CARTESIAN_POINT('Ctrl Pts',(-13.2916876962094,-19.981316520717,
12.));
#229406=CARTESIAN_POINT('Ctrl Pts',(-13.286629559915,-19.9605947170586,
0.));
#229407=CARTESIAN_POINT('Ctrl Pts',(-13.286629559915,-19.9605947170586,
12.));
#229408=CARTESIAN_POINT('Ctrl Pts',(-13.2815416545663,-19.9399848444019,
0.));
#229409=CARTESIAN_POINT('Ctrl Pts',(-13.2815416545663,-19.9399848444019,
12.));
#229410=CARTESIAN_POINT('Ctrl Pts',(-13.2764245494357,-19.9194875559422,
0.));
#229411=CARTESIAN_POINT('Ctrl Pts',(-13.2764245494357,-19.9194875559422,
12.));
#229412=CARTESIAN_POINT('Ctrl Pts',(-13.271278821502,-19.8991035111745,
0.));
#229413=CARTESIAN_POINT('Ctrl Pts',(-13.271278821502,-19.8991035111745,
12.));
#229414=CARTESIAN_POINT('Ctrl Pts',(-13.2661050556132,-19.8788333760577,
0.));
#229415=CARTESIAN_POINT('Ctrl Pts',(-13.2661050556132,-19.8788333760577,
12.));
#229416=CARTESIAN_POINT('Ctrl Pts',(-13.2609038446529,-19.8586778231715,
0.));
#229417=CARTESIAN_POINT('Ctrl Pts',(-13.2609038446529,-19.8586778231715,
12.));
#229418=CARTESIAN_POINT('Ctrl Pts',(-13.2556757897086,-19.8386375318634,
0.));
#229419=CARTESIAN_POINT('Ctrl Pts',(-13.2556757897086,-19.8386375318634,
12.));
#229420=CARTESIAN_POINT('Ctrl Pts',(-13.2504215002457,-19.8187131883917,
0.));
#229421=CARTESIAN_POINT('Ctrl Pts',(-13.2504215002457,-19.8187131883917,
12.));
#229422=CARTESIAN_POINT('Ctrl Pts',(-13.2451415942805,-19.7989054860495,
0.));
#229423=CARTESIAN_POINT('Ctrl Pts',(-13.2451415942805,-19.7989054860495,
12.));
#229424=CARTESIAN_POINT('Ctrl Pts',(-13.2398366985675,-19.7792151253289,
0.));
#229425=CARTESIAN_POINT('Ctrl Pts',(-13.2398366985675,-19.7792151253289,
12.));
#229426=CARTESIAN_POINT('Ctrl Pts',(-13.2345074487963,-19.7596428141168,
0.));
#229427=CARTESIAN_POINT('Ctrl Pts',(-13.2345074487963,-19.7596428141168,
12.));
#229428=CARTESIAN_POINT('Ctrl Pts',(-13.2291544897899,-19.7401892678697,
0.));
#229429=CARTESIAN_POINT('Ctrl Pts',(-13.2291544897899,-19.7401892678697,
12.));
#229430=CARTESIAN_POINT('Ctrl Pts',(-13.2237784757066,-19.7208552097868,
0.));
#229431=CARTESIAN_POINT('Ctrl Pts',(-13.2237784757066,-19.7208552097868,
12.));
#229432=CARTESIAN_POINT('Ctrl Pts',(-13.2183800702436,-19.7016413709685,
0.));
#229433=CARTESIAN_POINT('Ctrl Pts',(-13.2183800702436,-19.7016413709685,
12.));
#229434=CARTESIAN_POINT('Ctrl Pts',(-13.2129599468485,-19.6825484905823,
0.));
#229435=CARTESIAN_POINT('Ctrl Pts',(-13.2129599468485,-19.6825484905823,
12.));
#229436=CARTESIAN_POINT('Ctrl Pts',(-13.2075187889529,-19.6635773160936,
0.));
#229437=CARTESIAN_POINT('Ctrl Pts',(-13.2075187889529,-19.6635773160936,
12.));
#229438=CARTESIAN_POINT('Ctrl Pts',(-13.2020572902065,-19.6447286034772,
0.));
#229439=CARTESIAN_POINT('Ctrl Pts',(-13.2020572902065,-19.6447286034772,
12.));
#229440=CARTESIAN_POINT('Ctrl Pts',(-13.1965761547151,-19.6260031174244,
0.));
#229441=CARTESIAN_POINT('Ctrl Pts',(-13.1965761547151,-19.6260031174244,
12.));
#229442=CARTESIAN_POINT('Ctrl Pts',(-13.1910760972814,-19.6074016315414,
0.));
#229443=CARTESIAN_POINT('Ctrl Pts',(-13.1910760972814,-19.6074016315414,
12.));
#229444=CARTESIAN_POINT('Ctrl Pts',(-13.1855578436471,-19.5889249285338,
0.));
#229445=CARTESIAN_POINT('Ctrl Pts',(-13.1855578436471,-19.5889249285338,
12.));
#229446=CARTESIAN_POINT('Ctrl Pts',(-13.1800221307673,-19.5705738004667,
0.));
#229447=CARTESIAN_POINT('Ctrl Pts',(-13.1800221307673,-19.5705738004667,
12.));
#229448=CARTESIAN_POINT('Ctrl Pts',(-13.1744697070911,-19.5523490490244,
0.));
#229449=CARTESIAN_POINT('Ctrl Pts',(-13.1744697070911,-19.5523490490244,
12.));
#229450=CARTESIAN_POINT('Ctrl Pts',(-13.1689013328431,-19.5342514857562,
0.));
#229451=CARTESIAN_POINT('Ctrl Pts',(-13.1689013328431,-19.5342514857562,
12.));
#229452=CARTESIAN_POINT('Ctrl Pts',(-13.1633177803101,-19.5162819323213,
0.));
#229453=CARTESIAN_POINT('Ctrl Pts',(-13.1633177803101,-19.5162819323213,
12.));
#229454=CARTESIAN_POINT('Ctrl Pts',(-13.1577198341245,-19.4984412207081,
0.));
#229455=CARTESIAN_POINT('Ctrl Pts',(-13.1577198341245,-19.4984412207081,
12.));
#229456=CARTESIAN_POINT('Ctrl Pts',(-13.1521082915853,-19.4807301935268,
0.));
#229457=CARTESIAN_POINT('Ctrl Pts',(-13.1521082915853,-19.4807301935268,
12.));
#229458=CARTESIAN_POINT('Ctrl Pts',(-13.1464839629971,-19.4631497043258,
0.));
#229459=CARTESIAN_POINT('Ctrl Pts',(-13.1464839629971,-19.4631497043258,
12.));
#229460=CARTESIAN_POINT('Ctrl Pts',(-13.1408476720061,-19.4457006178876,
0.));
#229461=CARTESIAN_POINT('Ctrl Pts',(-13.1408476720061,-19.4457006178876,
12.));
#229462=CARTESIAN_POINT('Ctrl Pts',(-13.1352002559438,-19.4283838105262,
0.));
#229463=CARTESIAN_POINT('Ctrl Pts',(-13.1352002559438,-19.4283838105262,
12.));
#229464=CARTESIAN_POINT('Ctrl Pts',(-13.1295425661634,-19.4112001703557,
0.));
#229465=CARTESIAN_POINT('Ctrl Pts',(-13.1295425661634,-19.4112001703557,
12.));
#229466=CARTESIAN_POINT('Ctrl Pts',(-13.1238754684177,-19.3941505976263,
0.));
#229467=CARTESIAN_POINT('Ctrl Pts',(-13.1238754684177,-19.3941505976263,
12.));
#229468=CARTESIAN_POINT('Ctrl Pts',(-13.118199843271,-19.3772360051091,
0.));
#229469=CARTESIAN_POINT('Ctrl Pts',(-13.118199843271,-19.3772360051091,
12.));
#229470=CARTESIAN_POINT('Ctrl Pts',(-13.1125165865022,-19.3604573184515,
0.));
#229471=CARTESIAN_POINT('Ctrl Pts',(-13.1125165865022,-19.3604573184515,
12.));
#229472=CARTESIAN_POINT('Ctrl Pts',(-13.1068266095186,-19.3438154765395,
0.));
#229473=CARTESIAN_POINT('Ctrl Pts',(-13.1068266095186,-19.3438154765395,
12.));
#229474=CARTESIAN_POINT('Ctrl Pts',(-13.1011308397591,-19.3273114318269,
0.));
#229475=CARTESIAN_POINT('Ctrl Pts',(-13.1011308397591,-19.3273114318269,
12.));
#229476=CARTESIAN_POINT('Ctrl Pts',(-13.0954302211479,-19.310946150736,
0.));
#229477=CARTESIAN_POINT('Ctrl Pts',(-13.0954302211479,-19.310946150736,
12.));
#229478=CARTESIAN_POINT('Ctrl Pts',(-13.0897257145969,-19.2947206141247,
0.));
#229479=CARTESIAN_POINT('Ctrl Pts',(-13.0897257145969,-19.2947206141247,
12.));
#229480=CARTESIAN_POINT('Ctrl Pts',(-13.0840182984949,-19.2786358177198,
0.));
#229481=CARTESIAN_POINT('Ctrl Pts',(-13.0840182984949,-19.2786358177198,
12.));
#229482=CARTESIAN_POINT('Ctrl Pts',(-13.0783089692118,-19.2626927725596,
0.));
#229483=CARTESIAN_POINT('Ctrl Pts',(-13.0783089692118,-19.2626927725596,
12.));
#229484=CARTESIAN_POINT('Ctrl Pts',(-13.0725987415859,-19.2468925053989,
0.));
#229485=CARTESIAN_POINT('Ctrl Pts',(-13.0725987415859,-19.2468925053989,
12.));
#229486=CARTESIAN_POINT('Ctrl Pts',(-13.0668886494795,-19.2312360592033,
0.));
#229487=CARTESIAN_POINT('Ctrl Pts',(-13.0668886494795,-19.2312360592033,
12.));
#229488=CARTESIAN_POINT('Ctrl Pts',(-13.0611797463915,-19.2157244937142,
0.));
#229489=CARTESIAN_POINT('Ctrl Pts',(-13.0611797463915,-19.2157244937142,
12.));
#229490=CARTESIAN_POINT('Ctrl Pts',(-13.0554731060538,-19.2003588859772,
0.));
#229491=CARTESIAN_POINT('Ctrl Pts',(-13.0554731060538,-19.2003588859772,
12.));
#229492=CARTESIAN_POINT('Ctrl Pts',(-13.0497698230441,-19.1851403308825,
0.));
#229493=CARTESIAN_POINT('Ctrl Pts',(-13.0497698230441,-19.1851403308825,
12.));
#229494=CARTESIAN_POINT('Ctrl Pts',(-13.0440710133772,-19.1700699416622,
0.));
#229495=CARTESIAN_POINT('Ctrl Pts',(-13.0440710133772,-19.1700699416622,
12.));
#229496=CARTESIAN_POINT('Ctrl Pts',(-13.0383778152068,-19.155148850523,
0.));
#229497=CARTESIAN_POINT('Ctrl Pts',(-13.0383778152068,-19.155148850523,
12.));
#229498=CARTESIAN_POINT('Ctrl Pts',(-13.0326913895838,-19.1403782093386,
0.));
#229499=CARTESIAN_POINT('Ctrl Pts',(-13.0326913895838,-19.1403782093386,
12.));
#229500=CARTESIAN_POINT('Ctrl Pts',(-13.0270129211976,-19.1257591903099,
0.));
#229501=CARTESIAN_POINT('Ctrl Pts',(-13.0270129211976,-19.1257591903099,
12.));
#229502=CARTESIAN_POINT('Ctrl Pts',(-13.0213436191328,-19.111292986631,
0.));
#229503=CARTESIAN_POINT('Ctrl Pts',(-13.0213436191328,-19.111292986631,
12.));
#229504=CARTESIAN_POINT('Ctrl Pts',(-13.0156847176097,-19.0969808131228,
0.));
#229505=CARTESIAN_POINT('Ctrl Pts',(-13.0156847176097,-19.0969808131228,
12.));
#229506=CARTESIAN_POINT('Ctrl Pts',(-13.0100374768788,-19.0828239070484,
0.));
#229507=CARTESIAN_POINT('Ctrl Pts',(-13.0100374768788,-19.0828239070484,
12.));
#229508=CARTESIAN_POINT('Ctrl Pts',(-13.0044031841382,-19.0688235289437,
0.));
#229509=CARTESIAN_POINT('Ctrl Pts',(-13.0044031841382,-19.0688235289437,
12.));
#229510=CARTESIAN_POINT('Ctrl Pts',(-12.9987831544502,-19.0549809634354,
0.));
#229511=CARTESIAN_POINT('Ctrl Pts',(-12.9987831544502,-19.0549809634354,
12.));
#229512=CARTESIAN_POINT('Ctrl Pts',(-12.9931787316514,-19.0412975200398,
0.));
#229513=CARTESIAN_POINT('Ctrl Pts',(-12.9931787316514,-19.0412975200398,
12.));
#229514=CARTESIAN_POINT('Ctrl Pts',(-12.9875912893003,-19.0277745339908,
0.));
#229515=CARTESIAN_POINT('Ctrl Pts',(-12.9875912893003,-19.0277745339908,
12.));
#229516=CARTESIAN_POINT('Ctrl Pts',(-12.9820222318716,-19.014413367335,
0.));
#229517=CARTESIAN_POINT('Ctrl Pts',(-12.9820222318716,-19.014413367335,
12.));
#229518=CARTESIAN_POINT('Ctrl Pts',(-12.9764729959206,-19.0012154099792,
0.));
#229519=CARTESIAN_POINT('Ctrl Pts',(-12.9764729959206,-19.0012154099792,
12.));
#229520=CARTESIAN_POINT('Ctrl Pts',(-12.9709450512747,-18.9881820807585,
0.));
#229521=CARTESIAN_POINT('Ctrl Pts',(-12.9709450512747,-18.9881820807585,
12.));
#229522=CARTESIAN_POINT('Ctrl Pts',(-12.9654399021868,-18.9753148284473,
0.));
#229523=CARTESIAN_POINT('Ctrl Pts',(-12.9654399021868,-18.9753148284473,
12.));
#229524=CARTESIAN_POINT('Ctrl Pts',(-12.9599590886318,-18.9626151329226,
0.));
#229525=CARTESIAN_POINT('Ctrl Pts',(-12.9599590886318,-18.9626151329226,
12.));
#229526=CARTESIAN_POINT('Ctrl Pts',(-12.9545041877377,-18.9500845064714,
0.));
#229527=CARTESIAN_POINT('Ctrl Pts',(-12.9545041877377,-18.9500845064714,
12.));
#229528=CARTESIAN_POINT('Ctrl Pts',(-12.9490768151821,-18.9377244950435,
0.));
#229529=CARTESIAN_POINT('Ctrl Pts',(-12.9490768151821,-18.9377244950435,
12.));
#229530=CARTESIAN_POINT('Ctrl Pts',(-12.9436786266106,-18.9255366795196,
0.));
#229531=CARTESIAN_POINT('Ctrl Pts',(-12.9436786266106,-18.9255366795196,
12.));
#229532=CARTESIAN_POINT('Ctrl Pts',(-12.9383113190375,-18.9135226769466,
0.));
#229533=CARTESIAN_POINT('Ctrl Pts',(-12.9383113190375,-18.9135226769466,
12.));
#229534=CARTESIAN_POINT('Ctrl Pts',(-12.9329766328184,-18.9016841423402,
0.));
#229535=CARTESIAN_POINT('Ctrl Pts',(-12.9329766328184,-18.9016841423402,
12.));
#229536=CARTESIAN_POINT('Ctrl Pts',(-12.9276763536373,-18.8900227704888,
0.));
#229537=CARTESIAN_POINT('Ctrl Pts',(-12.9276763536373,-18.8900227704888,
12.));
#229538=CARTESIAN_POINT('Ctrl Pts',(-12.9224123144982,-18.8785402977528,
0.));
#229539=CARTESIAN_POINT('Ctrl Pts',(-12.9224123144982,-18.8785402977528,
12.));
#229540=CARTESIAN_POINT('Ctrl Pts',(-12.9171863977047,-18.8672385038328,
0.));
#229541=CARTESIAN_POINT('Ctrl Pts',(-12.9171863977047,-18.8672385038328,
12.));
#229542=CARTESIAN_POINT('Ctrl Pts',(-12.9120005369066,-18.8561192136201,
0.));
#229543=CARTESIAN_POINT('Ctrl Pts',(-12.9120005369066,-18.8561192136201,
12.));
#229544=CARTESIAN_POINT('Ctrl Pts',(-12.9068567191856,-18.8451842990986,
0.));
#229545=CARTESIAN_POINT('Ctrl Pts',(-12.9068567191856,-18.8451842990986,
12.));
#229546=CARTESIAN_POINT('Ctrl Pts',(-12.9017569871738,-18.834435681259,
0.));
#229547=CARTESIAN_POINT('Ctrl Pts',(-12.9017569871738,-18.834435681259,
12.));
#229548=CARTESIAN_POINT('Ctrl Pts',(-12.8967034410752,-18.8238753319124,
0.));
#229549=CARTESIAN_POINT('Ctrl Pts',(-12.8967034410752,-18.8238753319124,
12.));
#229550=CARTESIAN_POINT('Ctrl Pts',(-12.8916982409931,-18.8135052757815,
0.));
#229551=CARTESIAN_POINT('Ctrl Pts',(-12.8916982409931,-18.8135052757815,
12.));
#229552=CARTESIAN_POINT('Ctrl Pts',(-12.8867436109543,-18.8033275941939,
0.));
#229553=CARTESIAN_POINT('Ctrl Pts',(-12.8867436109543,-18.8033275941939,
12.));
#229554=CARTESIAN_POINT('Ctrl Pts',(-12.8818418427474,-18.7933444285867,
0.));
#229555=CARTESIAN_POINT('Ctrl Pts',(-12.8818418427474,-18.7933444285867,
12.));
#229556=CARTESIAN_POINT('Ctrl Pts',(-12.8769952998097,-18.7835579840481,
0.));
#229557=CARTESIAN_POINT('Ctrl Pts',(-12.8769952998097,-18.7835579840481,
12.));
#229558=CARTESIAN_POINT('Ctrl Pts',(-12.8722064211814,-18.7739705329028,
0.));
#229559=CARTESIAN_POINT('Ctrl Pts',(-12.8722064211814,-18.7739705329028,
12.));
#229560=CARTESIAN_POINT('Ctrl Pts',(-12.8674777239656,-18.7645844169568,
0.));
#229561=CARTESIAN_POINT('Ctrl Pts',(-12.8674777239656,-18.7645844169568,
12.));
#229562=CARTESIAN_POINT('Ctrl Pts',(-12.8628118054172,-18.7554020493888,
0.));
#229563=CARTESIAN_POINT('Ctrl Pts',(-12.8628118054172,-18.7554020493888,
12.));
#229564=CARTESIAN_POINT('Ctrl Pts',(-12.8582113455645,-18.7464259171248,
0.));
#229565=CARTESIAN_POINT('Ctrl Pts',(-12.8582113455645,-18.7464259171248,
12.));
#229566=CARTESIAN_POINT('Ctrl Pts',(-12.8536791086315,-18.7376585820851,
0.));
#229567=CARTESIAN_POINT('Ctrl Pts',(-12.8536791086315,-18.7376585820851,
12.));
#229568=CARTESIAN_POINT('Ctrl Pts',(-12.849217951159,-18.7291026886552,
0.));
#229569=CARTESIAN_POINT('Ctrl Pts',(-12.849217951159,-18.7291026886552,
12.));
#229570=CARTESIAN_POINT('Ctrl Pts',(-12.8448308329494,-18.7207609737701,
0.));
#229571=CARTESIAN_POINT('Ctrl Pts',(-12.8448308329494,-18.7207609737701,
12.));
#229572=CARTESIAN_POINT('Ctrl Pts',(-12.8405208263432,-18.7126362754446,
0.));
#229573=CARTESIAN_POINT('Ctrl Pts',(-12.8405208263432,-18.7126362754446,
12.));
#229574=CARTESIAN_POINT('Ctrl Pts',(-12.8362911280362,-18.7047315436296,
0.));
#229575=CARTESIAN_POINT('Ctrl Pts',(-12.8362911280362,-18.7047315436296,
12.));
#229576=CARTESIAN_POINT('Ctrl Pts',(-12.832145059979,-18.6970498410173,
0.));
#229577=CARTESIAN_POINT('Ctrl Pts',(-12.832145059979,-18.6970498410173,
12.));
#229578=CARTESIAN_POINT('Ctrl Pts',(-12.8280860635231,-18.6895943376172,
0.));
#229579=CARTESIAN_POINT('Ctrl Pts',(-12.8280860635231,-18.6895943376172,
12.));
#229580=CARTESIAN_POINT('Ctrl Pts',(-12.8241176980016,-18.6823683094138,
0.));
#229581=CARTESIAN_POINT('Ctrl Pts',(-12.8241176980016,-18.6823683094138,
12.));
#229582=CARTESIAN_POINT('Ctrl Pts',(-12.8202436318473,-18.6753751301091,
0.));
#229583=CARTESIAN_POINT('Ctrl Pts',(-12.8202436318473,-18.6753751301091,
12.));
#229584=CARTESIAN_POINT('Ctrl Pts',(-12.8164676687361,-18.6686182952798,
0.));
#229585=CARTESIAN_POINT('Ctrl Pts',(-12.8164676687361,-18.6686182952798,
12.));
#229586=CARTESIAN_POINT('Ctrl Pts',(-12.8127937909632,-18.6621014624746,
0.));
#229587=CARTESIAN_POINT('Ctrl Pts',(-12.8127937909632,-18.6621014624746,
12.));
#229588=CARTESIAN_POINT('Ctrl Pts',(-12.8092261933858,-18.6558284825772,
0.));
#229589=CARTESIAN_POINT('Ctrl Pts',(-12.8092261933858,-18.6558284825772,
12.));
#229590=CARTESIAN_POINT('Ctrl Pts',(-12.805769331162,-18.6498034438986,
0.));
#229591=CARTESIAN_POINT('Ctrl Pts',(-12.805769331162,-18.6498034438986,
12.));
#229592=CARTESIAN_POINT('Ctrl Pts',(-12.8024278770153,-18.6440306327457,
0.));
#229593=CARTESIAN_POINT('Ctrl Pts',(-12.8024278770153,-18.6440306327457,
12.));
#229594=CARTESIAN_POINT('Ctrl Pts',(-12.7992066625264,-18.63851447924,0.));
#229595=CARTESIAN_POINT('Ctrl Pts',(-12.7992066625264,-18.63851447924,12.));
#229596=CARTESIAN_POINT('Ctrl Pts',(-12.7961106222251,-18.6332595057005,
0.));
#229597=CARTESIAN_POINT('Ctrl Pts',(-12.7961106222251,-18.6332595057005,
12.));
#229598=CARTESIAN_POINT('Ctrl Pts',(-12.7931447451556,-18.6282702819371,
0.));
#229599=CARTESIAN_POINT('Ctrl Pts',(-12.7931447451556,-18.6282702819371,
12.));
#229600=CARTESIAN_POINT('Ctrl Pts',(-12.7903142925235,-18.6235516265575,
0.));
#229601=CARTESIAN_POINT('Ctrl Pts',(-12.7903142925235,-18.6235516265575,
12.));
#229602=CARTESIAN_POINT('Ctrl Pts',(-12.7876249657834,-18.6191087624752,
0.));
#229603=CARTESIAN_POINT('Ctrl Pts',(-12.7876249657834,-18.6191087624752,
12.));
#229604=CARTESIAN_POINT('Ctrl Pts',(-12.78508316579,-18.6149475565189,0.));
#229605=CARTESIAN_POINT('Ctrl Pts',(-12.78508316579,-18.6149475565189,12.));
#229606=CARTESIAN_POINT('Ctrl Pts',(-12.7826959526924,-18.611074482622,
0.));
#229607=CARTESIAN_POINT('Ctrl Pts',(-12.7826959526924,-18.611074482622,
12.));
#229608=CARTESIAN_POINT('Ctrl Pts',(-12.7804705387658,-18.6074961535723,
0.));
#229609=CARTESIAN_POINT('Ctrl Pts',(-12.7804705387658,-18.6074961535723,
12.));
#229610=CARTESIAN_POINT('Ctrl Pts',(-12.7784139605067,-18.6042190183703,
0.));
#229611=CARTESIAN_POINT('Ctrl Pts',(-12.7784139605067,-18.6042190183703,
12.));
#229612=CARTESIAN_POINT('Ctrl Pts',(-12.7765325225083,-18.6012488486708,
0.));
#229613=CARTESIAN_POINT('Ctrl Pts',(-12.7765325225083,-18.6012488486708,
12.));
#229614=CARTESIAN_POINT('Ctrl Pts',(-12.7748328937639,-18.5985917525949,
0.));
#229615=CARTESIAN_POINT('Ctrl Pts',(-12.7748328937639,-18.5985917525949,
12.));
#229616=CARTESIAN_POINT('Ctrl Pts',(-12.7733231262107,-18.5962551167772,
0.));
#229617=CARTESIAN_POINT('Ctrl Pts',(-12.7733231262107,-18.5962551167772,
12.));
#229618=CARTESIAN_POINT('Ctrl Pts',(-12.7720142287169,-18.5942490615409,
0.));
#229619=CARTESIAN_POINT('Ctrl Pts',(-12.7720142287169,-18.5942490615409,
12.));
#229620=CARTESIAN_POINT('Ctrl Pts',(-12.7709195951154,-18.5925859134582,
0.));
#229621=CARTESIAN_POINT('Ctrl Pts',(-12.7709195951154,-18.5925859134582,
12.));
#229622=CARTESIAN_POINT('Ctrl Pts',(-12.7700520897174,-18.5912775137806,
0.));
#229623=CARTESIAN_POINT('Ctrl Pts',(-12.7700520897174,-18.5912775137806,
12.));
#229624=CARTESIAN_POINT('Ctrl Pts',(-12.7694215127923,-18.590332877722,
0.));
#229625=CARTESIAN_POINT('Ctrl Pts',(-12.7694215127923,-18.590332877722,
12.));
#229626=CARTESIAN_POINT('Ctrl Pts',(-12.7691103481996,-18.589871621842,
0.));
#229627=CARTESIAN_POINT('Ctrl Pts',(-12.7691103481996,-18.589871621842,
12.));
#229628=CARTESIAN_POINT('Ctrl Pts',(-12.7689864266924,-18.5896919669158,
0.));
#229629=CARTESIAN_POINT('Ctrl Pts',(-12.7689864266924,-18.5896919669158,
12.));
#229630=CARTESIAN_POINT('Ctrl Pts',(-12.7689524524484,-18.5896460962961,
0.));
#229631=CARTESIAN_POINT('Ctrl Pts',(-12.7689524524484,-18.5896460962961,
12.));
#229632=CARTESIAN_POINT('Ctrl Pts',(-12.7689476255363,-18.5896416359912,
0.));
#229633=CARTESIAN_POINT('Ctrl Pts',(-12.7689476255363,-18.5896416359912,
12.));
#229634=CARTESIAN_POINT('',(-13.5685075571671,-22.1787195904339,0.));
#229635=CARTESIAN_POINT('Ctrl Pts',(-13.5685075571671,-22.1787195904339,
0.));
#229636=CARTESIAN_POINT('Ctrl Pts',(-13.5683460612913,-22.1730081264583,
0.));
#229637=CARTESIAN_POINT('Ctrl Pts',(-13.5680170531724,-22.1615922804939,
0.));
#229638=CARTESIAN_POINT('Ctrl Pts',(-13.5675054918922,-22.1444897575076,
0.));
#229639=CARTESIAN_POINT('Ctrl Pts',(-13.5667873105179,-22.1217288871823,
0.));
#229640=CARTESIAN_POINT('Ctrl Pts',(-13.5658294169107,-22.0933486464442,
0.));
#229641=CARTESIAN_POINT('Ctrl Pts',(-13.5648113688895,-22.0650393089492,
0.));
#229642=CARTESIAN_POINT('Ctrl Pts',(-13.5637332022393,-22.0368009736227,
0.));
#229643=CARTESIAN_POINT('Ctrl Pts',(-13.5625949868313,-22.0086337943431,
0.));
#229644=CARTESIAN_POINT('Ctrl Pts',(-13.5613968357589,-21.9805379899192,
0.));
#229645=CARTESIAN_POINT('Ctrl Pts',(-13.5601389185315,-21.9525138592862,
0.));
#229646=CARTESIAN_POINT('Ctrl Pts',(-13.5588214586672,-21.9245617765827,
0.));
#229647=CARTESIAN_POINT('Ctrl Pts',(-13.5574447178485,-21.8966821688876,
0.));
#229648=CARTESIAN_POINT('Ctrl Pts',(-13.5560089839426,-21.8688754989401,
0.));
#229649=CARTESIAN_POINT('Ctrl Pts',(-13.5545145573049,-21.841142245609,
0.));
#229650=CARTESIAN_POINT('Ctrl Pts',(-13.5529617381569,-21.8134828857963,
0.));
#229651=CARTESIAN_POINT('Ctrl Pts',(-13.5513508127232,-21.7858978745848,
0.));
#229652=CARTESIAN_POINT('Ctrl Pts',(-13.5496820422187,-21.7583876294532,
0.));
#229653=CARTESIAN_POINT('Ctrl Pts',(-13.5479556704457,-21.730952541226,
0.));
#229654=CARTESIAN_POINT('Ctrl Pts',(-13.546171929503,-21.7035929822939,
0.));
#229655=CARTESIAN_POINT('Ctrl Pts',(-13.5443310461516,-21.676309315769,
0.));
#229656=CARTESIAN_POINT('Ctrl Pts',(-13.5424332480698,-21.6491019044647,
0.));
#229657=CARTESIAN_POINT('Ctrl Pts',(-13.5404787697798,-21.6219711193951,
0.));
#229658=CARTESIAN_POINT('Ctrl Pts',(-13.5384678597206,-21.5949173499022,
0.));
#229659=CARTESIAN_POINT('Ctrl Pts',(-13.5364007790292,-21.5679410019011,
0.));
#229660=CARTESIAN_POINT('Ctrl Pts',(-13.5342777983225,-21.5410424932511,
0.));
#229661=CARTESIAN_POINT('Ctrl Pts',(-13.5320991952145,-21.5142222501671,
0.));
#229662=CARTESIAN_POINT('Ctrl Pts',(-13.5298652514357,-21.487480703047,
0.));
#229663=CARTESIAN_POINT('Ctrl Pts',(-13.5275762503553,-21.4608182828695,
0.));
#229664=CARTESIAN_POINT('Ctrl Pts',(-13.5252324737795,-21.4342354165253,
0.));
#229665=CARTESIAN_POINT('Ctrl Pts',(-13.5228342013508,-21.4077325259318,
0.));
#229666=CARTESIAN_POINT('Ctrl Pts',(-13.5203817122497,-21.3813100304967,
0.));
#229667=CARTESIAN_POINT('Ctrl Pts',(-13.5178752862461,-21.3549683486219,
0.));
#229668=CARTESIAN_POINT('Ctrl Pts',(-13.5153152050554,-21.328707899634,
0.));
#229669=CARTESIAN_POINT('Ctrl Pts',(-13.5127017534972,-21.3025291054236,
0.));
#229670=CARTESIAN_POINT('Ctrl Pts',(-13.5100352209207,-21.2764323924442,
0.));
#229671=CARTESIAN_POINT('Ctrl Pts',(-13.5073159019454,-21.2504181927429,
0.));
#229672=CARTESIAN_POINT('Ctrl Pts',(-13.5045440957404,-21.224486942933,
0.));
#229673=CARTESIAN_POINT('Ctrl Pts',(-13.5017201056088,-21.1986390835825,
0.));
#229674=CARTESIAN_POINT('Ctrl Pts',(-13.4988442384491,-21.1728750584173,
0.));
#229675=CARTESIAN_POINT('Ctrl Pts',(-13.4959168042934,-21.1471953136209,
0.));
#229676=CARTESIAN_POINT('Ctrl Pts',(-13.4929381157778,-21.1216002970209,
0.));
#229677=CARTESIAN_POINT('Ctrl Pts',(-13.4899084877718,-21.0960904575048,
0.));
#229678=CARTESIAN_POINT('Ctrl Pts',(-13.4868282377192,-21.0706662455202,
0.));
#229679=CARTESIAN_POINT('Ctrl Pts',(-13.4836976858912,-21.0453281134247,
0.));
#229680=CARTESIAN_POINT('Ctrl Pts',(-13.4805171556822,-21.0200765158885,
0.));
#229681=CARTESIAN_POINT('Ctrl Pts',(-13.4772869738879,-20.9949119102592,
0.));
#229682=CARTESIAN_POINT('Ctrl Pts',(-13.4740074710087,-20.9698347569476,
0.));
#229683=CARTESIAN_POINT('Ctrl Pts',(-13.4706789815167,-20.9448455197557,
0.));
#229684=CARTESIAN_POINT('Ctrl Pts',(-13.4673018437718,-20.9199446657584,
0.));
#229685=CARTESIAN_POINT('Ctrl Pts',(-13.4638763999726,-20.8951326652158,
0.));
#229686=CARTESIAN_POINT('Ctrl Pts',(-13.4604029960983,-20.8704099914641,
0.));
#229687=CARTESIAN_POINT('Ctrl Pts',(-13.4568819818631,-20.8457771208082,
0.));
#229688=CARTESIAN_POINT('Ctrl Pts',(-13.4533137106667,-20.821234532398,
0.));
#229689=CARTESIAN_POINT('Ctrl Pts',(-13.4496985395637,-20.7967827081227,
0.));
#229690=CARTESIAN_POINT('Ctrl Pts',(-13.4460368293688,-20.7724221327608,
0.));
#229691=CARTESIAN_POINT('Ctrl Pts',(-13.4423289447561,-20.7481532941013,
0.));
#229692=CARTESIAN_POINT('Ctrl Pts',(-13.4385752543663,-20.7239766830675,
0.));
#229693=CARTESIAN_POINT('Ctrl Pts',(-13.4347761309154,-20.6998927938288,
0.));
#229694=CARTESIAN_POINT('Ctrl Pts',(-13.4309319513119,-20.6759021239103,
0.));
#229695=CARTESIAN_POINT('Ctrl Pts',(-13.4270430967652,-20.6520051742869,
0.));
#229696=CARTESIAN_POINT('Ctrl Pts',(-13.4231099528179,-20.6282024494237,
0.));
#229697=CARTESIAN_POINT('Ctrl Pts',(-13.4191329093933,-20.6044944573153,
0.));
#229698=CARTESIAN_POINT('Ctrl Pts',(-13.4151123608411,-20.5808817095155,
0.));
#229699=CARTESIAN_POINT('Ctrl Pts',(-13.4110487059912,-20.5573647211639,
0.));
#229700=CARTESIAN_POINT('Ctrl Pts',(-13.4069423482076,-20.5339440109956,
0.));
#229701=CARTESIAN_POINT('Ctrl Pts',(-13.4027936954529,-20.5106201013753,
0.));
#229702=CARTESIAN_POINT('Ctrl Pts',(-13.3986031603716,-20.487393518404,
0.));
#229703=CARTESIAN_POINT('Ctrl Pts',(-13.3943711603739,-20.4642647920037,
0.));
#229704=CARTESIAN_POINT('Ctrl Pts',(-13.3900981177255,-20.4412344560007,
0.));
#229705=CARTESIAN_POINT('Ctrl Pts',(-13.3857844596387,-20.4183030482002,
0.));
#229706=CARTESIAN_POINT('Ctrl Pts',(-13.3814306183719,-20.3954711104502,
0.));
#229707=CARTESIAN_POINT('Ctrl Pts',(-13.3770370313188,-20.3727391887184,
0.));
#229708=CARTESIAN_POINT('Ctrl Pts',(-13.3726041410867,-20.3501078331814,
0.));
#229709=CARTESIAN_POINT('Ctrl Pts',(-13.3681323955826,-20.3275775983029,
0.));
#229710=CARTESIAN_POINT('Ctrl Pts',(-13.3636222481016,-20.3051490429048,
0.));
#229711=CARTESIAN_POINT('Ctrl Pts',(-13.3590741574195,-20.2828227302339,
0.));
#229712=CARTESIAN_POINT('Ctrl Pts',(-13.3544885878889,-20.2605992280122,
0.));
#229713=CARTESIAN_POINT('Ctrl Pts',(-13.3498660095386,-20.2384791085359,
0.));
#229714=CARTESIAN_POINT('Ctrl Pts',(-13.3452068981766,-20.216462948786,
0.));
#229715=CARTESIAN_POINT('Ctrl Pts',(-13.3405117354971,-20.1945513305235,
0.));
#229716=CARTESIAN_POINT('Ctrl Pts',(-13.3357810091903,-20.1727448403817,
0.));
#229717=CARTESIAN_POINT('Ctrl Pts',(-13.3310152130564,-20.1510440699474,
0.));
#229718=CARTESIAN_POINT('Ctrl Pts',(-13.3262148471226,-20.1294496158402,
0.));
#229719=CARTESIAN_POINT('Ctrl Pts',(-13.3213804177587,-20.1079620798375,
0.));
#229720=CARTESIAN_POINT('Ctrl Pts',(-13.3165124377963,-20.0865820689882,
0.));
#229721=CARTESIAN_POINT('Ctrl Pts',(-13.3116114266515,-20.0653101957188,
0.));
#229722=CARTESIAN_POINT('Ctrl Pts',(-13.3066779104515,-20.0441470779345,
0.));
#229723=CARTESIAN_POINT('Ctrl Pts',(-13.3017124221637,-20.0230933391038,
0.));
#229724=CARTESIAN_POINT('Ctrl Pts',(-13.2967155017306,-20.0021496083738,
0.));
#229725=CARTESIAN_POINT('Ctrl Pts',(-13.2916876962094,-19.981316520717,
0.));
#229726=CARTESIAN_POINT('Ctrl Pts',(-13.286629559915,-19.9605947170586,
0.));
#229727=CARTESIAN_POINT('Ctrl Pts',(-13.2815416545663,-19.9399848444019,
0.));
#229728=CARTESIAN_POINT('Ctrl Pts',(-13.2764245494357,-19.9194875559422,
0.));
#229729=CARTESIAN_POINT('Ctrl Pts',(-13.271278821502,-19.8991035111745,
0.));
#229730=CARTESIAN_POINT('Ctrl Pts',(-13.2661050556132,-19.8788333760577,
0.));
#229731=CARTESIAN_POINT('Ctrl Pts',(-13.2609038446529,-19.8586778231715,
0.));
#229732=CARTESIAN_POINT('Ctrl Pts',(-13.2556757897086,-19.8386375318634,
0.));
#229733=CARTESIAN_POINT('Ctrl Pts',(-13.2504215002457,-19.8187131883917,
0.));
#229734=CARTESIAN_POINT('Ctrl Pts',(-13.2451415942805,-19.7989054860495,
0.));
#229735=CARTESIAN_POINT('Ctrl Pts',(-13.2398366985675,-19.7792151253289,
0.));
#229736=CARTESIAN_POINT('Ctrl Pts',(-13.2345074487963,-19.7596428141168,
0.));
#229737=CARTESIAN_POINT('Ctrl Pts',(-13.2291544897899,-19.7401892678697,
0.));
#229738=CARTESIAN_POINT('Ctrl Pts',(-13.2237784757066,-19.7208552097868,
0.));
#229739=CARTESIAN_POINT('Ctrl Pts',(-13.2183800702436,-19.7016413709685,
0.));
#229740=CARTESIAN_POINT('Ctrl Pts',(-13.2129599468485,-19.6825484905823,
0.));
#229741=CARTESIAN_POINT('Ctrl Pts',(-13.2075187889529,-19.6635773160936,
0.));
#229742=CARTESIAN_POINT('Ctrl Pts',(-13.2020572902065,-19.6447286034772,
0.));
#229743=CARTESIAN_POINT('Ctrl Pts',(-13.1965761547151,-19.6260031174244,
0.));
#229744=CARTESIAN_POINT('Ctrl Pts',(-13.1910760972814,-19.6074016315414,
0.));
#229745=CARTESIAN_POINT('Ctrl Pts',(-13.1855578436471,-19.5889249285338,
0.));
#229746=CARTESIAN_POINT('Ctrl Pts',(-13.1800221307673,-19.5705738004667,
0.));
#229747=CARTESIAN_POINT('Ctrl Pts',(-13.1744697070911,-19.5523490490244,
0.));
#229748=CARTESIAN_POINT('Ctrl Pts',(-13.1689013328431,-19.5342514857562,
0.));
#229749=CARTESIAN_POINT('Ctrl Pts',(-13.1633177803101,-19.5162819323213,
0.));
#229750=CARTESIAN_POINT('Ctrl Pts',(-13.1577198341245,-19.4984412207081,
0.));
#229751=CARTESIAN_POINT('Ctrl Pts',(-13.1521082915853,-19.4807301935268,
0.));
#229752=CARTESIAN_POINT('Ctrl Pts',(-13.1464839629971,-19.4631497043258,
0.));
#229753=CARTESIAN_POINT('Ctrl Pts',(-13.1408476720061,-19.4457006178876,
0.));
#229754=CARTESIAN_POINT('Ctrl Pts',(-13.1352002559438,-19.4283838105262,
0.));
#229755=CARTESIAN_POINT('Ctrl Pts',(-13.1295425661634,-19.4112001703557,
0.));
#229756=CARTESIAN_POINT('Ctrl Pts',(-13.1238754684177,-19.3941505976263,
0.));
#229757=CARTESIAN_POINT('Ctrl Pts',(-13.118199843271,-19.3772360051091,
0.));
#229758=CARTESIAN_POINT('Ctrl Pts',(-13.1125165865022,-19.3604573184515,
0.));
#229759=CARTESIAN_POINT('Ctrl Pts',(-13.1068266095186,-19.3438154765395,
0.));
#229760=CARTESIAN_POINT('Ctrl Pts',(-13.1011308397591,-19.3273114318269,
0.));
#229761=CARTESIAN_POINT('Ctrl Pts',(-13.0954302211479,-19.310946150736,
0.));
#229762=CARTESIAN_POINT('Ctrl Pts',(-13.0897257145969,-19.2947206141247,
0.));
#229763=CARTESIAN_POINT('Ctrl Pts',(-13.0840182984949,-19.2786358177198,
0.));
#229764=CARTESIAN_POINT('Ctrl Pts',(-13.0783089692118,-19.2626927725596,
0.));
#229765=CARTESIAN_POINT('Ctrl Pts',(-13.0725987415859,-19.2468925053989,
0.));
#229766=CARTESIAN_POINT('Ctrl Pts',(-13.0668886494795,-19.2312360592033,
0.));
#229767=CARTESIAN_POINT('Ctrl Pts',(-13.0611797463915,-19.2157244937142,
0.));
#229768=CARTESIAN_POINT('Ctrl Pts',(-13.0554731060538,-19.2003588859772,
0.));
#229769=CARTESIAN_POINT('Ctrl Pts',(-13.0497698230441,-19.1851403308825,
0.));
#229770=CARTESIAN_POINT('Ctrl Pts',(-13.0440710133772,-19.1700699416622,
0.));
#229771=CARTESIAN_POINT('Ctrl Pts',(-13.0383778152068,-19.155148850523,
0.));
#229772=CARTESIAN_POINT('Ctrl Pts',(-13.0326913895838,-19.1403782093386,
0.));
#229773=CARTESIAN_POINT('Ctrl Pts',(-13.0270129211976,-19.1257591903099,
0.));
#229774=CARTESIAN_POINT('Ctrl Pts',(-13.0213436191328,-19.111292986631,
0.));
#229775=CARTESIAN_POINT('Ctrl Pts',(-13.0156847176097,-19.0969808131228,
0.));
#229776=CARTESIAN_POINT('Ctrl Pts',(-13.0100374768788,-19.0828239070484,
0.));
#229777=CARTESIAN_POINT('Ctrl Pts',(-13.0044031841382,-19.0688235289437,
0.));
#229778=CARTESIAN_POINT('Ctrl Pts',(-12.9987831544502,-19.0549809634354,
0.));
#229779=CARTESIAN_POINT('Ctrl Pts',(-12.9931787316514,-19.0412975200398,
0.));
#229780=CARTESIAN_POINT('Ctrl Pts',(-12.9875912893003,-19.0277745339908,
0.));
#229781=CARTESIAN_POINT('Ctrl Pts',(-12.9820222318716,-19.014413367335,
0.));
#229782=CARTESIAN_POINT('Ctrl Pts',(-12.9764729959206,-19.0012154099792,
0.));
#229783=CARTESIAN_POINT('Ctrl Pts',(-12.9709450512747,-18.9881820807585,
0.));
#229784=CARTESIAN_POINT('Ctrl Pts',(-12.9654399021868,-18.9753148284473,
0.));
#229785=CARTESIAN_POINT('Ctrl Pts',(-12.9599590886318,-18.9626151329226,
0.));
#229786=CARTESIAN_POINT('Ctrl Pts',(-12.9545041877377,-18.9500845064714,
0.));
#229787=CARTESIAN_POINT('Ctrl Pts',(-12.9490768151821,-18.9377244950435,
0.));
#229788=CARTESIAN_POINT('Ctrl Pts',(-12.9436786266106,-18.9255366795196,
0.));
#229789=CARTESIAN_POINT('Ctrl Pts',(-12.9383113190375,-18.9135226769466,
0.));
#229790=CARTESIAN_POINT('Ctrl Pts',(-12.9329766328184,-18.9016841423402,
0.));
#229791=CARTESIAN_POINT('Ctrl Pts',(-12.9276763536373,-18.8900227704888,
0.));
#229792=CARTESIAN_POINT('Ctrl Pts',(-12.9224123144982,-18.8785402977528,
0.));
#229793=CARTESIAN_POINT('Ctrl Pts',(-12.9171863977047,-18.8672385038328,
0.));
#229794=CARTESIAN_POINT('Ctrl Pts',(-12.9120005369066,-18.8561192136201,
0.));
#229795=CARTESIAN_POINT('Ctrl Pts',(-12.9068567191856,-18.8451842990986,
0.));
#229796=CARTESIAN_POINT('Ctrl Pts',(-12.9017569871738,-18.834435681259,
0.));
#229797=CARTESIAN_POINT('Ctrl Pts',(-12.8967034410752,-18.8238753319124,
0.));
#229798=CARTESIAN_POINT('Ctrl Pts',(-12.8916982409931,-18.8135052757815,
0.));
#229799=CARTESIAN_POINT('Ctrl Pts',(-12.8867436109543,-18.8033275941939,
0.));
#229800=CARTESIAN_POINT('Ctrl Pts',(-12.8818418427474,-18.7933444285867,
0.));
#229801=CARTESIAN_POINT('Ctrl Pts',(-12.8769952998097,-18.7835579840481,
0.));
#229802=CARTESIAN_POINT('Ctrl Pts',(-12.8722064211814,-18.7739705329028,
0.));
#229803=CARTESIAN_POINT('Ctrl Pts',(-12.8674777239656,-18.7645844169568,
0.));
#229804=CARTESIAN_POINT('Ctrl Pts',(-12.8628118054172,-18.7554020493888,
0.));
#229805=CARTESIAN_POINT('Ctrl Pts',(-12.8582113455645,-18.7464259171248,
0.));
#229806=CARTESIAN_POINT('Ctrl Pts',(-12.8536791086315,-18.7376585820851,
0.));
#229807=CARTESIAN_POINT('Ctrl Pts',(-12.849217951159,-18.7291026886552,
0.));
#229808=CARTESIAN_POINT('Ctrl Pts',(-12.8448308329494,-18.7207609737701,
0.));
#229809=CARTESIAN_POINT('Ctrl Pts',(-12.8405208263432,-18.7126362754446,
0.));
#229810=CARTESIAN_POINT('Ctrl Pts',(-12.8362911280362,-18.7047315436296,
0.));
#229811=CARTESIAN_POINT('Ctrl Pts',(-12.832145059979,-18.6970498410173,
0.));
#229812=CARTESIAN_POINT('Ctrl Pts',(-12.8280860635231,-18.6895943376172,
0.));
#229813=CARTESIAN_POINT('Ctrl Pts',(-12.8241176980016,-18.6823683094138,
0.));
#229814=CARTESIAN_POINT('Ctrl Pts',(-12.8202436318473,-18.6753751301091,
0.));
#229815=CARTESIAN_POINT('Ctrl Pts',(-12.8164676687361,-18.6686182952798,
0.));
#229816=CARTESIAN_POINT('Ctrl Pts',(-12.8127937909632,-18.6621014624746,
0.));
#229817=CARTESIAN_POINT('Ctrl Pts',(-12.8092261933858,-18.6558284825772,
0.));
#229818=CARTESIAN_POINT('Ctrl Pts',(-12.805769331162,-18.6498034438986,
0.));
#229819=CARTESIAN_POINT('Ctrl Pts',(-12.8024278770153,-18.6440306327457,
0.));
#229820=CARTESIAN_POINT('Ctrl Pts',(-12.7992066625264,-18.63851447924,0.));
#229821=CARTESIAN_POINT('Ctrl Pts',(-12.7961106222251,-18.6332595057005,
0.));
#229822=CARTESIAN_POINT('Ctrl Pts',(-12.7931447451556,-18.6282702819371,
0.));
#229823=CARTESIAN_POINT('Ctrl Pts',(-12.7903142925235,-18.6235516265575,
0.));
#229824=CARTESIAN_POINT('Ctrl Pts',(-12.7876249657834,-18.6191087624752,
0.));
#229825=CARTESIAN_POINT('Ctrl Pts',(-12.78508316579,-18.6149475565189,0.));
#229826=CARTESIAN_POINT('Ctrl Pts',(-12.7826959526924,-18.611074482622,
0.));
#229827=CARTESIAN_POINT('Ctrl Pts',(-12.7804705387658,-18.6074961535723,
0.));
#229828=CARTESIAN_POINT('Ctrl Pts',(-12.7784139605067,-18.6042190183703,
0.));
#229829=CARTESIAN_POINT('Ctrl Pts',(-12.7765325225083,-18.6012488486708,
0.));
#229830=CARTESIAN_POINT('Ctrl Pts',(-12.7748328937639,-18.5985917525949,
0.));
#229831=CARTESIAN_POINT('Ctrl Pts',(-12.7733231262107,-18.5962551167772,
0.));
#229832=CARTESIAN_POINT('Ctrl Pts',(-12.7720142287169,-18.5942490615409,
0.));
#229833=CARTESIAN_POINT('Ctrl Pts',(-12.7709195951154,-18.5925859134582,
0.));
#229834=CARTESIAN_POINT('Ctrl Pts',(-12.7700520897174,-18.5912775137806,
0.));
#229835=CARTESIAN_POINT('Ctrl Pts',(-12.7694215127923,-18.590332877722,
0.));
#229836=CARTESIAN_POINT('Ctrl Pts',(-12.7691103481996,-18.589871621842,
0.));
#229837=CARTESIAN_POINT('Ctrl Pts',(-12.7689864266924,-18.5896919669158,
0.));
#229838=CARTESIAN_POINT('Ctrl Pts',(-12.7689524524484,-18.5896460962961,
0.));
#229839=CARTESIAN_POINT('Ctrl Pts',(-12.7689476255363,-18.5896416359912,
0.));
#229840=CARTESIAN_POINT('',(-13.5685075571671,-22.1787195904339,12.));
#229841=CARTESIAN_POINT('',(-13.5685075571671,-22.1787195904339,0.));
#229842=CARTESIAN_POINT('Ctrl Pts',(-12.7689476255363,-18.5896416359912,
12.));
#229843=CARTESIAN_POINT('Ctrl Pts',(-12.7689524524484,-18.5896460962961,
12.));
#229844=CARTESIAN_POINT('Ctrl Pts',(-12.7689864266924,-18.5896919669158,
12.));
#229845=CARTESIAN_POINT('Ctrl Pts',(-12.7691103481996,-18.589871621842,
12.));
#229846=CARTESIAN_POINT('Ctrl Pts',(-12.7694215127923,-18.590332877722,
12.));
#229847=CARTESIAN_POINT('Ctrl Pts',(-12.7700520897174,-18.5912775137806,
12.));
#229848=CARTESIAN_POINT('Ctrl Pts',(-12.7709195951154,-18.5925859134582,
12.));
#229849=CARTESIAN_POINT('Ctrl Pts',(-12.7720142287169,-18.5942490615409,
12.));
#229850=CARTESIAN_POINT('Ctrl Pts',(-12.7733231262107,-18.5962551167772,
12.));
#229851=CARTESIAN_POINT('Ctrl Pts',(-12.7748328937639,-18.5985917525949,
12.));
#229852=CARTESIAN_POINT('Ctrl Pts',(-12.7765325225083,-18.6012488486708,
12.));
#229853=CARTESIAN_POINT('Ctrl Pts',(-12.7784139605067,-18.6042190183703,
12.));
#229854=CARTESIAN_POINT('Ctrl Pts',(-12.7804705387658,-18.6074961535723,
12.));
#229855=CARTESIAN_POINT('Ctrl Pts',(-12.7826959526924,-18.611074482622,
12.));
#229856=CARTESIAN_POINT('Ctrl Pts',(-12.78508316579,-18.6149475565189,12.));
#229857=CARTESIAN_POINT('Ctrl Pts',(-12.7876249657834,-18.6191087624752,
12.));
#229858=CARTESIAN_POINT('Ctrl Pts',(-12.7903142925235,-18.6235516265575,
12.));
#229859=CARTESIAN_POINT('Ctrl Pts',(-12.7931447451556,-18.6282702819371,
12.));
#229860=CARTESIAN_POINT('Ctrl Pts',(-12.7961106222251,-18.6332595057005,
12.));
#229861=CARTESIAN_POINT('Ctrl Pts',(-12.7992066625264,-18.63851447924,12.));
#229862=CARTESIAN_POINT('Ctrl Pts',(-12.8024278770153,-18.6440306327457,
12.));
#229863=CARTESIAN_POINT('Ctrl Pts',(-12.805769331162,-18.6498034438986,
12.));
#229864=CARTESIAN_POINT('Ctrl Pts',(-12.8092261933858,-18.6558284825772,
12.));
#229865=CARTESIAN_POINT('Ctrl Pts',(-12.8127937909632,-18.6621014624746,
12.));
#229866=CARTESIAN_POINT('Ctrl Pts',(-12.8164676687361,-18.6686182952798,
12.));
#229867=CARTESIAN_POINT('Ctrl Pts',(-12.8202436318473,-18.6753751301091,
12.));
#229868=CARTESIAN_POINT('Ctrl Pts',(-12.8241176980016,-18.6823683094138,
12.));
#229869=CARTESIAN_POINT('Ctrl Pts',(-12.8280860635231,-18.6895943376172,
12.));
#229870=CARTESIAN_POINT('Ctrl Pts',(-12.832145059979,-18.6970498410173,
12.));
#229871=CARTESIAN_POINT('Ctrl Pts',(-12.8362911280362,-18.7047315436296,
12.));
#229872=CARTESIAN_POINT('Ctrl Pts',(-12.8405208263432,-18.7126362754446,
12.));
#229873=CARTESIAN_POINT('Ctrl Pts',(-12.8448308329494,-18.7207609737701,
12.));
#229874=CARTESIAN_POINT('Ctrl Pts',(-12.849217951159,-18.7291026886552,
12.));
#229875=CARTESIAN_POINT('Ctrl Pts',(-12.8536791086315,-18.7376585820851,
12.));
#229876=CARTESIAN_POINT('Ctrl Pts',(-12.8582113455645,-18.7464259171248,
12.));
#229877=CARTESIAN_POINT('Ctrl Pts',(-12.8628118054172,-18.7554020493888,
12.));
#229878=CARTESIAN_POINT('Ctrl Pts',(-12.8674777239656,-18.7645844169568,
12.));
#229879=CARTESIAN_POINT('Ctrl Pts',(-12.8722064211814,-18.7739705329028,
12.));
#229880=CARTESIAN_POINT('Ctrl Pts',(-12.8769952998097,-18.7835579840481,
12.));
#229881=CARTESIAN_POINT('Ctrl Pts',(-12.8818418427474,-18.7933444285867,
12.));
#229882=CARTESIAN_POINT('Ctrl Pts',(-12.8867436109543,-18.8033275941939,
12.));
#229883=CARTESIAN_POINT('Ctrl Pts',(-12.8916982409931,-18.8135052757815,
12.));
#229884=CARTESIAN_POINT('Ctrl Pts',(-12.8967034410752,-18.8238753319124,
12.));
#229885=CARTESIAN_POINT('Ctrl Pts',(-12.9017569871738,-18.834435681259,
12.));
#229886=CARTESIAN_POINT('Ctrl Pts',(-12.9068567191856,-18.8451842990986,
12.));
#229887=CARTESIAN_POINT('Ctrl Pts',(-12.9120005369066,-18.8561192136201,
12.));
#229888=CARTESIAN_POINT('Ctrl Pts',(-12.9171863977047,-18.8672385038328,
12.));
#229889=CARTESIAN_POINT('Ctrl Pts',(-12.9224123144982,-18.8785402977528,
12.));
#229890=CARTESIAN_POINT('Ctrl Pts',(-12.9276763536373,-18.8900227704888,
12.));
#229891=CARTESIAN_POINT('Ctrl Pts',(-12.9329766328184,-18.9016841423402,
12.));
#229892=CARTESIAN_POINT('Ctrl Pts',(-12.9383113190375,-18.9135226769466,
12.));
#229893=CARTESIAN_POINT('Ctrl Pts',(-12.9436786266106,-18.9255366795196,
12.));
#229894=CARTESIAN_POINT('Ctrl Pts',(-12.9490768151821,-18.9377244950435,
12.));
#229895=CARTESIAN_POINT('Ctrl Pts',(-12.9545041877377,-18.9500845064714,
12.));
#229896=CARTESIAN_POINT('Ctrl Pts',(-12.9599590886318,-18.9626151329226,
12.));
#229897=CARTESIAN_POINT('Ctrl Pts',(-12.9654399021868,-18.9753148284473,
12.));
#229898=CARTESIAN_POINT('Ctrl Pts',(-12.9709450512747,-18.9881820807585,
12.));
#229899=CARTESIAN_POINT('Ctrl Pts',(-12.9764729959206,-19.0012154099792,
12.));
#229900=CARTESIAN_POINT('Ctrl Pts',(-12.9820222318716,-19.014413367335,
12.));
#229901=CARTESIAN_POINT('Ctrl Pts',(-12.9875912893003,-19.0277745339908,
12.));
#229902=CARTESIAN_POINT('Ctrl Pts',(-12.9931787316514,-19.0412975200398,
12.));
#229903=CARTESIAN_POINT('Ctrl Pts',(-12.9987831544502,-19.0549809634354,
12.));
#229904=CARTESIAN_POINT('Ctrl Pts',(-13.0044031841382,-19.0688235289437,
12.));
#229905=CARTESIAN_POINT('Ctrl Pts',(-13.0100374768788,-19.0828239070484,
12.));
#229906=CARTESIAN_POINT('Ctrl Pts',(-13.0156847176097,-19.0969808131228,
12.));
#229907=CARTESIAN_POINT('Ctrl Pts',(-13.0213436191328,-19.111292986631,
12.));
#229908=CARTESIAN_POINT('Ctrl Pts',(-13.0270129211976,-19.1257591903099,
12.));
#229909=CARTESIAN_POINT('Ctrl Pts',(-13.0326913895838,-19.1403782093386,
12.));
#229910=CARTESIAN_POINT('Ctrl Pts',(-13.0383778152068,-19.155148850523,
12.));
#229911=CARTESIAN_POINT('Ctrl Pts',(-13.0440710133772,-19.1700699416622,
12.));
#229912=CARTESIAN_POINT('Ctrl Pts',(-13.0497698230441,-19.1851403308825,
12.));
#229913=CARTESIAN_POINT('Ctrl Pts',(-13.0554731060538,-19.2003588859772,
12.));
#229914=CARTESIAN_POINT('Ctrl Pts',(-13.0611797463915,-19.2157244937142,
12.));
#229915=CARTESIAN_POINT('Ctrl Pts',(-13.0668886494795,-19.2312360592033,
12.));
#229916=CARTESIAN_POINT('Ctrl Pts',(-13.0725987415859,-19.2468925053989,
12.));
#229917=CARTESIAN_POINT('Ctrl Pts',(-13.0783089692118,-19.2626927725596,
12.));
#229918=CARTESIAN_POINT('Ctrl Pts',(-13.0840182984949,-19.2786358177198,
12.));
#229919=CARTESIAN_POINT('Ctrl Pts',(-13.0897257145969,-19.2947206141247,
12.));
#229920=CARTESIAN_POINT('Ctrl Pts',(-13.0954302211479,-19.310946150736,
12.));
#229921=CARTESIAN_POINT('Ctrl Pts',(-13.1011308397591,-19.3273114318269,
12.));
#229922=CARTESIAN_POINT('Ctrl Pts',(-13.1068266095186,-19.3438154765395,
12.));
#229923=CARTESIAN_POINT('Ctrl Pts',(-13.1125165865022,-19.3604573184515,
12.));
#229924=CARTESIAN_POINT('Ctrl Pts',(-13.118199843271,-19.3772360051091,
12.));
#229925=CARTESIAN_POINT('Ctrl Pts',(-13.1238754684177,-19.3941505976263,
12.));
#229926=CARTESIAN_POINT('Ctrl Pts',(-13.1295425661634,-19.4112001703557,
12.));
#229927=CARTESIAN_POINT('Ctrl Pts',(-13.1352002559438,-19.4283838105262,
12.));
#229928=CARTESIAN_POINT('Ctrl Pts',(-13.1408476720061,-19.4457006178876,
12.));
#229929=CARTESIAN_POINT('Ctrl Pts',(-13.1464839629971,-19.4631497043258,
12.));
#229930=CARTESIAN_POINT('Ctrl Pts',(-13.1521082915853,-19.4807301935268,
12.));
#229931=CARTESIAN_POINT('Ctrl Pts',(-13.1577198341245,-19.4984412207081,
12.));
#229932=CARTESIAN_POINT('Ctrl Pts',(-13.1633177803101,-19.5162819323213,
12.));
#229933=CARTESIAN_POINT('Ctrl Pts',(-13.1689013328431,-19.5342514857562,
12.));
#229934=CARTESIAN_POINT('Ctrl Pts',(-13.1744697070911,-19.5523490490244,
12.));
#229935=CARTESIAN_POINT('Ctrl Pts',(-13.1800221307673,-19.5705738004667,
12.));
#229936=CARTESIAN_POINT('Ctrl Pts',(-13.1855578436471,-19.5889249285338,
12.));
#229937=CARTESIAN_POINT('Ctrl Pts',(-13.1910760972814,-19.6074016315414,
12.));
#229938=CARTESIAN_POINT('Ctrl Pts',(-13.1965761547151,-19.6260031174244,
12.));
#229939=CARTESIAN_POINT('Ctrl Pts',(-13.2020572902065,-19.6447286034772,
12.));
#229940=CARTESIAN_POINT('Ctrl Pts',(-13.2075187889529,-19.6635773160936,
12.));
#229941=CARTESIAN_POINT('Ctrl Pts',(-13.2129599468485,-19.6825484905823,
12.));
#229942=CARTESIAN_POINT('Ctrl Pts',(-13.2183800702436,-19.7016413709685,
12.));
#229943=CARTESIAN_POINT('Ctrl Pts',(-13.2237784757066,-19.7208552097868,
12.));
#229944=CARTESIAN_POINT('Ctrl Pts',(-13.2291544897899,-19.7401892678697,
12.));
#229945=CARTESIAN_POINT('Ctrl Pts',(-13.2345074487963,-19.7596428141168,
12.));
#229946=CARTESIAN_POINT('Ctrl Pts',(-13.2398366985675,-19.7792151253289,
12.));
#229947=CARTESIAN_POINT('Ctrl Pts',(-13.2451415942805,-19.7989054860495,
12.));
#229948=CARTESIAN_POINT('Ctrl Pts',(-13.2504215002457,-19.8187131883917,
12.));
#229949=CARTESIAN_POINT('Ctrl Pts',(-13.2556757897086,-19.8386375318634,
12.));
#229950=CARTESIAN_POINT('Ctrl Pts',(-13.2609038446529,-19.8586778231715,
12.));
#229951=CARTESIAN_POINT('Ctrl Pts',(-13.2661050556132,-19.8788333760577,
12.));
#229952=CARTESIAN_POINT('Ctrl Pts',(-13.271278821502,-19.8991035111745,
12.));
#229953=CARTESIAN_POINT('Ctrl Pts',(-13.2764245494357,-19.9194875559422,
12.));
#229954=CARTESIAN_POINT('Ctrl Pts',(-13.2815416545663,-19.9399848444019,
12.));
#229955=CARTESIAN_POINT('Ctrl Pts',(-13.286629559915,-19.9605947170586,
12.));
#229956=CARTESIAN_POINT('Ctrl Pts',(-13.2916876962094,-19.981316520717,
12.));
#229957=CARTESIAN_POINT('Ctrl Pts',(-13.2967155017306,-20.0021496083738,
12.));
#229958=CARTESIAN_POINT('Ctrl Pts',(-13.3017124221637,-20.0230933391038,
12.));
#229959=CARTESIAN_POINT('Ctrl Pts',(-13.3066779104515,-20.0441470779345,
12.));
#229960=CARTESIAN_POINT('Ctrl Pts',(-13.3116114266515,-20.0653101957188,
12.));
#229961=CARTESIAN_POINT('Ctrl Pts',(-13.3165124377963,-20.0865820689882,
12.));
#229962=CARTESIAN_POINT('Ctrl Pts',(-13.3213804177587,-20.1079620798375,
12.));
#229963=CARTESIAN_POINT('Ctrl Pts',(-13.3262148471226,-20.1294496158402,
12.));
#229964=CARTESIAN_POINT('Ctrl Pts',(-13.3310152130564,-20.1510440699474,
12.));
#229965=CARTESIAN_POINT('Ctrl Pts',(-13.3357810091903,-20.1727448403817,
12.));
#229966=CARTESIAN_POINT('Ctrl Pts',(-13.3405117354971,-20.1945513305235,
12.));
#229967=CARTESIAN_POINT('Ctrl Pts',(-13.3452068981766,-20.216462948786,
12.));
#229968=CARTESIAN_POINT('Ctrl Pts',(-13.3498660095386,-20.2384791085359,
12.));
#229969=CARTESIAN_POINT('Ctrl Pts',(-13.3544885878889,-20.2605992280122,
12.));
#229970=CARTESIAN_POINT('Ctrl Pts',(-13.3590741574195,-20.2828227302339,
12.));
#229971=CARTESIAN_POINT('Ctrl Pts',(-13.3636222481016,-20.3051490429048,
12.));
#229972=CARTESIAN_POINT('Ctrl Pts',(-13.3681323955826,-20.3275775983029,
12.));
#229973=CARTESIAN_POINT('Ctrl Pts',(-13.3726041410867,-20.3501078331814,
12.));
#229974=CARTESIAN_POINT('Ctrl Pts',(-13.3770370313188,-20.3727391887184,
12.));
#229975=CARTESIAN_POINT('Ctrl Pts',(-13.3814306183719,-20.3954711104502,
12.));
#229976=CARTESIAN_POINT('Ctrl Pts',(-13.3857844596387,-20.4183030482002,
12.));
#229977=CARTESIAN_POINT('Ctrl Pts',(-13.3900981177255,-20.4412344560007,
12.));
#229978=CARTESIAN_POINT('Ctrl Pts',(-13.3943711603739,-20.4642647920037,
12.));
#229979=CARTESIAN_POINT('Ctrl Pts',(-13.3986031603716,-20.487393518404,
12.));
#229980=CARTESIAN_POINT('Ctrl Pts',(-13.4027936954529,-20.5106201013753,
12.));
#229981=CARTESIAN_POINT('Ctrl Pts',(-13.4069423482076,-20.5339440109956,
12.));
#229982=CARTESIAN_POINT('Ctrl Pts',(-13.4110487059912,-20.5573647211639,
12.));
#229983=CARTESIAN_POINT('Ctrl Pts',(-13.4151123608411,-20.5808817095155,
12.));
#229984=CARTESIAN_POINT('Ctrl Pts',(-13.4191329093933,-20.6044944573153,
12.));
#229985=CARTESIAN_POINT('Ctrl Pts',(-13.4231099528179,-20.6282024494237,
12.));
#229986=CARTESIAN_POINT('Ctrl Pts',(-13.4270430967652,-20.6520051742869,
12.));
#229987=CARTESIAN_POINT('Ctrl Pts',(-13.4309319513119,-20.6759021239103,
12.));
#229988=CARTESIAN_POINT('Ctrl Pts',(-13.4347761309154,-20.6998927938288,
12.));
#229989=CARTESIAN_POINT('Ctrl Pts',(-13.4385752543663,-20.7239766830675,
12.));
#229990=CARTESIAN_POINT('Ctrl Pts',(-13.4423289447561,-20.7481532941013,
12.));
#229991=CARTESIAN_POINT('Ctrl Pts',(-13.4460368293688,-20.7724221327608,
12.));
#229992=CARTESIAN_POINT('Ctrl Pts',(-13.4496985395637,-20.7967827081227,
12.));
#229993=CARTESIAN_POINT('Ctrl Pts',(-13.4533137106667,-20.821234532398,
12.));
#229994=CARTESIAN_POINT('Ctrl Pts',(-13.4568819818631,-20.8457771208082,
12.));
#229995=CARTESIAN_POINT('Ctrl Pts',(-13.4604029960983,-20.8704099914641,
12.));
#229996=CARTESIAN_POINT('Ctrl Pts',(-13.4638763999726,-20.8951326652158,
12.));
#229997=CARTESIAN_POINT('Ctrl Pts',(-13.4673018437718,-20.9199446657584,
12.));
#229998=CARTESIAN_POINT('Ctrl Pts',(-13.4706789815167,-20.9448455197557,
12.));
#229999=CARTESIAN_POINT('Ctrl Pts',(-13.4740074710087,-20.9698347569476,
12.));
#230000=CARTESIAN_POINT('Ctrl Pts',(-13.4772869738879,-20.9949119102592,
12.));
#230001=CARTESIAN_POINT('Ctrl Pts',(-13.4805171556822,-21.0200765158885,
12.));
#230002=CARTESIAN_POINT('Ctrl Pts',(-13.4836976858912,-21.0453281134247,
12.));
#230003=CARTESIAN_POINT('Ctrl Pts',(-13.4868282377192,-21.0706662455202,
12.));
#230004=CARTESIAN_POINT('Ctrl Pts',(-13.4899084877718,-21.0960904575048,
12.));
#230005=CARTESIAN_POINT('Ctrl Pts',(-13.4929381157778,-21.1216002970209,
12.));
#230006=CARTESIAN_POINT('Ctrl Pts',(-13.4959168042934,-21.1471953136209,
12.));
#230007=CARTESIAN_POINT('Ctrl Pts',(-13.4988442384491,-21.1728750584173,
12.));
#230008=CARTESIAN_POINT('Ctrl Pts',(-13.5017201056088,-21.1986390835825,
12.));
#230009=CARTESIAN_POINT('Ctrl Pts',(-13.5045440957404,-21.224486942933,
12.));
#230010=CARTESIAN_POINT('Ctrl Pts',(-13.5073159019454,-21.2504181927429,
12.));
#230011=CARTESIAN_POINT('Ctrl Pts',(-13.5100352209207,-21.2764323924442,
12.));
#230012=CARTESIAN_POINT('Ctrl Pts',(-13.5127017534972,-21.3025291054236,
12.));
#230013=CARTESIAN_POINT('Ctrl Pts',(-13.5153152050554,-21.328707899634,
12.));
#230014=CARTESIAN_POINT('Ctrl Pts',(-13.5178752862461,-21.3549683486219,
12.));
#230015=CARTESIAN_POINT('Ctrl Pts',(-13.5203817122497,-21.3813100304967,
12.));
#230016=CARTESIAN_POINT('Ctrl Pts',(-13.5228342013508,-21.4077325259318,
12.));
#230017=CARTESIAN_POINT('Ctrl Pts',(-13.5252324737795,-21.4342354165253,
12.));
#230018=CARTESIAN_POINT('Ctrl Pts',(-13.5275762503553,-21.4608182828695,
12.));
#230019=CARTESIAN_POINT('Ctrl Pts',(-13.5298652514357,-21.487480703047,
12.));
#230020=CARTESIAN_POINT('Ctrl Pts',(-13.5320991952145,-21.5142222501671,
12.));
#230021=CARTESIAN_POINT('Ctrl Pts',(-13.5342777983225,-21.5410424932511,
12.));
#230022=CARTESIAN_POINT('Ctrl Pts',(-13.5364007790292,-21.5679410019011,
12.));
#230023=CARTESIAN_POINT('Ctrl Pts',(-13.5384678597206,-21.5949173499022,
12.));
#230024=CARTESIAN_POINT('Ctrl Pts',(-13.5404787697798,-21.6219711193951,
12.));
#230025=CARTESIAN_POINT('Ctrl Pts',(-13.5424332480698,-21.6491019044647,
12.));
#230026=CARTESIAN_POINT('Ctrl Pts',(-13.5443310461516,-21.676309315769,
12.));
#230027=CARTESIAN_POINT('Ctrl Pts',(-13.546171929503,-21.7035929822939,
12.));
#230028=CARTESIAN_POINT('Ctrl Pts',(-13.5479556704457,-21.730952541226,
12.));
#230029=CARTESIAN_POINT('Ctrl Pts',(-13.5496820422187,-21.7583876294532,
12.));
#230030=CARTESIAN_POINT('Ctrl Pts',(-13.5513508127232,-21.7858978745848,
12.));
#230031=CARTESIAN_POINT('Ctrl Pts',(-13.5529617381569,-21.8134828857963,
12.));
#230032=CARTESIAN_POINT('Ctrl Pts',(-13.5545145573049,-21.841142245609,
12.));
#230033=CARTESIAN_POINT('Ctrl Pts',(-13.5560089839426,-21.8688754989401,
12.));
#230034=CARTESIAN_POINT('Ctrl Pts',(-13.5574447178485,-21.8966821688876,
12.));
#230035=CARTESIAN_POINT('Ctrl Pts',(-13.5588214586672,-21.9245617765827,
12.));
#230036=CARTESIAN_POINT('Ctrl Pts',(-13.5601389185315,-21.9525138592862,
12.));
#230037=CARTESIAN_POINT('Ctrl Pts',(-13.5613968357589,-21.9805379899192,
12.));
#230038=CARTESIAN_POINT('Ctrl Pts',(-13.5625949868313,-22.0086337943431,
12.));
#230039=CARTESIAN_POINT('Ctrl Pts',(-13.5637332022393,-22.0368009736227,
12.));
#230040=CARTESIAN_POINT('Ctrl Pts',(-13.5648113688895,-22.0650393089492,
12.));
#230041=CARTESIAN_POINT('Ctrl Pts',(-13.5658294169107,-22.0933486464442,
12.));
#230042=CARTESIAN_POINT('Ctrl Pts',(-13.5667873105179,-22.1217288871823,
12.));
#230043=CARTESIAN_POINT('Ctrl Pts',(-13.5675054918922,-22.1444897575076,
12.));
#230044=CARTESIAN_POINT('Ctrl Pts',(-13.5680170531724,-22.1615922804939,
12.));
#230045=CARTESIAN_POINT('Ctrl Pts',(-13.5683460612913,-22.1730081264583,
12.));
#230046=CARTESIAN_POINT('Ctrl Pts',(-13.5685075571671,-22.1787195904339,
12.));
#230047=CARTESIAN_POINT('Ctrl Pts',(-14.6513681262571,-17.1452095830632,
0.));
#230048=CARTESIAN_POINT('Ctrl Pts',(-14.6513681262571,-17.1452095830632,
12.));
#230049=CARTESIAN_POINT('Ctrl Pts',(-14.6513711852843,-17.1452153999142,
0.));
#230050=CARTESIAN_POINT('Ctrl Pts',(-14.6513711852843,-17.1452153999142,
12.));
#230051=CARTESIAN_POINT('Ctrl Pts',(-14.6514066997196,-17.1452600887037,
0.));
#230052=CARTESIAN_POINT('Ctrl Pts',(-14.6514066997196,-17.1452600887037,
12.));
#230053=CARTESIAN_POINT('Ctrl Pts',(-14.6515481598068,-17.1454262858043,
0.));
#230054=CARTESIAN_POINT('Ctrl Pts',(-14.6515481598068,-17.1454262858043,
12.));
#230055=CARTESIAN_POINT('Ctrl Pts',(-14.6519131634508,-17.1458462295271,
0.));
#230056=CARTESIAN_POINT('Ctrl Pts',(-14.6519131634508,-17.1458462295271,
12.));
#230057=CARTESIAN_POINT('Ctrl Pts',(-14.6526624064978,-17.1466998098673,
0.));
#230058=CARTESIAN_POINT('Ctrl Pts',(-14.6526624064978,-17.1466998098673,
12.));
#230059=CARTESIAN_POINT('Ctrl Pts',(-14.6537016966184,-17.147876394491,
0.));
#230060=CARTESIAN_POINT('Ctrl Pts',(-14.6537016966184,-17.147876394491,
12.));
#230061=CARTESIAN_POINT('Ctrl Pts',(-14.655024862281,-17.1493641837558,
0.));
#230062=CARTESIAN_POINT('Ctrl Pts',(-14.655024862281,-17.1493641837558,
12.));
#230063=CARTESIAN_POINT('Ctrl Pts',(-14.6566237952435,-17.1511476869496,
0.));
#230064=CARTESIAN_POINT('Ctrl Pts',(-14.6566237952435,-17.1511476869496,
12.));
#230065=CARTESIAN_POINT('Ctrl Pts',(-14.6584900555302,-17.1532107762718,
0.));
#230066=CARTESIAN_POINT('Ctrl Pts',(-14.6584900555302,-17.1532107762718,
12.));
#230067=CARTESIAN_POINT('Ctrl Pts',(-14.6606167169642,-17.1555401986401,
0.));
#230068=CARTESIAN_POINT('Ctrl Pts',(-14.6606167169642,-17.1555401986401,
12.));
#230069=CARTESIAN_POINT('Ctrl Pts',(-14.6629987285992,-17.1581262646789,
0.));
#230070=CARTESIAN_POINT('Ctrl Pts',(-14.6629987285992,-17.1581262646789,
12.));
#230071=CARTESIAN_POINT('Ctrl Pts',(-14.6656319165057,-17.1609609517369,
0.));
#230072=CARTESIAN_POINT('Ctrl Pts',(-14.6656319165057,-17.1609609517369,
12.));
#230073=CARTESIAN_POINT('Ctrl Pts',(-14.6685123374423,-17.1640366762305,
0.));
#230074=CARTESIAN_POINT('Ctrl Pts',(-14.6685123374423,-17.1640366762305,
12.));
#230075=CARTESIAN_POINT('Ctrl Pts',(-14.671635583332,-17.167344972302,0.));
#230076=CARTESIAN_POINT('Ctrl Pts',(-14.671635583332,-17.167344972302,12.));
#230077=CARTESIAN_POINT('Ctrl Pts',(-14.6749971333867,-17.1708771619129,
0.));
#230078=CARTESIAN_POINT('Ctrl Pts',(-14.6749971333867,-17.1708771619129,
12.));
#230079=CARTESIAN_POINT('Ctrl Pts',(-14.6785925615677,-17.1746247499056,
0.));
#230080=CARTESIAN_POINT('Ctrl Pts',(-14.6785925615677,-17.1746247499056,
12.));
#230081=CARTESIAN_POINT('Ctrl Pts',(-14.6824178576167,-17.1785800350826,
0.));
#230082=CARTESIAN_POINT('Ctrl Pts',(-14.6824178576167,-17.1785800350826,
12.));
#230083=CARTESIAN_POINT('Ctrl Pts',(-14.686469452232,-17.1827361584719,
0.));
#230084=CARTESIAN_POINT('Ctrl Pts',(-14.686469452232,-17.1827361584719,
12.));
#230085=CARTESIAN_POINT('Ctrl Pts',(-14.6907440526958,-17.1870867909918,
0.));
#230086=CARTESIAN_POINT('Ctrl Pts',(-14.6907440526958,-17.1870867909918,
12.));
#230087=CARTESIAN_POINT('Ctrl Pts',(-14.6952385361706,-17.1916259308415,
0.));
#230088=CARTESIAN_POINT('Ctrl Pts',(-14.6952385361706,-17.1916259308415,
12.));
#230089=CARTESIAN_POINT('Ctrl Pts',(-14.699949811582,-17.1963476411694,
0.));
#230090=CARTESIAN_POINT('Ctrl Pts',(-14.699949811582,-17.1963476411694,
12.));
#230091=CARTESIAN_POINT('Ctrl Pts',(-14.7048748502663,-17.2012461084268,
0.));
#230092=CARTESIAN_POINT('Ctrl Pts',(-14.7048748502663,-17.2012461084268,
12.));
#230093=CARTESIAN_POINT('Ctrl Pts',(-14.7100107213586,-17.2063157097315,
0.));
#230094=CARTESIAN_POINT('Ctrl Pts',(-14.7100107213586,-17.2063157097315,
12.));
#230095=CARTESIAN_POINT('Ctrl Pts',(-14.7153546289339,-17.2115510835989,
0.));
#230096=CARTESIAN_POINT('Ctrl Pts',(-14.7153546289339,-17.2115510835989,
12.));
#230097=CARTESIAN_POINT('Ctrl Pts',(-14.7209039390327,-17.2169471814256,
0.));
#230098=CARTESIAN_POINT('Ctrl Pts',(-14.7209039390327,-17.2169471814256,
12.));
#230099=CARTESIAN_POINT('Ctrl Pts',(-14.7266561494282,-17.2224992099666,
0.));
#230100=CARTESIAN_POINT('Ctrl Pts',(-14.7266561494282,-17.2224992099666,
12.));
#230101=CARTESIAN_POINT('Ctrl Pts',(-14.7326088681163,-17.2282025904314,
0.));
#230102=CARTESIAN_POINT('Ctrl Pts',(-14.7326088681163,-17.2282025904314,
12.));
#230103=CARTESIAN_POINT('Ctrl Pts',(-14.7387597858117,-17.2340529062076,
0.));
#230104=CARTESIAN_POINT('Ctrl Pts',(-14.7387597858117,-17.2340529062076,
12.));
#230105=CARTESIAN_POINT('Ctrl Pts',(-14.7451066593792,-17.2400458713565,
0.));
#230106=CARTESIAN_POINT('Ctrl Pts',(-14.7451066593792,-17.2400458713565,
12.));
#230107=CARTESIAN_POINT('Ctrl Pts',(-14.7516473175124,-17.2461773413288,
0.));
#230108=CARTESIAN_POINT('Ctrl Pts',(-14.7516473175124,-17.2461773413288,
12.));
#230109=CARTESIAN_POINT('Ctrl Pts',(-14.7583796616617,-17.2524433146837,
0.));
#230110=CARTESIAN_POINT('Ctrl Pts',(-14.7583796616617,-17.2524433146837,
12.));
#230111=CARTESIAN_POINT('Ctrl Pts',(-14.7653016697591,-17.2588399401465,
0.));
#230112=CARTESIAN_POINT('Ctrl Pts',(-14.7653016697591,-17.2588399401465,
12.));
#230113=CARTESIAN_POINT('Ctrl Pts',(-14.7724113956731,-17.2653635155319,
0.));
#230114=CARTESIAN_POINT('Ctrl Pts',(-14.7724113956731,-17.2653635155319,
12.));
#230115=CARTESIAN_POINT('Ctrl Pts',(-14.7797069617804,-17.2720104735194,
0.));
#230116=CARTESIAN_POINT('Ctrl Pts',(-14.7797069617804,-17.2720104735194,
12.));
#230117=CARTESIAN_POINT('Ctrl Pts',(-14.787186553128,-17.2787773704849,
0.));
#230118=CARTESIAN_POINT('Ctrl Pts',(-14.787186553128,-17.2787773704849,
12.));
#230119=CARTESIAN_POINT('Ctrl Pts',(-14.7948484105249,-17.2856608733196,
0.));
#230120=CARTESIAN_POINT('Ctrl Pts',(-14.7948484105249,-17.2856608733196,
12.));
#230121=CARTESIAN_POINT('Ctrl Pts',(-14.8026908254276,-17.2926577496513,
0.));
#230122=CARTESIAN_POINT('Ctrl Pts',(-14.8026908254276,-17.2926577496513,
12.));
#230123=CARTESIAN_POINT('Ctrl Pts',(-14.8107121391036,-17.299764866148,
0.));
#230124=CARTESIAN_POINT('Ctrl Pts',(-14.8107121391036,-17.299764866148,
12.));
#230125=CARTESIAN_POINT('Ctrl Pts',(-14.8189107410162,-17.3069791853706,
0.));
#230126=CARTESIAN_POINT('Ctrl Pts',(-14.8189107410162,-17.3069791853706,
12.));
#230127=CARTESIAN_POINT('Ctrl Pts',(-14.8272850675379,-17.3142977632659,
0.));
#230128=CARTESIAN_POINT('Ctrl Pts',(-14.8272850675379,-17.3142977632659,
12.));
#230129=CARTESIAN_POINT('Ctrl Pts',(-14.8358336004197,-17.3217177462101,
0.));
#230130=CARTESIAN_POINT('Ctrl Pts',(-14.8358336004197,-17.3217177462101,
12.));
#230131=CARTESIAN_POINT('Ctrl Pts',(-14.8445548643508,-17.3292363662605,
0.));
#230132=CARTESIAN_POINT('Ctrl Pts',(-14.8445548643508,-17.3292363662605,
12.));
#230133=CARTESIAN_POINT('Ctrl Pts',(-14.8534474245434,-17.336850936485,
0.));
#230134=CARTESIAN_POINT('Ctrl Pts',(-14.8534474245434,-17.336850936485,
12.));
#230135=CARTESIAN_POINT('Ctrl Pts',(-14.8625098843417,-17.3445588463474,
0.));
#230136=CARTESIAN_POINT('Ctrl Pts',(-14.8625098843417,-17.3445588463474,
12.));
#230137=CARTESIAN_POINT('Ctrl Pts',(-14.8717408826956,-17.3523575568645,
0.));
#230138=CARTESIAN_POINT('Ctrl Pts',(-14.8717408826956,-17.3523575568645,
12.));
#230139=CARTESIAN_POINT('Ctrl Pts',(-14.8811390927423,-17.3602445978161,
0.));
#230140=CARTESIAN_POINT('Ctrl Pts',(-14.8811390927423,-17.3602445978161,
12.));
#230141=CARTESIAN_POINT('Ctrl Pts',(-14.8907032205788,-17.3682175653235,
0.));
#230142=CARTESIAN_POINT('Ctrl Pts',(-14.8907032205788,-17.3682175653235,
12.));
#230143=CARTESIAN_POINT('Ctrl Pts',(-14.900432003961,-17.3762741193076,
0.));
#230144=CARTESIAN_POINT('Ctrl Pts',(-14.900432003961,-17.3762741193076,
12.));
#230145=CARTESIAN_POINT('Ctrl Pts',(-14.9103242110058,-17.3844119809824,
0.));
#230146=CARTESIAN_POINT('Ctrl Pts',(-14.9103242110058,-17.3844119809824,
12.));
#230147=CARTESIAN_POINT('Ctrl Pts',(-14.9203786389342,-17.3926289303986,
0.));
#230148=CARTESIAN_POINT('Ctrl Pts',(-14.9203786389342,-17.3926289303986,
12.));
#230149=CARTESIAN_POINT('Ctrl Pts',(-14.9305941128757,-17.4009228040749,
0.));
#230150=CARTESIAN_POINT('Ctrl Pts',(-14.9305941128757,-17.4009228040749,
12.));
#230151=CARTESIAN_POINT('Ctrl Pts',(-14.940969484645,-17.4092914926071,
0.));
#230152=CARTESIAN_POINT('Ctrl Pts',(-14.940969484645,-17.4092914926071,
12.));
#230153=CARTESIAN_POINT('Ctrl Pts',(-14.9515036315143,-17.4177329382828,
0.));
#230154=CARTESIAN_POINT('Ctrl Pts',(-14.9515036315143,-17.4177329382828,
12.));
#230155=CARTESIAN_POINT('Ctrl Pts',(-14.9621954549827,-17.426245132709,
0.));
#230156=CARTESIAN_POINT('Ctrl Pts',(-14.9621954549827,-17.426245132709,
12.));
#230157=CARTESIAN_POINT('Ctrl Pts',(-14.9730438799452,-17.4348261151396,
0.));
#230158=CARTESIAN_POINT('Ctrl Pts',(-14.9730438799452,-17.4348261151396,
12.));
#230159=CARTESIAN_POINT('Ctrl Pts',(-14.9840478538358,-17.4434739707773,
0.));
#230160=CARTESIAN_POINT('Ctrl Pts',(-14.9840478538358,-17.4434739707773,
12.));
#230161=CARTESIAN_POINT('Ctrl Pts',(-14.9952063457778,-17.4521868291004,
0.));
#230162=CARTESIAN_POINT('Ctrl Pts',(-14.9952063457778,-17.4521868291004,
12.));
#230163=CARTESIAN_POINT('Ctrl Pts',(-15.0065183456921,-17.4609628621418,
0.));
#230164=CARTESIAN_POINT('Ctrl Pts',(-15.0065183456921,-17.4609628621418,
12.));
#230165=CARTESIAN_POINT('Ctrl Pts',(-15.0179828635086,-17.4698002829356,
0.));
#230166=CARTESIAN_POINT('Ctrl Pts',(-15.0179828635086,-17.4698002829356,
12.));
#230167=CARTESIAN_POINT('Ctrl Pts',(-15.029598928488,-17.4786973441417,
0.));
#230168=CARTESIAN_POINT('Ctrl Pts',(-15.029598928488,-17.4786973441417,
12.));
#230169=CARTESIAN_POINT('Ctrl Pts',(-15.0413655884993,-17.4876523366178,
0.));
#230170=CARTESIAN_POINT('Ctrl Pts',(-15.0413655884993,-17.4876523366178,
12.));
#230171=CARTESIAN_POINT('Ctrl Pts',(-15.0532819093085,-17.4966635880245,
0.));
#230172=CARTESIAN_POINT('Ctrl Pts',(-15.0532819093085,-17.4966635880245,
12.));
#230173=CARTESIAN_POINT('Ctrl Pts',(-15.0653469738306,-17.5057294613874,
0.));
#230174=CARTESIAN_POINT('Ctrl Pts',(-15.0653469738306,-17.5057294613874,
12.));
#230175=CARTESIAN_POINT('Ctrl Pts',(-15.0775598815748,-17.5148483539683,
0.));
#230176=CARTESIAN_POINT('Ctrl Pts',(-15.0775598815748,-17.5148483539683,
12.));
#230177=CARTESIAN_POINT('Ctrl Pts',(-15.0899197481082,-17.5240186961788,
0.));
#230178=CARTESIAN_POINT('Ctrl Pts',(-15.0899197481082,-17.5240186961788,
12.));
#230179=CARTESIAN_POINT('Ctrl Pts',(-15.1024257045033,-17.5332389504829,
0.));
#230180=CARTESIAN_POINT('Ctrl Pts',(-15.1024257045033,-17.5332389504829,
12.));
#230181=CARTESIAN_POINT('Ctrl Pts',(-15.1150768967729,-17.5425076102966,
0.));
#230182=CARTESIAN_POINT('Ctrl Pts',(-15.1150768967729,-17.5425076102966,
12.));
#230183=CARTESIAN_POINT('Ctrl Pts',(-15.127872485314,-17.5518231989122,
0.));
#230184=CARTESIAN_POINT('Ctrl Pts',(-15.127872485314,-17.5518231989122,
12.));
#230185=CARTESIAN_POINT('Ctrl Pts',(-15.1408116444877,-17.5611842686196,
0.));
#230186=CARTESIAN_POINT('Ctrl Pts',(-15.1408116444877,-17.5611842686196,
12.));
#230187=CARTESIAN_POINT('Ctrl Pts',(-15.1538935621715,-17.570589399803,
0.));
#230188=CARTESIAN_POINT('Ctrl Pts',(-15.1538935621715,-17.570589399803,
12.));
#230189=CARTESIAN_POINT('Ctrl Pts',(-15.1671174393137,-17.5800372000539,
0.));
#230190=CARTESIAN_POINT('Ctrl Pts',(-15.1671174393137,-17.5800372000539,
12.));
#230191=CARTESIAN_POINT('Ctrl Pts',(-15.1804824894605,-17.5895263032592,
0.));
#230192=CARTESIAN_POINT('Ctrl Pts',(-15.1804824894605,-17.5895263032592,
12.));
#230193=CARTESIAN_POINT('Ctrl Pts',(-15.1939879383268,-17.5990553687595,
0.));
#230194=CARTESIAN_POINT('Ctrl Pts',(-15.1939879383268,-17.5990553687595,
12.));
#230195=CARTESIAN_POINT('Ctrl Pts',(-15.2076330234686,-17.6086230806497,
0.));
#230196=CARTESIAN_POINT('Ctrl Pts',(-15.2076330234686,-17.6086230806497,
12.));
#230197=CARTESIAN_POINT('Ctrl Pts',(-15.22141699392,-17.6182281470467,0.));
#230198=CARTESIAN_POINT('Ctrl Pts',(-15.22141699392,-17.6182281470467,12.));
#230199=CARTESIAN_POINT('Ctrl Pts',(-15.2353391098367,-17.6278692993765,
0.));
#230200=CARTESIAN_POINT('Ctrl Pts',(-15.2353391098367,-17.6278692993765,
12.));
#230201=CARTESIAN_POINT('Ctrl Pts',(-15.2493986421091,-17.637545291637,
0.));
#230202=CARTESIAN_POINT('Ctrl Pts',(-15.2493986421091,-17.637545291637,
12.));
#230203=CARTESIAN_POINT('Ctrl Pts',(-15.263594872029,-17.6472548997329,
0.));
#230204=CARTESIAN_POINT('Ctrl Pts',(-15.263594872029,-17.6472548997329,
12.));
#230205=CARTESIAN_POINT('Ctrl Pts',(-15.2779270910238,-17.6569969209,0.));
#230206=CARTESIAN_POINT('Ctrl Pts',(-15.2779270910238,-17.6569969209,12.));
#230207=CARTESIAN_POINT('Ctrl Pts',(-15.2923946003598,-17.6667701731041,
0.));
#230208=CARTESIAN_POINT('Ctrl Pts',(-15.2923946003598,-17.6667701731041,
12.));
#230209=CARTESIAN_POINT('Ctrl Pts',(-15.3069967108501,-17.6765734944559,
0.));
#230210=CARTESIAN_POINT('Ctrl Pts',(-15.3069967108501,-17.6765734944559,
12.));
#230211=CARTESIAN_POINT('Ctrl Pts',(-15.3217327425341,-17.6864057426052,
0.));
#230212=CARTESIAN_POINT('Ctrl Pts',(-15.3217327425341,-17.6864057426052,
12.));
#230213=CARTESIAN_POINT('Ctrl Pts',(-15.3366020244069,-17.6962657941984,
0.));
#230214=CARTESIAN_POINT('Ctrl Pts',(-15.3366020244069,-17.6962657941984,
12.));
#230215=CARTESIAN_POINT('Ctrl Pts',(-15.3516038942064,-17.7061525444044,
0.));
#230216=CARTESIAN_POINT('Ctrl Pts',(-15.3516038942064,-17.7061525444044,
12.));
#230217=CARTESIAN_POINT('Ctrl Pts',(-15.3667376981702,-17.7160649064208,
0.));
#230218=CARTESIAN_POINT('Ctrl Pts',(-15.3667376981702,-17.7160649064208,
12.));
#230219=CARTESIAN_POINT('Ctrl Pts',(-15.3820027907965,-17.7260018109923,
0.));
#230220=CARTESIAN_POINT('Ctrl Pts',(-15.3820027907965,-17.7260018109923,
12.));
#230221=CARTESIAN_POINT('Ctrl Pts',(-15.3973985345796,-17.7359622059143,
0.));
#230222=CARTESIAN_POINT('Ctrl Pts',(-15.3973985345796,-17.7359622059143,
12.));
#230223=CARTESIAN_POINT('Ctrl Pts',(-15.4129242997828,-17.7459450555803,
0.));
#230224=CARTESIAN_POINT('Ctrl Pts',(-15.4129242997828,-17.7459450555803,
12.));
#230225=CARTESIAN_POINT('Ctrl Pts',(-15.4285794642658,-17.7559493405871,
0.));
#230226=CARTESIAN_POINT('Ctrl Pts',(-15.4285794642658,-17.7559493405871,
12.));
#230227=CARTESIAN_POINT('Ctrl Pts',(-15.4443634132865,-17.765974057326,
0.));
#230228=CARTESIAN_POINT('Ctrl Pts',(-15.4443634132865,-17.765974057326,
12.));
#230229=CARTESIAN_POINT('Ctrl Pts',(-15.460275539302,-17.7760182175817,
0.));
#230230=CARTESIAN_POINT('Ctrl Pts',(-15.460275539302,-17.7760182175817,
12.));
#230231=CARTESIAN_POINT('Ctrl Pts',(-15.4763152417506,-17.7860808481229,
0.));
#230232=CARTESIAN_POINT('Ctrl Pts',(-15.4763152417506,-17.7860808481229,
12.));
#230233=CARTESIAN_POINT('Ctrl Pts',(-15.4924819268529,-17.7961609903161,
0.));
#230234=CARTESIAN_POINT('Ctrl Pts',(-15.4924819268529,-17.7961609903161,
12.));
#230235=CARTESIAN_POINT('Ctrl Pts',(-15.5087750074728,-17.8062576997964,
0.));
#230236=CARTESIAN_POINT('Ctrl Pts',(-15.5087750074728,-17.8062576997964,
12.));
#230237=CARTESIAN_POINT('Ctrl Pts',(-15.5251939029558,-17.8163700461262,
0.));
#230238=CARTESIAN_POINT('Ctrl Pts',(-15.5251939029558,-17.8163700461262,
12.));
#230239=CARTESIAN_POINT('Ctrl Pts',(-15.5417380389639,-17.8264971124606,
0.));
#230240=CARTESIAN_POINT('Ctrl Pts',(-15.5417380389639,-17.8264971124606,
12.));
#230241=CARTESIAN_POINT('Ctrl Pts',(-15.5584068472976,-17.8366379952078,
0.));
#230242=CARTESIAN_POINT('Ctrl Pts',(-15.5584068472976,-17.8366379952078,
12.));
#230243=CARTESIAN_POINT('Ctrl Pts',(-15.5751997657154,-17.8467918036976,
0.));
#230244=CARTESIAN_POINT('Ctrl Pts',(-15.5751997657154,-17.8467918036976,
12.));
#230245=CARTESIAN_POINT('Ctrl Pts',(-15.5921162378183,-17.8569576598996,
0.));
#230246=CARTESIAN_POINT('Ctrl Pts',(-15.5921162378183,-17.8569576598996,
12.));
#230247=CARTESIAN_POINT('Ctrl Pts',(-15.6091557129205,-17.8671346981388,
0.));
#230248=CARTESIAN_POINT('Ctrl Pts',(-15.6091557129205,-17.8671346981388,
12.));
#230249=CARTESIAN_POINT('Ctrl Pts',(-15.6263176459107,-17.8773220648125,
0.));
#230250=CARTESIAN_POINT('Ctrl Pts',(-15.6263176459107,-17.8773220648125,
12.));
#230251=CARTESIAN_POINT('Ctrl Pts',(-15.6436014971088,-17.8875189181095,
0.));
#230252=CARTESIAN_POINT('Ctrl Pts',(-15.6436014971088,-17.8875189181095,
12.));
#230253=CARTESIAN_POINT('Ctrl Pts',(-15.6610067321036,-17.8977244277247,
0.));
#230254=CARTESIAN_POINT('Ctrl Pts',(-15.6610067321036,-17.8977244277247,
12.));
#230255=CARTESIAN_POINT('Ctrl Pts',(-15.6785328216467,-17.9079377746118,
0.));
#230256=CARTESIAN_POINT('Ctrl Pts',(-15.6785328216467,-17.9079377746118,
12.));
#230257=CARTESIAN_POINT('Ctrl Pts',(-15.6961792415526,-17.918158150746,
0.));
#230258=CARTESIAN_POINT('Ctrl Pts',(-15.6961792415526,-17.918158150746,
12.));
#230259=CARTESIAN_POINT('Ctrl Pts',(-15.713945472584,-17.9283847588837,
0.));
#230260=CARTESIAN_POINT('Ctrl Pts',(-15.713945472584,-17.9283847588837,
12.));
#230261=CARTESIAN_POINT('Ctrl Pts',(-15.7318310003334,-17.9386168123261,
0.));
#230262=CARTESIAN_POINT('Ctrl Pts',(-15.7318310003334,-17.9386168123261,
12.));
#230263=CARTESIAN_POINT('Ctrl Pts',(-15.7498353150856,-17.9488535346776,
0.));
#230264=CARTESIAN_POINT('Ctrl Pts',(-15.7498353150856,-17.9488535346776,
12.));
#230265=CARTESIAN_POINT('Ctrl Pts',(-15.7679579117072,-17.9590941596236,
0.));
#230266=CARTESIAN_POINT('Ctrl Pts',(-15.7679579117072,-17.9590941596236,
12.));
#230267=CARTESIAN_POINT('Ctrl Pts',(-15.786198289572,-17.9693379307297,
0.));
#230268=CARTESIAN_POINT('Ctrl Pts',(-15.786198289572,-17.9693379307297,
12.));
#230269=CARTESIAN_POINT('Ctrl Pts',(-15.8045559524674,-17.9795841012383,
0.));
#230270=CARTESIAN_POINT('Ctrl Pts',(-15.8045559524674,-17.9795841012383,
12.));
#230271=CARTESIAN_POINT('Ctrl Pts',(-15.8230304084963,-17.9898319338664,
0.));
#230272=CARTESIAN_POINT('Ctrl Pts',(-15.8230304084963,-17.9898319338664,
12.));
#230273=CARTESIAN_POINT('Ctrl Pts',(-15.8416211699682,-18.0000807006055,
0.));
#230274=CARTESIAN_POINT('Ctrl Pts',(-15.8416211699682,-18.0000807006055,
12.));
#230275=CARTESIAN_POINT('Ctrl Pts',(-15.8603277532834,-18.010329682521,
0.));
#230276=CARTESIAN_POINT('Ctrl Pts',(-15.8603277532834,-18.010329682521,
12.));
#230277=CARTESIAN_POINT('Ctrl Pts',(-15.8791496788685,-18.0205781695773,
0.));
#230278=CARTESIAN_POINT('Ctrl Pts',(-15.8791496788685,-18.0205781695773,
12.));
#230279=CARTESIAN_POINT('Ctrl Pts',(-15.8980864711043,-18.0308254604638,
0.));
#230280=CARTESIAN_POINT('Ctrl Pts',(-15.8980864711043,-18.0308254604638,
12.));
#230281=CARTESIAN_POINT('Ctrl Pts',(-15.9171376582436,-18.0410708624208,
0.));
#230282=CARTESIAN_POINT('Ctrl Pts',(-15.9171376582436,-18.0410708624208,
12.));
#230283=CARTESIAN_POINT('Ctrl Pts',(-15.9363027723244,-18.0513136910691,
0.));
#230284=CARTESIAN_POINT('Ctrl Pts',(-15.9363027723244,-18.0513136910691,
12.));
#230285=CARTESIAN_POINT('Ctrl Pts',(-15.9555813490645,-18.061553270236,
0.));
#230286=CARTESIAN_POINT('Ctrl Pts',(-15.9555813490645,-18.061553270236,
12.));
#230287=CARTESIAN_POINT('Ctrl Pts',(-15.9749729277848,-18.071788931796,
0.));
#230288=CARTESIAN_POINT('Ctrl Pts',(-15.9749729277848,-18.071788931796,
12.));
#230289=CARTESIAN_POINT('Ctrl Pts',(-15.9944770513616,-18.0820200155238,
0.));
#230290=CARTESIAN_POINT('Ctrl Pts',(-15.9944770513616,-18.0820200155238,
12.));
#230291=CARTESIAN_POINT('Ctrl Pts',(-16.0140932661612,-18.0922458689464,
0.));
#230292=CARTESIAN_POINT('Ctrl Pts',(-16.0140932661612,-18.0922458689464,
12.));
#230293=CARTESIAN_POINT('Ctrl Pts',(-16.0338211219694,-18.1024658471966,
0.));
#230294=CARTESIAN_POINT('Ctrl Pts',(-16.0338211219694,-18.1024658471966,
12.));
#230295=CARTESIAN_POINT('Ctrl Pts',(-16.0536601719124,-18.1126793128688,
0.));
#230296=CARTESIAN_POINT('Ctrl Pts',(-16.0536601719124,-18.1126793128688,
12.));
#230297=CARTESIAN_POINT('Ctrl Pts',(-16.0736099723665,-18.1228856358746,
0.));
#230298=CARTESIAN_POINT('Ctrl Pts',(-16.0736099723665,-18.1228856358746,
12.));
#230299=CARTESIAN_POINT('Ctrl Pts',(-16.0936700829108,-18.1330841933099,
0.));
#230300=CARTESIAN_POINT('Ctrl Pts',(-16.0936700829108,-18.1330841933099,
12.));
#230301=CARTESIAN_POINT('Ctrl Pts',(-16.1138400662791,-18.1432743693231,
0.));
#230302=CARTESIAN_POINT('Ctrl Pts',(-16.1138400662791,-18.1432743693231,
12.));
#230303=CARTESIAN_POINT('Ctrl Pts',(-16.1341194882987,-18.153455554985,
0.));
#230304=CARTESIAN_POINT('Ctrl Pts',(-16.1341194882987,-18.153455554985,
12.));
#230305=CARTESIAN_POINT('Ctrl Pts',(-16.1545079178261,-18.1636271481616,
0.));
#230306=CARTESIAN_POINT('Ctrl Pts',(-16.1545079178261,-18.1636271481616,
12.));
#230307=CARTESIAN_POINT('Ctrl Pts',(-16.1750049266673,-18.1737885533852,
0.));
#230308=CARTESIAN_POINT('Ctrl Pts',(-16.1750049266673,-18.1737885533852,
12.));
#230309=CARTESIAN_POINT('Ctrl Pts',(-16.1956100895076,-18.1839391817335,
0.));
#230310=CARTESIAN_POINT('Ctrl Pts',(-16.1956100895076,-18.1839391817335,
12.));
#230311=CARTESIAN_POINT('Ctrl Pts',(-16.2163229838878,-18.1940784507232,
0.));
#230312=CARTESIAN_POINT('Ctrl Pts',(-16.2163229838878,-18.1940784507232,
12.));
#230313=CARTESIAN_POINT('Ctrl Pts',(-16.237143190164,-18.2042057842037,
0.));
#230314=CARTESIAN_POINT('Ctrl Pts',(-16.237143190164,-18.2042057842037,
12.));
#230315=CARTESIAN_POINT('Ctrl Pts',(-16.2580702914615,-18.214320612253,
0.));
#230316=CARTESIAN_POINT('Ctrl Pts',(-16.2580702914615,-18.214320612253,
12.));
#230317=CARTESIAN_POINT('Ctrl Pts',(-16.2791038736223,-18.2244223710745,
0.));
#230318=CARTESIAN_POINT('Ctrl Pts',(-16.2791038736223,-18.2244223710745,
12.));
#230319=CARTESIAN_POINT('Ctrl Pts',(-16.3002435251378,-18.2345105028981,
0.));
#230320=CARTESIAN_POINT('Ctrl Pts',(-16.3002435251378,-18.2345105028981,
12.));
#230321=CARTESIAN_POINT('Ctrl Pts',(-16.3214888370988,-18.2445844558742,
0.));
#230322=CARTESIAN_POINT('Ctrl Pts',(-16.3214888370988,-18.2445844558742,
12.));
#230323=CARTESIAN_POINT('Ctrl Pts',(-16.342839403159,-18.2546436839609,
0.));
#230324=CARTESIAN_POINT('Ctrl Pts',(-16.342839403159,-18.2546436839609,
12.));
#230325=CARTESIAN_POINT('Ctrl Pts',(-16.3642948194869,-18.2646876468169,
0.));
#230326=CARTESIAN_POINT('Ctrl Pts',(-16.3642948194869,-18.2646876468169,
12.));
#230327=CARTESIAN_POINT('Ctrl Pts',(-16.385854684708,-18.2747158096934,
0.));
#230328=CARTESIAN_POINT('Ctrl Pts',(-16.385854684708,-18.2747158096934,
12.));
#230329=CARTESIAN_POINT('Ctrl Pts',(-16.4075185998454,-18.2847276433308,
0.));
#230330=CARTESIAN_POINT('Ctrl Pts',(-16.4075185998454,-18.2847276433308,
12.));
#230331=CARTESIAN_POINT('Ctrl Pts',(-16.4292861682377,-18.2947226238509,
0.));
#230332=CARTESIAN_POINT('Ctrl Pts',(-16.4292861682377,-18.2947226238509,
12.));
#230333=CARTESIAN_POINT('Ctrl Pts',(-16.4511569955231,-18.3047002326858,
0.));
#230334=CARTESIAN_POINT('Ctrl Pts',(-16.4511569955231,-18.3047002326858,
12.));
#230335=CARTESIAN_POINT('Ctrl Pts',(-16.4731306896439,-18.3146599565229,
0.));
#230336=CARTESIAN_POINT('Ctrl Pts',(-16.4731306896439,-18.3146599565229,
12.));
#230337=CARTESIAN_POINT('Ctrl Pts',(-16.4952068608344,-18.3246012872468,
0.));
#230338=CARTESIAN_POINT('Ctrl Pts',(-16.4952068608344,-18.3246012872468,
12.));
#230339=CARTESIAN_POINT('Ctrl Pts',(-16.5173851216045,-18.3345237218864,
0.));
#230340=CARTESIAN_POINT('Ctrl Pts',(-16.5173851216045,-18.3345237218864,
12.));
#230341=CARTESIAN_POINT('Ctrl Pts',(-16.539665086714,-18.3444267625601,
0.));
#230342=CARTESIAN_POINT('Ctrl Pts',(-16.539665086714,-18.3444267625601,
12.));
#230343=CARTESIAN_POINT('Ctrl Pts',(-16.5620463731414,-18.3543099164331,
0.));
#230344=CARTESIAN_POINT('Ctrl Pts',(-16.5620463731414,-18.3543099164331,
12.));
#230345=CARTESIAN_POINT('Ctrl Pts',(-16.5845286000219,-18.364172695589,
0.));
#230346=CARTESIAN_POINT('Ctrl Pts',(-16.5845286000219,-18.364172695589,
12.));
#230347=CARTESIAN_POINT('Ctrl Pts',(-16.6071113885711,-18.3740146168879,
0.));
#230348=CARTESIAN_POINT('Ctrl Pts',(-16.6071113885711,-18.3740146168879,
12.));
#230349=CARTESIAN_POINT('Ctrl Pts',(-16.6297943620056,-18.3838352018327,
0.));
#230350=CARTESIAN_POINT('Ctrl Pts',(-16.6297943620056,-18.3838352018327,
12.));
#230351=CARTESIAN_POINT('Ctrl Pts',(-16.6525771454513,-18.3936339764332,
0.));
#230352=CARTESIAN_POINT('Ctrl Pts',(-16.6525771454513,-18.3936339764332,
12.));
#230353=CARTESIAN_POINT('Ctrl Pts',(-16.6754593658513,-18.4034104710789,
0.));
#230354=CARTESIAN_POINT('Ctrl Pts',(-16.6754593658513,-18.4034104710789,
12.));
#230355=CARTESIAN_POINT('Ctrl Pts',(-16.698440651849,-18.4131642203989,
0.));
#230356=CARTESIAN_POINT('Ctrl Pts',(-16.698440651849,-18.4131642203989,
12.));
#230357=CARTESIAN_POINT('Ctrl Pts',(-16.7215206338818,-18.4228947633186,
0.));
#230358=CARTESIAN_POINT('Ctrl Pts',(-16.7215206338818,-18.4228947633186,
12.));
#230359=CARTESIAN_POINT('Ctrl Pts',(-16.7446989442882,-18.4326016431392,
0.));
#230360=CARTESIAN_POINT('Ctrl Pts',(-16.7446989442882,-18.4326016431392,
12.));
#230361=CARTESIAN_POINT('Ctrl Pts',(-16.7679752173992,-18.4422844076099,
0.));
#230362=CARTESIAN_POINT('Ctrl Pts',(-16.7679752173992,-18.4422844076099,
12.));
#230363=CARTESIAN_POINT('Ctrl Pts',(-16.791349089629,-18.4519426090124,
0.));
#230364=CARTESIAN_POINT('Ctrl Pts',(-16.791349089629,-18.4519426090124,
12.));
#230365=CARTESIAN_POINT('Ctrl Pts',(-16.8148201995472,-18.4615758042305,
0.));
#230366=CARTESIAN_POINT('Ctrl Pts',(-16.8148201995472,-18.4615758042305,
12.));
#230367=CARTESIAN_POINT('Ctrl Pts',(-16.8383881879707,-18.4711835548622,
0.));
#230368=CARTESIAN_POINT('Ctrl Pts',(-16.8383881879707,-18.4711835548622,
12.));
#230369=CARTESIAN_POINT('Ctrl Pts',(-16.8620526977169,-18.4807654268769,
0.));
#230370=CARTESIAN_POINT('Ctrl Pts',(-16.8620526977169,-18.4807654268769,
12.));
#230371=CARTESIAN_POINT('Ctrl Pts',(-16.8858133733086,-18.4903209902226,
0.));
#230372=CARTESIAN_POINT('Ctrl Pts',(-16.8858133733086,-18.4903209902226,
12.));
#230373=CARTESIAN_POINT('Ctrl Pts',(-16.9096698606942,-18.4998498184619,
0.));
#230374=CARTESIAN_POINT('Ctrl Pts',(-16.9096698606942,-18.4998498184619,
12.));
#230375=CARTESIAN_POINT('Ctrl Pts',(-16.9336218069353,-18.5093514883835,
0.));
#230376=CARTESIAN_POINT('Ctrl Pts',(-16.9336218069353,-18.5093514883835,
12.));
#230377=CARTESIAN_POINT('Ctrl Pts',(-16.957668859934,-18.518825579666,0.));
#230378=CARTESIAN_POINT('Ctrl Pts',(-16.957668859934,-18.518825579666,12.));
#230379=CARTESIAN_POINT('Ctrl Pts',(-16.9818106680382,-18.5282716744198,
0.));
#230380=CARTESIAN_POINT('Ctrl Pts',(-16.9818106680382,-18.5282716744198,
12.));
#230381=CARTESIAN_POINT('Ctrl Pts',(-17.0060468805099,-18.5376893576961,
0.));
#230382=CARTESIAN_POINT('Ctrl Pts',(-17.0060468805099,-18.5376893576961,
12.));
#230383=CARTESIAN_POINT('Ctrl Pts',(-17.030377148174,-18.5470782182089,
0.));
#230384=CARTESIAN_POINT('Ctrl Pts',(-17.030377148174,-18.5470782182089,
12.));
#230385=CARTESIAN_POINT('Ctrl Pts',(-17.0548011239751,-18.5564378489628,
0.));
#230386=CARTESIAN_POINT('Ctrl Pts',(-17.0548011239751,-18.5564378489628,
12.));
#230387=CARTESIAN_POINT('Ctrl Pts',(-17.0793184636079,-18.5657678479788,
0.));
#230388=CARTESIAN_POINT('Ctrl Pts',(-17.0793184636079,-18.5657678479788,
12.));
#230389=CARTESIAN_POINT('Ctrl Pts',(-17.1039288260002,-18.5750678188543,
0.));
#230390=CARTESIAN_POINT('Ctrl Pts',(-17.1039288260002,-18.5750678188543,
12.));
#230391=CARTESIAN_POINT('Ctrl Pts',(-17.1286318741185,-18.5843373717253,
0.));
#230392=CARTESIAN_POINT('Ctrl Pts',(-17.1286318741185,-18.5843373717253,
12.));
#230393=CARTESIAN_POINT('Ctrl Pts',(-17.1534272741646,-18.5935761222833,
0.));
#230394=CARTESIAN_POINT('Ctrl Pts',(-17.1534272741646,-18.5935761222833,
12.));
#230395=CARTESIAN_POINT('Ctrl Pts',(-17.1783146940131,-18.6027836898826,
0.));
#230396=CARTESIAN_POINT('Ctrl Pts',(-17.1783146940131,-18.6027836898826,
12.));
#230397=CARTESIAN_POINT('Ctrl Pts',(-17.2032938019288,-18.6119596959957,
0.));
#230398=CARTESIAN_POINT('Ctrl Pts',(-17.2032938019288,-18.6119596959957,
12.));
#230399=CARTESIAN_POINT('Ctrl Pts',(-17.2283642650519,-18.6211037624041,
0.));
#230400=CARTESIAN_POINT('Ctrl Pts',(-17.2283642650519,-18.6211037624041,
12.));
#230401=CARTESIAN_POINT('Ctrl Pts',(-17.2535257482186,-18.630215509794,
0.));
#230402=CARTESIAN_POINT('Ctrl Pts',(-17.2535257482186,-18.630215509794,
12.));
#230403=CARTESIAN_POINT('Ctrl Pts',(-17.278777912021,-18.639294555474,0.));
#230404=CARTESIAN_POINT('Ctrl Pts',(-17.278777912021,-18.639294555474,12.));
#230405=CARTESIAN_POINT('Ctrl Pts',(-17.3041204135069,-18.6483405141853,
0.));
#230406=CARTESIAN_POINT('Ctrl Pts',(-17.3041204135069,-18.6483405141853,
12.));
#230407=CARTESIAN_POINT('Ctrl Pts',(-17.3295529098612,-18.6573530024019,
0.));
#230408=CARTESIAN_POINT('Ctrl Pts',(-17.3295529098612,-18.6573530024019,
12.));
#230409=CARTESIAN_POINT('Ctrl Pts',(-17.3550750612438,-18.6663316416569,
0.));
#230410=CARTESIAN_POINT('Ctrl Pts',(-17.3550750612438,-18.6663316416569,
12.));
#230411=CARTESIAN_POINT('Ctrl Pts',(-17.3806865340744,-18.6752760624045,
0.));
#230412=CARTESIAN_POINT('Ctrl Pts',(-17.3806865340744,-18.6752760624045,
12.));
#230413=CARTESIAN_POINT('Ctrl Pts',(-17.4063870038563,-18.6841859073472,
0.));
#230414=CARTESIAN_POINT('Ctrl Pts',(-17.4063870038563,-18.6841859073472,
12.));
#230415=CARTESIAN_POINT('Ctrl Pts',(-17.4321761588148,-18.6930608357421,
0.));
#230416=CARTESIAN_POINT('Ctrl Pts',(-17.4321761588148,-18.6930608357421,
12.));
#230417=CARTESIAN_POINT('Ctrl Pts',(-17.4580537012764,-18.7019005250322,
0.));
#230418=CARTESIAN_POINT('Ctrl Pts',(-17.4580537012764,-18.7019005250322,
12.));
#230419=CARTESIAN_POINT('Ctrl Pts',(-17.4840193397176,-18.7107046613941,
0.));
#230420=CARTESIAN_POINT('Ctrl Pts',(-17.4840193397176,-18.7107046613941,
12.));
#230421=CARTESIAN_POINT('Ctrl Pts',(-17.5100727820891,-18.7194729318127,
0.));
#230422=CARTESIAN_POINT('Ctrl Pts',(-17.5100727820891,-18.7194729318127,
12.));
#230423=CARTESIAN_POINT('Ctrl Pts',(-17.5362137287604,-18.728205015716,
0.));
#230424=CARTESIAN_POINT('Ctrl Pts',(-17.5362137287604,-18.728205015716,
12.));
#230425=CARTESIAN_POINT('Ctrl Pts',(-17.5624418653248,-18.7369005764558,
0.));
#230426=CARTESIAN_POINT('Ctrl Pts',(-17.5624418653248,-18.7369005764558,
12.));
#230427=CARTESIAN_POINT('Ctrl Pts',(-17.5887568561361,-18.7455592536667,
0.));
#230428=CARTESIAN_POINT('Ctrl Pts',(-17.5887568561361,-18.7455592536667,
12.));
#230429=CARTESIAN_POINT('Ctrl Pts',(-17.6151583356989,-18.7541806530935,
0.));
#230430=CARTESIAN_POINT('Ctrl Pts',(-17.6151583356989,-18.7541806530935,
12.));
#230431=CARTESIAN_POINT('Ctrl Pts',(-17.6416459210646,-18.7627643613138,
0.));
#230432=CARTESIAN_POINT('Ctrl Pts',(-17.6416459210646,-18.7627643613138,
12.));
#230433=CARTESIAN_POINT('Ctrl Pts',(-17.6682192274197,-18.7713099642673,
0.));
#230434=CARTESIAN_POINT('Ctrl Pts',(-17.6682192274197,-18.7713099642673,
12.));
#230435=CARTESIAN_POINT('Ctrl Pts',(-17.6948778822982,-18.7798170641305,
0.));
#230436=CARTESIAN_POINT('Ctrl Pts',(-17.6948778822982,-18.7798170641305,
12.));
#230437=CARTESIAN_POINT('Ctrl Pts',(-17.7216215409019,-18.7882852976016,
0.));
#230438=CARTESIAN_POINT('Ctrl Pts',(-17.7216215409019,-18.7882852976016,
12.));
#230439=CARTESIAN_POINT('Ctrl Pts',(-17.7484498996917,-18.7967143519444,
0.));
#230440=CARTESIAN_POINT('Ctrl Pts',(-17.7484498996917,-18.7967143519444,
12.));
#230441=CARTESIAN_POINT('Ctrl Pts',(-17.7753627137898,-18.8051039860543,
0.));
#230442=CARTESIAN_POINT('Ctrl Pts',(-17.7753627137898,-18.8051039860543,
12.));
#230443=CARTESIAN_POINT('Ctrl Pts',(-17.8023598011135,-18.8134540340581,
0.));
#230444=CARTESIAN_POINT('Ctrl Pts',(-17.8023598011135,-18.8134540340581,
12.));
#230445=CARTESIAN_POINT('Ctrl Pts',(-17.8294410311105,-18.8217643886368,
0.));
#230446=CARTESIAN_POINT('Ctrl Pts',(-17.8294410311105,-18.8217643886368,
12.));
#230447=CARTESIAN_POINT('Ctrl Pts',(-17.8566063174871,-18.8300349896187,
0.));
#230448=CARTESIAN_POINT('Ctrl Pts',(-17.8566063174871,-18.8300349896187,
12.));
#230449=CARTESIAN_POINT('Ctrl Pts',(-17.8784057509434,-18.8366196462746,
0.));
#230450=CARTESIAN_POINT('Ctrl Pts',(-17.8784057509434,-18.8366196462746,
12.));
#230451=CARTESIAN_POINT('Ctrl Pts',(-17.8947931177853,-18.8415402351882,
0.));
#230452=CARTESIAN_POINT('Ctrl Pts',(-17.8947931177853,-18.8415402351882,
12.));
#230453=CARTESIAN_POINT('Ctrl Pts',(-17.9057348246611,-18.8448126709726,
0.));
#230454=CARTESIAN_POINT('Ctrl Pts',(-17.9057348246611,-18.8448126709726,
12.));
#230455=CARTESIAN_POINT('Ctrl Pts',(-17.9112098770111,-18.8464468996588,
0.));
#230456=CARTESIAN_POINT('Ctrl Pts',(-17.9112098770111,-18.8464468996588,
12.));
#230457=CARTESIAN_POINT('',(-17.9112098770111,-18.8464468996588,0.));
#230458=CARTESIAN_POINT('Ctrl Pts',(-14.6513681262571,-17.1452095830632,
0.));
#230459=CARTESIAN_POINT('Ctrl Pts',(-14.6513711852843,-17.1452153999142,
0.));
#230460=CARTESIAN_POINT('Ctrl Pts',(-14.6514066997196,-17.1452600887037,
0.));
#230461=CARTESIAN_POINT('Ctrl Pts',(-14.6515481598068,-17.1454262858043,
0.));
#230462=CARTESIAN_POINT('Ctrl Pts',(-14.6519131634508,-17.1458462295271,
0.));
#230463=CARTESIAN_POINT('Ctrl Pts',(-14.6526624064978,-17.1466998098673,
0.));
#230464=CARTESIAN_POINT('Ctrl Pts',(-14.6537016966184,-17.147876394491,
0.));
#230465=CARTESIAN_POINT('Ctrl Pts',(-14.655024862281,-17.1493641837558,
0.));
#230466=CARTESIAN_POINT('Ctrl Pts',(-14.6566237952435,-17.1511476869496,
0.));
#230467=CARTESIAN_POINT('Ctrl Pts',(-14.6584900555302,-17.1532107762718,
0.));
#230468=CARTESIAN_POINT('Ctrl Pts',(-14.6606167169642,-17.1555401986401,
0.));
#230469=CARTESIAN_POINT('Ctrl Pts',(-14.6629987285992,-17.1581262646789,
0.));
#230470=CARTESIAN_POINT('Ctrl Pts',(-14.6656319165057,-17.1609609517369,
0.));
#230471=CARTESIAN_POINT('Ctrl Pts',(-14.6685123374423,-17.1640366762305,
0.));
#230472=CARTESIAN_POINT('Ctrl Pts',(-14.671635583332,-17.167344972302,0.));
#230473=CARTESIAN_POINT('Ctrl Pts',(-14.6749971333867,-17.1708771619129,
0.));
#230474=CARTESIAN_POINT('Ctrl Pts',(-14.6785925615677,-17.1746247499056,
0.));
#230475=CARTESIAN_POINT('Ctrl Pts',(-14.6824178576167,-17.1785800350826,
0.));
#230476=CARTESIAN_POINT('Ctrl Pts',(-14.686469452232,-17.1827361584719,
0.));
#230477=CARTESIAN_POINT('Ctrl Pts',(-14.6907440526958,-17.1870867909918,
0.));
#230478=CARTESIAN_POINT('Ctrl Pts',(-14.6952385361706,-17.1916259308415,
0.));
#230479=CARTESIAN_POINT('Ctrl Pts',(-14.699949811582,-17.1963476411694,
0.));
#230480=CARTESIAN_POINT('Ctrl Pts',(-14.7048748502663,-17.2012461084268,
0.));
#230481=CARTESIAN_POINT('Ctrl Pts',(-14.7100107213586,-17.2063157097315,
0.));
#230482=CARTESIAN_POINT('Ctrl Pts',(-14.7153546289339,-17.2115510835989,
0.));
#230483=CARTESIAN_POINT('Ctrl Pts',(-14.7209039390327,-17.2169471814256,
0.));
#230484=CARTESIAN_POINT('Ctrl Pts',(-14.7266561494282,-17.2224992099666,
0.));
#230485=CARTESIAN_POINT('Ctrl Pts',(-14.7326088681163,-17.2282025904314,
0.));
#230486=CARTESIAN_POINT('Ctrl Pts',(-14.7387597858117,-17.2340529062076,
0.));
#230487=CARTESIAN_POINT('Ctrl Pts',(-14.7451066593792,-17.2400458713565,
0.));
#230488=CARTESIAN_POINT('Ctrl Pts',(-14.7516473175124,-17.2461773413288,
0.));
#230489=CARTESIAN_POINT('Ctrl Pts',(-14.7583796616617,-17.2524433146837,
0.));
#230490=CARTESIAN_POINT('Ctrl Pts',(-14.7653016697591,-17.2588399401465,
0.));
#230491=CARTESIAN_POINT('Ctrl Pts',(-14.7724113956731,-17.2653635155319,
0.));
#230492=CARTESIAN_POINT('Ctrl Pts',(-14.7797069617804,-17.2720104735194,
0.));
#230493=CARTESIAN_POINT('Ctrl Pts',(-14.787186553128,-17.2787773704849,
0.));
#230494=CARTESIAN_POINT('Ctrl Pts',(-14.7948484105249,-17.2856608733196,
0.));
#230495=CARTESIAN_POINT('Ctrl Pts',(-14.8026908254276,-17.2926577496513,
0.));
#230496=CARTESIAN_POINT('Ctrl Pts',(-14.8107121391036,-17.299764866148,
0.));
#230497=CARTESIAN_POINT('Ctrl Pts',(-14.8189107410162,-17.3069791853706,
0.));
#230498=CARTESIAN_POINT('Ctrl Pts',(-14.8272850675379,-17.3142977632659,
0.));
#230499=CARTESIAN_POINT('Ctrl Pts',(-14.8358336004197,-17.3217177462101,
0.));
#230500=CARTESIAN_POINT('Ctrl Pts',(-14.8445548643508,-17.3292363662605,
0.));
#230501=CARTESIAN_POINT('Ctrl Pts',(-14.8534474245434,-17.336850936485,
0.));
#230502=CARTESIAN_POINT('Ctrl Pts',(-14.8625098843417,-17.3445588463474,
0.));
#230503=CARTESIAN_POINT('Ctrl Pts',(-14.8717408826956,-17.3523575568645,
0.));
#230504=CARTESIAN_POINT('Ctrl Pts',(-14.8811390927423,-17.3602445978161,
0.));
#230505=CARTESIAN_POINT('Ctrl Pts',(-14.8907032205788,-17.3682175653235,
0.));
#230506=CARTESIAN_POINT('Ctrl Pts',(-14.900432003961,-17.3762741193076,
0.));
#230507=CARTESIAN_POINT('Ctrl Pts',(-14.9103242110058,-17.3844119809824,
0.));
#230508=CARTESIAN_POINT('Ctrl Pts',(-14.9203786389342,-17.3926289303986,
0.));
#230509=CARTESIAN_POINT('Ctrl Pts',(-14.9305941128757,-17.4009228040749,
0.));
#230510=CARTESIAN_POINT('Ctrl Pts',(-14.940969484645,-17.4092914926071,
0.));
#230511=CARTESIAN_POINT('Ctrl Pts',(-14.9515036315143,-17.4177329382828,
0.));
#230512=CARTESIAN_POINT('Ctrl Pts',(-14.9621954549827,-17.426245132709,
0.));
#230513=CARTESIAN_POINT('Ctrl Pts',(-14.9730438799452,-17.4348261151396,
0.));
#230514=CARTESIAN_POINT('Ctrl Pts',(-14.9840478538358,-17.4434739707773,
0.));
#230515=CARTESIAN_POINT('Ctrl Pts',(-14.9952063457778,-17.4521868291004,
0.));
#230516=CARTESIAN_POINT('Ctrl Pts',(-15.0065183456921,-17.4609628621418,
0.));
#230517=CARTESIAN_POINT('Ctrl Pts',(-15.0179828635086,-17.4698002829356,
0.));
#230518=CARTESIAN_POINT('Ctrl Pts',(-15.029598928488,-17.4786973441417,
0.));
#230519=CARTESIAN_POINT('Ctrl Pts',(-15.0413655884993,-17.4876523366178,
0.));
#230520=CARTESIAN_POINT('Ctrl Pts',(-15.0532819093085,-17.4966635880245,
0.));
#230521=CARTESIAN_POINT('Ctrl Pts',(-15.0653469738306,-17.5057294613874,
0.));
#230522=CARTESIAN_POINT('Ctrl Pts',(-15.0775598815748,-17.5148483539683,
0.));
#230523=CARTESIAN_POINT('Ctrl Pts',(-15.0899197481082,-17.5240186961788,
0.));
#230524=CARTESIAN_POINT('Ctrl Pts',(-15.1024257045033,-17.5332389504829,
0.));
#230525=CARTESIAN_POINT('Ctrl Pts',(-15.1150768967729,-17.5425076102966,
0.));
#230526=CARTESIAN_POINT('Ctrl Pts',(-15.127872485314,-17.5518231989122,
0.));
#230527=CARTESIAN_POINT('Ctrl Pts',(-15.1408116444877,-17.5611842686196,
0.));
#230528=CARTESIAN_POINT('Ctrl Pts',(-15.1538935621715,-17.570589399803,
0.));
#230529=CARTESIAN_POINT('Ctrl Pts',(-15.1671174393137,-17.5800372000539,
0.));
#230530=CARTESIAN_POINT('Ctrl Pts',(-15.1804824894605,-17.5895263032592,
0.));
#230531=CARTESIAN_POINT('Ctrl Pts',(-15.1939879383268,-17.5990553687595,
0.));
#230532=CARTESIAN_POINT('Ctrl Pts',(-15.2076330234686,-17.6086230806497,
0.));
#230533=CARTESIAN_POINT('Ctrl Pts',(-15.22141699392,-17.6182281470467,0.));
#230534=CARTESIAN_POINT('Ctrl Pts',(-15.2353391098367,-17.6278692993765,
0.));
#230535=CARTESIAN_POINT('Ctrl Pts',(-15.2493986421091,-17.637545291637,
0.));
#230536=CARTESIAN_POINT('Ctrl Pts',(-15.263594872029,-17.6472548997329,
0.));
#230537=CARTESIAN_POINT('Ctrl Pts',(-15.2779270910238,-17.6569969209,0.));
#230538=CARTESIAN_POINT('Ctrl Pts',(-15.2923946003598,-17.6667701731041,
0.));
#230539=CARTESIAN_POINT('Ctrl Pts',(-15.3069967108501,-17.6765734944559,
0.));
#230540=CARTESIAN_POINT('Ctrl Pts',(-15.3217327425341,-17.6864057426052,
0.));
#230541=CARTESIAN_POINT('Ctrl Pts',(-15.3366020244069,-17.6962657941984,
0.));
#230542=CARTESIAN_POINT('Ctrl Pts',(-15.3516038942064,-17.7061525444044,
0.));
#230543=CARTESIAN_POINT('Ctrl Pts',(-15.3667376981702,-17.7160649064208,
0.));
#230544=CARTESIAN_POINT('Ctrl Pts',(-15.3820027907965,-17.7260018109923,
0.));
#230545=CARTESIAN_POINT('Ctrl Pts',(-15.3973985345796,-17.7359622059143,
0.));
#230546=CARTESIAN_POINT('Ctrl Pts',(-15.4129242997828,-17.7459450555803,
0.));
#230547=CARTESIAN_POINT('Ctrl Pts',(-15.4285794642658,-17.7559493405871,
0.));
#230548=CARTESIAN_POINT('Ctrl Pts',(-15.4443634132865,-17.765974057326,
0.));
#230549=CARTESIAN_POINT('Ctrl Pts',(-15.460275539302,-17.7760182175817,
0.));
#230550=CARTESIAN_POINT('Ctrl Pts',(-15.4763152417506,-17.7860808481229,
0.));
#230551=CARTESIAN_POINT('Ctrl Pts',(-15.4924819268529,-17.7961609903161,
0.));
#230552=CARTESIAN_POINT('Ctrl Pts',(-15.5087750074728,-17.8062576997964,
0.));
#230553=CARTESIAN_POINT('Ctrl Pts',(-15.5251939029558,-17.8163700461262,
0.));
#230554=CARTESIAN_POINT('Ctrl Pts',(-15.5417380389639,-17.8264971124606,
0.));
#230555=CARTESIAN_POINT('Ctrl Pts',(-15.5584068472976,-17.8366379952078,
0.));
#230556=CARTESIAN_POINT('Ctrl Pts',(-15.5751997657154,-17.8467918036976,
0.));
#230557=CARTESIAN_POINT('Ctrl Pts',(-15.5921162378183,-17.8569576598996,
0.));
#230558=CARTESIAN_POINT('Ctrl Pts',(-15.6091557129205,-17.8671346981388,
0.));
#230559=CARTESIAN_POINT('Ctrl Pts',(-15.6263176459107,-17.8773220648125,
0.));
#230560=CARTESIAN_POINT('Ctrl Pts',(-15.6436014971088,-17.8875189181095,
0.));
#230561=CARTESIAN_POINT('Ctrl Pts',(-15.6610067321036,-17.8977244277247,
0.));
#230562=CARTESIAN_POINT('Ctrl Pts',(-15.6785328216467,-17.9079377746118,
0.));
#230563=CARTESIAN_POINT('Ctrl Pts',(-15.6961792415526,-17.918158150746,
0.));
#230564=CARTESIAN_POINT('Ctrl Pts',(-15.713945472584,-17.9283847588837,
0.));
#230565=CARTESIAN_POINT('Ctrl Pts',(-15.7318310003334,-17.9386168123261,
0.));
#230566=CARTESIAN_POINT('Ctrl Pts',(-15.7498353150856,-17.9488535346776,
0.));
#230567=CARTESIAN_POINT('Ctrl Pts',(-15.7679579117072,-17.9590941596236,
0.));
#230568=CARTESIAN_POINT('Ctrl Pts',(-15.786198289572,-17.9693379307297,
0.));
#230569=CARTESIAN_POINT('Ctrl Pts',(-15.8045559524674,-17.9795841012383,
0.));
#230570=CARTESIAN_POINT('Ctrl Pts',(-15.8230304084963,-17.9898319338664,
0.));
#230571=CARTESIAN_POINT('Ctrl Pts',(-15.8416211699682,-18.0000807006055,
0.));
#230572=CARTESIAN_POINT('Ctrl Pts',(-15.8603277532834,-18.010329682521,
0.));
#230573=CARTESIAN_POINT('Ctrl Pts',(-15.8791496788685,-18.0205781695773,
0.));
#230574=CARTESIAN_POINT('Ctrl Pts',(-15.8980864711043,-18.0308254604638,
0.));
#230575=CARTESIAN_POINT('Ctrl Pts',(-15.9171376582436,-18.0410708624208,
0.));
#230576=CARTESIAN_POINT('Ctrl Pts',(-15.9363027723244,-18.0513136910691,
0.));
#230577=CARTESIAN_POINT('Ctrl Pts',(-15.9555813490645,-18.061553270236,
0.));
#230578=CARTESIAN_POINT('Ctrl Pts',(-15.9749729277848,-18.071788931796,
0.));
#230579=CARTESIAN_POINT('Ctrl Pts',(-15.9944770513616,-18.0820200155238,
0.));
#230580=CARTESIAN_POINT('Ctrl Pts',(-16.0140932661612,-18.0922458689464,
0.));
#230581=CARTESIAN_POINT('Ctrl Pts',(-16.0338211219694,-18.1024658471966,
0.));
#230582=CARTESIAN_POINT('Ctrl Pts',(-16.0536601719124,-18.1126793128688,
0.));
#230583=CARTESIAN_POINT('Ctrl Pts',(-16.0736099723665,-18.1228856358746,
0.));
#230584=CARTESIAN_POINT('Ctrl Pts',(-16.0936700829108,-18.1330841933099,
0.));
#230585=CARTESIAN_POINT('Ctrl Pts',(-16.1138400662791,-18.1432743693231,
0.));
#230586=CARTESIAN_POINT('Ctrl Pts',(-16.1341194882987,-18.153455554985,
0.));
#230587=CARTESIAN_POINT('Ctrl Pts',(-16.1545079178261,-18.1636271481616,
0.));
#230588=CARTESIAN_POINT('Ctrl Pts',(-16.1750049266673,-18.1737885533852,
0.));
#230589=CARTESIAN_POINT('Ctrl Pts',(-16.1956100895076,-18.1839391817335,
0.));
#230590=CARTESIAN_POINT('Ctrl Pts',(-16.2163229838878,-18.1940784507232,
0.));
#230591=CARTESIAN_POINT('Ctrl Pts',(-16.237143190164,-18.2042057842037,
0.));
#230592=CARTESIAN_POINT('Ctrl Pts',(-16.2580702914615,-18.214320612253,
0.));
#230593=CARTESIAN_POINT('Ctrl Pts',(-16.2791038736223,-18.2244223710745,
0.));
#230594=CARTESIAN_POINT('Ctrl Pts',(-16.3002435251378,-18.2345105028981,
0.));
#230595=CARTESIAN_POINT('Ctrl Pts',(-16.3214888370988,-18.2445844558742,
0.));
#230596=CARTESIAN_POINT('Ctrl Pts',(-16.342839403159,-18.2546436839609,
0.));
#230597=CARTESIAN_POINT('Ctrl Pts',(-16.3642948194869,-18.2646876468169,
0.));
#230598=CARTESIAN_POINT('Ctrl Pts',(-16.385854684708,-18.2747158096934,
0.));
#230599=CARTESIAN_POINT('Ctrl Pts',(-16.4075185998454,-18.2847276433308,
0.));
#230600=CARTESIAN_POINT('Ctrl Pts',(-16.4292861682377,-18.2947226238509,
0.));
#230601=CARTESIAN_POINT('Ctrl Pts',(-16.4511569955231,-18.3047002326858,
0.));
#230602=CARTESIAN_POINT('Ctrl Pts',(-16.4731306896439,-18.3146599565229,
0.));
#230603=CARTESIAN_POINT('Ctrl Pts',(-16.4952068608344,-18.3246012872468,
0.));
#230604=CARTESIAN_POINT('Ctrl Pts',(-16.5173851216045,-18.3345237218864,
0.));
#230605=CARTESIAN_POINT('Ctrl Pts',(-16.539665086714,-18.3444267625601,
0.));
#230606=CARTESIAN_POINT('Ctrl Pts',(-16.5620463731414,-18.3543099164331,
0.));
#230607=CARTESIAN_POINT('Ctrl Pts',(-16.5845286000219,-18.364172695589,
0.));
#230608=CARTESIAN_POINT('Ctrl Pts',(-16.6071113885711,-18.3740146168879,
0.));
#230609=CARTESIAN_POINT('Ctrl Pts',(-16.6297943620056,-18.3838352018327,
0.));
#230610=CARTESIAN_POINT('Ctrl Pts',(-16.6525771454513,-18.3936339764332,
0.));
#230611=CARTESIAN_POINT('Ctrl Pts',(-16.6754593658513,-18.4034104710789,
0.));
#230612=CARTESIAN_POINT('Ctrl Pts',(-16.698440651849,-18.4131642203989,
0.));
#230613=CARTESIAN_POINT('Ctrl Pts',(-16.7215206338818,-18.4228947633186,
0.));
#230614=CARTESIAN_POINT('Ctrl Pts',(-16.7446989442882,-18.4326016431392,
0.));
#230615=CARTESIAN_POINT('Ctrl Pts',(-16.7679752173992,-18.4422844076099,
0.));
#230616=CARTESIAN_POINT('Ctrl Pts',(-16.791349089629,-18.4519426090124,
0.));
#230617=CARTESIAN_POINT('Ctrl Pts',(-16.8148201995472,-18.4615758042305,
0.));
#230618=CARTESIAN_POINT('Ctrl Pts',(-16.8383881879707,-18.4711835548622,
0.));
#230619=CARTESIAN_POINT('Ctrl Pts',(-16.8620526977169,-18.4807654268769,
0.));
#230620=CARTESIAN_POINT('Ctrl Pts',(-16.8858133733086,-18.4903209902226,
0.));
#230621=CARTESIAN_POINT('Ctrl Pts',(-16.9096698606942,-18.4998498184619,
0.));
#230622=CARTESIAN_POINT('Ctrl Pts',(-16.9336218069353,-18.5093514883835,
0.));
#230623=CARTESIAN_POINT('Ctrl Pts',(-16.957668859934,-18.518825579666,0.));
#230624=CARTESIAN_POINT('Ctrl Pts',(-16.9818106680382,-18.5282716744198,
0.));
#230625=CARTESIAN_POINT('Ctrl Pts',(-17.0060468805099,-18.5376893576961,
0.));
#230626=CARTESIAN_POINT('Ctrl Pts',(-17.030377148174,-18.5470782182089,
0.));
#230627=CARTESIAN_POINT('Ctrl Pts',(-17.0548011239751,-18.5564378489628,
0.));
#230628=CARTESIAN_POINT('Ctrl Pts',(-17.0793184636079,-18.5657678479788,
0.));
#230629=CARTESIAN_POINT('Ctrl Pts',(-17.1039288260002,-18.5750678188543,
0.));
#230630=CARTESIAN_POINT('Ctrl Pts',(-17.1286318741185,-18.5843373717253,
0.));
#230631=CARTESIAN_POINT('Ctrl Pts',(-17.1534272741646,-18.5935761222833,
0.));
#230632=CARTESIAN_POINT('Ctrl Pts',(-17.1783146940131,-18.6027836898826,
0.));
#230633=CARTESIAN_POINT('Ctrl Pts',(-17.2032938019288,-18.6119596959957,
0.));
#230634=CARTESIAN_POINT('Ctrl Pts',(-17.2283642650519,-18.6211037624041,
0.));
#230635=CARTESIAN_POINT('Ctrl Pts',(-17.2535257482186,-18.630215509794,
0.));
#230636=CARTESIAN_POINT('Ctrl Pts',(-17.278777912021,-18.639294555474,0.));
#230637=CARTESIAN_POINT('Ctrl Pts',(-17.3041204135069,-18.6483405141853,
0.));
#230638=CARTESIAN_POINT('Ctrl Pts',(-17.3295529098612,-18.6573530024019,
0.));
#230639=CARTESIAN_POINT('Ctrl Pts',(-17.3550750612438,-18.6663316416569,
0.));
#230640=CARTESIAN_POINT('Ctrl Pts',(-17.3806865340744,-18.6752760624045,
0.));
#230641=CARTESIAN_POINT('Ctrl Pts',(-17.4063870038563,-18.6841859073472,
0.));
#230642=CARTESIAN_POINT('Ctrl Pts',(-17.4321761588148,-18.6930608357421,
0.));
#230643=CARTESIAN_POINT('Ctrl Pts',(-17.4580537012764,-18.7019005250322,
0.));
#230644=CARTESIAN_POINT('Ctrl Pts',(-17.4840193397176,-18.7107046613941,
0.));
#230645=CARTESIAN_POINT('Ctrl Pts',(-17.5100727820891,-18.7194729318127,
0.));
#230646=CARTESIAN_POINT('Ctrl Pts',(-17.5362137287604,-18.728205015716,
0.));
#230647=CARTESIAN_POINT('Ctrl Pts',(-17.5624418653248,-18.7369005764558,
0.));
#230648=CARTESIAN_POINT('Ctrl Pts',(-17.5887568561361,-18.7455592536667,
0.));
#230649=CARTESIAN_POINT('Ctrl Pts',(-17.6151583356989,-18.7541806530935,
0.));
#230650=CARTESIAN_POINT('Ctrl Pts',(-17.6416459210646,-18.7627643613138,
0.));
#230651=CARTESIAN_POINT('Ctrl Pts',(-17.6682192274197,-18.7713099642673,
0.));
#230652=CARTESIAN_POINT('Ctrl Pts',(-17.6948778822982,-18.7798170641305,
0.));
#230653=CARTESIAN_POINT('Ctrl Pts',(-17.7216215409019,-18.7882852976016,
0.));
#230654=CARTESIAN_POINT('Ctrl Pts',(-17.7484498996917,-18.7967143519444,
0.));
#230655=CARTESIAN_POINT('Ctrl Pts',(-17.7753627137898,-18.8051039860543,
0.));
#230656=CARTESIAN_POINT('Ctrl Pts',(-17.8023598011135,-18.8134540340581,
0.));
#230657=CARTESIAN_POINT('Ctrl Pts',(-17.8294410311105,-18.8217643886368,
0.));
#230658=CARTESIAN_POINT('Ctrl Pts',(-17.8566063174871,-18.8300349896187,
0.));
#230659=CARTESIAN_POINT('Ctrl Pts',(-17.8784057509434,-18.8366196462746,
0.));
#230660=CARTESIAN_POINT('Ctrl Pts',(-17.8947931177853,-18.8415402351882,
0.));
#230661=CARTESIAN_POINT('Ctrl Pts',(-17.9057348246611,-18.8448126709726,
0.));
#230662=CARTESIAN_POINT('Ctrl Pts',(-17.9112098770111,-18.8464468996588,
0.));
#230663=CARTESIAN_POINT('',(-17.9112098770111,-18.8464468996588,12.));
#230664=CARTESIAN_POINT('Ctrl Pts',(-17.9112098770111,-18.8464468996588,
12.));
#230665=CARTESIAN_POINT('Ctrl Pts',(-17.9057348246611,-18.8448126709726,
12.));
#230666=CARTESIAN_POINT('Ctrl Pts',(-17.8947931177853,-18.8415402351882,
12.));
#230667=CARTESIAN_POINT('Ctrl Pts',(-17.8784057509434,-18.8366196462746,
12.));
#230668=CARTESIAN_POINT('Ctrl Pts',(-17.8566063174871,-18.8300349896187,
12.));
#230669=CARTESIAN_POINT('Ctrl Pts',(-17.8294410311105,-18.8217643886368,
12.));
#230670=CARTESIAN_POINT('Ctrl Pts',(-17.8023598011135,-18.8134540340581,
12.));
#230671=CARTESIAN_POINT('Ctrl Pts',(-17.7753627137898,-18.8051039860543,
12.));
#230672=CARTESIAN_POINT('Ctrl Pts',(-17.7484498996917,-18.7967143519444,
12.));
#230673=CARTESIAN_POINT('Ctrl Pts',(-17.7216215409019,-18.7882852976016,
12.));
#230674=CARTESIAN_POINT('Ctrl Pts',(-17.6948778822982,-18.7798170641305,
12.));
#230675=CARTESIAN_POINT('Ctrl Pts',(-17.6682192274197,-18.7713099642673,
12.));
#230676=CARTESIAN_POINT('Ctrl Pts',(-17.6416459210646,-18.7627643613138,
12.));
#230677=CARTESIAN_POINT('Ctrl Pts',(-17.6151583356989,-18.7541806530935,
12.));
#230678=CARTESIAN_POINT('Ctrl Pts',(-17.5887568561361,-18.7455592536667,
12.));
#230679=CARTESIAN_POINT('Ctrl Pts',(-17.5624418653248,-18.7369005764558,
12.));
#230680=CARTESIAN_POINT('Ctrl Pts',(-17.5362137287604,-18.728205015716,
12.));
#230681=CARTESIAN_POINT('Ctrl Pts',(-17.5100727820891,-18.7194729318127,
12.));
#230682=CARTESIAN_POINT('Ctrl Pts',(-17.4840193397176,-18.7107046613941,
12.));
#230683=CARTESIAN_POINT('Ctrl Pts',(-17.4580537012764,-18.7019005250322,
12.));
#230684=CARTESIAN_POINT('Ctrl Pts',(-17.4321761588148,-18.6930608357421,
12.));
#230685=CARTESIAN_POINT('Ctrl Pts',(-17.4063870038563,-18.6841859073472,
12.));
#230686=CARTESIAN_POINT('Ctrl Pts',(-17.3806865340744,-18.6752760624045,
12.));
#230687=CARTESIAN_POINT('Ctrl Pts',(-17.3550750612438,-18.6663316416569,
12.));
#230688=CARTESIAN_POINT('Ctrl Pts',(-17.3295529098612,-18.6573530024019,
12.));
#230689=CARTESIAN_POINT('Ctrl Pts',(-17.3041204135069,-18.6483405141853,
12.));
#230690=CARTESIAN_POINT('Ctrl Pts',(-17.278777912021,-18.639294555474,12.));
#230691=CARTESIAN_POINT('Ctrl Pts',(-17.2535257482186,-18.630215509794,
12.));
#230692=CARTESIAN_POINT('Ctrl Pts',(-17.2283642650519,-18.6211037624041,
12.));
#230693=CARTESIAN_POINT('Ctrl Pts',(-17.2032938019288,-18.6119596959957,
12.));
#230694=CARTESIAN_POINT('Ctrl Pts',(-17.1783146940131,-18.6027836898826,
12.));
#230695=CARTESIAN_POINT('Ctrl Pts',(-17.1534272741646,-18.5935761222833,
12.));
#230696=CARTESIAN_POINT('Ctrl Pts',(-17.1286318741185,-18.5843373717253,
12.));
#230697=CARTESIAN_POINT('Ctrl Pts',(-17.1039288260002,-18.5750678188543,
12.));
#230698=CARTESIAN_POINT('Ctrl Pts',(-17.0793184636079,-18.5657678479788,
12.));
#230699=CARTESIAN_POINT('Ctrl Pts',(-17.0548011239751,-18.5564378489628,
12.));
#230700=CARTESIAN_POINT('Ctrl Pts',(-17.030377148174,-18.5470782182089,
12.));
#230701=CARTESIAN_POINT('Ctrl Pts',(-17.0060468805099,-18.5376893576961,
12.));
#230702=CARTESIAN_POINT('Ctrl Pts',(-16.9818106680382,-18.5282716744198,
12.));
#230703=CARTESIAN_POINT('Ctrl Pts',(-16.957668859934,-18.518825579666,12.));
#230704=CARTESIAN_POINT('Ctrl Pts',(-16.9336218069353,-18.5093514883835,
12.));
#230705=CARTESIAN_POINT('Ctrl Pts',(-16.9096698606942,-18.4998498184619,
12.));
#230706=CARTESIAN_POINT('Ctrl Pts',(-16.8858133733086,-18.4903209902226,
12.));
#230707=CARTESIAN_POINT('Ctrl Pts',(-16.8620526977169,-18.4807654268769,
12.));
#230708=CARTESIAN_POINT('Ctrl Pts',(-16.8383881879707,-18.4711835548622,
12.));
#230709=CARTESIAN_POINT('Ctrl Pts',(-16.8148201995472,-18.4615758042305,
12.));
#230710=CARTESIAN_POINT('Ctrl Pts',(-16.791349089629,-18.4519426090124,
12.));
#230711=CARTESIAN_POINT('Ctrl Pts',(-16.7679752173992,-18.4422844076099,
12.));
#230712=CARTESIAN_POINT('Ctrl Pts',(-16.7446989442882,-18.4326016431392,
12.));
#230713=CARTESIAN_POINT('Ctrl Pts',(-16.7215206338818,-18.4228947633186,
12.));
#230714=CARTESIAN_POINT('Ctrl Pts',(-16.698440651849,-18.4131642203989,
12.));
#230715=CARTESIAN_POINT('Ctrl Pts',(-16.6754593658513,-18.4034104710789,
12.));
#230716=CARTESIAN_POINT('Ctrl Pts',(-16.6525771454513,-18.3936339764332,
12.));
#230717=CARTESIAN_POINT('Ctrl Pts',(-16.6297943620056,-18.3838352018327,
12.));
#230718=CARTESIAN_POINT('Ctrl Pts',(-16.6071113885711,-18.3740146168879,
12.));
#230719=CARTESIAN_POINT('Ctrl Pts',(-16.5845286000219,-18.364172695589,
12.));
#230720=CARTESIAN_POINT('Ctrl Pts',(-16.5620463731414,-18.3543099164331,
12.));
#230721=CARTESIAN_POINT('Ctrl Pts',(-16.539665086714,-18.3444267625601,
12.));
#230722=CARTESIAN_POINT('Ctrl Pts',(-16.5173851216045,-18.3345237218864,
12.));
#230723=CARTESIAN_POINT('Ctrl Pts',(-16.4952068608344,-18.3246012872468,
12.));
#230724=CARTESIAN_POINT('Ctrl Pts',(-16.4731306896439,-18.3146599565229,
12.));
#230725=CARTESIAN_POINT('Ctrl Pts',(-16.4511569955231,-18.3047002326858,
12.));
#230726=CARTESIAN_POINT('Ctrl Pts',(-16.4292861682377,-18.2947226238509,
12.));
#230727=CARTESIAN_POINT('Ctrl Pts',(-16.4075185998454,-18.2847276433308,
12.));
#230728=CARTESIAN_POINT('Ctrl Pts',(-16.385854684708,-18.2747158096934,
12.));
#230729=CARTESIAN_POINT('Ctrl Pts',(-16.3642948194869,-18.2646876468169,
12.));
#230730=CARTESIAN_POINT('Ctrl Pts',(-16.342839403159,-18.2546436839609,
12.));
#230731=CARTESIAN_POINT('Ctrl Pts',(-16.3214888370988,-18.2445844558742,
12.));
#230732=CARTESIAN_POINT('Ctrl Pts',(-16.3002435251378,-18.2345105028981,
12.));
#230733=CARTESIAN_POINT('Ctrl Pts',(-16.2791038736223,-18.2244223710745,
12.));
#230734=CARTESIAN_POINT('Ctrl Pts',(-16.2580702914615,-18.214320612253,
12.));
#230735=CARTESIAN_POINT('Ctrl Pts',(-16.237143190164,-18.2042057842037,
12.));
#230736=CARTESIAN_POINT('Ctrl Pts',(-16.2163229838878,-18.1940784507232,
12.));
#230737=CARTESIAN_POINT('Ctrl Pts',(-16.1956100895076,-18.1839391817335,
12.));
#230738=CARTESIAN_POINT('Ctrl Pts',(-16.1750049266673,-18.1737885533852,
12.));
#230739=CARTESIAN_POINT('Ctrl Pts',(-16.1545079178261,-18.1636271481616,
12.));
#230740=CARTESIAN_POINT('Ctrl Pts',(-16.1341194882987,-18.153455554985,
12.));
#230741=CARTESIAN_POINT('Ctrl Pts',(-16.1138400662791,-18.1432743693231,
12.));
#230742=CARTESIAN_POINT('Ctrl Pts',(-16.0936700829108,-18.1330841933099,
12.));
#230743=CARTESIAN_POINT('Ctrl Pts',(-16.0736099723665,-18.1228856358746,
12.));
#230744=CARTESIAN_POINT('Ctrl Pts',(-16.0536601719124,-18.1126793128688,
12.));
#230745=CARTESIAN_POINT('Ctrl Pts',(-16.0338211219694,-18.1024658471966,
12.));
#230746=CARTESIAN_POINT('Ctrl Pts',(-16.0140932661612,-18.0922458689464,
12.));
#230747=CARTESIAN_POINT('Ctrl Pts',(-15.9944770513616,-18.0820200155238,
12.));
#230748=CARTESIAN_POINT('Ctrl Pts',(-15.9749729277848,-18.071788931796,
12.));
#230749=CARTESIAN_POINT('Ctrl Pts',(-15.9555813490645,-18.061553270236,
12.));
#230750=CARTESIAN_POINT('Ctrl Pts',(-15.9363027723244,-18.0513136910691,
12.));
#230751=CARTESIAN_POINT('Ctrl Pts',(-15.9171376582436,-18.0410708624208,
12.));
#230752=CARTESIAN_POINT('Ctrl Pts',(-15.8980864711043,-18.0308254604638,
12.));
#230753=CARTESIAN_POINT('Ctrl Pts',(-15.8791496788685,-18.0205781695773,
12.));
#230754=CARTESIAN_POINT('Ctrl Pts',(-15.8603277532834,-18.010329682521,
12.));
#230755=CARTESIAN_POINT('Ctrl Pts',(-15.8416211699682,-18.0000807006055,
12.));
#230756=CARTESIAN_POINT('Ctrl Pts',(-15.8230304084963,-17.9898319338664,
12.));
#230757=CARTESIAN_POINT('Ctrl Pts',(-15.8045559524674,-17.9795841012383,
12.));
#230758=CARTESIAN_POINT('Ctrl Pts',(-15.786198289572,-17.9693379307297,
12.));
#230759=CARTESIAN_POINT('Ctrl Pts',(-15.7679579117072,-17.9590941596236,
12.));
#230760=CARTESIAN_POINT('Ctrl Pts',(-15.7498353150856,-17.9488535346776,
12.));
#230761=CARTESIAN_POINT('Ctrl Pts',(-15.7318310003334,-17.9386168123261,
12.));
#230762=CARTESIAN_POINT('Ctrl Pts',(-15.713945472584,-17.9283847588837,
12.));
#230763=CARTESIAN_POINT('Ctrl Pts',(-15.6961792415526,-17.918158150746,
12.));
#230764=CARTESIAN_POINT('Ctrl Pts',(-15.6785328216467,-17.9079377746118,
12.));
#230765=CARTESIAN_POINT('Ctrl Pts',(-15.6610067321036,-17.8977244277247,
12.));
#230766=CARTESIAN_POINT('Ctrl Pts',(-15.6436014971088,-17.8875189181095,
12.));
#230767=CARTESIAN_POINT('Ctrl Pts',(-15.6263176459107,-17.8773220648125,
12.));
#230768=CARTESIAN_POINT('Ctrl Pts',(-15.6091557129205,-17.8671346981388,
12.));
#230769=CARTESIAN_POINT('Ctrl Pts',(-15.5921162378183,-17.8569576598996,
12.));
#230770=CARTESIAN_POINT('Ctrl Pts',(-15.5751997657154,-17.8467918036976,
12.));
#230771=CARTESIAN_POINT('Ctrl Pts',(-15.5584068472976,-17.8366379952078,
12.));
#230772=CARTESIAN_POINT('Ctrl Pts',(-15.5417380389639,-17.8264971124606,
12.));
#230773=CARTESIAN_POINT('Ctrl Pts',(-15.5251939029558,-17.8163700461262,
12.));
#230774=CARTESIAN_POINT('Ctrl Pts',(-15.5087750074728,-17.8062576997964,
12.));
#230775=CARTESIAN_POINT('Ctrl Pts',(-15.4924819268529,-17.7961609903161,
12.));
#230776=CARTESIAN_POINT('Ctrl Pts',(-15.4763152417506,-17.7860808481229,
12.));
#230777=CARTESIAN_POINT('Ctrl Pts',(-15.460275539302,-17.7760182175817,
12.));
#230778=CARTESIAN_POINT('Ctrl Pts',(-15.4443634132865,-17.765974057326,
12.));
#230779=CARTESIAN_POINT('Ctrl Pts',(-15.4285794642658,-17.7559493405871,
12.));
#230780=CARTESIAN_POINT('Ctrl Pts',(-15.4129242997828,-17.7459450555803,
12.));
#230781=CARTESIAN_POINT('Ctrl Pts',(-15.3973985345796,-17.7359622059143,
12.));
#230782=CARTESIAN_POINT('Ctrl Pts',(-15.3820027907965,-17.7260018109923,
12.));
#230783=CARTESIAN_POINT('Ctrl Pts',(-15.3667376981702,-17.7160649064208,
12.));
#230784=CARTESIAN_POINT('Ctrl Pts',(-15.3516038942064,-17.7061525444044,
12.));
#230785=CARTESIAN_POINT('Ctrl Pts',(-15.3366020244069,-17.6962657941984,
12.));
#230786=CARTESIAN_POINT('Ctrl Pts',(-15.3217327425341,-17.6864057426052,
12.));
#230787=CARTESIAN_POINT('Ctrl Pts',(-15.3069967108501,-17.6765734944559,
12.));
#230788=CARTESIAN_POINT('Ctrl Pts',(-15.2923946003598,-17.6667701731041,
12.));
#230789=CARTESIAN_POINT('Ctrl Pts',(-15.2779270910238,-17.6569969209,12.));
#230790=CARTESIAN_POINT('Ctrl Pts',(-15.263594872029,-17.6472548997329,
12.));
#230791=CARTESIAN_POINT('Ctrl Pts',(-15.2493986421091,-17.637545291637,
12.));
#230792=CARTESIAN_POINT('Ctrl Pts',(-15.2353391098367,-17.6278692993765,
12.));
#230793=CARTESIAN_POINT('Ctrl Pts',(-15.22141699392,-17.6182281470467,12.));
#230794=CARTESIAN_POINT('Ctrl Pts',(-15.2076330234686,-17.6086230806497,
12.));
#230795=CARTESIAN_POINT('Ctrl Pts',(-15.1939879383268,-17.5990553687595,
12.));
#230796=CARTESIAN_POINT('Ctrl Pts',(-15.1804824894605,-17.5895263032592,
12.));
#230797=CARTESIAN_POINT('Ctrl Pts',(-15.1671174393137,-17.5800372000539,
12.));
#230798=CARTESIAN_POINT('Ctrl Pts',(-15.1538935621715,-17.570589399803,
12.));
#230799=CARTESIAN_POINT('Ctrl Pts',(-15.1408116444877,-17.5611842686196,
12.));
#230800=CARTESIAN_POINT('Ctrl Pts',(-15.127872485314,-17.5518231989122,
12.));
#230801=CARTESIAN_POINT('Ctrl Pts',(-15.1150768967729,-17.5425076102966,
12.));
#230802=CARTESIAN_POINT('Ctrl Pts',(-15.1024257045033,-17.5332389504829,
12.));
#230803=CARTESIAN_POINT('Ctrl Pts',(-15.0899197481082,-17.5240186961788,
12.));
#230804=CARTESIAN_POINT('Ctrl Pts',(-15.0775598815748,-17.5148483539683,
12.));
#230805=CARTESIAN_POINT('Ctrl Pts',(-15.0653469738306,-17.5057294613874,
12.));
#230806=CARTESIAN_POINT('Ctrl Pts',(-15.0532819093085,-17.4966635880245,
12.));
#230807=CARTESIAN_POINT('Ctrl Pts',(-15.0413655884993,-17.4876523366178,
12.));
#230808=CARTESIAN_POINT('Ctrl Pts',(-15.029598928488,-17.4786973441417,
12.));
#230809=CARTESIAN_POINT('Ctrl Pts',(-15.0179828635086,-17.4698002829356,
12.));
#230810=CARTESIAN_POINT('Ctrl Pts',(-15.0065183456921,-17.4609628621418,
12.));
#230811=CARTESIAN_POINT('Ctrl Pts',(-14.9952063457778,-17.4521868291004,
12.));
#230812=CARTESIAN_POINT('Ctrl Pts',(-14.9840478538358,-17.4434739707773,
12.));
#230813=CARTESIAN_POINT('Ctrl Pts',(-14.9730438799452,-17.4348261151396,
12.));
#230814=CARTESIAN_POINT('Ctrl Pts',(-14.9621954549827,-17.426245132709,
12.));
#230815=CARTESIAN_POINT('Ctrl Pts',(-14.9515036315143,-17.4177329382828,
12.));
#230816=CARTESIAN_POINT('Ctrl Pts',(-14.940969484645,-17.4092914926071,
12.));
#230817=CARTESIAN_POINT('Ctrl Pts',(-14.9305941128757,-17.4009228040749,
12.));
#230818=CARTESIAN_POINT('Ctrl Pts',(-14.9203786389342,-17.3926289303986,
12.));
#230819=CARTESIAN_POINT('Ctrl Pts',(-14.9103242110058,-17.3844119809824,
12.));
#230820=CARTESIAN_POINT('Ctrl Pts',(-14.900432003961,-17.3762741193076,
12.));
#230821=CARTESIAN_POINT('Ctrl Pts',(-14.8907032205788,-17.3682175653235,
12.));
#230822=CARTESIAN_POINT('Ctrl Pts',(-14.8811390927423,-17.3602445978161,
12.));
#230823=CARTESIAN_POINT('Ctrl Pts',(-14.8717408826956,-17.3523575568645,
12.));
#230824=CARTESIAN_POINT('Ctrl Pts',(-14.8625098843417,-17.3445588463474,
12.));
#230825=CARTESIAN_POINT('Ctrl Pts',(-14.8534474245434,-17.336850936485,
12.));
#230826=CARTESIAN_POINT('Ctrl Pts',(-14.8445548643508,-17.3292363662605,
12.));
#230827=CARTESIAN_POINT('Ctrl Pts',(-14.8358336004197,-17.3217177462101,
12.));
#230828=CARTESIAN_POINT('Ctrl Pts',(-14.8272850675379,-17.3142977632659,
12.));
#230829=CARTESIAN_POINT('Ctrl Pts',(-14.8189107410162,-17.3069791853706,
12.));
#230830=CARTESIAN_POINT('Ctrl Pts',(-14.8107121391036,-17.299764866148,
12.));
#230831=CARTESIAN_POINT('Ctrl Pts',(-14.8026908254276,-17.2926577496513,
12.));
#230832=CARTESIAN_POINT('Ctrl Pts',(-14.7948484105249,-17.2856608733196,
12.));
#230833=CARTESIAN_POINT('Ctrl Pts',(-14.787186553128,-17.2787773704849,
12.));
#230834=CARTESIAN_POINT('Ctrl Pts',(-14.7797069617804,-17.2720104735194,
12.));
#230835=CARTESIAN_POINT('Ctrl Pts',(-14.7724113956731,-17.2653635155319,
12.));
#230836=CARTESIAN_POINT('Ctrl Pts',(-14.7653016697591,-17.2588399401465,
12.));
#230837=CARTESIAN_POINT('Ctrl Pts',(-14.7583796616617,-17.2524433146837,
12.));
#230838=CARTESIAN_POINT('Ctrl Pts',(-14.7516473175124,-17.2461773413288,
12.));
#230839=CARTESIAN_POINT('Ctrl Pts',(-14.7451066593792,-17.2400458713565,
12.));
#230840=CARTESIAN_POINT('Ctrl Pts',(-14.7387597858117,-17.2340529062076,
12.));
#230841=CARTESIAN_POINT('Ctrl Pts',(-14.7326088681163,-17.2282025904314,
12.));
#230842=CARTESIAN_POINT('Ctrl Pts',(-14.7266561494282,-17.2224992099666,
12.));
#230843=CARTESIAN_POINT('Ctrl Pts',(-14.7209039390327,-17.2169471814256,
12.));
#230844=CARTESIAN_POINT('Ctrl Pts',(-14.7153546289339,-17.2115510835989,
12.));
#230845=CARTESIAN_POINT('Ctrl Pts',(-14.7100107213586,-17.2063157097315,
12.));
#230846=CARTESIAN_POINT('Ctrl Pts',(-14.7048748502663,-17.2012461084268,
12.));
#230847=CARTESIAN_POINT('Ctrl Pts',(-14.699949811582,-17.1963476411694,
12.));
#230848=CARTESIAN_POINT('Ctrl Pts',(-14.6952385361706,-17.1916259308415,
12.));
#230849=CARTESIAN_POINT('Ctrl Pts',(-14.6907440526958,-17.1870867909918,
12.));
#230850=CARTESIAN_POINT('Ctrl Pts',(-14.686469452232,-17.1827361584719,
12.));
#230851=CARTESIAN_POINT('Ctrl Pts',(-14.6824178576167,-17.1785800350826,
12.));
#230852=CARTESIAN_POINT('Ctrl Pts',(-14.6785925615677,-17.1746247499056,
12.));
#230853=CARTESIAN_POINT('Ctrl Pts',(-14.6749971333867,-17.1708771619129,
12.));
#230854=CARTESIAN_POINT('Ctrl Pts',(-14.671635583332,-17.167344972302,12.));
#230855=CARTESIAN_POINT('Ctrl Pts',(-14.6685123374423,-17.1640366762305,
12.));
#230856=CARTESIAN_POINT('Ctrl Pts',(-14.6656319165057,-17.1609609517369,
12.));
#230857=CARTESIAN_POINT('Ctrl Pts',(-14.6629987285992,-17.1581262646789,
12.));
#230858=CARTESIAN_POINT('Ctrl Pts',(-14.6606167169642,-17.1555401986401,
12.));
#230859=CARTESIAN_POINT('Ctrl Pts',(-14.6584900555302,-17.1532107762718,
12.));
#230860=CARTESIAN_POINT('Ctrl Pts',(-14.6566237952435,-17.1511476869496,
12.));
#230861=CARTESIAN_POINT('Ctrl Pts',(-14.655024862281,-17.1493641837558,
12.));
#230862=CARTESIAN_POINT('Ctrl Pts',(-14.6537016966184,-17.147876394491,
12.));
#230863=CARTESIAN_POINT('Ctrl Pts',(-14.6526624064978,-17.1466998098673,
12.));
#230864=CARTESIAN_POINT('Ctrl Pts',(-14.6519131634508,-17.1458462295271,
12.));
#230865=CARTESIAN_POINT('Ctrl Pts',(-14.6515481598068,-17.1454262858043,
12.));
#230866=CARTESIAN_POINT('Ctrl Pts',(-14.6514066997196,-17.1452600887037,
12.));
#230867=CARTESIAN_POINT('Ctrl Pts',(-14.6513711852843,-17.1452153999142,
12.));
#230868=CARTESIAN_POINT('Ctrl Pts',(-14.6513681262571,-17.1452095830632,
12.));
#230869=CARTESIAN_POINT('',(-17.9112098770111,-18.8464468996588,0.));
#230870=CARTESIAN_POINT('Origin',(-17.7219872369693,-12.1729687575668,0.));
#230871=CARTESIAN_POINT('',(-18.5896416359912,-12.7689476255363,12.));
#230872=CARTESIAN_POINT('',(-8.86099361848466,-6.08648437878338,12.));
#230873=CARTESIAN_POINT('',(-18.5896416359912,-12.7689476255363,0.));
#230874=CARTESIAN_POINT('',(-18.5896416359912,-12.7689476255363,0.));
#230875=CARTESIAN_POINT('',(-8.86099361848466,-6.08648437878338,0.));
#230876=CARTESIAN_POINT('Ctrl Pts',(-18.8464468996588,-17.9112098770111,
0.));
#230877=CARTESIAN_POINT('Ctrl Pts',(-18.8464468996588,-17.9112098770111,
12.));
#230878=CARTESIAN_POINT('Ctrl Pts',(-18.8448126709692,-17.9057348246595,
0.));
#230879=CARTESIAN_POINT('Ctrl Pts',(-18.8448126709692,-17.9057348246595,
12.));
#230880=CARTESIAN_POINT('Ctrl Pts',(-18.8415402351786,-17.8947931177807,
0.));
#230881=CARTESIAN_POINT('Ctrl Pts',(-18.8415402351786,-17.8947931177807,
12.));
#230882=CARTESIAN_POINT('Ctrl Pts',(-18.8366196462581,-17.8784057509356,
0.));
#230883=CARTESIAN_POINT('Ctrl Pts',(-18.8366196462581,-17.8784057509356,
12.));
#230884=CARTESIAN_POINT('Ctrl Pts',(-18.8300349895974,-17.8566063174771,
0.));
#230885=CARTESIAN_POINT('Ctrl Pts',(-18.8300349895974,-17.8566063174771,
12.));
#230886=CARTESIAN_POINT('Ctrl Pts',(-18.8217643886157,-17.8294410311006,
0.));
#230887=CARTESIAN_POINT('Ctrl Pts',(-18.8217643886157,-17.8294410311006,
12.));
#230888=CARTESIAN_POINT('Ctrl Pts',(-18.8134540340417,-17.8023598011057,
0.));
#230889=CARTESIAN_POINT('Ctrl Pts',(-18.8134540340417,-17.8023598011057,
12.));
#230890=CARTESIAN_POINT('Ctrl Pts',(-18.8051039860448,-17.7753627137853,
0.));
#230891=CARTESIAN_POINT('Ctrl Pts',(-18.8051039860448,-17.7753627137853,
12.));
#230892=CARTESIAN_POINT('Ctrl Pts',(-18.7967143519419,-17.7484498996905,
0.));
#230893=CARTESIAN_POINT('Ctrl Pts',(-18.7967143519419,-17.7484498996905,
12.));
#230894=CARTESIAN_POINT('Ctrl Pts',(-18.788285297605,-17.7216215409035,
0.));
#230895=CARTESIAN_POINT('Ctrl Pts',(-18.788285297605,-17.7216215409035,
12.));
#230896=CARTESIAN_POINT('Ctrl Pts',(-18.7798170641374,-17.6948778823014,
0.));
#230897=CARTESIAN_POINT('Ctrl Pts',(-18.7798170641374,-17.6948778823014,
12.));
#230898=CARTESIAN_POINT('Ctrl Pts',(-18.7713099642754,-17.6682192274236,
0.));
#230899=CARTESIAN_POINT('Ctrl Pts',(-18.7713099642754,-17.6682192274236,
12.));
#230900=CARTESIAN_POINT('Ctrl Pts',(-18.762764361321,-17.6416459210681,
0.));
#230901=CARTESIAN_POINT('Ctrl Pts',(-18.762764361321,-17.6416459210681,
12.));
#230902=CARTESIAN_POINT('Ctrl Pts',(-18.7541806530984,-17.6151583357012,
0.));
#230903=CARTESIAN_POINT('Ctrl Pts',(-18.7541806530984,-17.6151583357012,
12.));
#230904=CARTESIAN_POINT('Ctrl Pts',(-18.7455592536687,-17.5887568561371,
0.));
#230905=CARTESIAN_POINT('Ctrl Pts',(-18.7455592536687,-17.5887568561371,
12.));
#230906=CARTESIAN_POINT('Ctrl Pts',(-18.7369005764553,-17.5624418653245,
0.));
#230907=CARTESIAN_POINT('Ctrl Pts',(-18.7369005764553,-17.5624418653245,
12.));
#230908=CARTESIAN_POINT('Ctrl Pts',(-18.7282050157138,-17.5362137287593,
0.));
#230909=CARTESIAN_POINT('Ctrl Pts',(-18.7282050157138,-17.5362137287593,
12.));
#230910=CARTESIAN_POINT('Ctrl Pts',(-18.7194729318098,-17.5100727820876,
0.));
#230911=CARTESIAN_POINT('Ctrl Pts',(-18.7194729318098,-17.5100727820876,
12.));
#230912=CARTESIAN_POINT('Ctrl Pts',(-18.7107046613912,-17.4840193397162,
0.));
#230913=CARTESIAN_POINT('Ctrl Pts',(-18.7107046613912,-17.4840193397162,
12.));
#230914=CARTESIAN_POINT('Ctrl Pts',(-18.70190052503,-17.4580537012753,0.));
#230915=CARTESIAN_POINT('Ctrl Pts',(-18.70190052503,-17.4580537012753,12.));
#230916=CARTESIAN_POINT('Ctrl Pts',(-18.6930608357409,-17.4321761588142,
0.));
#230917=CARTESIAN_POINT('Ctrl Pts',(-18.6930608357409,-17.4321761588142,
12.));
#230918=CARTESIAN_POINT('Ctrl Pts',(-18.6841859073471,-17.4063870038562,
0.));
#230919=CARTESIAN_POINT('Ctrl Pts',(-18.6841859073471,-17.4063870038562,
12.));
#230920=CARTESIAN_POINT('Ctrl Pts',(-18.6752760624052,-17.3806865340747,
0.));
#230921=CARTESIAN_POINT('Ctrl Pts',(-18.6752760624052,-17.3806865340747,
12.));
#230922=CARTESIAN_POINT('Ctrl Pts',(-18.6663316416582,-17.3550750612443,
0.));
#230923=CARTESIAN_POINT('Ctrl Pts',(-18.6663316416582,-17.3550750612443,
12.));
#230924=CARTESIAN_POINT('Ctrl Pts',(-18.6573530024033,-17.3295529098618,
0.));
#230925=CARTESIAN_POINT('Ctrl Pts',(-18.6573530024033,-17.3295529098618,
12.));
#230926=CARTESIAN_POINT('Ctrl Pts',(-18.6483405141865,-17.3041204135074,
0.));
#230927=CARTESIAN_POINT('Ctrl Pts',(-18.6483405141865,-17.3041204135074,
12.));
#230928=CARTESIAN_POINT('Ctrl Pts',(-18.6392945554748,-17.2787779120213,
0.));
#230929=CARTESIAN_POINT('Ctrl Pts',(-18.6392945554748,-17.2787779120213,
12.));
#230930=CARTESIAN_POINT('Ctrl Pts',(-18.6302155097943,-17.2535257482187,
0.));
#230931=CARTESIAN_POINT('Ctrl Pts',(-18.6302155097943,-17.2535257482187,
12.));
#230932=CARTESIAN_POINT('Ctrl Pts',(-18.6211037624038,-17.2283642650518,
0.));
#230933=CARTESIAN_POINT('Ctrl Pts',(-18.6211037624038,-17.2283642650518,
12.));
#230934=CARTESIAN_POINT('Ctrl Pts',(-18.6119596959949,-17.2032938019284,
0.));
#230935=CARTESIAN_POINT('Ctrl Pts',(-18.6119596959949,-17.2032938019284,
12.));
#230936=CARTESIAN_POINT('Ctrl Pts',(-18.6027836898817,-17.1783146940127,
0.));
#230937=CARTESIAN_POINT('Ctrl Pts',(-18.6027836898817,-17.1783146940127,
12.));
#230938=CARTESIAN_POINT('Ctrl Pts',(-18.5935761222825,-17.1534272741643,
0.));
#230939=CARTESIAN_POINT('Ctrl Pts',(-18.5935761222825,-17.1534272741643,
12.));
#230940=CARTESIAN_POINT('Ctrl Pts',(-18.5843373717247,-17.1286318741183,
0.));
#230941=CARTESIAN_POINT('Ctrl Pts',(-18.5843373717247,-17.1286318741183,
12.));
#230942=CARTESIAN_POINT('Ctrl Pts',(-18.5750678188542,-17.1039288260001,
0.));
#230943=CARTESIAN_POINT('Ctrl Pts',(-18.5750678188542,-17.1039288260001,
12.));
#230944=CARTESIAN_POINT('Ctrl Pts',(-18.5657678479789,-17.0793184636079,
0.));
#230945=CARTESIAN_POINT('Ctrl Pts',(-18.5657678479789,-17.0793184636079,
12.));
#230946=CARTESIAN_POINT('Ctrl Pts',(-18.556437848963,-17.0548011239751,
0.));
#230947=CARTESIAN_POINT('Ctrl Pts',(-18.556437848963,-17.0548011239751,
12.));
#230948=CARTESIAN_POINT('Ctrl Pts',(-18.547078218209,-17.0303771481738,
0.));
#230949=CARTESIAN_POINT('Ctrl Pts',(-18.547078218209,-17.0303771481738,
12.));
#230950=CARTESIAN_POINT('Ctrl Pts',(-18.5376893576961,-17.0060468805097,
0.));
#230951=CARTESIAN_POINT('Ctrl Pts',(-18.5376893576961,-17.0060468805097,
12.));
#230952=CARTESIAN_POINT('Ctrl Pts',(-18.5282716744197,-16.981810668038,
0.));
#230953=CARTESIAN_POINT('Ctrl Pts',(-18.5282716744197,-16.981810668038,
12.));
#230954=CARTESIAN_POINT('Ctrl Pts',(-18.5188255796659,-16.9576688599339,
0.));
#230955=CARTESIAN_POINT('Ctrl Pts',(-18.5188255796659,-16.9576688599339,
12.));
#230956=CARTESIAN_POINT('Ctrl Pts',(-18.5093514883835,-16.9336218069353,
0.));
#230957=CARTESIAN_POINT('Ctrl Pts',(-18.5093514883835,-16.9336218069353,
12.));
#230958=CARTESIAN_POINT('Ctrl Pts',(-18.499849818462,-16.9096698606943,
0.));
#230959=CARTESIAN_POINT('Ctrl Pts',(-18.499849818462,-16.9096698606943,
12.));
#230960=CARTESIAN_POINT('Ctrl Pts',(-18.4903209902227,-16.8858133733088,
0.));
#230961=CARTESIAN_POINT('Ctrl Pts',(-18.4903209902227,-16.8858133733088,
12.));
#230962=CARTESIAN_POINT('Ctrl Pts',(-18.4807654268771,-16.8620526977171,
0.));
#230963=CARTESIAN_POINT('Ctrl Pts',(-18.4807654268771,-16.8620526977171,
12.));
#230964=CARTESIAN_POINT('Ctrl Pts',(-18.4711835548623,-16.8383881879709,
0.));
#230965=CARTESIAN_POINT('Ctrl Pts',(-18.4711835548623,-16.8383881879709,
12.));
#230966=CARTESIAN_POINT('Ctrl Pts',(-18.4615758042305,-16.8148201995472,
0.));
#230967=CARTESIAN_POINT('Ctrl Pts',(-18.4615758042305,-16.8148201995472,
12.));
#230968=CARTESIAN_POINT('Ctrl Pts',(-18.4519426090124,-16.791349089629,
0.));
#230969=CARTESIAN_POINT('Ctrl Pts',(-18.4519426090124,-16.791349089629,
12.));
#230970=CARTESIAN_POINT('Ctrl Pts',(-18.44228440761,-16.7679752173992,0.));
#230971=CARTESIAN_POINT('Ctrl Pts',(-18.44228440761,-16.7679752173992,12.));
#230972=CARTESIAN_POINT('Ctrl Pts',(-18.4326016431392,-16.7446989442882,
0.));
#230973=CARTESIAN_POINT('Ctrl Pts',(-18.4326016431392,-16.7446989442882,
12.));
#230974=CARTESIAN_POINT('Ctrl Pts',(-18.4228947633187,-16.7215206338818,
0.));
#230975=CARTESIAN_POINT('Ctrl Pts',(-18.4228947633187,-16.7215206338818,
12.));
#230976=CARTESIAN_POINT('Ctrl Pts',(-18.413164220399,-16.6984406518491,
0.));
#230977=CARTESIAN_POINT('Ctrl Pts',(-18.413164220399,-16.6984406518491,
12.));
#230978=CARTESIAN_POINT('Ctrl Pts',(-18.403410471079,-16.6754593658513,
0.));
#230979=CARTESIAN_POINT('Ctrl Pts',(-18.403410471079,-16.6754593658513,
12.));
#230980=CARTESIAN_POINT('Ctrl Pts',(-18.3936339764332,-16.6525771454513,
0.));
#230981=CARTESIAN_POINT('Ctrl Pts',(-18.3936339764332,-16.6525771454513,
12.));
#230982=CARTESIAN_POINT('Ctrl Pts',(-18.3838352018327,-16.6297943620056,
0.));
#230983=CARTESIAN_POINT('Ctrl Pts',(-18.3838352018327,-16.6297943620056,
12.));
#230984=CARTESIAN_POINT('Ctrl Pts',(-18.3740146168879,-16.607111388571,
0.));
#230985=CARTESIAN_POINT('Ctrl Pts',(-18.3740146168879,-16.607111388571,
12.));
#230986=CARTESIAN_POINT('Ctrl Pts',(-18.3641726955889,-16.5845286000217,
0.));
#230987=CARTESIAN_POINT('Ctrl Pts',(-18.3641726955889,-16.5845286000217,
12.));
#230988=CARTESIAN_POINT('Ctrl Pts',(-18.354309916433,-16.5620463731413,
0.));
#230989=CARTESIAN_POINT('Ctrl Pts',(-18.354309916433,-16.5620463731413,
12.));
#230990=CARTESIAN_POINT('Ctrl Pts',(-18.34442676256,-16.5396650867139,0.));
#230991=CARTESIAN_POINT('Ctrl Pts',(-18.34442676256,-16.5396650867139,12.));
#230992=CARTESIAN_POINT('Ctrl Pts',(-18.3345237218864,-16.5173851216045,
0.));
#230993=CARTESIAN_POINT('Ctrl Pts',(-18.3345237218864,-16.5173851216045,
12.));
#230994=CARTESIAN_POINT('Ctrl Pts',(-18.3246012872469,-16.4952068608345,
0.));
#230995=CARTESIAN_POINT('Ctrl Pts',(-18.3246012872469,-16.4952068608345,
12.));
#230996=CARTESIAN_POINT('Ctrl Pts',(-18.3146599565231,-16.4731306896441,
0.));
#230997=CARTESIAN_POINT('Ctrl Pts',(-18.3146599565231,-16.4731306896441,
12.));
#230998=CARTESIAN_POINT('Ctrl Pts',(-18.304700232686,-16.4511569955233,
0.));
#230999=CARTESIAN_POINT('Ctrl Pts',(-18.304700232686,-16.4511569955233,
12.));
#231000=CARTESIAN_POINT('Ctrl Pts',(-18.294722623851,-16.4292861682379,
0.));
#231001=CARTESIAN_POINT('Ctrl Pts',(-18.294722623851,-16.4292861682379,
12.));
#231002=CARTESIAN_POINT('Ctrl Pts',(-18.2847276433309,-16.4075185998455,
0.));
#231003=CARTESIAN_POINT('Ctrl Pts',(-18.2847276433309,-16.4075185998455,
12.));
#231004=CARTESIAN_POINT('Ctrl Pts',(-18.2747158096934,-16.385854684708,
0.));
#231005=CARTESIAN_POINT('Ctrl Pts',(-18.2747158096934,-16.385854684708,
12.));
#231006=CARTESIAN_POINT('Ctrl Pts',(-18.2646876468169,-16.3642948194868,
0.));
#231007=CARTESIAN_POINT('Ctrl Pts',(-18.2646876468169,-16.3642948194868,
12.));
#231008=CARTESIAN_POINT('Ctrl Pts',(-18.2546436839608,-16.3428394031589,
0.));
#231009=CARTESIAN_POINT('Ctrl Pts',(-18.2546436839608,-16.3428394031589,
12.));
#231010=CARTESIAN_POINT('Ctrl Pts',(-18.2445844558742,-16.3214888370987,
0.));
#231011=CARTESIAN_POINT('Ctrl Pts',(-18.2445844558742,-16.3214888370987,
12.));
#231012=CARTESIAN_POINT('Ctrl Pts',(-18.2345105028982,-16.3002435251378,
0.));
#231013=CARTESIAN_POINT('Ctrl Pts',(-18.2345105028982,-16.3002435251378,
12.));
#231014=CARTESIAN_POINT('Ctrl Pts',(-18.2244223710746,-16.2791038736223,
0.));
#231015=CARTESIAN_POINT('Ctrl Pts',(-18.2244223710746,-16.2791038736223,
12.));
#231016=CARTESIAN_POINT('Ctrl Pts',(-18.2143206122529,-16.2580702914615,
0.));
#231017=CARTESIAN_POINT('Ctrl Pts',(-18.2143206122529,-16.2580702914615,
12.));
#231018=CARTESIAN_POINT('Ctrl Pts',(-18.2042057842035,-16.2371431901638,
0.));
#231019=CARTESIAN_POINT('Ctrl Pts',(-18.2042057842035,-16.2371431901638,
12.));
#231020=CARTESIAN_POINT('Ctrl Pts',(-18.1940784507229,-16.2163229838875,
0.));
#231021=CARTESIAN_POINT('Ctrl Pts',(-18.1940784507229,-16.2163229838875,
12.));
#231022=CARTESIAN_POINT('Ctrl Pts',(-18.1839391817331,-16.1956100895073,
0.));
#231023=CARTESIAN_POINT('Ctrl Pts',(-18.1839391817331,-16.1956100895073,
12.));
#231024=CARTESIAN_POINT('Ctrl Pts',(-18.1737885533849,-16.1750049266671,
0.));
#231025=CARTESIAN_POINT('Ctrl Pts',(-18.1737885533849,-16.1750049266671,
12.));
#231026=CARTESIAN_POINT('Ctrl Pts',(-18.1636271481615,-16.154507917826,
0.));
#231027=CARTESIAN_POINT('Ctrl Pts',(-18.1636271481615,-16.154507917826,
12.));
#231028=CARTESIAN_POINT('Ctrl Pts',(-18.1534555549852,-16.1341194882988,
0.));
#231029=CARTESIAN_POINT('Ctrl Pts',(-18.1534555549852,-16.1341194882988,
12.));
#231030=CARTESIAN_POINT('Ctrl Pts',(-18.1432743693235,-16.1138400662794,
0.));
#231031=CARTESIAN_POINT('Ctrl Pts',(-18.1432743693235,-16.1138400662794,
12.));
#231032=CARTESIAN_POINT('Ctrl Pts',(-18.1330841933105,-16.0936700829112,
0.));
#231033=CARTESIAN_POINT('Ctrl Pts',(-18.1330841933105,-16.0936700829112,
12.));
#231034=CARTESIAN_POINT('Ctrl Pts',(-18.1228856358751,-16.0736099723668,
0.));
#231035=CARTESIAN_POINT('Ctrl Pts',(-18.1228856358751,-16.0736099723668,
12.));
#231036=CARTESIAN_POINT('Ctrl Pts',(-18.112679312869,-16.0536601719126,
0.));
#231037=CARTESIAN_POINT('Ctrl Pts',(-18.112679312869,-16.0536601719126,
12.));
#231038=CARTESIAN_POINT('Ctrl Pts',(-18.1024658471966,-16.0338211219693,
0.));
#231039=CARTESIAN_POINT('Ctrl Pts',(-18.1024658471966,-16.0338211219693,
12.));
#231040=CARTESIAN_POINT('Ctrl Pts',(-18.0922458689462,-16.014093266161,
0.));
#231041=CARTESIAN_POINT('Ctrl Pts',(-18.0922458689462,-16.014093266161,
12.));
#231042=CARTESIAN_POINT('Ctrl Pts',(-18.0820200155236,-15.9944770513613,
0.));
#231043=CARTESIAN_POINT('Ctrl Pts',(-18.0820200155236,-15.9944770513613,
12.));
#231044=CARTESIAN_POINT('Ctrl Pts',(-18.0717889317958,-15.9749729277846,
0.));
#231045=CARTESIAN_POINT('Ctrl Pts',(-18.0717889317958,-15.9749729277846,
12.));
#231046=CARTESIAN_POINT('Ctrl Pts',(-18.061553270236,-15.9555813490644,
0.));
#231047=CARTESIAN_POINT('Ctrl Pts',(-18.061553270236,-15.9555813490644,
12.));
#231048=CARTESIAN_POINT('Ctrl Pts',(-18.0513136910691,-15.9363027723244,
0.));
#231049=CARTESIAN_POINT('Ctrl Pts',(-18.0513136910691,-15.9363027723244,
12.));
#231050=CARTESIAN_POINT('Ctrl Pts',(-18.0410708624208,-15.9171376582436,
0.));
#231051=CARTESIAN_POINT('Ctrl Pts',(-18.0410708624208,-15.9171376582436,
12.));
#231052=CARTESIAN_POINT('Ctrl Pts',(-18.0308254604636,-15.8980864711042,
0.));
#231053=CARTESIAN_POINT('Ctrl Pts',(-18.0308254604636,-15.8980864711042,
12.));
#231054=CARTESIAN_POINT('Ctrl Pts',(-18.0205781695769,-15.8791496788682,
0.));
#231055=CARTESIAN_POINT('Ctrl Pts',(-18.0205781695769,-15.8791496788682,
12.));
#231056=CARTESIAN_POINT('Ctrl Pts',(-18.0103296825205,-15.8603277532831,
0.));
#231057=CARTESIAN_POINT('Ctrl Pts',(-18.0103296825205,-15.8603277532831,
12.));
#231058=CARTESIAN_POINT('Ctrl Pts',(-18.0000807006052,-15.8416211699679,
0.));
#231059=CARTESIAN_POINT('Ctrl Pts',(-18.0000807006052,-15.8416211699679,
12.));
#231060=CARTESIAN_POINT('Ctrl Pts',(-17.9898319338664,-15.8230304084962,
0.));
#231061=CARTESIAN_POINT('Ctrl Pts',(-17.9898319338664,-15.8230304084962,
12.));
#231062=CARTESIAN_POINT('Ctrl Pts',(-17.9795841012386,-15.8045559524676,
0.));
#231063=CARTESIAN_POINT('Ctrl Pts',(-17.9795841012386,-15.8045559524676,
12.));
#231064=CARTESIAN_POINT('Ctrl Pts',(-17.9693379307303,-15.7861982895724,
0.));
#231065=CARTESIAN_POINT('Ctrl Pts',(-17.9693379307303,-15.7861982895724,
12.));
#231066=CARTESIAN_POINT('Ctrl Pts',(-17.9590941596242,-15.7679579117077,
0.));
#231067=CARTESIAN_POINT('Ctrl Pts',(-17.9590941596242,-15.7679579117077,
12.));
#231068=CARTESIAN_POINT('Ctrl Pts',(-17.9488535346781,-15.749835315086,
0.));
#231069=CARTESIAN_POINT('Ctrl Pts',(-17.9488535346781,-15.749835315086,
12.));
#231070=CARTESIAN_POINT('Ctrl Pts',(-17.9386168123262,-15.7318310003335,
0.));
#231071=CARTESIAN_POINT('Ctrl Pts',(-17.9386168123262,-15.7318310003335,
12.));
#231072=CARTESIAN_POINT('Ctrl Pts',(-17.9283847588836,-15.7139454725838,
0.));
#231073=CARTESIAN_POINT('Ctrl Pts',(-17.9283847588836,-15.7139454725838,
12.));
#231074=CARTESIAN_POINT('Ctrl Pts',(-17.9181581507455,-15.6961792415522,
0.));
#231075=CARTESIAN_POINT('Ctrl Pts',(-17.9181581507455,-15.6961792415522,
12.));
#231076=CARTESIAN_POINT('Ctrl Pts',(-17.9079377746111,-15.678532821646,
0.));
#231077=CARTESIAN_POINT('Ctrl Pts',(-17.9079377746111,-15.678532821646,
12.));
#231078=CARTESIAN_POINT('Ctrl Pts',(-17.897724427724,-15.661006732103,0.));
#231079=CARTESIAN_POINT('Ctrl Pts',(-17.897724427724,-15.661006732103,12.));
#231080=CARTESIAN_POINT('Ctrl Pts',(-17.8875189181091,-15.6436014971084,
0.));
#231081=CARTESIAN_POINT('Ctrl Pts',(-17.8875189181091,-15.6436014971084,
12.));
#231082=CARTESIAN_POINT('Ctrl Pts',(-17.8773220648125,-15.6263176459108,
0.));
#231083=CARTESIAN_POINT('Ctrl Pts',(-17.8773220648125,-15.6263176459108,
12.));
#231084=CARTESIAN_POINT('Ctrl Pts',(-17.8671346981394,-15.609155712921,
0.));
#231085=CARTESIAN_POINT('Ctrl Pts',(-17.8671346981394,-15.609155712921,
12.));
#231086=CARTESIAN_POINT('Ctrl Pts',(-17.8569576599006,-15.5921162378192,
0.));
#231087=CARTESIAN_POINT('Ctrl Pts',(-17.8569576599006,-15.5921162378192,
12.));
#231088=CARTESIAN_POINT('Ctrl Pts',(-17.8467918036987,-15.5751997657163,
0.));
#231089=CARTESIAN_POINT('Ctrl Pts',(-17.8467918036987,-15.5751997657163,
12.));
#231090=CARTESIAN_POINT('Ctrl Pts',(-17.8366379952085,-15.5584068472982,
0.));
#231091=CARTESIAN_POINT('Ctrl Pts',(-17.8366379952085,-15.5584068472982,
12.));
#231092=CARTESIAN_POINT('Ctrl Pts',(-17.8264971124607,-15.541738038964,
0.));
#231093=CARTESIAN_POINT('Ctrl Pts',(-17.8264971124607,-15.541738038964,
12.));
#231094=CARTESIAN_POINT('Ctrl Pts',(-17.8163700461256,-15.5251939029552,
0.));
#231095=CARTESIAN_POINT('Ctrl Pts',(-17.8163700461256,-15.5251939029552,
12.));
#231096=CARTESIAN_POINT('Ctrl Pts',(-17.8062576997952,-15.5087750074718,
0.));
#231097=CARTESIAN_POINT('Ctrl Pts',(-17.8062576997952,-15.5087750074718,
12.));
#231098=CARTESIAN_POINT('Ctrl Pts',(-17.7961609903148,-15.4924819268517,
0.));
#231099=CARTESIAN_POINT('Ctrl Pts',(-17.7961609903148,-15.4924819268517,
12.));
#231100=CARTESIAN_POINT('Ctrl Pts',(-17.786080848122,-15.4763152417497,
0.));
#231101=CARTESIAN_POINT('Ctrl Pts',(-17.786080848122,-15.4763152417497,
12.));
#231102=CARTESIAN_POINT('Ctrl Pts',(-17.7760182175815,-15.4602755393017,
0.));
#231103=CARTESIAN_POINT('Ctrl Pts',(-17.7760182175815,-15.4602755393017,
12.));
#231104=CARTESIAN_POINT('Ctrl Pts',(-17.7659740573265,-15.4443634132869,
0.));
#231105=CARTESIAN_POINT('Ctrl Pts',(-17.7659740573265,-15.4443634132869,
12.));
#231106=CARTESIAN_POINT('Ctrl Pts',(-17.7559493405881,-15.4285794642668,
0.));
#231107=CARTESIAN_POINT('Ctrl Pts',(-17.7559493405881,-15.4285794642668,
12.));
#231108=CARTESIAN_POINT('Ctrl Pts',(-17.7459450555812,-15.4129242997837,
0.));
#231109=CARTESIAN_POINT('Ctrl Pts',(-17.7459450555812,-15.4129242997837,
12.));
#231110=CARTESIAN_POINT('Ctrl Pts',(-17.735962205915,-15.3973985345802,
0.));
#231111=CARTESIAN_POINT('Ctrl Pts',(-17.735962205915,-15.3973985345802,
12.));
#231112=CARTESIAN_POINT('Ctrl Pts',(-17.7260018109924,-15.3820027907967,
0.));
#231113=CARTESIAN_POINT('Ctrl Pts',(-17.7260018109924,-15.3820027907967,
12.));
#231114=CARTESIAN_POINT('Ctrl Pts',(-17.7160649064206,-15.3667376981699,
0.));
#231115=CARTESIAN_POINT('Ctrl Pts',(-17.7160649064206,-15.3667376981699,
12.));
#231116=CARTESIAN_POINT('Ctrl Pts',(-17.7061525444042,-15.351603894206,
0.));
#231117=CARTESIAN_POINT('Ctrl Pts',(-17.7061525444042,-15.351603894206,
12.));
#231118=CARTESIAN_POINT('Ctrl Pts',(-17.6962657941983,-15.3366020244066,
0.));
#231119=CARTESIAN_POINT('Ctrl Pts',(-17.6962657941983,-15.3366020244066,
12.));
#231120=CARTESIAN_POINT('Ctrl Pts',(-17.6864057426052,-15.3217327425338,
0.));
#231121=CARTESIAN_POINT('Ctrl Pts',(-17.6864057426052,-15.3217327425338,
12.));
#231122=CARTESIAN_POINT('Ctrl Pts',(-17.676573494456,-15.3069967108501,
0.));
#231123=CARTESIAN_POINT('Ctrl Pts',(-17.676573494456,-15.3069967108501,
12.));
#231124=CARTESIAN_POINT('Ctrl Pts',(-17.6667701731041,-15.2923946003598,
0.));
#231125=CARTESIAN_POINT('Ctrl Pts',(-17.6667701731041,-15.2923946003598,
12.));
#231126=CARTESIAN_POINT('Ctrl Pts',(-17.6569969209,-15.2779270910239,0.));
#231127=CARTESIAN_POINT('Ctrl Pts',(-17.6569969209,-15.2779270910239,12.));
#231128=CARTESIAN_POINT('Ctrl Pts',(-17.6472548997328,-15.2635948720292,
0.));
#231129=CARTESIAN_POINT('Ctrl Pts',(-17.6472548997328,-15.2635948720292,
12.));
#231130=CARTESIAN_POINT('Ctrl Pts',(-17.6375452916369,-15.2493986421092,
0.));
#231131=CARTESIAN_POINT('Ctrl Pts',(-17.6375452916369,-15.2493986421092,
12.));
#231132=CARTESIAN_POINT('Ctrl Pts',(-17.6278692993764,-15.2353391098366,
0.));
#231133=CARTESIAN_POINT('Ctrl Pts',(-17.6278692993764,-15.2353391098366,
12.));
#231134=CARTESIAN_POINT('Ctrl Pts',(-17.6182281470468,-15.2214169939199,
0.));
#231135=CARTESIAN_POINT('Ctrl Pts',(-17.6182281470468,-15.2214169939199,
12.));
#231136=CARTESIAN_POINT('Ctrl Pts',(-17.60862308065,-15.2076330234686,0.));
#231137=CARTESIAN_POINT('Ctrl Pts',(-17.60862308065,-15.2076330234686,12.));
#231138=CARTESIAN_POINT('Ctrl Pts',(-17.5990553687599,-15.1939879383268,
0.));
#231139=CARTESIAN_POINT('Ctrl Pts',(-17.5990553687599,-15.1939879383268,
12.));
#231140=CARTESIAN_POINT('Ctrl Pts',(-17.5895263032595,-15.1804824894605,
0.));
#231141=CARTESIAN_POINT('Ctrl Pts',(-17.5895263032595,-15.1804824894605,
12.));
#231142=CARTESIAN_POINT('Ctrl Pts',(-17.580037200054,-15.1671174393137,
0.));
#231143=CARTESIAN_POINT('Ctrl Pts',(-17.580037200054,-15.1671174393137,
12.));
#231144=CARTESIAN_POINT('Ctrl Pts',(-17.5705893998029,-15.1538935621714,
0.));
#231145=CARTESIAN_POINT('Ctrl Pts',(-17.5705893998029,-15.1538935621714,
12.));
#231146=CARTESIAN_POINT('Ctrl Pts',(-17.5611842686192,-15.1408116444876,
0.));
#231147=CARTESIAN_POINT('Ctrl Pts',(-17.5611842686192,-15.1408116444876,
12.));
#231148=CARTESIAN_POINT('Ctrl Pts',(-17.5518231989117,-15.1278724853138,
0.));
#231149=CARTESIAN_POINT('Ctrl Pts',(-17.5518231989117,-15.1278724853138,
12.));
#231150=CARTESIAN_POINT('Ctrl Pts',(-17.5425076102963,-15.1150768967728,
0.));
#231151=CARTESIAN_POINT('Ctrl Pts',(-17.5425076102963,-15.1150768967728,
12.));
#231152=CARTESIAN_POINT('Ctrl Pts',(-17.5332389504829,-15.1024257045033,
0.));
#231153=CARTESIAN_POINT('Ctrl Pts',(-17.5332389504829,-15.1024257045033,
12.));
#231154=CARTESIAN_POINT('Ctrl Pts',(-17.5240186961791,-15.0899197481082,
0.));
#231155=CARTESIAN_POINT('Ctrl Pts',(-17.5240186961791,-15.0899197481082,
12.));
#231156=CARTESIAN_POINT('Ctrl Pts',(-17.5148483539687,-15.0775598815749,
0.));
#231157=CARTESIAN_POINT('Ctrl Pts',(-17.5148483539687,-15.0775598815749,
12.));
#231158=CARTESIAN_POINT('Ctrl Pts',(-17.5057294613877,-15.0653469738307,
0.));
#231159=CARTESIAN_POINT('Ctrl Pts',(-17.5057294613877,-15.0653469738307,
12.));
#231160=CARTESIAN_POINT('Ctrl Pts',(-17.4966635880246,-15.0532819093085,
0.));
#231161=CARTESIAN_POINT('Ctrl Pts',(-17.4966635880246,-15.0532819093085,
12.));
#231162=CARTESIAN_POINT('Ctrl Pts',(-17.4876523366178,-15.0413655884993,
0.));
#231163=CARTESIAN_POINT('Ctrl Pts',(-17.4876523366178,-15.0413655884993,
12.));
#231164=CARTESIAN_POINT('Ctrl Pts',(-17.4786973441417,-15.029598928488,
0.));
#231165=CARTESIAN_POINT('Ctrl Pts',(-17.4786973441417,-15.029598928488,
12.));
#231166=CARTESIAN_POINT('Ctrl Pts',(-17.4698002829357,-15.0179828635087,
0.));
#231167=CARTESIAN_POINT('Ctrl Pts',(-17.4698002829357,-15.0179828635087,
12.));
#231168=CARTESIAN_POINT('Ctrl Pts',(-17.4609628621419,-15.0065183456922,
0.));
#231169=CARTESIAN_POINT('Ctrl Pts',(-17.4609628621419,-15.0065183456922,
12.));
#231170=CARTESIAN_POINT('Ctrl Pts',(-17.4521868291005,-14.9952063457779,
0.));
#231171=CARTESIAN_POINT('Ctrl Pts',(-17.4521868291005,-14.9952063457779,
12.));
#231172=CARTESIAN_POINT('Ctrl Pts',(-17.4434739707773,-14.9840478538357,
0.));
#231173=CARTESIAN_POINT('Ctrl Pts',(-17.4434739707773,-14.9840478538357,
12.));
#231174=CARTESIAN_POINT('Ctrl Pts',(-17.4348261151395,-14.973043879945,
0.));
#231175=CARTESIAN_POINT('Ctrl Pts',(-17.4348261151395,-14.973043879945,
12.));
#231176=CARTESIAN_POINT('Ctrl Pts',(-17.4262451327088,-14.9621954549825,
0.));
#231177=CARTESIAN_POINT('Ctrl Pts',(-17.4262451327088,-14.9621954549825,
12.));
#231178=CARTESIAN_POINT('Ctrl Pts',(-17.4177329382827,-14.9515036315142,
0.));
#231179=CARTESIAN_POINT('Ctrl Pts',(-17.4177329382827,-14.9515036315142,
12.));
#231180=CARTESIAN_POINT('Ctrl Pts',(-17.4092914926071,-14.940969484645,
0.));
#231181=CARTESIAN_POINT('Ctrl Pts',(-17.4092914926071,-14.940969484645,
12.));
#231182=CARTESIAN_POINT('Ctrl Pts',(-17.400922804075,-14.9305941128758,
0.));
#231183=CARTESIAN_POINT('Ctrl Pts',(-17.400922804075,-14.9305941128758,
12.));
#231184=CARTESIAN_POINT('Ctrl Pts',(-17.3926289303987,-14.9203786389343,
0.));
#231185=CARTESIAN_POINT('Ctrl Pts',(-17.3926289303987,-14.9203786389343,
12.));
#231186=CARTESIAN_POINT('Ctrl Pts',(-17.3844119809823,-14.9103242110057,
0.));
#231187=CARTESIAN_POINT('Ctrl Pts',(-17.3844119809823,-14.9103242110057,
12.));
#231188=CARTESIAN_POINT('Ctrl Pts',(-17.3762741193075,-14.9004320039609,
0.));
#231189=CARTESIAN_POINT('Ctrl Pts',(-17.3762741193075,-14.9004320039609,
12.));
#231190=CARTESIAN_POINT('Ctrl Pts',(-17.3682175653236,-14.8907032205789,
0.));
#231191=CARTESIAN_POINT('Ctrl Pts',(-17.3682175653236,-14.8907032205789,
12.));
#231192=CARTESIAN_POINT('Ctrl Pts',(-17.3602445978163,-14.8811390927424,
0.));
#231193=CARTESIAN_POINT('Ctrl Pts',(-17.3602445978163,-14.8811390927424,
12.));
#231194=CARTESIAN_POINT('Ctrl Pts',(-17.3523575568648,-14.8717408826958,
0.));
#231195=CARTESIAN_POINT('Ctrl Pts',(-17.3523575568648,-14.8717408826958,
12.));
#231196=CARTESIAN_POINT('Ctrl Pts',(-17.3445588463477,-14.8625098843419,
0.));
#231197=CARTESIAN_POINT('Ctrl Pts',(-17.3445588463477,-14.8625098843419,
12.));
#231198=CARTESIAN_POINT('Ctrl Pts',(-17.336850936485,-14.8534474245433,
0.));
#231199=CARTESIAN_POINT('Ctrl Pts',(-17.336850936485,-14.8534474245433,
12.));
#231200=CARTESIAN_POINT('Ctrl Pts',(-17.3292363662601,-14.8445548643505,
0.));
#231201=CARTESIAN_POINT('Ctrl Pts',(-17.3292363662601,-14.8445548643505,
12.));
#231202=CARTESIAN_POINT('Ctrl Pts',(-17.3217177462096,-14.8358336004193,
0.));
#231203=CARTESIAN_POINT('Ctrl Pts',(-17.3217177462096,-14.8358336004193,
12.));
#231204=CARTESIAN_POINT('Ctrl Pts',(-17.3142977632656,-14.8272850675375,
0.));
#231205=CARTESIAN_POINT('Ctrl Pts',(-17.3142977632656,-14.8272850675375,
12.));
#231206=CARTESIAN_POINT('Ctrl Pts',(-17.3069791853705,-14.8189107410161,
0.));
#231207=CARTESIAN_POINT('Ctrl Pts',(-17.3069791853705,-14.8189107410161,
12.));
#231208=CARTESIAN_POINT('Ctrl Pts',(-17.2997648661483,-14.8107121391038,
0.));
#231209=CARTESIAN_POINT('Ctrl Pts',(-17.2997648661483,-14.8107121391038,
12.));
#231210=CARTESIAN_POINT('Ctrl Pts',(-17.2926577496519,-14.8026908254281,
0.));
#231211=CARTESIAN_POINT('Ctrl Pts',(-17.2926577496519,-14.8026908254281,
12.));
#231212=CARTESIAN_POINT('Ctrl Pts',(-17.28566087332,-14.7948484105253,0.));
#231213=CARTESIAN_POINT('Ctrl Pts',(-17.28566087332,-14.7948484105253,12.));
#231214=CARTESIAN_POINT('Ctrl Pts',(-17.278777370485,-14.787186553128,0.));
#231215=CARTESIAN_POINT('Ctrl Pts',(-17.278777370485,-14.787186553128,12.));
#231216=CARTESIAN_POINT('Ctrl Pts',(-17.2720104735192,-14.7797069617802,
0.));
#231217=CARTESIAN_POINT('Ctrl Pts',(-17.2720104735192,-14.7797069617802,
12.));
#231218=CARTESIAN_POINT('Ctrl Pts',(-17.2653635155317,-14.7724113956728,
0.));
#231219=CARTESIAN_POINT('Ctrl Pts',(-17.2653635155317,-14.7724113956728,
12.));
#231220=CARTESIAN_POINT('Ctrl Pts',(-17.2588399401464,-14.7653016697589,
0.));
#231221=CARTESIAN_POINT('Ctrl Pts',(-17.2588399401464,-14.7653016697589,
12.));
#231222=CARTESIAN_POINT('Ctrl Pts',(-17.2524433146837,-14.7583796616617,
0.));
#231223=CARTESIAN_POINT('Ctrl Pts',(-17.2524433146837,-14.7583796616617,
12.));
#231224=CARTESIAN_POINT('Ctrl Pts',(-17.2461773413289,-14.7516473175125,
0.));
#231225=CARTESIAN_POINT('Ctrl Pts',(-17.2461773413289,-14.7516473175125,
12.));
#231226=CARTESIAN_POINT('Ctrl Pts',(-17.2400458713566,-14.7451066593793,
0.));
#231227=CARTESIAN_POINT('Ctrl Pts',(-17.2400458713566,-14.7451066593793,
12.));
#231228=CARTESIAN_POINT('Ctrl Pts',(-17.2340529062077,-14.7387597858117,
0.));
#231229=CARTESIAN_POINT('Ctrl Pts',(-17.2340529062077,-14.7387597858117,
12.));
#231230=CARTESIAN_POINT('Ctrl Pts',(-17.2282025904314,-14.7326088681163,
0.));
#231231=CARTESIAN_POINT('Ctrl Pts',(-17.2282025904314,-14.7326088681163,
12.));
#231232=CARTESIAN_POINT('Ctrl Pts',(-17.2224992099666,-14.7266561494282,
0.));
#231233=CARTESIAN_POINT('Ctrl Pts',(-17.2224992099666,-14.7266561494282,
12.));
#231234=CARTESIAN_POINT('Ctrl Pts',(-17.2169471814255,-14.7209039390326,
0.));
#231235=CARTESIAN_POINT('Ctrl Pts',(-17.2169471814255,-14.7209039390326,
12.));
#231236=CARTESIAN_POINT('Ctrl Pts',(-17.2115510835988,-14.7153546289338,
0.));
#231237=CARTESIAN_POINT('Ctrl Pts',(-17.2115510835988,-14.7153546289338,
12.));
#231238=CARTESIAN_POINT('Ctrl Pts',(-17.2063157097316,-14.7100107213586,
0.));
#231239=CARTESIAN_POINT('Ctrl Pts',(-17.2063157097316,-14.7100107213586,
12.));
#231240=CARTESIAN_POINT('Ctrl Pts',(-17.2012461084268,-14.7048748502663,
0.));
#231241=CARTESIAN_POINT('Ctrl Pts',(-17.2012461084268,-14.7048748502663,
12.));
#231242=CARTESIAN_POINT('Ctrl Pts',(-17.1963476411694,-14.699949811582,
0.));
#231243=CARTESIAN_POINT('Ctrl Pts',(-17.1963476411694,-14.699949811582,
12.));
#231244=CARTESIAN_POINT('Ctrl Pts',(-17.1916259308416,-14.6952385361706,
0.));
#231245=CARTESIAN_POINT('Ctrl Pts',(-17.1916259308416,-14.6952385361706,
12.));
#231246=CARTESIAN_POINT('Ctrl Pts',(-17.1870867909918,-14.6907440526958,
0.));
#231247=CARTESIAN_POINT('Ctrl Pts',(-17.1870867909918,-14.6907440526958,
12.));
#231248=CARTESIAN_POINT('Ctrl Pts',(-17.182736158472,-14.6864694522319,
0.));
#231249=CARTESIAN_POINT('Ctrl Pts',(-17.182736158472,-14.6864694522319,
12.));
#231250=CARTESIAN_POINT('Ctrl Pts',(-17.1785800350827,-14.6824178576167,
0.));
#231251=CARTESIAN_POINT('Ctrl Pts',(-17.1785800350827,-14.6824178576167,
12.));
#231252=CARTESIAN_POINT('Ctrl Pts',(-17.1746247499057,-14.6785925615676,
0.));
#231253=CARTESIAN_POINT('Ctrl Pts',(-17.1746247499057,-14.6785925615676,
12.));
#231254=CARTESIAN_POINT('Ctrl Pts',(-17.1708771619129,-14.6749971333867,
0.));
#231255=CARTESIAN_POINT('Ctrl Pts',(-17.1708771619129,-14.6749971333867,
12.));
#231256=CARTESIAN_POINT('Ctrl Pts',(-17.1673449723019,-14.6716355833321,
0.));
#231257=CARTESIAN_POINT('Ctrl Pts',(-17.1673449723019,-14.6716355833321,
12.));
#231258=CARTESIAN_POINT('Ctrl Pts',(-17.1640366762304,-14.6685123374424,
0.));
#231259=CARTESIAN_POINT('Ctrl Pts',(-17.1640366762304,-14.6685123374424,
12.));
#231260=CARTESIAN_POINT('Ctrl Pts',(-17.1609609517369,-14.6656319165057,
0.));
#231261=CARTESIAN_POINT('Ctrl Pts',(-17.1609609517369,-14.6656319165057,
12.));
#231262=CARTESIAN_POINT('Ctrl Pts',(-17.1581262646789,-14.662998728599,
0.));
#231263=CARTESIAN_POINT('Ctrl Pts',(-17.1581262646789,-14.662998728599,
12.));
#231264=CARTESIAN_POINT('Ctrl Pts',(-17.1555401986403,-14.660616716964,
0.));
#231265=CARTESIAN_POINT('Ctrl Pts',(-17.1555401986403,-14.660616716964,
12.));
#231266=CARTESIAN_POINT('Ctrl Pts',(-17.1532107762719,-14.6584900555301,
0.));
#231267=CARTESIAN_POINT('Ctrl Pts',(-17.1532107762719,-14.6584900555301,
12.));
#231268=CARTESIAN_POINT('Ctrl Pts',(-17.1511476869495,-14.6566237952435,
0.));
#231269=CARTESIAN_POINT('Ctrl Pts',(-17.1511476869495,-14.6566237952435,
12.));
#231270=CARTESIAN_POINT('Ctrl Pts',(-17.1493641837556,-14.6550248622813,
0.));
#231271=CARTESIAN_POINT('Ctrl Pts',(-17.1493641837556,-14.6550248622813,
12.));
#231272=CARTESIAN_POINT('Ctrl Pts',(-17.1478763944909,-14.6537016966188,
0.));
#231273=CARTESIAN_POINT('Ctrl Pts',(-17.1478763944909,-14.6537016966188,
12.));
#231274=CARTESIAN_POINT('Ctrl Pts',(-17.1466998098673,-14.6526624064978,
0.));
#231275=CARTESIAN_POINT('Ctrl Pts',(-17.1466998098673,-14.6526624064978,
12.));
#231276=CARTESIAN_POINT('Ctrl Pts',(-17.1458462295273,-14.65191316345,0.));
#231277=CARTESIAN_POINT('Ctrl Pts',(-17.1458462295273,-14.65191316345,12.));
#231278=CARTESIAN_POINT('Ctrl Pts',(-17.1454262858045,-14.6515481598057,
0.));
#231279=CARTESIAN_POINT('Ctrl Pts',(-17.1454262858045,-14.6515481598057,
12.));
#231280=CARTESIAN_POINT('Ctrl Pts',(-17.1452600887039,-14.6514066997188,
0.));
#231281=CARTESIAN_POINT('Ctrl Pts',(-17.1452600887039,-14.6514066997188,
12.));
#231282=CARTESIAN_POINT('Ctrl Pts',(-17.1452153999142,-14.651371185284,
0.));
#231283=CARTESIAN_POINT('Ctrl Pts',(-17.1452153999142,-14.651371185284,
12.));
#231284=CARTESIAN_POINT('Ctrl Pts',(-17.1452095830633,-14.6513681262571,
0.));
#231285=CARTESIAN_POINT('Ctrl Pts',(-17.1452095830633,-14.6513681262571,
12.));
#231286=CARTESIAN_POINT('',(-18.8464468996588,-17.9112098770111,0.));
#231287=CARTESIAN_POINT('Ctrl Pts',(-18.8464468996588,-17.9112098770111,
0.));
#231288=CARTESIAN_POINT('Ctrl Pts',(-18.8448126709692,-17.9057348246595,
0.));
#231289=CARTESIAN_POINT('Ctrl Pts',(-18.8415402351786,-17.8947931177807,
0.));
#231290=CARTESIAN_POINT('Ctrl Pts',(-18.8366196462581,-17.8784057509356,
0.));
#231291=CARTESIAN_POINT('Ctrl Pts',(-18.8300349895974,-17.8566063174771,
0.));
#231292=CARTESIAN_POINT('Ctrl Pts',(-18.8217643886157,-17.8294410311006,
0.));
#231293=CARTESIAN_POINT('Ctrl Pts',(-18.8134540340417,-17.8023598011057,
0.));
#231294=CARTESIAN_POINT('Ctrl Pts',(-18.8051039860448,-17.7753627137853,
0.));
#231295=CARTESIAN_POINT('Ctrl Pts',(-18.7967143519419,-17.7484498996905,
0.));
#231296=CARTESIAN_POINT('Ctrl Pts',(-18.788285297605,-17.7216215409035,
0.));
#231297=CARTESIAN_POINT('Ctrl Pts',(-18.7798170641374,-17.6948778823014,
0.));
#231298=CARTESIAN_POINT('Ctrl Pts',(-18.7713099642754,-17.6682192274236,
0.));
#231299=CARTESIAN_POINT('Ctrl Pts',(-18.762764361321,-17.6416459210681,
0.));
#231300=CARTESIAN_POINT('Ctrl Pts',(-18.7541806530984,-17.6151583357012,
0.));
#231301=CARTESIAN_POINT('Ctrl Pts',(-18.7455592536687,-17.5887568561371,
0.));
#231302=CARTESIAN_POINT('Ctrl Pts',(-18.7369005764553,-17.5624418653245,
0.));
#231303=CARTESIAN_POINT('Ctrl Pts',(-18.7282050157138,-17.5362137287593,
0.));
#231304=CARTESIAN_POINT('Ctrl Pts',(-18.7194729318098,-17.5100727820876,
0.));
#231305=CARTESIAN_POINT('Ctrl Pts',(-18.7107046613912,-17.4840193397162,
0.));
#231306=CARTESIAN_POINT('Ctrl Pts',(-18.70190052503,-17.4580537012753,0.));
#231307=CARTESIAN_POINT('Ctrl Pts',(-18.6930608357409,-17.4321761588142,
0.));
#231308=CARTESIAN_POINT('Ctrl Pts',(-18.6841859073471,-17.4063870038562,
0.));
#231309=CARTESIAN_POINT('Ctrl Pts',(-18.6752760624052,-17.3806865340747,
0.));
#231310=CARTESIAN_POINT('Ctrl Pts',(-18.6663316416582,-17.3550750612443,
0.));
#231311=CARTESIAN_POINT('Ctrl Pts',(-18.6573530024033,-17.3295529098618,
0.));
#231312=CARTESIAN_POINT('Ctrl Pts',(-18.6483405141865,-17.3041204135074,
0.));
#231313=CARTESIAN_POINT('Ctrl Pts',(-18.6392945554748,-17.2787779120213,
0.));
#231314=CARTESIAN_POINT('Ctrl Pts',(-18.6302155097943,-17.2535257482187,
0.));
#231315=CARTESIAN_POINT('Ctrl Pts',(-18.6211037624038,-17.2283642650518,
0.));
#231316=CARTESIAN_POINT('Ctrl Pts',(-18.6119596959949,-17.2032938019284,
0.));
#231317=CARTESIAN_POINT('Ctrl Pts',(-18.6027836898817,-17.1783146940127,
0.));
#231318=CARTESIAN_POINT('Ctrl Pts',(-18.5935761222825,-17.1534272741643,
0.));
#231319=CARTESIAN_POINT('Ctrl Pts',(-18.5843373717247,-17.1286318741183,
0.));
#231320=CARTESIAN_POINT('Ctrl Pts',(-18.5750678188542,-17.1039288260001,
0.));
#231321=CARTESIAN_POINT('Ctrl Pts',(-18.5657678479789,-17.0793184636079,
0.));
#231322=CARTESIAN_POINT('Ctrl Pts',(-18.556437848963,-17.0548011239751,
0.));
#231323=CARTESIAN_POINT('Ctrl Pts',(-18.547078218209,-17.0303771481738,
0.));
#231324=CARTESIAN_POINT('Ctrl Pts',(-18.5376893576961,-17.0060468805097,
0.));
#231325=CARTESIAN_POINT('Ctrl Pts',(-18.5282716744197,-16.981810668038,
0.));
#231326=CARTESIAN_POINT('Ctrl Pts',(-18.5188255796659,-16.9576688599339,
0.));
#231327=CARTESIAN_POINT('Ctrl Pts',(-18.5093514883835,-16.9336218069353,
0.));
#231328=CARTESIAN_POINT('Ctrl Pts',(-18.499849818462,-16.9096698606943,
0.));
#231329=CARTESIAN_POINT('Ctrl Pts',(-18.4903209902227,-16.8858133733088,
0.));
#231330=CARTESIAN_POINT('Ctrl Pts',(-18.4807654268771,-16.8620526977171,
0.));
#231331=CARTESIAN_POINT('Ctrl Pts',(-18.4711835548623,-16.8383881879709,
0.));
#231332=CARTESIAN_POINT('Ctrl Pts',(-18.4615758042305,-16.8148201995472,
0.));
#231333=CARTESIAN_POINT('Ctrl Pts',(-18.4519426090124,-16.791349089629,
0.));
#231334=CARTESIAN_POINT('Ctrl Pts',(-18.44228440761,-16.7679752173992,0.));
#231335=CARTESIAN_POINT('Ctrl Pts',(-18.4326016431392,-16.7446989442882,
0.));
#231336=CARTESIAN_POINT('Ctrl Pts',(-18.4228947633187,-16.7215206338818,
0.));
#231337=CARTESIAN_POINT('Ctrl Pts',(-18.413164220399,-16.6984406518491,
0.));
#231338=CARTESIAN_POINT('Ctrl Pts',(-18.403410471079,-16.6754593658513,
0.));
#231339=CARTESIAN_POINT('Ctrl Pts',(-18.3936339764332,-16.6525771454513,
0.));
#231340=CARTESIAN_POINT('Ctrl Pts',(-18.3838352018327,-16.6297943620056,
0.));
#231341=CARTESIAN_POINT('Ctrl Pts',(-18.3740146168879,-16.607111388571,
0.));
#231342=CARTESIAN_POINT('Ctrl Pts',(-18.3641726955889,-16.5845286000217,
0.));
#231343=CARTESIAN_POINT('Ctrl Pts',(-18.354309916433,-16.5620463731413,
0.));
#231344=CARTESIAN_POINT('Ctrl Pts',(-18.34442676256,-16.5396650867139,0.));
#231345=CARTESIAN_POINT('Ctrl Pts',(-18.3345237218864,-16.5173851216045,
0.));
#231346=CARTESIAN_POINT('Ctrl Pts',(-18.3246012872469,-16.4952068608345,
0.));
#231347=CARTESIAN_POINT('Ctrl Pts',(-18.3146599565231,-16.4731306896441,
0.));
#231348=CARTESIAN_POINT('Ctrl Pts',(-18.304700232686,-16.4511569955233,
0.));
#231349=CARTESIAN_POINT('Ctrl Pts',(-18.294722623851,-16.4292861682379,
0.));
#231350=CARTESIAN_POINT('Ctrl Pts',(-18.2847276433309,-16.4075185998455,
0.));
#231351=CARTESIAN_POINT('Ctrl Pts',(-18.2747158096934,-16.385854684708,
0.));
#231352=CARTESIAN_POINT('Ctrl Pts',(-18.2646876468169,-16.3642948194868,
0.));
#231353=CARTESIAN_POINT('Ctrl Pts',(-18.2546436839608,-16.3428394031589,
0.));
#231354=CARTESIAN_POINT('Ctrl Pts',(-18.2445844558742,-16.3214888370987,
0.));
#231355=CARTESIAN_POINT('Ctrl Pts',(-18.2345105028982,-16.3002435251378,
0.));
#231356=CARTESIAN_POINT('Ctrl Pts',(-18.2244223710746,-16.2791038736223,
0.));
#231357=CARTESIAN_POINT('Ctrl Pts',(-18.2143206122529,-16.2580702914615,
0.));
#231358=CARTESIAN_POINT('Ctrl Pts',(-18.2042057842035,-16.2371431901638,
0.));
#231359=CARTESIAN_POINT('Ctrl Pts',(-18.1940784507229,-16.2163229838875,
0.));
#231360=CARTESIAN_POINT('Ctrl Pts',(-18.1839391817331,-16.1956100895073,
0.));
#231361=CARTESIAN_POINT('Ctrl Pts',(-18.1737885533849,-16.1750049266671,
0.));
#231362=CARTESIAN_POINT('Ctrl Pts',(-18.1636271481615,-16.154507917826,
0.));
#231363=CARTESIAN_POINT('Ctrl Pts',(-18.1534555549852,-16.1341194882988,
0.));
#231364=CARTESIAN_POINT('Ctrl Pts',(-18.1432743693235,-16.1138400662794,
0.));
#231365=CARTESIAN_POINT('Ctrl Pts',(-18.1330841933105,-16.0936700829112,
0.));
#231366=CARTESIAN_POINT('Ctrl Pts',(-18.1228856358751,-16.0736099723668,
0.));
#231367=CARTESIAN_POINT('Ctrl Pts',(-18.112679312869,-16.0536601719126,
0.));
#231368=CARTESIAN_POINT('Ctrl Pts',(-18.1024658471966,-16.0338211219693,
0.));
#231369=CARTESIAN_POINT('Ctrl Pts',(-18.0922458689462,-16.014093266161,
0.));
#231370=CARTESIAN_POINT('Ctrl Pts',(-18.0820200155236,-15.9944770513613,
0.));
#231371=CARTESIAN_POINT('Ctrl Pts',(-18.0717889317958,-15.9749729277846,
0.));
#231372=CARTESIAN_POINT('Ctrl Pts',(-18.061553270236,-15.9555813490644,
0.));
#231373=CARTESIAN_POINT('Ctrl Pts',(-18.0513136910691,-15.9363027723244,
0.));
#231374=CARTESIAN_POINT('Ctrl Pts',(-18.0410708624208,-15.9171376582436,
0.));
#231375=CARTESIAN_POINT('Ctrl Pts',(-18.0308254604636,-15.8980864711042,
0.));
#231376=CARTESIAN_POINT('Ctrl Pts',(-18.0205781695769,-15.8791496788682,
0.));
#231377=CARTESIAN_POINT('Ctrl Pts',(-18.0103296825205,-15.8603277532831,
0.));
#231378=CARTESIAN_POINT('Ctrl Pts',(-18.0000807006052,-15.8416211699679,
0.));
#231379=CARTESIAN_POINT('Ctrl Pts',(-17.9898319338664,-15.8230304084962,
0.));
#231380=CARTESIAN_POINT('Ctrl Pts',(-17.9795841012386,-15.8045559524676,
0.));
#231381=CARTESIAN_POINT('Ctrl Pts',(-17.9693379307303,-15.7861982895724,
0.));
#231382=CARTESIAN_POINT('Ctrl Pts',(-17.9590941596242,-15.7679579117077,
0.));
#231383=CARTESIAN_POINT('Ctrl Pts',(-17.9488535346781,-15.749835315086,
0.));
#231384=CARTESIAN_POINT('Ctrl Pts',(-17.9386168123262,-15.7318310003335,
0.));
#231385=CARTESIAN_POINT('Ctrl Pts',(-17.9283847588836,-15.7139454725838,
0.));
#231386=CARTESIAN_POINT('Ctrl Pts',(-17.9181581507455,-15.6961792415522,
0.));
#231387=CARTESIAN_POINT('Ctrl Pts',(-17.9079377746111,-15.678532821646,
0.));
#231388=CARTESIAN_POINT('Ctrl Pts',(-17.897724427724,-15.661006732103,0.));
#231389=CARTESIAN_POINT('Ctrl Pts',(-17.8875189181091,-15.6436014971084,
0.));
#231390=CARTESIAN_POINT('Ctrl Pts',(-17.8773220648125,-15.6263176459108,
0.));
#231391=CARTESIAN_POINT('Ctrl Pts',(-17.8671346981394,-15.609155712921,
0.));
#231392=CARTESIAN_POINT('Ctrl Pts',(-17.8569576599006,-15.5921162378192,
0.));
#231393=CARTESIAN_POINT('Ctrl Pts',(-17.8467918036987,-15.5751997657163,
0.));
#231394=CARTESIAN_POINT('Ctrl Pts',(-17.8366379952085,-15.5584068472982,
0.));
#231395=CARTESIAN_POINT('Ctrl Pts',(-17.8264971124607,-15.541738038964,
0.));
#231396=CARTESIAN_POINT('Ctrl Pts',(-17.8163700461256,-15.5251939029552,
0.));
#231397=CARTESIAN_POINT('Ctrl Pts',(-17.8062576997952,-15.5087750074718,
0.));
#231398=CARTESIAN_POINT('Ctrl Pts',(-17.7961609903148,-15.4924819268517,
0.));
#231399=CARTESIAN_POINT('Ctrl Pts',(-17.786080848122,-15.4763152417497,
0.));
#231400=CARTESIAN_POINT('Ctrl Pts',(-17.7760182175815,-15.4602755393017,
0.));
#231401=CARTESIAN_POINT('Ctrl Pts',(-17.7659740573265,-15.4443634132869,
0.));
#231402=CARTESIAN_POINT('Ctrl Pts',(-17.7559493405881,-15.4285794642668,
0.));
#231403=CARTESIAN_POINT('Ctrl Pts',(-17.7459450555812,-15.4129242997837,
0.));
#231404=CARTESIAN_POINT('Ctrl Pts',(-17.735962205915,-15.3973985345802,
0.));
#231405=CARTESIAN_POINT('Ctrl Pts',(-17.7260018109924,-15.3820027907967,
0.));
#231406=CARTESIAN_POINT('Ctrl Pts',(-17.7160649064206,-15.3667376981699,
0.));
#231407=CARTESIAN_POINT('Ctrl Pts',(-17.7061525444042,-15.351603894206,
0.));
#231408=CARTESIAN_POINT('Ctrl Pts',(-17.6962657941983,-15.3366020244066,
0.));
#231409=CARTESIAN_POINT('Ctrl Pts',(-17.6864057426052,-15.3217327425338,
0.));
#231410=CARTESIAN_POINT('Ctrl Pts',(-17.676573494456,-15.3069967108501,
0.));
#231411=CARTESIAN_POINT('Ctrl Pts',(-17.6667701731041,-15.2923946003598,
0.));
#231412=CARTESIAN_POINT('Ctrl Pts',(-17.6569969209,-15.2779270910239,0.));
#231413=CARTESIAN_POINT('Ctrl Pts',(-17.6472548997328,-15.2635948720292,
0.));
#231414=CARTESIAN_POINT('Ctrl Pts',(-17.6375452916369,-15.2493986421092,
0.));
#231415=CARTESIAN_POINT('Ctrl Pts',(-17.6278692993764,-15.2353391098366,
0.));
#231416=CARTESIAN_POINT('Ctrl Pts',(-17.6182281470468,-15.2214169939199,
0.));
#231417=CARTESIAN_POINT('Ctrl Pts',(-17.60862308065,-15.2076330234686,0.));
#231418=CARTESIAN_POINT('Ctrl Pts',(-17.5990553687599,-15.1939879383268,
0.));
#231419=CARTESIAN_POINT('Ctrl Pts',(-17.5895263032595,-15.1804824894605,
0.));
#231420=CARTESIAN_POINT('Ctrl Pts',(-17.580037200054,-15.1671174393137,
0.));
#231421=CARTESIAN_POINT('Ctrl Pts',(-17.5705893998029,-15.1538935621714,
0.));
#231422=CARTESIAN_POINT('Ctrl Pts',(-17.5611842686192,-15.1408116444876,
0.));
#231423=CARTESIAN_POINT('Ctrl Pts',(-17.5518231989117,-15.1278724853138,
0.));
#231424=CARTESIAN_POINT('Ctrl Pts',(-17.5425076102963,-15.1150768967728,
0.));
#231425=CARTESIAN_POINT('Ctrl Pts',(-17.5332389504829,-15.1024257045033,
0.));
#231426=CARTESIAN_POINT('Ctrl Pts',(-17.5240186961791,-15.0899197481082,
0.));
#231427=CARTESIAN_POINT('Ctrl Pts',(-17.5148483539687,-15.0775598815749,
0.));
#231428=CARTESIAN_POINT('Ctrl Pts',(-17.5057294613877,-15.0653469738307,
0.));
#231429=CARTESIAN_POINT('Ctrl Pts',(-17.4966635880246,-15.0532819093085,
0.));
#231430=CARTESIAN_POINT('Ctrl Pts',(-17.4876523366178,-15.0413655884993,
0.));
#231431=CARTESIAN_POINT('Ctrl Pts',(-17.4786973441417,-15.029598928488,
0.));
#231432=CARTESIAN_POINT('Ctrl Pts',(-17.4698002829357,-15.0179828635087,
0.));
#231433=CARTESIAN_POINT('Ctrl Pts',(-17.4609628621419,-15.0065183456922,
0.));
#231434=CARTESIAN_POINT('Ctrl Pts',(-17.4521868291005,-14.9952063457779,
0.));
#231435=CARTESIAN_POINT('Ctrl Pts',(-17.4434739707773,-14.9840478538357,
0.));
#231436=CARTESIAN_POINT('Ctrl Pts',(-17.4348261151395,-14.973043879945,
0.));
#231437=CARTESIAN_POINT('Ctrl Pts',(-17.4262451327088,-14.9621954549825,
0.));
#231438=CARTESIAN_POINT('Ctrl Pts',(-17.4177329382827,-14.9515036315142,
0.));
#231439=CARTESIAN_POINT('Ctrl Pts',(-17.4092914926071,-14.940969484645,
0.));
#231440=CARTESIAN_POINT('Ctrl Pts',(-17.400922804075,-14.9305941128758,
0.));
#231441=CARTESIAN_POINT('Ctrl Pts',(-17.3926289303987,-14.9203786389343,
0.));
#231442=CARTESIAN_POINT('Ctrl Pts',(-17.3844119809823,-14.9103242110057,
0.));
#231443=CARTESIAN_POINT('Ctrl Pts',(-17.3762741193075,-14.9004320039609,
0.));
#231444=CARTESIAN_POINT('Ctrl Pts',(-17.3682175653236,-14.8907032205789,
0.));
#231445=CARTESIAN_POINT('Ctrl Pts',(-17.3602445978163,-14.8811390927424,
0.));
#231446=CARTESIAN_POINT('Ctrl Pts',(-17.3523575568648,-14.8717408826958,
0.));
#231447=CARTESIAN_POINT('Ctrl Pts',(-17.3445588463477,-14.8625098843419,
0.));
#231448=CARTESIAN_POINT('Ctrl Pts',(-17.336850936485,-14.8534474245433,
0.));
#231449=CARTESIAN_POINT('Ctrl Pts',(-17.3292363662601,-14.8445548643505,
0.));
#231450=CARTESIAN_POINT('Ctrl Pts',(-17.3217177462096,-14.8358336004193,
0.));
#231451=CARTESIAN_POINT('Ctrl Pts',(-17.3142977632656,-14.8272850675375,
0.));
#231452=CARTESIAN_POINT('Ctrl Pts',(-17.3069791853705,-14.8189107410161,
0.));
#231453=CARTESIAN_POINT('Ctrl Pts',(-17.2997648661483,-14.8107121391038,
0.));
#231454=CARTESIAN_POINT('Ctrl Pts',(-17.2926577496519,-14.8026908254281,
0.));
#231455=CARTESIAN_POINT('Ctrl Pts',(-17.28566087332,-14.7948484105253,0.));
#231456=CARTESIAN_POINT('Ctrl Pts',(-17.278777370485,-14.787186553128,0.));
#231457=CARTESIAN_POINT('Ctrl Pts',(-17.2720104735192,-14.7797069617802,
0.));
#231458=CARTESIAN_POINT('Ctrl Pts',(-17.2653635155317,-14.7724113956728,
0.));
#231459=CARTESIAN_POINT('Ctrl Pts',(-17.2588399401464,-14.7653016697589,
0.));
#231460=CARTESIAN_POINT('Ctrl Pts',(-17.2524433146837,-14.7583796616617,
0.));
#231461=CARTESIAN_POINT('Ctrl Pts',(-17.2461773413289,-14.7516473175125,
0.));
#231462=CARTESIAN_POINT('Ctrl Pts',(-17.2400458713566,-14.7451066593793,
0.));
#231463=CARTESIAN_POINT('Ctrl Pts',(-17.2340529062077,-14.7387597858117,
0.));
#231464=CARTESIAN_POINT('Ctrl Pts',(-17.2282025904314,-14.7326088681163,
0.));
#231465=CARTESIAN_POINT('Ctrl Pts',(-17.2224992099666,-14.7266561494282,
0.));
#231466=CARTESIAN_POINT('Ctrl Pts',(-17.2169471814255,-14.7209039390326,
0.));
#231467=CARTESIAN_POINT('Ctrl Pts',(-17.2115510835988,-14.7153546289338,
0.));
#231468=CARTESIAN_POINT('Ctrl Pts',(-17.2063157097316,-14.7100107213586,
0.));
#231469=CARTESIAN_POINT('Ctrl Pts',(-17.2012461084268,-14.7048748502663,
0.));
#231470=CARTESIAN_POINT('Ctrl Pts',(-17.1963476411694,-14.699949811582,
0.));
#231471=CARTESIAN_POINT('Ctrl Pts',(-17.1916259308416,-14.6952385361706,
0.));
#231472=CARTESIAN_POINT('Ctrl Pts',(-17.1870867909918,-14.6907440526958,
0.));
#231473=CARTESIAN_POINT('Ctrl Pts',(-17.182736158472,-14.6864694522319,
0.));
#231474=CARTESIAN_POINT('Ctrl Pts',(-17.1785800350827,-14.6824178576167,
0.));
#231475=CARTESIAN_POINT('Ctrl Pts',(-17.1746247499057,-14.6785925615676,
0.));
#231476=CARTESIAN_POINT('Ctrl Pts',(-17.1708771619129,-14.6749971333867,
0.));
#231477=CARTESIAN_POINT('Ctrl Pts',(-17.1673449723019,-14.6716355833321,
0.));
#231478=CARTESIAN_POINT('Ctrl Pts',(-17.1640366762304,-14.6685123374424,
0.));
#231479=CARTESIAN_POINT('Ctrl Pts',(-17.1609609517369,-14.6656319165057,
0.));
#231480=CARTESIAN_POINT('Ctrl Pts',(-17.1581262646789,-14.662998728599,
0.));
#231481=CARTESIAN_POINT('Ctrl Pts',(-17.1555401986403,-14.660616716964,
0.));
#231482=CARTESIAN_POINT('Ctrl Pts',(-17.1532107762719,-14.6584900555301,
0.));
#231483=CARTESIAN_POINT('Ctrl Pts',(-17.1511476869495,-14.6566237952435,
0.));
#231484=CARTESIAN_POINT('Ctrl Pts',(-17.1493641837556,-14.6550248622813,
0.));
#231485=CARTESIAN_POINT('Ctrl Pts',(-17.1478763944909,-14.6537016966188,
0.));
#231486=CARTESIAN_POINT('Ctrl Pts',(-17.1466998098673,-14.6526624064978,
0.));
#231487=CARTESIAN_POINT('Ctrl Pts',(-17.1458462295273,-14.65191316345,0.));
#231488=CARTESIAN_POINT('Ctrl Pts',(-17.1454262858045,-14.6515481598057,
0.));
#231489=CARTESIAN_POINT('Ctrl Pts',(-17.1452600887039,-14.6514066997188,
0.));
#231490=CARTESIAN_POINT('Ctrl Pts',(-17.1452153999142,-14.651371185284,
0.));
#231491=CARTESIAN_POINT('Ctrl Pts',(-17.1452095830633,-14.6513681262571,
0.));
#231492=CARTESIAN_POINT('',(-18.8464468996588,-17.9112098770111,12.));
#231493=CARTESIAN_POINT('',(-18.8464468996588,-17.9112098770111,0.));
#231494=CARTESIAN_POINT('Ctrl Pts',(-17.1452095830633,-14.6513681262571,
12.));
#231495=CARTESIAN_POINT('Ctrl Pts',(-17.1452153999142,-14.651371185284,
12.));
#231496=CARTESIAN_POINT('Ctrl Pts',(-17.1452600887039,-14.6514066997188,
12.));
#231497=CARTESIAN_POINT('Ctrl Pts',(-17.1454262858045,-14.6515481598057,
12.));
#231498=CARTESIAN_POINT('Ctrl Pts',(-17.1458462295273,-14.65191316345,12.));
#231499=CARTESIAN_POINT('Ctrl Pts',(-17.1466998098673,-14.6526624064978,
12.));
#231500=CARTESIAN_POINT('Ctrl Pts',(-17.1478763944909,-14.6537016966188,
12.));
#231501=CARTESIAN_POINT('Ctrl Pts',(-17.1493641837556,-14.6550248622813,
12.));
#231502=CARTESIAN_POINT('Ctrl Pts',(-17.1511476869495,-14.6566237952435,
12.));
#231503=CARTESIAN_POINT('Ctrl Pts',(-17.1532107762719,-14.6584900555301,
12.));
#231504=CARTESIAN_POINT('Ctrl Pts',(-17.1555401986403,-14.660616716964,
12.));
#231505=CARTESIAN_POINT('Ctrl Pts',(-17.1581262646789,-14.662998728599,
12.));
#231506=CARTESIAN_POINT('Ctrl Pts',(-17.1609609517369,-14.6656319165057,
12.));
#231507=CARTESIAN_POINT('Ctrl Pts',(-17.1640366762304,-14.6685123374424,
12.));
#231508=CARTESIAN_POINT('Ctrl Pts',(-17.1673449723019,-14.6716355833321,
12.));
#231509=CARTESIAN_POINT('Ctrl Pts',(-17.1708771619129,-14.6749971333867,
12.));
#231510=CARTESIAN_POINT('Ctrl Pts',(-17.1746247499057,-14.6785925615676,
12.));
#231511=CARTESIAN_POINT('Ctrl Pts',(-17.1785800350827,-14.6824178576167,
12.));
#231512=CARTESIAN_POINT('Ctrl Pts',(-17.182736158472,-14.6864694522319,
12.));
#231513=CARTESIAN_POINT('Ctrl Pts',(-17.1870867909918,-14.6907440526958,
12.));
#231514=CARTESIAN_POINT('Ctrl Pts',(-17.1916259308416,-14.6952385361706,
12.));
#231515=CARTESIAN_POINT('Ctrl Pts',(-17.1963476411694,-14.699949811582,
12.));
#231516=CARTESIAN_POINT('Ctrl Pts',(-17.2012461084268,-14.7048748502663,
12.));
#231517=CARTESIAN_POINT('Ctrl Pts',(-17.2063157097316,-14.7100107213586,
12.));
#231518=CARTESIAN_POINT('Ctrl Pts',(-17.2115510835988,-14.7153546289338,
12.));
#231519=CARTESIAN_POINT('Ctrl Pts',(-17.2169471814255,-14.7209039390326,
12.));
#231520=CARTESIAN_POINT('Ctrl Pts',(-17.2224992099666,-14.7266561494282,
12.));
#231521=CARTESIAN_POINT('Ctrl Pts',(-17.2282025904314,-14.7326088681163,
12.));
#231522=CARTESIAN_POINT('Ctrl Pts',(-17.2340529062077,-14.7387597858117,
12.));
#231523=CARTESIAN_POINT('Ctrl Pts',(-17.2400458713566,-14.7451066593793,
12.));
#231524=CARTESIAN_POINT('Ctrl Pts',(-17.2461773413289,-14.7516473175125,
12.));
#231525=CARTESIAN_POINT('Ctrl Pts',(-17.2524433146837,-14.7583796616617,
12.));
#231526=CARTESIAN_POINT('Ctrl Pts',(-17.2588399401464,-14.7653016697589,
12.));
#231527=CARTESIAN_POINT('Ctrl Pts',(-17.2653635155317,-14.7724113956728,
12.));
#231528=CARTESIAN_POINT('Ctrl Pts',(-17.2720104735192,-14.7797069617802,
12.));
#231529=CARTESIAN_POINT('Ctrl Pts',(-17.278777370485,-14.787186553128,12.));
#231530=CARTESIAN_POINT('Ctrl Pts',(-17.28566087332,-14.7948484105253,12.));
#231531=CARTESIAN_POINT('Ctrl Pts',(-17.2926577496519,-14.8026908254281,
12.));
#231532=CARTESIAN_POINT('Ctrl Pts',(-17.2997648661483,-14.8107121391038,
12.));
#231533=CARTESIAN_POINT('Ctrl Pts',(-17.3069791853705,-14.8189107410161,
12.));
#231534=CARTESIAN_POINT('Ctrl Pts',(-17.3142977632656,-14.8272850675375,
12.));
#231535=CARTESIAN_POINT('Ctrl Pts',(-17.3217177462096,-14.8358336004193,
12.));
#231536=CARTESIAN_POINT('Ctrl Pts',(-17.3292363662601,-14.8445548643505,
12.));
#231537=CARTESIAN_POINT('Ctrl Pts',(-17.336850936485,-14.8534474245433,
12.));
#231538=CARTESIAN_POINT('Ctrl Pts',(-17.3445588463477,-14.8625098843419,
12.));
#231539=CARTESIAN_POINT('Ctrl Pts',(-17.3523575568648,-14.8717408826958,
12.));
#231540=CARTESIAN_POINT('Ctrl Pts',(-17.3602445978163,-14.8811390927424,
12.));
#231541=CARTESIAN_POINT('Ctrl Pts',(-17.3682175653236,-14.8907032205789,
12.));
#231542=CARTESIAN_POINT('Ctrl Pts',(-17.3762741193075,-14.9004320039609,
12.));
#231543=CARTESIAN_POINT('Ctrl Pts',(-17.3844119809823,-14.9103242110057,
12.));
#231544=CARTESIAN_POINT('Ctrl Pts',(-17.3926289303987,-14.9203786389343,
12.));
#231545=CARTESIAN_POINT('Ctrl Pts',(-17.400922804075,-14.9305941128758,
12.));
#231546=CARTESIAN_POINT('Ctrl Pts',(-17.4092914926071,-14.940969484645,
12.));
#231547=CARTESIAN_POINT('Ctrl Pts',(-17.4177329382827,-14.9515036315142,
12.));
#231548=CARTESIAN_POINT('Ctrl Pts',(-17.4262451327088,-14.9621954549825,
12.));
#231549=CARTESIAN_POINT('Ctrl Pts',(-17.4348261151395,-14.973043879945,
12.));
#231550=CARTESIAN_POINT('Ctrl Pts',(-17.4434739707773,-14.9840478538357,
12.));
#231551=CARTESIAN_POINT('Ctrl Pts',(-17.4521868291005,-14.9952063457779,
12.));
#231552=CARTESIAN_POINT('Ctrl Pts',(-17.4609628621419,-15.0065183456922,
12.));
#231553=CARTESIAN_POINT('Ctrl Pts',(-17.4698002829357,-15.0179828635087,
12.));
#231554=CARTESIAN_POINT('Ctrl Pts',(-17.4786973441417,-15.029598928488,
12.));
#231555=CARTESIAN_POINT('Ctrl Pts',(-17.4876523366178,-15.0413655884993,
12.));
#231556=CARTESIAN_POINT('Ctrl Pts',(-17.4966635880246,-15.0532819093085,
12.));
#231557=CARTESIAN_POINT('Ctrl Pts',(-17.5057294613877,-15.0653469738307,
12.));
#231558=CARTESIAN_POINT('Ctrl Pts',(-17.5148483539687,-15.0775598815749,
12.));
#231559=CARTESIAN_POINT('Ctrl Pts',(-17.5240186961791,-15.0899197481082,
12.));
#231560=CARTESIAN_POINT('Ctrl Pts',(-17.5332389504829,-15.1024257045033,
12.));
#231561=CARTESIAN_POINT('Ctrl Pts',(-17.5425076102963,-15.1150768967728,
12.));
#231562=CARTESIAN_POINT('Ctrl Pts',(-17.5518231989117,-15.1278724853138,
12.));
#231563=CARTESIAN_POINT('Ctrl Pts',(-17.5611842686192,-15.1408116444876,
12.));
#231564=CARTESIAN_POINT('Ctrl Pts',(-17.5705893998029,-15.1538935621714,
12.));
#231565=CARTESIAN_POINT('Ctrl Pts',(-17.580037200054,-15.1671174393137,
12.));
#231566=CARTESIAN_POINT('Ctrl Pts',(-17.5895263032595,-15.1804824894605,
12.));
#231567=CARTESIAN_POINT('Ctrl Pts',(-17.5990553687599,-15.1939879383268,
12.));
#231568=CARTESIAN_POINT('Ctrl Pts',(-17.60862308065,-15.2076330234686,12.));
#231569=CARTESIAN_POINT('Ctrl Pts',(-17.6182281470468,-15.2214169939199,
12.));
#231570=CARTESIAN_POINT('Ctrl Pts',(-17.6278692993764,-15.2353391098366,
12.));
#231571=CARTESIAN_POINT('Ctrl Pts',(-17.6375452916369,-15.2493986421092,
12.));
#231572=CARTESIAN_POINT('Ctrl Pts',(-17.6472548997328,-15.2635948720292,
12.));
#231573=CARTESIAN_POINT('Ctrl Pts',(-17.6569969209,-15.2779270910239,12.));
#231574=CARTESIAN_POINT('Ctrl Pts',(-17.6667701731041,-15.2923946003598,
12.));
#231575=CARTESIAN_POINT('Ctrl Pts',(-17.676573494456,-15.3069967108501,
12.));
#231576=CARTESIAN_POINT('Ctrl Pts',(-17.6864057426052,-15.3217327425338,
12.));
#231577=CARTESIAN_POINT('Ctrl Pts',(-17.6962657941983,-15.3366020244066,
12.));
#231578=CARTESIAN_POINT('Ctrl Pts',(-17.7061525444042,-15.351603894206,
12.));
#231579=CARTESIAN_POINT('Ctrl Pts',(-17.7160649064206,-15.3667376981699,
12.));
#231580=CARTESIAN_POINT('Ctrl Pts',(-17.7260018109924,-15.3820027907967,
12.));
#231581=CARTESIAN_POINT('Ctrl Pts',(-17.735962205915,-15.3973985345802,
12.));
#231582=CARTESIAN_POINT('Ctrl Pts',(-17.7459450555812,-15.4129242997837,
12.));
#231583=CARTESIAN_POINT('Ctrl Pts',(-17.7559493405881,-15.4285794642668,
12.));
#231584=CARTESIAN_POINT('Ctrl Pts',(-17.7659740573265,-15.4443634132869,
12.));
#231585=CARTESIAN_POINT('Ctrl Pts',(-17.7760182175815,-15.4602755393017,
12.));
#231586=CARTESIAN_POINT('Ctrl Pts',(-17.786080848122,-15.4763152417497,
12.));
#231587=CARTESIAN_POINT('Ctrl Pts',(-17.7961609903148,-15.4924819268517,
12.));
#231588=CARTESIAN_POINT('Ctrl Pts',(-17.8062576997952,-15.5087750074718,
12.));
#231589=CARTESIAN_POINT('Ctrl Pts',(-17.8163700461256,-15.5251939029552,
12.));
#231590=CARTESIAN_POINT('Ctrl Pts',(-17.8264971124607,-15.541738038964,
12.));
#231591=CARTESIAN_POINT('Ctrl Pts',(-17.8366379952085,-15.5584068472982,
12.));
#231592=CARTESIAN_POINT('Ctrl Pts',(-17.8467918036987,-15.5751997657163,
12.));
#231593=CARTESIAN_POINT('Ctrl Pts',(-17.8569576599006,-15.5921162378192,
12.));
#231594=CARTESIAN_POINT('Ctrl Pts',(-17.8671346981394,-15.609155712921,
12.));
#231595=CARTESIAN_POINT('Ctrl Pts',(-17.8773220648125,-15.6263176459108,
12.));
#231596=CARTESIAN_POINT('Ctrl Pts',(-17.8875189181091,-15.6436014971084,
12.));
#231597=CARTESIAN_POINT('Ctrl Pts',(-17.897724427724,-15.661006732103,12.));
#231598=CARTESIAN_POINT('Ctrl Pts',(-17.9079377746111,-15.678532821646,
12.));
#231599=CARTESIAN_POINT('Ctrl Pts',(-17.9181581507455,-15.6961792415522,
12.));
#231600=CARTESIAN_POINT('Ctrl Pts',(-17.9283847588836,-15.7139454725838,
12.));
#231601=CARTESIAN_POINT('Ctrl Pts',(-17.9386168123262,-15.7318310003335,
12.));
#231602=CARTESIAN_POINT('Ctrl Pts',(-17.9488535346781,-15.749835315086,
12.));
#231603=CARTESIAN_POINT('Ctrl Pts',(-17.9590941596242,-15.7679579117077,
12.));
#231604=CARTESIAN_POINT('Ctrl Pts',(-17.9693379307303,-15.7861982895724,
12.));
#231605=CARTESIAN_POINT('Ctrl Pts',(-17.9795841012386,-15.8045559524676,
12.));
#231606=CARTESIAN_POINT('Ctrl Pts',(-17.9898319338664,-15.8230304084962,
12.));
#231607=CARTESIAN_POINT('Ctrl Pts',(-18.0000807006052,-15.8416211699679,
12.));
#231608=CARTESIAN_POINT('Ctrl Pts',(-18.0103296825205,-15.8603277532831,
12.));
#231609=CARTESIAN_POINT('Ctrl Pts',(-18.0205781695769,-15.8791496788682,
12.));
#231610=CARTESIAN_POINT('Ctrl Pts',(-18.0308254604636,-15.8980864711042,
12.));
#231611=CARTESIAN_POINT('Ctrl Pts',(-18.0410708624208,-15.9171376582436,
12.));
#231612=CARTESIAN_POINT('Ctrl Pts',(-18.0513136910691,-15.9363027723244,
12.));
#231613=CARTESIAN_POINT('Ctrl Pts',(-18.061553270236,-15.9555813490644,
12.));
#231614=CARTESIAN_POINT('Ctrl Pts',(-18.0717889317958,-15.9749729277846,
12.));
#231615=CARTESIAN_POINT('Ctrl Pts',(-18.0820200155236,-15.9944770513613,
12.));
#231616=CARTESIAN_POINT('Ctrl Pts',(-18.0922458689462,-16.014093266161,
12.));
#231617=CARTESIAN_POINT('Ctrl Pts',(-18.1024658471966,-16.0338211219693,
12.));
#231618=CARTESIAN_POINT('Ctrl Pts',(-18.112679312869,-16.0536601719126,
12.));
#231619=CARTESIAN_POINT('Ctrl Pts',(-18.1228856358751,-16.0736099723668,
12.));
#231620=CARTESIAN_POINT('Ctrl Pts',(-18.1330841933105,-16.0936700829112,
12.));
#231621=CARTESIAN_POINT('Ctrl Pts',(-18.1432743693235,-16.1138400662794,
12.));
#231622=CARTESIAN_POINT('Ctrl Pts',(-18.1534555549852,-16.1341194882988,
12.));
#231623=CARTESIAN_POINT('Ctrl Pts',(-18.1636271481615,-16.154507917826,
12.));
#231624=CARTESIAN_POINT('Ctrl Pts',(-18.1737885533849,-16.1750049266671,
12.));
#231625=CARTESIAN_POINT('Ctrl Pts',(-18.1839391817331,-16.1956100895073,
12.));
#231626=CARTESIAN_POINT('Ctrl Pts',(-18.1940784507229,-16.2163229838875,
12.));
#231627=CARTESIAN_POINT('Ctrl Pts',(-18.2042057842035,-16.2371431901638,
12.));
#231628=CARTESIAN_POINT('Ctrl Pts',(-18.2143206122529,-16.2580702914615,
12.));
#231629=CARTESIAN_POINT('Ctrl Pts',(-18.2244223710746,-16.2791038736223,
12.));
#231630=CARTESIAN_POINT('Ctrl Pts',(-18.2345105028982,-16.3002435251378,
12.));
#231631=CARTESIAN_POINT('Ctrl Pts',(-18.2445844558742,-16.3214888370987,
12.));
#231632=CARTESIAN_POINT('Ctrl Pts',(-18.2546436839608,-16.3428394031589,
12.));
#231633=CARTESIAN_POINT('Ctrl Pts',(-18.2646876468169,-16.3642948194868,
12.));
#231634=CARTESIAN_POINT('Ctrl Pts',(-18.2747158096934,-16.385854684708,
12.));
#231635=CARTESIAN_POINT('Ctrl Pts',(-18.2847276433309,-16.4075185998455,
12.));
#231636=CARTESIAN_POINT('Ctrl Pts',(-18.294722623851,-16.4292861682379,
12.));
#231637=CARTESIAN_POINT('Ctrl Pts',(-18.304700232686,-16.4511569955233,
12.));
#231638=CARTESIAN_POINT('Ctrl Pts',(-18.3146599565231,-16.4731306896441,
12.));
#231639=CARTESIAN_POINT('Ctrl Pts',(-18.3246012872469,-16.4952068608345,
12.));
#231640=CARTESIAN_POINT('Ctrl Pts',(-18.3345237218864,-16.5173851216045,
12.));
#231641=CARTESIAN_POINT('Ctrl Pts',(-18.34442676256,-16.5396650867139,12.));
#231642=CARTESIAN_POINT('Ctrl Pts',(-18.354309916433,-16.5620463731413,
12.));
#231643=CARTESIAN_POINT('Ctrl Pts',(-18.3641726955889,-16.5845286000217,
12.));
#231644=CARTESIAN_POINT('Ctrl Pts',(-18.3740146168879,-16.607111388571,
12.));
#231645=CARTESIAN_POINT('Ctrl Pts',(-18.3838352018327,-16.6297943620056,
12.));
#231646=CARTESIAN_POINT('Ctrl Pts',(-18.3936339764332,-16.6525771454513,
12.));
#231647=CARTESIAN_POINT('Ctrl Pts',(-18.403410471079,-16.6754593658513,
12.));
#231648=CARTESIAN_POINT('Ctrl Pts',(-18.413164220399,-16.6984406518491,
12.));
#231649=CARTESIAN_POINT('Ctrl Pts',(-18.4228947633187,-16.7215206338818,
12.));
#231650=CARTESIAN_POINT('Ctrl Pts',(-18.4326016431392,-16.7446989442882,
12.));
#231651=CARTESIAN_POINT('Ctrl Pts',(-18.44228440761,-16.7679752173992,12.));
#231652=CARTESIAN_POINT('Ctrl Pts',(-18.4519426090124,-16.791349089629,
12.));
#231653=CARTESIAN_POINT('Ctrl Pts',(-18.4615758042305,-16.8148201995472,
12.));
#231654=CARTESIAN_POINT('Ctrl Pts',(-18.4711835548623,-16.8383881879709,
12.));
#231655=CARTESIAN_POINT('Ctrl Pts',(-18.4807654268771,-16.8620526977171,
12.));
#231656=CARTESIAN_POINT('Ctrl Pts',(-18.4903209902227,-16.8858133733088,
12.));
#231657=CARTESIAN_POINT('Ctrl Pts',(-18.499849818462,-16.9096698606943,
12.));
#231658=CARTESIAN_POINT('Ctrl Pts',(-18.5093514883835,-16.9336218069353,
12.));
#231659=CARTESIAN_POINT('Ctrl Pts',(-18.5188255796659,-16.9576688599339,
12.));
#231660=CARTESIAN_POINT('Ctrl Pts',(-18.5282716744197,-16.981810668038,
12.));
#231661=CARTESIAN_POINT('Ctrl Pts',(-18.5376893576961,-17.0060468805097,
12.));
#231662=CARTESIAN_POINT('Ctrl Pts',(-18.547078218209,-17.0303771481738,
12.));
#231663=CARTESIAN_POINT('Ctrl Pts',(-18.556437848963,-17.0548011239751,
12.));
#231664=CARTESIAN_POINT('Ctrl Pts',(-18.5657678479789,-17.0793184636079,
12.));
#231665=CARTESIAN_POINT('Ctrl Pts',(-18.5750678188542,-17.1039288260001,
12.));
#231666=CARTESIAN_POINT('Ctrl Pts',(-18.5843373717247,-17.1286318741183,
12.));
#231667=CARTESIAN_POINT('Ctrl Pts',(-18.5935761222825,-17.1534272741643,
12.));
#231668=CARTESIAN_POINT('Ctrl Pts',(-18.6027836898817,-17.1783146940127,
12.));
#231669=CARTESIAN_POINT('Ctrl Pts',(-18.6119596959949,-17.2032938019284,
12.));
#231670=CARTESIAN_POINT('Ctrl Pts',(-18.6211037624038,-17.2283642650518,
12.));
#231671=CARTESIAN_POINT('Ctrl Pts',(-18.6302155097943,-17.2535257482187,
12.));
#231672=CARTESIAN_POINT('Ctrl Pts',(-18.6392945554748,-17.2787779120213,
12.));
#231673=CARTESIAN_POINT('Ctrl Pts',(-18.6483405141865,-17.3041204135074,
12.));
#231674=CARTESIAN_POINT('Ctrl Pts',(-18.6573530024033,-17.3295529098618,
12.));
#231675=CARTESIAN_POINT('Ctrl Pts',(-18.6663316416582,-17.3550750612443,
12.));
#231676=CARTESIAN_POINT('Ctrl Pts',(-18.6752760624052,-17.3806865340747,
12.));
#231677=CARTESIAN_POINT('Ctrl Pts',(-18.6841859073471,-17.4063870038562,
12.));
#231678=CARTESIAN_POINT('Ctrl Pts',(-18.6930608357409,-17.4321761588142,
12.));
#231679=CARTESIAN_POINT('Ctrl Pts',(-18.70190052503,-17.4580537012753,12.));
#231680=CARTESIAN_POINT('Ctrl Pts',(-18.7107046613912,-17.4840193397162,
12.));
#231681=CARTESIAN_POINT('Ctrl Pts',(-18.7194729318098,-17.5100727820876,
12.));
#231682=CARTESIAN_POINT('Ctrl Pts',(-18.7282050157138,-17.5362137287593,
12.));
#231683=CARTESIAN_POINT('Ctrl Pts',(-18.7369005764553,-17.5624418653245,
12.));
#231684=CARTESIAN_POINT('Ctrl Pts',(-18.7455592536687,-17.5887568561371,
12.));
#231685=CARTESIAN_POINT('Ctrl Pts',(-18.7541806530984,-17.6151583357012,
12.));
#231686=CARTESIAN_POINT('Ctrl Pts',(-18.762764361321,-17.6416459210681,
12.));
#231687=CARTESIAN_POINT('Ctrl Pts',(-18.7713099642754,-17.6682192274236,
12.));
#231688=CARTESIAN_POINT('Ctrl Pts',(-18.7798170641374,-17.6948778823014,
12.));
#231689=CARTESIAN_POINT('Ctrl Pts',(-18.788285297605,-17.7216215409035,
12.));
#231690=CARTESIAN_POINT('Ctrl Pts',(-18.7967143519419,-17.7484498996905,
12.));
#231691=CARTESIAN_POINT('Ctrl Pts',(-18.8051039860448,-17.7753627137853,
12.));
#231692=CARTESIAN_POINT('Ctrl Pts',(-18.8134540340417,-17.8023598011057,
12.));
#231693=CARTESIAN_POINT('Ctrl Pts',(-18.8217643886157,-17.8294410311006,
12.));
#231694=CARTESIAN_POINT('Ctrl Pts',(-18.8300349895974,-17.8566063174771,
12.));
#231695=CARTESIAN_POINT('Ctrl Pts',(-18.8366196462581,-17.8784057509356,
12.));
#231696=CARTESIAN_POINT('Ctrl Pts',(-18.8415402351786,-17.8947931177807,
12.));
#231697=CARTESIAN_POINT('Ctrl Pts',(-18.8448126709692,-17.9057348246595,
12.));
#231698=CARTESIAN_POINT('Ctrl Pts',(-18.8464468996588,-17.9112098770111,
12.));
#231699=CARTESIAN_POINT('Ctrl Pts',(-18.5896416359912,-12.7689476255363,
0.));
#231700=CARTESIAN_POINT('Ctrl Pts',(-18.5896416359912,-12.7689476255363,
12.));
#231701=CARTESIAN_POINT('Ctrl Pts',(-18.5896460962964,-12.7689524524483,
0.));
#231702=CARTESIAN_POINT('Ctrl Pts',(-18.5896460962964,-12.7689524524483,
12.));
#231703=CARTESIAN_POINT('Ctrl Pts',(-18.5896919669165,-12.768986426692,
0.));
#231704=CARTESIAN_POINT('Ctrl Pts',(-18.5896919669165,-12.768986426692,
12.));
#231705=CARTESIAN_POINT('Ctrl Pts',(-18.589871621843,-12.769110348199,0.));
#231706=CARTESIAN_POINT('Ctrl Pts',(-18.589871621843,-12.769110348199,12.));
#231707=CARTESIAN_POINT('Ctrl Pts',(-18.5903328777227,-12.7694215127919,
0.));
#231708=CARTESIAN_POINT('Ctrl Pts',(-18.5903328777227,-12.7694215127919,
12.));
#231709=CARTESIAN_POINT('Ctrl Pts',(-18.5912775137806,-12.7700520897173,
0.));
#231710=CARTESIAN_POINT('Ctrl Pts',(-18.5912775137806,-12.7700520897173,
12.));
#231711=CARTESIAN_POINT('Ctrl Pts',(-18.5925859134579,-12.7709195951156,
0.));
#231712=CARTESIAN_POINT('Ctrl Pts',(-18.5925859134579,-12.7709195951156,
12.));
#231713=CARTESIAN_POINT('Ctrl Pts',(-18.5942490615407,-12.7720142287172,
0.));
#231714=CARTESIAN_POINT('Ctrl Pts',(-18.5942490615407,-12.7720142287172,
12.));
#231715=CARTESIAN_POINT('Ctrl Pts',(-18.5962551167772,-12.7733231262108,
0.));
#231716=CARTESIAN_POINT('Ctrl Pts',(-18.5962551167772,-12.7733231262108,
12.));
#231717=CARTESIAN_POINT('Ctrl Pts',(-18.598591752595,-12.7748328937638,
0.));
#231718=CARTESIAN_POINT('Ctrl Pts',(-18.598591752595,-12.7748328937638,
12.));
#231719=CARTESIAN_POINT('Ctrl Pts',(-18.6012488486709,-12.7765325225081,
0.));
#231720=CARTESIAN_POINT('Ctrl Pts',(-18.6012488486709,-12.7765325225081,
12.));
#231721=CARTESIAN_POINT('Ctrl Pts',(-18.6042190183704,-12.7784139605066,
0.));
#231722=CARTESIAN_POINT('Ctrl Pts',(-18.6042190183704,-12.7784139605066,
12.));
#231723=CARTESIAN_POINT('Ctrl Pts',(-18.6074961535723,-12.7804705387658,
0.));
#231724=CARTESIAN_POINT('Ctrl Pts',(-18.6074961535723,-12.7804705387658,
12.));
#231725=CARTESIAN_POINT('Ctrl Pts',(-18.6110744826219,-12.7826959526925,
0.));
#231726=CARTESIAN_POINT('Ctrl Pts',(-18.6110744826219,-12.7826959526925,
12.));
#231727=CARTESIAN_POINT('Ctrl Pts',(-18.6149475565188,-12.7850831657901,
0.));
#231728=CARTESIAN_POINT('Ctrl Pts',(-18.6149475565188,-12.7850831657901,
12.));
#231729=CARTESIAN_POINT('Ctrl Pts',(-18.6191087624752,-12.7876249657834,
0.));
#231730=CARTESIAN_POINT('Ctrl Pts',(-18.6191087624752,-12.7876249657834,
12.));
#231731=CARTESIAN_POINT('Ctrl Pts',(-18.6235516265575,-12.7903142925234,
0.));
#231732=CARTESIAN_POINT('Ctrl Pts',(-18.6235516265575,-12.7903142925234,
12.));
#231733=CARTESIAN_POINT('Ctrl Pts',(-18.6282702819371,-12.7931447451555,
0.));
#231734=CARTESIAN_POINT('Ctrl Pts',(-18.6282702819371,-12.7931447451555,
12.));
#231735=CARTESIAN_POINT('Ctrl Pts',(-18.6332595057006,-12.7961106222251,
0.));
#231736=CARTESIAN_POINT('Ctrl Pts',(-18.6332595057006,-12.7961106222251,
12.));
#231737=CARTESIAN_POINT('Ctrl Pts',(-18.63851447924,-12.7992066625264,0.));
#231738=CARTESIAN_POINT('Ctrl Pts',(-18.63851447924,-12.7992066625264,12.));
#231739=CARTESIAN_POINT('Ctrl Pts',(-18.6440306327456,-12.8024278770152,
0.));
#231740=CARTESIAN_POINT('Ctrl Pts',(-18.6440306327456,-12.8024278770152,
12.));
#231741=CARTESIAN_POINT('Ctrl Pts',(-18.6498034438987,-12.805769331162,
0.));
#231742=CARTESIAN_POINT('Ctrl Pts',(-18.6498034438987,-12.805769331162,
12.));
#231743=CARTESIAN_POINT('Ctrl Pts',(-18.6558284825773,-12.8092261933858,
0.));
#231744=CARTESIAN_POINT('Ctrl Pts',(-18.6558284825773,-12.8092261933858,
12.));
#231745=CARTESIAN_POINT('Ctrl Pts',(-18.6621014624746,-12.8127937909631,
0.));
#231746=CARTESIAN_POINT('Ctrl Pts',(-18.6621014624746,-12.8127937909631,
12.));
#231747=CARTESIAN_POINT('Ctrl Pts',(-18.6686182952799,-12.8164676687362,
0.));
#231748=CARTESIAN_POINT('Ctrl Pts',(-18.6686182952799,-12.8164676687362,
12.));
#231749=CARTESIAN_POINT('Ctrl Pts',(-18.6753751301092,-12.8202436318474,
0.));
#231750=CARTESIAN_POINT('Ctrl Pts',(-18.6753751301092,-12.8202436318474,
12.));
#231751=CARTESIAN_POINT('Ctrl Pts',(-18.6823683094139,-12.8241176980017,
0.));
#231752=CARTESIAN_POINT('Ctrl Pts',(-18.6823683094139,-12.8241176980017,
12.));
#231753=CARTESIAN_POINT('Ctrl Pts',(-18.6895943376171,-12.8280860635231,
0.));
#231754=CARTESIAN_POINT('Ctrl Pts',(-18.6895943376171,-12.8280860635231,
12.));
#231755=CARTESIAN_POINT('Ctrl Pts',(-18.6970498410172,-12.8321450599789,
0.));
#231756=CARTESIAN_POINT('Ctrl Pts',(-18.6970498410172,-12.8321450599789,
12.));
#231757=CARTESIAN_POINT('Ctrl Pts',(-18.7047315436294,-12.8362911280361,
0.));
#231758=CARTESIAN_POINT('Ctrl Pts',(-18.7047315436294,-12.8362911280361,
12.));
#231759=CARTESIAN_POINT('Ctrl Pts',(-18.7126362754445,-12.8405208263431,
0.));
#231760=CARTESIAN_POINT('Ctrl Pts',(-18.7126362754445,-12.8405208263431,
12.));
#231761=CARTESIAN_POINT('Ctrl Pts',(-18.7207609737702,-12.8448308329494,
0.));
#231762=CARTESIAN_POINT('Ctrl Pts',(-18.7207609737702,-12.8448308329494,
12.));
#231763=CARTESIAN_POINT('Ctrl Pts',(-18.7291026886554,-12.8492179511591,
0.));
#231764=CARTESIAN_POINT('Ctrl Pts',(-18.7291026886554,-12.8492179511591,
12.));
#231765=CARTESIAN_POINT('Ctrl Pts',(-18.7376585820854,-12.8536791086316,
0.));
#231766=CARTESIAN_POINT('Ctrl Pts',(-18.7376585820854,-12.8536791086316,
12.));
#231767=CARTESIAN_POINT('Ctrl Pts',(-18.7464259171251,-12.8582113455646,
0.));
#231768=CARTESIAN_POINT('Ctrl Pts',(-18.7464259171251,-12.8582113455646,
12.));
#231769=CARTESIAN_POINT('Ctrl Pts',(-18.7554020493887,-12.8628118054171,
0.));
#231770=CARTESIAN_POINT('Ctrl Pts',(-18.7554020493887,-12.8628118054171,
12.));
#231771=CARTESIAN_POINT('Ctrl Pts',(-18.7645844169564,-12.8674777239653,
0.));
#231772=CARTESIAN_POINT('Ctrl Pts',(-18.7645844169564,-12.8674777239653,
12.));
#231773=CARTESIAN_POINT('Ctrl Pts',(-18.7739705329022,-12.872206421181,
0.));
#231774=CARTESIAN_POINT('Ctrl Pts',(-18.7739705329022,-12.872206421181,
12.));
#231775=CARTESIAN_POINT('Ctrl Pts',(-18.7835579840477,-12.8769952998095,
0.));
#231776=CARTESIAN_POINT('Ctrl Pts',(-18.7835579840477,-12.8769952998095,
12.));
#231777=CARTESIAN_POINT('Ctrl Pts',(-18.7933444285868,-12.8818418427475,
0.));
#231778=CARTESIAN_POINT('Ctrl Pts',(-18.7933444285868,-12.8818418427475,
12.));
#231779=CARTESIAN_POINT('Ctrl Pts',(-18.8033275941943,-12.8867436109546,
0.));
#231780=CARTESIAN_POINT('Ctrl Pts',(-18.8033275941943,-12.8867436109546,
12.));
#231781=CARTESIAN_POINT('Ctrl Pts',(-18.813505275782,-12.8916982409935,
0.));
#231782=CARTESIAN_POINT('Ctrl Pts',(-18.813505275782,-12.8916982409935,
12.));
#231783=CARTESIAN_POINT('Ctrl Pts',(-18.8238753319129,-12.8967034410755,
0.));
#231784=CARTESIAN_POINT('Ctrl Pts',(-18.8238753319129,-12.8967034410755,
12.));
#231785=CARTESIAN_POINT('Ctrl Pts',(-18.834435681259,-12.9017569871738,
0.));
#231786=CARTESIAN_POINT('Ctrl Pts',(-18.834435681259,-12.9017569871738,
12.));
#231787=CARTESIAN_POINT('Ctrl Pts',(-18.8451842990984,-12.9068567191854,
0.));
#231788=CARTESIAN_POINT('Ctrl Pts',(-18.8451842990984,-12.9068567191854,
12.));
#231789=CARTESIAN_POINT('Ctrl Pts',(-18.8561192136198,-12.9120005369063,
0.));
#231790=CARTESIAN_POINT('Ctrl Pts',(-18.8561192136198,-12.9120005369063,
12.));
#231791=CARTESIAN_POINT('Ctrl Pts',(-18.8672385038326,-12.9171863977045,
0.));
#231792=CARTESIAN_POINT('Ctrl Pts',(-18.8672385038326,-12.9171863977045,
12.));
#231793=CARTESIAN_POINT('Ctrl Pts',(-18.8785402977527,-12.9224123144982,
0.));
#231794=CARTESIAN_POINT('Ctrl Pts',(-18.8785402977527,-12.9224123144982,
12.));
#231795=CARTESIAN_POINT('Ctrl Pts',(-18.8900227704889,-12.9276763536373,
0.));
#231796=CARTESIAN_POINT('Ctrl Pts',(-18.8900227704889,-12.9276763536373,
12.));
#231797=CARTESIAN_POINT('Ctrl Pts',(-18.9016841423403,-12.9329766328185,
0.));
#231798=CARTESIAN_POINT('Ctrl Pts',(-18.9016841423403,-12.9329766328185,
12.));
#231799=CARTESIAN_POINT('Ctrl Pts',(-18.9135226769465,-12.9383113190375,
0.));
#231800=CARTESIAN_POINT('Ctrl Pts',(-18.9135226769465,-12.9383113190375,
12.));
#231801=CARTESIAN_POINT('Ctrl Pts',(-18.9255366795195,-12.9436786266105,
0.));
#231802=CARTESIAN_POINT('Ctrl Pts',(-18.9255366795195,-12.9436786266105,
12.));
#231803=CARTESIAN_POINT('Ctrl Pts',(-18.9377244950435,-12.9490768151821,
0.));
#231804=CARTESIAN_POINT('Ctrl Pts',(-18.9377244950435,-12.9490768151821,
12.));
#231805=CARTESIAN_POINT('Ctrl Pts',(-18.9500845064715,-12.9545041877377,
0.));
#231806=CARTESIAN_POINT('Ctrl Pts',(-18.9500845064715,-12.9545041877377,
12.));
#231807=CARTESIAN_POINT('Ctrl Pts',(-18.9626151329229,-12.9599590886319,
0.));
#231808=CARTESIAN_POINT('Ctrl Pts',(-18.9626151329229,-12.9599590886319,
12.));
#231809=CARTESIAN_POINT('Ctrl Pts',(-18.9753148284475,-12.9654399021869,
0.));
#231810=CARTESIAN_POINT('Ctrl Pts',(-18.9753148284475,-12.9654399021869,
12.));
#231811=CARTESIAN_POINT('Ctrl Pts',(-18.9881820807586,-12.9709450512747,
0.));
#231812=CARTESIAN_POINT('Ctrl Pts',(-18.9881820807586,-12.9709450512747,
12.));
#231813=CARTESIAN_POINT('Ctrl Pts',(-19.0012154099791,-12.9764729959205,
0.));
#231814=CARTESIAN_POINT('Ctrl Pts',(-19.0012154099791,-12.9764729959205,
12.));
#231815=CARTESIAN_POINT('Ctrl Pts',(-19.0144133673348,-12.9820222318716,
0.));
#231816=CARTESIAN_POINT('Ctrl Pts',(-19.0144133673348,-12.9820222318716,
12.));
#231817=CARTESIAN_POINT('Ctrl Pts',(-19.0277745339908,-12.9875912893003,
0.));
#231818=CARTESIAN_POINT('Ctrl Pts',(-19.0277745339908,-12.9875912893003,
12.));
#231819=CARTESIAN_POINT('Ctrl Pts',(-19.0412975200398,-12.9931787316515,
0.));
#231820=CARTESIAN_POINT('Ctrl Pts',(-19.0412975200398,-12.9931787316515,
12.));
#231821=CARTESIAN_POINT('Ctrl Pts',(-19.0549809634355,-12.9987831544502,
0.));
#231822=CARTESIAN_POINT('Ctrl Pts',(-19.0549809634355,-12.9987831544502,
12.));
#231823=CARTESIAN_POINT('Ctrl Pts',(-19.0688235289437,-13.0044031841381,
0.));
#231824=CARTESIAN_POINT('Ctrl Pts',(-19.0688235289437,-13.0044031841381,
12.));
#231825=CARTESIAN_POINT('Ctrl Pts',(-19.0828239070482,-13.0100374768785,
0.));
#231826=CARTESIAN_POINT('Ctrl Pts',(-19.0828239070482,-13.0100374768785,
12.));
#231827=CARTESIAN_POINT('Ctrl Pts',(-19.0969808131226,-13.0156847176093,
0.));
#231828=CARTESIAN_POINT('Ctrl Pts',(-19.0969808131226,-13.0156847176093,
12.));
#231829=CARTESIAN_POINT('Ctrl Pts',(-19.1112929866308,-13.0213436191326,
0.));
#231830=CARTESIAN_POINT('Ctrl Pts',(-19.1112929866308,-13.0213436191326,
12.));
#231831=CARTESIAN_POINT('Ctrl Pts',(-19.1257591903099,-13.0270129211976,
0.));
#231832=CARTESIAN_POINT('Ctrl Pts',(-19.1257591903099,-13.0270129211976,
12.));
#231833=CARTESIAN_POINT('Ctrl Pts',(-19.1403782093389,-13.0326913895841,
0.));
#231834=CARTESIAN_POINT('Ctrl Pts',(-19.1403782093389,-13.0326913895841,
12.));
#231835=CARTESIAN_POINT('Ctrl Pts',(-19.1551488505233,-13.0383778152072,
0.));
#231836=CARTESIAN_POINT('Ctrl Pts',(-19.1551488505233,-13.0383778152072,
12.));
#231837=CARTESIAN_POINT('Ctrl Pts',(-19.1700699416625,-13.0440710133775,
0.));
#231838=CARTESIAN_POINT('Ctrl Pts',(-19.1700699416625,-13.0440710133775,
12.));
#231839=CARTESIAN_POINT('Ctrl Pts',(-19.1851403308825,-13.0497698230442,
0.));
#231840=CARTESIAN_POINT('Ctrl Pts',(-19.1851403308825,-13.0497698230442,
12.));
#231841=CARTESIAN_POINT('Ctrl Pts',(-19.2003588859771,-13.0554731060537,
0.));
#231842=CARTESIAN_POINT('Ctrl Pts',(-19.2003588859771,-13.0554731060537,
12.));
#231843=CARTESIAN_POINT('Ctrl Pts',(-19.2157244937141,-13.0611797463913,
0.));
#231844=CARTESIAN_POINT('Ctrl Pts',(-19.2157244937141,-13.0611797463913,
12.));
#231845=CARTESIAN_POINT('Ctrl Pts',(-19.2312360592031,-13.0668886494791,
0.));
#231846=CARTESIAN_POINT('Ctrl Pts',(-19.2312360592031,-13.0668886494791,
12.));
#231847=CARTESIAN_POINT('Ctrl Pts',(-19.2468925053988,-13.0725987415856,
0.));
#231848=CARTESIAN_POINT('Ctrl Pts',(-19.2468925053988,-13.0725987415856,
12.));
#231849=CARTESIAN_POINT('Ctrl Pts',(-19.2626927725596,-13.0783089692118,
0.));
#231850=CARTESIAN_POINT('Ctrl Pts',(-19.2626927725596,-13.0783089692118,
12.));
#231851=CARTESIAN_POINT('Ctrl Pts',(-19.2786358177198,-13.0840182984949,
0.));
#231852=CARTESIAN_POINT('Ctrl Pts',(-19.2786358177198,-13.0840182984949,
12.));
#231853=CARTESIAN_POINT('Ctrl Pts',(-19.2947206141246,-13.0897257145969,
0.));
#231854=CARTESIAN_POINT('Ctrl Pts',(-19.2947206141246,-13.0897257145969,
12.));
#231855=CARTESIAN_POINT('Ctrl Pts',(-19.3109461507358,-13.095430221148,
0.));
#231856=CARTESIAN_POINT('Ctrl Pts',(-19.3109461507358,-13.095430221148,
12.));
#231857=CARTESIAN_POINT('Ctrl Pts',(-19.3273114318268,-13.1011308397592,
0.));
#231858=CARTESIAN_POINT('Ctrl Pts',(-19.3273114318268,-13.1011308397592,
12.));
#231859=CARTESIAN_POINT('Ctrl Pts',(-19.3438154765395,-13.1068266095186,
0.));
#231860=CARTESIAN_POINT('Ctrl Pts',(-19.3438154765395,-13.1068266095186,
12.));
#231861=CARTESIAN_POINT('Ctrl Pts',(-19.3604573184516,-13.1125165865021,
0.));
#231862=CARTESIAN_POINT('Ctrl Pts',(-19.3604573184516,-13.1125165865021,
12.));
#231863=CARTESIAN_POINT('Ctrl Pts',(-19.3772360051093,-13.118199843271,
0.));
#231864=CARTESIAN_POINT('Ctrl Pts',(-19.3772360051093,-13.118199843271,
12.));
#231865=CARTESIAN_POINT('Ctrl Pts',(-19.3941505976267,-13.1238754684177,
0.));
#231866=CARTESIAN_POINT('Ctrl Pts',(-19.3941505976267,-13.1238754684177,
12.));
#231867=CARTESIAN_POINT('Ctrl Pts',(-19.4112001703561,-13.1295425661635,
0.));
#231868=CARTESIAN_POINT('Ctrl Pts',(-19.4112001703561,-13.1295425661635,
12.));
#231869=CARTESIAN_POINT('Ctrl Pts',(-19.4283838105265,-13.1352002559439,
0.));
#231870=CARTESIAN_POINT('Ctrl Pts',(-19.4283838105265,-13.1352002559439,
12.));
#231871=CARTESIAN_POINT('Ctrl Pts',(-19.4457006178875,-13.140847672006,
0.));
#231872=CARTESIAN_POINT('Ctrl Pts',(-19.4457006178875,-13.140847672006,
12.));
#231873=CARTESIAN_POINT('Ctrl Pts',(-19.463149704325,-13.1464839629966,
0.));
#231874=CARTESIAN_POINT('Ctrl Pts',(-19.463149704325,-13.1464839629966,
12.));
#231875=CARTESIAN_POINT('Ctrl Pts',(-19.4807301935256,-13.1521082915846,
0.));
#231876=CARTESIAN_POINT('Ctrl Pts',(-19.4807301935256,-13.1521082915846,
12.));
#231877=CARTESIAN_POINT('Ctrl Pts',(-19.498441220707,-13.1577198341238,
0.));
#231878=CARTESIAN_POINT('Ctrl Pts',(-19.498441220707,-13.1577198341238,
12.));
#231879=CARTESIAN_POINT('Ctrl Pts',(-19.5162819323207,-13.1633177803097,
0.));
#231880=CARTESIAN_POINT('Ctrl Pts',(-19.5162819323207,-13.1633177803097,
12.));
#231881=CARTESIAN_POINT('Ctrl Pts',(-19.5342514857564,-13.1689013328432,
0.));
#231882=CARTESIAN_POINT('Ctrl Pts',(-19.5342514857564,-13.1689013328432,
12.));
#231883=CARTESIAN_POINT('Ctrl Pts',(-19.5523490490254,-13.1744697070918,
0.));
#231884=CARTESIAN_POINT('Ctrl Pts',(-19.5523490490254,-13.1744697070918,
12.));
#231885=CARTESIAN_POINT('Ctrl Pts',(-19.5705738004682,-13.1800221307682,
0.));
#231886=CARTESIAN_POINT('Ctrl Pts',(-19.5705738004682,-13.1800221307682,
12.));
#231887=CARTESIAN_POINT('Ctrl Pts',(-19.5889249285352,-13.1855578436479,
0.));
#231888=CARTESIAN_POINT('Ctrl Pts',(-19.5889249285352,-13.1855578436479,
12.));
#231889=CARTESIAN_POINT('Ctrl Pts',(-19.6074016315421,-13.1910760972818,
0.));
#231890=CARTESIAN_POINT('Ctrl Pts',(-19.6074016315421,-13.1910760972818,
12.));
#231891=CARTESIAN_POINT('Ctrl Pts',(-19.6260031174244,-13.196576154715,
0.));
#231892=CARTESIAN_POINT('Ctrl Pts',(-19.6260031174244,-13.196576154715,
12.));
#231893=CARTESIAN_POINT('Ctrl Pts',(-19.6447286034764,-13.202057290206,
0.));
#231894=CARTESIAN_POINT('Ctrl Pts',(-19.6447286034764,-13.202057290206,
12.));
#231895=CARTESIAN_POINT('Ctrl Pts',(-19.6635773160924,-13.2075187889522,
0.));
#231896=CARTESIAN_POINT('Ctrl Pts',(-19.6635773160924,-13.2075187889522,
12.));
#231897=CARTESIAN_POINT('Ctrl Pts',(-19.6825484905812,-13.2129599468478,
0.));
#231898=CARTESIAN_POINT('Ctrl Pts',(-19.6825484905812,-13.2129599468478,
12.));
#231899=CARTESIAN_POINT('Ctrl Pts',(-19.7016413709678,-13.2183800702431,
0.));
#231900=CARTESIAN_POINT('Ctrl Pts',(-19.7016413709678,-13.2183800702431,
12.));
#231901=CARTESIAN_POINT('Ctrl Pts',(-19.7208552097867,-13.2237784757065,
0.));
#231902=CARTESIAN_POINT('Ctrl Pts',(-19.7208552097867,-13.2237784757065,
12.));
#231903=CARTESIAN_POINT('Ctrl Pts',(-19.7401892678701,-13.2291544897902,
0.));
#231904=CARTESIAN_POINT('Ctrl Pts',(-19.7401892678701,-13.2291544897902,
12.));
#231905=CARTESIAN_POINT('Ctrl Pts',(-19.7596428141176,-13.2345074487968,
0.));
#231906=CARTESIAN_POINT('Ctrl Pts',(-19.7596428141176,-13.2345074487968,
12.));
#231907=CARTESIAN_POINT('Ctrl Pts',(-19.7792151253297,-13.239836698568,
0.));
#231908=CARTESIAN_POINT('Ctrl Pts',(-19.7792151253297,-13.239836698568,
12.));
#231909=CARTESIAN_POINT('Ctrl Pts',(-19.7989054860501,-13.2451415942809,
0.));
#231910=CARTESIAN_POINT('Ctrl Pts',(-19.7989054860501,-13.2451415942809,
12.));
#231911=CARTESIAN_POINT('Ctrl Pts',(-19.8187131883919,-13.2504215002458,
0.));
#231912=CARTESIAN_POINT('Ctrl Pts',(-19.8187131883919,-13.2504215002458,
12.));
#231913=CARTESIAN_POINT('Ctrl Pts',(-19.8386375318632,-13.2556757897085,
0.));
#231914=CARTESIAN_POINT('Ctrl Pts',(-19.8386375318632,-13.2556757897085,
12.));
#231915=CARTESIAN_POINT('Ctrl Pts',(-19.8586778231711,-13.2609038446525,
0.));
#231916=CARTESIAN_POINT('Ctrl Pts',(-19.8586778231711,-13.2609038446525,
12.));
#231917=CARTESIAN_POINT('Ctrl Pts',(-19.8788333760571,-13.2661050556128,
0.));
#231918=CARTESIAN_POINT('Ctrl Pts',(-19.8788333760571,-13.2661050556128,
12.));
#231919=CARTESIAN_POINT('Ctrl Pts',(-19.8991035111739,-13.2712788215015,
0.));
#231920=CARTESIAN_POINT('Ctrl Pts',(-19.8991035111739,-13.2712788215015,
12.));
#231921=CARTESIAN_POINT('Ctrl Pts',(-19.9194875559419,-13.2764245494354,
0.));
#231922=CARTESIAN_POINT('Ctrl Pts',(-19.9194875559419,-13.2764245494354,
12.));
#231923=CARTESIAN_POINT('Ctrl Pts',(-19.9399848444019,-13.2815416545663,
0.));
#231924=CARTESIAN_POINT('Ctrl Pts',(-19.9399848444019,-13.2815416545663,
12.));
#231925=CARTESIAN_POINT('Ctrl Pts',(-19.9605947170589,-13.2866295599152,
0.));
#231926=CARTESIAN_POINT('Ctrl Pts',(-19.9605947170589,-13.2866295599152,
12.));
#231927=CARTESIAN_POINT('Ctrl Pts',(-19.9813165207174,-13.2916876962098,
0.));
#231928=CARTESIAN_POINT('Ctrl Pts',(-19.9813165207174,-13.2916876962098,
12.));
#231929=CARTESIAN_POINT('Ctrl Pts',(-20.0021496083742,-13.296715501731,
0.));
#231930=CARTESIAN_POINT('Ctrl Pts',(-20.0021496083742,-13.296715501731,
12.));
#231931=CARTESIAN_POINT('Ctrl Pts',(-20.023093339104,-13.3017124221639,
0.));
#231932=CARTESIAN_POINT('Ctrl Pts',(-20.023093339104,-13.3017124221639,
12.));
#231933=CARTESIAN_POINT('Ctrl Pts',(-20.0441470779345,-13.3066779104515,
0.));
#231934=CARTESIAN_POINT('Ctrl Pts',(-20.0441470779345,-13.3066779104515,
12.));
#231935=CARTESIAN_POINT('Ctrl Pts',(-20.0653101957188,-13.3116114266514,
0.));
#231936=CARTESIAN_POINT('Ctrl Pts',(-20.0653101957188,-13.3116114266514,
12.));
#231937=CARTESIAN_POINT('Ctrl Pts',(-20.0865820689883,-13.3165124377963,
0.));
#231938=CARTESIAN_POINT('Ctrl Pts',(-20.0865820689883,-13.3165124377963,
12.));
#231939=CARTESIAN_POINT('Ctrl Pts',(-20.1079620798377,-13.3213804177588,
0.));
#231940=CARTESIAN_POINT('Ctrl Pts',(-20.1079620798377,-13.3213804177588,
12.));
#231941=CARTESIAN_POINT('Ctrl Pts',(-20.1294496158405,-13.3262148471228,
0.));
#231942=CARTESIAN_POINT('Ctrl Pts',(-20.1294496158405,-13.3262148471228,
12.));
#231943=CARTESIAN_POINT('Ctrl Pts',(-20.1510440699477,-13.3310152130565,
0.));
#231944=CARTESIAN_POINT('Ctrl Pts',(-20.1510440699477,-13.3310152130565,
12.));
#231945=CARTESIAN_POINT('Ctrl Pts',(-20.1727448403818,-13.3357810091903,
0.));
#231946=CARTESIAN_POINT('Ctrl Pts',(-20.1727448403818,-13.3357810091903,
12.));
#231947=CARTESIAN_POINT('Ctrl Pts',(-20.1945513305233,-13.3405117354969,
0.));
#231948=CARTESIAN_POINT('Ctrl Pts',(-20.1945513305233,-13.3405117354969,
12.));
#231949=CARTESIAN_POINT('Ctrl Pts',(-20.2164629487855,-13.3452068981763,
0.));
#231950=CARTESIAN_POINT('Ctrl Pts',(-20.2164629487855,-13.3452068981763,
12.));
#231951=CARTESIAN_POINT('Ctrl Pts',(-20.2384791085354,-13.3498660095382,
0.));
#231952=CARTESIAN_POINT('Ctrl Pts',(-20.2384791085354,-13.3498660095382,
12.));
#231953=CARTESIAN_POINT('Ctrl Pts',(-20.2605992280117,-13.3544885878886,
0.));
#231954=CARTESIAN_POINT('Ctrl Pts',(-20.2605992280117,-13.3544885878886,
12.));
#231955=CARTESIAN_POINT('Ctrl Pts',(-20.2828227302337,-13.3590741574194,
0.));
#231956=CARTESIAN_POINT('Ctrl Pts',(-20.2828227302337,-13.3590741574194,
12.));
#231957=CARTESIAN_POINT('Ctrl Pts',(-20.3051490429049,-13.3636222481017,
0.));
#231958=CARTESIAN_POINT('Ctrl Pts',(-20.3051490429049,-13.3636222481017,
12.));
#231959=CARTESIAN_POINT('Ctrl Pts',(-20.3275775983032,-13.3681323955828,
0.));
#231960=CARTESIAN_POINT('Ctrl Pts',(-20.3275775983032,-13.3681323955828,
12.));
#231961=CARTESIAN_POINT('Ctrl Pts',(-20.3501078331818,-13.3726041410869,
0.));
#231962=CARTESIAN_POINT('Ctrl Pts',(-20.3501078331818,-13.3726041410869,
12.));
#231963=CARTESIAN_POINT('Ctrl Pts',(-20.3727391887187,-13.377037031319,
0.));
#231964=CARTESIAN_POINT('Ctrl Pts',(-20.3727391887187,-13.377037031319,
12.));
#231965=CARTESIAN_POINT('Ctrl Pts',(-20.3954711104505,-13.3814306183721,
0.));
#231966=CARTESIAN_POINT('Ctrl Pts',(-20.3954711104505,-13.3814306183721,
12.));
#231967=CARTESIAN_POINT('Ctrl Pts',(-20.4183030482002,-13.3857844596387,
0.));
#231968=CARTESIAN_POINT('Ctrl Pts',(-20.4183030482002,-13.3857844596387,
12.));
#231969=CARTESIAN_POINT('Ctrl Pts',(-20.4412344560007,-13.3900981177254,
0.));
#231970=CARTESIAN_POINT('Ctrl Pts',(-20.4412344560007,-13.3900981177254,
12.));
#231971=CARTESIAN_POINT('Ctrl Pts',(-20.4642647920038,-13.3943711603739,
0.));
#231972=CARTESIAN_POINT('Ctrl Pts',(-20.4642647920038,-13.3943711603739,
12.));
#231973=CARTESIAN_POINT('Ctrl Pts',(-20.4873935184041,-13.3986031603716,
0.));
#231974=CARTESIAN_POINT('Ctrl Pts',(-20.4873935184041,-13.3986031603716,
12.));
#231975=CARTESIAN_POINT('Ctrl Pts',(-20.5106201013755,-13.4027936954529,
0.));
#231976=CARTESIAN_POINT('Ctrl Pts',(-20.5106201013755,-13.4027936954529,
12.));
#231977=CARTESIAN_POINT('Ctrl Pts',(-20.5339440109958,-13.4069423482076,
0.));
#231978=CARTESIAN_POINT('Ctrl Pts',(-20.5339440109958,-13.4069423482076,
12.));
#231979=CARTESIAN_POINT('Ctrl Pts',(-20.557364721164,-13.4110487059912,
0.));
#231980=CARTESIAN_POINT('Ctrl Pts',(-20.557364721164,-13.4110487059912,
12.));
#231981=CARTESIAN_POINT('Ctrl Pts',(-20.5808817095155,-13.4151123608411,
0.));
#231982=CARTESIAN_POINT('Ctrl Pts',(-20.5808817095155,-13.4151123608411,
12.));
#231983=CARTESIAN_POINT('Ctrl Pts',(-20.6044944573151,-13.4191329093932,
0.));
#231984=CARTESIAN_POINT('Ctrl Pts',(-20.6044944573151,-13.4191329093932,
12.));
#231985=CARTESIAN_POINT('Ctrl Pts',(-20.6282024494234,-13.4231099528178,
0.));
#231986=CARTESIAN_POINT('Ctrl Pts',(-20.6282024494234,-13.4231099528178,
12.));
#231987=CARTESIAN_POINT('Ctrl Pts',(-20.6520051742868,-13.427043096765,
0.));
#231988=CARTESIAN_POINT('Ctrl Pts',(-20.6520051742868,-13.427043096765,
12.));
#231989=CARTESIAN_POINT('Ctrl Pts',(-20.6759021239102,-13.4309319513119,
0.));
#231990=CARTESIAN_POINT('Ctrl Pts',(-20.6759021239102,-13.4309319513119,
12.));
#231991=CARTESIAN_POINT('Ctrl Pts',(-20.6998927938288,-13.4347761309154,
0.));
#231992=CARTESIAN_POINT('Ctrl Pts',(-20.6998927938288,-13.4347761309154,
12.));
#231993=CARTESIAN_POINT('Ctrl Pts',(-20.7239766830675,-13.4385752543663,
0.));
#231994=CARTESIAN_POINT('Ctrl Pts',(-20.7239766830675,-13.4385752543663,
12.));
#231995=CARTESIAN_POINT('Ctrl Pts',(-20.7481532941014,-13.4423289447561,
0.));
#231996=CARTESIAN_POINT('Ctrl Pts',(-20.7481532941014,-13.4423289447561,
12.));
#231997=CARTESIAN_POINT('Ctrl Pts',(-20.7724221327609,-13.4460368293689,
0.));
#231998=CARTESIAN_POINT('Ctrl Pts',(-20.7724221327609,-13.4460368293689,
12.));
#231999=CARTESIAN_POINT('Ctrl Pts',(-20.7967827081228,-13.4496985395637,
0.));
#232000=CARTESIAN_POINT('Ctrl Pts',(-20.7967827081228,-13.4496985395637,
12.));
#232001=CARTESIAN_POINT('Ctrl Pts',(-20.821234532398,-13.4533137106667,
0.));
#232002=CARTESIAN_POINT('Ctrl Pts',(-20.821234532398,-13.4533137106667,
12.));
#232003=CARTESIAN_POINT('Ctrl Pts',(-20.8457771208083,-13.4568819818631,
0.));
#232004=CARTESIAN_POINT('Ctrl Pts',(-20.8457771208083,-13.4568819818631,
12.));
#232005=CARTESIAN_POINT('Ctrl Pts',(-20.8704099914641,-13.4604029960983,
0.));
#232006=CARTESIAN_POINT('Ctrl Pts',(-20.8704099914641,-13.4604029960983,
12.));
#232007=CARTESIAN_POINT('Ctrl Pts',(-20.8951326652158,-13.4638763999725,
0.));
#232008=CARTESIAN_POINT('Ctrl Pts',(-20.8951326652158,-13.4638763999725,
12.));
#232009=CARTESIAN_POINT('Ctrl Pts',(-20.9199446657583,-13.4673018437717,
0.));
#232010=CARTESIAN_POINT('Ctrl Pts',(-20.9199446657583,-13.4673018437717,
12.));
#232011=CARTESIAN_POINT('Ctrl Pts',(-20.9448455197557,-13.4706789815166,
0.));
#232012=CARTESIAN_POINT('Ctrl Pts',(-20.9448455197557,-13.4706789815166,
12.));
#232013=CARTESIAN_POINT('Ctrl Pts',(-20.9698347569477,-13.4740074710086,
0.));
#232014=CARTESIAN_POINT('Ctrl Pts',(-20.9698347569477,-13.4740074710086,
12.));
#232015=CARTESIAN_POINT('Ctrl Pts',(-20.9949119102592,-13.4772869738879,
0.));
#232016=CARTESIAN_POINT('Ctrl Pts',(-20.9949119102592,-13.4772869738879,
12.));
#232017=CARTESIAN_POINT('Ctrl Pts',(-21.0200765158884,-13.4805171556822,
0.));
#232018=CARTESIAN_POINT('Ctrl Pts',(-21.0200765158884,-13.4805171556822,
12.));
#232019=CARTESIAN_POINT('Ctrl Pts',(-21.0453281134245,-13.4836976858912,
0.));
#232020=CARTESIAN_POINT('Ctrl Pts',(-21.0453281134245,-13.4836976858912,
12.));
#232021=CARTESIAN_POINT('Ctrl Pts',(-21.0706662455199,-13.4868282377191,
0.));
#232022=CARTESIAN_POINT('Ctrl Pts',(-21.0706662455199,-13.4868282377191,
12.));
#232023=CARTESIAN_POINT('Ctrl Pts',(-21.0960904575046,-13.4899084877717,
0.));
#232024=CARTESIAN_POINT('Ctrl Pts',(-21.0960904575046,-13.4899084877717,
12.));
#232025=CARTESIAN_POINT('Ctrl Pts',(-21.1216002970207,-13.4929381157778,
0.));
#232026=CARTESIAN_POINT('Ctrl Pts',(-21.1216002970207,-13.4929381157778,
12.));
#232027=CARTESIAN_POINT('Ctrl Pts',(-21.1471953136209,-13.4959168042934,
0.));
#232028=CARTESIAN_POINT('Ctrl Pts',(-21.1471953136209,-13.4959168042934,
12.));
#232029=CARTESIAN_POINT('Ctrl Pts',(-21.1728750584175,-13.4988442384491,
0.));
#232030=CARTESIAN_POINT('Ctrl Pts',(-21.1728750584175,-13.4988442384491,
12.));
#232031=CARTESIAN_POINT('Ctrl Pts',(-21.1986390835828,-13.5017201056088,
0.));
#232032=CARTESIAN_POINT('Ctrl Pts',(-21.1986390835828,-13.5017201056088,
12.));
#232033=CARTESIAN_POINT('Ctrl Pts',(-21.2244869429332,-13.5045440957404,
0.));
#232034=CARTESIAN_POINT('Ctrl Pts',(-21.2244869429332,-13.5045440957404,
12.));
#232035=CARTESIAN_POINT('Ctrl Pts',(-21.250418192743,-13.5073159019452,
0.));
#232036=CARTESIAN_POINT('Ctrl Pts',(-21.250418192743,-13.5073159019452,
12.));
#232037=CARTESIAN_POINT('Ctrl Pts',(-21.2764323924442,-13.5100352209205,
0.));
#232038=CARTESIAN_POINT('Ctrl Pts',(-21.2764323924442,-13.5100352209205,
12.));
#232039=CARTESIAN_POINT('Ctrl Pts',(-21.3025291054235,-13.5127017534971,
0.));
#232040=CARTESIAN_POINT('Ctrl Pts',(-21.3025291054235,-13.5127017534971,
12.));
#232041=CARTESIAN_POINT('Ctrl Pts',(-21.3287078996341,-13.5153152050555,
0.));
#232042=CARTESIAN_POINT('Ctrl Pts',(-21.3287078996341,-13.5153152050555,
12.));
#232043=CARTESIAN_POINT('Ctrl Pts',(-21.3549683486222,-13.5178752862466,
0.));
#232044=CARTESIAN_POINT('Ctrl Pts',(-21.3549683486222,-13.5178752862466,
12.));
#232045=CARTESIAN_POINT('Ctrl Pts',(-21.3813100304973,-13.5203817122504,
0.));
#232046=CARTESIAN_POINT('Ctrl Pts',(-21.3813100304973,-13.5203817122504,
12.));
#232047=CARTESIAN_POINT('Ctrl Pts',(-21.4077325259324,-13.5228342013516,
0.));
#232048=CARTESIAN_POINT('Ctrl Pts',(-21.4077325259324,-13.5228342013516,
12.));
#232049=CARTESIAN_POINT('Ctrl Pts',(-21.4342354165259,-13.5252324737802,
0.));
#232050=CARTESIAN_POINT('Ctrl Pts',(-21.4342354165259,-13.5252324737802,
12.));
#232051=CARTESIAN_POINT('Ctrl Pts',(-21.4608182828697,-13.5275762503555,
0.));
#232052=CARTESIAN_POINT('Ctrl Pts',(-21.4608182828697,-13.5275762503555,
12.));
#232053=CARTESIAN_POINT('Ctrl Pts',(-21.4874807030468,-13.5298652514355,
0.));
#232054=CARTESIAN_POINT('Ctrl Pts',(-21.4874807030468,-13.5298652514355,
12.));
#232055=CARTESIAN_POINT('Ctrl Pts',(-21.5142222501666,-13.5320991952138,
0.));
#232056=CARTESIAN_POINT('Ctrl Pts',(-21.5142222501666,-13.5320991952138,
12.));
#232057=CARTESIAN_POINT('Ctrl Pts',(-21.5410424932503,-13.5342777983215,
0.));
#232058=CARTESIAN_POINT('Ctrl Pts',(-21.5410424932503,-13.5342777983215,
12.));
#232059=CARTESIAN_POINT('Ctrl Pts',(-21.5679410019001,-13.536400779028,
0.));
#232060=CARTESIAN_POINT('Ctrl Pts',(-21.5679410019001,-13.536400779028,
12.));
#232061=CARTESIAN_POINT('Ctrl Pts',(-21.5949173499013,-13.5384678597195,
0.));
#232062=CARTESIAN_POINT('Ctrl Pts',(-21.5949173499013,-13.5384678597195,
12.));
#232063=CARTESIAN_POINT('Ctrl Pts',(-21.6219711193946,-13.5404787697792,
0.));
#232064=CARTESIAN_POINT('Ctrl Pts',(-21.6219711193946,-13.5404787697792,
12.));
#232065=CARTESIAN_POINT('Ctrl Pts',(-21.6491019044648,-13.5424332480699,
0.));
#232066=CARTESIAN_POINT('Ctrl Pts',(-21.6491019044648,-13.5424332480699,
12.));
#232067=CARTESIAN_POINT('Ctrl Pts',(-21.6763093157699,-13.5443310461526,
0.));
#232068=CARTESIAN_POINT('Ctrl Pts',(-21.6763093157699,-13.5443310461526,
12.));
#232069=CARTESIAN_POINT('Ctrl Pts',(-21.7035929822955,-13.5461719295048,
0.));
#232070=CARTESIAN_POINT('Ctrl Pts',(-21.7035929822955,-13.5461719295048,
12.));
#232071=CARTESIAN_POINT('Ctrl Pts',(-21.7309525412281,-13.5479556704481,
0.));
#232072=CARTESIAN_POINT('Ctrl Pts',(-21.7309525412281,-13.5479556704481,
12.));
#232073=CARTESIAN_POINT('Ctrl Pts',(-21.7583876294554,-13.5496820422211,
0.));
#232074=CARTESIAN_POINT('Ctrl Pts',(-21.7583876294554,-13.5496820422211,
12.));
#232075=CARTESIAN_POINT('Ctrl Pts',(-21.7858978745865,-13.551350812725,
0.));
#232076=CARTESIAN_POINT('Ctrl Pts',(-21.7858978745865,-13.551350812725,
12.));
#232077=CARTESIAN_POINT('Ctrl Pts',(-21.8134828857967,-13.5529617381573,
0.));
#232078=CARTESIAN_POINT('Ctrl Pts',(-21.8134828857967,-13.5529617381573,
12.));
#232079=CARTESIAN_POINT('Ctrl Pts',(-21.8411422456075,-13.5545145573031,
0.));
#232080=CARTESIAN_POINT('Ctrl Pts',(-21.8411422456075,-13.5545145573031,
12.));
#232081=CARTESIAN_POINT('Ctrl Pts',(-21.8688754989365,-13.5560089839385,
0.));
#232082=CARTESIAN_POINT('Ctrl Pts',(-21.8688754989365,-13.5560089839385,
12.));
#232083=CARTESIAN_POINT('Ctrl Pts',(-21.8966821688824,-13.5574447178424,
0.));
#232084=CARTESIAN_POINT('Ctrl Pts',(-21.8966821688824,-13.5574447178424,
12.));
#232085=CARTESIAN_POINT('Ctrl Pts',(-21.9245617765769,-13.5588214586604,
0.));
#232086=CARTESIAN_POINT('Ctrl Pts',(-21.9245617765769,-13.5588214586604,
12.));
#232087=CARTESIAN_POINT('Ctrl Pts',(-21.9525138592813,-13.5601389185257,
0.));
#232088=CARTESIAN_POINT('Ctrl Pts',(-21.9525138592813,-13.5601389185257,
12.));
#232089=CARTESIAN_POINT('Ctrl Pts',(-21.9805379899168,-13.5613968357561,
0.));
#232090=CARTESIAN_POINT('Ctrl Pts',(-21.9805379899168,-13.5613968357561,
12.));
#232091=CARTESIAN_POINT('Ctrl Pts',(-22.0086337943449,-13.5625949868333,
0.));
#232092=CARTESIAN_POINT('Ctrl Pts',(-22.0086337943449,-13.5625949868333,
12.));
#232093=CARTESIAN_POINT('Ctrl Pts',(-22.0368009736295,-13.5637332022473,
0.));
#232094=CARTESIAN_POINT('Ctrl Pts',(-22.0368009736295,-13.5637332022473,
12.));
#232095=CARTESIAN_POINT('Ctrl Pts',(-22.0650393089609,-13.5648113689033,
0.));
#232096=CARTESIAN_POINT('Ctrl Pts',(-22.0650393089609,-13.5648113689033,
12.));
#232097=CARTESIAN_POINT('Ctrl Pts',(-22.0933486464593,-13.5658294169284,
0.));
#232098=CARTESIAN_POINT('Ctrl Pts',(-22.0933486464593,-13.5658294169284,
12.));
#232099=CARTESIAN_POINT('Ctrl Pts',(-22.1217288871975,-13.5667873105359,
0.));
#232100=CARTESIAN_POINT('Ctrl Pts',(-22.1217288871975,-13.5667873105359,
12.));
#232101=CARTESIAN_POINT('Ctrl Pts',(-22.1444897575194,-13.5675054919061,
0.));
#232102=CARTESIAN_POINT('Ctrl Pts',(-22.1444897575194,-13.5675054919061,
12.));
#232103=CARTESIAN_POINT('Ctrl Pts',(-22.1615922805008,-13.5680170531805,
0.));
#232104=CARTESIAN_POINT('Ctrl Pts',(-22.1615922805008,-13.5680170531805,
12.));
#232105=CARTESIAN_POINT('Ctrl Pts',(-22.1730081264608,-13.5683460612942,
0.));
#232106=CARTESIAN_POINT('Ctrl Pts',(-22.1730081264608,-13.5683460612942,
12.));
#232107=CARTESIAN_POINT('Ctrl Pts',(-22.1787195904339,-13.5685075571671,
0.));
#232108=CARTESIAN_POINT('Ctrl Pts',(-22.1787195904339,-13.5685075571671,
12.));
#232109=CARTESIAN_POINT('',(-22.1787195904339,-13.5685075571671,0.));
#232110=CARTESIAN_POINT('Ctrl Pts',(-18.5896416359912,-12.7689476255363,
0.));
#232111=CARTESIAN_POINT('Ctrl Pts',(-18.5896460962964,-12.7689524524483,
0.));
#232112=CARTESIAN_POINT('Ctrl Pts',(-18.5896919669165,-12.768986426692,
0.));
#232113=CARTESIAN_POINT('Ctrl Pts',(-18.589871621843,-12.769110348199,0.));
#232114=CARTESIAN_POINT('Ctrl Pts',(-18.5903328777227,-12.7694215127919,
0.));
#232115=CARTESIAN_POINT('Ctrl Pts',(-18.5912775137806,-12.7700520897173,
0.));
#232116=CARTESIAN_POINT('Ctrl Pts',(-18.5925859134579,-12.7709195951156,
0.));
#232117=CARTESIAN_POINT('Ctrl Pts',(-18.5942490615407,-12.7720142287172,
0.));
#232118=CARTESIAN_POINT('Ctrl Pts',(-18.5962551167772,-12.7733231262108,
0.));
#232119=CARTESIAN_POINT('Ctrl Pts',(-18.598591752595,-12.7748328937638,
0.));
#232120=CARTESIAN_POINT('Ctrl Pts',(-18.6012488486709,-12.7765325225081,
0.));
#232121=CARTESIAN_POINT('Ctrl Pts',(-18.6042190183704,-12.7784139605066,
0.));
#232122=CARTESIAN_POINT('Ctrl Pts',(-18.6074961535723,-12.7804705387658,
0.));
#232123=CARTESIAN_POINT('Ctrl Pts',(-18.6110744826219,-12.7826959526925,
0.));
#232124=CARTESIAN_POINT('Ctrl Pts',(-18.6149475565188,-12.7850831657901,
0.));
#232125=CARTESIAN_POINT('Ctrl Pts',(-18.6191087624752,-12.7876249657834,
0.));
#232126=CARTESIAN_POINT('Ctrl Pts',(-18.6235516265575,-12.7903142925234,
0.));
#232127=CARTESIAN_POINT('Ctrl Pts',(-18.6282702819371,-12.7931447451555,
0.));
#232128=CARTESIAN_POINT('Ctrl Pts',(-18.6332595057006,-12.7961106222251,
0.));
#232129=CARTESIAN_POINT('Ctrl Pts',(-18.63851447924,-12.7992066625264,0.));
#232130=CARTESIAN_POINT('Ctrl Pts',(-18.6440306327456,-12.8024278770152,
0.));
#232131=CARTESIAN_POINT('Ctrl Pts',(-18.6498034438987,-12.805769331162,
0.));
#232132=CARTESIAN_POINT('Ctrl Pts',(-18.6558284825773,-12.8092261933858,
0.));
#232133=CARTESIAN_POINT('Ctrl Pts',(-18.6621014624746,-12.8127937909631,
0.));
#232134=CARTESIAN_POINT('Ctrl Pts',(-18.6686182952799,-12.8164676687362,
0.));
#232135=CARTESIAN_POINT('Ctrl Pts',(-18.6753751301092,-12.8202436318474,
0.));
#232136=CARTESIAN_POINT('Ctrl Pts',(-18.6823683094139,-12.8241176980017,
0.));
#232137=CARTESIAN_POINT('Ctrl Pts',(-18.6895943376171,-12.8280860635231,
0.));
#232138=CARTESIAN_POINT('Ctrl Pts',(-18.6970498410172,-12.8321450599789,
0.));
#232139=CARTESIAN_POINT('Ctrl Pts',(-18.7047315436294,-12.8362911280361,
0.));
#232140=CARTESIAN_POINT('Ctrl Pts',(-18.7126362754445,-12.8405208263431,
0.));
#232141=CARTESIAN_POINT('Ctrl Pts',(-18.7207609737702,-12.8448308329494,
0.));
#232142=CARTESIAN_POINT('Ctrl Pts',(-18.7291026886554,-12.8492179511591,
0.));
#232143=CARTESIAN_POINT('Ctrl Pts',(-18.7376585820854,-12.8536791086316,
0.));
#232144=CARTESIAN_POINT('Ctrl Pts',(-18.7464259171251,-12.8582113455646,
0.));
#232145=CARTESIAN_POINT('Ctrl Pts',(-18.7554020493887,-12.8628118054171,
0.));
#232146=CARTESIAN_POINT('Ctrl Pts',(-18.7645844169564,-12.8674777239653,
0.));
#232147=CARTESIAN_POINT('Ctrl Pts',(-18.7739705329022,-12.872206421181,
0.));
#232148=CARTESIAN_POINT('Ctrl Pts',(-18.7835579840477,-12.8769952998095,
0.));
#232149=CARTESIAN_POINT('Ctrl Pts',(-18.7933444285868,-12.8818418427475,
0.));
#232150=CARTESIAN_POINT('Ctrl Pts',(-18.8033275941943,-12.8867436109546,
0.));
#232151=CARTESIAN_POINT('Ctrl Pts',(-18.813505275782,-12.8916982409935,
0.));
#232152=CARTESIAN_POINT('Ctrl Pts',(-18.8238753319129,-12.8967034410755,
0.));
#232153=CARTESIAN_POINT('Ctrl Pts',(-18.834435681259,-12.9017569871738,
0.));
#232154=CARTESIAN_POINT('Ctrl Pts',(-18.8451842990984,-12.9068567191854,
0.));
#232155=CARTESIAN_POINT('Ctrl Pts',(-18.8561192136198,-12.9120005369063,
0.));
#232156=CARTESIAN_POINT('Ctrl Pts',(-18.8672385038326,-12.9171863977045,
0.));
#232157=CARTESIAN_POINT('Ctrl Pts',(-18.8785402977527,-12.9224123144982,
0.));
#232158=CARTESIAN_POINT('Ctrl Pts',(-18.8900227704889,-12.9276763536373,
0.));
#232159=CARTESIAN_POINT('Ctrl Pts',(-18.9016841423403,-12.9329766328185,
0.));
#232160=CARTESIAN_POINT('Ctrl Pts',(-18.9135226769465,-12.9383113190375,
0.));
#232161=CARTESIAN_POINT('Ctrl Pts',(-18.9255366795195,-12.9436786266105,
0.));
#232162=CARTESIAN_POINT('Ctrl Pts',(-18.9377244950435,-12.9490768151821,
0.));
#232163=CARTESIAN_POINT('Ctrl Pts',(-18.9500845064715,-12.9545041877377,
0.));
#232164=CARTESIAN_POINT('Ctrl Pts',(-18.9626151329229,-12.9599590886319,
0.));
#232165=CARTESIAN_POINT('Ctrl Pts',(-18.9753148284475,-12.9654399021869,
0.));
#232166=CARTESIAN_POINT('Ctrl Pts',(-18.9881820807586,-12.9709450512747,
0.));
#232167=CARTESIAN_POINT('Ctrl Pts',(-19.0012154099791,-12.9764729959205,
0.));
#232168=CARTESIAN_POINT('Ctrl Pts',(-19.0144133673348,-12.9820222318716,
0.));
#232169=CARTESIAN_POINT('Ctrl Pts',(-19.0277745339908,-12.9875912893003,
0.));
#232170=CARTESIAN_POINT('Ctrl Pts',(-19.0412975200398,-12.9931787316515,
0.));
#232171=CARTESIAN_POINT('Ctrl Pts',(-19.0549809634355,-12.9987831544502,
0.));
#232172=CARTESIAN_POINT('Ctrl Pts',(-19.0688235289437,-13.0044031841381,
0.));
#232173=CARTESIAN_POINT('Ctrl Pts',(-19.0828239070482,-13.0100374768785,
0.));
#232174=CARTESIAN_POINT('Ctrl Pts',(-19.0969808131226,-13.0156847176093,
0.));
#232175=CARTESIAN_POINT('Ctrl Pts',(-19.1112929866308,-13.0213436191326,
0.));
#232176=CARTESIAN_POINT('Ctrl Pts',(-19.1257591903099,-13.0270129211976,
0.));
#232177=CARTESIAN_POINT('Ctrl Pts',(-19.1403782093389,-13.0326913895841,
0.));
#232178=CARTESIAN_POINT('Ctrl Pts',(-19.1551488505233,-13.0383778152072,
0.));
#232179=CARTESIAN_POINT('Ctrl Pts',(-19.1700699416625,-13.0440710133775,
0.));
#232180=CARTESIAN_POINT('Ctrl Pts',(-19.1851403308825,-13.0497698230442,
0.));
#232181=CARTESIAN_POINT('Ctrl Pts',(-19.2003588859771,-13.0554731060537,
0.));
#232182=CARTESIAN_POINT('Ctrl Pts',(-19.2157244937141,-13.0611797463913,
0.));
#232183=CARTESIAN_POINT('Ctrl Pts',(-19.2312360592031,-13.0668886494791,
0.));
#232184=CARTESIAN_POINT('Ctrl Pts',(-19.2468925053988,-13.0725987415856,
0.));
#232185=CARTESIAN_POINT('Ctrl Pts',(-19.2626927725596,-13.0783089692118,
0.));
#232186=CARTESIAN_POINT('Ctrl Pts',(-19.2786358177198,-13.0840182984949,
0.));
#232187=CARTESIAN_POINT('Ctrl Pts',(-19.2947206141246,-13.0897257145969,
0.));
#232188=CARTESIAN_POINT('Ctrl Pts',(-19.3109461507358,-13.095430221148,
0.));
#232189=CARTESIAN_POINT('Ctrl Pts',(-19.3273114318268,-13.1011308397592,
0.));
#232190=CARTESIAN_POINT('Ctrl Pts',(-19.3438154765395,-13.1068266095186,
0.));
#232191=CARTESIAN_POINT('Ctrl Pts',(-19.3604573184516,-13.1125165865021,
0.));
#232192=CARTESIAN_POINT('Ctrl Pts',(-19.3772360051093,-13.118199843271,
0.));
#232193=CARTESIAN_POINT('Ctrl Pts',(-19.3941505976267,-13.1238754684177,
0.));
#232194=CARTESIAN_POINT('Ctrl Pts',(-19.4112001703561,-13.1295425661635,
0.));
#232195=CARTESIAN_POINT('Ctrl Pts',(-19.4283838105265,-13.1352002559439,
0.));
#232196=CARTESIAN_POINT('Ctrl Pts',(-19.4457006178875,-13.140847672006,
0.));
#232197=CARTESIAN_POINT('Ctrl Pts',(-19.463149704325,-13.1464839629966,
0.));
#232198=CARTESIAN_POINT('Ctrl Pts',(-19.4807301935256,-13.1521082915846,
0.));
#232199=CARTESIAN_POINT('Ctrl Pts',(-19.498441220707,-13.1577198341238,
0.));
#232200=CARTESIAN_POINT('Ctrl Pts',(-19.5162819323207,-13.1633177803097,
0.));
#232201=CARTESIAN_POINT('Ctrl Pts',(-19.5342514857564,-13.1689013328432,
0.));
#232202=CARTESIAN_POINT('Ctrl Pts',(-19.5523490490254,-13.1744697070918,
0.));
#232203=CARTESIAN_POINT('Ctrl Pts',(-19.5705738004682,-13.1800221307682,
0.));
#232204=CARTESIAN_POINT('Ctrl Pts',(-19.5889249285352,-13.1855578436479,
0.));
#232205=CARTESIAN_POINT('Ctrl Pts',(-19.6074016315421,-13.1910760972818,
0.));
#232206=CARTESIAN_POINT('Ctrl Pts',(-19.6260031174244,-13.196576154715,
0.));
#232207=CARTESIAN_POINT('Ctrl Pts',(-19.6447286034764,-13.202057290206,
0.));
#232208=CARTESIAN_POINT('Ctrl Pts',(-19.6635773160924,-13.2075187889522,
0.));
#232209=CARTESIAN_POINT('Ctrl Pts',(-19.6825484905812,-13.2129599468478,
0.));
#232210=CARTESIAN_POINT('Ctrl Pts',(-19.7016413709678,-13.2183800702431,
0.));
#232211=CARTESIAN_POINT('Ctrl Pts',(-19.7208552097867,-13.2237784757065,
0.));
#232212=CARTESIAN_POINT('Ctrl Pts',(-19.7401892678701,-13.2291544897902,
0.));
#232213=CARTESIAN_POINT('Ctrl Pts',(-19.7596428141176,-13.2345074487968,
0.));
#232214=CARTESIAN_POINT('Ctrl Pts',(-19.7792151253297,-13.239836698568,
0.));
#232215=CARTESIAN_POINT('Ctrl Pts',(-19.7989054860501,-13.2451415942809,
0.));
#232216=CARTESIAN_POINT('Ctrl Pts',(-19.8187131883919,-13.2504215002458,
0.));
#232217=CARTESIAN_POINT('Ctrl Pts',(-19.8386375318632,-13.2556757897085,
0.));
#232218=CARTESIAN_POINT('Ctrl Pts',(-19.8586778231711,-13.2609038446525,
0.));
#232219=CARTESIAN_POINT('Ctrl Pts',(-19.8788333760571,-13.2661050556128,
0.));
#232220=CARTESIAN_POINT('Ctrl Pts',(-19.8991035111739,-13.2712788215015,
0.));
#232221=CARTESIAN_POINT('Ctrl Pts',(-19.9194875559419,-13.2764245494354,
0.));
#232222=CARTESIAN_POINT('Ctrl Pts',(-19.9399848444019,-13.2815416545663,
0.));
#232223=CARTESIAN_POINT('Ctrl Pts',(-19.9605947170589,-13.2866295599152,
0.));
#232224=CARTESIAN_POINT('Ctrl Pts',(-19.9813165207174,-13.2916876962098,
0.));
#232225=CARTESIAN_POINT('Ctrl Pts',(-20.0021496083742,-13.296715501731,
0.));
#232226=CARTESIAN_POINT('Ctrl Pts',(-20.023093339104,-13.3017124221639,
0.));
#232227=CARTESIAN_POINT('Ctrl Pts',(-20.0441470779345,-13.3066779104515,
0.));
#232228=CARTESIAN_POINT('Ctrl Pts',(-20.0653101957188,-13.3116114266514,
0.));
#232229=CARTESIAN_POINT('Ctrl Pts',(-20.0865820689883,-13.3165124377963,
0.));
#232230=CARTESIAN_POINT('Ctrl Pts',(-20.1079620798377,-13.3213804177588,
0.));
#232231=CARTESIAN_POINT('Ctrl Pts',(-20.1294496158405,-13.3262148471228,
0.));
#232232=CARTESIAN_POINT('Ctrl Pts',(-20.1510440699477,-13.3310152130565,
0.));
#232233=CARTESIAN_POINT('Ctrl Pts',(-20.1727448403818,-13.3357810091903,
0.));
#232234=CARTESIAN_POINT('Ctrl Pts',(-20.1945513305233,-13.3405117354969,
0.));
#232235=CARTESIAN_POINT('Ctrl Pts',(-20.2164629487855,-13.3452068981763,
0.));
#232236=CARTESIAN_POINT('Ctrl Pts',(-20.2384791085354,-13.3498660095382,
0.));
#232237=CARTESIAN_POINT('Ctrl Pts',(-20.2605992280117,-13.3544885878886,
0.));
#232238=CARTESIAN_POINT('Ctrl Pts',(-20.2828227302337,-13.3590741574194,
0.));
#232239=CARTESIAN_POINT('Ctrl Pts',(-20.3051490429049,-13.3636222481017,
0.));
#232240=CARTESIAN_POINT('Ctrl Pts',(-20.3275775983032,-13.3681323955828,
0.));
#232241=CARTESIAN_POINT('Ctrl Pts',(-20.3501078331818,-13.3726041410869,
0.));
#232242=CARTESIAN_POINT('Ctrl Pts',(-20.3727391887187,-13.377037031319,
0.));
#232243=CARTESIAN_POINT('Ctrl Pts',(-20.3954711104505,-13.3814306183721,
0.));
#232244=CARTESIAN_POINT('Ctrl Pts',(-20.4183030482002,-13.3857844596387,
0.));
#232245=CARTESIAN_POINT('Ctrl Pts',(-20.4412344560007,-13.3900981177254,
0.));
#232246=CARTESIAN_POINT('Ctrl Pts',(-20.4642647920038,-13.3943711603739,
0.));
#232247=CARTESIAN_POINT('Ctrl Pts',(-20.4873935184041,-13.3986031603716,
0.));
#232248=CARTESIAN_POINT('Ctrl Pts',(-20.5106201013755,-13.4027936954529,
0.));
#232249=CARTESIAN_POINT('Ctrl Pts',(-20.5339440109958,-13.4069423482076,
0.));
#232250=CARTESIAN_POINT('Ctrl Pts',(-20.557364721164,-13.4110487059912,
0.));
#232251=CARTESIAN_POINT('Ctrl Pts',(-20.5808817095155,-13.4151123608411,
0.));
#232252=CARTESIAN_POINT('Ctrl Pts',(-20.6044944573151,-13.4191329093932,
0.));
#232253=CARTESIAN_POINT('Ctrl Pts',(-20.6282024494234,-13.4231099528178,
0.));
#232254=CARTESIAN_POINT('Ctrl Pts',(-20.6520051742868,-13.427043096765,
0.));
#232255=CARTESIAN_POINT('Ctrl Pts',(-20.6759021239102,-13.4309319513119,
0.));
#232256=CARTESIAN_POINT('Ctrl Pts',(-20.6998927938288,-13.4347761309154,
0.));
#232257=CARTESIAN_POINT('Ctrl Pts',(-20.7239766830675,-13.4385752543663,
0.));
#232258=CARTESIAN_POINT('Ctrl Pts',(-20.7481532941014,-13.4423289447561,
0.));
#232259=CARTESIAN_POINT('Ctrl Pts',(-20.7724221327609,-13.4460368293689,
0.));
#232260=CARTESIAN_POINT('Ctrl Pts',(-20.7967827081228,-13.4496985395637,
0.));
#232261=CARTESIAN_POINT('Ctrl Pts',(-20.821234532398,-13.4533137106667,
0.));
#232262=CARTESIAN_POINT('Ctrl Pts',(-20.8457771208083,-13.4568819818631,
0.));
#232263=CARTESIAN_POINT('Ctrl Pts',(-20.8704099914641,-13.4604029960983,
0.));
#232264=CARTESIAN_POINT('Ctrl Pts',(-20.8951326652158,-13.4638763999725,
0.));
#232265=CARTESIAN_POINT('Ctrl Pts',(-20.9199446657583,-13.4673018437717,
0.));
#232266=CARTESIAN_POINT('Ctrl Pts',(-20.9448455197557,-13.4706789815166,
0.));
#232267=CARTESIAN_POINT('Ctrl Pts',(-20.9698347569477,-13.4740074710086,
0.));
#232268=CARTESIAN_POINT('Ctrl Pts',(-20.9949119102592,-13.4772869738879,
0.));
#232269=CARTESIAN_POINT('Ctrl Pts',(-21.0200765158884,-13.4805171556822,
0.));
#232270=CARTESIAN_POINT('Ctrl Pts',(-21.0453281134245,-13.4836976858912,
0.));
#232271=CARTESIAN_POINT('Ctrl Pts',(-21.0706662455199,-13.4868282377191,
0.));
#232272=CARTESIAN_POINT('Ctrl Pts',(-21.0960904575046,-13.4899084877717,
0.));
#232273=CARTESIAN_POINT('Ctrl Pts',(-21.1216002970207,-13.4929381157778,
0.));
#232274=CARTESIAN_POINT('Ctrl Pts',(-21.1471953136209,-13.4959168042934,
0.));
#232275=CARTESIAN_POINT('Ctrl Pts',(-21.1728750584175,-13.4988442384491,
0.));
#232276=CARTESIAN_POINT('Ctrl Pts',(-21.1986390835828,-13.5017201056088,
0.));
#232277=CARTESIAN_POINT('Ctrl Pts',(-21.2244869429332,-13.5045440957404,
0.));
#232278=CARTESIAN_POINT('Ctrl Pts',(-21.250418192743,-13.5073159019452,
0.));
#232279=CARTESIAN_POINT('Ctrl Pts',(-21.2764323924442,-13.5100352209205,
0.));
#232280=CARTESIAN_POINT('Ctrl Pts',(-21.3025291054235,-13.5127017534971,
0.));
#232281=CARTESIAN_POINT('Ctrl Pts',(-21.3287078996341,-13.5153152050555,
0.));
#232282=CARTESIAN_POINT('Ctrl Pts',(-21.3549683486222,-13.5178752862466,
0.));
#232283=CARTESIAN_POINT('Ctrl Pts',(-21.3813100304973,-13.5203817122504,
0.));
#232284=CARTESIAN_POINT('Ctrl Pts',(-21.4077325259324,-13.5228342013516,
0.));
#232285=CARTESIAN_POINT('Ctrl Pts',(-21.4342354165259,-13.5252324737802,
0.));
#232286=CARTESIAN_POINT('Ctrl Pts',(-21.4608182828697,-13.5275762503555,
0.));
#232287=CARTESIAN_POINT('Ctrl Pts',(-21.4874807030468,-13.5298652514355,
0.));
#232288=CARTESIAN_POINT('Ctrl Pts',(-21.5142222501666,-13.5320991952138,
0.));
#232289=CARTESIAN_POINT('Ctrl Pts',(-21.5410424932503,-13.5342777983215,
0.));
#232290=CARTESIAN_POINT('Ctrl Pts',(-21.5679410019001,-13.536400779028,
0.));
#232291=CARTESIAN_POINT('Ctrl Pts',(-21.5949173499013,-13.5384678597195,
0.));
#232292=CARTESIAN_POINT('Ctrl Pts',(-21.6219711193946,-13.5404787697792,
0.));
#232293=CARTESIAN_POINT('Ctrl Pts',(-21.6491019044648,-13.5424332480699,
0.));
#232294=CARTESIAN_POINT('Ctrl Pts',(-21.6763093157699,-13.5443310461526,
0.));
#232295=CARTESIAN_POINT('Ctrl Pts',(-21.7035929822955,-13.5461719295048,
0.));
#232296=CARTESIAN_POINT('Ctrl Pts',(-21.7309525412281,-13.5479556704481,
0.));
#232297=CARTESIAN_POINT('Ctrl Pts',(-21.7583876294554,-13.5496820422211,
0.));
#232298=CARTESIAN_POINT('Ctrl Pts',(-21.7858978745865,-13.551350812725,
0.));
#232299=CARTESIAN_POINT('Ctrl Pts',(-21.8134828857967,-13.5529617381573,
0.));
#232300=CARTESIAN_POINT('Ctrl Pts',(-21.8411422456075,-13.5545145573031,
0.));
#232301=CARTESIAN_POINT('Ctrl Pts',(-21.8688754989365,-13.5560089839385,
0.));
#232302=CARTESIAN_POINT('Ctrl Pts',(-21.8966821688824,-13.5574447178424,
0.));
#232303=CARTESIAN_POINT('Ctrl Pts',(-21.9245617765769,-13.5588214586604,
0.));
#232304=CARTESIAN_POINT('Ctrl Pts',(-21.9525138592813,-13.5601389185257,
0.));
#232305=CARTESIAN_POINT('Ctrl Pts',(-21.9805379899168,-13.5613968357561,
0.));
#232306=CARTESIAN_POINT('Ctrl Pts',(-22.0086337943449,-13.5625949868333,
0.));
#232307=CARTESIAN_POINT('Ctrl Pts',(-22.0368009736295,-13.5637332022473,
0.));
#232308=CARTESIAN_POINT('Ctrl Pts',(-22.0650393089609,-13.5648113689033,
0.));
#232309=CARTESIAN_POINT('Ctrl Pts',(-22.0933486464593,-13.5658294169284,
0.));
#232310=CARTESIAN_POINT('Ctrl Pts',(-22.1217288871975,-13.5667873105359,
0.));
#232311=CARTESIAN_POINT('Ctrl Pts',(-22.1444897575194,-13.5675054919061,
0.));
#232312=CARTESIAN_POINT('Ctrl Pts',(-22.1615922805008,-13.5680170531805,
0.));
#232313=CARTESIAN_POINT('Ctrl Pts',(-22.1730081264608,-13.5683460612942,
0.));
#232314=CARTESIAN_POINT('Ctrl Pts',(-22.1787195904339,-13.5685075571671,
0.));
#232315=CARTESIAN_POINT('',(-22.1787195904339,-13.5685075571671,12.));
#232316=CARTESIAN_POINT('Ctrl Pts',(-22.1787195904339,-13.5685075571671,
12.));
#232317=CARTESIAN_POINT('Ctrl Pts',(-22.1730081264608,-13.5683460612942,
12.));
#232318=CARTESIAN_POINT('Ctrl Pts',(-22.1615922805008,-13.5680170531805,
12.));
#232319=CARTESIAN_POINT('Ctrl Pts',(-22.1444897575194,-13.5675054919061,
12.));
#232320=CARTESIAN_POINT('Ctrl Pts',(-22.1217288871975,-13.5667873105359,
12.));
#232321=CARTESIAN_POINT('Ctrl Pts',(-22.0933486464593,-13.5658294169284,
12.));
#232322=CARTESIAN_POINT('Ctrl Pts',(-22.0650393089609,-13.5648113689033,
12.));
#232323=CARTESIAN_POINT('Ctrl Pts',(-22.0368009736295,-13.5637332022473,
12.));
#232324=CARTESIAN_POINT('Ctrl Pts',(-22.0086337943449,-13.5625949868333,
12.));
#232325=CARTESIAN_POINT('Ctrl Pts',(-21.9805379899168,-13.5613968357561,
12.));
#232326=CARTESIAN_POINT('Ctrl Pts',(-21.9525138592813,-13.5601389185257,
12.));
#232327=CARTESIAN_POINT('Ctrl Pts',(-21.9245617765769,-13.5588214586604,
12.));
#232328=CARTESIAN_POINT('Ctrl Pts',(-21.8966821688824,-13.5574447178424,
12.));
#232329=CARTESIAN_POINT('Ctrl Pts',(-21.8688754989365,-13.5560089839385,
12.));
#232330=CARTESIAN_POINT('Ctrl Pts',(-21.8411422456075,-13.5545145573031,
12.));
#232331=CARTESIAN_POINT('Ctrl Pts',(-21.8134828857967,-13.5529617381573,
12.));
#232332=CARTESIAN_POINT('Ctrl Pts',(-21.7858978745865,-13.551350812725,
12.));
#232333=CARTESIAN_POINT('Ctrl Pts',(-21.7583876294554,-13.5496820422211,
12.));
#232334=CARTESIAN_POINT('Ctrl Pts',(-21.7309525412281,-13.5479556704481,
12.));
#232335=CARTESIAN_POINT('Ctrl Pts',(-21.7035929822955,-13.5461719295048,
12.));
#232336=CARTESIAN_POINT('Ctrl Pts',(-21.6763093157699,-13.5443310461526,
12.));
#232337=CARTESIAN_POINT('Ctrl Pts',(-21.6491019044648,-13.5424332480699,
12.));
#232338=CARTESIAN_POINT('Ctrl Pts',(-21.6219711193946,-13.5404787697792,
12.));
#232339=CARTESIAN_POINT('Ctrl Pts',(-21.5949173499013,-13.5384678597195,
12.));
#232340=CARTESIAN_POINT('Ctrl Pts',(-21.5679410019001,-13.536400779028,
12.));
#232341=CARTESIAN_POINT('Ctrl Pts',(-21.5410424932503,-13.5342777983215,
12.));
#232342=CARTESIAN_POINT('Ctrl Pts',(-21.5142222501666,-13.5320991952138,
12.));
#232343=CARTESIAN_POINT('Ctrl Pts',(-21.4874807030468,-13.5298652514355,
12.));
#232344=CARTESIAN_POINT('Ctrl Pts',(-21.4608182828697,-13.5275762503555,
12.));
#232345=CARTESIAN_POINT('Ctrl Pts',(-21.4342354165259,-13.5252324737802,
12.));
#232346=CARTESIAN_POINT('Ctrl Pts',(-21.4077325259324,-13.5228342013516,
12.));
#232347=CARTESIAN_POINT('Ctrl Pts',(-21.3813100304973,-13.5203817122504,
12.));
#232348=CARTESIAN_POINT('Ctrl Pts',(-21.3549683486222,-13.5178752862466,
12.));
#232349=CARTESIAN_POINT('Ctrl Pts',(-21.3287078996341,-13.5153152050555,
12.));
#232350=CARTESIAN_POINT('Ctrl Pts',(-21.3025291054235,-13.5127017534971,
12.));
#232351=CARTESIAN_POINT('Ctrl Pts',(-21.2764323924442,-13.5100352209205,
12.));
#232352=CARTESIAN_POINT('Ctrl Pts',(-21.250418192743,-13.5073159019452,
12.));
#232353=CARTESIAN_POINT('Ctrl Pts',(-21.2244869429332,-13.5045440957404,
12.));
#232354=CARTESIAN_POINT('Ctrl Pts',(-21.1986390835828,-13.5017201056088,
12.));
#232355=CARTESIAN_POINT('Ctrl Pts',(-21.1728750584175,-13.4988442384491,
12.));
#232356=CARTESIAN_POINT('Ctrl Pts',(-21.1471953136209,-13.4959168042934,
12.));
#232357=CARTESIAN_POINT('Ctrl Pts',(-21.1216002970207,-13.4929381157778,
12.));
#232358=CARTESIAN_POINT('Ctrl Pts',(-21.0960904575046,-13.4899084877717,
12.));
#232359=CARTESIAN_POINT('Ctrl Pts',(-21.0706662455199,-13.4868282377191,
12.));
#232360=CARTESIAN_POINT('Ctrl Pts',(-21.0453281134245,-13.4836976858912,
12.));
#232361=CARTESIAN_POINT('Ctrl Pts',(-21.0200765158884,-13.4805171556822,
12.));
#232362=CARTESIAN_POINT('Ctrl Pts',(-20.9949119102592,-13.4772869738879,
12.));
#232363=CARTESIAN_POINT('Ctrl Pts',(-20.9698347569477,-13.4740074710086,
12.));
#232364=CARTESIAN_POINT('Ctrl Pts',(-20.9448455197557,-13.4706789815166,
12.));
#232365=CARTESIAN_POINT('Ctrl Pts',(-20.9199446657583,-13.4673018437717,
12.));
#232366=CARTESIAN_POINT('Ctrl Pts',(-20.8951326652158,-13.4638763999725,
12.));
#232367=CARTESIAN_POINT('Ctrl Pts',(-20.8704099914641,-13.4604029960983,
12.));
#232368=CARTESIAN_POINT('Ctrl Pts',(-20.8457771208083,-13.4568819818631,
12.));
#232369=CARTESIAN_POINT('Ctrl Pts',(-20.821234532398,-13.4533137106667,
12.));
#232370=CARTESIAN_POINT('Ctrl Pts',(-20.7967827081228,-13.4496985395637,
12.));
#232371=CARTESIAN_POINT('Ctrl Pts',(-20.7724221327609,-13.4460368293689,
12.));
#232372=CARTESIAN_POINT('Ctrl Pts',(-20.7481532941014,-13.4423289447561,
12.));
#232373=CARTESIAN_POINT('Ctrl Pts',(-20.7239766830675,-13.4385752543663,
12.));
#232374=CARTESIAN_POINT('Ctrl Pts',(-20.6998927938288,-13.4347761309154,
12.));
#232375=CARTESIAN_POINT('Ctrl Pts',(-20.6759021239102,-13.4309319513119,
12.));
#232376=CARTESIAN_POINT('Ctrl Pts',(-20.6520051742868,-13.427043096765,
12.));
#232377=CARTESIAN_POINT('Ctrl Pts',(-20.6282024494234,-13.4231099528178,
12.));
#232378=CARTESIAN_POINT('Ctrl Pts',(-20.6044944573151,-13.4191329093932,
12.));
#232379=CARTESIAN_POINT('Ctrl Pts',(-20.5808817095155,-13.4151123608411,
12.));
#232380=CARTESIAN_POINT('Ctrl Pts',(-20.557364721164,-13.4110487059912,
12.));
#232381=CARTESIAN_POINT('Ctrl Pts',(-20.5339440109958,-13.4069423482076,
12.));
#232382=CARTESIAN_POINT('Ctrl Pts',(-20.5106201013755,-13.4027936954529,
12.));
#232383=CARTESIAN_POINT('Ctrl Pts',(-20.4873935184041,-13.3986031603716,
12.));
#232384=CARTESIAN_POINT('Ctrl Pts',(-20.4642647920038,-13.3943711603739,
12.));
#232385=CARTESIAN_POINT('Ctrl Pts',(-20.4412344560007,-13.3900981177254,
12.));
#232386=CARTESIAN_POINT('Ctrl Pts',(-20.4183030482002,-13.3857844596387,
12.));
#232387=CARTESIAN_POINT('Ctrl Pts',(-20.3954711104505,-13.3814306183721,
12.));
#232388=CARTESIAN_POINT('Ctrl Pts',(-20.3727391887187,-13.377037031319,
12.));
#232389=CARTESIAN_POINT('Ctrl Pts',(-20.3501078331818,-13.3726041410869,
12.));
#232390=CARTESIAN_POINT('Ctrl Pts',(-20.3275775983032,-13.3681323955828,
12.));
#232391=CARTESIAN_POINT('Ctrl Pts',(-20.3051490429049,-13.3636222481017,
12.));
#232392=CARTESIAN_POINT('Ctrl Pts',(-20.2828227302337,-13.3590741574194,
12.));
#232393=CARTESIAN_POINT('Ctrl Pts',(-20.2605992280117,-13.3544885878886,
12.));
#232394=CARTESIAN_POINT('Ctrl Pts',(-20.2384791085354,-13.3498660095382,
12.));
#232395=CARTESIAN_POINT('Ctrl Pts',(-20.2164629487855,-13.3452068981763,
12.));
#232396=CARTESIAN_POINT('Ctrl Pts',(-20.1945513305233,-13.3405117354969,
12.));
#232397=CARTESIAN_POINT('Ctrl Pts',(-20.1727448403818,-13.3357810091903,
12.));
#232398=CARTESIAN_POINT('Ctrl Pts',(-20.1510440699477,-13.3310152130565,
12.));
#232399=CARTESIAN_POINT('Ctrl Pts',(-20.1294496158405,-13.3262148471228,
12.));
#232400=CARTESIAN_POINT('Ctrl Pts',(-20.1079620798377,-13.3213804177588,
12.));
#232401=CARTESIAN_POINT('Ctrl Pts',(-20.0865820689883,-13.3165124377963,
12.));
#232402=CARTESIAN_POINT('Ctrl Pts',(-20.0653101957188,-13.3116114266514,
12.));
#232403=CARTESIAN_POINT('Ctrl Pts',(-20.0441470779345,-13.3066779104515,
12.));
#232404=CARTESIAN_POINT('Ctrl Pts',(-20.023093339104,-13.3017124221639,
12.));
#232405=CARTESIAN_POINT('Ctrl Pts',(-20.0021496083742,-13.296715501731,
12.));
#232406=CARTESIAN_POINT('Ctrl Pts',(-19.9813165207174,-13.2916876962098,
12.));
#232407=CARTESIAN_POINT('Ctrl Pts',(-19.9605947170589,-13.2866295599152,
12.));
#232408=CARTESIAN_POINT('Ctrl Pts',(-19.9399848444019,-13.2815416545663,
12.));
#232409=CARTESIAN_POINT('Ctrl Pts',(-19.9194875559419,-13.2764245494354,
12.));
#232410=CARTESIAN_POINT('Ctrl Pts',(-19.8991035111739,-13.2712788215015,
12.));
#232411=CARTESIAN_POINT('Ctrl Pts',(-19.8788333760571,-13.2661050556128,
12.));
#232412=CARTESIAN_POINT('Ctrl Pts',(-19.8586778231711,-13.2609038446525,
12.));
#232413=CARTESIAN_POINT('Ctrl Pts',(-19.8386375318632,-13.2556757897085,
12.));
#232414=CARTESIAN_POINT('Ctrl Pts',(-19.8187131883919,-13.2504215002458,
12.));
#232415=CARTESIAN_POINT('Ctrl Pts',(-19.7989054860501,-13.2451415942809,
12.));
#232416=CARTESIAN_POINT('Ctrl Pts',(-19.7792151253297,-13.239836698568,
12.));
#232417=CARTESIAN_POINT('Ctrl Pts',(-19.7596428141176,-13.2345074487968,
12.));
#232418=CARTESIAN_POINT('Ctrl Pts',(-19.7401892678701,-13.2291544897902,
12.));
#232419=CARTESIAN_POINT('Ctrl Pts',(-19.7208552097867,-13.2237784757065,
12.));
#232420=CARTESIAN_POINT('Ctrl Pts',(-19.7016413709678,-13.2183800702431,
12.));
#232421=CARTESIAN_POINT('Ctrl Pts',(-19.6825484905812,-13.2129599468478,
12.));
#232422=CARTESIAN_POINT('Ctrl Pts',(-19.6635773160924,-13.2075187889522,
12.));
#232423=CARTESIAN_POINT('Ctrl Pts',(-19.6447286034764,-13.202057290206,
12.));
#232424=CARTESIAN_POINT('Ctrl Pts',(-19.6260031174244,-13.196576154715,
12.));
#232425=CARTESIAN_POINT('Ctrl Pts',(-19.6074016315421,-13.1910760972818,
12.));
#232426=CARTESIAN_POINT('Ctrl Pts',(-19.5889249285352,-13.1855578436479,
12.));
#232427=CARTESIAN_POINT('Ctrl Pts',(-19.5705738004682,-13.1800221307682,
12.));
#232428=CARTESIAN_POINT('Ctrl Pts',(-19.5523490490254,-13.1744697070918,
12.));
#232429=CARTESIAN_POINT('Ctrl Pts',(-19.5342514857564,-13.1689013328432,
12.));
#232430=CARTESIAN_POINT('Ctrl Pts',(-19.5162819323207,-13.1633177803097,
12.));
#232431=CARTESIAN_POINT('Ctrl Pts',(-19.498441220707,-13.1577198341238,
12.));
#232432=CARTESIAN_POINT('Ctrl Pts',(-19.4807301935256,-13.1521082915846,
12.));
#232433=CARTESIAN_POINT('Ctrl Pts',(-19.463149704325,-13.1464839629966,
12.));
#232434=CARTESIAN_POINT('Ctrl Pts',(-19.4457006178875,-13.140847672006,
12.));
#232435=CARTESIAN_POINT('Ctrl Pts',(-19.4283838105265,-13.1352002559439,
12.));
#232436=CARTESIAN_POINT('Ctrl Pts',(-19.4112001703561,-13.1295425661635,
12.));
#232437=CARTESIAN_POINT('Ctrl Pts',(-19.3941505976267,-13.1238754684177,
12.));
#232438=CARTESIAN_POINT('Ctrl Pts',(-19.3772360051093,-13.118199843271,
12.));
#232439=CARTESIAN_POINT('Ctrl Pts',(-19.3604573184516,-13.1125165865021,
12.));
#232440=CARTESIAN_POINT('Ctrl Pts',(-19.3438154765395,-13.1068266095186,
12.));
#232441=CARTESIAN_POINT('Ctrl Pts',(-19.3273114318268,-13.1011308397592,
12.));
#232442=CARTESIAN_POINT('Ctrl Pts',(-19.3109461507358,-13.095430221148,
12.));
#232443=CARTESIAN_POINT('Ctrl Pts',(-19.2947206141246,-13.0897257145969,
12.));
#232444=CARTESIAN_POINT('Ctrl Pts',(-19.2786358177198,-13.0840182984949,
12.));
#232445=CARTESIAN_POINT('Ctrl Pts',(-19.2626927725596,-13.0783089692118,
12.));
#232446=CARTESIAN_POINT('Ctrl Pts',(-19.2468925053988,-13.0725987415856,
12.));
#232447=CARTESIAN_POINT('Ctrl Pts',(-19.2312360592031,-13.0668886494791,
12.));
#232448=CARTESIAN_POINT('Ctrl Pts',(-19.2157244937141,-13.0611797463913,
12.));
#232449=CARTESIAN_POINT('Ctrl Pts',(-19.2003588859771,-13.0554731060537,
12.));
#232450=CARTESIAN_POINT('Ctrl Pts',(-19.1851403308825,-13.0497698230442,
12.));
#232451=CARTESIAN_POINT('Ctrl Pts',(-19.1700699416625,-13.0440710133775,
12.));
#232452=CARTESIAN_POINT('Ctrl Pts',(-19.1551488505233,-13.0383778152072,
12.));
#232453=CARTESIAN_POINT('Ctrl Pts',(-19.1403782093389,-13.0326913895841,
12.));
#232454=CARTESIAN_POINT('Ctrl Pts',(-19.1257591903099,-13.0270129211976,
12.));
#232455=CARTESIAN_POINT('Ctrl Pts',(-19.1112929866308,-13.0213436191326,
12.));
#232456=CARTESIAN_POINT('Ctrl Pts',(-19.0969808131226,-13.0156847176093,
12.));
#232457=CARTESIAN_POINT('Ctrl Pts',(-19.0828239070482,-13.0100374768785,
12.));
#232458=CARTESIAN_POINT('Ctrl Pts',(-19.0688235289437,-13.0044031841381,
12.));
#232459=CARTESIAN_POINT('Ctrl Pts',(-19.0549809634355,-12.9987831544502,
12.));
#232460=CARTESIAN_POINT('Ctrl Pts',(-19.0412975200398,-12.9931787316515,
12.));
#232461=CARTESIAN_POINT('Ctrl Pts',(-19.0277745339908,-12.9875912893003,
12.));
#232462=CARTESIAN_POINT('Ctrl Pts',(-19.0144133673348,-12.9820222318716,
12.));
#232463=CARTESIAN_POINT('Ctrl Pts',(-19.0012154099791,-12.9764729959205,
12.));
#232464=CARTESIAN_POINT('Ctrl Pts',(-18.9881820807586,-12.9709450512747,
12.));
#232465=CARTESIAN_POINT('Ctrl Pts',(-18.9753148284475,-12.9654399021869,
12.));
#232466=CARTESIAN_POINT('Ctrl Pts',(-18.9626151329229,-12.9599590886319,
12.));
#232467=CARTESIAN_POINT('Ctrl Pts',(-18.9500845064715,-12.9545041877377,
12.));
#232468=CARTESIAN_POINT('Ctrl Pts',(-18.9377244950435,-12.9490768151821,
12.));
#232469=CARTESIAN_POINT('Ctrl Pts',(-18.9255366795195,-12.9436786266105,
12.));
#232470=CARTESIAN_POINT('Ctrl Pts',(-18.9135226769465,-12.9383113190375,
12.));
#232471=CARTESIAN_POINT('Ctrl Pts',(-18.9016841423403,-12.9329766328185,
12.));
#232472=CARTESIAN_POINT('Ctrl Pts',(-18.8900227704889,-12.9276763536373,
12.));
#232473=CARTESIAN_POINT('Ctrl Pts',(-18.8785402977527,-12.9224123144982,
12.));
#232474=CARTESIAN_POINT('Ctrl Pts',(-18.8672385038326,-12.9171863977045,
12.));
#232475=CARTESIAN_POINT('Ctrl Pts',(-18.8561192136198,-12.9120005369063,
12.));
#232476=CARTESIAN_POINT('Ctrl Pts',(-18.8451842990984,-12.9068567191854,
12.));
#232477=CARTESIAN_POINT('Ctrl Pts',(-18.834435681259,-12.9017569871738,
12.));
#232478=CARTESIAN_POINT('Ctrl Pts',(-18.8238753319129,-12.8967034410755,
12.));
#232479=CARTESIAN_POINT('Ctrl Pts',(-18.813505275782,-12.8916982409935,
12.));
#232480=CARTESIAN_POINT('Ctrl Pts',(-18.8033275941943,-12.8867436109546,
12.));
#232481=CARTESIAN_POINT('Ctrl Pts',(-18.7933444285868,-12.8818418427475,
12.));
#232482=CARTESIAN_POINT('Ctrl Pts',(-18.7835579840477,-12.8769952998095,
12.));
#232483=CARTESIAN_POINT('Ctrl Pts',(-18.7739705329022,-12.872206421181,
12.));
#232484=CARTESIAN_POINT('Ctrl Pts',(-18.7645844169564,-12.8674777239653,
12.));
#232485=CARTESIAN_POINT('Ctrl Pts',(-18.7554020493887,-12.8628118054171,
12.));
#232486=CARTESIAN_POINT('Ctrl Pts',(-18.7464259171251,-12.8582113455646,
12.));
#232487=CARTESIAN_POINT('Ctrl Pts',(-18.7376585820854,-12.8536791086316,
12.));
#232488=CARTESIAN_POINT('Ctrl Pts',(-18.7291026886554,-12.8492179511591,
12.));
#232489=CARTESIAN_POINT('Ctrl Pts',(-18.7207609737702,-12.8448308329494,
12.));
#232490=CARTESIAN_POINT('Ctrl Pts',(-18.7126362754445,-12.8405208263431,
12.));
#232491=CARTESIAN_POINT('Ctrl Pts',(-18.7047315436294,-12.8362911280361,
12.));
#232492=CARTESIAN_POINT('Ctrl Pts',(-18.6970498410172,-12.8321450599789,
12.));
#232493=CARTESIAN_POINT('Ctrl Pts',(-18.6895943376171,-12.8280860635231,
12.));
#232494=CARTESIAN_POINT('Ctrl Pts',(-18.6823683094139,-12.8241176980017,
12.));
#232495=CARTESIAN_POINT('Ctrl Pts',(-18.6753751301092,-12.8202436318474,
12.));
#232496=CARTESIAN_POINT('Ctrl Pts',(-18.6686182952799,-12.8164676687362,
12.));
#232497=CARTESIAN_POINT('Ctrl Pts',(-18.6621014624746,-12.8127937909631,
12.));
#232498=CARTESIAN_POINT('Ctrl Pts',(-18.6558284825773,-12.8092261933858,
12.));
#232499=CARTESIAN_POINT('Ctrl Pts',(-18.6498034438987,-12.805769331162,
12.));
#232500=CARTESIAN_POINT('Ctrl Pts',(-18.6440306327456,-12.8024278770152,
12.));
#232501=CARTESIAN_POINT('Ctrl Pts',(-18.63851447924,-12.7992066625264,12.));
#232502=CARTESIAN_POINT('Ctrl Pts',(-18.6332595057006,-12.7961106222251,
12.));
#232503=CARTESIAN_POINT('Ctrl Pts',(-18.6282702819371,-12.7931447451555,
12.));
#232504=CARTESIAN_POINT('Ctrl Pts',(-18.6235516265575,-12.7903142925234,
12.));
#232505=CARTESIAN_POINT('Ctrl Pts',(-18.6191087624752,-12.7876249657834,
12.));
#232506=CARTESIAN_POINT('Ctrl Pts',(-18.6149475565188,-12.7850831657901,
12.));
#232507=CARTESIAN_POINT('Ctrl Pts',(-18.6110744826219,-12.7826959526925,
12.));
#232508=CARTESIAN_POINT('Ctrl Pts',(-18.6074961535723,-12.7804705387658,
12.));
#232509=CARTESIAN_POINT('Ctrl Pts',(-18.6042190183704,-12.7784139605066,
12.));
#232510=CARTESIAN_POINT('Ctrl Pts',(-18.6012488486709,-12.7765325225081,
12.));
#232511=CARTESIAN_POINT('Ctrl Pts',(-18.598591752595,-12.7748328937638,
12.));
#232512=CARTESIAN_POINT('Ctrl Pts',(-18.5962551167772,-12.7733231262108,
12.));
#232513=CARTESIAN_POINT('Ctrl Pts',(-18.5942490615407,-12.7720142287172,
12.));
#232514=CARTESIAN_POINT('Ctrl Pts',(-18.5925859134579,-12.7709195951156,
12.));
#232515=CARTESIAN_POINT('Ctrl Pts',(-18.5912775137806,-12.7700520897173,
12.));
#232516=CARTESIAN_POINT('Ctrl Pts',(-18.5903328777227,-12.7694215127919,
12.));
#232517=CARTESIAN_POINT('Ctrl Pts',(-18.589871621843,-12.769110348199,12.));
#232518=CARTESIAN_POINT('Ctrl Pts',(-18.5896919669165,-12.768986426692,
12.));
#232519=CARTESIAN_POINT('Ctrl Pts',(-18.5896460962964,-12.7689524524483,
12.));
#232520=CARTESIAN_POINT('Ctrl Pts',(-18.5896416359912,-12.7689476255363,
12.));
#232521=CARTESIAN_POINT('',(-22.178719590434,-13.5685075571671,0.));
#232522=CARTESIAN_POINT('Origin',(-20.2687213152502,-7.17139709155223,0.));
#232523=CARTESIAN_POINT('',(-21.2610617890679,-7.52250298901264,12.));
#232524=CARTESIAN_POINT('',(-10.1343606576251,-3.58569854577611,12.));
#232525=CARTESIAN_POINT('',(-21.2610617890679,-7.52250298901264,0.));
#232526=CARTESIAN_POINT('',(-21.2610617890679,-7.52250298901264,0.));
#232527=CARTESIAN_POINT('',(-10.1343606576251,-3.58569854577611,0.));
#232528=CARTESIAN_POINT('Ctrl Pts',(-22.8400320311649,-12.4230808101438,
0.));
#232529=CARTESIAN_POINT('Ctrl Pts',(-22.8400320311649,-12.4230808101438,
12.));
#232530=CARTESIAN_POINT('Ctrl Pts',(-22.8370364396459,-12.418215285186,
0.));
#232531=CARTESIAN_POINT('Ctrl Pts',(-22.8370364396459,-12.418215285186,
12.));
#232532=CARTESIAN_POINT('Ctrl Pts',(-22.8310435872748,-12.4084933766346,
0.));
#232533=CARTESIAN_POINT('Ctrl Pts',(-22.8310435872748,-12.4084933766346,
12.));
#232534=CARTESIAN_POINT('Ctrl Pts',(-22.8220493007173,-12.3939379378998,
0.));
#232535=CARTESIAN_POINT('Ctrl Pts',(-22.8220493007173,-12.3939379378998,
12.));
#232536=CARTESIAN_POINT('Ctrl Pts',(-22.81004690224,-12.374585536673,0.));
#232537=CARTESIAN_POINT('Ctrl Pts',(-22.81004690224,-12.374585536673,12.));
#232538=CARTESIAN_POINT('Ctrl Pts',(-22.795027221673,-12.3504864740319,
0.));
#232539=CARTESIAN_POINT('Ctrl Pts',(-22.795027221673,-12.3504864740319,
12.));
#232540=CARTESIAN_POINT('Ctrl Pts',(-22.7799908974768,-12.3264788926075,
0.));
#232541=CARTESIAN_POINT('Ctrl Pts',(-22.7799908974768,-12.3264788926075,
12.));
#232542=CARTESIAN_POINT('Ctrl Pts',(-22.764938010105,-12.3025628601792,
0.));
#232543=CARTESIAN_POINT('Ctrl Pts',(-22.764938010105,-12.3025628601792,
12.));
#232544=CARTESIAN_POINT('Ctrl Pts',(-22.7498686970069,-12.2787384750742,
0.));
#232545=CARTESIAN_POINT('Ctrl Pts',(-22.7498686970069,-12.2787384750742,
12.));
#232546=CARTESIAN_POINT('Ctrl Pts',(-22.7347831655287,-12.2550058702395,
0.));
#232547=CARTESIAN_POINT('Ctrl Pts',(-22.7347831655287,-12.2550058702395,
12.));
#232548=CARTESIAN_POINT('Ctrl Pts',(-22.7196817119374,-12.2313652198061,
0.));
#232549=CARTESIAN_POINT('Ctrl Pts',(-22.7196817119374,-12.2313652198061,
12.));
#232550=CARTESIAN_POINT('Ctrl Pts',(-22.7045647168747,-12.2078167360284,
0.));
#232551=CARTESIAN_POINT('Ctrl Pts',(-22.7045647168747,-12.2078167360284,
12.));
#232552=CARTESIAN_POINT('Ctrl Pts',(-22.6894326205037,-12.1843606579261,
0.));
#232553=CARTESIAN_POINT('Ctrl Pts',(-22.6894326205037,-12.1843606579261,
12.));
#232554=CARTESIAN_POINT('Ctrl Pts',(-22.6742859034944,-12.1609972423099,
0.));
#232555=CARTESIAN_POINT('Ctrl Pts',(-22.6742859034944,-12.1609972423099,
12.));
#232556=CARTESIAN_POINT('Ctrl Pts',(-22.6591250653965,-12.1377267537145,
0.));
#232557=CARTESIAN_POINT('Ctrl Pts',(-22.6591250653965,-12.1377267537145,
12.));
#232558=CARTESIAN_POINT('Ctrl Pts',(-22.6439506046605,-12.1145494550383,
0.));
#232559=CARTESIAN_POINT('Ctrl Pts',(-22.6439506046605,-12.1145494550383,
12.));
#232560=CARTESIAN_POINT('Ctrl Pts',(-22.6287629967056,-12.0914655972823,
0.));
#232561=CARTESIAN_POINT('Ctrl Pts',(-22.6287629967056,-12.0914655972823,
12.));
#232562=CARTESIAN_POINT('Ctrl Pts',(-22.6135626764898,-12.0684754113862,
0.));
#232563=CARTESIAN_POINT('Ctrl Pts',(-22.6135626764898,-12.0684754113862,
12.));
#232564=CARTESIAN_POINT('Ctrl Pts',(-22.5983500505644,-12.0455791139128,
0.));
#232565=CARTESIAN_POINT('Ctrl Pts',(-22.5983500505644,-12.0455791139128,
12.));
#232566=CARTESIAN_POINT('Ctrl Pts',(-22.5831255061282,-12.0227769113127,
0.));
#232567=CARTESIAN_POINT('Ctrl Pts',(-22.5831255061282,-12.0227769113127,
12.));
#232568=CARTESIAN_POINT('Ctrl Pts',(-22.5678894211181,-12.0000690046695,
0.));
#232569=CARTESIAN_POINT('Ctrl Pts',(-22.5678894211181,-12.0000690046695,
12.));
#232570=CARTESIAN_POINT('Ctrl Pts',(-22.5526421741158,-11.9774555943496,
0.));
#232571=CARTESIAN_POINT('Ctrl Pts',(-22.5526421741158,-11.9774555943496,
12.));
#232572=CARTESIAN_POINT('Ctrl Pts',(-22.5373841537307,-11.9549368843997,
0.));
#232573=CARTESIAN_POINT('Ctrl Pts',(-22.5373841537307,-11.9549368843997,
12.));
#232574=CARTESIAN_POINT('Ctrl Pts',(-22.5221157697883,-11.9325130877803,
0.));
#232575=CARTESIAN_POINT('Ctrl Pts',(-22.5221157697883,-11.9325130877803,
12.));
#232576=CARTESIAN_POINT('Ctrl Pts',(-22.5068374513973,-11.9101844254557,
0.));
#232577=CARTESIAN_POINT('Ctrl Pts',(-22.5068374513973,-11.9101844254557,
12.));
#232578=CARTESIAN_POINT('Ctrl Pts',(-22.4915496418485,-11.8879511239942,
0.));
#232579=CARTESIAN_POINT('Ctrl Pts',(-22.4915496418485,-11.8879511239942,
12.));
#232580=CARTESIAN_POINT('Ctrl Pts',(-22.4762527946702,-11.8658134137019,
0.));
#232581=CARTESIAN_POINT('Ctrl Pts',(-22.4762527946702,-11.8658134137019,
12.));
#232582=CARTESIAN_POINT('Ctrl Pts',(-22.4609473690471,-11.8437715264487,
0.));
#232583=CARTESIAN_POINT('Ctrl Pts',(-22.4609473690471,-11.8437715264487,
12.));
#232584=CARTESIAN_POINT('Ctrl Pts',(-22.4456338258735,-11.8218256937889,
0.));
#232585=CARTESIAN_POINT('Ctrl Pts',(-22.4456338258735,-11.8218256937889,
12.));
#232586=CARTESIAN_POINT('Ctrl Pts',(-22.430312622646,-11.7999761445173,
0.));
#232587=CARTESIAN_POINT('Ctrl Pts',(-22.430312622646,-11.7999761445173,
12.));
#232588=CARTESIAN_POINT('Ctrl Pts',(-22.4149842125008,-11.7782231042039,
0.));
#232589=CARTESIAN_POINT('Ctrl Pts',(-22.4149842125008,-11.7782231042039,
12.));
#232590=CARTESIAN_POINT('Ctrl Pts',(-22.3996490469191,-11.7565667964764,
0.));
#232591=CARTESIAN_POINT('Ctrl Pts',(-22.3996490469191,-11.7565667964764,
12.));
#232592=CARTESIAN_POINT('Ctrl Pts',(-22.3843075773899,-11.7350074437961,
0.));
#232593=CARTESIAN_POINT('Ctrl Pts',(-22.3843075773899,-11.7350074437961,
12.));
#232594=CARTESIAN_POINT('Ctrl Pts',(-22.3689602575491,-11.7135452684532,
0.));
#232595=CARTESIAN_POINT('Ctrl Pts',(-22.3689602575491,-11.7135452684532,
12.));
#232596=CARTESIAN_POINT('Ctrl Pts',(-22.3536075450029,-11.6921804934056,
0.));
#232597=CARTESIAN_POINT('Ctrl Pts',(-22.3536075450029,-11.6921804934056,
12.));
#232598=CARTESIAN_POINT('Ctrl Pts',(-22.3382499035619,-11.6709133432985,
0.));
#232599=CARTESIAN_POINT('Ctrl Pts',(-22.3382499035619,-11.6709133432985,
12.));
#232600=CARTESIAN_POINT('Ctrl Pts',(-22.3228878043976,-11.6497440449857,
0.));
#232601=CARTESIAN_POINT('Ctrl Pts',(-22.3228878043976,-11.6497440449857,
12.));
#232602=CARTESIAN_POINT('Ctrl Pts',(-22.3075217249049,-11.6286728270009,
0.));
#232603=CARTESIAN_POINT('Ctrl Pts',(-22.3075217249049,-11.6286728270009,
12.));
#232604=CARTESIAN_POINT('Ctrl Pts',(-22.2921521480356,-11.6076999192357,
0.));
#232605=CARTESIAN_POINT('Ctrl Pts',(-22.2921521480356,-11.6076999192357,
12.));
#232606=CARTESIAN_POINT('Ctrl Pts',(-22.2767795614348,-11.5868255525188,
0.));
#232607=CARTESIAN_POINT('Ctrl Pts',(-22.2767795614348,-11.5868255525188,
12.));
#232608=CARTESIAN_POINT('Ctrl Pts',(-22.2614044566898,-11.5660499582403,
0.));
#232609=CARTESIAN_POINT('Ctrl Pts',(-22.2614044566898,-11.5660499582403,
12.));
#232610=CARTESIAN_POINT('Ctrl Pts',(-22.2460273284654,-11.5453733679121,
0.));
#232611=CARTESIAN_POINT('Ctrl Pts',(-22.2460273284654,-11.5453733679121,
12.));
#232612=CARTESIAN_POINT('Ctrl Pts',(-22.2306486738901,-11.5247960128477,
0.));
#232613=CARTESIAN_POINT('Ctrl Pts',(-22.2306486738901,-11.5247960128477,
12.));
#232614=CARTESIAN_POINT('Ctrl Pts',(-22.2152689931022,-11.5043181244242,
0.));
#232615=CARTESIAN_POINT('Ctrl Pts',(-22.2152689931022,-11.5043181244242,
12.));
#232616=CARTESIAN_POINT('Ctrl Pts',(-22.1998887896436,-11.483939934259,
0.));
#232617=CARTESIAN_POINT('Ctrl Pts',(-22.1998887896436,-11.483939934259,
12.));
#232618=CARTESIAN_POINT('Ctrl Pts',(-22.184508570917,-11.463661674411,0.));
#232619=CARTESIAN_POINT('Ctrl Pts',(-22.184508570917,-11.463661674411,12.));
#232620=CARTESIAN_POINT('Ctrl Pts',(-22.1691288486096,-11.443483577557,
0.));
#232621=CARTESIAN_POINT('Ctrl Pts',(-22.1691288486096,-11.443483577557,
12.));
#232622=CARTESIAN_POINT('Ctrl Pts',(-22.1537501391487,-11.4234058771742,
0.));
#232623=CARTESIAN_POINT('Ctrl Pts',(-22.1537501391487,-11.4234058771742,
12.));
#232624=CARTESIAN_POINT('Ctrl Pts',(-22.1383729640964,-11.4034288076908,
0.));
#232625=CARTESIAN_POINT('Ctrl Pts',(-22.1383729640964,-11.4034288076908,
12.));
#232626=CARTESIAN_POINT('Ctrl Pts',(-22.1229978500186,-11.3835526044256,
0.));
#232627=CARTESIAN_POINT('Ctrl Pts',(-22.1229978500186,-11.3835526044256,
12.));
#232628=CARTESIAN_POINT('Ctrl Pts',(-22.1076253283979,-11.3637775035367,
0.));
#232629=CARTESIAN_POINT('Ctrl Pts',(-22.1076253283979,-11.3637775035367,
12.));
#232630=CARTESIAN_POINT('Ctrl Pts',(-22.0922559355294,-11.3441037419553,
0.));
#232631=CARTESIAN_POINT('Ctrl Pts',(-22.0922559355294,-11.3441037419553,
12.));
#232632=CARTESIAN_POINT('Ctrl Pts',(-22.0768902124267,-11.3245315573168,
0.));
#232633=CARTESIAN_POINT('Ctrl Pts',(-22.0768902124267,-11.3245315573168,
12.));
#232634=CARTESIAN_POINT('Ctrl Pts',(-22.0615287047179,-11.3050611878771,
0.));
#232635=CARTESIAN_POINT('Ctrl Pts',(-22.0615287047179,-11.3050611878771,
12.));
#232636=CARTESIAN_POINT('Ctrl Pts',(-22.046171962566,-11.2856928724374,
0.));
#232637=CARTESIAN_POINT('Ctrl Pts',(-22.046171962566,-11.2856928724374,
12.));
#232638=CARTESIAN_POINT('Ctrl Pts',(-22.030820540835,-11.2664268504206,
0.));
#232639=CARTESIAN_POINT('Ctrl Pts',(-22.030820540835,-11.2664268504206,
12.));
#232640=CARTESIAN_POINT('Ctrl Pts',(-22.0154749992363,-11.2472633619275,
0.));
#232641=CARTESIAN_POINT('Ctrl Pts',(-22.0154749992363,-11.2472633619275,
12.));
#232642=CARTESIAN_POINT('Ctrl Pts',(-22.0001359024839,-11.2282026477896,
0.));
#232643=CARTESIAN_POINT('Ctrl Pts',(-22.0001359024839,-11.2282026477896,
12.));
#232644=CARTESIAN_POINT('Ctrl Pts',(-21.9848038204439,-11.2092449496125,
0.));
#232645=CARTESIAN_POINT('Ctrl Pts',(-21.9848038204439,-11.2092449496125,
12.));
#232646=CARTESIAN_POINT('Ctrl Pts',(-21.9694793282914,-11.190390509811,
0.));
#232647=CARTESIAN_POINT('Ctrl Pts',(-21.9694793282914,-11.190390509811,
12.));
#232648=CARTESIAN_POINT('Ctrl Pts',(-21.9541630066506,-11.1716395716376,
0.));
#232649=CARTESIAN_POINT('Ctrl Pts',(-21.9541630066506,-11.1716395716376,
12.));
#232650=CARTESIAN_POINT('Ctrl Pts',(-21.9388554416439,-11.1529923792003,
0.));
#232651=CARTESIAN_POINT('Ctrl Pts',(-21.9388554416439,-11.1529923792003,
12.));
#232652=CARTESIAN_POINT('Ctrl Pts',(-21.923557224952,-11.1344491774741,
0.));
#232653=CARTESIAN_POINT('Ctrl Pts',(-21.923557224952,-11.1344491774741,
12.));
#232654=CARTESIAN_POINT('Ctrl Pts',(-21.9082689538688,-11.1160102123024,
0.));
#232655=CARTESIAN_POINT('Ctrl Pts',(-21.9082689538688,-11.1160102123024,
12.));
#232656=CARTESIAN_POINT('Ctrl Pts',(-21.8929912313608,-11.0976757303944,
0.));
#232657=CARTESIAN_POINT('Ctrl Pts',(-21.8929912313608,-11.0976757303944,
12.));
#232658=CARTESIAN_POINT('Ctrl Pts',(-21.877724666119,-11.0794459793057,
0.));
#232659=CARTESIAN_POINT('Ctrl Pts',(-21.877724666119,-11.0794459793057,
12.));
#232660=CARTESIAN_POINT('Ctrl Pts',(-21.8624698726318,-11.0613212074363,
0.));
#232661=CARTESIAN_POINT('Ctrl Pts',(-21.8624698726318,-11.0613212074363,
12.));
#232662=CARTESIAN_POINT('Ctrl Pts',(-21.8472274713103,-11.0433016640807,
0.));
#232663=CARTESIAN_POINT('Ctrl Pts',(-21.8472274713103,-11.0433016640807,
12.));
#232664=CARTESIAN_POINT('Ctrl Pts',(-21.8319980886033,-11.0253875994598,
0.));
#232665=CARTESIAN_POINT('Ctrl Pts',(-21.8319980886033,-11.0253875994598,
12.));
#232666=CARTESIAN_POINT('Ctrl Pts',(-21.8167823571168,-11.0075792647477,
0.));
#232667=CARTESIAN_POINT('Ctrl Pts',(-21.8167823571168,-11.0075792647477,
12.));
#232668=CARTESIAN_POINT('Ctrl Pts',(-21.8015809157301,-10.9898769120912,
0.));
#232669=CARTESIAN_POINT('Ctrl Pts',(-21.8015809157301,-10.9898769120912,
12.));
#232670=CARTESIAN_POINT('Ctrl Pts',(-21.7863944097141,-10.9722807946155,
0.));
#232671=CARTESIAN_POINT('Ctrl Pts',(-21.7863944097141,-10.9722807946155,
12.));
#232672=CARTESIAN_POINT('Ctrl Pts',(-21.7712234908464,-10.9547911664455,
0.));
#232673=CARTESIAN_POINT('Ctrl Pts',(-21.7712234908464,-10.9547911664455,
12.));
#232674=CARTESIAN_POINT('Ctrl Pts',(-21.7560688175247,-10.9374082827444,
0.));
#232675=CARTESIAN_POINT('Ctrl Pts',(-21.7560688175247,-10.9374082827444,
12.));
#232676=CARTESIAN_POINT('Ctrl Pts',(-21.7409310548797,-10.9201323997384,
0.));
#232677=CARTESIAN_POINT('Ctrl Pts',(-21.7409310548797,-10.9201323997384,
12.));
#232678=CARTESIAN_POINT('Ctrl Pts',(-21.7258108748873,-10.902963774734,
0.));
#232679=CARTESIAN_POINT('Ctrl Pts',(-21.7258108748873,-10.902963774734,
12.));
#232680=CARTESIAN_POINT('Ctrl Pts',(-21.7107089564825,-10.8859026661293,
0.));
#232681=CARTESIAN_POINT('Ctrl Pts',(-21.7107089564825,-10.8859026661293,
12.));
#232682=CARTESIAN_POINT('Ctrl Pts',(-21.6956259856672,-10.8689493334095,
0.));
#232683=CARTESIAN_POINT('Ctrl Pts',(-21.6956259856672,-10.8689493334095,
12.));
#232684=CARTESIAN_POINT('Ctrl Pts',(-21.6805626556467,-10.8521040371835,
0.));
#232685=CARTESIAN_POINT('Ctrl Pts',(-21.6805626556467,-10.8521040371835,
12.));
#232686=CARTESIAN_POINT('Ctrl Pts',(-21.6655196669732,-10.8353670392272,
0.));
#232687=CARTESIAN_POINT('Ctrl Pts',(-21.6655196669732,-10.8353670392272,
12.));
#232688=CARTESIAN_POINT('Ctrl Pts',(-21.6504977276866,-10.8187386025136,
0.));
#232689=CARTESIAN_POINT('Ctrl Pts',(-21.6504977276866,-10.8187386025136,
12.));
#232690=CARTESIAN_POINT('Ctrl Pts',(-21.6354975534557,-10.8022189912369,
0.));
#232691=CARTESIAN_POINT('Ctrl Pts',(-21.6354975534557,-10.8022189912369,
12.));
#232692=CARTESIAN_POINT('Ctrl Pts',(-21.6205198677173,-10.7858084708261,
0.));
#232693=CARTESIAN_POINT('Ctrl Pts',(-21.6205198677173,-10.7858084708261,
12.));
#232694=CARTESIAN_POINT('Ctrl Pts',(-21.6055654018176,-10.7695073079552,
0.));
#232695=CARTESIAN_POINT('Ctrl Pts',(-21.6055654018176,-10.7695073079552,
12.));
#232696=CARTESIAN_POINT('Ctrl Pts',(-21.5906348951743,-10.7533157705941,
0.));
#232697=CARTESIAN_POINT('Ctrl Pts',(-21.5906348951743,-10.7533157705941,
12.));
#232698=CARTESIAN_POINT('Ctrl Pts',(-21.5757290954371,-10.7372341280467,
0.));
#232699=CARTESIAN_POINT('Ctrl Pts',(-21.5757290954371,-10.7372341280467,
12.));
#232700=CARTESIAN_POINT('Ctrl Pts',(-21.5608487586468,-10.7212626509816,
0.));
#232701=CARTESIAN_POINT('Ctrl Pts',(-21.5608487586468,-10.7212626509816,
12.));
#232702=CARTESIAN_POINT('Ctrl Pts',(-21.5459946493955,-10.7054016114571,
0.));
#232703=CARTESIAN_POINT('Ctrl Pts',(-21.5459946493955,-10.7054016114571,
12.));
#232704=CARTESIAN_POINT('Ctrl Pts',(-21.5311675409807,-10.689651282929,
0.));
#232705=CARTESIAN_POINT('Ctrl Pts',(-21.5311675409807,-10.689651282929,
12.));
#232706=CARTESIAN_POINT('Ctrl Pts',(-21.51636821558,-10.6740119402834,0.));
#232707=CARTESIAN_POINT('Ctrl Pts',(-21.51636821558,-10.6740119402834,12.));
#232708=CARTESIAN_POINT('Ctrl Pts',(-21.5015974644449,-10.6584838598939,
0.));
#232709=CARTESIAN_POINT('Ctrl Pts',(-21.5015974644449,-10.6584838598939,
12.));
#232710=CARTESIAN_POINT('Ctrl Pts',(-21.4868560880889,-10.6430673196607,
0.));
#232711=CARTESIAN_POINT('Ctrl Pts',(-21.4868560880889,-10.6430673196607,
12.));
#232712=CARTESIAN_POINT('Ctrl Pts',(-21.4721448964766,-10.6277625990456,
0.));
#232713=CARTESIAN_POINT('Ctrl Pts',(-21.4721448964766,-10.6277625990456,
12.));
#232714=CARTESIAN_POINT('Ctrl Pts',(-21.4574647092097,-10.6125699790961,
0.));
#232715=CARTESIAN_POINT('Ctrl Pts',(-21.4574647092097,-10.6125699790961,
12.));
#232716=CARTESIAN_POINT('Ctrl Pts',(-21.4428163557144,-10.5974897424622,
0.));
#232717=CARTESIAN_POINT('Ctrl Pts',(-21.4428163557144,-10.5974897424622,
12.));
#232718=CARTESIAN_POINT('Ctrl Pts',(-21.4282006754631,-10.5825221734573,
0.));
#232719=CARTESIAN_POINT('Ctrl Pts',(-21.4282006754631,-10.5825221734573,
12.));
#232720=CARTESIAN_POINT('Ctrl Pts',(-21.4136185181979,-10.5676675581108,
0.));
#232721=CARTESIAN_POINT('Ctrl Pts',(-21.4136185181979,-10.5676675581108,
12.));
#232722=CARTESIAN_POINT('Ctrl Pts',(-21.3990707441497,-10.5529261842108,
0.));
#232723=CARTESIAN_POINT('Ctrl Pts',(-21.3990707441497,-10.5529261842108,
12.));
#232724=CARTESIAN_POINT('Ctrl Pts',(-21.3845582242602,-10.5382983413421,
0.));
#232725=CARTESIAN_POINT('Ctrl Pts',(-21.3845582242602,-10.5382983413421,
12.));
#232726=CARTESIAN_POINT('Ctrl Pts',(-21.3700818403936,-10.5237843209057,
0.));
#232727=CARTESIAN_POINT('Ctrl Pts',(-21.3700818403936,-10.5237843209057,
12.));
#232728=CARTESIAN_POINT('Ctrl Pts',(-21.3556424855814,-10.5093844161685,
0.));
#232729=CARTESIAN_POINT('Ctrl Pts',(-21.3556424855814,-10.5093844161685,
12.));
#232730=CARTESIAN_POINT('Ctrl Pts',(-21.3412410642904,-10.4950989223337,
0.));
#232731=CARTESIAN_POINT('Ctrl Pts',(-21.3412410642904,-10.4950989223337,
12.));
#232732=CARTESIAN_POINT('Ctrl Pts',(-21.3268784926819,-10.4809281365931,
0.));
#232733=CARTESIAN_POINT('Ctrl Pts',(-21.3268784926819,-10.4809281365931,
12.));
#232734=CARTESIAN_POINT('Ctrl Pts',(-21.3125556988731,-10.4668723581768,
0.));
#232735=CARTESIAN_POINT('Ctrl Pts',(-21.3125556988731,-10.4668723581768,
12.));
#232736=CARTESIAN_POINT('Ctrl Pts',(-21.2982736231931,-10.4529318883874,
0.));
#232737=CARTESIAN_POINT('Ctrl Pts',(-21.2982736231931,-10.4529318883874,
12.));
#232738=CARTESIAN_POINT('Ctrl Pts',(-21.2840332184483,-10.4391070306391,
0.));
#232739=CARTESIAN_POINT('Ctrl Pts',(-21.2840332184483,-10.4391070306391,
12.));
#232740=CARTESIAN_POINT('Ctrl Pts',(-21.2698354502403,-10.42539809054,0.));
#232741=CARTESIAN_POINT('Ctrl Pts',(-21.2698354502403,-10.42539809054,12.));
#232742=CARTESIAN_POINT('Ctrl Pts',(-21.255681297275,-10.4118053759588,
0.));
#232743=CARTESIAN_POINT('Ctrl Pts',(-21.255681297275,-10.4118053759588,
12.));
#232744=CARTESIAN_POINT('Ctrl Pts',(-21.2415717516714,-10.3983291970846,
0.));
#232745=CARTESIAN_POINT('Ctrl Pts',(-21.2415717516714,-10.3983291970846,
12.));
#232746=CARTESIAN_POINT('Ctrl Pts',(-21.22750781927,-10.3849698664786,0.));
#232747=CARTESIAN_POINT('Ctrl Pts',(-21.22750781927,-10.3849698664786,12.));
#232748=CARTESIAN_POINT('Ctrl Pts',(-21.2134905199345,-10.371727699113,
0.));
#232749=CARTESIAN_POINT('Ctrl Pts',(-21.2134905199345,-10.371727699113,
12.));
#232750=CARTESIAN_POINT('Ctrl Pts',(-21.199520887919,-10.3586030124587,
0.));
#232751=CARTESIAN_POINT('Ctrl Pts',(-21.199520887919,-10.3586030124587,
12.));
#232752=CARTESIAN_POINT('Ctrl Pts',(-21.1855999722416,-10.34559612657,0.));
#232753=CARTESIAN_POINT('Ctrl Pts',(-21.1855999722416,-10.34559612657,12.));
#232754=CARTESIAN_POINT('Ctrl Pts',(-21.1717288370509,-10.3327073641572,
0.));
#232755=CARTESIAN_POINT('Ctrl Pts',(-21.1717288370509,-10.3327073641572,
12.));
#232756=CARTESIAN_POINT('Ctrl Pts',(-21.1579085619965,-10.3199370506544,
0.));
#232757=CARTESIAN_POINT('Ctrl Pts',(-21.1579085619965,-10.3199370506544,
12.));
#232758=CARTESIAN_POINT('Ctrl Pts',(-21.1441402425843,-10.3072855142687,
0.));
#232759=CARTESIAN_POINT('Ctrl Pts',(-21.1441402425843,-10.3072855142687,
12.));
#232760=CARTESIAN_POINT('Ctrl Pts',(-21.1304249906002,-10.2947530860721,
0.));
#232761=CARTESIAN_POINT('Ctrl Pts',(-21.1304249906002,-10.2947530860721,
12.));
#232762=CARTESIAN_POINT('Ctrl Pts',(-21.1167639345631,-10.2823401001072,
0.));
#232763=CARTESIAN_POINT('Ctrl Pts',(-21.1167639345631,-10.2823401001072,
12.));
#232764=CARTESIAN_POINT('Ctrl Pts',(-21.1031582201627,-10.2700468934744,
0.));
#232765=CARTESIAN_POINT('Ctrl Pts',(-21.1031582201627,-10.2700468934744,
12.));
#232766=CARTESIAN_POINT('Ctrl Pts',(-21.0896090107063,-10.2578738064181,
0.));
#232767=CARTESIAN_POINT('Ctrl Pts',(-21.0896090107063,-10.2578738064181,
12.));
#232768=CARTESIAN_POINT('Ctrl Pts',(-21.0761174875445,-10.2458211823912,
0.));
#232769=CARTESIAN_POINT('Ctrl Pts',(-21.0761174875445,-10.2458211823912,
12.));
#232770=CARTESIAN_POINT('Ctrl Pts',(-21.0626848505663,-10.2338893681567,
0.));
#232771=CARTESIAN_POINT('Ctrl Pts',(-21.0626848505663,-10.2338893681567,
12.));
#232772=CARTESIAN_POINT('Ctrl Pts',(-21.0493123187483,-10.2220787139154,
0.));
#232773=CARTESIAN_POINT('Ctrl Pts',(-21.0493123187483,-10.2220787139154,
12.));
#232774=CARTESIAN_POINT('Ctrl Pts',(-21.0360011306815,-10.2103895734123,
0.));
#232775=CARTESIAN_POINT('Ctrl Pts',(-21.0360011306815,-10.2103895734123,
12.));
#232776=CARTESIAN_POINT('Ctrl Pts',(-21.0227525451107,-10.1988223040425,
0.));
#232777=CARTESIAN_POINT('Ctrl Pts',(-21.0227525451107,-10.1988223040425,
12.));
#232778=CARTESIAN_POINT('Ctrl Pts',(-21.0095678414486,-10.187377266936,
0.));
#232779=CARTESIAN_POINT('Ctrl Pts',(-21.0095678414486,-10.187377266936,
12.));
#232780=CARTESIAN_POINT('Ctrl Pts',(-20.9964483203686,-10.1760548270767,
0.));
#232781=CARTESIAN_POINT('Ctrl Pts',(-20.9964483203686,-10.1760548270767,
12.));
#232782=CARTESIAN_POINT('Ctrl Pts',(-20.9833953044736,-10.1648553534568,
0.));
#232783=CARTESIAN_POINT('Ctrl Pts',(-20.9833953044736,-10.1648553534568,
12.));
#232784=CARTESIAN_POINT('Ctrl Pts',(-20.9704101389369,-10.1537792192065,
0.));
#232785=CARTESIAN_POINT('Ctrl Pts',(-20.9704101389369,-10.1537792192065,
12.));
#232786=CARTESIAN_POINT('Ctrl Pts',(-20.9574941921591,-10.1428268017256,
0.));
#232787=CARTESIAN_POINT('Ctrl Pts',(-20.9574941921591,-10.1428268017256,
12.));
#232788=CARTESIAN_POINT('Ctrl Pts',(-20.9446488563933,-10.1319984827908,
0.));
#232789=CARTESIAN_POINT('Ctrl Pts',(-20.9446488563933,-10.1319984827908,
12.));
#232790=CARTESIAN_POINT('Ctrl Pts',(-20.9318755484734,-10.1212946487057,
0.));
#232791=CARTESIAN_POINT('Ctrl Pts',(-20.9318755484734,-10.1212946487057,
12.));
#232792=CARTESIAN_POINT('Ctrl Pts',(-20.919175710627,-10.1107156904836,
0.));
#232793=CARTESIAN_POINT('Ctrl Pts',(-20.919175710627,-10.1107156904836,
12.));
#232794=CARTESIAN_POINT('Ctrl Pts',(-20.9065508112557,-10.1002620040076,
0.));
#232795=CARTESIAN_POINT('Ctrl Pts',(-20.9065508112557,-10.1002620040076,
12.));
#232796=CARTESIAN_POINT('Ctrl Pts',(-20.894002345737,-10.0899339901915,
0.));
#232797=CARTESIAN_POINT('Ctrl Pts',(-20.894002345737,-10.0899339901915,
12.));
#232798=CARTESIAN_POINT('Ctrl Pts',(-20.881531837184,-10.0797320551154,
0.));
#232799=CARTESIAN_POINT('Ctrl Pts',(-20.881531837184,-10.0797320551154,
12.));
#232800=CARTESIAN_POINT('Ctrl Pts',(-20.86914083737,-10.0696566102218,0.));
#232801=CARTESIAN_POINT('Ctrl Pts',(-20.86914083737,-10.0696566102218,12.));
#232802=CARTESIAN_POINT('Ctrl Pts',(-20.8568309277316,-10.0597080725375,
0.));
#232803=CARTESIAN_POINT('Ctrl Pts',(-20.8568309277316,-10.0597080725375,
12.));
#232804=CARTESIAN_POINT('Ctrl Pts',(-20.8446037203402,-10.0498868648733,
0.));
#232805=CARTESIAN_POINT('Ctrl Pts',(-20.8446037203402,-10.0498868648733,
12.));
#232806=CARTESIAN_POINT('Ctrl Pts',(-20.8324608588909,-10.0401934160234,
0.));
#232807=CARTESIAN_POINT('Ctrl Pts',(-20.8324608588909,-10.0401934160234,
12.));
#232808=CARTESIAN_POINT('Ctrl Pts',(-20.8204040196602,-10.0306281609435,
0.));
#232809=CARTESIAN_POINT('Ctrl Pts',(-20.8204040196602,-10.0306281609435,
12.));
#232810=CARTESIAN_POINT('Ctrl Pts',(-20.8084349126888,-10.0211915410095,
0.));
#232811=CARTESIAN_POINT('Ctrl Pts',(-20.8084349126888,-10.0211915410095,
12.));
#232812=CARTESIAN_POINT('Ctrl Pts',(-20.7965552829908,-10.0118840042786,
0.));
#232813=CARTESIAN_POINT('Ctrl Pts',(-20.7965552829908,-10.0118840042786,
12.));
#232814=CARTESIAN_POINT('Ctrl Pts',(-20.7847669117568,-10.0027060057389,
0.));
#232815=CARTESIAN_POINT('Ctrl Pts',(-20.7847669117568,-10.0027060057389,
12.));
#232816=CARTESIAN_POINT('Ctrl Pts',(-20.7730716175417,-9.9936580075464,
0.));
#232817=CARTESIAN_POINT('Ctrl Pts',(-20.7730716175417,-9.9936580075464,
12.));
#232818=CARTESIAN_POINT('Ctrl Pts',(-20.761471257499,-9.98474047926852,
0.));
#232819=CARTESIAN_POINT('Ctrl Pts',(-20.761471257499,-9.98474047926852,
12.));
#232820=CARTESIAN_POINT('Ctrl Pts',(-20.7499677289627,-9.9759538982347,
0.));
#232821=CARTESIAN_POINT('Ctrl Pts',(-20.7499677289627,-9.9759538982347,
12.));
#232822=CARTESIAN_POINT('Ctrl Pts',(-20.7385629709795,-9.96729874986201,
0.));
#232823=CARTESIAN_POINT('Ctrl Pts',(-20.7385629709795,-9.96729874986201,
12.));
#232824=CARTESIAN_POINT('Ctrl Pts',(-20.7272589658751,-9.95877552798397,
0.));
#232825=CARTESIAN_POINT('Ctrl Pts',(-20.7272589658751,-9.95877552798397,
12.));
#232826=CARTESIAN_POINT('Ctrl Pts',(-20.7160577407579,-9.95038473514948,
0.));
#232827=CARTESIAN_POINT('Ctrl Pts',(-20.7160577407579,-9.95038473514948,
12.));
#232828=CARTESIAN_POINT('Ctrl Pts',(-20.7049613692234,-9.94212688298236,
0.));
#232829=CARTESIAN_POINT('Ctrl Pts',(-20.7049613692234,-9.94212688298236,
12.));
#232830=CARTESIAN_POINT('Ctrl Pts',(-20.6939719732484,-9.93400249259729,
0.));
#232831=CARTESIAN_POINT('Ctrl Pts',(-20.6939719732484,-9.93400249259729,
12.));
#232832=CARTESIAN_POINT('Ctrl Pts',(-20.6830917250255,-9.92601209498748,
0.));
#232833=CARTESIAN_POINT('Ctrl Pts',(-20.6830917250255,-9.92601209498748,
12.));
#232834=CARTESIAN_POINT('Ctrl Pts',(-20.6723228488263,-9.91815623141288,
0.));
#232835=CARTESIAN_POINT('Ctrl Pts',(-20.6723228488263,-9.91815623141288,
12.));
#232836=CARTESIAN_POINT('Ctrl Pts',(-20.6616676228315,-9.91043545377007,
0.));
#232837=CARTESIAN_POINT('Ctrl Pts',(-20.6616676228315,-9.91043545377007,
12.));
#232838=CARTESIAN_POINT('Ctrl Pts',(-20.6511283817414,-9.90285032516692,
0.));
#232839=CARTESIAN_POINT('Ctrl Pts',(-20.6511283817414,-9.90285032516692,
12.));
#232840=CARTESIAN_POINT('Ctrl Pts',(-20.6407075193976,-9.89540142049119,
0.));
#232841=CARTESIAN_POINT('Ctrl Pts',(-20.6407075193976,-9.89540142049119,
12.));
#232842=CARTESIAN_POINT('Ctrl Pts',(-20.6304074914087,-9.88808932697306,
0.));
#232843=CARTESIAN_POINT('Ctrl Pts',(-20.6304074914087,-9.88808932697306,
12.));
#232844=CARTESIAN_POINT('Ctrl Pts',(-20.6202308177474,-9.88091464472675,
0.));
#232845=CARTESIAN_POINT('Ctrl Pts',(-20.6202308177474,-9.88091464472675,
12.));
#232846=CARTESIAN_POINT('Ctrl Pts',(-20.6101800854494,-9.87387798732956,
0.));
#232847=CARTESIAN_POINT('Ctrl Pts',(-20.6101800854494,-9.87387798732956,
12.));
#232848=CARTESIAN_POINT('Ctrl Pts',(-20.6002579513699,-9.86697998242622,
0.));
#232849=CARTESIAN_POINT('Ctrl Pts',(-20.6002579513699,-9.86697998242622,
12.));
#232850=CARTESIAN_POINT('Ctrl Pts',(-20.5904671449754,-9.86022127232747,
0.));
#232851=CARTESIAN_POINT('Ctrl Pts',(-20.5904671449754,-9.86022127232747,
12.));
#232852=CARTESIAN_POINT('Ctrl Pts',(-20.5808104710015,-9.8536025145698,
0.));
#232853=CARTESIAN_POINT('Ctrl Pts',(-20.5808104710015,-9.8536025145698,
12.));
#232854=CARTESIAN_POINT('Ctrl Pts',(-20.5712908125139,-9.84712438256277,
0.));
#232855=CARTESIAN_POINT('Ctrl Pts',(-20.5712908125139,-9.84712438256277,
12.));
#232856=CARTESIAN_POINT('Ctrl Pts',(-20.5619111362402,-9.84078756677565,
0.));
#232857=CARTESIAN_POINT('Ctrl Pts',(-20.5619111362402,-9.84078756677565,
12.));
#232858=CARTESIAN_POINT('Ctrl Pts',(-20.552674497646,-9.83459277585315,
0.));
#232859=CARTESIAN_POINT('Ctrl Pts',(-20.552674497646,-9.83459277585315,
12.));
#232860=CARTESIAN_POINT('Ctrl Pts',(-20.5435840460721,-9.82854073773877,
0.));
#232861=CARTESIAN_POINT('Ctrl Pts',(-20.5435840460721,-9.82854073773877,
12.));
#232862=CARTESIAN_POINT('Ctrl Pts',(-20.5346430299517,-9.82263220080362,
0.));
#232863=CARTESIAN_POINT('Ctrl Pts',(-20.5346430299517,-9.82263220080362,
12.));
#232864=CARTESIAN_POINT('Ctrl Pts',(-20.5258548000629,-9.81686793455942,
0.));
#232865=CARTESIAN_POINT('Ctrl Pts',(-20.5258548000629,-9.81686793455942,
12.));
#232866=CARTESIAN_POINT('Ctrl Pts',(-20.517222812284,-9.81124873025281,
0.));
#232867=CARTESIAN_POINT('Ctrl Pts',(-20.517222812284,-9.81124873025281,
12.));
#232868=CARTESIAN_POINT('Ctrl Pts',(-20.5087506310505,-9.80577540161087,
0.));
#232869=CARTESIAN_POINT('Ctrl Pts',(-20.5087506310505,-9.80577540161087,
12.));
#232870=CARTESIAN_POINT('Ctrl Pts',(-20.5004419312107,-9.80044878520948,
0.));
#232871=CARTESIAN_POINT('Ctrl Pts',(-20.5004419312107,-9.80044878520948,
12.));
#232872=CARTESIAN_POINT('Ctrl Pts',(-20.4923005087943,-9.7952697428833,
0.));
#232873=CARTESIAN_POINT('Ctrl Pts',(-20.4923005087943,-9.7952697428833,
12.));
#232874=CARTESIAN_POINT('Ctrl Pts',(-20.4843302955329,-9.79023916498655,
0.));
#232875=CARTESIAN_POINT('Ctrl Pts',(-20.4843302955329,-9.79023916498655,
12.));
#232876=CARTESIAN_POINT('Ctrl Pts',(-20.4765353711586,-9.78535797314166,
0.));
#232877=CARTESIAN_POINT('Ctrl Pts',(-20.4765353711586,-9.78535797314166,
12.));
#232878=CARTESIAN_POINT('Ctrl Pts',(-20.4689199790669,-9.7806271237332,
0.));
#232879=CARTESIAN_POINT('Ctrl Pts',(-20.4689199790669,-9.7806271237332,
12.));
#232880=CARTESIAN_POINT('Ctrl Pts',(-20.4614885274975,-9.77604760815528,
0.));
#232881=CARTESIAN_POINT('Ctrl Pts',(-20.4614885274975,-9.77604760815528,
12.));
#232882=CARTESIAN_POINT('Ctrl Pts',(-20.4542455817527,-9.77162045104069,
0.));
#232883=CARTESIAN_POINT('Ctrl Pts',(-20.4542455817527,-9.77162045104069,
12.));
#232884=CARTESIAN_POINT('Ctrl Pts',(-20.447195862298,-9.76734670980891,
0.));
#232885=CARTESIAN_POINT('Ctrl Pts',(-20.447195862298,-9.76734670980891,
12.));
#232886=CARTESIAN_POINT('Ctrl Pts',(-20.44034423294,-9.76322747195494,0.));
#232887=CARTESIAN_POINT('Ctrl Pts',(-20.44034423294,-9.76322747195494,12.));
#232888=CARTESIAN_POINT('Ctrl Pts',(-20.4336957355473,-9.75926386289922,
0.));
#232889=CARTESIAN_POINT('Ctrl Pts',(-20.4336957355473,-9.75926386289922,
12.));
#232890=CARTESIAN_POINT('Ctrl Pts',(-20.4272556476629,-9.75545705902417,
0.));
#232891=CARTESIAN_POINT('Ctrl Pts',(-20.4272556476629,-9.75545705902417,
12.));
#232892=CARTESIAN_POINT('Ctrl Pts',(-20.4210295275817,-9.7518082978643,
0.));
#232893=CARTESIAN_POINT('Ctrl Pts',(-20.4210295275817,-9.7518082978643,
12.));
#232894=CARTESIAN_POINT('Ctrl Pts',(-20.4150232777393,-9.74831889242174,
0.));
#232895=CARTESIAN_POINT('Ctrl Pts',(-20.4150232777393,-9.74831889242174,
12.));
#232896=CARTESIAN_POINT('Ctrl Pts',(-20.4092430879861,-9.74499021838537,
0.));
#232897=CARTESIAN_POINT('Ctrl Pts',(-20.4092430879861,-9.74499021838537,
12.));
#232898=CARTESIAN_POINT('Ctrl Pts',(-20.4036953576549,-9.74182369656271,
0.));
#232899=CARTESIAN_POINT('Ctrl Pts',(-20.4036953576549,-9.74182369656271,
12.));
#232900=CARTESIAN_POINT('Ctrl Pts',(-20.3983866213331,-9.738820776132,0.));
#232901=CARTESIAN_POINT('Ctrl Pts',(-20.3983866213331,-9.738820776132,12.));
#232902=CARTESIAN_POINT('Ctrl Pts',(-20.3933234845647,-9.73598292014242,
0.));
#232903=CARTESIAN_POINT('Ctrl Pts',(-20.3933234845647,-9.73598292014242,
12.));
#232904=CARTESIAN_POINT('Ctrl Pts',(-20.3885129129912,-9.73331167102807,
0.));
#232905=CARTESIAN_POINT('Ctrl Pts',(-20.3885129129912,-9.73331167102807,
12.));
#232906=CARTESIAN_POINT('Ctrl Pts',(-20.3839624556742,-9.73080870123727,
0.));
#232907=CARTESIAN_POINT('Ctrl Pts',(-20.3839624556742,-9.73080870123727,
12.));
#232908=CARTESIAN_POINT('Ctrl Pts',(-20.3796805893304,-9.72847589116541,
0.));
#232909=CARTESIAN_POINT('Ctrl Pts',(-20.3796805893304,-9.72847589116541,
12.));
#232910=CARTESIAN_POINT('Ctrl Pts',(-20.3756766651951,-9.7263153173288,
0.));
#232911=CARTESIAN_POINT('Ctrl Pts',(-20.3756766651951,-9.7263153173288,
12.));
#232912=CARTESIAN_POINT('Ctrl Pts',(-20.371960235676,-9.72432910043194,
0.));
#232913=CARTESIAN_POINT('Ctrl Pts',(-20.371960235676,-9.72432910043194,
12.));
#232914=CARTESIAN_POINT('Ctrl Pts',(-20.3685406190576,-9.72251930722489,
0.));
#232915=CARTESIAN_POINT('Ctrl Pts',(-20.3685406190576,-9.72251930722489,
12.));
#232916=CARTESIAN_POINT('Ctrl Pts',(-20.3654261611056,-9.7208877838108,
0.));
#232917=CARTESIAN_POINT('Ctrl Pts',(-20.3654261611056,-9.7208877838108,
12.));
#232918=CARTESIAN_POINT('Ctrl Pts',(-20.3626256913981,-9.71943648548099,
0.));
#232919=CARTESIAN_POINT('Ctrl Pts',(-20.3626256913981,-9.71943648548099,
12.));
#232920=CARTESIAN_POINT('Ctrl Pts',(-20.3601498764344,-9.71816778328006,
0.));
#232921=CARTESIAN_POINT('Ctrl Pts',(-20.3601498764344,-9.71816778328006,
12.));
#232922=CARTESIAN_POINT('Ctrl Pts',(-20.3580133103356,-9.71708493723096,
0.));
#232923=CARTESIAN_POINT('Ctrl Pts',(-20.3580133103356,-9.71708493723096,
12.));
#232924=CARTESIAN_POINT('Ctrl Pts',(-20.3562337557875,-9.71619192554185,
0.));
#232925=CARTESIAN_POINT('Ctrl Pts',(-20.3562337557875,-9.71619192554185,
12.));
#232926=CARTESIAN_POINT('Ctrl Pts',(-20.3548282742361,-9.71549257088172,
0.));
#232927=CARTESIAN_POINT('Ctrl Pts',(-20.3548282742361,-9.71549257088172,
12.));
#232928=CARTESIAN_POINT('Ctrl Pts',(-20.3538098605706,-9.7149897805202,
0.));
#232929=CARTESIAN_POINT('Ctrl Pts',(-20.3538098605706,-9.7149897805202,
12.));
#232930=CARTESIAN_POINT('Ctrl Pts',(-20.3533097561886,-9.7147459035068,
0.));
#232931=CARTESIAN_POINT('Ctrl Pts',(-20.3533097561886,-9.7147459035068,
12.));
#232932=CARTESIAN_POINT('Ctrl Pts',(-20.3531126095522,-9.71465227853041,
0.));
#232933=CARTESIAN_POINT('Ctrl Pts',(-20.3531126095522,-9.71465227853041,
12.));
#232934=CARTESIAN_POINT('Ctrl Pts',(-20.353060251684,-9.71462954053041,
0.));
#232935=CARTESIAN_POINT('Ctrl Pts',(-20.353060251684,-9.71462954053041,
12.));
#232936=CARTESIAN_POINT('Ctrl Pts',(-20.353053841303,-9.71462809124915,
0.));
#232937=CARTESIAN_POINT('Ctrl Pts',(-20.353053841303,-9.71462809124915,
12.));
#232938=CARTESIAN_POINT('',(-22.8400320311649,-12.4230808101438,0.));
#232939=CARTESIAN_POINT('Ctrl Pts',(-22.8400320311649,-12.4230808101438,
0.));
#232940=CARTESIAN_POINT('Ctrl Pts',(-22.8370364396459,-12.418215285186,
0.));
#232941=CARTESIAN_POINT('Ctrl Pts',(-22.8310435872748,-12.4084933766346,
0.));
#232942=CARTESIAN_POINT('Ctrl Pts',(-22.8220493007173,-12.3939379378998,
0.));
#232943=CARTESIAN_POINT('Ctrl Pts',(-22.81004690224,-12.374585536673,0.));
#232944=CARTESIAN_POINT('Ctrl Pts',(-22.795027221673,-12.3504864740319,
0.));
#232945=CARTESIAN_POINT('Ctrl Pts',(-22.7799908974768,-12.3264788926075,
0.));
#232946=CARTESIAN_POINT('Ctrl Pts',(-22.764938010105,-12.3025628601792,
0.));
#232947=CARTESIAN_POINT('Ctrl Pts',(-22.7498686970069,-12.2787384750742,
0.));
#232948=CARTESIAN_POINT('Ctrl Pts',(-22.7347831655287,-12.2550058702395,
0.));
#232949=CARTESIAN_POINT('Ctrl Pts',(-22.7196817119374,-12.2313652198061,
0.));
#232950=CARTESIAN_POINT('Ctrl Pts',(-22.7045647168747,-12.2078167360284,
0.));
#232951=CARTESIAN_POINT('Ctrl Pts',(-22.6894326205037,-12.1843606579261,
0.));
#232952=CARTESIAN_POINT('Ctrl Pts',(-22.6742859034944,-12.1609972423099,
0.));
#232953=CARTESIAN_POINT('Ctrl Pts',(-22.6591250653965,-12.1377267537145,
0.));
#232954=CARTESIAN_POINT('Ctrl Pts',(-22.6439506046605,-12.1145494550383,
0.));
#232955=CARTESIAN_POINT('Ctrl Pts',(-22.6287629967056,-12.0914655972823,
0.));
#232956=CARTESIAN_POINT('Ctrl Pts',(-22.6135626764898,-12.0684754113862,
0.));
#232957=CARTESIAN_POINT('Ctrl Pts',(-22.5983500505644,-12.0455791139128,
0.));
#232958=CARTESIAN_POINT('Ctrl Pts',(-22.5831255061282,-12.0227769113127,
0.));
#232959=CARTESIAN_POINT('Ctrl Pts',(-22.5678894211181,-12.0000690046695,
0.));
#232960=CARTESIAN_POINT('Ctrl Pts',(-22.5526421741158,-11.9774555943496,
0.));
#232961=CARTESIAN_POINT('Ctrl Pts',(-22.5373841537307,-11.9549368843997,
0.));
#232962=CARTESIAN_POINT('Ctrl Pts',(-22.5221157697883,-11.9325130877803,
0.));
#232963=CARTESIAN_POINT('Ctrl Pts',(-22.5068374513973,-11.9101844254557,
0.));
#232964=CARTESIAN_POINT('Ctrl Pts',(-22.4915496418485,-11.8879511239942,
0.));
#232965=CARTESIAN_POINT('Ctrl Pts',(-22.4762527946702,-11.8658134137019,
0.));
#232966=CARTESIAN_POINT('Ctrl Pts',(-22.4609473690471,-11.8437715264487,
0.));
#232967=CARTESIAN_POINT('Ctrl Pts',(-22.4456338258735,-11.8218256937889,
0.));
#232968=CARTESIAN_POINT('Ctrl Pts',(-22.430312622646,-11.7999761445173,
0.));
#232969=CARTESIAN_POINT('Ctrl Pts',(-22.4149842125008,-11.7782231042039,
0.));
#232970=CARTESIAN_POINT('Ctrl Pts',(-22.3996490469191,-11.7565667964764,
0.));
#232971=CARTESIAN_POINT('Ctrl Pts',(-22.3843075773899,-11.7350074437961,
0.));
#232972=CARTESIAN_POINT('Ctrl Pts',(-22.3689602575491,-11.7135452684532,
0.));
#232973=CARTESIAN_POINT('Ctrl Pts',(-22.3536075450029,-11.6921804934056,
0.));
#232974=CARTESIAN_POINT('Ctrl Pts',(-22.3382499035619,-11.6709133432985,
0.));
#232975=CARTESIAN_POINT('Ctrl Pts',(-22.3228878043976,-11.6497440449857,
0.));
#232976=CARTESIAN_POINT('Ctrl Pts',(-22.3075217249049,-11.6286728270009,
0.));
#232977=CARTESIAN_POINT('Ctrl Pts',(-22.2921521480356,-11.6076999192357,
0.));
#232978=CARTESIAN_POINT('Ctrl Pts',(-22.2767795614348,-11.5868255525188,
0.));
#232979=CARTESIAN_POINT('Ctrl Pts',(-22.2614044566898,-11.5660499582403,
0.));
#232980=CARTESIAN_POINT('Ctrl Pts',(-22.2460273284654,-11.5453733679121,
0.));
#232981=CARTESIAN_POINT('Ctrl Pts',(-22.2306486738901,-11.5247960128477,
0.));
#232982=CARTESIAN_POINT('Ctrl Pts',(-22.2152689931022,-11.5043181244242,
0.));
#232983=CARTESIAN_POINT('Ctrl Pts',(-22.1998887896436,-11.483939934259,
0.));
#232984=CARTESIAN_POINT('Ctrl Pts',(-22.184508570917,-11.463661674411,0.));
#232985=CARTESIAN_POINT('Ctrl Pts',(-22.1691288486096,-11.443483577557,
0.));
#232986=CARTESIAN_POINT('Ctrl Pts',(-22.1537501391487,-11.4234058771742,
0.));
#232987=CARTESIAN_POINT('Ctrl Pts',(-22.1383729640964,-11.4034288076908,
0.));
#232988=CARTESIAN_POINT('Ctrl Pts',(-22.1229978500186,-11.3835526044256,
0.));
#232989=CARTESIAN_POINT('Ctrl Pts',(-22.1076253283979,-11.3637775035367,
0.));
#232990=CARTESIAN_POINT('Ctrl Pts',(-22.0922559355294,-11.3441037419553,
0.));
#232991=CARTESIAN_POINT('Ctrl Pts',(-22.0768902124267,-11.3245315573168,
0.));
#232992=CARTESIAN_POINT('Ctrl Pts',(-22.0615287047179,-11.3050611878771,
0.));
#232993=CARTESIAN_POINT('Ctrl Pts',(-22.046171962566,-11.2856928724374,
0.));
#232994=CARTESIAN_POINT('Ctrl Pts',(-22.030820540835,-11.2664268504206,
0.));
#232995=CARTESIAN_POINT('Ctrl Pts',(-22.0154749992363,-11.2472633619275,
0.));
#232996=CARTESIAN_POINT('Ctrl Pts',(-22.0001359024839,-11.2282026477896,
0.));
#232997=CARTESIAN_POINT('Ctrl Pts',(-21.9848038204439,-11.2092449496125,
0.));
#232998=CARTESIAN_POINT('Ctrl Pts',(-21.9694793282914,-11.190390509811,
0.));
#232999=CARTESIAN_POINT('Ctrl Pts',(-21.9541630066506,-11.1716395716376,
0.));
#233000=CARTESIAN_POINT('Ctrl Pts',(-21.9388554416439,-11.1529923792003,
0.));
#233001=CARTESIAN_POINT('Ctrl Pts',(-21.923557224952,-11.1344491774741,
0.));
#233002=CARTESIAN_POINT('Ctrl Pts',(-21.9082689538688,-11.1160102123024,
0.));
#233003=CARTESIAN_POINT('Ctrl Pts',(-21.8929912313608,-11.0976757303944,
0.));
#233004=CARTESIAN_POINT('Ctrl Pts',(-21.877724666119,-11.0794459793057,
0.));
#233005=CARTESIAN_POINT('Ctrl Pts',(-21.8624698726318,-11.0613212074363,
0.));
#233006=CARTESIAN_POINT('Ctrl Pts',(-21.8472274713103,-11.0433016640807,
0.));
#233007=CARTESIAN_POINT('Ctrl Pts',(-21.8319980886033,-11.0253875994598,
0.));
#233008=CARTESIAN_POINT('Ctrl Pts',(-21.8167823571168,-11.0075792647477,
0.));
#233009=CARTESIAN_POINT('Ctrl Pts',(-21.8015809157301,-10.9898769120912,
0.));
#233010=CARTESIAN_POINT('Ctrl Pts',(-21.7863944097141,-10.9722807946155,
0.));
#233011=CARTESIAN_POINT('Ctrl Pts',(-21.7712234908464,-10.9547911664455,
0.));
#233012=CARTESIAN_POINT('Ctrl Pts',(-21.7560688175247,-10.9374082827444,
0.));
#233013=CARTESIAN_POINT('Ctrl Pts',(-21.7409310548797,-10.9201323997384,
0.));
#233014=CARTESIAN_POINT('Ctrl Pts',(-21.7258108748873,-10.902963774734,
0.));
#233015=CARTESIAN_POINT('Ctrl Pts',(-21.7107089564825,-10.8859026661293,
0.));
#233016=CARTESIAN_POINT('Ctrl Pts',(-21.6956259856672,-10.8689493334095,
0.));
#233017=CARTESIAN_POINT('Ctrl Pts',(-21.6805626556467,-10.8521040371835,
0.));
#233018=CARTESIAN_POINT('Ctrl Pts',(-21.6655196669732,-10.8353670392272,
0.));
#233019=CARTESIAN_POINT('Ctrl Pts',(-21.6504977276866,-10.8187386025136,
0.));
#233020=CARTESIAN_POINT('Ctrl Pts',(-21.6354975534557,-10.8022189912369,
0.));
#233021=CARTESIAN_POINT('Ctrl Pts',(-21.6205198677173,-10.7858084708261,
0.));
#233022=CARTESIAN_POINT('Ctrl Pts',(-21.6055654018176,-10.7695073079552,
0.));
#233023=CARTESIAN_POINT('Ctrl Pts',(-21.5906348951743,-10.7533157705941,
0.));
#233024=CARTESIAN_POINT('Ctrl Pts',(-21.5757290954371,-10.7372341280467,
0.));
#233025=CARTESIAN_POINT('Ctrl Pts',(-21.5608487586468,-10.7212626509816,
0.));
#233026=CARTESIAN_POINT('Ctrl Pts',(-21.5459946493955,-10.7054016114571,
0.));
#233027=CARTESIAN_POINT('Ctrl Pts',(-21.5311675409807,-10.689651282929,
0.));
#233028=CARTESIAN_POINT('Ctrl Pts',(-21.51636821558,-10.6740119402834,0.));
#233029=CARTESIAN_POINT('Ctrl Pts',(-21.5015974644449,-10.6584838598939,
0.));
#233030=CARTESIAN_POINT('Ctrl Pts',(-21.4868560880889,-10.6430673196607,
0.));
#233031=CARTESIAN_POINT('Ctrl Pts',(-21.4721448964766,-10.6277625990456,
0.));
#233032=CARTESIAN_POINT('Ctrl Pts',(-21.4574647092097,-10.6125699790961,
0.));
#233033=CARTESIAN_POINT('Ctrl Pts',(-21.4428163557144,-10.5974897424622,
0.));
#233034=CARTESIAN_POINT('Ctrl Pts',(-21.4282006754631,-10.5825221734573,
0.));
#233035=CARTESIAN_POINT('Ctrl Pts',(-21.4136185181979,-10.5676675581108,
0.));
#233036=CARTESIAN_POINT('Ctrl Pts',(-21.3990707441497,-10.5529261842108,
0.));
#233037=CARTESIAN_POINT('Ctrl Pts',(-21.3845582242602,-10.5382983413421,
0.));
#233038=CARTESIAN_POINT('Ctrl Pts',(-21.3700818403936,-10.5237843209057,
0.));
#233039=CARTESIAN_POINT('Ctrl Pts',(-21.3556424855814,-10.5093844161685,
0.));
#233040=CARTESIAN_POINT('Ctrl Pts',(-21.3412410642904,-10.4950989223337,
0.));
#233041=CARTESIAN_POINT('Ctrl Pts',(-21.3268784926819,-10.4809281365931,
0.));
#233042=CARTESIAN_POINT('Ctrl Pts',(-21.3125556988731,-10.4668723581768,
0.));
#233043=CARTESIAN_POINT('Ctrl Pts',(-21.2982736231931,-10.4529318883874,
0.));
#233044=CARTESIAN_POINT('Ctrl Pts',(-21.2840332184483,-10.4391070306391,
0.));
#233045=CARTESIAN_POINT('Ctrl Pts',(-21.2698354502403,-10.42539809054,0.));
#233046=CARTESIAN_POINT('Ctrl Pts',(-21.255681297275,-10.4118053759588,
0.));
#233047=CARTESIAN_POINT('Ctrl Pts',(-21.2415717516714,-10.3983291970846,
0.));
#233048=CARTESIAN_POINT('Ctrl Pts',(-21.22750781927,-10.3849698664786,0.));
#233049=CARTESIAN_POINT('Ctrl Pts',(-21.2134905199345,-10.371727699113,
0.));
#233050=CARTESIAN_POINT('Ctrl Pts',(-21.199520887919,-10.3586030124587,
0.));
#233051=CARTESIAN_POINT('Ctrl Pts',(-21.1855999722416,-10.34559612657,0.));
#233052=CARTESIAN_POINT('Ctrl Pts',(-21.1717288370509,-10.3327073641572,
0.));
#233053=CARTESIAN_POINT('Ctrl Pts',(-21.1579085619965,-10.3199370506544,
0.));
#233054=CARTESIAN_POINT('Ctrl Pts',(-21.1441402425843,-10.3072855142687,
0.));
#233055=CARTESIAN_POINT('Ctrl Pts',(-21.1304249906002,-10.2947530860721,
0.));
#233056=CARTESIAN_POINT('Ctrl Pts',(-21.1167639345631,-10.2823401001072,
0.));
#233057=CARTESIAN_POINT('Ctrl Pts',(-21.1031582201627,-10.2700468934744,
0.));
#233058=CARTESIAN_POINT('Ctrl Pts',(-21.0896090107063,-10.2578738064181,
0.));
#233059=CARTESIAN_POINT('Ctrl Pts',(-21.0761174875445,-10.2458211823912,
0.));
#233060=CARTESIAN_POINT('Ctrl Pts',(-21.0626848505663,-10.2338893681567,
0.));
#233061=CARTESIAN_POINT('Ctrl Pts',(-21.0493123187483,-10.2220787139154,
0.));
#233062=CARTESIAN_POINT('Ctrl Pts',(-21.0360011306815,-10.2103895734123,
0.));
#233063=CARTESIAN_POINT('Ctrl Pts',(-21.0227525451107,-10.1988223040425,
0.));
#233064=CARTESIAN_POINT('Ctrl Pts',(-21.0095678414486,-10.187377266936,
0.));
#233065=CARTESIAN_POINT('Ctrl Pts',(-20.9964483203686,-10.1760548270767,
0.));
#233066=CARTESIAN_POINT('Ctrl Pts',(-20.9833953044736,-10.1648553534568,
0.));
#233067=CARTESIAN_POINT('Ctrl Pts',(-20.9704101389369,-10.1537792192065,
0.));
#233068=CARTESIAN_POINT('Ctrl Pts',(-20.9574941921591,-10.1428268017256,
0.));
#233069=CARTESIAN_POINT('Ctrl Pts',(-20.9446488563933,-10.1319984827908,
0.));
#233070=CARTESIAN_POINT('Ctrl Pts',(-20.9318755484734,-10.1212946487057,
0.));
#233071=CARTESIAN_POINT('Ctrl Pts',(-20.919175710627,-10.1107156904836,
0.));
#233072=CARTESIAN_POINT('Ctrl Pts',(-20.9065508112557,-10.1002620040076,
0.));
#233073=CARTESIAN_POINT('Ctrl Pts',(-20.894002345737,-10.0899339901915,
0.));
#233074=CARTESIAN_POINT('Ctrl Pts',(-20.881531837184,-10.0797320551154,
0.));
#233075=CARTESIAN_POINT('Ctrl Pts',(-20.86914083737,-10.0696566102218,0.));
#233076=CARTESIAN_POINT('Ctrl Pts',(-20.8568309277316,-10.0597080725375,
0.));
#233077=CARTESIAN_POINT('Ctrl Pts',(-20.8446037203402,-10.0498868648733,
0.));
#233078=CARTESIAN_POINT('Ctrl Pts',(-20.8324608588909,-10.0401934160234,
0.));
#233079=CARTESIAN_POINT('Ctrl Pts',(-20.8204040196602,-10.0306281609435,
0.));
#233080=CARTESIAN_POINT('Ctrl Pts',(-20.8084349126888,-10.0211915410095,
0.));
#233081=CARTESIAN_POINT('Ctrl Pts',(-20.7965552829908,-10.0118840042786,
0.));
#233082=CARTESIAN_POINT('Ctrl Pts',(-20.7847669117568,-10.0027060057389,
0.));
#233083=CARTESIAN_POINT('Ctrl Pts',(-20.7730716175417,-9.9936580075464,
0.));
#233084=CARTESIAN_POINT('Ctrl Pts',(-20.761471257499,-9.98474047926852,
0.));
#233085=CARTESIAN_POINT('Ctrl Pts',(-20.7499677289627,-9.9759538982347,
0.));
#233086=CARTESIAN_POINT('Ctrl Pts',(-20.7385629709795,-9.96729874986201,
0.));
#233087=CARTESIAN_POINT('Ctrl Pts',(-20.7272589658751,-9.95877552798397,
0.));
#233088=CARTESIAN_POINT('Ctrl Pts',(-20.7160577407579,-9.95038473514948,
0.));
#233089=CARTESIAN_POINT('Ctrl Pts',(-20.7049613692234,-9.94212688298236,
0.));
#233090=CARTESIAN_POINT('Ctrl Pts',(-20.6939719732484,-9.93400249259729,
0.));
#233091=CARTESIAN_POINT('Ctrl Pts',(-20.6830917250255,-9.92601209498748,
0.));
#233092=CARTESIAN_POINT('Ctrl Pts',(-20.6723228488263,-9.91815623141288,
0.));
#233093=CARTESIAN_POINT('Ctrl Pts',(-20.6616676228315,-9.91043545377007,
0.));
#233094=CARTESIAN_POINT('Ctrl Pts',(-20.6511283817414,-9.90285032516692,
0.));
#233095=CARTESIAN_POINT('Ctrl Pts',(-20.6407075193976,-9.89540142049119,
0.));
#233096=CARTESIAN_POINT('Ctrl Pts',(-20.6304074914087,-9.88808932697306,
0.));
#233097=CARTESIAN_POINT('Ctrl Pts',(-20.6202308177474,-9.88091464472675,
0.));
#233098=CARTESIAN_POINT('Ctrl Pts',(-20.6101800854494,-9.87387798732956,
0.));
#233099=CARTESIAN_POINT('Ctrl Pts',(-20.6002579513699,-9.86697998242622,
0.));
#233100=CARTESIAN_POINT('Ctrl Pts',(-20.5904671449754,-9.86022127232747,
0.));
#233101=CARTESIAN_POINT('Ctrl Pts',(-20.5808104710015,-9.8536025145698,
0.));
#233102=CARTESIAN_POINT('Ctrl Pts',(-20.5712908125139,-9.84712438256277,
0.));
#233103=CARTESIAN_POINT('Ctrl Pts',(-20.5619111362402,-9.84078756677565,
0.));
#233104=CARTESIAN_POINT('Ctrl Pts',(-20.552674497646,-9.83459277585315,
0.));
#233105=CARTESIAN_POINT('Ctrl Pts',(-20.5435840460721,-9.82854073773877,
0.));
#233106=CARTESIAN_POINT('Ctrl Pts',(-20.5346430299517,-9.82263220080362,
0.));
#233107=CARTESIAN_POINT('Ctrl Pts',(-20.5258548000629,-9.81686793455942,
0.));
#233108=CARTESIAN_POINT('Ctrl Pts',(-20.517222812284,-9.81124873025281,
0.));
#233109=CARTESIAN_POINT('Ctrl Pts',(-20.5087506310505,-9.80577540161087,
0.));
#233110=CARTESIAN_POINT('Ctrl Pts',(-20.5004419312107,-9.80044878520948,
0.));
#233111=CARTESIAN_POINT('Ctrl Pts',(-20.4923005087943,-9.7952697428833,
0.));
#233112=CARTESIAN_POINT('Ctrl Pts',(-20.4843302955329,-9.79023916498655,
0.));
#233113=CARTESIAN_POINT('Ctrl Pts',(-20.4765353711586,-9.78535797314166,
0.));
#233114=CARTESIAN_POINT('Ctrl Pts',(-20.4689199790669,-9.7806271237332,
0.));
#233115=CARTESIAN_POINT('Ctrl Pts',(-20.4614885274975,-9.77604760815528,
0.));
#233116=CARTESIAN_POINT('Ctrl Pts',(-20.4542455817527,-9.77162045104069,
0.));
#233117=CARTESIAN_POINT('Ctrl Pts',(-20.447195862298,-9.76734670980891,
0.));
#233118=CARTESIAN_POINT('Ctrl Pts',(-20.44034423294,-9.76322747195494,0.));
#233119=CARTESIAN_POINT('Ctrl Pts',(-20.4336957355473,-9.75926386289922,
0.));
#233120=CARTESIAN_POINT('Ctrl Pts',(-20.4272556476629,-9.75545705902417,
0.));
#233121=CARTESIAN_POINT('Ctrl Pts',(-20.4210295275817,-9.7518082978643,
0.));
#233122=CARTESIAN_POINT('Ctrl Pts',(-20.4150232777393,-9.74831889242174,
0.));
#233123=CARTESIAN_POINT('Ctrl Pts',(-20.4092430879861,-9.74499021838537,
0.));
#233124=CARTESIAN_POINT('Ctrl Pts',(-20.4036953576549,-9.74182369656271,
0.));
#233125=CARTESIAN_POINT('Ctrl Pts',(-20.3983866213331,-9.738820776132,0.));
#233126=CARTESIAN_POINT('Ctrl Pts',(-20.3933234845647,-9.73598292014242,
0.));
#233127=CARTESIAN_POINT('Ctrl Pts',(-20.3885129129912,-9.73331167102807,
0.));
#233128=CARTESIAN_POINT('Ctrl Pts',(-20.3839624556742,-9.73080870123727,
0.));
#233129=CARTESIAN_POINT('Ctrl Pts',(-20.3796805893304,-9.72847589116541,
0.));
#233130=CARTESIAN_POINT('Ctrl Pts',(-20.3756766651951,-9.7263153173288,
0.));
#233131=CARTESIAN_POINT('Ctrl Pts',(-20.371960235676,-9.72432910043194,
0.));
#233132=CARTESIAN_POINT('Ctrl Pts',(-20.3685406190576,-9.72251930722489,
0.));
#233133=CARTESIAN_POINT('Ctrl Pts',(-20.3654261611056,-9.7208877838108,
0.));
#233134=CARTESIAN_POINT('Ctrl Pts',(-20.3626256913981,-9.71943648548099,
0.));
#233135=CARTESIAN_POINT('Ctrl Pts',(-20.3601498764344,-9.71816778328006,
0.));
#233136=CARTESIAN_POINT('Ctrl Pts',(-20.3580133103356,-9.71708493723096,
0.));
#233137=CARTESIAN_POINT('Ctrl Pts',(-20.3562337557875,-9.71619192554185,
0.));
#233138=CARTESIAN_POINT('Ctrl Pts',(-20.3548282742361,-9.71549257088172,
0.));
#233139=CARTESIAN_POINT('Ctrl Pts',(-20.3538098605706,-9.7149897805202,
0.));
#233140=CARTESIAN_POINT('Ctrl Pts',(-20.3533097561886,-9.7147459035068,
0.));
#233141=CARTESIAN_POINT('Ctrl Pts',(-20.3531126095522,-9.71465227853041,
0.));
#233142=CARTESIAN_POINT('Ctrl Pts',(-20.353060251684,-9.71462954053041,
0.));
#233143=CARTESIAN_POINT('Ctrl Pts',(-20.353053841303,-9.71462809124915,
0.));
#233144=CARTESIAN_POINT('',(-22.8400320311649,-12.4230808101438,12.));
#233145=CARTESIAN_POINT('',(-22.8400320311649,-12.4230808101438,0.));
#233146=CARTESIAN_POINT('Ctrl Pts',(-20.353053841303,-9.71462809124915,
12.));
#233147=CARTESIAN_POINT('Ctrl Pts',(-20.353060251684,-9.71462954053041,
12.));
#233148=CARTESIAN_POINT('Ctrl Pts',(-20.3531126095522,-9.71465227853041,
12.));
#233149=CARTESIAN_POINT('Ctrl Pts',(-20.3533097561886,-9.7147459035068,
12.));
#233150=CARTESIAN_POINT('Ctrl Pts',(-20.3538098605706,-9.7149897805202,
12.));
#233151=CARTESIAN_POINT('Ctrl Pts',(-20.3548282742361,-9.71549257088172,
12.));
#233152=CARTESIAN_POINT('Ctrl Pts',(-20.3562337557875,-9.71619192554185,
12.));
#233153=CARTESIAN_POINT('Ctrl Pts',(-20.3580133103356,-9.71708493723096,
12.));
#233154=CARTESIAN_POINT('Ctrl Pts',(-20.3601498764344,-9.71816778328006,
12.));
#233155=CARTESIAN_POINT('Ctrl Pts',(-20.3626256913981,-9.71943648548099,
12.));
#233156=CARTESIAN_POINT('Ctrl Pts',(-20.3654261611056,-9.7208877838108,
12.));
#233157=CARTESIAN_POINT('Ctrl Pts',(-20.3685406190576,-9.72251930722489,
12.));
#233158=CARTESIAN_POINT('Ctrl Pts',(-20.371960235676,-9.72432910043194,
12.));
#233159=CARTESIAN_POINT('Ctrl Pts',(-20.3756766651951,-9.7263153173288,
12.));
#233160=CARTESIAN_POINT('Ctrl Pts',(-20.3796805893304,-9.72847589116541,
12.));
#233161=CARTESIAN_POINT('Ctrl Pts',(-20.3839624556742,-9.73080870123727,
12.));
#233162=CARTESIAN_POINT('Ctrl Pts',(-20.3885129129912,-9.73331167102807,
12.));
#233163=CARTESIAN_POINT('Ctrl Pts',(-20.3933234845647,-9.73598292014242,
12.));
#233164=CARTESIAN_POINT('Ctrl Pts',(-20.3983866213331,-9.738820776132,12.));
#233165=CARTESIAN_POINT('Ctrl Pts',(-20.4036953576549,-9.74182369656271,
12.));
#233166=CARTESIAN_POINT('Ctrl Pts',(-20.4092430879861,-9.74499021838537,
12.));
#233167=CARTESIAN_POINT('Ctrl Pts',(-20.4150232777393,-9.74831889242174,
12.));
#233168=CARTESIAN_POINT('Ctrl Pts',(-20.4210295275817,-9.7518082978643,
12.));
#233169=CARTESIAN_POINT('Ctrl Pts',(-20.4272556476629,-9.75545705902417,
12.));
#233170=CARTESIAN_POINT('Ctrl Pts',(-20.4336957355473,-9.75926386289922,
12.));
#233171=CARTESIAN_POINT('Ctrl Pts',(-20.44034423294,-9.76322747195494,12.));
#233172=CARTESIAN_POINT('Ctrl Pts',(-20.447195862298,-9.76734670980891,
12.));
#233173=CARTESIAN_POINT('Ctrl Pts',(-20.4542455817527,-9.77162045104069,
12.));
#233174=CARTESIAN_POINT('Ctrl Pts',(-20.4614885274975,-9.77604760815528,
12.));
#233175=CARTESIAN_POINT('Ctrl Pts',(-20.4689199790669,-9.7806271237332,
12.));
#233176=CARTESIAN_POINT('Ctrl Pts',(-20.4765353711586,-9.78535797314166,
12.));
#233177=CARTESIAN_POINT('Ctrl Pts',(-20.4843302955329,-9.79023916498655,
12.));
#233178=CARTESIAN_POINT('Ctrl Pts',(-20.4923005087943,-9.7952697428833,
12.));
#233179=CARTESIAN_POINT('Ctrl Pts',(-20.5004419312107,-9.80044878520948,
12.));
#233180=CARTESIAN_POINT('Ctrl Pts',(-20.5087506310505,-9.80577540161087,
12.));
#233181=CARTESIAN_POINT('Ctrl Pts',(-20.517222812284,-9.81124873025281,
12.));
#233182=CARTESIAN_POINT('Ctrl Pts',(-20.5258548000629,-9.81686793455942,
12.));
#233183=CARTESIAN_POINT('Ctrl Pts',(-20.5346430299517,-9.82263220080362,
12.));
#233184=CARTESIAN_POINT('Ctrl Pts',(-20.5435840460721,-9.82854073773877,
12.));
#233185=CARTESIAN_POINT('Ctrl Pts',(-20.552674497646,-9.83459277585315,
12.));
#233186=CARTESIAN_POINT('Ctrl Pts',(-20.5619111362402,-9.84078756677565,
12.));
#233187=CARTESIAN_POINT('Ctrl Pts',(-20.5712908125139,-9.84712438256277,
12.));
#233188=CARTESIAN_POINT('Ctrl Pts',(-20.5808104710015,-9.8536025145698,
12.));
#233189=CARTESIAN_POINT('Ctrl Pts',(-20.5904671449754,-9.86022127232747,
12.));
#233190=CARTESIAN_POINT('Ctrl Pts',(-20.6002579513699,-9.86697998242622,
12.));
#233191=CARTESIAN_POINT('Ctrl Pts',(-20.6101800854494,-9.87387798732956,
12.));
#233192=CARTESIAN_POINT('Ctrl Pts',(-20.6202308177474,-9.88091464472675,
12.));
#233193=CARTESIAN_POINT('Ctrl Pts',(-20.6304074914087,-9.88808932697306,
12.));
#233194=CARTESIAN_POINT('Ctrl Pts',(-20.6407075193976,-9.89540142049119,
12.));
#233195=CARTESIAN_POINT('Ctrl Pts',(-20.6511283817414,-9.90285032516692,
12.));
#233196=CARTESIAN_POINT('Ctrl Pts',(-20.6616676228315,-9.91043545377007,
12.));
#233197=CARTESIAN_POINT('Ctrl Pts',(-20.6723228488263,-9.91815623141288,
12.));
#233198=CARTESIAN_POINT('Ctrl Pts',(-20.6830917250255,-9.92601209498748,
12.));
#233199=CARTESIAN_POINT('Ctrl Pts',(-20.6939719732484,-9.93400249259729,
12.));
#233200=CARTESIAN_POINT('Ctrl Pts',(-20.7049613692234,-9.94212688298236,
12.));
#233201=CARTESIAN_POINT('Ctrl Pts',(-20.7160577407579,-9.95038473514948,
12.));
#233202=CARTESIAN_POINT('Ctrl Pts',(-20.7272589658751,-9.95877552798397,
12.));
#233203=CARTESIAN_POINT('Ctrl Pts',(-20.7385629709795,-9.96729874986201,
12.));
#233204=CARTESIAN_POINT('Ctrl Pts',(-20.7499677289627,-9.9759538982347,
12.));
#233205=CARTESIAN_POINT('Ctrl Pts',(-20.761471257499,-9.98474047926852,
12.));
#233206=CARTESIAN_POINT('Ctrl Pts',(-20.7730716175417,-9.9936580075464,
12.));
#233207=CARTESIAN_POINT('Ctrl Pts',(-20.7847669117568,-10.0027060057389,
12.));
#233208=CARTESIAN_POINT('Ctrl Pts',(-20.7965552829908,-10.0118840042786,
12.));
#233209=CARTESIAN_POINT('Ctrl Pts',(-20.8084349126888,-10.0211915410095,
12.));
#233210=CARTESIAN_POINT('Ctrl Pts',(-20.8204040196602,-10.0306281609435,
12.));
#233211=CARTESIAN_POINT('Ctrl Pts',(-20.8324608588909,-10.0401934160234,
12.));
#233212=CARTESIAN_POINT('Ctrl Pts',(-20.8446037203402,-10.0498868648733,
12.));
#233213=CARTESIAN_POINT('Ctrl Pts',(-20.8568309277316,-10.0597080725375,
12.));
#233214=CARTESIAN_POINT('Ctrl Pts',(-20.86914083737,-10.0696566102218,12.));
#233215=CARTESIAN_POINT('Ctrl Pts',(-20.881531837184,-10.0797320551154,
12.));
#233216=CARTESIAN_POINT('Ctrl Pts',(-20.894002345737,-10.0899339901915,
12.));
#233217=CARTESIAN_POINT('Ctrl Pts',(-20.9065508112557,-10.1002620040076,
12.));
#233218=CARTESIAN_POINT('Ctrl Pts',(-20.919175710627,-10.1107156904836,
12.));
#233219=CARTESIAN_POINT('Ctrl Pts',(-20.9318755484734,-10.1212946487057,
12.));
#233220=CARTESIAN_POINT('Ctrl Pts',(-20.9446488563933,-10.1319984827908,
12.));
#233221=CARTESIAN_POINT('Ctrl Pts',(-20.9574941921591,-10.1428268017256,
12.));
#233222=CARTESIAN_POINT('Ctrl Pts',(-20.9704101389369,-10.1537792192065,
12.));
#233223=CARTESIAN_POINT('Ctrl Pts',(-20.9833953044736,-10.1648553534568,
12.));
#233224=CARTESIAN_POINT('Ctrl Pts',(-20.9964483203686,-10.1760548270767,
12.));
#233225=CARTESIAN_POINT('Ctrl Pts',(-21.0095678414486,-10.187377266936,
12.));
#233226=CARTESIAN_POINT('Ctrl Pts',(-21.0227525451107,-10.1988223040425,
12.));
#233227=CARTESIAN_POINT('Ctrl Pts',(-21.0360011306815,-10.2103895734123,
12.));
#233228=CARTESIAN_POINT('Ctrl Pts',(-21.0493123187483,-10.2220787139154,
12.));
#233229=CARTESIAN_POINT('Ctrl Pts',(-21.0626848505663,-10.2338893681567,
12.));
#233230=CARTESIAN_POINT('Ctrl Pts',(-21.0761174875445,-10.2458211823912,
12.));
#233231=CARTESIAN_POINT('Ctrl Pts',(-21.0896090107063,-10.2578738064181,
12.));
#233232=CARTESIAN_POINT('Ctrl Pts',(-21.1031582201627,-10.2700468934744,
12.));
#233233=CARTESIAN_POINT('Ctrl Pts',(-21.1167639345631,-10.2823401001072,
12.));
#233234=CARTESIAN_POINT('Ctrl Pts',(-21.1304249906002,-10.2947530860721,
12.));
#233235=CARTESIAN_POINT('Ctrl Pts',(-21.1441402425843,-10.3072855142687,
12.));
#233236=CARTESIAN_POINT('Ctrl Pts',(-21.1579085619965,-10.3199370506544,
12.));
#233237=CARTESIAN_POINT('Ctrl Pts',(-21.1717288370509,-10.3327073641572,
12.));
#233238=CARTESIAN_POINT('Ctrl Pts',(-21.1855999722416,-10.34559612657,12.));
#233239=CARTESIAN_POINT('Ctrl Pts',(-21.199520887919,-10.3586030124587,
12.));
#233240=CARTESIAN_POINT('Ctrl Pts',(-21.2134905199345,-10.371727699113,
12.));
#233241=CARTESIAN_POINT('Ctrl Pts',(-21.22750781927,-10.3849698664786,12.));
#233242=CARTESIAN_POINT('Ctrl Pts',(-21.2415717516714,-10.3983291970846,
12.));
#233243=CARTESIAN_POINT('Ctrl Pts',(-21.255681297275,-10.4118053759588,
12.));
#233244=CARTESIAN_POINT('Ctrl Pts',(-21.2698354502403,-10.42539809054,12.));
#233245=CARTESIAN_POINT('Ctrl Pts',(-21.2840332184483,-10.4391070306391,
12.));
#233246=CARTESIAN_POINT('Ctrl Pts',(-21.2982736231931,-10.4529318883874,
12.));
#233247=CARTESIAN_POINT('Ctrl Pts',(-21.3125556988731,-10.4668723581768,
12.));
#233248=CARTESIAN_POINT('Ctrl Pts',(-21.3268784926819,-10.4809281365931,
12.));
#233249=CARTESIAN_POINT('Ctrl Pts',(-21.3412410642904,-10.4950989223337,
12.));
#233250=CARTESIAN_POINT('Ctrl Pts',(-21.3556424855814,-10.5093844161685,
12.));
#233251=CARTESIAN_POINT('Ctrl Pts',(-21.3700818403936,-10.5237843209057,
12.));
#233252=CARTESIAN_POINT('Ctrl Pts',(-21.3845582242602,-10.5382983413421,
12.));
#233253=CARTESIAN_POINT('Ctrl Pts',(-21.3990707441497,-10.5529261842108,
12.));
#233254=CARTESIAN_POINT('Ctrl Pts',(-21.4136185181979,-10.5676675581108,
12.));
#233255=CARTESIAN_POINT('Ctrl Pts',(-21.4282006754631,-10.5825221734573,
12.));
#233256=CARTESIAN_POINT('Ctrl Pts',(-21.4428163557144,-10.5974897424622,
12.));
#233257=CARTESIAN_POINT('Ctrl Pts',(-21.4574647092097,-10.6125699790961,
12.));
#233258=CARTESIAN_POINT('Ctrl Pts',(-21.4721448964766,-10.6277625990456,
12.));
#233259=CARTESIAN_POINT('Ctrl Pts',(-21.4868560880889,-10.6430673196607,
12.));
#233260=CARTESIAN_POINT('Ctrl Pts',(-21.5015974644449,-10.6584838598939,
12.));
#233261=CARTESIAN_POINT('Ctrl Pts',(-21.51636821558,-10.6740119402834,12.));
#233262=CARTESIAN_POINT('Ctrl Pts',(-21.5311675409807,-10.689651282929,
12.));
#233263=CARTESIAN_POINT('Ctrl Pts',(-21.5459946493955,-10.7054016114571,
12.));
#233264=CARTESIAN_POINT('Ctrl Pts',(-21.5608487586468,-10.7212626509816,
12.));
#233265=CARTESIAN_POINT('Ctrl Pts',(-21.5757290954371,-10.7372341280467,
12.));
#233266=CARTESIAN_POINT('Ctrl Pts',(-21.5906348951743,-10.7533157705941,
12.));
#233267=CARTESIAN_POINT('Ctrl Pts',(-21.6055654018176,-10.7695073079552,
12.));
#233268=CARTESIAN_POINT('Ctrl Pts',(-21.6205198677173,-10.7858084708261,
12.));
#233269=CARTESIAN_POINT('Ctrl Pts',(-21.6354975534557,-10.8022189912369,
12.));
#233270=CARTESIAN_POINT('Ctrl Pts',(-21.6504977276866,-10.8187386025136,
12.));
#233271=CARTESIAN_POINT('Ctrl Pts',(-21.6655196669732,-10.8353670392272,
12.));
#233272=CARTESIAN_POINT('Ctrl Pts',(-21.6805626556467,-10.8521040371835,
12.));
#233273=CARTESIAN_POINT('Ctrl Pts',(-21.6956259856672,-10.8689493334095,
12.));
#233274=CARTESIAN_POINT('Ctrl Pts',(-21.7107089564825,-10.8859026661293,
12.));
#233275=CARTESIAN_POINT('Ctrl Pts',(-21.7258108748873,-10.902963774734,
12.));
#233276=CARTESIAN_POINT('Ctrl Pts',(-21.7409310548797,-10.9201323997384,
12.));
#233277=CARTESIAN_POINT('Ctrl Pts',(-21.7560688175247,-10.9374082827444,
12.));
#233278=CARTESIAN_POINT('Ctrl Pts',(-21.7712234908464,-10.9547911664455,
12.));
#233279=CARTESIAN_POINT('Ctrl Pts',(-21.7863944097141,-10.9722807946155,
12.));
#233280=CARTESIAN_POINT('Ctrl Pts',(-21.8015809157301,-10.9898769120912,
12.));
#233281=CARTESIAN_POINT('Ctrl Pts',(-21.8167823571168,-11.0075792647477,
12.));
#233282=CARTESIAN_POINT('Ctrl Pts',(-21.8319980886033,-11.0253875994598,
12.));
#233283=CARTESIAN_POINT('Ctrl Pts',(-21.8472274713103,-11.0433016640807,
12.));
#233284=CARTESIAN_POINT('Ctrl Pts',(-21.8624698726318,-11.0613212074363,
12.));
#233285=CARTESIAN_POINT('Ctrl Pts',(-21.877724666119,-11.0794459793057,
12.));
#233286=CARTESIAN_POINT('Ctrl Pts',(-21.8929912313608,-11.0976757303944,
12.));
#233287=CARTESIAN_POINT('Ctrl Pts',(-21.9082689538688,-11.1160102123024,
12.));
#233288=CARTESIAN_POINT('Ctrl Pts',(-21.923557224952,-11.1344491774741,
12.));
#233289=CARTESIAN_POINT('Ctrl Pts',(-21.9388554416439,-11.1529923792003,
12.));
#233290=CARTESIAN_POINT('Ctrl Pts',(-21.9541630066506,-11.1716395716376,
12.));
#233291=CARTESIAN_POINT('Ctrl Pts',(-21.9694793282914,-11.190390509811,
12.));
#233292=CARTESIAN_POINT('Ctrl Pts',(-21.9848038204439,-11.2092449496125,
12.));
#233293=CARTESIAN_POINT('Ctrl Pts',(-22.0001359024839,-11.2282026477896,
12.));
#233294=CARTESIAN_POINT('Ctrl Pts',(-22.0154749992363,-11.2472633619275,
12.));
#233295=CARTESIAN_POINT('Ctrl Pts',(-22.030820540835,-11.2664268504206,
12.));
#233296=CARTESIAN_POINT('Ctrl Pts',(-22.046171962566,-11.2856928724374,
12.));
#233297=CARTESIAN_POINT('Ctrl Pts',(-22.0615287047179,-11.3050611878771,
12.));
#233298=CARTESIAN_POINT('Ctrl Pts',(-22.0768902124267,-11.3245315573168,
12.));
#233299=CARTESIAN_POINT('Ctrl Pts',(-22.0922559355294,-11.3441037419553,
12.));
#233300=CARTESIAN_POINT('Ctrl Pts',(-22.1076253283979,-11.3637775035367,
12.));
#233301=CARTESIAN_POINT('Ctrl Pts',(-22.1229978500186,-11.3835526044256,
12.));
#233302=CARTESIAN_POINT('Ctrl Pts',(-22.1383729640964,-11.4034288076908,
12.));
#233303=CARTESIAN_POINT('Ctrl Pts',(-22.1537501391487,-11.4234058771742,
12.));
#233304=CARTESIAN_POINT('Ctrl Pts',(-22.1691288486096,-11.443483577557,
12.));
#233305=CARTESIAN_POINT('Ctrl Pts',(-22.184508570917,-11.463661674411,12.));
#233306=CARTESIAN_POINT('Ctrl Pts',(-22.1998887896436,-11.483939934259,
12.));
#233307=CARTESIAN_POINT('Ctrl Pts',(-22.2152689931022,-11.5043181244242,
12.));
#233308=CARTESIAN_POINT('Ctrl Pts',(-22.2306486738901,-11.5247960128477,
12.));
#233309=CARTESIAN_POINT('Ctrl Pts',(-22.2460273284654,-11.5453733679121,
12.));
#233310=CARTESIAN_POINT('Ctrl Pts',(-22.2614044566898,-11.5660499582403,
12.));
#233311=CARTESIAN_POINT('Ctrl Pts',(-22.2767795614348,-11.5868255525188,
12.));
#233312=CARTESIAN_POINT('Ctrl Pts',(-22.2921521480356,-11.6076999192357,
12.));
#233313=CARTESIAN_POINT('Ctrl Pts',(-22.3075217249049,-11.6286728270009,
12.));
#233314=CARTESIAN_POINT('Ctrl Pts',(-22.3228878043976,-11.6497440449857,
12.));
#233315=CARTESIAN_POINT('Ctrl Pts',(-22.3382499035619,-11.6709133432985,
12.));
#233316=CARTESIAN_POINT('Ctrl Pts',(-22.3536075450029,-11.6921804934056,
12.));
#233317=CARTESIAN_POINT('Ctrl Pts',(-22.3689602575491,-11.7135452684532,
12.));
#233318=CARTESIAN_POINT('Ctrl Pts',(-22.3843075773899,-11.7350074437961,
12.));
#233319=CARTESIAN_POINT('Ctrl Pts',(-22.3996490469191,-11.7565667964764,
12.));
#233320=CARTESIAN_POINT('Ctrl Pts',(-22.4149842125008,-11.7782231042039,
12.));
#233321=CARTESIAN_POINT('Ctrl Pts',(-22.430312622646,-11.7999761445173,
12.));
#233322=CARTESIAN_POINT('Ctrl Pts',(-22.4456338258735,-11.8218256937889,
12.));
#233323=CARTESIAN_POINT('Ctrl Pts',(-22.4609473690471,-11.8437715264487,
12.));
#233324=CARTESIAN_POINT('Ctrl Pts',(-22.4762527946702,-11.8658134137019,
12.));
#233325=CARTESIAN_POINT('Ctrl Pts',(-22.4915496418485,-11.8879511239942,
12.));
#233326=CARTESIAN_POINT('Ctrl Pts',(-22.5068374513973,-11.9101844254557,
12.));
#233327=CARTESIAN_POINT('Ctrl Pts',(-22.5221157697883,-11.9325130877803,
12.));
#233328=CARTESIAN_POINT('Ctrl Pts',(-22.5373841537307,-11.9549368843997,
12.));
#233329=CARTESIAN_POINT('Ctrl Pts',(-22.5526421741158,-11.9774555943496,
12.));
#233330=CARTESIAN_POINT('Ctrl Pts',(-22.5678894211181,-12.0000690046695,
12.));
#233331=CARTESIAN_POINT('Ctrl Pts',(-22.5831255061282,-12.0227769113127,
12.));
#233332=CARTESIAN_POINT('Ctrl Pts',(-22.5983500505644,-12.0455791139128,
12.));
#233333=CARTESIAN_POINT('Ctrl Pts',(-22.6135626764898,-12.0684754113862,
12.));
#233334=CARTESIAN_POINT('Ctrl Pts',(-22.6287629967056,-12.0914655972823,
12.));
#233335=CARTESIAN_POINT('Ctrl Pts',(-22.6439506046605,-12.1145494550383,
12.));
#233336=CARTESIAN_POINT('Ctrl Pts',(-22.6591250653965,-12.1377267537145,
12.));
#233337=CARTESIAN_POINT('Ctrl Pts',(-22.6742859034944,-12.1609972423099,
12.));
#233338=CARTESIAN_POINT('Ctrl Pts',(-22.6894326205037,-12.1843606579261,
12.));
#233339=CARTESIAN_POINT('Ctrl Pts',(-22.7045647168747,-12.2078167360284,
12.));
#233340=CARTESIAN_POINT('Ctrl Pts',(-22.7196817119374,-12.2313652198061,
12.));
#233341=CARTESIAN_POINT('Ctrl Pts',(-22.7347831655287,-12.2550058702395,
12.));
#233342=CARTESIAN_POINT('Ctrl Pts',(-22.7498686970069,-12.2787384750742,
12.));
#233343=CARTESIAN_POINT('Ctrl Pts',(-22.764938010105,-12.3025628601792,
12.));
#233344=CARTESIAN_POINT('Ctrl Pts',(-22.7799908974768,-12.3264788926075,
12.));
#233345=CARTESIAN_POINT('Ctrl Pts',(-22.795027221673,-12.3504864740319,
12.));
#233346=CARTESIAN_POINT('Ctrl Pts',(-22.81004690224,-12.374585536673,12.));
#233347=CARTESIAN_POINT('Ctrl Pts',(-22.8220493007173,-12.3939379378998,
12.));
#233348=CARTESIAN_POINT('Ctrl Pts',(-22.8310435872748,-12.4084933766346,
12.));
#233349=CARTESIAN_POINT('Ctrl Pts',(-22.8370364396459,-12.418215285186,
12.));
#233350=CARTESIAN_POINT('Ctrl Pts',(-22.8400320311649,-12.4230808101438,
12.));
#233351=CARTESIAN_POINT('Ctrl Pts',(-21.2610617890679,-7.52250298901264,
0.));
#233352=CARTESIAN_POINT('Ctrl Pts',(-21.2610617890679,-7.52250298901264,
12.));
#233353=CARTESIAN_POINT('Ctrl Pts',(-21.2610673466886,-7.5225064970397,
0.));
#233354=CARTESIAN_POINT('Ctrl Pts',(-21.2610673466886,-7.5225064970397,
12.));
#233355=CARTESIAN_POINT('Ctrl Pts',(-21.2611204474866,-7.52252744144903,
0.));
#233356=CARTESIAN_POINT('Ctrl Pts',(-21.2611204474866,-7.52252744144903,
12.));
#233357=CARTESIAN_POINT('Ctrl Pts',(-21.261326054066,-7.5226006423166,0.));
#233358=CARTESIAN_POINT('Ctrl Pts',(-21.261326054066,-7.5226006423166,12.));
#233359=CARTESIAN_POINT('Ctrl Pts',(-21.2618521283555,-7.52278182242669,
0.));
#233360=CARTESIAN_POINT('Ctrl Pts',(-21.2618521283555,-7.52278182242669,
12.));
#233361=CARTESIAN_POINT('Ctrl Pts',(-21.262927782038,-7.52314642316199,
0.));
#233362=CARTESIAN_POINT('Ctrl Pts',(-21.262927782038,-7.52314642316199,
12.));
#233363=CARTESIAN_POINT('Ctrl Pts',(-21.2644161259962,-7.52364573027552,
0.));
#233364=CARTESIAN_POINT('Ctrl Pts',(-21.2644161259962,-7.52364573027552,
12.));
#233365=CARTESIAN_POINT('Ctrl Pts',(-21.2663059157058,-7.52427261074297,
0.));
#233366=CARTESIAN_POINT('Ctrl Pts',(-21.2663059157058,-7.52427261074297,
12.));
#233367=CARTESIAN_POINT('Ctrl Pts',(-21.2685823838671,-7.5250177033353,
0.));
#233368=CARTESIAN_POINT('Ctrl Pts',(-21.2685823838671,-7.5250177033353,
12.));
#233369=CARTESIAN_POINT('Ctrl Pts',(-21.2712301573466,-7.52587126095529,
0.));
#233370=CARTESIAN_POINT('Ctrl Pts',(-21.2712301573466,-7.52587126095529,
12.));
#233371=CARTESIAN_POINT('Ctrl Pts',(-21.2742366113579,-7.5268252691854,
0.));
#233372=CARTESIAN_POINT('Ctrl Pts',(-21.2742366113579,-7.5268252691854,
12.));
#233373=CARTESIAN_POINT('Ctrl Pts',(-21.2775925269652,-7.52787386225332,
0.));
#233374=CARTESIAN_POINT('Ctrl Pts',(-21.2775925269652,-7.52787386225332,
12.));
#233375=CARTESIAN_POINT('Ctrl Pts',(-21.2812902781143,-7.52901217930407,
0.));
#233376=CARTESIAN_POINT('Ctrl Pts',(-21.2812902781143,-7.52901217930407,
12.));
#233377=CARTESIAN_POINT('Ctrl Pts',(-21.2853226580657,-7.53023562438229,
0.));
#233378=CARTESIAN_POINT('Ctrl Pts',(-21.2853226580657,-7.53023562438229,
12.));
#233379=CARTESIAN_POINT('Ctrl Pts',(-21.2896816163842,-7.53153906987855,
0.));
#233380=CARTESIAN_POINT('Ctrl Pts',(-21.2896816163842,-7.53153906987855,
12.));
#233381=CARTESIAN_POINT('Ctrl Pts',(-21.2943588989331,-7.53291726078526,
0.));
#233382=CARTESIAN_POINT('Ctrl Pts',(-21.2943588989331,-7.53291726078526,
12.));
#233383=CARTESIAN_POINT('Ctrl Pts',(-21.2993464250717,-7.53436505309942,
0.));
#233384=CARTESIAN_POINT('Ctrl Pts',(-21.2993464250717,-7.53436505309942,
12.));
#233385=CARTESIAN_POINT('Ctrl Pts',(-21.3046368712157,-7.53587778251735,
0.));
#233386=CARTESIAN_POINT('Ctrl Pts',(-21.3046368712157,-7.53587778251735,
12.));
#233387=CARTESIAN_POINT('Ctrl Pts',(-21.310223716773,-7.53745129364616,
0.));
#233388=CARTESIAN_POINT('Ctrl Pts',(-21.310223716773,-7.53745129364616,
12.));
#233389=CARTESIAN_POINT('Ctrl Pts',(-21.3161009456256,-7.53908175169898,
0.));
#233390=CARTESIAN_POINT('Ctrl Pts',(-21.3161009456256,-7.53908175169898,
12.));
#233391=CARTESIAN_POINT('Ctrl Pts',(-21.3222628524165,-7.54076552038278,
0.));
#233392=CARTESIAN_POINT('Ctrl Pts',(-21.3222628524165,-7.54076552038278,
12.));
#233393=CARTESIAN_POINT('Ctrl Pts',(-21.328703791771,-7.5424990037703,0.));
#233394=CARTESIAN_POINT('Ctrl Pts',(-21.328703791771,-7.5424990037703,12.));
#233395=CARTESIAN_POINT('Ctrl Pts',(-21.3354182340149,-7.54427868151267,
0.));
#233396=CARTESIAN_POINT('Ctrl Pts',(-21.3354182340149,-7.54427868151267,
12.));
#233397=CARTESIAN_POINT('Ctrl Pts',(-21.3424008295038,-7.54610114948346,
0.));
#233398=CARTESIAN_POINT('Ctrl Pts',(-21.3424008295038,-7.54610114948346,
12.));
#233399=CARTESIAN_POINT('Ctrl Pts',(-21.3496464761531,-7.5479631624633,
0.));
#233400=CARTESIAN_POINT('Ctrl Pts',(-21.3496464761531,-7.5479631624633,
12.));
#233401=CARTESIAN_POINT('Ctrl Pts',(-21.3571503685855,-7.54986166521309,
0.));
#233402=CARTESIAN_POINT('Ctrl Pts',(-21.3571503685855,-7.54986166521309,
12.));
#233403=CARTESIAN_POINT('Ctrl Pts',(-21.3649079431865,-7.55179375777443,
0.));
#233404=CARTESIAN_POINT('Ctrl Pts',(-21.3649079431865,-7.55179375777443,
12.));
#233405=CARTESIAN_POINT('Ctrl Pts',(-21.3729148390243,-7.55375667080028,
0.));
#233406=CARTESIAN_POINT('Ctrl Pts',(-21.3729148390243,-7.55375667080028,
12.));
#233407=CARTESIAN_POINT('Ctrl Pts',(-21.3811668478932,-7.55574773403502,
0.));
#233408=CARTESIAN_POINT('Ctrl Pts',(-21.3811668478932,-7.55574773403502,
12.));
#233409=CARTESIAN_POINT('Ctrl Pts',(-21.3896598842117,-7.55776435731416,
0.));
#233410=CARTESIAN_POINT('Ctrl Pts',(-21.3896598842117,-7.55776435731416,
12.));
#233411=CARTESIAN_POINT('Ctrl Pts',(-21.3983899952987,-7.5598040370061,
0.));
#233412=CARTESIAN_POINT('Ctrl Pts',(-21.3983899952987,-7.5598040370061,
12.));
#233413=CARTESIAN_POINT('Ctrl Pts',(-21.4073533630365,-7.56186435703621,
0.));
#233414=CARTESIAN_POINT('Ctrl Pts',(-21.4073533630365,-7.56186435703621,
12.));
#233415=CARTESIAN_POINT('Ctrl Pts',(-21.4165463106254,-7.56394299313684,
0.));
#233416=CARTESIAN_POINT('Ctrl Pts',(-21.4165463106254,-7.56394299313684,
12.));
#233417=CARTESIAN_POINT('Ctrl Pts',(-21.4259653015736,-7.56603771218712,
0.));
#233418=CARTESIAN_POINT('Ctrl Pts',(-21.4259653015736,-7.56603771218712,
12.));
#233419=CARTESIAN_POINT('Ctrl Pts',(-21.4356069261513,-7.56814636360847,
0.));
#233420=CARTESIAN_POINT('Ctrl Pts',(-21.4356069261513,-7.56814636360847,
12.));
#233421=CARTESIAN_POINT('Ctrl Pts',(-21.4454678907509,-7.57026687261165,
0.));
#233422=CARTESIAN_POINT('Ctrl Pts',(-21.4454678907509,-7.57026687261165,
12.));
#233423=CARTESIAN_POINT('Ctrl Pts',(-21.4555450053142,-7.57239723223505,
0.));
#233424=CARTESIAN_POINT('Ctrl Pts',(-21.4555450053142,-7.57239723223505,
12.));
#233425=CARTESIAN_POINT('Ctrl Pts',(-21.4658351740128,-7.57453549743411,
0.));
#233426=CARTESIAN_POINT('Ctrl Pts',(-21.4658351740128,-7.57453549743411,
12.));
#233427=CARTESIAN_POINT('Ctrl Pts',(-21.4763353936762,-7.57667978402987,
0.));
#233428=CARTESIAN_POINT('Ctrl Pts',(-21.4763353936762,-7.57667978402987,
12.));
#233429=CARTESIAN_POINT('Ctrl Pts',(-21.4870427508194,-7.57882826679131,
0.));
#233430=CARTESIAN_POINT('Ctrl Pts',(-21.4870427508194,-7.57882826679131,
12.));
#233431=CARTESIAN_POINT('Ctrl Pts',(-21.4979544192744,-7.58097917790744,
0.));
#233432=CARTESIAN_POINT('Ctrl Pts',(-21.4979544192744,-7.58097917790744,
12.));
#233433=CARTESIAN_POINT('Ctrl Pts',(-21.5090676573873,-7.58313080519179,
0.));
#233434=CARTESIAN_POINT('Ctrl Pts',(-21.5090676573873,-7.58313080519179,
12.));
#233435=CARTESIAN_POINT('Ctrl Pts',(-21.5203798035299,-7.58528148919129,
0.));
#233436=CARTESIAN_POINT('Ctrl Pts',(-21.5203798035299,-7.58528148919129,
12.));
#233437=CARTESIAN_POINT('Ctrl Pts',(-21.5318882716736,-7.58742962034833,
0.));
#233438=CARTESIAN_POINT('Ctrl Pts',(-21.5318882716736,-7.58742962034833,
12.));
#233439=CARTESIAN_POINT('Ctrl Pts',(-21.543590547011,-7.58957363620013,
0.));
#233440=CARTESIAN_POINT('Ctrl Pts',(-21.543590547011,-7.58957363620013,
12.));
#233441=CARTESIAN_POINT('Ctrl Pts',(-21.5554841813462,-7.59171201844776,
0.));
#233442=CARTESIAN_POINT('Ctrl Pts',(-21.5554841813462,-7.59171201844776,
12.));
#233443=CARTESIAN_POINT('Ctrl Pts',(-21.5675667904726,-7.59384329124918,
0.));
#233444=CARTESIAN_POINT('Ctrl Pts',(-21.5675667904726,-7.59384329124918,
12.));
#233445=CARTESIAN_POINT('Ctrl Pts',(-21.5798360518978,-7.59596601973583,
0.));
#233446=CARTESIAN_POINT('Ctrl Pts',(-21.5798360518978,-7.59596601973583,
12.));
#233447=CARTESIAN_POINT('Ctrl Pts',(-21.5922897024466,-7.59807880846194,
0.));
#233448=CARTESIAN_POINT('Ctrl Pts',(-21.5922897024466,-7.59807880846194,
12.));
#233449=CARTESIAN_POINT('Ctrl Pts',(-21.6049255358843,-7.6001802998824,
0.));
#233450=CARTESIAN_POINT('Ctrl Pts',(-21.6049255358843,-7.6001802998824,
12.));
#233451=CARTESIAN_POINT('Ctrl Pts',(-21.617741400599,-7.60226917285428,
0.));
#233452=CARTESIAN_POINT('Ctrl Pts',(-21.617741400599,-7.60226917285428,
12.));
#233453=CARTESIAN_POINT('Ctrl Pts',(-21.6307351973822,-7.60434414118295,
0.));
#233454=CARTESIAN_POINT('Ctrl Pts',(-21.6307351973822,-7.60434414118295,
12.));
#233455=CARTESIAN_POINT('Ctrl Pts',(-21.6439048771743,-7.60640395216356,
0.));
#233456=CARTESIAN_POINT('Ctrl Pts',(-21.6439048771743,-7.60640395216356,
12.));
#233457=CARTESIAN_POINT('Ctrl Pts',(-21.6572484388081,-7.60844738512873,
0.));
#233458=CARTESIAN_POINT('Ctrl Pts',(-21.6572484388081,-7.60844738512873,
12.));
#233459=CARTESIAN_POINT('Ctrl Pts',(-21.6707639267576,-7.61047325000955,
0.));
#233460=CARTESIAN_POINT('Ctrl Pts',(-21.6707639267576,-7.61047325000955,
12.));
#233461=CARTESIAN_POINT('Ctrl Pts',(-21.6844494295815,-7.61248038630268,
0.));
#233462=CARTESIAN_POINT('Ctrl Pts',(-21.6844494295815,-7.61248038630268,
12.));
#233463=CARTESIAN_POINT('Ctrl Pts',(-21.6983030783322,-7.61446766202786,
0.));
#233464=CARTESIAN_POINT('Ctrl Pts',(-21.6983030783322,-7.61446766202786,
12.));
#233465=CARTESIAN_POINT('Ctrl Pts',(-21.7123230449834,-7.6164339727042,
0.));
#233466=CARTESIAN_POINT('Ctrl Pts',(-21.7123230449834,-7.6164339727042,
12.));
#233467=CARTESIAN_POINT('Ctrl Pts',(-21.7265075407975,-7.61837824030537,
0.));
#233468=CARTESIAN_POINT('Ctrl Pts',(-21.7265075407975,-7.61837824030537,
12.));
#233469=CARTESIAN_POINT('Ctrl Pts',(-21.7408548148656,-7.62029941230854,
0.));
#233470=CARTESIAN_POINT('Ctrl Pts',(-21.7408548148656,-7.62029941230854,
12.));
#233471=CARTESIAN_POINT('Ctrl Pts',(-21.7553631528328,-7.62219646084228,
0.));
#233472=CARTESIAN_POINT('Ctrl Pts',(-21.7553631528328,-7.62219646084228,
12.));
#233473=CARTESIAN_POINT('Ctrl Pts',(-21.7700308755584,-7.62406838181166,
0.));
#233474=CARTESIAN_POINT('Ctrl Pts',(-21.7700308755584,-7.62406838181166,
12.));
#233475=CARTESIAN_POINT('Ctrl Pts',(-21.7848563378021,-7.62591419404512,
0.));
#233476=CARTESIAN_POINT('Ctrl Pts',(-21.7848563378021,-7.62591419404512,
12.));
#233477=CARTESIAN_POINT('Ctrl Pts',(-21.799837926858,-7.62773293842389,
0.));
#233478=CARTESIAN_POINT('Ctrl Pts',(-21.799837926858,-7.62773293842389,
12.));
#233479=CARTESIAN_POINT('Ctrl Pts',(-21.814974061509,-7.62952367718126,
0.));
#233480=CARTESIAN_POINT('Ctrl Pts',(-21.814974061509,-7.62952367718126,
12.));
#233481=CARTESIAN_POINT('Ctrl Pts',(-21.8302631910195,-7.63128549323022,
0.));
#233482=CARTESIAN_POINT('Ctrl Pts',(-21.8302631910195,-7.63128549323022,
12.));
#233483=CARTESIAN_POINT('Ctrl Pts',(-21.8457037941084,-7.63301748948935,
0.));
#233484=CARTESIAN_POINT('Ctrl Pts',(-21.8457037941084,-7.63301748948935,
12.));
#233485=CARTESIAN_POINT('Ctrl Pts',(-21.8612943779089,-7.63471878821225,
0.));
#233486=CARTESIAN_POINT('Ctrl Pts',(-21.8612943779089,-7.63471878821225,
12.));
#233487=CARTESIAN_POINT('Ctrl Pts',(-21.8770334769496,-7.63638853033399,
0.));
#233488=CARTESIAN_POINT('Ctrl Pts',(-21.8770334769496,-7.63638853033399,
12.));
#233489=CARTESIAN_POINT('Ctrl Pts',(-21.8929196523514,-7.63802587492034,
0.));
#233490=CARTESIAN_POINT('Ctrl Pts',(-21.8929196523514,-7.63802587492034,
12.));
#233491=CARTESIAN_POINT('Ctrl Pts',(-21.9089514909874,-7.63962999860927,
0.));
#233492=CARTESIAN_POINT('Ctrl Pts',(-21.9089514909874,-7.63962999860927,
12.));
#233493=CARTESIAN_POINT('Ctrl Pts',(-21.9251276046546,-7.64120009506531,
0.));
#233494=CARTESIAN_POINT('Ctrl Pts',(-21.9251276046546,-7.64120009506531,
12.));
#233495=CARTESIAN_POINT('Ctrl Pts',(-21.9414466292072,-7.64273537442682,
0.));
#233496=CARTESIAN_POINT('Ctrl Pts',(-21.9414466292072,-7.64273537442682,
12.));
#233497=CARTESIAN_POINT('Ctrl Pts',(-21.9579072237651,-7.64423506279122,
0.));
#233498=CARTESIAN_POINT('Ctrl Pts',(-21.9579072237651,-7.64423506279122,
12.));
#233499=CARTESIAN_POINT('Ctrl Pts',(-21.9745080700798,-7.64569840177335,
0.));
#233500=CARTESIAN_POINT('Ctrl Pts',(-21.9745080700798,-7.64569840177335,
12.));
#233501=CARTESIAN_POINT('Ctrl Pts',(-21.9912478718542,-7.64712464805249,
0.));
#233502=CARTESIAN_POINT('Ctrl Pts',(-21.9912478718542,-7.64712464805249,
12.));
#233503=CARTESIAN_POINT('Ctrl Pts',(-22.0081253540774,-7.64851307293351,
0.));
#233504=CARTESIAN_POINT('Ctrl Pts',(-22.0081253540774,-7.64851307293351,
12.));
#233505=CARTESIAN_POINT('Ctrl Pts',(-22.0251392623209,-7.64986296190168,
0.));
#233506=CARTESIAN_POINT('Ctrl Pts',(-22.0251392623209,-7.64986296190168,
12.));
#233507=CARTESIAN_POINT('Ctrl Pts',(-22.0422883621174,-7.65117361421358,
0.));
#233508=CARTESIAN_POINT('Ctrl Pts',(-22.0422883621174,-7.65117361421358,
12.));
#233509=CARTESIAN_POINT('Ctrl Pts',(-22.0595714384431,-7.65244434253112,
0.));
#233510=CARTESIAN_POINT('Ctrl Pts',(-22.0595714384431,-7.65244434253112,
12.));
#233511=CARTESIAN_POINT('Ctrl Pts',(-22.0769872951596,-7.65367447254949,
0.));
#233512=CARTESIAN_POINT('Ctrl Pts',(-22.0769872951596,-7.65367447254949,
12.));
#233513=CARTESIAN_POINT('Ctrl Pts',(-22.094534754469,-7.65486334263643,
0.));
#233514=CARTESIAN_POINT('Ctrl Pts',(-22.094534754469,-7.65486334263643,
12.));
#233515=CARTESIAN_POINT('Ctrl Pts',(-22.1122126563329,-7.65601030346806,
0.));
#233516=CARTESIAN_POINT('Ctrl Pts',(-22.1122126563329,-7.65601030346806,
12.));
#233517=CARTESIAN_POINT('Ctrl Pts',(-22.1300198579675,-7.65711471769396,
0.));
#233518=CARTESIAN_POINT('Ctrl Pts',(-22.1300198579675,-7.65711471769396,
12.));
#233519=CARTESIAN_POINT('Ctrl Pts',(-22.1479552334211,-7.65817595963349,
0.));
#233520=CARTESIAN_POINT('Ctrl Pts',(-22.1479552334211,-7.65817595963349,
12.));
#233521=CARTESIAN_POINT('Ctrl Pts',(-22.1660176731178,-7.6591934149693,
0.));
#233522=CARTESIAN_POINT('Ctrl Pts',(-22.1660176731178,-7.6591934149693,
12.));
#233523=CARTESIAN_POINT('Ctrl Pts',(-22.1842060834091,-7.66016648045004,
0.));
#233524=CARTESIAN_POINT('Ctrl Pts',(-22.1842060834091,-7.66016648045004,
12.));
#233525=CARTESIAN_POINT('Ctrl Pts',(-22.2025193860964,-7.6610945635927,
0.));
#233526=CARTESIAN_POINT('Ctrl Pts',(-22.2025193860964,-7.6610945635927,
12.));
#233527=CARTESIAN_POINT('Ctrl Pts',(-22.2209565180085,-7.66197708240399,
0.));
#233528=CARTESIAN_POINT('Ctrl Pts',(-22.2209565180085,-7.66197708240399,
12.));
#233529=CARTESIAN_POINT('Ctrl Pts',(-22.2395164306547,-7.66281346512508,
0.));
#233530=CARTESIAN_POINT('Ctrl Pts',(-22.2395164306547,-7.66281346512508,
12.));
#233531=CARTESIAN_POINT('Ctrl Pts',(-22.258198089848,-7.6636031499764,0.));
#233532=CARTESIAN_POINT('Ctrl Pts',(-22.258198089848,-7.6636031499764,12.));
#233533=CARTESIAN_POINT('Ctrl Pts',(-22.2770004753335,-7.66434558490978,
0.));
#233534=CARTESIAN_POINT('Ctrl Pts',(-22.2770004753335,-7.66434558490978,
12.));
#233535=CARTESIAN_POINT('Ctrl Pts',(-22.2959225803937,-7.66504022736298,
0.));
#233536=CARTESIAN_POINT('Ctrl Pts',(-22.2959225803937,-7.66504022736298,
12.));
#233537=CARTESIAN_POINT('Ctrl Pts',(-22.314963411484,-7.66568654402493,
0.));
#233538=CARTESIAN_POINT('Ctrl Pts',(-22.314963411484,-7.66568654402493,
12.));
#233539=CARTESIAN_POINT('Ctrl Pts',(-22.3341219879469,-7.66628401061952,
0.));
#233540=CARTESIAN_POINT('Ctrl Pts',(-22.3341219879469,-7.66628401061952,
12.));
#233541=CARTESIAN_POINT('Ctrl Pts',(-22.3533973417021,-7.66683211169158,
0.));
#233542=CARTESIAN_POINT('Ctrl Pts',(-22.3533973417021,-7.66683211169158,
12.));
#233543=CARTESIAN_POINT('Ctrl Pts',(-22.372788516936,-7.66733034039882,
0.));
#233544=CARTESIAN_POINT('Ctrl Pts',(-22.372788516936,-7.66733034039882,
12.));
#233545=CARTESIAN_POINT('Ctrl Pts',(-22.3922945697773,-7.66777819830789,
0.));
#233546=CARTESIAN_POINT('Ctrl Pts',(-22.3922945697773,-7.66777819830789,
12.));
#233547=CARTESIAN_POINT('Ctrl Pts',(-22.4119145679758,-7.66817519519639,
0.));
#233548=CARTESIAN_POINT('Ctrl Pts',(-22.4119145679758,-7.66817519519639,
12.));
#233549=CARTESIAN_POINT('Ctrl Pts',(-22.4316475906603,-7.66852084886704,
0.));
#233550=CARTESIAN_POINT('Ctrl Pts',(-22.4316475906603,-7.66852084886704,
12.));
#233551=CARTESIAN_POINT('Ctrl Pts',(-22.4514927280855,-7.66881468496634,
0.));
#233552=CARTESIAN_POINT('Ctrl Pts',(-22.4514927280855,-7.66881468496634,
12.));
#233553=CARTESIAN_POINT('Ctrl Pts',(-22.47144908137,-7.6690562368083,0.));
#233554=CARTESIAN_POINT('Ctrl Pts',(-22.47144908137,-7.6690562368083,12.));
#233555=CARTESIAN_POINT('Ctrl Pts',(-22.4915157622312,-7.66924504520314,
0.));
#233556=CARTESIAN_POINT('Ctrl Pts',(-22.4915157622312,-7.66924504520314,
12.));
#233557=CARTESIAN_POINT('Ctrl Pts',(-22.5116918927032,-7.66938065829107,
0.));
#233558=CARTESIAN_POINT('Ctrl Pts',(-22.5116918927032,-7.66938065829107,
12.));
#233559=CARTESIAN_POINT('Ctrl Pts',(-22.53197660492,-7.66946263138143,0.));
#233560=CARTESIAN_POINT('Ctrl Pts',(-22.53197660492,-7.66946263138143,12.));
#233561=CARTESIAN_POINT('Ctrl Pts',(-22.5523690409116,-7.66949052679692,
0.));
#233562=CARTESIAN_POINT('Ctrl Pts',(-22.5523690409116,-7.66949052679692,
12.));
#233563=CARTESIAN_POINT('Ctrl Pts',(-22.5728683523831,-7.66946391372305,
0.));
#233564=CARTESIAN_POINT('Ctrl Pts',(-22.5728683523831,-7.66946391372305,
12.));
#233565=CARTESIAN_POINT('Ctrl Pts',(-22.5934737004953,-7.66938236806232,
0.));
#233566=CARTESIAN_POINT('Ctrl Pts',(-22.5934737004953,-7.66938236806232,
12.));
#233567=CARTESIAN_POINT('Ctrl Pts',(-22.6141842556243,-7.66924547229413,
0.));
#233568=CARTESIAN_POINT('Ctrl Pts',(-22.6141842556243,-7.66924547229413,
12.));
#233569=CARTESIAN_POINT('Ctrl Pts',(-22.6349991971541,-7.66905281533714,
0.));
#233570=CARTESIAN_POINT('Ctrl Pts',(-22.6349991971541,-7.66905281533714,
12.));
#233571=CARTESIAN_POINT('Ctrl Pts',(-22.6559177133127,-7.66880399241322,
0.));
#233572=CARTESIAN_POINT('Ctrl Pts',(-22.6559177133127,-7.66880399241322,
12.));
#233573=CARTESIAN_POINT('Ctrl Pts',(-22.6769390009885,-7.66849860491742,
0.));
#233574=CARTESIAN_POINT('Ctrl Pts',(-22.6769390009885,-7.66849860491742,
12.));
#233575=CARTESIAN_POINT('Ctrl Pts',(-22.6980622655446,-7.66813626029274,
0.));
#233576=CARTESIAN_POINT('Ctrl Pts',(-22.6980622655446,-7.66813626029274,
12.));
#233577=CARTESIAN_POINT('Ctrl Pts',(-22.7192867206245,-7.66771657191027,
0.));
#233578=CARTESIAN_POINT('Ctrl Pts',(-22.7192867206245,-7.66771657191027,
12.));
#233579=CARTESIAN_POINT('Ctrl Pts',(-22.7406115879513,-7.66723915895439,
0.));
#233580=CARTESIAN_POINT('Ctrl Pts',(-22.7406115879513,-7.66723915895439,
12.));
#233581=CARTESIAN_POINT('Ctrl Pts',(-22.7620360971843,-7.66670364630298,
0.));
#233582=CARTESIAN_POINT('Ctrl Pts',(-22.7620360971843,-7.66670364630298,
12.));
#233583=CARTESIAN_POINT('Ctrl Pts',(-22.7835594857699,-7.66610966441272,
0.));
#233584=CARTESIAN_POINT('Ctrl Pts',(-22.7835594857699,-7.66610966441272,
12.));
#233585=CARTESIAN_POINT('Ctrl Pts',(-22.8051809987833,-7.66545684920987,
0.));
#233586=CARTESIAN_POINT('Ctrl Pts',(-22.8051809987833,-7.66545684920987,
12.));
#233587=CARTESIAN_POINT('Ctrl Pts',(-22.8268998887678,-7.66474484198548,
0.));
#233588=CARTESIAN_POINT('Ctrl Pts',(-22.8268998887678,-7.66474484198548,
12.));
#233589=CARTESIAN_POINT('Ctrl Pts',(-22.848715415557,-7.66397328929802,
0.));
#233590=CARTESIAN_POINT('Ctrl Pts',(-22.848715415557,-7.66397328929802,
12.));
#233591=CARTESIAN_POINT('Ctrl Pts',(-22.8706268461283,-7.66314184287336,
0.));
#233592=CARTESIAN_POINT('Ctrl Pts',(-22.8706268461283,-7.66314184287336,
12.));
#233593=CARTESIAN_POINT('Ctrl Pts',(-22.8926334544883,-7.66225015950155,
0.));
#233594=CARTESIAN_POINT('Ctrl Pts',(-22.8926334544883,-7.66225015950155,
12.));
#233595=CARTESIAN_POINT('Ctrl Pts',(-22.9147345215421,-7.66129790094107,
0.));
#233596=CARTESIAN_POINT('Ctrl Pts',(-22.9147345215421,-7.66129790094107,
12.));
#233597=CARTESIAN_POINT('Ctrl Pts',(-22.9369293349593,-7.66028473382777,
0.));
#233598=CARTESIAN_POINT('Ctrl Pts',(-22.9369293349593,-7.66028473382777,
12.));
#233599=CARTESIAN_POINT('Ctrl Pts',(-22.959217189033,-7.65921032958901,
0.));
#233600=CARTESIAN_POINT('Ctrl Pts',(-22.959217189033,-7.65921032958901,
12.));
#233601=CARTESIAN_POINT('Ctrl Pts',(-22.9815973845296,-7.65807436436431,
0.));
#233602=CARTESIAN_POINT('Ctrl Pts',(-22.9815973845296,-7.65807436436431,
12.));
#233603=CARTESIAN_POINT('Ctrl Pts',(-23.0040692285814,-7.65687651891304,
0.));
#233604=CARTESIAN_POINT('Ctrl Pts',(-23.0040692285814,-7.65687651891304,
12.));
#233605=CARTESIAN_POINT('Ctrl Pts',(-23.0266320345787,-7.65561647852533,
0.));
#233606=CARTESIAN_POINT('Ctrl Pts',(-23.0266320345787,-7.65561647852533,
12.));
#233607=CARTESIAN_POINT('Ctrl Pts',(-23.0492851220528,-7.65429393293945,
0.));
#233608=CARTESIAN_POINT('Ctrl Pts',(-23.0492851220528,-7.65429393293945,
12.));
#233609=CARTESIAN_POINT('Ctrl Pts',(-23.072027816555,-7.65290857626357,
0.));
#233610=CARTESIAN_POINT('Ctrl Pts',(-23.072027816555,-7.65290857626357,
12.));
#233611=CARTESIAN_POINT('Ctrl Pts',(-23.094859449525,-7.65146010690475,
0.));
#233612=CARTESIAN_POINT('Ctrl Pts',(-23.094859449525,-7.65146010690475,
12.));
#233613=CARTESIAN_POINT('Ctrl Pts',(-23.1177793581679,-7.64994822749859,
0.));
#233614=CARTESIAN_POINT('Ctrl Pts',(-23.1177793581679,-7.64994822749859,
12.));
#233615=CARTESIAN_POINT('Ctrl Pts',(-23.1407868853819,-7.64837264482942,
0.));
#233616=CARTESIAN_POINT('Ctrl Pts',(-23.1407868853819,-7.64837264482942,
12.));
#233617=CARTESIAN_POINT('Ctrl Pts',(-23.1638813796694,-7.64673306975804,
0.));
#233618=CARTESIAN_POINT('Ctrl Pts',(-23.1638813796694,-7.64673306975804,
12.));
#233619=CARTESIAN_POINT('Ctrl Pts',(-23.1870621950452,-7.64502921715482,
0.));
#233620=CARTESIAN_POINT('Ctrl Pts',(-23.1870621950452,-7.64502921715482,
12.));
#233621=CARTESIAN_POINT('Ctrl Pts',(-23.2103286909398,-7.64326080583679,
0.));
#233622=CARTESIAN_POINT('Ctrl Pts',(-23.2103286909398,-7.64326080583679,
12.));
#233623=CARTESIAN_POINT('Ctrl Pts',(-23.2336802320912,-7.64142755851504,
0.));
#233624=CARTESIAN_POINT('Ctrl Pts',(-23.2336802320912,-7.64142755851504,
12.));
#233625=CARTESIAN_POINT('Ctrl Pts',(-23.2571161884488,-7.63952920172835,
0.));
#233626=CARTESIAN_POINT('Ctrl Pts',(-23.2571161884488,-7.63952920172835,
12.));
#233627=CARTESIAN_POINT('Ctrl Pts',(-23.2806359350855,-7.63756546576374,
0.));
#233628=CARTESIAN_POINT('Ctrl Pts',(-23.2806359350855,-7.63756546576374,
12.));
#233629=CARTESIAN_POINT('Ctrl Pts',(-23.3042388521022,-7.63553608458782,
0.));
#233630=CARTESIAN_POINT('Ctrl Pts',(-23.3042388521022,-7.63553608458782,
12.));
#233631=CARTESIAN_POINT('Ctrl Pts',(-23.3279243245241,-7.63344079578161,
0.));
#233632=CARTESIAN_POINT('Ctrl Pts',(-23.3279243245241,-7.63344079578161,
12.));
#233633=CARTESIAN_POINT('Ctrl Pts',(-23.3516917421972,-7.63127934048136,
0.));
#233634=CARTESIAN_POINT('Ctrl Pts',(-23.3516917421972,-7.63127934048136,
12.));
#233635=CARTESIAN_POINT('Ctrl Pts',(-23.3755404996636,-7.62905146332592,
0.));
#233636=CARTESIAN_POINT('Ctrl Pts',(-23.3755404996636,-7.62905146332592,
12.));
#233637=CARTESIAN_POINT('Ctrl Pts',(-23.399469996112,-7.62675691240328,
0.));
#233638=CARTESIAN_POINT('Ctrl Pts',(-23.399469996112,-7.62675691240328,
12.));
#233639=CARTESIAN_POINT('Ctrl Pts',(-23.4234796353542,-7.62439543920049,
0.));
#233640=CARTESIAN_POINT('Ctrl Pts',(-23.4234796353542,-7.62439543920049,
12.));
#233641=CARTESIAN_POINT('Ctrl Pts',(-23.4475688257854,-7.62196679855954,
0.));
#233642=CARTESIAN_POINT('Ctrl Pts',(-23.4475688257854,-7.62196679855954,
12.));
#233643=CARTESIAN_POINT('Ctrl Pts',(-23.4717369803438,-7.61947074863976,
0.));
#233644=CARTESIAN_POINT('Ctrl Pts',(-23.4717369803438,-7.61947074863976,
12.));
#233645=CARTESIAN_POINT('Ctrl Pts',(-23.4959835164609,-7.61690705088318,
0.));
#233646=CARTESIAN_POINT('Ctrl Pts',(-23.4959835164609,-7.61690705088318,
12.));
#233647=CARTESIAN_POINT('Ctrl Pts',(-23.5203078560129,-7.61427546999297,
0.));
#233648=CARTESIAN_POINT('Ctrl Pts',(-23.5203078560129,-7.61427546999297,
12.));
#233649=CARTESIAN_POINT('Ctrl Pts',(-23.544709425203,-7.61157577385371,
0.));
#233650=CARTESIAN_POINT('Ctrl Pts',(-23.544709425203,-7.61157577385371,
12.));
#233651=CARTESIAN_POINT('Ctrl Pts',(-23.5691876544244,-7.60880773344599,
0.));
#233652=CARTESIAN_POINT('Ctrl Pts',(-23.5691876544244,-7.60880773344599,
12.));
#233653=CARTESIAN_POINT('Ctrl Pts',(-23.5937419781245,-7.60597112277093,
0.));
#233654=CARTESIAN_POINT('Ctrl Pts',(-23.5937419781245,-7.60597112277093,
12.));
#233655=CARTESIAN_POINT('Ctrl Pts',(-23.6183718346576,-7.60306571877805,
0.));
#233656=CARTESIAN_POINT('Ctrl Pts',(-23.6183718346576,-7.60306571877805,
12.));
#233657=CARTESIAN_POINT('Ctrl Pts',(-23.6430766661418,-7.60009130130125,
0.));
#233658=CARTESIAN_POINT('Ctrl Pts',(-23.6430766661418,-7.60009130130125,
12.));
#233659=CARTESIAN_POINT('Ctrl Pts',(-23.6678559182875,-7.59704765299566,
0.));
#233660=CARTESIAN_POINT('Ctrl Pts',(-23.6678559182875,-7.59704765299566,
12.));
#233661=CARTESIAN_POINT('Ctrl Pts',(-23.6927090405066,-7.59393455934034,
0.));
#233662=CARTESIAN_POINT('Ctrl Pts',(-23.6927090405066,-7.59393455934034,
12.));
#233663=CARTESIAN_POINT('Ctrl Pts',(-23.7176354860457,-7.5907518086532,
0.));
#233664=CARTESIAN_POINT('Ctrl Pts',(-23.7176354860457,-7.5907518086532,
12.));
#233665=CARTESIAN_POINT('Ctrl Pts',(-23.7426347121006,-7.58749919210825,
0.));
#233666=CARTESIAN_POINT('Ctrl Pts',(-23.7426347121006,-7.58749919210825,
12.));
#233667=CARTESIAN_POINT('Ctrl Pts',(-23.7677061799376,-7.5841765037627,
0.));
#233668=CARTESIAN_POINT('Ctrl Pts',(-23.7677061799376,-7.5841765037627,
12.));
#233669=CARTESIAN_POINT('Ctrl Pts',(-23.7928493549908,-7.58078354058212,
0.));
#233670=CARTESIAN_POINT('Ctrl Pts',(-23.7928493549908,-7.58078354058212,
12.));
#233671=CARTESIAN_POINT('Ctrl Pts',(-23.8180637069976,-7.57732010249065,
0.));
#233672=CARTESIAN_POINT('Ctrl Pts',(-23.8180637069976,-7.57732010249065,
12.));
#233673=CARTESIAN_POINT('Ctrl Pts',(-23.8433487096132,-7.57378599219814,
0.));
#233674=CARTESIAN_POINT('Ctrl Pts',(-23.8433487096132,-7.57378599219814,
12.));
#233675=CARTESIAN_POINT('Ctrl Pts',(-23.8687038399595,-7.57018101500709,
0.));
#233676=CARTESIAN_POINT('Ctrl Pts',(-23.8687038399595,-7.57018101500709,
12.));
#233677=CARTESIAN_POINT('Ctrl Pts',(-23.8941285782002,-7.5665049786379,
0.));
#233678=CARTESIAN_POINT('Ctrl Pts',(-23.8941285782002,-7.5665049786379,
12.));
#233679=CARTESIAN_POINT('Ctrl Pts',(-23.9196224070759,-7.56275769304772,
0.));
#233680=CARTESIAN_POINT('Ctrl Pts',(-23.9196224070759,-7.56275769304772,
12.));
#233681=CARTESIAN_POINT('Ctrl Pts',(-23.9451848115002,-7.55893897027679,
0.));
#233682=CARTESIAN_POINT('Ctrl Pts',(-23.9451848115002,-7.55893897027679,
12.));
#233683=CARTESIAN_POINT('Ctrl Pts',(-23.9708152779886,-7.55504862424807,
0.));
#233684=CARTESIAN_POINT('Ctrl Pts',(-23.9708152779886,-7.55504862424807,
12.));
#233685=CARTESIAN_POINT('Ctrl Pts',(-23.9965132953187,-7.55108647097431,
0.));
#233686=CARTESIAN_POINT('Ctrl Pts',(-23.9965132953187,-7.55108647097431,
12.));
#233687=CARTESIAN_POINT('Ctrl Pts',(-24.0222783554531,-7.54705232885894,
0.));
#233688=CARTESIAN_POINT('Ctrl Pts',(-24.0222783554531,-7.54705232885894,
12.));
#233689=CARTESIAN_POINT('Ctrl Pts',(-24.0481099543353,-7.54294601896127,
0.));
#233690=CARTESIAN_POINT('Ctrl Pts',(-24.0481099543353,-7.54294601896127,
12.));
#233691=CARTESIAN_POINT('Ctrl Pts',(-24.0740075927984,-7.53876736531004,
0.));
#233692=CARTESIAN_POINT('Ctrl Pts',(-24.0740075927984,-7.53876736531004,
12.));
#233693=CARTESIAN_POINT('Ctrl Pts',(-24.0999707772643,-7.53451619514658,
0.));
#233694=CARTESIAN_POINT('Ctrl Pts',(-24.0999707772643,-7.53451619514658,
12.));
#233695=CARTESIAN_POINT('Ctrl Pts',(-24.1259990209211,-7.53019233935536,
0.));
#233696=CARTESIAN_POINT('Ctrl Pts',(-24.1259990209211,-7.53019233935536,
12.));
#233697=CARTESIAN_POINT('Ctrl Pts',(-24.152091842537,-7.52579563201478,
0.));
#233698=CARTESIAN_POINT('Ctrl Pts',(-24.152091842537,-7.52579563201478,
12.));
#233699=CARTESIAN_POINT('Ctrl Pts',(-24.1782487641602,-7.52132590953862,
0.));
#233700=CARTESIAN_POINT('Ctrl Pts',(-24.1782487641602,-7.52132590953862,
12.));
#233701=CARTESIAN_POINT('Ctrl Pts',(-24.2044693092356,-7.51678300997997,
0.));
#233702=CARTESIAN_POINT('Ctrl Pts',(-24.2044693092356,-7.51678300997997,
12.));
#233703=CARTESIAN_POINT('Ctrl Pts',(-24.230753000389,-7.51216677222198,
0.));
#233704=CARTESIAN_POINT('Ctrl Pts',(-24.230753000389,-7.51216677222198,
12.));
#233705=CARTESIAN_POINT('Ctrl Pts',(-24.2570993577032,-7.50747703535114,
0.));
#233706=CARTESIAN_POINT('Ctrl Pts',(-24.2570993577032,-7.50747703535114,
12.));
#233707=CARTESIAN_POINT('Ctrl Pts',(-24.2835078958966,-7.50271363765098,
0.));
#233708=CARTESIAN_POINT('Ctrl Pts',(-24.2835078958966,-7.50271363765098,
12.));
#233709=CARTESIAN_POINT('Ctrl Pts',(-24.3099781253345,-7.49787641695358,
0.));
#233710=CARTESIAN_POINT('Ctrl Pts',(-24.3099781253345,-7.49787641695358,
12.));
#233711=CARTESIAN_POINT('Ctrl Pts',(-24.3365095573673,-7.49296521252329,
0.));
#233712=CARTESIAN_POINT('Ctrl Pts',(-24.3365095573673,-7.49296521252329,
12.));
#233713=CARTESIAN_POINT('Ctrl Pts',(-24.3631017084513,-7.48797986651827,
0.));
#233714=CARTESIAN_POINT('Ctrl Pts',(-24.3631017084513,-7.48797986651827,
12.));
#233715=CARTESIAN_POINT('Ctrl Pts',(-24.3897541049248,-7.48292022569253,
0.));
#233716=CARTESIAN_POINT('Ctrl Pts',(-24.3897541049248,-7.48292022569253,
12.));
#233717=CARTESIAN_POINT('Ctrl Pts',(-24.4164662871165,-7.47778614286573,
0.));
#233718=CARTESIAN_POINT('Ctrl Pts',(-24.4164662871165,-7.47778614286573,
12.));
#233719=CARTESIAN_POINT('Ctrl Pts',(-24.4432378146501,-7.47257747883318,
0.));
#233720=CARTESIAN_POINT('Ctrl Pts',(-24.4432378146501,-7.47257747883318,
12.));
#233721=CARTESIAN_POINT('Ctrl Pts',(-24.4700682684544,-7.46729410308922,
0.));
#233722=CARTESIAN_POINT('Ctrl Pts',(-24.4700682684544,-7.46729410308922,
12.));
#233723=CARTESIAN_POINT('Ctrl Pts',(-24.4969572391509,-7.46193588961641,
0.));
#233724=CARTESIAN_POINT('Ctrl Pts',(-24.4969572391509,-7.46193588961641,
12.));
#233725=CARTESIAN_POINT('Ctrl Pts',(-24.52390431731,-7.45650271336045,0.));
#233726=CARTESIAN_POINT('Ctrl Pts',(-24.52390431731,-7.45650271336045,12.));
#233727=CARTESIAN_POINT('Ctrl Pts',(-24.5509090831579,-7.45099444651295,
0.));
#233728=CARTESIAN_POINT('Ctrl Pts',(-24.5509090831579,-7.45099444651295,
12.));
#233729=CARTESIAN_POINT('Ctrl Pts',(-24.5779710960865,-7.44541095473162,
0.));
#233730=CARTESIAN_POINT('Ctrl Pts',(-24.5779710960865,-7.44541095473162,
12.));
#233731=CARTESIAN_POINT('Ctrl Pts',(-24.6050898852349,-7.43975209375374,
0.));
#233732=CARTESIAN_POINT('Ctrl Pts',(-24.6050898852349,-7.43975209375374,
12.));
#233733=CARTESIAN_POINT('Ctrl Pts',(-24.6322649369472,-7.4340177048922,
0.));
#233734=CARTESIAN_POINT('Ctrl Pts',(-24.6322649369472,-7.4340177048922,
12.));
#233735=CARTESIAN_POINT('Ctrl Pts',(-24.659495712869,-7.4282076215868,0.));
#233736=CARTESIAN_POINT('Ctrl Pts',(-24.659495712869,-7.4282076215868,12.));
#233737=CARTESIAN_POINT('Ctrl Pts',(-24.6867816727118,-7.42232167765762,
0.));
#233738=CARTESIAN_POINT('Ctrl Pts',(-24.6867816727118,-7.42232167765762,
12.));
#233739=CARTESIAN_POINT('Ctrl Pts',(-24.7141222949988,-7.41635971481243,
0.));
#233740=CARTESIAN_POINT('Ctrl Pts',(-24.7141222949988,-7.41635971481243,
12.));
#233741=CARTESIAN_POINT('Ctrl Pts',(-24.7415170994754,-7.41032159082173,
0.));
#233742=CARTESIAN_POINT('Ctrl Pts',(-24.7415170994754,-7.41032159082173,
12.));
#233743=CARTESIAN_POINT('Ctrl Pts',(-24.7689656669005,-7.40420718661754,
0.));
#233744=CARTESIAN_POINT('Ctrl Pts',(-24.7689656669005,-7.40420718661754,
12.));
#233745=CARTESIAN_POINT('Ctrl Pts',(-24.7964676646518,-7.39801641583612,
0.));
#233746=CARTESIAN_POINT('Ctrl Pts',(-24.7964676646518,-7.39801641583612,
12.));
#233747=CARTESIAN_POINT('Ctrl Pts',(-24.8240228521042,-7.39174922586841,
0.));
#233748=CARTESIAN_POINT('Ctrl Pts',(-24.8240228521042,-7.39174922586841,
12.));
#233749=CARTESIAN_POINT('Ctrl Pts',(-24.8516310625367,-7.38540558904945,
0.));
#233750=CARTESIAN_POINT('Ctrl Pts',(-24.8516310625367,-7.38540558904945,
12.));
#233751=CARTESIAN_POINT('Ctrl Pts',(-24.8792921911309,-7.3789854964161,
0.));
#233752=CARTESIAN_POINT('Ctrl Pts',(-24.8792921911309,-7.3789854964161,
12.));
#233753=CARTESIAN_POINT('Ctrl Pts',(-24.9014633826201,-7.37378825962717,
0.));
#233754=CARTESIAN_POINT('Ctrl Pts',(-24.9014633826201,-7.37378825962717,
12.));
#233755=CARTESIAN_POINT('Ctrl Pts',(-24.9181155530631,-7.36985593120696,
0.));
#233756=CARTESIAN_POINT('Ctrl Pts',(-24.9181155530631,-7.36985593120696,
12.));
#233757=CARTESIAN_POINT('Ctrl Pts',(-24.9292275670705,-7.36721909029059,
0.));
#233758=CARTESIAN_POINT('Ctrl Pts',(-24.9292275670705,-7.36721909029059,
12.));
#233759=CARTESIAN_POINT('Ctrl Pts',(-24.9347862158358,-7.36589684767343,
0.));
#233760=CARTESIAN_POINT('Ctrl Pts',(-24.9347862158358,-7.36589684767343,
12.));
#233761=CARTESIAN_POINT('',(-24.9347862158358,-7.36589684767343,0.));
#233762=CARTESIAN_POINT('Ctrl Pts',(-21.2610617890679,-7.52250298901264,
0.));
#233763=CARTESIAN_POINT('Ctrl Pts',(-21.2610673466886,-7.5225064970397,
0.));
#233764=CARTESIAN_POINT('Ctrl Pts',(-21.2611204474866,-7.52252744144903,
0.));
#233765=CARTESIAN_POINT('Ctrl Pts',(-21.261326054066,-7.5226006423166,0.));
#233766=CARTESIAN_POINT('Ctrl Pts',(-21.2618521283555,-7.52278182242669,
0.));
#233767=CARTESIAN_POINT('Ctrl Pts',(-21.262927782038,-7.52314642316199,
0.));
#233768=CARTESIAN_POINT('Ctrl Pts',(-21.2644161259962,-7.52364573027552,
0.));
#233769=CARTESIAN_POINT('Ctrl Pts',(-21.2663059157058,-7.52427261074297,
0.));
#233770=CARTESIAN_POINT('Ctrl Pts',(-21.2685823838671,-7.5250177033353,
0.));
#233771=CARTESIAN_POINT('Ctrl Pts',(-21.2712301573466,-7.52587126095529,
0.));
#233772=CARTESIAN_POINT('Ctrl Pts',(-21.2742366113579,-7.5268252691854,
0.));
#233773=CARTESIAN_POINT('Ctrl Pts',(-21.2775925269652,-7.52787386225332,
0.));
#233774=CARTESIAN_POINT('Ctrl Pts',(-21.2812902781143,-7.52901217930407,
0.));
#233775=CARTESIAN_POINT('Ctrl Pts',(-21.2853226580657,-7.53023562438229,
0.));
#233776=CARTESIAN_POINT('Ctrl Pts',(-21.2896816163842,-7.53153906987855,
0.));
#233777=CARTESIAN_POINT('Ctrl Pts',(-21.2943588989331,-7.53291726078526,
0.));
#233778=CARTESIAN_POINT('Ctrl Pts',(-21.2993464250717,-7.53436505309942,
0.));
#233779=CARTESIAN_POINT('Ctrl Pts',(-21.3046368712157,-7.53587778251735,
0.));
#233780=CARTESIAN_POINT('Ctrl Pts',(-21.310223716773,-7.53745129364616,
0.));
#233781=CARTESIAN_POINT('Ctrl Pts',(-21.3161009456256,-7.53908175169898,
0.));
#233782=CARTESIAN_POINT('Ctrl Pts',(-21.3222628524165,-7.54076552038278,
0.));
#233783=CARTESIAN_POINT('Ctrl Pts',(-21.328703791771,-7.5424990037703,0.));
#233784=CARTESIAN_POINT('Ctrl Pts',(-21.3354182340149,-7.54427868151267,
0.));
#233785=CARTESIAN_POINT('Ctrl Pts',(-21.3424008295038,-7.54610114948346,
0.));
#233786=CARTESIAN_POINT('Ctrl Pts',(-21.3496464761531,-7.5479631624633,
0.));
#233787=CARTESIAN_POINT('Ctrl Pts',(-21.3571503685855,-7.54986166521309,
0.));
#233788=CARTESIAN_POINT('Ctrl Pts',(-21.3649079431865,-7.55179375777443,
0.));
#233789=CARTESIAN_POINT('Ctrl Pts',(-21.3729148390243,-7.55375667080028,
0.));
#233790=CARTESIAN_POINT('Ctrl Pts',(-21.3811668478932,-7.55574773403502,
0.));
#233791=CARTESIAN_POINT('Ctrl Pts',(-21.3896598842117,-7.55776435731416,
0.));
#233792=CARTESIAN_POINT('Ctrl Pts',(-21.3983899952987,-7.5598040370061,
0.));
#233793=CARTESIAN_POINT('Ctrl Pts',(-21.4073533630365,-7.56186435703621,
0.));
#233794=CARTESIAN_POINT('Ctrl Pts',(-21.4165463106254,-7.56394299313684,
0.));
#233795=CARTESIAN_POINT('Ctrl Pts',(-21.4259653015736,-7.56603771218712,
0.));
#233796=CARTESIAN_POINT('Ctrl Pts',(-21.4356069261513,-7.56814636360847,
0.));
#233797=CARTESIAN_POINT('Ctrl Pts',(-21.4454678907509,-7.57026687261165,
0.));
#233798=CARTESIAN_POINT('Ctrl Pts',(-21.4555450053142,-7.57239723223505,
0.));
#233799=CARTESIAN_POINT('Ctrl Pts',(-21.4658351740128,-7.57453549743411,
0.));
#233800=CARTESIAN_POINT('Ctrl Pts',(-21.4763353936762,-7.57667978402987,
0.));
#233801=CARTESIAN_POINT('Ctrl Pts',(-21.4870427508194,-7.57882826679131,
0.));
#233802=CARTESIAN_POINT('Ctrl Pts',(-21.4979544192744,-7.58097917790744,
0.));
#233803=CARTESIAN_POINT('Ctrl Pts',(-21.5090676573873,-7.58313080519179,
0.));
#233804=CARTESIAN_POINT('Ctrl Pts',(-21.5203798035299,-7.58528148919129,
0.));
#233805=CARTESIAN_POINT('Ctrl Pts',(-21.5318882716736,-7.58742962034833,
0.));
#233806=CARTESIAN_POINT('Ctrl Pts',(-21.543590547011,-7.58957363620013,
0.));
#233807=CARTESIAN_POINT('Ctrl Pts',(-21.5554841813462,-7.59171201844776,
0.));
#233808=CARTESIAN_POINT('Ctrl Pts',(-21.5675667904726,-7.59384329124918,
0.));
#233809=CARTESIAN_POINT('Ctrl Pts',(-21.5798360518978,-7.59596601973583,
0.));
#233810=CARTESIAN_POINT('Ctrl Pts',(-21.5922897024466,-7.59807880846194,
0.));
#233811=CARTESIAN_POINT('Ctrl Pts',(-21.6049255358843,-7.6001802998824,
0.));
#233812=CARTESIAN_POINT('Ctrl Pts',(-21.617741400599,-7.60226917285428,
0.));
#233813=CARTESIAN_POINT('Ctrl Pts',(-21.6307351973822,-7.60434414118295,
0.));
#233814=CARTESIAN_POINT('Ctrl Pts',(-21.6439048771743,-7.60640395216356,
0.));
#233815=CARTESIAN_POINT('Ctrl Pts',(-21.6572484388081,-7.60844738512873,
0.));
#233816=CARTESIAN_POINT('Ctrl Pts',(-21.6707639267576,-7.61047325000955,
0.));
#233817=CARTESIAN_POINT('Ctrl Pts',(-21.6844494295815,-7.61248038630268,
0.));
#233818=CARTESIAN_POINT('Ctrl Pts',(-21.6983030783322,-7.61446766202786,
0.));
#233819=CARTESIAN_POINT('Ctrl Pts',(-21.7123230449834,-7.6164339727042,
0.));
#233820=CARTESIAN_POINT('Ctrl Pts',(-21.7265075407975,-7.61837824030537,
0.));
#233821=CARTESIAN_POINT('Ctrl Pts',(-21.7408548148656,-7.62029941230854,
0.));
#233822=CARTESIAN_POINT('Ctrl Pts',(-21.7553631528328,-7.62219646084228,
0.));
#233823=CARTESIAN_POINT('Ctrl Pts',(-21.7700308755584,-7.62406838181166,
0.));
#233824=CARTESIAN_POINT('Ctrl Pts',(-21.7848563378021,-7.62591419404512,
0.));
#233825=CARTESIAN_POINT('Ctrl Pts',(-21.799837926858,-7.62773293842389,
0.));
#233826=CARTESIAN_POINT('Ctrl Pts',(-21.814974061509,-7.62952367718126,
0.));
#233827=CARTESIAN_POINT('Ctrl Pts',(-21.8302631910195,-7.63128549323022,
0.));
#233828=CARTESIAN_POINT('Ctrl Pts',(-21.8457037941084,-7.63301748948935,
0.));
#233829=CARTESIAN_POINT('Ctrl Pts',(-21.8612943779089,-7.63471878821225,
0.));
#233830=CARTESIAN_POINT('Ctrl Pts',(-21.8770334769496,-7.63638853033399,
0.));
#233831=CARTESIAN_POINT('Ctrl Pts',(-21.8929196523514,-7.63802587492034,
0.));
#233832=CARTESIAN_POINT('Ctrl Pts',(-21.9089514909874,-7.63962999860927,
0.));
#233833=CARTESIAN_POINT('Ctrl Pts',(-21.9251276046546,-7.64120009506531,
0.));
#233834=CARTESIAN_POINT('Ctrl Pts',(-21.9414466292072,-7.64273537442682,
0.));
#233835=CARTESIAN_POINT('Ctrl Pts',(-21.9579072237651,-7.64423506279122,
0.));
#233836=CARTESIAN_POINT('Ctrl Pts',(-21.9745080700798,-7.64569840177335,
0.));
#233837=CARTESIAN_POINT('Ctrl Pts',(-21.9912478718542,-7.64712464805249,
0.));
#233838=CARTESIAN_POINT('Ctrl Pts',(-22.0081253540774,-7.64851307293351,
0.));
#233839=CARTESIAN_POINT('Ctrl Pts',(-22.0251392623209,-7.64986296190168,
0.));
#233840=CARTESIAN_POINT('Ctrl Pts',(-22.0422883621174,-7.65117361421358,
0.));
#233841=CARTESIAN_POINT('Ctrl Pts',(-22.0595714384431,-7.65244434253112,
0.));
#233842=CARTESIAN_POINT('Ctrl Pts',(-22.0769872951596,-7.65367447254949,
0.));
#233843=CARTESIAN_POINT('Ctrl Pts',(-22.094534754469,-7.65486334263643,
0.));
#233844=CARTESIAN_POINT('Ctrl Pts',(-22.1122126563329,-7.65601030346806,
0.));
#233845=CARTESIAN_POINT('Ctrl Pts',(-22.1300198579675,-7.65711471769396,
0.));
#233846=CARTESIAN_POINT('Ctrl Pts',(-22.1479552334211,-7.65817595963349,
0.));
#233847=CARTESIAN_POINT('Ctrl Pts',(-22.1660176731178,-7.6591934149693,
0.));
#233848=CARTESIAN_POINT('Ctrl Pts',(-22.1842060834091,-7.66016648045004,
0.));
#233849=CARTESIAN_POINT('Ctrl Pts',(-22.2025193860964,-7.6610945635927,
0.));
#233850=CARTESIAN_POINT('Ctrl Pts',(-22.2209565180085,-7.66197708240399,
0.));
#233851=CARTESIAN_POINT('Ctrl Pts',(-22.2395164306547,-7.66281346512508,
0.));
#233852=CARTESIAN_POINT('Ctrl Pts',(-22.258198089848,-7.6636031499764,0.));
#233853=CARTESIAN_POINT('Ctrl Pts',(-22.2770004753335,-7.66434558490978,
0.));
#233854=CARTESIAN_POINT('Ctrl Pts',(-22.2959225803937,-7.66504022736298,
0.));
#233855=CARTESIAN_POINT('Ctrl Pts',(-22.314963411484,-7.66568654402493,
0.));
#233856=CARTESIAN_POINT('Ctrl Pts',(-22.3341219879469,-7.66628401061952,
0.));
#233857=CARTESIAN_POINT('Ctrl Pts',(-22.3533973417021,-7.66683211169158,
0.));
#233858=CARTESIAN_POINT('Ctrl Pts',(-22.372788516936,-7.66733034039882,
0.));
#233859=CARTESIAN_POINT('Ctrl Pts',(-22.3922945697773,-7.66777819830789,
0.));
#233860=CARTESIAN_POINT('Ctrl Pts',(-22.4119145679758,-7.66817519519639,
0.));
#233861=CARTESIAN_POINT('Ctrl Pts',(-22.4316475906603,-7.66852084886704,
0.));
#233862=CARTESIAN_POINT('Ctrl Pts',(-22.4514927280855,-7.66881468496634,
0.));
#233863=CARTESIAN_POINT('Ctrl Pts',(-22.47144908137,-7.6690562368083,0.));
#233864=CARTESIAN_POINT('Ctrl Pts',(-22.4915157622312,-7.66924504520314,
0.));
#233865=CARTESIAN_POINT('Ctrl Pts',(-22.5116918927032,-7.66938065829107,
0.));
#233866=CARTESIAN_POINT('Ctrl Pts',(-22.53197660492,-7.66946263138143,0.));
#233867=CARTESIAN_POINT('Ctrl Pts',(-22.5523690409116,-7.66949052679692,
0.));
#233868=CARTESIAN_POINT('Ctrl Pts',(-22.5728683523831,-7.66946391372305,
0.));
#233869=CARTESIAN_POINT('Ctrl Pts',(-22.5934737004953,-7.66938236806232,
0.));
#233870=CARTESIAN_POINT('Ctrl Pts',(-22.6141842556243,-7.66924547229413,
0.));
#233871=CARTESIAN_POINT('Ctrl Pts',(-22.6349991971541,-7.66905281533714,
0.));
#233872=CARTESIAN_POINT('Ctrl Pts',(-22.6559177133127,-7.66880399241322,
0.));
#233873=CARTESIAN_POINT('Ctrl Pts',(-22.6769390009885,-7.66849860491742,
0.));
#233874=CARTESIAN_POINT('Ctrl Pts',(-22.6980622655446,-7.66813626029274,
0.));
#233875=CARTESIAN_POINT('Ctrl Pts',(-22.7192867206245,-7.66771657191027,
0.));
#233876=CARTESIAN_POINT('Ctrl Pts',(-22.7406115879513,-7.66723915895439,
0.));
#233877=CARTESIAN_POINT('Ctrl Pts',(-22.7620360971843,-7.66670364630298,
0.));
#233878=CARTESIAN_POINT('Ctrl Pts',(-22.7835594857699,-7.66610966441272,
0.));
#233879=CARTESIAN_POINT('Ctrl Pts',(-22.8051809987833,-7.66545684920987,
0.));
#233880=CARTESIAN_POINT('Ctrl Pts',(-22.8268998887678,-7.66474484198548,
0.));
#233881=CARTESIAN_POINT('Ctrl Pts',(-22.848715415557,-7.66397328929802,
0.));
#233882=CARTESIAN_POINT('Ctrl Pts',(-22.8706268461283,-7.66314184287336,
0.));
#233883=CARTESIAN_POINT('Ctrl Pts',(-22.8926334544883,-7.66225015950155,
0.));
#233884=CARTESIAN_POINT('Ctrl Pts',(-22.9147345215421,-7.66129790094107,
0.));
#233885=CARTESIAN_POINT('Ctrl Pts',(-22.9369293349593,-7.66028473382777,
0.));
#233886=CARTESIAN_POINT('Ctrl Pts',(-22.959217189033,-7.65921032958901,
0.));
#233887=CARTESIAN_POINT('Ctrl Pts',(-22.9815973845296,-7.65807436436431,
0.));
#233888=CARTESIAN_POINT('Ctrl Pts',(-23.0040692285814,-7.65687651891304,
0.));
#233889=CARTESIAN_POINT('Ctrl Pts',(-23.0266320345787,-7.65561647852533,
0.));
#233890=CARTESIAN_POINT('Ctrl Pts',(-23.0492851220528,-7.65429393293945,
0.));
#233891=CARTESIAN_POINT('Ctrl Pts',(-23.072027816555,-7.65290857626357,
0.));
#233892=CARTESIAN_POINT('Ctrl Pts',(-23.094859449525,-7.65146010690475,
0.));
#233893=CARTESIAN_POINT('Ctrl Pts',(-23.1177793581679,-7.64994822749859,
0.));
#233894=CARTESIAN_POINT('Ctrl Pts',(-23.1407868853819,-7.64837264482942,
0.));
#233895=CARTESIAN_POINT('Ctrl Pts',(-23.1638813796694,-7.64673306975804,
0.));
#233896=CARTESIAN_POINT('Ctrl Pts',(-23.1870621950452,-7.64502921715482,
0.));
#233897=CARTESIAN_POINT('Ctrl Pts',(-23.2103286909398,-7.64326080583679,
0.));
#233898=CARTESIAN_POINT('Ctrl Pts',(-23.2336802320912,-7.64142755851504,
0.));
#233899=CARTESIAN_POINT('Ctrl Pts',(-23.2571161884488,-7.63952920172835,
0.));
#233900=CARTESIAN_POINT('Ctrl Pts',(-23.2806359350855,-7.63756546576374,
0.));
#233901=CARTESIAN_POINT('Ctrl Pts',(-23.3042388521022,-7.63553608458782,
0.));
#233902=CARTESIAN_POINT('Ctrl Pts',(-23.3279243245241,-7.63344079578161,
0.));
#233903=CARTESIAN_POINT('Ctrl Pts',(-23.3516917421972,-7.63127934048136,
0.));
#233904=CARTESIAN_POINT('Ctrl Pts',(-23.3755404996636,-7.62905146332592,
0.));
#233905=CARTESIAN_POINT('Ctrl Pts',(-23.399469996112,-7.62675691240328,
0.));
#233906=CARTESIAN_POINT('Ctrl Pts',(-23.4234796353542,-7.62439543920049,
0.));
#233907=CARTESIAN_POINT('Ctrl Pts',(-23.4475688257854,-7.62196679855954,
0.));
#233908=CARTESIAN_POINT('Ctrl Pts',(-23.4717369803438,-7.61947074863976,
0.));
#233909=CARTESIAN_POINT('Ctrl Pts',(-23.4959835164609,-7.61690705088318,
0.));
#233910=CARTESIAN_POINT('Ctrl Pts',(-23.5203078560129,-7.61427546999297,
0.));
#233911=CARTESIAN_POINT('Ctrl Pts',(-23.544709425203,-7.61157577385371,
0.));
#233912=CARTESIAN_POINT('Ctrl Pts',(-23.5691876544244,-7.60880773344599,
0.));
#233913=CARTESIAN_POINT('Ctrl Pts',(-23.5937419781245,-7.60597112277093,
0.));
#233914=CARTESIAN_POINT('Ctrl Pts',(-23.6183718346576,-7.60306571877805,
0.));
#233915=CARTESIAN_POINT('Ctrl Pts',(-23.6430766661418,-7.60009130130125,
0.));
#233916=CARTESIAN_POINT('Ctrl Pts',(-23.6678559182875,-7.59704765299566,
0.));
#233917=CARTESIAN_POINT('Ctrl Pts',(-23.6927090405066,-7.59393455934034,
0.));
#233918=CARTESIAN_POINT('Ctrl Pts',(-23.7176354860457,-7.5907518086532,
0.));
#233919=CARTESIAN_POINT('Ctrl Pts',(-23.7426347121006,-7.58749919210825,
0.));
#233920=CARTESIAN_POINT('Ctrl Pts',(-23.7677061799376,-7.5841765037627,
0.));
#233921=CARTESIAN_POINT('Ctrl Pts',(-23.7928493549908,-7.58078354058212,
0.));
#233922=CARTESIAN_POINT('Ctrl Pts',(-23.8180637069976,-7.57732010249065,
0.));
#233923=CARTESIAN_POINT('Ctrl Pts',(-23.8433487096132,-7.57378599219814,
0.));
#233924=CARTESIAN_POINT('Ctrl Pts',(-23.8687038399595,-7.57018101500709,
0.));
#233925=CARTESIAN_POINT('Ctrl Pts',(-23.8941285782002,-7.5665049786379,
0.));
#233926=CARTESIAN_POINT('Ctrl Pts',(-23.9196224070759,-7.56275769304772,
0.));
#233927=CARTESIAN_POINT('Ctrl Pts',(-23.9451848115002,-7.55893897027679,
0.));
#233928=CARTESIAN_POINT('Ctrl Pts',(-23.9708152779886,-7.55504862424807,
0.));
#233929=CARTESIAN_POINT('Ctrl Pts',(-23.9965132953187,-7.55108647097431,
0.));
#233930=CARTESIAN_POINT('Ctrl Pts',(-24.0222783554531,-7.54705232885894,
0.));
#233931=CARTESIAN_POINT('Ctrl Pts',(-24.0481099543353,-7.54294601896127,
0.));
#233932=CARTESIAN_POINT('Ctrl Pts',(-24.0740075927984,-7.53876736531004,
0.));
#233933=CARTESIAN_POINT('Ctrl Pts',(-24.0999707772643,-7.53451619514658,
0.));
#233934=CARTESIAN_POINT('Ctrl Pts',(-24.1259990209211,-7.53019233935536,
0.));
#233935=CARTESIAN_POINT('Ctrl Pts',(-24.152091842537,-7.52579563201478,
0.));
#233936=CARTESIAN_POINT('Ctrl Pts',(-24.1782487641602,-7.52132590953862,
0.));
#233937=CARTESIAN_POINT('Ctrl Pts',(-24.2044693092356,-7.51678300997997,
0.));
#233938=CARTESIAN_POINT('Ctrl Pts',(-24.230753000389,-7.51216677222198,
0.));
#233939=CARTESIAN_POINT('Ctrl Pts',(-24.2570993577032,-7.50747703535114,
0.));
#233940=CARTESIAN_POINT('Ctrl Pts',(-24.2835078958966,-7.50271363765098,
0.));
#233941=CARTESIAN_POINT('Ctrl Pts',(-24.3099781253345,-7.49787641695358,
0.));
#233942=CARTESIAN_POINT('Ctrl Pts',(-24.3365095573673,-7.49296521252329,
0.));
#233943=CARTESIAN_POINT('Ctrl Pts',(-24.3631017084513,-7.48797986651827,
0.));
#233944=CARTESIAN_POINT('Ctrl Pts',(-24.3897541049248,-7.48292022569253,
0.));
#233945=CARTESIAN_POINT('Ctrl Pts',(-24.4164662871165,-7.47778614286573,
0.));
#233946=CARTESIAN_POINT('Ctrl Pts',(-24.4432378146501,-7.47257747883318,
0.));
#233947=CARTESIAN_POINT('Ctrl Pts',(-24.4700682684544,-7.46729410308922,
0.));
#233948=CARTESIAN_POINT('Ctrl Pts',(-24.4969572391509,-7.46193588961641,
0.));
#233949=CARTESIAN_POINT('Ctrl Pts',(-24.52390431731,-7.45650271336045,0.));
#233950=CARTESIAN_POINT('Ctrl Pts',(-24.5509090831579,-7.45099444651295,
0.));
#233951=CARTESIAN_POINT('Ctrl Pts',(-24.5779710960865,-7.44541095473162,
0.));
#233952=CARTESIAN_POINT('Ctrl Pts',(-24.6050898852349,-7.43975209375374,
0.));
#233953=CARTESIAN_POINT('Ctrl Pts',(-24.6322649369472,-7.4340177048922,
0.));
#233954=CARTESIAN_POINT('Ctrl Pts',(-24.659495712869,-7.4282076215868,0.));
#233955=CARTESIAN_POINT('Ctrl Pts',(-24.6867816727118,-7.42232167765762,
0.));
#233956=CARTESIAN_POINT('Ctrl Pts',(-24.7141222949988,-7.41635971481243,
0.));
#233957=CARTESIAN_POINT('Ctrl Pts',(-24.7415170994754,-7.41032159082173,
0.));
#233958=CARTESIAN_POINT('Ctrl Pts',(-24.7689656669005,-7.40420718661754,
0.));
#233959=CARTESIAN_POINT('Ctrl Pts',(-24.7964676646518,-7.39801641583612,
0.));
#233960=CARTESIAN_POINT('Ctrl Pts',(-24.8240228521042,-7.39174922586841,
0.));
#233961=CARTESIAN_POINT('Ctrl Pts',(-24.8516310625367,-7.38540558904945,
0.));
#233962=CARTESIAN_POINT('Ctrl Pts',(-24.8792921911309,-7.3789854964161,
0.));
#233963=CARTESIAN_POINT('Ctrl Pts',(-24.9014633826201,-7.37378825962717,
0.));
#233964=CARTESIAN_POINT('Ctrl Pts',(-24.9181155530631,-7.36985593120696,
0.));
#233965=CARTESIAN_POINT('Ctrl Pts',(-24.9292275670705,-7.36721909029059,
0.));
#233966=CARTESIAN_POINT('Ctrl Pts',(-24.9347862158358,-7.36589684767343,
0.));
#233967=CARTESIAN_POINT('',(-24.9347862158358,-7.36589684767343,12.));
#233968=CARTESIAN_POINT('Ctrl Pts',(-24.9347862158358,-7.36589684767343,
12.));
#233969=CARTESIAN_POINT('Ctrl Pts',(-24.9292275670705,-7.36721909029059,
12.));
#233970=CARTESIAN_POINT('Ctrl Pts',(-24.9181155530631,-7.36985593120696,
12.));
#233971=CARTESIAN_POINT('Ctrl Pts',(-24.9014633826201,-7.37378825962717,
12.));
#233972=CARTESIAN_POINT('Ctrl Pts',(-24.8792921911309,-7.3789854964161,
12.));
#233973=CARTESIAN_POINT('Ctrl Pts',(-24.8516310625367,-7.38540558904945,
12.));
#233974=CARTESIAN_POINT('Ctrl Pts',(-24.8240228521042,-7.39174922586841,
12.));
#233975=CARTESIAN_POINT('Ctrl Pts',(-24.7964676646518,-7.39801641583612,
12.));
#233976=CARTESIAN_POINT('Ctrl Pts',(-24.7689656669005,-7.40420718661754,
12.));
#233977=CARTESIAN_POINT('Ctrl Pts',(-24.7415170994754,-7.41032159082173,
12.));
#233978=CARTESIAN_POINT('Ctrl Pts',(-24.7141222949988,-7.41635971481243,
12.));
#233979=CARTESIAN_POINT('Ctrl Pts',(-24.6867816727118,-7.42232167765762,
12.));
#233980=CARTESIAN_POINT('Ctrl Pts',(-24.659495712869,-7.4282076215868,12.));
#233981=CARTESIAN_POINT('Ctrl Pts',(-24.6322649369472,-7.4340177048922,
12.));
#233982=CARTESIAN_POINT('Ctrl Pts',(-24.6050898852349,-7.43975209375374,
12.));
#233983=CARTESIAN_POINT('Ctrl Pts',(-24.5779710960865,-7.44541095473162,
12.));
#233984=CARTESIAN_POINT('Ctrl Pts',(-24.5509090831579,-7.45099444651295,
12.));
#233985=CARTESIAN_POINT('Ctrl Pts',(-24.52390431731,-7.45650271336045,12.));
#233986=CARTESIAN_POINT('Ctrl Pts',(-24.4969572391509,-7.46193588961641,
12.));
#233987=CARTESIAN_POINT('Ctrl Pts',(-24.4700682684544,-7.46729410308922,
12.));
#233988=CARTESIAN_POINT('Ctrl Pts',(-24.4432378146501,-7.47257747883318,
12.));
#233989=CARTESIAN_POINT('Ctrl Pts',(-24.4164662871165,-7.47778614286573,
12.));
#233990=CARTESIAN_POINT('Ctrl Pts',(-24.3897541049248,-7.48292022569253,
12.));
#233991=CARTESIAN_POINT('Ctrl Pts',(-24.3631017084513,-7.48797986651827,
12.));
#233992=CARTESIAN_POINT('Ctrl Pts',(-24.3365095573673,-7.49296521252329,
12.));
#233993=CARTESIAN_POINT('Ctrl Pts',(-24.3099781253345,-7.49787641695358,
12.));
#233994=CARTESIAN_POINT('Ctrl Pts',(-24.2835078958966,-7.50271363765098,
12.));
#233995=CARTESIAN_POINT('Ctrl Pts',(-24.2570993577032,-7.50747703535114,
12.));
#233996=CARTESIAN_POINT('Ctrl Pts',(-24.230753000389,-7.51216677222198,
12.));
#233997=CARTESIAN_POINT('Ctrl Pts',(-24.2044693092356,-7.51678300997997,
12.));
#233998=CARTESIAN_POINT('Ctrl Pts',(-24.1782487641602,-7.52132590953862,
12.));
#233999=CARTESIAN_POINT('Ctrl Pts',(-24.152091842537,-7.52579563201478,
12.));
#234000=CARTESIAN_POINT('Ctrl Pts',(-24.1259990209211,-7.53019233935536,
12.));
#234001=CARTESIAN_POINT('Ctrl Pts',(-24.0999707772643,-7.53451619514658,
12.));
#234002=CARTESIAN_POINT('Ctrl Pts',(-24.0740075927984,-7.53876736531004,
12.));
#234003=CARTESIAN_POINT('Ctrl Pts',(-24.0481099543353,-7.54294601896127,
12.));
#234004=CARTESIAN_POINT('Ctrl Pts',(-24.0222783554531,-7.54705232885894,
12.));
#234005=CARTESIAN_POINT('Ctrl Pts',(-23.9965132953187,-7.55108647097431,
12.));
#234006=CARTESIAN_POINT('Ctrl Pts',(-23.9708152779886,-7.55504862424807,
12.));
#234007=CARTESIAN_POINT('Ctrl Pts',(-23.9451848115002,-7.55893897027679,
12.));
#234008=CARTESIAN_POINT('Ctrl Pts',(-23.9196224070759,-7.56275769304772,
12.));
#234009=CARTESIAN_POINT('Ctrl Pts',(-23.8941285782002,-7.5665049786379,
12.));
#234010=CARTESIAN_POINT('Ctrl Pts',(-23.8687038399595,-7.57018101500709,
12.));
#234011=CARTESIAN_POINT('Ctrl Pts',(-23.8433487096132,-7.57378599219814,
12.));
#234012=CARTESIAN_POINT('Ctrl Pts',(-23.8180637069976,-7.57732010249065,
12.));
#234013=CARTESIAN_POINT('Ctrl Pts',(-23.7928493549908,-7.58078354058212,
12.));
#234014=CARTESIAN_POINT('Ctrl Pts',(-23.7677061799376,-7.5841765037627,
12.));
#234015=CARTESIAN_POINT('Ctrl Pts',(-23.7426347121006,-7.58749919210825,
12.));
#234016=CARTESIAN_POINT('Ctrl Pts',(-23.7176354860457,-7.5907518086532,
12.));
#234017=CARTESIAN_POINT('Ctrl Pts',(-23.6927090405066,-7.59393455934034,
12.));
#234018=CARTESIAN_POINT('Ctrl Pts',(-23.6678559182875,-7.59704765299566,
12.));
#234019=CARTESIAN_POINT('Ctrl Pts',(-23.6430766661418,-7.60009130130125,
12.));
#234020=CARTESIAN_POINT('Ctrl Pts',(-23.6183718346576,-7.60306571877805,
12.));
#234021=CARTESIAN_POINT('Ctrl Pts',(-23.5937419781245,-7.60597112277093,
12.));
#234022=CARTESIAN_POINT('Ctrl Pts',(-23.5691876544244,-7.60880773344599,
12.));
#234023=CARTESIAN_POINT('Ctrl Pts',(-23.544709425203,-7.61157577385371,
12.));
#234024=CARTESIAN_POINT('Ctrl Pts',(-23.5203078560129,-7.61427546999297,
12.));
#234025=CARTESIAN_POINT('Ctrl Pts',(-23.4959835164609,-7.61690705088318,
12.));
#234026=CARTESIAN_POINT('Ctrl Pts',(-23.4717369803438,-7.61947074863976,
12.));
#234027=CARTESIAN_POINT('Ctrl Pts',(-23.4475688257854,-7.62196679855954,
12.));
#234028=CARTESIAN_POINT('Ctrl Pts',(-23.4234796353542,-7.62439543920049,
12.));
#234029=CARTESIAN_POINT('Ctrl Pts',(-23.399469996112,-7.62675691240328,
12.));
#234030=CARTESIAN_POINT('Ctrl Pts',(-23.3755404996636,-7.62905146332592,
12.));
#234031=CARTESIAN_POINT('Ctrl Pts',(-23.3516917421972,-7.63127934048136,
12.));
#234032=CARTESIAN_POINT('Ctrl Pts',(-23.3279243245241,-7.63344079578161,
12.));
#234033=CARTESIAN_POINT('Ctrl Pts',(-23.3042388521022,-7.63553608458782,
12.));
#234034=CARTESIAN_POINT('Ctrl Pts',(-23.2806359350855,-7.63756546576374,
12.));
#234035=CARTESIAN_POINT('Ctrl Pts',(-23.2571161884488,-7.63952920172835,
12.));
#234036=CARTESIAN_POINT('Ctrl Pts',(-23.2336802320912,-7.64142755851504,
12.));
#234037=CARTESIAN_POINT('Ctrl Pts',(-23.2103286909398,-7.64326080583679,
12.));
#234038=CARTESIAN_POINT('Ctrl Pts',(-23.1870621950452,-7.64502921715482,
12.));
#234039=CARTESIAN_POINT('Ctrl Pts',(-23.1638813796694,-7.64673306975804,
12.));
#234040=CARTESIAN_POINT('Ctrl Pts',(-23.1407868853819,-7.64837264482942,
12.));
#234041=CARTESIAN_POINT('Ctrl Pts',(-23.1177793581679,-7.64994822749859,
12.));
#234042=CARTESIAN_POINT('Ctrl Pts',(-23.094859449525,-7.65146010690475,
12.));
#234043=CARTESIAN_POINT('Ctrl Pts',(-23.072027816555,-7.65290857626357,
12.));
#234044=CARTESIAN_POINT('Ctrl Pts',(-23.0492851220528,-7.65429393293945,
12.));
#234045=CARTESIAN_POINT('Ctrl Pts',(-23.0266320345787,-7.65561647852533,
12.));
#234046=CARTESIAN_POINT('Ctrl Pts',(-23.0040692285814,-7.65687651891304,
12.));
#234047=CARTESIAN_POINT('Ctrl Pts',(-22.9815973845296,-7.65807436436431,
12.));
#234048=CARTESIAN_POINT('Ctrl Pts',(-22.959217189033,-7.65921032958901,
12.));
#234049=CARTESIAN_POINT('Ctrl Pts',(-22.9369293349593,-7.66028473382777,
12.));
#234050=CARTESIAN_POINT('Ctrl Pts',(-22.9147345215421,-7.66129790094107,
12.));
#234051=CARTESIAN_POINT('Ctrl Pts',(-22.8926334544883,-7.66225015950155,
12.));
#234052=CARTESIAN_POINT('Ctrl Pts',(-22.8706268461283,-7.66314184287336,
12.));
#234053=CARTESIAN_POINT('Ctrl Pts',(-22.848715415557,-7.66397328929802,
12.));
#234054=CARTESIAN_POINT('Ctrl Pts',(-22.8268998887678,-7.66474484198548,
12.));
#234055=CARTESIAN_POINT('Ctrl Pts',(-22.8051809987833,-7.66545684920987,
12.));
#234056=CARTESIAN_POINT('Ctrl Pts',(-22.7835594857699,-7.66610966441272,
12.));
#234057=CARTESIAN_POINT('Ctrl Pts',(-22.7620360971843,-7.66670364630298,
12.));
#234058=CARTESIAN_POINT('Ctrl Pts',(-22.7406115879513,-7.66723915895439,
12.));
#234059=CARTESIAN_POINT('Ctrl Pts',(-22.7192867206245,-7.66771657191027,
12.));
#234060=CARTESIAN_POINT('Ctrl Pts',(-22.6980622655446,-7.66813626029274,
12.));
#234061=CARTESIAN_POINT('Ctrl Pts',(-22.6769390009885,-7.66849860491742,
12.));
#234062=CARTESIAN_POINT('Ctrl Pts',(-22.6559177133127,-7.66880399241322,
12.));
#234063=CARTESIAN_POINT('Ctrl Pts',(-22.6349991971541,-7.66905281533714,
12.));
#234064=CARTESIAN_POINT('Ctrl Pts',(-22.6141842556243,-7.66924547229413,
12.));
#234065=CARTESIAN_POINT('Ctrl Pts',(-22.5934737004953,-7.66938236806232,
12.));
#234066=CARTESIAN_POINT('Ctrl Pts',(-22.5728683523831,-7.66946391372305,
12.));
#234067=CARTESIAN_POINT('Ctrl Pts',(-22.5523690409116,-7.66949052679692,
12.));
#234068=CARTESIAN_POINT('Ctrl Pts',(-22.53197660492,-7.66946263138143,12.));
#234069=CARTESIAN_POINT('Ctrl Pts',(-22.5116918927032,-7.66938065829107,
12.));
#234070=CARTESIAN_POINT('Ctrl Pts',(-22.4915157622312,-7.66924504520314,
12.));
#234071=CARTESIAN_POINT('Ctrl Pts',(-22.47144908137,-7.6690562368083,12.));
#234072=CARTESIAN_POINT('Ctrl Pts',(-22.4514927280855,-7.66881468496634,
12.));
#234073=CARTESIAN_POINT('Ctrl Pts',(-22.4316475906603,-7.66852084886704,
12.));
#234074=CARTESIAN_POINT('Ctrl Pts',(-22.4119145679758,-7.66817519519639,
12.));
#234075=CARTESIAN_POINT('Ctrl Pts',(-22.3922945697773,-7.66777819830789,
12.));
#234076=CARTESIAN_POINT('Ctrl Pts',(-22.372788516936,-7.66733034039882,
12.));
#234077=CARTESIAN_POINT('Ctrl Pts',(-22.3533973417021,-7.66683211169158,
12.));
#234078=CARTESIAN_POINT('Ctrl Pts',(-22.3341219879469,-7.66628401061952,
12.));
#234079=CARTESIAN_POINT('Ctrl Pts',(-22.314963411484,-7.66568654402493,
12.));
#234080=CARTESIAN_POINT('Ctrl Pts',(-22.2959225803937,-7.66504022736298,
12.));
#234081=CARTESIAN_POINT('Ctrl Pts',(-22.2770004753335,-7.66434558490978,
12.));
#234082=CARTESIAN_POINT('Ctrl Pts',(-22.258198089848,-7.6636031499764,12.));
#234083=CARTESIAN_POINT('Ctrl Pts',(-22.2395164306547,-7.66281346512508,
12.));
#234084=CARTESIAN_POINT('Ctrl Pts',(-22.2209565180085,-7.66197708240399,
12.));
#234085=CARTESIAN_POINT('Ctrl Pts',(-22.2025193860964,-7.6610945635927,
12.));
#234086=CARTESIAN_POINT('Ctrl Pts',(-22.1842060834091,-7.66016648045004,
12.));
#234087=CARTESIAN_POINT('Ctrl Pts',(-22.1660176731178,-7.6591934149693,
12.));
#234088=CARTESIAN_POINT('Ctrl Pts',(-22.1479552334211,-7.65817595963349,
12.));
#234089=CARTESIAN_POINT('Ctrl Pts',(-22.1300198579675,-7.65711471769396,
12.));
#234090=CARTESIAN_POINT('Ctrl Pts',(-22.1122126563329,-7.65601030346806,
12.));
#234091=CARTESIAN_POINT('Ctrl Pts',(-22.094534754469,-7.65486334263643,
12.));
#234092=CARTESIAN_POINT('Ctrl Pts',(-22.0769872951596,-7.65367447254949,
12.));
#234093=CARTESIAN_POINT('Ctrl Pts',(-22.0595714384431,-7.65244434253112,
12.));
#234094=CARTESIAN_POINT('Ctrl Pts',(-22.0422883621174,-7.65117361421358,
12.));
#234095=CARTESIAN_POINT('Ctrl Pts',(-22.0251392623209,-7.64986296190168,
12.));
#234096=CARTESIAN_POINT('Ctrl Pts',(-22.0081253540774,-7.64851307293351,
12.));
#234097=CARTESIAN_POINT('Ctrl Pts',(-21.9912478718542,-7.64712464805249,
12.));
#234098=CARTESIAN_POINT('Ctrl Pts',(-21.9745080700798,-7.64569840177335,
12.));
#234099=CARTESIAN_POINT('Ctrl Pts',(-21.9579072237651,-7.64423506279122,
12.));
#234100=CARTESIAN_POINT('Ctrl Pts',(-21.9414466292072,-7.64273537442682,
12.));
#234101=CARTESIAN_POINT('Ctrl Pts',(-21.9251276046546,-7.64120009506531,
12.));
#234102=CARTESIAN_POINT('Ctrl Pts',(-21.9089514909874,-7.63962999860927,
12.));
#234103=CARTESIAN_POINT('Ctrl Pts',(-21.8929196523514,-7.63802587492034,
12.));
#234104=CARTESIAN_POINT('Ctrl Pts',(-21.8770334769496,-7.63638853033399,
12.));
#234105=CARTESIAN_POINT('Ctrl Pts',(-21.8612943779089,-7.63471878821225,
12.));
#234106=CARTESIAN_POINT('Ctrl Pts',(-21.8457037941084,-7.63301748948935,
12.));
#234107=CARTESIAN_POINT('Ctrl Pts',(-21.8302631910195,-7.63128549323022,
12.));
#234108=CARTESIAN_POINT('Ctrl Pts',(-21.814974061509,-7.62952367718126,
12.));
#234109=CARTESIAN_POINT('Ctrl Pts',(-21.799837926858,-7.62773293842389,
12.));
#234110=CARTESIAN_POINT('Ctrl Pts',(-21.7848563378021,-7.62591419404512,
12.));
#234111=CARTESIAN_POINT('Ctrl Pts',(-21.7700308755584,-7.62406838181166,
12.));
#234112=CARTESIAN_POINT('Ctrl Pts',(-21.7553631528328,-7.62219646084228,
12.));
#234113=CARTESIAN_POINT('Ctrl Pts',(-21.7408548148656,-7.62029941230854,
12.));
#234114=CARTESIAN_POINT('Ctrl Pts',(-21.7265075407975,-7.61837824030537,
12.));
#234115=CARTESIAN_POINT('Ctrl Pts',(-21.7123230449834,-7.6164339727042,
12.));
#234116=CARTESIAN_POINT('Ctrl Pts',(-21.6983030783322,-7.61446766202786,
12.));
#234117=CARTESIAN_POINT('Ctrl Pts',(-21.6844494295815,-7.61248038630268,
12.));
#234118=CARTESIAN_POINT('Ctrl Pts',(-21.6707639267576,-7.61047325000955,
12.));
#234119=CARTESIAN_POINT('Ctrl Pts',(-21.6572484388081,-7.60844738512873,
12.));
#234120=CARTESIAN_POINT('Ctrl Pts',(-21.6439048771743,-7.60640395216356,
12.));
#234121=CARTESIAN_POINT('Ctrl Pts',(-21.6307351973822,-7.60434414118295,
12.));
#234122=CARTESIAN_POINT('Ctrl Pts',(-21.617741400599,-7.60226917285428,
12.));
#234123=CARTESIAN_POINT('Ctrl Pts',(-21.6049255358843,-7.6001802998824,
12.));
#234124=CARTESIAN_POINT('Ctrl Pts',(-21.5922897024466,-7.59807880846194,
12.));
#234125=CARTESIAN_POINT('Ctrl Pts',(-21.5798360518978,-7.59596601973583,
12.));
#234126=CARTESIAN_POINT('Ctrl Pts',(-21.5675667904726,-7.59384329124918,
12.));
#234127=CARTESIAN_POINT('Ctrl Pts',(-21.5554841813462,-7.59171201844776,
12.));
#234128=CARTESIAN_POINT('Ctrl Pts',(-21.543590547011,-7.58957363620013,
12.));
#234129=CARTESIAN_POINT('Ctrl Pts',(-21.5318882716736,-7.58742962034833,
12.));
#234130=CARTESIAN_POINT('Ctrl Pts',(-21.5203798035299,-7.58528148919129,
12.));
#234131=CARTESIAN_POINT('Ctrl Pts',(-21.5090676573873,-7.58313080519179,
12.));
#234132=CARTESIAN_POINT('Ctrl Pts',(-21.4979544192744,-7.58097917790744,
12.));
#234133=CARTESIAN_POINT('Ctrl Pts',(-21.4870427508194,-7.57882826679131,
12.));
#234134=CARTESIAN_POINT('Ctrl Pts',(-21.4763353936762,-7.57667978402987,
12.));
#234135=CARTESIAN_POINT('Ctrl Pts',(-21.4658351740128,-7.57453549743411,
12.));
#234136=CARTESIAN_POINT('Ctrl Pts',(-21.4555450053142,-7.57239723223505,
12.));
#234137=CARTESIAN_POINT('Ctrl Pts',(-21.4454678907509,-7.57026687261165,
12.));
#234138=CARTESIAN_POINT('Ctrl Pts',(-21.4356069261513,-7.56814636360847,
12.));
#234139=CARTESIAN_POINT('Ctrl Pts',(-21.4259653015736,-7.56603771218712,
12.));
#234140=CARTESIAN_POINT('Ctrl Pts',(-21.4165463106254,-7.56394299313684,
12.));
#234141=CARTESIAN_POINT('Ctrl Pts',(-21.4073533630365,-7.56186435703621,
12.));
#234142=CARTESIAN_POINT('Ctrl Pts',(-21.3983899952987,-7.5598040370061,
12.));
#234143=CARTESIAN_POINT('Ctrl Pts',(-21.3896598842117,-7.55776435731416,
12.));
#234144=CARTESIAN_POINT('Ctrl Pts',(-21.3811668478932,-7.55574773403502,
12.));
#234145=CARTESIAN_POINT('Ctrl Pts',(-21.3729148390243,-7.55375667080028,
12.));
#234146=CARTESIAN_POINT('Ctrl Pts',(-21.3649079431865,-7.55179375777443,
12.));
#234147=CARTESIAN_POINT('Ctrl Pts',(-21.3571503685855,-7.54986166521309,
12.));
#234148=CARTESIAN_POINT('Ctrl Pts',(-21.3496464761531,-7.5479631624633,
12.));
#234149=CARTESIAN_POINT('Ctrl Pts',(-21.3424008295038,-7.54610114948346,
12.));
#234150=CARTESIAN_POINT('Ctrl Pts',(-21.3354182340149,-7.54427868151267,
12.));
#234151=CARTESIAN_POINT('Ctrl Pts',(-21.328703791771,-7.5424990037703,12.));
#234152=CARTESIAN_POINT('Ctrl Pts',(-21.3222628524165,-7.54076552038278,
12.));
#234153=CARTESIAN_POINT('Ctrl Pts',(-21.3161009456256,-7.53908175169898,
12.));
#234154=CARTESIAN_POINT('Ctrl Pts',(-21.310223716773,-7.53745129364616,
12.));
#234155=CARTESIAN_POINT('Ctrl Pts',(-21.3046368712157,-7.53587778251735,
12.));
#234156=CARTESIAN_POINT('Ctrl Pts',(-21.2993464250717,-7.53436505309942,
12.));
#234157=CARTESIAN_POINT('Ctrl Pts',(-21.2943588989331,-7.53291726078526,
12.));
#234158=CARTESIAN_POINT('Ctrl Pts',(-21.2896816163842,-7.53153906987855,
12.));
#234159=CARTESIAN_POINT('Ctrl Pts',(-21.2853226580657,-7.53023562438229,
12.));
#234160=CARTESIAN_POINT('Ctrl Pts',(-21.2812902781143,-7.52901217930407,
12.));
#234161=CARTESIAN_POINT('Ctrl Pts',(-21.2775925269652,-7.52787386225332,
12.));
#234162=CARTESIAN_POINT('Ctrl Pts',(-21.2742366113579,-7.5268252691854,
12.));
#234163=CARTESIAN_POINT('Ctrl Pts',(-21.2712301573466,-7.52587126095529,
12.));
#234164=CARTESIAN_POINT('Ctrl Pts',(-21.2685823838671,-7.5250177033353,
12.));
#234165=CARTESIAN_POINT('Ctrl Pts',(-21.2663059157058,-7.52427261074297,
12.));
#234166=CARTESIAN_POINT('Ctrl Pts',(-21.2644161259962,-7.52364573027552,
12.));
#234167=CARTESIAN_POINT('Ctrl Pts',(-21.262927782038,-7.52314642316199,
12.));
#234168=CARTESIAN_POINT('Ctrl Pts',(-21.2618521283555,-7.52278182242669,
12.));
#234169=CARTESIAN_POINT('Ctrl Pts',(-21.261326054066,-7.5226006423166,12.));
#234170=CARTESIAN_POINT('Ctrl Pts',(-21.2611204474866,-7.52252744144903,
12.));
#234171=CARTESIAN_POINT('Ctrl Pts',(-21.2610673466886,-7.5225064970397,
12.));
#234172=CARTESIAN_POINT('Ctrl Pts',(-21.2610617890679,-7.52250298901264,
12.));
#234173=CARTESIAN_POINT('',(-24.9347862158358,-7.36589684767343,0.));
#234174=CARTESIAN_POINT('Origin',(-21.4341755315424,-1.68110656504246,0.));
#234175=CARTESIAN_POINT('',(-22.4835757167854,-1.76341220531179,12.));
#234176=CARTESIAN_POINT('',(-10.7170877657712,-0.840553282521227,12.));
#234177=CARTESIAN_POINT('',(-22.4835757167854,-1.76341220531179,0.));
#234178=CARTESIAN_POINT('',(-22.4835757167854,-1.76341220531179,0.));
#234179=CARTESIAN_POINT('',(-10.7170877657712,-0.840553282521227,0.));
#234180=CARTESIAN_POINT('Ctrl Pts',(-25.2771067246846,-6.08833931617698,
0.));
#234181=CARTESIAN_POINT('Ctrl Pts',(-25.2771067246846,-6.08833931617698,
12.));
#234182=CARTESIAN_POINT('Ctrl Pts',(-25.2729539149479,-6.08441489609824,
0.));
#234183=CARTESIAN_POINT('Ctrl Pts',(-25.2729539149479,-6.08441489609824,
12.));
#234184=CARTESIAN_POINT('Ctrl Pts',(-25.2646490489816,-6.07657531787577,
0.));
#234185=CARTESIAN_POINT('Ctrl Pts',(-25.2646490489816,-6.07657531787577,
12.));
#234186=CARTESIAN_POINT('Ctrl Pts',(-25.2521940105523,-6.06484373634696,
0.));
#234187=CARTESIAN_POINT('Ctrl Pts',(-25.2521940105523,-6.06484373634696,
12.));
#234188=CARTESIAN_POINT('Ctrl Pts',(-25.2355918138798,-6.04925720151412,
0.));
#234189=CARTESIAN_POINT('Ctrl Pts',(-25.2355918138798,-6.04925720151412,
12.));
#234190=CARTESIAN_POINT('Ctrl Pts',(-25.2148466201368,-6.02986667390187,
0.));
#234191=CARTESIAN_POINT('Ctrl Pts',(-25.2148466201368,-6.02986667390187,
12.));
#234192=CARTESIAN_POINT('Ctrl Pts',(-25.1941090269638,-6.0105688180476,
0.));
#234193=CARTESIAN_POINT('Ctrl Pts',(-25.1941090269638,-6.0105688180476,
12.));
#234194=CARTESIAN_POINT('Ctrl Pts',(-25.1733791296154,-5.99136367859838,
0.));
#234195=CARTESIAN_POINT('Ctrl Pts',(-25.1733791296154,-5.99136367859838,
12.));
#234196=CARTESIAN_POINT('Ctrl Pts',(-25.1526570863065,-5.97225131495636,
0.));
#234197=CARTESIAN_POINT('Ctrl Pts',(-25.1526570863065,-5.97225131495636,
12.));
#234198=CARTESIAN_POINT('Ctrl Pts',(-25.1319431317273,-5.95323180187348,
0.));
#234199=CARTESIAN_POINT('Ctrl Pts',(-25.1319431317273,-5.95323180187348,
12.));
#234200=CARTESIAN_POINT('Ctrl Pts',(-25.1112375971182,-5.93430523086776,
0.));
#234201=CARTESIAN_POINT('Ctrl Pts',(-25.1112375971182,-5.93430523086776,
12.));
#234202=CARTESIAN_POINT('Ctrl Pts',(-25.0905409050863,-5.91547170844382,
0.));
#234203=CARTESIAN_POINT('Ctrl Pts',(-25.0905409050863,-5.91547170844382,
12.));
#234204=CARTESIAN_POINT('Ctrl Pts',(-25.0698535426593,-5.89673135155459,
0.));
#234205=CARTESIAN_POINT('Ctrl Pts',(-25.0698535426593,-5.89673135155459,
12.));
#234206=CARTESIAN_POINT('Ctrl Pts',(-25.0491760405965,-5.87808428385329,
0.));
#234207=CARTESIAN_POINT('Ctrl Pts',(-25.0491760405965,-5.87808428385329,
12.));
#234208=CARTESIAN_POINT('Ctrl Pts',(-25.0285089498922,-5.8595306315681,
0.));
#234209=CARTESIAN_POINT('Ctrl Pts',(-25.0285089498922,-5.8595306315681,
12.));
#234210=CARTESIAN_POINT('Ctrl Pts',(-25.0078528200558,-5.84107051963073,
0.));
#234211=CARTESIAN_POINT('Ctrl Pts',(-25.0078528200558,-5.84107051963073,
12.));
#234212=CARTESIAN_POINT('Ctrl Pts',(-24.9872081752709,-5.82270406744214,
0.));
#234213=CARTESIAN_POINT('Ctrl Pts',(-24.9872081752709,-5.82270406744214,
12.));
#234214=CARTESIAN_POINT('Ctrl Pts',(-24.9665754954462,-5.80443138549747,
0.));
#234215=CARTESIAN_POINT('Ctrl Pts',(-24.9665754954462,-5.80443138549747,
12.));
#234216=CARTESIAN_POINT('Ctrl Pts',(-24.9459552293308,-5.78625257775703,
0.));
#234217=CARTESIAN_POINT('Ctrl Pts',(-24.9459552293308,-5.78625257775703,
12.));
#234218=CARTESIAN_POINT('Ctrl Pts',(-24.9253478043632,-5.76816774342236,
0.));
#234219=CARTESIAN_POINT('Ctrl Pts',(-24.9253478043632,-5.76816774342236,
12.));
#234220=CARTESIAN_POINT('Ctrl Pts',(-24.9047536376467,-5.75017697890813,
0.));
#234221=CARTESIAN_POINT('Ctrl Pts',(-24.9047536376467,-5.75017697890813,
12.));
#234222=CARTESIAN_POINT('Ctrl Pts',(-24.8841731467219,-5.73228037976926,
0.));
#234223=CARTESIAN_POINT('Ctrl Pts',(-24.8841731467219,-5.73228037976926,
12.));
#234224=CARTESIAN_POINT('Ctrl Pts',(-24.8636067597677,-5.71447804252019,
0.));
#234225=CARTESIAN_POINT('Ctrl Pts',(-24.8636067597677,-5.71447804252019,
12.));
#234226=CARTESIAN_POINT('Ctrl Pts',(-24.8430549277634,-5.69677006679429,
0.));
#234227=CARTESIAN_POINT('Ctrl Pts',(-24.8430549277634,-5.69677006679429,
12.));
#234228=CARTESIAN_POINT('Ctrl Pts',(-24.822518122386,-5.67915655496524,
0.));
#234229=CARTESIAN_POINT('Ctrl Pts',(-24.822518122386,-5.67915655496524,
12.));
#234230=CARTESIAN_POINT('Ctrl Pts',(-24.8019968304618,-5.66163761114903,
0.));
#234231=CARTESIAN_POINT('Ctrl Pts',(-24.8019968304618,-5.66163761114903,
12.));
#234232=CARTESIAN_POINT('Ctrl Pts',(-24.7814915496728,-5.64421334042247,
0.));
#234233=CARTESIAN_POINT('Ctrl Pts',(-24.7814915496728,-5.64421334042247,
12.));
#234234=CARTESIAN_POINT('Ctrl Pts',(-24.76100278357,-5.62688384790919,0.));
#234235=CARTESIAN_POINT('Ctrl Pts',(-24.76100278357,-5.62688384790919,12.));
#234236=CARTESIAN_POINT('Ctrl Pts',(-24.7405310372736,-5.60964923798495,
0.));
#234237=CARTESIAN_POINT('Ctrl Pts',(-24.7405310372736,-5.60964923798495,
12.));
#234238=CARTESIAN_POINT('Ctrl Pts',(-24.7200768119079,-5.59250961323995,
0.));
#234239=CARTESIAN_POINT('Ctrl Pts',(-24.7200768119079,-5.59250961323995,
12.));
#234240=CARTESIAN_POINT('Ctrl Pts',(-24.6996406035507,-5.57546507427766,
0.));
#234241=CARTESIAN_POINT('Ctrl Pts',(-24.6996406035507,-5.57546507427766,
12.));
#234242=CARTESIAN_POINT('Ctrl Pts',(-24.6792229061785,-5.55851572025389,
0.));
#234243=CARTESIAN_POINT('Ctrl Pts',(-24.6792229061785,-5.55851572025389,
12.));
#234244=CARTESIAN_POINT('Ctrl Pts',(-24.6588242134733,-5.54166164919593,
0.));
#234245=CARTESIAN_POINT('Ctrl Pts',(-24.6588242134733,-5.54166164919593,
12.));
#234246=CARTESIAN_POINT('Ctrl Pts',(-24.6384450211466,-5.52490295840996,
0.));
#234247=CARTESIAN_POINT('Ctrl Pts',(-24.6384450211466,-5.52490295840996,
12.));
#234248=CARTESIAN_POINT('Ctrl Pts',(-24.618085828918,-5.50823974481959,
0.));
#234249=CARTESIAN_POINT('Ctrl Pts',(-24.618085828918,-5.50823974481959,
12.));
#234250=CARTESIAN_POINT('Ctrl Pts',(-24.5977471429365,-5.49167210537235,
0.));
#234251=CARTESIAN_POINT('Ctrl Pts',(-24.5977471429365,-5.49167210537235,
12.));
#234252=CARTESIAN_POINT('Ctrl Pts',(-24.5774294770329,-5.47520013724403,
0.));
#234253=CARTESIAN_POINT('Ctrl Pts',(-24.5774294770329,-5.47520013724403,
12.));
#234254=CARTESIAN_POINT('Ctrl Pts',(-24.5571333514841,-5.45882393762244,
0.));
#234255=CARTESIAN_POINT('Ctrl Pts',(-24.5571333514841,-5.45882393762244,
12.));
#234256=CARTESIAN_POINT('Ctrl Pts',(-24.5368592922861,-5.44254360356865,
0.));
#234257=CARTESIAN_POINT('Ctrl Pts',(-24.5368592922861,-5.44254360356865,
12.));
#234258=CARTESIAN_POINT('Ctrl Pts',(-24.5166078302107,-5.42635923183411,
0.));
#234259=CARTESIAN_POINT('Ctrl Pts',(-24.5166078302107,-5.42635923183411,
12.));
#234260=CARTESIAN_POINT('Ctrl Pts',(-24.4963794999831,-5.41027091869242,
0.));
#234261=CARTESIAN_POINT('Ctrl Pts',(-24.4963794999831,-5.41027091869242,
12.));
#234262=CARTESIAN_POINT('Ctrl Pts',(-24.4761748393322,-5.3942787597383,
0.));
#234263=CARTESIAN_POINT('Ctrl Pts',(-24.4761748393322,-5.3942787597383,
12.));
#234264=CARTESIAN_POINT('Ctrl Pts',(-24.4559943883159,-5.37838284973706,
0.));
#234265=CARTESIAN_POINT('Ctrl Pts',(-24.4559943883159,-5.37838284973706,
12.));
#234266=CARTESIAN_POINT('Ctrl Pts',(-24.4358386899152,-5.36258328273639,
0.));
#234267=CARTESIAN_POINT('Ctrl Pts',(-24.4358386899152,-5.36258328273639,
12.));
#234268=CARTESIAN_POINT('Ctrl Pts',(-24.4157082904615,-5.34688015213546,
0.));
#234269=CARTESIAN_POINT('Ctrl Pts',(-24.4157082904615,-5.34688015213546,
12.));
#234270=CARTESIAN_POINT('Ctrl Pts',(-24.3956037401293,-5.33127355076036,
0.));
#234271=CARTESIAN_POINT('Ctrl Pts',(-24.3956037401293,-5.33127355076036,
12.));
#234272=CARTESIAN_POINT('Ctrl Pts',(-24.3755255933917,-5.31576357092524,
0.));
#234273=CARTESIAN_POINT('Ctrl Pts',(-24.3755255933917,-5.31576357092524,
12.));
#234274=CARTESIAN_POINT('Ctrl Pts',(-24.3554744095075,-5.30035030449058,
0.));
#234275=CARTESIAN_POINT('Ctrl Pts',(-24.3554744095075,-5.30035030449058,
12.));
#234276=CARTESIAN_POINT('Ctrl Pts',(-24.3354507529415,-5.28503384290644,
0.));
#234277=CARTESIAN_POINT('Ctrl Pts',(-24.3354507529415,-5.28503384290644,
12.));
#234278=CARTESIAN_POINT('Ctrl Pts',(-24.3154551932222,-5.26981427718796,
0.));
#234279=CARTESIAN_POINT('Ctrl Pts',(-24.3154551932222,-5.26981427718796,
12.));
#234280=CARTESIAN_POINT('Ctrl Pts',(-24.2954883048448,-5.25469169788856,
0.));
#234281=CARTESIAN_POINT('Ctrl Pts',(-24.2954883048448,-5.25469169788856,
12.));
#234282=CARTESIAN_POINT('Ctrl Pts',(-24.2755506671526,-5.23966619506289,
0.));
#234283=CARTESIAN_POINT('Ctrl Pts',(-24.2755506671526,-5.23966619506289,
12.));
#234284=CARTESIAN_POINT('Ctrl Pts',(-24.2556428642294,-5.22473785822441,
0.));
#234285=CARTESIAN_POINT('Ctrl Pts',(-24.2556428642294,-5.22473785822441,
12.));
#234286=CARTESIAN_POINT('Ctrl Pts',(-24.2357654847765,-5.20990677629173,
0.));
#234287=CARTESIAN_POINT('Ctrl Pts',(-24.2357654847765,-5.20990677629173,
12.));
#234288=CARTESIAN_POINT('Ctrl Pts',(-24.215919122017,-5.19517303753643,
0.));
#234289=CARTESIAN_POINT('Ctrl Pts',(-24.215919122017,-5.19517303753643,
12.));
#234290=CARTESIAN_POINT('Ctrl Pts',(-24.1961043738754,-5.18053672961392,
0.));
#234291=CARTESIAN_POINT('Ctrl Pts',(-24.1961043738754,-5.18053672961392,
12.));
#234292=CARTESIAN_POINT('Ctrl Pts',(-24.1763218431343,-5.16599793957979,
0.));
#234293=CARTESIAN_POINT('Ctrl Pts',(-24.1763218431343,-5.16599793957979,
12.));
#234294=CARTESIAN_POINT('Ctrl Pts',(-24.156572137597,-5.15155675390075,
0.));
#234295=CARTESIAN_POINT('Ctrl Pts',(-24.156572137597,-5.15155675390075,
12.));
#234296=CARTESIAN_POINT('Ctrl Pts',(-24.1368558702443,-5.13721325845744,
0.));
#234297=CARTESIAN_POINT('Ctrl Pts',(-24.1368558702443,-5.13721325845744,
12.));
#234298=CARTESIAN_POINT('Ctrl Pts',(-24.117173659394,-5.12296753853859,
0.));
#234299=CARTESIAN_POINT('Ctrl Pts',(-24.117173659394,-5.12296753853859,
12.));
#234300=CARTESIAN_POINT('Ctrl Pts',(-24.0975261288446,-5.10881967883132,
0.));
#234301=CARTESIAN_POINT('Ctrl Pts',(-24.0975261288446,-5.10881967883132,
12.));
#234302=CARTESIAN_POINT('Ctrl Pts',(-24.0779139079266,-5.09476976342625,
0.));
#234303=CARTESIAN_POINT('Ctrl Pts',(-24.0779139079266,-5.09476976342625,
12.));
#234304=CARTESIAN_POINT('Ctrl Pts',(-24.0583376315638,-5.08081787581276,
0.));
#234305=CARTESIAN_POINT('Ctrl Pts',(-24.0583376315638,-5.08081787581276,
12.));
#234306=CARTESIAN_POINT('Ctrl Pts',(-24.0387979403268,-5.06696409886641,
0.));
#234307=CARTESIAN_POINT('Ctrl Pts',(-24.0387979403268,-5.06696409886641,
12.));
#234308=CARTESIAN_POINT('Ctrl Pts',(-24.0192954804896,-5.05320851483065,
0.));
#234309=CARTESIAN_POINT('Ctrl Pts',(-24.0192954804896,-5.05320851483065,
12.));
#234310=CARTESIAN_POINT('Ctrl Pts',(-23.9998309040746,-5.03955120528521,
0.));
#234311=CARTESIAN_POINT('Ctrl Pts',(-23.9998309040746,-5.03955120528521,
12.));
#234312=CARTESIAN_POINT('Ctrl Pts',(-23.9804048689227,-5.02599225112454,
0.));
#234313=CARTESIAN_POINT('Ctrl Pts',(-23.9804048689227,-5.02599225112454,
12.));
#234314=CARTESIAN_POINT('Ctrl Pts',(-23.9610180388271,-5.01253173257453,
0.));
#234315=CARTESIAN_POINT('Ctrl Pts',(-23.9610180388271,-5.01253173257453,
12.));
#234316=CARTESIAN_POINT('Ctrl Pts',(-23.9416710836529,-4.99916972919306,
0.));
#234317=CARTESIAN_POINT('Ctrl Pts',(-23.9416710836529,-4.99916972919306,
12.));
#234318=CARTESIAN_POINT('Ctrl Pts',(-23.9223646794592,-4.98590631986532,
0.));
#234319=CARTESIAN_POINT('Ctrl Pts',(-23.9223646794592,-4.98590631986532,
12.));
#234320=CARTESIAN_POINT('Ctrl Pts',(-23.9030995086163,-4.97274158279226,
0.));
#234321=CARTESIAN_POINT('Ctrl Pts',(-23.9030995086163,-4.97274158279226,
12.));
#234322=CARTESIAN_POINT('Ctrl Pts',(-23.8838762599218,-4.9596755954656,
0.));
#234323=CARTESIAN_POINT('Ctrl Pts',(-23.8838762599218,-4.9596755954656,
12.));
#234324=CARTESIAN_POINT('Ctrl Pts',(-23.8646956287168,-4.9467084346586,
0.));
#234325=CARTESIAN_POINT('Ctrl Pts',(-23.8646956287168,-4.9467084346586,
12.));
#234326=CARTESIAN_POINT('Ctrl Pts',(-23.8455583170057,-4.93384017643432,
0.));
#234327=CARTESIAN_POINT('Ctrl Pts',(-23.8455583170057,-4.93384017643432,
12.));
#234328=CARTESIAN_POINT('Ctrl Pts',(-23.8264650335717,-4.92107089613969,
0.));
#234329=CARTESIAN_POINT('Ctrl Pts',(-23.8264650335717,-4.92107089613969,
12.));
#234330=CARTESIAN_POINT('Ctrl Pts',(-23.8074164940896,-4.90840066839344,
0.));
#234331=CARTESIAN_POINT('Ctrl Pts',(-23.8074164940896,-4.90840066839344,
12.));
#234332=CARTESIAN_POINT('Ctrl Pts',(-23.7884134212384,-4.89582956706775,
0.));
#234333=CARTESIAN_POINT('Ctrl Pts',(-23.7884134212384,-4.89582956706775,
12.));
#234334=CARTESIAN_POINT('Ctrl Pts',(-23.7694565448049,-4.88335766525573,
0.));
#234335=CARTESIAN_POINT('Ctrl Pts',(-23.7694565448049,-4.88335766525573,
12.));
#234336=CARTESIAN_POINT('Ctrl Pts',(-23.7505466018245,-4.87098503527152,
0.));
#234337=CARTESIAN_POINT('Ctrl Pts',(-23.7505466018245,-4.87098503527152,
12.));
#234338=CARTESIAN_POINT('Ctrl Pts',(-23.7316843367313,-4.85871174865499,
0.));
#234339=CARTESIAN_POINT('Ctrl Pts',(-23.7316843367313,-4.85871174865499,
12.));
#234340=CARTESIAN_POINT('Ctrl Pts',(-23.7128705015017,-4.84653787616425,
0.));
#234341=CARTESIAN_POINT('Ctrl Pts',(-23.7128705015017,-4.84653787616425,
12.));
#234342=CARTESIAN_POINT('Ctrl Pts',(-23.6941058557971,-4.83446348776265,
0.));
#234343=CARTESIAN_POINT('Ctrl Pts',(-23.6941058557971,-4.83446348776265,
12.));
#234344=CARTESIAN_POINT('Ctrl Pts',(-23.675391167102,-4.82248865259562,
0.));
#234345=CARTESIAN_POINT('Ctrl Pts',(-23.675391167102,-4.82248865259562,
12.));
#234346=CARTESIAN_POINT('Ctrl Pts',(-23.6567272108628,-4.81061343896432,
0.));
#234347=CARTESIAN_POINT('Ctrl Pts',(-23.6567272108628,-4.81061343896432,
12.));
#234348=CARTESIAN_POINT('Ctrl Pts',(-23.6381147706579,-4.7988379143322,
0.));
#234349=CARTESIAN_POINT('Ctrl Pts',(-23.6381147706579,-4.7988379143322,
12.));
#234350=CARTESIAN_POINT('Ctrl Pts',(-23.6195546383624,-4.78716214532098,
0.));
#234351=CARTESIAN_POINT('Ctrl Pts',(-23.6195546383624,-4.78716214532098,
12.));
#234352=CARTESIAN_POINT('Ctrl Pts',(-23.6010476143099,-4.77558619769872,
0.));
#234353=CARTESIAN_POINT('Ctrl Pts',(-23.6010476143099,-4.77558619769872,
12.));
#234354=CARTESIAN_POINT('Ctrl Pts',(-23.5825945074535,-4.76411013636251,
0.));
#234355=CARTESIAN_POINT('Ctrl Pts',(-23.5825945074535,-4.76411013636251,
12.));
#234356=CARTESIAN_POINT('Ctrl Pts',(-23.5641961355168,-4.75273402530617,
0.));
#234357=CARTESIAN_POINT('Ctrl Pts',(-23.5641961355168,-4.75273402530617,
12.));
#234358=CARTESIAN_POINT('Ctrl Pts',(-23.545853325171,-4.74145792760698,
0.));
#234359=CARTESIAN_POINT('Ctrl Pts',(-23.545853325171,-4.74145792760698,
12.));
#234360=CARTESIAN_POINT('Ctrl Pts',(-23.5275669122372,-4.7302819054303,
0.));
#234361=CARTESIAN_POINT('Ctrl Pts',(-23.5275669122372,-4.7302819054303,
12.));
#234362=CARTESIAN_POINT('Ctrl Pts',(-23.509337741878,-4.71920602001901,
0.));
#234363=CARTESIAN_POINT('Ctrl Pts',(-23.509337741878,-4.71920602001901,
12.));
#234364=CARTESIAN_POINT('Ctrl Pts',(-23.491166668789,-4.70823033167818,
0.));
#234365=CARTESIAN_POINT('Ctrl Pts',(-23.491166668789,-4.70823033167818,
12.));
#234366=CARTESIAN_POINT('Ctrl Pts',(-23.4730545573853,-4.69735489975024,
0.));
#234367=CARTESIAN_POINT('Ctrl Pts',(-23.4730545573853,-4.69735489975024,
12.));
#234368=CARTESIAN_POINT('Ctrl Pts',(-23.455002281986,-4.68657978258303,
0.));
#234369=CARTESIAN_POINT('Ctrl Pts',(-23.455002281986,-4.68657978258303,
12.));
#234370=CARTESIAN_POINT('Ctrl Pts',(-23.4370107270451,-4.67590503753058,
0.));
#234371=CARTESIAN_POINT('Ctrl Pts',(-23.4370107270451,-4.67590503753058,
12.));
#234372=CARTESIAN_POINT('Ctrl Pts',(-23.4190807873803,-4.6653307209467,
0.));
#234373=CARTESIAN_POINT('Ctrl Pts',(-23.4190807873803,-4.6653307209467,
12.));
#234374=CARTESIAN_POINT('Ctrl Pts',(-23.4012133683959,-4.65485688816924,
0.));
#234375=CARTESIAN_POINT('Ctrl Pts',(-23.4012133683959,-4.65485688816924,
12.));
#234376=CARTESIAN_POINT('Ctrl Pts',(-23.3834093863068,-4.6444835934993,
0.));
#234377=CARTESIAN_POINT('Ctrl Pts',(-23.3834093863068,-4.6444835934993,
12.));
#234378=CARTESIAN_POINT('Ctrl Pts',(-23.3656697683489,-4.63421089016541,
0.));
#234379=CARTESIAN_POINT('Ctrl Pts',(-23.3656697683489,-4.63421089016541,
12.));
#234380=CARTESIAN_POINT('Ctrl Pts',(-23.3479954530272,-4.62403883030805,
0.));
#234381=CARTESIAN_POINT('Ctrl Pts',(-23.3479954530272,-4.62403883030805,
12.));
#234382=CARTESIAN_POINT('Ctrl Pts',(-23.3303873903938,-4.6139674649783,
0.));
#234383=CARTESIAN_POINT('Ctrl Pts',(-23.3303873903938,-4.6139674649783,
12.));
#234384=CARTESIAN_POINT('Ctrl Pts',(-23.3128465423115,-4.60399684412163,
0.));
#234385=CARTESIAN_POINT('Ctrl Pts',(-23.3128465423115,-4.60399684412163,
12.));
#234386=CARTESIAN_POINT('Ctrl Pts',(-23.2953738827191,-4.5941270165575,
0.));
#234387=CARTESIAN_POINT('Ctrl Pts',(-23.2953738827191,-4.5941270165575,
12.));
#234388=CARTESIAN_POINT('Ctrl Pts',(-23.2779703978876,-4.5843580299469,
0.));
#234389=CARTESIAN_POINT('Ctrl Pts',(-23.2779703978876,-4.5843580299469,
12.));
#234390=CARTESIAN_POINT('Ctrl Pts',(-23.2606370866866,-4.57468993076097,
0.));
#234391=CARTESIAN_POINT('Ctrl Pts',(-23.2606370866866,-4.57468993076097,
12.));
#234392=CARTESIAN_POINT('Ctrl Pts',(-23.2433749609131,-4.56512276427839,
0.));
#234393=CARTESIAN_POINT('Ctrl Pts',(-23.2433749609131,-4.56512276427839,
12.));
#234394=CARTESIAN_POINT('Ctrl Pts',(-23.2261850456064,-4.55565657456975,
0.));
#234395=CARTESIAN_POINT('Ctrl Pts',(-23.2261850456064,-4.55565657456975,
12.));
#234396=CARTESIAN_POINT('Ctrl Pts',(-23.2090683793629,-4.54629140447544,
0.));
#234397=CARTESIAN_POINT('Ctrl Pts',(-23.2090683793629,-4.54629140447544,
12.));
#234398=CARTESIAN_POINT('Ctrl Pts',(-23.1920260146465,-4.53702729557566,
0.));
#234399=CARTESIAN_POINT('Ctrl Pts',(-23.1920260146465,-4.53702729557566,
12.));
#234400=CARTESIAN_POINT('Ctrl Pts',(-23.1750590180908,-4.52786428815014,
0.));
#234401=CARTESIAN_POINT('Ctrl Pts',(-23.1750590180908,-4.52786428815014,
12.));
#234402=CARTESIAN_POINT('Ctrl Pts',(-23.1581684708761,-4.51880242116748,
0.));
#234403=CARTESIAN_POINT('Ctrl Pts',(-23.1581684708761,-4.51880242116748,
12.));
#234404=CARTESIAN_POINT('Ctrl Pts',(-23.1413554691123,-4.5098417322706,
0.));
#234405=CARTESIAN_POINT('Ctrl Pts',(-23.1413554691123,-4.5098417322706,
12.));
#234406=CARTESIAN_POINT('Ctrl Pts',(-23.1246211242115,-4.50098225775171,
0.));
#234407=CARTESIAN_POINT('Ctrl Pts',(-23.1246211242115,-4.50098225775171,
12.));
#234408=CARTESIAN_POINT('Ctrl Pts',(-23.1079665632636,-4.49222403252216,
0.));
#234409=CARTESIAN_POINT('Ctrl Pts',(-23.1079665632636,-4.49222403252216,
12.));
#234410=CARTESIAN_POINT('Ctrl Pts',(-23.0913929293922,-4.48356709006788,
0.));
#234411=CARTESIAN_POINT('Ctrl Pts',(-23.0913929293922,-4.48356709006788,
12.));
#234412=CARTESIAN_POINT('Ctrl Pts',(-23.0749013821881,-4.47501146242856,
0.));
#234413=CARTESIAN_POINT('Ctrl Pts',(-23.0749013821881,-4.47501146242856,
12.));
#234414=CARTESIAN_POINT('Ctrl Pts',(-23.0584930981732,-4.4665571801823,
0.));
#234415=CARTESIAN_POINT('Ctrl Pts',(-23.0584930981732,-4.4665571801823,
12.));
#234416=CARTESIAN_POINT('Ctrl Pts',(-23.0421692712467,-4.45820427241683,
0.));
#234417=CARTESIAN_POINT('Ctrl Pts',(-23.0421692712467,-4.45820427241683,
12.));
#234418=CARTESIAN_POINT('Ctrl Pts',(-23.0259311131392,-4.44995276669686,
0.));
#234419=CARTESIAN_POINT('Ctrl Pts',(-23.0259311131392,-4.44995276669686,
12.));
#234420=CARTESIAN_POINT('Ctrl Pts',(-23.0097798538395,-4.44180268901643,
0.));
#234421=CARTESIAN_POINT('Ctrl Pts',(-23.0097798538395,-4.44180268901643,
12.));
#234422=CARTESIAN_POINT('Ctrl Pts',(-22.9937167421006,-4.43375406376879,
0.));
#234423=CARTESIAN_POINT('Ctrl Pts',(-22.9937167421006,-4.43375406376879,
12.));
#234424=CARTESIAN_POINT('Ctrl Pts',(-22.977743046002,-4.42580691372751,
0.));
#234425=CARTESIAN_POINT('Ctrl Pts',(-22.977743046002,-4.42580691372751,
12.));
#234426=CARTESIAN_POINT('Ctrl Pts',(-22.9618600534866,-4.41796126001302,
0.));
#234427=CARTESIAN_POINT('Ctrl Pts',(-22.9618600534866,-4.41796126001302,
12.));
#234428=CARTESIAN_POINT('Ctrl Pts',(-22.9460690729093,-4.41021712205553,
0.));
#234429=CARTESIAN_POINT('Ctrl Pts',(-22.9460690729093,-4.41021712205553,
12.));
#234430=CARTESIAN_POINT('Ctrl Pts',(-22.930371433555,-4.40257451754323,
0.));
#234431=CARTESIAN_POINT('Ctrl Pts',(-22.930371433555,-4.40257451754323,
12.));
#234432=CARTESIAN_POINT('Ctrl Pts',(-22.9147684862426,-4.39503346238473,
0.));
#234433=CARTESIAN_POINT('Ctrl Pts',(-22.9147684862426,-4.39503346238473,
12.));
#234434=CARTESIAN_POINT('Ctrl Pts',(-22.8992616040108,-4.38759397068406,
0.));
#234435=CARTESIAN_POINT('Ctrl Pts',(-22.8992616040108,-4.38759397068406,
12.));
#234436=CARTESIAN_POINT('Ctrl Pts',(-22.8838521827701,-4.38025605470093,
0.));
#234437=CARTESIAN_POINT('Ctrl Pts',(-22.8838521827701,-4.38025605470093,
12.));
#234438=CARTESIAN_POINT('Ctrl Pts',(-22.8685416419725,-4.37301972480745,
0.));
#234439=CARTESIAN_POINT('Ctrl Pts',(-22.8685416419725,-4.37301972480745,
12.));
#234440=CARTESIAN_POINT('Ctrl Pts',(-22.8533314252422,-4.36588498942997,
0.));
#234441=CARTESIAN_POINT('Ctrl Pts',(-22.8533314252422,-4.36588498942997,
12.));
#234442=CARTESIAN_POINT('Ctrl Pts',(-22.8382230011184,-4.35885185500546,
0.));
#234443=CARTESIAN_POINT('Ctrl Pts',(-22.8382230011184,-4.35885185500546,
12.));
#234444=CARTESIAN_POINT('Ctrl Pts',(-22.8232178638876,-4.35192032594791,
0.));
#234445=CARTESIAN_POINT('Ctrl Pts',(-22.8232178638876,-4.35192032594791,
12.));
#234446=CARTESIAN_POINT('Ctrl Pts',(-22.8083175343791,-4.34509040460062,
0.));
#234447=CARTESIAN_POINT('Ctrl Pts',(-22.8083175343791,-4.34509040460062,
12.));
#234448=CARTESIAN_POINT('Ctrl Pts',(-22.7935235607806,-4.33836209118446,
0.));
#234449=CARTESIAN_POINT('Ctrl Pts',(-22.7935235607806,-4.33836209118446,
12.));
#234450=CARTESIAN_POINT('Ctrl Pts',(-22.7788375194076,-4.3317353837319,
0.));
#234451=CARTESIAN_POINT('Ctrl Pts',(-22.7788375194076,-4.3317353837319,
12.));
#234452=CARTESIAN_POINT('Ctrl Pts',(-22.7642610156475,-4.32521027803754,
0.));
#234453=CARTESIAN_POINT('Ctrl Pts',(-22.7642610156475,-4.32521027803754,
12.));
#234454=CARTESIAN_POINT('Ctrl Pts',(-22.7497956849848,-4.31878676761235,
0.));
#234455=CARTESIAN_POINT('Ctrl Pts',(-22.7497956849848,-4.31878676761235,
12.));
#234456=CARTESIAN_POINT('Ctrl Pts',(-22.7354431939926,-4.31246484362549,
0.));
#234457=CARTESIAN_POINT('Ctrl Pts',(-22.7354431939926,-4.31246484362549,
12.));
#234458=CARTESIAN_POINT('Ctrl Pts',(-22.7212052413386,-4.30624449484069,
0.));
#234459=CARTESIAN_POINT('Ctrl Pts',(-22.7212052413386,-4.30624449484069,
12.));
#234460=CARTESIAN_POINT('Ctrl Pts',(-22.7070835587564,-4.3001257075406,
0.));
#234461=CARTESIAN_POINT('Ctrl Pts',(-22.7070835587564,-4.3001257075406,
12.));
#234462=CARTESIAN_POINT('Ctrl Pts',(-22.6930799122548,-4.29410846547056,
0.));
#234463=CARTESIAN_POINT('Ctrl Pts',(-22.6930799122548,-4.29410846547056,
12.));
#234464=CARTESIAN_POINT('Ctrl Pts',(-22.6791961033538,-4.28819274977763,
0.));
#234465=CARTESIAN_POINT('Ctrl Pts',(-22.6791961033538,-4.28819274977763,
12.));
#234466=CARTESIAN_POINT('Ctrl Pts',(-22.6654339703109,-4.28237853894059,
0.));
#234467=CARTESIAN_POINT('Ctrl Pts',(-22.6654339703109,-4.28237853894059,
12.));
#234468=CARTESIAN_POINT('Ctrl Pts',(-22.6517953893303,-4.2766658086912,
0.));
#234469=CARTESIAN_POINT('Ctrl Pts',(-22.6517953893303,-4.2766658086912,
12.));
#234470=CARTESIAN_POINT('Ctrl Pts',(-22.6382822758172,-4.27105453193004,
0.));
#234471=CARTESIAN_POINT('Ctrl Pts',(-22.6382822758172,-4.27105453193004,
12.));
#234472=CARTESIAN_POINT('Ctrl Pts',(-22.6248965859977,-4.26554467865576,
0.));
#234473=CARTESIAN_POINT('Ctrl Pts',(-22.6248965859977,-4.26554467865576,
12.));
#234474=CARTESIAN_POINT('Ctrl Pts',(-22.6116403184821,-4.26013621588305,
0.));
#234475=CARTESIAN_POINT('Ctrl Pts',(-22.6116403184821,-4.26013621588305,
12.));
#234476=CARTESIAN_POINT('Ctrl Pts',(-22.5985155158636,-4.25482910755481,
0.));
#234477=CARTESIAN_POINT('Ctrl Pts',(-22.5985155158636,-4.25482910755481,
12.));
#234478=CARTESIAN_POINT('Ctrl Pts',(-22.5855242662477,-4.24962331444177,
0.));
#234479=CARTESIAN_POINT('Ctrl Pts',(-22.5855242662477,-4.24962331444177,
12.));
#234480=CARTESIAN_POINT('Ctrl Pts',(-22.572668704992,-4.24451879404851,
0.));
#234481=CARTESIAN_POINT('Ctrl Pts',(-22.572668704992,-4.24451879404851,
12.));
#234482=CARTESIAN_POINT('Ctrl Pts',(-22.5599510166429,-4.23951550052522,
0.));
#234483=CARTESIAN_POINT('Ctrl Pts',(-22.5599510166429,-4.23951550052522,
12.));
#234484=CARTESIAN_POINT('Ctrl Pts',(-22.5473734368086,-4.23461338456712,
0.));
#234485=CARTESIAN_POINT('Ctrl Pts',(-22.5473734368086,-4.23461338456712,
12.));
#234486=CARTESIAN_POINT('Ctrl Pts',(-22.5349382540588,-4.22981239330733,
0.));
#234487=CARTESIAN_POINT('Ctrl Pts',(-22.5349382540588,-4.22981239330733,
12.));
#234488=CARTESIAN_POINT('Ctrl Pts',(-22.5226478117886,-4.22511247020041,
0.));
#234489=CARTESIAN_POINT('Ctrl Pts',(-22.5226478117886,-4.22511247020041,
12.));
#234490=CARTESIAN_POINT('Ctrl Pts',(-22.5105045108881,-4.22051355490196,
0.));
#234491=CARTESIAN_POINT('Ctrl Pts',(-22.5105045108881,-4.22051355490196,
12.));
#234492=CARTESIAN_POINT('Ctrl Pts',(-22.4985108124228,-4.21601558313906,
0.));
#234493=CARTESIAN_POINT('Ctrl Pts',(-22.4985108124228,-4.21601558313906,
12.));
#234494=CARTESIAN_POINT('Ctrl Pts',(-22.4866692403147,-4.21161848657428,
0.));
#234495=CARTESIAN_POINT('Ctrl Pts',(-22.4866692403147,-4.21161848657428,
12.));
#234496=CARTESIAN_POINT('Ctrl Pts',(-22.4749823839917,-4.20732219265649,
0.));
#234497=CARTESIAN_POINT('Ctrl Pts',(-22.4749823839917,-4.20732219265649,
12.));
#234498=CARTESIAN_POINT('Ctrl Pts',(-22.4634529011437,-4.20312662448174,
0.));
#234499=CARTESIAN_POINT('Ctrl Pts',(-22.4634529011437,-4.20312662448174,
12.));
#234500=CARTESIAN_POINT('Ctrl Pts',(-22.4520835205422,-4.19903170066358,
0.));
#234501=CARTESIAN_POINT('Ctrl Pts',(-22.4520835205422,-4.19903170066358,
12.));
#234502=CARTESIAN_POINT('Ctrl Pts',(-22.4408770448917,-4.1950373351886,
0.));
#234503=CARTESIAN_POINT('Ctrl Pts',(-22.4408770448917,-4.1950373351886,
12.));
#234504=CARTESIAN_POINT('Ctrl Pts',(-22.4298363535416,-4.19114343726932,
0.));
#234505=CARTESIAN_POINT('Ctrl Pts',(-22.4298363535416,-4.19114343726932,
12.));
#234506=CARTESIAN_POINT('Ctrl Pts',(-22.4189644056109,-4.18734991117707,
0.));
#234507=CARTESIAN_POINT('Ctrl Pts',(-22.4189644056109,-4.18734991117707,
12.));
#234508=CARTESIAN_POINT('Ctrl Pts',(-22.4082642454448,-4.18365665600839,
0.));
#234509=CARTESIAN_POINT('Ctrl Pts',(-22.4082642454448,-4.18365665600839,
12.));
#234510=CARTESIAN_POINT('Ctrl Pts',(-22.3977390078074,-4.18006356544879,
0.));
#234511=CARTESIAN_POINT('Ctrl Pts',(-22.3977390078074,-4.18006356544879,
12.));
#234512=CARTESIAN_POINT('Ctrl Pts',(-22.3873919231339,-4.17657052752834,
0.));
#234513=CARTESIAN_POINT('Ctrl Pts',(-22.3873919231339,-4.17657052752834,
12.));
#234514=CARTESIAN_POINT('Ctrl Pts',(-22.3772263228624,-4.17317742436162,
0.));
#234515=CARTESIAN_POINT('Ctrl Pts',(-22.3772263228624,-4.17317742436162,
12.));
#234516=CARTESIAN_POINT('Ctrl Pts',(-22.3672456427605,-4.16988413199469,
0.));
#234517=CARTESIAN_POINT('Ctrl Pts',(-22.3672456427605,-4.16988413199469,
12.));
#234518=CARTESIAN_POINT('Ctrl Pts',(-22.3574534257397,-4.16669052026602,
0.));
#234519=CARTESIAN_POINT('Ctrl Pts',(-22.3574534257397,-4.16669052026602,
12.));
#234520=CARTESIAN_POINT('Ctrl Pts',(-22.3478533253886,-4.1635964526318,
0.));
#234521=CARTESIAN_POINT('Ctrl Pts',(-22.3478533253886,-4.1635964526318,
12.));
#234522=CARTESIAN_POINT('Ctrl Pts',(-22.3384491078599,-4.16060178604154,
0.));
#234523=CARTESIAN_POINT('Ctrl Pts',(-22.3384491078599,-4.16060178604154,
12.));
#234524=CARTESIAN_POINT('Ctrl Pts',(-22.3292446628957,-4.15770637047882,
0.));
#234525=CARTESIAN_POINT('Ctrl Pts',(-22.3292446628957,-4.15770637047882,
12.));
#234526=CARTESIAN_POINT('Ctrl Pts',(-22.3202440186979,-4.15491004835278,
0.));
#234527=CARTESIAN_POINT('Ctrl Pts',(-22.3202440186979,-4.15491004835278,
12.));
#234528=CARTESIAN_POINT('Ctrl Pts',(-22.3114513545186,-4.15221265396993,
0.));
#234529=CARTESIAN_POINT('Ctrl Pts',(-22.3114513545186,-4.15221265396993,
12.));
#234530=CARTESIAN_POINT('Ctrl Pts',(-22.3028710166935,-4.14961401285525,
0.));
#234531=CARTESIAN_POINT('Ctrl Pts',(-22.3028710166935,-4.14961401285525,
12.));
#234532=CARTESIAN_POINT('Ctrl Pts',(-22.2945075198468,-4.14711394168559,
0.));
#234533=CARTESIAN_POINT('Ctrl Pts',(-22.2945075198468,-4.14711394168559,
12.));
#234534=CARTESIAN_POINT('Ctrl Pts',(-22.2863655389167,-4.14471224859295,
0.));
#234535=CARTESIAN_POINT('Ctrl Pts',(-22.2863655389167,-4.14471224859295,
12.));
#234536=CARTESIAN_POINT('Ctrl Pts',(-22.2784499072026,-4.14240873321982,
0.));
#234537=CARTESIAN_POINT('Ctrl Pts',(-22.2784499072026,-4.14240873321982,
12.));
#234538=CARTESIAN_POINT('Ctrl Pts',(-22.2707656042456,-4.14020318715988,
0.));
#234539=CARTESIAN_POINT('Ctrl Pts',(-22.2707656042456,-4.14020318715988,
12.));
#234540=CARTESIAN_POINT('Ctrl Pts',(-22.263317791397,-4.13809539255418,
0.));
#234541=CARTESIAN_POINT('Ctrl Pts',(-22.263317791397,-4.13809539255418,
12.));
#234542=CARTESIAN_POINT('Ctrl Pts',(-22.2561118708422,-4.13608511977226,
0.));
#234543=CARTESIAN_POINT('Ctrl Pts',(-22.2561118708422,-4.13608511977226,
12.));
#234544=CARTESIAN_POINT('Ctrl Pts',(-22.2491535317789,-4.13417212558808,
0.));
#234545=CARTESIAN_POINT('Ctrl Pts',(-22.2491535317789,-4.13417212558808,
12.));
#234546=CARTESIAN_POINT('Ctrl Pts',(-22.2424488153523,-4.1323561506016,
0.));
#234547=CARTESIAN_POINT('Ctrl Pts',(-22.2424488153523,-4.1323561506016,
12.));
#234548=CARTESIAN_POINT('Ctrl Pts',(-22.2360040565534,-4.13063692157499,
0.));
#234549=CARTESIAN_POINT('Ctrl Pts',(-22.2360040565534,-4.13063692157499,
12.));
#234550=CARTESIAN_POINT('Ctrl Pts',(-22.2298258043947,-4.12901415463379,
0.));
#234551=CARTESIAN_POINT('Ctrl Pts',(-22.2298258043947,-4.12901415463379,
12.));
#234552=CARTESIAN_POINT('Ctrl Pts',(-22.2239207458781,-4.12748755830099,
0.));
#234553=CARTESIAN_POINT('Ctrl Pts',(-22.2239207458781,-4.12748755830099,
12.));
#234554=CARTESIAN_POINT('Ctrl Pts',(-22.2182956401341,-4.126056836133,0.));
#234555=CARTESIAN_POINT('Ctrl Pts',(-22.2182956401341,-4.126056836133,12.));
#234556=CARTESIAN_POINT('Ctrl Pts',(-22.2129576146671,-4.12472167516602,
0.));
#234557=CARTESIAN_POINT('Ctrl Pts',(-22.2129576146671,-4.12472167516602,
12.));
#234558=CARTESIAN_POINT('Ctrl Pts',(-22.2079143941719,-4.12348173702024,
0.));
#234559=CARTESIAN_POINT('Ctrl Pts',(-22.2079143941719,-4.12348173702024,
12.));
#234560=CARTESIAN_POINT('Ctrl Pts',(-22.2031746532106,-4.12233664408237,
0.));
#234561=CARTESIAN_POINT('Ctrl Pts',(-22.2031746532106,-4.12233664408237,
12.));
#234562=CARTESIAN_POINT('Ctrl Pts',(-22.1987479618246,-4.12128598183533,
0.));
#234563=CARTESIAN_POINT('Ctrl Pts',(-22.1987479618246,-4.12128598183533,
12.));
#234564=CARTESIAN_POINT('Ctrl Pts',(-22.1946440958098,-4.12032932637738,
0.));
#234565=CARTESIAN_POINT('Ctrl Pts',(-22.1946440958098,-4.12032932637738,
12.));
#234566=CARTESIAN_POINT('Ctrl Pts',(-22.1908725908525,-4.11946626228623,
0.));
#234567=CARTESIAN_POINT('Ctrl Pts',(-22.1908725908525,-4.11946626228623,
12.));
#234568=CARTESIAN_POINT('Ctrl Pts',(-22.1874419861496,-4.11869641271752,
0.));
#234569=CARTESIAN_POINT('Ctrl Pts',(-22.1874419861496,-4.11869641271752,
12.));
#234570=CARTESIAN_POINT('Ctrl Pts',(-22.1843613164855,-4.11801938107464,
0.));
#234571=CARTESIAN_POINT('Ctrl Pts',(-22.1843613164855,-4.11801938107464,
12.));
#234572=CARTESIAN_POINT('Ctrl Pts',(-22.1816414985788,-4.11743469691765,
0.));
#234573=CARTESIAN_POINT('Ctrl Pts',(-22.1816414985788,-4.11743469691765,
12.));
#234574=CARTESIAN_POINT('Ctrl Pts',(-22.179297473024,-4.11694173195041,
0.));
#234575=CARTESIAN_POINT('Ctrl Pts',(-22.179297473024,-4.11694173195041,
12.));
#234576=CARTESIAN_POINT('Ctrl Pts',(-22.177347426894,-4.11653973150558,
0.));
#234577=CARTESIAN_POINT('Ctrl Pts',(-22.177347426894,-4.11653973150558,
12.));
#234578=CARTESIAN_POINT('Ctrl Pts',(-22.1758088296598,-4.11622797217066,
0.));
#234579=CARTESIAN_POINT('Ctrl Pts',(-22.1758088296598,-4.11622797217066,
12.));
#234580=CARTESIAN_POINT('Ctrl Pts',(-22.1746949858773,-4.11600589882767,
0.));
#234581=CARTESIAN_POINT('Ctrl Pts',(-22.1746949858773,-4.11600589882767,
12.));
#234582=CARTESIAN_POINT('Ctrl Pts',(-22.174148802123,-4.11589976826061,
0.));
#234583=CARTESIAN_POINT('Ctrl Pts',(-22.174148802123,-4.11589976826061,
12.));
#234584=CARTESIAN_POINT('Ctrl Pts',(-22.1739341411684,-4.1158603587821,
0.));
#234585=CARTESIAN_POINT('Ctrl Pts',(-22.1739341411684,-4.1158603587821,
12.));
#234586=CARTESIAN_POINT('Ctrl Pts',(-22.1738776823239,-4.11585194677412,
0.));
#234587=CARTESIAN_POINT('Ctrl Pts',(-22.1738776823239,-4.11585194677412,
12.));
#234588=CARTESIAN_POINT('Ctrl Pts',(-22.1738711152697,-4.11585220600461,
0.));
#234589=CARTESIAN_POINT('Ctrl Pts',(-22.1738711152697,-4.11585220600461,
12.));
#234590=CARTESIAN_POINT('',(-25.2771067246846,-6.08833931617698,0.));
#234591=CARTESIAN_POINT('Ctrl Pts',(-25.2771067246846,-6.08833931617698,
0.));
#234592=CARTESIAN_POINT('Ctrl Pts',(-25.2729539149479,-6.08441489609824,
0.));
#234593=CARTESIAN_POINT('Ctrl Pts',(-25.2646490489816,-6.07657531787577,
0.));
#234594=CARTESIAN_POINT('Ctrl Pts',(-25.2521940105523,-6.06484373634696,
0.));
#234595=CARTESIAN_POINT('Ctrl Pts',(-25.2355918138798,-6.04925720151412,
0.));
#234596=CARTESIAN_POINT('Ctrl Pts',(-25.2148466201368,-6.02986667390187,
0.));
#234597=CARTESIAN_POINT('Ctrl Pts',(-25.1941090269638,-6.0105688180476,
0.));
#234598=CARTESIAN_POINT('Ctrl Pts',(-25.1733791296154,-5.99136367859838,
0.));
#234599=CARTESIAN_POINT('Ctrl Pts',(-25.1526570863065,-5.97225131495636,
0.));
#234600=CARTESIAN_POINT('Ctrl Pts',(-25.1319431317273,-5.95323180187348,
0.));
#234601=CARTESIAN_POINT('Ctrl Pts',(-25.1112375971182,-5.93430523086776,
0.));
#234602=CARTESIAN_POINT('Ctrl Pts',(-25.0905409050863,-5.91547170844382,
0.));
#234603=CARTESIAN_POINT('Ctrl Pts',(-25.0698535426593,-5.89673135155459,
0.));
#234604=CARTESIAN_POINT('Ctrl Pts',(-25.0491760405965,-5.87808428385329,
0.));
#234605=CARTESIAN_POINT('Ctrl Pts',(-25.0285089498922,-5.8595306315681,
0.));
#234606=CARTESIAN_POINT('Ctrl Pts',(-25.0078528200558,-5.84107051963073,
0.));
#234607=CARTESIAN_POINT('Ctrl Pts',(-24.9872081752709,-5.82270406744214,
0.));
#234608=CARTESIAN_POINT('Ctrl Pts',(-24.9665754954462,-5.80443138549747,
0.));
#234609=CARTESIAN_POINT('Ctrl Pts',(-24.9459552293308,-5.78625257775703,
0.));
#234610=CARTESIAN_POINT('Ctrl Pts',(-24.9253478043632,-5.76816774342236,
0.));
#234611=CARTESIAN_POINT('Ctrl Pts',(-24.9047536376467,-5.75017697890813,
0.));
#234612=CARTESIAN_POINT('Ctrl Pts',(-24.8841731467219,-5.73228037976926,
0.));
#234613=CARTESIAN_POINT('Ctrl Pts',(-24.8636067597677,-5.71447804252019,
0.));
#234614=CARTESIAN_POINT('Ctrl Pts',(-24.8430549277634,-5.69677006679429,
0.));
#234615=CARTESIAN_POINT('Ctrl Pts',(-24.822518122386,-5.67915655496524,
0.));
#234616=CARTESIAN_POINT('Ctrl Pts',(-24.8019968304618,-5.66163761114903,
0.));
#234617=CARTESIAN_POINT('Ctrl Pts',(-24.7814915496728,-5.64421334042247,
0.));
#234618=CARTESIAN_POINT('Ctrl Pts',(-24.76100278357,-5.62688384790919,0.));
#234619=CARTESIAN_POINT('Ctrl Pts',(-24.7405310372736,-5.60964923798495,
0.));
#234620=CARTESIAN_POINT('Ctrl Pts',(-24.7200768119079,-5.59250961323995,
0.));
#234621=CARTESIAN_POINT('Ctrl Pts',(-24.6996406035507,-5.57546507427766,
0.));
#234622=CARTESIAN_POINT('Ctrl Pts',(-24.6792229061785,-5.55851572025389,
0.));
#234623=CARTESIAN_POINT('Ctrl Pts',(-24.6588242134733,-5.54166164919593,
0.));
#234624=CARTESIAN_POINT('Ctrl Pts',(-24.6384450211466,-5.52490295840996,
0.));
#234625=CARTESIAN_POINT('Ctrl Pts',(-24.618085828918,-5.50823974481959,
0.));
#234626=CARTESIAN_POINT('Ctrl Pts',(-24.5977471429365,-5.49167210537235,
0.));
#234627=CARTESIAN_POINT('Ctrl Pts',(-24.5774294770329,-5.47520013724403,
0.));
#234628=CARTESIAN_POINT('Ctrl Pts',(-24.5571333514841,-5.45882393762244,
0.));
#234629=CARTESIAN_POINT('Ctrl Pts',(-24.5368592922861,-5.44254360356865,
0.));
#234630=CARTESIAN_POINT('Ctrl Pts',(-24.5166078302107,-5.42635923183411,
0.));
#234631=CARTESIAN_POINT('Ctrl Pts',(-24.4963794999831,-5.41027091869242,
0.));
#234632=CARTESIAN_POINT('Ctrl Pts',(-24.4761748393322,-5.3942787597383,
0.));
#234633=CARTESIAN_POINT('Ctrl Pts',(-24.4559943883159,-5.37838284973706,
0.));
#234634=CARTESIAN_POINT('Ctrl Pts',(-24.4358386899152,-5.36258328273639,
0.));
#234635=CARTESIAN_POINT('Ctrl Pts',(-24.4157082904615,-5.34688015213546,
0.));
#234636=CARTESIAN_POINT('Ctrl Pts',(-24.3956037401293,-5.33127355076036,
0.));
#234637=CARTESIAN_POINT('Ctrl Pts',(-24.3755255933917,-5.31576357092524,
0.));
#234638=CARTESIAN_POINT('Ctrl Pts',(-24.3554744095075,-5.30035030449058,
0.));
#234639=CARTESIAN_POINT('Ctrl Pts',(-24.3354507529415,-5.28503384290644,
0.));
#234640=CARTESIAN_POINT('Ctrl Pts',(-24.3154551932222,-5.26981427718796,
0.));
#234641=CARTESIAN_POINT('Ctrl Pts',(-24.2954883048448,-5.25469169788856,
0.));
#234642=CARTESIAN_POINT('Ctrl Pts',(-24.2755506671526,-5.23966619506289,
0.));
#234643=CARTESIAN_POINT('Ctrl Pts',(-24.2556428642294,-5.22473785822441,
0.));
#234644=CARTESIAN_POINT('Ctrl Pts',(-24.2357654847765,-5.20990677629173,
0.));
#234645=CARTESIAN_POINT('Ctrl Pts',(-24.215919122017,-5.19517303753643,
0.));
#234646=CARTESIAN_POINT('Ctrl Pts',(-24.1961043738754,-5.18053672961392,
0.));
#234647=CARTESIAN_POINT('Ctrl Pts',(-24.1763218431343,-5.16599793957979,
0.));
#234648=CARTESIAN_POINT('Ctrl Pts',(-24.156572137597,-5.15155675390075,
0.));
#234649=CARTESIAN_POINT('Ctrl Pts',(-24.1368558702443,-5.13721325845744,
0.));
#234650=CARTESIAN_POINT('Ctrl Pts',(-24.117173659394,-5.12296753853859,
0.));
#234651=CARTESIAN_POINT('Ctrl Pts',(-24.0975261288446,-5.10881967883132,
0.));
#234652=CARTESIAN_POINT('Ctrl Pts',(-24.0779139079266,-5.09476976342625,
0.));
#234653=CARTESIAN_POINT('Ctrl Pts',(-24.0583376315638,-5.08081787581276,
0.));
#234654=CARTESIAN_POINT('Ctrl Pts',(-24.0387979403268,-5.06696409886641,
0.));
#234655=CARTESIAN_POINT('Ctrl Pts',(-24.0192954804896,-5.05320851483065,
0.));
#234656=CARTESIAN_POINT('Ctrl Pts',(-23.9998309040746,-5.03955120528521,
0.));
#234657=CARTESIAN_POINT('Ctrl Pts',(-23.9804048689227,-5.02599225112454,
0.));
#234658=CARTESIAN_POINT('Ctrl Pts',(-23.9610180388271,-5.01253173257453,
0.));
#234659=CARTESIAN_POINT('Ctrl Pts',(-23.9416710836529,-4.99916972919306,
0.));
#234660=CARTESIAN_POINT('Ctrl Pts',(-23.9223646794592,-4.98590631986532,
0.));
#234661=CARTESIAN_POINT('Ctrl Pts',(-23.9030995086163,-4.97274158279226,
0.));
#234662=CARTESIAN_POINT('Ctrl Pts',(-23.8838762599218,-4.9596755954656,
0.));
#234663=CARTESIAN_POINT('Ctrl Pts',(-23.8646956287168,-4.9467084346586,
0.));
#234664=CARTESIAN_POINT('Ctrl Pts',(-23.8455583170057,-4.93384017643432,
0.));
#234665=CARTESIAN_POINT('Ctrl Pts',(-23.8264650335717,-4.92107089613969,
0.));
#234666=CARTESIAN_POINT('Ctrl Pts',(-23.8074164940896,-4.90840066839344,
0.));
#234667=CARTESIAN_POINT('Ctrl Pts',(-23.7884134212384,-4.89582956706775,
0.));
#234668=CARTESIAN_POINT('Ctrl Pts',(-23.7694565448049,-4.88335766525573,
0.));
#234669=CARTESIAN_POINT('Ctrl Pts',(-23.7505466018245,-4.87098503527152,
0.));
#234670=CARTESIAN_POINT('Ctrl Pts',(-23.7316843367313,-4.85871174865499,
0.));
#234671=CARTESIAN_POINT('Ctrl Pts',(-23.7128705015017,-4.84653787616425,
0.));
#234672=CARTESIAN_POINT('Ctrl Pts',(-23.6941058557971,-4.83446348776265,
0.));
#234673=CARTESIAN_POINT('Ctrl Pts',(-23.675391167102,-4.82248865259562,
0.));
#234674=CARTESIAN_POINT('Ctrl Pts',(-23.6567272108628,-4.81061343896432,
0.));
#234675=CARTESIAN_POINT('Ctrl Pts',(-23.6381147706579,-4.7988379143322,
0.));
#234676=CARTESIAN_POINT('Ctrl Pts',(-23.6195546383624,-4.78716214532098,
0.));
#234677=CARTESIAN_POINT('Ctrl Pts',(-23.6010476143099,-4.77558619769872,
0.));
#234678=CARTESIAN_POINT('Ctrl Pts',(-23.5825945074535,-4.76411013636251,
0.));
#234679=CARTESIAN_POINT('Ctrl Pts',(-23.5641961355168,-4.75273402530617,
0.));
#234680=CARTESIAN_POINT('Ctrl Pts',(-23.545853325171,-4.74145792760698,
0.));
#234681=CARTESIAN_POINT('Ctrl Pts',(-23.5275669122372,-4.7302819054303,
0.));
#234682=CARTESIAN_POINT('Ctrl Pts',(-23.509337741878,-4.71920602001901,
0.));
#234683=CARTESIAN_POINT('Ctrl Pts',(-23.491166668789,-4.70823033167818,
0.));
#234684=CARTESIAN_POINT('Ctrl Pts',(-23.4730545573853,-4.69735489975024,
0.));
#234685=CARTESIAN_POINT('Ctrl Pts',(-23.455002281986,-4.68657978258303,
0.));
#234686=CARTESIAN_POINT('Ctrl Pts',(-23.4370107270451,-4.67590503753058,
0.));
#234687=CARTESIAN_POINT('Ctrl Pts',(-23.4190807873803,-4.6653307209467,
0.));
#234688=CARTESIAN_POINT('Ctrl Pts',(-23.4012133683959,-4.65485688816924,
0.));
#234689=CARTESIAN_POINT('Ctrl Pts',(-23.3834093863068,-4.6444835934993,
0.));
#234690=CARTESIAN_POINT('Ctrl Pts',(-23.3656697683489,-4.63421089016541,
0.));
#234691=CARTESIAN_POINT('Ctrl Pts',(-23.3479954530272,-4.62403883030805,
0.));
#234692=CARTESIAN_POINT('Ctrl Pts',(-23.3303873903938,-4.6139674649783,
0.));
#234693=CARTESIAN_POINT('Ctrl Pts',(-23.3128465423115,-4.60399684412163,
0.));
#234694=CARTESIAN_POINT('Ctrl Pts',(-23.2953738827191,-4.5941270165575,
0.));
#234695=CARTESIAN_POINT('Ctrl Pts',(-23.2779703978876,-4.5843580299469,
0.));
#234696=CARTESIAN_POINT('Ctrl Pts',(-23.2606370866866,-4.57468993076097,
0.));
#234697=CARTESIAN_POINT('Ctrl Pts',(-23.2433749609131,-4.56512276427839,
0.));
#234698=CARTESIAN_POINT('Ctrl Pts',(-23.2261850456064,-4.55565657456975,
0.));
#234699=CARTESIAN_POINT('Ctrl Pts',(-23.2090683793629,-4.54629140447544,
0.));
#234700=CARTESIAN_POINT('Ctrl Pts',(-23.1920260146465,-4.53702729557566,
0.));
#234701=CARTESIAN_POINT('Ctrl Pts',(-23.1750590180908,-4.52786428815014,
0.));
#234702=CARTESIAN_POINT('Ctrl Pts',(-23.1581684708761,-4.51880242116748,
0.));
#234703=CARTESIAN_POINT('Ctrl Pts',(-23.1413554691123,-4.5098417322706,
0.));
#234704=CARTESIAN_POINT('Ctrl Pts',(-23.1246211242115,-4.50098225775171,
0.));
#234705=CARTESIAN_POINT('Ctrl Pts',(-23.1079665632636,-4.49222403252216,
0.));
#234706=CARTESIAN_POINT('Ctrl Pts',(-23.0913929293922,-4.48356709006788,
0.));
#234707=CARTESIAN_POINT('Ctrl Pts',(-23.0749013821881,-4.47501146242856,
0.));
#234708=CARTESIAN_POINT('Ctrl Pts',(-23.0584930981732,-4.4665571801823,
0.));
#234709=CARTESIAN_POINT('Ctrl Pts',(-23.0421692712467,-4.45820427241683,
0.));
#234710=CARTESIAN_POINT('Ctrl Pts',(-23.0259311131392,-4.44995276669686,
0.));
#234711=CARTESIAN_POINT('Ctrl Pts',(-23.0097798538395,-4.44180268901643,
0.));
#234712=CARTESIAN_POINT('Ctrl Pts',(-22.9937167421006,-4.43375406376879,
0.));
#234713=CARTESIAN_POINT('Ctrl Pts',(-22.977743046002,-4.42580691372751,
0.));
#234714=CARTESIAN_POINT('Ctrl Pts',(-22.9618600534866,-4.41796126001302,
0.));
#234715=CARTESIAN_POINT('Ctrl Pts',(-22.9460690729093,-4.41021712205553,
0.));
#234716=CARTESIAN_POINT('Ctrl Pts',(-22.930371433555,-4.40257451754323,
0.));
#234717=CARTESIAN_POINT('Ctrl Pts',(-22.9147684862426,-4.39503346238473,
0.));
#234718=CARTESIAN_POINT('Ctrl Pts',(-22.8992616040108,-4.38759397068406,
0.));
#234719=CARTESIAN_POINT('Ctrl Pts',(-22.8838521827701,-4.38025605470093,
0.));
#234720=CARTESIAN_POINT('Ctrl Pts',(-22.8685416419725,-4.37301972480745,
0.));
#234721=CARTESIAN_POINT('Ctrl Pts',(-22.8533314252422,-4.36588498942997,
0.));
#234722=CARTESIAN_POINT('Ctrl Pts',(-22.8382230011184,-4.35885185500546,
0.));
#234723=CARTESIAN_POINT('Ctrl Pts',(-22.8232178638876,-4.35192032594791,
0.));
#234724=CARTESIAN_POINT('Ctrl Pts',(-22.8083175343791,-4.34509040460062,
0.));
#234725=CARTESIAN_POINT('Ctrl Pts',(-22.7935235607806,-4.33836209118446,
0.));
#234726=CARTESIAN_POINT('Ctrl Pts',(-22.7788375194076,-4.3317353837319,
0.));
#234727=CARTESIAN_POINT('Ctrl Pts',(-22.7642610156475,-4.32521027803754,
0.));
#234728=CARTESIAN_POINT('Ctrl Pts',(-22.7497956849848,-4.31878676761235,
0.));
#234729=CARTESIAN_POINT('Ctrl Pts',(-22.7354431939926,-4.31246484362549,
0.));
#234730=CARTESIAN_POINT('Ctrl Pts',(-22.7212052413386,-4.30624449484069,
0.));
#234731=CARTESIAN_POINT('Ctrl Pts',(-22.7070835587564,-4.3001257075406,
0.));
#234732=CARTESIAN_POINT('Ctrl Pts',(-22.6930799122548,-4.29410846547056,
0.));
#234733=CARTESIAN_POINT('Ctrl Pts',(-22.6791961033538,-4.28819274977763,
0.));
#234734=CARTESIAN_POINT('Ctrl Pts',(-22.6654339703109,-4.28237853894059,
0.));
#234735=CARTESIAN_POINT('Ctrl Pts',(-22.6517953893303,-4.2766658086912,
0.));
#234736=CARTESIAN_POINT('Ctrl Pts',(-22.6382822758172,-4.27105453193004,
0.));
#234737=CARTESIAN_POINT('Ctrl Pts',(-22.6248965859977,-4.26554467865576,
0.));
#234738=CARTESIAN_POINT('Ctrl Pts',(-22.6116403184821,-4.26013621588305,
0.));
#234739=CARTESIAN_POINT('Ctrl Pts',(-22.5985155158636,-4.25482910755481,
0.));
#234740=CARTESIAN_POINT('Ctrl Pts',(-22.5855242662477,-4.24962331444177,
0.));
#234741=CARTESIAN_POINT('Ctrl Pts',(-22.572668704992,-4.24451879404851,
0.));
#234742=CARTESIAN_POINT('Ctrl Pts',(-22.5599510166429,-4.23951550052522,
0.));
#234743=CARTESIAN_POINT('Ctrl Pts',(-22.5473734368086,-4.23461338456712,
0.));
#234744=CARTESIAN_POINT('Ctrl Pts',(-22.5349382540588,-4.22981239330733,
0.));
#234745=CARTESIAN_POINT('Ctrl Pts',(-22.5226478117886,-4.22511247020041,
0.));
#234746=CARTESIAN_POINT('Ctrl Pts',(-22.5105045108881,-4.22051355490196,
0.));
#234747=CARTESIAN_POINT('Ctrl Pts',(-22.4985108124228,-4.21601558313906,
0.));
#234748=CARTESIAN_POINT('Ctrl Pts',(-22.4866692403147,-4.21161848657428,
0.));
#234749=CARTESIAN_POINT('Ctrl Pts',(-22.4749823839917,-4.20732219265649,
0.));
#234750=CARTESIAN_POINT('Ctrl Pts',(-22.4634529011437,-4.20312662448174,
0.));
#234751=CARTESIAN_POINT('Ctrl Pts',(-22.4520835205422,-4.19903170066358,
0.));
#234752=CARTESIAN_POINT('Ctrl Pts',(-22.4408770448917,-4.1950373351886,
0.));
#234753=CARTESIAN_POINT('Ctrl Pts',(-22.4298363535416,-4.19114343726932,
0.));
#234754=CARTESIAN_POINT('Ctrl Pts',(-22.4189644056109,-4.18734991117707,
0.));
#234755=CARTESIAN_POINT('Ctrl Pts',(-22.4082642454448,-4.18365665600839,
0.));
#234756=CARTESIAN_POINT('Ctrl Pts',(-22.3977390078074,-4.18006356544879,
0.));
#234757=CARTESIAN_POINT('Ctrl Pts',(-22.3873919231339,-4.17657052752834,
0.));
#234758=CARTESIAN_POINT('Ctrl Pts',(-22.3772263228624,-4.17317742436162,
0.));
#234759=CARTESIAN_POINT('Ctrl Pts',(-22.3672456427605,-4.16988413199469,
0.));
#234760=CARTESIAN_POINT('Ctrl Pts',(-22.3574534257397,-4.16669052026602,
0.));
#234761=CARTESIAN_POINT('Ctrl Pts',(-22.3478533253886,-4.1635964526318,
0.));
#234762=CARTESIAN_POINT('Ctrl Pts',(-22.3384491078599,-4.16060178604154,
0.));
#234763=CARTESIAN_POINT('Ctrl Pts',(-22.3292446628957,-4.15770637047882,
0.));
#234764=CARTESIAN_POINT('Ctrl Pts',(-22.3202440186979,-4.15491004835278,
0.));
#234765=CARTESIAN_POINT('Ctrl Pts',(-22.3114513545186,-4.15221265396993,
0.));
#234766=CARTESIAN_POINT('Ctrl Pts',(-22.3028710166935,-4.14961401285525,
0.));
#234767=CARTESIAN_POINT('Ctrl Pts',(-22.2945075198468,-4.14711394168559,
0.));
#234768=CARTESIAN_POINT('Ctrl Pts',(-22.2863655389167,-4.14471224859295,
0.));
#234769=CARTESIAN_POINT('Ctrl Pts',(-22.2784499072026,-4.14240873321982,
0.));
#234770=CARTESIAN_POINT('Ctrl Pts',(-22.2707656042456,-4.14020318715988,
0.));
#234771=CARTESIAN_POINT('Ctrl Pts',(-22.263317791397,-4.13809539255418,
0.));
#234772=CARTESIAN_POINT('Ctrl Pts',(-22.2561118708422,-4.13608511977226,
0.));
#234773=CARTESIAN_POINT('Ctrl Pts',(-22.2491535317789,-4.13417212558808,
0.));
#234774=CARTESIAN_POINT('Ctrl Pts',(-22.2424488153523,-4.1323561506016,
0.));
#234775=CARTESIAN_POINT('Ctrl Pts',(-22.2360040565534,-4.13063692157499,
0.));
#234776=CARTESIAN_POINT('Ctrl Pts',(-22.2298258043947,-4.12901415463379,
0.));
#234777=CARTESIAN_POINT('Ctrl Pts',(-22.2239207458781,-4.12748755830099,
0.));
#234778=CARTESIAN_POINT('Ctrl Pts',(-22.2182956401341,-4.126056836133,0.));
#234779=CARTESIAN_POINT('Ctrl Pts',(-22.2129576146671,-4.12472167516602,
0.));
#234780=CARTESIAN_POINT('Ctrl Pts',(-22.2079143941719,-4.12348173702024,
0.));
#234781=CARTESIAN_POINT('Ctrl Pts',(-22.2031746532106,-4.12233664408237,
0.));
#234782=CARTESIAN_POINT('Ctrl Pts',(-22.1987479618246,-4.12128598183533,
0.));
#234783=CARTESIAN_POINT('Ctrl Pts',(-22.1946440958098,-4.12032932637738,
0.));
#234784=CARTESIAN_POINT('Ctrl Pts',(-22.1908725908525,-4.11946626228623,
0.));
#234785=CARTESIAN_POINT('Ctrl Pts',(-22.1874419861496,-4.11869641271752,
0.));
#234786=CARTESIAN_POINT('Ctrl Pts',(-22.1843613164855,-4.11801938107464,
0.));
#234787=CARTESIAN_POINT('Ctrl Pts',(-22.1816414985788,-4.11743469691765,
0.));
#234788=CARTESIAN_POINT('Ctrl Pts',(-22.179297473024,-4.11694173195041,
0.));
#234789=CARTESIAN_POINT('Ctrl Pts',(-22.177347426894,-4.11653973150558,
0.));
#234790=CARTESIAN_POINT('Ctrl Pts',(-22.1758088296598,-4.11622797217066,
0.));
#234791=CARTESIAN_POINT('Ctrl Pts',(-22.1746949858773,-4.11600589882767,
0.));
#234792=CARTESIAN_POINT('Ctrl Pts',(-22.174148802123,-4.11589976826061,
0.));
#234793=CARTESIAN_POINT('Ctrl Pts',(-22.1739341411684,-4.1158603587821,
0.));
#234794=CARTESIAN_POINT('Ctrl Pts',(-22.1738776823239,-4.11585194677412,
0.));
#234795=CARTESIAN_POINT('Ctrl Pts',(-22.1738711152697,-4.11585220600461,
0.));
#234796=CARTESIAN_POINT('',(-25.2771067246846,-6.08833931617698,12.));
#234797=CARTESIAN_POINT('',(-25.2771067246846,-6.08833931617698,0.));
#234798=CARTESIAN_POINT('Ctrl Pts',(-22.1738711152697,-4.11585220600461,
12.));
#234799=CARTESIAN_POINT('Ctrl Pts',(-22.1738776823239,-4.11585194677412,
12.));
#234800=CARTESIAN_POINT('Ctrl Pts',(-22.1739341411684,-4.1158603587821,
12.));
#234801=CARTESIAN_POINT('Ctrl Pts',(-22.174148802123,-4.11589976826061,
12.));
#234802=CARTESIAN_POINT('Ctrl Pts',(-22.1746949858773,-4.11600589882767,
12.));
#234803=CARTESIAN_POINT('Ctrl Pts',(-22.1758088296598,-4.11622797217066,
12.));
#234804=CARTESIAN_POINT('Ctrl Pts',(-22.177347426894,-4.11653973150558,
12.));
#234805=CARTESIAN_POINT('Ctrl Pts',(-22.179297473024,-4.11694173195041,
12.));
#234806=CARTESIAN_POINT('Ctrl Pts',(-22.1816414985788,-4.11743469691765,
12.));
#234807=CARTESIAN_POINT('Ctrl Pts',(-22.1843613164855,-4.11801938107464,
12.));
#234808=CARTESIAN_POINT('Ctrl Pts',(-22.1874419861496,-4.11869641271752,
12.));
#234809=CARTESIAN_POINT('Ctrl Pts',(-22.1908725908525,-4.11946626228623,
12.));
#234810=CARTESIAN_POINT('Ctrl Pts',(-22.1946440958098,-4.12032932637738,
12.));
#234811=CARTESIAN_POINT('Ctrl Pts',(-22.1987479618246,-4.12128598183533,
12.));
#234812=CARTESIAN_POINT('Ctrl Pts',(-22.2031746532106,-4.12233664408237,
12.));
#234813=CARTESIAN_POINT('Ctrl Pts',(-22.2079143941719,-4.12348173702024,
12.));
#234814=CARTESIAN_POINT('Ctrl Pts',(-22.2129576146671,-4.12472167516602,
12.));
#234815=CARTESIAN_POINT('Ctrl Pts',(-22.2182956401341,-4.126056836133,12.));
#234816=CARTESIAN_POINT('Ctrl Pts',(-22.2239207458781,-4.12748755830099,
12.));
#234817=CARTESIAN_POINT('Ctrl Pts',(-22.2298258043947,-4.12901415463379,
12.));
#234818=CARTESIAN_POINT('Ctrl Pts',(-22.2360040565534,-4.13063692157499,
12.));
#234819=CARTESIAN_POINT('Ctrl Pts',(-22.2424488153523,-4.1323561506016,
12.));
#234820=CARTESIAN_POINT('Ctrl Pts',(-22.2491535317789,-4.13417212558808,
12.));
#234821=CARTESIAN_POINT('Ctrl Pts',(-22.2561118708422,-4.13608511977226,
12.));
#234822=CARTESIAN_POINT('Ctrl Pts',(-22.263317791397,-4.13809539255418,
12.));
#234823=CARTESIAN_POINT('Ctrl Pts',(-22.2707656042456,-4.14020318715988,
12.));
#234824=CARTESIAN_POINT('Ctrl Pts',(-22.2784499072026,-4.14240873321982,
12.));
#234825=CARTESIAN_POINT('Ctrl Pts',(-22.2863655389167,-4.14471224859295,
12.));
#234826=CARTESIAN_POINT('Ctrl Pts',(-22.2945075198468,-4.14711394168559,
12.));
#234827=CARTESIAN_POINT('Ctrl Pts',(-22.3028710166935,-4.14961401285525,
12.));
#234828=CARTESIAN_POINT('Ctrl Pts',(-22.3114513545186,-4.15221265396993,
12.));
#234829=CARTESIAN_POINT('Ctrl Pts',(-22.3202440186979,-4.15491004835278,
12.));
#234830=CARTESIAN_POINT('Ctrl Pts',(-22.3292446628957,-4.15770637047882,
12.));
#234831=CARTESIAN_POINT('Ctrl Pts',(-22.3384491078599,-4.16060178604154,
12.));
#234832=CARTESIAN_POINT('Ctrl Pts',(-22.3478533253886,-4.1635964526318,
12.));
#234833=CARTESIAN_POINT('Ctrl Pts',(-22.3574534257397,-4.16669052026602,
12.));
#234834=CARTESIAN_POINT('Ctrl Pts',(-22.3672456427605,-4.16988413199469,
12.));
#234835=CARTESIAN_POINT('Ctrl Pts',(-22.3772263228624,-4.17317742436162,
12.));
#234836=CARTESIAN_POINT('Ctrl Pts',(-22.3873919231339,-4.17657052752834,
12.));
#234837=CARTESIAN_POINT('Ctrl Pts',(-22.3977390078074,-4.18006356544879,
12.));
#234838=CARTESIAN_POINT('Ctrl Pts',(-22.4082642454448,-4.18365665600839,
12.));
#234839=CARTESIAN_POINT('Ctrl Pts',(-22.4189644056109,-4.18734991117707,
12.));
#234840=CARTESIAN_POINT('Ctrl Pts',(-22.4298363535416,-4.19114343726932,
12.));
#234841=CARTESIAN_POINT('Ctrl Pts',(-22.4408770448917,-4.1950373351886,
12.));
#234842=CARTESIAN_POINT('Ctrl Pts',(-22.4520835205422,-4.19903170066358,
12.));
#234843=CARTESIAN_POINT('Ctrl Pts',(-22.4634529011437,-4.20312662448174,
12.));
#234844=CARTESIAN_POINT('Ctrl Pts',(-22.4749823839917,-4.20732219265649,
12.));
#234845=CARTESIAN_POINT('Ctrl Pts',(-22.4866692403147,-4.21161848657428,
12.));
#234846=CARTESIAN_POINT('Ctrl Pts',(-22.4985108124228,-4.21601558313906,
12.));
#234847=CARTESIAN_POINT('Ctrl Pts',(-22.5105045108881,-4.22051355490196,
12.));
#234848=CARTESIAN_POINT('Ctrl Pts',(-22.5226478117886,-4.22511247020041,
12.));
#234849=CARTESIAN_POINT('Ctrl Pts',(-22.5349382540588,-4.22981239330733,
12.));
#234850=CARTESIAN_POINT('Ctrl Pts',(-22.5473734368086,-4.23461338456712,
12.));
#234851=CARTESIAN_POINT('Ctrl Pts',(-22.5599510166429,-4.23951550052522,
12.));
#234852=CARTESIAN_POINT('Ctrl Pts',(-22.572668704992,-4.24451879404851,
12.));
#234853=CARTESIAN_POINT('Ctrl Pts',(-22.5855242662477,-4.24962331444177,
12.));
#234854=CARTESIAN_POINT('Ctrl Pts',(-22.5985155158636,-4.25482910755481,
12.));
#234855=CARTESIAN_POINT('Ctrl Pts',(-22.6116403184821,-4.26013621588305,
12.));
#234856=CARTESIAN_POINT('Ctrl Pts',(-22.6248965859977,-4.26554467865576,
12.));
#234857=CARTESIAN_POINT('Ctrl Pts',(-22.6382822758172,-4.27105453193004,
12.));
#234858=CARTESIAN_POINT('Ctrl Pts',(-22.6517953893303,-4.2766658086912,
12.));
#234859=CARTESIAN_POINT('Ctrl Pts',(-22.6654339703109,-4.28237853894059,
12.));
#234860=CARTESIAN_POINT('Ctrl Pts',(-22.6791961033538,-4.28819274977763,
12.));
#234861=CARTESIAN_POINT('Ctrl Pts',(-22.6930799122548,-4.29410846547056,
12.));
#234862=CARTESIAN_POINT('Ctrl Pts',(-22.7070835587564,-4.3001257075406,
12.));
#234863=CARTESIAN_POINT('Ctrl Pts',(-22.7212052413386,-4.30624449484069,
12.));
#234864=CARTESIAN_POINT('Ctrl Pts',(-22.7354431939926,-4.31246484362549,
12.));
#234865=CARTESIAN_POINT('Ctrl Pts',(-22.7497956849848,-4.31878676761235,
12.));
#234866=CARTESIAN_POINT('Ctrl Pts',(-22.7642610156475,-4.32521027803754,
12.));
#234867=CARTESIAN_POINT('Ctrl Pts',(-22.7788375194076,-4.3317353837319,
12.));
#234868=CARTESIAN_POINT('Ctrl Pts',(-22.7935235607806,-4.33836209118446,
12.));
#234869=CARTESIAN_POINT('Ctrl Pts',(-22.8083175343791,-4.34509040460062,
12.));
#234870=CARTESIAN_POINT('Ctrl Pts',(-22.8232178638876,-4.35192032594791,
12.));
#234871=CARTESIAN_POINT('Ctrl Pts',(-22.8382230011184,-4.35885185500546,
12.));
#234872=CARTESIAN_POINT('Ctrl Pts',(-22.8533314252422,-4.36588498942997,
12.));
#234873=CARTESIAN_POINT('Ctrl Pts',(-22.8685416419725,-4.37301972480745,
12.));
#234874=CARTESIAN_POINT('Ctrl Pts',(-22.8838521827701,-4.38025605470093,
12.));
#234875=CARTESIAN_POINT('Ctrl Pts',(-22.8992616040108,-4.38759397068406,
12.));
#234876=CARTESIAN_POINT('Ctrl Pts',(-22.9147684862426,-4.39503346238473,
12.));
#234877=CARTESIAN_POINT('Ctrl Pts',(-22.930371433555,-4.40257451754323,
12.));
#234878=CARTESIAN_POINT('Ctrl Pts',(-22.9460690729093,-4.41021712205553,
12.));
#234879=CARTESIAN_POINT('Ctrl Pts',(-22.9618600534866,-4.41796126001302,
12.));
#234880=CARTESIAN_POINT('Ctrl Pts',(-22.977743046002,-4.42580691372751,
12.));
#234881=CARTESIAN_POINT('Ctrl Pts',(-22.9937167421006,-4.43375406376879,
12.));
#234882=CARTESIAN_POINT('Ctrl Pts',(-23.0097798538395,-4.44180268901643,
12.));
#234883=CARTESIAN_POINT('Ctrl Pts',(-23.0259311131392,-4.44995276669686,
12.));
#234884=CARTESIAN_POINT('Ctrl Pts',(-23.0421692712467,-4.45820427241683,
12.));
#234885=CARTESIAN_POINT('Ctrl Pts',(-23.0584930981732,-4.4665571801823,
12.));
#234886=CARTESIAN_POINT('Ctrl Pts',(-23.0749013821881,-4.47501146242856,
12.));
#234887=CARTESIAN_POINT('Ctrl Pts',(-23.0913929293922,-4.48356709006788,
12.));
#234888=CARTESIAN_POINT('Ctrl Pts',(-23.1079665632636,-4.49222403252216,
12.));
#234889=CARTESIAN_POINT('Ctrl Pts',(-23.1246211242115,-4.50098225775171,
12.));
#234890=CARTESIAN_POINT('Ctrl Pts',(-23.1413554691123,-4.5098417322706,
12.));
#234891=CARTESIAN_POINT('Ctrl Pts',(-23.1581684708761,-4.51880242116748,
12.));
#234892=CARTESIAN_POINT('Ctrl Pts',(-23.1750590180908,-4.52786428815014,
12.));
#234893=CARTESIAN_POINT('Ctrl Pts',(-23.1920260146465,-4.53702729557566,
12.));
#234894=CARTESIAN_POINT('Ctrl Pts',(-23.2090683793629,-4.54629140447544,
12.));
#234895=CARTESIAN_POINT('Ctrl Pts',(-23.2261850456064,-4.55565657456975,
12.));
#234896=CARTESIAN_POINT('Ctrl Pts',(-23.2433749609131,-4.56512276427839,
12.));
#234897=CARTESIAN_POINT('Ctrl Pts',(-23.2606370866866,-4.57468993076097,
12.));
#234898=CARTESIAN_POINT('Ctrl Pts',(-23.2779703978876,-4.5843580299469,
12.));
#234899=CARTESIAN_POINT('Ctrl Pts',(-23.2953738827191,-4.5941270165575,
12.));
#234900=CARTESIAN_POINT('Ctrl Pts',(-23.3128465423115,-4.60399684412163,
12.));
#234901=CARTESIAN_POINT('Ctrl Pts',(-23.3303873903938,-4.6139674649783,
12.));
#234902=CARTESIAN_POINT('Ctrl Pts',(-23.3479954530272,-4.62403883030805,
12.));
#234903=CARTESIAN_POINT('Ctrl Pts',(-23.3656697683489,-4.63421089016541,
12.));
#234904=CARTESIAN_POINT('Ctrl Pts',(-23.3834093863068,-4.6444835934993,
12.));
#234905=CARTESIAN_POINT('Ctrl Pts',(-23.4012133683959,-4.65485688816924,
12.));
#234906=CARTESIAN_POINT('Ctrl Pts',(-23.4190807873803,-4.6653307209467,
12.));
#234907=CARTESIAN_POINT('Ctrl Pts',(-23.4370107270451,-4.67590503753058,
12.));
#234908=CARTESIAN_POINT('Ctrl Pts',(-23.455002281986,-4.68657978258303,
12.));
#234909=CARTESIAN_POINT('Ctrl Pts',(-23.4730545573853,-4.69735489975024,
12.));
#234910=CARTESIAN_POINT('Ctrl Pts',(-23.491166668789,-4.70823033167818,
12.));
#234911=CARTESIAN_POINT('Ctrl Pts',(-23.509337741878,-4.71920602001901,
12.));
#234912=CARTESIAN_POINT('Ctrl Pts',(-23.5275669122372,-4.7302819054303,
12.));
#234913=CARTESIAN_POINT('Ctrl Pts',(-23.545853325171,-4.74145792760698,
12.));
#234914=CARTESIAN_POINT('Ctrl Pts',(-23.5641961355168,-4.75273402530617,
12.));
#234915=CARTESIAN_POINT('Ctrl Pts',(-23.5825945074535,-4.76411013636251,
12.));
#234916=CARTESIAN_POINT('Ctrl Pts',(-23.6010476143099,-4.77558619769872,
12.));
#234917=CARTESIAN_POINT('Ctrl Pts',(-23.6195546383624,-4.78716214532098,
12.));
#234918=CARTESIAN_POINT('Ctrl Pts',(-23.6381147706579,-4.7988379143322,
12.));
#234919=CARTESIAN_POINT('Ctrl Pts',(-23.6567272108628,-4.81061343896432,
12.));
#234920=CARTESIAN_POINT('Ctrl Pts',(-23.675391167102,-4.82248865259562,
12.));
#234921=CARTESIAN_POINT('Ctrl Pts',(-23.6941058557971,-4.83446348776265,
12.));
#234922=CARTESIAN_POINT('Ctrl Pts',(-23.7128705015017,-4.84653787616425,
12.));
#234923=CARTESIAN_POINT('Ctrl Pts',(-23.7316843367313,-4.85871174865499,
12.));
#234924=CARTESIAN_POINT('Ctrl Pts',(-23.7505466018245,-4.87098503527152,
12.));
#234925=CARTESIAN_POINT('Ctrl Pts',(-23.7694565448049,-4.88335766525573,
12.));
#234926=CARTESIAN_POINT('Ctrl Pts',(-23.7884134212384,-4.89582956706775,
12.));
#234927=CARTESIAN_POINT('Ctrl Pts',(-23.8074164940896,-4.90840066839344,
12.));
#234928=CARTESIAN_POINT('Ctrl Pts',(-23.8264650335717,-4.92107089613969,
12.));
#234929=CARTESIAN_POINT('Ctrl Pts',(-23.8455583170057,-4.93384017643432,
12.));
#234930=CARTESIAN_POINT('Ctrl Pts',(-23.8646956287168,-4.9467084346586,
12.));
#234931=CARTESIAN_POINT('Ctrl Pts',(-23.8838762599218,-4.9596755954656,
12.));
#234932=CARTESIAN_POINT('Ctrl Pts',(-23.9030995086163,-4.97274158279226,
12.));
#234933=CARTESIAN_POINT('Ctrl Pts',(-23.9223646794592,-4.98590631986532,
12.));
#234934=CARTESIAN_POINT('Ctrl Pts',(-23.9416710836529,-4.99916972919306,
12.));
#234935=CARTESIAN_POINT('Ctrl Pts',(-23.9610180388271,-5.01253173257453,
12.));
#234936=CARTESIAN_POINT('Ctrl Pts',(-23.9804048689227,-5.02599225112454,
12.));
#234937=CARTESIAN_POINT('Ctrl Pts',(-23.9998309040746,-5.03955120528521,
12.));
#234938=CARTESIAN_POINT('Ctrl Pts',(-24.0192954804896,-5.05320851483065,
12.));
#234939=CARTESIAN_POINT('Ctrl Pts',(-24.0387979403268,-5.06696409886641,
12.));
#234940=CARTESIAN_POINT('Ctrl Pts',(-24.0583376315638,-5.08081787581276,
12.));
#234941=CARTESIAN_POINT('Ctrl Pts',(-24.0779139079266,-5.09476976342625,
12.));
#234942=CARTESIAN_POINT('Ctrl Pts',(-24.0975261288446,-5.10881967883132,
12.));
#234943=CARTESIAN_POINT('Ctrl Pts',(-24.117173659394,-5.12296753853859,
12.));
#234944=CARTESIAN_POINT('Ctrl Pts',(-24.1368558702443,-5.13721325845744,
12.));
#234945=CARTESIAN_POINT('Ctrl Pts',(-24.156572137597,-5.15155675390075,
12.));
#234946=CARTESIAN_POINT('Ctrl Pts',(-24.1763218431343,-5.16599793957979,
12.));
#234947=CARTESIAN_POINT('Ctrl Pts',(-24.1961043738754,-5.18053672961392,
12.));
#234948=CARTESIAN_POINT('Ctrl Pts',(-24.215919122017,-5.19517303753643,
12.));
#234949=CARTESIAN_POINT('Ctrl Pts',(-24.2357654847765,-5.20990677629173,
12.));
#234950=CARTESIAN_POINT('Ctrl Pts',(-24.2556428642294,-5.22473785822441,
12.));
#234951=CARTESIAN_POINT('Ctrl Pts',(-24.2755506671526,-5.23966619506289,
12.));
#234952=CARTESIAN_POINT('Ctrl Pts',(-24.2954883048448,-5.25469169788856,
12.));
#234953=CARTESIAN_POINT('Ctrl Pts',(-24.3154551932222,-5.26981427718796,
12.));
#234954=CARTESIAN_POINT('Ctrl Pts',(-24.3354507529415,-5.28503384290644,
12.));
#234955=CARTESIAN_POINT('Ctrl Pts',(-24.3554744095075,-5.30035030449058,
12.));
#234956=CARTESIAN_POINT('Ctrl Pts',(-24.3755255933917,-5.31576357092524,
12.));
#234957=CARTESIAN_POINT('Ctrl Pts',(-24.3956037401293,-5.33127355076036,
12.));
#234958=CARTESIAN_POINT('Ctrl Pts',(-24.4157082904615,-5.34688015213546,
12.));
#234959=CARTESIAN_POINT('Ctrl Pts',(-24.4358386899152,-5.36258328273639,
12.));
#234960=CARTESIAN_POINT('Ctrl Pts',(-24.4559943883159,-5.37838284973706,
12.));
#234961=CARTESIAN_POINT('Ctrl Pts',(-24.4761748393322,-5.3942787597383,
12.));
#234962=CARTESIAN_POINT('Ctrl Pts',(-24.4963794999831,-5.41027091869242,
12.));
#234963=CARTESIAN_POINT('Ctrl Pts',(-24.5166078302107,-5.42635923183411,
12.));
#234964=CARTESIAN_POINT('Ctrl Pts',(-24.5368592922861,-5.44254360356865,
12.));
#234965=CARTESIAN_POINT('Ctrl Pts',(-24.5571333514841,-5.45882393762244,
12.));
#234966=CARTESIAN_POINT('Ctrl Pts',(-24.5774294770329,-5.47520013724403,
12.));
#234967=CARTESIAN_POINT('Ctrl Pts',(-24.5977471429365,-5.49167210537235,
12.));
#234968=CARTESIAN_POINT('Ctrl Pts',(-24.618085828918,-5.50823974481959,
12.));
#234969=CARTESIAN_POINT('Ctrl Pts',(-24.6384450211466,-5.52490295840996,
12.));
#234970=CARTESIAN_POINT('Ctrl Pts',(-24.6588242134733,-5.54166164919593,
12.));
#234971=CARTESIAN_POINT('Ctrl Pts',(-24.6792229061785,-5.55851572025389,
12.));
#234972=CARTESIAN_POINT('Ctrl Pts',(-24.6996406035507,-5.57546507427766,
12.));
#234973=CARTESIAN_POINT('Ctrl Pts',(-24.7200768119079,-5.59250961323995,
12.));
#234974=CARTESIAN_POINT('Ctrl Pts',(-24.7405310372736,-5.60964923798495,
12.));
#234975=CARTESIAN_POINT('Ctrl Pts',(-24.76100278357,-5.62688384790919,12.));
#234976=CARTESIAN_POINT('Ctrl Pts',(-24.7814915496728,-5.64421334042247,
12.));
#234977=CARTESIAN_POINT('Ctrl Pts',(-24.8019968304618,-5.66163761114903,
12.));
#234978=CARTESIAN_POINT('Ctrl Pts',(-24.822518122386,-5.67915655496524,
12.));
#234979=CARTESIAN_POINT('Ctrl Pts',(-24.8430549277634,-5.69677006679429,
12.));
#234980=CARTESIAN_POINT('Ctrl Pts',(-24.8636067597677,-5.71447804252019,
12.));
#234981=CARTESIAN_POINT('Ctrl Pts',(-24.8841731467219,-5.73228037976926,
12.));
#234982=CARTESIAN_POINT('Ctrl Pts',(-24.9047536376467,-5.75017697890813,
12.));
#234983=CARTESIAN_POINT('Ctrl Pts',(-24.9253478043632,-5.76816774342236,
12.));
#234984=CARTESIAN_POINT('Ctrl Pts',(-24.9459552293308,-5.78625257775703,
12.));
#234985=CARTESIAN_POINT('Ctrl Pts',(-24.9665754954462,-5.80443138549747,
12.));
#234986=CARTESIAN_POINT('Ctrl Pts',(-24.9872081752709,-5.82270406744214,
12.));
#234987=CARTESIAN_POINT('Ctrl Pts',(-25.0078528200558,-5.84107051963073,
12.));
#234988=CARTESIAN_POINT('Ctrl Pts',(-25.0285089498922,-5.8595306315681,
12.));
#234989=CARTESIAN_POINT('Ctrl Pts',(-25.0491760405965,-5.87808428385329,
12.));
#234990=CARTESIAN_POINT('Ctrl Pts',(-25.0698535426593,-5.89673135155459,
12.));
#234991=CARTESIAN_POINT('Ctrl Pts',(-25.0905409050863,-5.91547170844382,
12.));
#234992=CARTESIAN_POINT('Ctrl Pts',(-25.1112375971182,-5.93430523086776,
12.));
#234993=CARTESIAN_POINT('Ctrl Pts',(-25.1319431317273,-5.95323180187348,
12.));
#234994=CARTESIAN_POINT('Ctrl Pts',(-25.1526570863065,-5.97225131495636,
12.));
#234995=CARTESIAN_POINT('Ctrl Pts',(-25.1733791296154,-5.99136367859838,
12.));
#234996=CARTESIAN_POINT('Ctrl Pts',(-25.1941090269638,-6.0105688180476,
12.));
#234997=CARTESIAN_POINT('Ctrl Pts',(-25.2148466201368,-6.02986667390187,
12.));
#234998=CARTESIAN_POINT('Ctrl Pts',(-25.2355918138798,-6.04925720151412,
12.));
#234999=CARTESIAN_POINT('Ctrl Pts',(-25.2521940105523,-6.06484373634696,
12.));
#235000=CARTESIAN_POINT('Ctrl Pts',(-25.2646490489816,-6.07657531787577,
12.));
#235001=CARTESIAN_POINT('Ctrl Pts',(-25.2729539149479,-6.08441489609824,
12.));
#235002=CARTESIAN_POINT('Ctrl Pts',(-25.2771067246846,-6.08833931617698,
12.));
#235003=CARTESIAN_POINT('Ctrl Pts',(-22.4835757167854,-1.76341220531179,
0.));
#235004=CARTESIAN_POINT('Ctrl Pts',(-22.4835757167854,-1.76341220531179,
12.));
#235005=CARTESIAN_POINT('Ctrl Pts',(-22.483581992979,-1.76341415538764,
0.));
#235006=CARTESIAN_POINT('Ctrl Pts',(-22.483581992979,-1.76341415538764,
12.));
#235007=CARTESIAN_POINT('Ctrl Pts',(-22.4836387052232,-1.7634206426357,
0.));
#235008=CARTESIAN_POINT('Ctrl Pts',(-22.4836387052232,-1.7634206426357,
12.));
#235009=CARTESIAN_POINT('Ctrl Pts',(-22.483856251707,-1.76343813434565,
0.));
#235010=CARTESIAN_POINT('Ctrl Pts',(-22.483856251707,-1.76343813434565,
12.));
#235011=CARTESIAN_POINT('Ctrl Pts',(-22.4844112933129,-1.76347698284792,
0.));
#235012=CARTESIAN_POINT('Ctrl Pts',(-22.4844112933129,-1.76347698284792,
12.));
#235013=CARTESIAN_POINT('Ctrl Pts',(-22.4855446605991,-1.76355076045546,
0.));
#235014=CARTESIAN_POINT('Ctrl Pts',(-22.4855446605991,-1.76355076045546,
12.));
#235015=CARTESIAN_POINT('Ctrl Pts',(-22.4871115206571,-1.76364784232963,
0.));
#235016=CARTESIAN_POINT('Ctrl Pts',(-22.4871115206571,-1.76364784232963,
12.));
#235017=CARTESIAN_POINT('Ctrl Pts',(-22.4890991659478,-1.76376424879505,
0.));
#235018=CARTESIAN_POINT('Ctrl Pts',(-22.4890991659478,-1.76376424879505,
12.));
#235019=CARTESIAN_POINT('Ctrl Pts',(-22.4914909094908,-1.76389475965724,
0.));
#235020=CARTESIAN_POINT('Ctrl Pts',(-22.4914909094908,-1.76389475965724,
12.));
#235021=CARTESIAN_POINT('Ctrl Pts',(-22.4942693792449,-1.764033938803,0.));
#235022=CARTESIAN_POINT('Ctrl Pts',(-22.4942693792449,-1.764033938803,12.));
#235023=CARTESIAN_POINT('Ctrl Pts',(-22.4974203063191,-1.76417731243462,
0.));
#235024=CARTESIAN_POINT('Ctrl Pts',(-22.4974203063191,-1.76417731243462,
12.));
#235025=CARTESIAN_POINT('Ctrl Pts',(-22.5009332677316,-1.76432160068725,
0.));
#235026=CARTESIAN_POINT('Ctrl Pts',(-22.5009332677316,-1.76432160068725,
12.));
#235027=CARTESIAN_POINT('Ctrl Pts',(-22.5047996391978,-1.76446408210366,
0.));
#235028=CARTESIAN_POINT('Ctrl Pts',(-22.5047996391978,-1.76446408210366,
12.));
#235029=CARTESIAN_POINT('Ctrl Pts',(-22.5090112700212,-1.76460218257323,
0.));
#235030=CARTESIAN_POINT('Ctrl Pts',(-22.5090112700212,-1.76460218257323,
12.));
#235031=CARTESIAN_POINT('Ctrl Pts',(-22.5135590569554,-1.76473303281159,
0.));
#235032=CARTESIAN_POINT('Ctrl Pts',(-22.5135590569554,-1.76473303281159,
12.));
#235033=CARTESIAN_POINT('Ctrl Pts',(-22.5184336670207,-1.76485369319896,
0.));
#235034=CARTESIAN_POINT('Ctrl Pts',(-22.5184336670207,-1.76485369319896,
12.));
#235035=CARTESIAN_POINT('Ctrl Pts',(-22.5236259635515,-1.76496128643369,
0.));
#235036=CARTESIAN_POINT('Ctrl Pts',(-22.5236259635515,-1.76496128643369,
12.));
#235037=CARTESIAN_POINT('Ctrl Pts',(-22.529127665298,-1.76505320262751,
0.));
#235038=CARTESIAN_POINT('Ctrl Pts',(-22.529127665298,-1.76505320262751,
12.));
#235039=CARTESIAN_POINT('Ctrl Pts',(-22.5349313983571,-1.7651271156325,
0.));
#235040=CARTESIAN_POINT('Ctrl Pts',(-22.5349313983571,-1.7651271156325,
12.));
#235041=CARTESIAN_POINT('Ctrl Pts',(-22.5410303590891,-1.76518087841492,
0.));
#235042=CARTESIAN_POINT('Ctrl Pts',(-22.5410303590891,-1.76518087841492,
12.));
#235043=CARTESIAN_POINT('Ctrl Pts',(-22.5474180954006,-1.76521245524047,
0.));
#235044=CARTESIAN_POINT('Ctrl Pts',(-22.5474180954006,-1.76521245524047,
12.));
#235045=CARTESIAN_POINT('Ctrl Pts',(-22.5540882235837,-1.76521983384063,
0.));
#235046=CARTESIAN_POINT('Ctrl Pts',(-22.5540882235837,-1.76521983384063,
12.));
#235047=CARTESIAN_POINT('Ctrl Pts',(-22.5610344912501,-1.76520104500449,
0.));
#235048=CARTESIAN_POINT('Ctrl Pts',(-22.5610344912501,-1.76520104500449,
12.));
#235049=CARTESIAN_POINT('Ctrl Pts',(-22.5682508499873,-1.76515418518829,
0.));
#235050=CARTESIAN_POINT('Ctrl Pts',(-22.5682508499873,-1.76515418518829,
12.));
#235051=CARTESIAN_POINT('Ctrl Pts',(-22.5757315316355,-1.76507744026747,
0.));
#235052=CARTESIAN_POINT('Ctrl Pts',(-22.5757315316355,-1.76507744026747,
12.));
#235053=CARTESIAN_POINT('Ctrl Pts',(-22.5834711038024,-1.76496910283088,
0.));
#235054=CARTESIAN_POINT('Ctrl Pts',(-22.5834711038024,-1.76496910283088,
12.));
#235055=CARTESIAN_POINT('Ctrl Pts',(-22.5914644078106,-1.76482755288411,
0.));
#235056=CARTESIAN_POINT('Ctrl Pts',(-22.5914644078106,-1.76482755288411,
12.));
#235057=CARTESIAN_POINT('Ctrl Pts',(-22.5997065145638,-1.76465124413556,
0.));
#235058=CARTESIAN_POINT('Ctrl Pts',(-22.5997065145638,-1.76465124413556,
12.));
#235059=CARTESIAN_POINT('Ctrl Pts',(-22.6081926681342,-1.76443868648015,
0.));
#235060=CARTESIAN_POINT('Ctrl Pts',(-22.6081926681342,-1.76443868648015,
12.));
#235061=CARTESIAN_POINT('Ctrl Pts',(-22.6169182517693,-1.76418843543739,
0.));
#235062=CARTESIAN_POINT('Ctrl Pts',(-22.6169182517693,-1.76418843543739,
12.));
#235063=CARTESIAN_POINT('Ctrl Pts',(-22.6258787994847,-1.76389909571402,
0.));
#235064=CARTESIAN_POINT('Ctrl Pts',(-22.6258787994847,-1.76389909571402,
12.));
#235065=CARTESIAN_POINT('Ctrl Pts',(-22.635069997936,-1.76356932176272,
0.));
#235066=CARTESIAN_POINT('Ctrl Pts',(-22.635069997936,-1.76356932176272,
12.));
#235067=CARTESIAN_POINT('Ctrl Pts',(-22.6444876940425,-1.76319782013914,
0.));
#235068=CARTESIAN_POINT('Ctrl Pts',(-22.6444876940425,-1.76319782013914,
12.));
#235069=CARTESIAN_POINT('Ctrl Pts',(-22.6541278938413,-1.76278334912559,
0.));
#235070=CARTESIAN_POINT('Ctrl Pts',(-22.6541278938413,-1.76278334912559,
12.));
#235071=CARTESIAN_POINT('Ctrl Pts',(-22.6639867471756,-1.76232471392567,
0.));
#235072=CARTESIAN_POINT('Ctrl Pts',(-22.6639867471756,-1.76232471392567,
12.));
#235073=CARTESIAN_POINT('Ctrl Pts',(-22.6740605356699,-1.76182076289525,
0.));
#235074=CARTESIAN_POINT('Ctrl Pts',(-22.6740605356699,-1.76182076289525,
12.));
#235075=CARTESIAN_POINT('Ctrl Pts',(-22.6843456585245,-1.76127038310612,
0.));
#235076=CARTESIAN_POINT('Ctrl Pts',(-22.6843456585245,-1.76127038310612,
12.));
#235077=CARTESIAN_POINT('Ctrl Pts',(-22.6948386219843,-1.76067249704884,
0.));
#235078=CARTESIAN_POINT('Ctrl Pts',(-22.6948386219843,-1.76067249704884,
12.));
#235079=CARTESIAN_POINT('Ctrl Pts',(-22.7055360375481,-1.76002606202399,
0.));
#235080=CARTESIAN_POINT('Ctrl Pts',(-22.7055360375481,-1.76002606202399,
12.));
#235081=CARTESIAN_POINT('Ctrl Pts',(-22.7164346186007,-1.75933006905924,
0.));
#235082=CARTESIAN_POINT('Ctrl Pts',(-22.7164346186007,-1.75933006905924,
12.));
#235083=CARTESIAN_POINT('Ctrl Pts',(-22.7275311777305,-1.75858354204635,
0.));
#235084=CARTESIAN_POINT('Ctrl Pts',(-22.7275311777305,-1.75858354204635,
12.));
#235085=CARTESIAN_POINT('Ctrl Pts',(-22.7388226235565,-1.75778553673249,
0.));
#235086=CARTESIAN_POINT('Ctrl Pts',(-22.7388226235565,-1.75778553673249,
12.));
#235087=CARTESIAN_POINT('Ctrl Pts',(-22.7503059556455,-1.75693513908911,
0.));
#235088=CARTESIAN_POINT('Ctrl Pts',(-22.7503059556455,-1.75693513908911,
12.));
#235089=CARTESIAN_POINT('Ctrl Pts',(-22.7619782595013,-1.7560314637164,
0.));
#235090=CARTESIAN_POINT('Ctrl Pts',(-22.7619782595013,-1.7560314637164,
12.));
#235091=CARTESIAN_POINT('Ctrl Pts',(-22.7738367016115,-1.75507365227127,
0.));
#235092=CARTESIAN_POINT('Ctrl Pts',(-22.7738367016115,-1.75507365227127,
12.));
#235093=CARTESIAN_POINT('Ctrl Pts',(-22.7858785242358,-1.75406087182929,
0.));
#235094=CARTESIAN_POINT('Ctrl Pts',(-22.7858785242358,-1.75406087182929,
12.));
#235095=CARTESIAN_POINT('Ctrl Pts',(-22.7981010424312,-1.75299231391461,
0.));
#235096=CARTESIAN_POINT('Ctrl Pts',(-22.7981010424312,-1.75299231391461,
12.));
#235097=CARTESIAN_POINT('Ctrl Pts',(-22.8105016414712,-1.75186719365589,
0.));
#235098=CARTESIAN_POINT('Ctrl Pts',(-22.8105016414712,-1.75186719365589,
12.));
#235099=CARTESIAN_POINT('Ctrl Pts',(-22.8230777741285,-1.75068474890884,
0.));
#235100=CARTESIAN_POINT('Ctrl Pts',(-22.8230777741285,-1.75068474890884,
12.));
#235101=CARTESIAN_POINT('Ctrl Pts',(-22.8358269579854,-1.74944423940117,
0.));
#235102=CARTESIAN_POINT('Ctrl Pts',(-22.8358269579854,-1.74944423940117,
12.));
#235103=CARTESIAN_POINT('Ctrl Pts',(-22.8487467728075,-1.74814494588492,
0.));
#235104=CARTESIAN_POINT('Ctrl Pts',(-22.8487467728075,-1.74814494588492,
12.));
#235105=CARTESIAN_POINT('Ctrl Pts',(-22.8618348580234,-1.74678616930663,
0.));
#235106=CARTESIAN_POINT('Ctrl Pts',(-22.8618348580234,-1.74678616930663,
12.));
#235107=CARTESIAN_POINT('Ctrl Pts',(-22.8750889101696,-1.745367229982,0.));
#235108=CARTESIAN_POINT('Ctrl Pts',(-22.8750889101696,-1.745367229982,12.));
#235109=CARTESIAN_POINT('Ctrl Pts',(-22.8885066803351,-1.74388746677702,
0.));
#235110=CARTESIAN_POINT('Ctrl Pts',(-22.8885066803351,-1.74388746677702,
12.));
#235111=CARTESIAN_POINT('Ctrl Pts',(-22.9020859716144,-1.74234623630079,
0.));
#235112=CARTESIAN_POINT('Ctrl Pts',(-22.9020859716144,-1.74234623630079,
12.));
#235113=CARTESIAN_POINT('Ctrl Pts',(-22.9158246373365,-1.74074291231057,
0.));
#235114=CARTESIAN_POINT('Ctrl Pts',(-22.9158246373365,-1.74074291231057,
12.));
#235115=CARTESIAN_POINT('Ctrl Pts',(-22.9297205792587,-1.73907688511664,
0.));
#235116=CARTESIAN_POINT('Ctrl Pts',(-22.9297205792587,-1.73907688511664,
12.));
#235117=CARTESIAN_POINT('Ctrl Pts',(-22.9437717457825,-1.73734756100038,
0.));
#235118=CARTESIAN_POINT('Ctrl Pts',(-22.9437717457825,-1.73734756100038,
12.));
#235119=CARTESIAN_POINT('Ctrl Pts',(-22.9579761301062,-1.73555436162771,
0.));
#235120=CARTESIAN_POINT('Ctrl Pts',(-22.9579761301062,-1.73555436162771,
12.));
#235121=CARTESIAN_POINT('Ctrl Pts',(-22.9723317685688,-1.73369672350817,
0.));
#235122=CARTESIAN_POINT('Ctrl Pts',(-22.9723317685688,-1.73369672350817,
12.));
#235123=CARTESIAN_POINT('Ctrl Pts',(-22.9868367391978,-1.73177409750193,
0.));
#235124=CARTESIAN_POINT('Ctrl Pts',(-22.9868367391978,-1.73177409750193,
12.));
#235125=CARTESIAN_POINT('Ctrl Pts',(-23.0014891601891,-1.72978594832137,
0.));
#235126=CARTESIAN_POINT('Ctrl Pts',(-23.0014891601891,-1.72978594832137,
12.));
#235127=CARTESIAN_POINT('Ctrl Pts',(-23.0162871884167,-1.72773175404702,
0.));
#235128=CARTESIAN_POINT('Ctrl Pts',(-23.0162871884167,-1.72773175404702,
12.));
#235129=CARTESIAN_POINT('Ctrl Pts',(-23.031229017888,-1.72561100564033,
0.));
#235130=CARTESIAN_POINT('Ctrl Pts',(-23.031229017888,-1.72561100564033,
12.));
#235131=CARTESIAN_POINT('Ctrl Pts',(-23.0463128785528,-1.72342320653731,
0.));
#235132=CARTESIAN_POINT('Ctrl Pts',(-23.0463128785528,-1.72342320653731,
12.));
#235133=CARTESIAN_POINT('Ctrl Pts',(-23.061537035156,-1.7211678722598,0.));
#235134=CARTESIAN_POINT('Ctrl Pts',(-23.061537035156,-1.7211678722598,12.));
#235135=CARTESIAN_POINT('Ctrl Pts',(-23.0768997860709,-1.71884453003027,
0.));
#235136=CARTESIAN_POINT('Ctrl Pts',(-23.0768997860709,-1.71884453003027,
12.));
#235137=CARTESIAN_POINT('Ctrl Pts',(-23.0923994621216,-1.71645271839311,
0.));
#235138=CARTESIAN_POINT('Ctrl Pts',(-23.0923994621216,-1.71645271839311,
12.));
#235139=CARTESIAN_POINT('Ctrl Pts',(-23.1080344254291,-1.71399198684724,
0.));
#235140=CARTESIAN_POINT('Ctrl Pts',(-23.1080344254291,-1.71399198684724,
12.));
#235141=CARTESIAN_POINT('Ctrl Pts',(-23.1238030684929,-1.71146189552192,
0.));
#235142=CARTESIAN_POINT('Ctrl Pts',(-23.1238030684929,-1.71146189552192,
12.));
#235143=CARTESIAN_POINT('Ctrl Pts',(-23.1397038132358,-1.7088620148546,
0.));
#235144=CARTESIAN_POINT('Ctrl Pts',(-23.1397038132358,-1.7088620148546,
12.));
#235145=CARTESIAN_POINT('Ctrl Pts',(-23.1557351100613,-1.70619192527847,
0.));
#235146=CARTESIAN_POINT('Ctrl Pts',(-23.1557351100613,-1.70619192527847,
12.));
#235147=CARTESIAN_POINT('Ctrl Pts',(-23.1718954368749,-1.70345121691259,
0.));
#235148=CARTESIAN_POINT('Ctrl Pts',(-23.1718954368749,-1.70345121691259,
12.));
#235149=CARTESIAN_POINT('Ctrl Pts',(-23.1881832981848,-1.70063948926987,
0.));
#235150=CARTESIAN_POINT('Ctrl Pts',(-23.1881832981848,-1.70063948926987,
12.));
#235151=CARTESIAN_POINT('Ctrl Pts',(-23.2045972243765,-1.69775635099425,
0.));
#235152=CARTESIAN_POINT('Ctrl Pts',(-23.2045972243765,-1.69775635099425,
12.));
#235153=CARTESIAN_POINT('Ctrl Pts',(-23.2211357709374,-1.69480141959945,
0.));
#235154=CARTESIAN_POINT('Ctrl Pts',(-23.2211357709374,-1.69480141959945,
12.));
#235155=CARTESIAN_POINT('Ctrl Pts',(-23.2377975177014,-1.69177432121716,
0.));
#235156=CARTESIAN_POINT('Ctrl Pts',(-23.2377975177014,-1.69177432121716,
12.));
#235157=CARTESIAN_POINT('Ctrl Pts',(-23.2545810680536,-1.6886746903491,
0.));
#235158=CARTESIAN_POINT('Ctrl Pts',(-23.2545810680536,-1.6886746903491,
12.));
#235159=CARTESIAN_POINT('Ctrl Pts',(-23.2714850482245,-1.68550216963275,
0.));
#235160=CARTESIAN_POINT('Ctrl Pts',(-23.2714850482245,-1.68550216963275,
12.));
#235161=CARTESIAN_POINT('Ctrl Pts',(-23.2885081066949,-1.68225640962181,
0.));
#235162=CARTESIAN_POINT('Ctrl Pts',(-23.2885081066949,-1.68225640962181,
12.));
#235163=CARTESIAN_POINT('Ctrl Pts',(-23.3056489135611,-1.67893706857123,
0.));
#235164=CARTESIAN_POINT('Ctrl Pts',(-23.3056489135611,-1.67893706857123,
12.));
#235165=CARTESIAN_POINT('Ctrl Pts',(-23.3229061599145,-1.67554381222987,
0.));
#235166=CARTESIAN_POINT('Ctrl Pts',(-23.3229061599145,-1.67554381222987,
12.));
#235167=CARTESIAN_POINT('Ctrl Pts',(-23.3402785571866,-1.67207631363905,
0.));
#235168=CARTESIAN_POINT('Ctrl Pts',(-23.3402785571866,-1.67207631363905,
12.));
#235169=CARTESIAN_POINT('Ctrl Pts',(-23.3577648365747,-1.66853425293977,
0.));
#235170=CARTESIAN_POINT('Ctrl Pts',(-23.3577648365747,-1.66853425293977,
12.));
#235171=CARTESIAN_POINT('Ctrl Pts',(-23.375363748555,-1.66491731718864,
0.));
#235172=CARTESIAN_POINT('Ctrl Pts',(-23.375363748555,-1.66491731718864,
12.));
#235173=CARTESIAN_POINT('Ctrl Pts',(-23.3930740623622,-1.66122520018008,
0.));
#235174=CARTESIAN_POINT('Ctrl Pts',(-23.3930740623622,-1.66122520018008,
12.));
#235175=CARTESIAN_POINT('Ctrl Pts',(-23.4108945654803,-1.65745760227507,
0.));
#235176=CARTESIAN_POINT('Ctrl Pts',(-23.4108945654803,-1.65745760227507,
12.));
#235177=CARTESIAN_POINT('Ctrl Pts',(-23.4288240631034,-1.6536142302373,
0.));
#235178=CARTESIAN_POINT('Ctrl Pts',(-23.4288240631034,-1.6536142302373,
12.));
#235179=CARTESIAN_POINT('Ctrl Pts',(-23.446861377656,-1.64969479707339,
0.));
#235180=CARTESIAN_POINT('Ctrl Pts',(-23.446861377656,-1.64969479707339,
12.));
#235181=CARTESIAN_POINT('Ctrl Pts',(-23.4650053483919,-1.64569902187608,
0.));
#235182=CARTESIAN_POINT('Ctrl Pts',(-23.4650053483919,-1.64569902187608,
12.));
#235183=CARTESIAN_POINT('Ctrl Pts',(-23.4832548309638,-1.64162662967524,
0.));
#235184=CARTESIAN_POINT('Ctrl Pts',(-23.4832548309638,-1.64162662967524,
12.));
#235185=CARTESIAN_POINT('Ctrl Pts',(-23.5016086970006,-1.63747735129474,
0.));
#235186=CARTESIAN_POINT('Ctrl Pts',(-23.5016086970006,-1.63747735129474,
12.));
#235187=CARTESIAN_POINT('Ctrl Pts',(-23.5200658336624,-1.63325092321731,
0.));
#235188=CARTESIAN_POINT('Ctrl Pts',(-23.5200658336624,-1.63325092321731,
12.));
#235189=CARTESIAN_POINT('Ctrl Pts',(-23.5386251432278,-1.62894708745231,
0.));
#235190=CARTESIAN_POINT('Ctrl Pts',(-23.5386251432278,-1.62894708745231,
12.));
#235191=CARTESIAN_POINT('Ctrl Pts',(-23.5572855427617,-1.62456559140072,
0.));
#235192=CARTESIAN_POINT('Ctrl Pts',(-23.5572855427617,-1.62456559140072,
12.));
#235193=CARTESIAN_POINT('Ctrl Pts',(-23.5760459637608,-1.62010618772869,
0.));
#235194=CARTESIAN_POINT('Ctrl Pts',(-23.5760459637608,-1.62010618772869,
12.));
#235195=CARTESIAN_POINT('Ctrl Pts',(-23.5949053517996,-1.61556863424697,
0.));
#235196=CARTESIAN_POINT('Ctrl Pts',(-23.5949053517996,-1.61556863424697,
12.));
#235197=CARTESIAN_POINT('Ctrl Pts',(-23.6138626661644,-1.61095269379773,
0.));
#235198=CARTESIAN_POINT('Ctrl Pts',(-23.6138626661644,-1.61095269379773,
12.));
#235199=CARTESIAN_POINT('Ctrl Pts',(-23.6329168794916,-1.60625813414666,
0.));
#235200=CARTESIAN_POINT('Ctrl Pts',(-23.6329168794916,-1.60625813414666,
12.));
#235201=CARTESIAN_POINT('Ctrl Pts',(-23.6520669774863,-1.60148472786588,
0.));
#235202=CARTESIAN_POINT('Ctrl Pts',(-23.6520669774863,-1.60148472786588,
12.));
#235203=CARTESIAN_POINT('Ctrl Pts',(-23.6713119586302,-1.59663225222458,
0.));
#235204=CARTESIAN_POINT('Ctrl Pts',(-23.6713119586302,-1.59663225222458,
12.));
#235205=CARTESIAN_POINT('Ctrl Pts',(-23.6906508338833,-1.59170048908631,
0.));
#235206=CARTESIAN_POINT('Ctrl Pts',(-23.6906508338833,-1.59170048908631,
12.));
#235207=CARTESIAN_POINT('Ctrl Pts',(-23.7100826263835,-1.58668922481222,
0.));
#235208=CARTESIAN_POINT('Ctrl Pts',(-23.7100826263835,-1.58668922481222,
12.));
#235209=CARTESIAN_POINT('Ctrl Pts',(-23.7296063711308,-1.58159825017362,
0.));
#235210=CARTESIAN_POINT('Ctrl Pts',(-23.7296063711308,-1.58159825017362,
12.));
#235211=CARTESIAN_POINT('Ctrl Pts',(-23.7492211147369,-1.57642736025251,
0.));
#235212=CARTESIAN_POINT('Ctrl Pts',(-23.7492211147369,-1.57642736025251,
12.));
#235213=CARTESIAN_POINT('Ctrl Pts',(-23.7689259151869,-1.57117635434412,
0.));
#235214=CARTESIAN_POINT('Ctrl Pts',(-23.7689259151869,-1.57117635434412,
12.));
#235215=CARTESIAN_POINT('Ctrl Pts',(-23.788719841588,-1.56584503586844,
0.));
#235216=CARTESIAN_POINT('Ctrl Pts',(-23.788719841588,-1.56584503586844,
12.));
#235217=CARTESIAN_POINT('Ctrl Pts',(-23.8086019739192,-1.56043321228631,
0.));
#235218=CARTESIAN_POINT('Ctrl Pts',(-23.8086019739192,-1.56043321228631,
12.));
#235219=CARTESIAN_POINT('Ctrl Pts',(-23.8285714027631,-1.55494069502628,
0.));
#235220=CARTESIAN_POINT('Ctrl Pts',(-23.8285714027631,-1.55494069502628,
12.));
#235221=CARTESIAN_POINT('Ctrl Pts',(-23.8486272290698,-1.5493672994053,
0.));
#235222=CARTESIAN_POINT('Ctrl Pts',(-23.8486272290698,-1.5493672994053,
12.));
#235223=CARTESIAN_POINT('Ctrl Pts',(-23.8687685639635,-1.54371284453978,
0.));
#235224=CARTESIAN_POINT('Ctrl Pts',(-23.8687685639635,-1.54371284453978,
12.));
#235225=CARTESIAN_POINT('Ctrl Pts',(-23.8889945285313,-1.53797715326748,
0.));
#235226=CARTESIAN_POINT('Ctrl Pts',(-23.8889945285313,-1.53797715326748,
12.));
#235227=CARTESIAN_POINT('Ctrl Pts',(-23.9093042536119,-1.53216005207462,
0.));
#235228=CARTESIAN_POINT('Ctrl Pts',(-23.9093042536119,-1.53216005207462,
12.));
#235229=CARTESIAN_POINT('Ctrl Pts',(-23.9296968795761,-1.52626137103039,
0.));
#235230=CARTESIAN_POINT('Ctrl Pts',(-23.9296968795761,-1.52626137103039,
12.));
#235231=CARTESIAN_POINT('Ctrl Pts',(-23.9501715561038,-1.52028094372806,
0.));
#235232=CARTESIAN_POINT('Ctrl Pts',(-23.9501715561038,-1.52028094372806,
12.));
#235233=CARTESIAN_POINT('Ctrl Pts',(-23.9707274420145,-1.51421860720628,
0.));
#235234=CARTESIAN_POINT('Ctrl Pts',(-23.9707274420145,-1.51421860720628,
12.));
#235235=CARTESIAN_POINT('Ctrl Pts',(-23.991363705093,-1.50807420187702,
0.));
#235236=CARTESIAN_POINT('Ctrl Pts',(-23.991363705093,-1.50807420187702,
12.));
#235237=CARTESIAN_POINT('Ctrl Pts',(-24.0120795219086,-1.50184757146099,
0.));
#235238=CARTESIAN_POINT('Ctrl Pts',(-24.0120795219086,-1.50184757146099,
12.));
#235239=CARTESIAN_POINT('Ctrl Pts',(-24.0328740776331,-1.49553856292798,
0.));
#235240=CARTESIAN_POINT('Ctrl Pts',(-24.0328740776331,-1.49553856292798,
12.));
#235241=CARTESIAN_POINT('Ctrl Pts',(-24.053746565843,-1.48914702644883,
0.));
#235242=CARTESIAN_POINT('Ctrl Pts',(-24.053746565843,-1.48914702644883,
12.));
#235243=CARTESIAN_POINT('Ctrl Pts',(-24.074696188353,-1.4826728153368,0.));
#235244=CARTESIAN_POINT('Ctrl Pts',(-24.074696188353,-1.4826728153368,12.));
#235245=CARTESIAN_POINT('Ctrl Pts',(-24.0957221550782,-1.47611578597741,
0.));
#235246=CARTESIAN_POINT('Ctrl Pts',(-24.0957221550782,-1.47611578597741,
12.));
#235247=CARTESIAN_POINT('Ctrl Pts',(-24.1168236838827,-1.46947579776992,
0.));
#235248=CARTESIAN_POINT('Ctrl Pts',(-24.1168236838827,-1.46947579776992,
12.));
#235249=CARTESIAN_POINT('Ctrl Pts',(-24.1380000004272,-1.46275271307398,
0.));
#235250=CARTESIAN_POINT('Ctrl Pts',(-24.1380000004272,-1.46275271307398,
12.));
#235251=CARTESIAN_POINT('Ctrl Pts',(-24.1592503380105,-1.45594639716314,
0.));
#235252=CARTESIAN_POINT('Ctrl Pts',(-24.1592503380105,-1.45594639716314,
12.));
#235253=CARTESIAN_POINT('Ctrl Pts',(-24.1805739374033,-1.44905671818721,
0.));
#235254=CARTESIAN_POINT('Ctrl Pts',(-24.1805739374033,-1.44905671818721,
12.));
#235255=CARTESIAN_POINT('Ctrl Pts',(-24.2019700467214,-1.44208354711074,
0.));
#235256=CARTESIAN_POINT('Ctrl Pts',(-24.2019700467214,-1.44208354711074,
12.));
#235257=CARTESIAN_POINT('Ctrl Pts',(-24.2234379212978,-1.43502675765502,
0.));
#235258=CARTESIAN_POINT('Ctrl Pts',(-24.2234379212978,-1.43502675765502,
12.));
#235259=CARTESIAN_POINT('Ctrl Pts',(-24.2449768235485,-1.42788622624851,
0.));
#235260=CARTESIAN_POINT('Ctrl Pts',(-24.2449768235485,-1.42788622624851,
12.));
#235261=CARTESIAN_POINT('Ctrl Pts',(-24.2665860228357,-1.42066183198252,
0.));
#235262=CARTESIAN_POINT('Ctrl Pts',(-24.2665860228357,-1.42066183198252,
12.));
#235263=CARTESIAN_POINT('Ctrl Pts',(-24.2882647953214,-1.41335345657685,
0.));
#235264=CARTESIAN_POINT('Ctrl Pts',(-24.2882647953214,-1.41335345657685,
12.));
#235265=CARTESIAN_POINT('Ctrl Pts',(-24.3100124238316,-1.4059609843434,
0.));
#235266=CARTESIAN_POINT('Ctrl Pts',(-24.3100124238316,-1.4059609843434,
12.));
#235267=CARTESIAN_POINT('Ctrl Pts',(-24.3318281977647,-1.3984843021281,
0.));
#235268=CARTESIAN_POINT('Ctrl Pts',(-24.3318281977647,-1.3984843021281,
12.));
#235269=CARTESIAN_POINT('Ctrl Pts',(-24.3537114129877,-1.3909232992639,
0.));
#235270=CARTESIAN_POINT('Ctrl Pts',(-24.3537114129877,-1.3909232992639,
12.));
#235271=CARTESIAN_POINT('Ctrl Pts',(-24.37566137173,-1.38327786752998,0.));
#235272=CARTESIAN_POINT('Ctrl Pts',(-24.37566137173,-1.38327786752998,12.));
#235273=CARTESIAN_POINT('Ctrl Pts',(-24.3976773824731,-1.37554790111607,
0.));
#235274=CARTESIAN_POINT('Ctrl Pts',(-24.3976773824731,-1.37554790111607,
12.));
#235275=CARTESIAN_POINT('Ctrl Pts',(-24.4197587598337,-1.36773329659954,
0.));
#235276=CARTESIAN_POINT('Ctrl Pts',(-24.4197587598337,-1.36773329659954,
12.));
#235277=CARTESIAN_POINT('Ctrl Pts',(-24.4419048244524,-1.35983395290624,
0.));
#235278=CARTESIAN_POINT('Ctrl Pts',(-24.4419048244524,-1.35983395290624,
12.));
#235279=CARTESIAN_POINT('Ctrl Pts',(-24.4641149028894,-1.35184977125644,
0.));
#235280=CARTESIAN_POINT('Ctrl Pts',(-24.4641149028894,-1.35184977125644,
12.));
#235281=CARTESIAN_POINT('Ctrl Pts',(-24.4863883275135,-1.34378065512335,
0.));
#235282=CARTESIAN_POINT('Ctrl Pts',(-24.4863883275135,-1.34378065512335,
12.));
#235283=CARTESIAN_POINT('Ctrl Pts',(-24.5087244363856,-1.33562651019684,
0.));
#235284=CARTESIAN_POINT('Ctrl Pts',(-24.5087244363856,-1.33562651019684,
12.));
#235285=CARTESIAN_POINT('Ctrl Pts',(-24.5311225731434,-1.32738724435326,
0.));
#235286=CARTESIAN_POINT('Ctrl Pts',(-24.5311225731434,-1.32738724435326,
12.));
#235287=CARTESIAN_POINT('Ctrl Pts',(-24.5535820868671,-1.31906276763669,
0.));
#235288=CARTESIAN_POINT('Ctrl Pts',(-24.5535820868671,-1.31906276763669,
12.));
#235289=CARTESIAN_POINT('Ctrl Pts',(-24.576102332018,-1.31065299222023,
0.));
#235290=CARTESIAN_POINT('Ctrl Pts',(-24.576102332018,-1.31065299222023,
12.));
#235291=CARTESIAN_POINT('Ctrl Pts',(-24.5986826684025,-1.30215783236364,
0.));
#235292=CARTESIAN_POINT('Ctrl Pts',(-24.5986826684025,-1.30215783236364,
12.));
#235293=CARTESIAN_POINT('Ctrl Pts',(-24.6213224611228,-1.29357720438107,
0.));
#235294=CARTESIAN_POINT('Ctrl Pts',(-24.6213224611228,-1.29357720438107,
12.));
#235295=CARTESIAN_POINT('Ctrl Pts',(-24.6440210805278,-1.28491102661513,
0.));
#235296=CARTESIAN_POINT('Ctrl Pts',(-24.6440210805278,-1.28491102661513,
12.));
#235297=CARTESIAN_POINT('Ctrl Pts',(-24.666777902156,-1.2761592194164,0.));
#235298=CARTESIAN_POINT('Ctrl Pts',(-24.666777902156,-1.2761592194164,12.));
#235299=CARTESIAN_POINT('Ctrl Pts',(-24.6895923066837,-1.26732170513497,
0.));
#235300=CARTESIAN_POINT('Ctrl Pts',(-24.6895923066837,-1.26732170513497,
12.));
#235301=CARTESIAN_POINT('Ctrl Pts',(-24.7124636797895,-1.25839840807415,
0.));
#235302=CARTESIAN_POINT('Ctrl Pts',(-24.7124636797895,-1.25839840807415,
12.));
#235303=CARTESIAN_POINT('Ctrl Pts',(-24.7353914120012,-1.24938925444323,
0.));
#235304=CARTESIAN_POINT('Ctrl Pts',(-24.7353914120012,-1.24938925444323,
12.));
#235305=CARTESIAN_POINT('Ctrl Pts',(-24.7583748985439,-1.24029417231988,
0.));
#235306=CARTESIAN_POINT('Ctrl Pts',(-24.7583748985439,-1.24029417231988,
12.));
#235307=CARTESIAN_POINT('Ctrl Pts',(-24.78141353918,-1.23111309161843,0.));
#235308=CARTESIAN_POINT('Ctrl Pts',(-24.78141353918,-1.23111309161843,12.));
#235309=CARTESIAN_POINT('Ctrl Pts',(-24.8045067380536,-1.22184594406526,
0.));
#235310=CARTESIAN_POINT('Ctrl Pts',(-24.8045067380536,-1.22184594406526,
12.));
#235311=CARTESIAN_POINT('Ctrl Pts',(-24.8276539035092,-1.21249266318205,
0.));
#235312=CARTESIAN_POINT('Ctrl Pts',(-24.8276539035092,-1.21249266318205,
12.));
#235313=CARTESIAN_POINT('Ctrl Pts',(-24.8508544481973,-1.20305318426015,
0.));
#235314=CARTESIAN_POINT('Ctrl Pts',(-24.8508544481973,-1.20305318426015,
12.));
#235315=CARTESIAN_POINT('Ctrl Pts',(-24.8741077892074,-1.19352744434059,
0.));
#235316=CARTESIAN_POINT('Ctrl Pts',(-24.8741077892074,-1.19352744434059,
12.));
#235317=CARTESIAN_POINT('Ctrl Pts',(-24.8974133481829,-1.18391538220098,
0.));
#235318=CARTESIAN_POINT('Ctrl Pts',(-24.8974133481829,-1.18391538220098,
12.));
#235319=CARTESIAN_POINT('Ctrl Pts',(-24.9207705514449,-1.17421693835039,
0.));
#235320=CARTESIAN_POINT('Ctrl Pts',(-24.9207705514449,-1.17421693835039,
12.));
#235321=CARTESIAN_POINT('Ctrl Pts',(-24.9441788300932,-1.16443205502852,
0.));
#235322=CARTESIAN_POINT('Ctrl Pts',(-24.9441788300932,-1.16443205502852,
12.));
#235323=CARTESIAN_POINT('Ctrl Pts',(-24.9676376201501,-1.15456067621894,
0.));
#235324=CARTESIAN_POINT('Ctrl Pts',(-24.9676376201501,-1.15456067621894,
12.));
#235325=CARTESIAN_POINT('Ctrl Pts',(-24.9911463621431,-1.14460274758206,
0.));
#235326=CARTESIAN_POINT('Ctrl Pts',(-24.9911463621431,-1.14460274758206,
12.));
#235327=CARTESIAN_POINT('Ctrl Pts',(-25.0147045006193,-1.13455821638535,
0.));
#235328=CARTESIAN_POINT('Ctrl Pts',(-25.0147045006193,-1.13455821638535,
12.));
#235329=CARTESIAN_POINT('Ctrl Pts',(-25.0383114836898,-1.12442703144455,
0.));
#235330=CARTESIAN_POINT('Ctrl Pts',(-25.0383114836898,-1.12442703144455,
12.));
#235331=CARTESIAN_POINT('Ctrl Pts',(-25.0619667625336,-1.1142091430689,
0.));
#235332=CARTESIAN_POINT('Ctrl Pts',(-25.0619667625336,-1.1142091430689,
12.));
#235333=CARTESIAN_POINT('Ctrl Pts',(-25.085669790968,-1.1039045030174,0.));
#235334=CARTESIAN_POINT('Ctrl Pts',(-25.085669790968,-1.1039045030174,12.));
#235335=CARTESIAN_POINT('Ctrl Pts',(-25.1094200248448,-1.09351306445299,
0.));
#235336=CARTESIAN_POINT('Ctrl Pts',(-25.1094200248448,-1.09351306445299,
12.));
#235337=CARTESIAN_POINT('Ctrl Pts',(-25.1332169227415,-1.08303478197174,
0.));
#235338=CARTESIAN_POINT('Ctrl Pts',(-25.1332169227415,-1.08303478197174,
12.));
#235339=CARTESIAN_POINT('Ctrl Pts',(-25.1570599469311,-1.0724696116546,
0.));
#235340=CARTESIAN_POINT('Ctrl Pts',(-25.1570599469311,-1.0724696116546,
12.));
#235341=CARTESIAN_POINT('Ctrl Pts',(-25.1809485642191,-1.06181751111754,
0.));
#235342=CARTESIAN_POINT('Ctrl Pts',(-25.1809485642191,-1.06181751111754,
12.));
#235343=CARTESIAN_POINT('Ctrl Pts',(-25.2048822469027,-1.05107843957925,
0.));
#235344=CARTESIAN_POINT('Ctrl Pts',(-25.2048822469027,-1.05107843957925,
12.));
#235345=CARTESIAN_POINT('Ctrl Pts',(-25.2288604735087,-1.04025235791515,
0.));
#235346=CARTESIAN_POINT('Ctrl Pts',(-25.2288604735087,-1.04025235791515,
12.));
#235347=CARTESIAN_POINT('Ctrl Pts',(-25.2528827300427,-1.0293392287683,
0.));
#235348=CARTESIAN_POINT('Ctrl Pts',(-25.2528827300427,-1.0293392287683,
12.));
#235349=CARTESIAN_POINT('Ctrl Pts',(-25.2769485087268,-1.01833901642272,
0.));
#235350=CARTESIAN_POINT('Ctrl Pts',(-25.2769485087268,-1.01833901642272,
12.));
#235351=CARTESIAN_POINT('Ctrl Pts',(-25.3010573055557,-1.00725168656933,
0.));
#235352=CARTESIAN_POINT('Ctrl Pts',(-25.3010573055557,-1.00725168656933,
12.));
#235353=CARTESIAN_POINT('Ctrl Pts',(-25.3252086182976,-0.996077206120919,
0.));
#235354=CARTESIAN_POINT('Ctrl Pts',(-25.3252086182976,-0.996077206120919,
12.));
#235355=CARTESIAN_POINT('Ctrl Pts',(-25.3494019441444,-0.984815543004089,
0.));
#235356=CARTESIAN_POINT('Ctrl Pts',(-25.3494019441444,-0.984815543004089,
12.));
#235357=CARTESIAN_POINT('Ctrl Pts',(-25.3736367778842,-0.973466666000048,
0.));
#235358=CARTESIAN_POINT('Ctrl Pts',(-25.3736367778842,-0.973466666000048,
12.));
#235359=CARTESIAN_POINT('Ctrl Pts',(-25.3979126089155,-0.962030544502802,
0.));
#235360=CARTESIAN_POINT('Ctrl Pts',(-25.3979126089155,-0.962030544502802,
12.));
#235361=CARTESIAN_POINT('Ctrl Pts',(-25.4222289223155,-0.950507148596968,
0.));
#235362=CARTESIAN_POINT('Ctrl Pts',(-25.4222289223155,-0.950507148596968,
12.));
#235363=CARTESIAN_POINT('Ctrl Pts',(-25.4465852044835,-0.938896449495632,
0.));
#235364=CARTESIAN_POINT('Ctrl Pts',(-25.4465852044835,-0.938896449495632,
12.));
#235365=CARTESIAN_POINT('Ctrl Pts',(-25.4709809474996,-0.927198419885604,
0.));
#235366=CARTESIAN_POINT('Ctrl Pts',(-25.4709809474996,-0.927198419885604,
12.));
#235367=CARTESIAN_POINT('Ctrl Pts',(-25.4954156541787,-0.915413034335333,
0.));
#235368=CARTESIAN_POINT('Ctrl Pts',(-25.4954156541787,-0.915413034335333,
12.));
#235369=CARTESIAN_POINT('Ctrl Pts',(-25.5198888424195,-0.903540269651154,
0.));
#235370=CARTESIAN_POINT('Ctrl Pts',(-25.5198888424195,-0.903540269651154,
12.));
#235371=CARTESIAN_POINT('Ctrl Pts',(-25.5444000508223,-0.891580105349467,
0.));
#235372=CARTESIAN_POINT('Ctrl Pts',(-25.5444000508223,-0.891580105349467,
12.));
#235373=CARTESIAN_POINT('Ctrl Pts',(-25.568948840818,-0.87953252383509,
0.));
#235374=CARTESIAN_POINT('Ctrl Pts',(-25.568948840818,-0.87953252383509,
12.));
#235375=CARTESIAN_POINT('Ctrl Pts',(-25.5935347843616,-0.86739750933947,
0.));
#235376=CARTESIAN_POINT('Ctrl Pts',(-25.5935347843616,-0.86739750933947,
12.));
#235377=CARTESIAN_POINT('Ctrl Pts',(-25.618157453608,-0.855175047037614,
0.));
#235378=CARTESIAN_POINT('Ctrl Pts',(-25.618157453608,-0.855175047037614,
12.));
#235379=CARTESIAN_POINT('Ctrl Pts',(-25.6428164100078,-0.842865122121544,
0.));
#235380=CARTESIAN_POINT('Ctrl Pts',(-25.6428164100078,-0.842865122121544,
12.));
#235381=CARTESIAN_POINT('Ctrl Pts',(-25.6675111931957,-0.830467718864367,
0.));
#235382=CARTESIAN_POINT('Ctrl Pts',(-25.6675111931957,-0.830467718864367,
12.));
#235383=CARTESIAN_POINT('Ctrl Pts',(-25.6922413110172,-0.817982819786719,
0.));
#235384=CARTESIAN_POINT('Ctrl Pts',(-25.6922413110172,-0.817982819786719,
12.));
#235385=CARTESIAN_POINT('Ctrl Pts',(-25.7170062262474,-0.805410404552594,
0.));
#235386=CARTESIAN_POINT('Ctrl Pts',(-25.7170062262474,-0.805410404552594,
12.));
#235387=CARTESIAN_POINT('Ctrl Pts',(-25.7418053757671,-0.792750451613534,
0.));
#235388=CARTESIAN_POINT('Ctrl Pts',(-25.7418053757671,-0.792750451613534,
12.));
#235389=CARTESIAN_POINT('Ctrl Pts',(-25.7666381946871,-0.780002940289025,
0.));
#235390=CARTESIAN_POINT('Ctrl Pts',(-25.7666381946871,-0.780002940289025,
12.));
#235391=CARTESIAN_POINT('Ctrl Pts',(-25.7915041383304,-0.767167852648639,
0.));
#235392=CARTESIAN_POINT('Ctrl Pts',(-25.7915041383304,-0.767167852648639,
12.));
#235393=CARTESIAN_POINT('Ctrl Pts',(-25.816402705995,-0.754245175608288,
0.));
#235394=CARTESIAN_POINT('Ctrl Pts',(-25.816402705995,-0.754245175608288,
12.));
#235395=CARTESIAN_POINT('Ctrl Pts',(-25.841333461908,-0.741234902664697,
0.));
#235396=CARTESIAN_POINT('Ctrl Pts',(-25.841333461908,-0.741234902664697,
12.));
#235397=CARTESIAN_POINT('Ctrl Pts',(-25.8662960624285,-0.728137036485877,
0.));
#235398=CARTESIAN_POINT('Ctrl Pts',(-25.8662960624285,-0.728137036485877,
12.));
#235399=CARTESIAN_POINT('Ctrl Pts',(-25.8912902615141,-0.714951588533753,
0.));
#235400=CARTESIAN_POINT('Ctrl Pts',(-25.8912902615141,-0.714951588533753,
12.));
#235401=CARTESIAN_POINT('Ctrl Pts',(-25.9163158909645,-0.701678575236602,
0.));
#235402=CARTESIAN_POINT('Ctrl Pts',(-25.9163158909645,-0.701678575236602,
12.));
#235403=CARTESIAN_POINT('Ctrl Pts',(-25.941372847213,-0.688318015065678,
0.));
#235404=CARTESIAN_POINT('Ctrl Pts',(-25.941372847213,-0.688318015065678,
12.));
#235405=CARTESIAN_POINT('Ctrl Pts',(-25.9614434298092,-0.677559543215902,
0.));
#235406=CARTESIAN_POINT('Ctrl Pts',(-25.9614434298092,-0.677559543215902,
12.));
#235407=CARTESIAN_POINT('Ctrl Pts',(-25.9765104298171,-0.669451306784415,
0.));
#235408=CARTESIAN_POINT('Ctrl Pts',(-25.9765104298171,-0.669451306784415,
12.));
#235409=CARTESIAN_POINT('Ctrl Pts',(-25.9865613464809,-0.664028313188912,
0.));
#235410=CARTESIAN_POINT('Ctrl Pts',(-25.9865613464809,-0.664028313188912,
12.));
#235411=CARTESIAN_POINT('Ctrl Pts',(-25.991588367311,-0.661312440730891,
0.));
#235412=CARTESIAN_POINT('Ctrl Pts',(-25.991588367311,-0.661312440730891,
12.));
#235413=CARTESIAN_POINT('',(-25.991588367311,-0.661312440730891,0.));
#235414=CARTESIAN_POINT('Ctrl Pts',(-22.4835757167854,-1.76341220531179,
0.));
#235415=CARTESIAN_POINT('Ctrl Pts',(-22.483581992979,-1.76341415538764,
0.));
#235416=CARTESIAN_POINT('Ctrl Pts',(-22.4836387052232,-1.7634206426357,
0.));
#235417=CARTESIAN_POINT('Ctrl Pts',(-22.483856251707,-1.76343813434565,
0.));
#235418=CARTESIAN_POINT('Ctrl Pts',(-22.4844112933129,-1.76347698284792,
0.));
#235419=CARTESIAN_POINT('Ctrl Pts',(-22.4855446605991,-1.76355076045546,
0.));
#235420=CARTESIAN_POINT('Ctrl Pts',(-22.4871115206571,-1.76364784232963,
0.));
#235421=CARTESIAN_POINT('Ctrl Pts',(-22.4890991659478,-1.76376424879505,
0.));
#235422=CARTESIAN_POINT('Ctrl Pts',(-22.4914909094908,-1.76389475965724,
0.));
#235423=CARTESIAN_POINT('Ctrl Pts',(-22.4942693792449,-1.764033938803,0.));
#235424=CARTESIAN_POINT('Ctrl Pts',(-22.4974203063191,-1.76417731243462,
0.));
#235425=CARTESIAN_POINT('Ctrl Pts',(-22.5009332677316,-1.76432160068725,
0.));
#235426=CARTESIAN_POINT('Ctrl Pts',(-22.5047996391978,-1.76446408210366,
0.));
#235427=CARTESIAN_POINT('Ctrl Pts',(-22.5090112700212,-1.76460218257323,
0.));
#235428=CARTESIAN_POINT('Ctrl Pts',(-22.5135590569554,-1.76473303281159,
0.));
#235429=CARTESIAN_POINT('Ctrl Pts',(-22.5184336670207,-1.76485369319896,
0.));
#235430=CARTESIAN_POINT('Ctrl Pts',(-22.5236259635515,-1.76496128643369,
0.));
#235431=CARTESIAN_POINT('Ctrl Pts',(-22.529127665298,-1.76505320262751,
0.));
#235432=CARTESIAN_POINT('Ctrl Pts',(-22.5349313983571,-1.7651271156325,
0.));
#235433=CARTESIAN_POINT('Ctrl Pts',(-22.5410303590891,-1.76518087841492,
0.));
#235434=CARTESIAN_POINT('Ctrl Pts',(-22.5474180954006,-1.76521245524047,
0.));
#235435=CARTESIAN_POINT('Ctrl Pts',(-22.5540882235837,-1.76521983384063,
0.));
#235436=CARTESIAN_POINT('Ctrl Pts',(-22.5610344912501,-1.76520104500449,
0.));
#235437=CARTESIAN_POINT('Ctrl Pts',(-22.5682508499873,-1.76515418518829,
0.));
#235438=CARTESIAN_POINT('Ctrl Pts',(-22.5757315316355,-1.76507744026747,
0.));
#235439=CARTESIAN_POINT('Ctrl Pts',(-22.5834711038024,-1.76496910283088,
0.));
#235440=CARTESIAN_POINT('Ctrl Pts',(-22.5914644078106,-1.76482755288411,
0.));
#235441=CARTESIAN_POINT('Ctrl Pts',(-22.5997065145638,-1.76465124413556,
0.));
#235442=CARTESIAN_POINT('Ctrl Pts',(-22.6081926681342,-1.76443868648015,
0.));
#235443=CARTESIAN_POINT('Ctrl Pts',(-22.6169182517693,-1.76418843543739,
0.));
#235444=CARTESIAN_POINT('Ctrl Pts',(-22.6258787994847,-1.76389909571402,
0.));
#235445=CARTESIAN_POINT('Ctrl Pts',(-22.635069997936,-1.76356932176272,
0.));
#235446=CARTESIAN_POINT('Ctrl Pts',(-22.6444876940425,-1.76319782013914,
0.));
#235447=CARTESIAN_POINT('Ctrl Pts',(-22.6541278938413,-1.76278334912559,
0.));
#235448=CARTESIAN_POINT('Ctrl Pts',(-22.6639867471756,-1.76232471392567,
0.));
#235449=CARTESIAN_POINT('Ctrl Pts',(-22.6740605356699,-1.76182076289525,
0.));
#235450=CARTESIAN_POINT('Ctrl Pts',(-22.6843456585245,-1.76127038310612,
0.));
#235451=CARTESIAN_POINT('Ctrl Pts',(-22.6948386219843,-1.76067249704884,
0.));
#235452=CARTESIAN_POINT('Ctrl Pts',(-22.7055360375481,-1.76002606202399,
0.));
#235453=CARTESIAN_POINT('Ctrl Pts',(-22.7164346186007,-1.75933006905924,
0.));
#235454=CARTESIAN_POINT('Ctrl Pts',(-22.7275311777305,-1.75858354204635,
0.));
#235455=CARTESIAN_POINT('Ctrl Pts',(-22.7388226235565,-1.75778553673249,
0.));
#235456=CARTESIAN_POINT('Ctrl Pts',(-22.7503059556455,-1.75693513908911,
0.));
#235457=CARTESIAN_POINT('Ctrl Pts',(-22.7619782595013,-1.7560314637164,
0.));
#235458=CARTESIAN_POINT('Ctrl Pts',(-22.7738367016115,-1.75507365227127,
0.));
#235459=CARTESIAN_POINT('Ctrl Pts',(-22.7858785242358,-1.75406087182929,
0.));
#235460=CARTESIAN_POINT('Ctrl Pts',(-22.7981010424312,-1.75299231391461,
0.));
#235461=CARTESIAN_POINT('Ctrl Pts',(-22.8105016414712,-1.75186719365589,
0.));
#235462=CARTESIAN_POINT('Ctrl Pts',(-22.8230777741285,-1.75068474890884,
0.));
#235463=CARTESIAN_POINT('Ctrl Pts',(-22.8358269579854,-1.74944423940117,
0.));
#235464=CARTESIAN_POINT('Ctrl Pts',(-22.8487467728075,-1.74814494588492,
0.));
#235465=CARTESIAN_POINT('Ctrl Pts',(-22.8618348580234,-1.74678616930663,
0.));
#235466=CARTESIAN_POINT('Ctrl Pts',(-22.8750889101696,-1.745367229982,0.));
#235467=CARTESIAN_POINT('Ctrl Pts',(-22.8885066803351,-1.74388746677702,
0.));
#235468=CARTESIAN_POINT('Ctrl Pts',(-22.9020859716144,-1.74234623630079,
0.));
#235469=CARTESIAN_POINT('Ctrl Pts',(-22.9158246373365,-1.74074291231057,
0.));
#235470=CARTESIAN_POINT('Ctrl Pts',(-22.9297205792587,-1.73907688511664,
0.));
#235471=CARTESIAN_POINT('Ctrl Pts',(-22.9437717457825,-1.73734756100038,
0.));
#235472=CARTESIAN_POINT('Ctrl Pts',(-22.9579761301062,-1.73555436162771,
0.));
#235473=CARTESIAN_POINT('Ctrl Pts',(-22.9723317685688,-1.73369672350817,
0.));
#235474=CARTESIAN_POINT('Ctrl Pts',(-22.9868367391978,-1.73177409750193,
0.));
#235475=CARTESIAN_POINT('Ctrl Pts',(-23.0014891601891,-1.72978594832137,
0.));
#235476=CARTESIAN_POINT('Ctrl Pts',(-23.0162871884167,-1.72773175404702,
0.));
#235477=CARTESIAN_POINT('Ctrl Pts',(-23.031229017888,-1.72561100564033,
0.));
#235478=CARTESIAN_POINT('Ctrl Pts',(-23.0463128785528,-1.72342320653731,
0.));
#235479=CARTESIAN_POINT('Ctrl Pts',(-23.061537035156,-1.7211678722598,0.));
#235480=CARTESIAN_POINT('Ctrl Pts',(-23.0768997860709,-1.71884453003027,
0.));
#235481=CARTESIAN_POINT('Ctrl Pts',(-23.0923994621216,-1.71645271839311,
0.));
#235482=CARTESIAN_POINT('Ctrl Pts',(-23.1080344254291,-1.71399198684724,
0.));
#235483=CARTESIAN_POINT('Ctrl Pts',(-23.1238030684929,-1.71146189552192,
0.));
#235484=CARTESIAN_POINT('Ctrl Pts',(-23.1397038132358,-1.7088620148546,
0.));
#235485=CARTESIAN_POINT('Ctrl Pts',(-23.1557351100613,-1.70619192527847,
0.));
#235486=CARTESIAN_POINT('Ctrl Pts',(-23.1718954368749,-1.70345121691259,
0.));
#235487=CARTESIAN_POINT('Ctrl Pts',(-23.1881832981848,-1.70063948926987,
0.));
#235488=CARTESIAN_POINT('Ctrl Pts',(-23.2045972243765,-1.69775635099425,
0.));
#235489=CARTESIAN_POINT('Ctrl Pts',(-23.2211357709374,-1.69480141959945,
0.));
#235490=CARTESIAN_POINT('Ctrl Pts',(-23.2377975177014,-1.69177432121716,
0.));
#235491=CARTESIAN_POINT('Ctrl Pts',(-23.2545810680536,-1.6886746903491,
0.));
#235492=CARTESIAN_POINT('Ctrl Pts',(-23.2714850482245,-1.68550216963275,
0.));
#235493=CARTESIAN_POINT('Ctrl Pts',(-23.2885081066949,-1.68225640962181,
0.));
#235494=CARTESIAN_POINT('Ctrl Pts',(-23.3056489135611,-1.67893706857123,
0.));
#235495=CARTESIAN_POINT('Ctrl Pts',(-23.3229061599145,-1.67554381222987,
0.));
#235496=CARTESIAN_POINT('Ctrl Pts',(-23.3402785571866,-1.67207631363905,
0.));
#235497=CARTESIAN_POINT('Ctrl Pts',(-23.3577648365747,-1.66853425293977,
0.));
#235498=CARTESIAN_POINT('Ctrl Pts',(-23.375363748555,-1.66491731718864,
0.));
#235499=CARTESIAN_POINT('Ctrl Pts',(-23.3930740623622,-1.66122520018008,
0.));
#235500=CARTESIAN_POINT('Ctrl Pts',(-23.4108945654803,-1.65745760227507,
0.));
#235501=CARTESIAN_POINT('Ctrl Pts',(-23.4288240631034,-1.6536142302373,
0.));
#235502=CARTESIAN_POINT('Ctrl Pts',(-23.446861377656,-1.64969479707339,
0.));
#235503=CARTESIAN_POINT('Ctrl Pts',(-23.4650053483919,-1.64569902187608,
0.));
#235504=CARTESIAN_POINT('Ctrl Pts',(-23.4832548309638,-1.64162662967524,
0.));
#235505=CARTESIAN_POINT('Ctrl Pts',(-23.5016086970006,-1.63747735129474,
0.));
#235506=CARTESIAN_POINT('Ctrl Pts',(-23.5200658336624,-1.63325092321731,
0.));
#235507=CARTESIAN_POINT('Ctrl Pts',(-23.5386251432278,-1.62894708745231,
0.));
#235508=CARTESIAN_POINT('Ctrl Pts',(-23.5572855427617,-1.62456559140072,
0.));
#235509=CARTESIAN_POINT('Ctrl Pts',(-23.5760459637608,-1.62010618772869,
0.));
#235510=CARTESIAN_POINT('Ctrl Pts',(-23.5949053517996,-1.61556863424697,
0.));
#235511=CARTESIAN_POINT('Ctrl Pts',(-23.6138626661644,-1.61095269379773,
0.));
#235512=CARTESIAN_POINT('Ctrl Pts',(-23.6329168794916,-1.60625813414666,
0.));
#235513=CARTESIAN_POINT('Ctrl Pts',(-23.6520669774863,-1.60148472786588,
0.));
#235514=CARTESIAN_POINT('Ctrl Pts',(-23.6713119586302,-1.59663225222458,
0.));
#235515=CARTESIAN_POINT('Ctrl Pts',(-23.6906508338833,-1.59170048908631,
0.));
#235516=CARTESIAN_POINT('Ctrl Pts',(-23.7100826263835,-1.58668922481222,
0.));
#235517=CARTESIAN_POINT('Ctrl Pts',(-23.7296063711308,-1.58159825017362,
0.));
#235518=CARTESIAN_POINT('Ctrl Pts',(-23.7492211147369,-1.57642736025251,
0.));
#235519=CARTESIAN_POINT('Ctrl Pts',(-23.7689259151869,-1.57117635434412,
0.));
#235520=CARTESIAN_POINT('Ctrl Pts',(-23.788719841588,-1.56584503586844,
0.));
#235521=CARTESIAN_POINT('Ctrl Pts',(-23.8086019739192,-1.56043321228631,
0.));
#235522=CARTESIAN_POINT('Ctrl Pts',(-23.8285714027631,-1.55494069502628,
0.));
#235523=CARTESIAN_POINT('Ctrl Pts',(-23.8486272290698,-1.5493672994053,
0.));
#235524=CARTESIAN_POINT('Ctrl Pts',(-23.8687685639635,-1.54371284453978,
0.));
#235525=CARTESIAN_POINT('Ctrl Pts',(-23.8889945285313,-1.53797715326748,
0.));
#235526=CARTESIAN_POINT('Ctrl Pts',(-23.9093042536119,-1.53216005207462,
0.));
#235527=CARTESIAN_POINT('Ctrl Pts',(-23.9296968795761,-1.52626137103039,
0.));
#235528=CARTESIAN_POINT('Ctrl Pts',(-23.9501715561038,-1.52028094372806,
0.));
#235529=CARTESIAN_POINT('Ctrl Pts',(-23.9707274420145,-1.51421860720628,
0.));
#235530=CARTESIAN_POINT('Ctrl Pts',(-23.991363705093,-1.50807420187702,
0.));
#235531=CARTESIAN_POINT('Ctrl Pts',(-24.0120795219086,-1.50184757146099,
0.));
#235532=CARTESIAN_POINT('Ctrl Pts',(-24.0328740776331,-1.49553856292798,
0.));
#235533=CARTESIAN_POINT('Ctrl Pts',(-24.053746565843,-1.48914702644883,
0.));
#235534=CARTESIAN_POINT('Ctrl Pts',(-24.074696188353,-1.4826728153368,0.));
#235535=CARTESIAN_POINT('Ctrl Pts',(-24.0957221550782,-1.47611578597741,
0.));
#235536=CARTESIAN_POINT('Ctrl Pts',(-24.1168236838827,-1.46947579776992,
0.));
#235537=CARTESIAN_POINT('Ctrl Pts',(-24.1380000004272,-1.46275271307398,
0.));
#235538=CARTESIAN_POINT('Ctrl Pts',(-24.1592503380105,-1.45594639716314,
0.));
#235539=CARTESIAN_POINT('Ctrl Pts',(-24.1805739374033,-1.44905671818721,
0.));
#235540=CARTESIAN_POINT('Ctrl Pts',(-24.2019700467214,-1.44208354711074,
0.));
#235541=CARTESIAN_POINT('Ctrl Pts',(-24.2234379212978,-1.43502675765502,
0.));
#235542=CARTESIAN_POINT('Ctrl Pts',(-24.2449768235485,-1.42788622624851,
0.));
#235543=CARTESIAN_POINT('Ctrl Pts',(-24.2665860228357,-1.42066183198252,
0.));
#235544=CARTESIAN_POINT('Ctrl Pts',(-24.2882647953214,-1.41335345657685,
0.));
#235545=CARTESIAN_POINT('Ctrl Pts',(-24.3100124238316,-1.4059609843434,
0.));
#235546=CARTESIAN_POINT('Ctrl Pts',(-24.3318281977647,-1.3984843021281,
0.));
#235547=CARTESIAN_POINT('Ctrl Pts',(-24.3537114129877,-1.3909232992639,
0.));
#235548=CARTESIAN_POINT('Ctrl Pts',(-24.37566137173,-1.38327786752998,0.));
#235549=CARTESIAN_POINT('Ctrl Pts',(-24.3976773824731,-1.37554790111607,
0.));
#235550=CARTESIAN_POINT('Ctrl Pts',(-24.4197587598337,-1.36773329659954,
0.));
#235551=CARTESIAN_POINT('Ctrl Pts',(-24.4419048244524,-1.35983395290624,
0.));
#235552=CARTESIAN_POINT('Ctrl Pts',(-24.4641149028894,-1.35184977125644,
0.));
#235553=CARTESIAN_POINT('Ctrl Pts',(-24.4863883275135,-1.34378065512335,
0.));
#235554=CARTESIAN_POINT('Ctrl Pts',(-24.5087244363856,-1.33562651019684,
0.));
#235555=CARTESIAN_POINT('Ctrl Pts',(-24.5311225731434,-1.32738724435326,
0.));
#235556=CARTESIAN_POINT('Ctrl Pts',(-24.5535820868671,-1.31906276763669,
0.));
#235557=CARTESIAN_POINT('Ctrl Pts',(-24.576102332018,-1.31065299222023,
0.));
#235558=CARTESIAN_POINT('Ctrl Pts',(-24.5986826684025,-1.30215783236364,
0.));
#235559=CARTESIAN_POINT('Ctrl Pts',(-24.6213224611228,-1.29357720438107,
0.));
#235560=CARTESIAN_POINT('Ctrl Pts',(-24.6440210805278,-1.28491102661513,
0.));
#235561=CARTESIAN_POINT('Ctrl Pts',(-24.666777902156,-1.2761592194164,0.));
#235562=CARTESIAN_POINT('Ctrl Pts',(-24.6895923066837,-1.26732170513497,
0.));
#235563=CARTESIAN_POINT('Ctrl Pts',(-24.7124636797895,-1.25839840807415,
0.));
#235564=CARTESIAN_POINT('Ctrl Pts',(-24.7353914120012,-1.24938925444323,
0.));
#235565=CARTESIAN_POINT('Ctrl Pts',(-24.7583748985439,-1.24029417231988,
0.));
#235566=CARTESIAN_POINT('Ctrl Pts',(-24.78141353918,-1.23111309161843,0.));
#235567=CARTESIAN_POINT('Ctrl Pts',(-24.8045067380536,-1.22184594406526,
0.));
#235568=CARTESIAN_POINT('Ctrl Pts',(-24.8276539035092,-1.21249266318205,
0.));
#235569=CARTESIAN_POINT('Ctrl Pts',(-24.8508544481973,-1.20305318426015,
0.));
#235570=CARTESIAN_POINT('Ctrl Pts',(-24.8741077892074,-1.19352744434059,
0.));
#235571=CARTESIAN_POINT('Ctrl Pts',(-24.8974133481829,-1.18391538220098,
0.));
#235572=CARTESIAN_POINT('Ctrl Pts',(-24.9207705514449,-1.17421693835039,
0.));
#235573=CARTESIAN_POINT('Ctrl Pts',(-24.9441788300932,-1.16443205502852,
0.));
#235574=CARTESIAN_POINT('Ctrl Pts',(-24.9676376201501,-1.15456067621894,
0.));
#235575=CARTESIAN_POINT('Ctrl Pts',(-24.9911463621431,-1.14460274758206,
0.));
#235576=CARTESIAN_POINT('Ctrl Pts',(-25.0147045006193,-1.13455821638535,
0.));
#235577=CARTESIAN_POINT('Ctrl Pts',(-25.0383114836898,-1.12442703144455,
0.));
#235578=CARTESIAN_POINT('Ctrl Pts',(-25.0619667625336,-1.1142091430689,
0.));
#235579=CARTESIAN_POINT('Ctrl Pts',(-25.085669790968,-1.1039045030174,0.));
#235580=CARTESIAN_POINT('Ctrl Pts',(-25.1094200248448,-1.09351306445299,
0.));
#235581=CARTESIAN_POINT('Ctrl Pts',(-25.1332169227415,-1.08303478197174,
0.));
#235582=CARTESIAN_POINT('Ctrl Pts',(-25.1570599469311,-1.0724696116546,
0.));
#235583=CARTESIAN_POINT('Ctrl Pts',(-25.1809485642191,-1.06181751111754,
0.));
#235584=CARTESIAN_POINT('Ctrl Pts',(-25.2048822469027,-1.05107843957925,
0.));
#235585=CARTESIAN_POINT('Ctrl Pts',(-25.2288604735087,-1.04025235791515,
0.));
#235586=CARTESIAN_POINT('Ctrl Pts',(-25.2528827300427,-1.0293392287683,
0.));
#235587=CARTESIAN_POINT('Ctrl Pts',(-25.2769485087268,-1.01833901642272,
0.));
#235588=CARTESIAN_POINT('Ctrl Pts',(-25.3010573055557,-1.00725168656933,
0.));
#235589=CARTESIAN_POINT('Ctrl Pts',(-25.3252086182976,-0.996077206120919,
0.));
#235590=CARTESIAN_POINT('Ctrl Pts',(-25.3494019441444,-0.984815543004089,
0.));
#235591=CARTESIAN_POINT('Ctrl Pts',(-25.3736367778842,-0.973466666000048,
0.));
#235592=CARTESIAN_POINT('Ctrl Pts',(-25.3979126089155,-0.962030544502802,
0.));
#235593=CARTESIAN_POINT('Ctrl Pts',(-25.4222289223155,-0.950507148596968,
0.));
#235594=CARTESIAN_POINT('Ctrl Pts',(-25.4465852044835,-0.938896449495632,
0.));
#235595=CARTESIAN_POINT('Ctrl Pts',(-25.4709809474996,-0.927198419885604,
0.));
#235596=CARTESIAN_POINT('Ctrl Pts',(-25.4954156541787,-0.915413034335333,
0.));
#235597=CARTESIAN_POINT('Ctrl Pts',(-25.5198888424195,-0.903540269651154,
0.));
#235598=CARTESIAN_POINT('Ctrl Pts',(-25.5444000508223,-0.891580105349467,
0.));
#235599=CARTESIAN_POINT('Ctrl Pts',(-25.568948840818,-0.87953252383509,
0.));
#235600=CARTESIAN_POINT('Ctrl Pts',(-25.5935347843616,-0.86739750933947,
0.));
#235601=CARTESIAN_POINT('Ctrl Pts',(-25.618157453608,-0.855175047037614,
0.));
#235602=CARTESIAN_POINT('Ctrl Pts',(-25.6428164100078,-0.842865122121544,
0.));
#235603=CARTESIAN_POINT('Ctrl Pts',(-25.6675111931957,-0.830467718864367,
0.));
#235604=CARTESIAN_POINT('Ctrl Pts',(-25.6922413110172,-0.817982819786719,
0.));
#235605=CARTESIAN_POINT('Ctrl Pts',(-25.7170062262474,-0.805410404552594,
0.));
#235606=CARTESIAN_POINT('Ctrl Pts',(-25.7418053757671,-0.792750451613534,
0.));
#235607=CARTESIAN_POINT('Ctrl Pts',(-25.7666381946871,-0.780002940289025,
0.));
#235608=CARTESIAN_POINT('Ctrl Pts',(-25.7915041383304,-0.767167852648639,
0.));
#235609=CARTESIAN_POINT('Ctrl Pts',(-25.816402705995,-0.754245175608288,
0.));
#235610=CARTESIAN_POINT('Ctrl Pts',(-25.841333461908,-0.741234902664697,
0.));
#235611=CARTESIAN_POINT('Ctrl Pts',(-25.8662960624285,-0.728137036485877,
0.));
#235612=CARTESIAN_POINT('Ctrl Pts',(-25.8912902615141,-0.714951588533753,
0.));
#235613=CARTESIAN_POINT('Ctrl Pts',(-25.9163158909645,-0.701678575236602,
0.));
#235614=CARTESIAN_POINT('Ctrl Pts',(-25.941372847213,-0.688318015065678,
0.));
#235615=CARTESIAN_POINT('Ctrl Pts',(-25.9614434298092,-0.677559543215902,
0.));
#235616=CARTESIAN_POINT('Ctrl Pts',(-25.9765104298171,-0.669451306784415,
0.));
#235617=CARTESIAN_POINT('Ctrl Pts',(-25.9865613464809,-0.664028313188912,
0.));
#235618=CARTESIAN_POINT('Ctrl Pts',(-25.991588367311,-0.661312440730891,
0.));
#235619=CARTESIAN_POINT('',(-25.991588367311,-0.661312440730891,12.));
#235620=CARTESIAN_POINT('Ctrl Pts',(-25.991588367311,-0.661312440730891,
12.));
#235621=CARTESIAN_POINT('Ctrl Pts',(-25.9865613464809,-0.664028313188912,
12.));
#235622=CARTESIAN_POINT('Ctrl Pts',(-25.9765104298171,-0.669451306784415,
12.));
#235623=CARTESIAN_POINT('Ctrl Pts',(-25.9614434298092,-0.677559543215902,
12.));
#235624=CARTESIAN_POINT('Ctrl Pts',(-25.941372847213,-0.688318015065678,
12.));
#235625=CARTESIAN_POINT('Ctrl Pts',(-25.9163158909645,-0.701678575236602,
12.));
#235626=CARTESIAN_POINT('Ctrl Pts',(-25.8912902615141,-0.714951588533753,
12.));
#235627=CARTESIAN_POINT('Ctrl Pts',(-25.8662960624285,-0.728137036485877,
12.));
#235628=CARTESIAN_POINT('Ctrl Pts',(-25.841333461908,-0.741234902664697,
12.));
#235629=CARTESIAN_POINT('Ctrl Pts',(-25.816402705995,-0.754245175608288,
12.));
#235630=CARTESIAN_POINT('Ctrl Pts',(-25.7915041383304,-0.767167852648639,
12.));
#235631=CARTESIAN_POINT('Ctrl Pts',(-25.7666381946871,-0.780002940289025,
12.));
#235632=CARTESIAN_POINT('Ctrl Pts',(-25.7418053757671,-0.792750451613534,
12.));
#235633=CARTESIAN_POINT('Ctrl Pts',(-25.7170062262474,-0.805410404552594,
12.));
#235634=CARTESIAN_POINT('Ctrl Pts',(-25.6922413110172,-0.817982819786719,
12.));
#235635=CARTESIAN_POINT('Ctrl Pts',(-25.6675111931957,-0.830467718864367,
12.));
#235636=CARTESIAN_POINT('Ctrl Pts',(-25.6428164100078,-0.842865122121544,
12.));
#235637=CARTESIAN_POINT('Ctrl Pts',(-25.618157453608,-0.855175047037614,
12.));
#235638=CARTESIAN_POINT('Ctrl Pts',(-25.5935347843616,-0.86739750933947,
12.));
#235639=CARTESIAN_POINT('Ctrl Pts',(-25.568948840818,-0.87953252383509,
12.));
#235640=CARTESIAN_POINT('Ctrl Pts',(-25.5444000508223,-0.891580105349467,
12.));
#235641=CARTESIAN_POINT('Ctrl Pts',(-25.5198888424195,-0.903540269651154,
12.));
#235642=CARTESIAN_POINT('Ctrl Pts',(-25.4954156541787,-0.915413034335333,
12.));
#235643=CARTESIAN_POINT('Ctrl Pts',(-25.4709809474996,-0.927198419885604,
12.));
#235644=CARTESIAN_POINT('Ctrl Pts',(-25.4465852044835,-0.938896449495632,
12.));
#235645=CARTESIAN_POINT('Ctrl Pts',(-25.4222289223155,-0.950507148596968,
12.));
#235646=CARTESIAN_POINT('Ctrl Pts',(-25.3979126089155,-0.962030544502802,
12.));
#235647=CARTESIAN_POINT('Ctrl Pts',(-25.3736367778842,-0.973466666000048,
12.));
#235648=CARTESIAN_POINT('Ctrl Pts',(-25.3494019441444,-0.984815543004089,
12.));
#235649=CARTESIAN_POINT('Ctrl Pts',(-25.3252086182976,-0.996077206120919,
12.));
#235650=CARTESIAN_POINT('Ctrl Pts',(-25.3010573055557,-1.00725168656933,
12.));
#235651=CARTESIAN_POINT('Ctrl Pts',(-25.2769485087268,-1.01833901642272,
12.));
#235652=CARTESIAN_POINT('Ctrl Pts',(-25.2528827300427,-1.0293392287683,
12.));
#235653=CARTESIAN_POINT('Ctrl Pts',(-25.2288604735087,-1.04025235791515,
12.));
#235654=CARTESIAN_POINT('Ctrl Pts',(-25.2048822469027,-1.05107843957925,
12.));
#235655=CARTESIAN_POINT('Ctrl Pts',(-25.1809485642191,-1.06181751111754,
12.));
#235656=CARTESIAN_POINT('Ctrl Pts',(-25.1570599469311,-1.0724696116546,
12.));
#235657=CARTESIAN_POINT('Ctrl Pts',(-25.1332169227415,-1.08303478197174,
12.));
#235658=CARTESIAN_POINT('Ctrl Pts',(-25.1094200248448,-1.09351306445299,
12.));
#235659=CARTESIAN_POINT('Ctrl Pts',(-25.085669790968,-1.1039045030174,12.));
#235660=CARTESIAN_POINT('Ctrl Pts',(-25.0619667625336,-1.1142091430689,
12.));
#235661=CARTESIAN_POINT('Ctrl Pts',(-25.0383114836898,-1.12442703144455,
12.));
#235662=CARTESIAN_POINT('Ctrl Pts',(-25.0147045006193,-1.13455821638535,
12.));
#235663=CARTESIAN_POINT('Ctrl Pts',(-24.9911463621431,-1.14460274758206,
12.));
#235664=CARTESIAN_POINT('Ctrl Pts',(-24.9676376201501,-1.15456067621894,
12.));
#235665=CARTESIAN_POINT('Ctrl Pts',(-24.9441788300932,-1.16443205502852,
12.));
#235666=CARTESIAN_POINT('Ctrl Pts',(-24.9207705514449,-1.17421693835039,
12.));
#235667=CARTESIAN_POINT('Ctrl Pts',(-24.8974133481829,-1.18391538220098,
12.));
#235668=CARTESIAN_POINT('Ctrl Pts',(-24.8741077892074,-1.19352744434059,
12.));
#235669=CARTESIAN_POINT('Ctrl Pts',(-24.8508544481973,-1.20305318426015,
12.));
#235670=CARTESIAN_POINT('Ctrl Pts',(-24.8276539035092,-1.21249266318205,
12.));
#235671=CARTESIAN_POINT('Ctrl Pts',(-24.8045067380536,-1.22184594406526,
12.));
#235672=CARTESIAN_POINT('Ctrl Pts',(-24.78141353918,-1.23111309161843,12.));
#235673=CARTESIAN_POINT('Ctrl Pts',(-24.7583748985439,-1.24029417231988,
12.));
#235674=CARTESIAN_POINT('Ctrl Pts',(-24.7353914120012,-1.24938925444323,
12.));
#235675=CARTESIAN_POINT('Ctrl Pts',(-24.7124636797895,-1.25839840807415,
12.));
#235676=CARTESIAN_POINT('Ctrl Pts',(-24.6895923066837,-1.26732170513497,
12.));
#235677=CARTESIAN_POINT('Ctrl Pts',(-24.666777902156,-1.2761592194164,12.));
#235678=CARTESIAN_POINT('Ctrl Pts',(-24.6440210805278,-1.28491102661513,
12.));
#235679=CARTESIAN_POINT('Ctrl Pts',(-24.6213224611228,-1.29357720438107,
12.));
#235680=CARTESIAN_POINT('Ctrl Pts',(-24.5986826684025,-1.30215783236364,
12.));
#235681=CARTESIAN_POINT('Ctrl Pts',(-24.576102332018,-1.31065299222023,
12.));
#235682=CARTESIAN_POINT('Ctrl Pts',(-24.5535820868671,-1.31906276763669,
12.));
#235683=CARTESIAN_POINT('Ctrl Pts',(-24.5311225731434,-1.32738724435326,
12.));
#235684=CARTESIAN_POINT('Ctrl Pts',(-24.5087244363856,-1.33562651019684,
12.));
#235685=CARTESIAN_POINT('Ctrl Pts',(-24.4863883275135,-1.34378065512335,
12.));
#235686=CARTESIAN_POINT('Ctrl Pts',(-24.4641149028894,-1.35184977125644,
12.));
#235687=CARTESIAN_POINT('Ctrl Pts',(-24.4419048244524,-1.35983395290624,
12.));
#235688=CARTESIAN_POINT('Ctrl Pts',(-24.4197587598337,-1.36773329659954,
12.));
#235689=CARTESIAN_POINT('Ctrl Pts',(-24.3976773824731,-1.37554790111607,
12.));
#235690=CARTESIAN_POINT('Ctrl Pts',(-24.37566137173,-1.38327786752998,12.));
#235691=CARTESIAN_POINT('Ctrl Pts',(-24.3537114129877,-1.3909232992639,
12.));
#235692=CARTESIAN_POINT('Ctrl Pts',(-24.3318281977647,-1.3984843021281,
12.));
#235693=CARTESIAN_POINT('Ctrl Pts',(-24.3100124238316,-1.4059609843434,
12.));
#235694=CARTESIAN_POINT('Ctrl Pts',(-24.2882647953214,-1.41335345657685,
12.));
#235695=CARTESIAN_POINT('Ctrl Pts',(-24.2665860228357,-1.42066183198252,
12.));
#235696=CARTESIAN_POINT('Ctrl Pts',(-24.2449768235485,-1.42788622624851,
12.));
#235697=CARTESIAN_POINT('Ctrl Pts',(-24.2234379212978,-1.43502675765502,
12.));
#235698=CARTESIAN_POINT('Ctrl Pts',(-24.2019700467214,-1.44208354711074,
12.));
#235699=CARTESIAN_POINT('Ctrl Pts',(-24.1805739374033,-1.44905671818721,
12.));
#235700=CARTESIAN_POINT('Ctrl Pts',(-24.1592503380105,-1.45594639716314,
12.));
#235701=CARTESIAN_POINT('Ctrl Pts',(-24.1380000004272,-1.46275271307398,
12.));
#235702=CARTESIAN_POINT('Ctrl Pts',(-24.1168236838827,-1.46947579776992,
12.));
#235703=CARTESIAN_POINT('Ctrl Pts',(-24.0957221550782,-1.47611578597741,
12.));
#235704=CARTESIAN_POINT('Ctrl Pts',(-24.074696188353,-1.4826728153368,12.));
#235705=CARTESIAN_POINT('Ctrl Pts',(-24.053746565843,-1.48914702644883,
12.));
#235706=CARTESIAN_POINT('Ctrl Pts',(-24.0328740776331,-1.49553856292798,
12.));
#235707=CARTESIAN_POINT('Ctrl Pts',(-24.0120795219086,-1.50184757146099,
12.));
#235708=CARTESIAN_POINT('Ctrl Pts',(-23.991363705093,-1.50807420187702,
12.));
#235709=CARTESIAN_POINT('Ctrl Pts',(-23.9707274420145,-1.51421860720628,
12.));
#235710=CARTESIAN_POINT('Ctrl Pts',(-23.9501715561038,-1.52028094372806,
12.));
#235711=CARTESIAN_POINT('Ctrl Pts',(-23.9296968795761,-1.52626137103039,
12.));
#235712=CARTESIAN_POINT('Ctrl Pts',(-23.9093042536119,-1.53216005207462,
12.));
#235713=CARTESIAN_POINT('Ctrl Pts',(-23.8889945285313,-1.53797715326748,
12.));
#235714=CARTESIAN_POINT('Ctrl Pts',(-23.8687685639635,-1.54371284453978,
12.));
#235715=CARTESIAN_POINT('Ctrl Pts',(-23.8486272290698,-1.5493672994053,
12.));
#235716=CARTESIAN_POINT('Ctrl Pts',(-23.8285714027631,-1.55494069502628,
12.));
#235717=CARTESIAN_POINT('Ctrl Pts',(-23.8086019739192,-1.56043321228631,
12.));
#235718=CARTESIAN_POINT('Ctrl Pts',(-23.788719841588,-1.56584503586844,
12.));
#235719=CARTESIAN_POINT('Ctrl Pts',(-23.7689259151869,-1.57117635434412,
12.));
#235720=CARTESIAN_POINT('Ctrl Pts',(-23.7492211147369,-1.57642736025251,
12.));
#235721=CARTESIAN_POINT('Ctrl Pts',(-23.7296063711308,-1.58159825017362,
12.));
#235722=CARTESIAN_POINT('Ctrl Pts',(-23.7100826263835,-1.58668922481222,
12.));
#235723=CARTESIAN_POINT('Ctrl Pts',(-23.6906508338833,-1.59170048908631,
12.));
#235724=CARTESIAN_POINT('Ctrl Pts',(-23.6713119586302,-1.59663225222458,
12.));
#235725=CARTESIAN_POINT('Ctrl Pts',(-23.6520669774863,-1.60148472786588,
12.));
#235726=CARTESIAN_POINT('Ctrl Pts',(-23.6329168794916,-1.60625813414666,
12.));
#235727=CARTESIAN_POINT('Ctrl Pts',(-23.6138626661644,-1.61095269379773,
12.));
#235728=CARTESIAN_POINT('Ctrl Pts',(-23.5949053517996,-1.61556863424697,
12.));
#235729=CARTESIAN_POINT('Ctrl Pts',(-23.5760459637608,-1.62010618772869,
12.));
#235730=CARTESIAN_POINT('Ctrl Pts',(-23.5572855427617,-1.62456559140072,
12.));
#235731=CARTESIAN_POINT('Ctrl Pts',(-23.5386251432278,-1.62894708745231,
12.));
#235732=CARTESIAN_POINT('Ctrl Pts',(-23.5200658336624,-1.63325092321731,
12.));
#235733=CARTESIAN_POINT('Ctrl Pts',(-23.5016086970006,-1.63747735129474,
12.));
#235734=CARTESIAN_POINT('Ctrl Pts',(-23.4832548309638,-1.64162662967524,
12.));
#235735=CARTESIAN_POINT('Ctrl Pts',(-23.4650053483919,-1.64569902187608,
12.));
#235736=CARTESIAN_POINT('Ctrl Pts',(-23.446861377656,-1.64969479707339,
12.));
#235737=CARTESIAN_POINT('Ctrl Pts',(-23.4288240631034,-1.6536142302373,
12.));
#235738=CARTESIAN_POINT('Ctrl Pts',(-23.4108945654803,-1.65745760227507,
12.));
#235739=CARTESIAN_POINT('Ctrl Pts',(-23.3930740623622,-1.66122520018008,
12.));
#235740=CARTESIAN_POINT('Ctrl Pts',(-23.375363748555,-1.66491731718864,
12.));
#235741=CARTESIAN_POINT('Ctrl Pts',(-23.3577648365747,-1.66853425293977,
12.));
#235742=CARTESIAN_POINT('Ctrl Pts',(-23.3402785571866,-1.67207631363905,
12.));
#235743=CARTESIAN_POINT('Ctrl Pts',(-23.3229061599145,-1.67554381222987,
12.));
#235744=CARTESIAN_POINT('Ctrl Pts',(-23.3056489135611,-1.67893706857123,
12.));
#235745=CARTESIAN_POINT('Ctrl Pts',(-23.2885081066949,-1.68225640962181,
12.));
#235746=CARTESIAN_POINT('Ctrl Pts',(-23.2714850482245,-1.68550216963275,
12.));
#235747=CARTESIAN_POINT('Ctrl Pts',(-23.2545810680536,-1.6886746903491,
12.));
#235748=CARTESIAN_POINT('Ctrl Pts',(-23.2377975177014,-1.69177432121716,
12.));
#235749=CARTESIAN_POINT('Ctrl Pts',(-23.2211357709374,-1.69480141959945,
12.));
#235750=CARTESIAN_POINT('Ctrl Pts',(-23.2045972243765,-1.69775635099425,
12.));
#235751=CARTESIAN_POINT('Ctrl Pts',(-23.1881832981848,-1.70063948926987,
12.));
#235752=CARTESIAN_POINT('Ctrl Pts',(-23.1718954368749,-1.70345121691259,
12.));
#235753=CARTESIAN_POINT('Ctrl Pts',(-23.1557351100613,-1.70619192527847,
12.));
#235754=CARTESIAN_POINT('Ctrl Pts',(-23.1397038132358,-1.7088620148546,
12.));
#235755=CARTESIAN_POINT('Ctrl Pts',(-23.1238030684929,-1.71146189552192,
12.));
#235756=CARTESIAN_POINT('Ctrl Pts',(-23.1080344254291,-1.71399198684724,
12.));
#235757=CARTESIAN_POINT('Ctrl Pts',(-23.0923994621216,-1.71645271839311,
12.));
#235758=CARTESIAN_POINT('Ctrl Pts',(-23.0768997860709,-1.71884453003027,
12.));
#235759=CARTESIAN_POINT('Ctrl Pts',(-23.061537035156,-1.7211678722598,12.));
#235760=CARTESIAN_POINT('Ctrl Pts',(-23.0463128785528,-1.72342320653731,
12.));
#235761=CARTESIAN_POINT('Ctrl Pts',(-23.031229017888,-1.72561100564033,
12.));
#235762=CARTESIAN_POINT('Ctrl Pts',(-23.0162871884167,-1.72773175404702,
12.));
#235763=CARTESIAN_POINT('Ctrl Pts',(-23.0014891601891,-1.72978594832137,
12.));
#235764=CARTESIAN_POINT('Ctrl Pts',(-22.9868367391978,-1.73177409750193,
12.));
#235765=CARTESIAN_POINT('Ctrl Pts',(-22.9723317685688,-1.73369672350817,
12.));
#235766=CARTESIAN_POINT('Ctrl Pts',(-22.9579761301062,-1.73555436162771,
12.));
#235767=CARTESIAN_POINT('Ctrl Pts',(-22.9437717457825,-1.73734756100038,
12.));
#235768=CARTESIAN_POINT('Ctrl Pts',(-22.9297205792587,-1.73907688511664,
12.));
#235769=CARTESIAN_POINT('Ctrl Pts',(-22.9158246373365,-1.74074291231057,
12.));
#235770=CARTESIAN_POINT('Ctrl Pts',(-22.9020859716144,-1.74234623630079,
12.));
#235771=CARTESIAN_POINT('Ctrl Pts',(-22.8885066803351,-1.74388746677702,
12.));
#235772=CARTESIAN_POINT('Ctrl Pts',(-22.8750889101696,-1.745367229982,12.));
#235773=CARTESIAN_POINT('Ctrl Pts',(-22.8618348580234,-1.74678616930663,
12.));
#235774=CARTESIAN_POINT('Ctrl Pts',(-22.8487467728075,-1.74814494588492,
12.));
#235775=CARTESIAN_POINT('Ctrl Pts',(-22.8358269579854,-1.74944423940117,
12.));
#235776=CARTESIAN_POINT('Ctrl Pts',(-22.8230777741285,-1.75068474890884,
12.));
#235777=CARTESIAN_POINT('Ctrl Pts',(-22.8105016414712,-1.75186719365589,
12.));
#235778=CARTESIAN_POINT('Ctrl Pts',(-22.7981010424312,-1.75299231391461,
12.));
#235779=CARTESIAN_POINT('Ctrl Pts',(-22.7858785242358,-1.75406087182929,
12.));
#235780=CARTESIAN_POINT('Ctrl Pts',(-22.7738367016115,-1.75507365227127,
12.));
#235781=CARTESIAN_POINT('Ctrl Pts',(-22.7619782595013,-1.7560314637164,
12.));
#235782=CARTESIAN_POINT('Ctrl Pts',(-22.7503059556455,-1.75693513908911,
12.));
#235783=CARTESIAN_POINT('Ctrl Pts',(-22.7388226235565,-1.75778553673249,
12.));
#235784=CARTESIAN_POINT('Ctrl Pts',(-22.7275311777305,-1.75858354204635,
12.));
#235785=CARTESIAN_POINT('Ctrl Pts',(-22.7164346186007,-1.75933006905924,
12.));
#235786=CARTESIAN_POINT('Ctrl Pts',(-22.7055360375481,-1.76002606202399,
12.));
#235787=CARTESIAN_POINT('Ctrl Pts',(-22.6948386219843,-1.76067249704884,
12.));
#235788=CARTESIAN_POINT('Ctrl Pts',(-22.6843456585245,-1.76127038310612,
12.));
#235789=CARTESIAN_POINT('Ctrl Pts',(-22.6740605356699,-1.76182076289525,
12.));
#235790=CARTESIAN_POINT('Ctrl Pts',(-22.6639867471756,-1.76232471392567,
12.));
#235791=CARTESIAN_POINT('Ctrl Pts',(-22.6541278938413,-1.76278334912559,
12.));
#235792=CARTESIAN_POINT('Ctrl Pts',(-22.6444876940425,-1.76319782013914,
12.));
#235793=CARTESIAN_POINT('Ctrl Pts',(-22.635069997936,-1.76356932176272,
12.));
#235794=CARTESIAN_POINT('Ctrl Pts',(-22.6258787994847,-1.76389909571402,
12.));
#235795=CARTESIAN_POINT('Ctrl Pts',(-22.6169182517693,-1.76418843543739,
12.));
#235796=CARTESIAN_POINT('Ctrl Pts',(-22.6081926681342,-1.76443868648015,
12.));
#235797=CARTESIAN_POINT('Ctrl Pts',(-22.5997065145638,-1.76465124413556,
12.));
#235798=CARTESIAN_POINT('Ctrl Pts',(-22.5914644078106,-1.76482755288411,
12.));
#235799=CARTESIAN_POINT('Ctrl Pts',(-22.5834711038024,-1.76496910283088,
12.));
#235800=CARTESIAN_POINT('Ctrl Pts',(-22.5757315316355,-1.76507744026747,
12.));
#235801=CARTESIAN_POINT('Ctrl Pts',(-22.5682508499873,-1.76515418518829,
12.));
#235802=CARTESIAN_POINT('Ctrl Pts',(-22.5610344912501,-1.76520104500449,
12.));
#235803=CARTESIAN_POINT('Ctrl Pts',(-22.5540882235837,-1.76521983384063,
12.));
#235804=CARTESIAN_POINT('Ctrl Pts',(-22.5474180954006,-1.76521245524047,
12.));
#235805=CARTESIAN_POINT('Ctrl Pts',(-22.5410303590891,-1.76518087841492,
12.));
#235806=CARTESIAN_POINT('Ctrl Pts',(-22.5349313983571,-1.7651271156325,
12.));
#235807=CARTESIAN_POINT('Ctrl Pts',(-22.529127665298,-1.76505320262751,
12.));
#235808=CARTESIAN_POINT('Ctrl Pts',(-22.5236259635515,-1.76496128643369,
12.));
#235809=CARTESIAN_POINT('Ctrl Pts',(-22.5184336670207,-1.76485369319896,
12.));
#235810=CARTESIAN_POINT('Ctrl Pts',(-22.5135590569554,-1.76473303281159,
12.));
#235811=CARTESIAN_POINT('Ctrl Pts',(-22.5090112700212,-1.76460218257323,
12.));
#235812=CARTESIAN_POINT('Ctrl Pts',(-22.5047996391978,-1.76446408210366,
12.));
#235813=CARTESIAN_POINT('Ctrl Pts',(-22.5009332677316,-1.76432160068725,
12.));
#235814=CARTESIAN_POINT('Ctrl Pts',(-22.4974203063191,-1.76417731243462,
12.));
#235815=CARTESIAN_POINT('Ctrl Pts',(-22.4942693792449,-1.764033938803,12.));
#235816=CARTESIAN_POINT('Ctrl Pts',(-22.4914909094908,-1.76389475965724,
12.));
#235817=CARTESIAN_POINT('Ctrl Pts',(-22.4890991659478,-1.76376424879505,
12.));
#235818=CARTESIAN_POINT('Ctrl Pts',(-22.4871115206571,-1.76364784232963,
12.));
#235819=CARTESIAN_POINT('Ctrl Pts',(-22.4855446605991,-1.76355076045546,
12.));
#235820=CARTESIAN_POINT('Ctrl Pts',(-22.4844112933129,-1.76347698284792,
12.));
#235821=CARTESIAN_POINT('Ctrl Pts',(-22.483856251707,-1.76343813434565,
12.));
#235822=CARTESIAN_POINT('Ctrl Pts',(-22.4836387052232,-1.7634206426357,
12.));
#235823=CARTESIAN_POINT('Ctrl Pts',(-22.483581992979,-1.76341415538764,
12.));
#235824=CARTESIAN_POINT('Ctrl Pts',(-22.4835757167854,-1.76341220531179,
12.));
#235825=CARTESIAN_POINT('',(-25.991588367311,-0.661312440730891,0.));
#235826=CARTESIAN_POINT('Origin',(-21.1389261070099,3.92374859571501,0.));
#235827=CARTESIAN_POINT('',(-22.1738711152697,4.11585220600461,12.));
#235828=CARTESIAN_POINT('',(-10.5694630535049,1.96187429785751,12.));
#235829=CARTESIAN_POINT('',(-22.1738711152697,4.11585220600461,0.));
#235830=CARTESIAN_POINT('',(-22.1738711152697,4.11585220600461,0.));
#235831=CARTESIAN_POINT('',(-10.5694630535049,1.96187429785751,0.));
#235832=CARTESIAN_POINT('Ctrl Pts',(-25.991588367311,0.661312440730901,
0.));
#235833=CARTESIAN_POINT('Ctrl Pts',(-25.991588367311,0.661312440730901,
12.));
#235834=CARTESIAN_POINT('Ctrl Pts',(-25.9865613464773,0.664028313187627,
0.));
#235835=CARTESIAN_POINT('Ctrl Pts',(-25.9865613464773,0.664028313187627,
12.));
#235836=CARTESIAN_POINT('Ctrl Pts',(-25.9765104298071,0.669451306780825,
0.));
#235837=CARTESIAN_POINT('Ctrl Pts',(-25.9765104298071,0.669451306780825,
12.));
#235838=CARTESIAN_POINT('Ctrl Pts',(-25.9614434297919,0.677559543209725,
0.));
#235839=CARTESIAN_POINT('Ctrl Pts',(-25.9614434297919,0.677559543209725,
12.));
#235840=CARTESIAN_POINT('Ctrl Pts',(-25.9413728471909,0.688318015057729,
0.));
#235841=CARTESIAN_POINT('Ctrl Pts',(-25.9413728471909,0.688318015057729,
12.));
#235842=CARTESIAN_POINT('Ctrl Pts',(-25.9163158909426,0.701678575228756,
0.));
#235843=CARTESIAN_POINT('Ctrl Pts',(-25.9163158909426,0.701678575228756,
12.));
#235844=CARTESIAN_POINT('Ctrl Pts',(-25.891290261497,0.714951588527638,
0.));
#235845=CARTESIAN_POINT('Ctrl Pts',(-25.891290261497,0.714951588527638,
12.));
#235846=CARTESIAN_POINT('Ctrl Pts',(-25.8662960624185,0.728137036482335,
0.));
#235847=CARTESIAN_POINT('Ctrl Pts',(-25.8662960624185,0.728137036482335,
12.));
#235848=CARTESIAN_POINT('Ctrl Pts',(-25.8413334619055,0.741234902663807,
0.));
#235849=CARTESIAN_POINT('Ctrl Pts',(-25.8413334619055,0.741234902663807,
12.));
#235850=CARTESIAN_POINT('Ctrl Pts',(-25.8164027059984,0.754245175609524,
0.));
#235851=CARTESIAN_POINT('Ctrl Pts',(-25.8164027059984,0.754245175609524,
12.));
#235852=CARTESIAN_POINT('Ctrl Pts',(-25.7915041383376,0.767167852651168,
0.));
#235853=CARTESIAN_POINT('Ctrl Pts',(-25.7915041383376,0.767167852651168,
12.));
#235854=CARTESIAN_POINT('Ctrl Pts',(-25.7666381946955,0.780002940291965,
0.));
#235855=CARTESIAN_POINT('Ctrl Pts',(-25.7666381946955,0.780002940291965,
12.));
#235856=CARTESIAN_POINT('Ctrl Pts',(-25.7418053757746,0.792750451616127,
0.));
#235857=CARTESIAN_POINT('Ctrl Pts',(-25.7418053757746,0.792750451616127,
12.));
#235858=CARTESIAN_POINT('Ctrl Pts',(-25.7170062262525,0.805410404554352,
0.));
#235859=CARTESIAN_POINT('Ctrl Pts',(-25.7170062262525,0.805410404554352,
12.));
#235860=CARTESIAN_POINT('Ctrl Pts',(-25.6922413110194,0.817982819787464,
0.));
#235861=CARTESIAN_POINT('Ctrl Pts',(-25.6922413110194,0.817982819787464,
12.));
#235862=CARTESIAN_POINT('Ctrl Pts',(-25.6675111931952,0.830467718864205,
0.));
#235863=CARTESIAN_POINT('Ctrl Pts',(-25.6675111931952,0.830467718864205,
12.));
#235864=CARTESIAN_POINT('Ctrl Pts',(-25.6428164100055,0.842865122120758,
0.));
#235865=CARTESIAN_POINT('Ctrl Pts',(-25.6428164100055,0.842865122120758,
12.));
#235866=CARTESIAN_POINT('Ctrl Pts',(-25.6181574536049,0.855175047036549,
0.));
#235867=CARTESIAN_POINT('Ctrl Pts',(-25.6181574536049,0.855175047036549,
12.));
#235868=CARTESIAN_POINT('Ctrl Pts',(-25.5935347843585,0.867397509338431,
0.));
#235869=CARTESIAN_POINT('Ctrl Pts',(-25.5935347843585,0.867397509338431,
12.));
#235870=CARTESIAN_POINT('Ctrl Pts',(-25.5689488408156,0.879532523834294,
0.));
#235871=CARTESIAN_POINT('Ctrl Pts',(-25.5689488408156,0.879532523834294,
12.));
#235872=CARTESIAN_POINT('Ctrl Pts',(-25.5444000508211,0.89158010534904,
0.));
#235873=CARTESIAN_POINT('Ctrl Pts',(-25.5444000508211,0.89158010534904,
12.));
#235874=CARTESIAN_POINT('Ctrl Pts',(-25.5198888424194,0.903540269651106,
0.));
#235875=CARTESIAN_POINT('Ctrl Pts',(-25.5198888424194,0.903540269651106,
12.));
#235876=CARTESIAN_POINT('Ctrl Pts',(-25.4954156541795,0.915413034335613,
0.));
#235877=CARTESIAN_POINT('Ctrl Pts',(-25.4954156541795,0.915413034335613,
12.));
#235878=CARTESIAN_POINT('Ctrl Pts',(-25.4709809475009,0.927198419886094,
0.));
#235879=CARTESIAN_POINT('Ctrl Pts',(-25.4709809475009,0.927198419886094,
12.));
#235880=CARTESIAN_POINT('Ctrl Pts',(-25.4465852044849,0.938896449496192,
0.));
#235881=CARTESIAN_POINT('Ctrl Pts',(-25.4465852044849,0.938896449496192,
12.));
#235882=CARTESIAN_POINT('Ctrl Pts',(-25.4222289223167,0.950507148597468,
0.));
#235883=CARTESIAN_POINT('Ctrl Pts',(-25.4222289223167,0.950507148597468,
12.));
#235884=CARTESIAN_POINT('Ctrl Pts',(-25.3979126089163,0.962030544503142,
0.));
#235885=CARTESIAN_POINT('Ctrl Pts',(-25.3979126089163,0.962030544503142,
12.));
#235886=CARTESIAN_POINT('Ctrl Pts',(-25.3736367778845,0.973466666000163,
0.));
#235887=CARTESIAN_POINT('Ctrl Pts',(-25.3736367778845,0.973466666000163,
12.));
#235888=CARTESIAN_POINT('Ctrl Pts',(-25.3494019441441,0.984815543003973,
0.));
#235889=CARTESIAN_POINT('Ctrl Pts',(-25.3494019441441,0.984815543003973,
12.));
#235890=CARTESIAN_POINT('Ctrl Pts',(-25.3252086182968,0.996077206120624,
0.));
#235891=CARTESIAN_POINT('Ctrl Pts',(-25.3252086182968,0.996077206120624,
12.));
#235892=CARTESIAN_POINT('Ctrl Pts',(-25.3010573055547,1.00725168656896,
0.));
#235893=CARTESIAN_POINT('Ctrl Pts',(-25.3010573055547,1.00725168656896,
12.));
#235894=CARTESIAN_POINT('Ctrl Pts',(-25.276948508726,1.01833901642237,0.));
#235895=CARTESIAN_POINT('Ctrl Pts',(-25.276948508726,1.01833901642237,12.));
#235896=CARTESIAN_POINT('Ctrl Pts',(-25.2528827300422,1.02933922876806,
0.));
#235897=CARTESIAN_POINT('Ctrl Pts',(-25.2528827300422,1.02933922876806,
12.));
#235898=CARTESIAN_POINT('Ctrl Pts',(-25.2288604735086,1.04025235791507,
0.));
#235899=CARTESIAN_POINT('Ctrl Pts',(-25.2288604735086,1.04025235791507,
12.));
#235900=CARTESIAN_POINT('Ctrl Pts',(-25.2048822469028,1.05107843957931,
0.));
#235901=CARTESIAN_POINT('Ctrl Pts',(-25.2048822469028,1.05107843957931,
12.));
#235902=CARTESIAN_POINT('Ctrl Pts',(-25.1809485642192,1.06181751111768,
0.));
#235903=CARTESIAN_POINT('Ctrl Pts',(-25.1809485642192,1.06181751111768,
12.));
#235904=CARTESIAN_POINT('Ctrl Pts',(-25.157059946931,1.07246961165475,0.));
#235905=CARTESIAN_POINT('Ctrl Pts',(-25.157059946931,1.07246961165475,12.));
#235906=CARTESIAN_POINT('Ctrl Pts',(-25.1332169227413,1.08303478197187,
0.));
#235907=CARTESIAN_POINT('Ctrl Pts',(-25.1332169227413,1.08303478197187,
12.));
#235908=CARTESIAN_POINT('Ctrl Pts',(-25.1094200248446,1.09351306445308,
0.));
#235909=CARTESIAN_POINT('Ctrl Pts',(-25.1094200248446,1.09351306445308,
12.));
#235910=CARTESIAN_POINT('Ctrl Pts',(-25.0856697909679,1.10390450301745,
0.));
#235911=CARTESIAN_POINT('Ctrl Pts',(-25.0856697909679,1.10390450301745,
12.));
#235912=CARTESIAN_POINT('Ctrl Pts',(-25.0619667625336,1.11420914306889,
0.));
#235913=CARTESIAN_POINT('Ctrl Pts',(-25.0619667625336,1.11420914306889,
12.));
#235914=CARTESIAN_POINT('Ctrl Pts',(-25.0383114836899,1.12442703144451,
0.));
#235915=CARTESIAN_POINT('Ctrl Pts',(-25.0383114836899,1.12442703144451,
12.));
#235916=CARTESIAN_POINT('Ctrl Pts',(-25.0147045006196,1.1345582163853,0.));
#235917=CARTESIAN_POINT('Ctrl Pts',(-25.0147045006196,1.1345582163853,12.));
#235918=CARTESIAN_POINT('Ctrl Pts',(-24.9911463621433,1.144602747582,0.));
#235919=CARTESIAN_POINT('Ctrl Pts',(-24.9911463621433,1.144602747582,12.));
#235920=CARTESIAN_POINT('Ctrl Pts',(-24.9676376201502,1.15456067621889,
0.));
#235921=CARTESIAN_POINT('Ctrl Pts',(-24.9676376201502,1.15456067621889,
12.));
#235922=CARTESIAN_POINT('Ctrl Pts',(-24.9441788300932,1.16443205502849,
0.));
#235923=CARTESIAN_POINT('Ctrl Pts',(-24.9441788300932,1.16443205502849,
12.));
#235924=CARTESIAN_POINT('Ctrl Pts',(-24.9207705514449,1.17421693835041,
0.));
#235925=CARTESIAN_POINT('Ctrl Pts',(-24.9207705514449,1.17421693835041,
12.));
#235926=CARTESIAN_POINT('Ctrl Pts',(-24.8974133481829,1.18391538220103,
0.));
#235927=CARTESIAN_POINT('Ctrl Pts',(-24.8974133481829,1.18391538220103,
12.));
#235928=CARTESIAN_POINT('Ctrl Pts',(-24.8741077892075,1.19352744434064,
0.));
#235929=CARTESIAN_POINT('Ctrl Pts',(-24.8741077892075,1.19352744434064,
12.));
#235930=CARTESIAN_POINT('Ctrl Pts',(-24.8508544481974,1.2030531842602,0.));
#235931=CARTESIAN_POINT('Ctrl Pts',(-24.8508544481974,1.2030531842602,12.));
#235932=CARTESIAN_POINT('Ctrl Pts',(-24.8276539035092,1.21249266318208,
0.));
#235933=CARTESIAN_POINT('Ctrl Pts',(-24.8276539035092,1.21249266318208,
12.));
#235934=CARTESIAN_POINT('Ctrl Pts',(-24.8045067380536,1.22184594406528,
0.));
#235935=CARTESIAN_POINT('Ctrl Pts',(-24.8045067380536,1.22184594406528,
12.));
#235936=CARTESIAN_POINT('Ctrl Pts',(-24.7814135391799,1.23111309161843,
0.));
#235937=CARTESIAN_POINT('Ctrl Pts',(-24.7814135391799,1.23111309161843,
12.));
#235938=CARTESIAN_POINT('Ctrl Pts',(-24.7583748985438,1.24029417231989,
0.));
#235939=CARTESIAN_POINT('Ctrl Pts',(-24.7583748985438,1.24029417231989,
12.));
#235940=CARTESIAN_POINT('Ctrl Pts',(-24.7353914120011,1.24938925444325,
0.));
#235941=CARTESIAN_POINT('Ctrl Pts',(-24.7353914120011,1.24938925444325,
12.));
#235942=CARTESIAN_POINT('Ctrl Pts',(-24.7124636797894,1.25839840807418,
0.));
#235943=CARTESIAN_POINT('Ctrl Pts',(-24.7124636797894,1.25839840807418,
12.));
#235944=CARTESIAN_POINT('Ctrl Pts',(-24.6895923066836,1.267321705135,0.));
#235945=CARTESIAN_POINT('Ctrl Pts',(-24.6895923066836,1.267321705135,12.));
#235946=CARTESIAN_POINT('Ctrl Pts',(-24.666777902156,1.27615921941642,0.));
#235947=CARTESIAN_POINT('Ctrl Pts',(-24.666777902156,1.27615921941642,12.));
#235948=CARTESIAN_POINT('Ctrl Pts',(-24.6440210805278,1.28491102661514,
0.));
#235949=CARTESIAN_POINT('Ctrl Pts',(-24.6440210805278,1.28491102661514,
12.));
#235950=CARTESIAN_POINT('Ctrl Pts',(-24.6213224611229,1.29357720438107,
0.));
#235951=CARTESIAN_POINT('Ctrl Pts',(-24.6213224611229,1.29357720438107,
12.));
#235952=CARTESIAN_POINT('Ctrl Pts',(-24.5986826684027,1.30215783236362,
0.));
#235953=CARTESIAN_POINT('Ctrl Pts',(-24.5986826684027,1.30215783236362,
12.));
#235954=CARTESIAN_POINT('Ctrl Pts',(-24.5761023320183,1.31065299222021,
0.));
#235955=CARTESIAN_POINT('Ctrl Pts',(-24.5761023320183,1.31065299222021,
12.));
#235956=CARTESIAN_POINT('Ctrl Pts',(-24.5535820868674,1.31906276763668,
0.));
#235957=CARTESIAN_POINT('Ctrl Pts',(-24.5535820868674,1.31906276763668,
12.));
#235958=CARTESIAN_POINT('Ctrl Pts',(-24.5311225731435,1.32738724435326,
0.));
#235959=CARTESIAN_POINT('Ctrl Pts',(-24.5311225731435,1.32738724435326,
12.));
#235960=CARTESIAN_POINT('Ctrl Pts',(-24.5087244363856,1.33562651019686,
0.));
#235961=CARTESIAN_POINT('Ctrl Pts',(-24.5087244363856,1.33562651019686,
12.));
#235962=CARTESIAN_POINT('Ctrl Pts',(-24.4863883275134,1.34378065512337,
0.));
#235963=CARTESIAN_POINT('Ctrl Pts',(-24.4863883275134,1.34378065512337,
12.));
#235964=CARTESIAN_POINT('Ctrl Pts',(-24.4641149028892,1.35184977125648,
0.));
#235965=CARTESIAN_POINT('Ctrl Pts',(-24.4641149028892,1.35184977125648,
12.));
#235966=CARTESIAN_POINT('Ctrl Pts',(-24.4419048244523,1.35983395290627,
0.));
#235967=CARTESIAN_POINT('Ctrl Pts',(-24.4419048244523,1.35983395290627,
12.));
#235968=CARTESIAN_POINT('Ctrl Pts',(-24.4197587598337,1.36773329659956,
0.));
#235969=CARTESIAN_POINT('Ctrl Pts',(-24.4197587598337,1.36773329659956,
12.));
#235970=CARTESIAN_POINT('Ctrl Pts',(-24.3976773824732,1.37554790111609,
0.));
#235971=CARTESIAN_POINT('Ctrl Pts',(-24.3976773824732,1.37554790111609,
12.));
#235972=CARTESIAN_POINT('Ctrl Pts',(-24.3756613717299,1.38327786752998,
0.));
#235973=CARTESIAN_POINT('Ctrl Pts',(-24.3756613717299,1.38327786752998,
12.));
#235974=CARTESIAN_POINT('Ctrl Pts',(-24.3537114129875,1.39092329926388,
0.));
#235975=CARTESIAN_POINT('Ctrl Pts',(-24.3537114129875,1.39092329926388,
12.));
#235976=CARTESIAN_POINT('Ctrl Pts',(-24.3318281977643,1.39848430212807,
0.));
#235977=CARTESIAN_POINT('Ctrl Pts',(-24.3318281977643,1.39848430212807,
12.));
#235978=CARTESIAN_POINT('Ctrl Pts',(-24.3100124238311,1.40596098434337,
0.));
#235979=CARTESIAN_POINT('Ctrl Pts',(-24.3100124238311,1.40596098434337,
12.));
#235980=CARTESIAN_POINT('Ctrl Pts',(-24.288264795321,1.41335345657682,0.));
#235981=CARTESIAN_POINT('Ctrl Pts',(-24.288264795321,1.41335345657682,12.));
#235982=CARTESIAN_POINT('Ctrl Pts',(-24.2665860228356,1.42066183198252,
0.));
#235983=CARTESIAN_POINT('Ctrl Pts',(-24.2665860228356,1.42066183198252,
12.));
#235984=CARTESIAN_POINT('Ctrl Pts',(-24.2449768235488,1.42788622624854,
0.));
#235985=CARTESIAN_POINT('Ctrl Pts',(-24.2449768235488,1.42788622624854,
12.));
#235986=CARTESIAN_POINT('Ctrl Pts',(-24.2234379212984,1.43502675765508,
0.));
#235987=CARTESIAN_POINT('Ctrl Pts',(-24.2234379212984,1.43502675765508,
12.));
#235988=CARTESIAN_POINT('Ctrl Pts',(-24.201970046722,1.44208354711082,0.));
#235989=CARTESIAN_POINT('Ctrl Pts',(-24.201970046722,1.44208354711082,12.));
#235990=CARTESIAN_POINT('Ctrl Pts',(-24.1805739374038,1.44905671818727,
0.));
#235991=CARTESIAN_POINT('Ctrl Pts',(-24.1805739374038,1.44905671818727,
12.));
#235992=CARTESIAN_POINT('Ctrl Pts',(-24.1592503380107,1.45594639716317,
0.));
#235993=CARTESIAN_POINT('Ctrl Pts',(-24.1592503380107,1.45594639716317,
12.));
#235994=CARTESIAN_POINT('Ctrl Pts',(-24.1380000004272,1.46275271307397,
0.));
#235995=CARTESIAN_POINT('Ctrl Pts',(-24.1380000004272,1.46275271307397,
12.));
#235996=CARTESIAN_POINT('Ctrl Pts',(-24.1168236838824,1.46947579776991,
0.));
#235997=CARTESIAN_POINT('Ctrl Pts',(-24.1168236838824,1.46947579776991,
12.));
#235998=CARTESIAN_POINT('Ctrl Pts',(-24.0957221550778,1.47611578597742,
0.));
#235999=CARTESIAN_POINT('Ctrl Pts',(-24.0957221550778,1.47611578597742,
12.));
#236000=CARTESIAN_POINT('Ctrl Pts',(-24.0746961883528,1.48267281533683,
0.));
#236001=CARTESIAN_POINT('Ctrl Pts',(-24.0746961883528,1.48267281533683,
12.));
#236002=CARTESIAN_POINT('Ctrl Pts',(-24.0537465658429,1.48914702644887,
0.));
#236003=CARTESIAN_POINT('Ctrl Pts',(-24.0537465658429,1.48914702644887,
12.));
#236004=CARTESIAN_POINT('Ctrl Pts',(-24.0328740776331,1.49553856292801,
0.));
#236005=CARTESIAN_POINT('Ctrl Pts',(-24.0328740776331,1.49553856292801,
12.));
#236006=CARTESIAN_POINT('Ctrl Pts',(-24.0120795219086,1.50184757146098,
0.));
#236007=CARTESIAN_POINT('Ctrl Pts',(-24.0120795219086,1.50184757146098,
12.));
#236008=CARTESIAN_POINT('Ctrl Pts',(-23.9913637050927,1.50807420187694,
0.));
#236009=CARTESIAN_POINT('Ctrl Pts',(-23.9913637050927,1.50807420187694,
12.));
#236010=CARTESIAN_POINT('Ctrl Pts',(-23.970727442014,1.51421860720614,0.));
#236011=CARTESIAN_POINT('Ctrl Pts',(-23.970727442014,1.51421860720614,12.));
#236012=CARTESIAN_POINT('Ctrl Pts',(-23.9501715561033,1.52028094372792,
0.));
#236013=CARTESIAN_POINT('Ctrl Pts',(-23.9501715561033,1.52028094372792,
12.));
#236014=CARTESIAN_POINT('Ctrl Pts',(-23.9296968795757,1.52626137103032,
0.));
#236015=CARTESIAN_POINT('Ctrl Pts',(-23.9296968795757,1.52626137103032,
12.));
#236016=CARTESIAN_POINT('Ctrl Pts',(-23.9093042536119,1.53216005207463,
0.));
#236017=CARTESIAN_POINT('Ctrl Pts',(-23.9093042536119,1.53216005207463,
12.));
#236018=CARTESIAN_POINT('Ctrl Pts',(-23.8889945285318,1.53797715326758,
0.));
#236019=CARTESIAN_POINT('Ctrl Pts',(-23.8889945285318,1.53797715326758,
12.));
#236020=CARTESIAN_POINT('Ctrl Pts',(-23.8687685639642,1.5437128445399,0.));
#236021=CARTESIAN_POINT('Ctrl Pts',(-23.8687685639642,1.5437128445399,12.));
#236022=CARTESIAN_POINT('Ctrl Pts',(-23.8486272290705,1.54936729940541,
0.));
#236023=CARTESIAN_POINT('Ctrl Pts',(-23.8486272290705,1.54936729940541,
12.));
#236024=CARTESIAN_POINT('Ctrl Pts',(-23.8285714027636,1.55494069502635,
0.));
#236025=CARTESIAN_POINT('Ctrl Pts',(-23.8285714027636,1.55494069502635,
12.));
#236026=CARTESIAN_POINT('Ctrl Pts',(-23.8086019739194,1.56043321228633,
0.));
#236027=CARTESIAN_POINT('Ctrl Pts',(-23.8086019739194,1.56043321228633,
12.));
#236028=CARTESIAN_POINT('Ctrl Pts',(-23.7887198415878,1.56584503586843,
0.));
#236029=CARTESIAN_POINT('Ctrl Pts',(-23.7887198415878,1.56584503586843,
12.));
#236030=CARTESIAN_POINT('Ctrl Pts',(-23.7689259151862,1.57117635434408,
0.));
#236031=CARTESIAN_POINT('Ctrl Pts',(-23.7689259151862,1.57117635434408,
12.));
#236032=CARTESIAN_POINT('Ctrl Pts',(-23.749221114736,1.57642736025246,0.));
#236033=CARTESIAN_POINT('Ctrl Pts',(-23.749221114736,1.57642736025246,12.));
#236034=CARTESIAN_POINT('Ctrl Pts',(-23.72960637113,1.58159825017358,0.));
#236035=CARTESIAN_POINT('Ctrl Pts',(-23.72960637113,1.58159825017358,12.));
#236036=CARTESIAN_POINT('Ctrl Pts',(-23.710082626383,1.58668922481221,0.));
#236037=CARTESIAN_POINT('Ctrl Pts',(-23.710082626383,1.58668922481221,12.));
#236038=CARTESIAN_POINT('Ctrl Pts',(-23.6906508338833,1.59170048908633,
0.));
#236039=CARTESIAN_POINT('Ctrl Pts',(-23.6906508338833,1.59170048908633,
12.));
#236040=CARTESIAN_POINT('Ctrl Pts',(-23.671311958631,1.59663225222463,0.));
#236041=CARTESIAN_POINT('Ctrl Pts',(-23.671311958631,1.59663225222463,12.));
#236042=CARTESIAN_POINT('Ctrl Pts',(-23.6520669774876,1.60148472786595,
0.));
#236043=CARTESIAN_POINT('Ctrl Pts',(-23.6520669774876,1.60148472786595,
12.));
#236044=CARTESIAN_POINT('Ctrl Pts',(-23.6329168794929,1.60625813414672,
0.));
#236045=CARTESIAN_POINT('Ctrl Pts',(-23.6329168794929,1.60625813414672,
12.));
#236046=CARTESIAN_POINT('Ctrl Pts',(-23.6138626661653,1.61095269379778,
0.));
#236047=CARTESIAN_POINT('Ctrl Pts',(-23.6138626661653,1.61095269379778,
12.));
#236048=CARTESIAN_POINT('Ctrl Pts',(-23.5949053517997,1.61556863424698,
0.));
#236049=CARTESIAN_POINT('Ctrl Pts',(-23.5949053517997,1.61556863424698,
12.));
#236050=CARTESIAN_POINT('Ctrl Pts',(-23.57604596376,1.62010618772866,0.));
#236051=CARTESIAN_POINT('Ctrl Pts',(-23.57604596376,1.62010618772866,12.));
#236052=CARTESIAN_POINT('Ctrl Pts',(-23.5572855427601,1.62456559140064,
0.));
#236053=CARTESIAN_POINT('Ctrl Pts',(-23.5572855427601,1.62456559140064,
12.));
#236054=CARTESIAN_POINT('Ctrl Pts',(-23.538625143226,1.62894708745223,0.));
#236055=CARTESIAN_POINT('Ctrl Pts',(-23.538625143226,1.62894708745223,12.));
#236056=CARTESIAN_POINT('Ctrl Pts',(-23.5200658336612,1.63325092321725,
0.));
#236057=CARTESIAN_POINT('Ctrl Pts',(-23.5200658336612,1.63325092321725,
12.));
#236058=CARTESIAN_POINT('Ctrl Pts',(-23.5016086970003,1.63747735129474,
0.));
#236059=CARTESIAN_POINT('Ctrl Pts',(-23.5016086970003,1.63747735129474,
12.));
#236060=CARTESIAN_POINT('Ctrl Pts',(-23.4832548309645,1.64162662967528,
0.));
#236061=CARTESIAN_POINT('Ctrl Pts',(-23.4832548309645,1.64162662967528,
12.));
#236062=CARTESIAN_POINT('Ctrl Pts',(-23.4650053483932,1.64569902187611,
0.));
#236063=CARTESIAN_POINT('Ctrl Pts',(-23.4650053483932,1.64569902187611,
12.));
#236064=CARTESIAN_POINT('Ctrl Pts',(-23.4468613776574,1.6496947970734,0.));
#236065=CARTESIAN_POINT('Ctrl Pts',(-23.4468613776574,1.6496947970734,12.));
#236066=CARTESIAN_POINT('Ctrl Pts',(-23.4288240631043,1.65361423023728,
0.));
#236067=CARTESIAN_POINT('Ctrl Pts',(-23.4288240631043,1.65361423023728,
12.));
#236068=CARTESIAN_POINT('Ctrl Pts',(-23.4108945654805,1.65745760227505,
0.));
#236069=CARTESIAN_POINT('Ctrl Pts',(-23.4108945654805,1.65745760227505,
12.));
#236070=CARTESIAN_POINT('Ctrl Pts',(-23.3930740623619,1.66122520018011,
0.));
#236071=CARTESIAN_POINT('Ctrl Pts',(-23.3930740623619,1.66122520018011,
12.));
#236072=CARTESIAN_POINT('Ctrl Pts',(-23.3753637485545,1.66491731718876,
0.));
#236073=CARTESIAN_POINT('Ctrl Pts',(-23.3753637485545,1.66491731718876,
12.));
#236074=CARTESIAN_POINT('Ctrl Pts',(-23.3577648365744,1.66853425293995,
0.));
#236075=CARTESIAN_POINT('Ctrl Pts',(-23.3577648365744,1.66853425293995,
12.));
#236076=CARTESIAN_POINT('Ctrl Pts',(-23.3402785571865,1.67207631363921,
0.));
#236077=CARTESIAN_POINT('Ctrl Pts',(-23.3402785571865,1.67207631363921,
12.));
#236078=CARTESIAN_POINT('Ctrl Pts',(-23.3229061599145,1.67554381222994,
0.));
#236079=CARTESIAN_POINT('Ctrl Pts',(-23.3229061599145,1.67554381222994,
12.));
#236080=CARTESIAN_POINT('Ctrl Pts',(-23.3056489135611,1.67893706857117,
0.));
#236081=CARTESIAN_POINT('Ctrl Pts',(-23.3056489135611,1.67893706857117,
12.));
#236082=CARTESIAN_POINT('Ctrl Pts',(-23.2885081066951,1.68225640962168,
0.));
#236083=CARTESIAN_POINT('Ctrl Pts',(-23.2885081066951,1.68225640962168,
12.));
#236084=CARTESIAN_POINT('Ctrl Pts',(-23.2714850482246,1.68550216963258,
0.));
#236085=CARTESIAN_POINT('Ctrl Pts',(-23.2714850482246,1.68550216963258,
12.));
#236086=CARTESIAN_POINT('Ctrl Pts',(-23.2545810680537,1.68867469034896,
0.));
#236087=CARTESIAN_POINT('Ctrl Pts',(-23.2545810680537,1.68867469034896,
12.));
#236088=CARTESIAN_POINT('Ctrl Pts',(-23.2377975177013,1.69177432121711,
0.));
#236089=CARTESIAN_POINT('Ctrl Pts',(-23.2377975177013,1.69177432121711,
12.));
#236090=CARTESIAN_POINT('Ctrl Pts',(-23.2211357709374,1.69480141959953,
0.));
#236091=CARTESIAN_POINT('Ctrl Pts',(-23.2211357709374,1.69480141959953,
12.));
#236092=CARTESIAN_POINT('Ctrl Pts',(-23.2045972243767,1.69775635099443,
0.));
#236093=CARTESIAN_POINT('Ctrl Pts',(-23.2045972243767,1.69775635099443,
12.));
#236094=CARTESIAN_POINT('Ctrl Pts',(-23.1881832981851,1.7006394892701,0.));
#236095=CARTESIAN_POINT('Ctrl Pts',(-23.1881832981851,1.7006394892701,12.));
#236096=CARTESIAN_POINT('Ctrl Pts',(-23.1718954368751,1.70345121691276,
0.));
#236097=CARTESIAN_POINT('Ctrl Pts',(-23.1718954368751,1.70345121691276,
12.));
#236098=CARTESIAN_POINT('Ctrl Pts',(-23.1557351100614,1.70619192527852,
0.));
#236099=CARTESIAN_POINT('Ctrl Pts',(-23.1557351100614,1.70619192527852,
12.));
#236100=CARTESIAN_POINT('Ctrl Pts',(-23.1397038132356,1.70886201485452,
0.));
#236101=CARTESIAN_POINT('Ctrl Pts',(-23.1397038132356,1.70886201485452,
12.));
#236102=CARTESIAN_POINT('Ctrl Pts',(-23.1238030684925,1.71146189552174,
0.));
#236103=CARTESIAN_POINT('Ctrl Pts',(-23.1238030684925,1.71146189552174,
12.));
#236104=CARTESIAN_POINT('Ctrl Pts',(-23.1080344254286,1.71399198684704,
0.));
#236105=CARTESIAN_POINT('Ctrl Pts',(-23.1080344254286,1.71399198684704,
12.));
#236106=CARTESIAN_POINT('Ctrl Pts',(-23.0923994621213,1.71645271839296,
0.));
#236107=CARTESIAN_POINT('Ctrl Pts',(-23.0923994621213,1.71645271839296,
12.));
#236108=CARTESIAN_POINT('Ctrl Pts',(-23.0768997860709,1.71884453003027,
0.));
#236109=CARTESIAN_POINT('Ctrl Pts',(-23.0768997860709,1.71884453003027,
12.));
#236110=CARTESIAN_POINT('Ctrl Pts',(-23.0615370351562,1.72116787225991,
0.));
#236111=CARTESIAN_POINT('Ctrl Pts',(-23.0615370351562,1.72116787225991,
12.));
#236112=CARTESIAN_POINT('Ctrl Pts',(-23.0463128785531,1.72342320653746,
0.));
#236113=CARTESIAN_POINT('Ctrl Pts',(-23.0463128785531,1.72342320653746,
12.));
#236114=CARTESIAN_POINT('Ctrl Pts',(-23.0312290178883,1.72561100564045,
0.));
#236115=CARTESIAN_POINT('Ctrl Pts',(-23.0312290178883,1.72561100564045,
12.));
#236116=CARTESIAN_POINT('Ctrl Pts',(-23.0162871884168,1.72773175404708,
0.));
#236117=CARTESIAN_POINT('Ctrl Pts',(-23.0162871884168,1.72773175404708,
12.));
#236118=CARTESIAN_POINT('Ctrl Pts',(-23.001489160189,1.72978594832136,0.));
#236119=CARTESIAN_POINT('Ctrl Pts',(-23.001489160189,1.72978594832136,12.));
#236120=CARTESIAN_POINT('Ctrl Pts',(-22.9868367391978,1.7317740975019,0.));
#236121=CARTESIAN_POINT('Ctrl Pts',(-22.9868367391978,1.7317740975019,12.));
#236122=CARTESIAN_POINT('Ctrl Pts',(-22.9723317685688,1.73369672350814,
0.));
#236123=CARTESIAN_POINT('Ctrl Pts',(-22.9723317685688,1.73369672350814,
12.));
#236124=CARTESIAN_POINT('Ctrl Pts',(-22.9579761301063,1.73555436162769,
0.));
#236125=CARTESIAN_POINT('Ctrl Pts',(-22.9579761301063,1.73555436162769,
12.));
#236126=CARTESIAN_POINT('Ctrl Pts',(-22.9437717457826,1.73734756100039,
0.));
#236127=CARTESIAN_POINT('Ctrl Pts',(-22.9437717457826,1.73734756100039,
12.));
#236128=CARTESIAN_POINT('Ctrl Pts',(-22.9297205792586,1.73907688511666,
0.));
#236129=CARTESIAN_POINT('Ctrl Pts',(-22.9297205792586,1.73907688511666,
12.));
#236130=CARTESIAN_POINT('Ctrl Pts',(-22.9158246373363,1.74074291231058,
0.));
#236131=CARTESIAN_POINT('Ctrl Pts',(-22.9158246373363,1.74074291231058,
12.));
#236132=CARTESIAN_POINT('Ctrl Pts',(-22.9020859716141,1.7423462363008,0.));
#236133=CARTESIAN_POINT('Ctrl Pts',(-22.9020859716141,1.7423462363008,12.));
#236134=CARTESIAN_POINT('Ctrl Pts',(-22.888506680335,1.74388746677702,0.));
#236135=CARTESIAN_POINT('Ctrl Pts',(-22.888506680335,1.74388746677702,12.));
#236136=CARTESIAN_POINT('Ctrl Pts',(-22.8750889101696,1.74536722998201,
0.));
#236137=CARTESIAN_POINT('Ctrl Pts',(-22.8750889101696,1.74536722998201,
12.));
#236138=CARTESIAN_POINT('Ctrl Pts',(-22.8618348580235,1.74678616930664,
0.));
#236139=CARTESIAN_POINT('Ctrl Pts',(-22.8618348580235,1.74678616930664,
12.));
#236140=CARTESIAN_POINT('Ctrl Pts',(-22.8487467728076,1.74814494588492,
0.));
#236141=CARTESIAN_POINT('Ctrl Pts',(-22.8487467728076,1.74814494588492,
12.));
#236142=CARTESIAN_POINT('Ctrl Pts',(-22.8358269579853,1.74944423940115,
0.));
#236143=CARTESIAN_POINT('Ctrl Pts',(-22.8358269579853,1.74944423940115,
12.));
#236144=CARTESIAN_POINT('Ctrl Pts',(-22.8230777741284,1.75068474890883,
0.));
#236145=CARTESIAN_POINT('Ctrl Pts',(-22.8230777741284,1.75068474890883,
12.));
#236146=CARTESIAN_POINT('Ctrl Pts',(-22.8105016414713,1.75186719365592,
0.));
#236147=CARTESIAN_POINT('Ctrl Pts',(-22.8105016414713,1.75186719365592,
12.));
#236148=CARTESIAN_POINT('Ctrl Pts',(-22.7981010424314,1.75299231391466,
0.));
#236149=CARTESIAN_POINT('Ctrl Pts',(-22.7981010424314,1.75299231391466,
12.));
#236150=CARTESIAN_POINT('Ctrl Pts',(-22.7858785242361,1.75406087182936,
0.));
#236151=CARTESIAN_POINT('Ctrl Pts',(-22.7858785242361,1.75406087182936,
12.));
#236152=CARTESIAN_POINT('Ctrl Pts',(-22.7738367016118,1.75507365227131,
0.));
#236153=CARTESIAN_POINT('Ctrl Pts',(-22.7738367016118,1.75507365227131,
12.));
#236154=CARTESIAN_POINT('Ctrl Pts',(-22.7619782595013,1.75603146371641,
0.));
#236155=CARTESIAN_POINT('Ctrl Pts',(-22.7619782595013,1.75603146371641,
12.));
#236156=CARTESIAN_POINT('Ctrl Pts',(-22.750305955645,1.75693513908907,0.));
#236157=CARTESIAN_POINT('Ctrl Pts',(-22.750305955645,1.75693513908907,12.));
#236158=CARTESIAN_POINT('Ctrl Pts',(-22.7388226235559,1.75778553673244,
0.));
#236159=CARTESIAN_POINT('Ctrl Pts',(-22.7388226235559,1.75778553673244,
12.));
#236160=CARTESIAN_POINT('Ctrl Pts',(-22.72753117773,1.75858354204633,0.));
#236161=CARTESIAN_POINT('Ctrl Pts',(-22.72753117773,1.75858354204633,12.));
#236162=CARTESIAN_POINT('Ctrl Pts',(-22.7164346186006,1.75933006905925,
0.));
#236163=CARTESIAN_POINT('Ctrl Pts',(-22.7164346186006,1.75933006905925,
12.));
#236164=CARTESIAN_POINT('Ctrl Pts',(-22.7055360375485,1.76002606202401,
0.));
#236165=CARTESIAN_POINT('Ctrl Pts',(-22.7055360375485,1.76002606202401,
12.));
#236166=CARTESIAN_POINT('Ctrl Pts',(-22.6948386219851,1.76067249704886,
0.));
#236167=CARTESIAN_POINT('Ctrl Pts',(-22.6948386219851,1.76067249704886,
12.));
#236168=CARTESIAN_POINT('Ctrl Pts',(-22.684345658525,1.76127038310614,0.));
#236169=CARTESIAN_POINT('Ctrl Pts',(-22.684345658525,1.76127038310614,12.));
#236170=CARTESIAN_POINT('Ctrl Pts',(-22.67406053567,1.76182076289525,0.));
#236171=CARTESIAN_POINT('Ctrl Pts',(-22.67406053567,1.76182076289525,12.));
#236172=CARTESIAN_POINT('Ctrl Pts',(-22.6639867471753,1.76232471392568,
0.));
#236173=CARTESIAN_POINT('Ctrl Pts',(-22.6639867471753,1.76232471392568,
12.));
#236174=CARTESIAN_POINT('Ctrl Pts',(-22.6541278938409,1.76278334912561,
0.));
#236175=CARTESIAN_POINT('Ctrl Pts',(-22.6541278938409,1.76278334912561,
12.));
#236176=CARTESIAN_POINT('Ctrl Pts',(-22.6444876940423,1.76319782013916,
0.));
#236177=CARTESIAN_POINT('Ctrl Pts',(-22.6444876940423,1.76319782013916,
12.));
#236178=CARTESIAN_POINT('Ctrl Pts',(-22.6350699979359,1.76356932176273,
0.));
#236179=CARTESIAN_POINT('Ctrl Pts',(-22.6350699979359,1.76356932176273,
12.));
#236180=CARTESIAN_POINT('Ctrl Pts',(-22.6258787994848,1.76389909571403,
0.));
#236181=CARTESIAN_POINT('Ctrl Pts',(-22.6258787994848,1.76389909571403,
12.));
#236182=CARTESIAN_POINT('Ctrl Pts',(-22.6169182517694,1.76418843543739,
0.));
#236183=CARTESIAN_POINT('Ctrl Pts',(-22.6169182517694,1.76418843543739,
12.));
#236184=CARTESIAN_POINT('Ctrl Pts',(-22.6081926681343,1.76443868648015,
0.));
#236185=CARTESIAN_POINT('Ctrl Pts',(-22.6081926681343,1.76443868648015,
12.));
#236186=CARTESIAN_POINT('Ctrl Pts',(-22.5997065145638,1.76465124413557,
0.));
#236187=CARTESIAN_POINT('Ctrl Pts',(-22.5997065145638,1.76465124413557,
12.));
#236188=CARTESIAN_POINT('Ctrl Pts',(-22.5914644078106,1.76482755288411,
0.));
#236189=CARTESIAN_POINT('Ctrl Pts',(-22.5914644078106,1.76482755288411,
12.));
#236190=CARTESIAN_POINT('Ctrl Pts',(-22.5834711038022,1.76496910283088,
0.));
#236191=CARTESIAN_POINT('Ctrl Pts',(-22.5834711038022,1.76496910283088,
12.));
#236192=CARTESIAN_POINT('Ctrl Pts',(-22.5757315316353,1.76507744026746,
0.));
#236193=CARTESIAN_POINT('Ctrl Pts',(-22.5757315316353,1.76507744026746,
12.));
#236194=CARTESIAN_POINT('Ctrl Pts',(-22.5682508499873,1.76515418518831,
0.));
#236195=CARTESIAN_POINT('Ctrl Pts',(-22.5682508499873,1.76515418518831,
12.));
#236196=CARTESIAN_POINT('Ctrl Pts',(-22.5610344912501,1.7652010450045,0.));
#236197=CARTESIAN_POINT('Ctrl Pts',(-22.5610344912501,1.7652010450045,12.));
#236198=CARTESIAN_POINT('Ctrl Pts',(-22.5540882235837,1.76521983384062,
0.));
#236199=CARTESIAN_POINT('Ctrl Pts',(-22.5540882235837,1.76521983384062,
12.));
#236200=CARTESIAN_POINT('Ctrl Pts',(-22.5474180954006,1.76521245524047,
0.));
#236201=CARTESIAN_POINT('Ctrl Pts',(-22.5474180954006,1.76521245524047,
12.));
#236202=CARTESIAN_POINT('Ctrl Pts',(-22.5410303590892,1.76518087841493,
0.));
#236203=CARTESIAN_POINT('Ctrl Pts',(-22.5410303590892,1.76518087841493,
12.));
#236204=CARTESIAN_POINT('Ctrl Pts',(-22.5349313983571,1.76512711563254,
0.));
#236205=CARTESIAN_POINT('Ctrl Pts',(-22.5349313983571,1.76512711563254,
12.));
#236206=CARTESIAN_POINT('Ctrl Pts',(-22.529127665298,1.76505320262759,0.));
#236207=CARTESIAN_POINT('Ctrl Pts',(-22.529127665298,1.76505320262759,12.));
#236208=CARTESIAN_POINT('Ctrl Pts',(-22.5236259635515,1.76496128643375,
0.));
#236209=CARTESIAN_POINT('Ctrl Pts',(-22.5236259635515,1.76496128643375,
12.));
#236210=CARTESIAN_POINT('Ctrl Pts',(-22.5184336670207,1.76485369319895,
0.));
#236211=CARTESIAN_POINT('Ctrl Pts',(-22.5184336670207,1.76485369319895,
12.));
#236212=CARTESIAN_POINT('Ctrl Pts',(-22.5135590569554,1.76473303281149,
0.));
#236213=CARTESIAN_POINT('Ctrl Pts',(-22.5135590569554,1.76473303281149,
12.));
#236214=CARTESIAN_POINT('Ctrl Pts',(-22.5090112700212,1.76460218257313,
0.));
#236215=CARTESIAN_POINT('Ctrl Pts',(-22.5090112700212,1.76460218257313,
12.));
#236216=CARTESIAN_POINT('Ctrl Pts',(-22.5047996391978,1.76446408210364,
0.));
#236217=CARTESIAN_POINT('Ctrl Pts',(-22.5047996391978,1.76446408210364,
12.));
#236218=CARTESIAN_POINT('Ctrl Pts',(-22.5009332677316,1.76432160068737,
0.));
#236219=CARTESIAN_POINT('Ctrl Pts',(-22.5009332677316,1.76432160068737,
12.));
#236220=CARTESIAN_POINT('Ctrl Pts',(-22.4974203063191,1.76417731243483,
0.));
#236221=CARTESIAN_POINT('Ctrl Pts',(-22.4974203063191,1.76417731243483,
12.));
#236222=CARTESIAN_POINT('Ctrl Pts',(-22.4942693792449,1.76403393880316,
0.));
#236223=CARTESIAN_POINT('Ctrl Pts',(-22.4942693792449,1.76403393880316,
12.));
#236224=CARTESIAN_POINT('Ctrl Pts',(-22.4914909094908,1.76389475965714,
0.));
#236225=CARTESIAN_POINT('Ctrl Pts',(-22.4914909094908,1.76389475965714,
12.));
#236226=CARTESIAN_POINT('Ctrl Pts',(-22.4890991659479,1.76376424879468,
0.));
#236227=CARTESIAN_POINT('Ctrl Pts',(-22.4890991659479,1.76376424879468,
12.));
#236228=CARTESIAN_POINT('Ctrl Pts',(-22.4871115206572,1.76364784232925,
0.));
#236229=CARTESIAN_POINT('Ctrl Pts',(-22.4871115206572,1.76364784232925,
12.));
#236230=CARTESIAN_POINT('Ctrl Pts',(-22.4855446605991,1.76355076045549,
0.));
#236231=CARTESIAN_POINT('Ctrl Pts',(-22.4855446605991,1.76355076045549,
12.));
#236232=CARTESIAN_POINT('Ctrl Pts',(-22.4844112933125,1.76347698284861,
0.));
#236233=CARTESIAN_POINT('Ctrl Pts',(-22.4844112933125,1.76347698284861,
12.));
#236234=CARTESIAN_POINT('Ctrl Pts',(-22.4838562517064,1.76343813434659,
0.));
#236235=CARTESIAN_POINT('Ctrl Pts',(-22.4838562517064,1.76343813434659,
12.));
#236236=CARTESIAN_POINT('Ctrl Pts',(-22.4836387052228,1.76342064263637,
0.));
#236237=CARTESIAN_POINT('Ctrl Pts',(-22.4836387052228,1.76342064263637,
12.));
#236238=CARTESIAN_POINT('Ctrl Pts',(-22.4835819929788,1.7634141553879,0.));
#236239=CARTESIAN_POINT('Ctrl Pts',(-22.4835819929788,1.7634141553879,12.));
#236240=CARTESIAN_POINT('Ctrl Pts',(-22.4835757167854,1.7634122053118,0.));
#236241=CARTESIAN_POINT('Ctrl Pts',(-22.4835757167854,1.7634122053118,12.));
#236242=CARTESIAN_POINT('',(-25.991588367311,0.661312440730901,0.));
#236243=CARTESIAN_POINT('Ctrl Pts',(-25.991588367311,0.661312440730901,
0.));
#236244=CARTESIAN_POINT('Ctrl Pts',(-25.9865613464773,0.664028313187627,
0.));
#236245=CARTESIAN_POINT('Ctrl Pts',(-25.9765104298071,0.669451306780825,
0.));
#236246=CARTESIAN_POINT('Ctrl Pts',(-25.9614434297919,0.677559543209725,
0.));
#236247=CARTESIAN_POINT('Ctrl Pts',(-25.9413728471909,0.688318015057729,
0.));
#236248=CARTESIAN_POINT('Ctrl Pts',(-25.9163158909426,0.701678575228756,
0.));
#236249=CARTESIAN_POINT('Ctrl Pts',(-25.891290261497,0.714951588527638,
0.));
#236250=CARTESIAN_POINT('Ctrl Pts',(-25.8662960624185,0.728137036482335,
0.));
#236251=CARTESIAN_POINT('Ctrl Pts',(-25.8413334619055,0.741234902663807,
0.));
#236252=CARTESIAN_POINT('Ctrl Pts',(-25.8164027059984,0.754245175609524,
0.));
#236253=CARTESIAN_POINT('Ctrl Pts',(-25.7915041383376,0.767167852651168,
0.));
#236254=CARTESIAN_POINT('Ctrl Pts',(-25.7666381946955,0.780002940291965,
0.));
#236255=CARTESIAN_POINT('Ctrl Pts',(-25.7418053757746,0.792750451616127,
0.));
#236256=CARTESIAN_POINT('Ctrl Pts',(-25.7170062262525,0.805410404554352,
0.));
#236257=CARTESIAN_POINT('Ctrl Pts',(-25.6922413110194,0.817982819787464,
0.));
#236258=CARTESIAN_POINT('Ctrl Pts',(-25.6675111931952,0.830467718864205,
0.));
#236259=CARTESIAN_POINT('Ctrl Pts',(-25.6428164100055,0.842865122120758,
0.));
#236260=CARTESIAN_POINT('Ctrl Pts',(-25.6181574536049,0.855175047036549,
0.));
#236261=CARTESIAN_POINT('Ctrl Pts',(-25.5935347843585,0.867397509338431,
0.));
#236262=CARTESIAN_POINT('Ctrl Pts',(-25.5689488408156,0.879532523834294,
0.));
#236263=CARTESIAN_POINT('Ctrl Pts',(-25.5444000508211,0.89158010534904,
0.));
#236264=CARTESIAN_POINT('Ctrl Pts',(-25.5198888424194,0.903540269651106,
0.));
#236265=CARTESIAN_POINT('Ctrl Pts',(-25.4954156541795,0.915413034335613,
0.));
#236266=CARTESIAN_POINT('Ctrl Pts',(-25.4709809475009,0.927198419886094,
0.));
#236267=CARTESIAN_POINT('Ctrl Pts',(-25.4465852044849,0.938896449496192,
0.));
#236268=CARTESIAN_POINT('Ctrl Pts',(-25.4222289223167,0.950507148597468,
0.));
#236269=CARTESIAN_POINT('Ctrl Pts',(-25.3979126089163,0.962030544503142,
0.));
#236270=CARTESIAN_POINT('Ctrl Pts',(-25.3736367778845,0.973466666000163,
0.));
#236271=CARTESIAN_POINT('Ctrl Pts',(-25.3494019441441,0.984815543003973,
0.));
#236272=CARTESIAN_POINT('Ctrl Pts',(-25.3252086182968,0.996077206120624,
0.));
#236273=CARTESIAN_POINT('Ctrl Pts',(-25.3010573055547,1.00725168656896,
0.));
#236274=CARTESIAN_POINT('Ctrl Pts',(-25.276948508726,1.01833901642237,0.));
#236275=CARTESIAN_POINT('Ctrl Pts',(-25.2528827300422,1.02933922876806,
0.));
#236276=CARTESIAN_POINT('Ctrl Pts',(-25.2288604735086,1.04025235791507,
0.));
#236277=CARTESIAN_POINT('Ctrl Pts',(-25.2048822469028,1.05107843957931,
0.));
#236278=CARTESIAN_POINT('Ctrl Pts',(-25.1809485642192,1.06181751111768,
0.));
#236279=CARTESIAN_POINT('Ctrl Pts',(-25.157059946931,1.07246961165475,0.));
#236280=CARTESIAN_POINT('Ctrl Pts',(-25.1332169227413,1.08303478197187,
0.));
#236281=CARTESIAN_POINT('Ctrl Pts',(-25.1094200248446,1.09351306445308,
0.));
#236282=CARTESIAN_POINT('Ctrl Pts',(-25.0856697909679,1.10390450301745,
0.));
#236283=CARTESIAN_POINT('Ctrl Pts',(-25.0619667625336,1.11420914306889,
0.));
#236284=CARTESIAN_POINT('Ctrl Pts',(-25.0383114836899,1.12442703144451,
0.));
#236285=CARTESIAN_POINT('Ctrl Pts',(-25.0147045006196,1.1345582163853,0.));
#236286=CARTESIAN_POINT('Ctrl Pts',(-24.9911463621433,1.144602747582,0.));
#236287=CARTESIAN_POINT('Ctrl Pts',(-24.9676376201502,1.15456067621889,
0.));
#236288=CARTESIAN_POINT('Ctrl Pts',(-24.9441788300932,1.16443205502849,
0.));
#236289=CARTESIAN_POINT('Ctrl Pts',(-24.9207705514449,1.17421693835041,
0.));
#236290=CARTESIAN_POINT('Ctrl Pts',(-24.8974133481829,1.18391538220103,
0.));
#236291=CARTESIAN_POINT('Ctrl Pts',(-24.8741077892075,1.19352744434064,
0.));
#236292=CARTESIAN_POINT('Ctrl Pts',(-24.8508544481974,1.2030531842602,0.));
#236293=CARTESIAN_POINT('Ctrl Pts',(-24.8276539035092,1.21249266318208,
0.));
#236294=CARTESIAN_POINT('Ctrl Pts',(-24.8045067380536,1.22184594406528,
0.));
#236295=CARTESIAN_POINT('Ctrl Pts',(-24.7814135391799,1.23111309161843,
0.));
#236296=CARTESIAN_POINT('Ctrl Pts',(-24.7583748985438,1.24029417231989,
0.));
#236297=CARTESIAN_POINT('Ctrl Pts',(-24.7353914120011,1.24938925444325,
0.));
#236298=CARTESIAN_POINT('Ctrl Pts',(-24.7124636797894,1.25839840807418,
0.));
#236299=CARTESIAN_POINT('Ctrl Pts',(-24.6895923066836,1.267321705135,0.));
#236300=CARTESIAN_POINT('Ctrl Pts',(-24.666777902156,1.27615921941642,0.));
#236301=CARTESIAN_POINT('Ctrl Pts',(-24.6440210805278,1.28491102661514,
0.));
#236302=CARTESIAN_POINT('Ctrl Pts',(-24.6213224611229,1.29357720438107,
0.));
#236303=CARTESIAN_POINT('Ctrl Pts',(-24.5986826684027,1.30215783236362,
0.));
#236304=CARTESIAN_POINT('Ctrl Pts',(-24.5761023320183,1.31065299222021,
0.));
#236305=CARTESIAN_POINT('Ctrl Pts',(-24.5535820868674,1.31906276763668,
0.));
#236306=CARTESIAN_POINT('Ctrl Pts',(-24.5311225731435,1.32738724435326,
0.));
#236307=CARTESIAN_POINT('Ctrl Pts',(-24.5087244363856,1.33562651019686,
0.));
#236308=CARTESIAN_POINT('Ctrl Pts',(-24.4863883275134,1.34378065512337,
0.));
#236309=CARTESIAN_POINT('Ctrl Pts',(-24.4641149028892,1.35184977125648,
0.));
#236310=CARTESIAN_POINT('Ctrl Pts',(-24.4419048244523,1.35983395290627,
0.));
#236311=CARTESIAN_POINT('Ctrl Pts',(-24.4197587598337,1.36773329659956,
0.));
#236312=CARTESIAN_POINT('Ctrl Pts',(-24.3976773824732,1.37554790111609,
0.));
#236313=CARTESIAN_POINT('Ctrl Pts',(-24.3756613717299,1.38327786752998,
0.));
#236314=CARTESIAN_POINT('Ctrl Pts',(-24.3537114129875,1.39092329926388,
0.));
#236315=CARTESIAN_POINT('Ctrl Pts',(-24.3318281977643,1.39848430212807,
0.));
#236316=CARTESIAN_POINT('Ctrl Pts',(-24.3100124238311,1.40596098434337,
0.));
#236317=CARTESIAN_POINT('Ctrl Pts',(-24.288264795321,1.41335345657682,0.));
#236318=CARTESIAN_POINT('Ctrl Pts',(-24.2665860228356,1.42066183198252,
0.));
#236319=CARTESIAN_POINT('Ctrl Pts',(-24.2449768235488,1.42788622624854,
0.));
#236320=CARTESIAN_POINT('Ctrl Pts',(-24.2234379212984,1.43502675765508,
0.));
#236321=CARTESIAN_POINT('Ctrl Pts',(-24.201970046722,1.44208354711082,0.));
#236322=CARTESIAN_POINT('Ctrl Pts',(-24.1805739374038,1.44905671818727,
0.));
#236323=CARTESIAN_POINT('Ctrl Pts',(-24.1592503380107,1.45594639716317,
0.));
#236324=CARTESIAN_POINT('Ctrl Pts',(-24.1380000004272,1.46275271307397,
0.));
#236325=CARTESIAN_POINT('Ctrl Pts',(-24.1168236838824,1.46947579776991,
0.));
#236326=CARTESIAN_POINT('Ctrl Pts',(-24.0957221550778,1.47611578597742,
0.));
#236327=CARTESIAN_POINT('Ctrl Pts',(-24.0746961883528,1.48267281533683,
0.));
#236328=CARTESIAN_POINT('Ctrl Pts',(-24.0537465658429,1.48914702644887,
0.));
#236329=CARTESIAN_POINT('Ctrl Pts',(-24.0328740776331,1.49553856292801,
0.));
#236330=CARTESIAN_POINT('Ctrl Pts',(-24.0120795219086,1.50184757146098,
0.));
#236331=CARTESIAN_POINT('Ctrl Pts',(-23.9913637050927,1.50807420187694,
0.));
#236332=CARTESIAN_POINT('Ctrl Pts',(-23.970727442014,1.51421860720614,0.));
#236333=CARTESIAN_POINT('Ctrl Pts',(-23.9501715561033,1.52028094372792,
0.));
#236334=CARTESIAN_POINT('Ctrl Pts',(-23.9296968795757,1.52626137103032,
0.));
#236335=CARTESIAN_POINT('Ctrl Pts',(-23.9093042536119,1.53216005207463,
0.));
#236336=CARTESIAN_POINT('Ctrl Pts',(-23.8889945285318,1.53797715326758,
0.));
#236337=CARTESIAN_POINT('Ctrl Pts',(-23.8687685639642,1.5437128445399,0.));
#236338=CARTESIAN_POINT('Ctrl Pts',(-23.8486272290705,1.54936729940541,
0.));
#236339=CARTESIAN_POINT('Ctrl Pts',(-23.8285714027636,1.55494069502635,
0.));
#236340=CARTESIAN_POINT('Ctrl Pts',(-23.8086019739194,1.56043321228633,
0.));
#236341=CARTESIAN_POINT('Ctrl Pts',(-23.7887198415878,1.56584503586843,
0.));
#236342=CARTESIAN_POINT('Ctrl Pts',(-23.7689259151862,1.57117635434408,
0.));
#236343=CARTESIAN_POINT('Ctrl Pts',(-23.749221114736,1.57642736025246,0.));
#236344=CARTESIAN_POINT('Ctrl Pts',(-23.72960637113,1.58159825017358,0.));
#236345=CARTESIAN_POINT('Ctrl Pts',(-23.710082626383,1.58668922481221,0.));
#236346=CARTESIAN_POINT('Ctrl Pts',(-23.6906508338833,1.59170048908633,
0.));
#236347=CARTESIAN_POINT('Ctrl Pts',(-23.671311958631,1.59663225222463,0.));
#236348=CARTESIAN_POINT('Ctrl Pts',(-23.6520669774876,1.60148472786595,
0.));
#236349=CARTESIAN_POINT('Ctrl Pts',(-23.6329168794929,1.60625813414672,
0.));
#236350=CARTESIAN_POINT('Ctrl Pts',(-23.6138626661653,1.61095269379778,
0.));
#236351=CARTESIAN_POINT('Ctrl Pts',(-23.5949053517997,1.61556863424698,
0.));
#236352=CARTESIAN_POINT('Ctrl Pts',(-23.57604596376,1.62010618772866,0.));
#236353=CARTESIAN_POINT('Ctrl Pts',(-23.5572855427601,1.62456559140064,
0.));
#236354=CARTESIAN_POINT('Ctrl Pts',(-23.538625143226,1.62894708745223,0.));
#236355=CARTESIAN_POINT('Ctrl Pts',(-23.5200658336612,1.63325092321725,
0.));
#236356=CARTESIAN_POINT('Ctrl Pts',(-23.5016086970003,1.63747735129474,
0.));
#236357=CARTESIAN_POINT('Ctrl Pts',(-23.4832548309645,1.64162662967528,
0.));
#236358=CARTESIAN_POINT('Ctrl Pts',(-23.4650053483932,1.64569902187611,
0.));
#236359=CARTESIAN_POINT('Ctrl Pts',(-23.4468613776574,1.6496947970734,0.));
#236360=CARTESIAN_POINT('Ctrl Pts',(-23.4288240631043,1.65361423023728,
0.));
#236361=CARTESIAN_POINT('Ctrl Pts',(-23.4108945654805,1.65745760227505,
0.));
#236362=CARTESIAN_POINT('Ctrl Pts',(-23.3930740623619,1.66122520018011,
0.));
#236363=CARTESIAN_POINT('Ctrl Pts',(-23.3753637485545,1.66491731718876,
0.));
#236364=CARTESIAN_POINT('Ctrl Pts',(-23.3577648365744,1.66853425293995,
0.));
#236365=CARTESIAN_POINT('Ctrl Pts',(-23.3402785571865,1.67207631363921,
0.));
#236366=CARTESIAN_POINT('Ctrl Pts',(-23.3229061599145,1.67554381222994,
0.));
#236367=CARTESIAN_POINT('Ctrl Pts',(-23.3056489135611,1.67893706857117,
0.));
#236368=CARTESIAN_POINT('Ctrl Pts',(-23.2885081066951,1.68225640962168,
0.));
#236369=CARTESIAN_POINT('Ctrl Pts',(-23.2714850482246,1.68550216963258,
0.));
#236370=CARTESIAN_POINT('Ctrl Pts',(-23.2545810680537,1.68867469034896,
0.));
#236371=CARTESIAN_POINT('Ctrl Pts',(-23.2377975177013,1.69177432121711,
0.));
#236372=CARTESIAN_POINT('Ctrl Pts',(-23.2211357709374,1.69480141959953,
0.));
#236373=CARTESIAN_POINT('Ctrl Pts',(-23.2045972243767,1.69775635099443,
0.));
#236374=CARTESIAN_POINT('Ctrl Pts',(-23.1881832981851,1.7006394892701,0.));
#236375=CARTESIAN_POINT('Ctrl Pts',(-23.1718954368751,1.70345121691276,
0.));
#236376=CARTESIAN_POINT('Ctrl Pts',(-23.1557351100614,1.70619192527852,
0.));
#236377=CARTESIAN_POINT('Ctrl Pts',(-23.1397038132356,1.70886201485452,
0.));
#236378=CARTESIAN_POINT('Ctrl Pts',(-23.1238030684925,1.71146189552174,
0.));
#236379=CARTESIAN_POINT('Ctrl Pts',(-23.1080344254286,1.71399198684704,
0.));
#236380=CARTESIAN_POINT('Ctrl Pts',(-23.0923994621213,1.71645271839296,
0.));
#236381=CARTESIAN_POINT('Ctrl Pts',(-23.0768997860709,1.71884453003027,
0.));
#236382=CARTESIAN_POINT('Ctrl Pts',(-23.0615370351562,1.72116787225991,
0.));
#236383=CARTESIAN_POINT('Ctrl Pts',(-23.0463128785531,1.72342320653746,
0.));
#236384=CARTESIAN_POINT('Ctrl Pts',(-23.0312290178883,1.72561100564045,
0.));
#236385=CARTESIAN_POINT('Ctrl Pts',(-23.0162871884168,1.72773175404708,
0.));
#236386=CARTESIAN_POINT('Ctrl Pts',(-23.001489160189,1.72978594832136,0.));
#236387=CARTESIAN_POINT('Ctrl Pts',(-22.9868367391978,1.7317740975019,0.));
#236388=CARTESIAN_POINT('Ctrl Pts',(-22.9723317685688,1.73369672350814,
0.));
#236389=CARTESIAN_POINT('Ctrl Pts',(-22.9579761301063,1.73555436162769,
0.));
#236390=CARTESIAN_POINT('Ctrl Pts',(-22.9437717457826,1.73734756100039,
0.));
#236391=CARTESIAN_POINT('Ctrl Pts',(-22.9297205792586,1.73907688511666,
0.));
#236392=CARTESIAN_POINT('Ctrl Pts',(-22.9158246373363,1.74074291231058,
0.));
#236393=CARTESIAN_POINT('Ctrl Pts',(-22.9020859716141,1.7423462363008,0.));
#236394=CARTESIAN_POINT('Ctrl Pts',(-22.888506680335,1.74388746677702,0.));
#236395=CARTESIAN_POINT('Ctrl Pts',(-22.8750889101696,1.74536722998201,
0.));
#236396=CARTESIAN_POINT('Ctrl Pts',(-22.8618348580235,1.74678616930664,
0.));
#236397=CARTESIAN_POINT('Ctrl Pts',(-22.8487467728076,1.74814494588492,
0.));
#236398=CARTESIAN_POINT('Ctrl Pts',(-22.8358269579853,1.74944423940115,
0.));
#236399=CARTESIAN_POINT('Ctrl Pts',(-22.8230777741284,1.75068474890883,
0.));
#236400=CARTESIAN_POINT('Ctrl Pts',(-22.8105016414713,1.75186719365592,
0.));
#236401=CARTESIAN_POINT('Ctrl Pts',(-22.7981010424314,1.75299231391466,
0.));
#236402=CARTESIAN_POINT('Ctrl Pts',(-22.7858785242361,1.75406087182936,
0.));
#236403=CARTESIAN_POINT('Ctrl Pts',(-22.7738367016118,1.75507365227131,
0.));
#236404=CARTESIAN_POINT('Ctrl Pts',(-22.7619782595013,1.75603146371641,
0.));
#236405=CARTESIAN_POINT('Ctrl Pts',(-22.750305955645,1.75693513908907,0.));
#236406=CARTESIAN_POINT('Ctrl Pts',(-22.7388226235559,1.75778553673244,
0.));
#236407=CARTESIAN_POINT('Ctrl Pts',(-22.72753117773,1.75858354204633,0.));
#236408=CARTESIAN_POINT('Ctrl Pts',(-22.7164346186006,1.75933006905925,
0.));
#236409=CARTESIAN_POINT('Ctrl Pts',(-22.7055360375485,1.76002606202401,
0.));
#236410=CARTESIAN_POINT('Ctrl Pts',(-22.6948386219851,1.76067249704886,
0.));
#236411=CARTESIAN_POINT('Ctrl Pts',(-22.684345658525,1.76127038310614,0.));
#236412=CARTESIAN_POINT('Ctrl Pts',(-22.67406053567,1.76182076289525,0.));
#236413=CARTESIAN_POINT('Ctrl Pts',(-22.6639867471753,1.76232471392568,
0.));
#236414=CARTESIAN_POINT('Ctrl Pts',(-22.6541278938409,1.76278334912561,
0.));
#236415=CARTESIAN_POINT('Ctrl Pts',(-22.6444876940423,1.76319782013916,
0.));
#236416=CARTESIAN_POINT('Ctrl Pts',(-22.6350699979359,1.76356932176273,
0.));
#236417=CARTESIAN_POINT('Ctrl Pts',(-22.6258787994848,1.76389909571403,
0.));
#236418=CARTESIAN_POINT('Ctrl Pts',(-22.6169182517694,1.76418843543739,
0.));
#236419=CARTESIAN_POINT('Ctrl Pts',(-22.6081926681343,1.76443868648015,
0.));
#236420=CARTESIAN_POINT('Ctrl Pts',(-22.5997065145638,1.76465124413557,
0.));
#236421=CARTESIAN_POINT('Ctrl Pts',(-22.5914644078106,1.76482755288411,
0.));
#236422=CARTESIAN_POINT('Ctrl Pts',(-22.5834711038022,1.76496910283088,
0.));
#236423=CARTESIAN_POINT('Ctrl Pts',(-22.5757315316353,1.76507744026746,
0.));
#236424=CARTESIAN_POINT('Ctrl Pts',(-22.5682508499873,1.76515418518831,
0.));
#236425=CARTESIAN_POINT('Ctrl Pts',(-22.5610344912501,1.7652010450045,0.));
#236426=CARTESIAN_POINT('Ctrl Pts',(-22.5540882235837,1.76521983384062,
0.));
#236427=CARTESIAN_POINT('Ctrl Pts',(-22.5474180954006,1.76521245524047,
0.));
#236428=CARTESIAN_POINT('Ctrl Pts',(-22.5410303590892,1.76518087841493,
0.));
#236429=CARTESIAN_POINT('Ctrl Pts',(-22.5349313983571,1.76512711563254,
0.));
#236430=CARTESIAN_POINT('Ctrl Pts',(-22.529127665298,1.76505320262759,0.));
#236431=CARTESIAN_POINT('Ctrl Pts',(-22.5236259635515,1.76496128643375,
0.));
#236432=CARTESIAN_POINT('Ctrl Pts',(-22.5184336670207,1.76485369319895,
0.));
#236433=CARTESIAN_POINT('Ctrl Pts',(-22.5135590569554,1.76473303281149,
0.));
#236434=CARTESIAN_POINT('Ctrl Pts',(-22.5090112700212,1.76460218257313,
0.));
#236435=CARTESIAN_POINT('Ctrl Pts',(-22.5047996391978,1.76446408210364,
0.));
#236436=CARTESIAN_POINT('Ctrl Pts',(-22.5009332677316,1.76432160068737,
0.));
#236437=CARTESIAN_POINT('Ctrl Pts',(-22.4974203063191,1.76417731243483,
0.));
#236438=CARTESIAN_POINT('Ctrl Pts',(-22.4942693792449,1.76403393880316,
0.));
#236439=CARTESIAN_POINT('Ctrl Pts',(-22.4914909094908,1.76389475965714,
0.));
#236440=CARTESIAN_POINT('Ctrl Pts',(-22.4890991659479,1.76376424879468,
0.));
#236441=CARTESIAN_POINT('Ctrl Pts',(-22.4871115206572,1.76364784232925,
0.));
#236442=CARTESIAN_POINT('Ctrl Pts',(-22.4855446605991,1.76355076045549,
0.));
#236443=CARTESIAN_POINT('Ctrl Pts',(-22.4844112933125,1.76347698284861,
0.));
#236444=CARTESIAN_POINT('Ctrl Pts',(-22.4838562517064,1.76343813434659,
0.));
#236445=CARTESIAN_POINT('Ctrl Pts',(-22.4836387052228,1.76342064263637,
0.));
#236446=CARTESIAN_POINT('Ctrl Pts',(-22.4835819929788,1.7634141553879,0.));
#236447=CARTESIAN_POINT('Ctrl Pts',(-22.4835757167854,1.7634122053118,0.));
#236448=CARTESIAN_POINT('',(-25.991588367311,0.661312440730901,12.));
#236449=CARTESIAN_POINT('',(-25.991588367311,0.661312440730901,0.));
#236450=CARTESIAN_POINT('Ctrl Pts',(-22.4835757167854,1.7634122053118,12.));
#236451=CARTESIAN_POINT('Ctrl Pts',(-22.4835819929788,1.7634141553879,12.));
#236452=CARTESIAN_POINT('Ctrl Pts',(-22.4836387052228,1.76342064263637,
12.));
#236453=CARTESIAN_POINT('Ctrl Pts',(-22.4838562517064,1.76343813434659,
12.));
#236454=CARTESIAN_POINT('Ctrl Pts',(-22.4844112933125,1.76347698284861,
12.));
#236455=CARTESIAN_POINT('Ctrl Pts',(-22.4855446605991,1.76355076045549,
12.));
#236456=CARTESIAN_POINT('Ctrl Pts',(-22.4871115206572,1.76364784232925,
12.));
#236457=CARTESIAN_POINT('Ctrl Pts',(-22.4890991659479,1.76376424879468,
12.));
#236458=CARTESIAN_POINT('Ctrl Pts',(-22.4914909094908,1.76389475965714,
12.));
#236459=CARTESIAN_POINT('Ctrl Pts',(-22.4942693792449,1.76403393880316,
12.));
#236460=CARTESIAN_POINT('Ctrl Pts',(-22.4974203063191,1.76417731243483,
12.));
#236461=CARTESIAN_POINT('Ctrl Pts',(-22.5009332677316,1.76432160068737,
12.));
#236462=CARTESIAN_POINT('Ctrl Pts',(-22.5047996391978,1.76446408210364,
12.));
#236463=CARTESIAN_POINT('Ctrl Pts',(-22.5090112700212,1.76460218257313,
12.));
#236464=CARTESIAN_POINT('Ctrl Pts',(-22.5135590569554,1.76473303281149,
12.));
#236465=CARTESIAN_POINT('Ctrl Pts',(-22.5184336670207,1.76485369319895,
12.));
#236466=CARTESIAN_POINT('Ctrl Pts',(-22.5236259635515,1.76496128643375,
12.));
#236467=CARTESIAN_POINT('Ctrl Pts',(-22.529127665298,1.76505320262759,12.));
#236468=CARTESIAN_POINT('Ctrl Pts',(-22.5349313983571,1.76512711563254,
12.));
#236469=CARTESIAN_POINT('Ctrl Pts',(-22.5410303590892,1.76518087841493,
12.));
#236470=CARTESIAN_POINT('Ctrl Pts',(-22.5474180954006,1.76521245524047,
12.));
#236471=CARTESIAN_POINT('Ctrl Pts',(-22.5540882235837,1.76521983384062,
12.));
#236472=CARTESIAN_POINT('Ctrl Pts',(-22.5610344912501,1.7652010450045,12.));
#236473=CARTESIAN_POINT('Ctrl Pts',(-22.5682508499873,1.76515418518831,
12.));
#236474=CARTESIAN_POINT('Ctrl Pts',(-22.5757315316353,1.76507744026746,
12.));
#236475=CARTESIAN_POINT('Ctrl Pts',(-22.5834711038022,1.76496910283088,
12.));
#236476=CARTESIAN_POINT('Ctrl Pts',(-22.5914644078106,1.76482755288411,
12.));
#236477=CARTESIAN_POINT('Ctrl Pts',(-22.5997065145638,1.76465124413557,
12.));
#236478=CARTESIAN_POINT('Ctrl Pts',(-22.6081926681343,1.76443868648015,
12.));
#236479=CARTESIAN_POINT('Ctrl Pts',(-22.6169182517694,1.76418843543739,
12.));
#236480=CARTESIAN_POINT('Ctrl Pts',(-22.6258787994848,1.76389909571403,
12.));
#236481=CARTESIAN_POINT('Ctrl Pts',(-22.6350699979359,1.76356932176273,
12.));
#236482=CARTESIAN_POINT('Ctrl Pts',(-22.6444876940423,1.76319782013916,
12.));
#236483=CARTESIAN_POINT('Ctrl Pts',(-22.6541278938409,1.76278334912561,
12.));
#236484=CARTESIAN_POINT('Ctrl Pts',(-22.6639867471753,1.76232471392568,
12.));
#236485=CARTESIAN_POINT('Ctrl Pts',(-22.67406053567,1.76182076289525,12.));
#236486=CARTESIAN_POINT('Ctrl Pts',(-22.684345658525,1.76127038310614,12.));
#236487=CARTESIAN_POINT('Ctrl Pts',(-22.6948386219851,1.76067249704886,
12.));
#236488=CARTESIAN_POINT('Ctrl Pts',(-22.7055360375485,1.76002606202401,
12.));
#236489=CARTESIAN_POINT('Ctrl Pts',(-22.7164346186006,1.75933006905925,
12.));
#236490=CARTESIAN_POINT('Ctrl Pts',(-22.72753117773,1.75858354204633,12.));
#236491=CARTESIAN_POINT('Ctrl Pts',(-22.7388226235559,1.75778553673244,
12.));
#236492=CARTESIAN_POINT('Ctrl Pts',(-22.750305955645,1.75693513908907,12.));
#236493=CARTESIAN_POINT('Ctrl Pts',(-22.7619782595013,1.75603146371641,
12.));
#236494=CARTESIAN_POINT('Ctrl Pts',(-22.7738367016118,1.75507365227131,
12.));
#236495=CARTESIAN_POINT('Ctrl Pts',(-22.7858785242361,1.75406087182936,
12.));
#236496=CARTESIAN_POINT('Ctrl Pts',(-22.7981010424314,1.75299231391466,
12.));
#236497=CARTESIAN_POINT('Ctrl Pts',(-22.8105016414713,1.75186719365592,
12.));
#236498=CARTESIAN_POINT('Ctrl Pts',(-22.8230777741284,1.75068474890883,
12.));
#236499=CARTESIAN_POINT('Ctrl Pts',(-22.8358269579853,1.74944423940115,
12.));
#236500=CARTESIAN_POINT('Ctrl Pts',(-22.8487467728076,1.74814494588492,
12.));
#236501=CARTESIAN_POINT('Ctrl Pts',(-22.8618348580235,1.74678616930664,
12.));
#236502=CARTESIAN_POINT('Ctrl Pts',(-22.8750889101696,1.74536722998201,
12.));
#236503=CARTESIAN_POINT('Ctrl Pts',(-22.888506680335,1.74388746677702,12.));
#236504=CARTESIAN_POINT('Ctrl Pts',(-22.9020859716141,1.7423462363008,12.));
#236505=CARTESIAN_POINT('Ctrl Pts',(-22.9158246373363,1.74074291231058,
12.));
#236506=CARTESIAN_POINT('Ctrl Pts',(-22.9297205792586,1.73907688511666,
12.));
#236507=CARTESIAN_POINT('Ctrl Pts',(-22.9437717457826,1.73734756100039,
12.));
#236508=CARTESIAN_POINT('Ctrl Pts',(-22.9579761301063,1.73555436162769,
12.));
#236509=CARTESIAN_POINT('Ctrl Pts',(-22.9723317685688,1.73369672350814,
12.));
#236510=CARTESIAN_POINT('Ctrl Pts',(-22.9868367391978,1.7317740975019,12.));
#236511=CARTESIAN_POINT('Ctrl Pts',(-23.001489160189,1.72978594832136,12.));
#236512=CARTESIAN_POINT('Ctrl Pts',(-23.0162871884168,1.72773175404708,
12.));
#236513=CARTESIAN_POINT('Ctrl Pts',(-23.0312290178883,1.72561100564045,
12.));
#236514=CARTESIAN_POINT('Ctrl Pts',(-23.0463128785531,1.72342320653746,
12.));
#236515=CARTESIAN_POINT('Ctrl Pts',(-23.0615370351562,1.72116787225991,
12.));
#236516=CARTESIAN_POINT('Ctrl Pts',(-23.0768997860709,1.71884453003027,
12.));
#236517=CARTESIAN_POINT('Ctrl Pts',(-23.0923994621213,1.71645271839296,
12.));
#236518=CARTESIAN_POINT('Ctrl Pts',(-23.1080344254286,1.71399198684704,
12.));
#236519=CARTESIAN_POINT('Ctrl Pts',(-23.1238030684925,1.71146189552174,
12.));
#236520=CARTESIAN_POINT('Ctrl Pts',(-23.1397038132356,1.70886201485452,
12.));
#236521=CARTESIAN_POINT('Ctrl Pts',(-23.1557351100614,1.70619192527852,
12.));
#236522=CARTESIAN_POINT('Ctrl Pts',(-23.1718954368751,1.70345121691276,
12.));
#236523=CARTESIAN_POINT('Ctrl Pts',(-23.1881832981851,1.7006394892701,12.));
#236524=CARTESIAN_POINT('Ctrl Pts',(-23.2045972243767,1.69775635099443,
12.));
#236525=CARTESIAN_POINT('Ctrl Pts',(-23.2211357709374,1.69480141959953,
12.));
#236526=CARTESIAN_POINT('Ctrl Pts',(-23.2377975177013,1.69177432121711,
12.));
#236527=CARTESIAN_POINT('Ctrl Pts',(-23.2545810680537,1.68867469034896,
12.));
#236528=CARTESIAN_POINT('Ctrl Pts',(-23.2714850482246,1.68550216963258,
12.));
#236529=CARTESIAN_POINT('Ctrl Pts',(-23.2885081066951,1.68225640962168,
12.));
#236530=CARTESIAN_POINT('Ctrl Pts',(-23.3056489135611,1.67893706857117,
12.));
#236531=CARTESIAN_POINT('Ctrl Pts',(-23.3229061599145,1.67554381222994,
12.));
#236532=CARTESIAN_POINT('Ctrl Pts',(-23.3402785571865,1.67207631363921,
12.));
#236533=CARTESIAN_POINT('Ctrl Pts',(-23.3577648365744,1.66853425293995,
12.));
#236534=CARTESIAN_POINT('Ctrl Pts',(-23.3753637485545,1.66491731718876,
12.));
#236535=CARTESIAN_POINT('Ctrl Pts',(-23.3930740623619,1.66122520018011,
12.));
#236536=CARTESIAN_POINT('Ctrl Pts',(-23.4108945654805,1.65745760227505,
12.));
#236537=CARTESIAN_POINT('Ctrl Pts',(-23.4288240631043,1.65361423023728,
12.));
#236538=CARTESIAN_POINT('Ctrl Pts',(-23.4468613776574,1.6496947970734,12.));
#236539=CARTESIAN_POINT('Ctrl Pts',(-23.4650053483932,1.64569902187611,
12.));
#236540=CARTESIAN_POINT('Ctrl Pts',(-23.4832548309645,1.64162662967528,
12.));
#236541=CARTESIAN_POINT('Ctrl Pts',(-23.5016086970003,1.63747735129474,
12.));
#236542=CARTESIAN_POINT('Ctrl Pts',(-23.5200658336612,1.63325092321725,
12.));
#236543=CARTESIAN_POINT('Ctrl Pts',(-23.538625143226,1.62894708745223,12.));
#236544=CARTESIAN_POINT('Ctrl Pts',(-23.5572855427601,1.62456559140064,
12.));
#236545=CARTESIAN_POINT('Ctrl Pts',(-23.57604596376,1.62010618772866,12.));
#236546=CARTESIAN_POINT('Ctrl Pts',(-23.5949053517997,1.61556863424698,
12.));
#236547=CARTESIAN_POINT('Ctrl Pts',(-23.6138626661653,1.61095269379778,
12.));
#236548=CARTESIAN_POINT('Ctrl Pts',(-23.6329168794929,1.60625813414672,
12.));
#236549=CARTESIAN_POINT('Ctrl Pts',(-23.6520669774876,1.60148472786595,
12.));
#236550=CARTESIAN_POINT('Ctrl Pts',(-23.671311958631,1.59663225222463,12.));
#236551=CARTESIAN_POINT('Ctrl Pts',(-23.6906508338833,1.59170048908633,
12.));
#236552=CARTESIAN_POINT('Ctrl Pts',(-23.710082626383,1.58668922481221,12.));
#236553=CARTESIAN_POINT('Ctrl Pts',(-23.72960637113,1.58159825017358,12.));
#236554=CARTESIAN_POINT('Ctrl Pts',(-23.749221114736,1.57642736025246,12.));
#236555=CARTESIAN_POINT('Ctrl Pts',(-23.7689259151862,1.57117635434408,
12.));
#236556=CARTESIAN_POINT('Ctrl Pts',(-23.7887198415878,1.56584503586843,
12.));
#236557=CARTESIAN_POINT('Ctrl Pts',(-23.8086019739194,1.56043321228633,
12.));
#236558=CARTESIAN_POINT('Ctrl Pts',(-23.8285714027636,1.55494069502635,
12.));
#236559=CARTESIAN_POINT('Ctrl Pts',(-23.8486272290705,1.54936729940541,
12.));
#236560=CARTESIAN_POINT('Ctrl Pts',(-23.8687685639642,1.5437128445399,12.));
#236561=CARTESIAN_POINT('Ctrl Pts',(-23.8889945285318,1.53797715326758,
12.));
#236562=CARTESIAN_POINT('Ctrl Pts',(-23.9093042536119,1.53216005207463,
12.));
#236563=CARTESIAN_POINT('Ctrl Pts',(-23.9296968795757,1.52626137103032,
12.));
#236564=CARTESIAN_POINT('Ctrl Pts',(-23.9501715561033,1.52028094372792,
12.));
#236565=CARTESIAN_POINT('Ctrl Pts',(-23.970727442014,1.51421860720614,12.));
#236566=CARTESIAN_POINT('Ctrl Pts',(-23.9913637050927,1.50807420187694,
12.));
#236567=CARTESIAN_POINT('Ctrl Pts',(-24.0120795219086,1.50184757146098,
12.));
#236568=CARTESIAN_POINT('Ctrl Pts',(-24.0328740776331,1.49553856292801,
12.));
#236569=CARTESIAN_POINT('Ctrl Pts',(-24.0537465658429,1.48914702644887,
12.));
#236570=CARTESIAN_POINT('Ctrl Pts',(-24.0746961883528,1.48267281533683,
12.));
#236571=CARTESIAN_POINT('Ctrl Pts',(-24.0957221550778,1.47611578597742,
12.));
#236572=CARTESIAN_POINT('Ctrl Pts',(-24.1168236838824,1.46947579776991,
12.));
#236573=CARTESIAN_POINT('Ctrl Pts',(-24.1380000004272,1.46275271307397,
12.));
#236574=CARTESIAN_POINT('Ctrl Pts',(-24.1592503380107,1.45594639716317,
12.));
#236575=CARTESIAN_POINT('Ctrl Pts',(-24.1805739374038,1.44905671818727,
12.));
#236576=CARTESIAN_POINT('Ctrl Pts',(-24.201970046722,1.44208354711082,12.));
#236577=CARTESIAN_POINT('Ctrl Pts',(-24.2234379212984,1.43502675765508,
12.));
#236578=CARTESIAN_POINT('Ctrl Pts',(-24.2449768235488,1.42788622624854,
12.));
#236579=CARTESIAN_POINT('Ctrl Pts',(-24.2665860228356,1.42066183198252,
12.));
#236580=CARTESIAN_POINT('Ctrl Pts',(-24.288264795321,1.41335345657682,12.));
#236581=CARTESIAN_POINT('Ctrl Pts',(-24.3100124238311,1.40596098434337,
12.));
#236582=CARTESIAN_POINT('Ctrl Pts',(-24.3318281977643,1.39848430212807,
12.));
#236583=CARTESIAN_POINT('Ctrl Pts',(-24.3537114129875,1.39092329926388,
12.));
#236584=CARTESIAN_POINT('Ctrl Pts',(-24.3756613717299,1.38327786752998,
12.));
#236585=CARTESIAN_POINT('Ctrl Pts',(-24.3976773824732,1.37554790111609,
12.));
#236586=CARTESIAN_POINT('Ctrl Pts',(-24.4197587598337,1.36773329659956,
12.));
#236587=CARTESIAN_POINT('Ctrl Pts',(-24.4419048244523,1.35983395290627,
12.));
#236588=CARTESIAN_POINT('Ctrl Pts',(-24.4641149028892,1.35184977125648,
12.));
#236589=CARTESIAN_POINT('Ctrl Pts',(-24.4863883275134,1.34378065512337,
12.));
#236590=CARTESIAN_POINT('Ctrl Pts',(-24.5087244363856,1.33562651019686,
12.));
#236591=CARTESIAN_POINT('Ctrl Pts',(-24.5311225731435,1.32738724435326,
12.));
#236592=CARTESIAN_POINT('Ctrl Pts',(-24.5535820868674,1.31906276763668,
12.));
#236593=CARTESIAN_POINT('Ctrl Pts',(-24.5761023320183,1.31065299222021,
12.));
#236594=CARTESIAN_POINT('Ctrl Pts',(-24.5986826684027,1.30215783236362,
12.));
#236595=CARTESIAN_POINT('Ctrl Pts',(-24.6213224611229,1.29357720438107,
12.));
#236596=CARTESIAN_POINT('Ctrl Pts',(-24.6440210805278,1.28491102661514,
12.));
#236597=CARTESIAN_POINT('Ctrl Pts',(-24.666777902156,1.27615921941642,12.));
#236598=CARTESIAN_POINT('Ctrl Pts',(-24.6895923066836,1.267321705135,12.));
#236599=CARTESIAN_POINT('Ctrl Pts',(-24.7124636797894,1.25839840807418,
12.));
#236600=CARTESIAN_POINT('Ctrl Pts',(-24.7353914120011,1.24938925444325,
12.));
#236601=CARTESIAN_POINT('Ctrl Pts',(-24.7583748985438,1.24029417231989,
12.));
#236602=CARTESIAN_POINT('Ctrl Pts',(-24.7814135391799,1.23111309161843,
12.));
#236603=CARTESIAN_POINT('Ctrl Pts',(-24.8045067380536,1.22184594406528,
12.));
#236604=CARTESIAN_POINT('Ctrl Pts',(-24.8276539035092,1.21249266318208,
12.));
#236605=CARTESIAN_POINT('Ctrl Pts',(-24.8508544481974,1.2030531842602,12.));
#236606=CARTESIAN_POINT('Ctrl Pts',(-24.8741077892075,1.19352744434064,
12.));
#236607=CARTESIAN_POINT('Ctrl Pts',(-24.8974133481829,1.18391538220103,
12.));
#236608=CARTESIAN_POINT('Ctrl Pts',(-24.9207705514449,1.17421693835041,
12.));
#236609=CARTESIAN_POINT('Ctrl Pts',(-24.9441788300932,1.16443205502849,
12.));
#236610=CARTESIAN_POINT('Ctrl Pts',(-24.9676376201502,1.15456067621889,
12.));
#236611=CARTESIAN_POINT('Ctrl Pts',(-24.9911463621433,1.144602747582,12.));
#236612=CARTESIAN_POINT('Ctrl Pts',(-25.0147045006196,1.1345582163853,12.));
#236613=CARTESIAN_POINT('Ctrl Pts',(-25.0383114836899,1.12442703144451,
12.));
#236614=CARTESIAN_POINT('Ctrl Pts',(-25.0619667625336,1.11420914306889,
12.));
#236615=CARTESIAN_POINT('Ctrl Pts',(-25.0856697909679,1.10390450301745,
12.));
#236616=CARTESIAN_POINT('Ctrl Pts',(-25.1094200248446,1.09351306445308,
12.));
#236617=CARTESIAN_POINT('Ctrl Pts',(-25.1332169227413,1.08303478197187,
12.));
#236618=CARTESIAN_POINT('Ctrl Pts',(-25.157059946931,1.07246961165475,12.));
#236619=CARTESIAN_POINT('Ctrl Pts',(-25.1809485642192,1.06181751111768,
12.));
#236620=CARTESIAN_POINT('Ctrl Pts',(-25.2048822469028,1.05107843957931,
12.));
#236621=CARTESIAN_POINT('Ctrl Pts',(-25.2288604735086,1.04025235791507,
12.));
#236622=CARTESIAN_POINT('Ctrl Pts',(-25.2528827300422,1.02933922876806,
12.));
#236623=CARTESIAN_POINT('Ctrl Pts',(-25.276948508726,1.01833901642237,12.));
#236624=CARTESIAN_POINT('Ctrl Pts',(-25.3010573055547,1.00725168656896,
12.));
#236625=CARTESIAN_POINT('Ctrl Pts',(-25.3252086182968,0.996077206120624,
12.));
#236626=CARTESIAN_POINT('Ctrl Pts',(-25.3494019441441,0.984815543003973,
12.));
#236627=CARTESIAN_POINT('Ctrl Pts',(-25.3736367778845,0.973466666000163,
12.));
#236628=CARTESIAN_POINT('Ctrl Pts',(-25.3979126089163,0.962030544503142,
12.));
#236629=CARTESIAN_POINT('Ctrl Pts',(-25.4222289223167,0.950507148597468,
12.));
#236630=CARTESIAN_POINT('Ctrl Pts',(-25.4465852044849,0.938896449496192,
12.));
#236631=CARTESIAN_POINT('Ctrl Pts',(-25.4709809475009,0.927198419886094,
12.));
#236632=CARTESIAN_POINT('Ctrl Pts',(-25.4954156541795,0.915413034335613,
12.));
#236633=CARTESIAN_POINT('Ctrl Pts',(-25.5198888424194,0.903540269651106,
12.));
#236634=CARTESIAN_POINT('Ctrl Pts',(-25.5444000508211,0.89158010534904,
12.));
#236635=CARTESIAN_POINT('Ctrl Pts',(-25.5689488408156,0.879532523834294,
12.));
#236636=CARTESIAN_POINT('Ctrl Pts',(-25.5935347843585,0.867397509338431,
12.));
#236637=CARTESIAN_POINT('Ctrl Pts',(-25.6181574536049,0.855175047036549,
12.));
#236638=CARTESIAN_POINT('Ctrl Pts',(-25.6428164100055,0.842865122120758,
12.));
#236639=CARTESIAN_POINT('Ctrl Pts',(-25.6675111931952,0.830467718864205,
12.));
#236640=CARTESIAN_POINT('Ctrl Pts',(-25.6922413110194,0.817982819787464,
12.));
#236641=CARTESIAN_POINT('Ctrl Pts',(-25.7170062262525,0.805410404554352,
12.));
#236642=CARTESIAN_POINT('Ctrl Pts',(-25.7418053757746,0.792750451616127,
12.));
#236643=CARTESIAN_POINT('Ctrl Pts',(-25.7666381946955,0.780002940291965,
12.));
#236644=CARTESIAN_POINT('Ctrl Pts',(-25.7915041383376,0.767167852651168,
12.));
#236645=CARTESIAN_POINT('Ctrl Pts',(-25.8164027059984,0.754245175609524,
12.));
#236646=CARTESIAN_POINT('Ctrl Pts',(-25.8413334619055,0.741234902663807,
12.));
#236647=CARTESIAN_POINT('Ctrl Pts',(-25.8662960624185,0.728137036482335,
12.));
#236648=CARTESIAN_POINT('Ctrl Pts',(-25.891290261497,0.714951588527638,
12.));
#236649=CARTESIAN_POINT('Ctrl Pts',(-25.9163158909426,0.701678575228756,
12.));
#236650=CARTESIAN_POINT('Ctrl Pts',(-25.9413728471909,0.688318015057729,
12.));
#236651=CARTESIAN_POINT('Ctrl Pts',(-25.9614434297919,0.677559543209725,
12.));
#236652=CARTESIAN_POINT('Ctrl Pts',(-25.9765104298071,0.669451306780825,
12.));
#236653=CARTESIAN_POINT('Ctrl Pts',(-25.9865613464773,0.664028313187627,
12.));
#236654=CARTESIAN_POINT('Ctrl Pts',(-25.991588367311,0.661312440730901,
12.));
#236655=CARTESIAN_POINT('Ctrl Pts',(-22.1738711152697,4.11585220600461,
0.));
#236656=CARTESIAN_POINT('Ctrl Pts',(-22.1738711152697,4.11585220600461,
12.));
#236657=CARTESIAN_POINT('Ctrl Pts',(-22.173877682324,4.11585194677442,0.));
#236658=CARTESIAN_POINT('Ctrl Pts',(-22.173877682324,4.11585194677442,12.));
#236659=CARTESIAN_POINT('Ctrl Pts',(-22.1739341411687,4.11586035878287,
0.));
#236660=CARTESIAN_POINT('Ctrl Pts',(-22.1739341411687,4.11586035878287,
12.));
#236661=CARTESIAN_POINT('Ctrl Pts',(-22.1741488021234,4.11589976826166,
0.));
#236662=CARTESIAN_POINT('Ctrl Pts',(-22.1741488021234,4.11589976826166,
12.));
#236663=CARTESIAN_POINT('Ctrl Pts',(-22.1746949858775,4.11600589882845,
0.));
#236664=CARTESIAN_POINT('Ctrl Pts',(-22.1746949858775,4.11600589882845,
12.));
#236665=CARTESIAN_POINT('Ctrl Pts',(-22.1758088296598,4.11622797217068,
0.));
#236666=CARTESIAN_POINT('Ctrl Pts',(-22.1758088296598,4.11622797217068,
12.));
#236667=CARTESIAN_POINT('Ctrl Pts',(-22.177347426894,4.11653973150518,0.));
#236668=CARTESIAN_POINT('Ctrl Pts',(-22.177347426894,4.11653973150518,12.));
#236669=CARTESIAN_POINT('Ctrl Pts',(-22.179297473024,4.11694173195003,0.));
#236670=CARTESIAN_POINT('Ctrl Pts',(-22.179297473024,4.11694173195003,12.));
#236671=CARTESIAN_POINT('Ctrl Pts',(-22.1816414985788,4.11743469691756,
0.));
#236672=CARTESIAN_POINT('Ctrl Pts',(-22.1816414985788,4.11743469691756,
12.));
#236673=CARTESIAN_POINT('Ctrl Pts',(-22.1843613164855,4.11801938107479,
0.));
#236674=CARTESIAN_POINT('Ctrl Pts',(-22.1843613164855,4.11801938107479,
12.));
#236675=CARTESIAN_POINT('Ctrl Pts',(-22.1874419861496,4.11869641271773,
0.));
#236676=CARTESIAN_POINT('Ctrl Pts',(-22.1874419861496,4.11869641271773,
12.));
#236677=CARTESIAN_POINT('Ctrl Pts',(-22.1908725908525,4.11946626228636,
0.));
#236678=CARTESIAN_POINT('Ctrl Pts',(-22.1908725908525,4.11946626228636,
12.));
#236679=CARTESIAN_POINT('Ctrl Pts',(-22.1946440958098,4.12032932637736,
0.));
#236680=CARTESIAN_POINT('Ctrl Pts',(-22.1946440958098,4.12032932637736,
12.));
#236681=CARTESIAN_POINT('Ctrl Pts',(-22.1987479618246,4.12128598183522,
0.));
#236682=CARTESIAN_POINT('Ctrl Pts',(-22.1987479618246,4.12128598183522,
12.));
#236683=CARTESIAN_POINT('Ctrl Pts',(-22.2031746532106,4.12233664408227,
0.));
#236684=CARTESIAN_POINT('Ctrl Pts',(-22.2031746532106,4.12233664408227,
12.));
#236685=CARTESIAN_POINT('Ctrl Pts',(-22.2079143941719,4.12348173702023,
0.));
#236686=CARTESIAN_POINT('Ctrl Pts',(-22.2079143941719,4.12348173702023,
12.));
#236687=CARTESIAN_POINT('Ctrl Pts',(-22.2129576146671,4.12472167516607,
0.));
#236688=CARTESIAN_POINT('Ctrl Pts',(-22.2129576146671,4.12472167516607,
12.));
#236689=CARTESIAN_POINT('Ctrl Pts',(-22.2182956401341,4.12605683613307,
0.));
#236690=CARTESIAN_POINT('Ctrl Pts',(-22.2182956401341,4.12605683613307,
12.));
#236691=CARTESIAN_POINT('Ctrl Pts',(-22.2239207458781,4.12748755830104,
0.));
#236692=CARTESIAN_POINT('Ctrl Pts',(-22.2239207458781,4.12748755830104,
12.));
#236693=CARTESIAN_POINT('Ctrl Pts',(-22.2298258043947,4.12901415463379,
0.));
#236694=CARTESIAN_POINT('Ctrl Pts',(-22.2298258043947,4.12901415463379,
12.));
#236695=CARTESIAN_POINT('Ctrl Pts',(-22.2360040565533,4.13063692157498,
0.));
#236696=CARTESIAN_POINT('Ctrl Pts',(-22.2360040565533,4.13063692157498,
12.));
#236697=CARTESIAN_POINT('Ctrl Pts',(-22.2424488153523,4.1323561506016,0.));
#236698=CARTESIAN_POINT('Ctrl Pts',(-22.2424488153523,4.1323561506016,12.));
#236699=CARTESIAN_POINT('Ctrl Pts',(-22.249153531779,4.1341721255881,0.));
#236700=CARTESIAN_POINT('Ctrl Pts',(-22.249153531779,4.1341721255881,12.));
#236701=CARTESIAN_POINT('Ctrl Pts',(-22.2561118708421,4.13608511977225,
0.));
#236702=CARTESIAN_POINT('Ctrl Pts',(-22.2561118708421,4.13608511977225,
12.));
#236703=CARTESIAN_POINT('Ctrl Pts',(-22.2633177913972,4.13809539255421,
0.));
#236704=CARTESIAN_POINT('Ctrl Pts',(-22.2633177913972,4.13809539255421,
12.));
#236705=CARTESIAN_POINT('Ctrl Pts',(-22.2707656042457,4.14020318715991,
0.));
#236706=CARTESIAN_POINT('Ctrl Pts',(-22.2707656042457,4.14020318715991,
12.));
#236707=CARTESIAN_POINT('Ctrl Pts',(-22.2784499072027,4.14240873321984,
0.));
#236708=CARTESIAN_POINT('Ctrl Pts',(-22.2784499072027,4.14240873321984,
12.));
#236709=CARTESIAN_POINT('Ctrl Pts',(-22.2863655389166,4.14471224859295,
0.));
#236710=CARTESIAN_POINT('Ctrl Pts',(-22.2863655389166,4.14471224859295,
12.));
#236711=CARTESIAN_POINT('Ctrl Pts',(-22.2945075198467,4.14711394168556,
0.));
#236712=CARTESIAN_POINT('Ctrl Pts',(-22.2945075198467,4.14711394168556,
12.));
#236713=CARTESIAN_POINT('Ctrl Pts',(-22.3028710166933,4.14961401285522,
0.));
#236714=CARTESIAN_POINT('Ctrl Pts',(-22.3028710166933,4.14961401285522,
12.));
#236715=CARTESIAN_POINT('Ctrl Pts',(-22.3114513545185,4.1522126539699,0.));
#236716=CARTESIAN_POINT('Ctrl Pts',(-22.3114513545185,4.1522126539699,12.));
#236717=CARTESIAN_POINT('Ctrl Pts',(-22.3202440186979,4.15491004835281,
0.));
#236718=CARTESIAN_POINT('Ctrl Pts',(-22.3202440186979,4.15491004835281,
12.));
#236719=CARTESIAN_POINT('Ctrl Pts',(-22.3292446628959,4.15770637047889,
0.));
#236720=CARTESIAN_POINT('Ctrl Pts',(-22.3292446628959,4.15770637047889,
12.));
#236721=CARTESIAN_POINT('Ctrl Pts',(-22.3384491078602,4.16060178604164,
0.));
#236722=CARTESIAN_POINT('Ctrl Pts',(-22.3384491078602,4.16060178604164,
12.));
#236723=CARTESIAN_POINT('Ctrl Pts',(-22.3478533253889,4.16359645263187,
0.));
#236724=CARTESIAN_POINT('Ctrl Pts',(-22.3478533253889,4.16359645263187,
12.));
#236725=CARTESIAN_POINT('Ctrl Pts',(-22.3574534257396,4.166690520266,0.));
#236726=CARTESIAN_POINT('Ctrl Pts',(-22.3574534257396,4.166690520266,12.));
#236727=CARTESIAN_POINT('Ctrl Pts',(-22.36724564276,4.16988413199457,0.));
#236728=CARTESIAN_POINT('Ctrl Pts',(-22.36724564276,4.16988413199457,12.));
#236729=CARTESIAN_POINT('Ctrl Pts',(-22.3772263228617,4.17317742436145,
0.));
#236730=CARTESIAN_POINT('Ctrl Pts',(-22.3772263228617,4.17317742436145,
12.));
#236731=CARTESIAN_POINT('Ctrl Pts',(-22.3873919231334,4.17657052752825,
0.));
#236732=CARTESIAN_POINT('Ctrl Pts',(-22.3873919231334,4.17657052752825,
12.));
#236733=CARTESIAN_POINT('Ctrl Pts',(-22.3977390078075,4.18006356544882,
0.));
#236734=CARTESIAN_POINT('Ctrl Pts',(-22.3977390078075,4.18006356544882,
12.));
#236735=CARTESIAN_POINT('Ctrl Pts',(-22.4082642454453,4.1836566560085,0.));
#236736=CARTESIAN_POINT('Ctrl Pts',(-22.4082642454453,4.1836566560085,12.));
#236737=CARTESIAN_POINT('Ctrl Pts',(-22.4189644056115,4.1873499111772,0.));
#236738=CARTESIAN_POINT('Ctrl Pts',(-22.4189644056115,4.1873499111772,12.));
#236739=CARTESIAN_POINT('Ctrl Pts',(-22.4298363535421,4.19114343726941,
0.));
#236740=CARTESIAN_POINT('Ctrl Pts',(-22.4298363535421,4.19114343726941,
12.));
#236741=CARTESIAN_POINT('Ctrl Pts',(-22.4408770448917,4.1950373351886,0.));
#236742=CARTESIAN_POINT('Ctrl Pts',(-22.4408770448917,4.1950373351886,12.));
#236743=CARTESIAN_POINT('Ctrl Pts',(-22.4520835205419,4.19903170066354,
0.));
#236744=CARTESIAN_POINT('Ctrl Pts',(-22.4520835205419,4.19903170066354,
12.));
#236745=CARTESIAN_POINT('Ctrl Pts',(-22.4634529011433,4.2031266244817,0.));
#236746=CARTESIAN_POINT('Ctrl Pts',(-22.4634529011433,4.2031266244817,12.));
#236747=CARTESIAN_POINT('Ctrl Pts',(-22.4749823839915,4.20732219265648,
0.));
#236748=CARTESIAN_POINT('Ctrl Pts',(-22.4749823839915,4.20732219265648,
12.));
#236749=CARTESIAN_POINT('Ctrl Pts',(-22.4866692403147,4.21161848657428,
0.));
#236750=CARTESIAN_POINT('Ctrl Pts',(-22.4866692403147,4.21161848657428,
12.));
#236751=CARTESIAN_POINT('Ctrl Pts',(-22.4985108124229,4.21601558313908,
0.));
#236752=CARTESIAN_POINT('Ctrl Pts',(-22.4985108124229,4.21601558313908,
12.));
#236753=CARTESIAN_POINT('Ctrl Pts',(-22.5105045108882,4.22051355490196,
0.));
#236754=CARTESIAN_POINT('Ctrl Pts',(-22.5105045108882,4.22051355490196,
12.));
#236755=CARTESIAN_POINT('Ctrl Pts',(-22.5226478117885,4.2251124702004,0.));
#236756=CARTESIAN_POINT('Ctrl Pts',(-22.5226478117885,4.2251124702004,12.));
#236757=CARTESIAN_POINT('Ctrl Pts',(-22.5349382540587,4.22981239330731,
0.));
#236758=CARTESIAN_POINT('Ctrl Pts',(-22.5349382540587,4.22981239330731,
12.));
#236759=CARTESIAN_POINT('Ctrl Pts',(-22.5473734368086,4.23461338456713,
0.));
#236760=CARTESIAN_POINT('Ctrl Pts',(-22.5473734368086,4.23461338456713,
12.));
#236761=CARTESIAN_POINT('Ctrl Pts',(-22.559951016643,4.23951550052526,0.));
#236762=CARTESIAN_POINT('Ctrl Pts',(-22.559951016643,4.23951550052526,12.));
#236763=CARTESIAN_POINT('Ctrl Pts',(-22.5726687049922,4.24451879404858,
0.));
#236764=CARTESIAN_POINT('Ctrl Pts',(-22.5726687049922,4.24451879404858,
12.));
#236765=CARTESIAN_POINT('Ctrl Pts',(-22.5855242662479,4.24962331444184,
0.));
#236766=CARTESIAN_POINT('Ctrl Pts',(-22.5855242662479,4.24962331444184,
12.));
#236767=CARTESIAN_POINT('Ctrl Pts',(-22.5985155158637,4.25482910755485,
0.));
#236768=CARTESIAN_POINT('Ctrl Pts',(-22.5985155158637,4.25482910755485,
12.));
#236769=CARTESIAN_POINT('Ctrl Pts',(-22.611640318482,4.26013621588303,0.));
#236770=CARTESIAN_POINT('Ctrl Pts',(-22.611640318482,4.26013621588303,12.));
#236771=CARTESIAN_POINT('Ctrl Pts',(-22.6248965859975,4.26554467865571,
0.));
#236772=CARTESIAN_POINT('Ctrl Pts',(-22.6248965859975,4.26554467865571,
12.));
#236773=CARTESIAN_POINT('Ctrl Pts',(-22.6382822758171,4.27105453192999,
0.));
#236774=CARTESIAN_POINT('Ctrl Pts',(-22.6382822758171,4.27105453192999,
12.));
#236775=CARTESIAN_POINT('Ctrl Pts',(-22.6517953893303,4.27666580869117,
0.));
#236776=CARTESIAN_POINT('Ctrl Pts',(-22.6517953893303,4.27666580869117,
12.));
#236777=CARTESIAN_POINT('Ctrl Pts',(-22.665433970311,4.28237853894059,0.));
#236778=CARTESIAN_POINT('Ctrl Pts',(-22.665433970311,4.28237853894059,12.));
#236779=CARTESIAN_POINT('Ctrl Pts',(-22.6791961033537,4.28819274977766,
0.));
#236780=CARTESIAN_POINT('Ctrl Pts',(-22.6791961033537,4.28819274977766,
12.));
#236781=CARTESIAN_POINT('Ctrl Pts',(-22.6930799122545,4.29410846547061,
0.));
#236782=CARTESIAN_POINT('Ctrl Pts',(-22.6930799122545,4.29410846547061,
12.));
#236783=CARTESIAN_POINT('Ctrl Pts',(-22.707083558756,4.30012570754066,0.));
#236784=CARTESIAN_POINT('Ctrl Pts',(-22.707083558756,4.30012570754066,12.));
#236785=CARTESIAN_POINT('Ctrl Pts',(-22.7212052413384,4.30624449484074,
0.));
#236786=CARTESIAN_POINT('Ctrl Pts',(-22.7212052413384,4.30624449484074,
12.));
#236787=CARTESIAN_POINT('Ctrl Pts',(-22.7354431939927,4.3124648436255,0.));
#236788=CARTESIAN_POINT('Ctrl Pts',(-22.7354431939927,4.3124648436255,12.));
#236789=CARTESIAN_POINT('Ctrl Pts',(-22.7497956849852,4.3187867676123,0.));
#236790=CARTESIAN_POINT('Ctrl Pts',(-22.7497956849852,4.3187867676123,12.));
#236791=CARTESIAN_POINT('Ctrl Pts',(-22.764261015648,4.32521027803747,0.));
#236792=CARTESIAN_POINT('Ctrl Pts',(-22.764261015648,4.32521027803747,12.));
#236793=CARTESIAN_POINT('Ctrl Pts',(-22.7788375194081,4.33173538373182,
0.));
#236794=CARTESIAN_POINT('Ctrl Pts',(-22.7788375194081,4.33173538373182,
12.));
#236795=CARTESIAN_POINT('Ctrl Pts',(-22.7935235607807,4.33836209118442,
0.));
#236796=CARTESIAN_POINT('Ctrl Pts',(-22.7935235607807,4.33836209118442,
12.));
#236797=CARTESIAN_POINT('Ctrl Pts',(-22.808317534379,4.34509040460065,0.));
#236798=CARTESIAN_POINT('Ctrl Pts',(-22.808317534379,4.34509040460065,12.));
#236799=CARTESIAN_POINT('Ctrl Pts',(-22.8232178638873,4.35192032594801,
0.));
#236800=CARTESIAN_POINT('Ctrl Pts',(-22.8232178638873,4.35192032594801,
12.));
#236801=CARTESIAN_POINT('Ctrl Pts',(-22.838223001118,4.35885185500559,0.));
#236802=CARTESIAN_POINT('Ctrl Pts',(-22.838223001118,4.35885185500559,12.));
#236803=CARTESIAN_POINT('Ctrl Pts',(-22.8533314252419,4.36588498943009,
0.));
#236804=CARTESIAN_POINT('Ctrl Pts',(-22.8533314252419,4.36588498943009,
12.));
#236805=CARTESIAN_POINT('Ctrl Pts',(-22.8685416419725,4.37301972480752,
0.));
#236806=CARTESIAN_POINT('Ctrl Pts',(-22.8685416419725,4.37301972480752,
12.));
#236807=CARTESIAN_POINT('Ctrl Pts',(-22.8838521827702,4.38025605470089,
0.));
#236808=CARTESIAN_POINT('Ctrl Pts',(-22.8838521827702,4.38025605470089,
12.));
#236809=CARTESIAN_POINT('Ctrl Pts',(-22.8992616040108,4.38759397068391,
0.));
#236810=CARTESIAN_POINT('Ctrl Pts',(-22.8992616040108,4.38759397068391,
12.));
#236811=CARTESIAN_POINT('Ctrl Pts',(-22.9147684862425,4.39503346238454,
0.));
#236812=CARTESIAN_POINT('Ctrl Pts',(-22.9147684862425,4.39503346238454,
12.));
#236813=CARTESIAN_POINT('Ctrl Pts',(-22.9303714335549,4.40257451754307,
0.));
#236814=CARTESIAN_POINT('Ctrl Pts',(-22.9303714335549,4.40257451754307,
12.));
#236815=CARTESIAN_POINT('Ctrl Pts',(-22.9460690729093,4.41021712205547,
0.));
#236816=CARTESIAN_POINT('Ctrl Pts',(-22.9460690729093,4.41021712205547,
12.));
#236817=CARTESIAN_POINT('Ctrl Pts',(-22.9618600534866,4.41796126001309,
0.));
#236818=CARTESIAN_POINT('Ctrl Pts',(-22.9618600534866,4.41796126001309,
12.));
#236819=CARTESIAN_POINT('Ctrl Pts',(-22.9777430460021,4.42580691372771,
0.));
#236820=CARTESIAN_POINT('Ctrl Pts',(-22.9777430460021,4.42580691372771,
12.));
#236821=CARTESIAN_POINT('Ctrl Pts',(-22.9937167421009,4.43375406376904,
0.));
#236822=CARTESIAN_POINT('Ctrl Pts',(-22.9937167421009,4.43375406376904,
12.));
#236823=CARTESIAN_POINT('Ctrl Pts',(-23.0097798538399,4.44180268901666,
0.));
#236824=CARTESIAN_POINT('Ctrl Pts',(-23.0097798538399,4.44180268901666,
12.));
#236825=CARTESIAN_POINT('Ctrl Pts',(-23.0259311131395,4.44995276669698,
0.));
#236826=CARTESIAN_POINT('Ctrl Pts',(-23.0259311131395,4.44995276669698,
12.));
#236827=CARTESIAN_POINT('Ctrl Pts',(-23.0421692712466,4.45820427241676,
0.));
#236828=CARTESIAN_POINT('Ctrl Pts',(-23.0421692712466,4.45820427241676,
12.));
#236829=CARTESIAN_POINT('Ctrl Pts',(-23.0584930981723,4.46655718018205,
0.));
#236830=CARTESIAN_POINT('Ctrl Pts',(-23.0584930981723,4.46655718018205,
12.));
#236831=CARTESIAN_POINT('Ctrl Pts',(-23.0749013821868,4.47501146242821,
0.));
#236832=CARTESIAN_POINT('Ctrl Pts',(-23.0749013821868,4.47501146242821,
12.));
#236833=CARTESIAN_POINT('Ctrl Pts',(-23.0913929293909,4.48356709006756,
0.));
#236834=CARTESIAN_POINT('Ctrl Pts',(-23.0913929293909,4.48356709006756,
12.));
#236835=CARTESIAN_POINT('Ctrl Pts',(-23.1079665632629,4.49222403252201,
0.));
#236836=CARTESIAN_POINT('Ctrl Pts',(-23.1079665632629,4.49222403252201,
12.));
#236837=CARTESIAN_POINT('Ctrl Pts',(-23.1246211242117,4.50098225775178,
0.));
#236838=CARTESIAN_POINT('Ctrl Pts',(-23.1246211242117,4.50098225775178,
12.));
#236839=CARTESIAN_POINT('Ctrl Pts',(-23.1413554691136,4.50984173227087,
0.));
#236840=CARTESIAN_POINT('Ctrl Pts',(-23.1413554691136,4.50984173227087,
12.));
#236841=CARTESIAN_POINT('Ctrl Pts',(-23.1581684708778,4.51880242116785,
0.));
#236842=CARTESIAN_POINT('Ctrl Pts',(-23.1581684708778,4.51880242116785,
12.));
#236843=CARTESIAN_POINT('Ctrl Pts',(-23.1750590180923,4.52786428815047,
0.));
#236844=CARTESIAN_POINT('Ctrl Pts',(-23.1750590180923,4.52786428815047,
12.));
#236845=CARTESIAN_POINT('Ctrl Pts',(-23.1920260146474,4.53702729557585,
0.));
#236846=CARTESIAN_POINT('Ctrl Pts',(-23.1920260146474,4.53702729557585,
12.));
#236847=CARTESIAN_POINT('Ctrl Pts',(-23.2090683793627,4.54629140447542,
0.));
#236848=CARTESIAN_POINT('Ctrl Pts',(-23.2090683793627,4.54629140447542,
12.));
#236849=CARTESIAN_POINT('Ctrl Pts',(-23.2261850456055,4.55565657456956,
0.));
#236850=CARTESIAN_POINT('Ctrl Pts',(-23.2261850456055,4.55565657456956,
12.));
#236851=CARTESIAN_POINT('Ctrl Pts',(-23.2433749609117,4.5651227642781,0.));
#236852=CARTESIAN_POINT('Ctrl Pts',(-23.2433749609117,4.5651227642781,12.));
#236853=CARTESIAN_POINT('Ctrl Pts',(-23.2606370866853,4.5746899307607,0.));
#236854=CARTESIAN_POINT('Ctrl Pts',(-23.2606370866853,4.5746899307607,12.));
#236855=CARTESIAN_POINT('Ctrl Pts',(-23.2779703978868,4.58435802994674,
0.));
#236856=CARTESIAN_POINT('Ctrl Pts',(-23.2779703978868,4.58435802994674,
12.));
#236857=CARTESIAN_POINT('Ctrl Pts',(-23.295373882719,4.59412701655749,0.));
#236858=CARTESIAN_POINT('Ctrl Pts',(-23.295373882719,4.59412701655749,12.));
#236859=CARTESIAN_POINT('Ctrl Pts',(-23.3128465423119,4.60399684412174,
0.));
#236860=CARTESIAN_POINT('Ctrl Pts',(-23.3128465423119,4.60399684412174,
12.));
#236861=CARTESIAN_POINT('Ctrl Pts',(-23.3303873903947,4.61396746497848,
0.));
#236862=CARTESIAN_POINT('Ctrl Pts',(-23.3303873903947,4.61396746497848,
12.));
#236863=CARTESIAN_POINT('Ctrl Pts',(-23.3479954530281,4.62403883030823,
0.));
#236864=CARTESIAN_POINT('Ctrl Pts',(-23.3479954530281,4.62403883030823,
12.));
#236865=CARTESIAN_POINT('Ctrl Pts',(-23.3656697683496,4.63421089016554,
0.));
#236866=CARTESIAN_POINT('Ctrl Pts',(-23.3656697683496,4.63421089016554,
12.));
#236867=CARTESIAN_POINT('Ctrl Pts',(-23.383409386307,4.64448359349935,0.));
#236868=CARTESIAN_POINT('Ctrl Pts',(-23.383409386307,4.64448359349935,12.));
#236869=CARTESIAN_POINT('Ctrl Pts',(-23.4012133683957,4.65485688816921,
0.));
#236870=CARTESIAN_POINT('Ctrl Pts',(-23.4012133683957,4.65485688816921,
12.));
#236871=CARTESIAN_POINT('Ctrl Pts',(-23.4190807873798,4.66533072094663,
0.));
#236872=CARTESIAN_POINT('Ctrl Pts',(-23.4190807873798,4.66533072094663,
12.));
#236873=CARTESIAN_POINT('Ctrl Pts',(-23.4370107270444,4.6759050375305,0.));
#236874=CARTESIAN_POINT('Ctrl Pts',(-23.4370107270444,4.6759050375305,12.));
#236875=CARTESIAN_POINT('Ctrl Pts',(-23.4550022819853,4.68657978258297,
0.));
#236876=CARTESIAN_POINT('Ctrl Pts',(-23.4550022819853,4.68657978258297,
12.));
#236877=CARTESIAN_POINT('Ctrl Pts',(-23.4730545573849,4.69735489975023,
0.));
#236878=CARTESIAN_POINT('Ctrl Pts',(-23.4730545573849,4.69735489975023,
12.));
#236879=CARTESIAN_POINT('Ctrl Pts',(-23.491166668789,4.7082303316782,0.));
#236880=CARTESIAN_POINT('Ctrl Pts',(-23.491166668789,4.7082303316782,12.));
#236881=CARTESIAN_POINT('Ctrl Pts',(-23.5093377418784,4.71920602001904,
0.));
#236882=CARTESIAN_POINT('Ctrl Pts',(-23.5093377418784,4.71920602001904,
12.));
#236883=CARTESIAN_POINT('Ctrl Pts',(-23.5275669122378,4.73028190543031,
0.));
#236884=CARTESIAN_POINT('Ctrl Pts',(-23.5275669122378,4.73028190543031,
12.));
#236885=CARTESIAN_POINT('Ctrl Pts',(-23.5458533251715,4.74145792760698,
0.));
#236886=CARTESIAN_POINT('Ctrl Pts',(-23.5458533251715,4.74145792760698,
12.));
#236887=CARTESIAN_POINT('Ctrl Pts',(-23.564196135517,4.75273402530615,0.));
#236888=CARTESIAN_POINT('Ctrl Pts',(-23.564196135517,4.75273402530615,12.));
#236889=CARTESIAN_POINT('Ctrl Pts',(-23.5825945074535,4.7641101363625,0.));
#236890=CARTESIAN_POINT('Ctrl Pts',(-23.5825945074535,4.7641101363625,12.));
#236891=CARTESIAN_POINT('Ctrl Pts',(-23.6010476143099,4.77558619769875,
0.));
#236892=CARTESIAN_POINT('Ctrl Pts',(-23.6010476143099,4.77558619769875,
12.));
#236893=CARTESIAN_POINT('Ctrl Pts',(-23.6195546383625,4.78716214532104,
0.));
#236894=CARTESIAN_POINT('Ctrl Pts',(-23.6195546383625,4.78716214532104,
12.));
#236895=CARTESIAN_POINT('Ctrl Pts',(-23.6381147706581,4.79883791433229,
0.));
#236896=CARTESIAN_POINT('Ctrl Pts',(-23.6381147706581,4.79883791433229,
12.));
#236897=CARTESIAN_POINT('Ctrl Pts',(-23.6567272108631,4.81061343896442,
0.));
#236898=CARTESIAN_POINT('Ctrl Pts',(-23.6567272108631,4.81061343896442,
12.));
#236899=CARTESIAN_POINT('Ctrl Pts',(-23.6753911671023,4.82248865259569,
0.));
#236900=CARTESIAN_POINT('Ctrl Pts',(-23.6753911671023,4.82248865259569,
12.));
#236901=CARTESIAN_POINT('Ctrl Pts',(-23.6941058557971,4.83446348776267,
0.));
#236902=CARTESIAN_POINT('Ctrl Pts',(-23.6941058557971,4.83446348776267,
12.));
#236903=CARTESIAN_POINT('Ctrl Pts',(-23.7128705015014,4.84653787616422,
0.));
#236904=CARTESIAN_POINT('Ctrl Pts',(-23.7128705015014,4.84653787616422,
12.));
#236905=CARTESIAN_POINT('Ctrl Pts',(-23.7316843367308,4.85871174865491,
0.));
#236906=CARTESIAN_POINT('Ctrl Pts',(-23.7316843367308,4.85871174865491,
12.));
#236907=CARTESIAN_POINT('Ctrl Pts',(-23.7505466018239,4.87098503527142,
0.));
#236908=CARTESIAN_POINT('Ctrl Pts',(-23.7505466018239,4.87098503527142,
12.));
#236909=CARTESIAN_POINT('Ctrl Pts',(-23.7694565448044,4.88335766525565,
0.));
#236910=CARTESIAN_POINT('Ctrl Pts',(-23.7694565448044,4.88335766525565,
12.));
#236911=CARTESIAN_POINT('Ctrl Pts',(-23.7884134212381,4.89582956706771,
0.));
#236912=CARTESIAN_POINT('Ctrl Pts',(-23.7884134212381,4.89582956706771,
12.));
#236913=CARTESIAN_POINT('Ctrl Pts',(-23.8074164940897,4.90840066839346,
0.));
#236914=CARTESIAN_POINT('Ctrl Pts',(-23.8074164940897,4.90840066839346,
12.));
#236915=CARTESIAN_POINT('Ctrl Pts',(-23.8264650335721,4.92107089613976,
0.));
#236916=CARTESIAN_POINT('Ctrl Pts',(-23.8264650335721,4.92107089613976,
12.));
#236917=CARTESIAN_POINT('Ctrl Pts',(-23.8455583170062,4.93384017643441,
0.));
#236918=CARTESIAN_POINT('Ctrl Pts',(-23.8455583170062,4.93384017643441,
12.));
#236919=CARTESIAN_POINT('Ctrl Pts',(-23.8646956287172,4.94670843465868,
0.));
#236920=CARTESIAN_POINT('Ctrl Pts',(-23.8646956287172,4.94670843465868,
12.));
#236921=CARTESIAN_POINT('Ctrl Pts',(-23.883876259922,4.95967559546565,0.));
#236922=CARTESIAN_POINT('Ctrl Pts',(-23.883876259922,4.95967559546565,12.));
#236923=CARTESIAN_POINT('Ctrl Pts',(-23.9030995086164,4.97274158279228,
0.));
#236924=CARTESIAN_POINT('Ctrl Pts',(-23.9030995086164,4.97274158279228,
12.));
#236925=CARTESIAN_POINT('Ctrl Pts',(-23.9223646794591,4.98590631986532,
0.));
#236926=CARTESIAN_POINT('Ctrl Pts',(-23.9223646794591,4.98590631986532,
12.));
#236927=CARTESIAN_POINT('Ctrl Pts',(-23.9416710836529,4.99916972919309,
0.));
#236928=CARTESIAN_POINT('Ctrl Pts',(-23.9416710836529,4.99916972919309,
12.));
#236929=CARTESIAN_POINT('Ctrl Pts',(-23.9610180388271,5.01253173257458,
0.));
#236930=CARTESIAN_POINT('Ctrl Pts',(-23.9610180388271,5.01253173257458,
12.));
#236931=CARTESIAN_POINT('Ctrl Pts',(-23.9804048689228,5.02599225112461,
0.));
#236932=CARTESIAN_POINT('Ctrl Pts',(-23.9804048689228,5.02599225112461,
12.));
#236933=CARTESIAN_POINT('Ctrl Pts',(-23.9998309040747,5.03955120528527,
0.));
#236934=CARTESIAN_POINT('Ctrl Pts',(-23.9998309040747,5.03955120528527,
12.));
#236935=CARTESIAN_POINT('Ctrl Pts',(-24.0192954804896,5.05320851483068,
0.));
#236936=CARTESIAN_POINT('Ctrl Pts',(-24.0192954804896,5.05320851483068,
12.));
#236937=CARTESIAN_POINT('Ctrl Pts',(-24.0387979403268,5.06696409886639,
0.));
#236938=CARTESIAN_POINT('Ctrl Pts',(-24.0387979403268,5.06696409886639,
12.));
#236939=CARTESIAN_POINT('Ctrl Pts',(-24.0583376315636,5.0808178758127,0.));
#236940=CARTESIAN_POINT('Ctrl Pts',(-24.0583376315636,5.0808178758127,12.));
#236941=CARTESIAN_POINT('Ctrl Pts',(-24.0779139079264,5.09476976342616,
0.));
#236942=CARTESIAN_POINT('Ctrl Pts',(-24.0779139079264,5.09476976342616,
12.));
#236943=CARTESIAN_POINT('Ctrl Pts',(-24.0975261288444,5.10881967883124,
0.));
#236944=CARTESIAN_POINT('Ctrl Pts',(-24.0975261288444,5.10881967883124,
12.));
#236945=CARTESIAN_POINT('Ctrl Pts',(-24.117173659394,5.12296753853857,0.));
#236946=CARTESIAN_POINT('Ctrl Pts',(-24.117173659394,5.12296753853857,12.));
#236947=CARTESIAN_POINT('Ctrl Pts',(-24.1368558702443,5.13721325845745,
0.));
#236948=CARTESIAN_POINT('Ctrl Pts',(-24.1368558702443,5.13721325845745,
12.));
#236949=CARTESIAN_POINT('Ctrl Pts',(-24.1565721375971,5.15155675390079,
0.));
#236950=CARTESIAN_POINT('Ctrl Pts',(-24.1565721375971,5.15155675390079,
12.));
#236951=CARTESIAN_POINT('Ctrl Pts',(-24.1763218431344,5.16599793957985,
0.));
#236952=CARTESIAN_POINT('Ctrl Pts',(-24.1763218431344,5.16599793957985,
12.));
#236953=CARTESIAN_POINT('Ctrl Pts',(-24.1961043738756,5.18053672961398,
0.));
#236954=CARTESIAN_POINT('Ctrl Pts',(-24.1961043738756,5.18053672961398,
12.));
#236955=CARTESIAN_POINT('Ctrl Pts',(-24.2159191220171,5.19517303753647,
0.));
#236956=CARTESIAN_POINT('Ctrl Pts',(-24.2159191220171,5.19517303753647,
12.));
#236957=CARTESIAN_POINT('Ctrl Pts',(-24.2357654847766,5.20990677629176,
0.));
#236958=CARTESIAN_POINT('Ctrl Pts',(-24.2357654847766,5.20990677629176,
12.));
#236959=CARTESIAN_POINT('Ctrl Pts',(-24.2556428642294,5.22473785822442,
0.));
#236960=CARTESIAN_POINT('Ctrl Pts',(-24.2556428642294,5.22473785822442,
12.));
#236961=CARTESIAN_POINT('Ctrl Pts',(-24.2755506671525,5.23966619506289,
0.));
#236962=CARTESIAN_POINT('Ctrl Pts',(-24.2755506671525,5.23966619506289,
12.));
#236963=CARTESIAN_POINT('Ctrl Pts',(-24.2954883048447,5.25469169788856,
0.));
#236964=CARTESIAN_POINT('Ctrl Pts',(-24.2954883048447,5.25469169788856,
12.));
#236965=CARTESIAN_POINT('Ctrl Pts',(-24.3154551932221,5.26981427718798,
0.));
#236966=CARTESIAN_POINT('Ctrl Pts',(-24.3154551932221,5.26981427718798,
12.));
#236967=CARTESIAN_POINT('Ctrl Pts',(-24.3354507529414,5.28503384290648,
0.));
#236968=CARTESIAN_POINT('Ctrl Pts',(-24.3354507529414,5.28503384290648,
12.));
#236969=CARTESIAN_POINT('Ctrl Pts',(-24.3554744095075,5.30035030449063,
0.));
#236970=CARTESIAN_POINT('Ctrl Pts',(-24.3554744095075,5.30035030449063,
12.));
#236971=CARTESIAN_POINT('Ctrl Pts',(-24.3755255933917,5.31576357092526,
0.));
#236972=CARTESIAN_POINT('Ctrl Pts',(-24.3755255933917,5.31576357092526,
12.));
#236973=CARTESIAN_POINT('Ctrl Pts',(-24.3956037401293,5.33127355076033,
0.));
#236974=CARTESIAN_POINT('Ctrl Pts',(-24.3956037401293,5.33127355076033,
12.));
#236975=CARTESIAN_POINT('Ctrl Pts',(-24.4157082904614,5.34688015213537,
0.));
#236976=CARTESIAN_POINT('Ctrl Pts',(-24.4157082904614,5.34688015213537,
12.));
#236977=CARTESIAN_POINT('Ctrl Pts',(-24.435838689915,5.36258328273627,0.));
#236978=CARTESIAN_POINT('Ctrl Pts',(-24.435838689915,5.36258328273627,12.));
#236979=CARTESIAN_POINT('Ctrl Pts',(-24.4559943883157,5.37838284973695,
0.));
#236980=CARTESIAN_POINT('Ctrl Pts',(-24.4559943883157,5.37838284973695,
12.));
#236981=CARTESIAN_POINT('Ctrl Pts',(-24.4761748393321,5.39427875973824,
0.));
#236982=CARTESIAN_POINT('Ctrl Pts',(-24.4761748393321,5.39427875973824,
12.));
#236983=CARTESIAN_POINT('Ctrl Pts',(-24.4963794999831,5.41027091869241,
0.));
#236984=CARTESIAN_POINT('Ctrl Pts',(-24.4963794999831,5.41027091869241,
12.));
#236985=CARTESIAN_POINT('Ctrl Pts',(-24.5166078302108,5.42635923183419,
0.));
#236986=CARTESIAN_POINT('Ctrl Pts',(-24.5166078302108,5.42635923183419,
12.));
#236987=CARTESIAN_POINT('Ctrl Pts',(-24.5368592922863,5.4425436035688,0.));
#236988=CARTESIAN_POINT('Ctrl Pts',(-24.5368592922863,5.4425436035688,12.));
#236989=CARTESIAN_POINT('Ctrl Pts',(-24.5571333514842,5.45882393762261,
0.));
#236990=CARTESIAN_POINT('Ctrl Pts',(-24.5571333514842,5.45882393762261,
12.));
#236991=CARTESIAN_POINT('Ctrl Pts',(-24.5774294770329,5.47520013724419,
0.));
#236992=CARTESIAN_POINT('Ctrl Pts',(-24.5774294770329,5.47520013724419,
12.));
#236993=CARTESIAN_POINT('Ctrl Pts',(-24.5977471429364,5.49167210537246,
0.));
#236994=CARTESIAN_POINT('Ctrl Pts',(-24.5977471429364,5.49167210537246,
12.));
#236995=CARTESIAN_POINT('Ctrl Pts',(-24.6180858289179,5.50823974481962,
0.));
#236996=CARTESIAN_POINT('Ctrl Pts',(-24.6180858289179,5.50823974481962,
12.));
#236997=CARTESIAN_POINT('Ctrl Pts',(-24.6384450211467,5.52490295840991,
0.));
#236998=CARTESIAN_POINT('Ctrl Pts',(-24.6384450211467,5.52490295840991,
12.));
#236999=CARTESIAN_POINT('Ctrl Pts',(-24.6588242134738,5.54166164919583,
0.));
#237000=CARTESIAN_POINT('Ctrl Pts',(-24.6588242134738,5.54166164919583,
12.));
#237001=CARTESIAN_POINT('Ctrl Pts',(-24.6792229061794,5.55851572025376,
0.));
#237002=CARTESIAN_POINT('Ctrl Pts',(-24.6792229061794,5.55851572025376,
12.));
#237003=CARTESIAN_POINT('Ctrl Pts',(-24.6996406035517,5.57546507427754,
0.));
#237004=CARTESIAN_POINT('Ctrl Pts',(-24.6996406035517,5.57546507427754,
12.));
#237005=CARTESIAN_POINT('Ctrl Pts',(-24.7200768119088,5.59250961323987,
0.));
#237006=CARTESIAN_POINT('Ctrl Pts',(-24.7200768119088,5.59250961323987,
12.));
#237007=CARTESIAN_POINT('Ctrl Pts',(-24.7405310372739,5.60964923798491,
0.));
#237008=CARTESIAN_POINT('Ctrl Pts',(-24.7405310372739,5.60964923798491,
12.));
#237009=CARTESIAN_POINT('Ctrl Pts',(-24.7610027835697,5.62688384790923,
0.));
#237010=CARTESIAN_POINT('Ctrl Pts',(-24.7610027835697,5.62688384790923,
12.));
#237011=CARTESIAN_POINT('Ctrl Pts',(-24.781491549672,5.6442133404226,0.));
#237012=CARTESIAN_POINT('Ctrl Pts',(-24.781491549672,5.6442133404226,12.));
#237013=CARTESIAN_POINT('Ctrl Pts',(-24.8019968304605,5.66163761114921,
0.));
#237014=CARTESIAN_POINT('Ctrl Pts',(-24.8019968304605,5.66163761114921,
12.));
#237015=CARTESIAN_POINT('Ctrl Pts',(-24.8225181223845,5.67915655496542,
0.));
#237016=CARTESIAN_POINT('Ctrl Pts',(-24.8225181223845,5.67915655496542,
12.));
#237017=CARTESIAN_POINT('Ctrl Pts',(-24.8430549277621,5.69677006679444,
0.));
#237018=CARTESIAN_POINT('Ctrl Pts',(-24.8430549277621,5.69677006679444,
12.));
#237019=CARTESIAN_POINT('Ctrl Pts',(-24.8636067597669,5.71447804252027,
0.));
#237020=CARTESIAN_POINT('Ctrl Pts',(-24.8636067597669,5.71447804252027,
12.));
#237021=CARTESIAN_POINT('Ctrl Pts',(-24.884173146722,5.73228037976926,0.));
#237022=CARTESIAN_POINT('Ctrl Pts',(-24.884173146722,5.73228037976926,12.));
#237023=CARTESIAN_POINT('Ctrl Pts',(-24.904753637648,5.75017697890804,0.));
#237024=CARTESIAN_POINT('Ctrl Pts',(-24.904753637648,5.75017697890804,12.));
#237025=CARTESIAN_POINT('Ctrl Pts',(-24.9253478043656,5.76816774342219,
0.));
#237026=CARTESIAN_POINT('Ctrl Pts',(-24.9253478043656,5.76816774342219,
12.));
#237027=CARTESIAN_POINT('Ctrl Pts',(-24.945955229334,5.78625257775681,0.));
#237028=CARTESIAN_POINT('Ctrl Pts',(-24.945955229334,5.78625257775681,12.));
#237029=CARTESIAN_POINT('Ctrl Pts',(-24.9665754954496,5.80443138549726,
0.));
#237030=CARTESIAN_POINT('Ctrl Pts',(-24.9665754954496,5.80443138549726,
12.));
#237031=CARTESIAN_POINT('Ctrl Pts',(-24.9872081752734,5.82270406744198,
0.));
#237032=CARTESIAN_POINT('Ctrl Pts',(-24.9872081752734,5.82270406744198,
12.));
#237033=CARTESIAN_POINT('Ctrl Pts',(-25.0078528200564,5.84107051963071,
0.));
#237034=CARTESIAN_POINT('Ctrl Pts',(-25.0078528200564,5.84107051963071,
12.));
#237035=CARTESIAN_POINT('Ctrl Pts',(-25.0285089498899,5.85953063156826,
0.));
#237036=CARTESIAN_POINT('Ctrl Pts',(-25.0285089498899,5.85953063156826,
12.));
#237037=CARTESIAN_POINT('Ctrl Pts',(-25.0491760405911,5.87808428385365,
0.));
#237038=CARTESIAN_POINT('Ctrl Pts',(-25.0491760405911,5.87808428385365,
12.));
#237039=CARTESIAN_POINT('Ctrl Pts',(-25.0698535426514,5.89673135155514,
0.));
#237040=CARTESIAN_POINT('Ctrl Pts',(-25.0698535426514,5.89673135155514,
12.));
#237041=CARTESIAN_POINT('Ctrl Pts',(-25.0905409050773,5.91547170844447,
0.));
#237042=CARTESIAN_POINT('Ctrl Pts',(-25.0905409050773,5.91547170844447,
12.));
#237043=CARTESIAN_POINT('Ctrl Pts',(-25.1112375971106,5.93430523086834,
0.));
#237044=CARTESIAN_POINT('Ctrl Pts',(-25.1112375971106,5.93430523086834,
12.));
#237045=CARTESIAN_POINT('Ctrl Pts',(-25.1319431317237,5.95323180187378,
0.));
#237046=CARTESIAN_POINT('Ctrl Pts',(-25.1319431317237,5.95323180187378,
12.));
#237047=CARTESIAN_POINT('Ctrl Pts',(-25.1526570863092,5.97225131495616,
0.));
#237048=CARTESIAN_POINT('Ctrl Pts',(-25.1526570863092,5.97225131495616,
12.));
#237049=CARTESIAN_POINT('Ctrl Pts',(-25.1733791296259,5.99136367859754,
0.));
#237050=CARTESIAN_POINT('Ctrl Pts',(-25.1733791296259,5.99136367859754,
12.));
#237051=CARTESIAN_POINT('Ctrl Pts',(-25.1941090269819,6.01056881804612,
0.));
#237052=CARTESIAN_POINT('Ctrl Pts',(-25.1941090269819,6.01056881804612,
12.));
#237053=CARTESIAN_POINT('Ctrl Pts',(-25.21484662016,6.02986667389996,0.));
#237054=CARTESIAN_POINT('Ctrl Pts',(-25.21484662016,6.02986667389996,12.));
#237055=CARTESIAN_POINT('Ctrl Pts',(-25.2355918139032,6.04925720151218,
0.));
#237056=CARTESIAN_POINT('Ctrl Pts',(-25.2355918139032,6.04925720151218,
12.));
#237057=CARTESIAN_POINT('Ctrl Pts',(-25.2521940105705,6.06484373634546,
0.));
#237058=CARTESIAN_POINT('Ctrl Pts',(-25.2521940105705,6.06484373634546,
12.));
#237059=CARTESIAN_POINT('Ctrl Pts',(-25.2646490489923,6.0765753178749,0.));
#237060=CARTESIAN_POINT('Ctrl Pts',(-25.2646490489923,6.0765753178749,12.));
#237061=CARTESIAN_POINT('Ctrl Pts',(-25.2729539149517,6.08441489609793,
0.));
#237062=CARTESIAN_POINT('Ctrl Pts',(-25.2729539149517,6.08441489609793,
12.));
#237063=CARTESIAN_POINT('Ctrl Pts',(-25.2771067246846,6.08833931617699,
0.));
#237064=CARTESIAN_POINT('Ctrl Pts',(-25.2771067246846,6.08833931617699,
12.));
#237065=CARTESIAN_POINT('',(-25.2771067246846,6.08833931617699,0.));
#237066=CARTESIAN_POINT('Ctrl Pts',(-22.1738711152697,4.11585220600461,
0.));
#237067=CARTESIAN_POINT('Ctrl Pts',(-22.173877682324,4.11585194677442,0.));
#237068=CARTESIAN_POINT('Ctrl Pts',(-22.1739341411687,4.11586035878287,
0.));
#237069=CARTESIAN_POINT('Ctrl Pts',(-22.1741488021234,4.11589976826166,
0.));
#237070=CARTESIAN_POINT('Ctrl Pts',(-22.1746949858775,4.11600589882845,
0.));
#237071=CARTESIAN_POINT('Ctrl Pts',(-22.1758088296598,4.11622797217068,
0.));
#237072=CARTESIAN_POINT('Ctrl Pts',(-22.177347426894,4.11653973150518,0.));
#237073=CARTESIAN_POINT('Ctrl Pts',(-22.179297473024,4.11694173195003,0.));
#237074=CARTESIAN_POINT('Ctrl Pts',(-22.1816414985788,4.11743469691756,
0.));
#237075=CARTESIAN_POINT('Ctrl Pts',(-22.1843613164855,4.11801938107479,
0.));
#237076=CARTESIAN_POINT('Ctrl Pts',(-22.1874419861496,4.11869641271773,
0.));
#237077=CARTESIAN_POINT('Ctrl Pts',(-22.1908725908525,4.11946626228636,
0.));
#237078=CARTESIAN_POINT('Ctrl Pts',(-22.1946440958098,4.12032932637736,
0.));
#237079=CARTESIAN_POINT('Ctrl Pts',(-22.1987479618246,4.12128598183522,
0.));
#237080=CARTESIAN_POINT('Ctrl Pts',(-22.2031746532106,4.12233664408227,
0.));
#237081=CARTESIAN_POINT('Ctrl Pts',(-22.2079143941719,4.12348173702023,
0.));
#237082=CARTESIAN_POINT('Ctrl Pts',(-22.2129576146671,4.12472167516607,
0.));
#237083=CARTESIAN_POINT('Ctrl Pts',(-22.2182956401341,4.12605683613307,
0.));
#237084=CARTESIAN_POINT('Ctrl Pts',(-22.2239207458781,4.12748755830104,
0.));
#237085=CARTESIAN_POINT('Ctrl Pts',(-22.2298258043947,4.12901415463379,
0.));
#237086=CARTESIAN_POINT('Ctrl Pts',(-22.2360040565533,4.13063692157498,
0.));
#237087=CARTESIAN_POINT('Ctrl Pts',(-22.2424488153523,4.1323561506016,0.));
#237088=CARTESIAN_POINT('Ctrl Pts',(-22.249153531779,4.1341721255881,0.));
#237089=CARTESIAN_POINT('Ctrl Pts',(-22.2561118708421,4.13608511977225,
0.));
#237090=CARTESIAN_POINT('Ctrl Pts',(-22.2633177913972,4.13809539255421,
0.));
#237091=CARTESIAN_POINT('Ctrl Pts',(-22.2707656042457,4.14020318715991,
0.));
#237092=CARTESIAN_POINT('Ctrl Pts',(-22.2784499072027,4.14240873321984,
0.));
#237093=CARTESIAN_POINT('Ctrl Pts',(-22.2863655389166,4.14471224859295,
0.));
#237094=CARTESIAN_POINT('Ctrl Pts',(-22.2945075198467,4.14711394168556,
0.));
#237095=CARTESIAN_POINT('Ctrl Pts',(-22.3028710166933,4.14961401285522,
0.));
#237096=CARTESIAN_POINT('Ctrl Pts',(-22.3114513545185,4.1522126539699,0.));
#237097=CARTESIAN_POINT('Ctrl Pts',(-22.3202440186979,4.15491004835281,
0.));
#237098=CARTESIAN_POINT('Ctrl Pts',(-22.3292446628959,4.15770637047889,
0.));
#237099=CARTESIAN_POINT('Ctrl Pts',(-22.3384491078602,4.16060178604164,
0.));
#237100=CARTESIAN_POINT('Ctrl Pts',(-22.3478533253889,4.16359645263187,
0.));
#237101=CARTESIAN_POINT('Ctrl Pts',(-22.3574534257396,4.166690520266,0.));
#237102=CARTESIAN_POINT('Ctrl Pts',(-22.36724564276,4.16988413199457,0.));
#237103=CARTESIAN_POINT('Ctrl Pts',(-22.3772263228617,4.17317742436145,
0.));
#237104=CARTESIAN_POINT('Ctrl Pts',(-22.3873919231334,4.17657052752825,
0.));
#237105=CARTESIAN_POINT('Ctrl Pts',(-22.3977390078075,4.18006356544882,
0.));
#237106=CARTESIAN_POINT('Ctrl Pts',(-22.4082642454453,4.1836566560085,0.));
#237107=CARTESIAN_POINT('Ctrl Pts',(-22.4189644056115,4.1873499111772,0.));
#237108=CARTESIAN_POINT('Ctrl Pts',(-22.4298363535421,4.19114343726941,
0.));
#237109=CARTESIAN_POINT('Ctrl Pts',(-22.4408770448917,4.1950373351886,0.));
#237110=CARTESIAN_POINT('Ctrl Pts',(-22.4520835205419,4.19903170066354,
0.));
#237111=CARTESIAN_POINT('Ctrl Pts',(-22.4634529011433,4.2031266244817,0.));
#237112=CARTESIAN_POINT('Ctrl Pts',(-22.4749823839915,4.20732219265648,
0.));
#237113=CARTESIAN_POINT('Ctrl Pts',(-22.4866692403147,4.21161848657428,
0.));
#237114=CARTESIAN_POINT('Ctrl Pts',(-22.4985108124229,4.21601558313908,
0.));
#237115=CARTESIAN_POINT('Ctrl Pts',(-22.5105045108882,4.22051355490196,
0.));
#237116=CARTESIAN_POINT('Ctrl Pts',(-22.5226478117885,4.2251124702004,0.));
#237117=CARTESIAN_POINT('Ctrl Pts',(-22.5349382540587,4.22981239330731,
0.));
#237118=CARTESIAN_POINT('Ctrl Pts',(-22.5473734368086,4.23461338456713,
0.));
#237119=CARTESIAN_POINT('Ctrl Pts',(-22.559951016643,4.23951550052526,0.));
#237120=CARTESIAN_POINT('Ctrl Pts',(-22.5726687049922,4.24451879404858,
0.));
#237121=CARTESIAN_POINT('Ctrl Pts',(-22.5855242662479,4.24962331444184,
0.));
#237122=CARTESIAN_POINT('Ctrl Pts',(-22.5985155158637,4.25482910755485,
0.));
#237123=CARTESIAN_POINT('Ctrl Pts',(-22.611640318482,4.26013621588303,0.));
#237124=CARTESIAN_POINT('Ctrl Pts',(-22.6248965859975,4.26554467865571,
0.));
#237125=CARTESIAN_POINT('Ctrl Pts',(-22.6382822758171,4.27105453192999,
0.));
#237126=CARTESIAN_POINT('Ctrl Pts',(-22.6517953893303,4.27666580869117,
0.));
#237127=CARTESIAN_POINT('Ctrl Pts',(-22.665433970311,4.28237853894059,0.));
#237128=CARTESIAN_POINT('Ctrl Pts',(-22.6791961033537,4.28819274977766,
0.));
#237129=CARTESIAN_POINT('Ctrl Pts',(-22.6930799122545,4.29410846547061,
0.));
#237130=CARTESIAN_POINT('Ctrl Pts',(-22.707083558756,4.30012570754066,0.));
#237131=CARTESIAN_POINT('Ctrl Pts',(-22.7212052413384,4.30624449484074,
0.));
#237132=CARTESIAN_POINT('Ctrl Pts',(-22.7354431939927,4.3124648436255,0.));
#237133=CARTESIAN_POINT('Ctrl Pts',(-22.7497956849852,4.3187867676123,0.));
#237134=CARTESIAN_POINT('Ctrl Pts',(-22.764261015648,4.32521027803747,0.));
#237135=CARTESIAN_POINT('Ctrl Pts',(-22.7788375194081,4.33173538373182,
0.));
#237136=CARTESIAN_POINT('Ctrl Pts',(-22.7935235607807,4.33836209118442,
0.));
#237137=CARTESIAN_POINT('Ctrl Pts',(-22.808317534379,4.34509040460065,0.));
#237138=CARTESIAN_POINT('Ctrl Pts',(-22.8232178638873,4.35192032594801,
0.));
#237139=CARTESIAN_POINT('Ctrl Pts',(-22.838223001118,4.35885185500559,0.));
#237140=CARTESIAN_POINT('Ctrl Pts',(-22.8533314252419,4.36588498943009,
0.));
#237141=CARTESIAN_POINT('Ctrl Pts',(-22.8685416419725,4.37301972480752,
0.));
#237142=CARTESIAN_POINT('Ctrl Pts',(-22.8838521827702,4.38025605470089,
0.));
#237143=CARTESIAN_POINT('Ctrl Pts',(-22.8992616040108,4.38759397068391,
0.));
#237144=CARTESIAN_POINT('Ctrl Pts',(-22.9147684862425,4.39503346238454,
0.));
#237145=CARTESIAN_POINT('Ctrl Pts',(-22.9303714335549,4.40257451754307,
0.));
#237146=CARTESIAN_POINT('Ctrl Pts',(-22.9460690729093,4.41021712205547,
0.));
#237147=CARTESIAN_POINT('Ctrl Pts',(-22.9618600534866,4.41796126001309,
0.));
#237148=CARTESIAN_POINT('Ctrl Pts',(-22.9777430460021,4.42580691372771,
0.));
#237149=CARTESIAN_POINT('Ctrl Pts',(-22.9937167421009,4.43375406376904,
0.));
#237150=CARTESIAN_POINT('Ctrl Pts',(-23.0097798538399,4.44180268901666,
0.));
#237151=CARTESIAN_POINT('Ctrl Pts',(-23.0259311131395,4.44995276669698,
0.));
#237152=CARTESIAN_POINT('Ctrl Pts',(-23.0421692712466,4.45820427241676,
0.));
#237153=CARTESIAN_POINT('Ctrl Pts',(-23.0584930981723,4.46655718018205,
0.));
#237154=CARTESIAN_POINT('Ctrl Pts',(-23.0749013821868,4.47501146242821,
0.));
#237155=CARTESIAN_POINT('Ctrl Pts',(-23.0913929293909,4.48356709006756,
0.));
#237156=CARTESIAN_POINT('Ctrl Pts',(-23.1079665632629,4.49222403252201,
0.));
#237157=CARTESIAN_POINT('Ctrl Pts',(-23.1246211242117,4.50098225775178,
0.));
#237158=CARTESIAN_POINT('Ctrl Pts',(-23.1413554691136,4.50984173227087,
0.));
#237159=CARTESIAN_POINT('Ctrl Pts',(-23.1581684708778,4.51880242116785,
0.));
#237160=CARTESIAN_POINT('Ctrl Pts',(-23.1750590180923,4.52786428815047,
0.));
#237161=CARTESIAN_POINT('Ctrl Pts',(-23.1920260146474,4.53702729557585,
0.));
#237162=CARTESIAN_POINT('Ctrl Pts',(-23.2090683793627,4.54629140447542,
0.));
#237163=CARTESIAN_POINT('Ctrl Pts',(-23.2261850456055,4.55565657456956,
0.));
#237164=CARTESIAN_POINT('Ctrl Pts',(-23.2433749609117,4.5651227642781,0.));
#237165=CARTESIAN_POINT('Ctrl Pts',(-23.2606370866853,4.5746899307607,0.));
#237166=CARTESIAN_POINT('Ctrl Pts',(-23.2779703978868,4.58435802994674,
0.));
#237167=CARTESIAN_POINT('Ctrl Pts',(-23.295373882719,4.59412701655749,0.));
#237168=CARTESIAN_POINT('Ctrl Pts',(-23.3128465423119,4.60399684412174,
0.));
#237169=CARTESIAN_POINT('Ctrl Pts',(-23.3303873903947,4.61396746497848,
0.));
#237170=CARTESIAN_POINT('Ctrl Pts',(-23.3479954530281,4.62403883030823,
0.));
#237171=CARTESIAN_POINT('Ctrl Pts',(-23.3656697683496,4.63421089016554,
0.));
#237172=CARTESIAN_POINT('Ctrl Pts',(-23.383409386307,4.64448359349935,0.));
#237173=CARTESIAN_POINT('Ctrl Pts',(-23.4012133683957,4.65485688816921,
0.));
#237174=CARTESIAN_POINT('Ctrl Pts',(-23.4190807873798,4.66533072094663,
0.));
#237175=CARTESIAN_POINT('Ctrl Pts',(-23.4370107270444,4.6759050375305,0.));
#237176=CARTESIAN_POINT('Ctrl Pts',(-23.4550022819853,4.68657978258297,
0.));
#237177=CARTESIAN_POINT('Ctrl Pts',(-23.4730545573849,4.69735489975023,
0.));
#237178=CARTESIAN_POINT('Ctrl Pts',(-23.491166668789,4.7082303316782,0.));
#237179=CARTESIAN_POINT('Ctrl Pts',(-23.5093377418784,4.71920602001904,
0.));
#237180=CARTESIAN_POINT('Ctrl Pts',(-23.5275669122378,4.73028190543031,
0.));
#237181=CARTESIAN_POINT('Ctrl Pts',(-23.5458533251715,4.74145792760698,
0.));
#237182=CARTESIAN_POINT('Ctrl Pts',(-23.564196135517,4.75273402530615,0.));
#237183=CARTESIAN_POINT('Ctrl Pts',(-23.5825945074535,4.7641101363625,0.));
#237184=CARTESIAN_POINT('Ctrl Pts',(-23.6010476143099,4.77558619769875,
0.));
#237185=CARTESIAN_POINT('Ctrl Pts',(-23.6195546383625,4.78716214532104,
0.));
#237186=CARTESIAN_POINT('Ctrl Pts',(-23.6381147706581,4.79883791433229,
0.));
#237187=CARTESIAN_POINT('Ctrl Pts',(-23.6567272108631,4.81061343896442,
0.));
#237188=CARTESIAN_POINT('Ctrl Pts',(-23.6753911671023,4.82248865259569,
0.));
#237189=CARTESIAN_POINT('Ctrl Pts',(-23.6941058557971,4.83446348776267,
0.));
#237190=CARTESIAN_POINT('Ctrl Pts',(-23.7128705015014,4.84653787616422,
0.));
#237191=CARTESIAN_POINT('Ctrl Pts',(-23.7316843367308,4.85871174865491,
0.));
#237192=CARTESIAN_POINT('Ctrl Pts',(-23.7505466018239,4.87098503527142,
0.));
#237193=CARTESIAN_POINT('Ctrl Pts',(-23.7694565448044,4.88335766525565,
0.));
#237194=CARTESIAN_POINT('Ctrl Pts',(-23.7884134212381,4.89582956706771,
0.));
#237195=CARTESIAN_POINT('Ctrl Pts',(-23.8074164940897,4.90840066839346,
0.));
#237196=CARTESIAN_POINT('Ctrl Pts',(-23.8264650335721,4.92107089613976,
0.));
#237197=CARTESIAN_POINT('Ctrl Pts',(-23.8455583170062,4.93384017643441,
0.));
#237198=CARTESIAN_POINT('Ctrl Pts',(-23.8646956287172,4.94670843465868,
0.));
#237199=CARTESIAN_POINT('Ctrl Pts',(-23.883876259922,4.95967559546565,0.));
#237200=CARTESIAN_POINT('Ctrl Pts',(-23.9030995086164,4.97274158279228,
0.));
#237201=CARTESIAN_POINT('Ctrl Pts',(-23.9223646794591,4.98590631986532,
0.));
#237202=CARTESIAN_POINT('Ctrl Pts',(-23.9416710836529,4.99916972919309,
0.));
#237203=CARTESIAN_POINT('Ctrl Pts',(-23.9610180388271,5.01253173257458,
0.));
#237204=CARTESIAN_POINT('Ctrl Pts',(-23.9804048689228,5.02599225112461,
0.));
#237205=CARTESIAN_POINT('Ctrl Pts',(-23.9998309040747,5.03955120528527,
0.));
#237206=CARTESIAN_POINT('Ctrl Pts',(-24.0192954804896,5.05320851483068,
0.));
#237207=CARTESIAN_POINT('Ctrl Pts',(-24.0387979403268,5.06696409886639,
0.));
#237208=CARTESIAN_POINT('Ctrl Pts',(-24.0583376315636,5.0808178758127,0.));
#237209=CARTESIAN_POINT('Ctrl Pts',(-24.0779139079264,5.09476976342616,
0.));
#237210=CARTESIAN_POINT('Ctrl Pts',(-24.0975261288444,5.10881967883124,
0.));
#237211=CARTESIAN_POINT('Ctrl Pts',(-24.117173659394,5.12296753853857,0.));
#237212=CARTESIAN_POINT('Ctrl Pts',(-24.1368558702443,5.13721325845745,
0.));
#237213=CARTESIAN_POINT('Ctrl Pts',(-24.1565721375971,5.15155675390079,
0.));
#237214=CARTESIAN_POINT('Ctrl Pts',(-24.1763218431344,5.16599793957985,
0.));
#237215=CARTESIAN_POINT('Ctrl Pts',(-24.1961043738756,5.18053672961398,
0.));
#237216=CARTESIAN_POINT('Ctrl Pts',(-24.2159191220171,5.19517303753647,
0.));
#237217=CARTESIAN_POINT('Ctrl Pts',(-24.2357654847766,5.20990677629176,
0.));
#237218=CARTESIAN_POINT('Ctrl Pts',(-24.2556428642294,5.22473785822442,
0.));
#237219=CARTESIAN_POINT('Ctrl Pts',(-24.2755506671525,5.23966619506289,
0.));
#237220=CARTESIAN_POINT('Ctrl Pts',(-24.2954883048447,5.25469169788856,
0.));
#237221=CARTESIAN_POINT('Ctrl Pts',(-24.3154551932221,5.26981427718798,
0.));
#237222=CARTESIAN_POINT('Ctrl Pts',(-24.3354507529414,5.28503384290648,
0.));
#237223=CARTESIAN_POINT('Ctrl Pts',(-24.3554744095075,5.30035030449063,
0.));
#237224=CARTESIAN_POINT('Ctrl Pts',(-24.3755255933917,5.31576357092526,
0.));
#237225=CARTESIAN_POINT('Ctrl Pts',(-24.3956037401293,5.33127355076033,
0.));
#237226=CARTESIAN_POINT('Ctrl Pts',(-24.4157082904614,5.34688015213537,
0.));
#237227=CARTESIAN_POINT('Ctrl Pts',(-24.435838689915,5.36258328273627,0.));
#237228=CARTESIAN_POINT('Ctrl Pts',(-24.4559943883157,5.37838284973695,
0.));
#237229=CARTESIAN_POINT('Ctrl Pts',(-24.4761748393321,5.39427875973824,
0.));
#237230=CARTESIAN_POINT('Ctrl Pts',(-24.4963794999831,5.41027091869241,
0.));
#237231=CARTESIAN_POINT('Ctrl Pts',(-24.5166078302108,5.42635923183419,
0.));
#237232=CARTESIAN_POINT('Ctrl Pts',(-24.5368592922863,5.4425436035688,0.));
#237233=CARTESIAN_POINT('Ctrl Pts',(-24.5571333514842,5.45882393762261,
0.));
#237234=CARTESIAN_POINT('Ctrl Pts',(-24.5774294770329,5.47520013724419,
0.));
#237235=CARTESIAN_POINT('Ctrl Pts',(-24.5977471429364,5.49167210537246,
0.));
#237236=CARTESIAN_POINT('Ctrl Pts',(-24.6180858289179,5.50823974481962,
0.));
#237237=CARTESIAN_POINT('Ctrl Pts',(-24.6384450211467,5.52490295840991,
0.));
#237238=CARTESIAN_POINT('Ctrl Pts',(-24.6588242134738,5.54166164919583,
0.));
#237239=CARTESIAN_POINT('Ctrl Pts',(-24.6792229061794,5.55851572025376,
0.));
#237240=CARTESIAN_POINT('Ctrl Pts',(-24.6996406035517,5.57546507427754,
0.));
#237241=CARTESIAN_POINT('Ctrl Pts',(-24.7200768119088,5.59250961323987,
0.));
#237242=CARTESIAN_POINT('Ctrl Pts',(-24.7405310372739,5.60964923798491,
0.));
#237243=CARTESIAN_POINT('Ctrl Pts',(-24.7610027835697,5.62688384790923,
0.));
#237244=CARTESIAN_POINT('Ctrl Pts',(-24.781491549672,5.6442133404226,0.));
#237245=CARTESIAN_POINT('Ctrl Pts',(-24.8019968304605,5.66163761114921,
0.));
#237246=CARTESIAN_POINT('Ctrl Pts',(-24.8225181223845,5.67915655496542,
0.));
#237247=CARTESIAN_POINT('Ctrl Pts',(-24.8430549277621,5.69677006679444,
0.));
#237248=CARTESIAN_POINT('Ctrl Pts',(-24.8636067597669,5.71447804252027,
0.));
#237249=CARTESIAN_POINT('Ctrl Pts',(-24.884173146722,5.73228037976926,0.));
#237250=CARTESIAN_POINT('Ctrl Pts',(-24.904753637648,5.75017697890804,0.));
#237251=CARTESIAN_POINT('Ctrl Pts',(-24.9253478043656,5.76816774342219,
0.));
#237252=CARTESIAN_POINT('Ctrl Pts',(-24.945955229334,5.78625257775681,0.));
#237253=CARTESIAN_POINT('Ctrl Pts',(-24.9665754954496,5.80443138549726,
0.));
#237254=CARTESIAN_POINT('Ctrl Pts',(-24.9872081752734,5.82270406744198,
0.));
#237255=CARTESIAN_POINT('Ctrl Pts',(-25.0078528200564,5.84107051963071,
0.));
#237256=CARTESIAN_POINT('Ctrl Pts',(-25.0285089498899,5.85953063156826,
0.));
#237257=CARTESIAN_POINT('Ctrl Pts',(-25.0491760405911,5.87808428385365,
0.));
#237258=CARTESIAN_POINT('Ctrl Pts',(-25.0698535426514,5.89673135155514,
0.));
#237259=CARTESIAN_POINT('Ctrl Pts',(-25.0905409050773,5.91547170844447,
0.));
#237260=CARTESIAN_POINT('Ctrl Pts',(-25.1112375971106,5.93430523086834,
0.));
#237261=CARTESIAN_POINT('Ctrl Pts',(-25.1319431317237,5.95323180187378,
0.));
#237262=CARTESIAN_POINT('Ctrl Pts',(-25.1526570863092,5.97225131495616,
0.));
#237263=CARTESIAN_POINT('Ctrl Pts',(-25.1733791296259,5.99136367859754,
0.));
#237264=CARTESIAN_POINT('Ctrl Pts',(-25.1941090269819,6.01056881804612,
0.));
#237265=CARTESIAN_POINT('Ctrl Pts',(-25.21484662016,6.02986667389996,0.));
#237266=CARTESIAN_POINT('Ctrl Pts',(-25.2355918139032,6.04925720151218,
0.));
#237267=CARTESIAN_POINT('Ctrl Pts',(-25.2521940105705,6.06484373634546,
0.));
#237268=CARTESIAN_POINT('Ctrl Pts',(-25.2646490489923,6.0765753178749,0.));
#237269=CARTESIAN_POINT('Ctrl Pts',(-25.2729539149517,6.08441489609793,
0.));
#237270=CARTESIAN_POINT('Ctrl Pts',(-25.2771067246846,6.08833931617699,
0.));
#237271=CARTESIAN_POINT('',(-25.2771067246846,6.08833931617699,12.));
#237272=CARTESIAN_POINT('Ctrl Pts',(-25.2771067246846,6.08833931617699,
12.));
#237273=CARTESIAN_POINT('Ctrl Pts',(-25.2729539149517,6.08441489609793,
12.));
#237274=CARTESIAN_POINT('Ctrl Pts',(-25.2646490489923,6.0765753178749,12.));
#237275=CARTESIAN_POINT('Ctrl Pts',(-25.2521940105705,6.06484373634546,
12.));
#237276=CARTESIAN_POINT('Ctrl Pts',(-25.2355918139032,6.04925720151218,
12.));
#237277=CARTESIAN_POINT('Ctrl Pts',(-25.21484662016,6.02986667389996,12.));
#237278=CARTESIAN_POINT('Ctrl Pts',(-25.1941090269819,6.01056881804612,
12.));
#237279=CARTESIAN_POINT('Ctrl Pts',(-25.1733791296259,5.99136367859754,
12.));
#237280=CARTESIAN_POINT('Ctrl Pts',(-25.1526570863092,5.97225131495616,
12.));
#237281=CARTESIAN_POINT('Ctrl Pts',(-25.1319431317237,5.95323180187378,
12.));
#237282=CARTESIAN_POINT('Ctrl Pts',(-25.1112375971106,5.93430523086834,
12.));
#237283=CARTESIAN_POINT('Ctrl Pts',(-25.0905409050773,5.91547170844447,
12.));
#237284=CARTESIAN_POINT('Ctrl Pts',(-25.0698535426514,5.89673135155514,
12.));
#237285=CARTESIAN_POINT('Ctrl Pts',(-25.0491760405911,5.87808428385365,
12.));
#237286=CARTESIAN_POINT('Ctrl Pts',(-25.0285089498899,5.85953063156826,
12.));
#237287=CARTESIAN_POINT('Ctrl Pts',(-25.0078528200564,5.84107051963071,
12.));
#237288=CARTESIAN_POINT('Ctrl Pts',(-24.9872081752734,5.82270406744198,
12.));
#237289=CARTESIAN_POINT('Ctrl Pts',(-24.9665754954496,5.80443138549726,
12.));
#237290=CARTESIAN_POINT('Ctrl Pts',(-24.945955229334,5.78625257775681,12.));
#237291=CARTESIAN_POINT('Ctrl Pts',(-24.9253478043656,5.76816774342219,
12.));
#237292=CARTESIAN_POINT('Ctrl Pts',(-24.904753637648,5.75017697890804,12.));
#237293=CARTESIAN_POINT('Ctrl Pts',(-24.884173146722,5.73228037976926,12.));
#237294=CARTESIAN_POINT('Ctrl Pts',(-24.8636067597669,5.71447804252027,
12.));
#237295=CARTESIAN_POINT('Ctrl Pts',(-24.8430549277621,5.69677006679444,
12.));
#237296=CARTESIAN_POINT('Ctrl Pts',(-24.8225181223845,5.67915655496542,
12.));
#237297=CARTESIAN_POINT('Ctrl Pts',(-24.8019968304605,5.66163761114921,
12.));
#237298=CARTESIAN_POINT('Ctrl Pts',(-24.781491549672,5.6442133404226,12.));
#237299=CARTESIAN_POINT('Ctrl Pts',(-24.7610027835697,5.62688384790923,
12.));
#237300=CARTESIAN_POINT('Ctrl Pts',(-24.7405310372739,5.60964923798491,
12.));
#237301=CARTESIAN_POINT('Ctrl Pts',(-24.7200768119088,5.59250961323987,
12.));
#237302=CARTESIAN_POINT('Ctrl Pts',(-24.6996406035517,5.57546507427754,
12.));
#237303=CARTESIAN_POINT('Ctrl Pts',(-24.6792229061794,5.55851572025376,
12.));
#237304=CARTESIAN_POINT('Ctrl Pts',(-24.6588242134738,5.54166164919583,
12.));
#237305=CARTESIAN_POINT('Ctrl Pts',(-24.6384450211467,5.52490295840991,
12.));
#237306=CARTESIAN_POINT('Ctrl Pts',(-24.6180858289179,5.50823974481962,
12.));
#237307=CARTESIAN_POINT('Ctrl Pts',(-24.5977471429364,5.49167210537246,
12.));
#237308=CARTESIAN_POINT('Ctrl Pts',(-24.5774294770329,5.47520013724419,
12.));
#237309=CARTESIAN_POINT('Ctrl Pts',(-24.5571333514842,5.45882393762261,
12.));
#237310=CARTESIAN_POINT('Ctrl Pts',(-24.5368592922863,5.4425436035688,12.));
#237311=CARTESIAN_POINT('Ctrl Pts',(-24.5166078302108,5.42635923183419,
12.));
#237312=CARTESIAN_POINT('Ctrl Pts',(-24.4963794999831,5.41027091869241,
12.));
#237313=CARTESIAN_POINT('Ctrl Pts',(-24.4761748393321,5.39427875973824,
12.));
#237314=CARTESIAN_POINT('Ctrl Pts',(-24.4559943883157,5.37838284973695,
12.));
#237315=CARTESIAN_POINT('Ctrl Pts',(-24.435838689915,5.36258328273627,12.));
#237316=CARTESIAN_POINT('Ctrl Pts',(-24.4157082904614,5.34688015213537,
12.));
#237317=CARTESIAN_POINT('Ctrl Pts',(-24.3956037401293,5.33127355076033,
12.));
#237318=CARTESIAN_POINT('Ctrl Pts',(-24.3755255933917,5.31576357092526,
12.));
#237319=CARTESIAN_POINT('Ctrl Pts',(-24.3554744095075,5.30035030449063,
12.));
#237320=CARTESIAN_POINT('Ctrl Pts',(-24.3354507529414,5.28503384290648,
12.));
#237321=CARTESIAN_POINT('Ctrl Pts',(-24.3154551932221,5.26981427718798,
12.));
#237322=CARTESIAN_POINT('Ctrl Pts',(-24.2954883048447,5.25469169788856,
12.));
#237323=CARTESIAN_POINT('Ctrl Pts',(-24.2755506671525,5.23966619506289,
12.));
#237324=CARTESIAN_POINT('Ctrl Pts',(-24.2556428642294,5.22473785822442,
12.));
#237325=CARTESIAN_POINT('Ctrl Pts',(-24.2357654847766,5.20990677629176,
12.));
#237326=CARTESIAN_POINT('Ctrl Pts',(-24.2159191220171,5.19517303753647,
12.));
#237327=CARTESIAN_POINT('Ctrl Pts',(-24.1961043738756,5.18053672961398,
12.));
#237328=CARTESIAN_POINT('Ctrl Pts',(-24.1763218431344,5.16599793957985,
12.));
#237329=CARTESIAN_POINT('Ctrl Pts',(-24.1565721375971,5.15155675390079,
12.));
#237330=CARTESIAN_POINT('Ctrl Pts',(-24.1368558702443,5.13721325845745,
12.));
#237331=CARTESIAN_POINT('Ctrl Pts',(-24.117173659394,5.12296753853857,12.));
#237332=CARTESIAN_POINT('Ctrl Pts',(-24.0975261288444,5.10881967883124,
12.));
#237333=CARTESIAN_POINT('Ctrl Pts',(-24.0779139079264,5.09476976342616,
12.));
#237334=CARTESIAN_POINT('Ctrl Pts',(-24.0583376315636,5.0808178758127,12.));
#237335=CARTESIAN_POINT('Ctrl Pts',(-24.0387979403268,5.06696409886639,
12.));
#237336=CARTESIAN_POINT('Ctrl Pts',(-24.0192954804896,5.05320851483068,
12.));
#237337=CARTESIAN_POINT('Ctrl Pts',(-23.9998309040747,5.03955120528527,
12.));
#237338=CARTESIAN_POINT('Ctrl Pts',(-23.9804048689228,5.02599225112461,
12.));
#237339=CARTESIAN_POINT('Ctrl Pts',(-23.9610180388271,5.01253173257458,
12.));
#237340=CARTESIAN_POINT('Ctrl Pts',(-23.9416710836529,4.99916972919309,
12.));
#237341=CARTESIAN_POINT('Ctrl Pts',(-23.9223646794591,4.98590631986532,
12.));
#237342=CARTESIAN_POINT('Ctrl Pts',(-23.9030995086164,4.97274158279228,
12.));
#237343=CARTESIAN_POINT('Ctrl Pts',(-23.883876259922,4.95967559546565,12.));
#237344=CARTESIAN_POINT('Ctrl Pts',(-23.8646956287172,4.94670843465868,
12.));
#237345=CARTESIAN_POINT('Ctrl Pts',(-23.8455583170062,4.93384017643441,
12.));
#237346=CARTESIAN_POINT('Ctrl Pts',(-23.8264650335721,4.92107089613976,
12.));
#237347=CARTESIAN_POINT('Ctrl Pts',(-23.8074164940897,4.90840066839346,
12.));
#237348=CARTESIAN_POINT('Ctrl Pts',(-23.7884134212381,4.89582956706771,
12.));
#237349=CARTESIAN_POINT('Ctrl Pts',(-23.7694565448044,4.88335766525565,
12.));
#237350=CARTESIAN_POINT('Ctrl Pts',(-23.7505466018239,4.87098503527142,
12.));
#237351=CARTESIAN_POINT('Ctrl Pts',(-23.7316843367308,4.85871174865491,
12.));
#237352=CARTESIAN_POINT('Ctrl Pts',(-23.7128705015014,4.84653787616422,
12.));
#237353=CARTESIAN_POINT('Ctrl Pts',(-23.6941058557971,4.83446348776267,
12.));
#237354=CARTESIAN_POINT('Ctrl Pts',(-23.6753911671023,4.82248865259569,
12.));
#237355=CARTESIAN_POINT('Ctrl Pts',(-23.6567272108631,4.81061343896442,
12.));
#237356=CARTESIAN_POINT('Ctrl Pts',(-23.6381147706581,4.79883791433229,
12.));
#237357=CARTESIAN_POINT('Ctrl Pts',(-23.6195546383625,4.78716214532104,
12.));
#237358=CARTESIAN_POINT('Ctrl Pts',(-23.6010476143099,4.77558619769875,
12.));
#237359=CARTESIAN_POINT('Ctrl Pts',(-23.5825945074535,4.7641101363625,12.));
#237360=CARTESIAN_POINT('Ctrl Pts',(-23.564196135517,4.75273402530615,12.));
#237361=CARTESIAN_POINT('Ctrl Pts',(-23.5458533251715,4.74145792760698,
12.));
#237362=CARTESIAN_POINT('Ctrl Pts',(-23.5275669122378,4.73028190543031,
12.));
#237363=CARTESIAN_POINT('Ctrl Pts',(-23.5093377418784,4.71920602001904,
12.));
#237364=CARTESIAN_POINT('Ctrl Pts',(-23.491166668789,4.7082303316782,12.));
#237365=CARTESIAN_POINT('Ctrl Pts',(-23.4730545573849,4.69735489975023,
12.));
#237366=CARTESIAN_POINT('Ctrl Pts',(-23.4550022819853,4.68657978258297,
12.));
#237367=CARTESIAN_POINT('Ctrl Pts',(-23.4370107270444,4.6759050375305,12.));
#237368=CARTESIAN_POINT('Ctrl Pts',(-23.4190807873798,4.66533072094663,
12.));
#237369=CARTESIAN_POINT('Ctrl Pts',(-23.4012133683957,4.65485688816921,
12.));
#237370=CARTESIAN_POINT('Ctrl Pts',(-23.383409386307,4.64448359349935,12.));
#237371=CARTESIAN_POINT('Ctrl Pts',(-23.3656697683496,4.63421089016554,
12.));
#237372=CARTESIAN_POINT('Ctrl Pts',(-23.3479954530281,4.62403883030823,
12.));
#237373=CARTESIAN_POINT('Ctrl Pts',(-23.3303873903947,4.61396746497848,
12.));
#237374=CARTESIAN_POINT('Ctrl Pts',(-23.3128465423119,4.60399684412174,
12.));
#237375=CARTESIAN_POINT('Ctrl Pts',(-23.295373882719,4.59412701655749,12.));
#237376=CARTESIAN_POINT('Ctrl Pts',(-23.2779703978868,4.58435802994674,
12.));
#237377=CARTESIAN_POINT('Ctrl Pts',(-23.2606370866853,4.5746899307607,12.));
#237378=CARTESIAN_POINT('Ctrl Pts',(-23.2433749609117,4.5651227642781,12.));
#237379=CARTESIAN_POINT('Ctrl Pts',(-23.2261850456055,4.55565657456956,
12.));
#237380=CARTESIAN_POINT('Ctrl Pts',(-23.2090683793627,4.54629140447542,
12.));
#237381=CARTESIAN_POINT('Ctrl Pts',(-23.1920260146474,4.53702729557585,
12.));
#237382=CARTESIAN_POINT('Ctrl Pts',(-23.1750590180923,4.52786428815047,
12.));
#237383=CARTESIAN_POINT('Ctrl Pts',(-23.1581684708778,4.51880242116785,
12.));
#237384=CARTESIAN_POINT('Ctrl Pts',(-23.1413554691136,4.50984173227087,
12.));
#237385=CARTESIAN_POINT('Ctrl Pts',(-23.1246211242117,4.50098225775178,
12.));
#237386=CARTESIAN_POINT('Ctrl Pts',(-23.1079665632629,4.49222403252201,
12.));
#237387=CARTESIAN_POINT('Ctrl Pts',(-23.0913929293909,4.48356709006756,
12.));
#237388=CARTESIAN_POINT('Ctrl Pts',(-23.0749013821868,4.47501146242821,
12.));
#237389=CARTESIAN_POINT('Ctrl Pts',(-23.0584930981723,4.46655718018205,
12.));
#237390=CARTESIAN_POINT('Ctrl Pts',(-23.0421692712466,4.45820427241676,
12.));
#237391=CARTESIAN_POINT('Ctrl Pts',(-23.0259311131395,4.44995276669698,
12.));
#237392=CARTESIAN_POINT('Ctrl Pts',(-23.0097798538399,4.44180268901666,
12.));
#237393=CARTESIAN_POINT('Ctrl Pts',(-22.9937167421009,4.43375406376904,
12.));
#237394=CARTESIAN_POINT('Ctrl Pts',(-22.9777430460021,4.42580691372771,
12.));
#237395=CARTESIAN_POINT('Ctrl Pts',(-22.9618600534866,4.41796126001309,
12.));
#237396=CARTESIAN_POINT('Ctrl Pts',(-22.9460690729093,4.41021712205547,
12.));
#237397=CARTESIAN_POINT('Ctrl Pts',(-22.9303714335549,4.40257451754307,
12.));
#237398=CARTESIAN_POINT('Ctrl Pts',(-22.9147684862425,4.39503346238454,
12.));
#237399=CARTESIAN_POINT('Ctrl Pts',(-22.8992616040108,4.38759397068391,
12.));
#237400=CARTESIAN_POINT('Ctrl Pts',(-22.8838521827702,4.38025605470089,
12.));
#237401=CARTESIAN_POINT('Ctrl Pts',(-22.8685416419725,4.37301972480752,
12.));
#237402=CARTESIAN_POINT('Ctrl Pts',(-22.8533314252419,4.36588498943009,
12.));
#237403=CARTESIAN_POINT('Ctrl Pts',(-22.838223001118,4.35885185500559,12.));
#237404=CARTESIAN_POINT('Ctrl Pts',(-22.8232178638873,4.35192032594801,
12.));
#237405=CARTESIAN_POINT('Ctrl Pts',(-22.808317534379,4.34509040460065,12.));
#237406=CARTESIAN_POINT('Ctrl Pts',(-22.7935235607807,4.33836209118442,
12.));
#237407=CARTESIAN_POINT('Ctrl Pts',(-22.7788375194081,4.33173538373182,
12.));
#237408=CARTESIAN_POINT('Ctrl Pts',(-22.764261015648,4.32521027803747,12.));
#237409=CARTESIAN_POINT('Ctrl Pts',(-22.7497956849852,4.3187867676123,12.));
#237410=CARTESIAN_POINT('Ctrl Pts',(-22.7354431939927,4.3124648436255,12.));
#237411=CARTESIAN_POINT('Ctrl Pts',(-22.7212052413384,4.30624449484074,
12.));
#237412=CARTESIAN_POINT('Ctrl Pts',(-22.707083558756,4.30012570754066,12.));
#237413=CARTESIAN_POINT('Ctrl Pts',(-22.6930799122545,4.29410846547061,
12.));
#237414=CARTESIAN_POINT('Ctrl Pts',(-22.6791961033537,4.28819274977766,
12.));
#237415=CARTESIAN_POINT('Ctrl Pts',(-22.665433970311,4.28237853894059,12.));
#237416=CARTESIAN_POINT('Ctrl Pts',(-22.6517953893303,4.27666580869117,
12.));
#237417=CARTESIAN_POINT('Ctrl Pts',(-22.6382822758171,4.27105453192999,
12.));
#237418=CARTESIAN_POINT('Ctrl Pts',(-22.6248965859975,4.26554467865571,
12.));
#237419=CARTESIAN_POINT('Ctrl Pts',(-22.611640318482,4.26013621588303,12.));
#237420=CARTESIAN_POINT('Ctrl Pts',(-22.5985155158637,4.25482910755485,
12.));
#237421=CARTESIAN_POINT('Ctrl Pts',(-22.5855242662479,4.24962331444184,
12.));
#237422=CARTESIAN_POINT('Ctrl Pts',(-22.5726687049922,4.24451879404858,
12.));
#237423=CARTESIAN_POINT('Ctrl Pts',(-22.559951016643,4.23951550052526,12.));
#237424=CARTESIAN_POINT('Ctrl Pts',(-22.5473734368086,4.23461338456713,
12.));
#237425=CARTESIAN_POINT('Ctrl Pts',(-22.5349382540587,4.22981239330731,
12.));
#237426=CARTESIAN_POINT('Ctrl Pts',(-22.5226478117885,4.2251124702004,12.));
#237427=CARTESIAN_POINT('Ctrl Pts',(-22.5105045108882,4.22051355490196,
12.));
#237428=CARTESIAN_POINT('Ctrl Pts',(-22.4985108124229,4.21601558313908,
12.));
#237429=CARTESIAN_POINT('Ctrl Pts',(-22.4866692403147,4.21161848657428,
12.));
#237430=CARTESIAN_POINT('Ctrl Pts',(-22.4749823839915,4.20732219265648,
12.));
#237431=CARTESIAN_POINT('Ctrl Pts',(-22.4634529011433,4.2031266244817,12.));
#237432=CARTESIAN_POINT('Ctrl Pts',(-22.4520835205419,4.19903170066354,
12.));
#237433=CARTESIAN_POINT('Ctrl Pts',(-22.4408770448917,4.1950373351886,12.));
#237434=CARTESIAN_POINT('Ctrl Pts',(-22.4298363535421,4.19114343726941,
12.));
#237435=CARTESIAN_POINT('Ctrl Pts',(-22.4189644056115,4.1873499111772,12.));
#237436=CARTESIAN_POINT('Ctrl Pts',(-22.4082642454453,4.1836566560085,12.));
#237437=CARTESIAN_POINT('Ctrl Pts',(-22.3977390078075,4.18006356544882,
12.));
#237438=CARTESIAN_POINT('Ctrl Pts',(-22.3873919231334,4.17657052752825,
12.));
#237439=CARTESIAN_POINT('Ctrl Pts',(-22.3772263228617,4.17317742436145,
12.));
#237440=CARTESIAN_POINT('Ctrl Pts',(-22.36724564276,4.16988413199457,12.));
#237441=CARTESIAN_POINT('Ctrl Pts',(-22.3574534257396,4.166690520266,12.));
#237442=CARTESIAN_POINT('Ctrl Pts',(-22.3478533253889,4.16359645263187,
12.));
#237443=CARTESIAN_POINT('Ctrl Pts',(-22.3384491078602,4.16060178604164,
12.));
#237444=CARTESIAN_POINT('Ctrl Pts',(-22.3292446628959,4.15770637047889,
12.));
#237445=CARTESIAN_POINT('Ctrl Pts',(-22.3202440186979,4.15491004835281,
12.));
#237446=CARTESIAN_POINT('Ctrl Pts',(-22.3114513545185,4.1522126539699,12.));
#237447=CARTESIAN_POINT('Ctrl Pts',(-22.3028710166933,4.14961401285522,
12.));
#237448=CARTESIAN_POINT('Ctrl Pts',(-22.2945075198467,4.14711394168556,
12.));
#237449=CARTESIAN_POINT('Ctrl Pts',(-22.2863655389166,4.14471224859295,
12.));
#237450=CARTESIAN_POINT('Ctrl Pts',(-22.2784499072027,4.14240873321984,
12.));
#237451=CARTESIAN_POINT('Ctrl Pts',(-22.2707656042457,4.14020318715991,
12.));
#237452=CARTESIAN_POINT('Ctrl Pts',(-22.2633177913972,4.13809539255421,
12.));
#237453=CARTESIAN_POINT('Ctrl Pts',(-22.2561118708421,4.13608511977225,
12.));
#237454=CARTESIAN_POINT('Ctrl Pts',(-22.249153531779,4.1341721255881,12.));
#237455=CARTESIAN_POINT('Ctrl Pts',(-22.2424488153523,4.1323561506016,12.));
#237456=CARTESIAN_POINT('Ctrl Pts',(-22.2360040565533,4.13063692157498,
12.));
#237457=CARTESIAN_POINT('Ctrl Pts',(-22.2298258043947,4.12901415463379,
12.));
#237458=CARTESIAN_POINT('Ctrl Pts',(-22.2239207458781,4.12748755830104,
12.));
#237459=CARTESIAN_POINT('Ctrl Pts',(-22.2182956401341,4.12605683613307,
12.));
#237460=CARTESIAN_POINT('Ctrl Pts',(-22.2129576146671,4.12472167516607,
12.));
#237461=CARTESIAN_POINT('Ctrl Pts',(-22.2079143941719,4.12348173702023,
12.));
#237462=CARTESIAN_POINT('Ctrl Pts',(-22.2031746532106,4.12233664408227,
12.));
#237463=CARTESIAN_POINT('Ctrl Pts',(-22.1987479618246,4.12128598183522,
12.));
#237464=CARTESIAN_POINT('Ctrl Pts',(-22.1946440958098,4.12032932637736,
12.));
#237465=CARTESIAN_POINT('Ctrl Pts',(-22.1908725908525,4.11946626228636,
12.));
#237466=CARTESIAN_POINT('Ctrl Pts',(-22.1874419861496,4.11869641271773,
12.));
#237467=CARTESIAN_POINT('Ctrl Pts',(-22.1843613164855,4.11801938107479,
12.));
#237468=CARTESIAN_POINT('Ctrl Pts',(-22.1816414985788,4.11743469691756,
12.));
#237469=CARTESIAN_POINT('Ctrl Pts',(-22.179297473024,4.11694173195003,12.));
#237470=CARTESIAN_POINT('Ctrl Pts',(-22.177347426894,4.11653973150518,12.));
#237471=CARTESIAN_POINT('Ctrl Pts',(-22.1758088296598,4.11622797217068,
12.));
#237472=CARTESIAN_POINT('Ctrl Pts',(-22.1746949858775,4.11600589882845,
12.));
#237473=CARTESIAN_POINT('Ctrl Pts',(-22.1741488021234,4.11589976826166,
12.));
#237474=CARTESIAN_POINT('Ctrl Pts',(-22.1739341411687,4.11586035878287,
12.));
#237475=CARTESIAN_POINT('Ctrl Pts',(-22.173877682324,4.11585194677442,12.));
#237476=CARTESIAN_POINT('Ctrl Pts',(-22.1738711152697,4.11585220600461,
12.));
#237477=CARTESIAN_POINT('',(-25.2771067246846,6.08833931617699,0.));
#237478=CARTESIAN_POINT('Origin',(-19.4030938020118,9.26120677397565,0.));
#237479=CARTESIAN_POINT('',(-20.353053841303,9.71462809124917,12.));
#237480=CARTESIAN_POINT('',(-9.70154690100589,4.63060338698782,12.));
#237481=CARTESIAN_POINT('',(-20.353053841303,9.71462809124917,0.));
#237482=CARTESIAN_POINT('',(-20.353053841303,9.71462809124917,0.));
#237483=CARTESIAN_POINT('',(-9.70154690100589,4.63060338698782,0.));
#237484=CARTESIAN_POINT('Ctrl Pts',(-24.9347862158358,7.36589684767345,
0.));
#237485=CARTESIAN_POINT('Ctrl Pts',(-24.9347862158358,7.36589684767345,
12.));
#237486=CARTESIAN_POINT('Ctrl Pts',(-24.9292275670674,7.36721909028843,
0.));
#237487=CARTESIAN_POINT('Ctrl Pts',(-24.9292275670674,7.36721909028843,
12.));
#237488=CARTESIAN_POINT('Ctrl Pts',(-24.9181155530543,7.3698559312009,0.));
#237489=CARTESIAN_POINT('Ctrl Pts',(-24.9181155530543,7.3698559312009,12.));
#237490=CARTESIAN_POINT('Ctrl Pts',(-24.901463382605,7.37378825961676,0.));
#237491=CARTESIAN_POINT('Ctrl Pts',(-24.901463382605,7.37378825961676,12.));
#237492=CARTESIAN_POINT('Ctrl Pts',(-24.8792921911115,7.3789854964027,0.));
#237493=CARTESIAN_POINT('Ctrl Pts',(-24.8792921911115,7.3789854964027,12.));
#237494=CARTESIAN_POINT('Ctrl Pts',(-24.8516310625176,7.38540558903621,
0.));
#237495=CARTESIAN_POINT('Ctrl Pts',(-24.8516310625176,7.38540558903621,
12.));
#237496=CARTESIAN_POINT('Ctrl Pts',(-24.8240228520893,7.39174922585808,
0.));
#237497=CARTESIAN_POINT('Ctrl Pts',(-24.8240228520893,7.39174922585808,
12.));
#237498=CARTESIAN_POINT('Ctrl Pts',(-24.7964676646431,7.39801641583013,
0.));
#237499=CARTESIAN_POINT('Ctrl Pts',(-24.7964676646431,7.39801641583013,
12.));
#237500=CARTESIAN_POINT('Ctrl Pts',(-24.7689656668983,7.40420718661603,
0.));
#237501=CARTESIAN_POINT('Ctrl Pts',(-24.7689656668983,7.40420718661603,
12.));
#237502=CARTESIAN_POINT('Ctrl Pts',(-24.7415170994784,7.41032159082382,
0.));
#237503=CARTESIAN_POINT('Ctrl Pts',(-24.7415170994784,7.41032159082382,
12.));
#237504=CARTESIAN_POINT('Ctrl Pts',(-24.7141222950051,7.41635971481674,
0.));
#237505=CARTESIAN_POINT('Ctrl Pts',(-24.7141222950051,7.41635971481674,
12.));
#237506=CARTESIAN_POINT('Ctrl Pts',(-24.6867816727192,7.42232167766265,
0.));
#237507=CARTESIAN_POINT('Ctrl Pts',(-24.6867816727192,7.42232167766265,
12.));
#237508=CARTESIAN_POINT('Ctrl Pts',(-24.6594957128756,7.42820762159126,
0.));
#237509=CARTESIAN_POINT('Ctrl Pts',(-24.6594957128756,7.42820762159126,
12.));
#237510=CARTESIAN_POINT('Ctrl Pts',(-24.6322649369517,7.43401770489524,
0.));
#237511=CARTESIAN_POINT('Ctrl Pts',(-24.6322649369517,7.43401770489524,
12.));
#237512=CARTESIAN_POINT('Ctrl Pts',(-24.6050898852368,7.43975209375504,
0.));
#237513=CARTESIAN_POINT('Ctrl Pts',(-24.6050898852368,7.43975209375504,
12.));
#237514=CARTESIAN_POINT('Ctrl Pts',(-24.577971096086,7.44541095473134,0.));
#237515=CARTESIAN_POINT('Ctrl Pts',(-24.577971096086,7.44541095473134,12.));
#237516=CARTESIAN_POINT('Ctrl Pts',(-24.5509090831559,7.4509944465116,0.));
#237517=CARTESIAN_POINT('Ctrl Pts',(-24.5509090831559,7.4509944465116,12.));
#237518=CARTESIAN_POINT('Ctrl Pts',(-24.5239043173072,7.45650271335862,
0.));
#237519=CARTESIAN_POINT('Ctrl Pts',(-24.5239043173072,7.45650271335862,
12.));
#237520=CARTESIAN_POINT('Ctrl Pts',(-24.4969572391483,7.46193588961463,
0.));
#237521=CARTESIAN_POINT('Ctrl Pts',(-24.4969572391483,7.46193588961463,
12.));
#237522=CARTESIAN_POINT('Ctrl Pts',(-24.4700682684524,7.46729410308786,
0.));
#237523=CARTESIAN_POINT('Ctrl Pts',(-24.4700682684524,7.46729410308786,
12.));
#237524=CARTESIAN_POINT('Ctrl Pts',(-24.443237814649,7.47257747883246,0.));
#237525=CARTESIAN_POINT('Ctrl Pts',(-24.443237814649,7.47257747883246,12.));
#237526=CARTESIAN_POINT('Ctrl Pts',(-24.4164662871163,7.47778614286565,
0.));
#237527=CARTESIAN_POINT('Ctrl Pts',(-24.4164662871163,7.47778614286565,
12.));
#237528=CARTESIAN_POINT('Ctrl Pts',(-24.3897541049254,7.48292022569301,
0.));
#237529=CARTESIAN_POINT('Ctrl Pts',(-24.3897541049254,7.48292022569301,
12.));
#237530=CARTESIAN_POINT('Ctrl Pts',(-24.3631017084524,7.48797986651908,
0.));
#237531=CARTESIAN_POINT('Ctrl Pts',(-24.3631017084524,7.48797986651908,
12.));
#237532=CARTESIAN_POINT('Ctrl Pts',(-24.3365095573685,7.4929652125242,0.));
#237533=CARTESIAN_POINT('Ctrl Pts',(-24.3365095573685,7.4929652125242,12.));
#237534=CARTESIAN_POINT('Ctrl Pts',(-24.3099781253355,7.49787641695439,
0.));
#237535=CARTESIAN_POINT('Ctrl Pts',(-24.3099781253355,7.49787641695439,
12.));
#237536=CARTESIAN_POINT('Ctrl Pts',(-24.2835078958973,7.50271363765152,
0.));
#237537=CARTESIAN_POINT('Ctrl Pts',(-24.2835078958973,7.50271363765152,
12.));
#237538=CARTESIAN_POINT('Ctrl Pts',(-24.2570993577034,7.50747703535133,
0.));
#237539=CARTESIAN_POINT('Ctrl Pts',(-24.2570993577034,7.50747703535133,
12.));
#237540=CARTESIAN_POINT('Ctrl Pts',(-24.2307530003887,7.51216677222181,
0.));
#237541=CARTESIAN_POINT('Ctrl Pts',(-24.2307530003887,7.51216677222181,
12.));
#237542=CARTESIAN_POINT('Ctrl Pts',(-24.2044693092349,7.51678300997949,
0.));
#237543=CARTESIAN_POINT('Ctrl Pts',(-24.2044693092349,7.51678300997949,
12.));
#237544=CARTESIAN_POINT('Ctrl Pts',(-24.1782487641594,7.52132590953802,
0.));
#237545=CARTESIAN_POINT('Ctrl Pts',(-24.1782487641594,7.52132590953802,
12.));
#237546=CARTESIAN_POINT('Ctrl Pts',(-24.1520918425364,7.52579563201424,
0.));
#237547=CARTESIAN_POINT('Ctrl Pts',(-24.1520918425364,7.52579563201424,
12.));
#237548=CARTESIAN_POINT('Ctrl Pts',(-24.1259990209207,7.53019233935501,
0.));
#237549=CARTESIAN_POINT('Ctrl Pts',(-24.1259990209207,7.53019233935501,
12.));
#237550=CARTESIAN_POINT('Ctrl Pts',(-24.0999707772642,7.53451619514649,
0.));
#237551=CARTESIAN_POINT('Ctrl Pts',(-24.0999707772642,7.53451619514649,
12.));
#237552=CARTESIAN_POINT('Ctrl Pts',(-24.0740075927985,7.53876736531014,
0.));
#237553=CARTESIAN_POINT('Ctrl Pts',(-24.0740075927985,7.53876736531014,
12.));
#237554=CARTESIAN_POINT('Ctrl Pts',(-24.0481099543353,7.54294601896144,
0.));
#237555=CARTESIAN_POINT('Ctrl Pts',(-24.0481099543353,7.54294601896144,
12.));
#237556=CARTESIAN_POINT('Ctrl Pts',(-24.022278355453,7.5470523288591,0.));
#237557=CARTESIAN_POINT('Ctrl Pts',(-24.022278355453,7.5470523288591,12.));
#237558=CARTESIAN_POINT('Ctrl Pts',(-23.9965132953185,7.55108647097441,
0.));
#237559=CARTESIAN_POINT('Ctrl Pts',(-23.9965132953185,7.55108647097441,
12.));
#237560=CARTESIAN_POINT('Ctrl Pts',(-23.9708152779884,7.55504862424812,
0.));
#237561=CARTESIAN_POINT('Ctrl Pts',(-23.9708152779884,7.55504862424812,
12.));
#237562=CARTESIAN_POINT('Ctrl Pts',(-23.9451848115,7.55893897027682,0.));
#237563=CARTESIAN_POINT('Ctrl Pts',(-23.9451848115,7.55893897027682,12.));
#237564=CARTESIAN_POINT('Ctrl Pts',(-23.9196224070759,7.56275769304773,
0.));
#237565=CARTESIAN_POINT('Ctrl Pts',(-23.9196224070759,7.56275769304773,
12.));
#237566=CARTESIAN_POINT('Ctrl Pts',(-23.8941285782003,7.56650497863792,
0.));
#237567=CARTESIAN_POINT('Ctrl Pts',(-23.8941285782003,7.56650497863792,
12.));
#237568=CARTESIAN_POINT('Ctrl Pts',(-23.8687038399598,7.57018101500711,
0.));
#237569=CARTESIAN_POINT('Ctrl Pts',(-23.8687038399598,7.57018101500711,
12.));
#237570=CARTESIAN_POINT('Ctrl Pts',(-23.8433487096134,7.57378599219816,
0.));
#237571=CARTESIAN_POINT('Ctrl Pts',(-23.8433487096134,7.57378599219816,
12.));
#237572=CARTESIAN_POINT('Ctrl Pts',(-23.8180637069977,7.57732010249066,
0.));
#237573=CARTESIAN_POINT('Ctrl Pts',(-23.8180637069977,7.57732010249066,
12.));
#237574=CARTESIAN_POINT('Ctrl Pts',(-23.7928493549908,7.58078354058212,
0.));
#237575=CARTESIAN_POINT('Ctrl Pts',(-23.7928493549908,7.58078354058212,
12.));
#237576=CARTESIAN_POINT('Ctrl Pts',(-23.7677061799376,7.58417650376272,
0.));
#237577=CARTESIAN_POINT('Ctrl Pts',(-23.7677061799376,7.58417650376272,
12.));
#237578=CARTESIAN_POINT('Ctrl Pts',(-23.7426347121006,7.58749919210832,
0.));
#237579=CARTESIAN_POINT('Ctrl Pts',(-23.7426347121006,7.58749919210832,
12.));
#237580=CARTESIAN_POINT('Ctrl Pts',(-23.7176354860457,7.59075180865327,
0.));
#237581=CARTESIAN_POINT('Ctrl Pts',(-23.7176354860457,7.59075180865327,
12.));
#237582=CARTESIAN_POINT('Ctrl Pts',(-23.6927090405067,7.59393455934042,
0.));
#237583=CARTESIAN_POINT('Ctrl Pts',(-23.6927090405067,7.59393455934042,
12.));
#237584=CARTESIAN_POINT('Ctrl Pts',(-23.6678559182876,7.59704765299572,
0.));
#237585=CARTESIAN_POINT('Ctrl Pts',(-23.6678559182876,7.59704765299572,
12.));
#237586=CARTESIAN_POINT('Ctrl Pts',(-23.6430766661419,7.60009130130129,
0.));
#237587=CARTESIAN_POINT('Ctrl Pts',(-23.6430766661419,7.60009130130129,
12.));
#237588=CARTESIAN_POINT('Ctrl Pts',(-23.6183718346576,7.60306571877806,
0.));
#237589=CARTESIAN_POINT('Ctrl Pts',(-23.6183718346576,7.60306571877806,
12.));
#237590=CARTESIAN_POINT('Ctrl Pts',(-23.5937419781244,7.60597112277094,
0.));
#237591=CARTESIAN_POINT('Ctrl Pts',(-23.5937419781244,7.60597112277094,
12.));
#237592=CARTESIAN_POINT('Ctrl Pts',(-23.5691876544243,7.60880773344599,
0.));
#237593=CARTESIAN_POINT('Ctrl Pts',(-23.5691876544243,7.60880773344599,
12.));
#237594=CARTESIAN_POINT('Ctrl Pts',(-23.5447094252029,7.61157577385372,
0.));
#237595=CARTESIAN_POINT('Ctrl Pts',(-23.5447094252029,7.61157577385372,
12.));
#237596=CARTESIAN_POINT('Ctrl Pts',(-23.5203078560128,7.61427546999299,
0.));
#237597=CARTESIAN_POINT('Ctrl Pts',(-23.5203078560128,7.61427546999299,
12.));
#237598=CARTESIAN_POINT('Ctrl Pts',(-23.4959835164608,7.61690705088319,
0.));
#237599=CARTESIAN_POINT('Ctrl Pts',(-23.4959835164608,7.61690705088319,
12.));
#237600=CARTESIAN_POINT('Ctrl Pts',(-23.4717369803438,7.61947074863977,
0.));
#237601=CARTESIAN_POINT('Ctrl Pts',(-23.4717369803438,7.61947074863977,
12.));
#237602=CARTESIAN_POINT('Ctrl Pts',(-23.4475688257854,7.62196679855957,
0.));
#237603=CARTESIAN_POINT('Ctrl Pts',(-23.4475688257854,7.62196679855957,
12.));
#237604=CARTESIAN_POINT('Ctrl Pts',(-23.4234796353544,7.62439543920054,
0.));
#237605=CARTESIAN_POINT('Ctrl Pts',(-23.4234796353544,7.62439543920054,
12.));
#237606=CARTESIAN_POINT('Ctrl Pts',(-23.3994699961122,7.62675691240335,
0.));
#237607=CARTESIAN_POINT('Ctrl Pts',(-23.3994699961122,7.62675691240335,
12.));
#237608=CARTESIAN_POINT('Ctrl Pts',(-23.3755404996638,7.62905146332598,
0.));
#237609=CARTESIAN_POINT('Ctrl Pts',(-23.3755404996638,7.62905146332598,
12.));
#237610=CARTESIAN_POINT('Ctrl Pts',(-23.3516917421973,7.63127934048139,
0.));
#237611=CARTESIAN_POINT('Ctrl Pts',(-23.3516917421973,7.63127934048139,
12.));
#237612=CARTESIAN_POINT('Ctrl Pts',(-23.3279243245241,7.63344079578162,
0.));
#237613=CARTESIAN_POINT('Ctrl Pts',(-23.3279243245241,7.63344079578162,
12.));
#237614=CARTESIAN_POINT('Ctrl Pts',(-23.3042388521021,7.63553608458784,
0.));
#237615=CARTESIAN_POINT('Ctrl Pts',(-23.3042388521021,7.63553608458784,
12.));
#237616=CARTESIAN_POINT('Ctrl Pts',(-23.2806359350853,7.63756546576375,
0.));
#237617=CARTESIAN_POINT('Ctrl Pts',(-23.2806359350853,7.63756546576375,
12.));
#237618=CARTESIAN_POINT('Ctrl Pts',(-23.2571161884487,7.63952920172837,
0.));
#237619=CARTESIAN_POINT('Ctrl Pts',(-23.2571161884487,7.63952920172837,
12.));
#237620=CARTESIAN_POINT('Ctrl Pts',(-23.2336802320912,7.64142755851508,
0.));
#237621=CARTESIAN_POINT('Ctrl Pts',(-23.2336802320912,7.64142755851508,
12.));
#237622=CARTESIAN_POINT('Ctrl Pts',(-23.2103286909399,7.64326080583684,
0.));
#237623=CARTESIAN_POINT('Ctrl Pts',(-23.2103286909399,7.64326080583684,
12.));
#237624=CARTESIAN_POINT('Ctrl Pts',(-23.1870621950452,7.64502921715483,
0.));
#237625=CARTESIAN_POINT('Ctrl Pts',(-23.1870621950452,7.64502921715483,
12.));
#237626=CARTESIAN_POINT('Ctrl Pts',(-23.1638813796691,7.64673306975797,
0.));
#237627=CARTESIAN_POINT('Ctrl Pts',(-23.1638813796691,7.64673306975797,
12.));
#237628=CARTESIAN_POINT('Ctrl Pts',(-23.1407868853815,7.64837264482929,
0.));
#237629=CARTESIAN_POINT('Ctrl Pts',(-23.1407868853815,7.64837264482929,
12.));
#237630=CARTESIAN_POINT('Ctrl Pts',(-23.1177793581674,7.64994822749845,
0.));
#237631=CARTESIAN_POINT('Ctrl Pts',(-23.1177793581674,7.64994822749845,
12.));
#237632=CARTESIAN_POINT('Ctrl Pts',(-23.0948594495246,7.65146010690464,
0.));
#237633=CARTESIAN_POINT('Ctrl Pts',(-23.0948594495246,7.65146010690464,
12.));
#237634=CARTESIAN_POINT('Ctrl Pts',(-23.072027816555,7.65290857626356,0.));
#237635=CARTESIAN_POINT('Ctrl Pts',(-23.072027816555,7.65290857626356,12.));
#237636=CARTESIAN_POINT('Ctrl Pts',(-23.049285122053,7.65429393293955,0.));
#237637=CARTESIAN_POINT('Ctrl Pts',(-23.049285122053,7.65429393293955,12.));
#237638=CARTESIAN_POINT('Ctrl Pts',(-23.0266320345792,7.65561647852555,
0.));
#237639=CARTESIAN_POINT('Ctrl Pts',(-23.0266320345792,7.65561647852555,
12.));
#237640=CARTESIAN_POINT('Ctrl Pts',(-23.004069228582,7.6568765189133,0.));
#237641=CARTESIAN_POINT('Ctrl Pts',(-23.004069228582,7.6568765189133,12.));
#237642=CARTESIAN_POINT('Ctrl Pts',(-22.9815973845301,7.65807436436453,
0.));
#237643=CARTESIAN_POINT('Ctrl Pts',(-22.9815973845301,7.65807436436453,
12.));
#237644=CARTESIAN_POINT('Ctrl Pts',(-22.9592171890332,7.65921032958912,
0.));
#237645=CARTESIAN_POINT('Ctrl Pts',(-22.9592171890332,7.65921032958912,
12.));
#237646=CARTESIAN_POINT('Ctrl Pts',(-22.9369293349592,7.66028473382777,
0.));
#237647=CARTESIAN_POINT('Ctrl Pts',(-22.9369293349592,7.66028473382777,
12.));
#237648=CARTESIAN_POINT('Ctrl Pts',(-22.9147345215418,7.661297900941,0.));
#237649=CARTESIAN_POINT('Ctrl Pts',(-22.9147345215418,7.661297900941,12.));
#237650=CARTESIAN_POINT('Ctrl Pts',(-22.8926334544879,7.66225015950147,
0.));
#237651=CARTESIAN_POINT('Ctrl Pts',(-22.8926334544879,7.66225015950147,
12.));
#237652=CARTESIAN_POINT('Ctrl Pts',(-22.870626846128,7.66314184287334,0.));
#237653=CARTESIAN_POINT('Ctrl Pts',(-22.870626846128,7.66314184287334,12.));
#237654=CARTESIAN_POINT('Ctrl Pts',(-22.8487154155569,7.66397328929805,
0.));
#237655=CARTESIAN_POINT('Ctrl Pts',(-22.8487154155569,7.66397328929805,
12.));
#237656=CARTESIAN_POINT('Ctrl Pts',(-22.8268998887679,7.66474484198553,
0.));
#237657=CARTESIAN_POINT('Ctrl Pts',(-22.8268998887679,7.66474484198553,
12.));
#237658=CARTESIAN_POINT('Ctrl Pts',(-22.8051809987834,7.66545684920987,
0.));
#237659=CARTESIAN_POINT('Ctrl Pts',(-22.8051809987834,7.66545684920987,
12.));
#237660=CARTESIAN_POINT('Ctrl Pts',(-22.7835594857697,7.66610966441259,
0.));
#237661=CARTESIAN_POINT('Ctrl Pts',(-22.7835594857697,7.66610966441259,
12.));
#237662=CARTESIAN_POINT('Ctrl Pts',(-22.7620360971839,7.66670364630273,
0.));
#237663=CARTESIAN_POINT('Ctrl Pts',(-22.7620360971839,7.66670364630273,
12.));
#237664=CARTESIAN_POINT('Ctrl Pts',(-22.7406115879508,7.66723915895412,
0.));
#237665=CARTESIAN_POINT('Ctrl Pts',(-22.7406115879508,7.66723915895412,
12.));
#237666=CARTESIAN_POINT('Ctrl Pts',(-22.7192867206242,7.6677165719101,0.));
#237667=CARTESIAN_POINT('Ctrl Pts',(-22.7192867206242,7.6677165719101,12.));
#237668=CARTESIAN_POINT('Ctrl Pts',(-22.6980622655446,7.66813626029276,
0.));
#237669=CARTESIAN_POINT('Ctrl Pts',(-22.6980622655446,7.66813626029276,
12.));
#237670=CARTESIAN_POINT('Ctrl Pts',(-22.6769390009889,7.66849860491763,
0.));
#237671=CARTESIAN_POINT('Ctrl Pts',(-22.6769390009889,7.66849860491763,
12.));
#237672=CARTESIAN_POINT('Ctrl Pts',(-22.6559177133133,7.66880399241354,
0.));
#237673=CARTESIAN_POINT('Ctrl Pts',(-22.6559177133133,7.66880399241354,
12.));
#237674=CARTESIAN_POINT('Ctrl Pts',(-22.6349991971547,7.66905281533745,
0.));
#237675=CARTESIAN_POINT('Ctrl Pts',(-22.6349991971547,7.66905281533745,
12.));
#237676=CARTESIAN_POINT('Ctrl Pts',(-22.6141842556248,7.66924547229435,
0.));
#237677=CARTESIAN_POINT('Ctrl Pts',(-22.6141842556248,7.66924547229435,
12.));
#237678=CARTESIAN_POINT('Ctrl Pts',(-22.5934737004955,7.66938236806241,
0.));
#237679=CARTESIAN_POINT('Ctrl Pts',(-22.5934737004955,7.66938236806241,
12.));
#237680=CARTESIAN_POINT('Ctrl Pts',(-22.5728683523829,7.66946391372299,
0.));
#237681=CARTESIAN_POINT('Ctrl Pts',(-22.5728683523829,7.66946391372299,
12.));
#237682=CARTESIAN_POINT('Ctrl Pts',(-22.5523690409109,7.66949052679671,
0.));
#237683=CARTESIAN_POINT('Ctrl Pts',(-22.5523690409109,7.66949052679671,
12.));
#237684=CARTESIAN_POINT('Ctrl Pts',(-22.5319766049191,7.66946263138116,
0.));
#237685=CARTESIAN_POINT('Ctrl Pts',(-22.5319766049191,7.66946263138116,
12.));
#237686=CARTESIAN_POINT('Ctrl Pts',(-22.5116918927023,7.66938065829082,
0.));
#237687=CARTESIAN_POINT('Ctrl Pts',(-22.5116918927023,7.66938065829082,
12.));
#237688=CARTESIAN_POINT('Ctrl Pts',(-22.4915157622308,7.66924504520302,
0.));
#237689=CARTESIAN_POINT('Ctrl Pts',(-22.4915157622308,7.66924504520302,
12.));
#237690=CARTESIAN_POINT('Ctrl Pts',(-22.47144908137,7.66905623680835,0.));
#237691=CARTESIAN_POINT('Ctrl Pts',(-22.47144908137,7.66905623680835,12.));
#237692=CARTESIAN_POINT('Ctrl Pts',(-22.4514927280863,7.6688146849666,0.));
#237693=CARTESIAN_POINT('Ctrl Pts',(-22.4514927280863,7.6688146849666,12.));
#237694=CARTESIAN_POINT('Ctrl Pts',(-22.4316475906616,7.66852084886745,
0.));
#237695=CARTESIAN_POINT('Ctrl Pts',(-22.4316475906616,7.66852084886745,
12.));
#237696=CARTESIAN_POINT('Ctrl Pts',(-22.411914567977,7.66817519519682,0.));
#237697=CARTESIAN_POINT('Ctrl Pts',(-22.411914567977,7.66817519519682,12.));
#237698=CARTESIAN_POINT('Ctrl Pts',(-22.3922945697782,7.66777819830819,
0.));
#237699=CARTESIAN_POINT('Ctrl Pts',(-22.3922945697782,7.66777819830819,
12.));
#237700=CARTESIAN_POINT('Ctrl Pts',(-22.3727885169361,7.66733034039887,
0.));
#237701=CARTESIAN_POINT('Ctrl Pts',(-22.3727885169361,7.66733034039887,
12.));
#237702=CARTESIAN_POINT('Ctrl Pts',(-22.3533973417013,7.66683211169134,
0.));
#237703=CARTESIAN_POINT('Ctrl Pts',(-22.3533973417013,7.66683211169134,
12.));
#237704=CARTESIAN_POINT('Ctrl Pts',(-22.3341219879454,7.66628401061905,
0.));
#237705=CARTESIAN_POINT('Ctrl Pts',(-22.3341219879454,7.66628401061905,
12.));
#237706=CARTESIAN_POINT('Ctrl Pts',(-22.3149634114823,7.66568654402441,
0.));
#237707=CARTESIAN_POINT('Ctrl Pts',(-22.3149634114823,7.66568654402441,
12.));
#237708=CARTESIAN_POINT('Ctrl Pts',(-22.2959225803925,7.66504022736262,
0.));
#237709=CARTESIAN_POINT('Ctrl Pts',(-22.2959225803925,7.66504022736262,
12.));
#237710=CARTESIAN_POINT('Ctrl Pts',(-22.2770004753332,7.66434558490972,
0.));
#237711=CARTESIAN_POINT('Ctrl Pts',(-22.2770004753332,7.66434558490972,
12.));
#237712=CARTESIAN_POINT('Ctrl Pts',(-22.2581980898487,7.66360314997662,
0.));
#237713=CARTESIAN_POINT('Ctrl Pts',(-22.2581980898487,7.66360314997662,
12.));
#237714=CARTESIAN_POINT('Ctrl Pts',(-22.239516430656,7.66281346512545,0.));
#237715=CARTESIAN_POINT('Ctrl Pts',(-22.239516430656,7.66281346512545,12.));
#237716=CARTESIAN_POINT('Ctrl Pts',(-22.2209565180098,7.66197708240435,
0.));
#237717=CARTESIAN_POINT('Ctrl Pts',(-22.2209565180098,7.66197708240435,
12.));
#237718=CARTESIAN_POINT('Ctrl Pts',(-22.2025193860972,7.66109456359292,
0.));
#237719=CARTESIAN_POINT('Ctrl Pts',(-22.2025193860972,7.66109456359292,
12.));
#237720=CARTESIAN_POINT('Ctrl Pts',(-22.1842060834092,7.66016648045008,
0.));
#237721=CARTESIAN_POINT('Ctrl Pts',(-22.1842060834092,7.66016648045008,
12.));
#237722=CARTESIAN_POINT('Ctrl Pts',(-22.1660176731174,7.65919341496925,
0.));
#237723=CARTESIAN_POINT('Ctrl Pts',(-22.1660176731174,7.65919341496925,
12.));
#237724=CARTESIAN_POINT('Ctrl Pts',(-22.1479552334206,7.65817595963351,
0.));
#237725=CARTESIAN_POINT('Ctrl Pts',(-22.1479552334206,7.65817595963351,
12.));
#237726=CARTESIAN_POINT('Ctrl Pts',(-22.1300198579671,7.65711471769407,
0.));
#237727=CARTESIAN_POINT('Ctrl Pts',(-22.1300198579671,7.65711471769407,
12.));
#237728=CARTESIAN_POINT('Ctrl Pts',(-22.1122126563327,7.65601030346819,
0.));
#237729=CARTESIAN_POINT('Ctrl Pts',(-22.1122126563327,7.65601030346819,
12.));
#237730=CARTESIAN_POINT('Ctrl Pts',(-22.094534754469,7.6548633426365,0.));
#237731=CARTESIAN_POINT('Ctrl Pts',(-22.094534754469,7.6548633426365,12.));
#237732=CARTESIAN_POINT('Ctrl Pts',(-22.0769872951596,7.65367447254945,
0.));
#237733=CARTESIAN_POINT('Ctrl Pts',(-22.0769872951596,7.65367447254945,
12.));
#237734=CARTESIAN_POINT('Ctrl Pts',(-22.0595714384432,7.65244434253104,
0.));
#237735=CARTESIAN_POINT('Ctrl Pts',(-22.0595714384432,7.65244434253104,
12.));
#237736=CARTESIAN_POINT('Ctrl Pts',(-22.0422883621176,7.65117361421346,
0.));
#237737=CARTESIAN_POINT('Ctrl Pts',(-22.0422883621176,7.65117361421346,
12.));
#237738=CARTESIAN_POINT('Ctrl Pts',(-22.0251392623209,7.64986296190156,
0.));
#237739=CARTESIAN_POINT('Ctrl Pts',(-22.0251392623209,7.64986296190156,
12.));
#237740=CARTESIAN_POINT('Ctrl Pts',(-22.0081253540773,7.64851307293346,
0.));
#237741=CARTESIAN_POINT('Ctrl Pts',(-22.0081253540773,7.64851307293346,
12.));
#237742=CARTESIAN_POINT('Ctrl Pts',(-21.9912478718542,7.64712464805258,
0.));
#237743=CARTESIAN_POINT('Ctrl Pts',(-21.9912478718542,7.64712464805258,
12.));
#237744=CARTESIAN_POINT('Ctrl Pts',(-21.97450807008,7.64569840177359,0.));
#237745=CARTESIAN_POINT('Ctrl Pts',(-21.97450807008,7.64569840177359,12.));
#237746=CARTESIAN_POINT('Ctrl Pts',(-21.9579072237653,7.64423506279153,
0.));
#237747=CARTESIAN_POINT('Ctrl Pts',(-21.9579072237653,7.64423506279153,
12.));
#237748=CARTESIAN_POINT('Ctrl Pts',(-21.9414466292074,7.64273537442706,
0.));
#237749=CARTESIAN_POINT('Ctrl Pts',(-21.9414466292074,7.64273537442706,
12.));
#237750=CARTESIAN_POINT('Ctrl Pts',(-21.9251276046546,7.6412000950654,0.));
#237751=CARTESIAN_POINT('Ctrl Pts',(-21.9251276046546,7.6412000950654,12.));
#237752=CARTESIAN_POINT('Ctrl Pts',(-21.9089514909873,7.63962999860916,
0.));
#237753=CARTESIAN_POINT('Ctrl Pts',(-21.9089514909873,7.63962999860916,
12.));
#237754=CARTESIAN_POINT('Ctrl Pts',(-21.8929196523511,7.63802587492007,
0.));
#237755=CARTESIAN_POINT('Ctrl Pts',(-21.8929196523511,7.63802587492007,
12.));
#237756=CARTESIAN_POINT('Ctrl Pts',(-21.8770334769492,7.63638853033367,
0.));
#237757=CARTESIAN_POINT('Ctrl Pts',(-21.8770334769492,7.63638853033367,
12.));
#237758=CARTESIAN_POINT('Ctrl Pts',(-21.8612943779086,7.63471878821203,
0.));
#237759=CARTESIAN_POINT('Ctrl Pts',(-21.8612943779086,7.63471878821203,
12.));
#237760=CARTESIAN_POINT('Ctrl Pts',(-21.8457037941084,7.63301748948936,
0.));
#237761=CARTESIAN_POINT('Ctrl Pts',(-21.8457037941084,7.63301748948936,
12.));
#237762=CARTESIAN_POINT('Ctrl Pts',(-21.8302631910197,7.6312854932304,0.));
#237763=CARTESIAN_POINT('Ctrl Pts',(-21.8302631910197,7.6312854932304,12.));
#237764=CARTESIAN_POINT('Ctrl Pts',(-21.8149740615093,7.62952367718151,
0.));
#237765=CARTESIAN_POINT('Ctrl Pts',(-21.8149740615093,7.62952367718151,
12.));
#237766=CARTESIAN_POINT('Ctrl Pts',(-21.7998379268583,7.62773293842409,
0.));
#237767=CARTESIAN_POINT('Ctrl Pts',(-21.7998379268583,7.62773293842409,
12.));
#237768=CARTESIAN_POINT('Ctrl Pts',(-21.7848563378022,7.62591419404521,
0.));
#237769=CARTESIAN_POINT('Ctrl Pts',(-21.7848563378022,7.62591419404521,
12.));
#237770=CARTESIAN_POINT('Ctrl Pts',(-21.7700308755583,7.62406838181164,
0.));
#237771=CARTESIAN_POINT('Ctrl Pts',(-21.7700308755583,7.62406838181164,
12.));
#237772=CARTESIAN_POINT('Ctrl Pts',(-21.7553631528329,7.62219646084226,
0.));
#237773=CARTESIAN_POINT('Ctrl Pts',(-21.7553631528329,7.62219646084226,
12.));
#237774=CARTESIAN_POINT('Ctrl Pts',(-21.7408548148657,7.62029941230855,
0.));
#237775=CARTESIAN_POINT('Ctrl Pts',(-21.7408548148657,7.62029941230855,
12.));
#237776=CARTESIAN_POINT('Ctrl Pts',(-21.7265075407977,7.61837824030541,
0.));
#237777=CARTESIAN_POINT('Ctrl Pts',(-21.7265075407977,7.61837824030541,
12.));
#237778=CARTESIAN_POINT('Ctrl Pts',(-21.7123230449835,7.61643397270425,
0.));
#237779=CARTESIAN_POINT('Ctrl Pts',(-21.7123230449835,7.61643397270425,
12.));
#237780=CARTESIAN_POINT('Ctrl Pts',(-21.6983030783321,7.61446766202787,
0.));
#237781=CARTESIAN_POINT('Ctrl Pts',(-21.6983030783321,7.61446766202787,
12.));
#237782=CARTESIAN_POINT('Ctrl Pts',(-21.6844494295813,7.61248038630265,
0.));
#237783=CARTESIAN_POINT('Ctrl Pts',(-21.6844494295813,7.61248038630265,
12.));
#237784=CARTESIAN_POINT('Ctrl Pts',(-21.6707639267573,7.6104732500095,0.));
#237785=CARTESIAN_POINT('Ctrl Pts',(-21.6707639267573,7.6104732500095,12.));
#237786=CARTESIAN_POINT('Ctrl Pts',(-21.6572484388079,7.60844738512872,
0.));
#237787=CARTESIAN_POINT('Ctrl Pts',(-21.6572484388079,7.60844738512872,
12.));
#237788=CARTESIAN_POINT('Ctrl Pts',(-21.6439048771743,7.60640395216358,
0.));
#237789=CARTESIAN_POINT('Ctrl Pts',(-21.6439048771743,7.60640395216358,
12.));
#237790=CARTESIAN_POINT('Ctrl Pts',(-21.6307351973823,7.604344141183,0.));
#237791=CARTESIAN_POINT('Ctrl Pts',(-21.6307351973823,7.604344141183,12.));
#237792=CARTESIAN_POINT('Ctrl Pts',(-21.6177414005991,7.60226917285432,
0.));
#237793=CARTESIAN_POINT('Ctrl Pts',(-21.6177414005991,7.60226917285432,
12.));
#237794=CARTESIAN_POINT('Ctrl Pts',(-21.6049255358843,7.60018029988238,
0.));
#237795=CARTESIAN_POINT('Ctrl Pts',(-21.6049255358843,7.60018029988238,
12.));
#237796=CARTESIAN_POINT('Ctrl Pts',(-21.5922897024466,7.59807880846192,
0.));
#237797=CARTESIAN_POINT('Ctrl Pts',(-21.5922897024466,7.59807880846192,
12.));
#237798=CARTESIAN_POINT('Ctrl Pts',(-21.5798360518978,7.59596601973588,
0.));
#237799=CARTESIAN_POINT('Ctrl Pts',(-21.5798360518978,7.59596601973588,
12.));
#237800=CARTESIAN_POINT('Ctrl Pts',(-21.5675667904728,7.5938432912493,0.));
#237801=CARTESIAN_POINT('Ctrl Pts',(-21.5675667904728,7.5938432912493,12.));
#237802=CARTESIAN_POINT('Ctrl Pts',(-21.5554841813465,7.59171201844793,
0.));
#237803=CARTESIAN_POINT('Ctrl Pts',(-21.5554841813465,7.59171201844793,
12.));
#237804=CARTESIAN_POINT('Ctrl Pts',(-21.5435905470113,7.58957363620026,
0.));
#237805=CARTESIAN_POINT('Ctrl Pts',(-21.5435905470113,7.58957363620026,
12.));
#237806=CARTESIAN_POINT('Ctrl Pts',(-21.5318882716735,7.58742962034834,
0.));
#237807=CARTESIAN_POINT('Ctrl Pts',(-21.5318882716735,7.58742962034834,
12.));
#237808=CARTESIAN_POINT('Ctrl Pts',(-21.5203798035294,7.58528148919113,
0.));
#237809=CARTESIAN_POINT('Ctrl Pts',(-21.5203798035294,7.58528148919113,
12.));
#237810=CARTESIAN_POINT('Ctrl Pts',(-21.5090676573866,7.58313080519158,
0.));
#237811=CARTESIAN_POINT('Ctrl Pts',(-21.5090676573866,7.58313080519158,
12.));
#237812=CARTESIAN_POINT('Ctrl Pts',(-21.497954419274,7.5809791779073,0.));
#237813=CARTESIAN_POINT('Ctrl Pts',(-21.497954419274,7.5809791779073,12.));
#237814=CARTESIAN_POINT('Ctrl Pts',(-21.4870427508193,7.57882826679131,
0.));
#237815=CARTESIAN_POINT('Ctrl Pts',(-21.4870427508193,7.57882826679131,
12.));
#237816=CARTESIAN_POINT('Ctrl Pts',(-21.4763353936766,7.57667978403002,
0.));
#237817=CARTESIAN_POINT('Ctrl Pts',(-21.4763353936766,7.57667978403002,
12.));
#237818=CARTESIAN_POINT('Ctrl Pts',(-21.4658351740135,7.57453549743435,
0.));
#237819=CARTESIAN_POINT('Ctrl Pts',(-21.4658351740135,7.57453549743435,
12.));
#237820=CARTESIAN_POINT('Ctrl Pts',(-21.4555450053147,7.57239723223521,
0.));
#237821=CARTESIAN_POINT('Ctrl Pts',(-21.4555450053147,7.57239723223521,
12.));
#237822=CARTESIAN_POINT('Ctrl Pts',(-21.445467890751,7.57026687261169,0.));
#237823=CARTESIAN_POINT('Ctrl Pts',(-21.445467890751,7.57026687261169,12.));
#237824=CARTESIAN_POINT('Ctrl Pts',(-21.435606926151,7.56814636360842,0.));
#237825=CARTESIAN_POINT('Ctrl Pts',(-21.435606926151,7.56814636360842,12.));
#237826=CARTESIAN_POINT('Ctrl Pts',(-21.4259653015732,7.56603771218706,
0.));
#237827=CARTESIAN_POINT('Ctrl Pts',(-21.4259653015732,7.56603771218706,
12.));
#237828=CARTESIAN_POINT('Ctrl Pts',(-21.4165463106252,7.56394299313682,
0.));
#237829=CARTESIAN_POINT('Ctrl Pts',(-21.4165463106252,7.56394299313682,
12.));
#237830=CARTESIAN_POINT('Ctrl Pts',(-21.4073533630364,7.56186435703622,
0.));
#237831=CARTESIAN_POINT('Ctrl Pts',(-21.4073533630364,7.56186435703622,
12.));
#237832=CARTESIAN_POINT('Ctrl Pts',(-21.3983899952988,7.55980403700615,
0.));
#237833=CARTESIAN_POINT('Ctrl Pts',(-21.3983899952988,7.55980403700615,
12.));
#237834=CARTESIAN_POINT('Ctrl Pts',(-21.3896598842119,7.55776435731422,
0.));
#237835=CARTESIAN_POINT('Ctrl Pts',(-21.3896598842119,7.55776435731422,
12.));
#237836=CARTESIAN_POINT('Ctrl Pts',(-21.3811668478933,7.55574773403507,
0.));
#237837=CARTESIAN_POINT('Ctrl Pts',(-21.3811668478933,7.55574773403507,
12.));
#237838=CARTESIAN_POINT('Ctrl Pts',(-21.3729148390244,7.55375667080032,
0.));
#237839=CARTESIAN_POINT('Ctrl Pts',(-21.3729148390244,7.55375667080032,
12.));
#237840=CARTESIAN_POINT('Ctrl Pts',(-21.3649079431864,7.55179375777441,
0.));
#237841=CARTESIAN_POINT('Ctrl Pts',(-21.3649079431864,7.55179375777441,
12.));
#237842=CARTESIAN_POINT('Ctrl Pts',(-21.3571503685853,7.54986166521306,
0.));
#237843=CARTESIAN_POINT('Ctrl Pts',(-21.3571503685853,7.54986166521306,
12.));
#237844=CARTESIAN_POINT('Ctrl Pts',(-21.349646476153,7.54796316246327,0.));
#237845=CARTESIAN_POINT('Ctrl Pts',(-21.349646476153,7.54796316246327,12.));
#237846=CARTESIAN_POINT('Ctrl Pts',(-21.3424008295038,7.54610114948351,
0.));
#237847=CARTESIAN_POINT('Ctrl Pts',(-21.3424008295038,7.54610114948351,
12.));
#237848=CARTESIAN_POINT('Ctrl Pts',(-21.3354182340149,7.54427868151268,
0.));
#237849=CARTESIAN_POINT('Ctrl Pts',(-21.3354182340149,7.54427868151268,
12.));
#237850=CARTESIAN_POINT('Ctrl Pts',(-21.328703791771,7.54249900377031,0.));
#237851=CARTESIAN_POINT('Ctrl Pts',(-21.328703791771,7.54249900377031,12.));
#237852=CARTESIAN_POINT('Ctrl Pts',(-21.3222628524165,7.5407655203828,0.));
#237853=CARTESIAN_POINT('Ctrl Pts',(-21.3222628524165,7.5407655203828,12.));
#237854=CARTESIAN_POINT('Ctrl Pts',(-21.3161009456256,7.53908175169899,
0.));
#237855=CARTESIAN_POINT('Ctrl Pts',(-21.3161009456256,7.53908175169899,
12.));
#237856=CARTESIAN_POINT('Ctrl Pts',(-21.3102237167729,7.53745129364619,
0.));
#237857=CARTESIAN_POINT('Ctrl Pts',(-21.3102237167729,7.53745129364619,
12.));
#237858=CARTESIAN_POINT('Ctrl Pts',(-21.3046368712156,7.53587778251743,
0.));
#237859=CARTESIAN_POINT('Ctrl Pts',(-21.3046368712156,7.53587778251743,
12.));
#237860=CARTESIAN_POINT('Ctrl Pts',(-21.2993464250717,7.53436505309949,
0.));
#237861=CARTESIAN_POINT('Ctrl Pts',(-21.2993464250717,7.53436505309949,
12.));
#237862=CARTESIAN_POINT('Ctrl Pts',(-21.2943588989331,7.53291726078526,
0.));
#237863=CARTESIAN_POINT('Ctrl Pts',(-21.2943588989331,7.53291726078526,
12.));
#237864=CARTESIAN_POINT('Ctrl Pts',(-21.2896816163843,7.53153906987847,
0.));
#237865=CARTESIAN_POINT('Ctrl Pts',(-21.2896816163843,7.53153906987847,
12.));
#237866=CARTESIAN_POINT('Ctrl Pts',(-21.2853226580658,7.53023562438221,
0.));
#237867=CARTESIAN_POINT('Ctrl Pts',(-21.2853226580658,7.53023562438221,
12.));
#237868=CARTESIAN_POINT('Ctrl Pts',(-21.2812902781143,7.52901217930407,
0.));
#237869=CARTESIAN_POINT('Ctrl Pts',(-21.2812902781143,7.52901217930407,
12.));
#237870=CARTESIAN_POINT('Ctrl Pts',(-21.2775925269651,7.52787386225343,
0.));
#237871=CARTESIAN_POINT('Ctrl Pts',(-21.2775925269651,7.52787386225343,
12.));
#237872=CARTESIAN_POINT('Ctrl Pts',(-21.2742366113578,7.5268252691856,0.));
#237873=CARTESIAN_POINT('Ctrl Pts',(-21.2742366113578,7.5268252691856,12.));
#237874=CARTESIAN_POINT('Ctrl Pts',(-21.2712301573465,7.52587126095544,
0.));
#237875=CARTESIAN_POINT('Ctrl Pts',(-21.2712301573465,7.52587126095544,
12.));
#237876=CARTESIAN_POINT('Ctrl Pts',(-21.2685823838672,7.52501770333522,
0.));
#237877=CARTESIAN_POINT('Ctrl Pts',(-21.2685823838672,7.52501770333522,
12.));
#237878=CARTESIAN_POINT('Ctrl Pts',(-21.266305915706,7.52427261074264,0.));
#237879=CARTESIAN_POINT('Ctrl Pts',(-21.266305915706,7.52427261074264,12.));
#237880=CARTESIAN_POINT('Ctrl Pts',(-21.2644161259965,7.52364573027521,
0.));
#237881=CARTESIAN_POINT('Ctrl Pts',(-21.2644161259965,7.52364573027521,
12.));
#237882=CARTESIAN_POINT('Ctrl Pts',(-21.262927782038,7.52314642316202,0.));
#237883=CARTESIAN_POINT('Ctrl Pts',(-21.262927782038,7.52314642316202,12.));
#237884=CARTESIAN_POINT('Ctrl Pts',(-21.261852128355,7.52278182242727,0.));
#237885=CARTESIAN_POINT('Ctrl Pts',(-21.261852128355,7.52278182242727,12.));
#237886=CARTESIAN_POINT('Ctrl Pts',(-21.2613260540651,7.52260064231736,
0.));
#237887=CARTESIAN_POINT('Ctrl Pts',(-21.2613260540651,7.52260064231736,
12.));
#237888=CARTESIAN_POINT('Ctrl Pts',(-21.261120447486,7.52252744144958,0.));
#237889=CARTESIAN_POINT('Ctrl Pts',(-21.261120447486,7.52252744144958,12.));
#237890=CARTESIAN_POINT('Ctrl Pts',(-21.2610673466883,7.52250649703992,
0.));
#237891=CARTESIAN_POINT('Ctrl Pts',(-21.2610673466883,7.52250649703992,
12.));
#237892=CARTESIAN_POINT('Ctrl Pts',(-21.2610617890679,7.52250298901265,
0.));
#237893=CARTESIAN_POINT('Ctrl Pts',(-21.2610617890679,7.52250298901265,
12.));
#237894=CARTESIAN_POINT('',(-24.9347862158358,7.36589684767345,0.));
#237895=CARTESIAN_POINT('Ctrl Pts',(-24.9347862158358,7.36589684767345,
0.));
#237896=CARTESIAN_POINT('Ctrl Pts',(-24.9292275670674,7.36721909028843,
0.));
#237897=CARTESIAN_POINT('Ctrl Pts',(-24.9181155530543,7.3698559312009,0.));
#237898=CARTESIAN_POINT('Ctrl Pts',(-24.901463382605,7.37378825961676,0.));
#237899=CARTESIAN_POINT('Ctrl Pts',(-24.8792921911115,7.3789854964027,0.));
#237900=CARTESIAN_POINT('Ctrl Pts',(-24.8516310625176,7.38540558903621,
0.));
#237901=CARTESIAN_POINT('Ctrl Pts',(-24.8240228520893,7.39174922585808,
0.));
#237902=CARTESIAN_POINT('Ctrl Pts',(-24.7964676646431,7.39801641583013,
0.));
#237903=CARTESIAN_POINT('Ctrl Pts',(-24.7689656668983,7.40420718661603,
0.));
#237904=CARTESIAN_POINT('Ctrl Pts',(-24.7415170994784,7.41032159082382,
0.));
#237905=CARTESIAN_POINT('Ctrl Pts',(-24.7141222950051,7.41635971481674,
0.));
#237906=CARTESIAN_POINT('Ctrl Pts',(-24.6867816727192,7.42232167766265,
0.));
#237907=CARTESIAN_POINT('Ctrl Pts',(-24.6594957128756,7.42820762159126,
0.));
#237908=CARTESIAN_POINT('Ctrl Pts',(-24.6322649369517,7.43401770489524,
0.));
#237909=CARTESIAN_POINT('Ctrl Pts',(-24.6050898852368,7.43975209375504,
0.));
#237910=CARTESIAN_POINT('Ctrl Pts',(-24.577971096086,7.44541095473134,0.));
#237911=CARTESIAN_POINT('Ctrl Pts',(-24.5509090831559,7.4509944465116,0.));
#237912=CARTESIAN_POINT('Ctrl Pts',(-24.5239043173072,7.45650271335862,
0.));
#237913=CARTESIAN_POINT('Ctrl Pts',(-24.4969572391483,7.46193588961463,
0.));
#237914=CARTESIAN_POINT('Ctrl Pts',(-24.4700682684524,7.46729410308786,
0.));
#237915=CARTESIAN_POINT('Ctrl Pts',(-24.443237814649,7.47257747883246,0.));
#237916=CARTESIAN_POINT('Ctrl Pts',(-24.4164662871163,7.47778614286565,
0.));
#237917=CARTESIAN_POINT('Ctrl Pts',(-24.3897541049254,7.48292022569301,
0.));
#237918=CARTESIAN_POINT('Ctrl Pts',(-24.3631017084524,7.48797986651908,
0.));
#237919=CARTESIAN_POINT('Ctrl Pts',(-24.3365095573685,7.4929652125242,0.));
#237920=CARTESIAN_POINT('Ctrl Pts',(-24.3099781253355,7.49787641695439,
0.));
#237921=CARTESIAN_POINT('Ctrl Pts',(-24.2835078958973,7.50271363765152,
0.));
#237922=CARTESIAN_POINT('Ctrl Pts',(-24.2570993577034,7.50747703535133,
0.));
#237923=CARTESIAN_POINT('Ctrl Pts',(-24.2307530003887,7.51216677222181,
0.));
#237924=CARTESIAN_POINT('Ctrl Pts',(-24.2044693092349,7.51678300997949,
0.));
#237925=CARTESIAN_POINT('Ctrl Pts',(-24.1782487641594,7.52132590953802,
0.));
#237926=CARTESIAN_POINT('Ctrl Pts',(-24.1520918425364,7.52579563201424,
0.));
#237927=CARTESIAN_POINT('Ctrl Pts',(-24.1259990209207,7.53019233935501,
0.));
#237928=CARTESIAN_POINT('Ctrl Pts',(-24.0999707772642,7.53451619514649,
0.));
#237929=CARTESIAN_POINT('Ctrl Pts',(-24.0740075927985,7.53876736531014,
0.));
#237930=CARTESIAN_POINT('Ctrl Pts',(-24.0481099543353,7.54294601896144,
0.));
#237931=CARTESIAN_POINT('Ctrl Pts',(-24.022278355453,7.5470523288591,0.));
#237932=CARTESIAN_POINT('Ctrl Pts',(-23.9965132953185,7.55108647097441,
0.));
#237933=CARTESIAN_POINT('Ctrl Pts',(-23.9708152779884,7.55504862424812,
0.));
#237934=CARTESIAN_POINT('Ctrl Pts',(-23.9451848115,7.55893897027682,0.));
#237935=CARTESIAN_POINT('Ctrl Pts',(-23.9196224070759,7.56275769304773,
0.));
#237936=CARTESIAN_POINT('Ctrl Pts',(-23.8941285782003,7.56650497863792,
0.));
#237937=CARTESIAN_POINT('Ctrl Pts',(-23.8687038399598,7.57018101500711,
0.));
#237938=CARTESIAN_POINT('Ctrl Pts',(-23.8433487096134,7.57378599219816,
0.));
#237939=CARTESIAN_POINT('Ctrl Pts',(-23.8180637069977,7.57732010249066,
0.));
#237940=CARTESIAN_POINT('Ctrl Pts',(-23.7928493549908,7.58078354058212,
0.));
#237941=CARTESIAN_POINT('Ctrl Pts',(-23.7677061799376,7.58417650376272,
0.));
#237942=CARTESIAN_POINT('Ctrl Pts',(-23.7426347121006,7.58749919210832,
0.));
#237943=CARTESIAN_POINT('Ctrl Pts',(-23.7176354860457,7.59075180865327,
0.));
#237944=CARTESIAN_POINT('Ctrl Pts',(-23.6927090405067,7.59393455934042,
0.));
#237945=CARTESIAN_POINT('Ctrl Pts',(-23.6678559182876,7.59704765299572,
0.));
#237946=CARTESIAN_POINT('Ctrl Pts',(-23.6430766661419,7.60009130130129,
0.));
#237947=CARTESIAN_POINT('Ctrl Pts',(-23.6183718346576,7.60306571877806,
0.));
#237948=CARTESIAN_POINT('Ctrl Pts',(-23.5937419781244,7.60597112277094,
0.));
#237949=CARTESIAN_POINT('Ctrl Pts',(-23.5691876544243,7.60880773344599,
0.));
#237950=CARTESIAN_POINT('Ctrl Pts',(-23.5447094252029,7.61157577385372,
0.));
#237951=CARTESIAN_POINT('Ctrl Pts',(-23.5203078560128,7.61427546999299,
0.));
#237952=CARTESIAN_POINT('Ctrl Pts',(-23.4959835164608,7.61690705088319,
0.));
#237953=CARTESIAN_POINT('Ctrl Pts',(-23.4717369803438,7.61947074863977,
0.));
#237954=CARTESIAN_POINT('Ctrl Pts',(-23.4475688257854,7.62196679855957,
0.));
#237955=CARTESIAN_POINT('Ctrl Pts',(-23.4234796353544,7.62439543920054,
0.));
#237956=CARTESIAN_POINT('Ctrl Pts',(-23.3994699961122,7.62675691240335,
0.));
#237957=CARTESIAN_POINT('Ctrl Pts',(-23.3755404996638,7.62905146332598,
0.));
#237958=CARTESIAN_POINT('Ctrl Pts',(-23.3516917421973,7.63127934048139,
0.));
#237959=CARTESIAN_POINT('Ctrl Pts',(-23.3279243245241,7.63344079578162,
0.));
#237960=CARTESIAN_POINT('Ctrl Pts',(-23.3042388521021,7.63553608458784,
0.));
#237961=CARTESIAN_POINT('Ctrl Pts',(-23.2806359350853,7.63756546576375,
0.));
#237962=CARTESIAN_POINT('Ctrl Pts',(-23.2571161884487,7.63952920172837,
0.));
#237963=CARTESIAN_POINT('Ctrl Pts',(-23.2336802320912,7.64142755851508,
0.));
#237964=CARTESIAN_POINT('Ctrl Pts',(-23.2103286909399,7.64326080583684,
0.));
#237965=CARTESIAN_POINT('Ctrl Pts',(-23.1870621950452,7.64502921715483,
0.));
#237966=CARTESIAN_POINT('Ctrl Pts',(-23.1638813796691,7.64673306975797,
0.));
#237967=CARTESIAN_POINT('Ctrl Pts',(-23.1407868853815,7.64837264482929,
0.));
#237968=CARTESIAN_POINT('Ctrl Pts',(-23.1177793581674,7.64994822749845,
0.));
#237969=CARTESIAN_POINT('Ctrl Pts',(-23.0948594495246,7.65146010690464,
0.));
#237970=CARTESIAN_POINT('Ctrl Pts',(-23.072027816555,7.65290857626356,0.));
#237971=CARTESIAN_POINT('Ctrl Pts',(-23.049285122053,7.65429393293955,0.));
#237972=CARTESIAN_POINT('Ctrl Pts',(-23.0266320345792,7.65561647852555,
0.));
#237973=CARTESIAN_POINT('Ctrl Pts',(-23.004069228582,7.6568765189133,0.));
#237974=CARTESIAN_POINT('Ctrl Pts',(-22.9815973845301,7.65807436436453,
0.));
#237975=CARTESIAN_POINT('Ctrl Pts',(-22.9592171890332,7.65921032958912,
0.));
#237976=CARTESIAN_POINT('Ctrl Pts',(-22.9369293349592,7.66028473382777,
0.));
#237977=CARTESIAN_POINT('Ctrl Pts',(-22.9147345215418,7.661297900941,0.));
#237978=CARTESIAN_POINT('Ctrl Pts',(-22.8926334544879,7.66225015950147,
0.));
#237979=CARTESIAN_POINT('Ctrl Pts',(-22.870626846128,7.66314184287334,0.));
#237980=CARTESIAN_POINT('Ctrl Pts',(-22.8487154155569,7.66397328929805,
0.));
#237981=CARTESIAN_POINT('Ctrl Pts',(-22.8268998887679,7.66474484198553,
0.));
#237982=CARTESIAN_POINT('Ctrl Pts',(-22.8051809987834,7.66545684920987,
0.));
#237983=CARTESIAN_POINT('Ctrl Pts',(-22.7835594857697,7.66610966441259,
0.));
#237984=CARTESIAN_POINT('Ctrl Pts',(-22.7620360971839,7.66670364630273,
0.));
#237985=CARTESIAN_POINT('Ctrl Pts',(-22.7406115879508,7.66723915895412,
0.));
#237986=CARTESIAN_POINT('Ctrl Pts',(-22.7192867206242,7.6677165719101,0.));
#237987=CARTESIAN_POINT('Ctrl Pts',(-22.6980622655446,7.66813626029276,
0.));
#237988=CARTESIAN_POINT('Ctrl Pts',(-22.6769390009889,7.66849860491763,
0.));
#237989=CARTESIAN_POINT('Ctrl Pts',(-22.6559177133133,7.66880399241354,
0.));
#237990=CARTESIAN_POINT('Ctrl Pts',(-22.6349991971547,7.66905281533745,
0.));
#237991=CARTESIAN_POINT('Ctrl Pts',(-22.6141842556248,7.66924547229435,
0.));
#237992=CARTESIAN_POINT('Ctrl Pts',(-22.5934737004955,7.66938236806241,
0.));
#237993=CARTESIAN_POINT('Ctrl Pts',(-22.5728683523829,7.66946391372299,
0.));
#237994=CARTESIAN_POINT('Ctrl Pts',(-22.5523690409109,7.66949052679671,
0.));
#237995=CARTESIAN_POINT('Ctrl Pts',(-22.5319766049191,7.66946263138116,
0.));
#237996=CARTESIAN_POINT('Ctrl Pts',(-22.5116918927023,7.66938065829082,
0.));
#237997=CARTESIAN_POINT('Ctrl Pts',(-22.4915157622308,7.66924504520302,
0.));
#237998=CARTESIAN_POINT('Ctrl Pts',(-22.47144908137,7.66905623680835,0.));
#237999=CARTESIAN_POINT('Ctrl Pts',(-22.4514927280863,7.6688146849666,0.));
#238000=CARTESIAN_POINT('Ctrl Pts',(-22.4316475906616,7.66852084886745,
0.));
#238001=CARTESIAN_POINT('Ctrl Pts',(-22.411914567977,7.66817519519682,0.));
#238002=CARTESIAN_POINT('Ctrl Pts',(-22.3922945697782,7.66777819830819,
0.));
#238003=CARTESIAN_POINT('Ctrl Pts',(-22.3727885169361,7.66733034039887,
0.));
#238004=CARTESIAN_POINT('Ctrl Pts',(-22.3533973417013,7.66683211169134,
0.));
#238005=CARTESIAN_POINT('Ctrl Pts',(-22.3341219879454,7.66628401061905,
0.));
#238006=CARTESIAN_POINT('Ctrl Pts',(-22.3149634114823,7.66568654402441,
0.));
#238007=CARTESIAN_POINT('Ctrl Pts',(-22.2959225803925,7.66504022736262,
0.));
#238008=CARTESIAN_POINT('Ctrl Pts',(-22.2770004753332,7.66434558490972,
0.));
#238009=CARTESIAN_POINT('Ctrl Pts',(-22.2581980898487,7.66360314997662,
0.));
#238010=CARTESIAN_POINT('Ctrl Pts',(-22.239516430656,7.66281346512545,0.));
#238011=CARTESIAN_POINT('Ctrl Pts',(-22.2209565180098,7.66197708240435,
0.));
#238012=CARTESIAN_POINT('Ctrl Pts',(-22.2025193860972,7.66109456359292,
0.));
#238013=CARTESIAN_POINT('Ctrl Pts',(-22.1842060834092,7.66016648045008,
0.));
#238014=CARTESIAN_POINT('Ctrl Pts',(-22.1660176731174,7.65919341496925,
0.));
#238015=CARTESIAN_POINT('Ctrl Pts',(-22.1479552334206,7.65817595963351,
0.));
#238016=CARTESIAN_POINT('Ctrl Pts',(-22.1300198579671,7.65711471769407,
0.));
#238017=CARTESIAN_POINT('Ctrl Pts',(-22.1122126563327,7.65601030346819,
0.));
#238018=CARTESIAN_POINT('Ctrl Pts',(-22.094534754469,7.6548633426365,0.));
#238019=CARTESIAN_POINT('Ctrl Pts',(-22.0769872951596,7.65367447254945,
0.));
#238020=CARTESIAN_POINT('Ctrl Pts',(-22.0595714384432,7.65244434253104,
0.));
#238021=CARTESIAN_POINT('Ctrl Pts',(-22.0422883621176,7.65117361421346,
0.));
#238022=CARTESIAN_POINT('Ctrl Pts',(-22.0251392623209,7.64986296190156,
0.));
#238023=CARTESIAN_POINT('Ctrl Pts',(-22.0081253540773,7.64851307293346,
0.));
#238024=CARTESIAN_POINT('Ctrl Pts',(-21.9912478718542,7.64712464805258,
0.));
#238025=CARTESIAN_POINT('Ctrl Pts',(-21.97450807008,7.64569840177359,0.));
#238026=CARTESIAN_POINT('Ctrl Pts',(-21.9579072237653,7.64423506279153,
0.));
#238027=CARTESIAN_POINT('Ctrl Pts',(-21.9414466292074,7.64273537442706,
0.));
#238028=CARTESIAN_POINT('Ctrl Pts',(-21.9251276046546,7.6412000950654,0.));
#238029=CARTESIAN_POINT('Ctrl Pts',(-21.9089514909873,7.63962999860916,
0.));
#238030=CARTESIAN_POINT('Ctrl Pts',(-21.8929196523511,7.63802587492007,
0.));
#238031=CARTESIAN_POINT('Ctrl Pts',(-21.8770334769492,7.63638853033367,
0.));
#238032=CARTESIAN_POINT('Ctrl Pts',(-21.8612943779086,7.63471878821203,
0.));
#238033=CARTESIAN_POINT('Ctrl Pts',(-21.8457037941084,7.63301748948936,
0.));
#238034=CARTESIAN_POINT('Ctrl Pts',(-21.8302631910197,7.6312854932304,0.));
#238035=CARTESIAN_POINT('Ctrl Pts',(-21.8149740615093,7.62952367718151,
0.));
#238036=CARTESIAN_POINT('Ctrl Pts',(-21.7998379268583,7.62773293842409,
0.));
#238037=CARTESIAN_POINT('Ctrl Pts',(-21.7848563378022,7.62591419404521,
0.));
#238038=CARTESIAN_POINT('Ctrl Pts',(-21.7700308755583,7.62406838181164,
0.));
#238039=CARTESIAN_POINT('Ctrl Pts',(-21.7553631528329,7.62219646084226,
0.));
#238040=CARTESIAN_POINT('Ctrl Pts',(-21.7408548148657,7.62029941230855,
0.));
#238041=CARTESIAN_POINT('Ctrl Pts',(-21.7265075407977,7.61837824030541,
0.));
#238042=CARTESIAN_POINT('Ctrl Pts',(-21.7123230449835,7.61643397270425,
0.));
#238043=CARTESIAN_POINT('Ctrl Pts',(-21.6983030783321,7.61446766202787,
0.));
#238044=CARTESIAN_POINT('Ctrl Pts',(-21.6844494295813,7.61248038630265,
0.));
#238045=CARTESIAN_POINT('Ctrl Pts',(-21.6707639267573,7.6104732500095,0.));
#238046=CARTESIAN_POINT('Ctrl Pts',(-21.6572484388079,7.60844738512872,
0.));
#238047=CARTESIAN_POINT('Ctrl Pts',(-21.6439048771743,7.60640395216358,
0.));
#238048=CARTESIAN_POINT('Ctrl Pts',(-21.6307351973823,7.604344141183,0.));
#238049=CARTESIAN_POINT('Ctrl Pts',(-21.6177414005991,7.60226917285432,
0.));
#238050=CARTESIAN_POINT('Ctrl Pts',(-21.6049255358843,7.60018029988238,
0.));
#238051=CARTESIAN_POINT('Ctrl Pts',(-21.5922897024466,7.59807880846192,
0.));
#238052=CARTESIAN_POINT('Ctrl Pts',(-21.5798360518978,7.59596601973588,
0.));
#238053=CARTESIAN_POINT('Ctrl Pts',(-21.5675667904728,7.5938432912493,0.));
#238054=CARTESIAN_POINT('Ctrl Pts',(-21.5554841813465,7.59171201844793,
0.));
#238055=CARTESIAN_POINT('Ctrl Pts',(-21.5435905470113,7.58957363620026,
0.));
#238056=CARTESIAN_POINT('Ctrl Pts',(-21.5318882716735,7.58742962034834,
0.));
#238057=CARTESIAN_POINT('Ctrl Pts',(-21.5203798035294,7.58528148919113,
0.));
#238058=CARTESIAN_POINT('Ctrl Pts',(-21.5090676573866,7.58313080519158,
0.));
#238059=CARTESIAN_POINT('Ctrl Pts',(-21.497954419274,7.5809791779073,0.));
#238060=CARTESIAN_POINT('Ctrl Pts',(-21.4870427508193,7.57882826679131,
0.));
#238061=CARTESIAN_POINT('Ctrl Pts',(-21.4763353936766,7.57667978403002,
0.));
#238062=CARTESIAN_POINT('Ctrl Pts',(-21.4658351740135,7.57453549743435,
0.));
#238063=CARTESIAN_POINT('Ctrl Pts',(-21.4555450053147,7.57239723223521,
0.));
#238064=CARTESIAN_POINT('Ctrl Pts',(-21.445467890751,7.57026687261169,0.));
#238065=CARTESIAN_POINT('Ctrl Pts',(-21.435606926151,7.56814636360842,0.));
#238066=CARTESIAN_POINT('Ctrl Pts',(-21.4259653015732,7.56603771218706,
0.));
#238067=CARTESIAN_POINT('Ctrl Pts',(-21.4165463106252,7.56394299313682,
0.));
#238068=CARTESIAN_POINT('Ctrl Pts',(-21.4073533630364,7.56186435703622,
0.));
#238069=CARTESIAN_POINT('Ctrl Pts',(-21.3983899952988,7.55980403700615,
0.));
#238070=CARTESIAN_POINT('Ctrl Pts',(-21.3896598842119,7.55776435731422,
0.));
#238071=CARTESIAN_POINT('Ctrl Pts',(-21.3811668478933,7.55574773403507,
0.));
#238072=CARTESIAN_POINT('Ctrl Pts',(-21.3729148390244,7.55375667080032,
0.));
#238073=CARTESIAN_POINT('Ctrl Pts',(-21.3649079431864,7.55179375777441,
0.));
#238074=CARTESIAN_POINT('Ctrl Pts',(-21.3571503685853,7.54986166521306,
0.));
#238075=CARTESIAN_POINT('Ctrl Pts',(-21.349646476153,7.54796316246327,0.));
#238076=CARTESIAN_POINT('Ctrl Pts',(-21.3424008295038,7.54610114948351,
0.));
#238077=CARTESIAN_POINT('Ctrl Pts',(-21.3354182340149,7.54427868151268,
0.));
#238078=CARTESIAN_POINT('Ctrl Pts',(-21.328703791771,7.54249900377031,0.));
#238079=CARTESIAN_POINT('Ctrl Pts',(-21.3222628524165,7.5407655203828,0.));
#238080=CARTESIAN_POINT('Ctrl Pts',(-21.3161009456256,7.53908175169899,
0.));
#238081=CARTESIAN_POINT('Ctrl Pts',(-21.3102237167729,7.53745129364619,
0.));
#238082=CARTESIAN_POINT('Ctrl Pts',(-21.3046368712156,7.53587778251743,
0.));
#238083=CARTESIAN_POINT('Ctrl Pts',(-21.2993464250717,7.53436505309949,
0.));
#238084=CARTESIAN_POINT('Ctrl Pts',(-21.2943588989331,7.53291726078526,
0.));
#238085=CARTESIAN_POINT('Ctrl Pts',(-21.2896816163843,7.53153906987847,
0.));
#238086=CARTESIAN_POINT('Ctrl Pts',(-21.2853226580658,7.53023562438221,
0.));
#238087=CARTESIAN_POINT('Ctrl Pts',(-21.2812902781143,7.52901217930407,
0.));
#238088=CARTESIAN_POINT('Ctrl Pts',(-21.2775925269651,7.52787386225343,
0.));
#238089=CARTESIAN_POINT('Ctrl Pts',(-21.2742366113578,7.5268252691856,0.));
#238090=CARTESIAN_POINT('Ctrl Pts',(-21.2712301573465,7.52587126095544,
0.));
#238091=CARTESIAN_POINT('Ctrl Pts',(-21.2685823838672,7.52501770333522,
0.));
#238092=CARTESIAN_POINT('Ctrl Pts',(-21.266305915706,7.52427261074264,0.));
#238093=CARTESIAN_POINT('Ctrl Pts',(-21.2644161259965,7.52364573027521,
0.));
#238094=CARTESIAN_POINT('Ctrl Pts',(-21.262927782038,7.52314642316202,0.));
#238095=CARTESIAN_POINT('Ctrl Pts',(-21.261852128355,7.52278182242727,0.));
#238096=CARTESIAN_POINT('Ctrl Pts',(-21.2613260540651,7.52260064231736,
0.));
#238097=CARTESIAN_POINT('Ctrl Pts',(-21.261120447486,7.52252744144958,0.));
#238098=CARTESIAN_POINT('Ctrl Pts',(-21.2610673466883,7.52250649703992,
0.));
#238099=CARTESIAN_POINT('Ctrl Pts',(-21.2610617890679,7.52250298901265,
0.));
#238100=CARTESIAN_POINT('',(-24.9347862158358,7.36589684767345,12.));
#238101=CARTESIAN_POINT('',(-24.9347862158358,7.36589684767345,0.));
#238102=CARTESIAN_POINT('Ctrl Pts',(-21.2610617890679,7.52250298901265,
12.));
#238103=CARTESIAN_POINT('Ctrl Pts',(-21.2610673466883,7.52250649703992,
12.));
#238104=CARTESIAN_POINT('Ctrl Pts',(-21.261120447486,7.52252744144958,12.));
#238105=CARTESIAN_POINT('Ctrl Pts',(-21.2613260540651,7.52260064231736,
12.));
#238106=CARTESIAN_POINT('Ctrl Pts',(-21.261852128355,7.52278182242727,12.));
#238107=CARTESIAN_POINT('Ctrl Pts',(-21.262927782038,7.52314642316202,12.));
#238108=CARTESIAN_POINT('Ctrl Pts',(-21.2644161259965,7.52364573027521,
12.));
#238109=CARTESIAN_POINT('Ctrl Pts',(-21.266305915706,7.52427261074264,12.));
#238110=CARTESIAN_POINT('Ctrl Pts',(-21.2685823838672,7.52501770333522,
12.));
#238111=CARTESIAN_POINT('Ctrl Pts',(-21.2712301573465,7.52587126095544,
12.));
#238112=CARTESIAN_POINT('Ctrl Pts',(-21.2742366113578,7.5268252691856,12.));
#238113=CARTESIAN_POINT('Ctrl Pts',(-21.2775925269651,7.52787386225343,
12.));
#238114=CARTESIAN_POINT('Ctrl Pts',(-21.2812902781143,7.52901217930407,
12.));
#238115=CARTESIAN_POINT('Ctrl Pts',(-21.2853226580658,7.53023562438221,
12.));
#238116=CARTESIAN_POINT('Ctrl Pts',(-21.2896816163843,7.53153906987847,
12.));
#238117=CARTESIAN_POINT('Ctrl Pts',(-21.2943588989331,7.53291726078526,
12.));
#238118=CARTESIAN_POINT('Ctrl Pts',(-21.2993464250717,7.53436505309949,
12.));
#238119=CARTESIAN_POINT('Ctrl Pts',(-21.3046368712156,7.53587778251743,
12.));
#238120=CARTESIAN_POINT('Ctrl Pts',(-21.3102237167729,7.53745129364619,
12.));
#238121=CARTESIAN_POINT('Ctrl Pts',(-21.3161009456256,7.53908175169899,
12.));
#238122=CARTESIAN_POINT('Ctrl Pts',(-21.3222628524165,7.5407655203828,12.));
#238123=CARTESIAN_POINT('Ctrl Pts',(-21.328703791771,7.54249900377031,12.));
#238124=CARTESIAN_POINT('Ctrl Pts',(-21.3354182340149,7.54427868151268,
12.));
#238125=CARTESIAN_POINT('Ctrl Pts',(-21.3424008295038,7.54610114948351,
12.));
#238126=CARTESIAN_POINT('Ctrl Pts',(-21.349646476153,7.54796316246327,12.));
#238127=CARTESIAN_POINT('Ctrl Pts',(-21.3571503685853,7.54986166521306,
12.));
#238128=CARTESIAN_POINT('Ctrl Pts',(-21.3649079431864,7.55179375777441,
12.));
#238129=CARTESIAN_POINT('Ctrl Pts',(-21.3729148390244,7.55375667080032,
12.));
#238130=CARTESIAN_POINT('Ctrl Pts',(-21.3811668478933,7.55574773403507,
12.));
#238131=CARTESIAN_POINT('Ctrl Pts',(-21.3896598842119,7.55776435731422,
12.));
#238132=CARTESIAN_POINT('Ctrl Pts',(-21.3983899952988,7.55980403700615,
12.));
#238133=CARTESIAN_POINT('Ctrl Pts',(-21.4073533630364,7.56186435703622,
12.));
#238134=CARTESIAN_POINT('Ctrl Pts',(-21.4165463106252,7.56394299313682,
12.));
#238135=CARTESIAN_POINT('Ctrl Pts',(-21.4259653015732,7.56603771218706,
12.));
#238136=CARTESIAN_POINT('Ctrl Pts',(-21.435606926151,7.56814636360842,12.));
#238137=CARTESIAN_POINT('Ctrl Pts',(-21.445467890751,7.57026687261169,12.));
#238138=CARTESIAN_POINT('Ctrl Pts',(-21.4555450053147,7.57239723223521,
12.));
#238139=CARTESIAN_POINT('Ctrl Pts',(-21.4658351740135,7.57453549743435,
12.));
#238140=CARTESIAN_POINT('Ctrl Pts',(-21.4763353936766,7.57667978403002,
12.));
#238141=CARTESIAN_POINT('Ctrl Pts',(-21.4870427508193,7.57882826679131,
12.));
#238142=CARTESIAN_POINT('Ctrl Pts',(-21.497954419274,7.5809791779073,12.));
#238143=CARTESIAN_POINT('Ctrl Pts',(-21.5090676573866,7.58313080519158,
12.));
#238144=CARTESIAN_POINT('Ctrl Pts',(-21.5203798035294,7.58528148919113,
12.));
#238145=CARTESIAN_POINT('Ctrl Pts',(-21.5318882716735,7.58742962034834,
12.));
#238146=CARTESIAN_POINT('Ctrl Pts',(-21.5435905470113,7.58957363620026,
12.));
#238147=CARTESIAN_POINT('Ctrl Pts',(-21.5554841813465,7.59171201844793,
12.));
#238148=CARTESIAN_POINT('Ctrl Pts',(-21.5675667904728,7.5938432912493,12.));
#238149=CARTESIAN_POINT('Ctrl Pts',(-21.5798360518978,7.59596601973588,
12.));
#238150=CARTESIAN_POINT('Ctrl Pts',(-21.5922897024466,7.59807880846192,
12.));
#238151=CARTESIAN_POINT('Ctrl Pts',(-21.6049255358843,7.60018029988238,
12.));
#238152=CARTESIAN_POINT('Ctrl Pts',(-21.6177414005991,7.60226917285432,
12.));
#238153=CARTESIAN_POINT('Ctrl Pts',(-21.6307351973823,7.604344141183,12.));
#238154=CARTESIAN_POINT('Ctrl Pts',(-21.6439048771743,7.60640395216358,
12.));
#238155=CARTESIAN_POINT('Ctrl Pts',(-21.6572484388079,7.60844738512872,
12.));
#238156=CARTESIAN_POINT('Ctrl Pts',(-21.6707639267573,7.6104732500095,12.));
#238157=CARTESIAN_POINT('Ctrl Pts',(-21.6844494295813,7.61248038630265,
12.));
#238158=CARTESIAN_POINT('Ctrl Pts',(-21.6983030783321,7.61446766202787,
12.));
#238159=CARTESIAN_POINT('Ctrl Pts',(-21.7123230449835,7.61643397270425,
12.));
#238160=CARTESIAN_POINT('Ctrl Pts',(-21.7265075407977,7.61837824030541,
12.));
#238161=CARTESIAN_POINT('Ctrl Pts',(-21.7408548148657,7.62029941230855,
12.));
#238162=CARTESIAN_POINT('Ctrl Pts',(-21.7553631528329,7.62219646084226,
12.));
#238163=CARTESIAN_POINT('Ctrl Pts',(-21.7700308755583,7.62406838181164,
12.));
#238164=CARTESIAN_POINT('Ctrl Pts',(-21.7848563378022,7.62591419404521,
12.));
#238165=CARTESIAN_POINT('Ctrl Pts',(-21.7998379268583,7.62773293842409,
12.));
#238166=CARTESIAN_POINT('Ctrl Pts',(-21.8149740615093,7.62952367718151,
12.));
#238167=CARTESIAN_POINT('Ctrl Pts',(-21.8302631910197,7.6312854932304,12.));
#238168=CARTESIAN_POINT('Ctrl Pts',(-21.8457037941084,7.63301748948936,
12.));
#238169=CARTESIAN_POINT('Ctrl Pts',(-21.8612943779086,7.63471878821203,
12.));
#238170=CARTESIAN_POINT('Ctrl Pts',(-21.8770334769492,7.63638853033367,
12.));
#238171=CARTESIAN_POINT('Ctrl Pts',(-21.8929196523511,7.63802587492007,
12.));
#238172=CARTESIAN_POINT('Ctrl Pts',(-21.9089514909873,7.63962999860916,
12.));
#238173=CARTESIAN_POINT('Ctrl Pts',(-21.9251276046546,7.6412000950654,12.));
#238174=CARTESIAN_POINT('Ctrl Pts',(-21.9414466292074,7.64273537442706,
12.));
#238175=CARTESIAN_POINT('Ctrl Pts',(-21.9579072237653,7.64423506279153,
12.));
#238176=CARTESIAN_POINT('Ctrl Pts',(-21.97450807008,7.64569840177359,12.));
#238177=CARTESIAN_POINT('Ctrl Pts',(-21.9912478718542,7.64712464805258,
12.));
#238178=CARTESIAN_POINT('Ctrl Pts',(-22.0081253540773,7.64851307293346,
12.));
#238179=CARTESIAN_POINT('Ctrl Pts',(-22.0251392623209,7.64986296190156,
12.));
#238180=CARTESIAN_POINT('Ctrl Pts',(-22.0422883621176,7.65117361421346,
12.));
#238181=CARTESIAN_POINT('Ctrl Pts',(-22.0595714384432,7.65244434253104,
12.));
#238182=CARTESIAN_POINT('Ctrl Pts',(-22.0769872951596,7.65367447254945,
12.));
#238183=CARTESIAN_POINT('Ctrl Pts',(-22.094534754469,7.6548633426365,12.));
#238184=CARTESIAN_POINT('Ctrl Pts',(-22.1122126563327,7.65601030346819,
12.));
#238185=CARTESIAN_POINT('Ctrl Pts',(-22.1300198579671,7.65711471769407,
12.));
#238186=CARTESIAN_POINT('Ctrl Pts',(-22.1479552334206,7.65817595963351,
12.));
#238187=CARTESIAN_POINT('Ctrl Pts',(-22.1660176731174,7.65919341496925,
12.));
#238188=CARTESIAN_POINT('Ctrl Pts',(-22.1842060834092,7.66016648045008,
12.));
#238189=CARTESIAN_POINT('Ctrl Pts',(-22.2025193860972,7.66109456359292,
12.));
#238190=CARTESIAN_POINT('Ctrl Pts',(-22.2209565180098,7.66197708240435,
12.));
#238191=CARTESIAN_POINT('Ctrl Pts',(-22.239516430656,7.66281346512545,12.));
#238192=CARTESIAN_POINT('Ctrl Pts',(-22.2581980898487,7.66360314997662,
12.));
#238193=CARTESIAN_POINT('Ctrl Pts',(-22.2770004753332,7.66434558490972,
12.));
#238194=CARTESIAN_POINT('Ctrl Pts',(-22.2959225803925,7.66504022736262,
12.));
#238195=CARTESIAN_POINT('Ctrl Pts',(-22.3149634114823,7.66568654402441,
12.));
#238196=CARTESIAN_POINT('Ctrl Pts',(-22.3341219879454,7.66628401061905,
12.));
#238197=CARTESIAN_POINT('Ctrl Pts',(-22.3533973417013,7.66683211169134,
12.));
#238198=CARTESIAN_POINT('Ctrl Pts',(-22.3727885169361,7.66733034039887,
12.));
#238199=CARTESIAN_POINT('Ctrl Pts',(-22.3922945697782,7.66777819830819,
12.));
#238200=CARTESIAN_POINT('Ctrl Pts',(-22.411914567977,7.66817519519682,12.));
#238201=CARTESIAN_POINT('Ctrl Pts',(-22.4316475906616,7.66852084886745,
12.));
#238202=CARTESIAN_POINT('Ctrl Pts',(-22.4514927280863,7.6688146849666,12.));
#238203=CARTESIAN_POINT('Ctrl Pts',(-22.47144908137,7.66905623680835,12.));
#238204=CARTESIAN_POINT('Ctrl Pts',(-22.4915157622308,7.66924504520302,
12.));
#238205=CARTESIAN_POINT('Ctrl Pts',(-22.5116918927023,7.66938065829082,
12.));
#238206=CARTESIAN_POINT('Ctrl Pts',(-22.5319766049191,7.66946263138116,
12.));
#238207=CARTESIAN_POINT('Ctrl Pts',(-22.5523690409109,7.66949052679671,
12.));
#238208=CARTESIAN_POINT('Ctrl Pts',(-22.5728683523829,7.66946391372299,
12.));
#238209=CARTESIAN_POINT('Ctrl Pts',(-22.5934737004955,7.66938236806241,
12.));
#238210=CARTESIAN_POINT('Ctrl Pts',(-22.6141842556248,7.66924547229435,
12.));
#238211=CARTESIAN_POINT('Ctrl Pts',(-22.6349991971547,7.66905281533745,
12.));
#238212=CARTESIAN_POINT('Ctrl Pts',(-22.6559177133133,7.66880399241354,
12.));
#238213=CARTESIAN_POINT('Ctrl Pts',(-22.6769390009889,7.66849860491763,
12.));
#238214=CARTESIAN_POINT('Ctrl Pts',(-22.6980622655446,7.66813626029276,
12.));
#238215=CARTESIAN_POINT('Ctrl Pts',(-22.7192867206242,7.6677165719101,12.));
#238216=CARTESIAN_POINT('Ctrl Pts',(-22.7406115879508,7.66723915895412,
12.));
#238217=CARTESIAN_POINT('Ctrl Pts',(-22.7620360971839,7.66670364630273,
12.));
#238218=CARTESIAN_POINT('Ctrl Pts',(-22.7835594857697,7.66610966441259,
12.));
#238219=CARTESIAN_POINT('Ctrl Pts',(-22.8051809987834,7.66545684920987,
12.));
#238220=CARTESIAN_POINT('Ctrl Pts',(-22.8268998887679,7.66474484198553,
12.));
#238221=CARTESIAN_POINT('Ctrl Pts',(-22.8487154155569,7.66397328929805,
12.));
#238222=CARTESIAN_POINT('Ctrl Pts',(-22.870626846128,7.66314184287334,12.));
#238223=CARTESIAN_POINT('Ctrl Pts',(-22.8926334544879,7.66225015950147,
12.));
#238224=CARTESIAN_POINT('Ctrl Pts',(-22.9147345215418,7.661297900941,12.));
#238225=CARTESIAN_POINT('Ctrl Pts',(-22.9369293349592,7.66028473382777,
12.));
#238226=CARTESIAN_POINT('Ctrl Pts',(-22.9592171890332,7.65921032958912,
12.));
#238227=CARTESIAN_POINT('Ctrl Pts',(-22.9815973845301,7.65807436436453,
12.));
#238228=CARTESIAN_POINT('Ctrl Pts',(-23.004069228582,7.6568765189133,12.));
#238229=CARTESIAN_POINT('Ctrl Pts',(-23.0266320345792,7.65561647852555,
12.));
#238230=CARTESIAN_POINT('Ctrl Pts',(-23.049285122053,7.65429393293955,12.));
#238231=CARTESIAN_POINT('Ctrl Pts',(-23.072027816555,7.65290857626356,12.));
#238232=CARTESIAN_POINT('Ctrl Pts',(-23.0948594495246,7.65146010690464,
12.));
#238233=CARTESIAN_POINT('Ctrl Pts',(-23.1177793581674,7.64994822749845,
12.));
#238234=CARTESIAN_POINT('Ctrl Pts',(-23.1407868853815,7.64837264482929,
12.));
#238235=CARTESIAN_POINT('Ctrl Pts',(-23.1638813796691,7.64673306975797,
12.));
#238236=CARTESIAN_POINT('Ctrl Pts',(-23.1870621950452,7.64502921715483,
12.));
#238237=CARTESIAN_POINT('Ctrl Pts',(-23.2103286909399,7.64326080583684,
12.));
#238238=CARTESIAN_POINT('Ctrl Pts',(-23.2336802320912,7.64142755851508,
12.));
#238239=CARTESIAN_POINT('Ctrl Pts',(-23.2571161884487,7.63952920172837,
12.));
#238240=CARTESIAN_POINT('Ctrl Pts',(-23.2806359350853,7.63756546576375,
12.));
#238241=CARTESIAN_POINT('Ctrl Pts',(-23.3042388521021,7.63553608458784,
12.));
#238242=CARTESIAN_POINT('Ctrl Pts',(-23.3279243245241,7.63344079578162,
12.));
#238243=CARTESIAN_POINT('Ctrl Pts',(-23.3516917421973,7.63127934048139,
12.));
#238244=CARTESIAN_POINT('Ctrl Pts',(-23.3755404996638,7.62905146332598,
12.));
#238245=CARTESIAN_POINT('Ctrl Pts',(-23.3994699961122,7.62675691240335,
12.));
#238246=CARTESIAN_POINT('Ctrl Pts',(-23.4234796353544,7.62439543920054,
12.));
#238247=CARTESIAN_POINT('Ctrl Pts',(-23.4475688257854,7.62196679855957,
12.));
#238248=CARTESIAN_POINT('Ctrl Pts',(-23.4717369803438,7.61947074863977,
12.));
#238249=CARTESIAN_POINT('Ctrl Pts',(-23.4959835164608,7.61690705088319,
12.));
#238250=CARTESIAN_POINT('Ctrl Pts',(-23.5203078560128,7.61427546999299,
12.));
#238251=CARTESIAN_POINT('Ctrl Pts',(-23.5447094252029,7.61157577385372,
12.));
#238252=CARTESIAN_POINT('Ctrl Pts',(-23.5691876544243,7.60880773344599,
12.));
#238253=CARTESIAN_POINT('Ctrl Pts',(-23.5937419781244,7.60597112277094,
12.));
#238254=CARTESIAN_POINT('Ctrl Pts',(-23.6183718346576,7.60306571877806,
12.));
#238255=CARTESIAN_POINT('Ctrl Pts',(-23.6430766661419,7.60009130130129,
12.));
#238256=CARTESIAN_POINT('Ctrl Pts',(-23.6678559182876,7.59704765299572,
12.));
#238257=CARTESIAN_POINT('Ctrl Pts',(-23.6927090405067,7.59393455934042,
12.));
#238258=CARTESIAN_POINT('Ctrl Pts',(-23.7176354860457,7.59075180865327,
12.));
#238259=CARTESIAN_POINT('Ctrl Pts',(-23.7426347121006,7.58749919210832,
12.));
#238260=CARTESIAN_POINT('Ctrl Pts',(-23.7677061799376,7.58417650376272,
12.));
#238261=CARTESIAN_POINT('Ctrl Pts',(-23.7928493549908,7.58078354058212,
12.));
#238262=CARTESIAN_POINT('Ctrl Pts',(-23.8180637069977,7.57732010249066,
12.));
#238263=CARTESIAN_POINT('Ctrl Pts',(-23.8433487096134,7.57378599219816,
12.));
#238264=CARTESIAN_POINT('Ctrl Pts',(-23.8687038399598,7.57018101500711,
12.));
#238265=CARTESIAN_POINT('Ctrl Pts',(-23.8941285782003,7.56650497863792,
12.));
#238266=CARTESIAN_POINT('Ctrl Pts',(-23.9196224070759,7.56275769304773,
12.));
#238267=CARTESIAN_POINT('Ctrl Pts',(-23.9451848115,7.55893897027682,12.));
#238268=CARTESIAN_POINT('Ctrl Pts',(-23.9708152779884,7.55504862424812,
12.));
#238269=CARTESIAN_POINT('Ctrl Pts',(-23.9965132953185,7.55108647097441,
12.));
#238270=CARTESIAN_POINT('Ctrl Pts',(-24.022278355453,7.5470523288591,12.));
#238271=CARTESIAN_POINT('Ctrl Pts',(-24.0481099543353,7.54294601896144,
12.));
#238272=CARTESIAN_POINT('Ctrl Pts',(-24.0740075927985,7.53876736531014,
12.));
#238273=CARTESIAN_POINT('Ctrl Pts',(-24.0999707772642,7.53451619514649,
12.));
#238274=CARTESIAN_POINT('Ctrl Pts',(-24.1259990209207,7.53019233935501,
12.));
#238275=CARTESIAN_POINT('Ctrl Pts',(-24.1520918425364,7.52579563201424,
12.));
#238276=CARTESIAN_POINT('Ctrl Pts',(-24.1782487641594,7.52132590953802,
12.));
#238277=CARTESIAN_POINT('Ctrl Pts',(-24.2044693092349,7.51678300997949,
12.));
#238278=CARTESIAN_POINT('Ctrl Pts',(-24.2307530003887,7.51216677222181,
12.));
#238279=CARTESIAN_POINT('Ctrl Pts',(-24.2570993577034,7.50747703535133,
12.));
#238280=CARTESIAN_POINT('Ctrl Pts',(-24.2835078958973,7.50271363765152,
12.));
#238281=CARTESIAN_POINT('Ctrl Pts',(-24.3099781253355,7.49787641695439,
12.));
#238282=CARTESIAN_POINT('Ctrl Pts',(-24.3365095573685,7.4929652125242,12.));
#238283=CARTESIAN_POINT('Ctrl Pts',(-24.3631017084524,7.48797986651908,
12.));
#238284=CARTESIAN_POINT('Ctrl Pts',(-24.3897541049254,7.48292022569301,
12.));
#238285=CARTESIAN_POINT('Ctrl Pts',(-24.4164662871163,7.47778614286565,
12.));
#238286=CARTESIAN_POINT('Ctrl Pts',(-24.443237814649,7.47257747883246,12.));
#238287=CARTESIAN_POINT('Ctrl Pts',(-24.4700682684524,7.46729410308786,
12.));
#238288=CARTESIAN_POINT('Ctrl Pts',(-24.4969572391483,7.46193588961463,
12.));
#238289=CARTESIAN_POINT('Ctrl Pts',(-24.5239043173072,7.45650271335862,
12.));
#238290=CARTESIAN_POINT('Ctrl Pts',(-24.5509090831559,7.4509944465116,12.));
#238291=CARTESIAN_POINT('Ctrl Pts',(-24.577971096086,7.44541095473134,12.));
#238292=CARTESIAN_POINT('Ctrl Pts',(-24.6050898852368,7.43975209375504,
12.));
#238293=CARTESIAN_POINT('Ctrl Pts',(-24.6322649369517,7.43401770489524,
12.));
#238294=CARTESIAN_POINT('Ctrl Pts',(-24.6594957128756,7.42820762159126,
12.));
#238295=CARTESIAN_POINT('Ctrl Pts',(-24.6867816727192,7.42232167766265,
12.));
#238296=CARTESIAN_POINT('Ctrl Pts',(-24.7141222950051,7.41635971481674,
12.));
#238297=CARTESIAN_POINT('Ctrl Pts',(-24.7415170994784,7.41032159082382,
12.));
#238298=CARTESIAN_POINT('Ctrl Pts',(-24.7689656668983,7.40420718661603,
12.));
#238299=CARTESIAN_POINT('Ctrl Pts',(-24.7964676646431,7.39801641583013,
12.));
#238300=CARTESIAN_POINT('Ctrl Pts',(-24.8240228520893,7.39174922585808,
12.));
#238301=CARTESIAN_POINT('Ctrl Pts',(-24.8516310625176,7.38540558903621,
12.));
#238302=CARTESIAN_POINT('Ctrl Pts',(-24.8792921911115,7.3789854964027,12.));
#238303=CARTESIAN_POINT('Ctrl Pts',(-24.901463382605,7.37378825961676,12.));
#238304=CARTESIAN_POINT('Ctrl Pts',(-24.9181155530543,7.3698559312009,12.));
#238305=CARTESIAN_POINT('Ctrl Pts',(-24.9292275670674,7.36721909028843,
12.));
#238306=CARTESIAN_POINT('Ctrl Pts',(-24.9347862158358,7.36589684767345,
12.));
#238307=CARTESIAN_POINT('Ctrl Pts',(-20.353053841303,9.71462809124917,0.));
#238308=CARTESIAN_POINT('Ctrl Pts',(-20.353053841303,9.71462809124917,12.));
#238309=CARTESIAN_POINT('Ctrl Pts',(-20.353060251684,9.71462954053074,0.));
#238310=CARTESIAN_POINT('Ctrl Pts',(-20.353060251684,9.71462954053074,12.));
#238311=CARTESIAN_POINT('Ctrl Pts',(-20.3531126095522,9.71465227853122,
0.));
#238312=CARTESIAN_POINT('Ctrl Pts',(-20.3531126095522,9.71465227853122,
12.));
#238313=CARTESIAN_POINT('Ctrl Pts',(-20.3533097561886,9.71474590350791,
0.));
#238314=CARTESIAN_POINT('Ctrl Pts',(-20.3533097561886,9.71474590350791,
12.));
#238315=CARTESIAN_POINT('Ctrl Pts',(-20.3538098605706,9.71498978052101,
0.));
#238316=CARTESIAN_POINT('Ctrl Pts',(-20.3538098605706,9.71498978052101,
12.));
#238317=CARTESIAN_POINT('Ctrl Pts',(-20.3548282742361,9.71549257088175,
0.));
#238318=CARTESIAN_POINT('Ctrl Pts',(-20.3548282742361,9.71549257088175,
12.));
#238319=CARTESIAN_POINT('Ctrl Pts',(-20.3562337557875,9.71619192554147,
0.));
#238320=CARTESIAN_POINT('Ctrl Pts',(-20.3562337557875,9.71619192554147,
12.));
#238321=CARTESIAN_POINT('Ctrl Pts',(-20.3580133103357,9.71708493723061,
0.));
#238322=CARTESIAN_POINT('Ctrl Pts',(-20.3580133103357,9.71708493723061,
12.));
#238323=CARTESIAN_POINT('Ctrl Pts',(-20.3601498764344,9.71816778327999,
0.));
#238324=CARTESIAN_POINT('Ctrl Pts',(-20.3601498764344,9.71816778327999,
12.));
#238325=CARTESIAN_POINT('Ctrl Pts',(-20.362625691398,9.71943648548114,0.));
#238326=CARTESIAN_POINT('Ctrl Pts',(-20.362625691398,9.71943648548114,12.));
#238327=CARTESIAN_POINT('Ctrl Pts',(-20.3654261611055,9.72088778381102,
0.));
#238328=CARTESIAN_POINT('Ctrl Pts',(-20.3654261611055,9.72088778381102,
12.));
#238329=CARTESIAN_POINT('Ctrl Pts',(-20.3685406190576,9.72251930722504,
0.));
#238330=CARTESIAN_POINT('Ctrl Pts',(-20.3685406190576,9.72251930722504,
12.));
#238331=CARTESIAN_POINT('Ctrl Pts',(-20.371960235676,9.72432910043193,0.));
#238332=CARTESIAN_POINT('Ctrl Pts',(-20.371960235676,9.72432910043193,12.));
#238333=CARTESIAN_POINT('Ctrl Pts',(-20.3756766651952,9.72631531732871,
0.));
#238334=CARTESIAN_POINT('Ctrl Pts',(-20.3756766651952,9.72631531732871,
12.));
#238335=CARTESIAN_POINT('Ctrl Pts',(-20.3796805893304,9.72847589116533,
0.));
#238336=CARTESIAN_POINT('Ctrl Pts',(-20.3796805893304,9.72847589116533,
12.));
#238337=CARTESIAN_POINT('Ctrl Pts',(-20.3839624556742,9.73080870123726,
0.));
#238338=CARTESIAN_POINT('Ctrl Pts',(-20.3839624556742,9.73080870123726,
12.));
#238339=CARTESIAN_POINT('Ctrl Pts',(-20.3885129129912,9.73331167102812,
0.));
#238340=CARTESIAN_POINT('Ctrl Pts',(-20.3885129129912,9.73331167102812,
12.));
#238341=CARTESIAN_POINT('Ctrl Pts',(-20.3933234845646,9.7359829201425,0.));
#238342=CARTESIAN_POINT('Ctrl Pts',(-20.3933234845646,9.7359829201425,12.));
#238343=CARTESIAN_POINT('Ctrl Pts',(-20.3983866213331,9.73882077613206,
0.));
#238344=CARTESIAN_POINT('Ctrl Pts',(-20.3983866213331,9.73882077613206,
12.));
#238345=CARTESIAN_POINT('Ctrl Pts',(-20.4036953576549,9.74182369656272,
0.));
#238346=CARTESIAN_POINT('Ctrl Pts',(-20.4036953576549,9.74182369656272,
12.));
#238347=CARTESIAN_POINT('Ctrl Pts',(-20.4092430879861,9.74499021838536,
0.));
#238348=CARTESIAN_POINT('Ctrl Pts',(-20.4092430879861,9.74499021838536,
12.));
#238349=CARTESIAN_POINT('Ctrl Pts',(-20.4150232777393,9.74831889242175,
0.));
#238350=CARTESIAN_POINT('Ctrl Pts',(-20.4150232777393,9.74831889242175,
12.));
#238351=CARTESIAN_POINT('Ctrl Pts',(-20.4210295275818,9.75180829786433,
0.));
#238352=CARTESIAN_POINT('Ctrl Pts',(-20.4210295275818,9.75180829786433,
12.));
#238353=CARTESIAN_POINT('Ctrl Pts',(-20.4272556476629,9.75545705902416,
0.));
#238354=CARTESIAN_POINT('Ctrl Pts',(-20.4272556476629,9.75545705902416,
12.));
#238355=CARTESIAN_POINT('Ctrl Pts',(-20.4336957355474,9.7592638628993,0.));
#238356=CARTESIAN_POINT('Ctrl Pts',(-20.4336957355474,9.7592638628993,12.));
#238357=CARTESIAN_POINT('Ctrl Pts',(-20.4403442329401,9.76322747195502,
0.));
#238358=CARTESIAN_POINT('Ctrl Pts',(-20.4403442329401,9.76322747195502,
12.));
#238359=CARTESIAN_POINT('Ctrl Pts',(-20.447195862298,9.76734670980897,0.));
#238360=CARTESIAN_POINT('Ctrl Pts',(-20.447195862298,9.76734670980897,12.));
#238361=CARTESIAN_POINT('Ctrl Pts',(-20.4542455817527,9.7716204510407,0.));
#238362=CARTESIAN_POINT('Ctrl Pts',(-20.4542455817527,9.7716204510407,12.));
#238363=CARTESIAN_POINT('Ctrl Pts',(-20.4614885274973,9.77604760815523,
0.));
#238364=CARTESIAN_POINT('Ctrl Pts',(-20.4614885274973,9.77604760815523,
12.));
#238365=CARTESIAN_POINT('Ctrl Pts',(-20.4689199790668,9.78062712373313,
0.));
#238366=CARTESIAN_POINT('Ctrl Pts',(-20.4689199790668,9.78062712373313,
12.));
#238367=CARTESIAN_POINT('Ctrl Pts',(-20.4765353711585,9.78535797314162,
0.));
#238368=CARTESIAN_POINT('Ctrl Pts',(-20.4765353711585,9.78535797314162,
12.));
#238369=CARTESIAN_POINT('Ctrl Pts',(-20.4843302955329,9.7902391649866,0.));
#238370=CARTESIAN_POINT('Ctrl Pts',(-20.4843302955329,9.7902391649866,12.));
#238371=CARTESIAN_POINT('Ctrl Pts',(-20.4923005087945,9.79526974288344,
0.));
#238372=CARTESIAN_POINT('Ctrl Pts',(-20.4923005087945,9.79526974288344,
12.));
#238373=CARTESIAN_POINT('Ctrl Pts',(-20.500441931211,9.80044878520967,0.));
#238374=CARTESIAN_POINT('Ctrl Pts',(-20.500441931211,9.80044878520967,12.));
#238375=CARTESIAN_POINT('Ctrl Pts',(-20.5087506310507,9.80577540161103,
0.));
#238376=CARTESIAN_POINT('Ctrl Pts',(-20.5087506310507,9.80577540161103,
12.));
#238377=CARTESIAN_POINT('Ctrl Pts',(-20.5172228122839,9.81124873025278,
0.));
#238378=CARTESIAN_POINT('Ctrl Pts',(-20.5172228122839,9.81124873025278,
12.));
#238379=CARTESIAN_POINT('Ctrl Pts',(-20.5258548000625,9.81686793455918,
0.));
#238380=CARTESIAN_POINT('Ctrl Pts',(-20.5258548000625,9.81686793455918,
12.));
#238381=CARTESIAN_POINT('Ctrl Pts',(-20.534643029951,9.82263220080328,0.));
#238382=CARTESIAN_POINT('Ctrl Pts',(-20.534643029951,9.82263220080328,12.));
#238383=CARTESIAN_POINT('Ctrl Pts',(-20.5435840460717,9.82854073773857,
0.));
#238384=CARTESIAN_POINT('Ctrl Pts',(-20.5435840460717,9.82854073773857,
12.));
#238385=CARTESIAN_POINT('Ctrl Pts',(-20.5526744976461,9.83459277585321,
0.));
#238386=CARTESIAN_POINT('Ctrl Pts',(-20.5526744976461,9.83459277585321,
12.));
#238387=CARTESIAN_POINT('Ctrl Pts',(-20.5619111362406,9.84078756677589,
0.));
#238388=CARTESIAN_POINT('Ctrl Pts',(-20.5619111362406,9.84078756677589,
12.));
#238389=CARTESIAN_POINT('Ctrl Pts',(-20.5712908125145,9.84712438256308,
0.));
#238390=CARTESIAN_POINT('Ctrl Pts',(-20.5712908125145,9.84712438256308,
12.));
#238391=CARTESIAN_POINT('Ctrl Pts',(-20.580810471002,9.85360251457004,0.));
#238392=CARTESIAN_POINT('Ctrl Pts',(-20.580810471002,9.85360251457004,12.));
#238393=CARTESIAN_POINT('Ctrl Pts',(-20.5904671449754,9.86022127232749,
0.));
#238394=CARTESIAN_POINT('Ctrl Pts',(-20.5904671449754,9.86022127232749,
12.));
#238395=CARTESIAN_POINT('Ctrl Pts',(-20.6002579513696,9.86697998242612,
0.));
#238396=CARTESIAN_POINT('Ctrl Pts',(-20.6002579513696,9.86697998242612,
12.));
#238397=CARTESIAN_POINT('Ctrl Pts',(-20.6101800854491,9.87387798732944,
0.));
#238398=CARTESIAN_POINT('Ctrl Pts',(-20.6101800854491,9.87387798732944,
12.));
#238399=CARTESIAN_POINT('Ctrl Pts',(-20.6202308177472,9.88091464472669,
0.));
#238400=CARTESIAN_POINT('Ctrl Pts',(-20.6202308177472,9.88091464472669,
12.));
#238401=CARTESIAN_POINT('Ctrl Pts',(-20.6304074914086,9.88808932697305,
0.));
#238402=CARTESIAN_POINT('Ctrl Pts',(-20.6304074914086,9.88808932697305,
12.));
#238403=CARTESIAN_POINT('Ctrl Pts',(-20.6407075193977,9.89540142049124,
0.));
#238404=CARTESIAN_POINT('Ctrl Pts',(-20.6407075193977,9.89540142049124,
12.));
#238405=CARTESIAN_POINT('Ctrl Pts',(-20.6511283817415,9.90285032516696,
0.));
#238406=CARTESIAN_POINT('Ctrl Pts',(-20.6511283817415,9.90285032516696,
12.));
#238407=CARTESIAN_POINT('Ctrl Pts',(-20.6616676228315,9.91043545377004,
0.));
#238408=CARTESIAN_POINT('Ctrl Pts',(-20.6616676228315,9.91043545377004,
12.));
#238409=CARTESIAN_POINT('Ctrl Pts',(-20.6723228488262,9.91815623141284,
0.));
#238410=CARTESIAN_POINT('Ctrl Pts',(-20.6723228488262,9.91815623141284,
12.));
#238411=CARTESIAN_POINT('Ctrl Pts',(-20.6830917250255,9.9260120949875,0.));
#238412=CARTESIAN_POINT('Ctrl Pts',(-20.6830917250255,9.9260120949875,12.));
#238413=CARTESIAN_POINT('Ctrl Pts',(-20.6939719732485,9.93400249259736,
0.));
#238414=CARTESIAN_POINT('Ctrl Pts',(-20.6939719732485,9.93400249259736,
12.));
#238415=CARTESIAN_POINT('Ctrl Pts',(-20.7049613692237,9.94212688298251,
0.));
#238416=CARTESIAN_POINT('Ctrl Pts',(-20.7049613692237,9.94212688298251,
12.));
#238417=CARTESIAN_POINT('Ctrl Pts',(-20.716057740758,9.95038473514962,0.));
#238418=CARTESIAN_POINT('Ctrl Pts',(-20.716057740758,9.95038473514962,12.));
#238419=CARTESIAN_POINT('Ctrl Pts',(-20.7272589658752,9.95877552798403,
0.));
#238420=CARTESIAN_POINT('Ctrl Pts',(-20.7272589658752,9.95877552798403,
12.));
#238421=CARTESIAN_POINT('Ctrl Pts',(-20.7385629709795,9.96729874986198,
0.));
#238422=CARTESIAN_POINT('Ctrl Pts',(-20.7385629709795,9.96729874986198,
12.));
#238423=CARTESIAN_POINT('Ctrl Pts',(-20.7499677289625,9.97595389823461,
0.));
#238424=CARTESIAN_POINT('Ctrl Pts',(-20.7499677289625,9.97595389823461,
12.));
#238425=CARTESIAN_POINT('Ctrl Pts',(-20.7614712574989,9.98474047926846,
0.));
#238426=CARTESIAN_POINT('Ctrl Pts',(-20.7614712574989,9.98474047926846,
12.));
#238427=CARTESIAN_POINT('Ctrl Pts',(-20.7730716175417,9.99365800754638,
0.));
#238428=CARTESIAN_POINT('Ctrl Pts',(-20.7730716175417,9.99365800754638,
12.));
#238429=CARTESIAN_POINT('Ctrl Pts',(-20.7847669117568,10.0027060057389,
0.));
#238430=CARTESIAN_POINT('Ctrl Pts',(-20.7847669117568,10.0027060057389,
12.));
#238431=CARTESIAN_POINT('Ctrl Pts',(-20.7965552829907,10.0118840042786,
0.));
#238432=CARTESIAN_POINT('Ctrl Pts',(-20.7965552829907,10.0118840042786,
12.));
#238433=CARTESIAN_POINT('Ctrl Pts',(-20.8084349126885,10.0211915410095,
0.));
#238434=CARTESIAN_POINT('Ctrl Pts',(-20.8084349126885,10.0211915410095,
12.));
#238435=CARTESIAN_POINT('Ctrl Pts',(-20.8204040196599,10.0306281609435,
0.));
#238436=CARTESIAN_POINT('Ctrl Pts',(-20.8204040196599,10.0306281609435,
12.));
#238437=CARTESIAN_POINT('Ctrl Pts',(-20.8324608588906,10.0401934160234,
0.));
#238438=CARTESIAN_POINT('Ctrl Pts',(-20.8324608588906,10.0401934160234,
12.));
#238439=CARTESIAN_POINT('Ctrl Pts',(-20.8446037203402,10.0498868648733,
0.));
#238440=CARTESIAN_POINT('Ctrl Pts',(-20.8446037203402,10.0498868648733,
12.));
#238441=CARTESIAN_POINT('Ctrl Pts',(-20.856830927732,10.0597080725375,0.));
#238442=CARTESIAN_POINT('Ctrl Pts',(-20.856830927732,10.0597080725375,12.));
#238443=CARTESIAN_POINT('Ctrl Pts',(-20.8691408373705,10.0696566102219,
0.));
#238444=CARTESIAN_POINT('Ctrl Pts',(-20.8691408373705,10.0696566102219,
12.));
#238445=CARTESIAN_POINT('Ctrl Pts',(-20.8815318371844,10.0797320551154,
0.));
#238446=CARTESIAN_POINT('Ctrl Pts',(-20.8815318371844,10.0797320551154,
12.));
#238447=CARTESIAN_POINT('Ctrl Pts',(-20.8940023457371,10.0899339901916,
0.));
#238448=CARTESIAN_POINT('Ctrl Pts',(-20.8940023457371,10.0899339901916,
12.));
#238449=CARTESIAN_POINT('Ctrl Pts',(-20.9065508112556,10.1002620040076,
0.));
#238450=CARTESIAN_POINT('Ctrl Pts',(-20.9065508112556,10.1002620040076,
12.));
#238451=CARTESIAN_POINT('Ctrl Pts',(-20.9191757106266,10.1107156904836,
0.));
#238452=CARTESIAN_POINT('Ctrl Pts',(-20.9191757106266,10.1107156904836,
12.));
#238453=CARTESIAN_POINT('Ctrl Pts',(-20.931875548473,10.1212946487057,0.));
#238454=CARTESIAN_POINT('Ctrl Pts',(-20.931875548473,10.1212946487057,12.));
#238455=CARTESIAN_POINT('Ctrl Pts',(-20.944648856393,10.1319984827909,0.));
#238456=CARTESIAN_POINT('Ctrl Pts',(-20.944648856393,10.1319984827909,12.));
#238457=CARTESIAN_POINT('Ctrl Pts',(-20.9574941921591,10.1428268017257,
0.));
#238458=CARTESIAN_POINT('Ctrl Pts',(-20.9574941921591,10.1428268017257,
12.));
#238459=CARTESIAN_POINT('Ctrl Pts',(-20.970410138937,10.1537792192065,0.));
#238460=CARTESIAN_POINT('Ctrl Pts',(-20.970410138937,10.1537792192065,12.));
#238461=CARTESIAN_POINT('Ctrl Pts',(-20.9833953044737,10.1648553534567,
0.));
#238462=CARTESIAN_POINT('Ctrl Pts',(-20.9833953044737,10.1648553534567,
12.));
#238463=CARTESIAN_POINT('Ctrl Pts',(-20.9964483203685,10.1760548270765,
0.));
#238464=CARTESIAN_POINT('Ctrl Pts',(-20.9964483203685,10.1760548270765,
12.));
#238465=CARTESIAN_POINT('Ctrl Pts',(-21.0095678414486,10.1873772669358,
0.));
#238466=CARTESIAN_POINT('Ctrl Pts',(-21.0095678414486,10.1873772669358,
12.));
#238467=CARTESIAN_POINT('Ctrl Pts',(-21.0227525451107,10.1988223040425,
0.));
#238468=CARTESIAN_POINT('Ctrl Pts',(-21.0227525451107,10.1988223040425,
12.));
#238469=CARTESIAN_POINT('Ctrl Pts',(-21.0360011306814,10.2103895734123,
0.));
#238470=CARTESIAN_POINT('Ctrl Pts',(-21.0360011306814,10.2103895734123,
12.));
#238471=CARTESIAN_POINT('Ctrl Pts',(-21.0493123187483,10.2220787139157,
0.));
#238472=CARTESIAN_POINT('Ctrl Pts',(-21.0493123187483,10.2220787139157,
12.));
#238473=CARTESIAN_POINT('Ctrl Pts',(-21.0626848505665,10.233889368157,0.));
#238474=CARTESIAN_POINT('Ctrl Pts',(-21.0626848505665,10.233889368157,12.));
#238475=CARTESIAN_POINT('Ctrl Pts',(-21.0761174875448,10.2458211823915,
0.));
#238476=CARTESIAN_POINT('Ctrl Pts',(-21.0761174875448,10.2458211823915,
12.));
#238477=CARTESIAN_POINT('Ctrl Pts',(-21.0896090107066,10.2578738064183,
0.));
#238478=CARTESIAN_POINT('Ctrl Pts',(-21.0896090107066,10.2578738064183,
12.));
#238479=CARTESIAN_POINT('Ctrl Pts',(-21.1031582201625,10.2700468934743,
0.));
#238480=CARTESIAN_POINT('Ctrl Pts',(-21.1031582201625,10.2700468934743,
12.));
#238481=CARTESIAN_POINT('Ctrl Pts',(-21.1167639345623,10.2823401001067,
0.));
#238482=CARTESIAN_POINT('Ctrl Pts',(-21.1167639345623,10.2823401001067,
12.));
#238483=CARTESIAN_POINT('Ctrl Pts',(-21.130424990599,10.2947530860714,0.));
#238484=CARTESIAN_POINT('Ctrl Pts',(-21.130424990599,10.2947530860714,12.));
#238485=CARTESIAN_POINT('Ctrl Pts',(-21.1441402425831,10.307285514268,0.));
#238486=CARTESIAN_POINT('Ctrl Pts',(-21.1441402425831,10.307285514268,12.));
#238487=CARTESIAN_POINT('Ctrl Pts',(-21.1579085619959,10.3199370506541,
0.));
#238488=CARTESIAN_POINT('Ctrl Pts',(-21.1579085619959,10.3199370506541,
12.));
#238489=CARTESIAN_POINT('Ctrl Pts',(-21.1717288370512,10.3327073641574,
0.));
#238490=CARTESIAN_POINT('Ctrl Pts',(-21.1717288370512,10.3327073641574,
12.));
#238491=CARTESIAN_POINT('Ctrl Pts',(-21.1855999722427,10.3455961265706,
0.));
#238492=CARTESIAN_POINT('Ctrl Pts',(-21.1855999722427,10.3455961265706,
12.));
#238493=CARTESIAN_POINT('Ctrl Pts',(-21.1995208879205,10.3586030124595,
0.));
#238494=CARTESIAN_POINT('Ctrl Pts',(-21.1995208879205,10.3586030124595,
12.));
#238495=CARTESIAN_POINT('Ctrl Pts',(-21.2134905199359,10.3717276991137,
0.));
#238496=CARTESIAN_POINT('Ctrl Pts',(-21.2134905199359,10.3717276991137,
12.));
#238497=CARTESIAN_POINT('Ctrl Pts',(-21.2275078192708,10.384969866479,0.));
#238498=CARTESIAN_POINT('Ctrl Pts',(-21.2275078192708,10.384969866479,12.));
#238499=CARTESIAN_POINT('Ctrl Pts',(-21.2415717516713,10.3983291970846,
0.));
#238500=CARTESIAN_POINT('Ctrl Pts',(-21.2415717516713,10.3983291970846,
12.));
#238501=CARTESIAN_POINT('Ctrl Pts',(-21.2556812972741,10.4118053759584,
0.));
#238502=CARTESIAN_POINT('Ctrl Pts',(-21.2556812972741,10.4118053759584,
12.));
#238503=CARTESIAN_POINT('Ctrl Pts',(-21.2698354502391,10.4253980905394,
0.));
#238504=CARTESIAN_POINT('Ctrl Pts',(-21.2698354502391,10.4253980905394,
12.));
#238505=CARTESIAN_POINT('Ctrl Pts',(-21.2840332184471,10.4391070306385,
0.));
#238506=CARTESIAN_POINT('Ctrl Pts',(-21.2840332184471,10.4391070306385,
12.));
#238507=CARTESIAN_POINT('Ctrl Pts',(-21.2982736231924,10.452931888387,0.));
#238508=CARTESIAN_POINT('Ctrl Pts',(-21.2982736231924,10.452931888387,12.));
#238509=CARTESIAN_POINT('Ctrl Pts',(-21.312555698873,10.4668723581768,0.));
#238510=CARTESIAN_POINT('Ctrl Pts',(-21.312555698873,10.4668723581768,12.));
#238511=CARTESIAN_POINT('Ctrl Pts',(-21.3268784926823,10.4809281365933,
0.));
#238512=CARTESIAN_POINT('Ctrl Pts',(-21.3268784926823,10.4809281365933,
12.));
#238513=CARTESIAN_POINT('Ctrl Pts',(-21.3412410642912,10.4950989223341,
0.));
#238514=CARTESIAN_POINT('Ctrl Pts',(-21.3412410642912,10.4950989223341,
12.));
#238515=CARTESIAN_POINT('Ctrl Pts',(-21.3556424855822,10.5093844161689,
0.));
#238516=CARTESIAN_POINT('Ctrl Pts',(-21.3556424855822,10.5093844161689,
12.));
#238517=CARTESIAN_POINT('Ctrl Pts',(-21.3700818403942,10.523784320906,0.));
#238518=CARTESIAN_POINT('Ctrl Pts',(-21.3700818403942,10.523784320906,12.));
#238519=CARTESIAN_POINT('Ctrl Pts',(-21.3845582242604,10.5382983413422,
0.));
#238520=CARTESIAN_POINT('Ctrl Pts',(-21.3845582242604,10.5382983413422,
12.));
#238521=CARTESIAN_POINT('Ctrl Pts',(-21.3990707441495,10.5529261842107,
0.));
#238522=CARTESIAN_POINT('Ctrl Pts',(-21.3990707441495,10.5529261842107,
12.));
#238523=CARTESIAN_POINT('Ctrl Pts',(-21.4136185181974,10.5676675581106,
0.));
#238524=CARTESIAN_POINT('Ctrl Pts',(-21.4136185181974,10.5676675581106,
12.));
#238525=CARTESIAN_POINT('Ctrl Pts',(-21.4282006754624,10.582522173457,0.));
#238526=CARTESIAN_POINT('Ctrl Pts',(-21.4282006754624,10.582522173457,12.));
#238527=CARTESIAN_POINT('Ctrl Pts',(-21.4428163557137,10.597489742462,0.));
#238528=CARTESIAN_POINT('Ctrl Pts',(-21.4428163557137,10.597489742462,12.));
#238529=CARTESIAN_POINT('Ctrl Pts',(-21.4574647092093,10.612569979096,0.));
#238530=CARTESIAN_POINT('Ctrl Pts',(-21.4574647092093,10.612569979096,12.));
#238531=CARTESIAN_POINT('Ctrl Pts',(-21.4721448964766,10.6277625990457,
0.));
#238532=CARTESIAN_POINT('Ctrl Pts',(-21.4721448964766,10.6277625990457,
12.));
#238533=CARTESIAN_POINT('Ctrl Pts',(-21.4868560880893,10.6430673196609,
0.));
#238534=CARTESIAN_POINT('Ctrl Pts',(-21.4868560880893,10.6430673196609,
12.));
#238535=CARTESIAN_POINT('Ctrl Pts',(-21.5015974644454,10.658483859894,0.));
#238536=CARTESIAN_POINT('Ctrl Pts',(-21.5015974644454,10.658483859894,12.));
#238537=CARTESIAN_POINT('Ctrl Pts',(-21.5163682155805,10.6740119402835,
0.));
#238538=CARTESIAN_POINT('Ctrl Pts',(-21.5163682155805,10.6740119402835,
12.));
#238539=CARTESIAN_POINT('Ctrl Pts',(-21.531167540981,10.689651282929,0.));
#238540=CARTESIAN_POINT('Ctrl Pts',(-21.531167540981,10.689651282929,12.));
#238541=CARTESIAN_POINT('Ctrl Pts',(-21.5459946493955,10.7054016114571,
0.));
#238542=CARTESIAN_POINT('Ctrl Pts',(-21.5459946493955,10.7054016114571,
12.));
#238543=CARTESIAN_POINT('Ctrl Pts',(-21.5608487586467,10.7212626509816,
0.));
#238544=CARTESIAN_POINT('Ctrl Pts',(-21.5608487586467,10.7212626509816,
12.));
#238545=CARTESIAN_POINT('Ctrl Pts',(-21.5757290954372,10.7372341280468,
0.));
#238546=CARTESIAN_POINT('Ctrl Pts',(-21.5757290954372,10.7372341280468,
12.));
#238547=CARTESIAN_POINT('Ctrl Pts',(-21.5906348951745,10.7533157705943,
0.));
#238548=CARTESIAN_POINT('Ctrl Pts',(-21.5906348951745,10.7533157705943,
12.));
#238549=CARTESIAN_POINT('Ctrl Pts',(-21.6055654018179,10.7695073079554,
0.));
#238550=CARTESIAN_POINT('Ctrl Pts',(-21.6055654018179,10.7695073079554,
12.));
#238551=CARTESIAN_POINT('Ctrl Pts',(-21.6205198677176,10.7858084708262,
0.));
#238552=CARTESIAN_POINT('Ctrl Pts',(-21.6205198677176,10.7858084708262,
12.));
#238553=CARTESIAN_POINT('Ctrl Pts',(-21.6354975534557,10.8022189912369,
0.));
#238554=CARTESIAN_POINT('Ctrl Pts',(-21.6354975534557,10.8022189912369,
12.));
#238555=CARTESIAN_POINT('Ctrl Pts',(-21.6504977276864,10.8187386025135,
0.));
#238556=CARTESIAN_POINT('Ctrl Pts',(-21.6504977276864,10.8187386025135,
12.));
#238557=CARTESIAN_POINT('Ctrl Pts',(-21.6655196669727,10.835367039227,0.));
#238558=CARTESIAN_POINT('Ctrl Pts',(-21.6655196669727,10.835367039227,12.));
#238559=CARTESIAN_POINT('Ctrl Pts',(-21.6805626556461,10.8521040371832,
0.));
#238560=CARTESIAN_POINT('Ctrl Pts',(-21.6805626556461,10.8521040371832,
12.));
#238561=CARTESIAN_POINT('Ctrl Pts',(-21.6956259856667,10.8689493334093,
0.));
#238562=CARTESIAN_POINT('Ctrl Pts',(-21.6956259856667,10.8689493334093,
12.));
#238563=CARTESIAN_POINT('Ctrl Pts',(-21.7107089564822,10.8859026661292,
0.));
#238564=CARTESIAN_POINT('Ctrl Pts',(-21.7107089564822,10.8859026661292,
12.));
#238565=CARTESIAN_POINT('Ctrl Pts',(-21.7258108748874,10.9029637747341,
0.));
#238566=CARTESIAN_POINT('Ctrl Pts',(-21.7258108748874,10.9029637747341,
12.));
#238567=CARTESIAN_POINT('Ctrl Pts',(-21.74093105488,10.9201323997386,0.));
#238568=CARTESIAN_POINT('Ctrl Pts',(-21.74093105488,10.9201323997386,12.));
#238569=CARTESIAN_POINT('Ctrl Pts',(-21.7560688175252,10.9374082827446,
0.));
#238570=CARTESIAN_POINT('Ctrl Pts',(-21.7560688175252,10.9374082827446,
12.));
#238571=CARTESIAN_POINT('Ctrl Pts',(-21.7712234908468,10.9547911664457,
0.));
#238572=CARTESIAN_POINT('Ctrl Pts',(-21.7712234908468,10.9547911664457,
12.));
#238573=CARTESIAN_POINT('Ctrl Pts',(-21.7863944097143,10.9722807946157,
0.));
#238574=CARTESIAN_POINT('Ctrl Pts',(-21.7863944097143,10.9722807946157,
12.));
#238575=CARTESIAN_POINT('Ctrl Pts',(-21.8015809157302,10.9898769120913,
0.));
#238576=CARTESIAN_POINT('Ctrl Pts',(-21.8015809157302,10.9898769120913,
12.));
#238577=CARTESIAN_POINT('Ctrl Pts',(-21.8167823571168,11.0075792647477,
0.));
#238578=CARTESIAN_POINT('Ctrl Pts',(-21.8167823571168,11.0075792647477,
12.));
#238579=CARTESIAN_POINT('Ctrl Pts',(-21.8319980886033,11.0253875994598,
0.));
#238580=CARTESIAN_POINT('Ctrl Pts',(-21.8319980886033,11.0253875994598,
12.));
#238581=CARTESIAN_POINT('Ctrl Pts',(-21.8472274713103,11.0433016640808,
0.));
#238582=CARTESIAN_POINT('Ctrl Pts',(-21.8472274713103,11.0433016640808,
12.));
#238583=CARTESIAN_POINT('Ctrl Pts',(-21.8624698726319,11.0613212074364,
0.));
#238584=CARTESIAN_POINT('Ctrl Pts',(-21.8624698726319,11.0613212074364,
12.));
#238585=CARTESIAN_POINT('Ctrl Pts',(-21.8777246661191,11.0794459793058,
0.));
#238586=CARTESIAN_POINT('Ctrl Pts',(-21.8777246661191,11.0794459793058,
12.));
#238587=CARTESIAN_POINT('Ctrl Pts',(-21.8929912313608,11.0976757303944,
0.));
#238588=CARTESIAN_POINT('Ctrl Pts',(-21.8929912313608,11.0976757303944,
12.));
#238589=CARTESIAN_POINT('Ctrl Pts',(-21.9082689538687,11.1160102123024,
0.));
#238590=CARTESIAN_POINT('Ctrl Pts',(-21.9082689538687,11.1160102123024,
12.));
#238591=CARTESIAN_POINT('Ctrl Pts',(-21.9235572249518,11.134449177474,0.));
#238592=CARTESIAN_POINT('Ctrl Pts',(-21.9235572249518,11.134449177474,12.));
#238593=CARTESIAN_POINT('Ctrl Pts',(-21.9388554416437,11.1529923792002,
0.));
#238594=CARTESIAN_POINT('Ctrl Pts',(-21.9388554416437,11.1529923792002,
12.));
#238595=CARTESIAN_POINT('Ctrl Pts',(-21.9541630066504,11.1716395716375,
0.));
#238596=CARTESIAN_POINT('Ctrl Pts',(-21.9541630066504,11.1716395716375,
12.));
#238597=CARTESIAN_POINT('Ctrl Pts',(-21.9694793282913,11.1903905098109,
0.));
#238598=CARTESIAN_POINT('Ctrl Pts',(-21.9694793282913,11.1903905098109,
12.));
#238599=CARTESIAN_POINT('Ctrl Pts',(-21.9848038204439,11.2092449496125,
0.));
#238600=CARTESIAN_POINT('Ctrl Pts',(-21.9848038204439,11.2092449496125,
12.));
#238601=CARTESIAN_POINT('Ctrl Pts',(-22.0001359024839,11.2282026477897,
0.));
#238602=CARTESIAN_POINT('Ctrl Pts',(-22.0001359024839,11.2282026477897,
12.));
#238603=CARTESIAN_POINT('Ctrl Pts',(-22.0154749992364,11.2472633619276,
0.));
#238604=CARTESIAN_POINT('Ctrl Pts',(-22.0154749992364,11.2472633619276,
12.));
#238605=CARTESIAN_POINT('Ctrl Pts',(-22.0308205408351,11.2664268504207,
0.));
#238606=CARTESIAN_POINT('Ctrl Pts',(-22.0308205408351,11.2664268504207,
12.));
#238607=CARTESIAN_POINT('Ctrl Pts',(-22.046171962566,11.2856928724374,0.));
#238608=CARTESIAN_POINT('Ctrl Pts',(-22.046171962566,11.2856928724374,12.));
#238609=CARTESIAN_POINT('Ctrl Pts',(-22.0615287047179,11.3050611878771,
0.));
#238610=CARTESIAN_POINT('Ctrl Pts',(-22.0615287047179,11.3050611878771,
12.));
#238611=CARTESIAN_POINT('Ctrl Pts',(-22.0768902124267,11.3245315573168,
0.));
#238612=CARTESIAN_POINT('Ctrl Pts',(-22.0768902124267,11.3245315573168,
12.));
#238613=CARTESIAN_POINT('Ctrl Pts',(-22.0922559355293,11.3441037419553,
0.));
#238614=CARTESIAN_POINT('Ctrl Pts',(-22.0922559355293,11.3441037419553,
12.));
#238615=CARTESIAN_POINT('Ctrl Pts',(-22.1076253283978,11.3637775035367,
0.));
#238616=CARTESIAN_POINT('Ctrl Pts',(-22.1076253283978,11.3637775035367,
12.));
#238617=CARTESIAN_POINT('Ctrl Pts',(-22.1229978500185,11.3835526044256,
0.));
#238618=CARTESIAN_POINT('Ctrl Pts',(-22.1229978500185,11.3835526044256,
12.));
#238619=CARTESIAN_POINT('Ctrl Pts',(-22.1383729640963,11.4034288076908,
0.));
#238620=CARTESIAN_POINT('Ctrl Pts',(-22.1383729640963,11.4034288076908,
12.));
#238621=CARTESIAN_POINT('Ctrl Pts',(-22.1537501391486,11.4234058771742,
0.));
#238622=CARTESIAN_POINT('Ctrl Pts',(-22.1537501391486,11.4234058771742,
12.));
#238623=CARTESIAN_POINT('Ctrl Pts',(-22.1691288486096,11.443483577557,0.));
#238624=CARTESIAN_POINT('Ctrl Pts',(-22.1691288486096,11.443483577557,12.));
#238625=CARTESIAN_POINT('Ctrl Pts',(-22.184508570917,11.463661674411,0.));
#238626=CARTESIAN_POINT('Ctrl Pts',(-22.184508570917,11.463661674411,12.));
#238627=CARTESIAN_POINT('Ctrl Pts',(-22.1998887896435,11.4839399342589,
0.));
#238628=CARTESIAN_POINT('Ctrl Pts',(-22.1998887896435,11.4839399342589,
12.));
#238629=CARTESIAN_POINT('Ctrl Pts',(-22.215268993102,11.504318124424,0.));
#238630=CARTESIAN_POINT('Ctrl Pts',(-22.215268993102,11.504318124424,12.));
#238631=CARTESIAN_POINT('Ctrl Pts',(-22.2306486738899,11.5247960128476,
0.));
#238632=CARTESIAN_POINT('Ctrl Pts',(-22.2306486738899,11.5247960128476,
12.));
#238633=CARTESIAN_POINT('Ctrl Pts',(-22.2460273284653,11.545373367912,0.));
#238634=CARTESIAN_POINT('Ctrl Pts',(-22.2460273284653,11.545373367912,12.));
#238635=CARTESIAN_POINT('Ctrl Pts',(-22.2614044566898,11.5660499582403,
0.));
#238636=CARTESIAN_POINT('Ctrl Pts',(-22.2614044566898,11.5660499582403,
12.));
#238637=CARTESIAN_POINT('Ctrl Pts',(-22.2767795614349,11.5868255525189,
0.));
#238638=CARTESIAN_POINT('Ctrl Pts',(-22.2767795614349,11.5868255525189,
12.));
#238639=CARTESIAN_POINT('Ctrl Pts',(-22.2921521480358,11.6076999192359,
0.));
#238640=CARTESIAN_POINT('Ctrl Pts',(-22.2921521480358,11.6076999192359,
12.));
#238641=CARTESIAN_POINT('Ctrl Pts',(-22.3075217249049,11.6286728270011,
0.));
#238642=CARTESIAN_POINT('Ctrl Pts',(-22.3075217249049,11.6286728270011,
12.));
#238643=CARTESIAN_POINT('Ctrl Pts',(-22.3228878043976,11.6497440449858,
0.));
#238644=CARTESIAN_POINT('Ctrl Pts',(-22.3228878043976,11.6497440449858,
12.));
#238645=CARTESIAN_POINT('Ctrl Pts',(-22.3382499035618,11.6709133432986,
0.));
#238646=CARTESIAN_POINT('Ctrl Pts',(-22.3382499035618,11.6709133432986,
12.));
#238647=CARTESIAN_POINT('Ctrl Pts',(-22.3536075450028,11.6921804934056,
0.));
#238648=CARTESIAN_POINT('Ctrl Pts',(-22.3536075450028,11.6921804934056,
12.));
#238649=CARTESIAN_POINT('Ctrl Pts',(-22.3689602575492,11.7135452684532,
0.));
#238650=CARTESIAN_POINT('Ctrl Pts',(-22.3689602575492,11.7135452684532,
12.));
#238651=CARTESIAN_POINT('Ctrl Pts',(-22.3843075773905,11.7350074437961,
0.));
#238652=CARTESIAN_POINT('Ctrl Pts',(-22.3843075773905,11.7350074437961,
12.));
#238653=CARTESIAN_POINT('Ctrl Pts',(-22.39964904692,11.7565667964765,0.));
#238654=CARTESIAN_POINT('Ctrl Pts',(-22.39964904692,11.7565667964765,12.));
#238655=CARTESIAN_POINT('Ctrl Pts',(-22.4149842125018,11.7782231042041,
0.));
#238656=CARTESIAN_POINT('Ctrl Pts',(-22.4149842125018,11.7782231042041,
12.));
#238657=CARTESIAN_POINT('Ctrl Pts',(-22.4303126226468,11.7999761445175,
0.));
#238658=CARTESIAN_POINT('Ctrl Pts',(-22.4303126226468,11.7999761445175,
12.));
#238659=CARTESIAN_POINT('Ctrl Pts',(-22.4456338258738,11.8218256937889,
0.));
#238660=CARTESIAN_POINT('Ctrl Pts',(-22.4456338258738,11.8218256937889,
12.));
#238661=CARTESIAN_POINT('Ctrl Pts',(-22.4609473690469,11.8437715264487,
0.));
#238662=CARTESIAN_POINT('Ctrl Pts',(-22.4609473690469,11.8437715264487,
12.));
#238663=CARTESIAN_POINT('Ctrl Pts',(-22.4762527946694,11.8658134137018,
0.));
#238664=CARTESIAN_POINT('Ctrl Pts',(-22.4762527946694,11.8658134137018,
12.));
#238665=CARTESIAN_POINT('Ctrl Pts',(-22.4915496418472,11.8879511239941,
0.));
#238666=CARTESIAN_POINT('Ctrl Pts',(-22.4915496418472,11.8879511239941,
12.));
#238667=CARTESIAN_POINT('Ctrl Pts',(-22.5068374513958,11.9101844254555,
0.));
#238668=CARTESIAN_POINT('Ctrl Pts',(-22.5068374513958,11.9101844254555,
12.));
#238669=CARTESIAN_POINT('Ctrl Pts',(-22.5221157697869,11.9325130877801,
0.));
#238670=CARTESIAN_POINT('Ctrl Pts',(-22.5221157697869,11.9325130877801,
12.));
#238671=CARTESIAN_POINT('Ctrl Pts',(-22.5373841537299,11.9549368843996,
0.));
#238672=CARTESIAN_POINT('Ctrl Pts',(-22.5373841537299,11.9549368843996,
12.));
#238673=CARTESIAN_POINT('Ctrl Pts',(-22.5526421741159,11.9774555943496,
0.));
#238674=CARTESIAN_POINT('Ctrl Pts',(-22.5526421741159,11.9774555943496,
12.));
#238675=CARTESIAN_POINT('Ctrl Pts',(-22.5678894211194,12.0000690046697,
0.));
#238676=CARTESIAN_POINT('Ctrl Pts',(-22.5678894211194,12.0000690046697,
12.));
#238677=CARTESIAN_POINT('Ctrl Pts',(-22.5831255061306,12.0227769113132,
0.));
#238678=CARTESIAN_POINT('Ctrl Pts',(-22.5831255061306,12.0227769113132,
12.));
#238679=CARTESIAN_POINT('Ctrl Pts',(-22.5983500505675,12.0455791139135,
0.));
#238680=CARTESIAN_POINT('Ctrl Pts',(-22.5983500505675,12.0455791139135,
12.));
#238681=CARTESIAN_POINT('Ctrl Pts',(-22.613562676493,12.0684754113869,0.));
#238682=CARTESIAN_POINT('Ctrl Pts',(-22.613562676493,12.0684754113869,12.));
#238683=CARTESIAN_POINT('Ctrl Pts',(-22.628762996708,12.0914655972828,0.));
#238684=CARTESIAN_POINT('Ctrl Pts',(-22.628762996708,12.0914655972828,12.));
#238685=CARTESIAN_POINT('Ctrl Pts',(-22.6439506046611,12.1145494550384,
0.));
#238686=CARTESIAN_POINT('Ctrl Pts',(-22.6439506046611,12.1145494550384,
12.));
#238687=CARTESIAN_POINT('Ctrl Pts',(-22.6591250653942,12.1377267537141,
0.));
#238688=CARTESIAN_POINT('Ctrl Pts',(-22.6591250653942,12.1377267537141,
12.));
#238689=CARTESIAN_POINT('Ctrl Pts',(-22.6742859034891,12.1609972423088,
0.));
#238690=CARTESIAN_POINT('Ctrl Pts',(-22.6742859034891,12.1609972423088,
12.));
#238691=CARTESIAN_POINT('Ctrl Pts',(-22.6894326204959,12.1843606579246,
0.));
#238692=CARTESIAN_POINT('Ctrl Pts',(-22.6894326204959,12.1843606579246,
12.));
#238693=CARTESIAN_POINT('Ctrl Pts',(-22.7045647168659,12.2078167360267,
0.));
#238694=CARTESIAN_POINT('Ctrl Pts',(-22.7045647168659,12.2078167360267,
12.));
#238695=CARTESIAN_POINT('Ctrl Pts',(-22.7196817119299,12.2313652198047,
0.));
#238696=CARTESIAN_POINT('Ctrl Pts',(-22.7196817119299,12.2313652198047,
12.));
#238697=CARTESIAN_POINT('Ctrl Pts',(-22.7347831655251,12.2550058702389,
0.));
#238698=CARTESIAN_POINT('Ctrl Pts',(-22.7347831655251,12.2550058702389,
12.));
#238699=CARTESIAN_POINT('Ctrl Pts',(-22.7498686970096,12.2787384750747,
0.));
#238700=CARTESIAN_POINT('Ctrl Pts',(-22.7498686970096,12.2787384750747,
12.));
#238701=CARTESIAN_POINT('Ctrl Pts',(-22.7649380101154,12.3025628601812,
0.));
#238702=CARTESIAN_POINT('Ctrl Pts',(-22.7649380101154,12.3025628601812,
12.));
#238703=CARTESIAN_POINT('Ctrl Pts',(-22.7799908974947,12.3264788926108,
0.));
#238704=CARTESIAN_POINT('Ctrl Pts',(-22.7799908974947,12.3264788926108,
12.));
#238705=CARTESIAN_POINT('Ctrl Pts',(-22.7950272216959,12.3504864740361,
0.));
#238706=CARTESIAN_POINT('Ctrl Pts',(-22.7950272216959,12.3504864740361,
12.));
#238707=CARTESIAN_POINT('Ctrl Pts',(-22.8100469022632,12.3745855366772,
0.));
#238708=CARTESIAN_POINT('Ctrl Pts',(-22.8100469022632,12.3745855366772,
12.));
#238709=CARTESIAN_POINT('Ctrl Pts',(-22.8220493007353,12.393937937903,0.));
#238710=CARTESIAN_POINT('Ctrl Pts',(-22.8220493007353,12.393937937903,12.));
#238711=CARTESIAN_POINT('Ctrl Pts',(-22.8310435872852,12.4084933766366,
0.));
#238712=CARTESIAN_POINT('Ctrl Pts',(-22.8310435872852,12.4084933766366,
12.));
#238713=CARTESIAN_POINT('Ctrl Pts',(-22.8370364396497,12.4182152851867,
0.));
#238714=CARTESIAN_POINT('Ctrl Pts',(-22.8370364396497,12.4182152851867,
12.));
#238715=CARTESIAN_POINT('Ctrl Pts',(-22.8400320311648,12.4230808101438,
0.));
#238716=CARTESIAN_POINT('Ctrl Pts',(-22.8400320311648,12.4230808101438,
12.));
#238717=CARTESIAN_POINT('',(-22.8400320311648,12.4230808101438,0.));
#238718=CARTESIAN_POINT('Ctrl Pts',(-20.353053841303,9.71462809124917,0.));
#238719=CARTESIAN_POINT('Ctrl Pts',(-20.353060251684,9.71462954053074,0.));
#238720=CARTESIAN_POINT('Ctrl Pts',(-20.3531126095522,9.71465227853122,
0.));
#238721=CARTESIAN_POINT('Ctrl Pts',(-20.3533097561886,9.71474590350791,
0.));
#238722=CARTESIAN_POINT('Ctrl Pts',(-20.3538098605706,9.71498978052101,
0.));
#238723=CARTESIAN_POINT('Ctrl Pts',(-20.3548282742361,9.71549257088175,
0.));
#238724=CARTESIAN_POINT('Ctrl Pts',(-20.3562337557875,9.71619192554147,
0.));
#238725=CARTESIAN_POINT('Ctrl Pts',(-20.3580133103357,9.71708493723061,
0.));
#238726=CARTESIAN_POINT('Ctrl Pts',(-20.3601498764344,9.71816778327999,
0.));
#238727=CARTESIAN_POINT('Ctrl Pts',(-20.362625691398,9.71943648548114,0.));
#238728=CARTESIAN_POINT('Ctrl Pts',(-20.3654261611055,9.72088778381102,
0.));
#238729=CARTESIAN_POINT('Ctrl Pts',(-20.3685406190576,9.72251930722504,
0.));
#238730=CARTESIAN_POINT('Ctrl Pts',(-20.371960235676,9.72432910043193,0.));
#238731=CARTESIAN_POINT('Ctrl Pts',(-20.3756766651952,9.72631531732871,
0.));
#238732=CARTESIAN_POINT('Ctrl Pts',(-20.3796805893304,9.72847589116533,
0.));
#238733=CARTESIAN_POINT('Ctrl Pts',(-20.3839624556742,9.73080870123726,
0.));
#238734=CARTESIAN_POINT('Ctrl Pts',(-20.3885129129912,9.73331167102812,
0.));
#238735=CARTESIAN_POINT('Ctrl Pts',(-20.3933234845646,9.7359829201425,0.));
#238736=CARTESIAN_POINT('Ctrl Pts',(-20.3983866213331,9.73882077613206,
0.));
#238737=CARTESIAN_POINT('Ctrl Pts',(-20.4036953576549,9.74182369656272,
0.));
#238738=CARTESIAN_POINT('Ctrl Pts',(-20.4092430879861,9.74499021838536,
0.));
#238739=CARTESIAN_POINT('Ctrl Pts',(-20.4150232777393,9.74831889242175,
0.));
#238740=CARTESIAN_POINT('Ctrl Pts',(-20.4210295275818,9.75180829786433,
0.));
#238741=CARTESIAN_POINT('Ctrl Pts',(-20.4272556476629,9.75545705902416,
0.));
#238742=CARTESIAN_POINT('Ctrl Pts',(-20.4336957355474,9.7592638628993,0.));
#238743=CARTESIAN_POINT('Ctrl Pts',(-20.4403442329401,9.76322747195502,
0.));
#238744=CARTESIAN_POINT('Ctrl Pts',(-20.447195862298,9.76734670980897,0.));
#238745=CARTESIAN_POINT('Ctrl Pts',(-20.4542455817527,9.7716204510407,0.));
#238746=CARTESIAN_POINT('Ctrl Pts',(-20.4614885274973,9.77604760815523,
0.));
#238747=CARTESIAN_POINT('Ctrl Pts',(-20.4689199790668,9.78062712373313,
0.));
#238748=CARTESIAN_POINT('Ctrl Pts',(-20.4765353711585,9.78535797314162,
0.));
#238749=CARTESIAN_POINT('Ctrl Pts',(-20.4843302955329,9.7902391649866,0.));
#238750=CARTESIAN_POINT('Ctrl Pts',(-20.4923005087945,9.79526974288344,
0.));
#238751=CARTESIAN_POINT('Ctrl Pts',(-20.500441931211,9.80044878520967,0.));
#238752=CARTESIAN_POINT('Ctrl Pts',(-20.5087506310507,9.80577540161103,
0.));
#238753=CARTESIAN_POINT('Ctrl Pts',(-20.5172228122839,9.81124873025278,
0.));
#238754=CARTESIAN_POINT('Ctrl Pts',(-20.5258548000625,9.81686793455918,
0.));
#238755=CARTESIAN_POINT('Ctrl Pts',(-20.534643029951,9.82263220080328,0.));
#238756=CARTESIAN_POINT('Ctrl Pts',(-20.5435840460717,9.82854073773857,
0.));
#238757=CARTESIAN_POINT('Ctrl Pts',(-20.5526744976461,9.83459277585321,
0.));
#238758=CARTESIAN_POINT('Ctrl Pts',(-20.5619111362406,9.84078756677589,
0.));
#238759=CARTESIAN_POINT('Ctrl Pts',(-20.5712908125145,9.84712438256308,
0.));
#238760=CARTESIAN_POINT('Ctrl Pts',(-20.580810471002,9.85360251457004,0.));
#238761=CARTESIAN_POINT('Ctrl Pts',(-20.5904671449754,9.86022127232749,
0.));
#238762=CARTESIAN_POINT('Ctrl Pts',(-20.6002579513696,9.86697998242612,
0.));
#238763=CARTESIAN_POINT('Ctrl Pts',(-20.6101800854491,9.87387798732944,
0.));
#238764=CARTESIAN_POINT('Ctrl Pts',(-20.6202308177472,9.88091464472669,
0.));
#238765=CARTESIAN_POINT('Ctrl Pts',(-20.6304074914086,9.88808932697305,
0.));
#238766=CARTESIAN_POINT('Ctrl Pts',(-20.6407075193977,9.89540142049124,
0.));
#238767=CARTESIAN_POINT('Ctrl Pts',(-20.6511283817415,9.90285032516696,
0.));
#238768=CARTESIAN_POINT('Ctrl Pts',(-20.6616676228315,9.91043545377004,
0.));
#238769=CARTESIAN_POINT('Ctrl Pts',(-20.6723228488262,9.91815623141284,
0.));
#238770=CARTESIAN_POINT('Ctrl Pts',(-20.6830917250255,9.9260120949875,0.));
#238771=CARTESIAN_POINT('Ctrl Pts',(-20.6939719732485,9.93400249259736,
0.));
#238772=CARTESIAN_POINT('Ctrl Pts',(-20.7049613692237,9.94212688298251,
0.));
#238773=CARTESIAN_POINT('Ctrl Pts',(-20.716057740758,9.95038473514962,0.));
#238774=CARTESIAN_POINT('Ctrl Pts',(-20.7272589658752,9.95877552798403,
0.));
#238775=CARTESIAN_POINT('Ctrl Pts',(-20.7385629709795,9.96729874986198,
0.));
#238776=CARTESIAN_POINT('Ctrl Pts',(-20.7499677289625,9.97595389823461,
0.));
#238777=CARTESIAN_POINT('Ctrl Pts',(-20.7614712574989,9.98474047926846,
0.));
#238778=CARTESIAN_POINT('Ctrl Pts',(-20.7730716175417,9.99365800754638,
0.));
#238779=CARTESIAN_POINT('Ctrl Pts',(-20.7847669117568,10.0027060057389,
0.));
#238780=CARTESIAN_POINT('Ctrl Pts',(-20.7965552829907,10.0118840042786,
0.));
#238781=CARTESIAN_POINT('Ctrl Pts',(-20.8084349126885,10.0211915410095,
0.));
#238782=CARTESIAN_POINT('Ctrl Pts',(-20.8204040196599,10.0306281609435,
0.));
#238783=CARTESIAN_POINT('Ctrl Pts',(-20.8324608588906,10.0401934160234,
0.));
#238784=CARTESIAN_POINT('Ctrl Pts',(-20.8446037203402,10.0498868648733,
0.));
#238785=CARTESIAN_POINT('Ctrl Pts',(-20.856830927732,10.0597080725375,0.));
#238786=CARTESIAN_POINT('Ctrl Pts',(-20.8691408373705,10.0696566102219,
0.));
#238787=CARTESIAN_POINT('Ctrl Pts',(-20.8815318371844,10.0797320551154,
0.));
#238788=CARTESIAN_POINT('Ctrl Pts',(-20.8940023457371,10.0899339901916,
0.));
#238789=CARTESIAN_POINT('Ctrl Pts',(-20.9065508112556,10.1002620040076,
0.));
#238790=CARTESIAN_POINT('Ctrl Pts',(-20.9191757106266,10.1107156904836,
0.));
#238791=CARTESIAN_POINT('Ctrl Pts',(-20.931875548473,10.1212946487057,0.));
#238792=CARTESIAN_POINT('Ctrl Pts',(-20.944648856393,10.1319984827909,0.));
#238793=CARTESIAN_POINT('Ctrl Pts',(-20.9574941921591,10.1428268017257,
0.));
#238794=CARTESIAN_POINT('Ctrl Pts',(-20.970410138937,10.1537792192065,0.));
#238795=CARTESIAN_POINT('Ctrl Pts',(-20.9833953044737,10.1648553534567,
0.));
#238796=CARTESIAN_POINT('Ctrl Pts',(-20.9964483203685,10.1760548270765,
0.));
#238797=CARTESIAN_POINT('Ctrl Pts',(-21.0095678414486,10.1873772669358,
0.));
#238798=CARTESIAN_POINT('Ctrl Pts',(-21.0227525451107,10.1988223040425,
0.));
#238799=CARTESIAN_POINT('Ctrl Pts',(-21.0360011306814,10.2103895734123,
0.));
#238800=CARTESIAN_POINT('Ctrl Pts',(-21.0493123187483,10.2220787139157,
0.));
#238801=CARTESIAN_POINT('Ctrl Pts',(-21.0626848505665,10.233889368157,0.));
#238802=CARTESIAN_POINT('Ctrl Pts',(-21.0761174875448,10.2458211823915,
0.));
#238803=CARTESIAN_POINT('Ctrl Pts',(-21.0896090107066,10.2578738064183,
0.));
#238804=CARTESIAN_POINT('Ctrl Pts',(-21.1031582201625,10.2700468934743,
0.));
#238805=CARTESIAN_POINT('Ctrl Pts',(-21.1167639345623,10.2823401001067,
0.));
#238806=CARTESIAN_POINT('Ctrl Pts',(-21.130424990599,10.2947530860714,0.));
#238807=CARTESIAN_POINT('Ctrl Pts',(-21.1441402425831,10.307285514268,0.));
#238808=CARTESIAN_POINT('Ctrl Pts',(-21.1579085619959,10.3199370506541,
0.));
#238809=CARTESIAN_POINT('Ctrl Pts',(-21.1717288370512,10.3327073641574,
0.));
#238810=CARTESIAN_POINT('Ctrl Pts',(-21.1855999722427,10.3455961265706,
0.));
#238811=CARTESIAN_POINT('Ctrl Pts',(-21.1995208879205,10.3586030124595,
0.));
#238812=CARTESIAN_POINT('Ctrl Pts',(-21.2134905199359,10.3717276991137,
0.));
#238813=CARTESIAN_POINT('Ctrl Pts',(-21.2275078192708,10.384969866479,0.));
#238814=CARTESIAN_POINT('Ctrl Pts',(-21.2415717516713,10.3983291970846,
0.));
#238815=CARTESIAN_POINT('Ctrl Pts',(-21.2556812972741,10.4118053759584,
0.));
#238816=CARTESIAN_POINT('Ctrl Pts',(-21.2698354502391,10.4253980905394,
0.));
#238817=CARTESIAN_POINT('Ctrl Pts',(-21.2840332184471,10.4391070306385,
0.));
#238818=CARTESIAN_POINT('Ctrl Pts',(-21.2982736231924,10.452931888387,0.));
#238819=CARTESIAN_POINT('Ctrl Pts',(-21.312555698873,10.4668723581768,0.));
#238820=CARTESIAN_POINT('Ctrl Pts',(-21.3268784926823,10.4809281365933,
0.));
#238821=CARTESIAN_POINT('Ctrl Pts',(-21.3412410642912,10.4950989223341,
0.));
#238822=CARTESIAN_POINT('Ctrl Pts',(-21.3556424855822,10.5093844161689,
0.));
#238823=CARTESIAN_POINT('Ctrl Pts',(-21.3700818403942,10.523784320906,0.));
#238824=CARTESIAN_POINT('Ctrl Pts',(-21.3845582242604,10.5382983413422,
0.));
#238825=CARTESIAN_POINT('Ctrl Pts',(-21.3990707441495,10.5529261842107,
0.));
#238826=CARTESIAN_POINT('Ctrl Pts',(-21.4136185181974,10.5676675581106,
0.));
#238827=CARTESIAN_POINT('Ctrl Pts',(-21.4282006754624,10.582522173457,0.));
#238828=CARTESIAN_POINT('Ctrl Pts',(-21.4428163557137,10.597489742462,0.));
#238829=CARTESIAN_POINT('Ctrl Pts',(-21.4574647092093,10.612569979096,0.));
#238830=CARTESIAN_POINT('Ctrl Pts',(-21.4721448964766,10.6277625990457,
0.));
#238831=CARTESIAN_POINT('Ctrl Pts',(-21.4868560880893,10.6430673196609,
0.));
#238832=CARTESIAN_POINT('Ctrl Pts',(-21.5015974644454,10.658483859894,0.));
#238833=CARTESIAN_POINT('Ctrl Pts',(-21.5163682155805,10.6740119402835,
0.));
#238834=CARTESIAN_POINT('Ctrl Pts',(-21.531167540981,10.689651282929,0.));
#238835=CARTESIAN_POINT('Ctrl Pts',(-21.5459946493955,10.7054016114571,
0.));
#238836=CARTESIAN_POINT('Ctrl Pts',(-21.5608487586467,10.7212626509816,
0.));
#238837=CARTESIAN_POINT('Ctrl Pts',(-21.5757290954372,10.7372341280468,
0.));
#238838=CARTESIAN_POINT('Ctrl Pts',(-21.5906348951745,10.7533157705943,
0.));
#238839=CARTESIAN_POINT('Ctrl Pts',(-21.6055654018179,10.7695073079554,
0.));
#238840=CARTESIAN_POINT('Ctrl Pts',(-21.6205198677176,10.7858084708262,
0.));
#238841=CARTESIAN_POINT('Ctrl Pts',(-21.6354975534557,10.8022189912369,
0.));
#238842=CARTESIAN_POINT('Ctrl Pts',(-21.6504977276864,10.8187386025135,
0.));
#238843=CARTESIAN_POINT('Ctrl Pts',(-21.6655196669727,10.835367039227,0.));
#238844=CARTESIAN_POINT('Ctrl Pts',(-21.6805626556461,10.8521040371832,
0.));
#238845=CARTESIAN_POINT('Ctrl Pts',(-21.6956259856667,10.8689493334093,
0.));
#238846=CARTESIAN_POINT('Ctrl Pts',(-21.7107089564822,10.8859026661292,
0.));
#238847=CARTESIAN_POINT('Ctrl Pts',(-21.7258108748874,10.9029637747341,
0.));
#238848=CARTESIAN_POINT('Ctrl Pts',(-21.74093105488,10.9201323997386,0.));
#238849=CARTESIAN_POINT('Ctrl Pts',(-21.7560688175252,10.9374082827446,
0.));
#238850=CARTESIAN_POINT('Ctrl Pts',(-21.7712234908468,10.9547911664457,
0.));
#238851=CARTESIAN_POINT('Ctrl Pts',(-21.7863944097143,10.9722807946157,
0.));
#238852=CARTESIAN_POINT('Ctrl Pts',(-21.8015809157302,10.9898769120913,
0.));
#238853=CARTESIAN_POINT('Ctrl Pts',(-21.8167823571168,11.0075792647477,
0.));
#238854=CARTESIAN_POINT('Ctrl Pts',(-21.8319980886033,11.0253875994598,
0.));
#238855=CARTESIAN_POINT('Ctrl Pts',(-21.8472274713103,11.0433016640808,
0.));
#238856=CARTESIAN_POINT('Ctrl Pts',(-21.8624698726319,11.0613212074364,
0.));
#238857=CARTESIAN_POINT('Ctrl Pts',(-21.8777246661191,11.0794459793058,
0.));
#238858=CARTESIAN_POINT('Ctrl Pts',(-21.8929912313608,11.0976757303944,
0.));
#238859=CARTESIAN_POINT('Ctrl Pts',(-21.9082689538687,11.1160102123024,
0.));
#238860=CARTESIAN_POINT('Ctrl Pts',(-21.9235572249518,11.134449177474,0.));
#238861=CARTESIAN_POINT('Ctrl Pts',(-21.9388554416437,11.1529923792002,
0.));
#238862=CARTESIAN_POINT('Ctrl Pts',(-21.9541630066504,11.1716395716375,
0.));
#238863=CARTESIAN_POINT('Ctrl Pts',(-21.9694793282913,11.1903905098109,
0.));
#238864=CARTESIAN_POINT('Ctrl Pts',(-21.9848038204439,11.2092449496125,
0.));
#238865=CARTESIAN_POINT('Ctrl Pts',(-22.0001359024839,11.2282026477897,
0.));
#238866=CARTESIAN_POINT('Ctrl Pts',(-22.0154749992364,11.2472633619276,
0.));
#238867=CARTESIAN_POINT('Ctrl Pts',(-22.0308205408351,11.2664268504207,
0.));
#238868=CARTESIAN_POINT('Ctrl Pts',(-22.046171962566,11.2856928724374,0.));
#238869=CARTESIAN_POINT('Ctrl Pts',(-22.0615287047179,11.3050611878771,
0.));
#238870=CARTESIAN_POINT('Ctrl Pts',(-22.0768902124267,11.3245315573168,
0.));
#238871=CARTESIAN_POINT('Ctrl Pts',(-22.0922559355293,11.3441037419553,
0.));
#238872=CARTESIAN_POINT('Ctrl Pts',(-22.1076253283978,11.3637775035367,
0.));
#238873=CARTESIAN_POINT('Ctrl Pts',(-22.1229978500185,11.3835526044256,
0.));
#238874=CARTESIAN_POINT('Ctrl Pts',(-22.1383729640963,11.4034288076908,
0.));
#238875=CARTESIAN_POINT('Ctrl Pts',(-22.1537501391486,11.4234058771742,
0.));
#238876=CARTESIAN_POINT('Ctrl Pts',(-22.1691288486096,11.443483577557,0.));
#238877=CARTESIAN_POINT('Ctrl Pts',(-22.184508570917,11.463661674411,0.));
#238878=CARTESIAN_POINT('Ctrl Pts',(-22.1998887896435,11.4839399342589,
0.));
#238879=CARTESIAN_POINT('Ctrl Pts',(-22.215268993102,11.504318124424,0.));
#238880=CARTESIAN_POINT('Ctrl Pts',(-22.2306486738899,11.5247960128476,
0.));
#238881=CARTESIAN_POINT('Ctrl Pts',(-22.2460273284653,11.545373367912,0.));
#238882=CARTESIAN_POINT('Ctrl Pts',(-22.2614044566898,11.5660499582403,
0.));
#238883=CARTESIAN_POINT('Ctrl Pts',(-22.2767795614349,11.5868255525189,
0.));
#238884=CARTESIAN_POINT('Ctrl Pts',(-22.2921521480358,11.6076999192359,
0.));
#238885=CARTESIAN_POINT('Ctrl Pts',(-22.3075217249049,11.6286728270011,
0.));
#238886=CARTESIAN_POINT('Ctrl Pts',(-22.3228878043976,11.6497440449858,
0.));
#238887=CARTESIAN_POINT('Ctrl Pts',(-22.3382499035618,11.6709133432986,
0.));
#238888=CARTESIAN_POINT('Ctrl Pts',(-22.3536075450028,11.6921804934056,
0.));
#238889=CARTESIAN_POINT('Ctrl Pts',(-22.3689602575492,11.7135452684532,
0.));
#238890=CARTESIAN_POINT('Ctrl Pts',(-22.3843075773905,11.7350074437961,
0.));
#238891=CARTESIAN_POINT('Ctrl Pts',(-22.39964904692,11.7565667964765,0.));
#238892=CARTESIAN_POINT('Ctrl Pts',(-22.4149842125018,11.7782231042041,
0.));
#238893=CARTESIAN_POINT('Ctrl Pts',(-22.4303126226468,11.7999761445175,
0.));
#238894=CARTESIAN_POINT('Ctrl Pts',(-22.4456338258738,11.8218256937889,
0.));
#238895=CARTESIAN_POINT('Ctrl Pts',(-22.4609473690469,11.8437715264487,
0.));
#238896=CARTESIAN_POINT('Ctrl Pts',(-22.4762527946694,11.8658134137018,
0.));
#238897=CARTESIAN_POINT('Ctrl Pts',(-22.4915496418472,11.8879511239941,
0.));
#238898=CARTESIAN_POINT('Ctrl Pts',(-22.5068374513958,11.9101844254555,
0.));
#238899=CARTESIAN_POINT('Ctrl Pts',(-22.5221157697869,11.9325130877801,
0.));
#238900=CARTESIAN_POINT('Ctrl Pts',(-22.5373841537299,11.9549368843996,
0.));
#238901=CARTESIAN_POINT('Ctrl Pts',(-22.5526421741159,11.9774555943496,
0.));
#238902=CARTESIAN_POINT('Ctrl Pts',(-22.5678894211194,12.0000690046697,
0.));
#238903=CARTESIAN_POINT('Ctrl Pts',(-22.5831255061306,12.0227769113132,
0.));
#238904=CARTESIAN_POINT('Ctrl Pts',(-22.5983500505675,12.0455791139135,
0.));
#238905=CARTESIAN_POINT('Ctrl Pts',(-22.613562676493,12.0684754113869,0.));
#238906=CARTESIAN_POINT('Ctrl Pts',(-22.628762996708,12.0914655972828,0.));
#238907=CARTESIAN_POINT('Ctrl Pts',(-22.6439506046611,12.1145494550384,
0.));
#238908=CARTESIAN_POINT('Ctrl Pts',(-22.6591250653942,12.1377267537141,
0.));
#238909=CARTESIAN_POINT('Ctrl Pts',(-22.6742859034891,12.1609972423088,
0.));
#238910=CARTESIAN_POINT('Ctrl Pts',(-22.6894326204959,12.1843606579246,
0.));
#238911=CARTESIAN_POINT('Ctrl Pts',(-22.7045647168659,12.2078167360267,
0.));
#238912=CARTESIAN_POINT('Ctrl Pts',(-22.7196817119299,12.2313652198047,
0.));
#238913=CARTESIAN_POINT('Ctrl Pts',(-22.7347831655251,12.2550058702389,
0.));
#238914=CARTESIAN_POINT('Ctrl Pts',(-22.7498686970096,12.2787384750747,
0.));
#238915=CARTESIAN_POINT('Ctrl Pts',(-22.7649380101154,12.3025628601812,
0.));
#238916=CARTESIAN_POINT('Ctrl Pts',(-22.7799908974947,12.3264788926108,
0.));
#238917=CARTESIAN_POINT('Ctrl Pts',(-22.7950272216959,12.3504864740361,
0.));
#238918=CARTESIAN_POINT('Ctrl Pts',(-22.8100469022632,12.3745855366772,
0.));
#238919=CARTESIAN_POINT('Ctrl Pts',(-22.8220493007353,12.393937937903,0.));
#238920=CARTESIAN_POINT('Ctrl Pts',(-22.8310435872852,12.4084933766366,
0.));
#238921=CARTESIAN_POINT('Ctrl Pts',(-22.8370364396497,12.4182152851867,
0.));
#238922=CARTESIAN_POINT('Ctrl Pts',(-22.8400320311648,12.4230808101438,
0.));
#238923=CARTESIAN_POINT('',(-22.8400320311648,12.4230808101438,12.));
#238924=CARTESIAN_POINT('Ctrl Pts',(-22.8400320311648,12.4230808101438,
12.));
#238925=CARTESIAN_POINT('Ctrl Pts',(-22.8370364396497,12.4182152851867,
12.));
#238926=CARTESIAN_POINT('Ctrl Pts',(-22.8310435872852,12.4084933766366,
12.));
#238927=CARTESIAN_POINT('Ctrl Pts',(-22.8220493007353,12.393937937903,12.));
#238928=CARTESIAN_POINT('Ctrl Pts',(-22.8100469022632,12.3745855366772,
12.));
#238929=CARTESIAN_POINT('Ctrl Pts',(-22.7950272216959,12.3504864740361,
12.));
#238930=CARTESIAN_POINT('Ctrl Pts',(-22.7799908974947,12.3264788926108,
12.));
#238931=CARTESIAN_POINT('Ctrl Pts',(-22.7649380101154,12.3025628601812,
12.));
#238932=CARTESIAN_POINT('Ctrl Pts',(-22.7498686970096,12.2787384750747,
12.));
#238933=CARTESIAN_POINT('Ctrl Pts',(-22.7347831655251,12.2550058702389,
12.));
#238934=CARTESIAN_POINT('Ctrl Pts',(-22.7196817119299,12.2313652198047,
12.));
#238935=CARTESIAN_POINT('Ctrl Pts',(-22.7045647168659,12.2078167360267,
12.));
#238936=CARTESIAN_POINT('Ctrl Pts',(-22.6894326204959,12.1843606579246,
12.));
#238937=CARTESIAN_POINT('Ctrl Pts',(-22.6742859034891,12.1609972423088,
12.));
#238938=CARTESIAN_POINT('Ctrl Pts',(-22.6591250653942,12.1377267537141,
12.));
#238939=CARTESIAN_POINT('Ctrl Pts',(-22.6439506046611,12.1145494550384,
12.));
#238940=CARTESIAN_POINT('Ctrl Pts',(-22.628762996708,12.0914655972828,12.));
#238941=CARTESIAN_POINT('Ctrl Pts',(-22.613562676493,12.0684754113869,12.));
#238942=CARTESIAN_POINT('Ctrl Pts',(-22.5983500505675,12.0455791139135,
12.));
#238943=CARTESIAN_POINT('Ctrl Pts',(-22.5831255061306,12.0227769113132,
12.));
#238944=CARTESIAN_POINT('Ctrl Pts',(-22.5678894211194,12.0000690046697,
12.));
#238945=CARTESIAN_POINT('Ctrl Pts',(-22.5526421741159,11.9774555943496,
12.));
#238946=CARTESIAN_POINT('Ctrl Pts',(-22.5373841537299,11.9549368843996,
12.));
#238947=CARTESIAN_POINT('Ctrl Pts',(-22.5221157697869,11.9325130877801,
12.));
#238948=CARTESIAN_POINT('Ctrl Pts',(-22.5068374513958,11.9101844254555,
12.));
#238949=CARTESIAN_POINT('Ctrl Pts',(-22.4915496418472,11.8879511239941,
12.));
#238950=CARTESIAN_POINT('Ctrl Pts',(-22.4762527946694,11.8658134137018,
12.));
#238951=CARTESIAN_POINT('Ctrl Pts',(-22.4609473690469,11.8437715264487,
12.));
#238952=CARTESIAN_POINT('Ctrl Pts',(-22.4456338258738,11.8218256937889,
12.));
#238953=CARTESIAN_POINT('Ctrl Pts',(-22.4303126226468,11.7999761445175,
12.));
#238954=CARTESIAN_POINT('Ctrl Pts',(-22.4149842125018,11.7782231042041,
12.));
#238955=CARTESIAN_POINT('Ctrl Pts',(-22.39964904692,11.7565667964765,12.));
#238956=CARTESIAN_POINT('Ctrl Pts',(-22.3843075773905,11.7350074437961,
12.));
#238957=CARTESIAN_POINT('Ctrl Pts',(-22.3689602575492,11.7135452684532,
12.));
#238958=CARTESIAN_POINT('Ctrl Pts',(-22.3536075450028,11.6921804934056,
12.));
#238959=CARTESIAN_POINT('Ctrl Pts',(-22.3382499035618,11.6709133432986,
12.));
#238960=CARTESIAN_POINT('Ctrl Pts',(-22.3228878043976,11.6497440449858,
12.));
#238961=CARTESIAN_POINT('Ctrl Pts',(-22.3075217249049,11.6286728270011,
12.));
#238962=CARTESIAN_POINT('Ctrl Pts',(-22.2921521480358,11.6076999192359,
12.));
#238963=CARTESIAN_POINT('Ctrl Pts',(-22.2767795614349,11.5868255525189,
12.));
#238964=CARTESIAN_POINT('Ctrl Pts',(-22.2614044566898,11.5660499582403,
12.));
#238965=CARTESIAN_POINT('Ctrl Pts',(-22.2460273284653,11.545373367912,12.));
#238966=CARTESIAN_POINT('Ctrl Pts',(-22.2306486738899,11.5247960128476,
12.));
#238967=CARTESIAN_POINT('Ctrl Pts',(-22.215268993102,11.504318124424,12.));
#238968=CARTESIAN_POINT('Ctrl Pts',(-22.1998887896435,11.4839399342589,
12.));
#238969=CARTESIAN_POINT('Ctrl Pts',(-22.184508570917,11.463661674411,12.));
#238970=CARTESIAN_POINT('Ctrl Pts',(-22.1691288486096,11.443483577557,12.));
#238971=CARTESIAN_POINT('Ctrl Pts',(-22.1537501391486,11.4234058771742,
12.));
#238972=CARTESIAN_POINT('Ctrl Pts',(-22.1383729640963,11.4034288076908,
12.));
#238973=CARTESIAN_POINT('Ctrl Pts',(-22.1229978500185,11.3835526044256,
12.));
#238974=CARTESIAN_POINT('Ctrl Pts',(-22.1076253283978,11.3637775035367,
12.));
#238975=CARTESIAN_POINT('Ctrl Pts',(-22.0922559355293,11.3441037419553,
12.));
#238976=CARTESIAN_POINT('Ctrl Pts',(-22.0768902124267,11.3245315573168,
12.));
#238977=CARTESIAN_POINT('Ctrl Pts',(-22.0615287047179,11.3050611878771,
12.));
#238978=CARTESIAN_POINT('Ctrl Pts',(-22.046171962566,11.2856928724374,12.));
#238979=CARTESIAN_POINT('Ctrl Pts',(-22.0308205408351,11.2664268504207,
12.));
#238980=CARTESIAN_POINT('Ctrl Pts',(-22.0154749992364,11.2472633619276,
12.));
#238981=CARTESIAN_POINT('Ctrl Pts',(-22.0001359024839,11.2282026477897,
12.));
#238982=CARTESIAN_POINT('Ctrl Pts',(-21.9848038204439,11.2092449496125,
12.));
#238983=CARTESIAN_POINT('Ctrl Pts',(-21.9694793282913,11.1903905098109,
12.));
#238984=CARTESIAN_POINT('Ctrl Pts',(-21.9541630066504,11.1716395716375,
12.));
#238985=CARTESIAN_POINT('Ctrl Pts',(-21.9388554416437,11.1529923792002,
12.));
#238986=CARTESIAN_POINT('Ctrl Pts',(-21.9235572249518,11.134449177474,12.));
#238987=CARTESIAN_POINT('Ctrl Pts',(-21.9082689538687,11.1160102123024,
12.));
#238988=CARTESIAN_POINT('Ctrl Pts',(-21.8929912313608,11.0976757303944,
12.));
#238989=CARTESIAN_POINT('Ctrl Pts',(-21.8777246661191,11.0794459793058,
12.));
#238990=CARTESIAN_POINT('Ctrl Pts',(-21.8624698726319,11.0613212074364,
12.));
#238991=CARTESIAN_POINT('Ctrl Pts',(-21.8472274713103,11.0433016640808,
12.));
#238992=CARTESIAN_POINT('Ctrl Pts',(-21.8319980886033,11.0253875994598,
12.));
#238993=CARTESIAN_POINT('Ctrl Pts',(-21.8167823571168,11.0075792647477,
12.));
#238994=CARTESIAN_POINT('Ctrl Pts',(-21.8015809157302,10.9898769120913,
12.));
#238995=CARTESIAN_POINT('Ctrl Pts',(-21.7863944097143,10.9722807946157,
12.));
#238996=CARTESIAN_POINT('Ctrl Pts',(-21.7712234908468,10.9547911664457,
12.));
#238997=CARTESIAN_POINT('Ctrl Pts',(-21.7560688175252,10.9374082827446,
12.));
#238998=CARTESIAN_POINT('Ctrl Pts',(-21.74093105488,10.9201323997386,12.));
#238999=CARTESIAN_POINT('Ctrl Pts',(-21.7258108748874,10.9029637747341,
12.));
#239000=CARTESIAN_POINT('Ctrl Pts',(-21.7107089564822,10.8859026661292,
12.));
#239001=CARTESIAN_POINT('Ctrl Pts',(-21.6956259856667,10.8689493334093,
12.));
#239002=CARTESIAN_POINT('Ctrl Pts',(-21.6805626556461,10.8521040371832,
12.));
#239003=CARTESIAN_POINT('Ctrl Pts',(-21.6655196669727,10.835367039227,12.));
#239004=CARTESIAN_POINT('Ctrl Pts',(-21.6504977276864,10.8187386025135,
12.));
#239005=CARTESIAN_POINT('Ctrl Pts',(-21.6354975534557,10.8022189912369,
12.));
#239006=CARTESIAN_POINT('Ctrl Pts',(-21.6205198677176,10.7858084708262,
12.));
#239007=CARTESIAN_POINT('Ctrl Pts',(-21.6055654018179,10.7695073079554,
12.));
#239008=CARTESIAN_POINT('Ctrl Pts',(-21.5906348951745,10.7533157705943,
12.));
#239009=CARTESIAN_POINT('Ctrl Pts',(-21.5757290954372,10.7372341280468,
12.));
#239010=CARTESIAN_POINT('Ctrl Pts',(-21.5608487586467,10.7212626509816,
12.));
#239011=CARTESIAN_POINT('Ctrl Pts',(-21.5459946493955,10.7054016114571,
12.));
#239012=CARTESIAN_POINT('Ctrl Pts',(-21.531167540981,10.689651282929,12.));
#239013=CARTESIAN_POINT('Ctrl Pts',(-21.5163682155805,10.6740119402835,
12.));
#239014=CARTESIAN_POINT('Ctrl Pts',(-21.5015974644454,10.658483859894,12.));
#239015=CARTESIAN_POINT('Ctrl Pts',(-21.4868560880893,10.6430673196609,
12.));
#239016=CARTESIAN_POINT('Ctrl Pts',(-21.4721448964766,10.6277625990457,
12.));
#239017=CARTESIAN_POINT('Ctrl Pts',(-21.4574647092093,10.612569979096,12.));
#239018=CARTESIAN_POINT('Ctrl Pts',(-21.4428163557137,10.597489742462,12.));
#239019=CARTESIAN_POINT('Ctrl Pts',(-21.4282006754624,10.582522173457,12.));
#239020=CARTESIAN_POINT('Ctrl Pts',(-21.4136185181974,10.5676675581106,
12.));
#239021=CARTESIAN_POINT('Ctrl Pts',(-21.3990707441495,10.5529261842107,
12.));
#239022=CARTESIAN_POINT('Ctrl Pts',(-21.3845582242604,10.5382983413422,
12.));
#239023=CARTESIAN_POINT('Ctrl Pts',(-21.3700818403942,10.523784320906,12.));
#239024=CARTESIAN_POINT('Ctrl Pts',(-21.3556424855822,10.5093844161689,
12.));
#239025=CARTESIAN_POINT('Ctrl Pts',(-21.3412410642912,10.4950989223341,
12.));
#239026=CARTESIAN_POINT('Ctrl Pts',(-21.3268784926823,10.4809281365933,
12.));
#239027=CARTESIAN_POINT('Ctrl Pts',(-21.312555698873,10.4668723581768,12.));
#239028=CARTESIAN_POINT('Ctrl Pts',(-21.2982736231924,10.452931888387,12.));
#239029=CARTESIAN_POINT('Ctrl Pts',(-21.2840332184471,10.4391070306385,
12.));
#239030=CARTESIAN_POINT('Ctrl Pts',(-21.2698354502391,10.4253980905394,
12.));
#239031=CARTESIAN_POINT('Ctrl Pts',(-21.2556812972741,10.4118053759584,
12.));
#239032=CARTESIAN_POINT('Ctrl Pts',(-21.2415717516713,10.3983291970846,
12.));
#239033=CARTESIAN_POINT('Ctrl Pts',(-21.2275078192708,10.384969866479,12.));
#239034=CARTESIAN_POINT('Ctrl Pts',(-21.2134905199359,10.3717276991137,
12.));
#239035=CARTESIAN_POINT('Ctrl Pts',(-21.1995208879205,10.3586030124595,
12.));
#239036=CARTESIAN_POINT('Ctrl Pts',(-21.1855999722427,10.3455961265706,
12.));
#239037=CARTESIAN_POINT('Ctrl Pts',(-21.1717288370512,10.3327073641574,
12.));
#239038=CARTESIAN_POINT('Ctrl Pts',(-21.1579085619959,10.3199370506541,
12.));
#239039=CARTESIAN_POINT('Ctrl Pts',(-21.1441402425831,10.307285514268,12.));
#239040=CARTESIAN_POINT('Ctrl Pts',(-21.130424990599,10.2947530860714,12.));
#239041=CARTESIAN_POINT('Ctrl Pts',(-21.1167639345623,10.2823401001067,
12.));
#239042=CARTESIAN_POINT('Ctrl Pts',(-21.1031582201625,10.2700468934743,
12.));
#239043=CARTESIAN_POINT('Ctrl Pts',(-21.0896090107066,10.2578738064183,
12.));
#239044=CARTESIAN_POINT('Ctrl Pts',(-21.0761174875448,10.2458211823915,
12.));
#239045=CARTESIAN_POINT('Ctrl Pts',(-21.0626848505665,10.233889368157,12.));
#239046=CARTESIAN_POINT('Ctrl Pts',(-21.0493123187483,10.2220787139157,
12.));
#239047=CARTESIAN_POINT('Ctrl Pts',(-21.0360011306814,10.2103895734123,
12.));
#239048=CARTESIAN_POINT('Ctrl Pts',(-21.0227525451107,10.1988223040425,
12.));
#239049=CARTESIAN_POINT('Ctrl Pts',(-21.0095678414486,10.1873772669358,
12.));
#239050=CARTESIAN_POINT('Ctrl Pts',(-20.9964483203685,10.1760548270765,
12.));
#239051=CARTESIAN_POINT('Ctrl Pts',(-20.9833953044737,10.1648553534567,
12.));
#239052=CARTESIAN_POINT('Ctrl Pts',(-20.970410138937,10.1537792192065,12.));
#239053=CARTESIAN_POINT('Ctrl Pts',(-20.9574941921591,10.1428268017257,
12.));
#239054=CARTESIAN_POINT('Ctrl Pts',(-20.944648856393,10.1319984827909,12.));
#239055=CARTESIAN_POINT('Ctrl Pts',(-20.931875548473,10.1212946487057,12.));
#239056=CARTESIAN_POINT('Ctrl Pts',(-20.9191757106266,10.1107156904836,
12.));
#239057=CARTESIAN_POINT('Ctrl Pts',(-20.9065508112556,10.1002620040076,
12.));
#239058=CARTESIAN_POINT('Ctrl Pts',(-20.8940023457371,10.0899339901916,
12.));
#239059=CARTESIAN_POINT('Ctrl Pts',(-20.8815318371844,10.0797320551154,
12.));
#239060=CARTESIAN_POINT('Ctrl Pts',(-20.8691408373705,10.0696566102219,
12.));
#239061=CARTESIAN_POINT('Ctrl Pts',(-20.856830927732,10.0597080725375,12.));
#239062=CARTESIAN_POINT('Ctrl Pts',(-20.8446037203402,10.0498868648733,
12.));
#239063=CARTESIAN_POINT('Ctrl Pts',(-20.8324608588906,10.0401934160234,
12.));
#239064=CARTESIAN_POINT('Ctrl Pts',(-20.8204040196599,10.0306281609435,
12.));
#239065=CARTESIAN_POINT('Ctrl Pts',(-20.8084349126885,10.0211915410095,
12.));
#239066=CARTESIAN_POINT('Ctrl Pts',(-20.7965552829907,10.0118840042786,
12.));
#239067=CARTESIAN_POINT('Ctrl Pts',(-20.7847669117568,10.0027060057389,
12.));
#239068=CARTESIAN_POINT('Ctrl Pts',(-20.7730716175417,9.99365800754638,
12.));
#239069=CARTESIAN_POINT('Ctrl Pts',(-20.7614712574989,9.98474047926846,
12.));
#239070=CARTESIAN_POINT('Ctrl Pts',(-20.7499677289625,9.97595389823461,
12.));
#239071=CARTESIAN_POINT('Ctrl Pts',(-20.7385629709795,9.96729874986198,
12.));
#239072=CARTESIAN_POINT('Ctrl Pts',(-20.7272589658752,9.95877552798403,
12.));
#239073=CARTESIAN_POINT('Ctrl Pts',(-20.716057740758,9.95038473514962,12.));
#239074=CARTESIAN_POINT('Ctrl Pts',(-20.7049613692237,9.94212688298251,
12.));
#239075=CARTESIAN_POINT('Ctrl Pts',(-20.6939719732485,9.93400249259736,
12.));
#239076=CARTESIAN_POINT('Ctrl Pts',(-20.6830917250255,9.9260120949875,12.));
#239077=CARTESIAN_POINT('Ctrl Pts',(-20.6723228488262,9.91815623141284,
12.));
#239078=CARTESIAN_POINT('Ctrl Pts',(-20.6616676228315,9.91043545377004,
12.));
#239079=CARTESIAN_POINT('Ctrl Pts',(-20.6511283817415,9.90285032516696,
12.));
#239080=CARTESIAN_POINT('Ctrl Pts',(-20.6407075193977,9.89540142049124,
12.));
#239081=CARTESIAN_POINT('Ctrl Pts',(-20.6304074914086,9.88808932697305,
12.));
#239082=CARTESIAN_POINT('Ctrl Pts',(-20.6202308177472,9.88091464472669,
12.));
#239083=CARTESIAN_POINT('Ctrl Pts',(-20.6101800854491,9.87387798732944,
12.));
#239084=CARTESIAN_POINT('Ctrl Pts',(-20.6002579513696,9.86697998242612,
12.));
#239085=CARTESIAN_POINT('Ctrl Pts',(-20.5904671449754,9.86022127232749,
12.));
#239086=CARTESIAN_POINT('Ctrl Pts',(-20.580810471002,9.85360251457004,12.));
#239087=CARTESIAN_POINT('Ctrl Pts',(-20.5712908125145,9.84712438256308,
12.));
#239088=CARTESIAN_POINT('Ctrl Pts',(-20.5619111362406,9.84078756677589,
12.));
#239089=CARTESIAN_POINT('Ctrl Pts',(-20.5526744976461,9.83459277585321,
12.));
#239090=CARTESIAN_POINT('Ctrl Pts',(-20.5435840460717,9.82854073773857,
12.));
#239091=CARTESIAN_POINT('Ctrl Pts',(-20.534643029951,9.82263220080328,12.));
#239092=CARTESIAN_POINT('Ctrl Pts',(-20.5258548000625,9.81686793455918,
12.));
#239093=CARTESIAN_POINT('Ctrl Pts',(-20.5172228122839,9.81124873025278,
12.));
#239094=CARTESIAN_POINT('Ctrl Pts',(-20.5087506310507,9.80577540161103,
12.));
#239095=CARTESIAN_POINT('Ctrl Pts',(-20.500441931211,9.80044878520967,12.));
#239096=CARTESIAN_POINT('Ctrl Pts',(-20.4923005087945,9.79526974288344,
12.));
#239097=CARTESIAN_POINT('Ctrl Pts',(-20.4843302955329,9.7902391649866,12.));
#239098=CARTESIAN_POINT('Ctrl Pts',(-20.4765353711585,9.78535797314162,
12.));
#239099=CARTESIAN_POINT('Ctrl Pts',(-20.4689199790668,9.78062712373313,
12.));
#239100=CARTESIAN_POINT('Ctrl Pts',(-20.4614885274973,9.77604760815523,
12.));
#239101=CARTESIAN_POINT('Ctrl Pts',(-20.4542455817527,9.7716204510407,12.));
#239102=CARTESIAN_POINT('Ctrl Pts',(-20.447195862298,9.76734670980897,12.));
#239103=CARTESIAN_POINT('Ctrl Pts',(-20.4403442329401,9.76322747195502,
12.));
#239104=CARTESIAN_POINT('Ctrl Pts',(-20.4336957355474,9.7592638628993,12.));
#239105=CARTESIAN_POINT('Ctrl Pts',(-20.4272556476629,9.75545705902416,
12.));
#239106=CARTESIAN_POINT('Ctrl Pts',(-20.4210295275818,9.75180829786433,
12.));
#239107=CARTESIAN_POINT('Ctrl Pts',(-20.4150232777393,9.74831889242175,
12.));
#239108=CARTESIAN_POINT('Ctrl Pts',(-20.4092430879861,9.74499021838536,
12.));
#239109=CARTESIAN_POINT('Ctrl Pts',(-20.4036953576549,9.74182369656272,
12.));
#239110=CARTESIAN_POINT('Ctrl Pts',(-20.3983866213331,9.73882077613206,
12.));
#239111=CARTESIAN_POINT('Ctrl Pts',(-20.3933234845646,9.7359829201425,12.));
#239112=CARTESIAN_POINT('Ctrl Pts',(-20.3885129129912,9.73331167102812,
12.));
#239113=CARTESIAN_POINT('Ctrl Pts',(-20.3839624556742,9.73080870123726,
12.));
#239114=CARTESIAN_POINT('Ctrl Pts',(-20.3796805893304,9.72847589116533,
12.));
#239115=CARTESIAN_POINT('Ctrl Pts',(-20.3756766651952,9.72631531732871,
12.));
#239116=CARTESIAN_POINT('Ctrl Pts',(-20.371960235676,9.72432910043193,12.));
#239117=CARTESIAN_POINT('Ctrl Pts',(-20.3685406190576,9.72251930722504,
12.));
#239118=CARTESIAN_POINT('Ctrl Pts',(-20.3654261611055,9.72088778381102,
12.));
#239119=CARTESIAN_POINT('Ctrl Pts',(-20.362625691398,9.71943648548114,12.));
#239120=CARTESIAN_POINT('Ctrl Pts',(-20.3601498764344,9.71816778327999,
12.));
#239121=CARTESIAN_POINT('Ctrl Pts',(-20.3580133103357,9.71708493723061,
12.));
#239122=CARTESIAN_POINT('Ctrl Pts',(-20.3562337557875,9.71619192554147,
12.));
#239123=CARTESIAN_POINT('Ctrl Pts',(-20.3548282742361,9.71549257088175,
12.));
#239124=CARTESIAN_POINT('Ctrl Pts',(-20.3538098605706,9.71498978052101,
12.));
#239125=CARTESIAN_POINT('Ctrl Pts',(-20.3533097561886,9.71474590350791,
12.));
#239126=CARTESIAN_POINT('Ctrl Pts',(-20.3531126095522,9.71465227853122,
12.));
#239127=CARTESIAN_POINT('Ctrl Pts',(-20.353060251684,9.71462954053074,12.));
#239128=CARTESIAN_POINT('Ctrl Pts',(-20.353053841303,9.71462809124917,12.));
#239129=CARTESIAN_POINT('',(-22.8400320311648,12.4230808101438,0.));
#239130=CARTESIAN_POINT('Origin',(-16.3449727195352,13.9675290154577,0.));
#239131=CARTESIAN_POINT('',(-17.1452095830633,14.6513681262571,12.));
#239132=CARTESIAN_POINT('',(-8.17248635976757,6.98376450772883,12.));
#239133=CARTESIAN_POINT('',(-17.1452095830633,14.6513681262571,0.));
#239134=CARTESIAN_POINT('',(-17.1452095830633,14.6513681262571,0.));
#239135=CARTESIAN_POINT('',(-8.17248635976757,6.98376450772883,0.));
#239136=CARTESIAN_POINT('Ctrl Pts',(-22.1787195904339,13.5685075571671,
0.));
#239137=CARTESIAN_POINT('Ctrl Pts',(-22.1787195904339,13.5685075571671,
12.));
#239138=CARTESIAN_POINT('Ctrl Pts',(-22.1730081264583,13.5683460612913,
0.));
#239139=CARTESIAN_POINT('Ctrl Pts',(-22.1730081264583,13.5683460612913,
12.));
#239140=CARTESIAN_POINT('Ctrl Pts',(-22.1615922804939,13.5680170531724,
0.));
#239141=CARTESIAN_POINT('Ctrl Pts',(-22.1615922804939,13.5680170531724,
12.));
#239142=CARTESIAN_POINT('Ctrl Pts',(-22.1444897575076,13.5675054918922,
0.));
#239143=CARTESIAN_POINT('Ctrl Pts',(-22.1444897575076,13.5675054918922,
12.));
#239144=CARTESIAN_POINT('Ctrl Pts',(-22.1217288871823,13.5667873105179,
0.));
#239145=CARTESIAN_POINT('Ctrl Pts',(-22.1217288871823,13.5667873105179,
12.));
#239146=CARTESIAN_POINT('Ctrl Pts',(-22.0933486464442,13.5658294169106,
0.));
#239147=CARTESIAN_POINT('Ctrl Pts',(-22.0933486464442,13.5658294169106,
12.));
#239148=CARTESIAN_POINT('Ctrl Pts',(-22.0650393089492,13.5648113688894,
0.));
#239149=CARTESIAN_POINT('Ctrl Pts',(-22.0650393089492,13.5648113688894,
12.));
#239150=CARTESIAN_POINT('Ctrl Pts',(-22.0368009736227,13.5637332022393,
0.));
#239151=CARTESIAN_POINT('Ctrl Pts',(-22.0368009736227,13.5637332022393,
12.));
#239152=CARTESIAN_POINT('Ctrl Pts',(-22.0086337943431,13.5625949868313,
0.));
#239153=CARTESIAN_POINT('Ctrl Pts',(-22.0086337943431,13.5625949868313,
12.));
#239154=CARTESIAN_POINT('Ctrl Pts',(-21.9805379899192,13.5613968357589,
0.));
#239155=CARTESIAN_POINT('Ctrl Pts',(-21.9805379899192,13.5613968357589,
12.));
#239156=CARTESIAN_POINT('Ctrl Pts',(-21.9525138592862,13.5601389185315,
0.));
#239157=CARTESIAN_POINT('Ctrl Pts',(-21.9525138592862,13.5601389185315,
12.));
#239158=CARTESIAN_POINT('Ctrl Pts',(-21.9245617765827,13.5588214586672,
0.));
#239159=CARTESIAN_POINT('Ctrl Pts',(-21.9245617765827,13.5588214586672,
12.));
#239160=CARTESIAN_POINT('Ctrl Pts',(-21.8966821688876,13.5574447178484,
0.));
#239161=CARTESIAN_POINT('Ctrl Pts',(-21.8966821688876,13.5574447178484,
12.));
#239162=CARTESIAN_POINT('Ctrl Pts',(-21.8688754989401,13.5560089839426,
0.));
#239163=CARTESIAN_POINT('Ctrl Pts',(-21.8688754989401,13.5560089839426,
12.));
#239164=CARTESIAN_POINT('Ctrl Pts',(-21.841142245609,13.5545145573048,0.));
#239165=CARTESIAN_POINT('Ctrl Pts',(-21.841142245609,13.5545145573048,12.));
#239166=CARTESIAN_POINT('Ctrl Pts',(-21.8134828857963,13.5529617381569,
0.));
#239167=CARTESIAN_POINT('Ctrl Pts',(-21.8134828857963,13.5529617381569,
12.));
#239168=CARTESIAN_POINT('Ctrl Pts',(-21.7858978745848,13.5513508127232,
0.));
#239169=CARTESIAN_POINT('Ctrl Pts',(-21.7858978745848,13.5513508127232,
12.));
#239170=CARTESIAN_POINT('Ctrl Pts',(-21.7583876294532,13.5496820422186,
0.));
#239171=CARTESIAN_POINT('Ctrl Pts',(-21.7583876294532,13.5496820422186,
12.));
#239172=CARTESIAN_POINT('Ctrl Pts',(-21.730952541226,13.5479556704457,0.));
#239173=CARTESIAN_POINT('Ctrl Pts',(-21.730952541226,13.5479556704457,12.));
#239174=CARTESIAN_POINT('Ctrl Pts',(-21.7035929822939,13.546171929503,0.));
#239175=CARTESIAN_POINT('Ctrl Pts',(-21.7035929822939,13.546171929503,12.));
#239176=CARTESIAN_POINT('Ctrl Pts',(-21.676309315769,13.5443310461516,0.));
#239177=CARTESIAN_POINT('Ctrl Pts',(-21.676309315769,13.5443310461516,12.));
#239178=CARTESIAN_POINT('Ctrl Pts',(-21.6491019044647,13.5424332480698,
0.));
#239179=CARTESIAN_POINT('Ctrl Pts',(-21.6491019044647,13.5424332480698,
12.));
#239180=CARTESIAN_POINT('Ctrl Pts',(-21.6219711193951,13.5404787697798,
0.));
#239181=CARTESIAN_POINT('Ctrl Pts',(-21.6219711193951,13.5404787697798,
12.));
#239182=CARTESIAN_POINT('Ctrl Pts',(-21.5949173499022,13.5384678597206,
0.));
#239183=CARTESIAN_POINT('Ctrl Pts',(-21.5949173499022,13.5384678597206,
12.));
#239184=CARTESIAN_POINT('Ctrl Pts',(-21.5679410019011,13.5364007790292,
0.));
#239185=CARTESIAN_POINT('Ctrl Pts',(-21.5679410019011,13.5364007790292,
12.));
#239186=CARTESIAN_POINT('Ctrl Pts',(-21.5410424932511,13.5342777983225,
0.));
#239187=CARTESIAN_POINT('Ctrl Pts',(-21.5410424932511,13.5342777983225,
12.));
#239188=CARTESIAN_POINT('Ctrl Pts',(-21.5142222501671,13.5320991952145,
0.));
#239189=CARTESIAN_POINT('Ctrl Pts',(-21.5142222501671,13.5320991952145,
12.));
#239190=CARTESIAN_POINT('Ctrl Pts',(-21.487480703047,13.5298652514357,0.));
#239191=CARTESIAN_POINT('Ctrl Pts',(-21.487480703047,13.5298652514357,12.));
#239192=CARTESIAN_POINT('Ctrl Pts',(-21.4608182828695,13.5275762503553,
0.));
#239193=CARTESIAN_POINT('Ctrl Pts',(-21.4608182828695,13.5275762503553,
12.));
#239194=CARTESIAN_POINT('Ctrl Pts',(-21.4342354165254,13.5252324737795,
0.));
#239195=CARTESIAN_POINT('Ctrl Pts',(-21.4342354165254,13.5252324737795,
12.));
#239196=CARTESIAN_POINT('Ctrl Pts',(-21.4077325259318,13.5228342013508,
0.));
#239197=CARTESIAN_POINT('Ctrl Pts',(-21.4077325259318,13.5228342013508,
12.));
#239198=CARTESIAN_POINT('Ctrl Pts',(-21.3813100304967,13.5203817122496,
0.));
#239199=CARTESIAN_POINT('Ctrl Pts',(-21.3813100304967,13.5203817122496,
12.));
#239200=CARTESIAN_POINT('Ctrl Pts',(-21.3549683486219,13.5178752862461,
0.));
#239201=CARTESIAN_POINT('Ctrl Pts',(-21.3549683486219,13.5178752862461,
12.));
#239202=CARTESIAN_POINT('Ctrl Pts',(-21.328707899634,13.5153152050554,0.));
#239203=CARTESIAN_POINT('Ctrl Pts',(-21.328707899634,13.5153152050554,12.));
#239204=CARTESIAN_POINT('Ctrl Pts',(-21.3025291054236,13.5127017534972,
0.));
#239205=CARTESIAN_POINT('Ctrl Pts',(-21.3025291054236,13.5127017534972,
12.));
#239206=CARTESIAN_POINT('Ctrl Pts',(-21.2764323924442,13.5100352209207,
0.));
#239207=CARTESIAN_POINT('Ctrl Pts',(-21.2764323924442,13.5100352209207,
12.));
#239208=CARTESIAN_POINT('Ctrl Pts',(-21.2504181927429,13.5073159019454,
0.));
#239209=CARTESIAN_POINT('Ctrl Pts',(-21.2504181927429,13.5073159019454,
12.));
#239210=CARTESIAN_POINT('Ctrl Pts',(-21.224486942933,13.5045440957404,0.));
#239211=CARTESIAN_POINT('Ctrl Pts',(-21.224486942933,13.5045440957404,12.));
#239212=CARTESIAN_POINT('Ctrl Pts',(-21.1986390835825,13.5017201056088,
0.));
#239213=CARTESIAN_POINT('Ctrl Pts',(-21.1986390835825,13.5017201056088,
12.));
#239214=CARTESIAN_POINT('Ctrl Pts',(-21.1728750584173,13.4988442384491,
0.));
#239215=CARTESIAN_POINT('Ctrl Pts',(-21.1728750584173,13.4988442384491,
12.));
#239216=CARTESIAN_POINT('Ctrl Pts',(-21.1471953136209,13.4959168042934,
0.));
#239217=CARTESIAN_POINT('Ctrl Pts',(-21.1471953136209,13.4959168042934,
12.));
#239218=CARTESIAN_POINT('Ctrl Pts',(-21.1216002970209,13.4929381157778,
0.));
#239219=CARTESIAN_POINT('Ctrl Pts',(-21.1216002970209,13.4929381157778,
12.));
#239220=CARTESIAN_POINT('Ctrl Pts',(-21.0960904575048,13.4899084877718,
0.));
#239221=CARTESIAN_POINT('Ctrl Pts',(-21.0960904575048,13.4899084877718,
12.));
#239222=CARTESIAN_POINT('Ctrl Pts',(-21.0706662455202,13.4868282377191,
0.));
#239223=CARTESIAN_POINT('Ctrl Pts',(-21.0706662455202,13.4868282377191,
12.));
#239224=CARTESIAN_POINT('Ctrl Pts',(-21.0453281134247,13.4836976858912,
0.));
#239225=CARTESIAN_POINT('Ctrl Pts',(-21.0453281134247,13.4836976858912,
12.));
#239226=CARTESIAN_POINT('Ctrl Pts',(-21.0200765158885,13.4805171556822,
0.));
#239227=CARTESIAN_POINT('Ctrl Pts',(-21.0200765158885,13.4805171556822,
12.));
#239228=CARTESIAN_POINT('Ctrl Pts',(-20.9949119102592,13.4772869738879,
0.));
#239229=CARTESIAN_POINT('Ctrl Pts',(-20.9949119102592,13.4772869738879,
12.));
#239230=CARTESIAN_POINT('Ctrl Pts',(-20.9698347569476,13.4740074710087,
0.));
#239231=CARTESIAN_POINT('Ctrl Pts',(-20.9698347569476,13.4740074710087,
12.));
#239232=CARTESIAN_POINT('Ctrl Pts',(-20.9448455197557,13.4706789815166,
0.));
#239233=CARTESIAN_POINT('Ctrl Pts',(-20.9448455197557,13.4706789815166,
12.));
#239234=CARTESIAN_POINT('Ctrl Pts',(-20.9199446657584,13.4673018437718,
0.));
#239235=CARTESIAN_POINT('Ctrl Pts',(-20.9199446657584,13.4673018437718,
12.));
#239236=CARTESIAN_POINT('Ctrl Pts',(-20.8951326652158,13.4638763999725,
0.));
#239237=CARTESIAN_POINT('Ctrl Pts',(-20.8951326652158,13.4638763999725,
12.));
#239238=CARTESIAN_POINT('Ctrl Pts',(-20.8704099914641,13.4604029960983,
0.));
#239239=CARTESIAN_POINT('Ctrl Pts',(-20.8704099914641,13.4604029960983,
12.));
#239240=CARTESIAN_POINT('Ctrl Pts',(-20.8457771208082,13.4568819818631,
0.));
#239241=CARTESIAN_POINT('Ctrl Pts',(-20.8457771208082,13.4568819818631,
12.));
#239242=CARTESIAN_POINT('Ctrl Pts',(-20.821234532398,13.4533137106667,0.));
#239243=CARTESIAN_POINT('Ctrl Pts',(-20.821234532398,13.4533137106667,12.));
#239244=CARTESIAN_POINT('Ctrl Pts',(-20.7967827081227,13.4496985395637,
0.));
#239245=CARTESIAN_POINT('Ctrl Pts',(-20.7967827081227,13.4496985395637,
12.));
#239246=CARTESIAN_POINT('Ctrl Pts',(-20.7724221327608,13.4460368293688,
0.));
#239247=CARTESIAN_POINT('Ctrl Pts',(-20.7724221327608,13.4460368293688,
12.));
#239248=CARTESIAN_POINT('Ctrl Pts',(-20.7481532941013,13.4423289447561,
0.));
#239249=CARTESIAN_POINT('Ctrl Pts',(-20.7481532941013,13.4423289447561,
12.));
#239250=CARTESIAN_POINT('Ctrl Pts',(-20.7239766830675,13.4385752543663,
0.));
#239251=CARTESIAN_POINT('Ctrl Pts',(-20.7239766830675,13.4385752543663,
12.));
#239252=CARTESIAN_POINT('Ctrl Pts',(-20.6998927938288,13.4347761309154,
0.));
#239253=CARTESIAN_POINT('Ctrl Pts',(-20.6998927938288,13.4347761309154,
12.));
#239254=CARTESIAN_POINT('Ctrl Pts',(-20.6759021239103,13.4309319513119,
0.));
#239255=CARTESIAN_POINT('Ctrl Pts',(-20.6759021239103,13.4309319513119,
12.));
#239256=CARTESIAN_POINT('Ctrl Pts',(-20.6520051742869,13.4270430967651,
0.));
#239257=CARTESIAN_POINT('Ctrl Pts',(-20.6520051742869,13.4270430967651,
12.));
#239258=CARTESIAN_POINT('Ctrl Pts',(-20.6282024494237,13.4231099528179,
0.));
#239259=CARTESIAN_POINT('Ctrl Pts',(-20.6282024494237,13.4231099528179,
12.));
#239260=CARTESIAN_POINT('Ctrl Pts',(-20.6044944573153,13.4191329093932,
0.));
#239261=CARTESIAN_POINT('Ctrl Pts',(-20.6044944573153,13.4191329093932,
12.));
#239262=CARTESIAN_POINT('Ctrl Pts',(-20.5808817095155,13.4151123608411,
0.));
#239263=CARTESIAN_POINT('Ctrl Pts',(-20.5808817095155,13.4151123608411,
12.));
#239264=CARTESIAN_POINT('Ctrl Pts',(-20.5573647211639,13.4110487059912,
0.));
#239265=CARTESIAN_POINT('Ctrl Pts',(-20.5573647211639,13.4110487059912,
12.));
#239266=CARTESIAN_POINT('Ctrl Pts',(-20.5339440109956,13.4069423482076,
0.));
#239267=CARTESIAN_POINT('Ctrl Pts',(-20.5339440109956,13.4069423482076,
12.));
#239268=CARTESIAN_POINT('Ctrl Pts',(-20.5106201013753,13.4027936954529,
0.));
#239269=CARTESIAN_POINT('Ctrl Pts',(-20.5106201013753,13.4027936954529,
12.));
#239270=CARTESIAN_POINT('Ctrl Pts',(-20.487393518404,13.3986031603716,0.));
#239271=CARTESIAN_POINT('Ctrl Pts',(-20.487393518404,13.3986031603716,12.));
#239272=CARTESIAN_POINT('Ctrl Pts',(-20.4642647920038,13.3943711603739,
0.));
#239273=CARTESIAN_POINT('Ctrl Pts',(-20.4642647920038,13.3943711603739,
12.));
#239274=CARTESIAN_POINT('Ctrl Pts',(-20.4412344560008,13.3900981177255,
0.));
#239275=CARTESIAN_POINT('Ctrl Pts',(-20.4412344560008,13.3900981177255,
12.));
#239276=CARTESIAN_POINT('Ctrl Pts',(-20.4183030482002,13.3857844596387,
0.));
#239277=CARTESIAN_POINT('Ctrl Pts',(-20.4183030482002,13.3857844596387,
12.));
#239278=CARTESIAN_POINT('Ctrl Pts',(-20.3954711104502,13.3814306183719,
0.));
#239279=CARTESIAN_POINT('Ctrl Pts',(-20.3954711104502,13.3814306183719,
12.));
#239280=CARTESIAN_POINT('Ctrl Pts',(-20.3727391887184,13.3770370313188,
0.));
#239281=CARTESIAN_POINT('Ctrl Pts',(-20.3727391887184,13.3770370313188,
12.));
#239282=CARTESIAN_POINT('Ctrl Pts',(-20.3501078331814,13.3726041410867,
0.));
#239283=CARTESIAN_POINT('Ctrl Pts',(-20.3501078331814,13.3726041410867,
12.));
#239284=CARTESIAN_POINT('Ctrl Pts',(-20.3275775983029,13.3681323955826,
0.));
#239285=CARTESIAN_POINT('Ctrl Pts',(-20.3275775983029,13.3681323955826,
12.));
#239286=CARTESIAN_POINT('Ctrl Pts',(-20.3051490429048,13.3636222481016,
0.));
#239287=CARTESIAN_POINT('Ctrl Pts',(-20.3051490429048,13.3636222481016,
12.));
#239288=CARTESIAN_POINT('Ctrl Pts',(-20.2828227302339,13.3590741574195,
0.));
#239289=CARTESIAN_POINT('Ctrl Pts',(-20.2828227302339,13.3590741574195,
12.));
#239290=CARTESIAN_POINT('Ctrl Pts',(-20.2605992280122,13.3544885878889,
0.));
#239291=CARTESIAN_POINT('Ctrl Pts',(-20.2605992280122,13.3544885878889,
12.));
#239292=CARTESIAN_POINT('Ctrl Pts',(-20.2384791085359,13.3498660095386,
0.));
#239293=CARTESIAN_POINT('Ctrl Pts',(-20.2384791085359,13.3498660095386,
12.));
#239294=CARTESIAN_POINT('Ctrl Pts',(-20.216462948786,13.3452068981766,0.));
#239295=CARTESIAN_POINT('Ctrl Pts',(-20.216462948786,13.3452068981766,12.));
#239296=CARTESIAN_POINT('Ctrl Pts',(-20.1945513305235,13.3405117354971,
0.));
#239297=CARTESIAN_POINT('Ctrl Pts',(-20.1945513305235,13.3405117354971,
12.));
#239298=CARTESIAN_POINT('Ctrl Pts',(-20.1727448403817,13.3357810091903,
0.));
#239299=CARTESIAN_POINT('Ctrl Pts',(-20.1727448403817,13.3357810091903,
12.));
#239300=CARTESIAN_POINT('Ctrl Pts',(-20.1510440699474,13.3310152130564,
0.));
#239301=CARTESIAN_POINT('Ctrl Pts',(-20.1510440699474,13.3310152130564,
12.));
#239302=CARTESIAN_POINT('Ctrl Pts',(-20.1294496158402,13.3262148471226,
0.));
#239303=CARTESIAN_POINT('Ctrl Pts',(-20.1294496158402,13.3262148471226,
12.));
#239304=CARTESIAN_POINT('Ctrl Pts',(-20.1079620798375,13.3213804177587,
0.));
#239305=CARTESIAN_POINT('Ctrl Pts',(-20.1079620798375,13.3213804177587,
12.));
#239306=CARTESIAN_POINT('Ctrl Pts',(-20.0865820689883,13.3165124377962,
0.));
#239307=CARTESIAN_POINT('Ctrl Pts',(-20.0865820689883,13.3165124377962,
12.));
#239308=CARTESIAN_POINT('Ctrl Pts',(-20.0653101957188,13.3116114266515,
0.));
#239309=CARTESIAN_POINT('Ctrl Pts',(-20.0653101957188,13.3116114266515,
12.));
#239310=CARTESIAN_POINT('Ctrl Pts',(-20.0441470779345,13.3066779104515,
0.));
#239311=CARTESIAN_POINT('Ctrl Pts',(-20.0441470779345,13.3066779104515,
12.));
#239312=CARTESIAN_POINT('Ctrl Pts',(-20.0230933391038,13.3017124221637,
0.));
#239313=CARTESIAN_POINT('Ctrl Pts',(-20.0230933391038,13.3017124221637,
12.));
#239314=CARTESIAN_POINT('Ctrl Pts',(-20.0021496083738,13.2967155017306,
0.));
#239315=CARTESIAN_POINT('Ctrl Pts',(-20.0021496083738,13.2967155017306,
12.));
#239316=CARTESIAN_POINT('Ctrl Pts',(-19.981316520717,13.2916876962094,0.));
#239317=CARTESIAN_POINT('Ctrl Pts',(-19.981316520717,13.2916876962094,12.));
#239318=CARTESIAN_POINT('Ctrl Pts',(-19.9605947170586,13.286629559915,0.));
#239319=CARTESIAN_POINT('Ctrl Pts',(-19.9605947170586,13.286629559915,12.));
#239320=CARTESIAN_POINT('Ctrl Pts',(-19.9399848444019,13.2815416545663,
0.));
#239321=CARTESIAN_POINT('Ctrl Pts',(-19.9399848444019,13.2815416545663,
12.));
#239322=CARTESIAN_POINT('Ctrl Pts',(-19.9194875559422,13.2764245494357,
0.));
#239323=CARTESIAN_POINT('Ctrl Pts',(-19.9194875559422,13.2764245494357,
12.));
#239324=CARTESIAN_POINT('Ctrl Pts',(-19.8991035111745,13.271278821502,0.));
#239325=CARTESIAN_POINT('Ctrl Pts',(-19.8991035111745,13.271278821502,12.));
#239326=CARTESIAN_POINT('Ctrl Pts',(-19.8788333760577,13.2661050556132,
0.));
#239327=CARTESIAN_POINT('Ctrl Pts',(-19.8788333760577,13.2661050556132,
12.));
#239328=CARTESIAN_POINT('Ctrl Pts',(-19.8586778231715,13.2609038446529,
0.));
#239329=CARTESIAN_POINT('Ctrl Pts',(-19.8586778231715,13.2609038446529,
12.));
#239330=CARTESIAN_POINT('Ctrl Pts',(-19.8386375318634,13.2556757897086,
0.));
#239331=CARTESIAN_POINT('Ctrl Pts',(-19.8386375318634,13.2556757897086,
12.));
#239332=CARTESIAN_POINT('Ctrl Pts',(-19.8187131883917,13.2504215002457,
0.));
#239333=CARTESIAN_POINT('Ctrl Pts',(-19.8187131883917,13.2504215002457,
12.));
#239334=CARTESIAN_POINT('Ctrl Pts',(-19.7989054860495,13.2451415942805,
0.));
#239335=CARTESIAN_POINT('Ctrl Pts',(-19.7989054860495,13.2451415942805,
12.));
#239336=CARTESIAN_POINT('Ctrl Pts',(-19.7792151253289,13.2398366985675,
0.));
#239337=CARTESIAN_POINT('Ctrl Pts',(-19.7792151253289,13.2398366985675,
12.));
#239338=CARTESIAN_POINT('Ctrl Pts',(-19.7596428141168,13.2345074487963,
0.));
#239339=CARTESIAN_POINT('Ctrl Pts',(-19.7596428141168,13.2345074487963,
12.));
#239340=CARTESIAN_POINT('Ctrl Pts',(-19.7401892678697,13.2291544897899,
0.));
#239341=CARTESIAN_POINT('Ctrl Pts',(-19.7401892678697,13.2291544897899,
12.));
#239342=CARTESIAN_POINT('Ctrl Pts',(-19.7208552097868,13.2237784757065,
0.));
#239343=CARTESIAN_POINT('Ctrl Pts',(-19.7208552097868,13.2237784757065,
12.));
#239344=CARTESIAN_POINT('Ctrl Pts',(-19.7016413709685,13.2183800702436,
0.));
#239345=CARTESIAN_POINT('Ctrl Pts',(-19.7016413709685,13.2183800702436,
12.));
#239346=CARTESIAN_POINT('Ctrl Pts',(-19.6825484905823,13.2129599468485,
0.));
#239347=CARTESIAN_POINT('Ctrl Pts',(-19.6825484905823,13.2129599468485,
12.));
#239348=CARTESIAN_POINT('Ctrl Pts',(-19.6635773160936,13.2075187889529,
0.));
#239349=CARTESIAN_POINT('Ctrl Pts',(-19.6635773160936,13.2075187889529,
12.));
#239350=CARTESIAN_POINT('Ctrl Pts',(-19.6447286034772,13.2020572902065,
0.));
#239351=CARTESIAN_POINT('Ctrl Pts',(-19.6447286034772,13.2020572902065,
12.));
#239352=CARTESIAN_POINT('Ctrl Pts',(-19.6260031174244,13.1965761547151,
0.));
#239353=CARTESIAN_POINT('Ctrl Pts',(-19.6260031174244,13.1965761547151,
12.));
#239354=CARTESIAN_POINT('Ctrl Pts',(-19.6074016315414,13.1910760972814,
0.));
#239355=CARTESIAN_POINT('Ctrl Pts',(-19.6074016315414,13.1910760972814,
12.));
#239356=CARTESIAN_POINT('Ctrl Pts',(-19.5889249285338,13.1855578436471,
0.));
#239357=CARTESIAN_POINT('Ctrl Pts',(-19.5889249285338,13.1855578436471,
12.));
#239358=CARTESIAN_POINT('Ctrl Pts',(-19.5705738004667,13.1800221307673,
0.));
#239359=CARTESIAN_POINT('Ctrl Pts',(-19.5705738004667,13.1800221307673,
12.));
#239360=CARTESIAN_POINT('Ctrl Pts',(-19.5523490490244,13.1744697070911,
0.));
#239361=CARTESIAN_POINT('Ctrl Pts',(-19.5523490490244,13.1744697070911,
12.));
#239362=CARTESIAN_POINT('Ctrl Pts',(-19.5342514857562,13.168901332843,0.));
#239363=CARTESIAN_POINT('Ctrl Pts',(-19.5342514857562,13.168901332843,12.));
#239364=CARTESIAN_POINT('Ctrl Pts',(-19.5162819323213,13.1633177803101,
0.));
#239365=CARTESIAN_POINT('Ctrl Pts',(-19.5162819323213,13.1633177803101,
12.));
#239366=CARTESIAN_POINT('Ctrl Pts',(-19.4984412207082,13.1577198341245,
0.));
#239367=CARTESIAN_POINT('Ctrl Pts',(-19.4984412207082,13.1577198341245,
12.));
#239368=CARTESIAN_POINT('Ctrl Pts',(-19.4807301935268,13.1521082915853,
0.));
#239369=CARTESIAN_POINT('Ctrl Pts',(-19.4807301935268,13.1521082915853,
12.));
#239370=CARTESIAN_POINT('Ctrl Pts',(-19.4631497043258,13.1464839629971,
0.));
#239371=CARTESIAN_POINT('Ctrl Pts',(-19.4631497043258,13.1464839629971,
12.));
#239372=CARTESIAN_POINT('Ctrl Pts',(-19.4457006178876,13.1408476720061,
0.));
#239373=CARTESIAN_POINT('Ctrl Pts',(-19.4457006178876,13.1408476720061,
12.));
#239374=CARTESIAN_POINT('Ctrl Pts',(-19.4283838105262,13.1352002559438,
0.));
#239375=CARTESIAN_POINT('Ctrl Pts',(-19.4283838105262,13.1352002559438,
12.));
#239376=CARTESIAN_POINT('Ctrl Pts',(-19.4112001703557,13.1295425661634,
0.));
#239377=CARTESIAN_POINT('Ctrl Pts',(-19.4112001703557,13.1295425661634,
12.));
#239378=CARTESIAN_POINT('Ctrl Pts',(-19.3941505976263,13.1238754684177,
0.));
#239379=CARTESIAN_POINT('Ctrl Pts',(-19.3941505976263,13.1238754684177,
12.));
#239380=CARTESIAN_POINT('Ctrl Pts',(-19.3772360051091,13.118199843271,0.));
#239381=CARTESIAN_POINT('Ctrl Pts',(-19.3772360051091,13.118199843271,12.));
#239382=CARTESIAN_POINT('Ctrl Pts',(-19.3604573184515,13.1125165865022,
0.));
#239383=CARTESIAN_POINT('Ctrl Pts',(-19.3604573184515,13.1125165865022,
12.));
#239384=CARTESIAN_POINT('Ctrl Pts',(-19.3438154765395,13.1068266095186,
0.));
#239385=CARTESIAN_POINT('Ctrl Pts',(-19.3438154765395,13.1068266095186,
12.));
#239386=CARTESIAN_POINT('Ctrl Pts',(-19.3273114318269,13.1011308397591,
0.));
#239387=CARTESIAN_POINT('Ctrl Pts',(-19.3273114318269,13.1011308397591,
12.));
#239388=CARTESIAN_POINT('Ctrl Pts',(-19.310946150736,13.0954302211479,0.));
#239389=CARTESIAN_POINT('Ctrl Pts',(-19.310946150736,13.0954302211479,12.));
#239390=CARTESIAN_POINT('Ctrl Pts',(-19.2947206141247,13.0897257145968,
0.));
#239391=CARTESIAN_POINT('Ctrl Pts',(-19.2947206141247,13.0897257145968,
12.));
#239392=CARTESIAN_POINT('Ctrl Pts',(-19.2786358177198,13.0840182984949,
0.));
#239393=CARTESIAN_POINT('Ctrl Pts',(-19.2786358177198,13.0840182984949,
12.));
#239394=CARTESIAN_POINT('Ctrl Pts',(-19.2626927725596,13.0783089692118,
0.));
#239395=CARTESIAN_POINT('Ctrl Pts',(-19.2626927725596,13.0783089692118,
12.));
#239396=CARTESIAN_POINT('Ctrl Pts',(-19.2468925053989,13.0725987415859,
0.));
#239397=CARTESIAN_POINT('Ctrl Pts',(-19.2468925053989,13.0725987415859,
12.));
#239398=CARTESIAN_POINT('Ctrl Pts',(-19.2312360592033,13.0668886494795,
0.));
#239399=CARTESIAN_POINT('Ctrl Pts',(-19.2312360592033,13.0668886494795,
12.));
#239400=CARTESIAN_POINT('Ctrl Pts',(-19.2157244937142,13.0611797463915,
0.));
#239401=CARTESIAN_POINT('Ctrl Pts',(-19.2157244937142,13.0611797463915,
12.));
#239402=CARTESIAN_POINT('Ctrl Pts',(-19.2003588859772,13.0554731060538,
0.));
#239403=CARTESIAN_POINT('Ctrl Pts',(-19.2003588859772,13.0554731060538,
12.));
#239404=CARTESIAN_POINT('Ctrl Pts',(-19.1851403308825,13.0497698230441,
0.));
#239405=CARTESIAN_POINT('Ctrl Pts',(-19.1851403308825,13.0497698230441,
12.));
#239406=CARTESIAN_POINT('Ctrl Pts',(-19.1700699416622,13.0440710133772,
0.));
#239407=CARTESIAN_POINT('Ctrl Pts',(-19.1700699416622,13.0440710133772,
12.));
#239408=CARTESIAN_POINT('Ctrl Pts',(-19.155148850523,13.0383778152068,0.));
#239409=CARTESIAN_POINT('Ctrl Pts',(-19.155148850523,13.0383778152068,12.));
#239410=CARTESIAN_POINT('Ctrl Pts',(-19.1403782093386,13.0326913895838,
0.));
#239411=CARTESIAN_POINT('Ctrl Pts',(-19.1403782093386,13.0326913895838,
12.));
#239412=CARTESIAN_POINT('Ctrl Pts',(-19.1257591903099,13.0270129211976,
0.));
#239413=CARTESIAN_POINT('Ctrl Pts',(-19.1257591903099,13.0270129211976,
12.));
#239414=CARTESIAN_POINT('Ctrl Pts',(-19.111292986631,13.0213436191328,0.));
#239415=CARTESIAN_POINT('Ctrl Pts',(-19.111292986631,13.0213436191328,12.));
#239416=CARTESIAN_POINT('Ctrl Pts',(-19.0969808131228,13.0156847176096,
0.));
#239417=CARTESIAN_POINT('Ctrl Pts',(-19.0969808131228,13.0156847176096,
12.));
#239418=CARTESIAN_POINT('Ctrl Pts',(-19.0828239070484,13.0100374768788,
0.));
#239419=CARTESIAN_POINT('Ctrl Pts',(-19.0828239070484,13.0100374768788,
12.));
#239420=CARTESIAN_POINT('Ctrl Pts',(-19.0688235289437,13.0044031841382,
0.));
#239421=CARTESIAN_POINT('Ctrl Pts',(-19.0688235289437,13.0044031841382,
12.));
#239422=CARTESIAN_POINT('Ctrl Pts',(-19.0549809634354,12.9987831544502,
0.));
#239423=CARTESIAN_POINT('Ctrl Pts',(-19.0549809634354,12.9987831544502,
12.));
#239424=CARTESIAN_POINT('Ctrl Pts',(-19.0412975200398,12.9931787316514,
0.));
#239425=CARTESIAN_POINT('Ctrl Pts',(-19.0412975200398,12.9931787316514,
12.));
#239426=CARTESIAN_POINT('Ctrl Pts',(-19.0277745339909,12.9875912893003,
0.));
#239427=CARTESIAN_POINT('Ctrl Pts',(-19.0277745339909,12.9875912893003,
12.));
#239428=CARTESIAN_POINT('Ctrl Pts',(-19.014413367335,12.9820222318716,0.));
#239429=CARTESIAN_POINT('Ctrl Pts',(-19.014413367335,12.9820222318716,12.));
#239430=CARTESIAN_POINT('Ctrl Pts',(-19.0012154099792,12.9764729959206,
0.));
#239431=CARTESIAN_POINT('Ctrl Pts',(-19.0012154099792,12.9764729959206,
12.));
#239432=CARTESIAN_POINT('Ctrl Pts',(-18.9881820807585,12.9709450512747,
0.));
#239433=CARTESIAN_POINT('Ctrl Pts',(-18.9881820807585,12.9709450512747,
12.));
#239434=CARTESIAN_POINT('Ctrl Pts',(-18.9753148284473,12.9654399021868,
0.));
#239435=CARTESIAN_POINT('Ctrl Pts',(-18.9753148284473,12.9654399021868,
12.));
#239436=CARTESIAN_POINT('Ctrl Pts',(-18.9626151329226,12.9599590886317,
0.));
#239437=CARTESIAN_POINT('Ctrl Pts',(-18.9626151329226,12.9599590886317,
12.));
#239438=CARTESIAN_POINT('Ctrl Pts',(-18.9500845064714,12.9545041877377,
0.));
#239439=CARTESIAN_POINT('Ctrl Pts',(-18.9500845064714,12.9545041877377,
12.));
#239440=CARTESIAN_POINT('Ctrl Pts',(-18.9377244950435,12.9490768151821,
0.));
#239441=CARTESIAN_POINT('Ctrl Pts',(-18.9377244950435,12.9490768151821,
12.));
#239442=CARTESIAN_POINT('Ctrl Pts',(-18.9255366795196,12.9436786266106,
0.));
#239443=CARTESIAN_POINT('Ctrl Pts',(-18.9255366795196,12.9436786266106,
12.));
#239444=CARTESIAN_POINT('Ctrl Pts',(-18.9135226769466,12.9383113190375,
0.));
#239445=CARTESIAN_POINT('Ctrl Pts',(-18.9135226769466,12.9383113190375,
12.));
#239446=CARTESIAN_POINT('Ctrl Pts',(-18.9016841423402,12.9329766328184,
0.));
#239447=CARTESIAN_POINT('Ctrl Pts',(-18.9016841423402,12.9329766328184,
12.));
#239448=CARTESIAN_POINT('Ctrl Pts',(-18.8900227704888,12.9276763536372,
0.));
#239449=CARTESIAN_POINT('Ctrl Pts',(-18.8900227704888,12.9276763536372,
12.));
#239450=CARTESIAN_POINT('Ctrl Pts',(-18.8785402977528,12.9224123144982,
0.));
#239451=CARTESIAN_POINT('Ctrl Pts',(-18.8785402977528,12.9224123144982,
12.));
#239452=CARTESIAN_POINT('Ctrl Pts',(-18.8672385038328,12.9171863977047,
0.));
#239453=CARTESIAN_POINT('Ctrl Pts',(-18.8672385038328,12.9171863977047,
12.));
#239454=CARTESIAN_POINT('Ctrl Pts',(-18.8561192136201,12.9120005369066,
0.));
#239455=CARTESIAN_POINT('Ctrl Pts',(-18.8561192136201,12.9120005369066,
12.));
#239456=CARTESIAN_POINT('Ctrl Pts',(-18.8451842990986,12.9068567191856,
0.));
#239457=CARTESIAN_POINT('Ctrl Pts',(-18.8451842990986,12.9068567191856,
12.));
#239458=CARTESIAN_POINT('Ctrl Pts',(-18.834435681259,12.9017569871738,0.));
#239459=CARTESIAN_POINT('Ctrl Pts',(-18.834435681259,12.9017569871738,12.));
#239460=CARTESIAN_POINT('Ctrl Pts',(-18.8238753319124,12.8967034410752,
0.));
#239461=CARTESIAN_POINT('Ctrl Pts',(-18.8238753319124,12.8967034410752,
12.));
#239462=CARTESIAN_POINT('Ctrl Pts',(-18.8135052757815,12.8916982409931,
0.));
#239463=CARTESIAN_POINT('Ctrl Pts',(-18.8135052757815,12.8916982409931,
12.));
#239464=CARTESIAN_POINT('Ctrl Pts',(-18.8033275941939,12.8867436109543,
0.));
#239465=CARTESIAN_POINT('Ctrl Pts',(-18.8033275941939,12.8867436109543,
12.));
#239466=CARTESIAN_POINT('Ctrl Pts',(-18.7933444285867,12.8818418427474,
0.));
#239467=CARTESIAN_POINT('Ctrl Pts',(-18.7933444285867,12.8818418427474,
12.));
#239468=CARTESIAN_POINT('Ctrl Pts',(-18.7835579840481,12.8769952998097,
0.));
#239469=CARTESIAN_POINT('Ctrl Pts',(-18.7835579840481,12.8769952998097,
12.));
#239470=CARTESIAN_POINT('Ctrl Pts',(-18.7739705329029,12.8722064211814,
0.));
#239471=CARTESIAN_POINT('Ctrl Pts',(-18.7739705329029,12.8722064211814,
12.));
#239472=CARTESIAN_POINT('Ctrl Pts',(-18.7645844169568,12.8674777239656,
0.));
#239473=CARTESIAN_POINT('Ctrl Pts',(-18.7645844169568,12.8674777239656,
12.));
#239474=CARTESIAN_POINT('Ctrl Pts',(-18.7554020493888,12.8628118054172,
0.));
#239475=CARTESIAN_POINT('Ctrl Pts',(-18.7554020493888,12.8628118054172,
12.));
#239476=CARTESIAN_POINT('Ctrl Pts',(-18.7464259171248,12.8582113455644,
0.));
#239477=CARTESIAN_POINT('Ctrl Pts',(-18.7464259171248,12.8582113455644,
12.));
#239478=CARTESIAN_POINT('Ctrl Pts',(-18.7376585820851,12.8536791086315,
0.));
#239479=CARTESIAN_POINT('Ctrl Pts',(-18.7376585820851,12.8536791086315,
12.));
#239480=CARTESIAN_POINT('Ctrl Pts',(-18.7291026886552,12.849217951159,0.));
#239481=CARTESIAN_POINT('Ctrl Pts',(-18.7291026886552,12.849217951159,12.));
#239482=CARTESIAN_POINT('Ctrl Pts',(-18.7207609737701,12.8448308329494,
0.));
#239483=CARTESIAN_POINT('Ctrl Pts',(-18.7207609737701,12.8448308329494,
12.));
#239484=CARTESIAN_POINT('Ctrl Pts',(-18.7126362754446,12.8405208263432,
0.));
#239485=CARTESIAN_POINT('Ctrl Pts',(-18.7126362754446,12.8405208263432,
12.));
#239486=CARTESIAN_POINT('Ctrl Pts',(-18.7047315436296,12.8362911280362,
0.));
#239487=CARTESIAN_POINT('Ctrl Pts',(-18.7047315436296,12.8362911280362,
12.));
#239488=CARTESIAN_POINT('Ctrl Pts',(-18.6970498410173,12.832145059979,0.));
#239489=CARTESIAN_POINT('Ctrl Pts',(-18.6970498410173,12.832145059979,12.));
#239490=CARTESIAN_POINT('Ctrl Pts',(-18.6895943376172,12.8280860635231,
0.));
#239491=CARTESIAN_POINT('Ctrl Pts',(-18.6895943376172,12.8280860635231,
12.));
#239492=CARTESIAN_POINT('Ctrl Pts',(-18.6823683094139,12.8241176980016,
0.));
#239493=CARTESIAN_POINT('Ctrl Pts',(-18.6823683094139,12.8241176980016,
12.));
#239494=CARTESIAN_POINT('Ctrl Pts',(-18.6753751301091,12.8202436318473,
0.));
#239495=CARTESIAN_POINT('Ctrl Pts',(-18.6753751301091,12.8202436318473,
12.));
#239496=CARTESIAN_POINT('Ctrl Pts',(-18.6686182952798,12.8164676687361,
0.));
#239497=CARTESIAN_POINT('Ctrl Pts',(-18.6686182952798,12.8164676687361,
12.));
#239498=CARTESIAN_POINT('Ctrl Pts',(-18.6621014624746,12.8127937909632,
0.));
#239499=CARTESIAN_POINT('Ctrl Pts',(-18.6621014624746,12.8127937909632,
12.));
#239500=CARTESIAN_POINT('Ctrl Pts',(-18.6558284825772,12.8092261933858,
0.));
#239501=CARTESIAN_POINT('Ctrl Pts',(-18.6558284825772,12.8092261933858,
12.));
#239502=CARTESIAN_POINT('Ctrl Pts',(-18.6498034438986,12.805769331162,0.));
#239503=CARTESIAN_POINT('Ctrl Pts',(-18.6498034438986,12.805769331162,12.));
#239504=CARTESIAN_POINT('Ctrl Pts',(-18.6440306327457,12.8024278770153,
0.));
#239505=CARTESIAN_POINT('Ctrl Pts',(-18.6440306327457,12.8024278770153,
12.));
#239506=CARTESIAN_POINT('Ctrl Pts',(-18.63851447924,12.7992066625264,0.));
#239507=CARTESIAN_POINT('Ctrl Pts',(-18.63851447924,12.7992066625264,12.));
#239508=CARTESIAN_POINT('Ctrl Pts',(-18.6332595057005,12.7961106222251,
0.));
#239509=CARTESIAN_POINT('Ctrl Pts',(-18.6332595057005,12.7961106222251,
12.));
#239510=CARTESIAN_POINT('Ctrl Pts',(-18.6282702819371,12.7931447451556,
0.));
#239511=CARTESIAN_POINT('Ctrl Pts',(-18.6282702819371,12.7931447451556,
12.));
#239512=CARTESIAN_POINT('Ctrl Pts',(-18.6235516265575,12.7903142925234,
0.));
#239513=CARTESIAN_POINT('Ctrl Pts',(-18.6235516265575,12.7903142925234,
12.));
#239514=CARTESIAN_POINT('Ctrl Pts',(-18.6191087624752,12.7876249657834,
0.));
#239515=CARTESIAN_POINT('Ctrl Pts',(-18.6191087624752,12.7876249657834,
12.));
#239516=CARTESIAN_POINT('Ctrl Pts',(-18.6149475565189,12.78508316579,0.));
#239517=CARTESIAN_POINT('Ctrl Pts',(-18.6149475565189,12.78508316579,12.));
#239518=CARTESIAN_POINT('Ctrl Pts',(-18.611074482622,12.7826959526924,0.));
#239519=CARTESIAN_POINT('Ctrl Pts',(-18.611074482622,12.7826959526924,12.));
#239520=CARTESIAN_POINT('Ctrl Pts',(-18.6074961535723,12.7804705387658,
0.));
#239521=CARTESIAN_POINT('Ctrl Pts',(-18.6074961535723,12.7804705387658,
12.));
#239522=CARTESIAN_POINT('Ctrl Pts',(-18.6042190183703,12.7784139605067,
0.));
#239523=CARTESIAN_POINT('Ctrl Pts',(-18.6042190183703,12.7784139605067,
12.));
#239524=CARTESIAN_POINT('Ctrl Pts',(-18.6012488486708,12.7765325225082,
0.));
#239525=CARTESIAN_POINT('Ctrl Pts',(-18.6012488486708,12.7765325225082,
12.));
#239526=CARTESIAN_POINT('Ctrl Pts',(-18.5985917525949,12.7748328937639,
0.));
#239527=CARTESIAN_POINT('Ctrl Pts',(-18.5985917525949,12.7748328937639,
12.));
#239528=CARTESIAN_POINT('Ctrl Pts',(-18.5962551167772,12.7733231262107,
0.));
#239529=CARTESIAN_POINT('Ctrl Pts',(-18.5962551167772,12.7733231262107,
12.));
#239530=CARTESIAN_POINT('Ctrl Pts',(-18.5942490615409,12.7720142287169,
0.));
#239531=CARTESIAN_POINT('Ctrl Pts',(-18.5942490615409,12.7720142287169,
12.));
#239532=CARTESIAN_POINT('Ctrl Pts',(-18.5925859134582,12.7709195951153,
0.));
#239533=CARTESIAN_POINT('Ctrl Pts',(-18.5925859134582,12.7709195951153,
12.));
#239534=CARTESIAN_POINT('Ctrl Pts',(-18.5912775137806,12.7700520897174,
0.));
#239535=CARTESIAN_POINT('Ctrl Pts',(-18.5912775137806,12.7700520897174,
12.));
#239536=CARTESIAN_POINT('Ctrl Pts',(-18.590332877722,12.7694215127923,0.));
#239537=CARTESIAN_POINT('Ctrl Pts',(-18.590332877722,12.7694215127923,12.));
#239538=CARTESIAN_POINT('Ctrl Pts',(-18.589871621842,12.7691103481996,0.));
#239539=CARTESIAN_POINT('Ctrl Pts',(-18.589871621842,12.7691103481996,12.));
#239540=CARTESIAN_POINT('Ctrl Pts',(-18.5896919669158,12.7689864266924,
0.));
#239541=CARTESIAN_POINT('Ctrl Pts',(-18.5896919669158,12.7689864266924,
12.));
#239542=CARTESIAN_POINT('Ctrl Pts',(-18.5896460962961,12.7689524524484,
0.));
#239543=CARTESIAN_POINT('Ctrl Pts',(-18.5896460962961,12.7689524524484,
12.));
#239544=CARTESIAN_POINT('Ctrl Pts',(-18.5896416359912,12.7689476255363,
0.));
#239545=CARTESIAN_POINT('Ctrl Pts',(-18.5896416359912,12.7689476255363,
12.));
#239546=CARTESIAN_POINT('',(-22.1787195904339,13.5685075571671,0.));
#239547=CARTESIAN_POINT('Ctrl Pts',(-22.1787195904339,13.5685075571671,
0.));
#239548=CARTESIAN_POINT('Ctrl Pts',(-22.1730081264583,13.5683460612913,
0.));
#239549=CARTESIAN_POINT('Ctrl Pts',(-22.1615922804939,13.5680170531724,
0.));
#239550=CARTESIAN_POINT('Ctrl Pts',(-22.1444897575076,13.5675054918922,
0.));
#239551=CARTESIAN_POINT('Ctrl Pts',(-22.1217288871823,13.5667873105179,
0.));
#239552=CARTESIAN_POINT('Ctrl Pts',(-22.0933486464442,13.5658294169106,
0.));
#239553=CARTESIAN_POINT('Ctrl Pts',(-22.0650393089492,13.5648113688894,
0.));
#239554=CARTESIAN_POINT('Ctrl Pts',(-22.0368009736227,13.5637332022393,
0.));
#239555=CARTESIAN_POINT('Ctrl Pts',(-22.0086337943431,13.5625949868313,
0.));
#239556=CARTESIAN_POINT('Ctrl Pts',(-21.9805379899192,13.5613968357589,
0.));
#239557=CARTESIAN_POINT('Ctrl Pts',(-21.9525138592862,13.5601389185315,
0.));
#239558=CARTESIAN_POINT('Ctrl Pts',(-21.9245617765827,13.5588214586672,
0.));
#239559=CARTESIAN_POINT('Ctrl Pts',(-21.8966821688876,13.5574447178484,
0.));
#239560=CARTESIAN_POINT('Ctrl Pts',(-21.8688754989401,13.5560089839426,
0.));
#239561=CARTESIAN_POINT('Ctrl Pts',(-21.841142245609,13.5545145573048,0.));
#239562=CARTESIAN_POINT('Ctrl Pts',(-21.8134828857963,13.5529617381569,
0.));
#239563=CARTESIAN_POINT('Ctrl Pts',(-21.7858978745848,13.5513508127232,
0.));
#239564=CARTESIAN_POINT('Ctrl Pts',(-21.7583876294532,13.5496820422186,
0.));
#239565=CARTESIAN_POINT('Ctrl Pts',(-21.730952541226,13.5479556704457,0.));
#239566=CARTESIAN_POINT('Ctrl Pts',(-21.7035929822939,13.546171929503,0.));
#239567=CARTESIAN_POINT('Ctrl Pts',(-21.676309315769,13.5443310461516,0.));
#239568=CARTESIAN_POINT('Ctrl Pts',(-21.6491019044647,13.5424332480698,
0.));
#239569=CARTESIAN_POINT('Ctrl Pts',(-21.6219711193951,13.5404787697798,
0.));
#239570=CARTESIAN_POINT('Ctrl Pts',(-21.5949173499022,13.5384678597206,
0.));
#239571=CARTESIAN_POINT('Ctrl Pts',(-21.5679410019011,13.5364007790292,
0.));
#239572=CARTESIAN_POINT('Ctrl Pts',(-21.5410424932511,13.5342777983225,
0.));
#239573=CARTESIAN_POINT('Ctrl Pts',(-21.5142222501671,13.5320991952145,
0.));
#239574=CARTESIAN_POINT('Ctrl Pts',(-21.487480703047,13.5298652514357,0.));
#239575=CARTESIAN_POINT('Ctrl Pts',(-21.4608182828695,13.5275762503553,
0.));
#239576=CARTESIAN_POINT('Ctrl Pts',(-21.4342354165254,13.5252324737795,
0.));
#239577=CARTESIAN_POINT('Ctrl Pts',(-21.4077325259318,13.5228342013508,
0.));
#239578=CARTESIAN_POINT('Ctrl Pts',(-21.3813100304967,13.5203817122496,
0.));
#239579=CARTESIAN_POINT('Ctrl Pts',(-21.3549683486219,13.5178752862461,
0.));
#239580=CARTESIAN_POINT('Ctrl Pts',(-21.328707899634,13.5153152050554,0.));
#239581=CARTESIAN_POINT('Ctrl Pts',(-21.3025291054236,13.5127017534972,
0.));
#239582=CARTESIAN_POINT('Ctrl Pts',(-21.2764323924442,13.5100352209207,
0.));
#239583=CARTESIAN_POINT('Ctrl Pts',(-21.2504181927429,13.5073159019454,
0.));
#239584=CARTESIAN_POINT('Ctrl Pts',(-21.224486942933,13.5045440957404,0.));
#239585=CARTESIAN_POINT('Ctrl Pts',(-21.1986390835825,13.5017201056088,
0.));
#239586=CARTESIAN_POINT('Ctrl Pts',(-21.1728750584173,13.4988442384491,
0.));
#239587=CARTESIAN_POINT('Ctrl Pts',(-21.1471953136209,13.4959168042934,
0.));
#239588=CARTESIAN_POINT('Ctrl Pts',(-21.1216002970209,13.4929381157778,
0.));
#239589=CARTESIAN_POINT('Ctrl Pts',(-21.0960904575048,13.4899084877718,
0.));
#239590=CARTESIAN_POINT('Ctrl Pts',(-21.0706662455202,13.4868282377191,
0.));
#239591=CARTESIAN_POINT('Ctrl Pts',(-21.0453281134247,13.4836976858912,
0.));
#239592=CARTESIAN_POINT('Ctrl Pts',(-21.0200765158885,13.4805171556822,
0.));
#239593=CARTESIAN_POINT('Ctrl Pts',(-20.9949119102592,13.4772869738879,
0.));
#239594=CARTESIAN_POINT('Ctrl Pts',(-20.9698347569476,13.4740074710087,
0.));
#239595=CARTESIAN_POINT('Ctrl Pts',(-20.9448455197557,13.4706789815166,
0.));
#239596=CARTESIAN_POINT('Ctrl Pts',(-20.9199446657584,13.4673018437718,
0.));
#239597=CARTESIAN_POINT('Ctrl Pts',(-20.8951326652158,13.4638763999725,
0.));
#239598=CARTESIAN_POINT('Ctrl Pts',(-20.8704099914641,13.4604029960983,
0.));
#239599=CARTESIAN_POINT('Ctrl Pts',(-20.8457771208082,13.4568819818631,
0.));
#239600=CARTESIAN_POINT('Ctrl Pts',(-20.821234532398,13.4533137106667,0.));
#239601=CARTESIAN_POINT('Ctrl Pts',(-20.7967827081227,13.4496985395637,
0.));
#239602=CARTESIAN_POINT('Ctrl Pts',(-20.7724221327608,13.4460368293688,
0.));
#239603=CARTESIAN_POINT('Ctrl Pts',(-20.7481532941013,13.4423289447561,
0.));
#239604=CARTESIAN_POINT('Ctrl Pts',(-20.7239766830675,13.4385752543663,
0.));
#239605=CARTESIAN_POINT('Ctrl Pts',(-20.6998927938288,13.4347761309154,
0.));
#239606=CARTESIAN_POINT('Ctrl Pts',(-20.6759021239103,13.4309319513119,
0.));
#239607=CARTESIAN_POINT('Ctrl Pts',(-20.6520051742869,13.4270430967651,
0.));
#239608=CARTESIAN_POINT('Ctrl Pts',(-20.6282024494237,13.4231099528179,
0.));
#239609=CARTESIAN_POINT('Ctrl Pts',(-20.6044944573153,13.4191329093932,
0.));
#239610=CARTESIAN_POINT('Ctrl Pts',(-20.5808817095155,13.4151123608411,
0.));
#239611=CARTESIAN_POINT('Ctrl Pts',(-20.5573647211639,13.4110487059912,
0.));
#239612=CARTESIAN_POINT('Ctrl Pts',(-20.5339440109956,13.4069423482076,
0.));
#239613=CARTESIAN_POINT('Ctrl Pts',(-20.5106201013753,13.4027936954529,
0.));
#239614=CARTESIAN_POINT('Ctrl Pts',(-20.487393518404,13.3986031603716,0.));
#239615=CARTESIAN_POINT('Ctrl Pts',(-20.4642647920038,13.3943711603739,
0.));
#239616=CARTESIAN_POINT('Ctrl Pts',(-20.4412344560008,13.3900981177255,
0.));
#239617=CARTESIAN_POINT('Ctrl Pts',(-20.4183030482002,13.3857844596387,
0.));
#239618=CARTESIAN_POINT('Ctrl Pts',(-20.3954711104502,13.3814306183719,
0.));
#239619=CARTESIAN_POINT('Ctrl Pts',(-20.3727391887184,13.3770370313188,
0.));
#239620=CARTESIAN_POINT('Ctrl Pts',(-20.3501078331814,13.3726041410867,
0.));
#239621=CARTESIAN_POINT('Ctrl Pts',(-20.3275775983029,13.3681323955826,
0.));
#239622=CARTESIAN_POINT('Ctrl Pts',(-20.3051490429048,13.3636222481016,
0.));
#239623=CARTESIAN_POINT('Ctrl Pts',(-20.2828227302339,13.3590741574195,
0.));
#239624=CARTESIAN_POINT('Ctrl Pts',(-20.2605992280122,13.3544885878889,
0.));
#239625=CARTESIAN_POINT('Ctrl Pts',(-20.2384791085359,13.3498660095386,
0.));
#239626=CARTESIAN_POINT('Ctrl Pts',(-20.216462948786,13.3452068981766,0.));
#239627=CARTESIAN_POINT('Ctrl Pts',(-20.1945513305235,13.3405117354971,
0.));
#239628=CARTESIAN_POINT('Ctrl Pts',(-20.1727448403817,13.3357810091903,
0.));
#239629=CARTESIAN_POINT('Ctrl Pts',(-20.1510440699474,13.3310152130564,
0.));
#239630=CARTESIAN_POINT('Ctrl Pts',(-20.1294496158402,13.3262148471226,
0.));
#239631=CARTESIAN_POINT('Ctrl Pts',(-20.1079620798375,13.3213804177587,
0.));
#239632=CARTESIAN_POINT('Ctrl Pts',(-20.0865820689883,13.3165124377962,
0.));
#239633=CARTESIAN_POINT('Ctrl Pts',(-20.0653101957188,13.3116114266515,
0.));
#239634=CARTESIAN_POINT('Ctrl Pts',(-20.0441470779345,13.3066779104515,
0.));
#239635=CARTESIAN_POINT('Ctrl Pts',(-20.0230933391038,13.3017124221637,
0.));
#239636=CARTESIAN_POINT('Ctrl Pts',(-20.0021496083738,13.2967155017306,
0.));
#239637=CARTESIAN_POINT('Ctrl Pts',(-19.981316520717,13.2916876962094,0.));
#239638=CARTESIAN_POINT('Ctrl Pts',(-19.9605947170586,13.286629559915,0.));
#239639=CARTESIAN_POINT('Ctrl Pts',(-19.9399848444019,13.2815416545663,
0.));
#239640=CARTESIAN_POINT('Ctrl Pts',(-19.9194875559422,13.2764245494357,
0.));
#239641=CARTESIAN_POINT('Ctrl Pts',(-19.8991035111745,13.271278821502,0.));
#239642=CARTESIAN_POINT('Ctrl Pts',(-19.8788333760577,13.2661050556132,
0.));
#239643=CARTESIAN_POINT('Ctrl Pts',(-19.8586778231715,13.2609038446529,
0.));
#239644=CARTESIAN_POINT('Ctrl Pts',(-19.8386375318634,13.2556757897086,
0.));
#239645=CARTESIAN_POINT('Ctrl Pts',(-19.8187131883917,13.2504215002457,
0.));
#239646=CARTESIAN_POINT('Ctrl Pts',(-19.7989054860495,13.2451415942805,
0.));
#239647=CARTESIAN_POINT('Ctrl Pts',(-19.7792151253289,13.2398366985675,
0.));
#239648=CARTESIAN_POINT('Ctrl Pts',(-19.7596428141168,13.2345074487963,
0.));
#239649=CARTESIAN_POINT('Ctrl Pts',(-19.7401892678697,13.2291544897899,
0.));
#239650=CARTESIAN_POINT('Ctrl Pts',(-19.7208552097868,13.2237784757065,
0.));
#239651=CARTESIAN_POINT('Ctrl Pts',(-19.7016413709685,13.2183800702436,
0.));
#239652=CARTESIAN_POINT('Ctrl Pts',(-19.6825484905823,13.2129599468485,
0.));
#239653=CARTESIAN_POINT('Ctrl Pts',(-19.6635773160936,13.2075187889529,
0.));
#239654=CARTESIAN_POINT('Ctrl Pts',(-19.6447286034772,13.2020572902065,
0.));
#239655=CARTESIAN_POINT('Ctrl Pts',(-19.6260031174244,13.1965761547151,
0.));
#239656=CARTESIAN_POINT('Ctrl Pts',(-19.6074016315414,13.1910760972814,
0.));
#239657=CARTESIAN_POINT('Ctrl Pts',(-19.5889249285338,13.1855578436471,
0.));
#239658=CARTESIAN_POINT('Ctrl Pts',(-19.5705738004667,13.1800221307673,
0.));
#239659=CARTESIAN_POINT('Ctrl Pts',(-19.5523490490244,13.1744697070911,
0.));
#239660=CARTESIAN_POINT('Ctrl Pts',(-19.5342514857562,13.168901332843,0.));
#239661=CARTESIAN_POINT('Ctrl Pts',(-19.5162819323213,13.1633177803101,
0.));
#239662=CARTESIAN_POINT('Ctrl Pts',(-19.4984412207082,13.1577198341245,
0.));
#239663=CARTESIAN_POINT('Ctrl Pts',(-19.4807301935268,13.1521082915853,
0.));
#239664=CARTESIAN_POINT('Ctrl Pts',(-19.4631497043258,13.1464839629971,
0.));
#239665=CARTESIAN_POINT('Ctrl Pts',(-19.4457006178876,13.1408476720061,
0.));
#239666=CARTESIAN_POINT('Ctrl Pts',(-19.4283838105262,13.1352002559438,
0.));
#239667=CARTESIAN_POINT('Ctrl Pts',(-19.4112001703557,13.1295425661634,
0.));
#239668=CARTESIAN_POINT('Ctrl Pts',(-19.3941505976263,13.1238754684177,
0.));
#239669=CARTESIAN_POINT('Ctrl Pts',(-19.3772360051091,13.118199843271,0.));
#239670=CARTESIAN_POINT('Ctrl Pts',(-19.3604573184515,13.1125165865022,
0.));
#239671=CARTESIAN_POINT('Ctrl Pts',(-19.3438154765395,13.1068266095186,
0.));
#239672=CARTESIAN_POINT('Ctrl Pts',(-19.3273114318269,13.1011308397591,
0.));
#239673=CARTESIAN_POINT('Ctrl Pts',(-19.310946150736,13.0954302211479,0.));
#239674=CARTESIAN_POINT('Ctrl Pts',(-19.2947206141247,13.0897257145968,
0.));
#239675=CARTESIAN_POINT('Ctrl Pts',(-19.2786358177198,13.0840182984949,
0.));
#239676=CARTESIAN_POINT('Ctrl Pts',(-19.2626927725596,13.0783089692118,
0.));
#239677=CARTESIAN_POINT('Ctrl Pts',(-19.2468925053989,13.0725987415859,
0.));
#239678=CARTESIAN_POINT('Ctrl Pts',(-19.2312360592033,13.0668886494795,
0.));
#239679=CARTESIAN_POINT('Ctrl Pts',(-19.2157244937142,13.0611797463915,
0.));
#239680=CARTESIAN_POINT('Ctrl Pts',(-19.2003588859772,13.0554731060538,
0.));
#239681=CARTESIAN_POINT('Ctrl Pts',(-19.1851403308825,13.0497698230441,
0.));
#239682=CARTESIAN_POINT('Ctrl Pts',(-19.1700699416622,13.0440710133772,
0.));
#239683=CARTESIAN_POINT('Ctrl Pts',(-19.155148850523,13.0383778152068,0.));
#239684=CARTESIAN_POINT('Ctrl Pts',(-19.1403782093386,13.0326913895838,
0.));
#239685=CARTESIAN_POINT('Ctrl Pts',(-19.1257591903099,13.0270129211976,
0.));
#239686=CARTESIAN_POINT('Ctrl Pts',(-19.111292986631,13.0213436191328,0.));
#239687=CARTESIAN_POINT('Ctrl Pts',(-19.0969808131228,13.0156847176096,
0.));
#239688=CARTESIAN_POINT('Ctrl Pts',(-19.0828239070484,13.0100374768788,
0.));
#239689=CARTESIAN_POINT('Ctrl Pts',(-19.0688235289437,13.0044031841382,
0.));
#239690=CARTESIAN_POINT('Ctrl Pts',(-19.0549809634354,12.9987831544502,
0.));
#239691=CARTESIAN_POINT('Ctrl Pts',(-19.0412975200398,12.9931787316514,
0.));
#239692=CARTESIAN_POINT('Ctrl Pts',(-19.0277745339909,12.9875912893003,
0.));
#239693=CARTESIAN_POINT('Ctrl Pts',(-19.014413367335,12.9820222318716,0.));
#239694=CARTESIAN_POINT('Ctrl Pts',(-19.0012154099792,12.9764729959206,
0.));
#239695=CARTESIAN_POINT('Ctrl Pts',(-18.9881820807585,12.9709450512747,
0.));
#239696=CARTESIAN_POINT('Ctrl Pts',(-18.9753148284473,12.9654399021868,
0.));
#239697=CARTESIAN_POINT('Ctrl Pts',(-18.9626151329226,12.9599590886317,
0.));
#239698=CARTESIAN_POINT('Ctrl Pts',(-18.9500845064714,12.9545041877377,
0.));
#239699=CARTESIAN_POINT('Ctrl Pts',(-18.9377244950435,12.9490768151821,
0.));
#239700=CARTESIAN_POINT('Ctrl Pts',(-18.9255366795196,12.9436786266106,
0.));
#239701=CARTESIAN_POINT('Ctrl Pts',(-18.9135226769466,12.9383113190375,
0.));
#239702=CARTESIAN_POINT('Ctrl Pts',(-18.9016841423402,12.9329766328184,
0.));
#239703=CARTESIAN_POINT('Ctrl Pts',(-18.8900227704888,12.9276763536372,
0.));
#239704=CARTESIAN_POINT('Ctrl Pts',(-18.8785402977528,12.9224123144982,
0.));
#239705=CARTESIAN_POINT('Ctrl Pts',(-18.8672385038328,12.9171863977047,
0.));
#239706=CARTESIAN_POINT('Ctrl Pts',(-18.8561192136201,12.9120005369066,
0.));
#239707=CARTESIAN_POINT('Ctrl Pts',(-18.8451842990986,12.9068567191856,
0.));
#239708=CARTESIAN_POINT('Ctrl Pts',(-18.834435681259,12.9017569871738,0.));
#239709=CARTESIAN_POINT('Ctrl Pts',(-18.8238753319124,12.8967034410752,
0.));
#239710=CARTESIAN_POINT('Ctrl Pts',(-18.8135052757815,12.8916982409931,
0.));
#239711=CARTESIAN_POINT('Ctrl Pts',(-18.8033275941939,12.8867436109543,
0.));
#239712=CARTESIAN_POINT('Ctrl Pts',(-18.7933444285867,12.8818418427474,
0.));
#239713=CARTESIAN_POINT('Ctrl Pts',(-18.7835579840481,12.8769952998097,
0.));
#239714=CARTESIAN_POINT('Ctrl Pts',(-18.7739705329029,12.8722064211814,
0.));
#239715=CARTESIAN_POINT('Ctrl Pts',(-18.7645844169568,12.8674777239656,
0.));
#239716=CARTESIAN_POINT('Ctrl Pts',(-18.7554020493888,12.8628118054172,
0.));
#239717=CARTESIAN_POINT('Ctrl Pts',(-18.7464259171248,12.8582113455644,
0.));
#239718=CARTESIAN_POINT('Ctrl Pts',(-18.7376585820851,12.8536791086315,
0.));
#239719=CARTESIAN_POINT('Ctrl Pts',(-18.7291026886552,12.849217951159,0.));
#239720=CARTESIAN_POINT('Ctrl Pts',(-18.7207609737701,12.8448308329494,
0.));
#239721=CARTESIAN_POINT('Ctrl Pts',(-18.7126362754446,12.8405208263432,
0.));
#239722=CARTESIAN_POINT('Ctrl Pts',(-18.7047315436296,12.8362911280362,
0.));
#239723=CARTESIAN_POINT('Ctrl Pts',(-18.6970498410173,12.832145059979,0.));
#239724=CARTESIAN_POINT('Ctrl Pts',(-18.6895943376172,12.8280860635231,
0.));
#239725=CARTESIAN_POINT('Ctrl Pts',(-18.6823683094139,12.8241176980016,
0.));
#239726=CARTESIAN_POINT('Ctrl Pts',(-18.6753751301091,12.8202436318473,
0.));
#239727=CARTESIAN_POINT('Ctrl Pts',(-18.6686182952798,12.8164676687361,
0.));
#239728=CARTESIAN_POINT('Ctrl Pts',(-18.6621014624746,12.8127937909632,
0.));
#239729=CARTESIAN_POINT('Ctrl Pts',(-18.6558284825772,12.8092261933858,
0.));
#239730=CARTESIAN_POINT('Ctrl Pts',(-18.6498034438986,12.805769331162,0.));
#239731=CARTESIAN_POINT('Ctrl Pts',(-18.6440306327457,12.8024278770153,
0.));
#239732=CARTESIAN_POINT('Ctrl Pts',(-18.63851447924,12.7992066625264,0.));
#239733=CARTESIAN_POINT('Ctrl Pts',(-18.6332595057005,12.7961106222251,
0.));
#239734=CARTESIAN_POINT('Ctrl Pts',(-18.6282702819371,12.7931447451556,
0.));
#239735=CARTESIAN_POINT('Ctrl Pts',(-18.6235516265575,12.7903142925234,
0.));
#239736=CARTESIAN_POINT('Ctrl Pts',(-18.6191087624752,12.7876249657834,
0.));
#239737=CARTESIAN_POINT('Ctrl Pts',(-18.6149475565189,12.78508316579,0.));
#239738=CARTESIAN_POINT('Ctrl Pts',(-18.611074482622,12.7826959526924,0.));
#239739=CARTESIAN_POINT('Ctrl Pts',(-18.6074961535723,12.7804705387658,
0.));
#239740=CARTESIAN_POINT('Ctrl Pts',(-18.6042190183703,12.7784139605067,
0.));
#239741=CARTESIAN_POINT('Ctrl Pts',(-18.6012488486708,12.7765325225082,
0.));
#239742=CARTESIAN_POINT('Ctrl Pts',(-18.5985917525949,12.7748328937639,
0.));
#239743=CARTESIAN_POINT('Ctrl Pts',(-18.5962551167772,12.7733231262107,
0.));
#239744=CARTESIAN_POINT('Ctrl Pts',(-18.5942490615409,12.7720142287169,
0.));
#239745=CARTESIAN_POINT('Ctrl Pts',(-18.5925859134582,12.7709195951153,
0.));
#239746=CARTESIAN_POINT('Ctrl Pts',(-18.5912775137806,12.7700520897174,
0.));
#239747=CARTESIAN_POINT('Ctrl Pts',(-18.590332877722,12.7694215127923,0.));
#239748=CARTESIAN_POINT('Ctrl Pts',(-18.589871621842,12.7691103481996,0.));
#239749=CARTESIAN_POINT('Ctrl Pts',(-18.5896919669158,12.7689864266924,
0.));
#239750=CARTESIAN_POINT('Ctrl Pts',(-18.5896460962961,12.7689524524484,
0.));
#239751=CARTESIAN_POINT('Ctrl Pts',(-18.5896416359912,12.7689476255363,
0.));
#239752=CARTESIAN_POINT('',(-22.1787195904339,13.5685075571671,12.));
#239753=CARTESIAN_POINT('',(-22.1787195904339,13.5685075571671,0.));
#239754=CARTESIAN_POINT('Ctrl Pts',(-18.5896416359912,12.7689476255363,
12.));
#239755=CARTESIAN_POINT('Ctrl Pts',(-18.5896460962961,12.7689524524484,
12.));
#239756=CARTESIAN_POINT('Ctrl Pts',(-18.5896919669158,12.7689864266924,
12.));
#239757=CARTESIAN_POINT('Ctrl Pts',(-18.589871621842,12.7691103481996,12.));
#239758=CARTESIAN_POINT('Ctrl Pts',(-18.590332877722,12.7694215127923,12.));
#239759=CARTESIAN_POINT('Ctrl Pts',(-18.5912775137806,12.7700520897174,
12.));
#239760=CARTESIAN_POINT('Ctrl Pts',(-18.5925859134582,12.7709195951153,
12.));
#239761=CARTESIAN_POINT('Ctrl Pts',(-18.5942490615409,12.7720142287169,
12.));
#239762=CARTESIAN_POINT('Ctrl Pts',(-18.5962551167772,12.7733231262107,
12.));
#239763=CARTESIAN_POINT('Ctrl Pts',(-18.5985917525949,12.7748328937639,
12.));
#239764=CARTESIAN_POINT('Ctrl Pts',(-18.6012488486708,12.7765325225082,
12.));
#239765=CARTESIAN_POINT('Ctrl Pts',(-18.6042190183703,12.7784139605067,
12.));
#239766=CARTESIAN_POINT('Ctrl Pts',(-18.6074961535723,12.7804705387658,
12.));
#239767=CARTESIAN_POINT('Ctrl Pts',(-18.611074482622,12.7826959526924,12.));
#239768=CARTESIAN_POINT('Ctrl Pts',(-18.6149475565189,12.78508316579,12.));
#239769=CARTESIAN_POINT('Ctrl Pts',(-18.6191087624752,12.7876249657834,
12.));
#239770=CARTESIAN_POINT('Ctrl Pts',(-18.6235516265575,12.7903142925234,
12.));
#239771=CARTESIAN_POINT('Ctrl Pts',(-18.6282702819371,12.7931447451556,
12.));
#239772=CARTESIAN_POINT('Ctrl Pts',(-18.6332595057005,12.7961106222251,
12.));
#239773=CARTESIAN_POINT('Ctrl Pts',(-18.63851447924,12.7992066625264,12.));
#239774=CARTESIAN_POINT('Ctrl Pts',(-18.6440306327457,12.8024278770153,
12.));
#239775=CARTESIAN_POINT('Ctrl Pts',(-18.6498034438986,12.805769331162,12.));
#239776=CARTESIAN_POINT('Ctrl Pts',(-18.6558284825772,12.8092261933858,
12.));
#239777=CARTESIAN_POINT('Ctrl Pts',(-18.6621014624746,12.8127937909632,
12.));
#239778=CARTESIAN_POINT('Ctrl Pts',(-18.6686182952798,12.8164676687361,
12.));
#239779=CARTESIAN_POINT('Ctrl Pts',(-18.6753751301091,12.8202436318473,
12.));
#239780=CARTESIAN_POINT('Ctrl Pts',(-18.6823683094139,12.8241176980016,
12.));
#239781=CARTESIAN_POINT('Ctrl Pts',(-18.6895943376172,12.8280860635231,
12.));
#239782=CARTESIAN_POINT('Ctrl Pts',(-18.6970498410173,12.832145059979,12.));
#239783=CARTESIAN_POINT('Ctrl Pts',(-18.7047315436296,12.8362911280362,
12.));
#239784=CARTESIAN_POINT('Ctrl Pts',(-18.7126362754446,12.8405208263432,
12.));
#239785=CARTESIAN_POINT('Ctrl Pts',(-18.7207609737701,12.8448308329494,
12.));
#239786=CARTESIAN_POINT('Ctrl Pts',(-18.7291026886552,12.849217951159,12.));
#239787=CARTESIAN_POINT('Ctrl Pts',(-18.7376585820851,12.8536791086315,
12.));
#239788=CARTESIAN_POINT('Ctrl Pts',(-18.7464259171248,12.8582113455644,
12.));
#239789=CARTESIAN_POINT('Ctrl Pts',(-18.7554020493888,12.8628118054172,
12.));
#239790=CARTESIAN_POINT('Ctrl Pts',(-18.7645844169568,12.8674777239656,
12.));
#239791=CARTESIAN_POINT('Ctrl Pts',(-18.7739705329029,12.8722064211814,
12.));
#239792=CARTESIAN_POINT('Ctrl Pts',(-18.7835579840481,12.8769952998097,
12.));
#239793=CARTESIAN_POINT('Ctrl Pts',(-18.7933444285867,12.8818418427474,
12.));
#239794=CARTESIAN_POINT('Ctrl Pts',(-18.8033275941939,12.8867436109543,
12.));
#239795=CARTESIAN_POINT('Ctrl Pts',(-18.8135052757815,12.8916982409931,
12.));
#239796=CARTESIAN_POINT('Ctrl Pts',(-18.8238753319124,12.8967034410752,
12.));
#239797=CARTESIAN_POINT('Ctrl Pts',(-18.834435681259,12.9017569871738,12.));
#239798=CARTESIAN_POINT('Ctrl Pts',(-18.8451842990986,12.9068567191856,
12.));
#239799=CARTESIAN_POINT('Ctrl Pts',(-18.8561192136201,12.9120005369066,
12.));
#239800=CARTESIAN_POINT('Ctrl Pts',(-18.8672385038328,12.9171863977047,
12.));
#239801=CARTESIAN_POINT('Ctrl Pts',(-18.8785402977528,12.9224123144982,
12.));
#239802=CARTESIAN_POINT('Ctrl Pts',(-18.8900227704888,12.9276763536372,
12.));
#239803=CARTESIAN_POINT('Ctrl Pts',(-18.9016841423402,12.9329766328184,
12.));
#239804=CARTESIAN_POINT('Ctrl Pts',(-18.9135226769466,12.9383113190375,
12.));
#239805=CARTESIAN_POINT('Ctrl Pts',(-18.9255366795196,12.9436786266106,
12.));
#239806=CARTESIAN_POINT('Ctrl Pts',(-18.9377244950435,12.9490768151821,
12.));
#239807=CARTESIAN_POINT('Ctrl Pts',(-18.9500845064714,12.9545041877377,
12.));
#239808=CARTESIAN_POINT('Ctrl Pts',(-18.9626151329226,12.9599590886317,
12.));
#239809=CARTESIAN_POINT('Ctrl Pts',(-18.9753148284473,12.9654399021868,
12.));
#239810=CARTESIAN_POINT('Ctrl Pts',(-18.9881820807585,12.9709450512747,
12.));
#239811=CARTESIAN_POINT('Ctrl Pts',(-19.0012154099792,12.9764729959206,
12.));
#239812=CARTESIAN_POINT('Ctrl Pts',(-19.014413367335,12.9820222318716,12.));
#239813=CARTESIAN_POINT('Ctrl Pts',(-19.0277745339909,12.9875912893003,
12.));
#239814=CARTESIAN_POINT('Ctrl Pts',(-19.0412975200398,12.9931787316514,
12.));
#239815=CARTESIAN_POINT('Ctrl Pts',(-19.0549809634354,12.9987831544502,
12.));
#239816=CARTESIAN_POINT('Ctrl Pts',(-19.0688235289437,13.0044031841382,
12.));
#239817=CARTESIAN_POINT('Ctrl Pts',(-19.0828239070484,13.0100374768788,
12.));
#239818=CARTESIAN_POINT('Ctrl Pts',(-19.0969808131228,13.0156847176096,
12.));
#239819=CARTESIAN_POINT('Ctrl Pts',(-19.111292986631,13.0213436191328,12.));
#239820=CARTESIAN_POINT('Ctrl Pts',(-19.1257591903099,13.0270129211976,
12.));
#239821=CARTESIAN_POINT('Ctrl Pts',(-19.1403782093386,13.0326913895838,
12.));
#239822=CARTESIAN_POINT('Ctrl Pts',(-19.155148850523,13.0383778152068,12.));
#239823=CARTESIAN_POINT('Ctrl Pts',(-19.1700699416622,13.0440710133772,
12.));
#239824=CARTESIAN_POINT('Ctrl Pts',(-19.1851403308825,13.0497698230441,
12.));
#239825=CARTESIAN_POINT('Ctrl Pts',(-19.2003588859772,13.0554731060538,
12.));
#239826=CARTESIAN_POINT('Ctrl Pts',(-19.2157244937142,13.0611797463915,
12.));
#239827=CARTESIAN_POINT('Ctrl Pts',(-19.2312360592033,13.0668886494795,
12.));
#239828=CARTESIAN_POINT('Ctrl Pts',(-19.2468925053989,13.0725987415859,
12.));
#239829=CARTESIAN_POINT('Ctrl Pts',(-19.2626927725596,13.0783089692118,
12.));
#239830=CARTESIAN_POINT('Ctrl Pts',(-19.2786358177198,13.0840182984949,
12.));
#239831=CARTESIAN_POINT('Ctrl Pts',(-19.2947206141247,13.0897257145968,
12.));
#239832=CARTESIAN_POINT('Ctrl Pts',(-19.310946150736,13.0954302211479,12.));
#239833=CARTESIAN_POINT('Ctrl Pts',(-19.3273114318269,13.1011308397591,
12.));
#239834=CARTESIAN_POINT('Ctrl Pts',(-19.3438154765395,13.1068266095186,
12.));
#239835=CARTESIAN_POINT('Ctrl Pts',(-19.3604573184515,13.1125165865022,
12.));
#239836=CARTESIAN_POINT('Ctrl Pts',(-19.3772360051091,13.118199843271,12.));
#239837=CARTESIAN_POINT('Ctrl Pts',(-19.3941505976263,13.1238754684177,
12.));
#239838=CARTESIAN_POINT('Ctrl Pts',(-19.4112001703557,13.1295425661634,
12.));
#239839=CARTESIAN_POINT('Ctrl Pts',(-19.4283838105262,13.1352002559438,
12.));
#239840=CARTESIAN_POINT('Ctrl Pts',(-19.4457006178876,13.1408476720061,
12.));
#239841=CARTESIAN_POINT('Ctrl Pts',(-19.4631497043258,13.1464839629971,
12.));
#239842=CARTESIAN_POINT('Ctrl Pts',(-19.4807301935268,13.1521082915853,
12.));
#239843=CARTESIAN_POINT('Ctrl Pts',(-19.4984412207082,13.1577198341245,
12.));
#239844=CARTESIAN_POINT('Ctrl Pts',(-19.5162819323213,13.1633177803101,
12.));
#239845=CARTESIAN_POINT('Ctrl Pts',(-19.5342514857562,13.168901332843,12.));
#239846=CARTESIAN_POINT('Ctrl Pts',(-19.5523490490244,13.1744697070911,
12.));
#239847=CARTESIAN_POINT('Ctrl Pts',(-19.5705738004667,13.1800221307673,
12.));
#239848=CARTESIAN_POINT('Ctrl Pts',(-19.5889249285338,13.1855578436471,
12.));
#239849=CARTESIAN_POINT('Ctrl Pts',(-19.6074016315414,13.1910760972814,
12.));
#239850=CARTESIAN_POINT('Ctrl Pts',(-19.6260031174244,13.1965761547151,
12.));
#239851=CARTESIAN_POINT('Ctrl Pts',(-19.6447286034772,13.2020572902065,
12.));
#239852=CARTESIAN_POINT('Ctrl Pts',(-19.6635773160936,13.2075187889529,
12.));
#239853=CARTESIAN_POINT('Ctrl Pts',(-19.6825484905823,13.2129599468485,
12.));
#239854=CARTESIAN_POINT('Ctrl Pts',(-19.7016413709685,13.2183800702436,
12.));
#239855=CARTESIAN_POINT('Ctrl Pts',(-19.7208552097868,13.2237784757065,
12.));
#239856=CARTESIAN_POINT('Ctrl Pts',(-19.7401892678697,13.2291544897899,
12.));
#239857=CARTESIAN_POINT('Ctrl Pts',(-19.7596428141168,13.2345074487963,
12.));
#239858=CARTESIAN_POINT('Ctrl Pts',(-19.7792151253289,13.2398366985675,
12.));
#239859=CARTESIAN_POINT('Ctrl Pts',(-19.7989054860495,13.2451415942805,
12.));
#239860=CARTESIAN_POINT('Ctrl Pts',(-19.8187131883917,13.2504215002457,
12.));
#239861=CARTESIAN_POINT('Ctrl Pts',(-19.8386375318634,13.2556757897086,
12.));
#239862=CARTESIAN_POINT('Ctrl Pts',(-19.8586778231715,13.2609038446529,
12.));
#239863=CARTESIAN_POINT('Ctrl Pts',(-19.8788333760577,13.2661050556132,
12.));
#239864=CARTESIAN_POINT('Ctrl Pts',(-19.8991035111745,13.271278821502,12.));
#239865=CARTESIAN_POINT('Ctrl Pts',(-19.9194875559422,13.2764245494357,
12.));
#239866=CARTESIAN_POINT('Ctrl Pts',(-19.9399848444019,13.2815416545663,
12.));
#239867=CARTESIAN_POINT('Ctrl Pts',(-19.9605947170586,13.286629559915,12.));
#239868=CARTESIAN_POINT('Ctrl Pts',(-19.981316520717,13.2916876962094,12.));
#239869=CARTESIAN_POINT('Ctrl Pts',(-20.0021496083738,13.2967155017306,
12.));
#239870=CARTESIAN_POINT('Ctrl Pts',(-20.0230933391038,13.3017124221637,
12.));
#239871=CARTESIAN_POINT('Ctrl Pts',(-20.0441470779345,13.3066779104515,
12.));
#239872=CARTESIAN_POINT('Ctrl Pts',(-20.0653101957188,13.3116114266515,
12.));
#239873=CARTESIAN_POINT('Ctrl Pts',(-20.0865820689883,13.3165124377962,
12.));
#239874=CARTESIAN_POINT('Ctrl Pts',(-20.1079620798375,13.3213804177587,
12.));
#239875=CARTESIAN_POINT('Ctrl Pts',(-20.1294496158402,13.3262148471226,
12.));
#239876=CARTESIAN_POINT('Ctrl Pts',(-20.1510440699474,13.3310152130564,
12.));
#239877=CARTESIAN_POINT('Ctrl Pts',(-20.1727448403817,13.3357810091903,
12.));
#239878=CARTESIAN_POINT('Ctrl Pts',(-20.1945513305235,13.3405117354971,
12.));
#239879=CARTESIAN_POINT('Ctrl Pts',(-20.216462948786,13.3452068981766,12.));
#239880=CARTESIAN_POINT('Ctrl Pts',(-20.2384791085359,13.3498660095386,
12.));
#239881=CARTESIAN_POINT('Ctrl Pts',(-20.2605992280122,13.3544885878889,
12.));
#239882=CARTESIAN_POINT('Ctrl Pts',(-20.2828227302339,13.3590741574195,
12.));
#239883=CARTESIAN_POINT('Ctrl Pts',(-20.3051490429048,13.3636222481016,
12.));
#239884=CARTESIAN_POINT('Ctrl Pts',(-20.3275775983029,13.3681323955826,
12.));
#239885=CARTESIAN_POINT('Ctrl Pts',(-20.3501078331814,13.3726041410867,
12.));
#239886=CARTESIAN_POINT('Ctrl Pts',(-20.3727391887184,13.3770370313188,
12.));
#239887=CARTESIAN_POINT('Ctrl Pts',(-20.3954711104502,13.3814306183719,
12.));
#239888=CARTESIAN_POINT('Ctrl Pts',(-20.4183030482002,13.3857844596387,
12.));
#239889=CARTESIAN_POINT('Ctrl Pts',(-20.4412344560008,13.3900981177255,
12.));
#239890=CARTESIAN_POINT('Ctrl Pts',(-20.4642647920038,13.3943711603739,
12.));
#239891=CARTESIAN_POINT('Ctrl Pts',(-20.487393518404,13.3986031603716,12.));
#239892=CARTESIAN_POINT('Ctrl Pts',(-20.5106201013753,13.4027936954529,
12.));
#239893=CARTESIAN_POINT('Ctrl Pts',(-20.5339440109956,13.4069423482076,
12.));
#239894=CARTESIAN_POINT('Ctrl Pts',(-20.5573647211639,13.4110487059912,
12.));
#239895=CARTESIAN_POINT('Ctrl Pts',(-20.5808817095155,13.4151123608411,
12.));
#239896=CARTESIAN_POINT('Ctrl Pts',(-20.6044944573153,13.4191329093932,
12.));
#239897=CARTESIAN_POINT('Ctrl Pts',(-20.6282024494237,13.4231099528179,
12.));
#239898=CARTESIAN_POINT('Ctrl Pts',(-20.6520051742869,13.4270430967651,
12.));
#239899=CARTESIAN_POINT('Ctrl Pts',(-20.6759021239103,13.4309319513119,
12.));
#239900=CARTESIAN_POINT('Ctrl Pts',(-20.6998927938288,13.4347761309154,
12.));
#239901=CARTESIAN_POINT('Ctrl Pts',(-20.7239766830675,13.4385752543663,
12.));
#239902=CARTESIAN_POINT('Ctrl Pts',(-20.7481532941013,13.4423289447561,
12.));
#239903=CARTESIAN_POINT('Ctrl Pts',(-20.7724221327608,13.4460368293688,
12.));
#239904=CARTESIAN_POINT('Ctrl Pts',(-20.7967827081227,13.4496985395637,
12.));
#239905=CARTESIAN_POINT('Ctrl Pts',(-20.821234532398,13.4533137106667,12.));
#239906=CARTESIAN_POINT('Ctrl Pts',(-20.8457771208082,13.4568819818631,
12.));
#239907=CARTESIAN_POINT('Ctrl Pts',(-20.8704099914641,13.4604029960983,
12.));
#239908=CARTESIAN_POINT('Ctrl Pts',(-20.8951326652158,13.4638763999725,
12.));
#239909=CARTESIAN_POINT('Ctrl Pts',(-20.9199446657584,13.4673018437718,
12.));
#239910=CARTESIAN_POINT('Ctrl Pts',(-20.9448455197557,13.4706789815166,
12.));
#239911=CARTESIAN_POINT('Ctrl Pts',(-20.9698347569476,13.4740074710087,
12.));
#239912=CARTESIAN_POINT('Ctrl Pts',(-20.9949119102592,13.4772869738879,
12.));
#239913=CARTESIAN_POINT('Ctrl Pts',(-21.0200765158885,13.4805171556822,
12.));
#239914=CARTESIAN_POINT('Ctrl Pts',(-21.0453281134247,13.4836976858912,
12.));
#239915=CARTESIAN_POINT('Ctrl Pts',(-21.0706662455202,13.4868282377191,
12.));
#239916=CARTESIAN_POINT('Ctrl Pts',(-21.0960904575048,13.4899084877718,
12.));
#239917=CARTESIAN_POINT('Ctrl Pts',(-21.1216002970209,13.4929381157778,
12.));
#239918=CARTESIAN_POINT('Ctrl Pts',(-21.1471953136209,13.4959168042934,
12.));
#239919=CARTESIAN_POINT('Ctrl Pts',(-21.1728750584173,13.4988442384491,
12.));
#239920=CARTESIAN_POINT('Ctrl Pts',(-21.1986390835825,13.5017201056088,
12.));
#239921=CARTESIAN_POINT('Ctrl Pts',(-21.224486942933,13.5045440957404,12.));
#239922=CARTESIAN_POINT('Ctrl Pts',(-21.2504181927429,13.5073159019454,
12.));
#239923=CARTESIAN_POINT('Ctrl Pts',(-21.2764323924442,13.5100352209207,
12.));
#239924=CARTESIAN_POINT('Ctrl Pts',(-21.3025291054236,13.5127017534972,
12.));
#239925=CARTESIAN_POINT('Ctrl Pts',(-21.328707899634,13.5153152050554,12.));
#239926=CARTESIAN_POINT('Ctrl Pts',(-21.3549683486219,13.5178752862461,
12.));
#239927=CARTESIAN_POINT('Ctrl Pts',(-21.3813100304967,13.5203817122496,
12.));
#239928=CARTESIAN_POINT('Ctrl Pts',(-21.4077325259318,13.5228342013508,
12.));
#239929=CARTESIAN_POINT('Ctrl Pts',(-21.4342354165254,13.5252324737795,
12.));
#239930=CARTESIAN_POINT('Ctrl Pts',(-21.4608182828695,13.5275762503553,
12.));
#239931=CARTESIAN_POINT('Ctrl Pts',(-21.487480703047,13.5298652514357,12.));
#239932=CARTESIAN_POINT('Ctrl Pts',(-21.5142222501671,13.5320991952145,
12.));
#239933=CARTESIAN_POINT('Ctrl Pts',(-21.5410424932511,13.5342777983225,
12.));
#239934=CARTESIAN_POINT('Ctrl Pts',(-21.5679410019011,13.5364007790292,
12.));
#239935=CARTESIAN_POINT('Ctrl Pts',(-21.5949173499022,13.5384678597206,
12.));
#239936=CARTESIAN_POINT('Ctrl Pts',(-21.6219711193951,13.5404787697798,
12.));
#239937=CARTESIAN_POINT('Ctrl Pts',(-21.6491019044647,13.5424332480698,
12.));
#239938=CARTESIAN_POINT('Ctrl Pts',(-21.676309315769,13.5443310461516,12.));
#239939=CARTESIAN_POINT('Ctrl Pts',(-21.7035929822939,13.546171929503,12.));
#239940=CARTESIAN_POINT('Ctrl Pts',(-21.730952541226,13.5479556704457,12.));
#239941=CARTESIAN_POINT('Ctrl Pts',(-21.7583876294532,13.5496820422186,
12.));
#239942=CARTESIAN_POINT('Ctrl Pts',(-21.7858978745848,13.5513508127232,
12.));
#239943=CARTESIAN_POINT('Ctrl Pts',(-21.8134828857963,13.5529617381569,
12.));
#239944=CARTESIAN_POINT('Ctrl Pts',(-21.841142245609,13.5545145573048,12.));
#239945=CARTESIAN_POINT('Ctrl Pts',(-21.8688754989401,13.5560089839426,
12.));
#239946=CARTESIAN_POINT('Ctrl Pts',(-21.8966821688876,13.5574447178484,
12.));
#239947=CARTESIAN_POINT('Ctrl Pts',(-21.9245617765827,13.5588214586672,
12.));
#239948=CARTESIAN_POINT('Ctrl Pts',(-21.9525138592862,13.5601389185315,
12.));
#239949=CARTESIAN_POINT('Ctrl Pts',(-21.9805379899192,13.5613968357589,
12.));
#239950=CARTESIAN_POINT('Ctrl Pts',(-22.0086337943431,13.5625949868313,
12.));
#239951=CARTESIAN_POINT('Ctrl Pts',(-22.0368009736227,13.5637332022393,
12.));
#239952=CARTESIAN_POINT('Ctrl Pts',(-22.0650393089492,13.5648113688894,
12.));
#239953=CARTESIAN_POINT('Ctrl Pts',(-22.0933486464442,13.5658294169106,
12.));
#239954=CARTESIAN_POINT('Ctrl Pts',(-22.1217288871823,13.5667873105179,
12.));
#239955=CARTESIAN_POINT('Ctrl Pts',(-22.1444897575076,13.5675054918922,
12.));
#239956=CARTESIAN_POINT('Ctrl Pts',(-22.1615922804939,13.5680170531724,
12.));
#239957=CARTESIAN_POINT('Ctrl Pts',(-22.1730081264583,13.5683460612913,
12.));
#239958=CARTESIAN_POINT('Ctrl Pts',(-22.1787195904339,13.5685075571671,
12.));
#239959=CARTESIAN_POINT('Ctrl Pts',(-17.1452095830633,14.6513681262571,
0.));
#239960=CARTESIAN_POINT('Ctrl Pts',(-17.1452095830633,14.6513681262571,
12.));
#239961=CARTESIAN_POINT('Ctrl Pts',(-17.1452153999142,14.6513711852843,
0.));
#239962=CARTESIAN_POINT('Ctrl Pts',(-17.1452153999142,14.6513711852843,
12.));
#239963=CARTESIAN_POINT('Ctrl Pts',(-17.1452600887037,14.6514066997196,
0.));
#239964=CARTESIAN_POINT('Ctrl Pts',(-17.1452600887037,14.6514066997196,
12.));
#239965=CARTESIAN_POINT('Ctrl Pts',(-17.1454262858043,14.6515481598068,
0.));
#239966=CARTESIAN_POINT('Ctrl Pts',(-17.1454262858043,14.6515481598068,
12.));
#239967=CARTESIAN_POINT('Ctrl Pts',(-17.1458462295271,14.6519131634508,
0.));
#239968=CARTESIAN_POINT('Ctrl Pts',(-17.1458462295271,14.6519131634508,
12.));
#239969=CARTESIAN_POINT('Ctrl Pts',(-17.1466998098673,14.6526624064978,
0.));
#239970=CARTESIAN_POINT('Ctrl Pts',(-17.1466998098673,14.6526624064978,
12.));
#239971=CARTESIAN_POINT('Ctrl Pts',(-17.147876394491,14.6537016966184,0.));
#239972=CARTESIAN_POINT('Ctrl Pts',(-17.147876394491,14.6537016966184,12.));
#239973=CARTESIAN_POINT('Ctrl Pts',(-17.1493641837558,14.655024862281,0.));
#239974=CARTESIAN_POINT('Ctrl Pts',(-17.1493641837558,14.655024862281,12.));
#239975=CARTESIAN_POINT('Ctrl Pts',(-17.1511476869496,14.6566237952435,
0.));
#239976=CARTESIAN_POINT('Ctrl Pts',(-17.1511476869496,14.6566237952435,
12.));
#239977=CARTESIAN_POINT('Ctrl Pts',(-17.1532107762718,14.6584900555302,
0.));
#239978=CARTESIAN_POINT('Ctrl Pts',(-17.1532107762718,14.6584900555302,
12.));
#239979=CARTESIAN_POINT('Ctrl Pts',(-17.1555401986401,14.6606167169642,
0.));
#239980=CARTESIAN_POINT('Ctrl Pts',(-17.1555401986401,14.6606167169642,
12.));
#239981=CARTESIAN_POINT('Ctrl Pts',(-17.1581262646789,14.6629987285992,
0.));
#239982=CARTESIAN_POINT('Ctrl Pts',(-17.1581262646789,14.6629987285992,
12.));
#239983=CARTESIAN_POINT('Ctrl Pts',(-17.1609609517369,14.6656319165057,
0.));
#239984=CARTESIAN_POINT('Ctrl Pts',(-17.1609609517369,14.6656319165057,
12.));
#239985=CARTESIAN_POINT('Ctrl Pts',(-17.1640366762305,14.6685123374423,
0.));
#239986=CARTESIAN_POINT('Ctrl Pts',(-17.1640366762305,14.6685123374423,
12.));
#239987=CARTESIAN_POINT('Ctrl Pts',(-17.167344972302,14.671635583332,0.));
#239988=CARTESIAN_POINT('Ctrl Pts',(-17.167344972302,14.671635583332,12.));
#239989=CARTESIAN_POINT('Ctrl Pts',(-17.1708771619129,14.6749971333867,
0.));
#239990=CARTESIAN_POINT('Ctrl Pts',(-17.1708771619129,14.6749971333867,
12.));
#239991=CARTESIAN_POINT('Ctrl Pts',(-17.1746247499057,14.6785925615677,
0.));
#239992=CARTESIAN_POINT('Ctrl Pts',(-17.1746247499057,14.6785925615677,
12.));
#239993=CARTESIAN_POINT('Ctrl Pts',(-17.1785800350826,14.6824178576167,
0.));
#239994=CARTESIAN_POINT('Ctrl Pts',(-17.1785800350826,14.6824178576167,
12.));
#239995=CARTESIAN_POINT('Ctrl Pts',(-17.182736158472,14.686469452232,0.));
#239996=CARTESIAN_POINT('Ctrl Pts',(-17.182736158472,14.686469452232,12.));
#239997=CARTESIAN_POINT('Ctrl Pts',(-17.1870867909918,14.6907440526958,
0.));
#239998=CARTESIAN_POINT('Ctrl Pts',(-17.1870867909918,14.6907440526958,
12.));
#239999=CARTESIAN_POINT('Ctrl Pts',(-17.1916259308415,14.6952385361705,
0.));
#240000=CARTESIAN_POINT('Ctrl Pts',(-17.1916259308415,14.6952385361705,
12.));
#240001=CARTESIAN_POINT('Ctrl Pts',(-17.1963476411694,14.699949811582,0.));
#240002=CARTESIAN_POINT('Ctrl Pts',(-17.1963476411694,14.699949811582,12.));
#240003=CARTESIAN_POINT('Ctrl Pts',(-17.2012461084268,14.7048748502663,
0.));
#240004=CARTESIAN_POINT('Ctrl Pts',(-17.2012461084268,14.7048748502663,
12.));
#240005=CARTESIAN_POINT('Ctrl Pts',(-17.2063157097315,14.7100107213586,
0.));
#240006=CARTESIAN_POINT('Ctrl Pts',(-17.2063157097315,14.7100107213586,
12.));
#240007=CARTESIAN_POINT('Ctrl Pts',(-17.2115510835989,14.7153546289339,
0.));
#240008=CARTESIAN_POINT('Ctrl Pts',(-17.2115510835989,14.7153546289339,
12.));
#240009=CARTESIAN_POINT('Ctrl Pts',(-17.2169471814256,14.7209039390327,
0.));
#240010=CARTESIAN_POINT('Ctrl Pts',(-17.2169471814256,14.7209039390327,
12.));
#240011=CARTESIAN_POINT('Ctrl Pts',(-17.2224992099667,14.7266561494282,
0.));
#240012=CARTESIAN_POINT('Ctrl Pts',(-17.2224992099667,14.7266561494282,
12.));
#240013=CARTESIAN_POINT('Ctrl Pts',(-17.2282025904314,14.7326088681163,
0.));
#240014=CARTESIAN_POINT('Ctrl Pts',(-17.2282025904314,14.7326088681163,
12.));
#240015=CARTESIAN_POINT('Ctrl Pts',(-17.2340529062076,14.7387597858116,
0.));
#240016=CARTESIAN_POINT('Ctrl Pts',(-17.2340529062076,14.7387597858116,
12.));
#240017=CARTESIAN_POINT('Ctrl Pts',(-17.2400458713565,14.7451066593792,
0.));
#240018=CARTESIAN_POINT('Ctrl Pts',(-17.2400458713565,14.7451066593792,
12.));
#240019=CARTESIAN_POINT('Ctrl Pts',(-17.2461773413288,14.7516473175124,
0.));
#240020=CARTESIAN_POINT('Ctrl Pts',(-17.2461773413288,14.7516473175124,
12.));
#240021=CARTESIAN_POINT('Ctrl Pts',(-17.2524433146837,14.7583796616617,
0.));
#240022=CARTESIAN_POINT('Ctrl Pts',(-17.2524433146837,14.7583796616617,
12.));
#240023=CARTESIAN_POINT('Ctrl Pts',(-17.2588399401465,14.7653016697591,
0.));
#240024=CARTESIAN_POINT('Ctrl Pts',(-17.2588399401465,14.7653016697591,
12.));
#240025=CARTESIAN_POINT('Ctrl Pts',(-17.2653635155319,14.7724113956731,
0.));
#240026=CARTESIAN_POINT('Ctrl Pts',(-17.2653635155319,14.7724113956731,
12.));
#240027=CARTESIAN_POINT('Ctrl Pts',(-17.2720104735194,14.7797069617804,
0.));
#240028=CARTESIAN_POINT('Ctrl Pts',(-17.2720104735194,14.7797069617804,
12.));
#240029=CARTESIAN_POINT('Ctrl Pts',(-17.2787773704849,14.787186553128,0.));
#240030=CARTESIAN_POINT('Ctrl Pts',(-17.2787773704849,14.787186553128,12.));
#240031=CARTESIAN_POINT('Ctrl Pts',(-17.2856608733196,14.7948484105249,
0.));
#240032=CARTESIAN_POINT('Ctrl Pts',(-17.2856608733196,14.7948484105249,
12.));
#240033=CARTESIAN_POINT('Ctrl Pts',(-17.2926577496513,14.8026908254276,
0.));
#240034=CARTESIAN_POINT('Ctrl Pts',(-17.2926577496513,14.8026908254276,
12.));
#240035=CARTESIAN_POINT('Ctrl Pts',(-17.299764866148,14.8107121391035,0.));
#240036=CARTESIAN_POINT('Ctrl Pts',(-17.299764866148,14.8107121391035,12.));
#240037=CARTESIAN_POINT('Ctrl Pts',(-17.3069791853706,14.8189107410162,
0.));
#240038=CARTESIAN_POINT('Ctrl Pts',(-17.3069791853706,14.8189107410162,
12.));
#240039=CARTESIAN_POINT('Ctrl Pts',(-17.3142977632659,14.8272850675379,
0.));
#240040=CARTESIAN_POINT('Ctrl Pts',(-17.3142977632659,14.8272850675379,
12.));
#240041=CARTESIAN_POINT('Ctrl Pts',(-17.3217177462101,14.8358336004197,
0.));
#240042=CARTESIAN_POINT('Ctrl Pts',(-17.3217177462101,14.8358336004197,
12.));
#240043=CARTESIAN_POINT('Ctrl Pts',(-17.3292363662605,14.8445548643508,
0.));
#240044=CARTESIAN_POINT('Ctrl Pts',(-17.3292363662605,14.8445548643508,
12.));
#240045=CARTESIAN_POINT('Ctrl Pts',(-17.336850936485,14.8534474245433,0.));
#240046=CARTESIAN_POINT('Ctrl Pts',(-17.336850936485,14.8534474245433,12.));
#240047=CARTESIAN_POINT('Ctrl Pts',(-17.3445588463475,14.8625098843417,
0.));
#240048=CARTESIAN_POINT('Ctrl Pts',(-17.3445588463475,14.8625098843417,
12.));
#240049=CARTESIAN_POINT('Ctrl Pts',(-17.3523575568645,14.8717408826955,
0.));
#240050=CARTESIAN_POINT('Ctrl Pts',(-17.3523575568645,14.8717408826955,
12.));
#240051=CARTESIAN_POINT('Ctrl Pts',(-17.3602445978161,14.8811390927423,
0.));
#240052=CARTESIAN_POINT('Ctrl Pts',(-17.3602445978161,14.8811390927423,
12.));
#240053=CARTESIAN_POINT('Ctrl Pts',(-17.3682175653235,14.8907032205788,
0.));
#240054=CARTESIAN_POINT('Ctrl Pts',(-17.3682175653235,14.8907032205788,
12.));
#240055=CARTESIAN_POINT('Ctrl Pts',(-17.3762741193076,14.900432003961,0.));
#240056=CARTESIAN_POINT('Ctrl Pts',(-17.3762741193076,14.900432003961,12.));
#240057=CARTESIAN_POINT('Ctrl Pts',(-17.3844119809824,14.9103242110057,
0.));
#240058=CARTESIAN_POINT('Ctrl Pts',(-17.3844119809824,14.9103242110057,
12.));
#240059=CARTESIAN_POINT('Ctrl Pts',(-17.3926289303986,14.9203786389342,
0.));
#240060=CARTESIAN_POINT('Ctrl Pts',(-17.3926289303986,14.9203786389342,
12.));
#240061=CARTESIAN_POINT('Ctrl Pts',(-17.4009228040749,14.9305941128757,
0.));
#240062=CARTESIAN_POINT('Ctrl Pts',(-17.4009228040749,14.9305941128757,
12.));
#240063=CARTESIAN_POINT('Ctrl Pts',(-17.4092914926071,14.940969484645,0.));
#240064=CARTESIAN_POINT('Ctrl Pts',(-17.4092914926071,14.940969484645,12.));
#240065=CARTESIAN_POINT('Ctrl Pts',(-17.4177329382828,14.9515036315143,
0.));
#240066=CARTESIAN_POINT('Ctrl Pts',(-17.4177329382828,14.9515036315143,
12.));
#240067=CARTESIAN_POINT('Ctrl Pts',(-17.426245132709,14.9621954549827,0.));
#240068=CARTESIAN_POINT('Ctrl Pts',(-17.426245132709,14.9621954549827,12.));
#240069=CARTESIAN_POINT('Ctrl Pts',(-17.4348261151396,14.9730438799452,
0.));
#240070=CARTESIAN_POINT('Ctrl Pts',(-17.4348261151396,14.9730438799452,
12.));
#240071=CARTESIAN_POINT('Ctrl Pts',(-17.4434739707773,14.9840478538358,
0.));
#240072=CARTESIAN_POINT('Ctrl Pts',(-17.4434739707773,14.9840478538358,
12.));
#240073=CARTESIAN_POINT('Ctrl Pts',(-17.4521868291004,14.9952063457778,
0.));
#240074=CARTESIAN_POINT('Ctrl Pts',(-17.4521868291004,14.9952063457778,
12.));
#240075=CARTESIAN_POINT('Ctrl Pts',(-17.4609628621418,15.0065183456921,
0.));
#240076=CARTESIAN_POINT('Ctrl Pts',(-17.4609628621418,15.0065183456921,
12.));
#240077=CARTESIAN_POINT('Ctrl Pts',(-17.4698002829357,15.0179828635086,
0.));
#240078=CARTESIAN_POINT('Ctrl Pts',(-17.4698002829357,15.0179828635086,
12.));
#240079=CARTESIAN_POINT('Ctrl Pts',(-17.4786973441417,15.029598928488,0.));
#240080=CARTESIAN_POINT('Ctrl Pts',(-17.4786973441417,15.029598928488,12.));
#240081=CARTESIAN_POINT('Ctrl Pts',(-17.4876523366178,15.0413655884993,
0.));
#240082=CARTESIAN_POINT('Ctrl Pts',(-17.4876523366178,15.0413655884993,
12.));
#240083=CARTESIAN_POINT('Ctrl Pts',(-17.4966635880245,15.0532819093085,
0.));
#240084=CARTESIAN_POINT('Ctrl Pts',(-17.4966635880245,15.0532819093085,
12.));
#240085=CARTESIAN_POINT('Ctrl Pts',(-17.5057294613874,15.0653469738306,
0.));
#240086=CARTESIAN_POINT('Ctrl Pts',(-17.5057294613874,15.0653469738306,
12.));
#240087=CARTESIAN_POINT('Ctrl Pts',(-17.5148483539684,15.0775598815748,
0.));
#240088=CARTESIAN_POINT('Ctrl Pts',(-17.5148483539684,15.0775598815748,
12.));
#240089=CARTESIAN_POINT('Ctrl Pts',(-17.5240186961788,15.0899197481082,
0.));
#240090=CARTESIAN_POINT('Ctrl Pts',(-17.5240186961788,15.0899197481082,
12.));
#240091=CARTESIAN_POINT('Ctrl Pts',(-17.5332389504829,15.1024257045033,
0.));
#240092=CARTESIAN_POINT('Ctrl Pts',(-17.5332389504829,15.1024257045033,
12.));
#240093=CARTESIAN_POINT('Ctrl Pts',(-17.5425076102966,15.1150768967729,
0.));
#240094=CARTESIAN_POINT('Ctrl Pts',(-17.5425076102966,15.1150768967729,
12.));
#240095=CARTESIAN_POINT('Ctrl Pts',(-17.5518231989122,15.127872485314,0.));
#240096=CARTESIAN_POINT('Ctrl Pts',(-17.5518231989122,15.127872485314,12.));
#240097=CARTESIAN_POINT('Ctrl Pts',(-17.5611842686196,15.1408116444877,
0.));
#240098=CARTESIAN_POINT('Ctrl Pts',(-17.5611842686196,15.1408116444877,
12.));
#240099=CARTESIAN_POINT('Ctrl Pts',(-17.570589399803,15.1538935621714,0.));
#240100=CARTESIAN_POINT('Ctrl Pts',(-17.570589399803,15.1538935621714,12.));
#240101=CARTESIAN_POINT('Ctrl Pts',(-17.5800372000539,15.1671174393136,
0.));
#240102=CARTESIAN_POINT('Ctrl Pts',(-17.5800372000539,15.1671174393136,
12.));
#240103=CARTESIAN_POINT('Ctrl Pts',(-17.5895263032592,15.1804824894605,
0.));
#240104=CARTESIAN_POINT('Ctrl Pts',(-17.5895263032592,15.1804824894605,
12.));
#240105=CARTESIAN_POINT('Ctrl Pts',(-17.5990553687595,15.1939879383268,
0.));
#240106=CARTESIAN_POINT('Ctrl Pts',(-17.5990553687595,15.1939879383268,
12.));
#240107=CARTESIAN_POINT('Ctrl Pts',(-17.6086230806497,15.2076330234686,
0.));
#240108=CARTESIAN_POINT('Ctrl Pts',(-17.6086230806497,15.2076330234686,
12.));
#240109=CARTESIAN_POINT('Ctrl Pts',(-17.6182281470467,15.22141699392,0.));
#240110=CARTESIAN_POINT('Ctrl Pts',(-17.6182281470467,15.22141699392,12.));
#240111=CARTESIAN_POINT('Ctrl Pts',(-17.6278692993765,15.2353391098367,
0.));
#240112=CARTESIAN_POINT('Ctrl Pts',(-17.6278692993765,15.2353391098367,
12.));
#240113=CARTESIAN_POINT('Ctrl Pts',(-17.637545291637,15.2493986421091,0.));
#240114=CARTESIAN_POINT('Ctrl Pts',(-17.637545291637,15.2493986421091,12.));
#240115=CARTESIAN_POINT('Ctrl Pts',(-17.6472548997329,15.263594872029,0.));
#240116=CARTESIAN_POINT('Ctrl Pts',(-17.6472548997329,15.263594872029,12.));
#240117=CARTESIAN_POINT('Ctrl Pts',(-17.6569969209,15.2779270910238,0.));
#240118=CARTESIAN_POINT('Ctrl Pts',(-17.6569969209,15.2779270910238,12.));
#240119=CARTESIAN_POINT('Ctrl Pts',(-17.6667701731041,15.2923946003598,
0.));
#240120=CARTESIAN_POINT('Ctrl Pts',(-17.6667701731041,15.2923946003598,
12.));
#240121=CARTESIAN_POINT('Ctrl Pts',(-17.6765734944559,15.3069967108501,
0.));
#240122=CARTESIAN_POINT('Ctrl Pts',(-17.6765734944559,15.3069967108501,
12.));
#240123=CARTESIAN_POINT('Ctrl Pts',(-17.6864057426052,15.3217327425341,
0.));
#240124=CARTESIAN_POINT('Ctrl Pts',(-17.6864057426052,15.3217327425341,
12.));
#240125=CARTESIAN_POINT('Ctrl Pts',(-17.6962657941984,15.3366020244069,
0.));
#240126=CARTESIAN_POINT('Ctrl Pts',(-17.6962657941984,15.3366020244069,
12.));
#240127=CARTESIAN_POINT('Ctrl Pts',(-17.7061525444044,15.3516038942064,
0.));
#240128=CARTESIAN_POINT('Ctrl Pts',(-17.7061525444044,15.3516038942064,
12.));
#240129=CARTESIAN_POINT('Ctrl Pts',(-17.7160649064208,15.3667376981702,
0.));
#240130=CARTESIAN_POINT('Ctrl Pts',(-17.7160649064208,15.3667376981702,
12.));
#240131=CARTESIAN_POINT('Ctrl Pts',(-17.7260018109923,15.3820027907965,
0.));
#240132=CARTESIAN_POINT('Ctrl Pts',(-17.7260018109923,15.3820027907965,
12.));
#240133=CARTESIAN_POINT('Ctrl Pts',(-17.7359622059143,15.3973985345796,
0.));
#240134=CARTESIAN_POINT('Ctrl Pts',(-17.7359622059143,15.3973985345796,
12.));
#240135=CARTESIAN_POINT('Ctrl Pts',(-17.7459450555803,15.4129242997828,
0.));
#240136=CARTESIAN_POINT('Ctrl Pts',(-17.7459450555803,15.4129242997828,
12.));
#240137=CARTESIAN_POINT('Ctrl Pts',(-17.7559493405871,15.4285794642658,
0.));
#240138=CARTESIAN_POINT('Ctrl Pts',(-17.7559493405871,15.4285794642658,
12.));
#240139=CARTESIAN_POINT('Ctrl Pts',(-17.765974057326,15.4443634132865,0.));
#240140=CARTESIAN_POINT('Ctrl Pts',(-17.765974057326,15.4443634132865,12.));
#240141=CARTESIAN_POINT('Ctrl Pts',(-17.7760182175817,15.4602755393019,
0.));
#240142=CARTESIAN_POINT('Ctrl Pts',(-17.7760182175817,15.4602755393019,
12.));
#240143=CARTESIAN_POINT('Ctrl Pts',(-17.7860808481229,15.4763152417506,
0.));
#240144=CARTESIAN_POINT('Ctrl Pts',(-17.7860808481229,15.4763152417506,
12.));
#240145=CARTESIAN_POINT('Ctrl Pts',(-17.7961609903161,15.4924819268529,
0.));
#240146=CARTESIAN_POINT('Ctrl Pts',(-17.7961609903161,15.4924819268529,
12.));
#240147=CARTESIAN_POINT('Ctrl Pts',(-17.8062576997964,15.5087750074728,
0.));
#240148=CARTESIAN_POINT('Ctrl Pts',(-17.8062576997964,15.5087750074728,
12.));
#240149=CARTESIAN_POINT('Ctrl Pts',(-17.8163700461263,15.5251939029558,
0.));
#240150=CARTESIAN_POINT('Ctrl Pts',(-17.8163700461263,15.5251939029558,
12.));
#240151=CARTESIAN_POINT('Ctrl Pts',(-17.8264971124606,15.5417380389639,
0.));
#240152=CARTESIAN_POINT('Ctrl Pts',(-17.8264971124606,15.5417380389639,
12.));
#240153=CARTESIAN_POINT('Ctrl Pts',(-17.8366379952078,15.5584068472976,
0.));
#240154=CARTESIAN_POINT('Ctrl Pts',(-17.8366379952078,15.5584068472976,
12.));
#240155=CARTESIAN_POINT('Ctrl Pts',(-17.8467918036977,15.5751997657153,
0.));
#240156=CARTESIAN_POINT('Ctrl Pts',(-17.8467918036977,15.5751997657153,
12.));
#240157=CARTESIAN_POINT('Ctrl Pts',(-17.8569576598996,15.5921162378183,
0.));
#240158=CARTESIAN_POINT('Ctrl Pts',(-17.8569576598996,15.5921162378183,
12.));
#240159=CARTESIAN_POINT('Ctrl Pts',(-17.8671346981388,15.6091557129205,
0.));
#240160=CARTESIAN_POINT('Ctrl Pts',(-17.8671346981388,15.6091557129205,
12.));
#240161=CARTESIAN_POINT('Ctrl Pts',(-17.8773220648125,15.6263176459107,
0.));
#240162=CARTESIAN_POINT('Ctrl Pts',(-17.8773220648125,15.6263176459107,
12.));
#240163=CARTESIAN_POINT('Ctrl Pts',(-17.8875189181095,15.6436014971088,
0.));
#240164=CARTESIAN_POINT('Ctrl Pts',(-17.8875189181095,15.6436014971088,
12.));
#240165=CARTESIAN_POINT('Ctrl Pts',(-17.8977244277247,15.6610067321036,
0.));
#240166=CARTESIAN_POINT('Ctrl Pts',(-17.8977244277247,15.6610067321036,
12.));
#240167=CARTESIAN_POINT('Ctrl Pts',(-17.9079377746118,15.6785328216467,
0.));
#240168=CARTESIAN_POINT('Ctrl Pts',(-17.9079377746118,15.6785328216467,
12.));
#240169=CARTESIAN_POINT('Ctrl Pts',(-17.918158150746,15.6961792415526,0.));
#240170=CARTESIAN_POINT('Ctrl Pts',(-17.918158150746,15.6961792415526,12.));
#240171=CARTESIAN_POINT('Ctrl Pts',(-17.9283847588837,15.713945472584,0.));
#240172=CARTESIAN_POINT('Ctrl Pts',(-17.9283847588837,15.713945472584,12.));
#240173=CARTESIAN_POINT('Ctrl Pts',(-17.9386168123261,15.7318310003334,
0.));
#240174=CARTESIAN_POINT('Ctrl Pts',(-17.9386168123261,15.7318310003334,
12.));
#240175=CARTESIAN_POINT('Ctrl Pts',(-17.9488535346776,15.7498353150856,
0.));
#240176=CARTESIAN_POINT('Ctrl Pts',(-17.9488535346776,15.7498353150856,
12.));
#240177=CARTESIAN_POINT('Ctrl Pts',(-17.9590941596236,15.7679579117072,
0.));
#240178=CARTESIAN_POINT('Ctrl Pts',(-17.9590941596236,15.7679579117072,
12.));
#240179=CARTESIAN_POINT('Ctrl Pts',(-17.9693379307297,15.786198289572,0.));
#240180=CARTESIAN_POINT('Ctrl Pts',(-17.9693379307297,15.786198289572,12.));
#240181=CARTESIAN_POINT('Ctrl Pts',(-17.9795841012383,15.8045559524674,
0.));
#240182=CARTESIAN_POINT('Ctrl Pts',(-17.9795841012383,15.8045559524674,
12.));
#240183=CARTESIAN_POINT('Ctrl Pts',(-17.9898319338664,15.8230304084963,
0.));
#240184=CARTESIAN_POINT('Ctrl Pts',(-17.9898319338664,15.8230304084963,
12.));
#240185=CARTESIAN_POINT('Ctrl Pts',(-18.0000807006055,15.8416211699681,
0.));
#240186=CARTESIAN_POINT('Ctrl Pts',(-18.0000807006055,15.8416211699681,
12.));
#240187=CARTESIAN_POINT('Ctrl Pts',(-18.010329682521,15.8603277532834,0.));
#240188=CARTESIAN_POINT('Ctrl Pts',(-18.010329682521,15.8603277532834,12.));
#240189=CARTESIAN_POINT('Ctrl Pts',(-18.0205781695773,15.8791496788685,
0.));
#240190=CARTESIAN_POINT('Ctrl Pts',(-18.0205781695773,15.8791496788685,
12.));
#240191=CARTESIAN_POINT('Ctrl Pts',(-18.0308254604638,15.8980864711043,
0.));
#240192=CARTESIAN_POINT('Ctrl Pts',(-18.0308254604638,15.8980864711043,
12.));
#240193=CARTESIAN_POINT('Ctrl Pts',(-18.0410708624208,15.9171376582436,
0.));
#240194=CARTESIAN_POINT('Ctrl Pts',(-18.0410708624208,15.9171376582436,
12.));
#240195=CARTESIAN_POINT('Ctrl Pts',(-18.0513136910691,15.9363027723244,
0.));
#240196=CARTESIAN_POINT('Ctrl Pts',(-18.0513136910691,15.9363027723244,
12.));
#240197=CARTESIAN_POINT('Ctrl Pts',(-18.061553270236,15.9555813490645,0.));
#240198=CARTESIAN_POINT('Ctrl Pts',(-18.061553270236,15.9555813490645,12.));
#240199=CARTESIAN_POINT('Ctrl Pts',(-18.071788931796,15.9749729277848,0.));
#240200=CARTESIAN_POINT('Ctrl Pts',(-18.071788931796,15.9749729277848,12.));
#240201=CARTESIAN_POINT('Ctrl Pts',(-18.0820200155239,15.9944770513616,
0.));
#240202=CARTESIAN_POINT('Ctrl Pts',(-18.0820200155239,15.9944770513616,
12.));
#240203=CARTESIAN_POINT('Ctrl Pts',(-18.0922458689464,16.0140932661612,
0.));
#240204=CARTESIAN_POINT('Ctrl Pts',(-18.0922458689464,16.0140932661612,
12.));
#240205=CARTESIAN_POINT('Ctrl Pts',(-18.1024658471966,16.0338211219693,
0.));
#240206=CARTESIAN_POINT('Ctrl Pts',(-18.1024658471966,16.0338211219693,
12.));
#240207=CARTESIAN_POINT('Ctrl Pts',(-18.1126793128688,16.0536601719124,
0.));
#240208=CARTESIAN_POINT('Ctrl Pts',(-18.1126793128688,16.0536601719124,
12.));
#240209=CARTESIAN_POINT('Ctrl Pts',(-18.1228856358746,16.0736099723664,
0.));
#240210=CARTESIAN_POINT('Ctrl Pts',(-18.1228856358746,16.0736099723664,
12.));
#240211=CARTESIAN_POINT('Ctrl Pts',(-18.1330841933099,16.0936700829108,
0.));
#240212=CARTESIAN_POINT('Ctrl Pts',(-18.1330841933099,16.0936700829108,
12.));
#240213=CARTESIAN_POINT('Ctrl Pts',(-18.1432743693231,16.113840066279,0.));
#240214=CARTESIAN_POINT('Ctrl Pts',(-18.1432743693231,16.113840066279,12.));
#240215=CARTESIAN_POINT('Ctrl Pts',(-18.1534555549851,16.1341194882987,
0.));
#240216=CARTESIAN_POINT('Ctrl Pts',(-18.1534555549851,16.1341194882987,
12.));
#240217=CARTESIAN_POINT('Ctrl Pts',(-18.1636271481616,16.1545079178261,
0.));
#240218=CARTESIAN_POINT('Ctrl Pts',(-18.1636271481616,16.1545079178261,
12.));
#240219=CARTESIAN_POINT('Ctrl Pts',(-18.1737885533852,16.1750049266673,
0.));
#240220=CARTESIAN_POINT('Ctrl Pts',(-18.1737885533852,16.1750049266673,
12.));
#240221=CARTESIAN_POINT('Ctrl Pts',(-18.1839391817335,16.1956100895076,
0.));
#240222=CARTESIAN_POINT('Ctrl Pts',(-18.1839391817335,16.1956100895076,
12.));
#240223=CARTESIAN_POINT('Ctrl Pts',(-18.1940784507232,16.2163229838878,
0.));
#240224=CARTESIAN_POINT('Ctrl Pts',(-18.1940784507232,16.2163229838878,
12.));
#240225=CARTESIAN_POINT('Ctrl Pts',(-18.2042057842037,16.237143190164,0.));
#240226=CARTESIAN_POINT('Ctrl Pts',(-18.2042057842037,16.237143190164,12.));
#240227=CARTESIAN_POINT('Ctrl Pts',(-18.214320612253,16.2580702914615,0.));
#240228=CARTESIAN_POINT('Ctrl Pts',(-18.214320612253,16.2580702914615,12.));
#240229=CARTESIAN_POINT('Ctrl Pts',(-18.2244223710745,16.2791038736223,
0.));
#240230=CARTESIAN_POINT('Ctrl Pts',(-18.2244223710745,16.2791038736223,
12.));
#240231=CARTESIAN_POINT('Ctrl Pts',(-18.2345105028981,16.3002435251378,
0.));
#240232=CARTESIAN_POINT('Ctrl Pts',(-18.2345105028981,16.3002435251378,
12.));
#240233=CARTESIAN_POINT('Ctrl Pts',(-18.2445844558742,16.3214888370988,
0.));
#240234=CARTESIAN_POINT('Ctrl Pts',(-18.2445844558742,16.3214888370988,
12.));
#240235=CARTESIAN_POINT('Ctrl Pts',(-18.2546436839609,16.342839403159,0.));
#240236=CARTESIAN_POINT('Ctrl Pts',(-18.2546436839609,16.342839403159,12.));
#240237=CARTESIAN_POINT('Ctrl Pts',(-18.2646876468169,16.3642948194869,
0.));
#240238=CARTESIAN_POINT('Ctrl Pts',(-18.2646876468169,16.3642948194869,
12.));
#240239=CARTESIAN_POINT('Ctrl Pts',(-18.2747158096934,16.385854684708,0.));
#240240=CARTESIAN_POINT('Ctrl Pts',(-18.2747158096934,16.385854684708,12.));
#240241=CARTESIAN_POINT('Ctrl Pts',(-18.2847276433308,16.4075185998454,
0.));
#240242=CARTESIAN_POINT('Ctrl Pts',(-18.2847276433308,16.4075185998454,
12.));
#240243=CARTESIAN_POINT('Ctrl Pts',(-18.2947226238509,16.4292861682377,
0.));
#240244=CARTESIAN_POINT('Ctrl Pts',(-18.2947226238509,16.4292861682377,
12.));
#240245=CARTESIAN_POINT('Ctrl Pts',(-18.3047002326858,16.4511569955231,
0.));
#240246=CARTESIAN_POINT('Ctrl Pts',(-18.3047002326858,16.4511569955231,
12.));
#240247=CARTESIAN_POINT('Ctrl Pts',(-18.3146599565229,16.4731306896439,
0.));
#240248=CARTESIAN_POINT('Ctrl Pts',(-18.3146599565229,16.4731306896439,
12.));
#240249=CARTESIAN_POINT('Ctrl Pts',(-18.3246012872468,16.4952068608344,
0.));
#240250=CARTESIAN_POINT('Ctrl Pts',(-18.3246012872468,16.4952068608344,
12.));
#240251=CARTESIAN_POINT('Ctrl Pts',(-18.3345237218864,16.5173851216045,
0.));
#240252=CARTESIAN_POINT('Ctrl Pts',(-18.3345237218864,16.5173851216045,
12.));
#240253=CARTESIAN_POINT('Ctrl Pts',(-18.3444267625601,16.5396650867139,
0.));
#240254=CARTESIAN_POINT('Ctrl Pts',(-18.3444267625601,16.5396650867139,
12.));
#240255=CARTESIAN_POINT('Ctrl Pts',(-18.3543099164331,16.5620463731414,
0.));
#240256=CARTESIAN_POINT('Ctrl Pts',(-18.3543099164331,16.5620463731414,
12.));
#240257=CARTESIAN_POINT('Ctrl Pts',(-18.364172695589,16.5845286000218,0.));
#240258=CARTESIAN_POINT('Ctrl Pts',(-18.364172695589,16.5845286000218,12.));
#240259=CARTESIAN_POINT('Ctrl Pts',(-18.3740146168879,16.6071113885711,
0.));
#240260=CARTESIAN_POINT('Ctrl Pts',(-18.3740146168879,16.6071113885711,
12.));
#240261=CARTESIAN_POINT('Ctrl Pts',(-18.3838352018327,16.6297943620056,
0.));
#240262=CARTESIAN_POINT('Ctrl Pts',(-18.3838352018327,16.6297943620056,
12.));
#240263=CARTESIAN_POINT('Ctrl Pts',(-18.3936339764332,16.6525771454513,
0.));
#240264=CARTESIAN_POINT('Ctrl Pts',(-18.3936339764332,16.6525771454513,
12.));
#240265=CARTESIAN_POINT('Ctrl Pts',(-18.4034104710789,16.6754593658513,
0.));
#240266=CARTESIAN_POINT('Ctrl Pts',(-18.4034104710789,16.6754593658513,
12.));
#240267=CARTESIAN_POINT('Ctrl Pts',(-18.413164220399,16.698440651849,0.));
#240268=CARTESIAN_POINT('Ctrl Pts',(-18.413164220399,16.698440651849,12.));
#240269=CARTESIAN_POINT('Ctrl Pts',(-18.4228947633186,16.7215206338818,
0.));
#240270=CARTESIAN_POINT('Ctrl Pts',(-18.4228947633186,16.7215206338818,
12.));
#240271=CARTESIAN_POINT('Ctrl Pts',(-18.4326016431392,16.7446989442882,
0.));
#240272=CARTESIAN_POINT('Ctrl Pts',(-18.4326016431392,16.7446989442882,
12.));
#240273=CARTESIAN_POINT('Ctrl Pts',(-18.4422844076099,16.7679752173992,
0.));
#240274=CARTESIAN_POINT('Ctrl Pts',(-18.4422844076099,16.7679752173992,
12.));
#240275=CARTESIAN_POINT('Ctrl Pts',(-18.4519426090124,16.791349089629,0.));
#240276=CARTESIAN_POINT('Ctrl Pts',(-18.4519426090124,16.791349089629,12.));
#240277=CARTESIAN_POINT('Ctrl Pts',(-18.4615758042305,16.8148201995472,
0.));
#240278=CARTESIAN_POINT('Ctrl Pts',(-18.4615758042305,16.8148201995472,
12.));
#240279=CARTESIAN_POINT('Ctrl Pts',(-18.4711835548622,16.8383881879707,
0.));
#240280=CARTESIAN_POINT('Ctrl Pts',(-18.4711835548622,16.8383881879707,
12.));
#240281=CARTESIAN_POINT('Ctrl Pts',(-18.4807654268769,16.8620526977169,
0.));
#240282=CARTESIAN_POINT('Ctrl Pts',(-18.4807654268769,16.8620526977169,
12.));
#240283=CARTESIAN_POINT('Ctrl Pts',(-18.4903209902226,16.8858133733086,
0.));
#240284=CARTESIAN_POINT('Ctrl Pts',(-18.4903209902226,16.8858133733086,
12.));
#240285=CARTESIAN_POINT('Ctrl Pts',(-18.4998498184619,16.9096698606942,
0.));
#240286=CARTESIAN_POINT('Ctrl Pts',(-18.4998498184619,16.9096698606942,
12.));
#240287=CARTESIAN_POINT('Ctrl Pts',(-18.5093514883835,16.9336218069353,
0.));
#240288=CARTESIAN_POINT('Ctrl Pts',(-18.5093514883835,16.9336218069353,
12.));
#240289=CARTESIAN_POINT('Ctrl Pts',(-18.518825579666,16.957668859934,0.));
#240290=CARTESIAN_POINT('Ctrl Pts',(-18.518825579666,16.957668859934,12.));
#240291=CARTESIAN_POINT('Ctrl Pts',(-18.5282716744198,16.9818106680382,
0.));
#240292=CARTESIAN_POINT('Ctrl Pts',(-18.5282716744198,16.9818106680382,
12.));
#240293=CARTESIAN_POINT('Ctrl Pts',(-18.5376893576961,17.0060468805099,
0.));
#240294=CARTESIAN_POINT('Ctrl Pts',(-18.5376893576961,17.0060468805099,
12.));
#240295=CARTESIAN_POINT('Ctrl Pts',(-18.5470782182089,17.030377148174,0.));
#240296=CARTESIAN_POINT('Ctrl Pts',(-18.5470782182089,17.030377148174,12.));
#240297=CARTESIAN_POINT('Ctrl Pts',(-18.5564378489628,17.0548011239751,
0.));
#240298=CARTESIAN_POINT('Ctrl Pts',(-18.5564378489628,17.0548011239751,
12.));
#240299=CARTESIAN_POINT('Ctrl Pts',(-18.5657678479788,17.0793184636079,
0.));
#240300=CARTESIAN_POINT('Ctrl Pts',(-18.5657678479788,17.0793184636079,
12.));
#240301=CARTESIAN_POINT('Ctrl Pts',(-18.5750678188543,17.1039288260001,
0.));
#240302=CARTESIAN_POINT('Ctrl Pts',(-18.5750678188543,17.1039288260001,
12.));
#240303=CARTESIAN_POINT('Ctrl Pts',(-18.5843373717253,17.1286318741185,
0.));
#240304=CARTESIAN_POINT('Ctrl Pts',(-18.5843373717253,17.1286318741185,
12.));
#240305=CARTESIAN_POINT('Ctrl Pts',(-18.5935761222833,17.1534272741646,
0.));
#240306=CARTESIAN_POINT('Ctrl Pts',(-18.5935761222833,17.1534272741646,
12.));
#240307=CARTESIAN_POINT('Ctrl Pts',(-18.6027836898826,17.1783146940131,
0.));
#240308=CARTESIAN_POINT('Ctrl Pts',(-18.6027836898826,17.1783146940131,
12.));
#240309=CARTESIAN_POINT('Ctrl Pts',(-18.6119596959957,17.2032938019288,
0.));
#240310=CARTESIAN_POINT('Ctrl Pts',(-18.6119596959957,17.2032938019288,
12.));
#240311=CARTESIAN_POINT('Ctrl Pts',(-18.6211037624041,17.2283642650519,
0.));
#240312=CARTESIAN_POINT('Ctrl Pts',(-18.6211037624041,17.2283642650519,
12.));
#240313=CARTESIAN_POINT('Ctrl Pts',(-18.630215509794,17.2535257482186,0.));
#240314=CARTESIAN_POINT('Ctrl Pts',(-18.630215509794,17.2535257482186,12.));
#240315=CARTESIAN_POINT('Ctrl Pts',(-18.639294555474,17.278777912021,0.));
#240316=CARTESIAN_POINT('Ctrl Pts',(-18.639294555474,17.278777912021,12.));
#240317=CARTESIAN_POINT('Ctrl Pts',(-18.6483405141853,17.3041204135069,
0.));
#240318=CARTESIAN_POINT('Ctrl Pts',(-18.6483405141853,17.3041204135069,
12.));
#240319=CARTESIAN_POINT('Ctrl Pts',(-18.6573530024019,17.3295529098612,
0.));
#240320=CARTESIAN_POINT('Ctrl Pts',(-18.6573530024019,17.3295529098612,
12.));
#240321=CARTESIAN_POINT('Ctrl Pts',(-18.6663316416569,17.3550750612438,
0.));
#240322=CARTESIAN_POINT('Ctrl Pts',(-18.6663316416569,17.3550750612438,
12.));
#240323=CARTESIAN_POINT('Ctrl Pts',(-18.6752760624045,17.3806865340744,
0.));
#240324=CARTESIAN_POINT('Ctrl Pts',(-18.6752760624045,17.3806865340744,
12.));
#240325=CARTESIAN_POINT('Ctrl Pts',(-18.6841859073472,17.4063870038563,
0.));
#240326=CARTESIAN_POINT('Ctrl Pts',(-18.6841859073472,17.4063870038563,
12.));
#240327=CARTESIAN_POINT('Ctrl Pts',(-18.6930608357421,17.4321761588148,
0.));
#240328=CARTESIAN_POINT('Ctrl Pts',(-18.6930608357421,17.4321761588148,
12.));
#240329=CARTESIAN_POINT('Ctrl Pts',(-18.7019005250322,17.4580537012764,
0.));
#240330=CARTESIAN_POINT('Ctrl Pts',(-18.7019005250322,17.4580537012764,
12.));
#240331=CARTESIAN_POINT('Ctrl Pts',(-18.7107046613941,17.4840193397176,
0.));
#240332=CARTESIAN_POINT('Ctrl Pts',(-18.7107046613941,17.4840193397176,
12.));
#240333=CARTESIAN_POINT('Ctrl Pts',(-18.7194729318128,17.5100727820891,
0.));
#240334=CARTESIAN_POINT('Ctrl Pts',(-18.7194729318128,17.5100727820891,
12.));
#240335=CARTESIAN_POINT('Ctrl Pts',(-18.728205015716,17.5362137287604,0.));
#240336=CARTESIAN_POINT('Ctrl Pts',(-18.728205015716,17.5362137287604,12.));
#240337=CARTESIAN_POINT('Ctrl Pts',(-18.7369005764558,17.5624418653248,
0.));
#240338=CARTESIAN_POINT('Ctrl Pts',(-18.7369005764558,17.5624418653248,
12.));
#240339=CARTESIAN_POINT('Ctrl Pts',(-18.7455592536667,17.5887568561361,
0.));
#240340=CARTESIAN_POINT('Ctrl Pts',(-18.7455592536667,17.5887568561361,
12.));
#240341=CARTESIAN_POINT('Ctrl Pts',(-18.7541806530935,17.6151583356988,
0.));
#240342=CARTESIAN_POINT('Ctrl Pts',(-18.7541806530935,17.6151583356988,
12.));
#240343=CARTESIAN_POINT('Ctrl Pts',(-18.7627643613139,17.6416459210646,
0.));
#240344=CARTESIAN_POINT('Ctrl Pts',(-18.7627643613139,17.6416459210646,
12.));
#240345=CARTESIAN_POINT('Ctrl Pts',(-18.7713099642673,17.6682192274197,
0.));
#240346=CARTESIAN_POINT('Ctrl Pts',(-18.7713099642673,17.6682192274197,
12.));
#240347=CARTESIAN_POINT('Ctrl Pts',(-18.7798170641305,17.6948778822981,
0.));
#240348=CARTESIAN_POINT('Ctrl Pts',(-18.7798170641305,17.6948778822981,
12.));
#240349=CARTESIAN_POINT('Ctrl Pts',(-18.7882852976016,17.7216215409019,
0.));
#240350=CARTESIAN_POINT('Ctrl Pts',(-18.7882852976016,17.7216215409019,
12.));
#240351=CARTESIAN_POINT('Ctrl Pts',(-18.7967143519444,17.7484498996916,
0.));
#240352=CARTESIAN_POINT('Ctrl Pts',(-18.7967143519444,17.7484498996916,
12.));
#240353=CARTESIAN_POINT('Ctrl Pts',(-18.8051039860543,17.7753627137898,
0.));
#240354=CARTESIAN_POINT('Ctrl Pts',(-18.8051039860543,17.7753627137898,
12.));
#240355=CARTESIAN_POINT('Ctrl Pts',(-18.8134540340581,17.8023598011135,
0.));
#240356=CARTESIAN_POINT('Ctrl Pts',(-18.8134540340581,17.8023598011135,
12.));
#240357=CARTESIAN_POINT('Ctrl Pts',(-18.8217643886368,17.8294410311105,
0.));
#240358=CARTESIAN_POINT('Ctrl Pts',(-18.8217643886368,17.8294410311105,
12.));
#240359=CARTESIAN_POINT('Ctrl Pts',(-18.8300349896187,17.8566063174871,
0.));
#240360=CARTESIAN_POINT('Ctrl Pts',(-18.8300349896187,17.8566063174871,
12.));
#240361=CARTESIAN_POINT('Ctrl Pts',(-18.8366196462746,17.8784057509434,
0.));
#240362=CARTESIAN_POINT('Ctrl Pts',(-18.8366196462746,17.8784057509434,
12.));
#240363=CARTESIAN_POINT('Ctrl Pts',(-18.8415402351882,17.8947931177853,
0.));
#240364=CARTESIAN_POINT('Ctrl Pts',(-18.8415402351882,17.8947931177853,
12.));
#240365=CARTESIAN_POINT('Ctrl Pts',(-18.8448126709726,17.9057348246611,
0.));
#240366=CARTESIAN_POINT('Ctrl Pts',(-18.8448126709726,17.9057348246611,
12.));
#240367=CARTESIAN_POINT('Ctrl Pts',(-18.8464468996588,17.9112098770111,
0.));
#240368=CARTESIAN_POINT('Ctrl Pts',(-18.8464468996588,17.9112098770111,
12.));
#240369=CARTESIAN_POINT('',(-18.8464468996588,17.9112098770111,0.));
#240370=CARTESIAN_POINT('Ctrl Pts',(-17.1452095830633,14.6513681262571,
0.));
#240371=CARTESIAN_POINT('Ctrl Pts',(-17.1452153999142,14.6513711852843,
0.));
#240372=CARTESIAN_POINT('Ctrl Pts',(-17.1452600887037,14.6514066997196,
0.));
#240373=CARTESIAN_POINT('Ctrl Pts',(-17.1454262858043,14.6515481598068,
0.));
#240374=CARTESIAN_POINT('Ctrl Pts',(-17.1458462295271,14.6519131634508,
0.));
#240375=CARTESIAN_POINT('Ctrl Pts',(-17.1466998098673,14.6526624064978,
0.));
#240376=CARTESIAN_POINT('Ctrl Pts',(-17.147876394491,14.6537016966184,0.));
#240377=CARTESIAN_POINT('Ctrl Pts',(-17.1493641837558,14.655024862281,0.));
#240378=CARTESIAN_POINT('Ctrl Pts',(-17.1511476869496,14.6566237952435,
0.));
#240379=CARTESIAN_POINT('Ctrl Pts',(-17.1532107762718,14.6584900555302,
0.));
#240380=CARTESIAN_POINT('Ctrl Pts',(-17.1555401986401,14.6606167169642,
0.));
#240381=CARTESIAN_POINT('Ctrl Pts',(-17.1581262646789,14.6629987285992,
0.));
#240382=CARTESIAN_POINT('Ctrl Pts',(-17.1609609517369,14.6656319165057,
0.));
#240383=CARTESIAN_POINT('Ctrl Pts',(-17.1640366762305,14.6685123374423,
0.));
#240384=CARTESIAN_POINT('Ctrl Pts',(-17.167344972302,14.671635583332,0.));
#240385=CARTESIAN_POINT('Ctrl Pts',(-17.1708771619129,14.6749971333867,
0.));
#240386=CARTESIAN_POINT('Ctrl Pts',(-17.1746247499057,14.6785925615677,
0.));
#240387=CARTESIAN_POINT('Ctrl Pts',(-17.1785800350826,14.6824178576167,
0.));
#240388=CARTESIAN_POINT('Ctrl Pts',(-17.182736158472,14.686469452232,0.));
#240389=CARTESIAN_POINT('Ctrl Pts',(-17.1870867909918,14.6907440526958,
0.));
#240390=CARTESIAN_POINT('Ctrl Pts',(-17.1916259308415,14.6952385361705,
0.));
#240391=CARTESIAN_POINT('Ctrl Pts',(-17.1963476411694,14.699949811582,0.));
#240392=CARTESIAN_POINT('Ctrl Pts',(-17.2012461084268,14.7048748502663,
0.));
#240393=CARTESIAN_POINT('Ctrl Pts',(-17.2063157097315,14.7100107213586,
0.));
#240394=CARTESIAN_POINT('Ctrl Pts',(-17.2115510835989,14.7153546289339,
0.));
#240395=CARTESIAN_POINT('Ctrl Pts',(-17.2169471814256,14.7209039390327,
0.));
#240396=CARTESIAN_POINT('Ctrl Pts',(-17.2224992099667,14.7266561494282,
0.));
#240397=CARTESIAN_POINT('Ctrl Pts',(-17.2282025904314,14.7326088681163,
0.));
#240398=CARTESIAN_POINT('Ctrl Pts',(-17.2340529062076,14.7387597858116,
0.));
#240399=CARTESIAN_POINT('Ctrl Pts',(-17.2400458713565,14.7451066593792,
0.));
#240400=CARTESIAN_POINT('Ctrl Pts',(-17.2461773413288,14.7516473175124,
0.));
#240401=CARTESIAN_POINT('Ctrl Pts',(-17.2524433146837,14.7583796616617,
0.));
#240402=CARTESIAN_POINT('Ctrl Pts',(-17.2588399401465,14.7653016697591,
0.));
#240403=CARTESIAN_POINT('Ctrl Pts',(-17.2653635155319,14.7724113956731,
0.));
#240404=CARTESIAN_POINT('Ctrl Pts',(-17.2720104735194,14.7797069617804,
0.));
#240405=CARTESIAN_POINT('Ctrl Pts',(-17.2787773704849,14.787186553128,0.));
#240406=CARTESIAN_POINT('Ctrl Pts',(-17.2856608733196,14.7948484105249,
0.));
#240407=CARTESIAN_POINT('Ctrl Pts',(-17.2926577496513,14.8026908254276,
0.));
#240408=CARTESIAN_POINT('Ctrl Pts',(-17.299764866148,14.8107121391035,0.));
#240409=CARTESIAN_POINT('Ctrl Pts',(-17.3069791853706,14.8189107410162,
0.));
#240410=CARTESIAN_POINT('Ctrl Pts',(-17.3142977632659,14.8272850675379,
0.));
#240411=CARTESIAN_POINT('Ctrl Pts',(-17.3217177462101,14.8358336004197,
0.));
#240412=CARTESIAN_POINT('Ctrl Pts',(-17.3292363662605,14.8445548643508,
0.));
#240413=CARTESIAN_POINT('Ctrl Pts',(-17.336850936485,14.8534474245433,0.));
#240414=CARTESIAN_POINT('Ctrl Pts',(-17.3445588463475,14.8625098843417,
0.));
#240415=CARTESIAN_POINT('Ctrl Pts',(-17.3523575568645,14.8717408826955,
0.));
#240416=CARTESIAN_POINT('Ctrl Pts',(-17.3602445978161,14.8811390927423,
0.));
#240417=CARTESIAN_POINT('Ctrl Pts',(-17.3682175653235,14.8907032205788,
0.));
#240418=CARTESIAN_POINT('Ctrl Pts',(-17.3762741193076,14.900432003961,0.));
#240419=CARTESIAN_POINT('Ctrl Pts',(-17.3844119809824,14.9103242110057,
0.));
#240420=CARTESIAN_POINT('Ctrl Pts',(-17.3926289303986,14.9203786389342,
0.));
#240421=CARTESIAN_POINT('Ctrl Pts',(-17.4009228040749,14.9305941128757,
0.));
#240422=CARTESIAN_POINT('Ctrl Pts',(-17.4092914926071,14.940969484645,0.));
#240423=CARTESIAN_POINT('Ctrl Pts',(-17.4177329382828,14.9515036315143,
0.));
#240424=CARTESIAN_POINT('Ctrl Pts',(-17.426245132709,14.9621954549827,0.));
#240425=CARTESIAN_POINT('Ctrl Pts',(-17.4348261151396,14.9730438799452,
0.));
#240426=CARTESIAN_POINT('Ctrl Pts',(-17.4434739707773,14.9840478538358,
0.));
#240427=CARTESIAN_POINT('Ctrl Pts',(-17.4521868291004,14.9952063457778,
0.));
#240428=CARTESIAN_POINT('Ctrl Pts',(-17.4609628621418,15.0065183456921,
0.));
#240429=CARTESIAN_POINT('Ctrl Pts',(-17.4698002829357,15.0179828635086,
0.));
#240430=CARTESIAN_POINT('Ctrl Pts',(-17.4786973441417,15.029598928488,0.));
#240431=CARTESIAN_POINT('Ctrl Pts',(-17.4876523366178,15.0413655884993,
0.));
#240432=CARTESIAN_POINT('Ctrl Pts',(-17.4966635880245,15.0532819093085,
0.));
#240433=CARTESIAN_POINT('Ctrl Pts',(-17.5057294613874,15.0653469738306,
0.));
#240434=CARTESIAN_POINT('Ctrl Pts',(-17.5148483539684,15.0775598815748,
0.));
#240435=CARTESIAN_POINT('Ctrl Pts',(-17.5240186961788,15.0899197481082,
0.));
#240436=CARTESIAN_POINT('Ctrl Pts',(-17.5332389504829,15.1024257045033,
0.));
#240437=CARTESIAN_POINT('Ctrl Pts',(-17.5425076102966,15.1150768967729,
0.));
#240438=CARTESIAN_POINT('Ctrl Pts',(-17.5518231989122,15.127872485314,0.));
#240439=CARTESIAN_POINT('Ctrl Pts',(-17.5611842686196,15.1408116444877,
0.));
#240440=CARTESIAN_POINT('Ctrl Pts',(-17.570589399803,15.1538935621714,0.));
#240441=CARTESIAN_POINT('Ctrl Pts',(-17.5800372000539,15.1671174393136,
0.));
#240442=CARTESIAN_POINT('Ctrl Pts',(-17.5895263032592,15.1804824894605,
0.));
#240443=CARTESIAN_POINT('Ctrl Pts',(-17.5990553687595,15.1939879383268,
0.));
#240444=CARTESIAN_POINT('Ctrl Pts',(-17.6086230806497,15.2076330234686,
0.));
#240445=CARTESIAN_POINT('Ctrl Pts',(-17.6182281470467,15.22141699392,0.));
#240446=CARTESIAN_POINT('Ctrl Pts',(-17.6278692993765,15.2353391098367,
0.));
#240447=CARTESIAN_POINT('Ctrl Pts',(-17.637545291637,15.2493986421091,0.));
#240448=CARTESIAN_POINT('Ctrl Pts',(-17.6472548997329,15.263594872029,0.));
#240449=CARTESIAN_POINT('Ctrl Pts',(-17.6569969209,15.2779270910238,0.));
#240450=CARTESIAN_POINT('Ctrl Pts',(-17.6667701731041,15.2923946003598,
0.));
#240451=CARTESIAN_POINT('Ctrl Pts',(-17.6765734944559,15.3069967108501,
0.));
#240452=CARTESIAN_POINT('Ctrl Pts',(-17.6864057426052,15.3217327425341,
0.));
#240453=CARTESIAN_POINT('Ctrl Pts',(-17.6962657941984,15.3366020244069,
0.));
#240454=CARTESIAN_POINT('Ctrl Pts',(-17.7061525444044,15.3516038942064,
0.));
#240455=CARTESIAN_POINT('Ctrl Pts',(-17.7160649064208,15.3667376981702,
0.));
#240456=CARTESIAN_POINT('Ctrl Pts',(-17.7260018109923,15.3820027907965,
0.));
#240457=CARTESIAN_POINT('Ctrl Pts',(-17.7359622059143,15.3973985345796,
0.));
#240458=CARTESIAN_POINT('Ctrl Pts',(-17.7459450555803,15.4129242997828,
0.));
#240459=CARTESIAN_POINT('Ctrl Pts',(-17.7559493405871,15.4285794642658,
0.));
#240460=CARTESIAN_POINT('Ctrl Pts',(-17.765974057326,15.4443634132865,0.));
#240461=CARTESIAN_POINT('Ctrl Pts',(-17.7760182175817,15.4602755393019,
0.));
#240462=CARTESIAN_POINT('Ctrl Pts',(-17.7860808481229,15.4763152417506,
0.));
#240463=CARTESIAN_POINT('Ctrl Pts',(-17.7961609903161,15.4924819268529,
0.));
#240464=CARTESIAN_POINT('Ctrl Pts',(-17.8062576997964,15.5087750074728,
0.));
#240465=CARTESIAN_POINT('Ctrl Pts',(-17.8163700461263,15.5251939029558,
0.));
#240466=CARTESIAN_POINT('Ctrl Pts',(-17.8264971124606,15.5417380389639,
0.));
#240467=CARTESIAN_POINT('Ctrl Pts',(-17.8366379952078,15.5584068472976,
0.));
#240468=CARTESIAN_POINT('Ctrl Pts',(-17.8467918036977,15.5751997657153,
0.));
#240469=CARTESIAN_POINT('Ctrl Pts',(-17.8569576598996,15.5921162378183,
0.));
#240470=CARTESIAN_POINT('Ctrl Pts',(-17.8671346981388,15.6091557129205,
0.));
#240471=CARTESIAN_POINT('Ctrl Pts',(-17.8773220648125,15.6263176459107,
0.));
#240472=CARTESIAN_POINT('Ctrl Pts',(-17.8875189181095,15.6436014971088,
0.));
#240473=CARTESIAN_POINT('Ctrl Pts',(-17.8977244277247,15.6610067321036,
0.));
#240474=CARTESIAN_POINT('Ctrl Pts',(-17.9079377746118,15.6785328216467,
0.));
#240475=CARTESIAN_POINT('Ctrl Pts',(-17.918158150746,15.6961792415526,0.));
#240476=CARTESIAN_POINT('Ctrl Pts',(-17.9283847588837,15.713945472584,0.));
#240477=CARTESIAN_POINT('Ctrl Pts',(-17.9386168123261,15.7318310003334,
0.));
#240478=CARTESIAN_POINT('Ctrl Pts',(-17.9488535346776,15.7498353150856,
0.));
#240479=CARTESIAN_POINT('Ctrl Pts',(-17.9590941596236,15.7679579117072,
0.));
#240480=CARTESIAN_POINT('Ctrl Pts',(-17.9693379307297,15.786198289572,0.));
#240481=CARTESIAN_POINT('Ctrl Pts',(-17.9795841012383,15.8045559524674,
0.));
#240482=CARTESIAN_POINT('Ctrl Pts',(-17.9898319338664,15.8230304084963,
0.));
#240483=CARTESIAN_POINT('Ctrl Pts',(-18.0000807006055,15.8416211699681,
0.));
#240484=CARTESIAN_POINT('Ctrl Pts',(-18.010329682521,15.8603277532834,0.));
#240485=CARTESIAN_POINT('Ctrl Pts',(-18.0205781695773,15.8791496788685,
0.));
#240486=CARTESIAN_POINT('Ctrl Pts',(-18.0308254604638,15.8980864711043,
0.));
#240487=CARTESIAN_POINT('Ctrl Pts',(-18.0410708624208,15.9171376582436,
0.));
#240488=CARTESIAN_POINT('Ctrl Pts',(-18.0513136910691,15.9363027723244,
0.));
#240489=CARTESIAN_POINT('Ctrl Pts',(-18.061553270236,15.9555813490645,0.));
#240490=CARTESIAN_POINT('Ctrl Pts',(-18.071788931796,15.9749729277848,0.));
#240491=CARTESIAN_POINT('Ctrl Pts',(-18.0820200155239,15.9944770513616,
0.));
#240492=CARTESIAN_POINT('Ctrl Pts',(-18.0922458689464,16.0140932661612,
0.));
#240493=CARTESIAN_POINT('Ctrl Pts',(-18.1024658471966,16.0338211219693,
0.));
#240494=CARTESIAN_POINT('Ctrl Pts',(-18.1126793128688,16.0536601719124,
0.));
#240495=CARTESIAN_POINT('Ctrl Pts',(-18.1228856358746,16.0736099723664,
0.));
#240496=CARTESIAN_POINT('Ctrl Pts',(-18.1330841933099,16.0936700829108,
0.));
#240497=CARTESIAN_POINT('Ctrl Pts',(-18.1432743693231,16.113840066279,0.));
#240498=CARTESIAN_POINT('Ctrl Pts',(-18.1534555549851,16.1341194882987,
0.));
#240499=CARTESIAN_POINT('Ctrl Pts',(-18.1636271481616,16.1545079178261,
0.));
#240500=CARTESIAN_POINT('Ctrl Pts',(-18.1737885533852,16.1750049266673,
0.));
#240501=CARTESIAN_POINT('Ctrl Pts',(-18.1839391817335,16.1956100895076,
0.));
#240502=CARTESIAN_POINT('Ctrl Pts',(-18.1940784507232,16.2163229838878,
0.));
#240503=CARTESIAN_POINT('Ctrl Pts',(-18.2042057842037,16.237143190164,0.));
#240504=CARTESIAN_POINT('Ctrl Pts',(-18.214320612253,16.2580702914615,0.));
#240505=CARTESIAN_POINT('Ctrl Pts',(-18.2244223710745,16.2791038736223,
0.));
#240506=CARTESIAN_POINT('Ctrl Pts',(-18.2345105028981,16.3002435251378,
0.));
#240507=CARTESIAN_POINT('Ctrl Pts',(-18.2445844558742,16.3214888370988,
0.));
#240508=CARTESIAN_POINT('Ctrl Pts',(-18.2546436839609,16.342839403159,0.));
#240509=CARTESIAN_POINT('Ctrl Pts',(-18.2646876468169,16.3642948194869,
0.));
#240510=CARTESIAN_POINT('Ctrl Pts',(-18.2747158096934,16.385854684708,0.));
#240511=CARTESIAN_POINT('Ctrl Pts',(-18.2847276433308,16.4075185998454,
0.));
#240512=CARTESIAN_POINT('Ctrl Pts',(-18.2947226238509,16.4292861682377,
0.));
#240513=CARTESIAN_POINT('Ctrl Pts',(-18.3047002326858,16.4511569955231,
0.));
#240514=CARTESIAN_POINT('Ctrl Pts',(-18.3146599565229,16.4731306896439,
0.));
#240515=CARTESIAN_POINT('Ctrl Pts',(-18.3246012872468,16.4952068608344,
0.));
#240516=CARTESIAN_POINT('Ctrl Pts',(-18.3345237218864,16.5173851216045,
0.));
#240517=CARTESIAN_POINT('Ctrl Pts',(-18.3444267625601,16.5396650867139,
0.));
#240518=CARTESIAN_POINT('Ctrl Pts',(-18.3543099164331,16.5620463731414,
0.));
#240519=CARTESIAN_POINT('Ctrl Pts',(-18.364172695589,16.5845286000218,0.));
#240520=CARTESIAN_POINT('Ctrl Pts',(-18.3740146168879,16.6071113885711,
0.));
#240521=CARTESIAN_POINT('Ctrl Pts',(-18.3838352018327,16.6297943620056,
0.));
#240522=CARTESIAN_POINT('Ctrl Pts',(-18.3936339764332,16.6525771454513,
0.));
#240523=CARTESIAN_POINT('Ctrl Pts',(-18.4034104710789,16.6754593658513,
0.));
#240524=CARTESIAN_POINT('Ctrl Pts',(-18.413164220399,16.698440651849,0.));
#240525=CARTESIAN_POINT('Ctrl Pts',(-18.4228947633186,16.7215206338818,
0.));
#240526=CARTESIAN_POINT('Ctrl Pts',(-18.4326016431392,16.7446989442882,
0.));
#240527=CARTESIAN_POINT('Ctrl Pts',(-18.4422844076099,16.7679752173992,
0.));
#240528=CARTESIAN_POINT('Ctrl Pts',(-18.4519426090124,16.791349089629,0.));
#240529=CARTESIAN_POINT('Ctrl Pts',(-18.4615758042305,16.8148201995472,
0.));
#240530=CARTESIAN_POINT('Ctrl Pts',(-18.4711835548622,16.8383881879707,
0.));
#240531=CARTESIAN_POINT('Ctrl Pts',(-18.4807654268769,16.8620526977169,
0.));
#240532=CARTESIAN_POINT('Ctrl Pts',(-18.4903209902226,16.8858133733086,
0.));
#240533=CARTESIAN_POINT('Ctrl Pts',(-18.4998498184619,16.9096698606942,
0.));
#240534=CARTESIAN_POINT('Ctrl Pts',(-18.5093514883835,16.9336218069353,
0.));
#240535=CARTESIAN_POINT('Ctrl Pts',(-18.518825579666,16.957668859934,0.));
#240536=CARTESIAN_POINT('Ctrl Pts',(-18.5282716744198,16.9818106680382,
0.));
#240537=CARTESIAN_POINT('Ctrl Pts',(-18.5376893576961,17.0060468805099,
0.));
#240538=CARTESIAN_POINT('Ctrl Pts',(-18.5470782182089,17.030377148174,0.));
#240539=CARTESIAN_POINT('Ctrl Pts',(-18.5564378489628,17.0548011239751,
0.));
#240540=CARTESIAN_POINT('Ctrl Pts',(-18.5657678479788,17.0793184636079,
0.));
#240541=CARTESIAN_POINT('Ctrl Pts',(-18.5750678188543,17.1039288260001,
0.));
#240542=CARTESIAN_POINT('Ctrl Pts',(-18.5843373717253,17.1286318741185,
0.));
#240543=CARTESIAN_POINT('Ctrl Pts',(-18.5935761222833,17.1534272741646,
0.));
#240544=CARTESIAN_POINT('Ctrl Pts',(-18.6027836898826,17.1783146940131,
0.));
#240545=CARTESIAN_POINT('Ctrl Pts',(-18.6119596959957,17.2032938019288,
0.));
#240546=CARTESIAN_POINT('Ctrl Pts',(-18.6211037624041,17.2283642650519,
0.));
#240547=CARTESIAN_POINT('Ctrl Pts',(-18.630215509794,17.2535257482186,0.));
#240548=CARTESIAN_POINT('Ctrl Pts',(-18.639294555474,17.278777912021,0.));
#240549=CARTESIAN_POINT('Ctrl Pts',(-18.6483405141853,17.3041204135069,
0.));
#240550=CARTESIAN_POINT('Ctrl Pts',(-18.6573530024019,17.3295529098612,
0.));
#240551=CARTESIAN_POINT('Ctrl Pts',(-18.6663316416569,17.3550750612438,
0.));
#240552=CARTESIAN_POINT('Ctrl Pts',(-18.6752760624045,17.3806865340744,
0.));
#240553=CARTESIAN_POINT('Ctrl Pts',(-18.6841859073472,17.4063870038563,
0.));
#240554=CARTESIAN_POINT('Ctrl Pts',(-18.6930608357421,17.4321761588148,
0.));
#240555=CARTESIAN_POINT('Ctrl Pts',(-18.7019005250322,17.4580537012764,
0.));
#240556=CARTESIAN_POINT('Ctrl Pts',(-18.7107046613941,17.4840193397176,
0.));
#240557=CARTESIAN_POINT('Ctrl Pts',(-18.7194729318128,17.5100727820891,
0.));
#240558=CARTESIAN_POINT('Ctrl Pts',(-18.728205015716,17.5362137287604,0.));
#240559=CARTESIAN_POINT('Ctrl Pts',(-18.7369005764558,17.5624418653248,
0.));
#240560=CARTESIAN_POINT('Ctrl Pts',(-18.7455592536667,17.5887568561361,
0.));
#240561=CARTESIAN_POINT('Ctrl Pts',(-18.7541806530935,17.6151583356988,
0.));
#240562=CARTESIAN_POINT('Ctrl Pts',(-18.7627643613139,17.6416459210646,
0.));
#240563=CARTESIAN_POINT('Ctrl Pts',(-18.7713099642673,17.6682192274197,
0.));
#240564=CARTESIAN_POINT('Ctrl Pts',(-18.7798170641305,17.6948778822981,
0.));
#240565=CARTESIAN_POINT('Ctrl Pts',(-18.7882852976016,17.7216215409019,
0.));
#240566=CARTESIAN_POINT('Ctrl Pts',(-18.7967143519444,17.7484498996916,
0.));
#240567=CARTESIAN_POINT('Ctrl Pts',(-18.8051039860543,17.7753627137898,
0.));
#240568=CARTESIAN_POINT('Ctrl Pts',(-18.8134540340581,17.8023598011135,
0.));
#240569=CARTESIAN_POINT('Ctrl Pts',(-18.8217643886368,17.8294410311105,
0.));
#240570=CARTESIAN_POINT('Ctrl Pts',(-18.8300349896187,17.8566063174871,
0.));
#240571=CARTESIAN_POINT('Ctrl Pts',(-18.8366196462746,17.8784057509434,
0.));
#240572=CARTESIAN_POINT('Ctrl Pts',(-18.8415402351882,17.8947931177853,
0.));
#240573=CARTESIAN_POINT('Ctrl Pts',(-18.8448126709726,17.9057348246611,
0.));
#240574=CARTESIAN_POINT('Ctrl Pts',(-18.8464468996588,17.9112098770111,
0.));
#240575=CARTESIAN_POINT('',(-18.8464468996588,17.9112098770111,12.));
#240576=CARTESIAN_POINT('Ctrl Pts',(-18.8464468996588,17.9112098770111,
12.));
#240577=CARTESIAN_POINT('Ctrl Pts',(-18.8448126709726,17.9057348246611,
12.));
#240578=CARTESIAN_POINT('Ctrl Pts',(-18.8415402351882,17.8947931177853,
12.));
#240579=CARTESIAN_POINT('Ctrl Pts',(-18.8366196462746,17.8784057509434,
12.));
#240580=CARTESIAN_POINT('Ctrl Pts',(-18.8300349896187,17.8566063174871,
12.));
#240581=CARTESIAN_POINT('Ctrl Pts',(-18.8217643886368,17.8294410311105,
12.));
#240582=CARTESIAN_POINT('Ctrl Pts',(-18.8134540340581,17.8023598011135,
12.));
#240583=CARTESIAN_POINT('Ctrl Pts',(-18.8051039860543,17.7753627137898,
12.));
#240584=CARTESIAN_POINT('Ctrl Pts',(-18.7967143519444,17.7484498996916,
12.));
#240585=CARTESIAN_POINT('Ctrl Pts',(-18.7882852976016,17.7216215409019,
12.));
#240586=CARTESIAN_POINT('Ctrl Pts',(-18.7798170641305,17.6948778822981,
12.));
#240587=CARTESIAN_POINT('Ctrl Pts',(-18.7713099642673,17.6682192274197,
12.));
#240588=CARTESIAN_POINT('Ctrl Pts',(-18.7627643613139,17.6416459210646,
12.));
#240589=CARTESIAN_POINT('Ctrl Pts',(-18.7541806530935,17.6151583356988,
12.));
#240590=CARTESIAN_POINT('Ctrl Pts',(-18.7455592536667,17.5887568561361,
12.));
#240591=CARTESIAN_POINT('Ctrl Pts',(-18.7369005764558,17.5624418653248,
12.));
#240592=CARTESIAN_POINT('Ctrl Pts',(-18.728205015716,17.5362137287604,12.));
#240593=CARTESIAN_POINT('Ctrl Pts',(-18.7194729318128,17.5100727820891,
12.));
#240594=CARTESIAN_POINT('Ctrl Pts',(-18.7107046613941,17.4840193397176,
12.));
#240595=CARTESIAN_POINT('Ctrl Pts',(-18.7019005250322,17.4580537012764,
12.));
#240596=CARTESIAN_POINT('Ctrl Pts',(-18.6930608357421,17.4321761588148,
12.));
#240597=CARTESIAN_POINT('Ctrl Pts',(-18.6841859073472,17.4063870038563,
12.));
#240598=CARTESIAN_POINT('Ctrl Pts',(-18.6752760624045,17.3806865340744,
12.));
#240599=CARTESIAN_POINT('Ctrl Pts',(-18.6663316416569,17.3550750612438,
12.));
#240600=CARTESIAN_POINT('Ctrl Pts',(-18.6573530024019,17.3295529098612,
12.));
#240601=CARTESIAN_POINT('Ctrl Pts',(-18.6483405141853,17.3041204135069,
12.));
#240602=CARTESIAN_POINT('Ctrl Pts',(-18.639294555474,17.278777912021,12.));
#240603=CARTESIAN_POINT('Ctrl Pts',(-18.630215509794,17.2535257482186,12.));
#240604=CARTESIAN_POINT('Ctrl Pts',(-18.6211037624041,17.2283642650519,
12.));
#240605=CARTESIAN_POINT('Ctrl Pts',(-18.6119596959957,17.2032938019288,
12.));
#240606=CARTESIAN_POINT('Ctrl Pts',(-18.6027836898826,17.1783146940131,
12.));
#240607=CARTESIAN_POINT('Ctrl Pts',(-18.5935761222833,17.1534272741646,
12.));
#240608=CARTESIAN_POINT('Ctrl Pts',(-18.5843373717253,17.1286318741185,
12.));
#240609=CARTESIAN_POINT('Ctrl Pts',(-18.5750678188543,17.1039288260001,
12.));
#240610=CARTESIAN_POINT('Ctrl Pts',(-18.5657678479788,17.0793184636079,
12.));
#240611=CARTESIAN_POINT('Ctrl Pts',(-18.5564378489628,17.0548011239751,
12.));
#240612=CARTESIAN_POINT('Ctrl Pts',(-18.5470782182089,17.030377148174,12.));
#240613=CARTESIAN_POINT('Ctrl Pts',(-18.5376893576961,17.0060468805099,
12.));
#240614=CARTESIAN_POINT('Ctrl Pts',(-18.5282716744198,16.9818106680382,
12.));
#240615=CARTESIAN_POINT('Ctrl Pts',(-18.518825579666,16.957668859934,12.));
#240616=CARTESIAN_POINT('Ctrl Pts',(-18.5093514883835,16.9336218069353,
12.));
#240617=CARTESIAN_POINT('Ctrl Pts',(-18.4998498184619,16.9096698606942,
12.));
#240618=CARTESIAN_POINT('Ctrl Pts',(-18.4903209902226,16.8858133733086,
12.));
#240619=CARTESIAN_POINT('Ctrl Pts',(-18.4807654268769,16.8620526977169,
12.));
#240620=CARTESIAN_POINT('Ctrl Pts',(-18.4711835548622,16.8383881879707,
12.));
#240621=CARTESIAN_POINT('Ctrl Pts',(-18.4615758042305,16.8148201995472,
12.));
#240622=CARTESIAN_POINT('Ctrl Pts',(-18.4519426090124,16.791349089629,12.));
#240623=CARTESIAN_POINT('Ctrl Pts',(-18.4422844076099,16.7679752173992,
12.));
#240624=CARTESIAN_POINT('Ctrl Pts',(-18.4326016431392,16.7446989442882,
12.));
#240625=CARTESIAN_POINT('Ctrl Pts',(-18.4228947633186,16.7215206338818,
12.));
#240626=CARTESIAN_POINT('Ctrl Pts',(-18.413164220399,16.698440651849,12.));
#240627=CARTESIAN_POINT('Ctrl Pts',(-18.4034104710789,16.6754593658513,
12.));
#240628=CARTESIAN_POINT('Ctrl Pts',(-18.3936339764332,16.6525771454513,
12.));
#240629=CARTESIAN_POINT('Ctrl Pts',(-18.3838352018327,16.6297943620056,
12.));
#240630=CARTESIAN_POINT('Ctrl Pts',(-18.3740146168879,16.6071113885711,
12.));
#240631=CARTESIAN_POINT('Ctrl Pts',(-18.364172695589,16.5845286000218,12.));
#240632=CARTESIAN_POINT('Ctrl Pts',(-18.3543099164331,16.5620463731414,
12.));
#240633=CARTESIAN_POINT('Ctrl Pts',(-18.3444267625601,16.5396650867139,
12.));
#240634=CARTESIAN_POINT('Ctrl Pts',(-18.3345237218864,16.5173851216045,
12.));
#240635=CARTESIAN_POINT('Ctrl Pts',(-18.3246012872468,16.4952068608344,
12.));
#240636=CARTESIAN_POINT('Ctrl Pts',(-18.3146599565229,16.4731306896439,
12.));
#240637=CARTESIAN_POINT('Ctrl Pts',(-18.3047002326858,16.4511569955231,
12.));
#240638=CARTESIAN_POINT('Ctrl Pts',(-18.2947226238509,16.4292861682377,
12.));
#240639=CARTESIAN_POINT('Ctrl Pts',(-18.2847276433308,16.4075185998454,
12.));
#240640=CARTESIAN_POINT('Ctrl Pts',(-18.2747158096934,16.385854684708,12.));
#240641=CARTESIAN_POINT('Ctrl Pts',(-18.2646876468169,16.3642948194869,
12.));
#240642=CARTESIAN_POINT('Ctrl Pts',(-18.2546436839609,16.342839403159,12.));
#240643=CARTESIAN_POINT('Ctrl Pts',(-18.2445844558742,16.3214888370988,
12.));
#240644=CARTESIAN_POINT('Ctrl Pts',(-18.2345105028981,16.3002435251378,
12.));
#240645=CARTESIAN_POINT('Ctrl Pts',(-18.2244223710745,16.2791038736223,
12.));
#240646=CARTESIAN_POINT('Ctrl Pts',(-18.214320612253,16.2580702914615,12.));
#240647=CARTESIAN_POINT('Ctrl Pts',(-18.2042057842037,16.237143190164,12.));
#240648=CARTESIAN_POINT('Ctrl Pts',(-18.1940784507232,16.2163229838878,
12.));
#240649=CARTESIAN_POINT('Ctrl Pts',(-18.1839391817335,16.1956100895076,
12.));
#240650=CARTESIAN_POINT('Ctrl Pts',(-18.1737885533852,16.1750049266673,
12.));
#240651=CARTESIAN_POINT('Ctrl Pts',(-18.1636271481616,16.1545079178261,
12.));
#240652=CARTESIAN_POINT('Ctrl Pts',(-18.1534555549851,16.1341194882987,
12.));
#240653=CARTESIAN_POINT('Ctrl Pts',(-18.1432743693231,16.113840066279,12.));
#240654=CARTESIAN_POINT('Ctrl Pts',(-18.1330841933099,16.0936700829108,
12.));
#240655=CARTESIAN_POINT('Ctrl Pts',(-18.1228856358746,16.0736099723664,
12.));
#240656=CARTESIAN_POINT('Ctrl Pts',(-18.1126793128688,16.0536601719124,
12.));
#240657=CARTESIAN_POINT('Ctrl Pts',(-18.1024658471966,16.0338211219693,
12.));
#240658=CARTESIAN_POINT('Ctrl Pts',(-18.0922458689464,16.0140932661612,
12.));
#240659=CARTESIAN_POINT('Ctrl Pts',(-18.0820200155239,15.9944770513616,
12.));
#240660=CARTESIAN_POINT('Ctrl Pts',(-18.071788931796,15.9749729277848,12.));
#240661=CARTESIAN_POINT('Ctrl Pts',(-18.061553270236,15.9555813490645,12.));
#240662=CARTESIAN_POINT('Ctrl Pts',(-18.0513136910691,15.9363027723244,
12.));
#240663=CARTESIAN_POINT('Ctrl Pts',(-18.0410708624208,15.9171376582436,
12.));
#240664=CARTESIAN_POINT('Ctrl Pts',(-18.0308254604638,15.8980864711043,
12.));
#240665=CARTESIAN_POINT('Ctrl Pts',(-18.0205781695773,15.8791496788685,
12.));
#240666=CARTESIAN_POINT('Ctrl Pts',(-18.010329682521,15.8603277532834,12.));
#240667=CARTESIAN_POINT('Ctrl Pts',(-18.0000807006055,15.8416211699681,
12.));
#240668=CARTESIAN_POINT('Ctrl Pts',(-17.9898319338664,15.8230304084963,
12.));
#240669=CARTESIAN_POINT('Ctrl Pts',(-17.9795841012383,15.8045559524674,
12.));
#240670=CARTESIAN_POINT('Ctrl Pts',(-17.9693379307297,15.786198289572,12.));
#240671=CARTESIAN_POINT('Ctrl Pts',(-17.9590941596236,15.7679579117072,
12.));
#240672=CARTESIAN_POINT('Ctrl Pts',(-17.9488535346776,15.7498353150856,
12.));
#240673=CARTESIAN_POINT('Ctrl Pts',(-17.9386168123261,15.7318310003334,
12.));
#240674=CARTESIAN_POINT('Ctrl Pts',(-17.9283847588837,15.713945472584,12.));
#240675=CARTESIAN_POINT('Ctrl Pts',(-17.918158150746,15.6961792415526,12.));
#240676=CARTESIAN_POINT('Ctrl Pts',(-17.9079377746118,15.6785328216467,
12.));
#240677=CARTESIAN_POINT('Ctrl Pts',(-17.8977244277247,15.6610067321036,
12.));
#240678=CARTESIAN_POINT('Ctrl Pts',(-17.8875189181095,15.6436014971088,
12.));
#240679=CARTESIAN_POINT('Ctrl Pts',(-17.8773220648125,15.6263176459107,
12.));
#240680=CARTESIAN_POINT('Ctrl Pts',(-17.8671346981388,15.6091557129205,
12.));
#240681=CARTESIAN_POINT('Ctrl Pts',(-17.8569576598996,15.5921162378183,
12.));
#240682=CARTESIAN_POINT('Ctrl Pts',(-17.8467918036977,15.5751997657153,
12.));
#240683=CARTESIAN_POINT('Ctrl Pts',(-17.8366379952078,15.5584068472976,
12.));
#240684=CARTESIAN_POINT('Ctrl Pts',(-17.8264971124606,15.5417380389639,
12.));
#240685=CARTESIAN_POINT('Ctrl Pts',(-17.8163700461263,15.5251939029558,
12.));
#240686=CARTESIAN_POINT('Ctrl Pts',(-17.8062576997964,15.5087750074728,
12.));
#240687=CARTESIAN_POINT('Ctrl Pts',(-17.7961609903161,15.4924819268529,
12.));
#240688=CARTESIAN_POINT('Ctrl Pts',(-17.7860808481229,15.4763152417506,
12.));
#240689=CARTESIAN_POINT('Ctrl Pts',(-17.7760182175817,15.4602755393019,
12.));
#240690=CARTESIAN_POINT('Ctrl Pts',(-17.765974057326,15.4443634132865,12.));
#240691=CARTESIAN_POINT('Ctrl Pts',(-17.7559493405871,15.4285794642658,
12.));
#240692=CARTESIAN_POINT('Ctrl Pts',(-17.7459450555803,15.4129242997828,
12.));
#240693=CARTESIAN_POINT('Ctrl Pts',(-17.7359622059143,15.3973985345796,
12.));
#240694=CARTESIAN_POINT('Ctrl Pts',(-17.7260018109923,15.3820027907965,
12.));
#240695=CARTESIAN_POINT('Ctrl Pts',(-17.7160649064208,15.3667376981702,
12.));
#240696=CARTESIAN_POINT('Ctrl Pts',(-17.7061525444044,15.3516038942064,
12.));
#240697=CARTESIAN_POINT('Ctrl Pts',(-17.6962657941984,15.3366020244069,
12.));
#240698=CARTESIAN_POINT('Ctrl Pts',(-17.6864057426052,15.3217327425341,
12.));
#240699=CARTESIAN_POINT('Ctrl Pts',(-17.6765734944559,15.3069967108501,
12.));
#240700=CARTESIAN_POINT('Ctrl Pts',(-17.6667701731041,15.2923946003598,
12.));
#240701=CARTESIAN_POINT('Ctrl Pts',(-17.6569969209,15.2779270910238,12.));
#240702=CARTESIAN_POINT('Ctrl Pts',(-17.6472548997329,15.263594872029,12.));
#240703=CARTESIAN_POINT('Ctrl Pts',(-17.637545291637,15.2493986421091,12.));
#240704=CARTESIAN_POINT('Ctrl Pts',(-17.6278692993765,15.2353391098367,
12.));
#240705=CARTESIAN_POINT('Ctrl Pts',(-17.6182281470467,15.22141699392,12.));
#240706=CARTESIAN_POINT('Ctrl Pts',(-17.6086230806497,15.2076330234686,
12.));
#240707=CARTESIAN_POINT('Ctrl Pts',(-17.5990553687595,15.1939879383268,
12.));
#240708=CARTESIAN_POINT('Ctrl Pts',(-17.5895263032592,15.1804824894605,
12.));
#240709=CARTESIAN_POINT('Ctrl Pts',(-17.5800372000539,15.1671174393136,
12.));
#240710=CARTESIAN_POINT('Ctrl Pts',(-17.570589399803,15.1538935621714,12.));
#240711=CARTESIAN_POINT('Ctrl Pts',(-17.5611842686196,15.1408116444877,
12.));
#240712=CARTESIAN_POINT('Ctrl Pts',(-17.5518231989122,15.127872485314,12.));
#240713=CARTESIAN_POINT('Ctrl Pts',(-17.5425076102966,15.1150768967729,
12.));
#240714=CARTESIAN_POINT('Ctrl Pts',(-17.5332389504829,15.1024257045033,
12.));
#240715=CARTESIAN_POINT('Ctrl Pts',(-17.5240186961788,15.0899197481082,
12.));
#240716=CARTESIAN_POINT('Ctrl Pts',(-17.5148483539684,15.0775598815748,
12.));
#240717=CARTESIAN_POINT('Ctrl Pts',(-17.5057294613874,15.0653469738306,
12.));
#240718=CARTESIAN_POINT('Ctrl Pts',(-17.4966635880245,15.0532819093085,
12.));
#240719=CARTESIAN_POINT('Ctrl Pts',(-17.4876523366178,15.0413655884993,
12.));
#240720=CARTESIAN_POINT('Ctrl Pts',(-17.4786973441417,15.029598928488,12.));
#240721=CARTESIAN_POINT('Ctrl Pts',(-17.4698002829357,15.0179828635086,
12.));
#240722=CARTESIAN_POINT('Ctrl Pts',(-17.4609628621418,15.0065183456921,
12.));
#240723=CARTESIAN_POINT('Ctrl Pts',(-17.4521868291004,14.9952063457778,
12.));
#240724=CARTESIAN_POINT('Ctrl Pts',(-17.4434739707773,14.9840478538358,
12.));
#240725=CARTESIAN_POINT('Ctrl Pts',(-17.4348261151396,14.9730438799452,
12.));
#240726=CARTESIAN_POINT('Ctrl Pts',(-17.426245132709,14.9621954549827,12.));
#240727=CARTESIAN_POINT('Ctrl Pts',(-17.4177329382828,14.9515036315143,
12.));
#240728=CARTESIAN_POINT('Ctrl Pts',(-17.4092914926071,14.940969484645,12.));
#240729=CARTESIAN_POINT('Ctrl Pts',(-17.4009228040749,14.9305941128757,
12.));
#240730=CARTESIAN_POINT('Ctrl Pts',(-17.3926289303986,14.9203786389342,
12.));
#240731=CARTESIAN_POINT('Ctrl Pts',(-17.3844119809824,14.9103242110057,
12.));
#240732=CARTESIAN_POINT('Ctrl Pts',(-17.3762741193076,14.900432003961,12.));
#240733=CARTESIAN_POINT('Ctrl Pts',(-17.3682175653235,14.8907032205788,
12.));
#240734=CARTESIAN_POINT('Ctrl Pts',(-17.3602445978161,14.8811390927423,
12.));
#240735=CARTESIAN_POINT('Ctrl Pts',(-17.3523575568645,14.8717408826955,
12.));
#240736=CARTESIAN_POINT('Ctrl Pts',(-17.3445588463475,14.8625098843417,
12.));
#240737=CARTESIAN_POINT('Ctrl Pts',(-17.336850936485,14.8534474245433,12.));
#240738=CARTESIAN_POINT('Ctrl Pts',(-17.3292363662605,14.8445548643508,
12.));
#240739=CARTESIAN_POINT('Ctrl Pts',(-17.3217177462101,14.8358336004197,
12.));
#240740=CARTESIAN_POINT('Ctrl Pts',(-17.3142977632659,14.8272850675379,
12.));
#240741=CARTESIAN_POINT('Ctrl Pts',(-17.3069791853706,14.8189107410162,
12.));
#240742=CARTESIAN_POINT('Ctrl Pts',(-17.299764866148,14.8107121391035,12.));
#240743=CARTESIAN_POINT('Ctrl Pts',(-17.2926577496513,14.8026908254276,
12.));
#240744=CARTESIAN_POINT('Ctrl Pts',(-17.2856608733196,14.7948484105249,
12.));
#240745=CARTESIAN_POINT('Ctrl Pts',(-17.2787773704849,14.787186553128,12.));
#240746=CARTESIAN_POINT('Ctrl Pts',(-17.2720104735194,14.7797069617804,
12.));
#240747=CARTESIAN_POINT('Ctrl Pts',(-17.2653635155319,14.7724113956731,
12.));
#240748=CARTESIAN_POINT('Ctrl Pts',(-17.2588399401465,14.7653016697591,
12.));
#240749=CARTESIAN_POINT('Ctrl Pts',(-17.2524433146837,14.7583796616617,
12.));
#240750=CARTESIAN_POINT('Ctrl Pts',(-17.2461773413288,14.7516473175124,
12.));
#240751=CARTESIAN_POINT('Ctrl Pts',(-17.2400458713565,14.7451066593792,
12.));
#240752=CARTESIAN_POINT('Ctrl Pts',(-17.2340529062076,14.7387597858116,
12.));
#240753=CARTESIAN_POINT('Ctrl Pts',(-17.2282025904314,14.7326088681163,
12.));
#240754=CARTESIAN_POINT('Ctrl Pts',(-17.2224992099667,14.7266561494282,
12.));
#240755=CARTESIAN_POINT('Ctrl Pts',(-17.2169471814256,14.7209039390327,
12.));
#240756=CARTESIAN_POINT('Ctrl Pts',(-17.2115510835989,14.7153546289339,
12.));
#240757=CARTESIAN_POINT('Ctrl Pts',(-17.2063157097315,14.7100107213586,
12.));
#240758=CARTESIAN_POINT('Ctrl Pts',(-17.2012461084268,14.7048748502663,
12.));
#240759=CARTESIAN_POINT('Ctrl Pts',(-17.1963476411694,14.699949811582,12.));
#240760=CARTESIAN_POINT('Ctrl Pts',(-17.1916259308415,14.6952385361705,
12.));
#240761=CARTESIAN_POINT('Ctrl Pts',(-17.1870867909918,14.6907440526958,
12.));
#240762=CARTESIAN_POINT('Ctrl Pts',(-17.182736158472,14.686469452232,12.));
#240763=CARTESIAN_POINT('Ctrl Pts',(-17.1785800350826,14.6824178576167,
12.));
#240764=CARTESIAN_POINT('Ctrl Pts',(-17.1746247499057,14.6785925615677,
12.));
#240765=CARTESIAN_POINT('Ctrl Pts',(-17.1708771619129,14.6749971333867,
12.));
#240766=CARTESIAN_POINT('Ctrl Pts',(-17.167344972302,14.671635583332,12.));
#240767=CARTESIAN_POINT('Ctrl Pts',(-17.1640366762305,14.6685123374423,
12.));
#240768=CARTESIAN_POINT('Ctrl Pts',(-17.1609609517369,14.6656319165057,
12.));
#240769=CARTESIAN_POINT('Ctrl Pts',(-17.1581262646789,14.6629987285992,
12.));
#240770=CARTESIAN_POINT('Ctrl Pts',(-17.1555401986401,14.6606167169642,
12.));
#240771=CARTESIAN_POINT('Ctrl Pts',(-17.1532107762718,14.6584900555302,
12.));
#240772=CARTESIAN_POINT('Ctrl Pts',(-17.1511476869496,14.6566237952435,
12.));
#240773=CARTESIAN_POINT('Ctrl Pts',(-17.1493641837558,14.655024862281,12.));
#240774=CARTESIAN_POINT('Ctrl Pts',(-17.147876394491,14.6537016966184,12.));
#240775=CARTESIAN_POINT('Ctrl Pts',(-17.1466998098673,14.6526624064978,
12.));
#240776=CARTESIAN_POINT('Ctrl Pts',(-17.1458462295271,14.6519131634508,
12.));
#240777=CARTESIAN_POINT('Ctrl Pts',(-17.1454262858043,14.6515481598068,
12.));
#240778=CARTESIAN_POINT('Ctrl Pts',(-17.1452600887037,14.6514066997196,
12.));
#240779=CARTESIAN_POINT('Ctrl Pts',(-17.1452153999142,14.6513711852843,
12.));
#240780=CARTESIAN_POINT('Ctrl Pts',(-17.1452095830633,14.6513681262571,
12.));
#240781=CARTESIAN_POINT('',(-18.8464468996588,17.9112098770111,0.));
#240782=CARTESIAN_POINT('Origin',(-12.1729687575668,17.7219872369693,0.));
#240783=CARTESIAN_POINT('',(-12.7689476255363,18.5896416359912,12.));
#240784=CARTESIAN_POINT('',(-6.08648437878338,8.86099361848466,12.));
#240785=CARTESIAN_POINT('',(-12.7689476255363,18.5896416359912,0.));
#240786=CARTESIAN_POINT('',(-12.7689476255363,18.5896416359912,0.));
#240787=CARTESIAN_POINT('',(-6.08648437878338,8.86099361848466,0.));
#240788=CARTESIAN_POINT('Ctrl Pts',(-17.9112098770111,18.8464468996588,
0.));
#240789=CARTESIAN_POINT('Ctrl Pts',(-17.9112098770111,18.8464468996588,
12.));
#240790=CARTESIAN_POINT('Ctrl Pts',(-17.9057348246595,18.8448126709691,
0.));
#240791=CARTESIAN_POINT('Ctrl Pts',(-17.9057348246595,18.8448126709691,
12.));
#240792=CARTESIAN_POINT('Ctrl Pts',(-17.8947931177807,18.8415402351786,
0.));
#240793=CARTESIAN_POINT('Ctrl Pts',(-17.8947931177807,18.8415402351786,
12.));
#240794=CARTESIAN_POINT('Ctrl Pts',(-17.8784057509356,18.8366196462581,
0.));
#240795=CARTESIAN_POINT('Ctrl Pts',(-17.8784057509356,18.8366196462581,
12.));
#240796=CARTESIAN_POINT('Ctrl Pts',(-17.8566063174771,18.8300349895974,
0.));
#240797=CARTESIAN_POINT('Ctrl Pts',(-17.8566063174771,18.8300349895974,
12.));
#240798=CARTESIAN_POINT('Ctrl Pts',(-17.8294410311006,18.8217643886157,
0.));
#240799=CARTESIAN_POINT('Ctrl Pts',(-17.8294410311006,18.8217643886157,
12.));
#240800=CARTESIAN_POINT('Ctrl Pts',(-17.8023598011057,18.8134540340417,
0.));
#240801=CARTESIAN_POINT('Ctrl Pts',(-17.8023598011057,18.8134540340417,
12.));
#240802=CARTESIAN_POINT('Ctrl Pts',(-17.7753627137853,18.8051039860448,
0.));
#240803=CARTESIAN_POINT('Ctrl Pts',(-17.7753627137853,18.8051039860448,
12.));
#240804=CARTESIAN_POINT('Ctrl Pts',(-17.7484498996905,18.7967143519419,
0.));
#240805=CARTESIAN_POINT('Ctrl Pts',(-17.7484498996905,18.7967143519419,
12.));
#240806=CARTESIAN_POINT('Ctrl Pts',(-17.7216215409035,18.7882852976049,
0.));
#240807=CARTESIAN_POINT('Ctrl Pts',(-17.7216215409035,18.7882852976049,
12.));
#240808=CARTESIAN_POINT('Ctrl Pts',(-17.6948778823014,18.7798170641374,
0.));
#240809=CARTESIAN_POINT('Ctrl Pts',(-17.6948778823014,18.7798170641374,
12.));
#240810=CARTESIAN_POINT('Ctrl Pts',(-17.6682192274236,18.7713099642754,
0.));
#240811=CARTESIAN_POINT('Ctrl Pts',(-17.6682192274236,18.7713099642754,
12.));
#240812=CARTESIAN_POINT('Ctrl Pts',(-17.6416459210681,18.762764361321,0.));
#240813=CARTESIAN_POINT('Ctrl Pts',(-17.6416459210681,18.762764361321,12.));
#240814=CARTESIAN_POINT('Ctrl Pts',(-17.6151583357012,18.7541806530984,
0.));
#240815=CARTESIAN_POINT('Ctrl Pts',(-17.6151583357012,18.7541806530984,
12.));
#240816=CARTESIAN_POINT('Ctrl Pts',(-17.5887568561371,18.7455592536687,
0.));
#240817=CARTESIAN_POINT('Ctrl Pts',(-17.5887568561371,18.7455592536687,
12.));
#240818=CARTESIAN_POINT('Ctrl Pts',(-17.5624418653245,18.7369005764553,
0.));
#240819=CARTESIAN_POINT('Ctrl Pts',(-17.5624418653245,18.7369005764553,
12.));
#240820=CARTESIAN_POINT('Ctrl Pts',(-17.5362137287593,18.7282050157138,
0.));
#240821=CARTESIAN_POINT('Ctrl Pts',(-17.5362137287593,18.7282050157138,
12.));
#240822=CARTESIAN_POINT('Ctrl Pts',(-17.5100727820876,18.7194729318098,
0.));
#240823=CARTESIAN_POINT('Ctrl Pts',(-17.5100727820876,18.7194729318098,
12.));
#240824=CARTESIAN_POINT('Ctrl Pts',(-17.4840193397162,18.7107046613912,
0.));
#240825=CARTESIAN_POINT('Ctrl Pts',(-17.4840193397162,18.7107046613912,
12.));
#240826=CARTESIAN_POINT('Ctrl Pts',(-17.4580537012753,18.70190052503,0.));
#240827=CARTESIAN_POINT('Ctrl Pts',(-17.4580537012753,18.70190052503,12.));
#240828=CARTESIAN_POINT('Ctrl Pts',(-17.4321761588142,18.6930608357409,
0.));
#240829=CARTESIAN_POINT('Ctrl Pts',(-17.4321761588142,18.6930608357409,
12.));
#240830=CARTESIAN_POINT('Ctrl Pts',(-17.4063870038562,18.6841859073471,
0.));
#240831=CARTESIAN_POINT('Ctrl Pts',(-17.4063870038562,18.6841859073471,
12.));
#240832=CARTESIAN_POINT('Ctrl Pts',(-17.3806865340747,18.6752760624052,
0.));
#240833=CARTESIAN_POINT('Ctrl Pts',(-17.3806865340747,18.6752760624052,
12.));
#240834=CARTESIAN_POINT('Ctrl Pts',(-17.3550750612443,18.6663316416582,
0.));
#240835=CARTESIAN_POINT('Ctrl Pts',(-17.3550750612443,18.6663316416582,
12.));
#240836=CARTESIAN_POINT('Ctrl Pts',(-17.3295529098618,18.6573530024033,
0.));
#240837=CARTESIAN_POINT('Ctrl Pts',(-17.3295529098618,18.6573530024033,
12.));
#240838=CARTESIAN_POINT('Ctrl Pts',(-17.3041204135074,18.6483405141865,
0.));
#240839=CARTESIAN_POINT('Ctrl Pts',(-17.3041204135074,18.6483405141865,
12.));
#240840=CARTESIAN_POINT('Ctrl Pts',(-17.2787779120213,18.6392945554748,
0.));
#240841=CARTESIAN_POINT('Ctrl Pts',(-17.2787779120213,18.6392945554748,
12.));
#240842=CARTESIAN_POINT('Ctrl Pts',(-17.2535257482187,18.6302155097943,
0.));
#240843=CARTESIAN_POINT('Ctrl Pts',(-17.2535257482187,18.6302155097943,
12.));
#240844=CARTESIAN_POINT('Ctrl Pts',(-17.2283642650518,18.6211037624038,
0.));
#240845=CARTESIAN_POINT('Ctrl Pts',(-17.2283642650518,18.6211037624038,
12.));
#240846=CARTESIAN_POINT('Ctrl Pts',(-17.2032938019284,18.6119596959949,
0.));
#240847=CARTESIAN_POINT('Ctrl Pts',(-17.2032938019284,18.6119596959949,
12.));
#240848=CARTESIAN_POINT('Ctrl Pts',(-17.1783146940127,18.6027836898817,
0.));
#240849=CARTESIAN_POINT('Ctrl Pts',(-17.1783146940127,18.6027836898817,
12.));
#240850=CARTESIAN_POINT('Ctrl Pts',(-17.1534272741643,18.5935761222825,
0.));
#240851=CARTESIAN_POINT('Ctrl Pts',(-17.1534272741643,18.5935761222825,
12.));
#240852=CARTESIAN_POINT('Ctrl Pts',(-17.1286318741183,18.5843373717247,
0.));
#240853=CARTESIAN_POINT('Ctrl Pts',(-17.1286318741183,18.5843373717247,
12.));
#240854=CARTESIAN_POINT('Ctrl Pts',(-17.1039288260001,18.5750678188542,
0.));
#240855=CARTESIAN_POINT('Ctrl Pts',(-17.1039288260001,18.5750678188542,
12.));
#240856=CARTESIAN_POINT('Ctrl Pts',(-17.0793184636079,18.5657678479789,
0.));
#240857=CARTESIAN_POINT('Ctrl Pts',(-17.0793184636079,18.5657678479789,
12.));
#240858=CARTESIAN_POINT('Ctrl Pts',(-17.0548011239751,18.556437848963,0.));
#240859=CARTESIAN_POINT('Ctrl Pts',(-17.0548011239751,18.556437848963,12.));
#240860=CARTESIAN_POINT('Ctrl Pts',(-17.0303771481738,18.547078218209,0.));
#240861=CARTESIAN_POINT('Ctrl Pts',(-17.0303771481738,18.547078218209,12.));
#240862=CARTESIAN_POINT('Ctrl Pts',(-17.0060468805097,18.5376893576961,
0.));
#240863=CARTESIAN_POINT('Ctrl Pts',(-17.0060468805097,18.5376893576961,
12.));
#240864=CARTESIAN_POINT('Ctrl Pts',(-16.981810668038,18.5282716744197,0.));
#240865=CARTESIAN_POINT('Ctrl Pts',(-16.981810668038,18.5282716744197,12.));
#240866=CARTESIAN_POINT('Ctrl Pts',(-16.9576688599339,18.5188255796659,
0.));
#240867=CARTESIAN_POINT('Ctrl Pts',(-16.9576688599339,18.5188255796659,
12.));
#240868=CARTESIAN_POINT('Ctrl Pts',(-16.9336218069353,18.5093514883835,
0.));
#240869=CARTESIAN_POINT('Ctrl Pts',(-16.9336218069353,18.5093514883835,
12.));
#240870=CARTESIAN_POINT('Ctrl Pts',(-16.9096698606943,18.499849818462,0.));
#240871=CARTESIAN_POINT('Ctrl Pts',(-16.9096698606943,18.499849818462,12.));
#240872=CARTESIAN_POINT('Ctrl Pts',(-16.8858133733088,18.4903209902227,
0.));
#240873=CARTESIAN_POINT('Ctrl Pts',(-16.8858133733088,18.4903209902227,
12.));
#240874=CARTESIAN_POINT('Ctrl Pts',(-16.8620526977171,18.480765426877,0.));
#240875=CARTESIAN_POINT('Ctrl Pts',(-16.8620526977171,18.480765426877,12.));
#240876=CARTESIAN_POINT('Ctrl Pts',(-16.8383881879709,18.4711835548623,
0.));
#240877=CARTESIAN_POINT('Ctrl Pts',(-16.8383881879709,18.4711835548623,
12.));
#240878=CARTESIAN_POINT('Ctrl Pts',(-16.8148201995472,18.4615758042305,
0.));
#240879=CARTESIAN_POINT('Ctrl Pts',(-16.8148201995472,18.4615758042305,
12.));
#240880=CARTESIAN_POINT('Ctrl Pts',(-16.791349089629,18.4519426090123,0.));
#240881=CARTESIAN_POINT('Ctrl Pts',(-16.791349089629,18.4519426090123,12.));
#240882=CARTESIAN_POINT('Ctrl Pts',(-16.7679752173992,18.44228440761,0.));
#240883=CARTESIAN_POINT('Ctrl Pts',(-16.7679752173992,18.44228440761,12.));
#240884=CARTESIAN_POINT('Ctrl Pts',(-16.7446989442882,18.4326016431392,
0.));
#240885=CARTESIAN_POINT('Ctrl Pts',(-16.7446989442882,18.4326016431392,
12.));
#240886=CARTESIAN_POINT('Ctrl Pts',(-16.7215206338818,18.4228947633187,
0.));
#240887=CARTESIAN_POINT('Ctrl Pts',(-16.7215206338818,18.4228947633187,
12.));
#240888=CARTESIAN_POINT('Ctrl Pts',(-16.6984406518491,18.413164220399,0.));
#240889=CARTESIAN_POINT('Ctrl Pts',(-16.6984406518491,18.413164220399,12.));
#240890=CARTESIAN_POINT('Ctrl Pts',(-16.6754593658513,18.403410471079,0.));
#240891=CARTESIAN_POINT('Ctrl Pts',(-16.6754593658513,18.403410471079,12.));
#240892=CARTESIAN_POINT('Ctrl Pts',(-16.6525771454513,18.3936339764332,
0.));
#240893=CARTESIAN_POINT('Ctrl Pts',(-16.6525771454513,18.3936339764332,
12.));
#240894=CARTESIAN_POINT('Ctrl Pts',(-16.6297943620056,18.3838352018327,
0.));
#240895=CARTESIAN_POINT('Ctrl Pts',(-16.6297943620056,18.3838352018327,
12.));
#240896=CARTESIAN_POINT('Ctrl Pts',(-16.607111388571,18.3740146168879,0.));
#240897=CARTESIAN_POINT('Ctrl Pts',(-16.607111388571,18.3740146168879,12.));
#240898=CARTESIAN_POINT('Ctrl Pts',(-16.5845286000217,18.3641726955889,
0.));
#240899=CARTESIAN_POINT('Ctrl Pts',(-16.5845286000217,18.3641726955889,
12.));
#240900=CARTESIAN_POINT('Ctrl Pts',(-16.5620463731413,18.354309916433,0.));
#240901=CARTESIAN_POINT('Ctrl Pts',(-16.5620463731413,18.354309916433,12.));
#240902=CARTESIAN_POINT('Ctrl Pts',(-16.5396650867139,18.34442676256,0.));
#240903=CARTESIAN_POINT('Ctrl Pts',(-16.5396650867139,18.34442676256,12.));
#240904=CARTESIAN_POINT('Ctrl Pts',(-16.5173851216045,18.3345237218864,
0.));
#240905=CARTESIAN_POINT('Ctrl Pts',(-16.5173851216045,18.3345237218864,
12.));
#240906=CARTESIAN_POINT('Ctrl Pts',(-16.4952068608345,18.3246012872469,
0.));
#240907=CARTESIAN_POINT('Ctrl Pts',(-16.4952068608345,18.3246012872469,
12.));
#240908=CARTESIAN_POINT('Ctrl Pts',(-16.4731306896441,18.3146599565231,
0.));
#240909=CARTESIAN_POINT('Ctrl Pts',(-16.4731306896441,18.3146599565231,
12.));
#240910=CARTESIAN_POINT('Ctrl Pts',(-16.4511569955233,18.304700232686,0.));
#240911=CARTESIAN_POINT('Ctrl Pts',(-16.4511569955233,18.304700232686,12.));
#240912=CARTESIAN_POINT('Ctrl Pts',(-16.4292861682379,18.294722623851,0.));
#240913=CARTESIAN_POINT('Ctrl Pts',(-16.4292861682379,18.294722623851,12.));
#240914=CARTESIAN_POINT('Ctrl Pts',(-16.4075185998455,18.2847276433309,
0.));
#240915=CARTESIAN_POINT('Ctrl Pts',(-16.4075185998455,18.2847276433309,
12.));
#240916=CARTESIAN_POINT('Ctrl Pts',(-16.385854684708,18.2747158096934,0.));
#240917=CARTESIAN_POINT('Ctrl Pts',(-16.385854684708,18.2747158096934,12.));
#240918=CARTESIAN_POINT('Ctrl Pts',(-16.3642948194868,18.2646876468169,
0.));
#240919=CARTESIAN_POINT('Ctrl Pts',(-16.3642948194868,18.2646876468169,
12.));
#240920=CARTESIAN_POINT('Ctrl Pts',(-16.3428394031589,18.2546436839608,
0.));
#240921=CARTESIAN_POINT('Ctrl Pts',(-16.3428394031589,18.2546436839608,
12.));
#240922=CARTESIAN_POINT('Ctrl Pts',(-16.3214888370987,18.2445844558741,
0.));
#240923=CARTESIAN_POINT('Ctrl Pts',(-16.3214888370987,18.2445844558741,
12.));
#240924=CARTESIAN_POINT('Ctrl Pts',(-16.3002435251378,18.2345105028982,
0.));
#240925=CARTESIAN_POINT('Ctrl Pts',(-16.3002435251378,18.2345105028982,
12.));
#240926=CARTESIAN_POINT('Ctrl Pts',(-16.2791038736223,18.2244223710745,
0.));
#240927=CARTESIAN_POINT('Ctrl Pts',(-16.2791038736223,18.2244223710745,
12.));
#240928=CARTESIAN_POINT('Ctrl Pts',(-16.2580702914615,18.2143206122529,
0.));
#240929=CARTESIAN_POINT('Ctrl Pts',(-16.2580702914615,18.2143206122529,
12.));
#240930=CARTESIAN_POINT('Ctrl Pts',(-16.2371431901638,18.2042057842035,
0.));
#240931=CARTESIAN_POINT('Ctrl Pts',(-16.2371431901638,18.2042057842035,
12.));
#240932=CARTESIAN_POINT('Ctrl Pts',(-16.2163229838875,18.1940784507229,
0.));
#240933=CARTESIAN_POINT('Ctrl Pts',(-16.2163229838875,18.1940784507229,
12.));
#240934=CARTESIAN_POINT('Ctrl Pts',(-16.1956100895073,18.1839391817331,
0.));
#240935=CARTESIAN_POINT('Ctrl Pts',(-16.1956100895073,18.1839391817331,
12.));
#240936=CARTESIAN_POINT('Ctrl Pts',(-16.1750049266671,18.1737885533849,
0.));
#240937=CARTESIAN_POINT('Ctrl Pts',(-16.1750049266671,18.1737885533849,
12.));
#240938=CARTESIAN_POINT('Ctrl Pts',(-16.154507917826,18.1636271481615,0.));
#240939=CARTESIAN_POINT('Ctrl Pts',(-16.154507917826,18.1636271481615,12.));
#240940=CARTESIAN_POINT('Ctrl Pts',(-16.1341194882988,18.1534555549852,
0.));
#240941=CARTESIAN_POINT('Ctrl Pts',(-16.1341194882988,18.1534555549852,
12.));
#240942=CARTESIAN_POINT('Ctrl Pts',(-16.1138400662794,18.1432743693235,
0.));
#240943=CARTESIAN_POINT('Ctrl Pts',(-16.1138400662794,18.1432743693235,
12.));
#240944=CARTESIAN_POINT('Ctrl Pts',(-16.0936700829112,18.1330841933105,
0.));
#240945=CARTESIAN_POINT('Ctrl Pts',(-16.0936700829112,18.1330841933105,
12.));
#240946=CARTESIAN_POINT('Ctrl Pts',(-16.0736099723668,18.1228856358751,
0.));
#240947=CARTESIAN_POINT('Ctrl Pts',(-16.0736099723668,18.1228856358751,
12.));
#240948=CARTESIAN_POINT('Ctrl Pts',(-16.0536601719126,18.112679312869,0.));
#240949=CARTESIAN_POINT('Ctrl Pts',(-16.0536601719126,18.112679312869,12.));
#240950=CARTESIAN_POINT('Ctrl Pts',(-16.0338211219693,18.1024658471966,
0.));
#240951=CARTESIAN_POINT('Ctrl Pts',(-16.0338211219693,18.1024658471966,
12.));
#240952=CARTESIAN_POINT('Ctrl Pts',(-16.014093266161,18.0922458689462,0.));
#240953=CARTESIAN_POINT('Ctrl Pts',(-16.014093266161,18.0922458689462,12.));
#240954=CARTESIAN_POINT('Ctrl Pts',(-15.9944770513613,18.0820200155236,
0.));
#240955=CARTESIAN_POINT('Ctrl Pts',(-15.9944770513613,18.0820200155236,
12.));
#240956=CARTESIAN_POINT('Ctrl Pts',(-15.9749729277846,18.0717889317958,
0.));
#240957=CARTESIAN_POINT('Ctrl Pts',(-15.9749729277846,18.0717889317958,
12.));
#240958=CARTESIAN_POINT('Ctrl Pts',(-15.9555813490644,18.0615532702359,
0.));
#240959=CARTESIAN_POINT('Ctrl Pts',(-15.9555813490644,18.0615532702359,
12.));
#240960=CARTESIAN_POINT('Ctrl Pts',(-15.9363027723244,18.0513136910691,
0.));
#240961=CARTESIAN_POINT('Ctrl Pts',(-15.9363027723244,18.0513136910691,
12.));
#240962=CARTESIAN_POINT('Ctrl Pts',(-15.9171376582436,18.0410708624208,
0.));
#240963=CARTESIAN_POINT('Ctrl Pts',(-15.9171376582436,18.0410708624208,
12.));
#240964=CARTESIAN_POINT('Ctrl Pts',(-15.8980864711042,18.0308254604636,
0.));
#240965=CARTESIAN_POINT('Ctrl Pts',(-15.8980864711042,18.0308254604636,
12.));
#240966=CARTESIAN_POINT('Ctrl Pts',(-15.8791496788683,18.0205781695769,
0.));
#240967=CARTESIAN_POINT('Ctrl Pts',(-15.8791496788683,18.0205781695769,
12.));
#240968=CARTESIAN_POINT('Ctrl Pts',(-15.8603277532831,18.0103296825205,
0.));
#240969=CARTESIAN_POINT('Ctrl Pts',(-15.8603277532831,18.0103296825205,
12.));
#240970=CARTESIAN_POINT('Ctrl Pts',(-15.8416211699679,18.0000807006052,
0.));
#240971=CARTESIAN_POINT('Ctrl Pts',(-15.8416211699679,18.0000807006052,
12.));
#240972=CARTESIAN_POINT('Ctrl Pts',(-15.8230304084962,17.9898319338664,
0.));
#240973=CARTESIAN_POINT('Ctrl Pts',(-15.8230304084962,17.9898319338664,
12.));
#240974=CARTESIAN_POINT('Ctrl Pts',(-15.8045559524676,17.9795841012386,
0.));
#240975=CARTESIAN_POINT('Ctrl Pts',(-15.8045559524676,17.9795841012386,
12.));
#240976=CARTESIAN_POINT('Ctrl Pts',(-15.7861982895724,17.9693379307303,
0.));
#240977=CARTESIAN_POINT('Ctrl Pts',(-15.7861982895724,17.9693379307303,
12.));
#240978=CARTESIAN_POINT('Ctrl Pts',(-15.7679579117077,17.9590941596242,
0.));
#240979=CARTESIAN_POINT('Ctrl Pts',(-15.7679579117077,17.9590941596242,
12.));
#240980=CARTESIAN_POINT('Ctrl Pts',(-15.749835315086,17.9488535346781,0.));
#240981=CARTESIAN_POINT('Ctrl Pts',(-15.749835315086,17.9488535346781,12.));
#240982=CARTESIAN_POINT('Ctrl Pts',(-15.7318310003335,17.9386168123262,
0.));
#240983=CARTESIAN_POINT('Ctrl Pts',(-15.7318310003335,17.9386168123262,
12.));
#240984=CARTESIAN_POINT('Ctrl Pts',(-15.7139454725838,17.9283847588835,
0.));
#240985=CARTESIAN_POINT('Ctrl Pts',(-15.7139454725838,17.9283847588835,
12.));
#240986=CARTESIAN_POINT('Ctrl Pts',(-15.6961792415522,17.9181581507455,
0.));
#240987=CARTESIAN_POINT('Ctrl Pts',(-15.6961792415522,17.9181581507455,
12.));
#240988=CARTESIAN_POINT('Ctrl Pts',(-15.678532821646,17.9079377746111,0.));
#240989=CARTESIAN_POINT('Ctrl Pts',(-15.678532821646,17.9079377746111,12.));
#240990=CARTESIAN_POINT('Ctrl Pts',(-15.661006732103,17.897724427724,0.));
#240991=CARTESIAN_POINT('Ctrl Pts',(-15.661006732103,17.897724427724,12.));
#240992=CARTESIAN_POINT('Ctrl Pts',(-15.6436014971084,17.8875189181091,
0.));
#240993=CARTESIAN_POINT('Ctrl Pts',(-15.6436014971084,17.8875189181091,
12.));
#240994=CARTESIAN_POINT('Ctrl Pts',(-15.6263176459108,17.8773220648125,
0.));
#240995=CARTESIAN_POINT('Ctrl Pts',(-15.6263176459108,17.8773220648125,
12.));
#240996=CARTESIAN_POINT('Ctrl Pts',(-15.609155712921,17.8671346981394,0.));
#240997=CARTESIAN_POINT('Ctrl Pts',(-15.609155712921,17.8671346981394,12.));
#240998=CARTESIAN_POINT('Ctrl Pts',(-15.5921162378192,17.8569576599006,
0.));
#240999=CARTESIAN_POINT('Ctrl Pts',(-15.5921162378192,17.8569576599006,
12.));
#241000=CARTESIAN_POINT('Ctrl Pts',(-15.5751997657163,17.8467918036987,
0.));
#241001=CARTESIAN_POINT('Ctrl Pts',(-15.5751997657163,17.8467918036987,
12.));
#241002=CARTESIAN_POINT('Ctrl Pts',(-15.5584068472982,17.8366379952085,
0.));
#241003=CARTESIAN_POINT('Ctrl Pts',(-15.5584068472982,17.8366379952085,
12.));
#241004=CARTESIAN_POINT('Ctrl Pts',(-15.541738038964,17.8264971124606,0.));
#241005=CARTESIAN_POINT('Ctrl Pts',(-15.541738038964,17.8264971124606,12.));
#241006=CARTESIAN_POINT('Ctrl Pts',(-15.5251939029552,17.8163700461256,
0.));
#241007=CARTESIAN_POINT('Ctrl Pts',(-15.5251939029552,17.8163700461256,
12.));
#241008=CARTESIAN_POINT('Ctrl Pts',(-15.5087750074718,17.8062576997952,
0.));
#241009=CARTESIAN_POINT('Ctrl Pts',(-15.5087750074718,17.8062576997952,
12.));
#241010=CARTESIAN_POINT('Ctrl Pts',(-15.4924819268517,17.7961609903148,
0.));
#241011=CARTESIAN_POINT('Ctrl Pts',(-15.4924819268517,17.7961609903148,
12.));
#241012=CARTESIAN_POINT('Ctrl Pts',(-15.4763152417497,17.7860808481219,
0.));
#241013=CARTESIAN_POINT('Ctrl Pts',(-15.4763152417497,17.7860808481219,
12.));
#241014=CARTESIAN_POINT('Ctrl Pts',(-15.4602755393017,17.7760182175815,
0.));
#241015=CARTESIAN_POINT('Ctrl Pts',(-15.4602755393017,17.7760182175815,
12.));
#241016=CARTESIAN_POINT('Ctrl Pts',(-15.4443634132869,17.7659740573265,
0.));
#241017=CARTESIAN_POINT('Ctrl Pts',(-15.4443634132869,17.7659740573265,
12.));
#241018=CARTESIAN_POINT('Ctrl Pts',(-15.4285794642668,17.7559493405881,
0.));
#241019=CARTESIAN_POINT('Ctrl Pts',(-15.4285794642668,17.7559493405881,
12.));
#241020=CARTESIAN_POINT('Ctrl Pts',(-15.4129242997837,17.7459450555812,
0.));
#241021=CARTESIAN_POINT('Ctrl Pts',(-15.4129242997837,17.7459450555812,
12.));
#241022=CARTESIAN_POINT('Ctrl Pts',(-15.3973985345802,17.7359622059149,
0.));
#241023=CARTESIAN_POINT('Ctrl Pts',(-15.3973985345802,17.7359622059149,
12.));
#241024=CARTESIAN_POINT('Ctrl Pts',(-15.3820027907967,17.7260018109924,
0.));
#241025=CARTESIAN_POINT('Ctrl Pts',(-15.3820027907967,17.7260018109924,
12.));
#241026=CARTESIAN_POINT('Ctrl Pts',(-15.3667376981699,17.7160649064206,
0.));
#241027=CARTESIAN_POINT('Ctrl Pts',(-15.3667376981699,17.7160649064206,
12.));
#241028=CARTESIAN_POINT('Ctrl Pts',(-15.351603894206,17.7061525444042,0.));
#241029=CARTESIAN_POINT('Ctrl Pts',(-15.351603894206,17.7061525444042,12.));
#241030=CARTESIAN_POINT('Ctrl Pts',(-15.3366020244066,17.6962657941983,
0.));
#241031=CARTESIAN_POINT('Ctrl Pts',(-15.3366020244066,17.6962657941983,
12.));
#241032=CARTESIAN_POINT('Ctrl Pts',(-15.3217327425338,17.6864057426052,
0.));
#241033=CARTESIAN_POINT('Ctrl Pts',(-15.3217327425338,17.6864057426052,
12.));
#241034=CARTESIAN_POINT('Ctrl Pts',(-15.3069967108501,17.676573494456,0.));
#241035=CARTESIAN_POINT('Ctrl Pts',(-15.3069967108501,17.676573494456,12.));
#241036=CARTESIAN_POINT('Ctrl Pts',(-15.2923946003598,17.6667701731041,
0.));
#241037=CARTESIAN_POINT('Ctrl Pts',(-15.2923946003598,17.6667701731041,
12.));
#241038=CARTESIAN_POINT('Ctrl Pts',(-15.2779270910239,17.6569969209,0.));
#241039=CARTESIAN_POINT('Ctrl Pts',(-15.2779270910239,17.6569969209,12.));
#241040=CARTESIAN_POINT('Ctrl Pts',(-15.2635948720292,17.6472548997328,
0.));
#241041=CARTESIAN_POINT('Ctrl Pts',(-15.2635948720292,17.6472548997328,
12.));
#241042=CARTESIAN_POINT('Ctrl Pts',(-15.2493986421092,17.6375452916369,
0.));
#241043=CARTESIAN_POINT('Ctrl Pts',(-15.2493986421092,17.6375452916369,
12.));
#241044=CARTESIAN_POINT('Ctrl Pts',(-15.2353391098366,17.6278692993764,
0.));
#241045=CARTESIAN_POINT('Ctrl Pts',(-15.2353391098366,17.6278692993764,
12.));
#241046=CARTESIAN_POINT('Ctrl Pts',(-15.2214169939199,17.6182281470468,
0.));
#241047=CARTESIAN_POINT('Ctrl Pts',(-15.2214169939199,17.6182281470468,
12.));
#241048=CARTESIAN_POINT('Ctrl Pts',(-15.2076330234686,17.60862308065,0.));
#241049=CARTESIAN_POINT('Ctrl Pts',(-15.2076330234686,17.60862308065,12.));
#241050=CARTESIAN_POINT('Ctrl Pts',(-15.1939879383268,17.5990553687599,
0.));
#241051=CARTESIAN_POINT('Ctrl Pts',(-15.1939879383268,17.5990553687599,
12.));
#241052=CARTESIAN_POINT('Ctrl Pts',(-15.1804824894605,17.5895263032595,
0.));
#241053=CARTESIAN_POINT('Ctrl Pts',(-15.1804824894605,17.5895263032595,
12.));
#241054=CARTESIAN_POINT('Ctrl Pts',(-15.1671174393137,17.580037200054,0.));
#241055=CARTESIAN_POINT('Ctrl Pts',(-15.1671174393137,17.580037200054,12.));
#241056=CARTESIAN_POINT('Ctrl Pts',(-15.1538935621714,17.5705893998029,
0.));
#241057=CARTESIAN_POINT('Ctrl Pts',(-15.1538935621714,17.5705893998029,
12.));
#241058=CARTESIAN_POINT('Ctrl Pts',(-15.1408116444876,17.5611842686192,
0.));
#241059=CARTESIAN_POINT('Ctrl Pts',(-15.1408116444876,17.5611842686192,
12.));
#241060=CARTESIAN_POINT('Ctrl Pts',(-15.1278724853138,17.5518231989117,
0.));
#241061=CARTESIAN_POINT('Ctrl Pts',(-15.1278724853138,17.5518231989117,
12.));
#241062=CARTESIAN_POINT('Ctrl Pts',(-15.1150768967728,17.5425076102963,
0.));
#241063=CARTESIAN_POINT('Ctrl Pts',(-15.1150768967728,17.5425076102963,
12.));
#241064=CARTESIAN_POINT('Ctrl Pts',(-15.1024257045033,17.5332389504829,
0.));
#241065=CARTESIAN_POINT('Ctrl Pts',(-15.1024257045033,17.5332389504829,
12.));
#241066=CARTESIAN_POINT('Ctrl Pts',(-15.0899197481082,17.524018696179,0.));
#241067=CARTESIAN_POINT('Ctrl Pts',(-15.0899197481082,17.524018696179,12.));
#241068=CARTESIAN_POINT('Ctrl Pts',(-15.0775598815749,17.5148483539687,
0.));
#241069=CARTESIAN_POINT('Ctrl Pts',(-15.0775598815749,17.5148483539687,
12.));
#241070=CARTESIAN_POINT('Ctrl Pts',(-15.0653469738307,17.5057294613877,
0.));
#241071=CARTESIAN_POINT('Ctrl Pts',(-15.0653469738307,17.5057294613877,
12.));
#241072=CARTESIAN_POINT('Ctrl Pts',(-15.0532819093085,17.4966635880246,
0.));
#241073=CARTESIAN_POINT('Ctrl Pts',(-15.0532819093085,17.4966635880246,
12.));
#241074=CARTESIAN_POINT('Ctrl Pts',(-15.0413655884993,17.4876523366178,
0.));
#241075=CARTESIAN_POINT('Ctrl Pts',(-15.0413655884993,17.4876523366178,
12.));
#241076=CARTESIAN_POINT('Ctrl Pts',(-15.029598928488,17.4786973441417,0.));
#241077=CARTESIAN_POINT('Ctrl Pts',(-15.029598928488,17.4786973441417,12.));
#241078=CARTESIAN_POINT('Ctrl Pts',(-15.0179828635087,17.4698002829357,
0.));
#241079=CARTESIAN_POINT('Ctrl Pts',(-15.0179828635087,17.4698002829357,
12.));
#241080=CARTESIAN_POINT('Ctrl Pts',(-15.0065183456922,17.4609628621419,
0.));
#241081=CARTESIAN_POINT('Ctrl Pts',(-15.0065183456922,17.4609628621419,
12.));
#241082=CARTESIAN_POINT('Ctrl Pts',(-14.9952063457779,17.4521868291005,
0.));
#241083=CARTESIAN_POINT('Ctrl Pts',(-14.9952063457779,17.4521868291005,
12.));
#241084=CARTESIAN_POINT('Ctrl Pts',(-14.9840478538357,17.4434739707773,
0.));
#241085=CARTESIAN_POINT('Ctrl Pts',(-14.9840478538357,17.4434739707773,
12.));
#241086=CARTESIAN_POINT('Ctrl Pts',(-14.973043879945,17.4348261151395,0.));
#241087=CARTESIAN_POINT('Ctrl Pts',(-14.973043879945,17.4348261151395,12.));
#241088=CARTESIAN_POINT('Ctrl Pts',(-14.9621954549825,17.4262451327088,
0.));
#241089=CARTESIAN_POINT('Ctrl Pts',(-14.9621954549825,17.4262451327088,
12.));
#241090=CARTESIAN_POINT('Ctrl Pts',(-14.9515036315142,17.4177329382827,
0.));
#241091=CARTESIAN_POINT('Ctrl Pts',(-14.9515036315142,17.4177329382827,
12.));
#241092=CARTESIAN_POINT('Ctrl Pts',(-14.940969484645,17.4092914926071,0.));
#241093=CARTESIAN_POINT('Ctrl Pts',(-14.940969484645,17.4092914926071,12.));
#241094=CARTESIAN_POINT('Ctrl Pts',(-14.9305941128758,17.400922804075,0.));
#241095=CARTESIAN_POINT('Ctrl Pts',(-14.9305941128758,17.400922804075,12.));
#241096=CARTESIAN_POINT('Ctrl Pts',(-14.9203786389343,17.3926289303987,
0.));
#241097=CARTESIAN_POINT('Ctrl Pts',(-14.9203786389343,17.3926289303987,
12.));
#241098=CARTESIAN_POINT('Ctrl Pts',(-14.9103242110057,17.3844119809823,
0.));
#241099=CARTESIAN_POINT('Ctrl Pts',(-14.9103242110057,17.3844119809823,
12.));
#241100=CARTESIAN_POINT('Ctrl Pts',(-14.9004320039609,17.3762741193075,
0.));
#241101=CARTESIAN_POINT('Ctrl Pts',(-14.9004320039609,17.3762741193075,
12.));
#241102=CARTESIAN_POINT('Ctrl Pts',(-14.8907032205789,17.3682175653236,
0.));
#241103=CARTESIAN_POINT('Ctrl Pts',(-14.8907032205789,17.3682175653236,
12.));
#241104=CARTESIAN_POINT('Ctrl Pts',(-14.8811390927424,17.3602445978163,
0.));
#241105=CARTESIAN_POINT('Ctrl Pts',(-14.8811390927424,17.3602445978163,
12.));
#241106=CARTESIAN_POINT('Ctrl Pts',(-14.8717408826958,17.3523575568648,
0.));
#241107=CARTESIAN_POINT('Ctrl Pts',(-14.8717408826958,17.3523575568648,
12.));
#241108=CARTESIAN_POINT('Ctrl Pts',(-14.8625098843419,17.3445588463477,
0.));
#241109=CARTESIAN_POINT('Ctrl Pts',(-14.8625098843419,17.3445588463477,
12.));
#241110=CARTESIAN_POINT('Ctrl Pts',(-14.8534474245433,17.336850936485,0.));
#241111=CARTESIAN_POINT('Ctrl Pts',(-14.8534474245433,17.336850936485,12.));
#241112=CARTESIAN_POINT('Ctrl Pts',(-14.8445548643504,17.3292363662601,
0.));
#241113=CARTESIAN_POINT('Ctrl Pts',(-14.8445548643504,17.3292363662601,
12.));
#241114=CARTESIAN_POINT('Ctrl Pts',(-14.8358336004193,17.3217177462096,
0.));
#241115=CARTESIAN_POINT('Ctrl Pts',(-14.8358336004193,17.3217177462096,
12.));
#241116=CARTESIAN_POINT('Ctrl Pts',(-14.8272850675375,17.3142977632656,
0.));
#241117=CARTESIAN_POINT('Ctrl Pts',(-14.8272850675375,17.3142977632656,
12.));
#241118=CARTESIAN_POINT('Ctrl Pts',(-14.8189107410161,17.3069791853705,
0.));
#241119=CARTESIAN_POINT('Ctrl Pts',(-14.8189107410161,17.3069791853705,
12.));
#241120=CARTESIAN_POINT('Ctrl Pts',(-14.8107121391038,17.2997648661483,
0.));
#241121=CARTESIAN_POINT('Ctrl Pts',(-14.8107121391038,17.2997648661483,
12.));
#241122=CARTESIAN_POINT('Ctrl Pts',(-14.8026908254281,17.2926577496519,
0.));
#241123=CARTESIAN_POINT('Ctrl Pts',(-14.8026908254281,17.2926577496519,
12.));
#241124=CARTESIAN_POINT('Ctrl Pts',(-14.7948484105253,17.28566087332,0.));
#241125=CARTESIAN_POINT('Ctrl Pts',(-14.7948484105253,17.28566087332,12.));
#241126=CARTESIAN_POINT('Ctrl Pts',(-14.787186553128,17.278777370485,0.));
#241127=CARTESIAN_POINT('Ctrl Pts',(-14.787186553128,17.278777370485,12.));
#241128=CARTESIAN_POINT('Ctrl Pts',(-14.7797069617802,17.2720104735192,
0.));
#241129=CARTESIAN_POINT('Ctrl Pts',(-14.7797069617802,17.2720104735192,
12.));
#241130=CARTESIAN_POINT('Ctrl Pts',(-14.7724113956728,17.2653635155317,
0.));
#241131=CARTESIAN_POINT('Ctrl Pts',(-14.7724113956728,17.2653635155317,
12.));
#241132=CARTESIAN_POINT('Ctrl Pts',(-14.7653016697589,17.2588399401464,
0.));
#241133=CARTESIAN_POINT('Ctrl Pts',(-14.7653016697589,17.2588399401464,
12.));
#241134=CARTESIAN_POINT('Ctrl Pts',(-14.7583796616617,17.2524433146837,
0.));
#241135=CARTESIAN_POINT('Ctrl Pts',(-14.7583796616617,17.2524433146837,
12.));
#241136=CARTESIAN_POINT('Ctrl Pts',(-14.7516473175125,17.2461773413289,
0.));
#241137=CARTESIAN_POINT('Ctrl Pts',(-14.7516473175125,17.2461773413289,
12.));
#241138=CARTESIAN_POINT('Ctrl Pts',(-14.7451066593793,17.2400458713566,
0.));
#241139=CARTESIAN_POINT('Ctrl Pts',(-14.7451066593793,17.2400458713566,
12.));
#241140=CARTESIAN_POINT('Ctrl Pts',(-14.7387597858117,17.2340529062077,
0.));
#241141=CARTESIAN_POINT('Ctrl Pts',(-14.7387597858117,17.2340529062077,
12.));
#241142=CARTESIAN_POINT('Ctrl Pts',(-14.7326088681163,17.2282025904314,
0.));
#241143=CARTESIAN_POINT('Ctrl Pts',(-14.7326088681163,17.2282025904314,
12.));
#241144=CARTESIAN_POINT('Ctrl Pts',(-14.7266561494282,17.2224992099666,
0.));
#241145=CARTESIAN_POINT('Ctrl Pts',(-14.7266561494282,17.2224992099666,
12.));
#241146=CARTESIAN_POINT('Ctrl Pts',(-14.7209039390326,17.2169471814255,
0.));
#241147=CARTESIAN_POINT('Ctrl Pts',(-14.7209039390326,17.2169471814255,
12.));
#241148=CARTESIAN_POINT('Ctrl Pts',(-14.7153546289338,17.2115510835988,
0.));
#241149=CARTESIAN_POINT('Ctrl Pts',(-14.7153546289338,17.2115510835988,
12.));
#241150=CARTESIAN_POINT('Ctrl Pts',(-14.7100107213586,17.2063157097316,
0.));
#241151=CARTESIAN_POINT('Ctrl Pts',(-14.7100107213586,17.2063157097316,
12.));
#241152=CARTESIAN_POINT('Ctrl Pts',(-14.7048748502663,17.2012461084268,
0.));
#241153=CARTESIAN_POINT('Ctrl Pts',(-14.7048748502663,17.2012461084268,
12.));
#241154=CARTESIAN_POINT('Ctrl Pts',(-14.699949811582,17.1963476411694,0.));
#241155=CARTESIAN_POINT('Ctrl Pts',(-14.699949811582,17.1963476411694,12.));
#241156=CARTESIAN_POINT('Ctrl Pts',(-14.6952385361706,17.1916259308415,
0.));
#241157=CARTESIAN_POINT('Ctrl Pts',(-14.6952385361706,17.1916259308415,
12.));
#241158=CARTESIAN_POINT('Ctrl Pts',(-14.6907440526958,17.1870867909918,
0.));
#241159=CARTESIAN_POINT('Ctrl Pts',(-14.6907440526958,17.1870867909918,
12.));
#241160=CARTESIAN_POINT('Ctrl Pts',(-14.6864694522319,17.182736158472,0.));
#241161=CARTESIAN_POINT('Ctrl Pts',(-14.6864694522319,17.182736158472,12.));
#241162=CARTESIAN_POINT('Ctrl Pts',(-14.6824178576167,17.1785800350827,
0.));
#241163=CARTESIAN_POINT('Ctrl Pts',(-14.6824178576167,17.1785800350827,
12.));
#241164=CARTESIAN_POINT('Ctrl Pts',(-14.6785925615676,17.1746247499057,
0.));
#241165=CARTESIAN_POINT('Ctrl Pts',(-14.6785925615676,17.1746247499057,
12.));
#241166=CARTESIAN_POINT('Ctrl Pts',(-14.6749971333867,17.1708771619129,
0.));
#241167=CARTESIAN_POINT('Ctrl Pts',(-14.6749971333867,17.1708771619129,
12.));
#241168=CARTESIAN_POINT('Ctrl Pts',(-14.6716355833321,17.1673449723019,
0.));
#241169=CARTESIAN_POINT('Ctrl Pts',(-14.6716355833321,17.1673449723019,
12.));
#241170=CARTESIAN_POINT('Ctrl Pts',(-14.6685123374424,17.1640366762304,
0.));
#241171=CARTESIAN_POINT('Ctrl Pts',(-14.6685123374424,17.1640366762304,
12.));
#241172=CARTESIAN_POINT('Ctrl Pts',(-14.6656319165057,17.1609609517369,
0.));
#241173=CARTESIAN_POINT('Ctrl Pts',(-14.6656319165057,17.1609609517369,
12.));
#241174=CARTESIAN_POINT('Ctrl Pts',(-14.662998728599,17.1581262646789,0.));
#241175=CARTESIAN_POINT('Ctrl Pts',(-14.662998728599,17.1581262646789,12.));
#241176=CARTESIAN_POINT('Ctrl Pts',(-14.660616716964,17.1555401986403,0.));
#241177=CARTESIAN_POINT('Ctrl Pts',(-14.660616716964,17.1555401986403,12.));
#241178=CARTESIAN_POINT('Ctrl Pts',(-14.6584900555301,17.1532107762719,
0.));
#241179=CARTESIAN_POINT('Ctrl Pts',(-14.6584900555301,17.1532107762719,
12.));
#241180=CARTESIAN_POINT('Ctrl Pts',(-14.6566237952435,17.1511476869495,
0.));
#241181=CARTESIAN_POINT('Ctrl Pts',(-14.6566237952435,17.1511476869495,
12.));
#241182=CARTESIAN_POINT('Ctrl Pts',(-14.6550248622813,17.1493641837556,
0.));
#241183=CARTESIAN_POINT('Ctrl Pts',(-14.6550248622813,17.1493641837556,
12.));
#241184=CARTESIAN_POINT('Ctrl Pts',(-14.6537016966188,17.1478763944909,
0.));
#241185=CARTESIAN_POINT('Ctrl Pts',(-14.6537016966188,17.1478763944909,
12.));
#241186=CARTESIAN_POINT('Ctrl Pts',(-14.6526624064978,17.1466998098673,
0.));
#241187=CARTESIAN_POINT('Ctrl Pts',(-14.6526624064978,17.1466998098673,
12.));
#241188=CARTESIAN_POINT('Ctrl Pts',(-14.65191316345,17.1458462295273,0.));
#241189=CARTESIAN_POINT('Ctrl Pts',(-14.65191316345,17.1458462295273,12.));
#241190=CARTESIAN_POINT('Ctrl Pts',(-14.6515481598057,17.1454262858045,
0.));
#241191=CARTESIAN_POINT('Ctrl Pts',(-14.6515481598057,17.1454262858045,
12.));
#241192=CARTESIAN_POINT('Ctrl Pts',(-14.6514066997188,17.1452600887039,
0.));
#241193=CARTESIAN_POINT('Ctrl Pts',(-14.6514066997188,17.1452600887039,
12.));
#241194=CARTESIAN_POINT('Ctrl Pts',(-14.651371185284,17.1452153999142,0.));
#241195=CARTESIAN_POINT('Ctrl Pts',(-14.651371185284,17.1452153999142,12.));
#241196=CARTESIAN_POINT('Ctrl Pts',(-14.6513681262571,17.1452095830633,
0.));
#241197=CARTESIAN_POINT('Ctrl Pts',(-14.6513681262571,17.1452095830633,
12.));
#241198=CARTESIAN_POINT('',(-17.9112098770111,18.8464468996588,0.));
#241199=CARTESIAN_POINT('Ctrl Pts',(-17.9112098770111,18.8464468996588,
0.));
#241200=CARTESIAN_POINT('Ctrl Pts',(-17.9057348246595,18.8448126709691,
0.));
#241201=CARTESIAN_POINT('Ctrl Pts',(-17.8947931177807,18.8415402351786,
0.));
#241202=CARTESIAN_POINT('Ctrl Pts',(-17.8784057509356,18.8366196462581,
0.));
#241203=CARTESIAN_POINT('Ctrl Pts',(-17.8566063174771,18.8300349895974,
0.));
#241204=CARTESIAN_POINT('Ctrl Pts',(-17.8294410311006,18.8217643886157,
0.));
#241205=CARTESIAN_POINT('Ctrl Pts',(-17.8023598011057,18.8134540340417,
0.));
#241206=CARTESIAN_POINT('Ctrl Pts',(-17.7753627137853,18.8051039860448,
0.));
#241207=CARTESIAN_POINT('Ctrl Pts',(-17.7484498996905,18.7967143519419,
0.));
#241208=CARTESIAN_POINT('Ctrl Pts',(-17.7216215409035,18.7882852976049,
0.));
#241209=CARTESIAN_POINT('Ctrl Pts',(-17.6948778823014,18.7798170641374,
0.));
#241210=CARTESIAN_POINT('Ctrl Pts',(-17.6682192274236,18.7713099642754,
0.));
#241211=CARTESIAN_POINT('Ctrl Pts',(-17.6416459210681,18.762764361321,0.));
#241212=CARTESIAN_POINT('Ctrl Pts',(-17.6151583357012,18.7541806530984,
0.));
#241213=CARTESIAN_POINT('Ctrl Pts',(-17.5887568561371,18.7455592536687,
0.));
#241214=CARTESIAN_POINT('Ctrl Pts',(-17.5624418653245,18.7369005764553,
0.));
#241215=CARTESIAN_POINT('Ctrl Pts',(-17.5362137287593,18.7282050157138,
0.));
#241216=CARTESIAN_POINT('Ctrl Pts',(-17.5100727820876,18.7194729318098,
0.));
#241217=CARTESIAN_POINT('Ctrl Pts',(-17.4840193397162,18.7107046613912,
0.));
#241218=CARTESIAN_POINT('Ctrl Pts',(-17.4580537012753,18.70190052503,0.));
#241219=CARTESIAN_POINT('Ctrl Pts',(-17.4321761588142,18.6930608357409,
0.));
#241220=CARTESIAN_POINT('Ctrl Pts',(-17.4063870038562,18.6841859073471,
0.));
#241221=CARTESIAN_POINT('Ctrl Pts',(-17.3806865340747,18.6752760624052,
0.));
#241222=CARTESIAN_POINT('Ctrl Pts',(-17.3550750612443,18.6663316416582,
0.));
#241223=CARTESIAN_POINT('Ctrl Pts',(-17.3295529098618,18.6573530024033,
0.));
#241224=CARTESIAN_POINT('Ctrl Pts',(-17.3041204135074,18.6483405141865,
0.));
#241225=CARTESIAN_POINT('Ctrl Pts',(-17.2787779120213,18.6392945554748,
0.));
#241226=CARTESIAN_POINT('Ctrl Pts',(-17.2535257482187,18.6302155097943,
0.));
#241227=CARTESIAN_POINT('Ctrl Pts',(-17.2283642650518,18.6211037624038,
0.));
#241228=CARTESIAN_POINT('Ctrl Pts',(-17.2032938019284,18.6119596959949,
0.));
#241229=CARTESIAN_POINT('Ctrl Pts',(-17.1783146940127,18.6027836898817,
0.));
#241230=CARTESIAN_POINT('Ctrl Pts',(-17.1534272741643,18.5935761222825,
0.));
#241231=CARTESIAN_POINT('Ctrl Pts',(-17.1286318741183,18.5843373717247,
0.));
#241232=CARTESIAN_POINT('Ctrl Pts',(-17.1039288260001,18.5750678188542,
0.));
#241233=CARTESIAN_POINT('Ctrl Pts',(-17.0793184636079,18.5657678479789,
0.));
#241234=CARTESIAN_POINT('Ctrl Pts',(-17.0548011239751,18.556437848963,0.));
#241235=CARTESIAN_POINT('Ctrl Pts',(-17.0303771481738,18.547078218209,0.));
#241236=CARTESIAN_POINT('Ctrl Pts',(-17.0060468805097,18.5376893576961,
0.));
#241237=CARTESIAN_POINT('Ctrl Pts',(-16.981810668038,18.5282716744197,0.));
#241238=CARTESIAN_POINT('Ctrl Pts',(-16.9576688599339,18.5188255796659,
0.));
#241239=CARTESIAN_POINT('Ctrl Pts',(-16.9336218069353,18.5093514883835,
0.));
#241240=CARTESIAN_POINT('Ctrl Pts',(-16.9096698606943,18.499849818462,0.));
#241241=CARTESIAN_POINT('Ctrl Pts',(-16.8858133733088,18.4903209902227,
0.));
#241242=CARTESIAN_POINT('Ctrl Pts',(-16.8620526977171,18.480765426877,0.));
#241243=CARTESIAN_POINT('Ctrl Pts',(-16.8383881879709,18.4711835548623,
0.));
#241244=CARTESIAN_POINT('Ctrl Pts',(-16.8148201995472,18.4615758042305,
0.));
#241245=CARTESIAN_POINT('Ctrl Pts',(-16.791349089629,18.4519426090123,0.));
#241246=CARTESIAN_POINT('Ctrl Pts',(-16.7679752173992,18.44228440761,0.));
#241247=CARTESIAN_POINT('Ctrl Pts',(-16.7446989442882,18.4326016431392,
0.));
#241248=CARTESIAN_POINT('Ctrl Pts',(-16.7215206338818,18.4228947633187,
0.));
#241249=CARTESIAN_POINT('Ctrl Pts',(-16.6984406518491,18.413164220399,0.));
#241250=CARTESIAN_POINT('Ctrl Pts',(-16.6754593658513,18.403410471079,0.));
#241251=CARTESIAN_POINT('Ctrl Pts',(-16.6525771454513,18.3936339764332,
0.));
#241252=CARTESIAN_POINT('Ctrl Pts',(-16.6297943620056,18.3838352018327,
0.));
#241253=CARTESIAN_POINT('Ctrl Pts',(-16.607111388571,18.3740146168879,0.));
#241254=CARTESIAN_POINT('Ctrl Pts',(-16.5845286000217,18.3641726955889,
0.));
#241255=CARTESIAN_POINT('Ctrl Pts',(-16.5620463731413,18.354309916433,0.));
#241256=CARTESIAN_POINT('Ctrl Pts',(-16.5396650867139,18.34442676256,0.));
#241257=CARTESIAN_POINT('Ctrl Pts',(-16.5173851216045,18.3345237218864,
0.));
#241258=CARTESIAN_POINT('Ctrl Pts',(-16.4952068608345,18.3246012872469,
0.));
#241259=CARTESIAN_POINT('Ctrl Pts',(-16.4731306896441,18.3146599565231,
0.));
#241260=CARTESIAN_POINT('Ctrl Pts',(-16.4511569955233,18.304700232686,0.));
#241261=CARTESIAN_POINT('Ctrl Pts',(-16.4292861682379,18.294722623851,0.));
#241262=CARTESIAN_POINT('Ctrl Pts',(-16.4075185998455,18.2847276433309,
0.));
#241263=CARTESIAN_POINT('Ctrl Pts',(-16.385854684708,18.2747158096934,0.));
#241264=CARTESIAN_POINT('Ctrl Pts',(-16.3642948194868,18.2646876468169,
0.));
#241265=CARTESIAN_POINT('Ctrl Pts',(-16.3428394031589,18.2546436839608,
0.));
#241266=CARTESIAN_POINT('Ctrl Pts',(-16.3214888370987,18.2445844558741,
0.));
#241267=CARTESIAN_POINT('Ctrl Pts',(-16.3002435251378,18.2345105028982,
0.));
#241268=CARTESIAN_POINT('Ctrl Pts',(-16.2791038736223,18.2244223710745,
0.));
#241269=CARTESIAN_POINT('Ctrl Pts',(-16.2580702914615,18.2143206122529,
0.));
#241270=CARTESIAN_POINT('Ctrl Pts',(-16.2371431901638,18.2042057842035,
0.));
#241271=CARTESIAN_POINT('Ctrl Pts',(-16.2163229838875,18.1940784507229,
0.));
#241272=CARTESIAN_POINT('Ctrl Pts',(-16.1956100895073,18.1839391817331,
0.));
#241273=CARTESIAN_POINT('Ctrl Pts',(-16.1750049266671,18.1737885533849,
0.));
#241274=CARTESIAN_POINT('Ctrl Pts',(-16.154507917826,18.1636271481615,0.));
#241275=CARTESIAN_POINT('Ctrl Pts',(-16.1341194882988,18.1534555549852,
0.));
#241276=CARTESIAN_POINT('Ctrl Pts',(-16.1138400662794,18.1432743693235,
0.));
#241277=CARTESIAN_POINT('Ctrl Pts',(-16.0936700829112,18.1330841933105,
0.));
#241278=CARTESIAN_POINT('Ctrl Pts',(-16.0736099723668,18.1228856358751,
0.));
#241279=CARTESIAN_POINT('Ctrl Pts',(-16.0536601719126,18.112679312869,0.));
#241280=CARTESIAN_POINT('Ctrl Pts',(-16.0338211219693,18.1024658471966,
0.));
#241281=CARTESIAN_POINT('Ctrl Pts',(-16.014093266161,18.0922458689462,0.));
#241282=CARTESIAN_POINT('Ctrl Pts',(-15.9944770513613,18.0820200155236,
0.));
#241283=CARTESIAN_POINT('Ctrl Pts',(-15.9749729277846,18.0717889317958,
0.));
#241284=CARTESIAN_POINT('Ctrl Pts',(-15.9555813490644,18.0615532702359,
0.));
#241285=CARTESIAN_POINT('Ctrl Pts',(-15.9363027723244,18.0513136910691,
0.));
#241286=CARTESIAN_POINT('Ctrl Pts',(-15.9171376582436,18.0410708624208,
0.));
#241287=CARTESIAN_POINT('Ctrl Pts',(-15.8980864711042,18.0308254604636,
0.));
#241288=CARTESIAN_POINT('Ctrl Pts',(-15.8791496788683,18.0205781695769,
0.));
#241289=CARTESIAN_POINT('Ctrl Pts',(-15.8603277532831,18.0103296825205,
0.));
#241290=CARTESIAN_POINT('Ctrl Pts',(-15.8416211699679,18.0000807006052,
0.));
#241291=CARTESIAN_POINT('Ctrl Pts',(-15.8230304084962,17.9898319338664,
0.));
#241292=CARTESIAN_POINT('Ctrl Pts',(-15.8045559524676,17.9795841012386,
0.));
#241293=CARTESIAN_POINT('Ctrl Pts',(-15.7861982895724,17.9693379307303,
0.));
#241294=CARTESIAN_POINT('Ctrl Pts',(-15.7679579117077,17.9590941596242,
0.));
#241295=CARTESIAN_POINT('Ctrl Pts',(-15.749835315086,17.9488535346781,0.));
#241296=CARTESIAN_POINT('Ctrl Pts',(-15.7318310003335,17.9386168123262,
0.));
#241297=CARTESIAN_POINT('Ctrl Pts',(-15.7139454725838,17.9283847588835,
0.));
#241298=CARTESIAN_POINT('Ctrl Pts',(-15.6961792415522,17.9181581507455,
0.));
#241299=CARTESIAN_POINT('Ctrl Pts',(-15.678532821646,17.9079377746111,0.));
#241300=CARTESIAN_POINT('Ctrl Pts',(-15.661006732103,17.897724427724,0.));
#241301=CARTESIAN_POINT('Ctrl Pts',(-15.6436014971084,17.8875189181091,
0.));
#241302=CARTESIAN_POINT('Ctrl Pts',(-15.6263176459108,17.8773220648125,
0.));
#241303=CARTESIAN_POINT('Ctrl Pts',(-15.609155712921,17.8671346981394,0.));
#241304=CARTESIAN_POINT('Ctrl Pts',(-15.5921162378192,17.8569576599006,
0.));
#241305=CARTESIAN_POINT('Ctrl Pts',(-15.5751997657163,17.8467918036987,
0.));
#241306=CARTESIAN_POINT('Ctrl Pts',(-15.5584068472982,17.8366379952085,
0.));
#241307=CARTESIAN_POINT('Ctrl Pts',(-15.541738038964,17.8264971124606,0.));
#241308=CARTESIAN_POINT('Ctrl Pts',(-15.5251939029552,17.8163700461256,
0.));
#241309=CARTESIAN_POINT('Ctrl Pts',(-15.5087750074718,17.8062576997952,
0.));
#241310=CARTESIAN_POINT('Ctrl Pts',(-15.4924819268517,17.7961609903148,
0.));
#241311=CARTESIAN_POINT('Ctrl Pts',(-15.4763152417497,17.7860808481219,
0.));
#241312=CARTESIAN_POINT('Ctrl Pts',(-15.4602755393017,17.7760182175815,
0.));
#241313=CARTESIAN_POINT('Ctrl Pts',(-15.4443634132869,17.7659740573265,
0.));
#241314=CARTESIAN_POINT('Ctrl Pts',(-15.4285794642668,17.7559493405881,
0.));
#241315=CARTESIAN_POINT('Ctrl Pts',(-15.4129242997837,17.7459450555812,
0.));
#241316=CARTESIAN_POINT('Ctrl Pts',(-15.3973985345802,17.7359622059149,
0.));
#241317=CARTESIAN_POINT('Ctrl Pts',(-15.3820027907967,17.7260018109924,
0.));
#241318=CARTESIAN_POINT('Ctrl Pts',(-15.3667376981699,17.7160649064206,
0.));
#241319=CARTESIAN_POINT('Ctrl Pts',(-15.351603894206,17.7061525444042,0.));
#241320=CARTESIAN_POINT('Ctrl Pts',(-15.3366020244066,17.6962657941983,
0.));
#241321=CARTESIAN_POINT('Ctrl Pts',(-15.3217327425338,17.6864057426052,
0.));
#241322=CARTESIAN_POINT('Ctrl Pts',(-15.3069967108501,17.676573494456,0.));
#241323=CARTESIAN_POINT('Ctrl Pts',(-15.2923946003598,17.6667701731041,
0.));
#241324=CARTESIAN_POINT('Ctrl Pts',(-15.2779270910239,17.6569969209,0.));
#241325=CARTESIAN_POINT('Ctrl Pts',(-15.2635948720292,17.6472548997328,
0.));
#241326=CARTESIAN_POINT('Ctrl Pts',(-15.2493986421092,17.6375452916369,
0.));
#241327=CARTESIAN_POINT('Ctrl Pts',(-15.2353391098366,17.6278692993764,
0.));
#241328=CARTESIAN_POINT('Ctrl Pts',(-15.2214169939199,17.6182281470468,
0.));
#241329=CARTESIAN_POINT('Ctrl Pts',(-15.2076330234686,17.60862308065,0.));
#241330=CARTESIAN_POINT('Ctrl Pts',(-15.1939879383268,17.5990553687599,
0.));
#241331=CARTESIAN_POINT('Ctrl Pts',(-15.1804824894605,17.5895263032595,
0.));
#241332=CARTESIAN_POINT('Ctrl Pts',(-15.1671174393137,17.580037200054,0.));
#241333=CARTESIAN_POINT('Ctrl Pts',(-15.1538935621714,17.5705893998029,
0.));
#241334=CARTESIAN_POINT('Ctrl Pts',(-15.1408116444876,17.5611842686192,
0.));
#241335=CARTESIAN_POINT('Ctrl Pts',(-15.1278724853138,17.5518231989117,
0.));
#241336=CARTESIAN_POINT('Ctrl Pts',(-15.1150768967728,17.5425076102963,
0.));
#241337=CARTESIAN_POINT('Ctrl Pts',(-15.1024257045033,17.5332389504829,
0.));
#241338=CARTESIAN_POINT('Ctrl Pts',(-15.0899197481082,17.524018696179,0.));
#241339=CARTESIAN_POINT('Ctrl Pts',(-15.0775598815749,17.5148483539687,
0.));
#241340=CARTESIAN_POINT('Ctrl Pts',(-15.0653469738307,17.5057294613877,
0.));
#241341=CARTESIAN_POINT('Ctrl Pts',(-15.0532819093085,17.4966635880246,
0.));
#241342=CARTESIAN_POINT('Ctrl Pts',(-15.0413655884993,17.4876523366178,
0.));
#241343=CARTESIAN_POINT('Ctrl Pts',(-15.029598928488,17.4786973441417,0.));
#241344=CARTESIAN_POINT('Ctrl Pts',(-15.0179828635087,17.4698002829357,
0.));
#241345=CARTESIAN_POINT('Ctrl Pts',(-15.0065183456922,17.4609628621419,
0.));
#241346=CARTESIAN_POINT('Ctrl Pts',(-14.9952063457779,17.4521868291005,
0.));
#241347=CARTESIAN_POINT('Ctrl Pts',(-14.9840478538357,17.4434739707773,
0.));
#241348=CARTESIAN_POINT('Ctrl Pts',(-14.973043879945,17.4348261151395,0.));
#241349=CARTESIAN_POINT('Ctrl Pts',(-14.9621954549825,17.4262451327088,
0.));
#241350=CARTESIAN_POINT('Ctrl Pts',(-14.9515036315142,17.4177329382827,
0.));
#241351=CARTESIAN_POINT('Ctrl Pts',(-14.940969484645,17.4092914926071,0.));
#241352=CARTESIAN_POINT('Ctrl Pts',(-14.9305941128758,17.400922804075,0.));
#241353=CARTESIAN_POINT('Ctrl Pts',(-14.9203786389343,17.3926289303987,
0.));
#241354=CARTESIAN_POINT('Ctrl Pts',(-14.9103242110057,17.3844119809823,
0.));
#241355=CARTESIAN_POINT('Ctrl Pts',(-14.9004320039609,17.3762741193075,
0.));
#241356=CARTESIAN_POINT('Ctrl Pts',(-14.8907032205789,17.3682175653236,
0.));
#241357=CARTESIAN_POINT('Ctrl Pts',(-14.8811390927424,17.3602445978163,
0.));
#241358=CARTESIAN_POINT('Ctrl Pts',(-14.8717408826958,17.3523575568648,
0.));
#241359=CARTESIAN_POINT('Ctrl Pts',(-14.8625098843419,17.3445588463477,
0.));
#241360=CARTESIAN_POINT('Ctrl Pts',(-14.8534474245433,17.336850936485,0.));
#241361=CARTESIAN_POINT('Ctrl Pts',(-14.8445548643504,17.3292363662601,
0.));
#241362=CARTESIAN_POINT('Ctrl Pts',(-14.8358336004193,17.3217177462096,
0.));
#241363=CARTESIAN_POINT('Ctrl Pts',(-14.8272850675375,17.3142977632656,
0.));
#241364=CARTESIAN_POINT('Ctrl Pts',(-14.8189107410161,17.3069791853705,
0.));
#241365=CARTESIAN_POINT('Ctrl Pts',(-14.8107121391038,17.2997648661483,
0.));
#241366=CARTESIAN_POINT('Ctrl Pts',(-14.8026908254281,17.2926577496519,
0.));
#241367=CARTESIAN_POINT('Ctrl Pts',(-14.7948484105253,17.28566087332,0.));
#241368=CARTESIAN_POINT('Ctrl Pts',(-14.787186553128,17.278777370485,0.));
#241369=CARTESIAN_POINT('Ctrl Pts',(-14.7797069617802,17.2720104735192,
0.));
#241370=CARTESIAN_POINT('Ctrl Pts',(-14.7724113956728,17.2653635155317,
0.));
#241371=CARTESIAN_POINT('Ctrl Pts',(-14.7653016697589,17.2588399401464,
0.));
#241372=CARTESIAN_POINT('Ctrl Pts',(-14.7583796616617,17.2524433146837,
0.));
#241373=CARTESIAN_POINT('Ctrl Pts',(-14.7516473175125,17.2461773413289,
0.));
#241374=CARTESIAN_POINT('Ctrl Pts',(-14.7451066593793,17.2400458713566,
0.));
#241375=CARTESIAN_POINT('Ctrl Pts',(-14.7387597858117,17.2340529062077,
0.));
#241376=CARTESIAN_POINT('Ctrl Pts',(-14.7326088681163,17.2282025904314,
0.));
#241377=CARTESIAN_POINT('Ctrl Pts',(-14.7266561494282,17.2224992099666,
0.));
#241378=CARTESIAN_POINT('Ctrl Pts',(-14.7209039390326,17.2169471814255,
0.));
#241379=CARTESIAN_POINT('Ctrl Pts',(-14.7153546289338,17.2115510835988,
0.));
#241380=CARTESIAN_POINT('Ctrl Pts',(-14.7100107213586,17.2063157097316,
0.));
#241381=CARTESIAN_POINT('Ctrl Pts',(-14.7048748502663,17.2012461084268,
0.));
#241382=CARTESIAN_POINT('Ctrl Pts',(-14.699949811582,17.1963476411694,0.));
#241383=CARTESIAN_POINT('Ctrl Pts',(-14.6952385361706,17.1916259308415,
0.));
#241384=CARTESIAN_POINT('Ctrl Pts',(-14.6907440526958,17.1870867909918,
0.));
#241385=CARTESIAN_POINT('Ctrl Pts',(-14.6864694522319,17.182736158472,0.));
#241386=CARTESIAN_POINT('Ctrl Pts',(-14.6824178576167,17.1785800350827,
0.));
#241387=CARTESIAN_POINT('Ctrl Pts',(-14.6785925615676,17.1746247499057,
0.));
#241388=CARTESIAN_POINT('Ctrl Pts',(-14.6749971333867,17.1708771619129,
0.));
#241389=CARTESIAN_POINT('Ctrl Pts',(-14.6716355833321,17.1673449723019,
0.));
#241390=CARTESIAN_POINT('Ctrl Pts',(-14.6685123374424,17.1640366762304,
0.));
#241391=CARTESIAN_POINT('Ctrl Pts',(-14.6656319165057,17.1609609517369,
0.));
#241392=CARTESIAN_POINT('Ctrl Pts',(-14.662998728599,17.1581262646789,0.));
#241393=CARTESIAN_POINT('Ctrl Pts',(-14.660616716964,17.1555401986403,0.));
#241394=CARTESIAN_POINT('Ctrl Pts',(-14.6584900555301,17.1532107762719,
0.));
#241395=CARTESIAN_POINT('Ctrl Pts',(-14.6566237952435,17.1511476869495,
0.));
#241396=CARTESIAN_POINT('Ctrl Pts',(-14.6550248622813,17.1493641837556,
0.));
#241397=CARTESIAN_POINT('Ctrl Pts',(-14.6537016966188,17.1478763944909,
0.));
#241398=CARTESIAN_POINT('Ctrl Pts',(-14.6526624064978,17.1466998098673,
0.));
#241399=CARTESIAN_POINT('Ctrl Pts',(-14.65191316345,17.1458462295273,0.));
#241400=CARTESIAN_POINT('Ctrl Pts',(-14.6515481598057,17.1454262858045,
0.));
#241401=CARTESIAN_POINT('Ctrl Pts',(-14.6514066997188,17.1452600887039,
0.));
#241402=CARTESIAN_POINT('Ctrl Pts',(-14.651371185284,17.1452153999142,0.));
#241403=CARTESIAN_POINT('Ctrl Pts',(-14.6513681262571,17.1452095830633,
0.));
#241404=CARTESIAN_POINT('',(-17.9112098770111,18.8464468996588,12.));
#241405=CARTESIAN_POINT('',(-17.9112098770111,18.8464468996588,0.));
#241406=CARTESIAN_POINT('Ctrl Pts',(-14.6513681262571,17.1452095830633,
12.));
#241407=CARTESIAN_POINT('Ctrl Pts',(-14.651371185284,17.1452153999142,12.));
#241408=CARTESIAN_POINT('Ctrl Pts',(-14.6514066997188,17.1452600887039,
12.));
#241409=CARTESIAN_POINT('Ctrl Pts',(-14.6515481598057,17.1454262858045,
12.));
#241410=CARTESIAN_POINT('Ctrl Pts',(-14.65191316345,17.1458462295273,12.));
#241411=CARTESIAN_POINT('Ctrl Pts',(-14.6526624064978,17.1466998098673,
12.));
#241412=CARTESIAN_POINT('Ctrl Pts',(-14.6537016966188,17.1478763944909,
12.));
#241413=CARTESIAN_POINT('Ctrl Pts',(-14.6550248622813,17.1493641837556,
12.));
#241414=CARTESIAN_POINT('Ctrl Pts',(-14.6566237952435,17.1511476869495,
12.));
#241415=CARTESIAN_POINT('Ctrl Pts',(-14.6584900555301,17.1532107762719,
12.));
#241416=CARTESIAN_POINT('Ctrl Pts',(-14.660616716964,17.1555401986403,12.));
#241417=CARTESIAN_POINT('Ctrl Pts',(-14.662998728599,17.1581262646789,12.));
#241418=CARTESIAN_POINT('Ctrl Pts',(-14.6656319165057,17.1609609517369,
12.));
#241419=CARTESIAN_POINT('Ctrl Pts',(-14.6685123374424,17.1640366762304,
12.));
#241420=CARTESIAN_POINT('Ctrl Pts',(-14.6716355833321,17.1673449723019,
12.));
#241421=CARTESIAN_POINT('Ctrl Pts',(-14.6749971333867,17.1708771619129,
12.));
#241422=CARTESIAN_POINT('Ctrl Pts',(-14.6785925615676,17.1746247499057,
12.));
#241423=CARTESIAN_POINT('Ctrl Pts',(-14.6824178576167,17.1785800350827,
12.));
#241424=CARTESIAN_POINT('Ctrl Pts',(-14.6864694522319,17.182736158472,12.));
#241425=CARTESIAN_POINT('Ctrl Pts',(-14.6907440526958,17.1870867909918,
12.));
#241426=CARTESIAN_POINT('Ctrl Pts',(-14.6952385361706,17.1916259308415,
12.));
#241427=CARTESIAN_POINT('Ctrl Pts',(-14.699949811582,17.1963476411694,12.));
#241428=CARTESIAN_POINT('Ctrl Pts',(-14.7048748502663,17.2012461084268,
12.));
#241429=CARTESIAN_POINT('Ctrl Pts',(-14.7100107213586,17.2063157097316,
12.));
#241430=CARTESIAN_POINT('Ctrl Pts',(-14.7153546289338,17.2115510835988,
12.));
#241431=CARTESIAN_POINT('Ctrl Pts',(-14.7209039390326,17.2169471814255,
12.));
#241432=CARTESIAN_POINT('Ctrl Pts',(-14.7266561494282,17.2224992099666,
12.));
#241433=CARTESIAN_POINT('Ctrl Pts',(-14.7326088681163,17.2282025904314,
12.));
#241434=CARTESIAN_POINT('Ctrl Pts',(-14.7387597858117,17.2340529062077,
12.));
#241435=CARTESIAN_POINT('Ctrl Pts',(-14.7451066593793,17.2400458713566,
12.));
#241436=CARTESIAN_POINT('Ctrl Pts',(-14.7516473175125,17.2461773413289,
12.));
#241437=CARTESIAN_POINT('Ctrl Pts',(-14.7583796616617,17.2524433146837,
12.));
#241438=CARTESIAN_POINT('Ctrl Pts',(-14.7653016697589,17.2588399401464,
12.));
#241439=CARTESIAN_POINT('Ctrl Pts',(-14.7724113956728,17.2653635155317,
12.));
#241440=CARTESIAN_POINT('Ctrl Pts',(-14.7797069617802,17.2720104735192,
12.));
#241441=CARTESIAN_POINT('Ctrl Pts',(-14.787186553128,17.278777370485,12.));
#241442=CARTESIAN_POINT('Ctrl Pts',(-14.7948484105253,17.28566087332,12.));
#241443=CARTESIAN_POINT('Ctrl Pts',(-14.8026908254281,17.2926577496519,
12.));
#241444=CARTESIAN_POINT('Ctrl Pts',(-14.8107121391038,17.2997648661483,
12.));
#241445=CARTESIAN_POINT('Ctrl Pts',(-14.8189107410161,17.3069791853705,
12.));
#241446=CARTESIAN_POINT('Ctrl Pts',(-14.8272850675375,17.3142977632656,
12.));
#241447=CARTESIAN_POINT('Ctrl Pts',(-14.8358336004193,17.3217177462096,
12.));
#241448=CARTESIAN_POINT('Ctrl Pts',(-14.8445548643504,17.3292363662601,
12.));
#241449=CARTESIAN_POINT('Ctrl Pts',(-14.8534474245433,17.336850936485,12.));
#241450=CARTESIAN_POINT('Ctrl Pts',(-14.8625098843419,17.3445588463477,
12.));
#241451=CARTESIAN_POINT('Ctrl Pts',(-14.8717408826958,17.3523575568648,
12.));
#241452=CARTESIAN_POINT('Ctrl Pts',(-14.8811390927424,17.3602445978163,
12.));
#241453=CARTESIAN_POINT('Ctrl Pts',(-14.8907032205789,17.3682175653236,
12.));
#241454=CARTESIAN_POINT('Ctrl Pts',(-14.9004320039609,17.3762741193075,
12.));
#241455=CARTESIAN_POINT('Ctrl Pts',(-14.9103242110057,17.3844119809823,
12.));
#241456=CARTESIAN_POINT('Ctrl Pts',(-14.9203786389343,17.3926289303987,
12.));
#241457=CARTESIAN_POINT('Ctrl Pts',(-14.9305941128758,17.400922804075,12.));
#241458=CARTESIAN_POINT('Ctrl Pts',(-14.940969484645,17.4092914926071,12.));
#241459=CARTESIAN_POINT('Ctrl Pts',(-14.9515036315142,17.4177329382827,
12.));
#241460=CARTESIAN_POINT('Ctrl Pts',(-14.9621954549825,17.4262451327088,
12.));
#241461=CARTESIAN_POINT('Ctrl Pts',(-14.973043879945,17.4348261151395,12.));
#241462=CARTESIAN_POINT('Ctrl Pts',(-14.9840478538357,17.4434739707773,
12.));
#241463=CARTESIAN_POINT('Ctrl Pts',(-14.9952063457779,17.4521868291005,
12.));
#241464=CARTESIAN_POINT('Ctrl Pts',(-15.0065183456922,17.4609628621419,
12.));
#241465=CARTESIAN_POINT('Ctrl Pts',(-15.0179828635087,17.4698002829357,
12.));
#241466=CARTESIAN_POINT('Ctrl Pts',(-15.029598928488,17.4786973441417,12.));
#241467=CARTESIAN_POINT('Ctrl Pts',(-15.0413655884993,17.4876523366178,
12.));
#241468=CARTESIAN_POINT('Ctrl Pts',(-15.0532819093085,17.4966635880246,
12.));
#241469=CARTESIAN_POINT('Ctrl Pts',(-15.0653469738307,17.5057294613877,
12.));
#241470=CARTESIAN_POINT('Ctrl Pts',(-15.0775598815749,17.5148483539687,
12.));
#241471=CARTESIAN_POINT('Ctrl Pts',(-15.0899197481082,17.524018696179,12.));
#241472=CARTESIAN_POINT('Ctrl Pts',(-15.1024257045033,17.5332389504829,
12.));
#241473=CARTESIAN_POINT('Ctrl Pts',(-15.1150768967728,17.5425076102963,
12.));
#241474=CARTESIAN_POINT('Ctrl Pts',(-15.1278724853138,17.5518231989117,
12.));
#241475=CARTESIAN_POINT('Ctrl Pts',(-15.1408116444876,17.5611842686192,
12.));
#241476=CARTESIAN_POINT('Ctrl Pts',(-15.1538935621714,17.5705893998029,
12.));
#241477=CARTESIAN_POINT('Ctrl Pts',(-15.1671174393137,17.580037200054,12.));
#241478=CARTESIAN_POINT('Ctrl Pts',(-15.1804824894605,17.5895263032595,
12.));
#241479=CARTESIAN_POINT('Ctrl Pts',(-15.1939879383268,17.5990553687599,
12.));
#241480=CARTESIAN_POINT('Ctrl Pts',(-15.2076330234686,17.60862308065,12.));
#241481=CARTESIAN_POINT('Ctrl Pts',(-15.2214169939199,17.6182281470468,
12.));
#241482=CARTESIAN_POINT('Ctrl Pts',(-15.2353391098366,17.6278692993764,
12.));
#241483=CARTESIAN_POINT('Ctrl Pts',(-15.2493986421092,17.6375452916369,
12.));
#241484=CARTESIAN_POINT('Ctrl Pts',(-15.2635948720292,17.6472548997328,
12.));
#241485=CARTESIAN_POINT('Ctrl Pts',(-15.2779270910239,17.6569969209,12.));
#241486=CARTESIAN_POINT('Ctrl Pts',(-15.2923946003598,17.6667701731041,
12.));
#241487=CARTESIAN_POINT('Ctrl Pts',(-15.3069967108501,17.676573494456,12.));
#241488=CARTESIAN_POINT('Ctrl Pts',(-15.3217327425338,17.6864057426052,
12.));
#241489=CARTESIAN_POINT('Ctrl Pts',(-15.3366020244066,17.6962657941983,
12.));
#241490=CARTESIAN_POINT('Ctrl Pts',(-15.351603894206,17.7061525444042,12.));
#241491=CARTESIAN_POINT('Ctrl Pts',(-15.3667376981699,17.7160649064206,
12.));
#241492=CARTESIAN_POINT('Ctrl Pts',(-15.3820027907967,17.7260018109924,
12.));
#241493=CARTESIAN_POINT('Ctrl Pts',(-15.3973985345802,17.7359622059149,
12.));
#241494=CARTESIAN_POINT('Ctrl Pts',(-15.4129242997837,17.7459450555812,
12.));
#241495=CARTESIAN_POINT('Ctrl Pts',(-15.4285794642668,17.7559493405881,
12.));
#241496=CARTESIAN_POINT('Ctrl Pts',(-15.4443634132869,17.7659740573265,
12.));
#241497=CARTESIAN_POINT('Ctrl Pts',(-15.4602755393017,17.7760182175815,
12.));
#241498=CARTESIAN_POINT('Ctrl Pts',(-15.4763152417497,17.7860808481219,
12.));
#241499=CARTESIAN_POINT('Ctrl Pts',(-15.4924819268517,17.7961609903148,
12.));
#241500=CARTESIAN_POINT('Ctrl Pts',(-15.5087750074718,17.8062576997952,
12.));
#241501=CARTESIAN_POINT('Ctrl Pts',(-15.5251939029552,17.8163700461256,
12.));
#241502=CARTESIAN_POINT('Ctrl Pts',(-15.541738038964,17.8264971124606,12.));
#241503=CARTESIAN_POINT('Ctrl Pts',(-15.5584068472982,17.8366379952085,
12.));
#241504=CARTESIAN_POINT('Ctrl Pts',(-15.5751997657163,17.8467918036987,
12.));
#241505=CARTESIAN_POINT('Ctrl Pts',(-15.5921162378192,17.8569576599006,
12.));
#241506=CARTESIAN_POINT('Ctrl Pts',(-15.609155712921,17.8671346981394,12.));
#241507=CARTESIAN_POINT('Ctrl Pts',(-15.6263176459108,17.8773220648125,
12.));
#241508=CARTESIAN_POINT('Ctrl Pts',(-15.6436014971084,17.8875189181091,
12.));
#241509=CARTESIAN_POINT('Ctrl Pts',(-15.661006732103,17.897724427724,12.));
#241510=CARTESIAN_POINT('Ctrl Pts',(-15.678532821646,17.9079377746111,12.));
#241511=CARTESIAN_POINT('Ctrl Pts',(-15.6961792415522,17.9181581507455,
12.));
#241512=CARTESIAN_POINT('Ctrl Pts',(-15.7139454725838,17.9283847588835,
12.));
#241513=CARTESIAN_POINT('Ctrl Pts',(-15.7318310003335,17.9386168123262,
12.));
#241514=CARTESIAN_POINT('Ctrl Pts',(-15.749835315086,17.9488535346781,12.));
#241515=CARTESIAN_POINT('Ctrl Pts',(-15.7679579117077,17.9590941596242,
12.));
#241516=CARTESIAN_POINT('Ctrl Pts',(-15.7861982895724,17.9693379307303,
12.));
#241517=CARTESIAN_POINT('Ctrl Pts',(-15.8045559524676,17.9795841012386,
12.));
#241518=CARTESIAN_POINT('Ctrl Pts',(-15.8230304084962,17.9898319338664,
12.));
#241519=CARTESIAN_POINT('Ctrl Pts',(-15.8416211699679,18.0000807006052,
12.));
#241520=CARTESIAN_POINT('Ctrl Pts',(-15.8603277532831,18.0103296825205,
12.));
#241521=CARTESIAN_POINT('Ctrl Pts',(-15.8791496788683,18.0205781695769,
12.));
#241522=CARTESIAN_POINT('Ctrl Pts',(-15.8980864711042,18.0308254604636,
12.));
#241523=CARTESIAN_POINT('Ctrl Pts',(-15.9171376582436,18.0410708624208,
12.));
#241524=CARTESIAN_POINT('Ctrl Pts',(-15.9363027723244,18.0513136910691,
12.));
#241525=CARTESIAN_POINT('Ctrl Pts',(-15.9555813490644,18.0615532702359,
12.));
#241526=CARTESIAN_POINT('Ctrl Pts',(-15.9749729277846,18.0717889317958,
12.));
#241527=CARTESIAN_POINT('Ctrl Pts',(-15.9944770513613,18.0820200155236,
12.));
#241528=CARTESIAN_POINT('Ctrl Pts',(-16.014093266161,18.0922458689462,12.));
#241529=CARTESIAN_POINT('Ctrl Pts',(-16.0338211219693,18.1024658471966,
12.));
#241530=CARTESIAN_POINT('Ctrl Pts',(-16.0536601719126,18.112679312869,12.));
#241531=CARTESIAN_POINT('Ctrl Pts',(-16.0736099723668,18.1228856358751,
12.));
#241532=CARTESIAN_POINT('Ctrl Pts',(-16.0936700829112,18.1330841933105,
12.));
#241533=CARTESIAN_POINT('Ctrl Pts',(-16.1138400662794,18.1432743693235,
12.));
#241534=CARTESIAN_POINT('Ctrl Pts',(-16.1341194882988,18.1534555549852,
12.));
#241535=CARTESIAN_POINT('Ctrl Pts',(-16.154507917826,18.1636271481615,12.));
#241536=CARTESIAN_POINT('Ctrl Pts',(-16.1750049266671,18.1737885533849,
12.));
#241537=CARTESIAN_POINT('Ctrl Pts',(-16.1956100895073,18.1839391817331,
12.));
#241538=CARTESIAN_POINT('Ctrl Pts',(-16.2163229838875,18.1940784507229,
12.));
#241539=CARTESIAN_POINT('Ctrl Pts',(-16.2371431901638,18.2042057842035,
12.));
#241540=CARTESIAN_POINT('Ctrl Pts',(-16.2580702914615,18.2143206122529,
12.));
#241541=CARTESIAN_POINT('Ctrl Pts',(-16.2791038736223,18.2244223710745,
12.));
#241542=CARTESIAN_POINT('Ctrl Pts',(-16.3002435251378,18.2345105028982,
12.));
#241543=CARTESIAN_POINT('Ctrl Pts',(-16.3214888370987,18.2445844558741,
12.));
#241544=CARTESIAN_POINT('Ctrl Pts',(-16.3428394031589,18.2546436839608,
12.));
#241545=CARTESIAN_POINT('Ctrl Pts',(-16.3642948194868,18.2646876468169,
12.));
#241546=CARTESIAN_POINT('Ctrl Pts',(-16.385854684708,18.2747158096934,12.));
#241547=CARTESIAN_POINT('Ctrl Pts',(-16.4075185998455,18.2847276433309,
12.));
#241548=CARTESIAN_POINT('Ctrl Pts',(-16.4292861682379,18.294722623851,12.));
#241549=CARTESIAN_POINT('Ctrl Pts',(-16.4511569955233,18.304700232686,12.));
#241550=CARTESIAN_POINT('Ctrl Pts',(-16.4731306896441,18.3146599565231,
12.));
#241551=CARTESIAN_POINT('Ctrl Pts',(-16.4952068608345,18.3246012872469,
12.));
#241552=CARTESIAN_POINT('Ctrl Pts',(-16.5173851216045,18.3345237218864,
12.));
#241553=CARTESIAN_POINT('Ctrl Pts',(-16.5396650867139,18.34442676256,12.));
#241554=CARTESIAN_POINT('Ctrl Pts',(-16.5620463731413,18.354309916433,12.));
#241555=CARTESIAN_POINT('Ctrl Pts',(-16.5845286000217,18.3641726955889,
12.));
#241556=CARTESIAN_POINT('Ctrl Pts',(-16.607111388571,18.3740146168879,12.));
#241557=CARTESIAN_POINT('Ctrl Pts',(-16.6297943620056,18.3838352018327,
12.));
#241558=CARTESIAN_POINT('Ctrl Pts',(-16.6525771454513,18.3936339764332,
12.));
#241559=CARTESIAN_POINT('Ctrl Pts',(-16.6754593658513,18.403410471079,12.));
#241560=CARTESIAN_POINT('Ctrl Pts',(-16.6984406518491,18.413164220399,12.));
#241561=CARTESIAN_POINT('Ctrl Pts',(-16.7215206338818,18.4228947633187,
12.));
#241562=CARTESIAN_POINT('Ctrl Pts',(-16.7446989442882,18.4326016431392,
12.));
#241563=CARTESIAN_POINT('Ctrl Pts',(-16.7679752173992,18.44228440761,12.));
#241564=CARTESIAN_POINT('Ctrl Pts',(-16.791349089629,18.4519426090123,12.));
#241565=CARTESIAN_POINT('Ctrl Pts',(-16.8148201995472,18.4615758042305,
12.));
#241566=CARTESIAN_POINT('Ctrl Pts',(-16.8383881879709,18.4711835548623,
12.));
#241567=CARTESIAN_POINT('Ctrl Pts',(-16.8620526977171,18.480765426877,12.));
#241568=CARTESIAN_POINT('Ctrl Pts',(-16.8858133733088,18.4903209902227,
12.));
#241569=CARTESIAN_POINT('Ctrl Pts',(-16.9096698606943,18.499849818462,12.));
#241570=CARTESIAN_POINT('Ctrl Pts',(-16.9336218069353,18.5093514883835,
12.));
#241571=CARTESIAN_POINT('Ctrl Pts',(-16.9576688599339,18.5188255796659,
12.));
#241572=CARTESIAN_POINT('Ctrl Pts',(-16.981810668038,18.5282716744197,12.));
#241573=CARTESIAN_POINT('Ctrl Pts',(-17.0060468805097,18.5376893576961,
12.));
#241574=CARTESIAN_POINT('Ctrl Pts',(-17.0303771481738,18.547078218209,12.));
#241575=CARTESIAN_POINT('Ctrl Pts',(-17.0548011239751,18.556437848963,12.));
#241576=CARTESIAN_POINT('Ctrl Pts',(-17.0793184636079,18.5657678479789,
12.));
#241577=CARTESIAN_POINT('Ctrl Pts',(-17.1039288260001,18.5750678188542,
12.));
#241578=CARTESIAN_POINT('Ctrl Pts',(-17.1286318741183,18.5843373717247,
12.));
#241579=CARTESIAN_POINT('Ctrl Pts',(-17.1534272741643,18.5935761222825,
12.));
#241580=CARTESIAN_POINT('Ctrl Pts',(-17.1783146940127,18.6027836898817,
12.));
#241581=CARTESIAN_POINT('Ctrl Pts',(-17.2032938019284,18.6119596959949,
12.));
#241582=CARTESIAN_POINT('Ctrl Pts',(-17.2283642650518,18.6211037624038,
12.));
#241583=CARTESIAN_POINT('Ctrl Pts',(-17.2535257482187,18.6302155097943,
12.));
#241584=CARTESIAN_POINT('Ctrl Pts',(-17.2787779120213,18.6392945554748,
12.));
#241585=CARTESIAN_POINT('Ctrl Pts',(-17.3041204135074,18.6483405141865,
12.));
#241586=CARTESIAN_POINT('Ctrl Pts',(-17.3295529098618,18.6573530024033,
12.));
#241587=CARTESIAN_POINT('Ctrl Pts',(-17.3550750612443,18.6663316416582,
12.));
#241588=CARTESIAN_POINT('Ctrl Pts',(-17.3806865340747,18.6752760624052,
12.));
#241589=CARTESIAN_POINT('Ctrl Pts',(-17.4063870038562,18.6841859073471,
12.));
#241590=CARTESIAN_POINT('Ctrl Pts',(-17.4321761588142,18.6930608357409,
12.));
#241591=CARTESIAN_POINT('Ctrl Pts',(-17.4580537012753,18.70190052503,12.));
#241592=CARTESIAN_POINT('Ctrl Pts',(-17.4840193397162,18.7107046613912,
12.));
#241593=CARTESIAN_POINT('Ctrl Pts',(-17.5100727820876,18.7194729318098,
12.));
#241594=CARTESIAN_POINT('Ctrl Pts',(-17.5362137287593,18.7282050157138,
12.));
#241595=CARTESIAN_POINT('Ctrl Pts',(-17.5624418653245,18.7369005764553,
12.));
#241596=CARTESIAN_POINT('Ctrl Pts',(-17.5887568561371,18.7455592536687,
12.));
#241597=CARTESIAN_POINT('Ctrl Pts',(-17.6151583357012,18.7541806530984,
12.));
#241598=CARTESIAN_POINT('Ctrl Pts',(-17.6416459210681,18.762764361321,12.));
#241599=CARTESIAN_POINT('Ctrl Pts',(-17.6682192274236,18.7713099642754,
12.));
#241600=CARTESIAN_POINT('Ctrl Pts',(-17.6948778823014,18.7798170641374,
12.));
#241601=CARTESIAN_POINT('Ctrl Pts',(-17.7216215409035,18.7882852976049,
12.));
#241602=CARTESIAN_POINT('Ctrl Pts',(-17.7484498996905,18.7967143519419,
12.));
#241603=CARTESIAN_POINT('Ctrl Pts',(-17.7753627137853,18.8051039860448,
12.));
#241604=CARTESIAN_POINT('Ctrl Pts',(-17.8023598011057,18.8134540340417,
12.));
#241605=CARTESIAN_POINT('Ctrl Pts',(-17.8294410311006,18.8217643886157,
12.));
#241606=CARTESIAN_POINT('Ctrl Pts',(-17.8566063174771,18.8300349895974,
12.));
#241607=CARTESIAN_POINT('Ctrl Pts',(-17.8784057509356,18.8366196462581,
12.));
#241608=CARTESIAN_POINT('Ctrl Pts',(-17.8947931177807,18.8415402351786,
12.));
#241609=CARTESIAN_POINT('Ctrl Pts',(-17.9057348246595,18.8448126709691,
12.));
#241610=CARTESIAN_POINT('Ctrl Pts',(-17.9112098770111,18.8464468996588,
12.));
#241611=CARTESIAN_POINT('Ctrl Pts',(-12.7689476255363,18.5896416359912,
0.));
#241612=CARTESIAN_POINT('Ctrl Pts',(-12.7689476255363,18.5896416359912,
12.));
#241613=CARTESIAN_POINT('Ctrl Pts',(-12.7689524524483,18.5896460962964,
0.));
#241614=CARTESIAN_POINT('Ctrl Pts',(-12.7689524524483,18.5896460962964,
12.));
#241615=CARTESIAN_POINT('Ctrl Pts',(-12.768986426692,18.5896919669165,0.));
#241616=CARTESIAN_POINT('Ctrl Pts',(-12.768986426692,18.5896919669165,12.));
#241617=CARTESIAN_POINT('Ctrl Pts',(-12.769110348199,18.589871621843,0.));
#241618=CARTESIAN_POINT('Ctrl Pts',(-12.769110348199,18.589871621843,12.));
#241619=CARTESIAN_POINT('Ctrl Pts',(-12.7694215127919,18.5903328777227,
0.));
#241620=CARTESIAN_POINT('Ctrl Pts',(-12.7694215127919,18.5903328777227,
12.));
#241621=CARTESIAN_POINT('Ctrl Pts',(-12.7700520897173,18.5912775137806,
0.));
#241622=CARTESIAN_POINT('Ctrl Pts',(-12.7700520897173,18.5912775137806,
12.));
#241623=CARTESIAN_POINT('Ctrl Pts',(-12.7709195951156,18.5925859134579,
0.));
#241624=CARTESIAN_POINT('Ctrl Pts',(-12.7709195951156,18.5925859134579,
12.));
#241625=CARTESIAN_POINT('Ctrl Pts',(-12.7720142287172,18.5942490615407,
0.));
#241626=CARTESIAN_POINT('Ctrl Pts',(-12.7720142287172,18.5942490615407,
12.));
#241627=CARTESIAN_POINT('Ctrl Pts',(-12.7733231262108,18.5962551167772,
0.));
#241628=CARTESIAN_POINT('Ctrl Pts',(-12.7733231262108,18.5962551167772,
12.));
#241629=CARTESIAN_POINT('Ctrl Pts',(-12.7748328937638,18.598591752595,0.));
#241630=CARTESIAN_POINT('Ctrl Pts',(-12.7748328937638,18.598591752595,12.));
#241631=CARTESIAN_POINT('Ctrl Pts',(-12.7765325225081,18.6012488486709,
0.));
#241632=CARTESIAN_POINT('Ctrl Pts',(-12.7765325225081,18.6012488486709,
12.));
#241633=CARTESIAN_POINT('Ctrl Pts',(-12.7784139605066,18.6042190183704,
0.));
#241634=CARTESIAN_POINT('Ctrl Pts',(-12.7784139605066,18.6042190183704,
12.));
#241635=CARTESIAN_POINT('Ctrl Pts',(-12.7804705387658,18.6074961535723,
0.));
#241636=CARTESIAN_POINT('Ctrl Pts',(-12.7804705387658,18.6074961535723,
12.));
#241637=CARTESIAN_POINT('Ctrl Pts',(-12.7826959526925,18.6110744826219,
0.));
#241638=CARTESIAN_POINT('Ctrl Pts',(-12.7826959526925,18.6110744826219,
12.));
#241639=CARTESIAN_POINT('Ctrl Pts',(-12.7850831657901,18.6149475565188,
0.));
#241640=CARTESIAN_POINT('Ctrl Pts',(-12.7850831657901,18.6149475565188,
12.));
#241641=CARTESIAN_POINT('Ctrl Pts',(-12.7876249657834,18.6191087624752,
0.));
#241642=CARTESIAN_POINT('Ctrl Pts',(-12.7876249657834,18.6191087624752,
12.));
#241643=CARTESIAN_POINT('Ctrl Pts',(-12.7903142925234,18.6235516265575,
0.));
#241644=CARTESIAN_POINT('Ctrl Pts',(-12.7903142925234,18.6235516265575,
12.));
#241645=CARTESIAN_POINT('Ctrl Pts',(-12.7931447451555,18.6282702819371,
0.));
#241646=CARTESIAN_POINT('Ctrl Pts',(-12.7931447451555,18.6282702819371,
12.));
#241647=CARTESIAN_POINT('Ctrl Pts',(-12.7961106222251,18.6332595057006,
0.));
#241648=CARTESIAN_POINT('Ctrl Pts',(-12.7961106222251,18.6332595057006,
12.));
#241649=CARTESIAN_POINT('Ctrl Pts',(-12.7992066625264,18.63851447924,0.));
#241650=CARTESIAN_POINT('Ctrl Pts',(-12.7992066625264,18.63851447924,12.));
#241651=CARTESIAN_POINT('Ctrl Pts',(-12.8024278770152,18.6440306327456,
0.));
#241652=CARTESIAN_POINT('Ctrl Pts',(-12.8024278770152,18.6440306327456,
12.));
#241653=CARTESIAN_POINT('Ctrl Pts',(-12.805769331162,18.6498034438986,0.));
#241654=CARTESIAN_POINT('Ctrl Pts',(-12.805769331162,18.6498034438986,12.));
#241655=CARTESIAN_POINT('Ctrl Pts',(-12.8092261933858,18.6558284825773,
0.));
#241656=CARTESIAN_POINT('Ctrl Pts',(-12.8092261933858,18.6558284825773,
12.));
#241657=CARTESIAN_POINT('Ctrl Pts',(-12.8127937909631,18.6621014624746,
0.));
#241658=CARTESIAN_POINT('Ctrl Pts',(-12.8127937909631,18.6621014624746,
12.));
#241659=CARTESIAN_POINT('Ctrl Pts',(-12.8164676687362,18.6686182952799,
0.));
#241660=CARTESIAN_POINT('Ctrl Pts',(-12.8164676687362,18.6686182952799,
12.));
#241661=CARTESIAN_POINT('Ctrl Pts',(-12.8202436318474,18.6753751301092,
0.));
#241662=CARTESIAN_POINT('Ctrl Pts',(-12.8202436318474,18.6753751301092,
12.));
#241663=CARTESIAN_POINT('Ctrl Pts',(-12.8241176980017,18.6823683094139,
0.));
#241664=CARTESIAN_POINT('Ctrl Pts',(-12.8241176980017,18.6823683094139,
12.));
#241665=CARTESIAN_POINT('Ctrl Pts',(-12.8280860635231,18.6895943376171,
0.));
#241666=CARTESIAN_POINT('Ctrl Pts',(-12.8280860635231,18.6895943376171,
12.));
#241667=CARTESIAN_POINT('Ctrl Pts',(-12.8321450599789,18.6970498410172,
0.));
#241668=CARTESIAN_POINT('Ctrl Pts',(-12.8321450599789,18.6970498410172,
12.));
#241669=CARTESIAN_POINT('Ctrl Pts',(-12.8362911280361,18.7047315436294,
0.));
#241670=CARTESIAN_POINT('Ctrl Pts',(-12.8362911280361,18.7047315436294,
12.));
#241671=CARTESIAN_POINT('Ctrl Pts',(-12.8405208263431,18.7126362754445,
0.));
#241672=CARTESIAN_POINT('Ctrl Pts',(-12.8405208263431,18.7126362754445,
12.));
#241673=CARTESIAN_POINT('Ctrl Pts',(-12.8448308329494,18.7207609737702,
0.));
#241674=CARTESIAN_POINT('Ctrl Pts',(-12.8448308329494,18.7207609737702,
12.));
#241675=CARTESIAN_POINT('Ctrl Pts',(-12.8492179511591,18.7291026886554,
0.));
#241676=CARTESIAN_POINT('Ctrl Pts',(-12.8492179511591,18.7291026886554,
12.));
#241677=CARTESIAN_POINT('Ctrl Pts',(-12.8536791086316,18.7376585820854,
0.));
#241678=CARTESIAN_POINT('Ctrl Pts',(-12.8536791086316,18.7376585820854,
12.));
#241679=CARTESIAN_POINT('Ctrl Pts',(-12.8582113455646,18.7464259171251,
0.));
#241680=CARTESIAN_POINT('Ctrl Pts',(-12.8582113455646,18.7464259171251,
12.));
#241681=CARTESIAN_POINT('Ctrl Pts',(-12.8628118054171,18.7554020493887,
0.));
#241682=CARTESIAN_POINT('Ctrl Pts',(-12.8628118054171,18.7554020493887,
12.));
#241683=CARTESIAN_POINT('Ctrl Pts',(-12.8674777239653,18.7645844169564,
0.));
#241684=CARTESIAN_POINT('Ctrl Pts',(-12.8674777239653,18.7645844169564,
12.));
#241685=CARTESIAN_POINT('Ctrl Pts',(-12.872206421181,18.7739705329022,0.));
#241686=CARTESIAN_POINT('Ctrl Pts',(-12.872206421181,18.7739705329022,12.));
#241687=CARTESIAN_POINT('Ctrl Pts',(-12.8769952998095,18.7835579840477,
0.));
#241688=CARTESIAN_POINT('Ctrl Pts',(-12.8769952998095,18.7835579840477,
12.));
#241689=CARTESIAN_POINT('Ctrl Pts',(-12.8818418427475,18.7933444285868,
0.));
#241690=CARTESIAN_POINT('Ctrl Pts',(-12.8818418427475,18.7933444285868,
12.));
#241691=CARTESIAN_POINT('Ctrl Pts',(-12.8867436109546,18.8033275941943,
0.));
#241692=CARTESIAN_POINT('Ctrl Pts',(-12.8867436109546,18.8033275941943,
12.));
#241693=CARTESIAN_POINT('Ctrl Pts',(-12.8916982409935,18.813505275782,0.));
#241694=CARTESIAN_POINT('Ctrl Pts',(-12.8916982409935,18.813505275782,12.));
#241695=CARTESIAN_POINT('Ctrl Pts',(-12.8967034410755,18.8238753319128,
0.));
#241696=CARTESIAN_POINT('Ctrl Pts',(-12.8967034410755,18.8238753319128,
12.));
#241697=CARTESIAN_POINT('Ctrl Pts',(-12.9017569871738,18.834435681259,0.));
#241698=CARTESIAN_POINT('Ctrl Pts',(-12.9017569871738,18.834435681259,12.));
#241699=CARTESIAN_POINT('Ctrl Pts',(-12.9068567191854,18.8451842990984,
0.));
#241700=CARTESIAN_POINT('Ctrl Pts',(-12.9068567191854,18.8451842990984,
12.));
#241701=CARTESIAN_POINT('Ctrl Pts',(-12.9120005369063,18.8561192136198,
0.));
#241702=CARTESIAN_POINT('Ctrl Pts',(-12.9120005369063,18.8561192136198,
12.));
#241703=CARTESIAN_POINT('Ctrl Pts',(-12.9171863977045,18.8672385038326,
0.));
#241704=CARTESIAN_POINT('Ctrl Pts',(-12.9171863977045,18.8672385038326,
12.));
#241705=CARTESIAN_POINT('Ctrl Pts',(-12.9224123144982,18.8785402977527,
0.));
#241706=CARTESIAN_POINT('Ctrl Pts',(-12.9224123144982,18.8785402977527,
12.));
#241707=CARTESIAN_POINT('Ctrl Pts',(-12.9276763536373,18.8900227704889,
0.));
#241708=CARTESIAN_POINT('Ctrl Pts',(-12.9276763536373,18.8900227704889,
12.));
#241709=CARTESIAN_POINT('Ctrl Pts',(-12.9329766328185,18.9016841423403,
0.));
#241710=CARTESIAN_POINT('Ctrl Pts',(-12.9329766328185,18.9016841423403,
12.));
#241711=CARTESIAN_POINT('Ctrl Pts',(-12.9383113190375,18.9135226769465,
0.));
#241712=CARTESIAN_POINT('Ctrl Pts',(-12.9383113190375,18.9135226769465,
12.));
#241713=CARTESIAN_POINT('Ctrl Pts',(-12.9436786266105,18.9255366795195,
0.));
#241714=CARTESIAN_POINT('Ctrl Pts',(-12.9436786266105,18.9255366795195,
12.));
#241715=CARTESIAN_POINT('Ctrl Pts',(-12.9490768151821,18.9377244950435,
0.));
#241716=CARTESIAN_POINT('Ctrl Pts',(-12.9490768151821,18.9377244950435,
12.));
#241717=CARTESIAN_POINT('Ctrl Pts',(-12.9545041877377,18.9500845064715,
0.));
#241718=CARTESIAN_POINT('Ctrl Pts',(-12.9545041877377,18.9500845064715,
12.));
#241719=CARTESIAN_POINT('Ctrl Pts',(-12.9599590886319,18.9626151329229,
0.));
#241720=CARTESIAN_POINT('Ctrl Pts',(-12.9599590886319,18.9626151329229,
12.));
#241721=CARTESIAN_POINT('Ctrl Pts',(-12.9654399021869,18.9753148284475,
0.));
#241722=CARTESIAN_POINT('Ctrl Pts',(-12.9654399021869,18.9753148284475,
12.));
#241723=CARTESIAN_POINT('Ctrl Pts',(-12.9709450512747,18.9881820807585,
0.));
#241724=CARTESIAN_POINT('Ctrl Pts',(-12.9709450512747,18.9881820807585,
12.));
#241725=CARTESIAN_POINT('Ctrl Pts',(-12.9764729959205,19.0012154099791,
0.));
#241726=CARTESIAN_POINT('Ctrl Pts',(-12.9764729959205,19.0012154099791,
12.));
#241727=CARTESIAN_POINT('Ctrl Pts',(-12.9820222318716,19.0144133673348,
0.));
#241728=CARTESIAN_POINT('Ctrl Pts',(-12.9820222318716,19.0144133673348,
12.));
#241729=CARTESIAN_POINT('Ctrl Pts',(-12.9875912893003,19.0277745339908,
0.));
#241730=CARTESIAN_POINT('Ctrl Pts',(-12.9875912893003,19.0277745339908,
12.));
#241731=CARTESIAN_POINT('Ctrl Pts',(-12.9931787316515,19.0412975200398,
0.));
#241732=CARTESIAN_POINT('Ctrl Pts',(-12.9931787316515,19.0412975200398,
12.));
#241733=CARTESIAN_POINT('Ctrl Pts',(-12.9987831544502,19.0549809634355,
0.));
#241734=CARTESIAN_POINT('Ctrl Pts',(-12.9987831544502,19.0549809634355,
12.));
#241735=CARTESIAN_POINT('Ctrl Pts',(-13.0044031841381,19.0688235289437,
0.));
#241736=CARTESIAN_POINT('Ctrl Pts',(-13.0044031841381,19.0688235289437,
12.));
#241737=CARTESIAN_POINT('Ctrl Pts',(-13.0100374768785,19.0828239070482,
0.));
#241738=CARTESIAN_POINT('Ctrl Pts',(-13.0100374768785,19.0828239070482,
12.));
#241739=CARTESIAN_POINT('Ctrl Pts',(-13.0156847176093,19.0969808131225,
0.));
#241740=CARTESIAN_POINT('Ctrl Pts',(-13.0156847176093,19.0969808131225,
12.));
#241741=CARTESIAN_POINT('Ctrl Pts',(-13.0213436191326,19.1112929866308,
0.));
#241742=CARTESIAN_POINT('Ctrl Pts',(-13.0213436191326,19.1112929866308,
12.));
#241743=CARTESIAN_POINT('Ctrl Pts',(-13.0270129211976,19.1257591903099,
0.));
#241744=CARTESIAN_POINT('Ctrl Pts',(-13.0270129211976,19.1257591903099,
12.));
#241745=CARTESIAN_POINT('Ctrl Pts',(-13.0326913895841,19.1403782093389,
0.));
#241746=CARTESIAN_POINT('Ctrl Pts',(-13.0326913895841,19.1403782093389,
12.));
#241747=CARTESIAN_POINT('Ctrl Pts',(-13.0383778152072,19.1551488505233,
0.));
#241748=CARTESIAN_POINT('Ctrl Pts',(-13.0383778152072,19.1551488505233,
12.));
#241749=CARTESIAN_POINT('Ctrl Pts',(-13.0440710133775,19.1700699416625,
0.));
#241750=CARTESIAN_POINT('Ctrl Pts',(-13.0440710133775,19.1700699416625,
12.));
#241751=CARTESIAN_POINT('Ctrl Pts',(-13.0497698230442,19.1851403308825,
0.));
#241752=CARTESIAN_POINT('Ctrl Pts',(-13.0497698230442,19.1851403308825,
12.));
#241753=CARTESIAN_POINT('Ctrl Pts',(-13.0554731060537,19.2003588859771,
0.));
#241754=CARTESIAN_POINT('Ctrl Pts',(-13.0554731060537,19.2003588859771,
12.));
#241755=CARTESIAN_POINT('Ctrl Pts',(-13.0611797463913,19.2157244937141,
0.));
#241756=CARTESIAN_POINT('Ctrl Pts',(-13.0611797463913,19.2157244937141,
12.));
#241757=CARTESIAN_POINT('Ctrl Pts',(-13.0668886494791,19.2312360592031,
0.));
#241758=CARTESIAN_POINT('Ctrl Pts',(-13.0668886494791,19.2312360592031,
12.));
#241759=CARTESIAN_POINT('Ctrl Pts',(-13.0725987415856,19.2468925053988,
0.));
#241760=CARTESIAN_POINT('Ctrl Pts',(-13.0725987415856,19.2468925053988,
12.));
#241761=CARTESIAN_POINT('Ctrl Pts',(-13.0783089692118,19.2626927725596,
0.));
#241762=CARTESIAN_POINT('Ctrl Pts',(-13.0783089692118,19.2626927725596,
12.));
#241763=CARTESIAN_POINT('Ctrl Pts',(-13.0840182984949,19.2786358177198,
0.));
#241764=CARTESIAN_POINT('Ctrl Pts',(-13.0840182984949,19.2786358177198,
12.));
#241765=CARTESIAN_POINT('Ctrl Pts',(-13.089725714597,19.2947206141246,0.));
#241766=CARTESIAN_POINT('Ctrl Pts',(-13.089725714597,19.2947206141246,12.));
#241767=CARTESIAN_POINT('Ctrl Pts',(-13.095430221148,19.3109461507358,0.));
#241768=CARTESIAN_POINT('Ctrl Pts',(-13.095430221148,19.3109461507358,12.));
#241769=CARTESIAN_POINT('Ctrl Pts',(-13.1011308397592,19.3273114318268,
0.));
#241770=CARTESIAN_POINT('Ctrl Pts',(-13.1011308397592,19.3273114318268,
12.));
#241771=CARTESIAN_POINT('Ctrl Pts',(-13.1068266095186,19.3438154765395,
0.));
#241772=CARTESIAN_POINT('Ctrl Pts',(-13.1068266095186,19.3438154765395,
12.));
#241773=CARTESIAN_POINT('Ctrl Pts',(-13.1125165865021,19.3604573184516,
0.));
#241774=CARTESIAN_POINT('Ctrl Pts',(-13.1125165865021,19.3604573184516,
12.));
#241775=CARTESIAN_POINT('Ctrl Pts',(-13.118199843271,19.3772360051093,0.));
#241776=CARTESIAN_POINT('Ctrl Pts',(-13.118199843271,19.3772360051093,12.));
#241777=CARTESIAN_POINT('Ctrl Pts',(-13.1238754684177,19.3941505976267,
0.));
#241778=CARTESIAN_POINT('Ctrl Pts',(-13.1238754684177,19.3941505976267,
12.));
#241779=CARTESIAN_POINT('Ctrl Pts',(-13.1295425661635,19.4112001703561,
0.));
#241780=CARTESIAN_POINT('Ctrl Pts',(-13.1295425661635,19.4112001703561,
12.));
#241781=CARTESIAN_POINT('Ctrl Pts',(-13.1352002559439,19.4283838105265,
0.));
#241782=CARTESIAN_POINT('Ctrl Pts',(-13.1352002559439,19.4283838105265,
12.));
#241783=CARTESIAN_POINT('Ctrl Pts',(-13.140847672006,19.4457006178875,0.));
#241784=CARTESIAN_POINT('Ctrl Pts',(-13.140847672006,19.4457006178875,12.));
#241785=CARTESIAN_POINT('Ctrl Pts',(-13.1464839629966,19.463149704325,0.));
#241786=CARTESIAN_POINT('Ctrl Pts',(-13.1464839629966,19.463149704325,12.));
#241787=CARTESIAN_POINT('Ctrl Pts',(-13.1521082915846,19.4807301935256,
0.));
#241788=CARTESIAN_POINT('Ctrl Pts',(-13.1521082915846,19.4807301935256,
12.));
#241789=CARTESIAN_POINT('Ctrl Pts',(-13.1577198341238,19.498441220707,0.));
#241790=CARTESIAN_POINT('Ctrl Pts',(-13.1577198341238,19.498441220707,12.));
#241791=CARTESIAN_POINT('Ctrl Pts',(-13.1633177803097,19.5162819323207,
0.));
#241792=CARTESIAN_POINT('Ctrl Pts',(-13.1633177803097,19.5162819323207,
12.));
#241793=CARTESIAN_POINT('Ctrl Pts',(-13.1689013328432,19.5342514857564,
0.));
#241794=CARTESIAN_POINT('Ctrl Pts',(-13.1689013328432,19.5342514857564,
12.));
#241795=CARTESIAN_POINT('Ctrl Pts',(-13.1744697070918,19.5523490490254,
0.));
#241796=CARTESIAN_POINT('Ctrl Pts',(-13.1744697070918,19.5523490490254,
12.));
#241797=CARTESIAN_POINT('Ctrl Pts',(-13.1800221307683,19.5705738004682,
0.));
#241798=CARTESIAN_POINT('Ctrl Pts',(-13.1800221307683,19.5705738004682,
12.));
#241799=CARTESIAN_POINT('Ctrl Pts',(-13.1855578436479,19.5889249285351,
0.));
#241800=CARTESIAN_POINT('Ctrl Pts',(-13.1855578436479,19.5889249285351,
12.));
#241801=CARTESIAN_POINT('Ctrl Pts',(-13.1910760972818,19.6074016315421,
0.));
#241802=CARTESIAN_POINT('Ctrl Pts',(-13.1910760972818,19.6074016315421,
12.));
#241803=CARTESIAN_POINT('Ctrl Pts',(-13.196576154715,19.6260031174244,0.));
#241804=CARTESIAN_POINT('Ctrl Pts',(-13.196576154715,19.6260031174244,12.));
#241805=CARTESIAN_POINT('Ctrl Pts',(-13.202057290206,19.6447286034764,0.));
#241806=CARTESIAN_POINT('Ctrl Pts',(-13.202057290206,19.6447286034764,12.));
#241807=CARTESIAN_POINT('Ctrl Pts',(-13.2075187889522,19.6635773160924,
0.));
#241808=CARTESIAN_POINT('Ctrl Pts',(-13.2075187889522,19.6635773160924,
12.));
#241809=CARTESIAN_POINT('Ctrl Pts',(-13.2129599468478,19.6825484905812,
0.));
#241810=CARTESIAN_POINT('Ctrl Pts',(-13.2129599468478,19.6825484905812,
12.));
#241811=CARTESIAN_POINT('Ctrl Pts',(-13.2183800702431,19.7016413709678,
0.));
#241812=CARTESIAN_POINT('Ctrl Pts',(-13.2183800702431,19.7016413709678,
12.));
#241813=CARTESIAN_POINT('Ctrl Pts',(-13.2237784757065,19.7208552097867,
0.));
#241814=CARTESIAN_POINT('Ctrl Pts',(-13.2237784757065,19.7208552097867,
12.));
#241815=CARTESIAN_POINT('Ctrl Pts',(-13.2291544897902,19.7401892678701,
0.));
#241816=CARTESIAN_POINT('Ctrl Pts',(-13.2291544897902,19.7401892678701,
12.));
#241817=CARTESIAN_POINT('Ctrl Pts',(-13.2345074487968,19.7596428141176,
0.));
#241818=CARTESIAN_POINT('Ctrl Pts',(-13.2345074487968,19.7596428141176,
12.));
#241819=CARTESIAN_POINT('Ctrl Pts',(-13.239836698568,19.7792151253297,0.));
#241820=CARTESIAN_POINT('Ctrl Pts',(-13.239836698568,19.7792151253297,12.));
#241821=CARTESIAN_POINT('Ctrl Pts',(-13.2451415942809,19.7989054860501,
0.));
#241822=CARTESIAN_POINT('Ctrl Pts',(-13.2451415942809,19.7989054860501,
12.));
#241823=CARTESIAN_POINT('Ctrl Pts',(-13.2504215002458,19.8187131883919,
0.));
#241824=CARTESIAN_POINT('Ctrl Pts',(-13.2504215002458,19.8187131883919,
12.));
#241825=CARTESIAN_POINT('Ctrl Pts',(-13.2556757897085,19.8386375318632,
0.));
#241826=CARTESIAN_POINT('Ctrl Pts',(-13.2556757897085,19.8386375318632,
12.));
#241827=CARTESIAN_POINT('Ctrl Pts',(-13.2609038446525,19.8586778231711,
0.));
#241828=CARTESIAN_POINT('Ctrl Pts',(-13.2609038446525,19.8586778231711,
12.));
#241829=CARTESIAN_POINT('Ctrl Pts',(-13.2661050556128,19.8788333760571,
0.));
#241830=CARTESIAN_POINT('Ctrl Pts',(-13.2661050556128,19.8788333760571,
12.));
#241831=CARTESIAN_POINT('Ctrl Pts',(-13.2712788215015,19.8991035111739,
0.));
#241832=CARTESIAN_POINT('Ctrl Pts',(-13.2712788215015,19.8991035111739,
12.));
#241833=CARTESIAN_POINT('Ctrl Pts',(-13.2764245494354,19.9194875559419,
0.));
#241834=CARTESIAN_POINT('Ctrl Pts',(-13.2764245494354,19.9194875559419,
12.));
#241835=CARTESIAN_POINT('Ctrl Pts',(-13.2815416545663,19.9399848444019,
0.));
#241836=CARTESIAN_POINT('Ctrl Pts',(-13.2815416545663,19.9399848444019,
12.));
#241837=CARTESIAN_POINT('Ctrl Pts',(-13.2866295599152,19.9605947170589,
0.));
#241838=CARTESIAN_POINT('Ctrl Pts',(-13.2866295599152,19.9605947170589,
12.));
#241839=CARTESIAN_POINT('Ctrl Pts',(-13.2916876962098,19.9813165207174,
0.));
#241840=CARTESIAN_POINT('Ctrl Pts',(-13.2916876962098,19.9813165207174,
12.));
#241841=CARTESIAN_POINT('Ctrl Pts',(-13.296715501731,20.0021496083742,0.));
#241842=CARTESIAN_POINT('Ctrl Pts',(-13.296715501731,20.0021496083742,12.));
#241843=CARTESIAN_POINT('Ctrl Pts',(-13.3017124221639,20.0230933391039,
0.));
#241844=CARTESIAN_POINT('Ctrl Pts',(-13.3017124221639,20.0230933391039,
12.));
#241845=CARTESIAN_POINT('Ctrl Pts',(-13.3066779104515,20.0441470779345,
0.));
#241846=CARTESIAN_POINT('Ctrl Pts',(-13.3066779104515,20.0441470779345,
12.));
#241847=CARTESIAN_POINT('Ctrl Pts',(-13.3116114266514,20.0653101957188,
0.));
#241848=CARTESIAN_POINT('Ctrl Pts',(-13.3116114266514,20.0653101957188,
12.));
#241849=CARTESIAN_POINT('Ctrl Pts',(-13.3165124377963,20.0865820689883,
0.));
#241850=CARTESIAN_POINT('Ctrl Pts',(-13.3165124377963,20.0865820689883,
12.));
#241851=CARTESIAN_POINT('Ctrl Pts',(-13.3213804177588,20.1079620798377,
0.));
#241852=CARTESIAN_POINT('Ctrl Pts',(-13.3213804177588,20.1079620798377,
12.));
#241853=CARTESIAN_POINT('Ctrl Pts',(-13.3262148471228,20.1294496158405,
0.));
#241854=CARTESIAN_POINT('Ctrl Pts',(-13.3262148471228,20.1294496158405,
12.));
#241855=CARTESIAN_POINT('Ctrl Pts',(-13.3310152130565,20.1510440699477,
0.));
#241856=CARTESIAN_POINT('Ctrl Pts',(-13.3310152130565,20.1510440699477,
12.));
#241857=CARTESIAN_POINT('Ctrl Pts',(-13.3357810091903,20.1727448403818,
0.));
#241858=CARTESIAN_POINT('Ctrl Pts',(-13.3357810091903,20.1727448403818,
12.));
#241859=CARTESIAN_POINT('Ctrl Pts',(-13.3405117354969,20.1945513305233,
0.));
#241860=CARTESIAN_POINT('Ctrl Pts',(-13.3405117354969,20.1945513305233,
12.));
#241861=CARTESIAN_POINT('Ctrl Pts',(-13.3452068981763,20.2164629487855,
0.));
#241862=CARTESIAN_POINT('Ctrl Pts',(-13.3452068981763,20.2164629487855,
12.));
#241863=CARTESIAN_POINT('Ctrl Pts',(-13.3498660095382,20.2384791085354,
0.));
#241864=CARTESIAN_POINT('Ctrl Pts',(-13.3498660095382,20.2384791085354,
12.));
#241865=CARTESIAN_POINT('Ctrl Pts',(-13.3544885878886,20.2605992280117,
0.));
#241866=CARTESIAN_POINT('Ctrl Pts',(-13.3544885878886,20.2605992280117,
12.));
#241867=CARTESIAN_POINT('Ctrl Pts',(-13.3590741574194,20.2828227302337,
0.));
#241868=CARTESIAN_POINT('Ctrl Pts',(-13.3590741574194,20.2828227302337,
12.));
#241869=CARTESIAN_POINT('Ctrl Pts',(-13.3636222481017,20.3051490429049,
0.));
#241870=CARTESIAN_POINT('Ctrl Pts',(-13.3636222481017,20.3051490429049,
12.));
#241871=CARTESIAN_POINT('Ctrl Pts',(-13.3681323955828,20.3275775983032,
0.));
#241872=CARTESIAN_POINT('Ctrl Pts',(-13.3681323955828,20.3275775983032,
12.));
#241873=CARTESIAN_POINT('Ctrl Pts',(-13.3726041410869,20.3501078331818,
0.));
#241874=CARTESIAN_POINT('Ctrl Pts',(-13.3726041410869,20.3501078331818,
12.));
#241875=CARTESIAN_POINT('Ctrl Pts',(-13.377037031319,20.3727391887187,0.));
#241876=CARTESIAN_POINT('Ctrl Pts',(-13.377037031319,20.3727391887187,12.));
#241877=CARTESIAN_POINT('Ctrl Pts',(-13.3814306183721,20.3954711104504,
0.));
#241878=CARTESIAN_POINT('Ctrl Pts',(-13.3814306183721,20.3954711104504,
12.));
#241879=CARTESIAN_POINT('Ctrl Pts',(-13.3857844596387,20.4183030482002,
0.));
#241880=CARTESIAN_POINT('Ctrl Pts',(-13.3857844596387,20.4183030482002,
12.));
#241881=CARTESIAN_POINT('Ctrl Pts',(-13.3900981177254,20.4412344560007,
0.));
#241882=CARTESIAN_POINT('Ctrl Pts',(-13.3900981177254,20.4412344560007,
12.));
#241883=CARTESIAN_POINT('Ctrl Pts',(-13.3943711603739,20.4642647920038,
0.));
#241884=CARTESIAN_POINT('Ctrl Pts',(-13.3943711603739,20.4642647920038,
12.));
#241885=CARTESIAN_POINT('Ctrl Pts',(-13.3986031603716,20.4873935184041,
0.));
#241886=CARTESIAN_POINT('Ctrl Pts',(-13.3986031603716,20.4873935184041,
12.));
#241887=CARTESIAN_POINT('Ctrl Pts',(-13.4027936954529,20.5106201013755,
0.));
#241888=CARTESIAN_POINT('Ctrl Pts',(-13.4027936954529,20.5106201013755,
12.));
#241889=CARTESIAN_POINT('Ctrl Pts',(-13.4069423482076,20.5339440109957,
0.));
#241890=CARTESIAN_POINT('Ctrl Pts',(-13.4069423482076,20.5339440109957,
12.));
#241891=CARTESIAN_POINT('Ctrl Pts',(-13.4110487059912,20.557364721164,0.));
#241892=CARTESIAN_POINT('Ctrl Pts',(-13.4110487059912,20.557364721164,12.));
#241893=CARTESIAN_POINT('Ctrl Pts',(-13.4151123608411,20.5808817095155,
0.));
#241894=CARTESIAN_POINT('Ctrl Pts',(-13.4151123608411,20.5808817095155,
12.));
#241895=CARTESIAN_POINT('Ctrl Pts',(-13.4191329093932,20.6044944573151,
0.));
#241896=CARTESIAN_POINT('Ctrl Pts',(-13.4191329093932,20.6044944573151,
12.));
#241897=CARTESIAN_POINT('Ctrl Pts',(-13.4231099528178,20.6282024494234,
0.));
#241898=CARTESIAN_POINT('Ctrl Pts',(-13.4231099528178,20.6282024494234,
12.));
#241899=CARTESIAN_POINT('Ctrl Pts',(-13.427043096765,20.6520051742867,0.));
#241900=CARTESIAN_POINT('Ctrl Pts',(-13.427043096765,20.6520051742867,12.));
#241901=CARTESIAN_POINT('Ctrl Pts',(-13.4309319513119,20.6759021239102,
0.));
#241902=CARTESIAN_POINT('Ctrl Pts',(-13.4309319513119,20.6759021239102,
12.));
#241903=CARTESIAN_POINT('Ctrl Pts',(-13.4347761309154,20.6998927938288,
0.));
#241904=CARTESIAN_POINT('Ctrl Pts',(-13.4347761309154,20.6998927938288,
12.));
#241905=CARTESIAN_POINT('Ctrl Pts',(-13.4385752543663,20.7239766830675,
0.));
#241906=CARTESIAN_POINT('Ctrl Pts',(-13.4385752543663,20.7239766830675,
12.));
#241907=CARTESIAN_POINT('Ctrl Pts',(-13.4423289447561,20.7481532941014,
0.));
#241908=CARTESIAN_POINT('Ctrl Pts',(-13.4423289447561,20.7481532941014,
12.));
#241909=CARTESIAN_POINT('Ctrl Pts',(-13.4460368293689,20.7724221327609,
0.));
#241910=CARTESIAN_POINT('Ctrl Pts',(-13.4460368293689,20.7724221327609,
12.));
#241911=CARTESIAN_POINT('Ctrl Pts',(-13.4496985395637,20.7967827081228,
0.));
#241912=CARTESIAN_POINT('Ctrl Pts',(-13.4496985395637,20.7967827081228,
12.));
#241913=CARTESIAN_POINT('Ctrl Pts',(-13.4533137106667,20.821234532398,0.));
#241914=CARTESIAN_POINT('Ctrl Pts',(-13.4533137106667,20.821234532398,12.));
#241915=CARTESIAN_POINT('Ctrl Pts',(-13.4568819818631,20.8457771208083,
0.));
#241916=CARTESIAN_POINT('Ctrl Pts',(-13.4568819818631,20.8457771208083,
12.));
#241917=CARTESIAN_POINT('Ctrl Pts',(-13.4604029960983,20.8704099914641,
0.));
#241918=CARTESIAN_POINT('Ctrl Pts',(-13.4604029960983,20.8704099914641,
12.));
#241919=CARTESIAN_POINT('Ctrl Pts',(-13.4638763999725,20.8951326652158,
0.));
#241920=CARTESIAN_POINT('Ctrl Pts',(-13.4638763999725,20.8951326652158,
12.));
#241921=CARTESIAN_POINT('Ctrl Pts',(-13.4673018437717,20.9199446657583,
0.));
#241922=CARTESIAN_POINT('Ctrl Pts',(-13.4673018437717,20.9199446657583,
12.));
#241923=CARTESIAN_POINT('Ctrl Pts',(-13.4706789815166,20.9448455197557,
0.));
#241924=CARTESIAN_POINT('Ctrl Pts',(-13.4706789815166,20.9448455197557,
12.));
#241925=CARTESIAN_POINT('Ctrl Pts',(-13.4740074710086,20.9698347569476,
0.));
#241926=CARTESIAN_POINT('Ctrl Pts',(-13.4740074710086,20.9698347569476,
12.));
#241927=CARTESIAN_POINT('Ctrl Pts',(-13.4772869738879,20.9949119102592,
0.));
#241928=CARTESIAN_POINT('Ctrl Pts',(-13.4772869738879,20.9949119102592,
12.));
#241929=CARTESIAN_POINT('Ctrl Pts',(-13.4805171556822,21.0200765158884,
0.));
#241930=CARTESIAN_POINT('Ctrl Pts',(-13.4805171556822,21.0200765158884,
12.));
#241931=CARTESIAN_POINT('Ctrl Pts',(-13.4836976858912,21.0453281134245,
0.));
#241932=CARTESIAN_POINT('Ctrl Pts',(-13.4836976858912,21.0453281134245,
12.));
#241933=CARTESIAN_POINT('Ctrl Pts',(-13.4868282377191,21.0706662455199,
0.));
#241934=CARTESIAN_POINT('Ctrl Pts',(-13.4868282377191,21.0706662455199,
12.));
#241935=CARTESIAN_POINT('Ctrl Pts',(-13.4899084877717,21.0960904575046,
0.));
#241936=CARTESIAN_POINT('Ctrl Pts',(-13.4899084877717,21.0960904575046,
12.));
#241937=CARTESIAN_POINT('Ctrl Pts',(-13.4929381157778,21.1216002970207,
0.));
#241938=CARTESIAN_POINT('Ctrl Pts',(-13.4929381157778,21.1216002970207,
12.));
#241939=CARTESIAN_POINT('Ctrl Pts',(-13.4959168042934,21.1471953136209,
0.));
#241940=CARTESIAN_POINT('Ctrl Pts',(-13.4959168042934,21.1471953136209,
12.));
#241941=CARTESIAN_POINT('Ctrl Pts',(-13.4988442384491,21.1728750584175,
0.));
#241942=CARTESIAN_POINT('Ctrl Pts',(-13.4988442384491,21.1728750584175,
12.));
#241943=CARTESIAN_POINT('Ctrl Pts',(-13.5017201056088,21.1986390835828,
0.));
#241944=CARTESIAN_POINT('Ctrl Pts',(-13.5017201056088,21.1986390835828,
12.));
#241945=CARTESIAN_POINT('Ctrl Pts',(-13.5045440957404,21.2244869429332,
0.));
#241946=CARTESIAN_POINT('Ctrl Pts',(-13.5045440957404,21.2244869429332,
12.));
#241947=CARTESIAN_POINT('Ctrl Pts',(-13.5073159019452,21.250418192743,0.));
#241948=CARTESIAN_POINT('Ctrl Pts',(-13.5073159019452,21.250418192743,12.));
#241949=CARTESIAN_POINT('Ctrl Pts',(-13.5100352209205,21.2764323924442,
0.));
#241950=CARTESIAN_POINT('Ctrl Pts',(-13.5100352209205,21.2764323924442,
12.));
#241951=CARTESIAN_POINT('Ctrl Pts',(-13.5127017534971,21.3025291054235,
0.));
#241952=CARTESIAN_POINT('Ctrl Pts',(-13.5127017534971,21.3025291054235,
12.));
#241953=CARTESIAN_POINT('Ctrl Pts',(-13.5153152050555,21.328707899634,0.));
#241954=CARTESIAN_POINT('Ctrl Pts',(-13.5153152050555,21.328707899634,12.));
#241955=CARTESIAN_POINT('Ctrl Pts',(-13.5178752862466,21.3549683486222,
0.));
#241956=CARTESIAN_POINT('Ctrl Pts',(-13.5178752862466,21.3549683486222,
12.));
#241957=CARTESIAN_POINT('Ctrl Pts',(-13.5203817122504,21.3813100304973,
0.));
#241958=CARTESIAN_POINT('Ctrl Pts',(-13.5203817122504,21.3813100304973,
12.));
#241959=CARTESIAN_POINT('Ctrl Pts',(-13.5228342013516,21.4077325259324,
0.));
#241960=CARTESIAN_POINT('Ctrl Pts',(-13.5228342013516,21.4077325259324,
12.));
#241961=CARTESIAN_POINT('Ctrl Pts',(-13.5252324737802,21.4342354165259,
0.));
#241962=CARTESIAN_POINT('Ctrl Pts',(-13.5252324737802,21.4342354165259,
12.));
#241963=CARTESIAN_POINT('Ctrl Pts',(-13.5275762503555,21.4608182828697,
0.));
#241964=CARTESIAN_POINT('Ctrl Pts',(-13.5275762503555,21.4608182828697,
12.));
#241965=CARTESIAN_POINT('Ctrl Pts',(-13.5298652514355,21.4874807030468,
0.));
#241966=CARTESIAN_POINT('Ctrl Pts',(-13.5298652514355,21.4874807030468,
12.));
#241967=CARTESIAN_POINT('Ctrl Pts',(-13.5320991952138,21.5142222501666,
0.));
#241968=CARTESIAN_POINT('Ctrl Pts',(-13.5320991952138,21.5142222501666,
12.));
#241969=CARTESIAN_POINT('Ctrl Pts',(-13.5342777983215,21.5410424932503,
0.));
#241970=CARTESIAN_POINT('Ctrl Pts',(-13.5342777983215,21.5410424932503,
12.));
#241971=CARTESIAN_POINT('Ctrl Pts',(-13.536400779028,21.5679410019001,0.));
#241972=CARTESIAN_POINT('Ctrl Pts',(-13.536400779028,21.5679410019001,12.));
#241973=CARTESIAN_POINT('Ctrl Pts',(-13.5384678597195,21.5949173499013,
0.));
#241974=CARTESIAN_POINT('Ctrl Pts',(-13.5384678597195,21.5949173499013,
12.));
#241975=CARTESIAN_POINT('Ctrl Pts',(-13.5404787697792,21.6219711193946,
0.));
#241976=CARTESIAN_POINT('Ctrl Pts',(-13.5404787697792,21.6219711193946,
12.));
#241977=CARTESIAN_POINT('Ctrl Pts',(-13.5424332480699,21.6491019044648,
0.));
#241978=CARTESIAN_POINT('Ctrl Pts',(-13.5424332480699,21.6491019044648,
12.));
#241979=CARTESIAN_POINT('Ctrl Pts',(-13.5443310461526,21.6763093157699,
0.));
#241980=CARTESIAN_POINT('Ctrl Pts',(-13.5443310461526,21.6763093157699,
12.));
#241981=CARTESIAN_POINT('Ctrl Pts',(-13.5461719295048,21.7035929822955,
0.));
#241982=CARTESIAN_POINT('Ctrl Pts',(-13.5461719295048,21.7035929822955,
12.));
#241983=CARTESIAN_POINT('Ctrl Pts',(-13.5479556704481,21.7309525412281,
0.));
#241984=CARTESIAN_POINT('Ctrl Pts',(-13.5479556704481,21.7309525412281,
12.));
#241985=CARTESIAN_POINT('Ctrl Pts',(-13.5496820422211,21.7583876294554,
0.));
#241986=CARTESIAN_POINT('Ctrl Pts',(-13.5496820422211,21.7583876294554,
12.));
#241987=CARTESIAN_POINT('Ctrl Pts',(-13.551350812725,21.7858978745865,0.));
#241988=CARTESIAN_POINT('Ctrl Pts',(-13.551350812725,21.7858978745865,12.));
#241989=CARTESIAN_POINT('Ctrl Pts',(-13.5529617381573,21.8134828857967,
0.));
#241990=CARTESIAN_POINT('Ctrl Pts',(-13.5529617381573,21.8134828857967,
12.));
#241991=CARTESIAN_POINT('Ctrl Pts',(-13.5545145573031,21.8411422456075,
0.));
#241992=CARTESIAN_POINT('Ctrl Pts',(-13.5545145573031,21.8411422456075,
12.));
#241993=CARTESIAN_POINT('Ctrl Pts',(-13.5560089839385,21.8688754989365,
0.));
#241994=CARTESIAN_POINT('Ctrl Pts',(-13.5560089839385,21.8688754989365,
12.));
#241995=CARTESIAN_POINT('Ctrl Pts',(-13.5574447178424,21.8966821688824,
0.));
#241996=CARTESIAN_POINT('Ctrl Pts',(-13.5574447178424,21.8966821688824,
12.));
#241997=CARTESIAN_POINT('Ctrl Pts',(-13.5588214586604,21.9245617765769,
0.));
#241998=CARTESIAN_POINT('Ctrl Pts',(-13.5588214586604,21.9245617765769,
12.));
#241999=CARTESIAN_POINT('Ctrl Pts',(-13.5601389185257,21.9525138592813,
0.));
#242000=CARTESIAN_POINT('Ctrl Pts',(-13.5601389185257,21.9525138592813,
12.));
#242001=CARTESIAN_POINT('Ctrl Pts',(-13.5613968357561,21.9805379899168,
0.));
#242002=CARTESIAN_POINT('Ctrl Pts',(-13.5613968357561,21.9805379899168,
12.));
#242003=CARTESIAN_POINT('Ctrl Pts',(-13.5625949868333,22.0086337943449,
0.));
#242004=CARTESIAN_POINT('Ctrl Pts',(-13.5625949868333,22.0086337943449,
12.));
#242005=CARTESIAN_POINT('Ctrl Pts',(-13.5637332022473,22.0368009736295,
0.));
#242006=CARTESIAN_POINT('Ctrl Pts',(-13.5637332022473,22.0368009736295,
12.));
#242007=CARTESIAN_POINT('Ctrl Pts',(-13.5648113689033,22.0650393089609,
0.));
#242008=CARTESIAN_POINT('Ctrl Pts',(-13.5648113689033,22.0650393089609,
12.));
#242009=CARTESIAN_POINT('Ctrl Pts',(-13.5658294169284,22.0933486464593,
0.));
#242010=CARTESIAN_POINT('Ctrl Pts',(-13.5658294169284,22.0933486464593,
12.));
#242011=CARTESIAN_POINT('Ctrl Pts',(-13.5667873105359,22.1217288871975,
0.));
#242012=CARTESIAN_POINT('Ctrl Pts',(-13.5667873105359,22.1217288871975,
12.));
#242013=CARTESIAN_POINT('Ctrl Pts',(-13.5675054919061,22.1444897575194,
0.));
#242014=CARTESIAN_POINT('Ctrl Pts',(-13.5675054919061,22.1444897575194,
12.));
#242015=CARTESIAN_POINT('Ctrl Pts',(-13.5680170531805,22.1615922805008,
0.));
#242016=CARTESIAN_POINT('Ctrl Pts',(-13.5680170531805,22.1615922805008,
12.));
#242017=CARTESIAN_POINT('Ctrl Pts',(-13.5683460612942,22.1730081264608,
0.));
#242018=CARTESIAN_POINT('Ctrl Pts',(-13.5683460612942,22.1730081264608,
12.));
#242019=CARTESIAN_POINT('Ctrl Pts',(-13.5685075571671,22.1787195904339,
0.));
#242020=CARTESIAN_POINT('Ctrl Pts',(-13.5685075571671,22.1787195904339,
12.));
#242021=CARTESIAN_POINT('',(-13.5685075571671,22.1787195904339,0.));
#242022=CARTESIAN_POINT('Ctrl Pts',(-12.7689476255363,18.5896416359912,
0.));
#242023=CARTESIAN_POINT('Ctrl Pts',(-12.7689524524483,18.5896460962964,
0.));
#242024=CARTESIAN_POINT('Ctrl Pts',(-12.768986426692,18.5896919669165,0.));
#242025=CARTESIAN_POINT('Ctrl Pts',(-12.769110348199,18.589871621843,0.));
#242026=CARTESIAN_POINT('Ctrl Pts',(-12.7694215127919,18.5903328777227,
0.));
#242027=CARTESIAN_POINT('Ctrl Pts',(-12.7700520897173,18.5912775137806,
0.));
#242028=CARTESIAN_POINT('Ctrl Pts',(-12.7709195951156,18.5925859134579,
0.));
#242029=CARTESIAN_POINT('Ctrl Pts',(-12.7720142287172,18.5942490615407,
0.));
#242030=CARTESIAN_POINT('Ctrl Pts',(-12.7733231262108,18.5962551167772,
0.));
#242031=CARTESIAN_POINT('Ctrl Pts',(-12.7748328937638,18.598591752595,0.));
#242032=CARTESIAN_POINT('Ctrl Pts',(-12.7765325225081,18.6012488486709,
0.));
#242033=CARTESIAN_POINT('Ctrl Pts',(-12.7784139605066,18.6042190183704,
0.));
#242034=CARTESIAN_POINT('Ctrl Pts',(-12.7804705387658,18.6074961535723,
0.));
#242035=CARTESIAN_POINT('Ctrl Pts',(-12.7826959526925,18.6110744826219,
0.));
#242036=CARTESIAN_POINT('Ctrl Pts',(-12.7850831657901,18.6149475565188,
0.));
#242037=CARTESIAN_POINT('Ctrl Pts',(-12.7876249657834,18.6191087624752,
0.));
#242038=CARTESIAN_POINT('Ctrl Pts',(-12.7903142925234,18.6235516265575,
0.));
#242039=CARTESIAN_POINT('Ctrl Pts',(-12.7931447451555,18.6282702819371,
0.));
#242040=CARTESIAN_POINT('Ctrl Pts',(-12.7961106222251,18.6332595057006,
0.));
#242041=CARTESIAN_POINT('Ctrl Pts',(-12.7992066625264,18.63851447924,0.));
#242042=CARTESIAN_POINT('Ctrl Pts',(-12.8024278770152,18.6440306327456,
0.));
#242043=CARTESIAN_POINT('Ctrl Pts',(-12.805769331162,18.6498034438986,0.));
#242044=CARTESIAN_POINT('Ctrl Pts',(-12.8092261933858,18.6558284825773,
0.));
#242045=CARTESIAN_POINT('Ctrl Pts',(-12.8127937909631,18.6621014624746,
0.));
#242046=CARTESIAN_POINT('Ctrl Pts',(-12.8164676687362,18.6686182952799,
0.));
#242047=CARTESIAN_POINT('Ctrl Pts',(-12.8202436318474,18.6753751301092,
0.));
#242048=CARTESIAN_POINT('Ctrl Pts',(-12.8241176980017,18.6823683094139,
0.));
#242049=CARTESIAN_POINT('Ctrl Pts',(-12.8280860635231,18.6895943376171,
0.));
#242050=CARTESIAN_POINT('Ctrl Pts',(-12.8321450599789,18.6970498410172,
0.));
#242051=CARTESIAN_POINT('Ctrl Pts',(-12.8362911280361,18.7047315436294,
0.));
#242052=CARTESIAN_POINT('Ctrl Pts',(-12.8405208263431,18.7126362754445,
0.));
#242053=CARTESIAN_POINT('Ctrl Pts',(-12.8448308329494,18.7207609737702,
0.));
#242054=CARTESIAN_POINT('Ctrl Pts',(-12.8492179511591,18.7291026886554,
0.));
#242055=CARTESIAN_POINT('Ctrl Pts',(-12.8536791086316,18.7376585820854,
0.));
#242056=CARTESIAN_POINT('Ctrl Pts',(-12.8582113455646,18.7464259171251,
0.));
#242057=CARTESIAN_POINT('Ctrl Pts',(-12.8628118054171,18.7554020493887,
0.));
#242058=CARTESIAN_POINT('Ctrl Pts',(-12.8674777239653,18.7645844169564,
0.));
#242059=CARTESIAN_POINT('Ctrl Pts',(-12.872206421181,18.7739705329022,0.));
#242060=CARTESIAN_POINT('Ctrl Pts',(-12.8769952998095,18.7835579840477,
0.));
#242061=CARTESIAN_POINT('Ctrl Pts',(-12.8818418427475,18.7933444285868,
0.));
#242062=CARTESIAN_POINT('Ctrl Pts',(-12.8867436109546,18.8033275941943,
0.));
#242063=CARTESIAN_POINT('Ctrl Pts',(-12.8916982409935,18.813505275782,0.));
#242064=CARTESIAN_POINT('Ctrl Pts',(-12.8967034410755,18.8238753319128,
0.));
#242065=CARTESIAN_POINT('Ctrl Pts',(-12.9017569871738,18.834435681259,0.));
#242066=CARTESIAN_POINT('Ctrl Pts',(-12.9068567191854,18.8451842990984,
0.));
#242067=CARTESIAN_POINT('Ctrl Pts',(-12.9120005369063,18.8561192136198,
0.));
#242068=CARTESIAN_POINT('Ctrl Pts',(-12.9171863977045,18.8672385038326,
0.));
#242069=CARTESIAN_POINT('Ctrl Pts',(-12.9224123144982,18.8785402977527,
0.));
#242070=CARTESIAN_POINT('Ctrl Pts',(-12.9276763536373,18.8900227704889,
0.));
#242071=CARTESIAN_POINT('Ctrl Pts',(-12.9329766328185,18.9016841423403,
0.));
#242072=CARTESIAN_POINT('Ctrl Pts',(-12.9383113190375,18.9135226769465,
0.));
#242073=CARTESIAN_POINT('Ctrl Pts',(-12.9436786266105,18.9255366795195,
0.));
#242074=CARTESIAN_POINT('Ctrl Pts',(-12.9490768151821,18.9377244950435,
0.));
#242075=CARTESIAN_POINT('Ctrl Pts',(-12.9545041877377,18.9500845064715,
0.));
#242076=CARTESIAN_POINT('Ctrl Pts',(-12.9599590886319,18.9626151329229,
0.));
#242077=CARTESIAN_POINT('Ctrl Pts',(-12.9654399021869,18.9753148284475,
0.));
#242078=CARTESIAN_POINT('Ctrl Pts',(-12.9709450512747,18.9881820807585,
0.));
#242079=CARTESIAN_POINT('Ctrl Pts',(-12.9764729959205,19.0012154099791,
0.));
#242080=CARTESIAN_POINT('Ctrl Pts',(-12.9820222318716,19.0144133673348,
0.));
#242081=CARTESIAN_POINT('Ctrl Pts',(-12.9875912893003,19.0277745339908,
0.));
#242082=CARTESIAN_POINT('Ctrl Pts',(-12.9931787316515,19.0412975200398,
0.));
#242083=CARTESIAN_POINT('Ctrl Pts',(-12.9987831544502,19.0549809634355,
0.));
#242084=CARTESIAN_POINT('Ctrl Pts',(-13.0044031841381,19.0688235289437,
0.));
#242085=CARTESIAN_POINT('Ctrl Pts',(-13.0100374768785,19.0828239070482,
0.));
#242086=CARTESIAN_POINT('Ctrl Pts',(-13.0156847176093,19.0969808131225,
0.));
#242087=CARTESIAN_POINT('Ctrl Pts',(-13.0213436191326,19.1112929866308,
0.));
#242088=CARTESIAN_POINT('Ctrl Pts',(-13.0270129211976,19.1257591903099,
0.));
#242089=CARTESIAN_POINT('Ctrl Pts',(-13.0326913895841,19.1403782093389,
0.));
#242090=CARTESIAN_POINT('Ctrl Pts',(-13.0383778152072,19.1551488505233,
0.));
#242091=CARTESIAN_POINT('Ctrl Pts',(-13.0440710133775,19.1700699416625,
0.));
#242092=CARTESIAN_POINT('Ctrl Pts',(-13.0497698230442,19.1851403308825,
0.));
#242093=CARTESIAN_POINT('Ctrl Pts',(-13.0554731060537,19.2003588859771,
0.));
#242094=CARTESIAN_POINT('Ctrl Pts',(-13.0611797463913,19.2157244937141,
0.));
#242095=CARTESIAN_POINT('Ctrl Pts',(-13.0668886494791,19.2312360592031,
0.));
#242096=CARTESIAN_POINT('Ctrl Pts',(-13.0725987415856,19.2468925053988,
0.));
#242097=CARTESIAN_POINT('Ctrl Pts',(-13.0783089692118,19.2626927725596,
0.));
#242098=CARTESIAN_POINT('Ctrl Pts',(-13.0840182984949,19.2786358177198,
0.));
#242099=CARTESIAN_POINT('Ctrl Pts',(-13.089725714597,19.2947206141246,0.));
#242100=CARTESIAN_POINT('Ctrl Pts',(-13.095430221148,19.3109461507358,0.));
#242101=CARTESIAN_POINT('Ctrl Pts',(-13.1011308397592,19.3273114318268,
0.));
#242102=CARTESIAN_POINT('Ctrl Pts',(-13.1068266095186,19.3438154765395,
0.));
#242103=CARTESIAN_POINT('Ctrl Pts',(-13.1125165865021,19.3604573184516,
0.));
#242104=CARTESIAN_POINT('Ctrl Pts',(-13.118199843271,19.3772360051093,0.));
#242105=CARTESIAN_POINT('Ctrl Pts',(-13.1238754684177,19.3941505976267,
0.));
#242106=CARTESIAN_POINT('Ctrl Pts',(-13.1295425661635,19.4112001703561,
0.));
#242107=CARTESIAN_POINT('Ctrl Pts',(-13.1352002559439,19.4283838105265,
0.));
#242108=CARTESIAN_POINT('Ctrl Pts',(-13.140847672006,19.4457006178875,0.));
#242109=CARTESIAN_POINT('Ctrl Pts',(-13.1464839629966,19.463149704325,0.));
#242110=CARTESIAN_POINT('Ctrl Pts',(-13.1521082915846,19.4807301935256,
0.));
#242111=CARTESIAN_POINT('Ctrl Pts',(-13.1577198341238,19.498441220707,0.));
#242112=CARTESIAN_POINT('Ctrl Pts',(-13.1633177803097,19.5162819323207,
0.));
#242113=CARTESIAN_POINT('Ctrl Pts',(-13.1689013328432,19.5342514857564,
0.));
#242114=CARTESIAN_POINT('Ctrl Pts',(-13.1744697070918,19.5523490490254,
0.));
#242115=CARTESIAN_POINT('Ctrl Pts',(-13.1800221307683,19.5705738004682,
0.));
#242116=CARTESIAN_POINT('Ctrl Pts',(-13.1855578436479,19.5889249285351,
0.));
#242117=CARTESIAN_POINT('Ctrl Pts',(-13.1910760972818,19.6074016315421,
0.));
#242118=CARTESIAN_POINT('Ctrl Pts',(-13.196576154715,19.6260031174244,0.));
#242119=CARTESIAN_POINT('Ctrl Pts',(-13.202057290206,19.6447286034764,0.));
#242120=CARTESIAN_POINT('Ctrl Pts',(-13.2075187889522,19.6635773160924,
0.));
#242121=CARTESIAN_POINT('Ctrl Pts',(-13.2129599468478,19.6825484905812,
0.));
#242122=CARTESIAN_POINT('Ctrl Pts',(-13.2183800702431,19.7016413709678,
0.));
#242123=CARTESIAN_POINT('Ctrl Pts',(-13.2237784757065,19.7208552097867,
0.));
#242124=CARTESIAN_POINT('Ctrl Pts',(-13.2291544897902,19.7401892678701,
0.));
#242125=CARTESIAN_POINT('Ctrl Pts',(-13.2345074487968,19.7596428141176,
0.));
#242126=CARTESIAN_POINT('Ctrl Pts',(-13.239836698568,19.7792151253297,0.));
#242127=CARTESIAN_POINT('Ctrl Pts',(-13.2451415942809,19.7989054860501,
0.));
#242128=CARTESIAN_POINT('Ctrl Pts',(-13.2504215002458,19.8187131883919,
0.));
#242129=CARTESIAN_POINT('Ctrl Pts',(-13.2556757897085,19.8386375318632,
0.));
#242130=CARTESIAN_POINT('Ctrl Pts',(-13.2609038446525,19.8586778231711,
0.));
#242131=CARTESIAN_POINT('Ctrl Pts',(-13.2661050556128,19.8788333760571,
0.));
#242132=CARTESIAN_POINT('Ctrl Pts',(-13.2712788215015,19.8991035111739,
0.));
#242133=CARTESIAN_POINT('Ctrl Pts',(-13.2764245494354,19.9194875559419,
0.));
#242134=CARTESIAN_POINT('Ctrl Pts',(-13.2815416545663,19.9399848444019,
0.));
#242135=CARTESIAN_POINT('Ctrl Pts',(-13.2866295599152,19.9605947170589,
0.));
#242136=CARTESIAN_POINT('Ctrl Pts',(-13.2916876962098,19.9813165207174,
0.));
#242137=CARTESIAN_POINT('Ctrl Pts',(-13.296715501731,20.0021496083742,0.));
#242138=CARTESIAN_POINT('Ctrl Pts',(-13.3017124221639,20.0230933391039,
0.));
#242139=CARTESIAN_POINT('Ctrl Pts',(-13.3066779104515,20.0441470779345,
0.));
#242140=CARTESIAN_POINT('Ctrl Pts',(-13.3116114266514,20.0653101957188,
0.));
#242141=CARTESIAN_POINT('Ctrl Pts',(-13.3165124377963,20.0865820689883,
0.));
#242142=CARTESIAN_POINT('Ctrl Pts',(-13.3213804177588,20.1079620798377,
0.));
#242143=CARTESIAN_POINT('Ctrl Pts',(-13.3262148471228,20.1294496158405,
0.));
#242144=CARTESIAN_POINT('Ctrl Pts',(-13.3310152130565,20.1510440699477,
0.));
#242145=CARTESIAN_POINT('Ctrl Pts',(-13.3357810091903,20.1727448403818,
0.));
#242146=CARTESIAN_POINT('Ctrl Pts',(-13.3405117354969,20.1945513305233,
0.));
#242147=CARTESIAN_POINT('Ctrl Pts',(-13.3452068981763,20.2164629487855,
0.));
#242148=CARTESIAN_POINT('Ctrl Pts',(-13.3498660095382,20.2384791085354,
0.));
#242149=CARTESIAN_POINT('Ctrl Pts',(-13.3544885878886,20.2605992280117,
0.));
#242150=CARTESIAN_POINT('Ctrl Pts',(-13.3590741574194,20.2828227302337,
0.));
#242151=CARTESIAN_POINT('Ctrl Pts',(-13.3636222481017,20.3051490429049,
0.));
#242152=CARTESIAN_POINT('Ctrl Pts',(-13.3681323955828,20.3275775983032,
0.));
#242153=CARTESIAN_POINT('Ctrl Pts',(-13.3726041410869,20.3501078331818,
0.));
#242154=CARTESIAN_POINT('Ctrl Pts',(-13.377037031319,20.3727391887187,0.));
#242155=CARTESIAN_POINT('Ctrl Pts',(-13.3814306183721,20.3954711104504,
0.));
#242156=CARTESIAN_POINT('Ctrl Pts',(-13.3857844596387,20.4183030482002,
0.));
#242157=CARTESIAN_POINT('Ctrl Pts',(-13.3900981177254,20.4412344560007,
0.));
#242158=CARTESIAN_POINT('Ctrl Pts',(-13.3943711603739,20.4642647920038,
0.));
#242159=CARTESIAN_POINT('Ctrl Pts',(-13.3986031603716,20.4873935184041,
0.));
#242160=CARTESIAN_POINT('Ctrl Pts',(-13.4027936954529,20.5106201013755,
0.));
#242161=CARTESIAN_POINT('Ctrl Pts',(-13.4069423482076,20.5339440109957,
0.));
#242162=CARTESIAN_POINT('Ctrl Pts',(-13.4110487059912,20.557364721164,0.));
#242163=CARTESIAN_POINT('Ctrl Pts',(-13.4151123608411,20.5808817095155,
0.));
#242164=CARTESIAN_POINT('Ctrl Pts',(-13.4191329093932,20.6044944573151,
0.));
#242165=CARTESIAN_POINT('Ctrl Pts',(-13.4231099528178,20.6282024494234,
0.));
#242166=CARTESIAN_POINT('Ctrl Pts',(-13.427043096765,20.6520051742867,0.));
#242167=CARTESIAN_POINT('Ctrl Pts',(-13.4309319513119,20.6759021239102,
0.));
#242168=CARTESIAN_POINT('Ctrl Pts',(-13.4347761309154,20.6998927938288,
0.));
#242169=CARTESIAN_POINT('Ctrl Pts',(-13.4385752543663,20.7239766830675,
0.));
#242170=CARTESIAN_POINT('Ctrl Pts',(-13.4423289447561,20.7481532941014,
0.));
#242171=CARTESIAN_POINT('Ctrl Pts',(-13.4460368293689,20.7724221327609,
0.));
#242172=CARTESIAN_POINT('Ctrl Pts',(-13.4496985395637,20.7967827081228,
0.));
#242173=CARTESIAN_POINT('Ctrl Pts',(-13.4533137106667,20.821234532398,0.));
#242174=CARTESIAN_POINT('Ctrl Pts',(-13.4568819818631,20.8457771208083,
0.));
#242175=CARTESIAN_POINT('Ctrl Pts',(-13.4604029960983,20.8704099914641,
0.));
#242176=CARTESIAN_POINT('Ctrl Pts',(-13.4638763999725,20.8951326652158,
0.));
#242177=CARTESIAN_POINT('Ctrl Pts',(-13.4673018437717,20.9199446657583,
0.));
#242178=CARTESIAN_POINT('Ctrl Pts',(-13.4706789815166,20.9448455197557,
0.));
#242179=CARTESIAN_POINT('Ctrl Pts',(-13.4740074710086,20.9698347569476,
0.));
#242180=CARTESIAN_POINT('Ctrl Pts',(-13.4772869738879,20.9949119102592,
0.));
#242181=CARTESIAN_POINT('Ctrl Pts',(-13.4805171556822,21.0200765158884,
0.));
#242182=CARTESIAN_POINT('Ctrl Pts',(-13.4836976858912,21.0453281134245,
0.));
#242183=CARTESIAN_POINT('Ctrl Pts',(-13.4868282377191,21.0706662455199,
0.));
#242184=CARTESIAN_POINT('Ctrl Pts',(-13.4899084877717,21.0960904575046,
0.));
#242185=CARTESIAN_POINT('Ctrl Pts',(-13.4929381157778,21.1216002970207,
0.));
#242186=CARTESIAN_POINT('Ctrl Pts',(-13.4959168042934,21.1471953136209,
0.));
#242187=CARTESIAN_POINT('Ctrl Pts',(-13.4988442384491,21.1728750584175,
0.));
#242188=CARTESIAN_POINT('Ctrl Pts',(-13.5017201056088,21.1986390835828,
0.));
#242189=CARTESIAN_POINT('Ctrl Pts',(-13.5045440957404,21.2244869429332,
0.));
#242190=CARTESIAN_POINT('Ctrl Pts',(-13.5073159019452,21.250418192743,0.));
#242191=CARTESIAN_POINT('Ctrl Pts',(-13.5100352209205,21.2764323924442,
0.));
#242192=CARTESIAN_POINT('Ctrl Pts',(-13.5127017534971,21.3025291054235,
0.));
#242193=CARTESIAN_POINT('Ctrl Pts',(-13.5153152050555,21.328707899634,0.));
#242194=CARTESIAN_POINT('Ctrl Pts',(-13.5178752862466,21.3549683486222,
0.));
#242195=CARTESIAN_POINT('Ctrl Pts',(-13.5203817122504,21.3813100304973,
0.));
#242196=CARTESIAN_POINT('Ctrl Pts',(-13.5228342013516,21.4077325259324,
0.));
#242197=CARTESIAN_POINT('Ctrl Pts',(-13.5252324737802,21.4342354165259,
0.));
#242198=CARTESIAN_POINT('Ctrl Pts',(-13.5275762503555,21.4608182828697,
0.));
#242199=CARTESIAN_POINT('Ctrl Pts',(-13.5298652514355,21.4874807030468,
0.));
#242200=CARTESIAN_POINT('Ctrl Pts',(-13.5320991952138,21.5142222501666,
0.));
#242201=CARTESIAN_POINT('Ctrl Pts',(-13.5342777983215,21.5410424932503,
0.));
#242202=CARTESIAN_POINT('Ctrl Pts',(-13.536400779028,21.5679410019001,0.));
#242203=CARTESIAN_POINT('Ctrl Pts',(-13.5384678597195,21.5949173499013,
0.));
#242204=CARTESIAN_POINT('Ctrl Pts',(-13.5404787697792,21.6219711193946,
0.));
#242205=CARTESIAN_POINT('Ctrl Pts',(-13.5424332480699,21.6491019044648,
0.));
#242206=CARTESIAN_POINT('Ctrl Pts',(-13.5443310461526,21.6763093157699,
0.));
#242207=CARTESIAN_POINT('Ctrl Pts',(-13.5461719295048,21.7035929822955,
0.));
#242208=CARTESIAN_POINT('Ctrl Pts',(-13.5479556704481,21.7309525412281,
0.));
#242209=CARTESIAN_POINT('Ctrl Pts',(-13.5496820422211,21.7583876294554,
0.));
#242210=CARTESIAN_POINT('Ctrl Pts',(-13.551350812725,21.7858978745865,0.));
#242211=CARTESIAN_POINT('Ctrl Pts',(-13.5529617381573,21.8134828857967,
0.));
#242212=CARTESIAN_POINT('Ctrl Pts',(-13.5545145573031,21.8411422456075,
0.));
#242213=CARTESIAN_POINT('Ctrl Pts',(-13.5560089839385,21.8688754989365,
0.));
#242214=CARTESIAN_POINT('Ctrl Pts',(-13.5574447178424,21.8966821688824,
0.));
#242215=CARTESIAN_POINT('Ctrl Pts',(-13.5588214586604,21.9245617765769,
0.));
#242216=CARTESIAN_POINT('Ctrl Pts',(-13.5601389185257,21.9525138592813,
0.));
#242217=CARTESIAN_POINT('Ctrl Pts',(-13.5613968357561,21.9805379899168,
0.));
#242218=CARTESIAN_POINT('Ctrl Pts',(-13.5625949868333,22.0086337943449,
0.));
#242219=CARTESIAN_POINT('Ctrl Pts',(-13.5637332022473,22.0368009736295,
0.));
#242220=CARTESIAN_POINT('Ctrl Pts',(-13.5648113689033,22.0650393089609,
0.));
#242221=CARTESIAN_POINT('Ctrl Pts',(-13.5658294169284,22.0933486464593,
0.));
#242222=CARTESIAN_POINT('Ctrl Pts',(-13.5667873105359,22.1217288871975,
0.));
#242223=CARTESIAN_POINT('Ctrl Pts',(-13.5675054919061,22.1444897575194,
0.));
#242224=CARTESIAN_POINT('Ctrl Pts',(-13.5680170531805,22.1615922805008,
0.));
#242225=CARTESIAN_POINT('Ctrl Pts',(-13.5683460612942,22.1730081264608,
0.));
#242226=CARTESIAN_POINT('Ctrl Pts',(-13.5685075571671,22.1787195904339,
0.));
#242227=CARTESIAN_POINT('',(-13.5685075571671,22.1787195904339,12.));
#242228=CARTESIAN_POINT('Ctrl Pts',(-13.5685075571671,22.1787195904339,
12.));
#242229=CARTESIAN_POINT('Ctrl Pts',(-13.5683460612942,22.1730081264608,
12.));
#242230=CARTESIAN_POINT('Ctrl Pts',(-13.5680170531805,22.1615922805008,
12.));
#242231=CARTESIAN_POINT('Ctrl Pts',(-13.5675054919061,22.1444897575194,
12.));
#242232=CARTESIAN_POINT('Ctrl Pts',(-13.5667873105359,22.1217288871975,
12.));
#242233=CARTESIAN_POINT('Ctrl Pts',(-13.5658294169284,22.0933486464593,
12.));
#242234=CARTESIAN_POINT('Ctrl Pts',(-13.5648113689033,22.0650393089609,
12.));
#242235=CARTESIAN_POINT('Ctrl Pts',(-13.5637332022473,22.0368009736295,
12.));
#242236=CARTESIAN_POINT('Ctrl Pts',(-13.5625949868333,22.0086337943449,
12.));
#242237=CARTESIAN_POINT('Ctrl Pts',(-13.5613968357561,21.9805379899168,
12.));
#242238=CARTESIAN_POINT('Ctrl Pts',(-13.5601389185257,21.9525138592813,
12.));
#242239=CARTESIAN_POINT('Ctrl Pts',(-13.5588214586604,21.9245617765769,
12.));
#242240=CARTESIAN_POINT('Ctrl Pts',(-13.5574447178424,21.8966821688824,
12.));
#242241=CARTESIAN_POINT('Ctrl Pts',(-13.5560089839385,21.8688754989365,
12.));
#242242=CARTESIAN_POINT('Ctrl Pts',(-13.5545145573031,21.8411422456075,
12.));
#242243=CARTESIAN_POINT('Ctrl Pts',(-13.5529617381573,21.8134828857967,
12.));
#242244=CARTESIAN_POINT('Ctrl Pts',(-13.551350812725,21.7858978745865,12.));
#242245=CARTESIAN_POINT('Ctrl Pts',(-13.5496820422211,21.7583876294554,
12.));
#242246=CARTESIAN_POINT('Ctrl Pts',(-13.5479556704481,21.7309525412281,
12.));
#242247=CARTESIAN_POINT('Ctrl Pts',(-13.5461719295048,21.7035929822955,
12.));
#242248=CARTESIAN_POINT('Ctrl Pts',(-13.5443310461526,21.6763093157699,
12.));
#242249=CARTESIAN_POINT('Ctrl Pts',(-13.5424332480699,21.6491019044648,
12.));
#242250=CARTESIAN_POINT('Ctrl Pts',(-13.5404787697792,21.6219711193946,
12.));
#242251=CARTESIAN_POINT('Ctrl Pts',(-13.5384678597195,21.5949173499013,
12.));
#242252=CARTESIAN_POINT('Ctrl Pts',(-13.536400779028,21.5679410019001,12.));
#242253=CARTESIAN_POINT('Ctrl Pts',(-13.5342777983215,21.5410424932503,
12.));
#242254=CARTESIAN_POINT('Ctrl Pts',(-13.5320991952138,21.5142222501666,
12.));
#242255=CARTESIAN_POINT('Ctrl Pts',(-13.5298652514355,21.4874807030468,
12.));
#242256=CARTESIAN_POINT('Ctrl Pts',(-13.5275762503555,21.4608182828697,
12.));
#242257=CARTESIAN_POINT('Ctrl Pts',(-13.5252324737802,21.4342354165259,
12.));
#242258=CARTESIAN_POINT('Ctrl Pts',(-13.5228342013516,21.4077325259324,
12.));
#242259=CARTESIAN_POINT('Ctrl Pts',(-13.5203817122504,21.3813100304973,
12.));
#242260=CARTESIAN_POINT('Ctrl Pts',(-13.5178752862466,21.3549683486222,
12.));
#242261=CARTESIAN_POINT('Ctrl Pts',(-13.5153152050555,21.328707899634,12.));
#242262=CARTESIAN_POINT('Ctrl Pts',(-13.5127017534971,21.3025291054235,
12.));
#242263=CARTESIAN_POINT('Ctrl Pts',(-13.5100352209205,21.2764323924442,
12.));
#242264=CARTESIAN_POINT('Ctrl Pts',(-13.5073159019452,21.250418192743,12.));
#242265=CARTESIAN_POINT('Ctrl Pts',(-13.5045440957404,21.2244869429332,
12.));
#242266=CARTESIAN_POINT('Ctrl Pts',(-13.5017201056088,21.1986390835828,
12.));
#242267=CARTESIAN_POINT('Ctrl Pts',(-13.4988442384491,21.1728750584175,
12.));
#242268=CARTESIAN_POINT('Ctrl Pts',(-13.4959168042934,21.1471953136209,
12.));
#242269=CARTESIAN_POINT('Ctrl Pts',(-13.4929381157778,21.1216002970207,
12.));
#242270=CARTESIAN_POINT('Ctrl Pts',(-13.4899084877717,21.0960904575046,
12.));
#242271=CARTESIAN_POINT('Ctrl Pts',(-13.4868282377191,21.0706662455199,
12.));
#242272=CARTESIAN_POINT('Ctrl Pts',(-13.4836976858912,21.0453281134245,
12.));
#242273=CARTESIAN_POINT('Ctrl Pts',(-13.4805171556822,21.0200765158884,
12.));
#242274=CARTESIAN_POINT('Ctrl Pts',(-13.4772869738879,20.9949119102592,
12.));
#242275=CARTESIAN_POINT('Ctrl Pts',(-13.4740074710086,20.9698347569476,
12.));
#242276=CARTESIAN_POINT('Ctrl Pts',(-13.4706789815166,20.9448455197557,
12.));
#242277=CARTESIAN_POINT('Ctrl Pts',(-13.4673018437717,20.9199446657583,
12.));
#242278=CARTESIAN_POINT('Ctrl Pts',(-13.4638763999725,20.8951326652158,
12.));
#242279=CARTESIAN_POINT('Ctrl Pts',(-13.4604029960983,20.8704099914641,
12.));
#242280=CARTESIAN_POINT('Ctrl Pts',(-13.4568819818631,20.8457771208083,
12.));
#242281=CARTESIAN_POINT('Ctrl Pts',(-13.4533137106667,20.821234532398,12.));
#242282=CARTESIAN_POINT('Ctrl Pts',(-13.4496985395637,20.7967827081228,
12.));
#242283=CARTESIAN_POINT('Ctrl Pts',(-13.4460368293689,20.7724221327609,
12.));
#242284=CARTESIAN_POINT('Ctrl Pts',(-13.4423289447561,20.7481532941014,
12.));
#242285=CARTESIAN_POINT('Ctrl Pts',(-13.4385752543663,20.7239766830675,
12.));
#242286=CARTESIAN_POINT('Ctrl Pts',(-13.4347761309154,20.6998927938288,
12.));
#242287=CARTESIAN_POINT('Ctrl Pts',(-13.4309319513119,20.6759021239102,
12.));
#242288=CARTESIAN_POINT('Ctrl Pts',(-13.427043096765,20.6520051742867,12.));
#242289=CARTESIAN_POINT('Ctrl Pts',(-13.4231099528178,20.6282024494234,
12.));
#242290=CARTESIAN_POINT('Ctrl Pts',(-13.4191329093932,20.6044944573151,
12.));
#242291=CARTESIAN_POINT('Ctrl Pts',(-13.4151123608411,20.5808817095155,
12.));
#242292=CARTESIAN_POINT('Ctrl Pts',(-13.4110487059912,20.557364721164,12.));
#242293=CARTESIAN_POINT('Ctrl Pts',(-13.4069423482076,20.5339440109957,
12.));
#242294=CARTESIAN_POINT('Ctrl Pts',(-13.4027936954529,20.5106201013755,
12.));
#242295=CARTESIAN_POINT('Ctrl Pts',(-13.3986031603716,20.4873935184041,
12.));
#242296=CARTESIAN_POINT('Ctrl Pts',(-13.3943711603739,20.4642647920038,
12.));
#242297=CARTESIAN_POINT('Ctrl Pts',(-13.3900981177254,20.4412344560007,
12.));
#242298=CARTESIAN_POINT('Ctrl Pts',(-13.3857844596387,20.4183030482002,
12.));
#242299=CARTESIAN_POINT('Ctrl Pts',(-13.3814306183721,20.3954711104504,
12.));
#242300=CARTESIAN_POINT('Ctrl Pts',(-13.377037031319,20.3727391887187,12.));
#242301=CARTESIAN_POINT('Ctrl Pts',(-13.3726041410869,20.3501078331818,
12.));
#242302=CARTESIAN_POINT('Ctrl Pts',(-13.3681323955828,20.3275775983032,
12.));
#242303=CARTESIAN_POINT('Ctrl Pts',(-13.3636222481017,20.3051490429049,
12.));
#242304=CARTESIAN_POINT('Ctrl Pts',(-13.3590741574194,20.2828227302337,
12.));
#242305=CARTESIAN_POINT('Ctrl Pts',(-13.3544885878886,20.2605992280117,
12.));
#242306=CARTESIAN_POINT('Ctrl Pts',(-13.3498660095382,20.2384791085354,
12.));
#242307=CARTESIAN_POINT('Ctrl Pts',(-13.3452068981763,20.2164629487855,
12.));
#242308=CARTESIAN_POINT('Ctrl Pts',(-13.3405117354969,20.1945513305233,
12.));
#242309=CARTESIAN_POINT('Ctrl Pts',(-13.3357810091903,20.1727448403818,
12.));
#242310=CARTESIAN_POINT('Ctrl Pts',(-13.3310152130565,20.1510440699477,
12.));
#242311=CARTESIAN_POINT('Ctrl Pts',(-13.3262148471228,20.1294496158405,
12.));
#242312=CARTESIAN_POINT('Ctrl Pts',(-13.3213804177588,20.1079620798377,
12.));
#242313=CARTESIAN_POINT('Ctrl Pts',(-13.3165124377963,20.0865820689883,
12.));
#242314=CARTESIAN_POINT('Ctrl Pts',(-13.3116114266514,20.0653101957188,
12.));
#242315=CARTESIAN_POINT('Ctrl Pts',(-13.3066779104515,20.0441470779345,
12.));
#242316=CARTESIAN_POINT('Ctrl Pts',(-13.3017124221639,20.0230933391039,
12.));
#242317=CARTESIAN_POINT('Ctrl Pts',(-13.296715501731,20.0021496083742,12.));
#242318=CARTESIAN_POINT('Ctrl Pts',(-13.2916876962098,19.9813165207174,
12.));
#242319=CARTESIAN_POINT('Ctrl Pts',(-13.2866295599152,19.9605947170589,
12.));
#242320=CARTESIAN_POINT('Ctrl Pts',(-13.2815416545663,19.9399848444019,
12.));
#242321=CARTESIAN_POINT('Ctrl Pts',(-13.2764245494354,19.9194875559419,
12.));
#242322=CARTESIAN_POINT('Ctrl Pts',(-13.2712788215015,19.8991035111739,
12.));
#242323=CARTESIAN_POINT('Ctrl Pts',(-13.2661050556128,19.8788333760571,
12.));
#242324=CARTESIAN_POINT('Ctrl Pts',(-13.2609038446525,19.8586778231711,
12.));
#242325=CARTESIAN_POINT('Ctrl Pts',(-13.2556757897085,19.8386375318632,
12.));
#242326=CARTESIAN_POINT('Ctrl Pts',(-13.2504215002458,19.8187131883919,
12.));
#242327=CARTESIAN_POINT('Ctrl Pts',(-13.2451415942809,19.7989054860501,
12.));
#242328=CARTESIAN_POINT('Ctrl Pts',(-13.239836698568,19.7792151253297,12.));
#242329=CARTESIAN_POINT('Ctrl Pts',(-13.2345074487968,19.7596428141176,
12.));
#242330=CARTESIAN_POINT('Ctrl Pts',(-13.2291544897902,19.7401892678701,
12.));
#242331=CARTESIAN_POINT('Ctrl Pts',(-13.2237784757065,19.7208552097867,
12.));
#242332=CARTESIAN_POINT('Ctrl Pts',(-13.2183800702431,19.7016413709678,
12.));
#242333=CARTESIAN_POINT('Ctrl Pts',(-13.2129599468478,19.6825484905812,
12.));
#242334=CARTESIAN_POINT('Ctrl Pts',(-13.2075187889522,19.6635773160924,
12.));
#242335=CARTESIAN_POINT('Ctrl Pts',(-13.202057290206,19.6447286034764,12.));
#242336=CARTESIAN_POINT('Ctrl Pts',(-13.196576154715,19.6260031174244,12.));
#242337=CARTESIAN_POINT('Ctrl Pts',(-13.1910760972818,19.6074016315421,
12.));
#242338=CARTESIAN_POINT('Ctrl Pts',(-13.1855578436479,19.5889249285351,
12.));
#242339=CARTESIAN_POINT('Ctrl Pts',(-13.1800221307683,19.5705738004682,
12.));
#242340=CARTESIAN_POINT('Ctrl Pts',(-13.1744697070918,19.5523490490254,
12.));
#242341=CARTESIAN_POINT('Ctrl Pts',(-13.1689013328432,19.5342514857564,
12.));
#242342=CARTESIAN_POINT('Ctrl Pts',(-13.1633177803097,19.5162819323207,
12.));
#242343=CARTESIAN_POINT('Ctrl Pts',(-13.1577198341238,19.498441220707,12.));
#242344=CARTESIAN_POINT('Ctrl Pts',(-13.1521082915846,19.4807301935256,
12.));
#242345=CARTESIAN_POINT('Ctrl Pts',(-13.1464839629966,19.463149704325,12.));
#242346=CARTESIAN_POINT('Ctrl Pts',(-13.140847672006,19.4457006178875,12.));
#242347=CARTESIAN_POINT('Ctrl Pts',(-13.1352002559439,19.4283838105265,
12.));
#242348=CARTESIAN_POINT('Ctrl Pts',(-13.1295425661635,19.4112001703561,
12.));
#242349=CARTESIAN_POINT('Ctrl Pts',(-13.1238754684177,19.3941505976267,
12.));
#242350=CARTESIAN_POINT('Ctrl Pts',(-13.118199843271,19.3772360051093,12.));
#242351=CARTESIAN_POINT('Ctrl Pts',(-13.1125165865021,19.3604573184516,
12.));
#242352=CARTESIAN_POINT('Ctrl Pts',(-13.1068266095186,19.3438154765395,
12.));
#242353=CARTESIAN_POINT('Ctrl Pts',(-13.1011308397592,19.3273114318268,
12.));
#242354=CARTESIAN_POINT('Ctrl Pts',(-13.095430221148,19.3109461507358,12.));
#242355=CARTESIAN_POINT('Ctrl Pts',(-13.089725714597,19.2947206141246,12.));
#242356=CARTESIAN_POINT('Ctrl Pts',(-13.0840182984949,19.2786358177198,
12.));
#242357=CARTESIAN_POINT('Ctrl Pts',(-13.0783089692118,19.2626927725596,
12.));
#242358=CARTESIAN_POINT('Ctrl Pts',(-13.0725987415856,19.2468925053988,
12.));
#242359=CARTESIAN_POINT('Ctrl Pts',(-13.0668886494791,19.2312360592031,
12.));
#242360=CARTESIAN_POINT('Ctrl Pts',(-13.0611797463913,19.2157244937141,
12.));
#242361=CARTESIAN_POINT('Ctrl Pts',(-13.0554731060537,19.2003588859771,
12.));
#242362=CARTESIAN_POINT('Ctrl Pts',(-13.0497698230442,19.1851403308825,
12.));
#242363=CARTESIAN_POINT('Ctrl Pts',(-13.0440710133775,19.1700699416625,
12.));
#242364=CARTESIAN_POINT('Ctrl Pts',(-13.0383778152072,19.1551488505233,
12.));
#242365=CARTESIAN_POINT('Ctrl Pts',(-13.0326913895841,19.1403782093389,
12.));
#242366=CARTESIAN_POINT('Ctrl Pts',(-13.0270129211976,19.1257591903099,
12.));
#242367=CARTESIAN_POINT('Ctrl Pts',(-13.0213436191326,19.1112929866308,
12.));
#242368=CARTESIAN_POINT('Ctrl Pts',(-13.0156847176093,19.0969808131225,
12.));
#242369=CARTESIAN_POINT('Ctrl Pts',(-13.0100374768785,19.0828239070482,
12.));
#242370=CARTESIAN_POINT('Ctrl Pts',(-13.0044031841381,19.0688235289437,
12.));
#242371=CARTESIAN_POINT('Ctrl Pts',(-12.9987831544502,19.0549809634355,
12.));
#242372=CARTESIAN_POINT('Ctrl Pts',(-12.9931787316515,19.0412975200398,
12.));
#242373=CARTESIAN_POINT('Ctrl Pts',(-12.9875912893003,19.0277745339908,
12.));
#242374=CARTESIAN_POINT('Ctrl Pts',(-12.9820222318716,19.0144133673348,
12.));
#242375=CARTESIAN_POINT('Ctrl Pts',(-12.9764729959205,19.0012154099791,
12.));
#242376=CARTESIAN_POINT('Ctrl Pts',(-12.9709450512747,18.9881820807585,
12.));
#242377=CARTESIAN_POINT('Ctrl Pts',(-12.9654399021869,18.9753148284475,
12.));
#242378=CARTESIAN_POINT('Ctrl Pts',(-12.9599590886319,18.9626151329229,
12.));
#242379=CARTESIAN_POINT('Ctrl Pts',(-12.9545041877377,18.9500845064715,
12.));
#242380=CARTESIAN_POINT('Ctrl Pts',(-12.9490768151821,18.9377244950435,
12.));
#242381=CARTESIAN_POINT('Ctrl Pts',(-12.9436786266105,18.9255366795195,
12.));
#242382=CARTESIAN_POINT('Ctrl Pts',(-12.9383113190375,18.9135226769465,
12.));
#242383=CARTESIAN_POINT('Ctrl Pts',(-12.9329766328185,18.9016841423403,
12.));
#242384=CARTESIAN_POINT('Ctrl Pts',(-12.9276763536373,18.8900227704889,
12.));
#242385=CARTESIAN_POINT('Ctrl Pts',(-12.9224123144982,18.8785402977527,
12.));
#242386=CARTESIAN_POINT('Ctrl Pts',(-12.9171863977045,18.8672385038326,
12.));
#242387=CARTESIAN_POINT('Ctrl Pts',(-12.9120005369063,18.8561192136198,
12.));
#242388=CARTESIAN_POINT('Ctrl Pts',(-12.9068567191854,18.8451842990984,
12.));
#242389=CARTESIAN_POINT('Ctrl Pts',(-12.9017569871738,18.834435681259,12.));
#242390=CARTESIAN_POINT('Ctrl Pts',(-12.8967034410755,18.8238753319128,
12.));
#242391=CARTESIAN_POINT('Ctrl Pts',(-12.8916982409935,18.813505275782,12.));
#242392=CARTESIAN_POINT('Ctrl Pts',(-12.8867436109546,18.8033275941943,
12.));
#242393=CARTESIAN_POINT('Ctrl Pts',(-12.8818418427475,18.7933444285868,
12.));
#242394=CARTESIAN_POINT('Ctrl Pts',(-12.8769952998095,18.7835579840477,
12.));
#242395=CARTESIAN_POINT('Ctrl Pts',(-12.872206421181,18.7739705329022,12.));
#242396=CARTESIAN_POINT('Ctrl Pts',(-12.8674777239653,18.7645844169564,
12.));
#242397=CARTESIAN_POINT('Ctrl Pts',(-12.8628118054171,18.7554020493887,
12.));
#242398=CARTESIAN_POINT('Ctrl Pts',(-12.8582113455646,18.7464259171251,
12.));
#242399=CARTESIAN_POINT('Ctrl Pts',(-12.8536791086316,18.7376585820854,
12.));
#242400=CARTESIAN_POINT('Ctrl Pts',(-12.8492179511591,18.7291026886554,
12.));
#242401=CARTESIAN_POINT('Ctrl Pts',(-12.8448308329494,18.7207609737702,
12.));
#242402=CARTESIAN_POINT('Ctrl Pts',(-12.8405208263431,18.7126362754445,
12.));
#242403=CARTESIAN_POINT('Ctrl Pts',(-12.8362911280361,18.7047315436294,
12.));
#242404=CARTESIAN_POINT('Ctrl Pts',(-12.8321450599789,18.6970498410172,
12.));
#242405=CARTESIAN_POINT('Ctrl Pts',(-12.8280860635231,18.6895943376171,
12.));
#242406=CARTESIAN_POINT('Ctrl Pts',(-12.8241176980017,18.6823683094139,
12.));
#242407=CARTESIAN_POINT('Ctrl Pts',(-12.8202436318474,18.6753751301092,
12.));
#242408=CARTESIAN_POINT('Ctrl Pts',(-12.8164676687362,18.6686182952799,
12.));
#242409=CARTESIAN_POINT('Ctrl Pts',(-12.8127937909631,18.6621014624746,
12.));
#242410=CARTESIAN_POINT('Ctrl Pts',(-12.8092261933858,18.6558284825773,
12.));
#242411=CARTESIAN_POINT('Ctrl Pts',(-12.805769331162,18.6498034438986,12.));
#242412=CARTESIAN_POINT('Ctrl Pts',(-12.8024278770152,18.6440306327456,
12.));
#242413=CARTESIAN_POINT('Ctrl Pts',(-12.7992066625264,18.63851447924,12.));
#242414=CARTESIAN_POINT('Ctrl Pts',(-12.7961106222251,18.6332595057006,
12.));
#242415=CARTESIAN_POINT('Ctrl Pts',(-12.7931447451555,18.6282702819371,
12.));
#242416=CARTESIAN_POINT('Ctrl Pts',(-12.7903142925234,18.6235516265575,
12.));
#242417=CARTESIAN_POINT('Ctrl Pts',(-12.7876249657834,18.6191087624752,
12.));
#242418=CARTESIAN_POINT('Ctrl Pts',(-12.7850831657901,18.6149475565188,
12.));
#242419=CARTESIAN_POINT('Ctrl Pts',(-12.7826959526925,18.6110744826219,
12.));
#242420=CARTESIAN_POINT('Ctrl Pts',(-12.7804705387658,18.6074961535723,
12.));
#242421=CARTESIAN_POINT('Ctrl Pts',(-12.7784139605066,18.6042190183704,
12.));
#242422=CARTESIAN_POINT('Ctrl Pts',(-12.7765325225081,18.6012488486709,
12.));
#242423=CARTESIAN_POINT('Ctrl Pts',(-12.7748328937638,18.598591752595,12.));
#242424=CARTESIAN_POINT('Ctrl Pts',(-12.7733231262108,18.5962551167772,
12.));
#242425=CARTESIAN_POINT('Ctrl Pts',(-12.7720142287172,18.5942490615407,
12.));
#242426=CARTESIAN_POINT('Ctrl Pts',(-12.7709195951156,18.5925859134579,
12.));
#242427=CARTESIAN_POINT('Ctrl Pts',(-12.7700520897173,18.5912775137806,
12.));
#242428=CARTESIAN_POINT('Ctrl Pts',(-12.7694215127919,18.5903328777227,
12.));
#242429=CARTESIAN_POINT('Ctrl Pts',(-12.769110348199,18.589871621843,12.));
#242430=CARTESIAN_POINT('Ctrl Pts',(-12.768986426692,18.5896919669165,12.));
#242431=CARTESIAN_POINT('Ctrl Pts',(-12.7689524524483,18.5896460962964,
12.));
#242432=CARTESIAN_POINT('Ctrl Pts',(-12.7689476255363,18.5896416359912,
12.));
#242433=CARTESIAN_POINT('',(-13.5685075571671,22.1787195904339,0.));
#242434=CARTESIAN_POINT('Origin',(-7.17139709155223,20.2687213152502,0.));
#242435=CARTESIAN_POINT('',(-7.52250298901264,21.2610617890679,12.));
#242436=CARTESIAN_POINT('',(-3.58569854577611,10.1343606576251,12.));
#242437=CARTESIAN_POINT('',(-7.52250298901264,21.2610617890679,0.));
#242438=CARTESIAN_POINT('',(-7.52250298901264,21.2610617890679,0.));
#242439=CARTESIAN_POINT('',(-3.58569854577611,10.1343606576251,0.));
#242440=CARTESIAN_POINT('Ctrl Pts',(-12.4230808101438,22.8400320311648,
0.));
#242441=CARTESIAN_POINT('Ctrl Pts',(-12.4230808101438,22.8400320311648,
12.));
#242442=CARTESIAN_POINT('Ctrl Pts',(-12.418215285186,22.8370364396459,0.));
#242443=CARTESIAN_POINT('Ctrl Pts',(-12.418215285186,22.8370364396459,12.));
#242444=CARTESIAN_POINT('Ctrl Pts',(-12.4084933766347,22.8310435872747,
0.));
#242445=CARTESIAN_POINT('Ctrl Pts',(-12.4084933766347,22.8310435872747,
12.));
#242446=CARTESIAN_POINT('Ctrl Pts',(-12.3939379378998,22.8220493007173,
0.));
#242447=CARTESIAN_POINT('Ctrl Pts',(-12.3939379378998,22.8220493007173,
12.));
#242448=CARTESIAN_POINT('Ctrl Pts',(-12.374585536673,22.81004690224,0.));
#242449=CARTESIAN_POINT('Ctrl Pts',(-12.374585536673,22.81004690224,12.));
#242450=CARTESIAN_POINT('Ctrl Pts',(-12.3504864740319,22.795027221673,0.));
#242451=CARTESIAN_POINT('Ctrl Pts',(-12.3504864740319,22.795027221673,12.));
#242452=CARTESIAN_POINT('Ctrl Pts',(-12.3264788926075,22.7799908974768,
0.));
#242453=CARTESIAN_POINT('Ctrl Pts',(-12.3264788926075,22.7799908974768,
12.));
#242454=CARTESIAN_POINT('Ctrl Pts',(-12.3025628601792,22.764938010105,0.));
#242455=CARTESIAN_POINT('Ctrl Pts',(-12.3025628601792,22.764938010105,12.));
#242456=CARTESIAN_POINT('Ctrl Pts',(-12.2787384750742,22.7498686970069,
0.));
#242457=CARTESIAN_POINT('Ctrl Pts',(-12.2787384750742,22.7498686970069,
12.));
#242458=CARTESIAN_POINT('Ctrl Pts',(-12.2550058702395,22.7347831655287,
0.));
#242459=CARTESIAN_POINT('Ctrl Pts',(-12.2550058702395,22.7347831655287,
12.));
#242460=CARTESIAN_POINT('Ctrl Pts',(-12.2313652198061,22.7196817119374,
0.));
#242461=CARTESIAN_POINT('Ctrl Pts',(-12.2313652198061,22.7196817119374,
12.));
#242462=CARTESIAN_POINT('Ctrl Pts',(-12.2078167360284,22.7045647168747,
0.));
#242463=CARTESIAN_POINT('Ctrl Pts',(-12.2078167360284,22.7045647168747,
12.));
#242464=CARTESIAN_POINT('Ctrl Pts',(-12.1843606579262,22.6894326205037,
0.));
#242465=CARTESIAN_POINT('Ctrl Pts',(-12.1843606579262,22.6894326205037,
12.));
#242466=CARTESIAN_POINT('Ctrl Pts',(-12.1609972423099,22.6742859034944,
0.));
#242467=CARTESIAN_POINT('Ctrl Pts',(-12.1609972423099,22.6742859034944,
12.));
#242468=CARTESIAN_POINT('Ctrl Pts',(-12.1377267537145,22.6591250653965,
0.));
#242469=CARTESIAN_POINT('Ctrl Pts',(-12.1377267537145,22.6591250653965,
12.));
#242470=CARTESIAN_POINT('Ctrl Pts',(-12.1145494550383,22.6439506046605,
0.));
#242471=CARTESIAN_POINT('Ctrl Pts',(-12.1145494550383,22.6439506046605,
12.));
#242472=CARTESIAN_POINT('Ctrl Pts',(-12.0914655972823,22.6287629967056,
0.));
#242473=CARTESIAN_POINT('Ctrl Pts',(-12.0914655972823,22.6287629967056,
12.));
#242474=CARTESIAN_POINT('Ctrl Pts',(-12.0684754113862,22.6135626764898,
0.));
#242475=CARTESIAN_POINT('Ctrl Pts',(-12.0684754113862,22.6135626764898,
12.));
#242476=CARTESIAN_POINT('Ctrl Pts',(-12.0455791139128,22.5983500505644,
0.));
#242477=CARTESIAN_POINT('Ctrl Pts',(-12.0455791139128,22.5983500505644,
12.));
#242478=CARTESIAN_POINT('Ctrl Pts',(-12.0227769113127,22.5831255061282,
0.));
#242479=CARTESIAN_POINT('Ctrl Pts',(-12.0227769113127,22.5831255061282,
12.));
#242480=CARTESIAN_POINT('Ctrl Pts',(-12.0000690046695,22.5678894211181,
0.));
#242481=CARTESIAN_POINT('Ctrl Pts',(-12.0000690046695,22.5678894211181,
12.));
#242482=CARTESIAN_POINT('Ctrl Pts',(-11.9774555943496,22.5526421741158,
0.));
#242483=CARTESIAN_POINT('Ctrl Pts',(-11.9774555943496,22.5526421741158,
12.));
#242484=CARTESIAN_POINT('Ctrl Pts',(-11.9549368843997,22.5373841537307,
0.));
#242485=CARTESIAN_POINT('Ctrl Pts',(-11.9549368843997,22.5373841537307,
12.));
#242486=CARTESIAN_POINT('Ctrl Pts',(-11.9325130877803,22.5221157697883,
0.));
#242487=CARTESIAN_POINT('Ctrl Pts',(-11.9325130877803,22.5221157697883,
12.));
#242488=CARTESIAN_POINT('Ctrl Pts',(-11.9101844254557,22.5068374513973,
0.));
#242489=CARTESIAN_POINT('Ctrl Pts',(-11.9101844254557,22.5068374513973,
12.));
#242490=CARTESIAN_POINT('Ctrl Pts',(-11.8879511239943,22.4915496418485,
0.));
#242491=CARTESIAN_POINT('Ctrl Pts',(-11.8879511239943,22.4915496418485,
12.));
#242492=CARTESIAN_POINT('Ctrl Pts',(-11.8658134137019,22.4762527946702,
0.));
#242493=CARTESIAN_POINT('Ctrl Pts',(-11.8658134137019,22.4762527946702,
12.));
#242494=CARTESIAN_POINT('Ctrl Pts',(-11.8437715264487,22.4609473690471,
0.));
#242495=CARTESIAN_POINT('Ctrl Pts',(-11.8437715264487,22.4609473690471,
12.));
#242496=CARTESIAN_POINT('Ctrl Pts',(-11.8218256937889,22.4456338258735,
0.));
#242497=CARTESIAN_POINT('Ctrl Pts',(-11.8218256937889,22.4456338258735,
12.));
#242498=CARTESIAN_POINT('Ctrl Pts',(-11.7999761445173,22.430312622646,0.));
#242499=CARTESIAN_POINT('Ctrl Pts',(-11.7999761445173,22.430312622646,12.));
#242500=CARTESIAN_POINT('Ctrl Pts',(-11.7782231042039,22.4149842125008,
0.));
#242501=CARTESIAN_POINT('Ctrl Pts',(-11.7782231042039,22.4149842125008,
12.));
#242502=CARTESIAN_POINT('Ctrl Pts',(-11.7565667964764,22.3996490469191,
0.));
#242503=CARTESIAN_POINT('Ctrl Pts',(-11.7565667964764,22.3996490469191,
12.));
#242504=CARTESIAN_POINT('Ctrl Pts',(-11.7350074437961,22.3843075773899,
0.));
#242505=CARTESIAN_POINT('Ctrl Pts',(-11.7350074437961,22.3843075773899,
12.));
#242506=CARTESIAN_POINT('Ctrl Pts',(-11.7135452684532,22.3689602575491,
0.));
#242507=CARTESIAN_POINT('Ctrl Pts',(-11.7135452684532,22.3689602575491,
12.));
#242508=CARTESIAN_POINT('Ctrl Pts',(-11.6921804934056,22.3536075450029,
0.));
#242509=CARTESIAN_POINT('Ctrl Pts',(-11.6921804934056,22.3536075450029,
12.));
#242510=CARTESIAN_POINT('Ctrl Pts',(-11.6709133432985,22.3382499035619,
0.));
#242511=CARTESIAN_POINT('Ctrl Pts',(-11.6709133432985,22.3382499035619,
12.));
#242512=CARTESIAN_POINT('Ctrl Pts',(-11.6497440449857,22.3228878043976,
0.));
#242513=CARTESIAN_POINT('Ctrl Pts',(-11.6497440449857,22.3228878043976,
12.));
#242514=CARTESIAN_POINT('Ctrl Pts',(-11.6286728270009,22.3075217249049,
0.));
#242515=CARTESIAN_POINT('Ctrl Pts',(-11.6286728270009,22.3075217249049,
12.));
#242516=CARTESIAN_POINT('Ctrl Pts',(-11.6076999192357,22.2921521480356,
0.));
#242517=CARTESIAN_POINT('Ctrl Pts',(-11.6076999192357,22.2921521480356,
12.));
#242518=CARTESIAN_POINT('Ctrl Pts',(-11.5868255525188,22.2767795614348,
0.));
#242519=CARTESIAN_POINT('Ctrl Pts',(-11.5868255525188,22.2767795614348,
12.));
#242520=CARTESIAN_POINT('Ctrl Pts',(-11.5660499582403,22.2614044566898,
0.));
#242521=CARTESIAN_POINT('Ctrl Pts',(-11.5660499582403,22.2614044566898,
12.));
#242522=CARTESIAN_POINT('Ctrl Pts',(-11.5453733679121,22.2460273284654,
0.));
#242523=CARTESIAN_POINT('Ctrl Pts',(-11.5453733679121,22.2460273284654,
12.));
#242524=CARTESIAN_POINT('Ctrl Pts',(-11.5247960128477,22.2306486738901,
0.));
#242525=CARTESIAN_POINT('Ctrl Pts',(-11.5247960128477,22.2306486738901,
12.));
#242526=CARTESIAN_POINT('Ctrl Pts',(-11.5043181244242,22.2152689931022,
0.));
#242527=CARTESIAN_POINT('Ctrl Pts',(-11.5043181244242,22.2152689931022,
12.));
#242528=CARTESIAN_POINT('Ctrl Pts',(-11.483939934259,22.1998887896436,0.));
#242529=CARTESIAN_POINT('Ctrl Pts',(-11.483939934259,22.1998887896436,12.));
#242530=CARTESIAN_POINT('Ctrl Pts',(-11.463661674411,22.184508570917,0.));
#242531=CARTESIAN_POINT('Ctrl Pts',(-11.463661674411,22.184508570917,12.));
#242532=CARTESIAN_POINT('Ctrl Pts',(-11.443483577557,22.1691288486096,0.));
#242533=CARTESIAN_POINT('Ctrl Pts',(-11.443483577557,22.1691288486096,12.));
#242534=CARTESIAN_POINT('Ctrl Pts',(-11.4234058771742,22.1537501391487,
0.));
#242535=CARTESIAN_POINT('Ctrl Pts',(-11.4234058771742,22.1537501391487,
12.));
#242536=CARTESIAN_POINT('Ctrl Pts',(-11.4034288076908,22.1383729640964,
0.));
#242537=CARTESIAN_POINT('Ctrl Pts',(-11.4034288076908,22.1383729640964,
12.));
#242538=CARTESIAN_POINT('Ctrl Pts',(-11.3835526044256,22.1229978500186,
0.));
#242539=CARTESIAN_POINT('Ctrl Pts',(-11.3835526044256,22.1229978500186,
12.));
#242540=CARTESIAN_POINT('Ctrl Pts',(-11.3637775035367,22.1076253283979,
0.));
#242541=CARTESIAN_POINT('Ctrl Pts',(-11.3637775035367,22.1076253283979,
12.));
#242542=CARTESIAN_POINT('Ctrl Pts',(-11.3441037419553,22.0922559355294,
0.));
#242543=CARTESIAN_POINT('Ctrl Pts',(-11.3441037419553,22.0922559355294,
12.));
#242544=CARTESIAN_POINT('Ctrl Pts',(-11.3245315573168,22.0768902124267,
0.));
#242545=CARTESIAN_POINT('Ctrl Pts',(-11.3245315573168,22.0768902124267,
12.));
#242546=CARTESIAN_POINT('Ctrl Pts',(-11.3050611878771,22.0615287047179,
0.));
#242547=CARTESIAN_POINT('Ctrl Pts',(-11.3050611878771,22.0615287047179,
12.));
#242548=CARTESIAN_POINT('Ctrl Pts',(-11.2856928724374,22.046171962566,0.));
#242549=CARTESIAN_POINT('Ctrl Pts',(-11.2856928724374,22.046171962566,12.));
#242550=CARTESIAN_POINT('Ctrl Pts',(-11.2664268504206,22.030820540835,0.));
#242551=CARTESIAN_POINT('Ctrl Pts',(-11.2664268504206,22.030820540835,12.));
#242552=CARTESIAN_POINT('Ctrl Pts',(-11.2472633619275,22.0154749992363,
0.));
#242553=CARTESIAN_POINT('Ctrl Pts',(-11.2472633619275,22.0154749992363,
12.));
#242554=CARTESIAN_POINT('Ctrl Pts',(-11.2282026477896,22.0001359024839,
0.));
#242555=CARTESIAN_POINT('Ctrl Pts',(-11.2282026477896,22.0001359024839,
12.));
#242556=CARTESIAN_POINT('Ctrl Pts',(-11.2092449496125,21.9848038204439,
0.));
#242557=CARTESIAN_POINT('Ctrl Pts',(-11.2092449496125,21.9848038204439,
12.));
#242558=CARTESIAN_POINT('Ctrl Pts',(-11.190390509811,21.9694793282914,0.));
#242559=CARTESIAN_POINT('Ctrl Pts',(-11.190390509811,21.9694793282914,12.));
#242560=CARTESIAN_POINT('Ctrl Pts',(-11.1716395716376,21.9541630066506,
0.));
#242561=CARTESIAN_POINT('Ctrl Pts',(-11.1716395716376,21.9541630066506,
12.));
#242562=CARTESIAN_POINT('Ctrl Pts',(-11.1529923792003,21.9388554416439,
0.));
#242563=CARTESIAN_POINT('Ctrl Pts',(-11.1529923792003,21.9388554416439,
12.));
#242564=CARTESIAN_POINT('Ctrl Pts',(-11.1344491774741,21.923557224952,0.));
#242565=CARTESIAN_POINT('Ctrl Pts',(-11.1344491774741,21.923557224952,12.));
#242566=CARTESIAN_POINT('Ctrl Pts',(-11.1160102123024,21.9082689538688,
0.));
#242567=CARTESIAN_POINT('Ctrl Pts',(-11.1160102123024,21.9082689538688,
12.));
#242568=CARTESIAN_POINT('Ctrl Pts',(-11.0976757303944,21.8929912313608,
0.));
#242569=CARTESIAN_POINT('Ctrl Pts',(-11.0976757303944,21.8929912313608,
12.));
#242570=CARTESIAN_POINT('Ctrl Pts',(-11.0794459793057,21.877724666119,0.));
#242571=CARTESIAN_POINT('Ctrl Pts',(-11.0794459793057,21.877724666119,12.));
#242572=CARTESIAN_POINT('Ctrl Pts',(-11.0613212074363,21.8624698726318,
0.));
#242573=CARTESIAN_POINT('Ctrl Pts',(-11.0613212074363,21.8624698726318,
12.));
#242574=CARTESIAN_POINT('Ctrl Pts',(-11.0433016640807,21.8472274713103,
0.));
#242575=CARTESIAN_POINT('Ctrl Pts',(-11.0433016640807,21.8472274713103,
12.));
#242576=CARTESIAN_POINT('Ctrl Pts',(-11.0253875994598,21.8319980886033,
0.));
#242577=CARTESIAN_POINT('Ctrl Pts',(-11.0253875994598,21.8319980886033,
12.));
#242578=CARTESIAN_POINT('Ctrl Pts',(-11.0075792647477,21.8167823571168,
0.));
#242579=CARTESIAN_POINT('Ctrl Pts',(-11.0075792647477,21.8167823571168,
12.));
#242580=CARTESIAN_POINT('Ctrl Pts',(-10.9898769120912,21.8015809157301,
0.));
#242581=CARTESIAN_POINT('Ctrl Pts',(-10.9898769120912,21.8015809157301,
12.));
#242582=CARTESIAN_POINT('Ctrl Pts',(-10.9722807946156,21.7863944097141,
0.));
#242583=CARTESIAN_POINT('Ctrl Pts',(-10.9722807946156,21.7863944097141,
12.));
#242584=CARTESIAN_POINT('Ctrl Pts',(-10.9547911664455,21.7712234908464,
0.));
#242585=CARTESIAN_POINT('Ctrl Pts',(-10.9547911664455,21.7712234908464,
12.));
#242586=CARTESIAN_POINT('Ctrl Pts',(-10.9374082827444,21.7560688175247,
0.));
#242587=CARTESIAN_POINT('Ctrl Pts',(-10.9374082827444,21.7560688175247,
12.));
#242588=CARTESIAN_POINT('Ctrl Pts',(-10.9201323997384,21.7409310548797,
0.));
#242589=CARTESIAN_POINT('Ctrl Pts',(-10.9201323997384,21.7409310548797,
12.));
#242590=CARTESIAN_POINT('Ctrl Pts',(-10.902963774734,21.7258108748873,0.));
#242591=CARTESIAN_POINT('Ctrl Pts',(-10.902963774734,21.7258108748873,12.));
#242592=CARTESIAN_POINT('Ctrl Pts',(-10.8859026661293,21.7107089564825,
0.));
#242593=CARTESIAN_POINT('Ctrl Pts',(-10.8859026661293,21.7107089564825,
12.));
#242594=CARTESIAN_POINT('Ctrl Pts',(-10.8689493334095,21.6956259856672,
0.));
#242595=CARTESIAN_POINT('Ctrl Pts',(-10.8689493334095,21.6956259856672,
12.));
#242596=CARTESIAN_POINT('Ctrl Pts',(-10.8521040371835,21.6805626556467,
0.));
#242597=CARTESIAN_POINT('Ctrl Pts',(-10.8521040371835,21.6805626556467,
12.));
#242598=CARTESIAN_POINT('Ctrl Pts',(-10.8353670392272,21.6655196669732,
0.));
#242599=CARTESIAN_POINT('Ctrl Pts',(-10.8353670392272,21.6655196669732,
12.));
#242600=CARTESIAN_POINT('Ctrl Pts',(-10.8187386025136,21.6504977276866,
0.));
#242601=CARTESIAN_POINT('Ctrl Pts',(-10.8187386025136,21.6504977276866,
12.));
#242602=CARTESIAN_POINT('Ctrl Pts',(-10.8022189912369,21.6354975534557,
0.));
#242603=CARTESIAN_POINT('Ctrl Pts',(-10.8022189912369,21.6354975534557,
12.));
#242604=CARTESIAN_POINT('Ctrl Pts',(-10.7858084708261,21.6205198677173,
0.));
#242605=CARTESIAN_POINT('Ctrl Pts',(-10.7858084708261,21.6205198677173,
12.));
#242606=CARTESIAN_POINT('Ctrl Pts',(-10.7695073079552,21.6055654018176,
0.));
#242607=CARTESIAN_POINT('Ctrl Pts',(-10.7695073079552,21.6055654018176,
12.));
#242608=CARTESIAN_POINT('Ctrl Pts',(-10.7533157705941,21.5906348951743,
0.));
#242609=CARTESIAN_POINT('Ctrl Pts',(-10.7533157705941,21.5906348951743,
12.));
#242610=CARTESIAN_POINT('Ctrl Pts',(-10.7372341280467,21.5757290954371,
0.));
#242611=CARTESIAN_POINT('Ctrl Pts',(-10.7372341280467,21.5757290954371,
12.));
#242612=CARTESIAN_POINT('Ctrl Pts',(-10.7212626509816,21.5608487586468,
0.));
#242613=CARTESIAN_POINT('Ctrl Pts',(-10.7212626509816,21.5608487586468,
12.));
#242614=CARTESIAN_POINT('Ctrl Pts',(-10.7054016114571,21.5459946493955,
0.));
#242615=CARTESIAN_POINT('Ctrl Pts',(-10.7054016114571,21.5459946493955,
12.));
#242616=CARTESIAN_POINT('Ctrl Pts',(-10.689651282929,21.5311675409807,0.));
#242617=CARTESIAN_POINT('Ctrl Pts',(-10.689651282929,21.5311675409807,12.));
#242618=CARTESIAN_POINT('Ctrl Pts',(-10.6740119402834,21.51636821558,0.));
#242619=CARTESIAN_POINT('Ctrl Pts',(-10.6740119402834,21.51636821558,12.));
#242620=CARTESIAN_POINT('Ctrl Pts',(-10.6584838598939,21.5015974644449,
0.));
#242621=CARTESIAN_POINT('Ctrl Pts',(-10.6584838598939,21.5015974644449,
12.));
#242622=CARTESIAN_POINT('Ctrl Pts',(-10.6430673196607,21.4868560880889,
0.));
#242623=CARTESIAN_POINT('Ctrl Pts',(-10.6430673196607,21.4868560880889,
12.));
#242624=CARTESIAN_POINT('Ctrl Pts',(-10.6277625990456,21.4721448964766,
0.));
#242625=CARTESIAN_POINT('Ctrl Pts',(-10.6277625990456,21.4721448964766,
12.));
#242626=CARTESIAN_POINT('Ctrl Pts',(-10.6125699790961,21.4574647092097,
0.));
#242627=CARTESIAN_POINT('Ctrl Pts',(-10.6125699790961,21.4574647092097,
12.));
#242628=CARTESIAN_POINT('Ctrl Pts',(-10.5974897424622,21.4428163557144,
0.));
#242629=CARTESIAN_POINT('Ctrl Pts',(-10.5974897424622,21.4428163557144,
12.));
#242630=CARTESIAN_POINT('Ctrl Pts',(-10.5825221734573,21.4282006754631,
0.));
#242631=CARTESIAN_POINT('Ctrl Pts',(-10.5825221734573,21.4282006754631,
12.));
#242632=CARTESIAN_POINT('Ctrl Pts',(-10.5676675581108,21.4136185181979,
0.));
#242633=CARTESIAN_POINT('Ctrl Pts',(-10.5676675581108,21.4136185181979,
12.));
#242634=CARTESIAN_POINT('Ctrl Pts',(-10.5529261842108,21.3990707441497,
0.));
#242635=CARTESIAN_POINT('Ctrl Pts',(-10.5529261842108,21.3990707441497,
12.));
#242636=CARTESIAN_POINT('Ctrl Pts',(-10.5382983413421,21.3845582242602,
0.));
#242637=CARTESIAN_POINT('Ctrl Pts',(-10.5382983413421,21.3845582242602,
12.));
#242638=CARTESIAN_POINT('Ctrl Pts',(-10.5237843209057,21.3700818403936,
0.));
#242639=CARTESIAN_POINT('Ctrl Pts',(-10.5237843209057,21.3700818403936,
12.));
#242640=CARTESIAN_POINT('Ctrl Pts',(-10.5093844161685,21.3556424855814,
0.));
#242641=CARTESIAN_POINT('Ctrl Pts',(-10.5093844161685,21.3556424855814,
12.));
#242642=CARTESIAN_POINT('Ctrl Pts',(-10.4950989223337,21.3412410642904,
0.));
#242643=CARTESIAN_POINT('Ctrl Pts',(-10.4950989223337,21.3412410642904,
12.));
#242644=CARTESIAN_POINT('Ctrl Pts',(-10.4809281365931,21.3268784926819,
0.));
#242645=CARTESIAN_POINT('Ctrl Pts',(-10.4809281365931,21.3268784926819,
12.));
#242646=CARTESIAN_POINT('Ctrl Pts',(-10.4668723581768,21.3125556988731,
0.));
#242647=CARTESIAN_POINT('Ctrl Pts',(-10.4668723581768,21.3125556988731,
12.));
#242648=CARTESIAN_POINT('Ctrl Pts',(-10.4529318883874,21.2982736231931,
0.));
#242649=CARTESIAN_POINT('Ctrl Pts',(-10.4529318883874,21.2982736231931,
12.));
#242650=CARTESIAN_POINT('Ctrl Pts',(-10.4391070306391,21.2840332184483,
0.));
#242651=CARTESIAN_POINT('Ctrl Pts',(-10.4391070306391,21.2840332184483,
12.));
#242652=CARTESIAN_POINT('Ctrl Pts',(-10.42539809054,21.2698354502403,0.));
#242653=CARTESIAN_POINT('Ctrl Pts',(-10.42539809054,21.2698354502403,12.));
#242654=CARTESIAN_POINT('Ctrl Pts',(-10.4118053759588,21.255681297275,0.));
#242655=CARTESIAN_POINT('Ctrl Pts',(-10.4118053759588,21.255681297275,12.));
#242656=CARTESIAN_POINT('Ctrl Pts',(-10.3983291970846,21.2415717516714,
0.));
#242657=CARTESIAN_POINT('Ctrl Pts',(-10.3983291970846,21.2415717516714,
12.));
#242658=CARTESIAN_POINT('Ctrl Pts',(-10.3849698664786,21.22750781927,0.));
#242659=CARTESIAN_POINT('Ctrl Pts',(-10.3849698664786,21.22750781927,12.));
#242660=CARTESIAN_POINT('Ctrl Pts',(-10.371727699113,21.2134905199345,0.));
#242661=CARTESIAN_POINT('Ctrl Pts',(-10.371727699113,21.2134905199345,12.));
#242662=CARTESIAN_POINT('Ctrl Pts',(-10.3586030124587,21.199520887919,0.));
#242663=CARTESIAN_POINT('Ctrl Pts',(-10.3586030124587,21.199520887919,12.));
#242664=CARTESIAN_POINT('Ctrl Pts',(-10.3455961265701,21.1855999722416,
0.));
#242665=CARTESIAN_POINT('Ctrl Pts',(-10.3455961265701,21.1855999722416,
12.));
#242666=CARTESIAN_POINT('Ctrl Pts',(-10.3327073641572,21.1717288370509,
0.));
#242667=CARTESIAN_POINT('Ctrl Pts',(-10.3327073641572,21.1717288370509,
12.));
#242668=CARTESIAN_POINT('Ctrl Pts',(-10.3199370506544,21.1579085619965,
0.));
#242669=CARTESIAN_POINT('Ctrl Pts',(-10.3199370506544,21.1579085619965,
12.));
#242670=CARTESIAN_POINT('Ctrl Pts',(-10.3072855142687,21.1441402425843,
0.));
#242671=CARTESIAN_POINT('Ctrl Pts',(-10.3072855142687,21.1441402425843,
12.));
#242672=CARTESIAN_POINT('Ctrl Pts',(-10.2947530860721,21.1304249906002,
0.));
#242673=CARTESIAN_POINT('Ctrl Pts',(-10.2947530860721,21.1304249906002,
12.));
#242674=CARTESIAN_POINT('Ctrl Pts',(-10.2823401001072,21.1167639345631,
0.));
#242675=CARTESIAN_POINT('Ctrl Pts',(-10.2823401001072,21.1167639345631,
12.));
#242676=CARTESIAN_POINT('Ctrl Pts',(-10.2700468934744,21.1031582201627,
0.));
#242677=CARTESIAN_POINT('Ctrl Pts',(-10.2700468934744,21.1031582201627,
12.));
#242678=CARTESIAN_POINT('Ctrl Pts',(-10.2578738064181,21.0896090107063,
0.));
#242679=CARTESIAN_POINT('Ctrl Pts',(-10.2578738064181,21.0896090107063,
12.));
#242680=CARTESIAN_POINT('Ctrl Pts',(-10.2458211823912,21.0761174875445,
0.));
#242681=CARTESIAN_POINT('Ctrl Pts',(-10.2458211823912,21.0761174875445,
12.));
#242682=CARTESIAN_POINT('Ctrl Pts',(-10.2338893681567,21.0626848505663,
0.));
#242683=CARTESIAN_POINT('Ctrl Pts',(-10.2338893681567,21.0626848505663,
12.));
#242684=CARTESIAN_POINT('Ctrl Pts',(-10.2220787139155,21.0493123187483,
0.));
#242685=CARTESIAN_POINT('Ctrl Pts',(-10.2220787139155,21.0493123187483,
12.));
#242686=CARTESIAN_POINT('Ctrl Pts',(-10.2103895734123,21.0360011306815,
0.));
#242687=CARTESIAN_POINT('Ctrl Pts',(-10.2103895734123,21.0360011306815,
12.));
#242688=CARTESIAN_POINT('Ctrl Pts',(-10.1988223040425,21.0227525451107,
0.));
#242689=CARTESIAN_POINT('Ctrl Pts',(-10.1988223040425,21.0227525451107,
12.));
#242690=CARTESIAN_POINT('Ctrl Pts',(-10.187377266936,21.0095678414486,0.));
#242691=CARTESIAN_POINT('Ctrl Pts',(-10.187377266936,21.0095678414486,12.));
#242692=CARTESIAN_POINT('Ctrl Pts',(-10.1760548270767,20.9964483203686,
0.));
#242693=CARTESIAN_POINT('Ctrl Pts',(-10.1760548270767,20.9964483203686,
12.));
#242694=CARTESIAN_POINT('Ctrl Pts',(-10.1648553534568,20.9833953044736,
0.));
#242695=CARTESIAN_POINT('Ctrl Pts',(-10.1648553534568,20.9833953044736,
12.));
#242696=CARTESIAN_POINT('Ctrl Pts',(-10.1537792192065,20.9704101389369,
0.));
#242697=CARTESIAN_POINT('Ctrl Pts',(-10.1537792192065,20.9704101389369,
12.));
#242698=CARTESIAN_POINT('Ctrl Pts',(-10.1428268017256,20.9574941921591,
0.));
#242699=CARTESIAN_POINT('Ctrl Pts',(-10.1428268017256,20.9574941921591,
12.));
#242700=CARTESIAN_POINT('Ctrl Pts',(-10.1319984827908,20.9446488563933,
0.));
#242701=CARTESIAN_POINT('Ctrl Pts',(-10.1319984827908,20.9446488563933,
12.));
#242702=CARTESIAN_POINT('Ctrl Pts',(-10.1212946487057,20.9318755484734,
0.));
#242703=CARTESIAN_POINT('Ctrl Pts',(-10.1212946487057,20.9318755484734,
12.));
#242704=CARTESIAN_POINT('Ctrl Pts',(-10.1107156904836,20.919175710627,0.));
#242705=CARTESIAN_POINT('Ctrl Pts',(-10.1107156904836,20.919175710627,12.));
#242706=CARTESIAN_POINT('Ctrl Pts',(-10.1002620040076,20.9065508112557,
0.));
#242707=CARTESIAN_POINT('Ctrl Pts',(-10.1002620040076,20.9065508112557,
12.));
#242708=CARTESIAN_POINT('Ctrl Pts',(-10.0899339901916,20.894002345737,0.));
#242709=CARTESIAN_POINT('Ctrl Pts',(-10.0899339901916,20.894002345737,12.));
#242710=CARTESIAN_POINT('Ctrl Pts',(-10.0797320551154,20.881531837184,0.));
#242711=CARTESIAN_POINT('Ctrl Pts',(-10.0797320551154,20.881531837184,12.));
#242712=CARTESIAN_POINT('Ctrl Pts',(-10.0696566102218,20.86914083737,0.));
#242713=CARTESIAN_POINT('Ctrl Pts',(-10.0696566102218,20.86914083737,12.));
#242714=CARTESIAN_POINT('Ctrl Pts',(-10.0597080725375,20.8568309277316,
0.));
#242715=CARTESIAN_POINT('Ctrl Pts',(-10.0597080725375,20.8568309277316,
12.));
#242716=CARTESIAN_POINT('Ctrl Pts',(-10.0498868648733,20.8446037203402,
0.));
#242717=CARTESIAN_POINT('Ctrl Pts',(-10.0498868648733,20.8446037203402,
12.));
#242718=CARTESIAN_POINT('Ctrl Pts',(-10.0401934160234,20.8324608588909,
0.));
#242719=CARTESIAN_POINT('Ctrl Pts',(-10.0401934160234,20.8324608588909,
12.));
#242720=CARTESIAN_POINT('Ctrl Pts',(-10.0306281609435,20.8204040196602,
0.));
#242721=CARTESIAN_POINT('Ctrl Pts',(-10.0306281609435,20.8204040196602,
12.));
#242722=CARTESIAN_POINT('Ctrl Pts',(-10.0211915410095,20.8084349126888,
0.));
#242723=CARTESIAN_POINT('Ctrl Pts',(-10.0211915410095,20.8084349126888,
12.));
#242724=CARTESIAN_POINT('Ctrl Pts',(-10.0118840042786,20.7965552829908,
0.));
#242725=CARTESIAN_POINT('Ctrl Pts',(-10.0118840042786,20.7965552829908,
12.));
#242726=CARTESIAN_POINT('Ctrl Pts',(-10.0027060057389,20.7847669117568,
0.));
#242727=CARTESIAN_POINT('Ctrl Pts',(-10.0027060057389,20.7847669117568,
12.));
#242728=CARTESIAN_POINT('Ctrl Pts',(-9.9936580075464,20.7730716175417,0.));
#242729=CARTESIAN_POINT('Ctrl Pts',(-9.9936580075464,20.7730716175417,12.));
#242730=CARTESIAN_POINT('Ctrl Pts',(-9.98474047926852,20.761471257499,0.));
#242731=CARTESIAN_POINT('Ctrl Pts',(-9.98474047926852,20.761471257499,12.));
#242732=CARTESIAN_POINT('Ctrl Pts',(-9.9759538982347,20.7499677289627,0.));
#242733=CARTESIAN_POINT('Ctrl Pts',(-9.9759538982347,20.7499677289627,12.));
#242734=CARTESIAN_POINT('Ctrl Pts',(-9.96729874986202,20.7385629709795,
0.));
#242735=CARTESIAN_POINT('Ctrl Pts',(-9.96729874986202,20.7385629709795,
12.));
#242736=CARTESIAN_POINT('Ctrl Pts',(-9.95877552798398,20.7272589658751,
0.));
#242737=CARTESIAN_POINT('Ctrl Pts',(-9.95877552798398,20.7272589658751,
12.));
#242738=CARTESIAN_POINT('Ctrl Pts',(-9.95038473514949,20.7160577407579,
0.));
#242739=CARTESIAN_POINT('Ctrl Pts',(-9.95038473514949,20.7160577407579,
12.));
#242740=CARTESIAN_POINT('Ctrl Pts',(-9.94212688298236,20.7049613692234,
0.));
#242741=CARTESIAN_POINT('Ctrl Pts',(-9.94212688298236,20.7049613692234,
12.));
#242742=CARTESIAN_POINT('Ctrl Pts',(-9.9340024925973,20.6939719732484,0.));
#242743=CARTESIAN_POINT('Ctrl Pts',(-9.9340024925973,20.6939719732484,12.));
#242744=CARTESIAN_POINT('Ctrl Pts',(-9.92601209498749,20.6830917250255,
0.));
#242745=CARTESIAN_POINT('Ctrl Pts',(-9.92601209498749,20.6830917250255,
12.));
#242746=CARTESIAN_POINT('Ctrl Pts',(-9.91815623141289,20.6723228488263,
0.));
#242747=CARTESIAN_POINT('Ctrl Pts',(-9.91815623141289,20.6723228488263,
12.));
#242748=CARTESIAN_POINT('Ctrl Pts',(-9.91043545377007,20.6616676228315,
0.));
#242749=CARTESIAN_POINT('Ctrl Pts',(-9.91043545377007,20.6616676228315,
12.));
#242750=CARTESIAN_POINT('Ctrl Pts',(-9.90285032516693,20.6511283817414,
0.));
#242751=CARTESIAN_POINT('Ctrl Pts',(-9.90285032516693,20.6511283817414,
12.));
#242752=CARTESIAN_POINT('Ctrl Pts',(-9.8954014204912,20.6407075193976,0.));
#242753=CARTESIAN_POINT('Ctrl Pts',(-9.8954014204912,20.6407075193976,12.));
#242754=CARTESIAN_POINT('Ctrl Pts',(-9.88808932697306,20.6304074914087,
0.));
#242755=CARTESIAN_POINT('Ctrl Pts',(-9.88808932697306,20.6304074914087,
12.));
#242756=CARTESIAN_POINT('Ctrl Pts',(-9.88091464472676,20.6202308177474,
0.));
#242757=CARTESIAN_POINT('Ctrl Pts',(-9.88091464472676,20.6202308177474,
12.));
#242758=CARTESIAN_POINT('Ctrl Pts',(-9.87387798732956,20.6101800854494,
0.));
#242759=CARTESIAN_POINT('Ctrl Pts',(-9.87387798732956,20.6101800854494,
12.));
#242760=CARTESIAN_POINT('Ctrl Pts',(-9.86697998242623,20.6002579513699,
0.));
#242761=CARTESIAN_POINT('Ctrl Pts',(-9.86697998242623,20.6002579513699,
12.));
#242762=CARTESIAN_POINT('Ctrl Pts',(-9.86022127232748,20.5904671449754,
0.));
#242763=CARTESIAN_POINT('Ctrl Pts',(-9.86022127232748,20.5904671449754,
12.));
#242764=CARTESIAN_POINT('Ctrl Pts',(-9.85360251456981,20.5808104710015,
0.));
#242765=CARTESIAN_POINT('Ctrl Pts',(-9.85360251456981,20.5808104710015,
12.));
#242766=CARTESIAN_POINT('Ctrl Pts',(-9.84712438256278,20.5712908125139,
0.));
#242767=CARTESIAN_POINT('Ctrl Pts',(-9.84712438256278,20.5712908125139,
12.));
#242768=CARTESIAN_POINT('Ctrl Pts',(-9.84078756677565,20.5619111362402,
0.));
#242769=CARTESIAN_POINT('Ctrl Pts',(-9.84078756677565,20.5619111362402,
12.));
#242770=CARTESIAN_POINT('Ctrl Pts',(-9.83459277585315,20.552674497646,0.));
#242771=CARTESIAN_POINT('Ctrl Pts',(-9.83459277585315,20.552674497646,12.));
#242772=CARTESIAN_POINT('Ctrl Pts',(-9.82854073773877,20.5435840460721,
0.));
#242773=CARTESIAN_POINT('Ctrl Pts',(-9.82854073773877,20.5435840460721,
12.));
#242774=CARTESIAN_POINT('Ctrl Pts',(-9.82263220080363,20.5346430299517,
0.));
#242775=CARTESIAN_POINT('Ctrl Pts',(-9.82263220080363,20.5346430299517,
12.));
#242776=CARTESIAN_POINT('Ctrl Pts',(-9.81686793455943,20.5258548000629,
0.));
#242777=CARTESIAN_POINT('Ctrl Pts',(-9.81686793455943,20.5258548000629,
12.));
#242778=CARTESIAN_POINT('Ctrl Pts',(-9.81124873025282,20.517222812284,0.));
#242779=CARTESIAN_POINT('Ctrl Pts',(-9.81124873025282,20.517222812284,12.));
#242780=CARTESIAN_POINT('Ctrl Pts',(-9.80577540161088,20.5087506310505,
0.));
#242781=CARTESIAN_POINT('Ctrl Pts',(-9.80577540161088,20.5087506310505,
12.));
#242782=CARTESIAN_POINT('Ctrl Pts',(-9.80044878520949,20.5004419312107,
0.));
#242783=CARTESIAN_POINT('Ctrl Pts',(-9.80044878520949,20.5004419312107,
12.));
#242784=CARTESIAN_POINT('Ctrl Pts',(-9.79526974288331,20.4923005087943,
0.));
#242785=CARTESIAN_POINT('Ctrl Pts',(-9.79526974288331,20.4923005087943,
12.));
#242786=CARTESIAN_POINT('Ctrl Pts',(-9.79023916498656,20.4843302955329,
0.));
#242787=CARTESIAN_POINT('Ctrl Pts',(-9.79023916498656,20.4843302955329,
12.));
#242788=CARTESIAN_POINT('Ctrl Pts',(-9.78535797314167,20.4765353711586,
0.));
#242789=CARTESIAN_POINT('Ctrl Pts',(-9.78535797314167,20.4765353711586,
12.));
#242790=CARTESIAN_POINT('Ctrl Pts',(-9.78062712373321,20.4689199790669,
0.));
#242791=CARTESIAN_POINT('Ctrl Pts',(-9.78062712373321,20.4689199790669,
12.));
#242792=CARTESIAN_POINT('Ctrl Pts',(-9.77604760815529,20.4614885274975,
0.));
#242793=CARTESIAN_POINT('Ctrl Pts',(-9.77604760815529,20.4614885274975,
12.));
#242794=CARTESIAN_POINT('Ctrl Pts',(-9.7716204510407,20.4542455817527,0.));
#242795=CARTESIAN_POINT('Ctrl Pts',(-9.7716204510407,20.4542455817527,12.));
#242796=CARTESIAN_POINT('Ctrl Pts',(-9.76734670980892,20.447195862298,0.));
#242797=CARTESIAN_POINT('Ctrl Pts',(-9.76734670980892,20.447195862298,12.));
#242798=CARTESIAN_POINT('Ctrl Pts',(-9.76322747195495,20.44034423294,0.));
#242799=CARTESIAN_POINT('Ctrl Pts',(-9.76322747195495,20.44034423294,12.));
#242800=CARTESIAN_POINT('Ctrl Pts',(-9.75926386289923,20.4336957355473,
0.));
#242801=CARTESIAN_POINT('Ctrl Pts',(-9.75926386289923,20.4336957355473,
12.));
#242802=CARTESIAN_POINT('Ctrl Pts',(-9.75545705902418,20.4272556476629,
0.));
#242803=CARTESIAN_POINT('Ctrl Pts',(-9.75545705902418,20.4272556476629,
12.));
#242804=CARTESIAN_POINT('Ctrl Pts',(-9.7518082978643,20.4210295275817,0.));
#242805=CARTESIAN_POINT('Ctrl Pts',(-9.7518082978643,20.4210295275817,12.));
#242806=CARTESIAN_POINT('Ctrl Pts',(-9.74831889242174,20.4150232777393,
0.));
#242807=CARTESIAN_POINT('Ctrl Pts',(-9.74831889242174,20.4150232777393,
12.));
#242808=CARTESIAN_POINT('Ctrl Pts',(-9.74499021838538,20.4092430879861,
0.));
#242809=CARTESIAN_POINT('Ctrl Pts',(-9.74499021838538,20.4092430879861,
12.));
#242810=CARTESIAN_POINT('Ctrl Pts',(-9.74182369656272,20.4036953576549,
0.));
#242811=CARTESIAN_POINT('Ctrl Pts',(-9.74182369656272,20.4036953576549,
12.));
#242812=CARTESIAN_POINT('Ctrl Pts',(-9.73882077613201,20.3983866213331,
0.));
#242813=CARTESIAN_POINT('Ctrl Pts',(-9.73882077613201,20.3983866213331,
12.));
#242814=CARTESIAN_POINT('Ctrl Pts',(-9.73598292014243,20.3933234845647,
0.));
#242815=CARTESIAN_POINT('Ctrl Pts',(-9.73598292014243,20.3933234845647,
12.));
#242816=CARTESIAN_POINT('Ctrl Pts',(-9.73331167102808,20.3885129129912,
0.));
#242817=CARTESIAN_POINT('Ctrl Pts',(-9.73331167102808,20.3885129129912,
12.));
#242818=CARTESIAN_POINT('Ctrl Pts',(-9.73080870123727,20.3839624556742,
0.));
#242819=CARTESIAN_POINT('Ctrl Pts',(-9.73080870123727,20.3839624556742,
12.));
#242820=CARTESIAN_POINT('Ctrl Pts',(-9.72847589116542,20.3796805893304,
0.));
#242821=CARTESIAN_POINT('Ctrl Pts',(-9.72847589116542,20.3796805893304,
12.));
#242822=CARTESIAN_POINT('Ctrl Pts',(-9.7263153173288,20.3756766651951,0.));
#242823=CARTESIAN_POINT('Ctrl Pts',(-9.7263153173288,20.3756766651951,12.));
#242824=CARTESIAN_POINT('Ctrl Pts',(-9.72432910043194,20.371960235676,0.));
#242825=CARTESIAN_POINT('Ctrl Pts',(-9.72432910043194,20.371960235676,12.));
#242826=CARTESIAN_POINT('Ctrl Pts',(-9.7225193072249,20.3685406190576,0.));
#242827=CARTESIAN_POINT('Ctrl Pts',(-9.7225193072249,20.3685406190576,12.));
#242828=CARTESIAN_POINT('Ctrl Pts',(-9.72088778381081,20.3654261611056,
0.));
#242829=CARTESIAN_POINT('Ctrl Pts',(-9.72088778381081,20.3654261611056,
12.));
#242830=CARTESIAN_POINT('Ctrl Pts',(-9.71943648548099,20.3626256913981,
0.));
#242831=CARTESIAN_POINT('Ctrl Pts',(-9.71943648548099,20.3626256913981,
12.));
#242832=CARTESIAN_POINT('Ctrl Pts',(-9.71816778328006,20.3601498764344,
0.));
#242833=CARTESIAN_POINT('Ctrl Pts',(-9.71816778328006,20.3601498764344,
12.));
#242834=CARTESIAN_POINT('Ctrl Pts',(-9.71708493723096,20.3580133103356,
0.));
#242835=CARTESIAN_POINT('Ctrl Pts',(-9.71708493723096,20.3580133103356,
12.));
#242836=CARTESIAN_POINT('Ctrl Pts',(-9.71619192554186,20.3562337557875,
0.));
#242837=CARTESIAN_POINT('Ctrl Pts',(-9.71619192554186,20.3562337557875,
12.));
#242838=CARTESIAN_POINT('Ctrl Pts',(-9.71549257088172,20.3548282742361,
0.));
#242839=CARTESIAN_POINT('Ctrl Pts',(-9.71549257088172,20.3548282742361,
12.));
#242840=CARTESIAN_POINT('Ctrl Pts',(-9.71498978052021,20.3538098605706,
0.));
#242841=CARTESIAN_POINT('Ctrl Pts',(-9.71498978052021,20.3538098605706,
12.));
#242842=CARTESIAN_POINT('Ctrl Pts',(-9.71474590350681,20.3533097561886,
0.));
#242843=CARTESIAN_POINT('Ctrl Pts',(-9.71474590350681,20.3533097561886,
12.));
#242844=CARTESIAN_POINT('Ctrl Pts',(-9.71465227853041,20.3531126095522,
0.));
#242845=CARTESIAN_POINT('Ctrl Pts',(-9.71465227853041,20.3531126095522,
12.));
#242846=CARTESIAN_POINT('Ctrl Pts',(-9.71462954053042,20.353060251684,0.));
#242847=CARTESIAN_POINT('Ctrl Pts',(-9.71462954053042,20.353060251684,12.));
#242848=CARTESIAN_POINT('Ctrl Pts',(-9.71462809124916,20.353053841303,0.));
#242849=CARTESIAN_POINT('Ctrl Pts',(-9.71462809124916,20.353053841303,12.));
#242850=CARTESIAN_POINT('',(-12.4230808101438,22.8400320311648,0.));
#242851=CARTESIAN_POINT('Ctrl Pts',(-12.4230808101438,22.8400320311648,
0.));
#242852=CARTESIAN_POINT('Ctrl Pts',(-12.418215285186,22.8370364396459,0.));
#242853=CARTESIAN_POINT('Ctrl Pts',(-12.4084933766347,22.8310435872747,
0.));
#242854=CARTESIAN_POINT('Ctrl Pts',(-12.3939379378998,22.8220493007173,
0.));
#242855=CARTESIAN_POINT('Ctrl Pts',(-12.374585536673,22.81004690224,0.));
#242856=CARTESIAN_POINT('Ctrl Pts',(-12.3504864740319,22.795027221673,0.));
#242857=CARTESIAN_POINT('Ctrl Pts',(-12.3264788926075,22.7799908974768,
0.));
#242858=CARTESIAN_POINT('Ctrl Pts',(-12.3025628601792,22.764938010105,0.));
#242859=CARTESIAN_POINT('Ctrl Pts',(-12.2787384750742,22.7498686970069,
0.));
#242860=CARTESIAN_POINT('Ctrl Pts',(-12.2550058702395,22.7347831655287,
0.));
#242861=CARTESIAN_POINT('Ctrl Pts',(-12.2313652198061,22.7196817119374,
0.));
#242862=CARTESIAN_POINT('Ctrl Pts',(-12.2078167360284,22.7045647168747,
0.));
#242863=CARTESIAN_POINT('Ctrl Pts',(-12.1843606579262,22.6894326205037,
0.));
#242864=CARTESIAN_POINT('Ctrl Pts',(-12.1609972423099,22.6742859034944,
0.));
#242865=CARTESIAN_POINT('Ctrl Pts',(-12.1377267537145,22.6591250653965,
0.));
#242866=CARTESIAN_POINT('Ctrl Pts',(-12.1145494550383,22.6439506046605,
0.));
#242867=CARTESIAN_POINT('Ctrl Pts',(-12.0914655972823,22.6287629967056,
0.));
#242868=CARTESIAN_POINT('Ctrl Pts',(-12.0684754113862,22.6135626764898,
0.));
#242869=CARTESIAN_POINT('Ctrl Pts',(-12.0455791139128,22.5983500505644,
0.));
#242870=CARTESIAN_POINT('Ctrl Pts',(-12.0227769113127,22.5831255061282,
0.));
#242871=CARTESIAN_POINT('Ctrl Pts',(-12.0000690046695,22.5678894211181,
0.));
#242872=CARTESIAN_POINT('Ctrl Pts',(-11.9774555943496,22.5526421741158,
0.));
#242873=CARTESIAN_POINT('Ctrl Pts',(-11.9549368843997,22.5373841537307,
0.));
#242874=CARTESIAN_POINT('Ctrl Pts',(-11.9325130877803,22.5221157697883,
0.));
#242875=CARTESIAN_POINT('Ctrl Pts',(-11.9101844254557,22.5068374513973,
0.));
#242876=CARTESIAN_POINT('Ctrl Pts',(-11.8879511239943,22.4915496418485,
0.));
#242877=CARTESIAN_POINT('Ctrl Pts',(-11.8658134137019,22.4762527946702,
0.));
#242878=CARTESIAN_POINT('Ctrl Pts',(-11.8437715264487,22.4609473690471,
0.));
#242879=CARTESIAN_POINT('Ctrl Pts',(-11.8218256937889,22.4456338258735,
0.));
#242880=CARTESIAN_POINT('Ctrl Pts',(-11.7999761445173,22.430312622646,0.));
#242881=CARTESIAN_POINT('Ctrl Pts',(-11.7782231042039,22.4149842125008,
0.));
#242882=CARTESIAN_POINT('Ctrl Pts',(-11.7565667964764,22.3996490469191,
0.));
#242883=CARTESIAN_POINT('Ctrl Pts',(-11.7350074437961,22.3843075773899,
0.));
#242884=CARTESIAN_POINT('Ctrl Pts',(-11.7135452684532,22.3689602575491,
0.));
#242885=CARTESIAN_POINT('Ctrl Pts',(-11.6921804934056,22.3536075450029,
0.));
#242886=CARTESIAN_POINT('Ctrl Pts',(-11.6709133432985,22.3382499035619,
0.));
#242887=CARTESIAN_POINT('Ctrl Pts',(-11.6497440449857,22.3228878043976,
0.));
#242888=CARTESIAN_POINT('Ctrl Pts',(-11.6286728270009,22.3075217249049,
0.));
#242889=CARTESIAN_POINT('Ctrl Pts',(-11.6076999192357,22.2921521480356,
0.));
#242890=CARTESIAN_POINT('Ctrl Pts',(-11.5868255525188,22.2767795614348,
0.));
#242891=CARTESIAN_POINT('Ctrl Pts',(-11.5660499582403,22.2614044566898,
0.));
#242892=CARTESIAN_POINT('Ctrl Pts',(-11.5453733679121,22.2460273284654,
0.));
#242893=CARTESIAN_POINT('Ctrl Pts',(-11.5247960128477,22.2306486738901,
0.));
#242894=CARTESIAN_POINT('Ctrl Pts',(-11.5043181244242,22.2152689931022,
0.));
#242895=CARTESIAN_POINT('Ctrl Pts',(-11.483939934259,22.1998887896436,0.));
#242896=CARTESIAN_POINT('Ctrl Pts',(-11.463661674411,22.184508570917,0.));
#242897=CARTESIAN_POINT('Ctrl Pts',(-11.443483577557,22.1691288486096,0.));
#242898=CARTESIAN_POINT('Ctrl Pts',(-11.4234058771742,22.1537501391487,
0.));
#242899=CARTESIAN_POINT('Ctrl Pts',(-11.4034288076908,22.1383729640964,
0.));
#242900=CARTESIAN_POINT('Ctrl Pts',(-11.3835526044256,22.1229978500186,
0.));
#242901=CARTESIAN_POINT('Ctrl Pts',(-11.3637775035367,22.1076253283979,
0.));
#242902=CARTESIAN_POINT('Ctrl Pts',(-11.3441037419553,22.0922559355294,
0.));
#242903=CARTESIAN_POINT('Ctrl Pts',(-11.3245315573168,22.0768902124267,
0.));
#242904=CARTESIAN_POINT('Ctrl Pts',(-11.3050611878771,22.0615287047179,
0.));
#242905=CARTESIAN_POINT('Ctrl Pts',(-11.2856928724374,22.046171962566,0.));
#242906=CARTESIAN_POINT('Ctrl Pts',(-11.2664268504206,22.030820540835,0.));
#242907=CARTESIAN_POINT('Ctrl Pts',(-11.2472633619275,22.0154749992363,
0.));
#242908=CARTESIAN_POINT('Ctrl Pts',(-11.2282026477896,22.0001359024839,
0.));
#242909=CARTESIAN_POINT('Ctrl Pts',(-11.2092449496125,21.9848038204439,
0.));
#242910=CARTESIAN_POINT('Ctrl Pts',(-11.190390509811,21.9694793282914,0.));
#242911=CARTESIAN_POINT('Ctrl Pts',(-11.1716395716376,21.9541630066506,
0.));
#242912=CARTESIAN_POINT('Ctrl Pts',(-11.1529923792003,21.9388554416439,
0.));
#242913=CARTESIAN_POINT('Ctrl Pts',(-11.1344491774741,21.923557224952,0.));
#242914=CARTESIAN_POINT('Ctrl Pts',(-11.1160102123024,21.9082689538688,
0.));
#242915=CARTESIAN_POINT('Ctrl Pts',(-11.0976757303944,21.8929912313608,
0.));
#242916=CARTESIAN_POINT('Ctrl Pts',(-11.0794459793057,21.877724666119,0.));
#242917=CARTESIAN_POINT('Ctrl Pts',(-11.0613212074363,21.8624698726318,
0.));
#242918=CARTESIAN_POINT('Ctrl Pts',(-11.0433016640807,21.8472274713103,
0.));
#242919=CARTESIAN_POINT('Ctrl Pts',(-11.0253875994598,21.8319980886033,
0.));
#242920=CARTESIAN_POINT('Ctrl Pts',(-11.0075792647477,21.8167823571168,
0.));
#242921=CARTESIAN_POINT('Ctrl Pts',(-10.9898769120912,21.8015809157301,
0.));
#242922=CARTESIAN_POINT('Ctrl Pts',(-10.9722807946156,21.7863944097141,
0.));
#242923=CARTESIAN_POINT('Ctrl Pts',(-10.9547911664455,21.7712234908464,
0.));
#242924=CARTESIAN_POINT('Ctrl Pts',(-10.9374082827444,21.7560688175247,
0.));
#242925=CARTESIAN_POINT('Ctrl Pts',(-10.9201323997384,21.7409310548797,
0.));
#242926=CARTESIAN_POINT('Ctrl Pts',(-10.902963774734,21.7258108748873,0.));
#242927=CARTESIAN_POINT('Ctrl Pts',(-10.8859026661293,21.7107089564825,
0.));
#242928=CARTESIAN_POINT('Ctrl Pts',(-10.8689493334095,21.6956259856672,
0.));
#242929=CARTESIAN_POINT('Ctrl Pts',(-10.8521040371835,21.6805626556467,
0.));
#242930=CARTESIAN_POINT('Ctrl Pts',(-10.8353670392272,21.6655196669732,
0.));
#242931=CARTESIAN_POINT('Ctrl Pts',(-10.8187386025136,21.6504977276866,
0.));
#242932=CARTESIAN_POINT('Ctrl Pts',(-10.8022189912369,21.6354975534557,
0.));
#242933=CARTESIAN_POINT('Ctrl Pts',(-10.7858084708261,21.6205198677173,
0.));
#242934=CARTESIAN_POINT('Ctrl Pts',(-10.7695073079552,21.6055654018176,
0.));
#242935=CARTESIAN_POINT('Ctrl Pts',(-10.7533157705941,21.5906348951743,
0.));
#242936=CARTESIAN_POINT('Ctrl Pts',(-10.7372341280467,21.5757290954371,
0.));
#242937=CARTESIAN_POINT('Ctrl Pts',(-10.7212626509816,21.5608487586468,
0.));
#242938=CARTESIAN_POINT('Ctrl Pts',(-10.7054016114571,21.5459946493955,
0.));
#242939=CARTESIAN_POINT('Ctrl Pts',(-10.689651282929,21.5311675409807,0.));
#242940=CARTESIAN_POINT('Ctrl Pts',(-10.6740119402834,21.51636821558,0.));
#242941=CARTESIAN_POINT('Ctrl Pts',(-10.6584838598939,21.5015974644449,
0.));
#242942=CARTESIAN_POINT('Ctrl Pts',(-10.6430673196607,21.4868560880889,
0.));
#242943=CARTESIAN_POINT('Ctrl Pts',(-10.6277625990456,21.4721448964766,
0.));
#242944=CARTESIAN_POINT('Ctrl Pts',(-10.6125699790961,21.4574647092097,
0.));
#242945=CARTESIAN_POINT('Ctrl Pts',(-10.5974897424622,21.4428163557144,
0.));
#242946=CARTESIAN_POINT('Ctrl Pts',(-10.5825221734573,21.4282006754631,
0.));
#242947=CARTESIAN_POINT('Ctrl Pts',(-10.5676675581108,21.4136185181979,
0.));
#242948=CARTESIAN_POINT('Ctrl Pts',(-10.5529261842108,21.3990707441497,
0.));
#242949=CARTESIAN_POINT('Ctrl Pts',(-10.5382983413421,21.3845582242602,
0.));
#242950=CARTESIAN_POINT('Ctrl Pts',(-10.5237843209057,21.3700818403936,
0.));
#242951=CARTESIAN_POINT('Ctrl Pts',(-10.5093844161685,21.3556424855814,
0.));
#242952=CARTESIAN_POINT('Ctrl Pts',(-10.4950989223337,21.3412410642904,
0.));
#242953=CARTESIAN_POINT('Ctrl Pts',(-10.4809281365931,21.3268784926819,
0.));
#242954=CARTESIAN_POINT('Ctrl Pts',(-10.4668723581768,21.3125556988731,
0.));
#242955=CARTESIAN_POINT('Ctrl Pts',(-10.4529318883874,21.2982736231931,
0.));
#242956=CARTESIAN_POINT('Ctrl Pts',(-10.4391070306391,21.2840332184483,
0.));
#242957=CARTESIAN_POINT('Ctrl Pts',(-10.42539809054,21.2698354502403,0.));
#242958=CARTESIAN_POINT('Ctrl Pts',(-10.4118053759588,21.255681297275,0.));
#242959=CARTESIAN_POINT('Ctrl Pts',(-10.3983291970846,21.2415717516714,
0.));
#242960=CARTESIAN_POINT('Ctrl Pts',(-10.3849698664786,21.22750781927,0.));
#242961=CARTESIAN_POINT('Ctrl Pts',(-10.371727699113,21.2134905199345,0.));
#242962=CARTESIAN_POINT('Ctrl Pts',(-10.3586030124587,21.199520887919,0.));
#242963=CARTESIAN_POINT('Ctrl Pts',(-10.3455961265701,21.1855999722416,
0.));
#242964=CARTESIAN_POINT('Ctrl Pts',(-10.3327073641572,21.1717288370509,
0.));
#242965=CARTESIAN_POINT('Ctrl Pts',(-10.3199370506544,21.1579085619965,
0.));
#242966=CARTESIAN_POINT('Ctrl Pts',(-10.3072855142687,21.1441402425843,
0.));
#242967=CARTESIAN_POINT('Ctrl Pts',(-10.2947530860721,21.1304249906002,
0.));
#242968=CARTESIAN_POINT('Ctrl Pts',(-10.2823401001072,21.1167639345631,
0.));
#242969=CARTESIAN_POINT('Ctrl Pts',(-10.2700468934744,21.1031582201627,
0.));
#242970=CARTESIAN_POINT('Ctrl Pts',(-10.2578738064181,21.0896090107063,
0.));
#242971=CARTESIAN_POINT('Ctrl Pts',(-10.2458211823912,21.0761174875445,
0.));
#242972=CARTESIAN_POINT('Ctrl Pts',(-10.2338893681567,21.0626848505663,
0.));
#242973=CARTESIAN_POINT('Ctrl Pts',(-10.2220787139155,21.0493123187483,
0.));
#242974=CARTESIAN_POINT('Ctrl Pts',(-10.2103895734123,21.0360011306815,
0.));
#242975=CARTESIAN_POINT('Ctrl Pts',(-10.1988223040425,21.0227525451107,
0.));
#242976=CARTESIAN_POINT('Ctrl Pts',(-10.187377266936,21.0095678414486,0.));
#242977=CARTESIAN_POINT('Ctrl Pts',(-10.1760548270767,20.9964483203686,
0.));
#242978=CARTESIAN_POINT('Ctrl Pts',(-10.1648553534568,20.9833953044736,
0.));
#242979=CARTESIAN_POINT('Ctrl Pts',(-10.1537792192065,20.9704101389369,
0.));
#242980=CARTESIAN_POINT('Ctrl Pts',(-10.1428268017256,20.9574941921591,
0.));
#242981=CARTESIAN_POINT('Ctrl Pts',(-10.1319984827908,20.9446488563933,
0.));
#242982=CARTESIAN_POINT('Ctrl Pts',(-10.1212946487057,20.9318755484734,
0.));
#242983=CARTESIAN_POINT('Ctrl Pts',(-10.1107156904836,20.919175710627,0.));
#242984=CARTESIAN_POINT('Ctrl Pts',(-10.1002620040076,20.9065508112557,
0.));
#242985=CARTESIAN_POINT('Ctrl Pts',(-10.0899339901916,20.894002345737,0.));
#242986=CARTESIAN_POINT('Ctrl Pts',(-10.0797320551154,20.881531837184,0.));
#242987=CARTESIAN_POINT('Ctrl Pts',(-10.0696566102218,20.86914083737,0.));
#242988=CARTESIAN_POINT('Ctrl Pts',(-10.0597080725375,20.8568309277316,
0.));
#242989=CARTESIAN_POINT('Ctrl Pts',(-10.0498868648733,20.8446037203402,
0.));
#242990=CARTESIAN_POINT('Ctrl Pts',(-10.0401934160234,20.8324608588909,
0.));
#242991=CARTESIAN_POINT('Ctrl Pts',(-10.0306281609435,20.8204040196602,
0.));
#242992=CARTESIAN_POINT('Ctrl Pts',(-10.0211915410095,20.8084349126888,
0.));
#242993=CARTESIAN_POINT('Ctrl Pts',(-10.0118840042786,20.7965552829908,
0.));
#242994=CARTESIAN_POINT('Ctrl Pts',(-10.0027060057389,20.7847669117568,
0.));
#242995=CARTESIAN_POINT('Ctrl Pts',(-9.9936580075464,20.7730716175417,0.));
#242996=CARTESIAN_POINT('Ctrl Pts',(-9.98474047926852,20.761471257499,0.));
#242997=CARTESIAN_POINT('Ctrl Pts',(-9.9759538982347,20.7499677289627,0.));
#242998=CARTESIAN_POINT('Ctrl Pts',(-9.96729874986202,20.7385629709795,
0.));
#242999=CARTESIAN_POINT('Ctrl Pts',(-9.95877552798398,20.7272589658751,
0.));
#243000=CARTESIAN_POINT('Ctrl Pts',(-9.95038473514949,20.7160577407579,
0.));
#243001=CARTESIAN_POINT('Ctrl Pts',(-9.94212688298236,20.7049613692234,
0.));
#243002=CARTESIAN_POINT('Ctrl Pts',(-9.9340024925973,20.6939719732484,0.));
#243003=CARTESIAN_POINT('Ctrl Pts',(-9.92601209498749,20.6830917250255,
0.));
#243004=CARTESIAN_POINT('Ctrl Pts',(-9.91815623141289,20.6723228488263,
0.));
#243005=CARTESIAN_POINT('Ctrl Pts',(-9.91043545377007,20.6616676228315,
0.));
#243006=CARTESIAN_POINT('Ctrl Pts',(-9.90285032516693,20.6511283817414,
0.));
#243007=CARTESIAN_POINT('Ctrl Pts',(-9.8954014204912,20.6407075193976,0.));
#243008=CARTESIAN_POINT('Ctrl Pts',(-9.88808932697306,20.6304074914087,
0.));
#243009=CARTESIAN_POINT('Ctrl Pts',(-9.88091464472676,20.6202308177474,
0.));
#243010=CARTESIAN_POINT('Ctrl Pts',(-9.87387798732956,20.6101800854494,
0.));
#243011=CARTESIAN_POINT('Ctrl Pts',(-9.86697998242623,20.6002579513699,
0.));
#243012=CARTESIAN_POINT('Ctrl Pts',(-9.86022127232748,20.5904671449754,
0.));
#243013=CARTESIAN_POINT('Ctrl Pts',(-9.85360251456981,20.5808104710015,
0.));
#243014=CARTESIAN_POINT('Ctrl Pts',(-9.84712438256278,20.5712908125139,
0.));
#243015=CARTESIAN_POINT('Ctrl Pts',(-9.84078756677565,20.5619111362402,
0.));
#243016=CARTESIAN_POINT('Ctrl Pts',(-9.83459277585315,20.552674497646,0.));
#243017=CARTESIAN_POINT('Ctrl Pts',(-9.82854073773877,20.5435840460721,
0.));
#243018=CARTESIAN_POINT('Ctrl Pts',(-9.82263220080363,20.5346430299517,
0.));
#243019=CARTESIAN_POINT('Ctrl Pts',(-9.81686793455943,20.5258548000629,
0.));
#243020=CARTESIAN_POINT('Ctrl Pts',(-9.81124873025282,20.517222812284,0.));
#243021=CARTESIAN_POINT('Ctrl Pts',(-9.80577540161088,20.5087506310505,
0.));
#243022=CARTESIAN_POINT('Ctrl Pts',(-9.80044878520949,20.5004419312107,
0.));
#243023=CARTESIAN_POINT('Ctrl Pts',(-9.79526974288331,20.4923005087943,
0.));
#243024=CARTESIAN_POINT('Ctrl Pts',(-9.79023916498656,20.4843302955329,
0.));
#243025=CARTESIAN_POINT('Ctrl Pts',(-9.78535797314167,20.4765353711586,
0.));
#243026=CARTESIAN_POINT('Ctrl Pts',(-9.78062712373321,20.4689199790669,
0.));
#243027=CARTESIAN_POINT('Ctrl Pts',(-9.77604760815529,20.4614885274975,
0.));
#243028=CARTESIAN_POINT('Ctrl Pts',(-9.7716204510407,20.4542455817527,0.));
#243029=CARTESIAN_POINT('Ctrl Pts',(-9.76734670980892,20.447195862298,0.));
#243030=CARTESIAN_POINT('Ctrl Pts',(-9.76322747195495,20.44034423294,0.));
#243031=CARTESIAN_POINT('Ctrl Pts',(-9.75926386289923,20.4336957355473,
0.));
#243032=CARTESIAN_POINT('Ctrl Pts',(-9.75545705902418,20.4272556476629,
0.));
#243033=CARTESIAN_POINT('Ctrl Pts',(-9.7518082978643,20.4210295275817,0.));
#243034=CARTESIAN_POINT('Ctrl Pts',(-9.74831889242174,20.4150232777393,
0.));
#243035=CARTESIAN_POINT('Ctrl Pts',(-9.74499021838538,20.4092430879861,
0.));
#243036=CARTESIAN_POINT('Ctrl Pts',(-9.74182369656272,20.4036953576549,
0.));
#243037=CARTESIAN_POINT('Ctrl Pts',(-9.73882077613201,20.3983866213331,
0.));
#243038=CARTESIAN_POINT('Ctrl Pts',(-9.73598292014243,20.3933234845647,
0.));
#243039=CARTESIAN_POINT('Ctrl Pts',(-9.73331167102808,20.3885129129912,
0.));
#243040=CARTESIAN_POINT('Ctrl Pts',(-9.73080870123727,20.3839624556742,
0.));
#243041=CARTESIAN_POINT('Ctrl Pts',(-9.72847589116542,20.3796805893304,
0.));
#243042=CARTESIAN_POINT('Ctrl Pts',(-9.7263153173288,20.3756766651951,0.));
#243043=CARTESIAN_POINT('Ctrl Pts',(-9.72432910043194,20.371960235676,0.));
#243044=CARTESIAN_POINT('Ctrl Pts',(-9.7225193072249,20.3685406190576,0.));
#243045=CARTESIAN_POINT('Ctrl Pts',(-9.72088778381081,20.3654261611056,
0.));
#243046=CARTESIAN_POINT('Ctrl Pts',(-9.71943648548099,20.3626256913981,
0.));
#243047=CARTESIAN_POINT('Ctrl Pts',(-9.71816778328006,20.3601498764344,
0.));
#243048=CARTESIAN_POINT('Ctrl Pts',(-9.71708493723096,20.3580133103356,
0.));
#243049=CARTESIAN_POINT('Ctrl Pts',(-9.71619192554186,20.3562337557875,
0.));
#243050=CARTESIAN_POINT('Ctrl Pts',(-9.71549257088172,20.3548282742361,
0.));
#243051=CARTESIAN_POINT('Ctrl Pts',(-9.71498978052021,20.3538098605706,
0.));
#243052=CARTESIAN_POINT('Ctrl Pts',(-9.71474590350681,20.3533097561886,
0.));
#243053=CARTESIAN_POINT('Ctrl Pts',(-9.71465227853041,20.3531126095522,
0.));
#243054=CARTESIAN_POINT('Ctrl Pts',(-9.71462954053042,20.353060251684,0.));
#243055=CARTESIAN_POINT('Ctrl Pts',(-9.71462809124916,20.353053841303,0.));
#243056=CARTESIAN_POINT('',(-12.4230808101438,22.8400320311648,12.));
#243057=CARTESIAN_POINT('',(-12.4230808101438,22.8400320311648,0.));
#243058=CARTESIAN_POINT('Ctrl Pts',(-9.71462809124916,20.353053841303,12.));
#243059=CARTESIAN_POINT('Ctrl Pts',(-9.71462954053042,20.353060251684,12.));
#243060=CARTESIAN_POINT('Ctrl Pts',(-9.71465227853041,20.3531126095522,
12.));
#243061=CARTESIAN_POINT('Ctrl Pts',(-9.71474590350681,20.3533097561886,
12.));
#243062=CARTESIAN_POINT('Ctrl Pts',(-9.71498978052021,20.3538098605706,
12.));
#243063=CARTESIAN_POINT('Ctrl Pts',(-9.71549257088172,20.3548282742361,
12.));
#243064=CARTESIAN_POINT('Ctrl Pts',(-9.71619192554186,20.3562337557875,
12.));
#243065=CARTESIAN_POINT('Ctrl Pts',(-9.71708493723096,20.3580133103356,
12.));
#243066=CARTESIAN_POINT('Ctrl Pts',(-9.71816778328006,20.3601498764344,
12.));
#243067=CARTESIAN_POINT('Ctrl Pts',(-9.71943648548099,20.3626256913981,
12.));
#243068=CARTESIAN_POINT('Ctrl Pts',(-9.72088778381081,20.3654261611056,
12.));
#243069=CARTESIAN_POINT('Ctrl Pts',(-9.7225193072249,20.3685406190576,12.));
#243070=CARTESIAN_POINT('Ctrl Pts',(-9.72432910043194,20.371960235676,12.));
#243071=CARTESIAN_POINT('Ctrl Pts',(-9.7263153173288,20.3756766651951,12.));
#243072=CARTESIAN_POINT('Ctrl Pts',(-9.72847589116542,20.3796805893304,
12.));
#243073=CARTESIAN_POINT('Ctrl Pts',(-9.73080870123727,20.3839624556742,
12.));
#243074=CARTESIAN_POINT('Ctrl Pts',(-9.73331167102808,20.3885129129912,
12.));
#243075=CARTESIAN_POINT('Ctrl Pts',(-9.73598292014243,20.3933234845647,
12.));
#243076=CARTESIAN_POINT('Ctrl Pts',(-9.73882077613201,20.3983866213331,
12.));
#243077=CARTESIAN_POINT('Ctrl Pts',(-9.74182369656272,20.4036953576549,
12.));
#243078=CARTESIAN_POINT('Ctrl Pts',(-9.74499021838538,20.4092430879861,
12.));
#243079=CARTESIAN_POINT('Ctrl Pts',(-9.74831889242174,20.4150232777393,
12.));
#243080=CARTESIAN_POINT('Ctrl Pts',(-9.7518082978643,20.4210295275817,12.));
#243081=CARTESIAN_POINT('Ctrl Pts',(-9.75545705902418,20.4272556476629,
12.));
#243082=CARTESIAN_POINT('Ctrl Pts',(-9.75926386289923,20.4336957355473,
12.));
#243083=CARTESIAN_POINT('Ctrl Pts',(-9.76322747195495,20.44034423294,12.));
#243084=CARTESIAN_POINT('Ctrl Pts',(-9.76734670980892,20.447195862298,12.));
#243085=CARTESIAN_POINT('Ctrl Pts',(-9.7716204510407,20.4542455817527,12.));
#243086=CARTESIAN_POINT('Ctrl Pts',(-9.77604760815529,20.4614885274975,
12.));
#243087=CARTESIAN_POINT('Ctrl Pts',(-9.78062712373321,20.4689199790669,
12.));
#243088=CARTESIAN_POINT('Ctrl Pts',(-9.78535797314167,20.4765353711586,
12.));
#243089=CARTESIAN_POINT('Ctrl Pts',(-9.79023916498656,20.4843302955329,
12.));
#243090=CARTESIAN_POINT('Ctrl Pts',(-9.79526974288331,20.4923005087943,
12.));
#243091=CARTESIAN_POINT('Ctrl Pts',(-9.80044878520949,20.5004419312107,
12.));
#243092=CARTESIAN_POINT('Ctrl Pts',(-9.80577540161088,20.5087506310505,
12.));
#243093=CARTESIAN_POINT('Ctrl Pts',(-9.81124873025282,20.517222812284,12.));
#243094=CARTESIAN_POINT('Ctrl Pts',(-9.81686793455943,20.5258548000629,
12.));
#243095=CARTESIAN_POINT('Ctrl Pts',(-9.82263220080363,20.5346430299517,
12.));
#243096=CARTESIAN_POINT('Ctrl Pts',(-9.82854073773877,20.5435840460721,
12.));
#243097=CARTESIAN_POINT('Ctrl Pts',(-9.83459277585315,20.552674497646,12.));
#243098=CARTESIAN_POINT('Ctrl Pts',(-9.84078756677565,20.5619111362402,
12.));
#243099=CARTESIAN_POINT('Ctrl Pts',(-9.84712438256278,20.5712908125139,
12.));
#243100=CARTESIAN_POINT('Ctrl Pts',(-9.85360251456981,20.5808104710015,
12.));
#243101=CARTESIAN_POINT('Ctrl Pts',(-9.86022127232748,20.5904671449754,
12.));
#243102=CARTESIAN_POINT('Ctrl Pts',(-9.86697998242623,20.6002579513699,
12.));
#243103=CARTESIAN_POINT('Ctrl Pts',(-9.87387798732956,20.6101800854494,
12.));
#243104=CARTESIAN_POINT('Ctrl Pts',(-9.88091464472676,20.6202308177474,
12.));
#243105=CARTESIAN_POINT('Ctrl Pts',(-9.88808932697306,20.6304074914087,
12.));
#243106=CARTESIAN_POINT('Ctrl Pts',(-9.8954014204912,20.6407075193976,12.));
#243107=CARTESIAN_POINT('Ctrl Pts',(-9.90285032516693,20.6511283817414,
12.));
#243108=CARTESIAN_POINT('Ctrl Pts',(-9.91043545377007,20.6616676228315,
12.));
#243109=CARTESIAN_POINT('Ctrl Pts',(-9.91815623141289,20.6723228488263,
12.));
#243110=CARTESIAN_POINT('Ctrl Pts',(-9.92601209498749,20.6830917250255,
12.));
#243111=CARTESIAN_POINT('Ctrl Pts',(-9.9340024925973,20.6939719732484,12.));
#243112=CARTESIAN_POINT('Ctrl Pts',(-9.94212688298236,20.7049613692234,
12.));
#243113=CARTESIAN_POINT('Ctrl Pts',(-9.95038473514949,20.7160577407579,
12.));
#243114=CARTESIAN_POINT('Ctrl Pts',(-9.95877552798398,20.7272589658751,
12.));
#243115=CARTESIAN_POINT('Ctrl Pts',(-9.96729874986202,20.7385629709795,
12.));
#243116=CARTESIAN_POINT('Ctrl Pts',(-9.9759538982347,20.7499677289627,12.));
#243117=CARTESIAN_POINT('Ctrl Pts',(-9.98474047926852,20.761471257499,12.));
#243118=CARTESIAN_POINT('Ctrl Pts',(-9.9936580075464,20.7730716175417,12.));
#243119=CARTESIAN_POINT('Ctrl Pts',(-10.0027060057389,20.7847669117568,
12.));
#243120=CARTESIAN_POINT('Ctrl Pts',(-10.0118840042786,20.7965552829908,
12.));
#243121=CARTESIAN_POINT('Ctrl Pts',(-10.0211915410095,20.8084349126888,
12.));
#243122=CARTESIAN_POINT('Ctrl Pts',(-10.0306281609435,20.8204040196602,
12.));
#243123=CARTESIAN_POINT('Ctrl Pts',(-10.0401934160234,20.8324608588909,
12.));
#243124=CARTESIAN_POINT('Ctrl Pts',(-10.0498868648733,20.8446037203402,
12.));
#243125=CARTESIAN_POINT('Ctrl Pts',(-10.0597080725375,20.8568309277316,
12.));
#243126=CARTESIAN_POINT('Ctrl Pts',(-10.0696566102218,20.86914083737,12.));
#243127=CARTESIAN_POINT('Ctrl Pts',(-10.0797320551154,20.881531837184,12.));
#243128=CARTESIAN_POINT('Ctrl Pts',(-10.0899339901916,20.894002345737,12.));
#243129=CARTESIAN_POINT('Ctrl Pts',(-10.1002620040076,20.9065508112557,
12.));
#243130=CARTESIAN_POINT('Ctrl Pts',(-10.1107156904836,20.919175710627,12.));
#243131=CARTESIAN_POINT('Ctrl Pts',(-10.1212946487057,20.9318755484734,
12.));
#243132=CARTESIAN_POINT('Ctrl Pts',(-10.1319984827908,20.9446488563933,
12.));
#243133=CARTESIAN_POINT('Ctrl Pts',(-10.1428268017256,20.9574941921591,
12.));
#243134=CARTESIAN_POINT('Ctrl Pts',(-10.1537792192065,20.9704101389369,
12.));
#243135=CARTESIAN_POINT('Ctrl Pts',(-10.1648553534568,20.9833953044736,
12.));
#243136=CARTESIAN_POINT('Ctrl Pts',(-10.1760548270767,20.9964483203686,
12.));
#243137=CARTESIAN_POINT('Ctrl Pts',(-10.187377266936,21.0095678414486,12.));
#243138=CARTESIAN_POINT('Ctrl Pts',(-10.1988223040425,21.0227525451107,
12.));
#243139=CARTESIAN_POINT('Ctrl Pts',(-10.2103895734123,21.0360011306815,
12.));
#243140=CARTESIAN_POINT('Ctrl Pts',(-10.2220787139155,21.0493123187483,
12.));
#243141=CARTESIAN_POINT('Ctrl Pts',(-10.2338893681567,21.0626848505663,
12.));
#243142=CARTESIAN_POINT('Ctrl Pts',(-10.2458211823912,21.0761174875445,
12.));
#243143=CARTESIAN_POINT('Ctrl Pts',(-10.2578738064181,21.0896090107063,
12.));
#243144=CARTESIAN_POINT('Ctrl Pts',(-10.2700468934744,21.1031582201627,
12.));
#243145=CARTESIAN_POINT('Ctrl Pts',(-10.2823401001072,21.1167639345631,
12.));
#243146=CARTESIAN_POINT('Ctrl Pts',(-10.2947530860721,21.1304249906002,
12.));
#243147=CARTESIAN_POINT('Ctrl Pts',(-10.3072855142687,21.1441402425843,
12.));
#243148=CARTESIAN_POINT('Ctrl Pts',(-10.3199370506544,21.1579085619965,
12.));
#243149=CARTESIAN_POINT('Ctrl Pts',(-10.3327073641572,21.1717288370509,
12.));
#243150=CARTESIAN_POINT('Ctrl Pts',(-10.3455961265701,21.1855999722416,
12.));
#243151=CARTESIAN_POINT('Ctrl Pts',(-10.3586030124587,21.199520887919,12.));
#243152=CARTESIAN_POINT('Ctrl Pts',(-10.371727699113,21.2134905199345,12.));
#243153=CARTESIAN_POINT('Ctrl Pts',(-10.3849698664786,21.22750781927,12.));
#243154=CARTESIAN_POINT('Ctrl Pts',(-10.3983291970846,21.2415717516714,
12.));
#243155=CARTESIAN_POINT('Ctrl Pts',(-10.4118053759588,21.255681297275,12.));
#243156=CARTESIAN_POINT('Ctrl Pts',(-10.42539809054,21.2698354502403,12.));
#243157=CARTESIAN_POINT('Ctrl Pts',(-10.4391070306391,21.2840332184483,
12.));
#243158=CARTESIAN_POINT('Ctrl Pts',(-10.4529318883874,21.2982736231931,
12.));
#243159=CARTESIAN_POINT('Ctrl Pts',(-10.4668723581768,21.3125556988731,
12.));
#243160=CARTESIAN_POINT('Ctrl Pts',(-10.4809281365931,21.3268784926819,
12.));
#243161=CARTESIAN_POINT('Ctrl Pts',(-10.4950989223337,21.3412410642904,
12.));
#243162=CARTESIAN_POINT('Ctrl Pts',(-10.5093844161685,21.3556424855814,
12.));
#243163=CARTESIAN_POINT('Ctrl Pts',(-10.5237843209057,21.3700818403936,
12.));
#243164=CARTESIAN_POINT('Ctrl Pts',(-10.5382983413421,21.3845582242602,
12.));
#243165=CARTESIAN_POINT('Ctrl Pts',(-10.5529261842108,21.3990707441497,
12.));
#243166=CARTESIAN_POINT('Ctrl Pts',(-10.5676675581108,21.4136185181979,
12.));
#243167=CARTESIAN_POINT('Ctrl Pts',(-10.5825221734573,21.4282006754631,
12.));
#243168=CARTESIAN_POINT('Ctrl Pts',(-10.5974897424622,21.4428163557144,
12.));
#243169=CARTESIAN_POINT('Ctrl Pts',(-10.6125699790961,21.4574647092097,
12.));
#243170=CARTESIAN_POINT('Ctrl Pts',(-10.6277625990456,21.4721448964766,
12.));
#243171=CARTESIAN_POINT('Ctrl Pts',(-10.6430673196607,21.4868560880889,
12.));
#243172=CARTESIAN_POINT('Ctrl Pts',(-10.6584838598939,21.5015974644449,
12.));
#243173=CARTESIAN_POINT('Ctrl Pts',(-10.6740119402834,21.51636821558,12.));
#243174=CARTESIAN_POINT('Ctrl Pts',(-10.689651282929,21.5311675409807,12.));
#243175=CARTESIAN_POINT('Ctrl Pts',(-10.7054016114571,21.5459946493955,
12.));
#243176=CARTESIAN_POINT('Ctrl Pts',(-10.7212626509816,21.5608487586468,
12.));
#243177=CARTESIAN_POINT('Ctrl Pts',(-10.7372341280467,21.5757290954371,
12.));
#243178=CARTESIAN_POINT('Ctrl Pts',(-10.7533157705941,21.5906348951743,
12.));
#243179=CARTESIAN_POINT('Ctrl Pts',(-10.7695073079552,21.6055654018176,
12.));
#243180=CARTESIAN_POINT('Ctrl Pts',(-10.7858084708261,21.6205198677173,
12.));
#243181=CARTESIAN_POINT('Ctrl Pts',(-10.8022189912369,21.6354975534557,
12.));
#243182=CARTESIAN_POINT('Ctrl Pts',(-10.8187386025136,21.6504977276866,
12.));
#243183=CARTESIAN_POINT('Ctrl Pts',(-10.8353670392272,21.6655196669732,
12.));
#243184=CARTESIAN_POINT('Ctrl Pts',(-10.8521040371835,21.6805626556467,
12.));
#243185=CARTESIAN_POINT('Ctrl Pts',(-10.8689493334095,21.6956259856672,
12.));
#243186=CARTESIAN_POINT('Ctrl Pts',(-10.8859026661293,21.7107089564825,
12.));
#243187=CARTESIAN_POINT('Ctrl Pts',(-10.902963774734,21.7258108748873,12.));
#243188=CARTESIAN_POINT('Ctrl Pts',(-10.9201323997384,21.7409310548797,
12.));
#243189=CARTESIAN_POINT('Ctrl Pts',(-10.9374082827444,21.7560688175247,
12.));
#243190=CARTESIAN_POINT('Ctrl Pts',(-10.9547911664455,21.7712234908464,
12.));
#243191=CARTESIAN_POINT('Ctrl Pts',(-10.9722807946156,21.7863944097141,
12.));
#243192=CARTESIAN_POINT('Ctrl Pts',(-10.9898769120912,21.8015809157301,
12.));
#243193=CARTESIAN_POINT('Ctrl Pts',(-11.0075792647477,21.8167823571168,
12.));
#243194=CARTESIAN_POINT('Ctrl Pts',(-11.0253875994598,21.8319980886033,
12.));
#243195=CARTESIAN_POINT('Ctrl Pts',(-11.0433016640807,21.8472274713103,
12.));
#243196=CARTESIAN_POINT('Ctrl Pts',(-11.0613212074363,21.8624698726318,
12.));
#243197=CARTESIAN_POINT('Ctrl Pts',(-11.0794459793057,21.877724666119,12.));
#243198=CARTESIAN_POINT('Ctrl Pts',(-11.0976757303944,21.8929912313608,
12.));
#243199=CARTESIAN_POINT('Ctrl Pts',(-11.1160102123024,21.9082689538688,
12.));
#243200=CARTESIAN_POINT('Ctrl Pts',(-11.1344491774741,21.923557224952,12.));
#243201=CARTESIAN_POINT('Ctrl Pts',(-11.1529923792003,21.9388554416439,
12.));
#243202=CARTESIAN_POINT('Ctrl Pts',(-11.1716395716376,21.9541630066506,
12.));
#243203=CARTESIAN_POINT('Ctrl Pts',(-11.190390509811,21.9694793282914,12.));
#243204=CARTESIAN_POINT('Ctrl Pts',(-11.2092449496125,21.9848038204439,
12.));
#243205=CARTESIAN_POINT('Ctrl Pts',(-11.2282026477896,22.0001359024839,
12.));
#243206=CARTESIAN_POINT('Ctrl Pts',(-11.2472633619275,22.0154749992363,
12.));
#243207=CARTESIAN_POINT('Ctrl Pts',(-11.2664268504206,22.030820540835,12.));
#243208=CARTESIAN_POINT('Ctrl Pts',(-11.2856928724374,22.046171962566,12.));
#243209=CARTESIAN_POINT('Ctrl Pts',(-11.3050611878771,22.0615287047179,
12.));
#243210=CARTESIAN_POINT('Ctrl Pts',(-11.3245315573168,22.0768902124267,
12.));
#243211=CARTESIAN_POINT('Ctrl Pts',(-11.3441037419553,22.0922559355294,
12.));
#243212=CARTESIAN_POINT('Ctrl Pts',(-11.3637775035367,22.1076253283979,
12.));
#243213=CARTESIAN_POINT('Ctrl Pts',(-11.3835526044256,22.1229978500186,
12.));
#243214=CARTESIAN_POINT('Ctrl Pts',(-11.4034288076908,22.1383729640964,
12.));
#243215=CARTESIAN_POINT('Ctrl Pts',(-11.4234058771742,22.1537501391487,
12.));
#243216=CARTESIAN_POINT('Ctrl Pts',(-11.443483577557,22.1691288486096,12.));
#243217=CARTESIAN_POINT('Ctrl Pts',(-11.463661674411,22.184508570917,12.));
#243218=CARTESIAN_POINT('Ctrl Pts',(-11.483939934259,22.1998887896436,12.));
#243219=CARTESIAN_POINT('Ctrl Pts',(-11.5043181244242,22.2152689931022,
12.));
#243220=CARTESIAN_POINT('Ctrl Pts',(-11.5247960128477,22.2306486738901,
12.));
#243221=CARTESIAN_POINT('Ctrl Pts',(-11.5453733679121,22.2460273284654,
12.));
#243222=CARTESIAN_POINT('Ctrl Pts',(-11.5660499582403,22.2614044566898,
12.));
#243223=CARTESIAN_POINT('Ctrl Pts',(-11.5868255525188,22.2767795614348,
12.));
#243224=CARTESIAN_POINT('Ctrl Pts',(-11.6076999192357,22.2921521480356,
12.));
#243225=CARTESIAN_POINT('Ctrl Pts',(-11.6286728270009,22.3075217249049,
12.));
#243226=CARTESIAN_POINT('Ctrl Pts',(-11.6497440449857,22.3228878043976,
12.));
#243227=CARTESIAN_POINT('Ctrl Pts',(-11.6709133432985,22.3382499035619,
12.));
#243228=CARTESIAN_POINT('Ctrl Pts',(-11.6921804934056,22.3536075450029,
12.));
#243229=CARTESIAN_POINT('Ctrl Pts',(-11.7135452684532,22.3689602575491,
12.));
#243230=CARTESIAN_POINT('Ctrl Pts',(-11.7350074437961,22.3843075773899,
12.));
#243231=CARTESIAN_POINT('Ctrl Pts',(-11.7565667964764,22.3996490469191,
12.));
#243232=CARTESIAN_POINT('Ctrl Pts',(-11.7782231042039,22.4149842125008,
12.));
#243233=CARTESIAN_POINT('Ctrl Pts',(-11.7999761445173,22.430312622646,12.));
#243234=CARTESIAN_POINT('Ctrl Pts',(-11.8218256937889,22.4456338258735,
12.));
#243235=CARTESIAN_POINT('Ctrl Pts',(-11.8437715264487,22.4609473690471,
12.));
#243236=CARTESIAN_POINT('Ctrl Pts',(-11.8658134137019,22.4762527946702,
12.));
#243237=CARTESIAN_POINT('Ctrl Pts',(-11.8879511239943,22.4915496418485,
12.));
#243238=CARTESIAN_POINT('Ctrl Pts',(-11.9101844254557,22.5068374513973,
12.));
#243239=CARTESIAN_POINT('Ctrl Pts',(-11.9325130877803,22.5221157697883,
12.));
#243240=CARTESIAN_POINT('Ctrl Pts',(-11.9549368843997,22.5373841537307,
12.));
#243241=CARTESIAN_POINT('Ctrl Pts',(-11.9774555943496,22.5526421741158,
12.));
#243242=CARTESIAN_POINT('Ctrl Pts',(-12.0000690046695,22.5678894211181,
12.));
#243243=CARTESIAN_POINT('Ctrl Pts',(-12.0227769113127,22.5831255061282,
12.));
#243244=CARTESIAN_POINT('Ctrl Pts',(-12.0455791139128,22.5983500505644,
12.));
#243245=CARTESIAN_POINT('Ctrl Pts',(-12.0684754113862,22.6135626764898,
12.));
#243246=CARTESIAN_POINT('Ctrl Pts',(-12.0914655972823,22.6287629967056,
12.));
#243247=CARTESIAN_POINT('Ctrl Pts',(-12.1145494550383,22.6439506046605,
12.));
#243248=CARTESIAN_POINT('Ctrl Pts',(-12.1377267537145,22.6591250653965,
12.));
#243249=CARTESIAN_POINT('Ctrl Pts',(-12.1609972423099,22.6742859034944,
12.));
#243250=CARTESIAN_POINT('Ctrl Pts',(-12.1843606579262,22.6894326205037,
12.));
#243251=CARTESIAN_POINT('Ctrl Pts',(-12.2078167360284,22.7045647168747,
12.));
#243252=CARTESIAN_POINT('Ctrl Pts',(-12.2313652198061,22.7196817119374,
12.));
#243253=CARTESIAN_POINT('Ctrl Pts',(-12.2550058702395,22.7347831655287,
12.));
#243254=CARTESIAN_POINT('Ctrl Pts',(-12.2787384750742,22.7498686970069,
12.));
#243255=CARTESIAN_POINT('Ctrl Pts',(-12.3025628601792,22.764938010105,12.));
#243256=CARTESIAN_POINT('Ctrl Pts',(-12.3264788926075,22.7799908974768,
12.));
#243257=CARTESIAN_POINT('Ctrl Pts',(-12.3504864740319,22.795027221673,12.));
#243258=CARTESIAN_POINT('Ctrl Pts',(-12.374585536673,22.81004690224,12.));
#243259=CARTESIAN_POINT('Ctrl Pts',(-12.3939379378998,22.8220493007173,
12.));
#243260=CARTESIAN_POINT('Ctrl Pts',(-12.4084933766347,22.8310435872747,
12.));
#243261=CARTESIAN_POINT('Ctrl Pts',(-12.418215285186,22.8370364396459,12.));
#243262=CARTESIAN_POINT('Ctrl Pts',(-12.4230808101438,22.8400320311648,
12.));
#243263=CARTESIAN_POINT('Ctrl Pts',(-7.52250298901264,21.2610617890679,
0.));
#243264=CARTESIAN_POINT('Ctrl Pts',(-7.52250298901264,21.2610617890679,
12.));
#243265=CARTESIAN_POINT('Ctrl Pts',(-7.5225064970397,21.2610673466886,0.));
#243266=CARTESIAN_POINT('Ctrl Pts',(-7.5225064970397,21.2610673466886,12.));
#243267=CARTESIAN_POINT('Ctrl Pts',(-7.52252744144904,21.2611204474866,
0.));
#243268=CARTESIAN_POINT('Ctrl Pts',(-7.52252744144904,21.2611204474866,
12.));
#243269=CARTESIAN_POINT('Ctrl Pts',(-7.52260064231661,21.261326054066,0.));
#243270=CARTESIAN_POINT('Ctrl Pts',(-7.52260064231661,21.261326054066,12.));
#243271=CARTESIAN_POINT('Ctrl Pts',(-7.5227818224267,21.2618521283555,0.));
#243272=CARTESIAN_POINT('Ctrl Pts',(-7.5227818224267,21.2618521283555,12.));
#243273=CARTESIAN_POINT('Ctrl Pts',(-7.52314642316199,21.262927782038,0.));
#243274=CARTESIAN_POINT('Ctrl Pts',(-7.52314642316199,21.262927782038,12.));
#243275=CARTESIAN_POINT('Ctrl Pts',(-7.52364573027553,21.2644161259962,
0.));
#243276=CARTESIAN_POINT('Ctrl Pts',(-7.52364573027553,21.2644161259962,
12.));
#243277=CARTESIAN_POINT('Ctrl Pts',(-7.52427261074298,21.2663059157058,
0.));
#243278=CARTESIAN_POINT('Ctrl Pts',(-7.52427261074298,21.2663059157058,
12.));
#243279=CARTESIAN_POINT('Ctrl Pts',(-7.5250177033353,21.2685823838671,0.));
#243280=CARTESIAN_POINT('Ctrl Pts',(-7.5250177033353,21.2685823838671,12.));
#243281=CARTESIAN_POINT('Ctrl Pts',(-7.5258712609553,21.2712301573466,0.));
#243282=CARTESIAN_POINT('Ctrl Pts',(-7.5258712609553,21.2712301573466,12.));
#243283=CARTESIAN_POINT('Ctrl Pts',(-7.52682526918541,21.2742366113579,
0.));
#243284=CARTESIAN_POINT('Ctrl Pts',(-7.52682526918541,21.2742366113579,
12.));
#243285=CARTESIAN_POINT('Ctrl Pts',(-7.52787386225333,21.2775925269652,
0.));
#243286=CARTESIAN_POINT('Ctrl Pts',(-7.52787386225333,21.2775925269652,
12.));
#243287=CARTESIAN_POINT('Ctrl Pts',(-7.52901217930408,21.2812902781143,
0.));
#243288=CARTESIAN_POINT('Ctrl Pts',(-7.52901217930408,21.2812902781143,
12.));
#243289=CARTESIAN_POINT('Ctrl Pts',(-7.53023562438229,21.2853226580657,
0.));
#243290=CARTESIAN_POINT('Ctrl Pts',(-7.53023562438229,21.2853226580657,
12.));
#243291=CARTESIAN_POINT('Ctrl Pts',(-7.53153906987855,21.2896816163842,
0.));
#243292=CARTESIAN_POINT('Ctrl Pts',(-7.53153906987855,21.2896816163842,
12.));
#243293=CARTESIAN_POINT('Ctrl Pts',(-7.53291726078527,21.2943588989331,
0.));
#243294=CARTESIAN_POINT('Ctrl Pts',(-7.53291726078527,21.2943588989331,
12.));
#243295=CARTESIAN_POINT('Ctrl Pts',(-7.53436505309943,21.2993464250717,
0.));
#243296=CARTESIAN_POINT('Ctrl Pts',(-7.53436505309943,21.2993464250717,
12.));
#243297=CARTESIAN_POINT('Ctrl Pts',(-7.53587778251736,21.3046368712157,
0.));
#243298=CARTESIAN_POINT('Ctrl Pts',(-7.53587778251736,21.3046368712157,
12.));
#243299=CARTESIAN_POINT('Ctrl Pts',(-7.53745129364616,21.310223716773,0.));
#243300=CARTESIAN_POINT('Ctrl Pts',(-7.53745129364616,21.310223716773,12.));
#243301=CARTESIAN_POINT('Ctrl Pts',(-7.53908175169898,21.3161009456256,
0.));
#243302=CARTESIAN_POINT('Ctrl Pts',(-7.53908175169898,21.3161009456256,
12.));
#243303=CARTESIAN_POINT('Ctrl Pts',(-7.54076552038279,21.3222628524165,
0.));
#243304=CARTESIAN_POINT('Ctrl Pts',(-7.54076552038279,21.3222628524165,
12.));
#243305=CARTESIAN_POINT('Ctrl Pts',(-7.54249900377031,21.328703791771,0.));
#243306=CARTESIAN_POINT('Ctrl Pts',(-7.54249900377031,21.328703791771,12.));
#243307=CARTESIAN_POINT('Ctrl Pts',(-7.54427868151268,21.3354182340149,
0.));
#243308=CARTESIAN_POINT('Ctrl Pts',(-7.54427868151268,21.3354182340149,
12.));
#243309=CARTESIAN_POINT('Ctrl Pts',(-7.54610114948347,21.3424008295038,
0.));
#243310=CARTESIAN_POINT('Ctrl Pts',(-7.54610114948347,21.3424008295038,
12.));
#243311=CARTESIAN_POINT('Ctrl Pts',(-7.5479631624633,21.3496464761531,0.));
#243312=CARTESIAN_POINT('Ctrl Pts',(-7.5479631624633,21.3496464761531,12.));
#243313=CARTESIAN_POINT('Ctrl Pts',(-7.5498616652131,21.3571503685855,0.));
#243314=CARTESIAN_POINT('Ctrl Pts',(-7.5498616652131,21.3571503685855,12.));
#243315=CARTESIAN_POINT('Ctrl Pts',(-7.55179375777444,21.3649079431865,
0.));
#243316=CARTESIAN_POINT('Ctrl Pts',(-7.55179375777444,21.3649079431865,
12.));
#243317=CARTESIAN_POINT('Ctrl Pts',(-7.55375667080029,21.3729148390243,
0.));
#243318=CARTESIAN_POINT('Ctrl Pts',(-7.55375667080029,21.3729148390243,
12.));
#243319=CARTESIAN_POINT('Ctrl Pts',(-7.55574773403503,21.3811668478932,
0.));
#243320=CARTESIAN_POINT('Ctrl Pts',(-7.55574773403503,21.3811668478932,
12.));
#243321=CARTESIAN_POINT('Ctrl Pts',(-7.55776435731417,21.3896598842117,
0.));
#243322=CARTESIAN_POINT('Ctrl Pts',(-7.55776435731417,21.3896598842117,
12.));
#243323=CARTESIAN_POINT('Ctrl Pts',(-7.55980403700611,21.3983899952987,
0.));
#243324=CARTESIAN_POINT('Ctrl Pts',(-7.55980403700611,21.3983899952987,
12.));
#243325=CARTESIAN_POINT('Ctrl Pts',(-7.56186435703622,21.4073533630365,
0.));
#243326=CARTESIAN_POINT('Ctrl Pts',(-7.56186435703622,21.4073533630365,
12.));
#243327=CARTESIAN_POINT('Ctrl Pts',(-7.56394299313685,21.4165463106254,
0.));
#243328=CARTESIAN_POINT('Ctrl Pts',(-7.56394299313685,21.4165463106254,
12.));
#243329=CARTESIAN_POINT('Ctrl Pts',(-7.56603771218712,21.4259653015736,
0.));
#243330=CARTESIAN_POINT('Ctrl Pts',(-7.56603771218712,21.4259653015736,
12.));
#243331=CARTESIAN_POINT('Ctrl Pts',(-7.56814636360847,21.4356069261513,
0.));
#243332=CARTESIAN_POINT('Ctrl Pts',(-7.56814636360847,21.4356069261513,
12.));
#243333=CARTESIAN_POINT('Ctrl Pts',(-7.57026687261166,21.4454678907509,
0.));
#243334=CARTESIAN_POINT('Ctrl Pts',(-7.57026687261166,21.4454678907509,
12.));
#243335=CARTESIAN_POINT('Ctrl Pts',(-7.57239723223506,21.4555450053142,
0.));
#243336=CARTESIAN_POINT('Ctrl Pts',(-7.57239723223506,21.4555450053142,
12.));
#243337=CARTESIAN_POINT('Ctrl Pts',(-7.57453549743412,21.4658351740128,
0.));
#243338=CARTESIAN_POINT('Ctrl Pts',(-7.57453549743412,21.4658351740128,
12.));
#243339=CARTESIAN_POINT('Ctrl Pts',(-7.57667978402987,21.4763353936762,
0.));
#243340=CARTESIAN_POINT('Ctrl Pts',(-7.57667978402987,21.4763353936762,
12.));
#243341=CARTESIAN_POINT('Ctrl Pts',(-7.57882826679132,21.4870427508194,
0.));
#243342=CARTESIAN_POINT('Ctrl Pts',(-7.57882826679132,21.4870427508194,
12.));
#243343=CARTESIAN_POINT('Ctrl Pts',(-7.58097917790744,21.4979544192744,
0.));
#243344=CARTESIAN_POINT('Ctrl Pts',(-7.58097917790744,21.4979544192744,
12.));
#243345=CARTESIAN_POINT('Ctrl Pts',(-7.5831308051918,21.5090676573873,0.));
#243346=CARTESIAN_POINT('Ctrl Pts',(-7.5831308051918,21.5090676573873,12.));
#243347=CARTESIAN_POINT('Ctrl Pts',(-7.5852814891913,21.5203798035299,0.));
#243348=CARTESIAN_POINT('Ctrl Pts',(-7.5852814891913,21.5203798035299,12.));
#243349=CARTESIAN_POINT('Ctrl Pts',(-7.58742962034834,21.5318882716736,
0.));
#243350=CARTESIAN_POINT('Ctrl Pts',(-7.58742962034834,21.5318882716736,
12.));
#243351=CARTESIAN_POINT('Ctrl Pts',(-7.58957363620014,21.543590547011,0.));
#243352=CARTESIAN_POINT('Ctrl Pts',(-7.58957363620014,21.543590547011,12.));
#243353=CARTESIAN_POINT('Ctrl Pts',(-7.59171201844777,21.5554841813462,
0.));
#243354=CARTESIAN_POINT('Ctrl Pts',(-7.59171201844777,21.5554841813462,
12.));
#243355=CARTESIAN_POINT('Ctrl Pts',(-7.59384329124918,21.5675667904726,
0.));
#243356=CARTESIAN_POINT('Ctrl Pts',(-7.59384329124918,21.5675667904726,
12.));
#243357=CARTESIAN_POINT('Ctrl Pts',(-7.59596601973584,21.5798360518978,
0.));
#243358=CARTESIAN_POINT('Ctrl Pts',(-7.59596601973584,21.5798360518978,
12.));
#243359=CARTESIAN_POINT('Ctrl Pts',(-7.59807880846195,21.5922897024466,
0.));
#243360=CARTESIAN_POINT('Ctrl Pts',(-7.59807880846195,21.5922897024466,
12.));
#243361=CARTESIAN_POINT('Ctrl Pts',(-7.60018029988241,21.6049255358843,
0.));
#243362=CARTESIAN_POINT('Ctrl Pts',(-7.60018029988241,21.6049255358843,
12.));
#243363=CARTESIAN_POINT('Ctrl Pts',(-7.60226917285429,21.617741400599,0.));
#243364=CARTESIAN_POINT('Ctrl Pts',(-7.60226917285429,21.617741400599,12.));
#243365=CARTESIAN_POINT('Ctrl Pts',(-7.60434414118296,21.6307351973822,
0.));
#243366=CARTESIAN_POINT('Ctrl Pts',(-7.60434414118296,21.6307351973822,
12.));
#243367=CARTESIAN_POINT('Ctrl Pts',(-7.60640395216357,21.6439048771743,
0.));
#243368=CARTESIAN_POINT('Ctrl Pts',(-7.60640395216357,21.6439048771743,
12.));
#243369=CARTESIAN_POINT('Ctrl Pts',(-7.60844738512874,21.6572484388081,
0.));
#243370=CARTESIAN_POINT('Ctrl Pts',(-7.60844738512874,21.6572484388081,
12.));
#243371=CARTESIAN_POINT('Ctrl Pts',(-7.61047325000956,21.6707639267576,
0.));
#243372=CARTESIAN_POINT('Ctrl Pts',(-7.61047325000956,21.6707639267576,
12.));
#243373=CARTESIAN_POINT('Ctrl Pts',(-7.61248038630268,21.6844494295815,
0.));
#243374=CARTESIAN_POINT('Ctrl Pts',(-7.61248038630268,21.6844494295815,
12.));
#243375=CARTESIAN_POINT('Ctrl Pts',(-7.61446766202787,21.6983030783322,
0.));
#243376=CARTESIAN_POINT('Ctrl Pts',(-7.61446766202787,21.6983030783322,
12.));
#243377=CARTESIAN_POINT('Ctrl Pts',(-7.61643397270421,21.7123230449834,
0.));
#243378=CARTESIAN_POINT('Ctrl Pts',(-7.61643397270421,21.7123230449834,
12.));
#243379=CARTESIAN_POINT('Ctrl Pts',(-7.61837824030538,21.7265075407975,
0.));
#243380=CARTESIAN_POINT('Ctrl Pts',(-7.61837824030538,21.7265075407975,
12.));
#243381=CARTESIAN_POINT('Ctrl Pts',(-7.62029941230855,21.7408548148656,
0.));
#243382=CARTESIAN_POINT('Ctrl Pts',(-7.62029941230855,21.7408548148656,
12.));
#243383=CARTESIAN_POINT('Ctrl Pts',(-7.62219646084228,21.7553631528328,
0.));
#243384=CARTESIAN_POINT('Ctrl Pts',(-7.62219646084228,21.7553631528328,
12.));
#243385=CARTESIAN_POINT('Ctrl Pts',(-7.62406838181166,21.7700308755584,
0.));
#243386=CARTESIAN_POINT('Ctrl Pts',(-7.62406838181166,21.7700308755584,
12.));
#243387=CARTESIAN_POINT('Ctrl Pts',(-7.62591419404512,21.7848563378021,
0.));
#243388=CARTESIAN_POINT('Ctrl Pts',(-7.62591419404512,21.7848563378021,
12.));
#243389=CARTESIAN_POINT('Ctrl Pts',(-7.62773293842389,21.799837926858,0.));
#243390=CARTESIAN_POINT('Ctrl Pts',(-7.62773293842389,21.799837926858,12.));
#243391=CARTESIAN_POINT('Ctrl Pts',(-7.62952367718127,21.814974061509,0.));
#243392=CARTESIAN_POINT('Ctrl Pts',(-7.62952367718127,21.814974061509,12.));
#243393=CARTESIAN_POINT('Ctrl Pts',(-7.63128549323023,21.8302631910195,
0.));
#243394=CARTESIAN_POINT('Ctrl Pts',(-7.63128549323023,21.8302631910195,
12.));
#243395=CARTESIAN_POINT('Ctrl Pts',(-7.63301748948936,21.8457037941084,
0.));
#243396=CARTESIAN_POINT('Ctrl Pts',(-7.63301748948936,21.8457037941084,
12.));
#243397=CARTESIAN_POINT('Ctrl Pts',(-7.63471878821226,21.8612943779089,
0.));
#243398=CARTESIAN_POINT('Ctrl Pts',(-7.63471878821226,21.8612943779089,
12.));
#243399=CARTESIAN_POINT('Ctrl Pts',(-7.636388530334,21.8770334769496,0.));
#243400=CARTESIAN_POINT('Ctrl Pts',(-7.636388530334,21.8770334769496,12.));
#243401=CARTESIAN_POINT('Ctrl Pts',(-7.63802587492035,21.8929196523514,
0.));
#243402=CARTESIAN_POINT('Ctrl Pts',(-7.63802587492035,21.8929196523514,
12.));
#243403=CARTESIAN_POINT('Ctrl Pts',(-7.63962999860927,21.9089514909874,
0.));
#243404=CARTESIAN_POINT('Ctrl Pts',(-7.63962999860927,21.9089514909874,
12.));
#243405=CARTESIAN_POINT('Ctrl Pts',(-7.64120009506532,21.9251276046546,
0.));
#243406=CARTESIAN_POINT('Ctrl Pts',(-7.64120009506532,21.9251276046546,
12.));
#243407=CARTESIAN_POINT('Ctrl Pts',(-7.64273537442682,21.9414466292072,
0.));
#243408=CARTESIAN_POINT('Ctrl Pts',(-7.64273537442682,21.9414466292072,
12.));
#243409=CARTESIAN_POINT('Ctrl Pts',(-7.64423506279123,21.9579072237651,
0.));
#243410=CARTESIAN_POINT('Ctrl Pts',(-7.64423506279123,21.9579072237651,
12.));
#243411=CARTESIAN_POINT('Ctrl Pts',(-7.64569840177336,21.9745080700798,
0.));
#243412=CARTESIAN_POINT('Ctrl Pts',(-7.64569840177336,21.9745080700798,
12.));
#243413=CARTESIAN_POINT('Ctrl Pts',(-7.6471246480525,21.9912478718542,0.));
#243414=CARTESIAN_POINT('Ctrl Pts',(-7.6471246480525,21.9912478718542,12.));
#243415=CARTESIAN_POINT('Ctrl Pts',(-7.64851307293352,22.0081253540774,
0.));
#243416=CARTESIAN_POINT('Ctrl Pts',(-7.64851307293352,22.0081253540774,
12.));
#243417=CARTESIAN_POINT('Ctrl Pts',(-7.64986296190168,22.0251392623209,
0.));
#243418=CARTESIAN_POINT('Ctrl Pts',(-7.64986296190168,22.0251392623209,
12.));
#243419=CARTESIAN_POINT('Ctrl Pts',(-7.65117361421358,22.0422883621174,
0.));
#243420=CARTESIAN_POINT('Ctrl Pts',(-7.65117361421358,22.0422883621174,
12.));
#243421=CARTESIAN_POINT('Ctrl Pts',(-7.65244434253113,22.0595714384431,
0.));
#243422=CARTESIAN_POINT('Ctrl Pts',(-7.65244434253113,22.0595714384431,
12.));
#243423=CARTESIAN_POINT('Ctrl Pts',(-7.65367447254949,22.0769872951596,
0.));
#243424=CARTESIAN_POINT('Ctrl Pts',(-7.65367447254949,22.0769872951596,
12.));
#243425=CARTESIAN_POINT('Ctrl Pts',(-7.65486334263644,22.094534754469,0.));
#243426=CARTESIAN_POINT('Ctrl Pts',(-7.65486334263644,22.094534754469,12.));
#243427=CARTESIAN_POINT('Ctrl Pts',(-7.65601030346807,22.1122126563329,
0.));
#243428=CARTESIAN_POINT('Ctrl Pts',(-7.65601030346807,22.1122126563329,
12.));
#243429=CARTESIAN_POINT('Ctrl Pts',(-7.65711471769397,22.1300198579675,
0.));
#243430=CARTESIAN_POINT('Ctrl Pts',(-7.65711471769397,22.1300198579675,
12.));
#243431=CARTESIAN_POINT('Ctrl Pts',(-7.65817595963349,22.1479552334211,
0.));
#243432=CARTESIAN_POINT('Ctrl Pts',(-7.65817595963349,22.1479552334211,
12.));
#243433=CARTESIAN_POINT('Ctrl Pts',(-7.6591934149693,22.1660176731178,0.));
#243434=CARTESIAN_POINT('Ctrl Pts',(-7.6591934149693,22.1660176731178,12.));
#243435=CARTESIAN_POINT('Ctrl Pts',(-7.66016648045005,22.1842060834091,
0.));
#243436=CARTESIAN_POINT('Ctrl Pts',(-7.66016648045005,22.1842060834091,
12.));
#243437=CARTESIAN_POINT('Ctrl Pts',(-7.66109456359271,22.2025193860964,
0.));
#243438=CARTESIAN_POINT('Ctrl Pts',(-7.66109456359271,22.2025193860964,
12.));
#243439=CARTESIAN_POINT('Ctrl Pts',(-7.661977082404,22.2209565180085,0.));
#243440=CARTESIAN_POINT('Ctrl Pts',(-7.661977082404,22.2209565180085,12.));
#243441=CARTESIAN_POINT('Ctrl Pts',(-7.66281346512509,22.2395164306547,
0.));
#243442=CARTESIAN_POINT('Ctrl Pts',(-7.66281346512509,22.2395164306547,
12.));
#243443=CARTESIAN_POINT('Ctrl Pts',(-7.66360314997641,22.258198089848,0.));
#243444=CARTESIAN_POINT('Ctrl Pts',(-7.66360314997641,22.258198089848,12.));
#243445=CARTESIAN_POINT('Ctrl Pts',(-7.66434558490979,22.2770004753335,
0.));
#243446=CARTESIAN_POINT('Ctrl Pts',(-7.66434558490979,22.2770004753335,
12.));
#243447=CARTESIAN_POINT('Ctrl Pts',(-7.66504022736299,22.2959225803937,
0.));
#243448=CARTESIAN_POINT('Ctrl Pts',(-7.66504022736299,22.2959225803937,
12.));
#243449=CARTESIAN_POINT('Ctrl Pts',(-7.66568654402494,22.314963411484,0.));
#243450=CARTESIAN_POINT('Ctrl Pts',(-7.66568654402494,22.314963411484,12.));
#243451=CARTESIAN_POINT('Ctrl Pts',(-7.66628401061952,22.3341219879469,
0.));
#243452=CARTESIAN_POINT('Ctrl Pts',(-7.66628401061952,22.3341219879469,
12.));
#243453=CARTESIAN_POINT('Ctrl Pts',(-7.66683211169158,22.3533973417021,
0.));
#243454=CARTESIAN_POINT('Ctrl Pts',(-7.66683211169158,22.3533973417021,
12.));
#243455=CARTESIAN_POINT('Ctrl Pts',(-7.66733034039883,22.372788516936,0.));
#243456=CARTESIAN_POINT('Ctrl Pts',(-7.66733034039883,22.372788516936,12.));
#243457=CARTESIAN_POINT('Ctrl Pts',(-7.6677781983079,22.3922945697773,0.));
#243458=CARTESIAN_POINT('Ctrl Pts',(-7.6677781983079,22.3922945697773,12.));
#243459=CARTESIAN_POINT('Ctrl Pts',(-7.6681751951964,22.4119145679758,0.));
#243460=CARTESIAN_POINT('Ctrl Pts',(-7.6681751951964,22.4119145679758,12.));
#243461=CARTESIAN_POINT('Ctrl Pts',(-7.66852084886704,22.4316475906603,
0.));
#243462=CARTESIAN_POINT('Ctrl Pts',(-7.66852084886704,22.4316475906603,
12.));
#243463=CARTESIAN_POINT('Ctrl Pts',(-7.66881468496635,22.4514927280855,
0.));
#243464=CARTESIAN_POINT('Ctrl Pts',(-7.66881468496635,22.4514927280855,
12.));
#243465=CARTESIAN_POINT('Ctrl Pts',(-7.66905623680831,22.47144908137,0.));
#243466=CARTESIAN_POINT('Ctrl Pts',(-7.66905623680831,22.47144908137,12.));
#243467=CARTESIAN_POINT('Ctrl Pts',(-7.66924504520315,22.4915157622312,
0.));
#243468=CARTESIAN_POINT('Ctrl Pts',(-7.66924504520315,22.4915157622312,
12.));
#243469=CARTESIAN_POINT('Ctrl Pts',(-7.66938065829108,22.5116918927031,
0.));
#243470=CARTESIAN_POINT('Ctrl Pts',(-7.66938065829108,22.5116918927031,
12.));
#243471=CARTESIAN_POINT('Ctrl Pts',(-7.66946263138144,22.53197660492,0.));
#243472=CARTESIAN_POINT('Ctrl Pts',(-7.66946263138144,22.53197660492,12.));
#243473=CARTESIAN_POINT('Ctrl Pts',(-7.66949052679693,22.5523690409116,
0.));
#243474=CARTESIAN_POINT('Ctrl Pts',(-7.66949052679693,22.5523690409116,
12.));
#243475=CARTESIAN_POINT('Ctrl Pts',(-7.66946391372306,22.5728683523831,
0.));
#243476=CARTESIAN_POINT('Ctrl Pts',(-7.66946391372306,22.5728683523831,
12.));
#243477=CARTESIAN_POINT('Ctrl Pts',(-7.66938236806233,22.5934737004953,
0.));
#243478=CARTESIAN_POINT('Ctrl Pts',(-7.66938236806233,22.5934737004953,
12.));
#243479=CARTESIAN_POINT('Ctrl Pts',(-7.66924547229414,22.6141842556243,
0.));
#243480=CARTESIAN_POINT('Ctrl Pts',(-7.66924547229414,22.6141842556243,
12.));
#243481=CARTESIAN_POINT('Ctrl Pts',(-7.66905281533715,22.6349991971541,
0.));
#243482=CARTESIAN_POINT('Ctrl Pts',(-7.66905281533715,22.6349991971541,
12.));
#243483=CARTESIAN_POINT('Ctrl Pts',(-7.66880399241323,22.6559177133127,
0.));
#243484=CARTESIAN_POINT('Ctrl Pts',(-7.66880399241323,22.6559177133127,
12.));
#243485=CARTESIAN_POINT('Ctrl Pts',(-7.66849860491743,22.6769390009885,
0.));
#243486=CARTESIAN_POINT('Ctrl Pts',(-7.66849860491743,22.6769390009885,
12.));
#243487=CARTESIAN_POINT('Ctrl Pts',(-7.66813626029275,22.6980622655446,
0.));
#243488=CARTESIAN_POINT('Ctrl Pts',(-7.66813626029275,22.6980622655446,
12.));
#243489=CARTESIAN_POINT('Ctrl Pts',(-7.66771657191027,22.7192867206245,
0.));
#243490=CARTESIAN_POINT('Ctrl Pts',(-7.66771657191027,22.7192867206245,
12.));
#243491=CARTESIAN_POINT('Ctrl Pts',(-7.6672391589544,22.7406115879513,0.));
#243492=CARTESIAN_POINT('Ctrl Pts',(-7.6672391589544,22.7406115879513,12.));
#243493=CARTESIAN_POINT('Ctrl Pts',(-7.66670364630299,22.7620360971843,
0.));
#243494=CARTESIAN_POINT('Ctrl Pts',(-7.66670364630299,22.7620360971843,
12.));
#243495=CARTESIAN_POINT('Ctrl Pts',(-7.66610966441273,22.7835594857699,
0.));
#243496=CARTESIAN_POINT('Ctrl Pts',(-7.66610966441273,22.7835594857699,
12.));
#243497=CARTESIAN_POINT('Ctrl Pts',(-7.66545684920987,22.8051809987833,
0.));
#243498=CARTESIAN_POINT('Ctrl Pts',(-7.66545684920987,22.8051809987833,
12.));
#243499=CARTESIAN_POINT('Ctrl Pts',(-7.66474484198549,22.8268998887678,
0.));
#243500=CARTESIAN_POINT('Ctrl Pts',(-7.66474484198549,22.8268998887678,
12.));
#243501=CARTESIAN_POINT('Ctrl Pts',(-7.66397328929803,22.848715415557,0.));
#243502=CARTESIAN_POINT('Ctrl Pts',(-7.66397328929803,22.848715415557,12.));
#243503=CARTESIAN_POINT('Ctrl Pts',(-7.66314184287337,22.8706268461283,
0.));
#243504=CARTESIAN_POINT('Ctrl Pts',(-7.66314184287337,22.8706268461283,
12.));
#243505=CARTESIAN_POINT('Ctrl Pts',(-7.66225015950156,22.8926334544883,
0.));
#243506=CARTESIAN_POINT('Ctrl Pts',(-7.66225015950156,22.8926334544883,
12.));
#243507=CARTESIAN_POINT('Ctrl Pts',(-7.66129790094108,22.9147345215421,
0.));
#243508=CARTESIAN_POINT('Ctrl Pts',(-7.66129790094108,22.9147345215421,
12.));
#243509=CARTESIAN_POINT('Ctrl Pts',(-7.66028473382778,22.9369293349593,
0.));
#243510=CARTESIAN_POINT('Ctrl Pts',(-7.66028473382778,22.9369293349593,
12.));
#243511=CARTESIAN_POINT('Ctrl Pts',(-7.65921032958902,22.959217189033,0.));
#243512=CARTESIAN_POINT('Ctrl Pts',(-7.65921032958902,22.959217189033,12.));
#243513=CARTESIAN_POINT('Ctrl Pts',(-7.65807436436432,22.9815973845296,
0.));
#243514=CARTESIAN_POINT('Ctrl Pts',(-7.65807436436432,22.9815973845296,
12.));
#243515=CARTESIAN_POINT('Ctrl Pts',(-7.65687651891304,23.0040692285814,
0.));
#243516=CARTESIAN_POINT('Ctrl Pts',(-7.65687651891304,23.0040692285814,
12.));
#243517=CARTESIAN_POINT('Ctrl Pts',(-7.65561647852534,23.0266320345787,
0.));
#243518=CARTESIAN_POINT('Ctrl Pts',(-7.65561647852534,23.0266320345787,
12.));
#243519=CARTESIAN_POINT('Ctrl Pts',(-7.65429393293946,23.0492851220528,
0.));
#243520=CARTESIAN_POINT('Ctrl Pts',(-7.65429393293946,23.0492851220528,
12.));
#243521=CARTESIAN_POINT('Ctrl Pts',(-7.65290857626358,23.072027816555,0.));
#243522=CARTESIAN_POINT('Ctrl Pts',(-7.65290857626358,23.072027816555,12.));
#243523=CARTESIAN_POINT('Ctrl Pts',(-7.65146010690476,23.094859449525,0.));
#243524=CARTESIAN_POINT('Ctrl Pts',(-7.65146010690476,23.094859449525,12.));
#243525=CARTESIAN_POINT('Ctrl Pts',(-7.6499482274986,23.1177793581679,0.));
#243526=CARTESIAN_POINT('Ctrl Pts',(-7.6499482274986,23.1177793581679,12.));
#243527=CARTESIAN_POINT('Ctrl Pts',(-7.64837264482943,23.1407868853819,
0.));
#243528=CARTESIAN_POINT('Ctrl Pts',(-7.64837264482943,23.1407868853819,
12.));
#243529=CARTESIAN_POINT('Ctrl Pts',(-7.64673306975805,23.1638813796694,
0.));
#243530=CARTESIAN_POINT('Ctrl Pts',(-7.64673306975805,23.1638813796694,
12.));
#243531=CARTESIAN_POINT('Ctrl Pts',(-7.64502921715483,23.1870621950452,
0.));
#243532=CARTESIAN_POINT('Ctrl Pts',(-7.64502921715483,23.1870621950452,
12.));
#243533=CARTESIAN_POINT('Ctrl Pts',(-7.6432608058368,23.2103286909398,0.));
#243534=CARTESIAN_POINT('Ctrl Pts',(-7.6432608058368,23.2103286909398,12.));
#243535=CARTESIAN_POINT('Ctrl Pts',(-7.64142755851504,23.2336802320912,
0.));
#243536=CARTESIAN_POINT('Ctrl Pts',(-7.64142755851504,23.2336802320912,
12.));
#243537=CARTESIAN_POINT('Ctrl Pts',(-7.63952920172835,23.2571161884488,
0.));
#243538=CARTESIAN_POINT('Ctrl Pts',(-7.63952920172835,23.2571161884488,
12.));
#243539=CARTESIAN_POINT('Ctrl Pts',(-7.63756546576374,23.2806359350855,
0.));
#243540=CARTESIAN_POINT('Ctrl Pts',(-7.63756546576374,23.2806359350855,
12.));
#243541=CARTESIAN_POINT('Ctrl Pts',(-7.63553608458783,23.3042388521022,
0.));
#243542=CARTESIAN_POINT('Ctrl Pts',(-7.63553608458783,23.3042388521022,
12.));
#243543=CARTESIAN_POINT('Ctrl Pts',(-7.63344079578161,23.3279243245241,
0.));
#243544=CARTESIAN_POINT('Ctrl Pts',(-7.63344079578161,23.3279243245241,
12.));
#243545=CARTESIAN_POINT('Ctrl Pts',(-7.63127934048136,23.3516917421972,
0.));
#243546=CARTESIAN_POINT('Ctrl Pts',(-7.63127934048136,23.3516917421972,
12.));
#243547=CARTESIAN_POINT('Ctrl Pts',(-7.62905146332593,23.3755404996636,
0.));
#243548=CARTESIAN_POINT('Ctrl Pts',(-7.62905146332593,23.3755404996636,
12.));
#243549=CARTESIAN_POINT('Ctrl Pts',(-7.62675691240329,23.399469996112,0.));
#243550=CARTESIAN_POINT('Ctrl Pts',(-7.62675691240329,23.399469996112,12.));
#243551=CARTESIAN_POINT('Ctrl Pts',(-7.6243954392005,23.4234796353542,0.));
#243552=CARTESIAN_POINT('Ctrl Pts',(-7.6243954392005,23.4234796353542,12.));
#243553=CARTESIAN_POINT('Ctrl Pts',(-7.62196679855955,23.4475688257854,
0.));
#243554=CARTESIAN_POINT('Ctrl Pts',(-7.62196679855955,23.4475688257854,
12.));
#243555=CARTESIAN_POINT('Ctrl Pts',(-7.61947074863977,23.4717369803438,
0.));
#243556=CARTESIAN_POINT('Ctrl Pts',(-7.61947074863977,23.4717369803438,
12.));
#243557=CARTESIAN_POINT('Ctrl Pts',(-7.61690705088319,23.4959835164609,
0.));
#243558=CARTESIAN_POINT('Ctrl Pts',(-7.61690705088319,23.4959835164609,
12.));
#243559=CARTESIAN_POINT('Ctrl Pts',(-7.61427546999298,23.5203078560129,
0.));
#243560=CARTESIAN_POINT('Ctrl Pts',(-7.61427546999298,23.5203078560129,
12.));
#243561=CARTESIAN_POINT('Ctrl Pts',(-7.61157577385372,23.544709425203,0.));
#243562=CARTESIAN_POINT('Ctrl Pts',(-7.61157577385372,23.544709425203,12.));
#243563=CARTESIAN_POINT('Ctrl Pts',(-7.608807733446,23.5691876544244,0.));
#243564=CARTESIAN_POINT('Ctrl Pts',(-7.608807733446,23.5691876544244,12.));
#243565=CARTESIAN_POINT('Ctrl Pts',(-7.60597112277094,23.5937419781245,
0.));
#243566=CARTESIAN_POINT('Ctrl Pts',(-7.60597112277094,23.5937419781245,
12.));
#243567=CARTESIAN_POINT('Ctrl Pts',(-7.60306571877806,23.6183718346576,
0.));
#243568=CARTESIAN_POINT('Ctrl Pts',(-7.60306571877806,23.6183718346576,
12.));
#243569=CARTESIAN_POINT('Ctrl Pts',(-7.60009130130126,23.6430766661418,
0.));
#243570=CARTESIAN_POINT('Ctrl Pts',(-7.60009130130126,23.6430766661418,
12.));
#243571=CARTESIAN_POINT('Ctrl Pts',(-7.59704765299567,23.6678559182875,
0.));
#243572=CARTESIAN_POINT('Ctrl Pts',(-7.59704765299567,23.6678559182875,
12.));
#243573=CARTESIAN_POINT('Ctrl Pts',(-7.59393455934035,23.6927090405066,
0.));
#243574=CARTESIAN_POINT('Ctrl Pts',(-7.59393455934035,23.6927090405066,
12.));
#243575=CARTESIAN_POINT('Ctrl Pts',(-7.5907518086532,23.7176354860456,0.));
#243576=CARTESIAN_POINT('Ctrl Pts',(-7.5907518086532,23.7176354860456,12.));
#243577=CARTESIAN_POINT('Ctrl Pts',(-7.58749919210826,23.7426347121006,
0.));
#243578=CARTESIAN_POINT('Ctrl Pts',(-7.58749919210826,23.7426347121006,
12.));
#243579=CARTESIAN_POINT('Ctrl Pts',(-7.58417650376271,23.7677061799376,
0.));
#243580=CARTESIAN_POINT('Ctrl Pts',(-7.58417650376271,23.7677061799376,
12.));
#243581=CARTESIAN_POINT('Ctrl Pts',(-7.58078354058213,23.7928493549908,
0.));
#243582=CARTESIAN_POINT('Ctrl Pts',(-7.58078354058213,23.7928493549908,
12.));
#243583=CARTESIAN_POINT('Ctrl Pts',(-7.57732010249066,23.8180637069976,
0.));
#243584=CARTESIAN_POINT('Ctrl Pts',(-7.57732010249066,23.8180637069976,
12.));
#243585=CARTESIAN_POINT('Ctrl Pts',(-7.57378599219814,23.8433487096132,
0.));
#243586=CARTESIAN_POINT('Ctrl Pts',(-7.57378599219814,23.8433487096132,
12.));
#243587=CARTESIAN_POINT('Ctrl Pts',(-7.57018101500709,23.8687038399595,
0.));
#243588=CARTESIAN_POINT('Ctrl Pts',(-7.57018101500709,23.8687038399595,
12.));
#243589=CARTESIAN_POINT('Ctrl Pts',(-7.56650497863791,23.8941285782002,
0.));
#243590=CARTESIAN_POINT('Ctrl Pts',(-7.56650497863791,23.8941285782002,
12.));
#243591=CARTESIAN_POINT('Ctrl Pts',(-7.56275769304773,23.9196224070759,
0.));
#243592=CARTESIAN_POINT('Ctrl Pts',(-7.56275769304773,23.9196224070759,
12.));
#243593=CARTESIAN_POINT('Ctrl Pts',(-7.5589389702768,23.9451848115002,0.));
#243594=CARTESIAN_POINT('Ctrl Pts',(-7.5589389702768,23.9451848115002,12.));
#243595=CARTESIAN_POINT('Ctrl Pts',(-7.55504862424808,23.9708152779886,
0.));
#243596=CARTESIAN_POINT('Ctrl Pts',(-7.55504862424808,23.9708152779886,
12.));
#243597=CARTESIAN_POINT('Ctrl Pts',(-7.55108647097432,23.9965132953187,
0.));
#243598=CARTESIAN_POINT('Ctrl Pts',(-7.55108647097432,23.9965132953187,
12.));
#243599=CARTESIAN_POINT('Ctrl Pts',(-7.54705232885895,24.0222783554531,
0.));
#243600=CARTESIAN_POINT('Ctrl Pts',(-7.54705232885895,24.0222783554531,
12.));
#243601=CARTESIAN_POINT('Ctrl Pts',(-7.54294601896128,24.0481099543353,
0.));
#243602=CARTESIAN_POINT('Ctrl Pts',(-7.54294601896128,24.0481099543353,
12.));
#243603=CARTESIAN_POINT('Ctrl Pts',(-7.53876736531005,24.0740075927984,
0.));
#243604=CARTESIAN_POINT('Ctrl Pts',(-7.53876736531005,24.0740075927984,
12.));
#243605=CARTESIAN_POINT('Ctrl Pts',(-7.53451619514658,24.0999707772643,
0.));
#243606=CARTESIAN_POINT('Ctrl Pts',(-7.53451619514658,24.0999707772643,
12.));
#243607=CARTESIAN_POINT('Ctrl Pts',(-7.53019233935536,24.1259990209211,
0.));
#243608=CARTESIAN_POINT('Ctrl Pts',(-7.53019233935536,24.1259990209211,
12.));
#243609=CARTESIAN_POINT('Ctrl Pts',(-7.52579563201479,24.152091842537,0.));
#243610=CARTESIAN_POINT('Ctrl Pts',(-7.52579563201479,24.152091842537,12.));
#243611=CARTESIAN_POINT('Ctrl Pts',(-7.52132590953862,24.1782487641602,
0.));
#243612=CARTESIAN_POINT('Ctrl Pts',(-7.52132590953862,24.1782487641602,
12.));
#243613=CARTESIAN_POINT('Ctrl Pts',(-7.51678300997998,24.2044693092356,
0.));
#243614=CARTESIAN_POINT('Ctrl Pts',(-7.51678300997998,24.2044693092356,
12.));
#243615=CARTESIAN_POINT('Ctrl Pts',(-7.51216677222199,24.230753000389,0.));
#243616=CARTESIAN_POINT('Ctrl Pts',(-7.51216677222199,24.230753000389,12.));
#243617=CARTESIAN_POINT('Ctrl Pts',(-7.50747703535115,24.2570993577032,
0.));
#243618=CARTESIAN_POINT('Ctrl Pts',(-7.50747703535115,24.2570993577032,
12.));
#243619=CARTESIAN_POINT('Ctrl Pts',(-7.50271363765098,24.2835078958966,
0.));
#243620=CARTESIAN_POINT('Ctrl Pts',(-7.50271363765098,24.2835078958966,
12.));
#243621=CARTESIAN_POINT('Ctrl Pts',(-7.49787641695359,24.3099781253345,
0.));
#243622=CARTESIAN_POINT('Ctrl Pts',(-7.49787641695359,24.3099781253345,
12.));
#243623=CARTESIAN_POINT('Ctrl Pts',(-7.4929652125233,24.3365095573673,0.));
#243624=CARTESIAN_POINT('Ctrl Pts',(-7.4929652125233,24.3365095573673,12.));
#243625=CARTESIAN_POINT('Ctrl Pts',(-7.48797986651828,24.3631017084513,
0.));
#243626=CARTESIAN_POINT('Ctrl Pts',(-7.48797986651828,24.3631017084513,
12.));
#243627=CARTESIAN_POINT('Ctrl Pts',(-7.48292022569254,24.3897541049248,
0.));
#243628=CARTESIAN_POINT('Ctrl Pts',(-7.48292022569254,24.3897541049248,
12.));
#243629=CARTESIAN_POINT('Ctrl Pts',(-7.47778614286573,24.4164662871165,
0.));
#243630=CARTESIAN_POINT('Ctrl Pts',(-7.47778614286573,24.4164662871165,
12.));
#243631=CARTESIAN_POINT('Ctrl Pts',(-7.47257747883319,24.4432378146501,
0.));
#243632=CARTESIAN_POINT('Ctrl Pts',(-7.47257747883319,24.4432378146501,
12.));
#243633=CARTESIAN_POINT('Ctrl Pts',(-7.46729410308923,24.4700682684544,
0.));
#243634=CARTESIAN_POINT('Ctrl Pts',(-7.46729410308923,24.4700682684544,
12.));
#243635=CARTESIAN_POINT('Ctrl Pts',(-7.46193588961642,24.4969572391509,
0.));
#243636=CARTESIAN_POINT('Ctrl Pts',(-7.46193588961642,24.4969572391509,
12.));
#243637=CARTESIAN_POINT('Ctrl Pts',(-7.45650271336045,24.52390431731,0.));
#243638=CARTESIAN_POINT('Ctrl Pts',(-7.45650271336045,24.52390431731,12.));
#243639=CARTESIAN_POINT('Ctrl Pts',(-7.45099444651296,24.5509090831579,
0.));
#243640=CARTESIAN_POINT('Ctrl Pts',(-7.45099444651296,24.5509090831579,
12.));
#243641=CARTESIAN_POINT('Ctrl Pts',(-7.44541095473163,24.5779710960865,
0.));
#243642=CARTESIAN_POINT('Ctrl Pts',(-7.44541095473163,24.5779710960865,
12.));
#243643=CARTESIAN_POINT('Ctrl Pts',(-7.43975209375375,24.6050898852349,
0.));
#243644=CARTESIAN_POINT('Ctrl Pts',(-7.43975209375375,24.6050898852349,
12.));
#243645=CARTESIAN_POINT('Ctrl Pts',(-7.4340177048922,24.6322649369472,0.));
#243646=CARTESIAN_POINT('Ctrl Pts',(-7.4340177048922,24.6322649369472,12.));
#243647=CARTESIAN_POINT('Ctrl Pts',(-7.42820762158681,24.659495712869,0.));
#243648=CARTESIAN_POINT('Ctrl Pts',(-7.42820762158681,24.659495712869,12.));
#243649=CARTESIAN_POINT('Ctrl Pts',(-7.42232167765763,24.6867816727118,
0.));
#243650=CARTESIAN_POINT('Ctrl Pts',(-7.42232167765763,24.6867816727118,
12.));
#243651=CARTESIAN_POINT('Ctrl Pts',(-7.41635971481243,24.7141222949988,
0.));
#243652=CARTESIAN_POINT('Ctrl Pts',(-7.41635971481243,24.7141222949988,
12.));
#243653=CARTESIAN_POINT('Ctrl Pts',(-7.41032159082173,24.7415170994754,
0.));
#243654=CARTESIAN_POINT('Ctrl Pts',(-7.41032159082173,24.7415170994754,
12.));
#243655=CARTESIAN_POINT('Ctrl Pts',(-7.40420718661754,24.7689656669005,
0.));
#243656=CARTESIAN_POINT('Ctrl Pts',(-7.40420718661754,24.7689656669005,
12.));
#243657=CARTESIAN_POINT('Ctrl Pts',(-7.39801641583612,24.7964676646518,
0.));
#243658=CARTESIAN_POINT('Ctrl Pts',(-7.39801641583612,24.7964676646518,
12.));
#243659=CARTESIAN_POINT('Ctrl Pts',(-7.39174922586841,24.8240228521042,
0.));
#243660=CARTESIAN_POINT('Ctrl Pts',(-7.39174922586841,24.8240228521042,
12.));
#243661=CARTESIAN_POINT('Ctrl Pts',(-7.38540558904946,24.8516310625367,
0.));
#243662=CARTESIAN_POINT('Ctrl Pts',(-7.38540558904946,24.8516310625367,
12.));
#243663=CARTESIAN_POINT('Ctrl Pts',(-7.3789854964161,24.8792921911309,0.));
#243664=CARTESIAN_POINT('Ctrl Pts',(-7.3789854964161,24.8792921911309,12.));
#243665=CARTESIAN_POINT('Ctrl Pts',(-7.37378825962718,24.9014633826201,
0.));
#243666=CARTESIAN_POINT('Ctrl Pts',(-7.37378825962718,24.9014633826201,
12.));
#243667=CARTESIAN_POINT('Ctrl Pts',(-7.36985593120696,24.9181155530631,
0.));
#243668=CARTESIAN_POINT('Ctrl Pts',(-7.36985593120696,24.9181155530631,
12.));
#243669=CARTESIAN_POINT('Ctrl Pts',(-7.3672190902906,24.9292275670705,0.));
#243670=CARTESIAN_POINT('Ctrl Pts',(-7.3672190902906,24.9292275670705,12.));
#243671=CARTESIAN_POINT('Ctrl Pts',(-7.36589684767344,24.9347862158358,
0.));
#243672=CARTESIAN_POINT('Ctrl Pts',(-7.36589684767344,24.9347862158358,
12.));
#243673=CARTESIAN_POINT('',(-7.36589684767344,24.9347862158358,0.));
#243674=CARTESIAN_POINT('Ctrl Pts',(-7.52250298901264,21.2610617890679,
0.));
#243675=CARTESIAN_POINT('Ctrl Pts',(-7.5225064970397,21.2610673466886,0.));
#243676=CARTESIAN_POINT('Ctrl Pts',(-7.52252744144904,21.2611204474866,
0.));
#243677=CARTESIAN_POINT('Ctrl Pts',(-7.52260064231661,21.261326054066,0.));
#243678=CARTESIAN_POINT('Ctrl Pts',(-7.5227818224267,21.2618521283555,0.));
#243679=CARTESIAN_POINT('Ctrl Pts',(-7.52314642316199,21.262927782038,0.));
#243680=CARTESIAN_POINT('Ctrl Pts',(-7.52364573027553,21.2644161259962,
0.));
#243681=CARTESIAN_POINT('Ctrl Pts',(-7.52427261074298,21.2663059157058,
0.));
#243682=CARTESIAN_POINT('Ctrl Pts',(-7.5250177033353,21.2685823838671,0.));
#243683=CARTESIAN_POINT('Ctrl Pts',(-7.5258712609553,21.2712301573466,0.));
#243684=CARTESIAN_POINT('Ctrl Pts',(-7.52682526918541,21.2742366113579,
0.));
#243685=CARTESIAN_POINT('Ctrl Pts',(-7.52787386225333,21.2775925269652,
0.));
#243686=CARTESIAN_POINT('Ctrl Pts',(-7.52901217930408,21.2812902781143,
0.));
#243687=CARTESIAN_POINT('Ctrl Pts',(-7.53023562438229,21.2853226580657,
0.));
#243688=CARTESIAN_POINT('Ctrl Pts',(-7.53153906987855,21.2896816163842,
0.));
#243689=CARTESIAN_POINT('Ctrl Pts',(-7.53291726078527,21.2943588989331,
0.));
#243690=CARTESIAN_POINT('Ctrl Pts',(-7.53436505309943,21.2993464250717,
0.));
#243691=CARTESIAN_POINT('Ctrl Pts',(-7.53587778251736,21.3046368712157,
0.));
#243692=CARTESIAN_POINT('Ctrl Pts',(-7.53745129364616,21.310223716773,0.));
#243693=CARTESIAN_POINT('Ctrl Pts',(-7.53908175169898,21.3161009456256,
0.));
#243694=CARTESIAN_POINT('Ctrl Pts',(-7.54076552038279,21.3222628524165,
0.));
#243695=CARTESIAN_POINT('Ctrl Pts',(-7.54249900377031,21.328703791771,0.));
#243696=CARTESIAN_POINT('Ctrl Pts',(-7.54427868151268,21.3354182340149,
0.));
#243697=CARTESIAN_POINT('Ctrl Pts',(-7.54610114948347,21.3424008295038,
0.));
#243698=CARTESIAN_POINT('Ctrl Pts',(-7.5479631624633,21.3496464761531,0.));
#243699=CARTESIAN_POINT('Ctrl Pts',(-7.5498616652131,21.3571503685855,0.));
#243700=CARTESIAN_POINT('Ctrl Pts',(-7.55179375777444,21.3649079431865,
0.));
#243701=CARTESIAN_POINT('Ctrl Pts',(-7.55375667080029,21.3729148390243,
0.));
#243702=CARTESIAN_POINT('Ctrl Pts',(-7.55574773403503,21.3811668478932,
0.));
#243703=CARTESIAN_POINT('Ctrl Pts',(-7.55776435731417,21.3896598842117,
0.));
#243704=CARTESIAN_POINT('Ctrl Pts',(-7.55980403700611,21.3983899952987,
0.));
#243705=CARTESIAN_POINT('Ctrl Pts',(-7.56186435703622,21.4073533630365,
0.));
#243706=CARTESIAN_POINT('Ctrl Pts',(-7.56394299313685,21.4165463106254,
0.));
#243707=CARTESIAN_POINT('Ctrl Pts',(-7.56603771218712,21.4259653015736,
0.));
#243708=CARTESIAN_POINT('Ctrl Pts',(-7.56814636360847,21.4356069261513,
0.));
#243709=CARTESIAN_POINT('Ctrl Pts',(-7.57026687261166,21.4454678907509,
0.));
#243710=CARTESIAN_POINT('Ctrl Pts',(-7.57239723223506,21.4555450053142,
0.));
#243711=CARTESIAN_POINT('Ctrl Pts',(-7.57453549743412,21.4658351740128,
0.));
#243712=CARTESIAN_POINT('Ctrl Pts',(-7.57667978402987,21.4763353936762,
0.));
#243713=CARTESIAN_POINT('Ctrl Pts',(-7.57882826679132,21.4870427508194,
0.));
#243714=CARTESIAN_POINT('Ctrl Pts',(-7.58097917790744,21.4979544192744,
0.));
#243715=CARTESIAN_POINT('Ctrl Pts',(-7.5831308051918,21.5090676573873,0.));
#243716=CARTESIAN_POINT('Ctrl Pts',(-7.5852814891913,21.5203798035299,0.));
#243717=CARTESIAN_POINT('Ctrl Pts',(-7.58742962034834,21.5318882716736,
0.));
#243718=CARTESIAN_POINT('Ctrl Pts',(-7.58957363620014,21.543590547011,0.));
#243719=CARTESIAN_POINT('Ctrl Pts',(-7.59171201844777,21.5554841813462,
0.));
#243720=CARTESIAN_POINT('Ctrl Pts',(-7.59384329124918,21.5675667904726,
0.));
#243721=CARTESIAN_POINT('Ctrl Pts',(-7.59596601973584,21.5798360518978,
0.));
#243722=CARTESIAN_POINT('Ctrl Pts',(-7.59807880846195,21.5922897024466,
0.));
#243723=CARTESIAN_POINT('Ctrl Pts',(-7.60018029988241,21.6049255358843,
0.));
#243724=CARTESIAN_POINT('Ctrl Pts',(-7.60226917285429,21.617741400599,0.));
#243725=CARTESIAN_POINT('Ctrl Pts',(-7.60434414118296,21.6307351973822,
0.));
#243726=CARTESIAN_POINT('Ctrl Pts',(-7.60640395216357,21.6439048771743,
0.));
#243727=CARTESIAN_POINT('Ctrl Pts',(-7.60844738512874,21.6572484388081,
0.));
#243728=CARTESIAN_POINT('Ctrl Pts',(-7.61047325000956,21.6707639267576,
0.));
#243729=CARTESIAN_POINT('Ctrl Pts',(-7.61248038630268,21.6844494295815,
0.));
#243730=CARTESIAN_POINT('Ctrl Pts',(-7.61446766202787,21.6983030783322,
0.));
#243731=CARTESIAN_POINT('Ctrl Pts',(-7.61643397270421,21.7123230449834,
0.));
#243732=CARTESIAN_POINT('Ctrl Pts',(-7.61837824030538,21.7265075407975,
0.));
#243733=CARTESIAN_POINT('Ctrl Pts',(-7.62029941230855,21.7408548148656,
0.));
#243734=CARTESIAN_POINT('Ctrl Pts',(-7.62219646084228,21.7553631528328,
0.));
#243735=CARTESIAN_POINT('Ctrl Pts',(-7.62406838181166,21.7700308755584,
0.));
#243736=CARTESIAN_POINT('Ctrl Pts',(-7.62591419404512,21.7848563378021,
0.));
#243737=CARTESIAN_POINT('Ctrl Pts',(-7.62773293842389,21.799837926858,0.));
#243738=CARTESIAN_POINT('Ctrl Pts',(-7.62952367718127,21.814974061509,0.));
#243739=CARTESIAN_POINT('Ctrl Pts',(-7.63128549323023,21.8302631910195,
0.));
#243740=CARTESIAN_POINT('Ctrl Pts',(-7.63301748948936,21.8457037941084,
0.));
#243741=CARTESIAN_POINT('Ctrl Pts',(-7.63471878821226,21.8612943779089,
0.));
#243742=CARTESIAN_POINT('Ctrl Pts',(-7.636388530334,21.8770334769496,0.));
#243743=CARTESIAN_POINT('Ctrl Pts',(-7.63802587492035,21.8929196523514,
0.));
#243744=CARTESIAN_POINT('Ctrl Pts',(-7.63962999860927,21.9089514909874,
0.));
#243745=CARTESIAN_POINT('Ctrl Pts',(-7.64120009506532,21.9251276046546,
0.));
#243746=CARTESIAN_POINT('Ctrl Pts',(-7.64273537442682,21.9414466292072,
0.));
#243747=CARTESIAN_POINT('Ctrl Pts',(-7.64423506279123,21.9579072237651,
0.));
#243748=CARTESIAN_POINT('Ctrl Pts',(-7.64569840177336,21.9745080700798,
0.));
#243749=CARTESIAN_POINT('Ctrl Pts',(-7.6471246480525,21.9912478718542,0.));
#243750=CARTESIAN_POINT('Ctrl Pts',(-7.64851307293352,22.0081253540774,
0.));
#243751=CARTESIAN_POINT('Ctrl Pts',(-7.64986296190168,22.0251392623209,
0.));
#243752=CARTESIAN_POINT('Ctrl Pts',(-7.65117361421358,22.0422883621174,
0.));
#243753=CARTESIAN_POINT('Ctrl Pts',(-7.65244434253113,22.0595714384431,
0.));
#243754=CARTESIAN_POINT('Ctrl Pts',(-7.65367447254949,22.0769872951596,
0.));
#243755=CARTESIAN_POINT('Ctrl Pts',(-7.65486334263644,22.094534754469,0.));
#243756=CARTESIAN_POINT('Ctrl Pts',(-7.65601030346807,22.1122126563329,
0.));
#243757=CARTESIAN_POINT('Ctrl Pts',(-7.65711471769397,22.1300198579675,
0.));
#243758=CARTESIAN_POINT('Ctrl Pts',(-7.65817595963349,22.1479552334211,
0.));
#243759=CARTESIAN_POINT('Ctrl Pts',(-7.6591934149693,22.1660176731178,0.));
#243760=CARTESIAN_POINT('Ctrl Pts',(-7.66016648045005,22.1842060834091,
0.));
#243761=CARTESIAN_POINT('Ctrl Pts',(-7.66109456359271,22.2025193860964,
0.));
#243762=CARTESIAN_POINT('Ctrl Pts',(-7.661977082404,22.2209565180085,0.));
#243763=CARTESIAN_POINT('Ctrl Pts',(-7.66281346512509,22.2395164306547,
0.));
#243764=CARTESIAN_POINT('Ctrl Pts',(-7.66360314997641,22.258198089848,0.));
#243765=CARTESIAN_POINT('Ctrl Pts',(-7.66434558490979,22.2770004753335,
0.));
#243766=CARTESIAN_POINT('Ctrl Pts',(-7.66504022736299,22.2959225803937,
0.));
#243767=CARTESIAN_POINT('Ctrl Pts',(-7.66568654402494,22.314963411484,0.));
#243768=CARTESIAN_POINT('Ctrl Pts',(-7.66628401061952,22.3341219879469,
0.));
#243769=CARTESIAN_POINT('Ctrl Pts',(-7.66683211169158,22.3533973417021,
0.));
#243770=CARTESIAN_POINT('Ctrl Pts',(-7.66733034039883,22.372788516936,0.));
#243771=CARTESIAN_POINT('Ctrl Pts',(-7.6677781983079,22.3922945697773,0.));
#243772=CARTESIAN_POINT('Ctrl Pts',(-7.6681751951964,22.4119145679758,0.));
#243773=CARTESIAN_POINT('Ctrl Pts',(-7.66852084886704,22.4316475906603,
0.));
#243774=CARTESIAN_POINT('Ctrl Pts',(-7.66881468496635,22.4514927280855,
0.));
#243775=CARTESIAN_POINT('Ctrl Pts',(-7.66905623680831,22.47144908137,0.));
#243776=CARTESIAN_POINT('Ctrl Pts',(-7.66924504520315,22.4915157622312,
0.));
#243777=CARTESIAN_POINT('Ctrl Pts',(-7.66938065829108,22.5116918927031,
0.));
#243778=CARTESIAN_POINT('Ctrl Pts',(-7.66946263138144,22.53197660492,0.));
#243779=CARTESIAN_POINT('Ctrl Pts',(-7.66949052679693,22.5523690409116,
0.));
#243780=CARTESIAN_POINT('Ctrl Pts',(-7.66946391372306,22.5728683523831,
0.));
#243781=CARTESIAN_POINT('Ctrl Pts',(-7.66938236806233,22.5934737004953,
0.));
#243782=CARTESIAN_POINT('Ctrl Pts',(-7.66924547229414,22.6141842556243,
0.));
#243783=CARTESIAN_POINT('Ctrl Pts',(-7.66905281533715,22.6349991971541,
0.));
#243784=CARTESIAN_POINT('Ctrl Pts',(-7.66880399241323,22.6559177133127,
0.));
#243785=CARTESIAN_POINT('Ctrl Pts',(-7.66849860491743,22.6769390009885,
0.));
#243786=CARTESIAN_POINT('Ctrl Pts',(-7.66813626029275,22.6980622655446,
0.));
#243787=CARTESIAN_POINT('Ctrl Pts',(-7.66771657191027,22.7192867206245,
0.));
#243788=CARTESIAN_POINT('Ctrl Pts',(-7.6672391589544,22.7406115879513,0.));
#243789=CARTESIAN_POINT('Ctrl Pts',(-7.66670364630299,22.7620360971843,
0.));
#243790=CARTESIAN_POINT('Ctrl Pts',(-7.66610966441273,22.7835594857699,
0.));
#243791=CARTESIAN_POINT('Ctrl Pts',(-7.66545684920987,22.8051809987833,
0.));
#243792=CARTESIAN_POINT('Ctrl Pts',(-7.66474484198549,22.8268998887678,
0.));
#243793=CARTESIAN_POINT('Ctrl Pts',(-7.66397328929803,22.848715415557,0.));
#243794=CARTESIAN_POINT('Ctrl Pts',(-7.66314184287337,22.8706268461283,
0.));
#243795=CARTESIAN_POINT('Ctrl Pts',(-7.66225015950156,22.8926334544883,
0.));
#243796=CARTESIAN_POINT('Ctrl Pts',(-7.66129790094108,22.9147345215421,
0.));
#243797=CARTESIAN_POINT('Ctrl Pts',(-7.66028473382778,22.9369293349593,
0.));
#243798=CARTESIAN_POINT('Ctrl Pts',(-7.65921032958902,22.959217189033,0.));
#243799=CARTESIAN_POINT('Ctrl Pts',(-7.65807436436432,22.9815973845296,
0.));
#243800=CARTESIAN_POINT('Ctrl Pts',(-7.65687651891304,23.0040692285814,
0.));
#243801=CARTESIAN_POINT('Ctrl Pts',(-7.65561647852534,23.0266320345787,
0.));
#243802=CARTESIAN_POINT('Ctrl Pts',(-7.65429393293946,23.0492851220528,
0.));
#243803=CARTESIAN_POINT('Ctrl Pts',(-7.65290857626358,23.072027816555,0.));
#243804=CARTESIAN_POINT('Ctrl Pts',(-7.65146010690476,23.094859449525,0.));
#243805=CARTESIAN_POINT('Ctrl Pts',(-7.6499482274986,23.1177793581679,0.));
#243806=CARTESIAN_POINT('Ctrl Pts',(-7.64837264482943,23.1407868853819,
0.));
#243807=CARTESIAN_POINT('Ctrl Pts',(-7.64673306975805,23.1638813796694,
0.));
#243808=CARTESIAN_POINT('Ctrl Pts',(-7.64502921715483,23.1870621950452,
0.));
#243809=CARTESIAN_POINT('Ctrl Pts',(-7.6432608058368,23.2103286909398,0.));
#243810=CARTESIAN_POINT('Ctrl Pts',(-7.64142755851504,23.2336802320912,
0.));
#243811=CARTESIAN_POINT('Ctrl Pts',(-7.63952920172835,23.2571161884488,
0.));
#243812=CARTESIAN_POINT('Ctrl Pts',(-7.63756546576374,23.2806359350855,
0.));
#243813=CARTESIAN_POINT('Ctrl Pts',(-7.63553608458783,23.3042388521022,
0.));
#243814=CARTESIAN_POINT('Ctrl Pts',(-7.63344079578161,23.3279243245241,
0.));
#243815=CARTESIAN_POINT('Ctrl Pts',(-7.63127934048136,23.3516917421972,
0.));
#243816=CARTESIAN_POINT('Ctrl Pts',(-7.62905146332593,23.3755404996636,
0.));
#243817=CARTESIAN_POINT('Ctrl Pts',(-7.62675691240329,23.399469996112,0.));
#243818=CARTESIAN_POINT('Ctrl Pts',(-7.6243954392005,23.4234796353542,0.));
#243819=CARTESIAN_POINT('Ctrl Pts',(-7.62196679855955,23.4475688257854,
0.));
#243820=CARTESIAN_POINT('Ctrl Pts',(-7.61947074863977,23.4717369803438,
0.));
#243821=CARTESIAN_POINT('Ctrl Pts',(-7.61690705088319,23.4959835164609,
0.));
#243822=CARTESIAN_POINT('Ctrl Pts',(-7.61427546999298,23.5203078560129,
0.));
#243823=CARTESIAN_POINT('Ctrl Pts',(-7.61157577385372,23.544709425203,0.));
#243824=CARTESIAN_POINT('Ctrl Pts',(-7.608807733446,23.5691876544244,0.));
#243825=CARTESIAN_POINT('Ctrl Pts',(-7.60597112277094,23.5937419781245,
0.));
#243826=CARTESIAN_POINT('Ctrl Pts',(-7.60306571877806,23.6183718346576,
0.));
#243827=CARTESIAN_POINT('Ctrl Pts',(-7.60009130130126,23.6430766661418,
0.));
#243828=CARTESIAN_POINT('Ctrl Pts',(-7.59704765299567,23.6678559182875,
0.));
#243829=CARTESIAN_POINT('Ctrl Pts',(-7.59393455934035,23.6927090405066,
0.));
#243830=CARTESIAN_POINT('Ctrl Pts',(-7.5907518086532,23.7176354860456,0.));
#243831=CARTESIAN_POINT('Ctrl Pts',(-7.58749919210826,23.7426347121006,
0.));
#243832=CARTESIAN_POINT('Ctrl Pts',(-7.58417650376271,23.7677061799376,
0.));
#243833=CARTESIAN_POINT('Ctrl Pts',(-7.58078354058213,23.7928493549908,
0.));
#243834=CARTESIAN_POINT('Ctrl Pts',(-7.57732010249066,23.8180637069976,
0.));
#243835=CARTESIAN_POINT('Ctrl Pts',(-7.57378599219814,23.8433487096132,
0.));
#243836=CARTESIAN_POINT('Ctrl Pts',(-7.57018101500709,23.8687038399595,
0.));
#243837=CARTESIAN_POINT('Ctrl Pts',(-7.56650497863791,23.8941285782002,
0.));
#243838=CARTESIAN_POINT('Ctrl Pts',(-7.56275769304773,23.9196224070759,
0.));
#243839=CARTESIAN_POINT('Ctrl Pts',(-7.5589389702768,23.9451848115002,0.));
#243840=CARTESIAN_POINT('Ctrl Pts',(-7.55504862424808,23.9708152779886,
0.));
#243841=CARTESIAN_POINT('Ctrl Pts',(-7.55108647097432,23.9965132953187,
0.));
#243842=CARTESIAN_POINT('Ctrl Pts',(-7.54705232885895,24.0222783554531,
0.));
#243843=CARTESIAN_POINT('Ctrl Pts',(-7.54294601896128,24.0481099543353,
0.));
#243844=CARTESIAN_POINT('Ctrl Pts',(-7.53876736531005,24.0740075927984,
0.));
#243845=CARTESIAN_POINT('Ctrl Pts',(-7.53451619514658,24.0999707772643,
0.));
#243846=CARTESIAN_POINT('Ctrl Pts',(-7.53019233935536,24.1259990209211,
0.));
#243847=CARTESIAN_POINT('Ctrl Pts',(-7.52579563201479,24.152091842537,0.));
#243848=CARTESIAN_POINT('Ctrl Pts',(-7.52132590953862,24.1782487641602,
0.));
#243849=CARTESIAN_POINT('Ctrl Pts',(-7.51678300997998,24.2044693092356,
0.));
#243850=CARTESIAN_POINT('Ctrl Pts',(-7.51216677222199,24.230753000389,0.));
#243851=CARTESIAN_POINT('Ctrl Pts',(-7.50747703535115,24.2570993577032,
0.));
#243852=CARTESIAN_POINT('Ctrl Pts',(-7.50271363765098,24.2835078958966,
0.));
#243853=CARTESIAN_POINT('Ctrl Pts',(-7.49787641695359,24.3099781253345,
0.));
#243854=CARTESIAN_POINT('Ctrl Pts',(-7.4929652125233,24.3365095573673,0.));
#243855=CARTESIAN_POINT('Ctrl Pts',(-7.48797986651828,24.3631017084513,
0.));
#243856=CARTESIAN_POINT('Ctrl Pts',(-7.48292022569254,24.3897541049248,
0.));
#243857=CARTESIAN_POINT('Ctrl Pts',(-7.47778614286573,24.4164662871165,
0.));
#243858=CARTESIAN_POINT('Ctrl Pts',(-7.47257747883319,24.4432378146501,
0.));
#243859=CARTESIAN_POINT('Ctrl Pts',(-7.46729410308923,24.4700682684544,
0.));
#243860=CARTESIAN_POINT('Ctrl Pts',(-7.46193588961642,24.4969572391509,
0.));
#243861=CARTESIAN_POINT('Ctrl Pts',(-7.45650271336045,24.52390431731,0.));
#243862=CARTESIAN_POINT('Ctrl Pts',(-7.45099444651296,24.5509090831579,
0.));
#243863=CARTESIAN_POINT('Ctrl Pts',(-7.44541095473163,24.5779710960865,
0.));
#243864=CARTESIAN_POINT('Ctrl Pts',(-7.43975209375375,24.6050898852349,
0.));
#243865=CARTESIAN_POINT('Ctrl Pts',(-7.4340177048922,24.6322649369472,0.));
#243866=CARTESIAN_POINT('Ctrl Pts',(-7.42820762158681,24.659495712869,0.));
#243867=CARTESIAN_POINT('Ctrl Pts',(-7.42232167765763,24.6867816727118,
0.));
#243868=CARTESIAN_POINT('Ctrl Pts',(-7.41635971481243,24.7141222949988,
0.));
#243869=CARTESIAN_POINT('Ctrl Pts',(-7.41032159082173,24.7415170994754,
0.));
#243870=CARTESIAN_POINT('Ctrl Pts',(-7.40420718661754,24.7689656669005,
0.));
#243871=CARTESIAN_POINT('Ctrl Pts',(-7.39801641583612,24.7964676646518,
0.));
#243872=CARTESIAN_POINT('Ctrl Pts',(-7.39174922586841,24.8240228521042,
0.));
#243873=CARTESIAN_POINT('Ctrl Pts',(-7.38540558904946,24.8516310625367,
0.));
#243874=CARTESIAN_POINT('Ctrl Pts',(-7.3789854964161,24.8792921911309,0.));
#243875=CARTESIAN_POINT('Ctrl Pts',(-7.37378825962718,24.9014633826201,
0.));
#243876=CARTESIAN_POINT('Ctrl Pts',(-7.36985593120696,24.9181155530631,
0.));
#243877=CARTESIAN_POINT('Ctrl Pts',(-7.3672190902906,24.9292275670705,0.));
#243878=CARTESIAN_POINT('Ctrl Pts',(-7.36589684767344,24.9347862158358,
0.));
#243879=CARTESIAN_POINT('',(-7.36589684767344,24.9347862158358,12.));
#243880=CARTESIAN_POINT('Ctrl Pts',(-7.36589684767344,24.9347862158358,
12.));
#243881=CARTESIAN_POINT('Ctrl Pts',(-7.3672190902906,24.9292275670705,12.));
#243882=CARTESIAN_POINT('Ctrl Pts',(-7.36985593120696,24.9181155530631,
12.));
#243883=CARTESIAN_POINT('Ctrl Pts',(-7.37378825962718,24.9014633826201,
12.));
#243884=CARTESIAN_POINT('Ctrl Pts',(-7.3789854964161,24.8792921911309,12.));
#243885=CARTESIAN_POINT('Ctrl Pts',(-7.38540558904946,24.8516310625367,
12.));
#243886=CARTESIAN_POINT('Ctrl Pts',(-7.39174922586841,24.8240228521042,
12.));
#243887=CARTESIAN_POINT('Ctrl Pts',(-7.39801641583612,24.7964676646518,
12.));
#243888=CARTESIAN_POINT('Ctrl Pts',(-7.40420718661754,24.7689656669005,
12.));
#243889=CARTESIAN_POINT('Ctrl Pts',(-7.41032159082173,24.7415170994754,
12.));
#243890=CARTESIAN_POINT('Ctrl Pts',(-7.41635971481243,24.7141222949988,
12.));
#243891=CARTESIAN_POINT('Ctrl Pts',(-7.42232167765763,24.6867816727118,
12.));
#243892=CARTESIAN_POINT('Ctrl Pts',(-7.42820762158681,24.659495712869,12.));
#243893=CARTESIAN_POINT('Ctrl Pts',(-7.4340177048922,24.6322649369472,12.));
#243894=CARTESIAN_POINT('Ctrl Pts',(-7.43975209375375,24.6050898852349,
12.));
#243895=CARTESIAN_POINT('Ctrl Pts',(-7.44541095473163,24.5779710960865,
12.));
#243896=CARTESIAN_POINT('Ctrl Pts',(-7.45099444651296,24.5509090831579,
12.));
#243897=CARTESIAN_POINT('Ctrl Pts',(-7.45650271336045,24.52390431731,12.));
#243898=CARTESIAN_POINT('Ctrl Pts',(-7.46193588961642,24.4969572391509,
12.));
#243899=CARTESIAN_POINT('Ctrl Pts',(-7.46729410308923,24.4700682684544,
12.));
#243900=CARTESIAN_POINT('Ctrl Pts',(-7.47257747883319,24.4432378146501,
12.));
#243901=CARTESIAN_POINT('Ctrl Pts',(-7.47778614286573,24.4164662871165,
12.));
#243902=CARTESIAN_POINT('Ctrl Pts',(-7.48292022569254,24.3897541049248,
12.));
#243903=CARTESIAN_POINT('Ctrl Pts',(-7.48797986651828,24.3631017084513,
12.));
#243904=CARTESIAN_POINT('Ctrl Pts',(-7.4929652125233,24.3365095573673,12.));
#243905=CARTESIAN_POINT('Ctrl Pts',(-7.49787641695359,24.3099781253345,
12.));
#243906=CARTESIAN_POINT('Ctrl Pts',(-7.50271363765098,24.2835078958966,
12.));
#243907=CARTESIAN_POINT('Ctrl Pts',(-7.50747703535115,24.2570993577032,
12.));
#243908=CARTESIAN_POINT('Ctrl Pts',(-7.51216677222199,24.230753000389,12.));
#243909=CARTESIAN_POINT('Ctrl Pts',(-7.51678300997998,24.2044693092356,
12.));
#243910=CARTESIAN_POINT('Ctrl Pts',(-7.52132590953862,24.1782487641602,
12.));
#243911=CARTESIAN_POINT('Ctrl Pts',(-7.52579563201479,24.152091842537,12.));
#243912=CARTESIAN_POINT('Ctrl Pts',(-7.53019233935536,24.1259990209211,
12.));
#243913=CARTESIAN_POINT('Ctrl Pts',(-7.53451619514658,24.0999707772643,
12.));
#243914=CARTESIAN_POINT('Ctrl Pts',(-7.53876736531005,24.0740075927984,
12.));
#243915=CARTESIAN_POINT('Ctrl Pts',(-7.54294601896128,24.0481099543353,
12.));
#243916=CARTESIAN_POINT('Ctrl Pts',(-7.54705232885895,24.0222783554531,
12.));
#243917=CARTESIAN_POINT('Ctrl Pts',(-7.55108647097432,23.9965132953187,
12.));
#243918=CARTESIAN_POINT('Ctrl Pts',(-7.55504862424808,23.9708152779886,
12.));
#243919=CARTESIAN_POINT('Ctrl Pts',(-7.5589389702768,23.9451848115002,12.));
#243920=CARTESIAN_POINT('Ctrl Pts',(-7.56275769304773,23.9196224070759,
12.));
#243921=CARTESIAN_POINT('Ctrl Pts',(-7.56650497863791,23.8941285782002,
12.));
#243922=CARTESIAN_POINT('Ctrl Pts',(-7.57018101500709,23.8687038399595,
12.));
#243923=CARTESIAN_POINT('Ctrl Pts',(-7.57378599219814,23.8433487096132,
12.));
#243924=CARTESIAN_POINT('Ctrl Pts',(-7.57732010249066,23.8180637069976,
12.));
#243925=CARTESIAN_POINT('Ctrl Pts',(-7.58078354058213,23.7928493549908,
12.));
#243926=CARTESIAN_POINT('Ctrl Pts',(-7.58417650376271,23.7677061799376,
12.));
#243927=CARTESIAN_POINT('Ctrl Pts',(-7.58749919210826,23.7426347121006,
12.));
#243928=CARTESIAN_POINT('Ctrl Pts',(-7.5907518086532,23.7176354860456,12.));
#243929=CARTESIAN_POINT('Ctrl Pts',(-7.59393455934035,23.6927090405066,
12.));
#243930=CARTESIAN_POINT('Ctrl Pts',(-7.59704765299567,23.6678559182875,
12.));
#243931=CARTESIAN_POINT('Ctrl Pts',(-7.60009130130126,23.6430766661418,
12.));
#243932=CARTESIAN_POINT('Ctrl Pts',(-7.60306571877806,23.6183718346576,
12.));
#243933=CARTESIAN_POINT('Ctrl Pts',(-7.60597112277094,23.5937419781245,
12.));
#243934=CARTESIAN_POINT('Ctrl Pts',(-7.608807733446,23.5691876544244,12.));
#243935=CARTESIAN_POINT('Ctrl Pts',(-7.61157577385372,23.544709425203,12.));
#243936=CARTESIAN_POINT('Ctrl Pts',(-7.61427546999298,23.5203078560129,
12.));
#243937=CARTESIAN_POINT('Ctrl Pts',(-7.61690705088319,23.4959835164609,
12.));
#243938=CARTESIAN_POINT('Ctrl Pts',(-7.61947074863977,23.4717369803438,
12.));
#243939=CARTESIAN_POINT('Ctrl Pts',(-7.62196679855955,23.4475688257854,
12.));
#243940=CARTESIAN_POINT('Ctrl Pts',(-7.6243954392005,23.4234796353542,12.));
#243941=CARTESIAN_POINT('Ctrl Pts',(-7.62675691240329,23.399469996112,12.));
#243942=CARTESIAN_POINT('Ctrl Pts',(-7.62905146332593,23.3755404996636,
12.));
#243943=CARTESIAN_POINT('Ctrl Pts',(-7.63127934048136,23.3516917421972,
12.));
#243944=CARTESIAN_POINT('Ctrl Pts',(-7.63344079578161,23.3279243245241,
12.));
#243945=CARTESIAN_POINT('Ctrl Pts',(-7.63553608458783,23.3042388521022,
12.));
#243946=CARTESIAN_POINT('Ctrl Pts',(-7.63756546576374,23.2806359350855,
12.));
#243947=CARTESIAN_POINT('Ctrl Pts',(-7.63952920172835,23.2571161884488,
12.));
#243948=CARTESIAN_POINT('Ctrl Pts',(-7.64142755851504,23.2336802320912,
12.));
#243949=CARTESIAN_POINT('Ctrl Pts',(-7.6432608058368,23.2103286909398,12.));
#243950=CARTESIAN_POINT('Ctrl Pts',(-7.64502921715483,23.1870621950452,
12.));
#243951=CARTESIAN_POINT('Ctrl Pts',(-7.64673306975805,23.1638813796694,
12.));
#243952=CARTESIAN_POINT('Ctrl Pts',(-7.64837264482943,23.1407868853819,
12.));
#243953=CARTESIAN_POINT('Ctrl Pts',(-7.6499482274986,23.1177793581679,12.));
#243954=CARTESIAN_POINT('Ctrl Pts',(-7.65146010690476,23.094859449525,12.));
#243955=CARTESIAN_POINT('Ctrl Pts',(-7.65290857626358,23.072027816555,12.));
#243956=CARTESIAN_POINT('Ctrl Pts',(-7.65429393293946,23.0492851220528,
12.));
#243957=CARTESIAN_POINT('Ctrl Pts',(-7.65561647852534,23.0266320345787,
12.));
#243958=CARTESIAN_POINT('Ctrl Pts',(-7.65687651891304,23.0040692285814,
12.));
#243959=CARTESIAN_POINT('Ctrl Pts',(-7.65807436436432,22.9815973845296,
12.));
#243960=CARTESIAN_POINT('Ctrl Pts',(-7.65921032958902,22.959217189033,12.));
#243961=CARTESIAN_POINT('Ctrl Pts',(-7.66028473382778,22.9369293349593,
12.));
#243962=CARTESIAN_POINT('Ctrl Pts',(-7.66129790094108,22.9147345215421,
12.));
#243963=CARTESIAN_POINT('Ctrl Pts',(-7.66225015950156,22.8926334544883,
12.));
#243964=CARTESIAN_POINT('Ctrl Pts',(-7.66314184287337,22.8706268461283,
12.));
#243965=CARTESIAN_POINT('Ctrl Pts',(-7.66397328929803,22.848715415557,12.));
#243966=CARTESIAN_POINT('Ctrl Pts',(-7.66474484198549,22.8268998887678,
12.));
#243967=CARTESIAN_POINT('Ctrl Pts',(-7.66545684920987,22.8051809987833,
12.));
#243968=CARTESIAN_POINT('Ctrl Pts',(-7.66610966441273,22.7835594857699,
12.));
#243969=CARTESIAN_POINT('Ctrl Pts',(-7.66670364630299,22.7620360971843,
12.));
#243970=CARTESIAN_POINT('Ctrl Pts',(-7.6672391589544,22.7406115879513,12.));
#243971=CARTESIAN_POINT('Ctrl Pts',(-7.66771657191027,22.7192867206245,
12.));
#243972=CARTESIAN_POINT('Ctrl Pts',(-7.66813626029275,22.6980622655446,
12.));
#243973=CARTESIAN_POINT('Ctrl Pts',(-7.66849860491743,22.6769390009885,
12.));
#243974=CARTESIAN_POINT('Ctrl Pts',(-7.66880399241323,22.6559177133127,
12.));
#243975=CARTESIAN_POINT('Ctrl Pts',(-7.66905281533715,22.6349991971541,
12.));
#243976=CARTESIAN_POINT('Ctrl Pts',(-7.66924547229414,22.6141842556243,
12.));
#243977=CARTESIAN_POINT('Ctrl Pts',(-7.66938236806233,22.5934737004953,
12.));
#243978=CARTESIAN_POINT('Ctrl Pts',(-7.66946391372306,22.5728683523831,
12.));
#243979=CARTESIAN_POINT('Ctrl Pts',(-7.66949052679693,22.5523690409116,
12.));
#243980=CARTESIAN_POINT('Ctrl Pts',(-7.66946263138144,22.53197660492,12.));
#243981=CARTESIAN_POINT('Ctrl Pts',(-7.66938065829108,22.5116918927031,
12.));
#243982=CARTESIAN_POINT('Ctrl Pts',(-7.66924504520315,22.4915157622312,
12.));
#243983=CARTESIAN_POINT('Ctrl Pts',(-7.66905623680831,22.47144908137,12.));
#243984=CARTESIAN_POINT('Ctrl Pts',(-7.66881468496635,22.4514927280855,
12.));
#243985=CARTESIAN_POINT('Ctrl Pts',(-7.66852084886704,22.4316475906603,
12.));
#243986=CARTESIAN_POINT('Ctrl Pts',(-7.6681751951964,22.4119145679758,12.));
#243987=CARTESIAN_POINT('Ctrl Pts',(-7.6677781983079,22.3922945697773,12.));
#243988=CARTESIAN_POINT('Ctrl Pts',(-7.66733034039883,22.372788516936,12.));
#243989=CARTESIAN_POINT('Ctrl Pts',(-7.66683211169158,22.3533973417021,
12.));
#243990=CARTESIAN_POINT('Ctrl Pts',(-7.66628401061952,22.3341219879469,
12.));
#243991=CARTESIAN_POINT('Ctrl Pts',(-7.66568654402494,22.314963411484,12.));
#243992=CARTESIAN_POINT('Ctrl Pts',(-7.66504022736299,22.2959225803937,
12.));
#243993=CARTESIAN_POINT('Ctrl Pts',(-7.66434558490979,22.2770004753335,
12.));
#243994=CARTESIAN_POINT('Ctrl Pts',(-7.66360314997641,22.258198089848,12.));
#243995=CARTESIAN_POINT('Ctrl Pts',(-7.66281346512509,22.2395164306547,
12.));
#243996=CARTESIAN_POINT('Ctrl Pts',(-7.661977082404,22.2209565180085,12.));
#243997=CARTESIAN_POINT('Ctrl Pts',(-7.66109456359271,22.2025193860964,
12.));
#243998=CARTESIAN_POINT('Ctrl Pts',(-7.66016648045005,22.1842060834091,
12.));
#243999=CARTESIAN_POINT('Ctrl Pts',(-7.6591934149693,22.1660176731178,12.));
#244000=CARTESIAN_POINT('Ctrl Pts',(-7.65817595963349,22.1479552334211,
12.));
#244001=CARTESIAN_POINT('Ctrl Pts',(-7.65711471769397,22.1300198579675,
12.));
#244002=CARTESIAN_POINT('Ctrl Pts',(-7.65601030346807,22.1122126563329,
12.));
#244003=CARTESIAN_POINT('Ctrl Pts',(-7.65486334263644,22.094534754469,12.));
#244004=CARTESIAN_POINT('Ctrl Pts',(-7.65367447254949,22.0769872951596,
12.));
#244005=CARTESIAN_POINT('Ctrl Pts',(-7.65244434253113,22.0595714384431,
12.));
#244006=CARTESIAN_POINT('Ctrl Pts',(-7.65117361421358,22.0422883621174,
12.));
#244007=CARTESIAN_POINT('Ctrl Pts',(-7.64986296190168,22.0251392623209,
12.));
#244008=CARTESIAN_POINT('Ctrl Pts',(-7.64851307293352,22.0081253540774,
12.));
#244009=CARTESIAN_POINT('Ctrl Pts',(-7.6471246480525,21.9912478718542,12.));
#244010=CARTESIAN_POINT('Ctrl Pts',(-7.64569840177336,21.9745080700798,
12.));
#244011=CARTESIAN_POINT('Ctrl Pts',(-7.64423506279123,21.9579072237651,
12.));
#244012=CARTESIAN_POINT('Ctrl Pts',(-7.64273537442682,21.9414466292072,
12.));
#244013=CARTESIAN_POINT('Ctrl Pts',(-7.64120009506532,21.9251276046546,
12.));
#244014=CARTESIAN_POINT('Ctrl Pts',(-7.63962999860927,21.9089514909874,
12.));
#244015=CARTESIAN_POINT('Ctrl Pts',(-7.63802587492035,21.8929196523514,
12.));
#244016=CARTESIAN_POINT('Ctrl Pts',(-7.636388530334,21.8770334769496,12.));
#244017=CARTESIAN_POINT('Ctrl Pts',(-7.63471878821226,21.8612943779089,
12.));
#244018=CARTESIAN_POINT('Ctrl Pts',(-7.63301748948936,21.8457037941084,
12.));
#244019=CARTESIAN_POINT('Ctrl Pts',(-7.63128549323023,21.8302631910195,
12.));
#244020=CARTESIAN_POINT('Ctrl Pts',(-7.62952367718127,21.814974061509,12.));
#244021=CARTESIAN_POINT('Ctrl Pts',(-7.62773293842389,21.799837926858,12.));
#244022=CARTESIAN_POINT('Ctrl Pts',(-7.62591419404512,21.7848563378021,
12.));
#244023=CARTESIAN_POINT('Ctrl Pts',(-7.62406838181166,21.7700308755584,
12.));
#244024=CARTESIAN_POINT('Ctrl Pts',(-7.62219646084228,21.7553631528328,
12.));
#244025=CARTESIAN_POINT('Ctrl Pts',(-7.62029941230855,21.7408548148656,
12.));
#244026=CARTESIAN_POINT('Ctrl Pts',(-7.61837824030538,21.7265075407975,
12.));
#244027=CARTESIAN_POINT('Ctrl Pts',(-7.61643397270421,21.7123230449834,
12.));
#244028=CARTESIAN_POINT('Ctrl Pts',(-7.61446766202787,21.6983030783322,
12.));
#244029=CARTESIAN_POINT('Ctrl Pts',(-7.61248038630268,21.6844494295815,
12.));
#244030=CARTESIAN_POINT('Ctrl Pts',(-7.61047325000956,21.6707639267576,
12.));
#244031=CARTESIAN_POINT('Ctrl Pts',(-7.60844738512874,21.6572484388081,
12.));
#244032=CARTESIAN_POINT('Ctrl Pts',(-7.60640395216357,21.6439048771743,
12.));
#244033=CARTESIAN_POINT('Ctrl Pts',(-7.60434414118296,21.6307351973822,
12.));
#244034=CARTESIAN_POINT('Ctrl Pts',(-7.60226917285429,21.617741400599,12.));
#244035=CARTESIAN_POINT('Ctrl Pts',(-7.60018029988241,21.6049255358843,
12.));
#244036=CARTESIAN_POINT('Ctrl Pts',(-7.59807880846195,21.5922897024466,
12.));
#244037=CARTESIAN_POINT('Ctrl Pts',(-7.59596601973584,21.5798360518978,
12.));
#244038=CARTESIAN_POINT('Ctrl Pts',(-7.59384329124918,21.5675667904726,
12.));
#244039=CARTESIAN_POINT('Ctrl Pts',(-7.59171201844777,21.5554841813462,
12.));
#244040=CARTESIAN_POINT('Ctrl Pts',(-7.58957363620014,21.543590547011,12.));
#244041=CARTESIAN_POINT('Ctrl Pts',(-7.58742962034834,21.5318882716736,
12.));
#244042=CARTESIAN_POINT('Ctrl Pts',(-7.5852814891913,21.5203798035299,12.));
#244043=CARTESIAN_POINT('Ctrl Pts',(-7.5831308051918,21.5090676573873,12.));
#244044=CARTESIAN_POINT('Ctrl Pts',(-7.58097917790744,21.4979544192744,
12.));
#244045=CARTESIAN_POINT('Ctrl Pts',(-7.57882826679132,21.4870427508194,
12.));
#244046=CARTESIAN_POINT('Ctrl Pts',(-7.57667978402987,21.4763353936762,
12.));
#244047=CARTESIAN_POINT('Ctrl Pts',(-7.57453549743412,21.4658351740128,
12.));
#244048=CARTESIAN_POINT('Ctrl Pts',(-7.57239723223506,21.4555450053142,
12.));
#244049=CARTESIAN_POINT('Ctrl Pts',(-7.57026687261166,21.4454678907509,
12.));
#244050=CARTESIAN_POINT('Ctrl Pts',(-7.56814636360847,21.4356069261513,
12.));
#244051=CARTESIAN_POINT('Ctrl Pts',(-7.56603771218712,21.4259653015736,
12.));
#244052=CARTESIAN_POINT('Ctrl Pts',(-7.56394299313685,21.4165463106254,
12.));
#244053=CARTESIAN_POINT('Ctrl Pts',(-7.56186435703622,21.4073533630365,
12.));
#244054=CARTESIAN_POINT('Ctrl Pts',(-7.55980403700611,21.3983899952987,
12.));
#244055=CARTESIAN_POINT('Ctrl Pts',(-7.55776435731417,21.3896598842117,
12.));
#244056=CARTESIAN_POINT('Ctrl Pts',(-7.55574773403503,21.3811668478932,
12.));
#244057=CARTESIAN_POINT('Ctrl Pts',(-7.55375667080029,21.3729148390243,
12.));
#244058=CARTESIAN_POINT('Ctrl Pts',(-7.55179375777444,21.3649079431865,
12.));
#244059=CARTESIAN_POINT('Ctrl Pts',(-7.5498616652131,21.3571503685855,12.));
#244060=CARTESIAN_POINT('Ctrl Pts',(-7.5479631624633,21.3496464761531,12.));
#244061=CARTESIAN_POINT('Ctrl Pts',(-7.54610114948347,21.3424008295038,
12.));
#244062=CARTESIAN_POINT('Ctrl Pts',(-7.54427868151268,21.3354182340149,
12.));
#244063=CARTESIAN_POINT('Ctrl Pts',(-7.54249900377031,21.328703791771,12.));
#244064=CARTESIAN_POINT('Ctrl Pts',(-7.54076552038279,21.3222628524165,
12.));
#244065=CARTESIAN_POINT('Ctrl Pts',(-7.53908175169898,21.3161009456256,
12.));
#244066=CARTESIAN_POINT('Ctrl Pts',(-7.53745129364616,21.310223716773,12.));
#244067=CARTESIAN_POINT('Ctrl Pts',(-7.53587778251736,21.3046368712157,
12.));
#244068=CARTESIAN_POINT('Ctrl Pts',(-7.53436505309943,21.2993464250717,
12.));
#244069=CARTESIAN_POINT('Ctrl Pts',(-7.53291726078527,21.2943588989331,
12.));
#244070=CARTESIAN_POINT('Ctrl Pts',(-7.53153906987855,21.2896816163842,
12.));
#244071=CARTESIAN_POINT('Ctrl Pts',(-7.53023562438229,21.2853226580657,
12.));
#244072=CARTESIAN_POINT('Ctrl Pts',(-7.52901217930408,21.2812902781143,
12.));
#244073=CARTESIAN_POINT('Ctrl Pts',(-7.52787386225333,21.2775925269652,
12.));
#244074=CARTESIAN_POINT('Ctrl Pts',(-7.52682526918541,21.2742366113579,
12.));
#244075=CARTESIAN_POINT('Ctrl Pts',(-7.5258712609553,21.2712301573466,12.));
#244076=CARTESIAN_POINT('Ctrl Pts',(-7.5250177033353,21.2685823838671,12.));
#244077=CARTESIAN_POINT('Ctrl Pts',(-7.52427261074298,21.2663059157058,
12.));
#244078=CARTESIAN_POINT('Ctrl Pts',(-7.52364573027553,21.2644161259962,
12.));
#244079=CARTESIAN_POINT('Ctrl Pts',(-7.52314642316199,21.262927782038,12.));
#244080=CARTESIAN_POINT('Ctrl Pts',(-7.5227818224267,21.2618521283555,12.));
#244081=CARTESIAN_POINT('Ctrl Pts',(-7.52260064231661,21.261326054066,12.));
#244082=CARTESIAN_POINT('Ctrl Pts',(-7.52252744144904,21.2611204474866,
12.));
#244083=CARTESIAN_POINT('Ctrl Pts',(-7.5225064970397,21.2610673466886,12.));
#244084=CARTESIAN_POINT('Ctrl Pts',(-7.52250298901264,21.2610617890679,
12.));
#244085=CARTESIAN_POINT('',(-7.36589684767344,24.9347862158358,0.));
#244086=CARTESIAN_POINT('Origin',(-1.68110656504246,21.4341755315424,0.));
#244087=CARTESIAN_POINT('',(-1.76341220531179,22.4835757167854,12.));
#244088=CARTESIAN_POINT('',(-0.840553282521227,10.7170877657712,12.));
#244089=CARTESIAN_POINT('',(-1.76341220531179,22.4835757167854,0.));
#244090=CARTESIAN_POINT('',(-1.76341220531179,22.4835757167854,0.));
#244091=CARTESIAN_POINT('',(-0.840553282521227,10.7170877657712,0.));
#244092=CARTESIAN_POINT('Ctrl Pts',(-6.08833931617698,25.2771067246846,
0.));
#244093=CARTESIAN_POINT('Ctrl Pts',(-6.08833931617698,25.2771067246846,
12.));
#244094=CARTESIAN_POINT('Ctrl Pts',(-6.08441489609824,25.2729539149479,
0.));
#244095=CARTESIAN_POINT('Ctrl Pts',(-6.08441489609824,25.2729539149479,
12.));
#244096=CARTESIAN_POINT('Ctrl Pts',(-6.07657531787578,25.2646490489816,
0.));
#244097=CARTESIAN_POINT('Ctrl Pts',(-6.07657531787578,25.2646490489816,
12.));
#244098=CARTESIAN_POINT('Ctrl Pts',(-6.06484373634697,25.2521940105523,
0.));
#244099=CARTESIAN_POINT('Ctrl Pts',(-6.06484373634697,25.2521940105523,
12.));
#244100=CARTESIAN_POINT('Ctrl Pts',(-6.04925720151412,25.2355918138798,
0.));
#244101=CARTESIAN_POINT('Ctrl Pts',(-6.04925720151412,25.2355918138798,
12.));
#244102=CARTESIAN_POINT('Ctrl Pts',(-6.02986667390187,25.2148466201368,
0.));
#244103=CARTESIAN_POINT('Ctrl Pts',(-6.02986667390187,25.2148466201368,
12.));
#244104=CARTESIAN_POINT('Ctrl Pts',(-6.0105688180476,25.1941090269638,0.));
#244105=CARTESIAN_POINT('Ctrl Pts',(-6.0105688180476,25.1941090269638,12.));
#244106=CARTESIAN_POINT('Ctrl Pts',(-5.99136367859838,25.1733791296154,
0.));
#244107=CARTESIAN_POINT('Ctrl Pts',(-5.99136367859838,25.1733791296154,
12.));
#244108=CARTESIAN_POINT('Ctrl Pts',(-5.97225131495636,25.1526570863065,
0.));
#244109=CARTESIAN_POINT('Ctrl Pts',(-5.97225131495636,25.1526570863065,
12.));
#244110=CARTESIAN_POINT('Ctrl Pts',(-5.95323180187348,25.1319431317273,
0.));
#244111=CARTESIAN_POINT('Ctrl Pts',(-5.95323180187348,25.1319431317273,
12.));
#244112=CARTESIAN_POINT('Ctrl Pts',(-5.93430523086776,25.1112375971182,
0.));
#244113=CARTESIAN_POINT('Ctrl Pts',(-5.93430523086776,25.1112375971182,
12.));
#244114=CARTESIAN_POINT('Ctrl Pts',(-5.91547170844382,25.0905409050863,
0.));
#244115=CARTESIAN_POINT('Ctrl Pts',(-5.91547170844382,25.0905409050863,
12.));
#244116=CARTESIAN_POINT('Ctrl Pts',(-5.89673135155459,25.0698535426593,
0.));
#244117=CARTESIAN_POINT('Ctrl Pts',(-5.89673135155459,25.0698535426593,
12.));
#244118=CARTESIAN_POINT('Ctrl Pts',(-5.87808428385329,25.0491760405965,
0.));
#244119=CARTESIAN_POINT('Ctrl Pts',(-5.87808428385329,25.0491760405965,
12.));
#244120=CARTESIAN_POINT('Ctrl Pts',(-5.8595306315681,25.0285089498922,0.));
#244121=CARTESIAN_POINT('Ctrl Pts',(-5.8595306315681,25.0285089498922,12.));
#244122=CARTESIAN_POINT('Ctrl Pts',(-5.84107051963073,25.0078528200558,
0.));
#244123=CARTESIAN_POINT('Ctrl Pts',(-5.84107051963073,25.0078528200558,
12.));
#244124=CARTESIAN_POINT('Ctrl Pts',(-5.82270406744214,24.9872081752709,
0.));
#244125=CARTESIAN_POINT('Ctrl Pts',(-5.82270406744214,24.9872081752709,
12.));
#244126=CARTESIAN_POINT('Ctrl Pts',(-5.80443138549747,24.9665754954462,
0.));
#244127=CARTESIAN_POINT('Ctrl Pts',(-5.80443138549747,24.9665754954462,
12.));
#244128=CARTESIAN_POINT('Ctrl Pts',(-5.78625257775703,24.9459552293308,
0.));
#244129=CARTESIAN_POINT('Ctrl Pts',(-5.78625257775703,24.9459552293308,
12.));
#244130=CARTESIAN_POINT('Ctrl Pts',(-5.76816774342236,24.9253478043632,
0.));
#244131=CARTESIAN_POINT('Ctrl Pts',(-5.76816774342236,24.9253478043632,
12.));
#244132=CARTESIAN_POINT('Ctrl Pts',(-5.75017697890813,24.9047536376467,
0.));
#244133=CARTESIAN_POINT('Ctrl Pts',(-5.75017697890813,24.9047536376467,
12.));
#244134=CARTESIAN_POINT('Ctrl Pts',(-5.73228037976927,24.8841731467219,
0.));
#244135=CARTESIAN_POINT('Ctrl Pts',(-5.73228037976927,24.8841731467219,
12.));
#244136=CARTESIAN_POINT('Ctrl Pts',(-5.71447804252019,24.8636067597677,
0.));
#244137=CARTESIAN_POINT('Ctrl Pts',(-5.71447804252019,24.8636067597677,
12.));
#244138=CARTESIAN_POINT('Ctrl Pts',(-5.69677006679429,24.8430549277634,
0.));
#244139=CARTESIAN_POINT('Ctrl Pts',(-5.69677006679429,24.8430549277634,
12.));
#244140=CARTESIAN_POINT('Ctrl Pts',(-5.67915655496524,24.822518122386,0.));
#244141=CARTESIAN_POINT('Ctrl Pts',(-5.67915655496524,24.822518122386,12.));
#244142=CARTESIAN_POINT('Ctrl Pts',(-5.66163761114903,24.8019968304618,
0.));
#244143=CARTESIAN_POINT('Ctrl Pts',(-5.66163761114903,24.8019968304618,
12.));
#244144=CARTESIAN_POINT('Ctrl Pts',(-5.64421334042248,24.7814915496728,
0.));
#244145=CARTESIAN_POINT('Ctrl Pts',(-5.64421334042248,24.7814915496728,
12.));
#244146=CARTESIAN_POINT('Ctrl Pts',(-5.62688384790919,24.76100278357,0.));
#244147=CARTESIAN_POINT('Ctrl Pts',(-5.62688384790919,24.76100278357,12.));
#244148=CARTESIAN_POINT('Ctrl Pts',(-5.60964923798495,24.7405310372736,
0.));
#244149=CARTESIAN_POINT('Ctrl Pts',(-5.60964923798495,24.7405310372736,
12.));
#244150=CARTESIAN_POINT('Ctrl Pts',(-5.59250961323995,24.7200768119079,
0.));
#244151=CARTESIAN_POINT('Ctrl Pts',(-5.59250961323995,24.7200768119079,
12.));
#244152=CARTESIAN_POINT('Ctrl Pts',(-5.57546507427767,24.6996406035507,
0.));
#244153=CARTESIAN_POINT('Ctrl Pts',(-5.57546507427767,24.6996406035507,
12.));
#244154=CARTESIAN_POINT('Ctrl Pts',(-5.55851572025389,24.6792229061785,
0.));
#244155=CARTESIAN_POINT('Ctrl Pts',(-5.55851572025389,24.6792229061785,
12.));
#244156=CARTESIAN_POINT('Ctrl Pts',(-5.54166164919593,24.6588242134733,
0.));
#244157=CARTESIAN_POINT('Ctrl Pts',(-5.54166164919593,24.6588242134733,
12.));
#244158=CARTESIAN_POINT('Ctrl Pts',(-5.52490295840996,24.6384450211466,
0.));
#244159=CARTESIAN_POINT('Ctrl Pts',(-5.52490295840996,24.6384450211466,
12.));
#244160=CARTESIAN_POINT('Ctrl Pts',(-5.50823974481959,24.618085828918,0.));
#244161=CARTESIAN_POINT('Ctrl Pts',(-5.50823974481959,24.618085828918,12.));
#244162=CARTESIAN_POINT('Ctrl Pts',(-5.49167210537235,24.5977471429365,
0.));
#244163=CARTESIAN_POINT('Ctrl Pts',(-5.49167210537235,24.5977471429365,
12.));
#244164=CARTESIAN_POINT('Ctrl Pts',(-5.47520013724403,24.5774294770329,
0.));
#244165=CARTESIAN_POINT('Ctrl Pts',(-5.47520013724403,24.5774294770329,
12.));
#244166=CARTESIAN_POINT('Ctrl Pts',(-5.45882393762244,24.5571333514841,
0.));
#244167=CARTESIAN_POINT('Ctrl Pts',(-5.45882393762244,24.5571333514841,
12.));
#244168=CARTESIAN_POINT('Ctrl Pts',(-5.44254360356865,24.5368592922861,
0.));
#244169=CARTESIAN_POINT('Ctrl Pts',(-5.44254360356865,24.5368592922861,
12.));
#244170=CARTESIAN_POINT('Ctrl Pts',(-5.42635923183411,24.5166078302107,
0.));
#244171=CARTESIAN_POINT('Ctrl Pts',(-5.42635923183411,24.5166078302107,
12.));
#244172=CARTESIAN_POINT('Ctrl Pts',(-5.41027091869242,24.4963794999831,
0.));
#244173=CARTESIAN_POINT('Ctrl Pts',(-5.41027091869242,24.4963794999831,
12.));
#244174=CARTESIAN_POINT('Ctrl Pts',(-5.3942787597383,24.4761748393322,0.));
#244175=CARTESIAN_POINT('Ctrl Pts',(-5.3942787597383,24.4761748393322,12.));
#244176=CARTESIAN_POINT('Ctrl Pts',(-5.37838284973706,24.4559943883159,
0.));
#244177=CARTESIAN_POINT('Ctrl Pts',(-5.37838284973706,24.4559943883159,
12.));
#244178=CARTESIAN_POINT('Ctrl Pts',(-5.36258328273639,24.4358386899152,
0.));
#244179=CARTESIAN_POINT('Ctrl Pts',(-5.36258328273639,24.4358386899152,
12.));
#244180=CARTESIAN_POINT('Ctrl Pts',(-5.34688015213546,24.4157082904615,
0.));
#244181=CARTESIAN_POINT('Ctrl Pts',(-5.34688015213546,24.4157082904615,
12.));
#244182=CARTESIAN_POINT('Ctrl Pts',(-5.33127355076037,24.3956037401293,
0.));
#244183=CARTESIAN_POINT('Ctrl Pts',(-5.33127355076037,24.3956037401293,
12.));
#244184=CARTESIAN_POINT('Ctrl Pts',(-5.31576357092524,24.3755255933917,
0.));
#244185=CARTESIAN_POINT('Ctrl Pts',(-5.31576357092524,24.3755255933917,
12.));
#244186=CARTESIAN_POINT('Ctrl Pts',(-5.30035030449059,24.3554744095075,
0.));
#244187=CARTESIAN_POINT('Ctrl Pts',(-5.30035030449059,24.3554744095075,
12.));
#244188=CARTESIAN_POINT('Ctrl Pts',(-5.28503384290644,24.3354507529415,
0.));
#244189=CARTESIAN_POINT('Ctrl Pts',(-5.28503384290644,24.3354507529415,
12.));
#244190=CARTESIAN_POINT('Ctrl Pts',(-5.26981427718796,24.3154551932222,
0.));
#244191=CARTESIAN_POINT('Ctrl Pts',(-5.26981427718796,24.3154551932222,
12.));
#244192=CARTESIAN_POINT('Ctrl Pts',(-5.25469169788856,24.2954883048448,
0.));
#244193=CARTESIAN_POINT('Ctrl Pts',(-5.25469169788856,24.2954883048448,
12.));
#244194=CARTESIAN_POINT('Ctrl Pts',(-5.23966619506289,24.2755506671526,
0.));
#244195=CARTESIAN_POINT('Ctrl Pts',(-5.23966619506289,24.2755506671526,
12.));
#244196=CARTESIAN_POINT('Ctrl Pts',(-5.22473785822441,24.2556428642294,
0.));
#244197=CARTESIAN_POINT('Ctrl Pts',(-5.22473785822441,24.2556428642294,
12.));
#244198=CARTESIAN_POINT('Ctrl Pts',(-5.20990677629173,24.2357654847765,
0.));
#244199=CARTESIAN_POINT('Ctrl Pts',(-5.20990677629173,24.2357654847765,
12.));
#244200=CARTESIAN_POINT('Ctrl Pts',(-5.19517303753643,24.215919122017,0.));
#244201=CARTESIAN_POINT('Ctrl Pts',(-5.19517303753643,24.215919122017,12.));
#244202=CARTESIAN_POINT('Ctrl Pts',(-5.18053672961392,24.1961043738754,
0.));
#244203=CARTESIAN_POINT('Ctrl Pts',(-5.18053672961392,24.1961043738754,
12.));
#244204=CARTESIAN_POINT('Ctrl Pts',(-5.16599793957979,24.1763218431343,
0.));
#244205=CARTESIAN_POINT('Ctrl Pts',(-5.16599793957979,24.1763218431343,
12.));
#244206=CARTESIAN_POINT('Ctrl Pts',(-5.15155675390075,24.156572137597,0.));
#244207=CARTESIAN_POINT('Ctrl Pts',(-5.15155675390075,24.156572137597,12.));
#244208=CARTESIAN_POINT('Ctrl Pts',(-5.13721325845745,24.1368558702443,
0.));
#244209=CARTESIAN_POINT('Ctrl Pts',(-5.13721325845745,24.1368558702443,
12.));
#244210=CARTESIAN_POINT('Ctrl Pts',(-5.12296753853859,24.117173659394,0.));
#244211=CARTESIAN_POINT('Ctrl Pts',(-5.12296753853859,24.117173659394,12.));
#244212=CARTESIAN_POINT('Ctrl Pts',(-5.10881967883132,24.0975261288446,
0.));
#244213=CARTESIAN_POINT('Ctrl Pts',(-5.10881967883132,24.0975261288446,
12.));
#244214=CARTESIAN_POINT('Ctrl Pts',(-5.09476976342625,24.0779139079266,
0.));
#244215=CARTESIAN_POINT('Ctrl Pts',(-5.09476976342625,24.0779139079266,
12.));
#244216=CARTESIAN_POINT('Ctrl Pts',(-5.08081787581276,24.0583376315638,
0.));
#244217=CARTESIAN_POINT('Ctrl Pts',(-5.08081787581276,24.0583376315638,
12.));
#244218=CARTESIAN_POINT('Ctrl Pts',(-5.06696409886641,24.0387979403268,
0.));
#244219=CARTESIAN_POINT('Ctrl Pts',(-5.06696409886641,24.0387979403268,
12.));
#244220=CARTESIAN_POINT('Ctrl Pts',(-5.05320851483065,24.0192954804896,
0.));
#244221=CARTESIAN_POINT('Ctrl Pts',(-5.05320851483065,24.0192954804896,
12.));
#244222=CARTESIAN_POINT('Ctrl Pts',(-5.03955120528521,23.9998309040746,
0.));
#244223=CARTESIAN_POINT('Ctrl Pts',(-5.03955120528521,23.9998309040746,
12.));
#244224=CARTESIAN_POINT('Ctrl Pts',(-5.02599225112454,23.9804048689227,
0.));
#244225=CARTESIAN_POINT('Ctrl Pts',(-5.02599225112454,23.9804048689227,
12.));
#244226=CARTESIAN_POINT('Ctrl Pts',(-5.01253173257453,23.9610180388271,
0.));
#244227=CARTESIAN_POINT('Ctrl Pts',(-5.01253173257453,23.9610180388271,
12.));
#244228=CARTESIAN_POINT('Ctrl Pts',(-4.99916972919307,23.9416710836529,
0.));
#244229=CARTESIAN_POINT('Ctrl Pts',(-4.99916972919307,23.9416710836529,
12.));
#244230=CARTESIAN_POINT('Ctrl Pts',(-4.98590631986533,23.9223646794592,
0.));
#244231=CARTESIAN_POINT('Ctrl Pts',(-4.98590631986533,23.9223646794592,
12.));
#244232=CARTESIAN_POINT('Ctrl Pts',(-4.97274158279227,23.9030995086163,
0.));
#244233=CARTESIAN_POINT('Ctrl Pts',(-4.97274158279227,23.9030995086163,
12.));
#244234=CARTESIAN_POINT('Ctrl Pts',(-4.95967559546561,23.8838762599218,
0.));
#244235=CARTESIAN_POINT('Ctrl Pts',(-4.95967559546561,23.8838762599218,
12.));
#244236=CARTESIAN_POINT('Ctrl Pts',(-4.9467084346586,23.8646956287168,0.));
#244237=CARTESIAN_POINT('Ctrl Pts',(-4.9467084346586,23.8646956287168,12.));
#244238=CARTESIAN_POINT('Ctrl Pts',(-4.93384017643432,23.8455583170057,
0.));
#244239=CARTESIAN_POINT('Ctrl Pts',(-4.93384017643432,23.8455583170057,
12.));
#244240=CARTESIAN_POINT('Ctrl Pts',(-4.92107089613969,23.8264650335717,
0.));
#244241=CARTESIAN_POINT('Ctrl Pts',(-4.92107089613969,23.8264650335717,
12.));
#244242=CARTESIAN_POINT('Ctrl Pts',(-4.90840066839344,23.8074164940896,
0.));
#244243=CARTESIAN_POINT('Ctrl Pts',(-4.90840066839344,23.8074164940896,
12.));
#244244=CARTESIAN_POINT('Ctrl Pts',(-4.89582956706775,23.7884134212384,
0.));
#244245=CARTESIAN_POINT('Ctrl Pts',(-4.89582956706775,23.7884134212384,
12.));
#244246=CARTESIAN_POINT('Ctrl Pts',(-4.88335766525573,23.7694565448049,
0.));
#244247=CARTESIAN_POINT('Ctrl Pts',(-4.88335766525573,23.7694565448049,
12.));
#244248=CARTESIAN_POINT('Ctrl Pts',(-4.87098503527152,23.7505466018245,
0.));
#244249=CARTESIAN_POINT('Ctrl Pts',(-4.87098503527152,23.7505466018245,
12.));
#244250=CARTESIAN_POINT('Ctrl Pts',(-4.85871174865499,23.7316843367313,
0.));
#244251=CARTESIAN_POINT('Ctrl Pts',(-4.85871174865499,23.7316843367313,
12.));
#244252=CARTESIAN_POINT('Ctrl Pts',(-4.84653787616425,23.7128705015017,
0.));
#244253=CARTESIAN_POINT('Ctrl Pts',(-4.84653787616425,23.7128705015017,
12.));
#244254=CARTESIAN_POINT('Ctrl Pts',(-4.83446348776266,23.6941058557971,
0.));
#244255=CARTESIAN_POINT('Ctrl Pts',(-4.83446348776266,23.6941058557971,
12.));
#244256=CARTESIAN_POINT('Ctrl Pts',(-4.82248865259562,23.675391167102,0.));
#244257=CARTESIAN_POINT('Ctrl Pts',(-4.82248865259562,23.675391167102,12.));
#244258=CARTESIAN_POINT('Ctrl Pts',(-4.81061343896432,23.6567272108628,
0.));
#244259=CARTESIAN_POINT('Ctrl Pts',(-4.81061343896432,23.6567272108628,
12.));
#244260=CARTESIAN_POINT('Ctrl Pts',(-4.7988379143322,23.6381147706579,0.));
#244261=CARTESIAN_POINT('Ctrl Pts',(-4.7988379143322,23.6381147706579,12.));
#244262=CARTESIAN_POINT('Ctrl Pts',(-4.78716214532098,23.6195546383624,
0.));
#244263=CARTESIAN_POINT('Ctrl Pts',(-4.78716214532098,23.6195546383624,
12.));
#244264=CARTESIAN_POINT('Ctrl Pts',(-4.77558619769872,23.6010476143099,
0.));
#244265=CARTESIAN_POINT('Ctrl Pts',(-4.77558619769872,23.6010476143099,
12.));
#244266=CARTESIAN_POINT('Ctrl Pts',(-4.76411013636251,23.5825945074535,
0.));
#244267=CARTESIAN_POINT('Ctrl Pts',(-4.76411013636251,23.5825945074535,
12.));
#244268=CARTESIAN_POINT('Ctrl Pts',(-4.75273402530617,23.5641961355168,
0.));
#244269=CARTESIAN_POINT('Ctrl Pts',(-4.75273402530617,23.5641961355168,
12.));
#244270=CARTESIAN_POINT('Ctrl Pts',(-4.74145792760698,23.545853325171,0.));
#244271=CARTESIAN_POINT('Ctrl Pts',(-4.74145792760698,23.545853325171,12.));
#244272=CARTESIAN_POINT('Ctrl Pts',(-4.7302819054303,23.5275669122372,0.));
#244273=CARTESIAN_POINT('Ctrl Pts',(-4.7302819054303,23.5275669122372,12.));
#244274=CARTESIAN_POINT('Ctrl Pts',(-4.71920602001902,23.509337741878,0.));
#244275=CARTESIAN_POINT('Ctrl Pts',(-4.71920602001902,23.509337741878,12.));
#244276=CARTESIAN_POINT('Ctrl Pts',(-4.70823033167819,23.491166668789,0.));
#244277=CARTESIAN_POINT('Ctrl Pts',(-4.70823033167819,23.491166668789,12.));
#244278=CARTESIAN_POINT('Ctrl Pts',(-4.69735489975024,23.4730545573853,
0.));
#244279=CARTESIAN_POINT('Ctrl Pts',(-4.69735489975024,23.4730545573853,
12.));
#244280=CARTESIAN_POINT('Ctrl Pts',(-4.68657978258303,23.455002281986,0.));
#244281=CARTESIAN_POINT('Ctrl Pts',(-4.68657978258303,23.455002281986,12.));
#244282=CARTESIAN_POINT('Ctrl Pts',(-4.67590503753058,23.4370107270451,
0.));
#244283=CARTESIAN_POINT('Ctrl Pts',(-4.67590503753058,23.4370107270451,
12.));
#244284=CARTESIAN_POINT('Ctrl Pts',(-4.6653307209467,23.4190807873803,0.));
#244285=CARTESIAN_POINT('Ctrl Pts',(-4.6653307209467,23.4190807873803,12.));
#244286=CARTESIAN_POINT('Ctrl Pts',(-4.65485688816924,23.4012133683959,
0.));
#244287=CARTESIAN_POINT('Ctrl Pts',(-4.65485688816924,23.4012133683959,
12.));
#244288=CARTESIAN_POINT('Ctrl Pts',(-4.6444835934993,23.3834093863068,0.));
#244289=CARTESIAN_POINT('Ctrl Pts',(-4.6444835934993,23.3834093863068,12.));
#244290=CARTESIAN_POINT('Ctrl Pts',(-4.63421089016541,23.3656697683489,
0.));
#244291=CARTESIAN_POINT('Ctrl Pts',(-4.63421089016541,23.3656697683489,
12.));
#244292=CARTESIAN_POINT('Ctrl Pts',(-4.62403883030805,23.3479954530272,
0.));
#244293=CARTESIAN_POINT('Ctrl Pts',(-4.62403883030805,23.3479954530272,
12.));
#244294=CARTESIAN_POINT('Ctrl Pts',(-4.6139674649783,23.3303873903938,0.));
#244295=CARTESIAN_POINT('Ctrl Pts',(-4.6139674649783,23.3303873903938,12.));
#244296=CARTESIAN_POINT('Ctrl Pts',(-4.60399684412163,23.3128465423115,
0.));
#244297=CARTESIAN_POINT('Ctrl Pts',(-4.60399684412163,23.3128465423115,
12.));
#244298=CARTESIAN_POINT('Ctrl Pts',(-4.5941270165575,23.2953738827191,0.));
#244299=CARTESIAN_POINT('Ctrl Pts',(-4.5941270165575,23.2953738827191,12.));
#244300=CARTESIAN_POINT('Ctrl Pts',(-4.5843580299469,23.2779703978876,0.));
#244301=CARTESIAN_POINT('Ctrl Pts',(-4.5843580299469,23.2779703978876,12.));
#244302=CARTESIAN_POINT('Ctrl Pts',(-4.57468993076097,23.2606370866866,
0.));
#244303=CARTESIAN_POINT('Ctrl Pts',(-4.57468993076097,23.2606370866866,
12.));
#244304=CARTESIAN_POINT('Ctrl Pts',(-4.56512276427839,23.2433749609131,
0.));
#244305=CARTESIAN_POINT('Ctrl Pts',(-4.56512276427839,23.2433749609131,
12.));
#244306=CARTESIAN_POINT('Ctrl Pts',(-4.55565657456975,23.2261850456064,
0.));
#244307=CARTESIAN_POINT('Ctrl Pts',(-4.55565657456975,23.2261850456064,
12.));
#244308=CARTESIAN_POINT('Ctrl Pts',(-4.54629140447544,23.2090683793629,
0.));
#244309=CARTESIAN_POINT('Ctrl Pts',(-4.54629140447544,23.2090683793629,
12.));
#244310=CARTESIAN_POINT('Ctrl Pts',(-4.53702729557566,23.1920260146465,
0.));
#244311=CARTESIAN_POINT('Ctrl Pts',(-4.53702729557566,23.1920260146465,
12.));
#244312=CARTESIAN_POINT('Ctrl Pts',(-4.52786428815015,23.1750590180908,
0.));
#244313=CARTESIAN_POINT('Ctrl Pts',(-4.52786428815015,23.1750590180908,
12.));
#244314=CARTESIAN_POINT('Ctrl Pts',(-4.51880242116748,23.1581684708761,
0.));
#244315=CARTESIAN_POINT('Ctrl Pts',(-4.51880242116748,23.1581684708761,
12.));
#244316=CARTESIAN_POINT('Ctrl Pts',(-4.5098417322706,23.1413554691123,0.));
#244317=CARTESIAN_POINT('Ctrl Pts',(-4.5098417322706,23.1413554691123,12.));
#244318=CARTESIAN_POINT('Ctrl Pts',(-4.50098225775171,23.1246211242115,
0.));
#244319=CARTESIAN_POINT('Ctrl Pts',(-4.50098225775171,23.1246211242115,
12.));
#244320=CARTESIAN_POINT('Ctrl Pts',(-4.49222403252216,23.1079665632636,
0.));
#244321=CARTESIAN_POINT('Ctrl Pts',(-4.49222403252216,23.1079665632636,
12.));
#244322=CARTESIAN_POINT('Ctrl Pts',(-4.48356709006788,23.0913929293922,
0.));
#244323=CARTESIAN_POINT('Ctrl Pts',(-4.48356709006788,23.0913929293922,
12.));
#244324=CARTESIAN_POINT('Ctrl Pts',(-4.47501146242856,23.0749013821881,
0.));
#244325=CARTESIAN_POINT('Ctrl Pts',(-4.47501146242856,23.0749013821881,
12.));
#244326=CARTESIAN_POINT('Ctrl Pts',(-4.4665571801823,23.0584930981732,0.));
#244327=CARTESIAN_POINT('Ctrl Pts',(-4.4665571801823,23.0584930981732,12.));
#244328=CARTESIAN_POINT('Ctrl Pts',(-4.45820427241683,23.0421692712467,
0.));
#244329=CARTESIAN_POINT('Ctrl Pts',(-4.45820427241683,23.0421692712467,
12.));
#244330=CARTESIAN_POINT('Ctrl Pts',(-4.44995276669686,23.0259311131392,
0.));
#244331=CARTESIAN_POINT('Ctrl Pts',(-4.44995276669686,23.0259311131392,
12.));
#244332=CARTESIAN_POINT('Ctrl Pts',(-4.44180268901643,23.0097798538395,
0.));
#244333=CARTESIAN_POINT('Ctrl Pts',(-4.44180268901643,23.0097798538395,
12.));
#244334=CARTESIAN_POINT('Ctrl Pts',(-4.43375406376879,22.9937167421006,
0.));
#244335=CARTESIAN_POINT('Ctrl Pts',(-4.43375406376879,22.9937167421006,
12.));
#244336=CARTESIAN_POINT('Ctrl Pts',(-4.42580691372751,22.977743046002,0.));
#244337=CARTESIAN_POINT('Ctrl Pts',(-4.42580691372751,22.977743046002,12.));
#244338=CARTESIAN_POINT('Ctrl Pts',(-4.41796126001302,22.9618600534866,
0.));
#244339=CARTESIAN_POINT('Ctrl Pts',(-4.41796126001302,22.9618600534866,
12.));
#244340=CARTESIAN_POINT('Ctrl Pts',(-4.41021712205553,22.9460690729093,
0.));
#244341=CARTESIAN_POINT('Ctrl Pts',(-4.41021712205553,22.9460690729093,
12.));
#244342=CARTESIAN_POINT('Ctrl Pts',(-4.40257451754323,22.930371433555,0.));
#244343=CARTESIAN_POINT('Ctrl Pts',(-4.40257451754323,22.930371433555,12.));
#244344=CARTESIAN_POINT('Ctrl Pts',(-4.39503346238473,22.9147684862426,
0.));
#244345=CARTESIAN_POINT('Ctrl Pts',(-4.39503346238473,22.9147684862426,
12.));
#244346=CARTESIAN_POINT('Ctrl Pts',(-4.38759397068406,22.8992616040108,
0.));
#244347=CARTESIAN_POINT('Ctrl Pts',(-4.38759397068406,22.8992616040108,
12.));
#244348=CARTESIAN_POINT('Ctrl Pts',(-4.38025605470093,22.8838521827701,
0.));
#244349=CARTESIAN_POINT('Ctrl Pts',(-4.38025605470093,22.8838521827701,
12.));
#244350=CARTESIAN_POINT('Ctrl Pts',(-4.37301972480746,22.8685416419725,
0.));
#244351=CARTESIAN_POINT('Ctrl Pts',(-4.37301972480746,22.8685416419725,
12.));
#244352=CARTESIAN_POINT('Ctrl Pts',(-4.36588498942997,22.8533314252422,
0.));
#244353=CARTESIAN_POINT('Ctrl Pts',(-4.36588498942997,22.8533314252422,
12.));
#244354=CARTESIAN_POINT('Ctrl Pts',(-4.35885185500546,22.8382230011184,
0.));
#244355=CARTESIAN_POINT('Ctrl Pts',(-4.35885185500546,22.8382230011184,
12.));
#244356=CARTESIAN_POINT('Ctrl Pts',(-4.35192032594791,22.8232178638876,
0.));
#244357=CARTESIAN_POINT('Ctrl Pts',(-4.35192032594791,22.8232178638876,
12.));
#244358=CARTESIAN_POINT('Ctrl Pts',(-4.34509040460062,22.8083175343791,
0.));
#244359=CARTESIAN_POINT('Ctrl Pts',(-4.34509040460062,22.8083175343791,
12.));
#244360=CARTESIAN_POINT('Ctrl Pts',(-4.33836209118446,22.7935235607806,
0.));
#244361=CARTESIAN_POINT('Ctrl Pts',(-4.33836209118446,22.7935235607806,
12.));
#244362=CARTESIAN_POINT('Ctrl Pts',(-4.3317353837319,22.7788375194076,0.));
#244363=CARTESIAN_POINT('Ctrl Pts',(-4.3317353837319,22.7788375194076,12.));
#244364=CARTESIAN_POINT('Ctrl Pts',(-4.32521027803754,22.7642610156475,
0.));
#244365=CARTESIAN_POINT('Ctrl Pts',(-4.32521027803754,22.7642610156475,
12.));
#244366=CARTESIAN_POINT('Ctrl Pts',(-4.31878676761235,22.7497956849848,
0.));
#244367=CARTESIAN_POINT('Ctrl Pts',(-4.31878676761235,22.7497956849848,
12.));
#244368=CARTESIAN_POINT('Ctrl Pts',(-4.31246484362549,22.7354431939926,
0.));
#244369=CARTESIAN_POINT('Ctrl Pts',(-4.31246484362549,22.7354431939926,
12.));
#244370=CARTESIAN_POINT('Ctrl Pts',(-4.30624449484069,22.7212052413386,
0.));
#244371=CARTESIAN_POINT('Ctrl Pts',(-4.30624449484069,22.7212052413386,
12.));
#244372=CARTESIAN_POINT('Ctrl Pts',(-4.3001257075406,22.7070835587564,0.));
#244373=CARTESIAN_POINT('Ctrl Pts',(-4.3001257075406,22.7070835587564,12.));
#244374=CARTESIAN_POINT('Ctrl Pts',(-4.29410846547056,22.6930799122548,
0.));
#244375=CARTESIAN_POINT('Ctrl Pts',(-4.29410846547056,22.6930799122548,
12.));
#244376=CARTESIAN_POINT('Ctrl Pts',(-4.28819274977763,22.6791961033538,
0.));
#244377=CARTESIAN_POINT('Ctrl Pts',(-4.28819274977763,22.6791961033538,
12.));
#244378=CARTESIAN_POINT('Ctrl Pts',(-4.28237853894059,22.6654339703109,
0.));
#244379=CARTESIAN_POINT('Ctrl Pts',(-4.28237853894059,22.6654339703109,
12.));
#244380=CARTESIAN_POINT('Ctrl Pts',(-4.2766658086912,22.6517953893303,0.));
#244381=CARTESIAN_POINT('Ctrl Pts',(-4.2766658086912,22.6517953893303,12.));
#244382=CARTESIAN_POINT('Ctrl Pts',(-4.27105453193004,22.6382822758172,
0.));
#244383=CARTESIAN_POINT('Ctrl Pts',(-4.27105453193004,22.6382822758172,
12.));
#244384=CARTESIAN_POINT('Ctrl Pts',(-4.26554467865576,22.6248965859977,
0.));
#244385=CARTESIAN_POINT('Ctrl Pts',(-4.26554467865576,22.6248965859977,
12.));
#244386=CARTESIAN_POINT('Ctrl Pts',(-4.26013621588305,22.6116403184821,
0.));
#244387=CARTESIAN_POINT('Ctrl Pts',(-4.26013621588305,22.6116403184821,
12.));
#244388=CARTESIAN_POINT('Ctrl Pts',(-4.25482910755481,22.5985155158636,
0.));
#244389=CARTESIAN_POINT('Ctrl Pts',(-4.25482910755481,22.5985155158636,
12.));
#244390=CARTESIAN_POINT('Ctrl Pts',(-4.24962331444177,22.5855242662477,
0.));
#244391=CARTESIAN_POINT('Ctrl Pts',(-4.24962331444177,22.5855242662477,
12.));
#244392=CARTESIAN_POINT('Ctrl Pts',(-4.24451879404851,22.572668704992,0.));
#244393=CARTESIAN_POINT('Ctrl Pts',(-4.24451879404851,22.572668704992,12.));
#244394=CARTESIAN_POINT('Ctrl Pts',(-4.23951550052523,22.5599510166429,
0.));
#244395=CARTESIAN_POINT('Ctrl Pts',(-4.23951550052523,22.5599510166429,
12.));
#244396=CARTESIAN_POINT('Ctrl Pts',(-4.23461338456712,22.5473734368086,
0.));
#244397=CARTESIAN_POINT('Ctrl Pts',(-4.23461338456712,22.5473734368086,
12.));
#244398=CARTESIAN_POINT('Ctrl Pts',(-4.22981239330733,22.5349382540588,
0.));
#244399=CARTESIAN_POINT('Ctrl Pts',(-4.22981239330733,22.5349382540588,
12.));
#244400=CARTESIAN_POINT('Ctrl Pts',(-4.22511247020041,22.5226478117886,
0.));
#244401=CARTESIAN_POINT('Ctrl Pts',(-4.22511247020041,22.5226478117886,
12.));
#244402=CARTESIAN_POINT('Ctrl Pts',(-4.22051355490196,22.5105045108881,
0.));
#244403=CARTESIAN_POINT('Ctrl Pts',(-4.22051355490196,22.5105045108881,
12.));
#244404=CARTESIAN_POINT('Ctrl Pts',(-4.21601558313906,22.4985108124228,
0.));
#244405=CARTESIAN_POINT('Ctrl Pts',(-4.21601558313906,22.4985108124228,
12.));
#244406=CARTESIAN_POINT('Ctrl Pts',(-4.21161848657428,22.4866692403147,
0.));
#244407=CARTESIAN_POINT('Ctrl Pts',(-4.21161848657428,22.4866692403147,
12.));
#244408=CARTESIAN_POINT('Ctrl Pts',(-4.20732219265649,22.4749823839917,
0.));
#244409=CARTESIAN_POINT('Ctrl Pts',(-4.20732219265649,22.4749823839917,
12.));
#244410=CARTESIAN_POINT('Ctrl Pts',(-4.20312662448174,22.4634529011437,
0.));
#244411=CARTESIAN_POINT('Ctrl Pts',(-4.20312662448174,22.4634529011437,
12.));
#244412=CARTESIAN_POINT('Ctrl Pts',(-4.19903170066358,22.4520835205422,
0.));
#244413=CARTESIAN_POINT('Ctrl Pts',(-4.19903170066358,22.4520835205422,
12.));
#244414=CARTESIAN_POINT('Ctrl Pts',(-4.1950373351886,22.4408770448917,0.));
#244415=CARTESIAN_POINT('Ctrl Pts',(-4.1950373351886,22.4408770448917,12.));
#244416=CARTESIAN_POINT('Ctrl Pts',(-4.19114343726932,22.4298363535416,
0.));
#244417=CARTESIAN_POINT('Ctrl Pts',(-4.19114343726932,22.4298363535416,
12.));
#244418=CARTESIAN_POINT('Ctrl Pts',(-4.18734991117707,22.4189644056109,
0.));
#244419=CARTESIAN_POINT('Ctrl Pts',(-4.18734991117707,22.4189644056109,
12.));
#244420=CARTESIAN_POINT('Ctrl Pts',(-4.18365665600839,22.4082642454448,
0.));
#244421=CARTESIAN_POINT('Ctrl Pts',(-4.18365665600839,22.4082642454448,
12.));
#244422=CARTESIAN_POINT('Ctrl Pts',(-4.18006356544879,22.3977390078074,
0.));
#244423=CARTESIAN_POINT('Ctrl Pts',(-4.18006356544879,22.3977390078074,
12.));
#244424=CARTESIAN_POINT('Ctrl Pts',(-4.17657052752834,22.3873919231339,
0.));
#244425=CARTESIAN_POINT('Ctrl Pts',(-4.17657052752834,22.3873919231339,
12.));
#244426=CARTESIAN_POINT('Ctrl Pts',(-4.17317742436162,22.3772263228624,
0.));
#244427=CARTESIAN_POINT('Ctrl Pts',(-4.17317742436162,22.3772263228624,
12.));
#244428=CARTESIAN_POINT('Ctrl Pts',(-4.1698841319947,22.3672456427605,0.));
#244429=CARTESIAN_POINT('Ctrl Pts',(-4.1698841319947,22.3672456427605,12.));
#244430=CARTESIAN_POINT('Ctrl Pts',(-4.16669052026602,22.3574534257397,
0.));
#244431=CARTESIAN_POINT('Ctrl Pts',(-4.16669052026602,22.3574534257397,
12.));
#244432=CARTESIAN_POINT('Ctrl Pts',(-4.1635964526318,22.3478533253886,0.));
#244433=CARTESIAN_POINT('Ctrl Pts',(-4.1635964526318,22.3478533253886,12.));
#244434=CARTESIAN_POINT('Ctrl Pts',(-4.16060178604154,22.3384491078599,
0.));
#244435=CARTESIAN_POINT('Ctrl Pts',(-4.16060178604154,22.3384491078599,
12.));
#244436=CARTESIAN_POINT('Ctrl Pts',(-4.15770637047882,22.3292446628957,
0.));
#244437=CARTESIAN_POINT('Ctrl Pts',(-4.15770637047882,22.3292446628957,
12.));
#244438=CARTESIAN_POINT('Ctrl Pts',(-4.15491004835278,22.3202440186979,
0.));
#244439=CARTESIAN_POINT('Ctrl Pts',(-4.15491004835278,22.3202440186979,
12.));
#244440=CARTESIAN_POINT('Ctrl Pts',(-4.15221265396992,22.3114513545186,
0.));
#244441=CARTESIAN_POINT('Ctrl Pts',(-4.15221265396992,22.3114513545186,
12.));
#244442=CARTESIAN_POINT('Ctrl Pts',(-4.14961401285526,22.3028710166935,
0.));
#244443=CARTESIAN_POINT('Ctrl Pts',(-4.14961401285526,22.3028710166935,
12.));
#244444=CARTESIAN_POINT('Ctrl Pts',(-4.14711394168559,22.2945075198468,
0.));
#244445=CARTESIAN_POINT('Ctrl Pts',(-4.14711394168559,22.2945075198468,
12.));
#244446=CARTESIAN_POINT('Ctrl Pts',(-4.14471224859295,22.2863655389166,
0.));
#244447=CARTESIAN_POINT('Ctrl Pts',(-4.14471224859295,22.2863655389166,
12.));
#244448=CARTESIAN_POINT('Ctrl Pts',(-4.14240873321982,22.2784499072026,
0.));
#244449=CARTESIAN_POINT('Ctrl Pts',(-4.14240873321982,22.2784499072026,
12.));
#244450=CARTESIAN_POINT('Ctrl Pts',(-4.14020318715988,22.2707656042456,
0.));
#244451=CARTESIAN_POINT('Ctrl Pts',(-4.14020318715988,22.2707656042456,
12.));
#244452=CARTESIAN_POINT('Ctrl Pts',(-4.13809539255419,22.263317791397,0.));
#244453=CARTESIAN_POINT('Ctrl Pts',(-4.13809539255419,22.263317791397,12.));
#244454=CARTESIAN_POINT('Ctrl Pts',(-4.13608511977226,22.2561118708422,
0.));
#244455=CARTESIAN_POINT('Ctrl Pts',(-4.13608511977226,22.2561118708422,
12.));
#244456=CARTESIAN_POINT('Ctrl Pts',(-4.13417212558808,22.2491535317789,
0.));
#244457=CARTESIAN_POINT('Ctrl Pts',(-4.13417212558808,22.2491535317789,
12.));
#244458=CARTESIAN_POINT('Ctrl Pts',(-4.1323561506016,22.2424488153523,0.));
#244459=CARTESIAN_POINT('Ctrl Pts',(-4.1323561506016,22.2424488153523,12.));
#244460=CARTESIAN_POINT('Ctrl Pts',(-4.13063692157499,22.2360040565534,
0.));
#244461=CARTESIAN_POINT('Ctrl Pts',(-4.13063692157499,22.2360040565534,
12.));
#244462=CARTESIAN_POINT('Ctrl Pts',(-4.12901415463379,22.2298258043947,
0.));
#244463=CARTESIAN_POINT('Ctrl Pts',(-4.12901415463379,22.2298258043947,
12.));
#244464=CARTESIAN_POINT('Ctrl Pts',(-4.12748755830099,22.2239207458781,
0.));
#244465=CARTESIAN_POINT('Ctrl Pts',(-4.12748755830099,22.2239207458781,
12.));
#244466=CARTESIAN_POINT('Ctrl Pts',(-4.126056836133,22.2182956401341,0.));
#244467=CARTESIAN_POINT('Ctrl Pts',(-4.126056836133,22.2182956401341,12.));
#244468=CARTESIAN_POINT('Ctrl Pts',(-4.12472167516602,22.2129576146671,
0.));
#244469=CARTESIAN_POINT('Ctrl Pts',(-4.12472167516602,22.2129576146671,
12.));
#244470=CARTESIAN_POINT('Ctrl Pts',(-4.12348173702025,22.2079143941719,
0.));
#244471=CARTESIAN_POINT('Ctrl Pts',(-4.12348173702025,22.2079143941719,
12.));
#244472=CARTESIAN_POINT('Ctrl Pts',(-4.12233664408237,22.2031746532106,
0.));
#244473=CARTESIAN_POINT('Ctrl Pts',(-4.12233664408237,22.2031746532106,
12.));
#244474=CARTESIAN_POINT('Ctrl Pts',(-4.12128598183533,22.1987479618246,
0.));
#244475=CARTESIAN_POINT('Ctrl Pts',(-4.12128598183533,22.1987479618246,
12.));
#244476=CARTESIAN_POINT('Ctrl Pts',(-4.12032932637738,22.1946440958098,
0.));
#244477=CARTESIAN_POINT('Ctrl Pts',(-4.12032932637738,22.1946440958098,
12.));
#244478=CARTESIAN_POINT('Ctrl Pts',(-4.11946626228623,22.1908725908525,
0.));
#244479=CARTESIAN_POINT('Ctrl Pts',(-4.11946626228623,22.1908725908525,
12.));
#244480=CARTESIAN_POINT('Ctrl Pts',(-4.11869641271752,22.1874419861496,
0.));
#244481=CARTESIAN_POINT('Ctrl Pts',(-4.11869641271752,22.1874419861496,
12.));
#244482=CARTESIAN_POINT('Ctrl Pts',(-4.11801938107464,22.1843613164855,
0.));
#244483=CARTESIAN_POINT('Ctrl Pts',(-4.11801938107464,22.1843613164855,
12.));
#244484=CARTESIAN_POINT('Ctrl Pts',(-4.11743469691765,22.1816414985788,
0.));
#244485=CARTESIAN_POINT('Ctrl Pts',(-4.11743469691765,22.1816414985788,
12.));
#244486=CARTESIAN_POINT('Ctrl Pts',(-4.11694173195041,22.179297473024,0.));
#244487=CARTESIAN_POINT('Ctrl Pts',(-4.11694173195041,22.179297473024,12.));
#244488=CARTESIAN_POINT('Ctrl Pts',(-4.11653973150558,22.177347426894,0.));
#244489=CARTESIAN_POINT('Ctrl Pts',(-4.11653973150558,22.177347426894,12.));
#244490=CARTESIAN_POINT('Ctrl Pts',(-4.11622797217066,22.1758088296598,
0.));
#244491=CARTESIAN_POINT('Ctrl Pts',(-4.11622797217066,22.1758088296598,
12.));
#244492=CARTESIAN_POINT('Ctrl Pts',(-4.11600589882767,22.1746949858773,
0.));
#244493=CARTESIAN_POINT('Ctrl Pts',(-4.11600589882767,22.1746949858773,
12.));
#244494=CARTESIAN_POINT('Ctrl Pts',(-4.11589976826061,22.174148802123,0.));
#244495=CARTESIAN_POINT('Ctrl Pts',(-4.11589976826061,22.174148802123,12.));
#244496=CARTESIAN_POINT('Ctrl Pts',(-4.1158603587821,22.1739341411684,0.));
#244497=CARTESIAN_POINT('Ctrl Pts',(-4.1158603587821,22.1739341411684,12.));
#244498=CARTESIAN_POINT('Ctrl Pts',(-4.11585194677412,22.1738776823239,
0.));
#244499=CARTESIAN_POINT('Ctrl Pts',(-4.11585194677412,22.1738776823239,
12.));
#244500=CARTESIAN_POINT('Ctrl Pts',(-4.11585220600461,22.1738711152697,
0.));
#244501=CARTESIAN_POINT('Ctrl Pts',(-4.11585220600461,22.1738711152697,
12.));
#244502=CARTESIAN_POINT('',(-6.08833931617698,25.2771067246846,0.));
#244503=CARTESIAN_POINT('Ctrl Pts',(-6.08833931617698,25.2771067246846,
0.));
#244504=CARTESIAN_POINT('Ctrl Pts',(-6.08441489609824,25.2729539149479,
0.));
#244505=CARTESIAN_POINT('Ctrl Pts',(-6.07657531787578,25.2646490489816,
0.));
#244506=CARTESIAN_POINT('Ctrl Pts',(-6.06484373634697,25.2521940105523,
0.));
#244507=CARTESIAN_POINT('Ctrl Pts',(-6.04925720151412,25.2355918138798,
0.));
#244508=CARTESIAN_POINT('Ctrl Pts',(-6.02986667390187,25.2148466201368,
0.));
#244509=CARTESIAN_POINT('Ctrl Pts',(-6.0105688180476,25.1941090269638,0.));
#244510=CARTESIAN_POINT('Ctrl Pts',(-5.99136367859838,25.1733791296154,
0.));
#244511=CARTESIAN_POINT('Ctrl Pts',(-5.97225131495636,25.1526570863065,
0.));
#244512=CARTESIAN_POINT('Ctrl Pts',(-5.95323180187348,25.1319431317273,
0.));
#244513=CARTESIAN_POINT('Ctrl Pts',(-5.93430523086776,25.1112375971182,
0.));
#244514=CARTESIAN_POINT('Ctrl Pts',(-5.91547170844382,25.0905409050863,
0.));
#244515=CARTESIAN_POINT('Ctrl Pts',(-5.89673135155459,25.0698535426593,
0.));
#244516=CARTESIAN_POINT('Ctrl Pts',(-5.87808428385329,25.0491760405965,
0.));
#244517=CARTESIAN_POINT('Ctrl Pts',(-5.8595306315681,25.0285089498922,0.));
#244518=CARTESIAN_POINT('Ctrl Pts',(-5.84107051963073,25.0078528200558,
0.));
#244519=CARTESIAN_POINT('Ctrl Pts',(-5.82270406744214,24.9872081752709,
0.));
#244520=CARTESIAN_POINT('Ctrl Pts',(-5.80443138549747,24.9665754954462,
0.));
#244521=CARTESIAN_POINT('Ctrl Pts',(-5.78625257775703,24.9459552293308,
0.));
#244522=CARTESIAN_POINT('Ctrl Pts',(-5.76816774342236,24.9253478043632,
0.));
#244523=CARTESIAN_POINT('Ctrl Pts',(-5.75017697890813,24.9047536376467,
0.));
#244524=CARTESIAN_POINT('Ctrl Pts',(-5.73228037976927,24.8841731467219,
0.));
#244525=CARTESIAN_POINT('Ctrl Pts',(-5.71447804252019,24.8636067597677,
0.));
#244526=CARTESIAN_POINT('Ctrl Pts',(-5.69677006679429,24.8430549277634,
0.));
#244527=CARTESIAN_POINT('Ctrl Pts',(-5.67915655496524,24.822518122386,0.));
#244528=CARTESIAN_POINT('Ctrl Pts',(-5.66163761114903,24.8019968304618,
0.));
#244529=CARTESIAN_POINT('Ctrl Pts',(-5.64421334042248,24.7814915496728,
0.));
#244530=CARTESIAN_POINT('Ctrl Pts',(-5.62688384790919,24.76100278357,0.));
#244531=CARTESIAN_POINT('Ctrl Pts',(-5.60964923798495,24.7405310372736,
0.));
#244532=CARTESIAN_POINT('Ctrl Pts',(-5.59250961323995,24.7200768119079,
0.));
#244533=CARTESIAN_POINT('Ctrl Pts',(-5.57546507427767,24.6996406035507,
0.));
#244534=CARTESIAN_POINT('Ctrl Pts',(-5.55851572025389,24.6792229061785,
0.));
#244535=CARTESIAN_POINT('Ctrl Pts',(-5.54166164919593,24.6588242134733,
0.));
#244536=CARTESIAN_POINT('Ctrl Pts',(-5.52490295840996,24.6384450211466,
0.));
#244537=CARTESIAN_POINT('Ctrl Pts',(-5.50823974481959,24.618085828918,0.));
#244538=CARTESIAN_POINT('Ctrl Pts',(-5.49167210537235,24.5977471429365,
0.));
#244539=CARTESIAN_POINT('Ctrl Pts',(-5.47520013724403,24.5774294770329,
0.));
#244540=CARTESIAN_POINT('Ctrl Pts',(-5.45882393762244,24.5571333514841,
0.));
#244541=CARTESIAN_POINT('Ctrl Pts',(-5.44254360356865,24.5368592922861,
0.));
#244542=CARTESIAN_POINT('Ctrl Pts',(-5.42635923183411,24.5166078302107,
0.));
#244543=CARTESIAN_POINT('Ctrl Pts',(-5.41027091869242,24.4963794999831,
0.));
#244544=CARTESIAN_POINT('Ctrl Pts',(-5.3942787597383,24.4761748393322,0.));
#244545=CARTESIAN_POINT('Ctrl Pts',(-5.37838284973706,24.4559943883159,
0.));
#244546=CARTESIAN_POINT('Ctrl Pts',(-5.36258328273639,24.4358386899152,
0.));
#244547=CARTESIAN_POINT('Ctrl Pts',(-5.34688015213546,24.4157082904615,
0.));
#244548=CARTESIAN_POINT('Ctrl Pts',(-5.33127355076037,24.3956037401293,
0.));
#244549=CARTESIAN_POINT('Ctrl Pts',(-5.31576357092524,24.3755255933917,
0.));
#244550=CARTESIAN_POINT('Ctrl Pts',(-5.30035030449059,24.3554744095075,
0.));
#244551=CARTESIAN_POINT('Ctrl Pts',(-5.28503384290644,24.3354507529415,
0.));
#244552=CARTESIAN_POINT('Ctrl Pts',(-5.26981427718796,24.3154551932222,
0.));
#244553=CARTESIAN_POINT('Ctrl Pts',(-5.25469169788856,24.2954883048448,
0.));
#244554=CARTESIAN_POINT('Ctrl Pts',(-5.23966619506289,24.2755506671526,
0.));
#244555=CARTESIAN_POINT('Ctrl Pts',(-5.22473785822441,24.2556428642294,
0.));
#244556=CARTESIAN_POINT('Ctrl Pts',(-5.20990677629173,24.2357654847765,
0.));
#244557=CARTESIAN_POINT('Ctrl Pts',(-5.19517303753643,24.215919122017,0.));
#244558=CARTESIAN_POINT('Ctrl Pts',(-5.18053672961392,24.1961043738754,
0.));
#244559=CARTESIAN_POINT('Ctrl Pts',(-5.16599793957979,24.1763218431343,
0.));
#244560=CARTESIAN_POINT('Ctrl Pts',(-5.15155675390075,24.156572137597,0.));
#244561=CARTESIAN_POINT('Ctrl Pts',(-5.13721325845745,24.1368558702443,
0.));
#244562=CARTESIAN_POINT('Ctrl Pts',(-5.12296753853859,24.117173659394,0.));
#244563=CARTESIAN_POINT('Ctrl Pts',(-5.10881967883132,24.0975261288446,
0.));
#244564=CARTESIAN_POINT('Ctrl Pts',(-5.09476976342625,24.0779139079266,
0.));
#244565=CARTESIAN_POINT('Ctrl Pts',(-5.08081787581276,24.0583376315638,
0.));
#244566=CARTESIAN_POINT('Ctrl Pts',(-5.06696409886641,24.0387979403268,
0.));
#244567=CARTESIAN_POINT('Ctrl Pts',(-5.05320851483065,24.0192954804896,
0.));
#244568=CARTESIAN_POINT('Ctrl Pts',(-5.03955120528521,23.9998309040746,
0.));
#244569=CARTESIAN_POINT('Ctrl Pts',(-5.02599225112454,23.9804048689227,
0.));
#244570=CARTESIAN_POINT('Ctrl Pts',(-5.01253173257453,23.9610180388271,
0.));
#244571=CARTESIAN_POINT('Ctrl Pts',(-4.99916972919307,23.9416710836529,
0.));
#244572=CARTESIAN_POINT('Ctrl Pts',(-4.98590631986533,23.9223646794592,
0.));
#244573=CARTESIAN_POINT('Ctrl Pts',(-4.97274158279227,23.9030995086163,
0.));
#244574=CARTESIAN_POINT('Ctrl Pts',(-4.95967559546561,23.8838762599218,
0.));
#244575=CARTESIAN_POINT('Ctrl Pts',(-4.9467084346586,23.8646956287168,0.));
#244576=CARTESIAN_POINT('Ctrl Pts',(-4.93384017643432,23.8455583170057,
0.));
#244577=CARTESIAN_POINT('Ctrl Pts',(-4.92107089613969,23.8264650335717,
0.));
#244578=CARTESIAN_POINT('Ctrl Pts',(-4.90840066839344,23.8074164940896,
0.));
#244579=CARTESIAN_POINT('Ctrl Pts',(-4.89582956706775,23.7884134212384,
0.));
#244580=CARTESIAN_POINT('Ctrl Pts',(-4.88335766525573,23.7694565448049,
0.));
#244581=CARTESIAN_POINT('Ctrl Pts',(-4.87098503527152,23.7505466018245,
0.));
#244582=CARTESIAN_POINT('Ctrl Pts',(-4.85871174865499,23.7316843367313,
0.));
#244583=CARTESIAN_POINT('Ctrl Pts',(-4.84653787616425,23.7128705015017,
0.));
#244584=CARTESIAN_POINT('Ctrl Pts',(-4.83446348776266,23.6941058557971,
0.));
#244585=CARTESIAN_POINT('Ctrl Pts',(-4.82248865259562,23.675391167102,0.));
#244586=CARTESIAN_POINT('Ctrl Pts',(-4.81061343896432,23.6567272108628,
0.));
#244587=CARTESIAN_POINT('Ctrl Pts',(-4.7988379143322,23.6381147706579,0.));
#244588=CARTESIAN_POINT('Ctrl Pts',(-4.78716214532098,23.6195546383624,
0.));
#244589=CARTESIAN_POINT('Ctrl Pts',(-4.77558619769872,23.6010476143099,
0.));
#244590=CARTESIAN_POINT('Ctrl Pts',(-4.76411013636251,23.5825945074535,
0.));
#244591=CARTESIAN_POINT('Ctrl Pts',(-4.75273402530617,23.5641961355168,
0.));
#244592=CARTESIAN_POINT('Ctrl Pts',(-4.74145792760698,23.545853325171,0.));
#244593=CARTESIAN_POINT('Ctrl Pts',(-4.7302819054303,23.5275669122372,0.));
#244594=CARTESIAN_POINT('Ctrl Pts',(-4.71920602001902,23.509337741878,0.));
#244595=CARTESIAN_POINT('Ctrl Pts',(-4.70823033167819,23.491166668789,0.));
#244596=CARTESIAN_POINT('Ctrl Pts',(-4.69735489975024,23.4730545573853,
0.));
#244597=CARTESIAN_POINT('Ctrl Pts',(-4.68657978258303,23.455002281986,0.));
#244598=CARTESIAN_POINT('Ctrl Pts',(-4.67590503753058,23.4370107270451,
0.));
#244599=CARTESIAN_POINT('Ctrl Pts',(-4.6653307209467,23.4190807873803,0.));
#244600=CARTESIAN_POINT('Ctrl Pts',(-4.65485688816924,23.4012133683959,
0.));
#244601=CARTESIAN_POINT('Ctrl Pts',(-4.6444835934993,23.3834093863068,0.));
#244602=CARTESIAN_POINT('Ctrl Pts',(-4.63421089016541,23.3656697683489,
0.));
#244603=CARTESIAN_POINT('Ctrl Pts',(-4.62403883030805,23.3479954530272,
0.));
#244604=CARTESIAN_POINT('Ctrl Pts',(-4.6139674649783,23.3303873903938,0.));
#244605=CARTESIAN_POINT('Ctrl Pts',(-4.60399684412163,23.3128465423115,
0.));
#244606=CARTESIAN_POINT('Ctrl Pts',(-4.5941270165575,23.2953738827191,0.));
#244607=CARTESIAN_POINT('Ctrl Pts',(-4.5843580299469,23.2779703978876,0.));
#244608=CARTESIAN_POINT('Ctrl Pts',(-4.57468993076097,23.2606370866866,
0.));
#244609=CARTESIAN_POINT('Ctrl Pts',(-4.56512276427839,23.2433749609131,
0.));
#244610=CARTESIAN_POINT('Ctrl Pts',(-4.55565657456975,23.2261850456064,
0.));
#244611=CARTESIAN_POINT('Ctrl Pts',(-4.54629140447544,23.2090683793629,
0.));
#244612=CARTESIAN_POINT('Ctrl Pts',(-4.53702729557566,23.1920260146465,
0.));
#244613=CARTESIAN_POINT('Ctrl Pts',(-4.52786428815015,23.1750590180908,
0.));
#244614=CARTESIAN_POINT('Ctrl Pts',(-4.51880242116748,23.1581684708761,
0.));
#244615=CARTESIAN_POINT('Ctrl Pts',(-4.5098417322706,23.1413554691123,0.));
#244616=CARTESIAN_POINT('Ctrl Pts',(-4.50098225775171,23.1246211242115,
0.));
#244617=CARTESIAN_POINT('Ctrl Pts',(-4.49222403252216,23.1079665632636,
0.));
#244618=CARTESIAN_POINT('Ctrl Pts',(-4.48356709006788,23.0913929293922,
0.));
#244619=CARTESIAN_POINT('Ctrl Pts',(-4.47501146242856,23.0749013821881,
0.));
#244620=CARTESIAN_POINT('Ctrl Pts',(-4.4665571801823,23.0584930981732,0.));
#244621=CARTESIAN_POINT('Ctrl Pts',(-4.45820427241683,23.0421692712467,
0.));
#244622=CARTESIAN_POINT('Ctrl Pts',(-4.44995276669686,23.0259311131392,
0.));
#244623=CARTESIAN_POINT('Ctrl Pts',(-4.44180268901643,23.0097798538395,
0.));
#244624=CARTESIAN_POINT('Ctrl Pts',(-4.43375406376879,22.9937167421006,
0.));
#244625=CARTESIAN_POINT('Ctrl Pts',(-4.42580691372751,22.977743046002,0.));
#244626=CARTESIAN_POINT('Ctrl Pts',(-4.41796126001302,22.9618600534866,
0.));
#244627=CARTESIAN_POINT('Ctrl Pts',(-4.41021712205553,22.9460690729093,
0.));
#244628=CARTESIAN_POINT('Ctrl Pts',(-4.40257451754323,22.930371433555,0.));
#244629=CARTESIAN_POINT('Ctrl Pts',(-4.39503346238473,22.9147684862426,
0.));
#244630=CARTESIAN_POINT('Ctrl Pts',(-4.38759397068406,22.8992616040108,
0.));
#244631=CARTESIAN_POINT('Ctrl Pts',(-4.38025605470093,22.8838521827701,
0.));
#244632=CARTESIAN_POINT('Ctrl Pts',(-4.37301972480746,22.8685416419725,
0.));
#244633=CARTESIAN_POINT('Ctrl Pts',(-4.36588498942997,22.8533314252422,
0.));
#244634=CARTESIAN_POINT('Ctrl Pts',(-4.35885185500546,22.8382230011184,
0.));
#244635=CARTESIAN_POINT('Ctrl Pts',(-4.35192032594791,22.8232178638876,
0.));
#244636=CARTESIAN_POINT('Ctrl Pts',(-4.34509040460062,22.8083175343791,
0.));
#244637=CARTESIAN_POINT('Ctrl Pts',(-4.33836209118446,22.7935235607806,
0.));
#244638=CARTESIAN_POINT('Ctrl Pts',(-4.3317353837319,22.7788375194076,0.));
#244639=CARTESIAN_POINT('Ctrl Pts',(-4.32521027803754,22.7642610156475,
0.));
#244640=CARTESIAN_POINT('Ctrl Pts',(-4.31878676761235,22.7497956849848,
0.));
#244641=CARTESIAN_POINT('Ctrl Pts',(-4.31246484362549,22.7354431939926,
0.));
#244642=CARTESIAN_POINT('Ctrl Pts',(-4.30624449484069,22.7212052413386,
0.));
#244643=CARTESIAN_POINT('Ctrl Pts',(-4.3001257075406,22.7070835587564,0.));
#244644=CARTESIAN_POINT('Ctrl Pts',(-4.29410846547056,22.6930799122548,
0.));
#244645=CARTESIAN_POINT('Ctrl Pts',(-4.28819274977763,22.6791961033538,
0.));
#244646=CARTESIAN_POINT('Ctrl Pts',(-4.28237853894059,22.6654339703109,
0.));
#244647=CARTESIAN_POINT('Ctrl Pts',(-4.2766658086912,22.6517953893303,0.));
#244648=CARTESIAN_POINT('Ctrl Pts',(-4.27105453193004,22.6382822758172,
0.));
#244649=CARTESIAN_POINT('Ctrl Pts',(-4.26554467865576,22.6248965859977,
0.));
#244650=CARTESIAN_POINT('Ctrl Pts',(-4.26013621588305,22.6116403184821,
0.));
#244651=CARTESIAN_POINT('Ctrl Pts',(-4.25482910755481,22.5985155158636,
0.));
#244652=CARTESIAN_POINT('Ctrl Pts',(-4.24962331444177,22.5855242662477,
0.));
#244653=CARTESIAN_POINT('Ctrl Pts',(-4.24451879404851,22.572668704992,0.));
#244654=CARTESIAN_POINT('Ctrl Pts',(-4.23951550052523,22.5599510166429,
0.));
#244655=CARTESIAN_POINT('Ctrl Pts',(-4.23461338456712,22.5473734368086,
0.));
#244656=CARTESIAN_POINT('Ctrl Pts',(-4.22981239330733,22.5349382540588,
0.));
#244657=CARTESIAN_POINT('Ctrl Pts',(-4.22511247020041,22.5226478117886,
0.));
#244658=CARTESIAN_POINT('Ctrl Pts',(-4.22051355490196,22.5105045108881,
0.));
#244659=CARTESIAN_POINT('Ctrl Pts',(-4.21601558313906,22.4985108124228,
0.));
#244660=CARTESIAN_POINT('Ctrl Pts',(-4.21161848657428,22.4866692403147,
0.));
#244661=CARTESIAN_POINT('Ctrl Pts',(-4.20732219265649,22.4749823839917,
0.));
#244662=CARTESIAN_POINT('Ctrl Pts',(-4.20312662448174,22.4634529011437,
0.));
#244663=CARTESIAN_POINT('Ctrl Pts',(-4.19903170066358,22.4520835205422,
0.));
#244664=CARTESIAN_POINT('Ctrl Pts',(-4.1950373351886,22.4408770448917,0.));
#244665=CARTESIAN_POINT('Ctrl Pts',(-4.19114343726932,22.4298363535416,
0.));
#244666=CARTESIAN_POINT('Ctrl Pts',(-4.18734991117707,22.4189644056109,
0.));
#244667=CARTESIAN_POINT('Ctrl Pts',(-4.18365665600839,22.4082642454448,
0.));
#244668=CARTESIAN_POINT('Ctrl Pts',(-4.18006356544879,22.3977390078074,
0.));
#244669=CARTESIAN_POINT('Ctrl Pts',(-4.17657052752834,22.3873919231339,
0.));
#244670=CARTESIAN_POINT('Ctrl Pts',(-4.17317742436162,22.3772263228624,
0.));
#244671=CARTESIAN_POINT('Ctrl Pts',(-4.1698841319947,22.3672456427605,0.));
#244672=CARTESIAN_POINT('Ctrl Pts',(-4.16669052026602,22.3574534257397,
0.));
#244673=CARTESIAN_POINT('Ctrl Pts',(-4.1635964526318,22.3478533253886,0.));
#244674=CARTESIAN_POINT('Ctrl Pts',(-4.16060178604154,22.3384491078599,
0.));
#244675=CARTESIAN_POINT('Ctrl Pts',(-4.15770637047882,22.3292446628957,
0.));
#244676=CARTESIAN_POINT('Ctrl Pts',(-4.15491004835278,22.3202440186979,
0.));
#244677=CARTESIAN_POINT('Ctrl Pts',(-4.15221265396992,22.3114513545186,
0.));
#244678=CARTESIAN_POINT('Ctrl Pts',(-4.14961401285526,22.3028710166935,
0.));
#244679=CARTESIAN_POINT('Ctrl Pts',(-4.14711394168559,22.2945075198468,
0.));
#244680=CARTESIAN_POINT('Ctrl Pts',(-4.14471224859295,22.2863655389166,
0.));
#244681=CARTESIAN_POINT('Ctrl Pts',(-4.14240873321982,22.2784499072026,
0.));
#244682=CARTESIAN_POINT('Ctrl Pts',(-4.14020318715988,22.2707656042456,
0.));
#244683=CARTESIAN_POINT('Ctrl Pts',(-4.13809539255419,22.263317791397,0.));
#244684=CARTESIAN_POINT('Ctrl Pts',(-4.13608511977226,22.2561118708422,
0.));
#244685=CARTESIAN_POINT('Ctrl Pts',(-4.13417212558808,22.2491535317789,
0.));
#244686=CARTESIAN_POINT('Ctrl Pts',(-4.1323561506016,22.2424488153523,0.));
#244687=CARTESIAN_POINT('Ctrl Pts',(-4.13063692157499,22.2360040565534,
0.));
#244688=CARTESIAN_POINT('Ctrl Pts',(-4.12901415463379,22.2298258043947,
0.));
#244689=CARTESIAN_POINT('Ctrl Pts',(-4.12748755830099,22.2239207458781,
0.));
#244690=CARTESIAN_POINT('Ctrl Pts',(-4.126056836133,22.2182956401341,0.));
#244691=CARTESIAN_POINT('Ctrl Pts',(-4.12472167516602,22.2129576146671,
0.));
#244692=CARTESIAN_POINT('Ctrl Pts',(-4.12348173702025,22.2079143941719,
0.));
#244693=CARTESIAN_POINT('Ctrl Pts',(-4.12233664408237,22.2031746532106,
0.));
#244694=CARTESIAN_POINT('Ctrl Pts',(-4.12128598183533,22.1987479618246,
0.));
#244695=CARTESIAN_POINT('Ctrl Pts',(-4.12032932637738,22.1946440958098,
0.));
#244696=CARTESIAN_POINT('Ctrl Pts',(-4.11946626228623,22.1908725908525,
0.));
#244697=CARTESIAN_POINT('Ctrl Pts',(-4.11869641271752,22.1874419861496,
0.));
#244698=CARTESIAN_POINT('Ctrl Pts',(-4.11801938107464,22.1843613164855,
0.));
#244699=CARTESIAN_POINT('Ctrl Pts',(-4.11743469691765,22.1816414985788,
0.));
#244700=CARTESIAN_POINT('Ctrl Pts',(-4.11694173195041,22.179297473024,0.));
#244701=CARTESIAN_POINT('Ctrl Pts',(-4.11653973150558,22.177347426894,0.));
#244702=CARTESIAN_POINT('Ctrl Pts',(-4.11622797217066,22.1758088296598,
0.));
#244703=CARTESIAN_POINT('Ctrl Pts',(-4.11600589882767,22.1746949858773,
0.));
#244704=CARTESIAN_POINT('Ctrl Pts',(-4.11589976826061,22.174148802123,0.));
#244705=CARTESIAN_POINT('Ctrl Pts',(-4.1158603587821,22.1739341411684,0.));
#244706=CARTESIAN_POINT('Ctrl Pts',(-4.11585194677412,22.1738776823239,
0.));
#244707=CARTESIAN_POINT('Ctrl Pts',(-4.11585220600461,22.1738711152697,
0.));
#244708=CARTESIAN_POINT('',(-6.08833931617698,25.2771067246846,12.));
#244709=CARTESIAN_POINT('',(-6.08833931617698,25.2771067246846,0.));
#244710=CARTESIAN_POINT('Ctrl Pts',(-4.11585220600461,22.1738711152697,
12.));
#244711=CARTESIAN_POINT('Ctrl Pts',(-4.11585194677412,22.1738776823239,
12.));
#244712=CARTESIAN_POINT('Ctrl Pts',(-4.1158603587821,22.1739341411684,12.));
#244713=CARTESIAN_POINT('Ctrl Pts',(-4.11589976826061,22.174148802123,12.));
#244714=CARTESIAN_POINT('Ctrl Pts',(-4.11600589882767,22.1746949858773,
12.));
#244715=CARTESIAN_POINT('Ctrl Pts',(-4.11622797217066,22.1758088296598,
12.));
#244716=CARTESIAN_POINT('Ctrl Pts',(-4.11653973150558,22.177347426894,12.));
#244717=CARTESIAN_POINT('Ctrl Pts',(-4.11694173195041,22.179297473024,12.));
#244718=CARTESIAN_POINT('Ctrl Pts',(-4.11743469691765,22.1816414985788,
12.));
#244719=CARTESIAN_POINT('Ctrl Pts',(-4.11801938107464,22.1843613164855,
12.));
#244720=CARTESIAN_POINT('Ctrl Pts',(-4.11869641271752,22.1874419861496,
12.));
#244721=CARTESIAN_POINT('Ctrl Pts',(-4.11946626228623,22.1908725908525,
12.));
#244722=CARTESIAN_POINT('Ctrl Pts',(-4.12032932637738,22.1946440958098,
12.));
#244723=CARTESIAN_POINT('Ctrl Pts',(-4.12128598183533,22.1987479618246,
12.));
#244724=CARTESIAN_POINT('Ctrl Pts',(-4.12233664408237,22.2031746532106,
12.));
#244725=CARTESIAN_POINT('Ctrl Pts',(-4.12348173702025,22.2079143941719,
12.));
#244726=CARTESIAN_POINT('Ctrl Pts',(-4.12472167516602,22.2129576146671,
12.));
#244727=CARTESIAN_POINT('Ctrl Pts',(-4.126056836133,22.2182956401341,12.));
#244728=CARTESIAN_POINT('Ctrl Pts',(-4.12748755830099,22.2239207458781,
12.));
#244729=CARTESIAN_POINT('Ctrl Pts',(-4.12901415463379,22.2298258043947,
12.));
#244730=CARTESIAN_POINT('Ctrl Pts',(-4.13063692157499,22.2360040565534,
12.));
#244731=CARTESIAN_POINT('Ctrl Pts',(-4.1323561506016,22.2424488153523,12.));
#244732=CARTESIAN_POINT('Ctrl Pts',(-4.13417212558808,22.2491535317789,
12.));
#244733=CARTESIAN_POINT('Ctrl Pts',(-4.13608511977226,22.2561118708422,
12.));
#244734=CARTESIAN_POINT('Ctrl Pts',(-4.13809539255419,22.263317791397,12.));
#244735=CARTESIAN_POINT('Ctrl Pts',(-4.14020318715988,22.2707656042456,
12.));
#244736=CARTESIAN_POINT('Ctrl Pts',(-4.14240873321982,22.2784499072026,
12.));
#244737=CARTESIAN_POINT('Ctrl Pts',(-4.14471224859295,22.2863655389166,
12.));
#244738=CARTESIAN_POINT('Ctrl Pts',(-4.14711394168559,22.2945075198468,
12.));
#244739=CARTESIAN_POINT('Ctrl Pts',(-4.14961401285526,22.3028710166935,
12.));
#244740=CARTESIAN_POINT('Ctrl Pts',(-4.15221265396992,22.3114513545186,
12.));
#244741=CARTESIAN_POINT('Ctrl Pts',(-4.15491004835278,22.3202440186979,
12.));
#244742=CARTESIAN_POINT('Ctrl Pts',(-4.15770637047882,22.3292446628957,
12.));
#244743=CARTESIAN_POINT('Ctrl Pts',(-4.16060178604154,22.3384491078599,
12.));
#244744=CARTESIAN_POINT('Ctrl Pts',(-4.1635964526318,22.3478533253886,12.));
#244745=CARTESIAN_POINT('Ctrl Pts',(-4.16669052026602,22.3574534257397,
12.));
#244746=CARTESIAN_POINT('Ctrl Pts',(-4.1698841319947,22.3672456427605,12.));
#244747=CARTESIAN_POINT('Ctrl Pts',(-4.17317742436162,22.3772263228624,
12.));
#244748=CARTESIAN_POINT('Ctrl Pts',(-4.17657052752834,22.3873919231339,
12.));
#244749=CARTESIAN_POINT('Ctrl Pts',(-4.18006356544879,22.3977390078074,
12.));
#244750=CARTESIAN_POINT('Ctrl Pts',(-4.18365665600839,22.4082642454448,
12.));
#244751=CARTESIAN_POINT('Ctrl Pts',(-4.18734991117707,22.4189644056109,
12.));
#244752=CARTESIAN_POINT('Ctrl Pts',(-4.19114343726932,22.4298363535416,
12.));
#244753=CARTESIAN_POINT('Ctrl Pts',(-4.1950373351886,22.4408770448917,12.));
#244754=CARTESIAN_POINT('Ctrl Pts',(-4.19903170066358,22.4520835205422,
12.));
#244755=CARTESIAN_POINT('Ctrl Pts',(-4.20312662448174,22.4634529011437,
12.));
#244756=CARTESIAN_POINT('Ctrl Pts',(-4.20732219265649,22.4749823839917,
12.));
#244757=CARTESIAN_POINT('Ctrl Pts',(-4.21161848657428,22.4866692403147,
12.));
#244758=CARTESIAN_POINT('Ctrl Pts',(-4.21601558313906,22.4985108124228,
12.));
#244759=CARTESIAN_POINT('Ctrl Pts',(-4.22051355490196,22.5105045108881,
12.));
#244760=CARTESIAN_POINT('Ctrl Pts',(-4.22511247020041,22.5226478117886,
12.));
#244761=CARTESIAN_POINT('Ctrl Pts',(-4.22981239330733,22.5349382540588,
12.));
#244762=CARTESIAN_POINT('Ctrl Pts',(-4.23461338456712,22.5473734368086,
12.));
#244763=CARTESIAN_POINT('Ctrl Pts',(-4.23951550052523,22.5599510166429,
12.));
#244764=CARTESIAN_POINT('Ctrl Pts',(-4.24451879404851,22.572668704992,12.));
#244765=CARTESIAN_POINT('Ctrl Pts',(-4.24962331444177,22.5855242662477,
12.));
#244766=CARTESIAN_POINT('Ctrl Pts',(-4.25482910755481,22.5985155158636,
12.));
#244767=CARTESIAN_POINT('Ctrl Pts',(-4.26013621588305,22.6116403184821,
12.));
#244768=CARTESIAN_POINT('Ctrl Pts',(-4.26554467865576,22.6248965859977,
12.));
#244769=CARTESIAN_POINT('Ctrl Pts',(-4.27105453193004,22.6382822758172,
12.));
#244770=CARTESIAN_POINT('Ctrl Pts',(-4.2766658086912,22.6517953893303,12.));
#244771=CARTESIAN_POINT('Ctrl Pts',(-4.28237853894059,22.6654339703109,
12.));
#244772=CARTESIAN_POINT('Ctrl Pts',(-4.28819274977763,22.6791961033538,
12.));
#244773=CARTESIAN_POINT('Ctrl Pts',(-4.29410846547056,22.6930799122548,
12.));
#244774=CARTESIAN_POINT('Ctrl Pts',(-4.3001257075406,22.7070835587564,12.));
#244775=CARTESIAN_POINT('Ctrl Pts',(-4.30624449484069,22.7212052413386,
12.));
#244776=CARTESIAN_POINT('Ctrl Pts',(-4.31246484362549,22.7354431939926,
12.));
#244777=CARTESIAN_POINT('Ctrl Pts',(-4.31878676761235,22.7497956849848,
12.));
#244778=CARTESIAN_POINT('Ctrl Pts',(-4.32521027803754,22.7642610156475,
12.));
#244779=CARTESIAN_POINT('Ctrl Pts',(-4.3317353837319,22.7788375194076,12.));
#244780=CARTESIAN_POINT('Ctrl Pts',(-4.33836209118446,22.7935235607806,
12.));
#244781=CARTESIAN_POINT('Ctrl Pts',(-4.34509040460062,22.8083175343791,
12.));
#244782=CARTESIAN_POINT('Ctrl Pts',(-4.35192032594791,22.8232178638876,
12.));
#244783=CARTESIAN_POINT('Ctrl Pts',(-4.35885185500546,22.8382230011184,
12.));
#244784=CARTESIAN_POINT('Ctrl Pts',(-4.36588498942997,22.8533314252422,
12.));
#244785=CARTESIAN_POINT('Ctrl Pts',(-4.37301972480746,22.8685416419725,
12.));
#244786=CARTESIAN_POINT('Ctrl Pts',(-4.38025605470093,22.8838521827701,
12.));
#244787=CARTESIAN_POINT('Ctrl Pts',(-4.38759397068406,22.8992616040108,
12.));
#244788=CARTESIAN_POINT('Ctrl Pts',(-4.39503346238473,22.9147684862426,
12.));
#244789=CARTESIAN_POINT('Ctrl Pts',(-4.40257451754323,22.930371433555,12.));
#244790=CARTESIAN_POINT('Ctrl Pts',(-4.41021712205553,22.9460690729093,
12.));
#244791=CARTESIAN_POINT('Ctrl Pts',(-4.41796126001302,22.9618600534866,
12.));
#244792=CARTESIAN_POINT('Ctrl Pts',(-4.42580691372751,22.977743046002,12.));
#244793=CARTESIAN_POINT('Ctrl Pts',(-4.43375406376879,22.9937167421006,
12.));
#244794=CARTESIAN_POINT('Ctrl Pts',(-4.44180268901643,23.0097798538395,
12.));
#244795=CARTESIAN_POINT('Ctrl Pts',(-4.44995276669686,23.0259311131392,
12.));
#244796=CARTESIAN_POINT('Ctrl Pts',(-4.45820427241683,23.0421692712467,
12.));
#244797=CARTESIAN_POINT('Ctrl Pts',(-4.4665571801823,23.0584930981732,12.));
#244798=CARTESIAN_POINT('Ctrl Pts',(-4.47501146242856,23.0749013821881,
12.));
#244799=CARTESIAN_POINT('Ctrl Pts',(-4.48356709006788,23.0913929293922,
12.));
#244800=CARTESIAN_POINT('Ctrl Pts',(-4.49222403252216,23.1079665632636,
12.));
#244801=CARTESIAN_POINT('Ctrl Pts',(-4.50098225775171,23.1246211242115,
12.));
#244802=CARTESIAN_POINT('Ctrl Pts',(-4.5098417322706,23.1413554691123,12.));
#244803=CARTESIAN_POINT('Ctrl Pts',(-4.51880242116748,23.1581684708761,
12.));
#244804=CARTESIAN_POINT('Ctrl Pts',(-4.52786428815015,23.1750590180908,
12.));
#244805=CARTESIAN_POINT('Ctrl Pts',(-4.53702729557566,23.1920260146465,
12.));
#244806=CARTESIAN_POINT('Ctrl Pts',(-4.54629140447544,23.2090683793629,
12.));
#244807=CARTESIAN_POINT('Ctrl Pts',(-4.55565657456975,23.2261850456064,
12.));
#244808=CARTESIAN_POINT('Ctrl Pts',(-4.56512276427839,23.2433749609131,
12.));
#244809=CARTESIAN_POINT('Ctrl Pts',(-4.57468993076097,23.2606370866866,
12.));
#244810=CARTESIAN_POINT('Ctrl Pts',(-4.5843580299469,23.2779703978876,12.));
#244811=CARTESIAN_POINT('Ctrl Pts',(-4.5941270165575,23.2953738827191,12.));
#244812=CARTESIAN_POINT('Ctrl Pts',(-4.60399684412163,23.3128465423115,
12.));
#244813=CARTESIAN_POINT('Ctrl Pts',(-4.6139674649783,23.3303873903938,12.));
#244814=CARTESIAN_POINT('Ctrl Pts',(-4.62403883030805,23.3479954530272,
12.));
#244815=CARTESIAN_POINT('Ctrl Pts',(-4.63421089016541,23.3656697683489,
12.));
#244816=CARTESIAN_POINT('Ctrl Pts',(-4.6444835934993,23.3834093863068,12.));
#244817=CARTESIAN_POINT('Ctrl Pts',(-4.65485688816924,23.4012133683959,
12.));
#244818=CARTESIAN_POINT('Ctrl Pts',(-4.6653307209467,23.4190807873803,12.));
#244819=CARTESIAN_POINT('Ctrl Pts',(-4.67590503753058,23.4370107270451,
12.));
#244820=CARTESIAN_POINT('Ctrl Pts',(-4.68657978258303,23.455002281986,12.));
#244821=CARTESIAN_POINT('Ctrl Pts',(-4.69735489975024,23.4730545573853,
12.));
#244822=CARTESIAN_POINT('Ctrl Pts',(-4.70823033167819,23.491166668789,12.));
#244823=CARTESIAN_POINT('Ctrl Pts',(-4.71920602001902,23.509337741878,12.));
#244824=CARTESIAN_POINT('Ctrl Pts',(-4.7302819054303,23.5275669122372,12.));
#244825=CARTESIAN_POINT('Ctrl Pts',(-4.74145792760698,23.545853325171,12.));
#244826=CARTESIAN_POINT('Ctrl Pts',(-4.75273402530617,23.5641961355168,
12.));
#244827=CARTESIAN_POINT('Ctrl Pts',(-4.76411013636251,23.5825945074535,
12.));
#244828=CARTESIAN_POINT('Ctrl Pts',(-4.77558619769872,23.6010476143099,
12.));
#244829=CARTESIAN_POINT('Ctrl Pts',(-4.78716214532098,23.6195546383624,
12.));
#244830=CARTESIAN_POINT('Ctrl Pts',(-4.7988379143322,23.6381147706579,12.));
#244831=CARTESIAN_POINT('Ctrl Pts',(-4.81061343896432,23.6567272108628,
12.));
#244832=CARTESIAN_POINT('Ctrl Pts',(-4.82248865259562,23.675391167102,12.));
#244833=CARTESIAN_POINT('Ctrl Pts',(-4.83446348776266,23.6941058557971,
12.));
#244834=CARTESIAN_POINT('Ctrl Pts',(-4.84653787616425,23.7128705015017,
12.));
#244835=CARTESIAN_POINT('Ctrl Pts',(-4.85871174865499,23.7316843367313,
12.));
#244836=CARTESIAN_POINT('Ctrl Pts',(-4.87098503527152,23.7505466018245,
12.));
#244837=CARTESIAN_POINT('Ctrl Pts',(-4.88335766525573,23.7694565448049,
12.));
#244838=CARTESIAN_POINT('Ctrl Pts',(-4.89582956706775,23.7884134212384,
12.));
#244839=CARTESIAN_POINT('Ctrl Pts',(-4.90840066839344,23.8074164940896,
12.));
#244840=CARTESIAN_POINT('Ctrl Pts',(-4.92107089613969,23.8264650335717,
12.));
#244841=CARTESIAN_POINT('Ctrl Pts',(-4.93384017643432,23.8455583170057,
12.));
#244842=CARTESIAN_POINT('Ctrl Pts',(-4.9467084346586,23.8646956287168,12.));
#244843=CARTESIAN_POINT('Ctrl Pts',(-4.95967559546561,23.8838762599218,
12.));
#244844=CARTESIAN_POINT('Ctrl Pts',(-4.97274158279227,23.9030995086163,
12.));
#244845=CARTESIAN_POINT('Ctrl Pts',(-4.98590631986533,23.9223646794592,
12.));
#244846=CARTESIAN_POINT('Ctrl Pts',(-4.99916972919307,23.9416710836529,
12.));
#244847=CARTESIAN_POINT('Ctrl Pts',(-5.01253173257453,23.9610180388271,
12.));
#244848=CARTESIAN_POINT('Ctrl Pts',(-5.02599225112454,23.9804048689227,
12.));
#244849=CARTESIAN_POINT('Ctrl Pts',(-5.03955120528521,23.9998309040746,
12.));
#244850=CARTESIAN_POINT('Ctrl Pts',(-5.05320851483065,24.0192954804896,
12.));
#244851=CARTESIAN_POINT('Ctrl Pts',(-5.06696409886641,24.0387979403268,
12.));
#244852=CARTESIAN_POINT('Ctrl Pts',(-5.08081787581276,24.0583376315638,
12.));
#244853=CARTESIAN_POINT('Ctrl Pts',(-5.09476976342625,24.0779139079266,
12.));
#244854=CARTESIAN_POINT('Ctrl Pts',(-5.10881967883132,24.0975261288446,
12.));
#244855=CARTESIAN_POINT('Ctrl Pts',(-5.12296753853859,24.117173659394,12.));
#244856=CARTESIAN_POINT('Ctrl Pts',(-5.13721325845745,24.1368558702443,
12.));
#244857=CARTESIAN_POINT('Ctrl Pts',(-5.15155675390075,24.156572137597,12.));
#244858=CARTESIAN_POINT('Ctrl Pts',(-5.16599793957979,24.1763218431343,
12.));
#244859=CARTESIAN_POINT('Ctrl Pts',(-5.18053672961392,24.1961043738754,
12.));
#244860=CARTESIAN_POINT('Ctrl Pts',(-5.19517303753643,24.215919122017,12.));
#244861=CARTESIAN_POINT('Ctrl Pts',(-5.20990677629173,24.2357654847765,
12.));
#244862=CARTESIAN_POINT('Ctrl Pts',(-5.22473785822441,24.2556428642294,
12.));
#244863=CARTESIAN_POINT('Ctrl Pts',(-5.23966619506289,24.2755506671526,
12.));
#244864=CARTESIAN_POINT('Ctrl Pts',(-5.25469169788856,24.2954883048448,
12.));
#244865=CARTESIAN_POINT('Ctrl Pts',(-5.26981427718796,24.3154551932222,
12.));
#244866=CARTESIAN_POINT('Ctrl Pts',(-5.28503384290644,24.3354507529415,
12.));
#244867=CARTESIAN_POINT('Ctrl Pts',(-5.30035030449059,24.3554744095075,
12.));
#244868=CARTESIAN_POINT('Ctrl Pts',(-5.31576357092524,24.3755255933917,
12.));
#244869=CARTESIAN_POINT('Ctrl Pts',(-5.33127355076037,24.3956037401293,
12.));
#244870=CARTESIAN_POINT('Ctrl Pts',(-5.34688015213546,24.4157082904615,
12.));
#244871=CARTESIAN_POINT('Ctrl Pts',(-5.36258328273639,24.4358386899152,
12.));
#244872=CARTESIAN_POINT('Ctrl Pts',(-5.37838284973706,24.4559943883159,
12.));
#244873=CARTESIAN_POINT('Ctrl Pts',(-5.3942787597383,24.4761748393322,12.));
#244874=CARTESIAN_POINT('Ctrl Pts',(-5.41027091869242,24.4963794999831,
12.));
#244875=CARTESIAN_POINT('Ctrl Pts',(-5.42635923183411,24.5166078302107,
12.));
#244876=CARTESIAN_POINT('Ctrl Pts',(-5.44254360356865,24.5368592922861,
12.));
#244877=CARTESIAN_POINT('Ctrl Pts',(-5.45882393762244,24.5571333514841,
12.));
#244878=CARTESIAN_POINT('Ctrl Pts',(-5.47520013724403,24.5774294770329,
12.));
#244879=CARTESIAN_POINT('Ctrl Pts',(-5.49167210537235,24.5977471429365,
12.));
#244880=CARTESIAN_POINT('Ctrl Pts',(-5.50823974481959,24.618085828918,12.));
#244881=CARTESIAN_POINT('Ctrl Pts',(-5.52490295840996,24.6384450211466,
12.));
#244882=CARTESIAN_POINT('Ctrl Pts',(-5.54166164919593,24.6588242134733,
12.));
#244883=CARTESIAN_POINT('Ctrl Pts',(-5.55851572025389,24.6792229061785,
12.));
#244884=CARTESIAN_POINT('Ctrl Pts',(-5.57546507427767,24.6996406035507,
12.));
#244885=CARTESIAN_POINT('Ctrl Pts',(-5.59250961323995,24.7200768119079,
12.));
#244886=CARTESIAN_POINT('Ctrl Pts',(-5.60964923798495,24.7405310372736,
12.));
#244887=CARTESIAN_POINT('Ctrl Pts',(-5.62688384790919,24.76100278357,12.));
#244888=CARTESIAN_POINT('Ctrl Pts',(-5.64421334042248,24.7814915496728,
12.));
#244889=CARTESIAN_POINT('Ctrl Pts',(-5.66163761114903,24.8019968304618,
12.));
#244890=CARTESIAN_POINT('Ctrl Pts',(-5.67915655496524,24.822518122386,12.));
#244891=CARTESIAN_POINT('Ctrl Pts',(-5.69677006679429,24.8430549277634,
12.));
#244892=CARTESIAN_POINT('Ctrl Pts',(-5.71447804252019,24.8636067597677,
12.));
#244893=CARTESIAN_POINT('Ctrl Pts',(-5.73228037976927,24.8841731467219,
12.));
#244894=CARTESIAN_POINT('Ctrl Pts',(-5.75017697890813,24.9047536376467,
12.));
#244895=CARTESIAN_POINT('Ctrl Pts',(-5.76816774342236,24.9253478043632,
12.));
#244896=CARTESIAN_POINT('Ctrl Pts',(-5.78625257775703,24.9459552293308,
12.));
#244897=CARTESIAN_POINT('Ctrl Pts',(-5.80443138549747,24.9665754954462,
12.));
#244898=CARTESIAN_POINT('Ctrl Pts',(-5.82270406744214,24.9872081752709,
12.));
#244899=CARTESIAN_POINT('Ctrl Pts',(-5.84107051963073,25.0078528200558,
12.));
#244900=CARTESIAN_POINT('Ctrl Pts',(-5.8595306315681,25.0285089498922,12.));
#244901=CARTESIAN_POINT('Ctrl Pts',(-5.87808428385329,25.0491760405965,
12.));
#244902=CARTESIAN_POINT('Ctrl Pts',(-5.89673135155459,25.0698535426593,
12.));
#244903=CARTESIAN_POINT('Ctrl Pts',(-5.91547170844382,25.0905409050863,
12.));
#244904=CARTESIAN_POINT('Ctrl Pts',(-5.93430523086776,25.1112375971182,
12.));
#244905=CARTESIAN_POINT('Ctrl Pts',(-5.95323180187348,25.1319431317273,
12.));
#244906=CARTESIAN_POINT('Ctrl Pts',(-5.97225131495636,25.1526570863065,
12.));
#244907=CARTESIAN_POINT('Ctrl Pts',(-5.99136367859838,25.1733791296154,
12.));
#244908=CARTESIAN_POINT('Ctrl Pts',(-6.0105688180476,25.1941090269638,12.));
#244909=CARTESIAN_POINT('Ctrl Pts',(-6.02986667390187,25.2148466201368,
12.));
#244910=CARTESIAN_POINT('Ctrl Pts',(-6.04925720151412,25.2355918138798,
12.));
#244911=CARTESIAN_POINT('Ctrl Pts',(-6.06484373634697,25.2521940105523,
12.));
#244912=CARTESIAN_POINT('Ctrl Pts',(-6.07657531787578,25.2646490489816,
12.));
#244913=CARTESIAN_POINT('Ctrl Pts',(-6.08441489609824,25.2729539149479,
12.));
#244914=CARTESIAN_POINT('Ctrl Pts',(-6.08833931617698,25.2771067246846,
12.));
#244915=CARTESIAN_POINT('Ctrl Pts',(-1.76341220531179,22.4835757167854,
0.));
#244916=CARTESIAN_POINT('Ctrl Pts',(-1.76341220531179,22.4835757167854,
12.));
#244917=CARTESIAN_POINT('Ctrl Pts',(-1.76341415538764,22.483581992979,0.));
#244918=CARTESIAN_POINT('Ctrl Pts',(-1.76341415538764,22.483581992979,12.));
#244919=CARTESIAN_POINT('Ctrl Pts',(-1.7634206426357,22.4836387052232,0.));
#244920=CARTESIAN_POINT('Ctrl Pts',(-1.7634206426357,22.4836387052232,12.));
#244921=CARTESIAN_POINT('Ctrl Pts',(-1.76343813434565,22.483856251707,0.));
#244922=CARTESIAN_POINT('Ctrl Pts',(-1.76343813434565,22.483856251707,12.));
#244923=CARTESIAN_POINT('Ctrl Pts',(-1.76347698284792,22.4844112933129,
0.));
#244924=CARTESIAN_POINT('Ctrl Pts',(-1.76347698284792,22.4844112933129,
12.));
#244925=CARTESIAN_POINT('Ctrl Pts',(-1.76355076045546,22.4855446605991,
0.));
#244926=CARTESIAN_POINT('Ctrl Pts',(-1.76355076045546,22.4855446605991,
12.));
#244927=CARTESIAN_POINT('Ctrl Pts',(-1.76364784232963,22.4871115206571,
0.));
#244928=CARTESIAN_POINT('Ctrl Pts',(-1.76364784232963,22.4871115206571,
12.));
#244929=CARTESIAN_POINT('Ctrl Pts',(-1.76376424879505,22.4890991659478,
0.));
#244930=CARTESIAN_POINT('Ctrl Pts',(-1.76376424879505,22.4890991659478,
12.));
#244931=CARTESIAN_POINT('Ctrl Pts',(-1.76389475965724,22.4914909094908,
0.));
#244932=CARTESIAN_POINT('Ctrl Pts',(-1.76389475965724,22.4914909094908,
12.));
#244933=CARTESIAN_POINT('Ctrl Pts',(-1.76403393880301,22.4942693792449,
0.));
#244934=CARTESIAN_POINT('Ctrl Pts',(-1.76403393880301,22.4942693792449,
12.));
#244935=CARTESIAN_POINT('Ctrl Pts',(-1.76417731243462,22.4974203063191,
0.));
#244936=CARTESIAN_POINT('Ctrl Pts',(-1.76417731243462,22.4974203063191,
12.));
#244937=CARTESIAN_POINT('Ctrl Pts',(-1.76432160068725,22.5009332677316,
0.));
#244938=CARTESIAN_POINT('Ctrl Pts',(-1.76432160068725,22.5009332677316,
12.));
#244939=CARTESIAN_POINT('Ctrl Pts',(-1.76446408210366,22.5047996391978,
0.));
#244940=CARTESIAN_POINT('Ctrl Pts',(-1.76446408210366,22.5047996391978,
12.));
#244941=CARTESIAN_POINT('Ctrl Pts',(-1.76460218257323,22.5090112700212,
0.));
#244942=CARTESIAN_POINT('Ctrl Pts',(-1.76460218257323,22.5090112700212,
12.));
#244943=CARTESIAN_POINT('Ctrl Pts',(-1.76473303281159,22.5135590569554,
0.));
#244944=CARTESIAN_POINT('Ctrl Pts',(-1.76473303281159,22.5135590569554,
12.));
#244945=CARTESIAN_POINT('Ctrl Pts',(-1.76485369319896,22.5184336670207,
0.));
#244946=CARTESIAN_POINT('Ctrl Pts',(-1.76485369319896,22.5184336670207,
12.));
#244947=CARTESIAN_POINT('Ctrl Pts',(-1.76496128643369,22.5236259635515,
0.));
#244948=CARTESIAN_POINT('Ctrl Pts',(-1.76496128643369,22.5236259635515,
12.));
#244949=CARTESIAN_POINT('Ctrl Pts',(-1.76505320262752,22.529127665298,0.));
#244950=CARTESIAN_POINT('Ctrl Pts',(-1.76505320262752,22.529127665298,12.));
#244951=CARTESIAN_POINT('Ctrl Pts',(-1.7651271156325,22.5349313983571,0.));
#244952=CARTESIAN_POINT('Ctrl Pts',(-1.7651271156325,22.5349313983571,12.));
#244953=CARTESIAN_POINT('Ctrl Pts',(-1.76518087841493,22.5410303590891,
0.));
#244954=CARTESIAN_POINT('Ctrl Pts',(-1.76518087841493,22.5410303590891,
12.));
#244955=CARTESIAN_POINT('Ctrl Pts',(-1.76521245524047,22.5474180954006,
0.));
#244956=CARTESIAN_POINT('Ctrl Pts',(-1.76521245524047,22.5474180954006,
12.));
#244957=CARTESIAN_POINT('Ctrl Pts',(-1.76521983384063,22.5540882235837,
0.));
#244958=CARTESIAN_POINT('Ctrl Pts',(-1.76521983384063,22.5540882235837,
12.));
#244959=CARTESIAN_POINT('Ctrl Pts',(-1.76520104500449,22.5610344912501,
0.));
#244960=CARTESIAN_POINT('Ctrl Pts',(-1.76520104500449,22.5610344912501,
12.));
#244961=CARTESIAN_POINT('Ctrl Pts',(-1.76515418518829,22.5682508499873,
0.));
#244962=CARTESIAN_POINT('Ctrl Pts',(-1.76515418518829,22.5682508499873,
12.));
#244963=CARTESIAN_POINT('Ctrl Pts',(-1.76507744026747,22.5757315316355,
0.));
#244964=CARTESIAN_POINT('Ctrl Pts',(-1.76507744026747,22.5757315316355,
12.));
#244965=CARTESIAN_POINT('Ctrl Pts',(-1.76496910283088,22.5834711038024,
0.));
#244966=CARTESIAN_POINT('Ctrl Pts',(-1.76496910283088,22.5834711038024,
12.));
#244967=CARTESIAN_POINT('Ctrl Pts',(-1.76482755288411,22.5914644078106,
0.));
#244968=CARTESIAN_POINT('Ctrl Pts',(-1.76482755288411,22.5914644078106,
12.));
#244969=CARTESIAN_POINT('Ctrl Pts',(-1.76465124413556,22.5997065145638,
0.));
#244970=CARTESIAN_POINT('Ctrl Pts',(-1.76465124413556,22.5997065145638,
12.));
#244971=CARTESIAN_POINT('Ctrl Pts',(-1.76443868648015,22.6081926681342,
0.));
#244972=CARTESIAN_POINT('Ctrl Pts',(-1.76443868648015,22.6081926681342,
12.));
#244973=CARTESIAN_POINT('Ctrl Pts',(-1.76418843543739,22.6169182517693,
0.));
#244974=CARTESIAN_POINT('Ctrl Pts',(-1.76418843543739,22.6169182517693,
12.));
#244975=CARTESIAN_POINT('Ctrl Pts',(-1.76389909571402,22.6258787994847,
0.));
#244976=CARTESIAN_POINT('Ctrl Pts',(-1.76389909571402,22.6258787994847,
12.));
#244977=CARTESIAN_POINT('Ctrl Pts',(-1.76356932176272,22.635069997936,0.));
#244978=CARTESIAN_POINT('Ctrl Pts',(-1.76356932176272,22.635069997936,12.));
#244979=CARTESIAN_POINT('Ctrl Pts',(-1.76319782013914,22.6444876940425,
0.));
#244980=CARTESIAN_POINT('Ctrl Pts',(-1.76319782013914,22.6444876940425,
12.));
#244981=CARTESIAN_POINT('Ctrl Pts',(-1.76278334912559,22.6541278938413,
0.));
#244982=CARTESIAN_POINT('Ctrl Pts',(-1.76278334912559,22.6541278938413,
12.));
#244983=CARTESIAN_POINT('Ctrl Pts',(-1.76232471392567,22.6639867471756,
0.));
#244984=CARTESIAN_POINT('Ctrl Pts',(-1.76232471392567,22.6639867471756,
12.));
#244985=CARTESIAN_POINT('Ctrl Pts',(-1.76182076289525,22.6740605356699,
0.));
#244986=CARTESIAN_POINT('Ctrl Pts',(-1.76182076289525,22.6740605356699,
12.));
#244987=CARTESIAN_POINT('Ctrl Pts',(-1.76127038310613,22.6843456585245,
0.));
#244988=CARTESIAN_POINT('Ctrl Pts',(-1.76127038310613,22.6843456585245,
12.));
#244989=CARTESIAN_POINT('Ctrl Pts',(-1.76067249704884,22.6948386219843,
0.));
#244990=CARTESIAN_POINT('Ctrl Pts',(-1.76067249704884,22.6948386219843,
12.));
#244991=CARTESIAN_POINT('Ctrl Pts',(-1.76002606202399,22.7055360375481,
0.));
#244992=CARTESIAN_POINT('Ctrl Pts',(-1.76002606202399,22.7055360375481,
12.));
#244993=CARTESIAN_POINT('Ctrl Pts',(-1.75933006905924,22.7164346186007,
0.));
#244994=CARTESIAN_POINT('Ctrl Pts',(-1.75933006905924,22.7164346186007,
12.));
#244995=CARTESIAN_POINT('Ctrl Pts',(-1.75858354204635,22.7275311777305,
0.));
#244996=CARTESIAN_POINT('Ctrl Pts',(-1.75858354204635,22.7275311777305,
12.));
#244997=CARTESIAN_POINT('Ctrl Pts',(-1.75778553673249,22.7388226235565,
0.));
#244998=CARTESIAN_POINT('Ctrl Pts',(-1.75778553673249,22.7388226235565,
12.));
#244999=CARTESIAN_POINT('Ctrl Pts',(-1.75693513908911,22.7503059556455,
0.));
#245000=CARTESIAN_POINT('Ctrl Pts',(-1.75693513908911,22.7503059556455,
12.));
#245001=CARTESIAN_POINT('Ctrl Pts',(-1.7560314637164,22.7619782595013,0.));
#245002=CARTESIAN_POINT('Ctrl Pts',(-1.7560314637164,22.7619782595013,12.));
#245003=CARTESIAN_POINT('Ctrl Pts',(-1.75507365227127,22.7738367016115,
0.));
#245004=CARTESIAN_POINT('Ctrl Pts',(-1.75507365227127,22.7738367016115,
12.));
#245005=CARTESIAN_POINT('Ctrl Pts',(-1.7540608718293,22.7858785242358,0.));
#245006=CARTESIAN_POINT('Ctrl Pts',(-1.7540608718293,22.7858785242358,12.));
#245007=CARTESIAN_POINT('Ctrl Pts',(-1.75299231391461,22.7981010424312,
0.));
#245008=CARTESIAN_POINT('Ctrl Pts',(-1.75299231391461,22.7981010424312,
12.));
#245009=CARTESIAN_POINT('Ctrl Pts',(-1.7518671936559,22.8105016414712,0.));
#245010=CARTESIAN_POINT('Ctrl Pts',(-1.7518671936559,22.8105016414712,12.));
#245011=CARTESIAN_POINT('Ctrl Pts',(-1.75068474890884,22.8230777741285,
0.));
#245012=CARTESIAN_POINT('Ctrl Pts',(-1.75068474890884,22.8230777741285,
12.));
#245013=CARTESIAN_POINT('Ctrl Pts',(-1.74944423940117,22.8358269579854,
0.));
#245014=CARTESIAN_POINT('Ctrl Pts',(-1.74944423940117,22.8358269579854,
12.));
#245015=CARTESIAN_POINT('Ctrl Pts',(-1.74814494588492,22.8487467728075,
0.));
#245016=CARTESIAN_POINT('Ctrl Pts',(-1.74814494588492,22.8487467728075,
12.));
#245017=CARTESIAN_POINT('Ctrl Pts',(-1.74678616930663,22.8618348580234,
0.));
#245018=CARTESIAN_POINT('Ctrl Pts',(-1.74678616930663,22.8618348580234,
12.));
#245019=CARTESIAN_POINT('Ctrl Pts',(-1.745367229982,22.8750889101696,0.));
#245020=CARTESIAN_POINT('Ctrl Pts',(-1.745367229982,22.8750889101696,12.));
#245021=CARTESIAN_POINT('Ctrl Pts',(-1.74388746677702,22.8885066803351,
0.));
#245022=CARTESIAN_POINT('Ctrl Pts',(-1.74388746677702,22.8885066803351,
12.));
#245023=CARTESIAN_POINT('Ctrl Pts',(-1.74234623630079,22.9020859716144,
0.));
#245024=CARTESIAN_POINT('Ctrl Pts',(-1.74234623630079,22.9020859716144,
12.));
#245025=CARTESIAN_POINT('Ctrl Pts',(-1.74074291231057,22.9158246373365,
0.));
#245026=CARTESIAN_POINT('Ctrl Pts',(-1.74074291231057,22.9158246373365,
12.));
#245027=CARTESIAN_POINT('Ctrl Pts',(-1.73907688511664,22.9297205792587,
0.));
#245028=CARTESIAN_POINT('Ctrl Pts',(-1.73907688511664,22.9297205792587,
12.));
#245029=CARTESIAN_POINT('Ctrl Pts',(-1.73734756100038,22.9437717457825,
0.));
#245030=CARTESIAN_POINT('Ctrl Pts',(-1.73734756100038,22.9437717457825,
12.));
#245031=CARTESIAN_POINT('Ctrl Pts',(-1.73555436162771,22.9579761301062,
0.));
#245032=CARTESIAN_POINT('Ctrl Pts',(-1.73555436162771,22.9579761301062,
12.));
#245033=CARTESIAN_POINT('Ctrl Pts',(-1.73369672350818,22.9723317685688,
0.));
#245034=CARTESIAN_POINT('Ctrl Pts',(-1.73369672350818,22.9723317685688,
12.));
#245035=CARTESIAN_POINT('Ctrl Pts',(-1.73177409750194,22.9868367391978,
0.));
#245036=CARTESIAN_POINT('Ctrl Pts',(-1.73177409750194,22.9868367391978,
12.));
#245037=CARTESIAN_POINT('Ctrl Pts',(-1.72978594832137,23.0014891601891,
0.));
#245038=CARTESIAN_POINT('Ctrl Pts',(-1.72978594832137,23.0014891601891,
12.));
#245039=CARTESIAN_POINT('Ctrl Pts',(-1.72773175404703,23.0162871884167,
0.));
#245040=CARTESIAN_POINT('Ctrl Pts',(-1.72773175404703,23.0162871884167,
12.));
#245041=CARTESIAN_POINT('Ctrl Pts',(-1.72561100564033,23.031229017888,0.));
#245042=CARTESIAN_POINT('Ctrl Pts',(-1.72561100564033,23.031229017888,12.));
#245043=CARTESIAN_POINT('Ctrl Pts',(-1.72342320653731,23.0463128785528,
0.));
#245044=CARTESIAN_POINT('Ctrl Pts',(-1.72342320653731,23.0463128785528,
12.));
#245045=CARTESIAN_POINT('Ctrl Pts',(-1.7211678722598,23.061537035156,0.));
#245046=CARTESIAN_POINT('Ctrl Pts',(-1.7211678722598,23.061537035156,12.));
#245047=CARTESIAN_POINT('Ctrl Pts',(-1.71884453003027,23.0768997860709,
0.));
#245048=CARTESIAN_POINT('Ctrl Pts',(-1.71884453003027,23.0768997860709,
12.));
#245049=CARTESIAN_POINT('Ctrl Pts',(-1.71645271839311,23.0923994621216,
0.));
#245050=CARTESIAN_POINT('Ctrl Pts',(-1.71645271839311,23.0923994621216,
12.));
#245051=CARTESIAN_POINT('Ctrl Pts',(-1.71399198684725,23.1080344254291,
0.));
#245052=CARTESIAN_POINT('Ctrl Pts',(-1.71399198684725,23.1080344254291,
12.));
#245053=CARTESIAN_POINT('Ctrl Pts',(-1.71146189552192,23.1238030684929,
0.));
#245054=CARTESIAN_POINT('Ctrl Pts',(-1.71146189552192,23.1238030684929,
12.));
#245055=CARTESIAN_POINT('Ctrl Pts',(-1.7088620148546,23.1397038132358,0.));
#245056=CARTESIAN_POINT('Ctrl Pts',(-1.7088620148546,23.1397038132358,12.));
#245057=CARTESIAN_POINT('Ctrl Pts',(-1.70619192527847,23.1557351100613,
0.));
#245058=CARTESIAN_POINT('Ctrl Pts',(-1.70619192527847,23.1557351100613,
12.));
#245059=CARTESIAN_POINT('Ctrl Pts',(-1.70345121691259,23.1718954368749,
0.));
#245060=CARTESIAN_POINT('Ctrl Pts',(-1.70345121691259,23.1718954368749,
12.));
#245061=CARTESIAN_POINT('Ctrl Pts',(-1.70063948926987,23.1881832981848,
0.));
#245062=CARTESIAN_POINT('Ctrl Pts',(-1.70063948926987,23.1881832981848,
12.));
#245063=CARTESIAN_POINT('Ctrl Pts',(-1.69775635099425,23.2045972243765,
0.));
#245064=CARTESIAN_POINT('Ctrl Pts',(-1.69775635099425,23.2045972243765,
12.));
#245065=CARTESIAN_POINT('Ctrl Pts',(-1.69480141959946,23.2211357709374,
0.));
#245066=CARTESIAN_POINT('Ctrl Pts',(-1.69480141959946,23.2211357709374,
12.));
#245067=CARTESIAN_POINT('Ctrl Pts',(-1.69177432121716,23.2377975177014,
0.));
#245068=CARTESIAN_POINT('Ctrl Pts',(-1.69177432121716,23.2377975177014,
12.));
#245069=CARTESIAN_POINT('Ctrl Pts',(-1.6886746903491,23.2545810680536,0.));
#245070=CARTESIAN_POINT('Ctrl Pts',(-1.6886746903491,23.2545810680536,12.));
#245071=CARTESIAN_POINT('Ctrl Pts',(-1.68550216963275,23.2714850482245,
0.));
#245072=CARTESIAN_POINT('Ctrl Pts',(-1.68550216963275,23.2714850482245,
12.));
#245073=CARTESIAN_POINT('Ctrl Pts',(-1.68225640962181,23.2885081066949,
0.));
#245074=CARTESIAN_POINT('Ctrl Pts',(-1.68225640962181,23.2885081066949,
12.));
#245075=CARTESIAN_POINT('Ctrl Pts',(-1.67893706857123,23.3056489135611,
0.));
#245076=CARTESIAN_POINT('Ctrl Pts',(-1.67893706857123,23.3056489135611,
12.));
#245077=CARTESIAN_POINT('Ctrl Pts',(-1.67554381222987,23.3229061599145,
0.));
#245078=CARTESIAN_POINT('Ctrl Pts',(-1.67554381222987,23.3229061599145,
12.));
#245079=CARTESIAN_POINT('Ctrl Pts',(-1.67207631363905,23.3402785571866,
0.));
#245080=CARTESIAN_POINT('Ctrl Pts',(-1.67207631363905,23.3402785571866,
12.));
#245081=CARTESIAN_POINT('Ctrl Pts',(-1.66853425293978,23.3577648365747,
0.));
#245082=CARTESIAN_POINT('Ctrl Pts',(-1.66853425293978,23.3577648365747,
12.));
#245083=CARTESIAN_POINT('Ctrl Pts',(-1.66491731718864,23.375363748555,0.));
#245084=CARTESIAN_POINT('Ctrl Pts',(-1.66491731718864,23.375363748555,12.));
#245085=CARTESIAN_POINT('Ctrl Pts',(-1.66122520018008,23.3930740623622,
0.));
#245086=CARTESIAN_POINT('Ctrl Pts',(-1.66122520018008,23.3930740623622,
12.));
#245087=CARTESIAN_POINT('Ctrl Pts',(-1.65745760227507,23.4108945654803,
0.));
#245088=CARTESIAN_POINT('Ctrl Pts',(-1.65745760227507,23.4108945654803,
12.));
#245089=CARTESIAN_POINT('Ctrl Pts',(-1.6536142302373,23.4288240631034,0.));
#245090=CARTESIAN_POINT('Ctrl Pts',(-1.6536142302373,23.4288240631034,12.));
#245091=CARTESIAN_POINT('Ctrl Pts',(-1.6496947970734,23.446861377656,0.));
#245092=CARTESIAN_POINT('Ctrl Pts',(-1.6496947970734,23.446861377656,12.));
#245093=CARTESIAN_POINT('Ctrl Pts',(-1.64569902187608,23.4650053483919,
0.));
#245094=CARTESIAN_POINT('Ctrl Pts',(-1.64569902187608,23.4650053483919,
12.));
#245095=CARTESIAN_POINT('Ctrl Pts',(-1.64162662967525,23.4832548309638,
0.));
#245096=CARTESIAN_POINT('Ctrl Pts',(-1.64162662967525,23.4832548309638,
12.));
#245097=CARTESIAN_POINT('Ctrl Pts',(-1.63747735129474,23.5016086970006,
0.));
#245098=CARTESIAN_POINT('Ctrl Pts',(-1.63747735129474,23.5016086970006,
12.));
#245099=CARTESIAN_POINT('Ctrl Pts',(-1.63325092321731,23.5200658336624,
0.));
#245100=CARTESIAN_POINT('Ctrl Pts',(-1.63325092321731,23.5200658336624,
12.));
#245101=CARTESIAN_POINT('Ctrl Pts',(-1.62894708745231,23.5386251432278,
0.));
#245102=CARTESIAN_POINT('Ctrl Pts',(-1.62894708745231,23.5386251432278,
12.));
#245103=CARTESIAN_POINT('Ctrl Pts',(-1.62456559140072,23.5572855427617,
0.));
#245104=CARTESIAN_POINT('Ctrl Pts',(-1.62456559140072,23.5572855427617,
12.));
#245105=CARTESIAN_POINT('Ctrl Pts',(-1.62010618772869,23.5760459637608,
0.));
#245106=CARTESIAN_POINT('Ctrl Pts',(-1.62010618772869,23.5760459637608,
12.));
#245107=CARTESIAN_POINT('Ctrl Pts',(-1.61556863424697,23.5949053517996,
0.));
#245108=CARTESIAN_POINT('Ctrl Pts',(-1.61556863424697,23.5949053517996,
12.));
#245109=CARTESIAN_POINT('Ctrl Pts',(-1.61095269379773,23.6138626661644,
0.));
#245110=CARTESIAN_POINT('Ctrl Pts',(-1.61095269379773,23.6138626661644,
12.));
#245111=CARTESIAN_POINT('Ctrl Pts',(-1.60625813414666,23.6329168794916,
0.));
#245112=CARTESIAN_POINT('Ctrl Pts',(-1.60625813414666,23.6329168794916,
12.));
#245113=CARTESIAN_POINT('Ctrl Pts',(-1.60148472786588,23.6520669774863,
0.));
#245114=CARTESIAN_POINT('Ctrl Pts',(-1.60148472786588,23.6520669774863,
12.));
#245115=CARTESIAN_POINT('Ctrl Pts',(-1.59663225222458,23.6713119586302,
0.));
#245116=CARTESIAN_POINT('Ctrl Pts',(-1.59663225222458,23.6713119586302,
12.));
#245117=CARTESIAN_POINT('Ctrl Pts',(-1.59170048908632,23.6906508338833,
0.));
#245118=CARTESIAN_POINT('Ctrl Pts',(-1.59170048908632,23.6906508338833,
12.));
#245119=CARTESIAN_POINT('Ctrl Pts',(-1.58668922481222,23.7100826263835,
0.));
#245120=CARTESIAN_POINT('Ctrl Pts',(-1.58668922481222,23.7100826263835,
12.));
#245121=CARTESIAN_POINT('Ctrl Pts',(-1.58159825017362,23.7296063711308,
0.));
#245122=CARTESIAN_POINT('Ctrl Pts',(-1.58159825017362,23.7296063711308,
12.));
#245123=CARTESIAN_POINT('Ctrl Pts',(-1.57642736025251,23.7492211147369,
0.));
#245124=CARTESIAN_POINT('Ctrl Pts',(-1.57642736025251,23.7492211147369,
12.));
#245125=CARTESIAN_POINT('Ctrl Pts',(-1.57117635434412,23.7689259151869,
0.));
#245126=CARTESIAN_POINT('Ctrl Pts',(-1.57117635434412,23.7689259151869,
12.));
#245127=CARTESIAN_POINT('Ctrl Pts',(-1.56584503586844,23.788719841588,0.));
#245128=CARTESIAN_POINT('Ctrl Pts',(-1.56584503586844,23.788719841588,12.));
#245129=CARTESIAN_POINT('Ctrl Pts',(-1.56043321228631,23.8086019739192,
0.));
#245130=CARTESIAN_POINT('Ctrl Pts',(-1.56043321228631,23.8086019739192,
12.));
#245131=CARTESIAN_POINT('Ctrl Pts',(-1.55494069502628,23.8285714027631,
0.));
#245132=CARTESIAN_POINT('Ctrl Pts',(-1.55494069502628,23.8285714027631,
12.));
#245133=CARTESIAN_POINT('Ctrl Pts',(-1.5493672994053,23.8486272290698,0.));
#245134=CARTESIAN_POINT('Ctrl Pts',(-1.5493672994053,23.8486272290698,12.));
#245135=CARTESIAN_POINT('Ctrl Pts',(-1.54371284453978,23.8687685639635,
0.));
#245136=CARTESIAN_POINT('Ctrl Pts',(-1.54371284453978,23.8687685639635,
12.));
#245137=CARTESIAN_POINT('Ctrl Pts',(-1.53797715326748,23.8889945285313,
0.));
#245138=CARTESIAN_POINT('Ctrl Pts',(-1.53797715326748,23.8889945285313,
12.));
#245139=CARTESIAN_POINT('Ctrl Pts',(-1.53216005207462,23.9093042536119,
0.));
#245140=CARTESIAN_POINT('Ctrl Pts',(-1.53216005207462,23.9093042536119,
12.));
#245141=CARTESIAN_POINT('Ctrl Pts',(-1.5262613710304,23.9296968795761,0.));
#245142=CARTESIAN_POINT('Ctrl Pts',(-1.5262613710304,23.9296968795761,12.));
#245143=CARTESIAN_POINT('Ctrl Pts',(-1.52028094372806,23.9501715561038,
0.));
#245144=CARTESIAN_POINT('Ctrl Pts',(-1.52028094372806,23.9501715561038,
12.));
#245145=CARTESIAN_POINT('Ctrl Pts',(-1.51421860720628,23.9707274420145,
0.));
#245146=CARTESIAN_POINT('Ctrl Pts',(-1.51421860720628,23.9707274420145,
12.));
#245147=CARTESIAN_POINT('Ctrl Pts',(-1.50807420187703,23.991363705093,0.));
#245148=CARTESIAN_POINT('Ctrl Pts',(-1.50807420187703,23.991363705093,12.));
#245149=CARTESIAN_POINT('Ctrl Pts',(-1.50184757146099,24.0120795219086,
0.));
#245150=CARTESIAN_POINT('Ctrl Pts',(-1.50184757146099,24.0120795219086,
12.));
#245151=CARTESIAN_POINT('Ctrl Pts',(-1.49553856292798,24.0328740776331,
0.));
#245152=CARTESIAN_POINT('Ctrl Pts',(-1.49553856292798,24.0328740776331,
12.));
#245153=CARTESIAN_POINT('Ctrl Pts',(-1.48914702644883,24.053746565843,0.));
#245154=CARTESIAN_POINT('Ctrl Pts',(-1.48914702644883,24.053746565843,12.));
#245155=CARTESIAN_POINT('Ctrl Pts',(-1.4826728153368,24.074696188353,0.));
#245156=CARTESIAN_POINT('Ctrl Pts',(-1.4826728153368,24.074696188353,12.));
#245157=CARTESIAN_POINT('Ctrl Pts',(-1.47611578597741,24.0957221550782,
0.));
#245158=CARTESIAN_POINT('Ctrl Pts',(-1.47611578597741,24.0957221550782,
12.));
#245159=CARTESIAN_POINT('Ctrl Pts',(-1.46947579776992,24.1168236838827,
0.));
#245160=CARTESIAN_POINT('Ctrl Pts',(-1.46947579776992,24.1168236838827,
12.));
#245161=CARTESIAN_POINT('Ctrl Pts',(-1.46275271307398,24.1380000004272,
0.));
#245162=CARTESIAN_POINT('Ctrl Pts',(-1.46275271307398,24.1380000004272,
12.));
#245163=CARTESIAN_POINT('Ctrl Pts',(-1.45594639716314,24.1592503380105,
0.));
#245164=CARTESIAN_POINT('Ctrl Pts',(-1.45594639716314,24.1592503380105,
12.));
#245165=CARTESIAN_POINT('Ctrl Pts',(-1.44905671818721,24.1805739374033,
0.));
#245166=CARTESIAN_POINT('Ctrl Pts',(-1.44905671818721,24.1805739374033,
12.));
#245167=CARTESIAN_POINT('Ctrl Pts',(-1.44208354711074,24.2019700467214,
0.));
#245168=CARTESIAN_POINT('Ctrl Pts',(-1.44208354711074,24.2019700467214,
12.));
#245169=CARTESIAN_POINT('Ctrl Pts',(-1.43502675765502,24.2234379212978,
0.));
#245170=CARTESIAN_POINT('Ctrl Pts',(-1.43502675765502,24.2234379212978,
12.));
#245171=CARTESIAN_POINT('Ctrl Pts',(-1.42788622624851,24.2449768235485,
0.));
#245172=CARTESIAN_POINT('Ctrl Pts',(-1.42788622624851,24.2449768235485,
12.));
#245173=CARTESIAN_POINT('Ctrl Pts',(-1.42066183198252,24.2665860228357,
0.));
#245174=CARTESIAN_POINT('Ctrl Pts',(-1.42066183198252,24.2665860228357,
12.));
#245175=CARTESIAN_POINT('Ctrl Pts',(-1.41335345657685,24.2882647953214,
0.));
#245176=CARTESIAN_POINT('Ctrl Pts',(-1.41335345657685,24.2882647953214,
12.));
#245177=CARTESIAN_POINT('Ctrl Pts',(-1.40596098434341,24.3100124238316,
0.));
#245178=CARTESIAN_POINT('Ctrl Pts',(-1.40596098434341,24.3100124238316,
12.));
#245179=CARTESIAN_POINT('Ctrl Pts',(-1.3984843021281,24.3318281977647,0.));
#245180=CARTESIAN_POINT('Ctrl Pts',(-1.3984843021281,24.3318281977647,12.));
#245181=CARTESIAN_POINT('Ctrl Pts',(-1.3909232992639,24.3537114129877,0.));
#245182=CARTESIAN_POINT('Ctrl Pts',(-1.3909232992639,24.3537114129877,12.));
#245183=CARTESIAN_POINT('Ctrl Pts',(-1.38327786752998,24.37566137173,0.));
#245184=CARTESIAN_POINT('Ctrl Pts',(-1.38327786752998,24.37566137173,12.));
#245185=CARTESIAN_POINT('Ctrl Pts',(-1.37554790111608,24.3976773824731,
0.));
#245186=CARTESIAN_POINT('Ctrl Pts',(-1.37554790111608,24.3976773824731,
12.));
#245187=CARTESIAN_POINT('Ctrl Pts',(-1.36773329659954,24.4197587598337,
0.));
#245188=CARTESIAN_POINT('Ctrl Pts',(-1.36773329659954,24.4197587598337,
12.));
#245189=CARTESIAN_POINT('Ctrl Pts',(-1.35983395290624,24.4419048244524,
0.));
#245190=CARTESIAN_POINT('Ctrl Pts',(-1.35983395290624,24.4419048244524,
12.));
#245191=CARTESIAN_POINT('Ctrl Pts',(-1.35184977125645,24.4641149028894,
0.));
#245192=CARTESIAN_POINT('Ctrl Pts',(-1.35184977125645,24.4641149028894,
12.));
#245193=CARTESIAN_POINT('Ctrl Pts',(-1.34378065512335,24.4863883275135,
0.));
#245194=CARTESIAN_POINT('Ctrl Pts',(-1.34378065512335,24.4863883275135,
12.));
#245195=CARTESIAN_POINT('Ctrl Pts',(-1.33562651019684,24.5087244363856,
0.));
#245196=CARTESIAN_POINT('Ctrl Pts',(-1.33562651019684,24.5087244363856,
12.));
#245197=CARTESIAN_POINT('Ctrl Pts',(-1.32738724435326,24.5311225731434,
0.));
#245198=CARTESIAN_POINT('Ctrl Pts',(-1.32738724435326,24.5311225731434,
12.));
#245199=CARTESIAN_POINT('Ctrl Pts',(-1.31906276763669,24.5535820868671,
0.));
#245200=CARTESIAN_POINT('Ctrl Pts',(-1.31906276763669,24.5535820868671,
12.));
#245201=CARTESIAN_POINT('Ctrl Pts',(-1.31065299222023,24.576102332018,0.));
#245202=CARTESIAN_POINT('Ctrl Pts',(-1.31065299222023,24.576102332018,12.));
#245203=CARTESIAN_POINT('Ctrl Pts',(-1.30215783236364,24.5986826684025,
0.));
#245204=CARTESIAN_POINT('Ctrl Pts',(-1.30215783236364,24.5986826684025,
12.));
#245205=CARTESIAN_POINT('Ctrl Pts',(-1.29357720438108,24.6213224611228,
0.));
#245206=CARTESIAN_POINT('Ctrl Pts',(-1.29357720438108,24.6213224611228,
12.));
#245207=CARTESIAN_POINT('Ctrl Pts',(-1.28491102661514,24.6440210805278,
0.));
#245208=CARTESIAN_POINT('Ctrl Pts',(-1.28491102661514,24.6440210805278,
12.));
#245209=CARTESIAN_POINT('Ctrl Pts',(-1.2761592194164,24.666777902156,0.));
#245210=CARTESIAN_POINT('Ctrl Pts',(-1.2761592194164,24.666777902156,12.));
#245211=CARTESIAN_POINT('Ctrl Pts',(-1.26732170513497,24.6895923066837,
0.));
#245212=CARTESIAN_POINT('Ctrl Pts',(-1.26732170513497,24.6895923066837,
12.));
#245213=CARTESIAN_POINT('Ctrl Pts',(-1.25839840807415,24.7124636797895,
0.));
#245214=CARTESIAN_POINT('Ctrl Pts',(-1.25839840807415,24.7124636797895,
12.));
#245215=CARTESIAN_POINT('Ctrl Pts',(-1.24938925444324,24.7353914120012,
0.));
#245216=CARTESIAN_POINT('Ctrl Pts',(-1.24938925444324,24.7353914120012,
12.));
#245217=CARTESIAN_POINT('Ctrl Pts',(-1.24029417231988,24.7583748985439,
0.));
#245218=CARTESIAN_POINT('Ctrl Pts',(-1.24029417231988,24.7583748985439,
12.));
#245219=CARTESIAN_POINT('Ctrl Pts',(-1.23111309161843,24.78141353918,0.));
#245220=CARTESIAN_POINT('Ctrl Pts',(-1.23111309161843,24.78141353918,12.));
#245221=CARTESIAN_POINT('Ctrl Pts',(-1.22184594406526,24.8045067380536,
0.));
#245222=CARTESIAN_POINT('Ctrl Pts',(-1.22184594406526,24.8045067380536,
12.));
#245223=CARTESIAN_POINT('Ctrl Pts',(-1.21249266318205,24.8276539035092,
0.));
#245224=CARTESIAN_POINT('Ctrl Pts',(-1.21249266318205,24.8276539035092,
12.));
#245225=CARTESIAN_POINT('Ctrl Pts',(-1.20305318426015,24.8508544481973,
0.));
#245226=CARTESIAN_POINT('Ctrl Pts',(-1.20305318426015,24.8508544481973,
12.));
#245227=CARTESIAN_POINT('Ctrl Pts',(-1.19352744434059,24.8741077892074,
0.));
#245228=CARTESIAN_POINT('Ctrl Pts',(-1.19352744434059,24.8741077892074,
12.));
#245229=CARTESIAN_POINT('Ctrl Pts',(-1.18391538220098,24.8974133481829,
0.));
#245230=CARTESIAN_POINT('Ctrl Pts',(-1.18391538220098,24.8974133481829,
12.));
#245231=CARTESIAN_POINT('Ctrl Pts',(-1.17421693835039,24.9207705514449,
0.));
#245232=CARTESIAN_POINT('Ctrl Pts',(-1.17421693835039,24.9207705514449,
12.));
#245233=CARTESIAN_POINT('Ctrl Pts',(-1.16443205502852,24.9441788300932,
0.));
#245234=CARTESIAN_POINT('Ctrl Pts',(-1.16443205502852,24.9441788300932,
12.));
#245235=CARTESIAN_POINT('Ctrl Pts',(-1.15456067621894,24.9676376201501,
0.));
#245236=CARTESIAN_POINT('Ctrl Pts',(-1.15456067621894,24.9676376201501,
12.));
#245237=CARTESIAN_POINT('Ctrl Pts',(-1.14460274758206,24.9911463621431,
0.));
#245238=CARTESIAN_POINT('Ctrl Pts',(-1.14460274758206,24.9911463621431,
12.));
#245239=CARTESIAN_POINT('Ctrl Pts',(-1.13455821638536,25.0147045006193,
0.));
#245240=CARTESIAN_POINT('Ctrl Pts',(-1.13455821638536,25.0147045006193,
12.));
#245241=CARTESIAN_POINT('Ctrl Pts',(-1.12442703144455,25.0383114836898,
0.));
#245242=CARTESIAN_POINT('Ctrl Pts',(-1.12442703144455,25.0383114836898,
12.));
#245243=CARTESIAN_POINT('Ctrl Pts',(-1.1142091430689,25.0619667625336,0.));
#245244=CARTESIAN_POINT('Ctrl Pts',(-1.1142091430689,25.0619667625336,12.));
#245245=CARTESIAN_POINT('Ctrl Pts',(-1.1039045030174,25.085669790968,0.));
#245246=CARTESIAN_POINT('Ctrl Pts',(-1.1039045030174,25.085669790968,12.));
#245247=CARTESIAN_POINT('Ctrl Pts',(-1.09351306445299,25.1094200248448,
0.));
#245248=CARTESIAN_POINT('Ctrl Pts',(-1.09351306445299,25.1094200248448,
12.));
#245249=CARTESIAN_POINT('Ctrl Pts',(-1.08303478197174,25.1332169227415,
0.));
#245250=CARTESIAN_POINT('Ctrl Pts',(-1.08303478197174,25.1332169227415,
12.));
#245251=CARTESIAN_POINT('Ctrl Pts',(-1.0724696116546,25.1570599469311,0.));
#245252=CARTESIAN_POINT('Ctrl Pts',(-1.0724696116546,25.1570599469311,12.));
#245253=CARTESIAN_POINT('Ctrl Pts',(-1.06181751111754,25.1809485642191,
0.));
#245254=CARTESIAN_POINT('Ctrl Pts',(-1.06181751111754,25.1809485642191,
12.));
#245255=CARTESIAN_POINT('Ctrl Pts',(-1.05107843957926,25.2048822469027,
0.));
#245256=CARTESIAN_POINT('Ctrl Pts',(-1.05107843957926,25.2048822469027,
12.));
#245257=CARTESIAN_POINT('Ctrl Pts',(-1.04025235791515,25.2288604735087,
0.));
#245258=CARTESIAN_POINT('Ctrl Pts',(-1.04025235791515,25.2288604735087,
12.));
#245259=CARTESIAN_POINT('Ctrl Pts',(-1.0293392287683,25.2528827300427,0.));
#245260=CARTESIAN_POINT('Ctrl Pts',(-1.0293392287683,25.2528827300427,12.));
#245261=CARTESIAN_POINT('Ctrl Pts',(-1.01833901642272,25.2769485087268,
0.));
#245262=CARTESIAN_POINT('Ctrl Pts',(-1.01833901642272,25.2769485087268,
12.));
#245263=CARTESIAN_POINT('Ctrl Pts',(-1.00725168656934,25.3010573055557,
0.));
#245264=CARTESIAN_POINT('Ctrl Pts',(-1.00725168656934,25.3010573055557,
12.));
#245265=CARTESIAN_POINT('Ctrl Pts',(-0.99607720612092,25.3252086182976,
0.));
#245266=CARTESIAN_POINT('Ctrl Pts',(-0.99607720612092,25.3252086182976,
12.));
#245267=CARTESIAN_POINT('Ctrl Pts',(-0.984815543004092,25.3494019441444,
0.));
#245268=CARTESIAN_POINT('Ctrl Pts',(-0.984815543004092,25.3494019441444,
12.));
#245269=CARTESIAN_POINT('Ctrl Pts',(-0.973466666000049,25.3736367778842,
0.));
#245270=CARTESIAN_POINT('Ctrl Pts',(-0.973466666000049,25.3736367778842,
12.));
#245271=CARTESIAN_POINT('Ctrl Pts',(-0.962030544502803,25.3979126089155,
0.));
#245272=CARTESIAN_POINT('Ctrl Pts',(-0.962030544502803,25.3979126089155,
12.));
#245273=CARTESIAN_POINT('Ctrl Pts',(-0.95050714859697,25.4222289223155,
0.));
#245274=CARTESIAN_POINT('Ctrl Pts',(-0.95050714859697,25.4222289223155,
12.));
#245275=CARTESIAN_POINT('Ctrl Pts',(-0.938896449495633,25.4465852044835,
0.));
#245276=CARTESIAN_POINT('Ctrl Pts',(-0.938896449495633,25.4465852044835,
12.));
#245277=CARTESIAN_POINT('Ctrl Pts',(-0.927198419885605,25.4709809474996,
0.));
#245278=CARTESIAN_POINT('Ctrl Pts',(-0.927198419885605,25.4709809474996,
12.));
#245279=CARTESIAN_POINT('Ctrl Pts',(-0.915413034335334,25.4954156541787,
0.));
#245280=CARTESIAN_POINT('Ctrl Pts',(-0.915413034335334,25.4954156541787,
12.));
#245281=CARTESIAN_POINT('Ctrl Pts',(-0.903540269651155,25.5198888424195,
0.));
#245282=CARTESIAN_POINT('Ctrl Pts',(-0.903540269651155,25.5198888424195,
12.));
#245283=CARTESIAN_POINT('Ctrl Pts',(-0.891580105349468,25.5444000508223,
0.));
#245284=CARTESIAN_POINT('Ctrl Pts',(-0.891580105349468,25.5444000508223,
12.));
#245285=CARTESIAN_POINT('Ctrl Pts',(-0.879532523835092,25.568948840818,
0.));
#245286=CARTESIAN_POINT('Ctrl Pts',(-0.879532523835092,25.568948840818,
12.));
#245287=CARTESIAN_POINT('Ctrl Pts',(-0.86739750933947,25.5935347843616,
0.));
#245288=CARTESIAN_POINT('Ctrl Pts',(-0.86739750933947,25.5935347843616,
12.));
#245289=CARTESIAN_POINT('Ctrl Pts',(-0.855175047037615,25.618157453608,
0.));
#245290=CARTESIAN_POINT('Ctrl Pts',(-0.855175047037615,25.618157453608,
12.));
#245291=CARTESIAN_POINT('Ctrl Pts',(-0.842865122121547,25.6428164100078,
0.));
#245292=CARTESIAN_POINT('Ctrl Pts',(-0.842865122121547,25.6428164100078,
12.));
#245293=CARTESIAN_POINT('Ctrl Pts',(-0.830467718864369,25.6675111931957,
0.));
#245294=CARTESIAN_POINT('Ctrl Pts',(-0.830467718864369,25.6675111931957,
12.));
#245295=CARTESIAN_POINT('Ctrl Pts',(-0.81798281978672,25.6922413110172,
0.));
#245296=CARTESIAN_POINT('Ctrl Pts',(-0.81798281978672,25.6922413110172,
12.));
#245297=CARTESIAN_POINT('Ctrl Pts',(-0.805410404552596,25.7170062262474,
0.));
#245298=CARTESIAN_POINT('Ctrl Pts',(-0.805410404552596,25.7170062262474,
12.));
#245299=CARTESIAN_POINT('Ctrl Pts',(-0.792750451613536,25.7418053757671,
0.));
#245300=CARTESIAN_POINT('Ctrl Pts',(-0.792750451613536,25.7418053757671,
12.));
#245301=CARTESIAN_POINT('Ctrl Pts',(-0.780002940289027,25.7666381946871,
0.));
#245302=CARTESIAN_POINT('Ctrl Pts',(-0.780002940289027,25.7666381946871,
12.));
#245303=CARTESIAN_POINT('Ctrl Pts',(-0.767167852648641,25.7915041383304,
0.));
#245304=CARTESIAN_POINT('Ctrl Pts',(-0.767167852648641,25.7915041383304,
12.));
#245305=CARTESIAN_POINT('Ctrl Pts',(-0.75424517560829,25.816402705995,0.));
#245306=CARTESIAN_POINT('Ctrl Pts',(-0.75424517560829,25.816402705995,12.));
#245307=CARTESIAN_POINT('Ctrl Pts',(-0.741234902664698,25.841333461908,
0.));
#245308=CARTESIAN_POINT('Ctrl Pts',(-0.741234902664698,25.841333461908,
12.));
#245309=CARTESIAN_POINT('Ctrl Pts',(-0.728137036485879,25.8662960624285,
0.));
#245310=CARTESIAN_POINT('Ctrl Pts',(-0.728137036485879,25.8662960624285,
12.));
#245311=CARTESIAN_POINT('Ctrl Pts',(-0.714951588533753,25.8912902615141,
0.));
#245312=CARTESIAN_POINT('Ctrl Pts',(-0.714951588533753,25.8912902615141,
12.));
#245313=CARTESIAN_POINT('Ctrl Pts',(-0.701678575236603,25.9163158909645,
0.));
#245314=CARTESIAN_POINT('Ctrl Pts',(-0.701678575236603,25.9163158909645,
12.));
#245315=CARTESIAN_POINT('Ctrl Pts',(-0.688318015065679,25.941372847213,
0.));
#245316=CARTESIAN_POINT('Ctrl Pts',(-0.688318015065679,25.941372847213,
12.));
#245317=CARTESIAN_POINT('Ctrl Pts',(-0.677559543215903,25.9614434298092,
0.));
#245318=CARTESIAN_POINT('Ctrl Pts',(-0.677559543215903,25.9614434298092,
12.));
#245319=CARTESIAN_POINT('Ctrl Pts',(-0.669451306784418,25.9765104298171,
0.));
#245320=CARTESIAN_POINT('Ctrl Pts',(-0.669451306784418,25.9765104298171,
12.));
#245321=CARTESIAN_POINT('Ctrl Pts',(-0.664028313188914,25.9865613464809,
0.));
#245322=CARTESIAN_POINT('Ctrl Pts',(-0.664028313188914,25.9865613464809,
12.));
#245323=CARTESIAN_POINT('Ctrl Pts',(-0.661312440730891,25.991588367311,
0.));
#245324=CARTESIAN_POINT('Ctrl Pts',(-0.661312440730891,25.991588367311,
12.));
#245325=CARTESIAN_POINT('',(-0.661312440730891,25.991588367311,0.));
#245326=CARTESIAN_POINT('Ctrl Pts',(-1.76341220531179,22.4835757167854,
0.));
#245327=CARTESIAN_POINT('Ctrl Pts',(-1.76341415538764,22.483581992979,0.));
#245328=CARTESIAN_POINT('Ctrl Pts',(-1.7634206426357,22.4836387052232,0.));
#245329=CARTESIAN_POINT('Ctrl Pts',(-1.76343813434565,22.483856251707,0.));
#245330=CARTESIAN_POINT('Ctrl Pts',(-1.76347698284792,22.4844112933129,
0.));
#245331=CARTESIAN_POINT('Ctrl Pts',(-1.76355076045546,22.4855446605991,
0.));
#245332=CARTESIAN_POINT('Ctrl Pts',(-1.76364784232963,22.4871115206571,
0.));
#245333=CARTESIAN_POINT('Ctrl Pts',(-1.76376424879505,22.4890991659478,
0.));
#245334=CARTESIAN_POINT('Ctrl Pts',(-1.76389475965724,22.4914909094908,
0.));
#245335=CARTESIAN_POINT('Ctrl Pts',(-1.76403393880301,22.4942693792449,
0.));
#245336=CARTESIAN_POINT('Ctrl Pts',(-1.76417731243462,22.4974203063191,
0.));
#245337=CARTESIAN_POINT('Ctrl Pts',(-1.76432160068725,22.5009332677316,
0.));
#245338=CARTESIAN_POINT('Ctrl Pts',(-1.76446408210366,22.5047996391978,
0.));
#245339=CARTESIAN_POINT('Ctrl Pts',(-1.76460218257323,22.5090112700212,
0.));
#245340=CARTESIAN_POINT('Ctrl Pts',(-1.76473303281159,22.5135590569554,
0.));
#245341=CARTESIAN_POINT('Ctrl Pts',(-1.76485369319896,22.5184336670207,
0.));
#245342=CARTESIAN_POINT('Ctrl Pts',(-1.76496128643369,22.5236259635515,
0.));
#245343=CARTESIAN_POINT('Ctrl Pts',(-1.76505320262752,22.529127665298,0.));
#245344=CARTESIAN_POINT('Ctrl Pts',(-1.7651271156325,22.5349313983571,0.));
#245345=CARTESIAN_POINT('Ctrl Pts',(-1.76518087841493,22.5410303590891,
0.));
#245346=CARTESIAN_POINT('Ctrl Pts',(-1.76521245524047,22.5474180954006,
0.));
#245347=CARTESIAN_POINT('Ctrl Pts',(-1.76521983384063,22.5540882235837,
0.));
#245348=CARTESIAN_POINT('Ctrl Pts',(-1.76520104500449,22.5610344912501,
0.));
#245349=CARTESIAN_POINT('Ctrl Pts',(-1.76515418518829,22.5682508499873,
0.));
#245350=CARTESIAN_POINT('Ctrl Pts',(-1.76507744026747,22.5757315316355,
0.));
#245351=CARTESIAN_POINT('Ctrl Pts',(-1.76496910283088,22.5834711038024,
0.));
#245352=CARTESIAN_POINT('Ctrl Pts',(-1.76482755288411,22.5914644078106,
0.));
#245353=CARTESIAN_POINT('Ctrl Pts',(-1.76465124413556,22.5997065145638,
0.));
#245354=CARTESIAN_POINT('Ctrl Pts',(-1.76443868648015,22.6081926681342,
0.));
#245355=CARTESIAN_POINT('Ctrl Pts',(-1.76418843543739,22.6169182517693,
0.));
#245356=CARTESIAN_POINT('Ctrl Pts',(-1.76389909571402,22.6258787994847,
0.));
#245357=CARTESIAN_POINT('Ctrl Pts',(-1.76356932176272,22.635069997936,0.));
#245358=CARTESIAN_POINT('Ctrl Pts',(-1.76319782013914,22.6444876940425,
0.));
#245359=CARTESIAN_POINT('Ctrl Pts',(-1.76278334912559,22.6541278938413,
0.));
#245360=CARTESIAN_POINT('Ctrl Pts',(-1.76232471392567,22.6639867471756,
0.));
#245361=CARTESIAN_POINT('Ctrl Pts',(-1.76182076289525,22.6740605356699,
0.));
#245362=CARTESIAN_POINT('Ctrl Pts',(-1.76127038310613,22.6843456585245,
0.));
#245363=CARTESIAN_POINT('Ctrl Pts',(-1.76067249704884,22.6948386219843,
0.));
#245364=CARTESIAN_POINT('Ctrl Pts',(-1.76002606202399,22.7055360375481,
0.));
#245365=CARTESIAN_POINT('Ctrl Pts',(-1.75933006905924,22.7164346186007,
0.));
#245366=CARTESIAN_POINT('Ctrl Pts',(-1.75858354204635,22.7275311777305,
0.));
#245367=CARTESIAN_POINT('Ctrl Pts',(-1.75778553673249,22.7388226235565,
0.));
#245368=CARTESIAN_POINT('Ctrl Pts',(-1.75693513908911,22.7503059556455,
0.));
#245369=CARTESIAN_POINT('Ctrl Pts',(-1.7560314637164,22.7619782595013,0.));
#245370=CARTESIAN_POINT('Ctrl Pts',(-1.75507365227127,22.7738367016115,
0.));
#245371=CARTESIAN_POINT('Ctrl Pts',(-1.7540608718293,22.7858785242358,0.));
#245372=CARTESIAN_POINT('Ctrl Pts',(-1.75299231391461,22.7981010424312,
0.));
#245373=CARTESIAN_POINT('Ctrl Pts',(-1.7518671936559,22.8105016414712,0.));
#245374=CARTESIAN_POINT('Ctrl Pts',(-1.75068474890884,22.8230777741285,
0.));
#245375=CARTESIAN_POINT('Ctrl Pts',(-1.74944423940117,22.8358269579854,
0.));
#245376=CARTESIAN_POINT('Ctrl Pts',(-1.74814494588492,22.8487467728075,
0.));
#245377=CARTESIAN_POINT('Ctrl Pts',(-1.74678616930663,22.8618348580234,
0.));
#245378=CARTESIAN_POINT('Ctrl Pts',(-1.745367229982,22.8750889101696,0.));
#245379=CARTESIAN_POINT('Ctrl Pts',(-1.74388746677702,22.8885066803351,
0.));
#245380=CARTESIAN_POINT('Ctrl Pts',(-1.74234623630079,22.9020859716144,
0.));
#245381=CARTESIAN_POINT('Ctrl Pts',(-1.74074291231057,22.9158246373365,
0.));
#245382=CARTESIAN_POINT('Ctrl Pts',(-1.73907688511664,22.9297205792587,
0.));
#245383=CARTESIAN_POINT('Ctrl Pts',(-1.73734756100038,22.9437717457825,
0.));
#245384=CARTESIAN_POINT('Ctrl Pts',(-1.73555436162771,22.9579761301062,
0.));
#245385=CARTESIAN_POINT('Ctrl Pts',(-1.73369672350818,22.9723317685688,
0.));
#245386=CARTESIAN_POINT('Ctrl Pts',(-1.73177409750194,22.9868367391978,
0.));
#245387=CARTESIAN_POINT('Ctrl Pts',(-1.72978594832137,23.0014891601891,
0.));
#245388=CARTESIAN_POINT('Ctrl Pts',(-1.72773175404703,23.0162871884167,
0.));
#245389=CARTESIAN_POINT('Ctrl Pts',(-1.72561100564033,23.031229017888,0.));
#245390=CARTESIAN_POINT('Ctrl Pts',(-1.72342320653731,23.0463128785528,
0.));
#245391=CARTESIAN_POINT('Ctrl Pts',(-1.7211678722598,23.061537035156,0.));
#245392=CARTESIAN_POINT('Ctrl Pts',(-1.71884453003027,23.0768997860709,
0.));
#245393=CARTESIAN_POINT('Ctrl Pts',(-1.71645271839311,23.0923994621216,
0.));
#245394=CARTESIAN_POINT('Ctrl Pts',(-1.71399198684725,23.1080344254291,
0.));
#245395=CARTESIAN_POINT('Ctrl Pts',(-1.71146189552192,23.1238030684929,
0.));
#245396=CARTESIAN_POINT('Ctrl Pts',(-1.7088620148546,23.1397038132358,0.));
#245397=CARTESIAN_POINT('Ctrl Pts',(-1.70619192527847,23.1557351100613,
0.));
#245398=CARTESIAN_POINT('Ctrl Pts',(-1.70345121691259,23.1718954368749,
0.));
#245399=CARTESIAN_POINT('Ctrl Pts',(-1.70063948926987,23.1881832981848,
0.));
#245400=CARTESIAN_POINT('Ctrl Pts',(-1.69775635099425,23.2045972243765,
0.));
#245401=CARTESIAN_POINT('Ctrl Pts',(-1.69480141959946,23.2211357709374,
0.));
#245402=CARTESIAN_POINT('Ctrl Pts',(-1.69177432121716,23.2377975177014,
0.));
#245403=CARTESIAN_POINT('Ctrl Pts',(-1.6886746903491,23.2545810680536,0.));
#245404=CARTESIAN_POINT('Ctrl Pts',(-1.68550216963275,23.2714850482245,
0.));
#245405=CARTESIAN_POINT('Ctrl Pts',(-1.68225640962181,23.2885081066949,
0.));
#245406=CARTESIAN_POINT('Ctrl Pts',(-1.67893706857123,23.3056489135611,
0.));
#245407=CARTESIAN_POINT('Ctrl Pts',(-1.67554381222987,23.3229061599145,
0.));
#245408=CARTESIAN_POINT('Ctrl Pts',(-1.67207631363905,23.3402785571866,
0.));
#245409=CARTESIAN_POINT('Ctrl Pts',(-1.66853425293978,23.3577648365747,
0.));
#245410=CARTESIAN_POINT('Ctrl Pts',(-1.66491731718864,23.375363748555,0.));
#245411=CARTESIAN_POINT('Ctrl Pts',(-1.66122520018008,23.3930740623622,
0.));
#245412=CARTESIAN_POINT('Ctrl Pts',(-1.65745760227507,23.4108945654803,
0.));
#245413=CARTESIAN_POINT('Ctrl Pts',(-1.6536142302373,23.4288240631034,0.));
#245414=CARTESIAN_POINT('Ctrl Pts',(-1.6496947970734,23.446861377656,0.));
#245415=CARTESIAN_POINT('Ctrl Pts',(-1.64569902187608,23.4650053483919,
0.));
#245416=CARTESIAN_POINT('Ctrl Pts',(-1.64162662967525,23.4832548309638,
0.));
#245417=CARTESIAN_POINT('Ctrl Pts',(-1.63747735129474,23.5016086970006,
0.));
#245418=CARTESIAN_POINT('Ctrl Pts',(-1.63325092321731,23.5200658336624,
0.));
#245419=CARTESIAN_POINT('Ctrl Pts',(-1.62894708745231,23.5386251432278,
0.));
#245420=CARTESIAN_POINT('Ctrl Pts',(-1.62456559140072,23.5572855427617,
0.));
#245421=CARTESIAN_POINT('Ctrl Pts',(-1.62010618772869,23.5760459637608,
0.));
#245422=CARTESIAN_POINT('Ctrl Pts',(-1.61556863424697,23.5949053517996,
0.));
#245423=CARTESIAN_POINT('Ctrl Pts',(-1.61095269379773,23.6138626661644,
0.));
#245424=CARTESIAN_POINT('Ctrl Pts',(-1.60625813414666,23.6329168794916,
0.));
#245425=CARTESIAN_POINT('Ctrl Pts',(-1.60148472786588,23.6520669774863,
0.));
#245426=CARTESIAN_POINT('Ctrl Pts',(-1.59663225222458,23.6713119586302,
0.));
#245427=CARTESIAN_POINT('Ctrl Pts',(-1.59170048908632,23.6906508338833,
0.));
#245428=CARTESIAN_POINT('Ctrl Pts',(-1.58668922481222,23.7100826263835,
0.));
#245429=CARTESIAN_POINT('Ctrl Pts',(-1.58159825017362,23.7296063711308,
0.));
#245430=CARTESIAN_POINT('Ctrl Pts',(-1.57642736025251,23.7492211147369,
0.));
#245431=CARTESIAN_POINT('Ctrl Pts',(-1.57117635434412,23.7689259151869,
0.));
#245432=CARTESIAN_POINT('Ctrl Pts',(-1.56584503586844,23.788719841588,0.));
#245433=CARTESIAN_POINT('Ctrl Pts',(-1.56043321228631,23.8086019739192,
0.));
#245434=CARTESIAN_POINT('Ctrl Pts',(-1.55494069502628,23.8285714027631,
0.));
#245435=CARTESIAN_POINT('Ctrl Pts',(-1.5493672994053,23.8486272290698,0.));
#245436=CARTESIAN_POINT('Ctrl Pts',(-1.54371284453978,23.8687685639635,
0.));
#245437=CARTESIAN_POINT('Ctrl Pts',(-1.53797715326748,23.8889945285313,
0.));
#245438=CARTESIAN_POINT('Ctrl Pts',(-1.53216005207462,23.9093042536119,
0.));
#245439=CARTESIAN_POINT('Ctrl Pts',(-1.5262613710304,23.9296968795761,0.));
#245440=CARTESIAN_POINT('Ctrl Pts',(-1.52028094372806,23.9501715561038,
0.));
#245441=CARTESIAN_POINT('Ctrl Pts',(-1.51421860720628,23.9707274420145,
0.));
#245442=CARTESIAN_POINT('Ctrl Pts',(-1.50807420187703,23.991363705093,0.));
#245443=CARTESIAN_POINT('Ctrl Pts',(-1.50184757146099,24.0120795219086,
0.));
#245444=CARTESIAN_POINT('Ctrl Pts',(-1.49553856292798,24.0328740776331,
0.));
#245445=CARTESIAN_POINT('Ctrl Pts',(-1.48914702644883,24.053746565843,0.));
#245446=CARTESIAN_POINT('Ctrl Pts',(-1.4826728153368,24.074696188353,0.));
#245447=CARTESIAN_POINT('Ctrl Pts',(-1.47611578597741,24.0957221550782,
0.));
#245448=CARTESIAN_POINT('Ctrl Pts',(-1.46947579776992,24.1168236838827,
0.));
#245449=CARTESIAN_POINT('Ctrl Pts',(-1.46275271307398,24.1380000004272,
0.));
#245450=CARTESIAN_POINT('Ctrl Pts',(-1.45594639716314,24.1592503380105,
0.));
#245451=CARTESIAN_POINT('Ctrl Pts',(-1.44905671818721,24.1805739374033,
0.));
#245452=CARTESIAN_POINT('Ctrl Pts',(-1.44208354711074,24.2019700467214,
0.));
#245453=CARTESIAN_POINT('Ctrl Pts',(-1.43502675765502,24.2234379212978,
0.));
#245454=CARTESIAN_POINT('Ctrl Pts',(-1.42788622624851,24.2449768235485,
0.));
#245455=CARTESIAN_POINT('Ctrl Pts',(-1.42066183198252,24.2665860228357,
0.));
#245456=CARTESIAN_POINT('Ctrl Pts',(-1.41335345657685,24.2882647953214,
0.));
#245457=CARTESIAN_POINT('Ctrl Pts',(-1.40596098434341,24.3100124238316,
0.));
#245458=CARTESIAN_POINT('Ctrl Pts',(-1.3984843021281,24.3318281977647,0.));
#245459=CARTESIAN_POINT('Ctrl Pts',(-1.3909232992639,24.3537114129877,0.));
#245460=CARTESIAN_POINT('Ctrl Pts',(-1.38327786752998,24.37566137173,0.));
#245461=CARTESIAN_POINT('Ctrl Pts',(-1.37554790111608,24.3976773824731,
0.));
#245462=CARTESIAN_POINT('Ctrl Pts',(-1.36773329659954,24.4197587598337,
0.));
#245463=CARTESIAN_POINT('Ctrl Pts',(-1.35983395290624,24.4419048244524,
0.));
#245464=CARTESIAN_POINT('Ctrl Pts',(-1.35184977125645,24.4641149028894,
0.));
#245465=CARTESIAN_POINT('Ctrl Pts',(-1.34378065512335,24.4863883275135,
0.));
#245466=CARTESIAN_POINT('Ctrl Pts',(-1.33562651019684,24.5087244363856,
0.));
#245467=CARTESIAN_POINT('Ctrl Pts',(-1.32738724435326,24.5311225731434,
0.));
#245468=CARTESIAN_POINT('Ctrl Pts',(-1.31906276763669,24.5535820868671,
0.));
#245469=CARTESIAN_POINT('Ctrl Pts',(-1.31065299222023,24.576102332018,0.));
#245470=CARTESIAN_POINT('Ctrl Pts',(-1.30215783236364,24.5986826684025,
0.));
#245471=CARTESIAN_POINT('Ctrl Pts',(-1.29357720438108,24.6213224611228,
0.));
#245472=CARTESIAN_POINT('Ctrl Pts',(-1.28491102661514,24.6440210805278,
0.));
#245473=CARTESIAN_POINT('Ctrl Pts',(-1.2761592194164,24.666777902156,0.));
#245474=CARTESIAN_POINT('Ctrl Pts',(-1.26732170513497,24.6895923066837,
0.));
#245475=CARTESIAN_POINT('Ctrl Pts',(-1.25839840807415,24.7124636797895,
0.));
#245476=CARTESIAN_POINT('Ctrl Pts',(-1.24938925444324,24.7353914120012,
0.));
#245477=CARTESIAN_POINT('Ctrl Pts',(-1.24029417231988,24.7583748985439,
0.));
#245478=CARTESIAN_POINT('Ctrl Pts',(-1.23111309161843,24.78141353918,0.));
#245479=CARTESIAN_POINT('Ctrl Pts',(-1.22184594406526,24.8045067380536,
0.));
#245480=CARTESIAN_POINT('Ctrl Pts',(-1.21249266318205,24.8276539035092,
0.));
#245481=CARTESIAN_POINT('Ctrl Pts',(-1.20305318426015,24.8508544481973,
0.));
#245482=CARTESIAN_POINT('Ctrl Pts',(-1.19352744434059,24.8741077892074,
0.));
#245483=CARTESIAN_POINT('Ctrl Pts',(-1.18391538220098,24.8974133481829,
0.));
#245484=CARTESIAN_POINT('Ctrl Pts',(-1.17421693835039,24.9207705514449,
0.));
#245485=CARTESIAN_POINT('Ctrl Pts',(-1.16443205502852,24.9441788300932,
0.));
#245486=CARTESIAN_POINT('Ctrl Pts',(-1.15456067621894,24.9676376201501,
0.));
#245487=CARTESIAN_POINT('Ctrl Pts',(-1.14460274758206,24.9911463621431,
0.));
#245488=CARTESIAN_POINT('Ctrl Pts',(-1.13455821638536,25.0147045006193,
0.));
#245489=CARTESIAN_POINT('Ctrl Pts',(-1.12442703144455,25.0383114836898,
0.));
#245490=CARTESIAN_POINT('Ctrl Pts',(-1.1142091430689,25.0619667625336,0.));
#245491=CARTESIAN_POINT('Ctrl Pts',(-1.1039045030174,25.085669790968,0.));
#245492=CARTESIAN_POINT('Ctrl Pts',(-1.09351306445299,25.1094200248448,
0.));
#245493=CARTESIAN_POINT('Ctrl Pts',(-1.08303478197174,25.1332169227415,
0.));
#245494=CARTESIAN_POINT('Ctrl Pts',(-1.0724696116546,25.1570599469311,0.));
#245495=CARTESIAN_POINT('Ctrl Pts',(-1.06181751111754,25.1809485642191,
0.));
#245496=CARTESIAN_POINT('Ctrl Pts',(-1.05107843957926,25.2048822469027,
0.));
#245497=CARTESIAN_POINT('Ctrl Pts',(-1.04025235791515,25.2288604735087,
0.));
#245498=CARTESIAN_POINT('Ctrl Pts',(-1.0293392287683,25.2528827300427,0.));
#245499=CARTESIAN_POINT('Ctrl Pts',(-1.01833901642272,25.2769485087268,
0.));
#245500=CARTESIAN_POINT('Ctrl Pts',(-1.00725168656934,25.3010573055557,
0.));
#245501=CARTESIAN_POINT('Ctrl Pts',(-0.99607720612092,25.3252086182976,
0.));
#245502=CARTESIAN_POINT('Ctrl Pts',(-0.984815543004092,25.3494019441444,
0.));
#245503=CARTESIAN_POINT('Ctrl Pts',(-0.973466666000049,25.3736367778842,
0.));
#245504=CARTESIAN_POINT('Ctrl Pts',(-0.962030544502803,25.3979126089155,
0.));
#245505=CARTESIAN_POINT('Ctrl Pts',(-0.95050714859697,25.4222289223155,
0.));
#245506=CARTESIAN_POINT('Ctrl Pts',(-0.938896449495633,25.4465852044835,
0.));
#245507=CARTESIAN_POINT('Ctrl Pts',(-0.927198419885605,25.4709809474996,
0.));
#245508=CARTESIAN_POINT('Ctrl Pts',(-0.915413034335334,25.4954156541787,
0.));
#245509=CARTESIAN_POINT('Ctrl Pts',(-0.903540269651155,25.5198888424195,
0.));
#245510=CARTESIAN_POINT('Ctrl Pts',(-0.891580105349468,25.5444000508223,
0.));
#245511=CARTESIAN_POINT('Ctrl Pts',(-0.879532523835092,25.568948840818,
0.));
#245512=CARTESIAN_POINT('Ctrl Pts',(-0.86739750933947,25.5935347843616,
0.));
#245513=CARTESIAN_POINT('Ctrl Pts',(-0.855175047037615,25.618157453608,
0.));
#245514=CARTESIAN_POINT('Ctrl Pts',(-0.842865122121547,25.6428164100078,
0.));
#245515=CARTESIAN_POINT('Ctrl Pts',(-0.830467718864369,25.6675111931957,
0.));
#245516=CARTESIAN_POINT('Ctrl Pts',(-0.81798281978672,25.6922413110172,
0.));
#245517=CARTESIAN_POINT('Ctrl Pts',(-0.805410404552596,25.7170062262474,
0.));
#245518=CARTESIAN_POINT('Ctrl Pts',(-0.792750451613536,25.7418053757671,
0.));
#245519=CARTESIAN_POINT('Ctrl Pts',(-0.780002940289027,25.7666381946871,
0.));
#245520=CARTESIAN_POINT('Ctrl Pts',(-0.767167852648641,25.7915041383304,
0.));
#245521=CARTESIAN_POINT('Ctrl Pts',(-0.75424517560829,25.816402705995,0.));
#245522=CARTESIAN_POINT('Ctrl Pts',(-0.741234902664698,25.841333461908,
0.));
#245523=CARTESIAN_POINT('Ctrl Pts',(-0.728137036485879,25.8662960624285,
0.));
#245524=CARTESIAN_POINT('Ctrl Pts',(-0.714951588533753,25.8912902615141,
0.));
#245525=CARTESIAN_POINT('Ctrl Pts',(-0.701678575236603,25.9163158909645,
0.));
#245526=CARTESIAN_POINT('Ctrl Pts',(-0.688318015065679,25.941372847213,
0.));
#245527=CARTESIAN_POINT('Ctrl Pts',(-0.677559543215903,25.9614434298092,
0.));
#245528=CARTESIAN_POINT('Ctrl Pts',(-0.669451306784418,25.9765104298171,
0.));
#245529=CARTESIAN_POINT('Ctrl Pts',(-0.664028313188914,25.9865613464809,
0.));
#245530=CARTESIAN_POINT('Ctrl Pts',(-0.661312440730891,25.991588367311,
0.));
#245531=CARTESIAN_POINT('',(-0.661312440730891,25.991588367311,12.));
#245532=CARTESIAN_POINT('Ctrl Pts',(-0.661312440730891,25.991588367311,
12.));
#245533=CARTESIAN_POINT('Ctrl Pts',(-0.664028313188914,25.9865613464809,
12.));
#245534=CARTESIAN_POINT('Ctrl Pts',(-0.669451306784418,25.9765104298171,
12.));
#245535=CARTESIAN_POINT('Ctrl Pts',(-0.677559543215903,25.9614434298092,
12.));
#245536=CARTESIAN_POINT('Ctrl Pts',(-0.688318015065679,25.941372847213,
12.));
#245537=CARTESIAN_POINT('Ctrl Pts',(-0.701678575236603,25.9163158909645,
12.));
#245538=CARTESIAN_POINT('Ctrl Pts',(-0.714951588533753,25.8912902615141,
12.));
#245539=CARTESIAN_POINT('Ctrl Pts',(-0.728137036485879,25.8662960624285,
12.));
#245540=CARTESIAN_POINT('Ctrl Pts',(-0.741234902664698,25.841333461908,
12.));
#245541=CARTESIAN_POINT('Ctrl Pts',(-0.75424517560829,25.816402705995,12.));
#245542=CARTESIAN_POINT('Ctrl Pts',(-0.767167852648641,25.7915041383304,
12.));
#245543=CARTESIAN_POINT('Ctrl Pts',(-0.780002940289027,25.7666381946871,
12.));
#245544=CARTESIAN_POINT('Ctrl Pts',(-0.792750451613536,25.7418053757671,
12.));
#245545=CARTESIAN_POINT('Ctrl Pts',(-0.805410404552596,25.7170062262474,
12.));
#245546=CARTESIAN_POINT('Ctrl Pts',(-0.81798281978672,25.6922413110172,
12.));
#245547=CARTESIAN_POINT('Ctrl Pts',(-0.830467718864369,25.6675111931957,
12.));
#245548=CARTESIAN_POINT('Ctrl Pts',(-0.842865122121547,25.6428164100078,
12.));
#245549=CARTESIAN_POINT('Ctrl Pts',(-0.855175047037615,25.618157453608,
12.));
#245550=CARTESIAN_POINT('Ctrl Pts',(-0.86739750933947,25.5935347843616,
12.));
#245551=CARTESIAN_POINT('Ctrl Pts',(-0.879532523835092,25.568948840818,
12.));
#245552=CARTESIAN_POINT('Ctrl Pts',(-0.891580105349468,25.5444000508223,
12.));
#245553=CARTESIAN_POINT('Ctrl Pts',(-0.903540269651155,25.5198888424195,
12.));
#245554=CARTESIAN_POINT('Ctrl Pts',(-0.915413034335334,25.4954156541787,
12.));
#245555=CARTESIAN_POINT('Ctrl Pts',(-0.927198419885605,25.4709809474996,
12.));
#245556=CARTESIAN_POINT('Ctrl Pts',(-0.938896449495633,25.4465852044835,
12.));
#245557=CARTESIAN_POINT('Ctrl Pts',(-0.95050714859697,25.4222289223155,
12.));
#245558=CARTESIAN_POINT('Ctrl Pts',(-0.962030544502803,25.3979126089155,
12.));
#245559=CARTESIAN_POINT('Ctrl Pts',(-0.973466666000049,25.3736367778842,
12.));
#245560=CARTESIAN_POINT('Ctrl Pts',(-0.984815543004092,25.3494019441444,
12.));
#245561=CARTESIAN_POINT('Ctrl Pts',(-0.99607720612092,25.3252086182976,
12.));
#245562=CARTESIAN_POINT('Ctrl Pts',(-1.00725168656934,25.3010573055557,
12.));
#245563=CARTESIAN_POINT('Ctrl Pts',(-1.01833901642272,25.2769485087268,
12.));
#245564=CARTESIAN_POINT('Ctrl Pts',(-1.0293392287683,25.2528827300427,12.));
#245565=CARTESIAN_POINT('Ctrl Pts',(-1.04025235791515,25.2288604735087,
12.));
#245566=CARTESIAN_POINT('Ctrl Pts',(-1.05107843957926,25.2048822469027,
12.));
#245567=CARTESIAN_POINT('Ctrl Pts',(-1.06181751111754,25.1809485642191,
12.));
#245568=CARTESIAN_POINT('Ctrl Pts',(-1.0724696116546,25.1570599469311,12.));
#245569=CARTESIAN_POINT('Ctrl Pts',(-1.08303478197174,25.1332169227415,
12.));
#245570=CARTESIAN_POINT('Ctrl Pts',(-1.09351306445299,25.1094200248448,
12.));
#245571=CARTESIAN_POINT('Ctrl Pts',(-1.1039045030174,25.085669790968,12.));
#245572=CARTESIAN_POINT('Ctrl Pts',(-1.1142091430689,25.0619667625336,12.));
#245573=CARTESIAN_POINT('Ctrl Pts',(-1.12442703144455,25.0383114836898,
12.));
#245574=CARTESIAN_POINT('Ctrl Pts',(-1.13455821638536,25.0147045006193,
12.));
#245575=CARTESIAN_POINT('Ctrl Pts',(-1.14460274758206,24.9911463621431,
12.));
#245576=CARTESIAN_POINT('Ctrl Pts',(-1.15456067621894,24.9676376201501,
12.));
#245577=CARTESIAN_POINT('Ctrl Pts',(-1.16443205502852,24.9441788300932,
12.));
#245578=CARTESIAN_POINT('Ctrl Pts',(-1.17421693835039,24.9207705514449,
12.));
#245579=CARTESIAN_POINT('Ctrl Pts',(-1.18391538220098,24.8974133481829,
12.));
#245580=CARTESIAN_POINT('Ctrl Pts',(-1.19352744434059,24.8741077892074,
12.));
#245581=CARTESIAN_POINT('Ctrl Pts',(-1.20305318426015,24.8508544481973,
12.));
#245582=CARTESIAN_POINT('Ctrl Pts',(-1.21249266318205,24.8276539035092,
12.));
#245583=CARTESIAN_POINT('Ctrl Pts',(-1.22184594406526,24.8045067380536,
12.));
#245584=CARTESIAN_POINT('Ctrl Pts',(-1.23111309161843,24.78141353918,12.));
#245585=CARTESIAN_POINT('Ctrl Pts',(-1.24029417231988,24.7583748985439,
12.));
#245586=CARTESIAN_POINT('Ctrl Pts',(-1.24938925444324,24.7353914120012,
12.));
#245587=CARTESIAN_POINT('Ctrl Pts',(-1.25839840807415,24.7124636797895,
12.));
#245588=CARTESIAN_POINT('Ctrl Pts',(-1.26732170513497,24.6895923066837,
12.));
#245589=CARTESIAN_POINT('Ctrl Pts',(-1.2761592194164,24.666777902156,12.));
#245590=CARTESIAN_POINT('Ctrl Pts',(-1.28491102661514,24.6440210805278,
12.));
#245591=CARTESIAN_POINT('Ctrl Pts',(-1.29357720438108,24.6213224611228,
12.));
#245592=CARTESIAN_POINT('Ctrl Pts',(-1.30215783236364,24.5986826684025,
12.));
#245593=CARTESIAN_POINT('Ctrl Pts',(-1.31065299222023,24.576102332018,12.));
#245594=CARTESIAN_POINT('Ctrl Pts',(-1.31906276763669,24.5535820868671,
12.));
#245595=CARTESIAN_POINT('Ctrl Pts',(-1.32738724435326,24.5311225731434,
12.));
#245596=CARTESIAN_POINT('Ctrl Pts',(-1.33562651019684,24.5087244363856,
12.));
#245597=CARTESIAN_POINT('Ctrl Pts',(-1.34378065512335,24.4863883275135,
12.));
#245598=CARTESIAN_POINT('Ctrl Pts',(-1.35184977125645,24.4641149028894,
12.));
#245599=CARTESIAN_POINT('Ctrl Pts',(-1.35983395290624,24.4419048244524,
12.));
#245600=CARTESIAN_POINT('Ctrl Pts',(-1.36773329659954,24.4197587598337,
12.));
#245601=CARTESIAN_POINT('Ctrl Pts',(-1.37554790111608,24.3976773824731,
12.));
#245602=CARTESIAN_POINT('Ctrl Pts',(-1.38327786752998,24.37566137173,12.));
#245603=CARTESIAN_POINT('Ctrl Pts',(-1.3909232992639,24.3537114129877,12.));
#245604=CARTESIAN_POINT('Ctrl Pts',(-1.3984843021281,24.3318281977647,12.));
#245605=CARTESIAN_POINT('Ctrl Pts',(-1.40596098434341,24.3100124238316,
12.));
#245606=CARTESIAN_POINT('Ctrl Pts',(-1.41335345657685,24.2882647953214,
12.));
#245607=CARTESIAN_POINT('Ctrl Pts',(-1.42066183198252,24.2665860228357,
12.));
#245608=CARTESIAN_POINT('Ctrl Pts',(-1.42788622624851,24.2449768235485,
12.));
#245609=CARTESIAN_POINT('Ctrl Pts',(-1.43502675765502,24.2234379212978,
12.));
#245610=CARTESIAN_POINT('Ctrl Pts',(-1.44208354711074,24.2019700467214,
12.));
#245611=CARTESIAN_POINT('Ctrl Pts',(-1.44905671818721,24.1805739374033,
12.));
#245612=CARTESIAN_POINT('Ctrl Pts',(-1.45594639716314,24.1592503380105,
12.));
#245613=CARTESIAN_POINT('Ctrl Pts',(-1.46275271307398,24.1380000004272,
12.));
#245614=CARTESIAN_POINT('Ctrl Pts',(-1.46947579776992,24.1168236838827,
12.));
#245615=CARTESIAN_POINT('Ctrl Pts',(-1.47611578597741,24.0957221550782,
12.));
#245616=CARTESIAN_POINT('Ctrl Pts',(-1.4826728153368,24.074696188353,12.));
#245617=CARTESIAN_POINT('Ctrl Pts',(-1.48914702644883,24.053746565843,12.));
#245618=CARTESIAN_POINT('Ctrl Pts',(-1.49553856292798,24.0328740776331,
12.));
#245619=CARTESIAN_POINT('Ctrl Pts',(-1.50184757146099,24.0120795219086,
12.));
#245620=CARTESIAN_POINT('Ctrl Pts',(-1.50807420187703,23.991363705093,12.));
#245621=CARTESIAN_POINT('Ctrl Pts',(-1.51421860720628,23.9707274420145,
12.));
#245622=CARTESIAN_POINT('Ctrl Pts',(-1.52028094372806,23.9501715561038,
12.));
#245623=CARTESIAN_POINT('Ctrl Pts',(-1.5262613710304,23.9296968795761,12.));
#245624=CARTESIAN_POINT('Ctrl Pts',(-1.53216005207462,23.9093042536119,
12.));
#245625=CARTESIAN_POINT('Ctrl Pts',(-1.53797715326748,23.8889945285313,
12.));
#245626=CARTESIAN_POINT('Ctrl Pts',(-1.54371284453978,23.8687685639635,
12.));
#245627=CARTESIAN_POINT('Ctrl Pts',(-1.5493672994053,23.8486272290698,12.));
#245628=CARTESIAN_POINT('Ctrl Pts',(-1.55494069502628,23.8285714027631,
12.));
#245629=CARTESIAN_POINT('Ctrl Pts',(-1.56043321228631,23.8086019739192,
12.));
#245630=CARTESIAN_POINT('Ctrl Pts',(-1.56584503586844,23.788719841588,12.));
#245631=CARTESIAN_POINT('Ctrl Pts',(-1.57117635434412,23.7689259151869,
12.));
#245632=CARTESIAN_POINT('Ctrl Pts',(-1.57642736025251,23.7492211147369,
12.));
#245633=CARTESIAN_POINT('Ctrl Pts',(-1.58159825017362,23.7296063711308,
12.));
#245634=CARTESIAN_POINT('Ctrl Pts',(-1.58668922481222,23.7100826263835,
12.));
#245635=CARTESIAN_POINT('Ctrl Pts',(-1.59170048908632,23.6906508338833,
12.));
#245636=CARTESIAN_POINT('Ctrl Pts',(-1.59663225222458,23.6713119586302,
12.));
#245637=CARTESIAN_POINT('Ctrl Pts',(-1.60148472786588,23.6520669774863,
12.));
#245638=CARTESIAN_POINT('Ctrl Pts',(-1.60625813414666,23.6329168794916,
12.));
#245639=CARTESIAN_POINT('Ctrl Pts',(-1.61095269379773,23.6138626661644,
12.));
#245640=CARTESIAN_POINT('Ctrl Pts',(-1.61556863424697,23.5949053517996,
12.));
#245641=CARTESIAN_POINT('Ctrl Pts',(-1.62010618772869,23.5760459637608,
12.));
#245642=CARTESIAN_POINT('Ctrl Pts',(-1.62456559140072,23.5572855427617,
12.));
#245643=CARTESIAN_POINT('Ctrl Pts',(-1.62894708745231,23.5386251432278,
12.));
#245644=CARTESIAN_POINT('Ctrl Pts',(-1.63325092321731,23.5200658336624,
12.));
#245645=CARTESIAN_POINT('Ctrl Pts',(-1.63747735129474,23.5016086970006,
12.));
#245646=CARTESIAN_POINT('Ctrl Pts',(-1.64162662967525,23.4832548309638,
12.));
#245647=CARTESIAN_POINT('Ctrl Pts',(-1.64569902187608,23.4650053483919,
12.));
#245648=CARTESIAN_POINT('Ctrl Pts',(-1.6496947970734,23.446861377656,12.));
#245649=CARTESIAN_POINT('Ctrl Pts',(-1.6536142302373,23.4288240631034,12.));
#245650=CARTESIAN_POINT('Ctrl Pts',(-1.65745760227507,23.4108945654803,
12.));
#245651=CARTESIAN_POINT('Ctrl Pts',(-1.66122520018008,23.3930740623622,
12.));
#245652=CARTESIAN_POINT('Ctrl Pts',(-1.66491731718864,23.375363748555,12.));
#245653=CARTESIAN_POINT('Ctrl Pts',(-1.66853425293978,23.3577648365747,
12.));
#245654=CARTESIAN_POINT('Ctrl Pts',(-1.67207631363905,23.3402785571866,
12.));
#245655=CARTESIAN_POINT('Ctrl Pts',(-1.67554381222987,23.3229061599145,
12.));
#245656=CARTESIAN_POINT('Ctrl Pts',(-1.67893706857123,23.3056489135611,
12.));
#245657=CARTESIAN_POINT('Ctrl Pts',(-1.68225640962181,23.2885081066949,
12.));
#245658=CARTESIAN_POINT('Ctrl Pts',(-1.68550216963275,23.2714850482245,
12.));
#245659=CARTESIAN_POINT('Ctrl Pts',(-1.6886746903491,23.2545810680536,12.));
#245660=CARTESIAN_POINT('Ctrl Pts',(-1.69177432121716,23.2377975177014,
12.));
#245661=CARTESIAN_POINT('Ctrl Pts',(-1.69480141959946,23.2211357709374,
12.));
#245662=CARTESIAN_POINT('Ctrl Pts',(-1.69775635099425,23.2045972243765,
12.));
#245663=CARTESIAN_POINT('Ctrl Pts',(-1.70063948926987,23.1881832981848,
12.));
#245664=CARTESIAN_POINT('Ctrl Pts',(-1.70345121691259,23.1718954368749,
12.));
#245665=CARTESIAN_POINT('Ctrl Pts',(-1.70619192527847,23.1557351100613,
12.));
#245666=CARTESIAN_POINT('Ctrl Pts',(-1.7088620148546,23.1397038132358,12.));
#245667=CARTESIAN_POINT('Ctrl Pts',(-1.71146189552192,23.1238030684929,
12.));
#245668=CARTESIAN_POINT('Ctrl Pts',(-1.71399198684725,23.1080344254291,
12.));
#245669=CARTESIAN_POINT('Ctrl Pts',(-1.71645271839311,23.0923994621216,
12.));
#245670=CARTESIAN_POINT('Ctrl Pts',(-1.71884453003027,23.0768997860709,
12.));
#245671=CARTESIAN_POINT('Ctrl Pts',(-1.7211678722598,23.061537035156,12.));
#245672=CARTESIAN_POINT('Ctrl Pts',(-1.72342320653731,23.0463128785528,
12.));
#245673=CARTESIAN_POINT('Ctrl Pts',(-1.72561100564033,23.031229017888,12.));
#245674=CARTESIAN_POINT('Ctrl Pts',(-1.72773175404703,23.0162871884167,
12.));
#245675=CARTESIAN_POINT('Ctrl Pts',(-1.72978594832137,23.0014891601891,
12.));
#245676=CARTESIAN_POINT('Ctrl Pts',(-1.73177409750194,22.9868367391978,
12.));
#245677=CARTESIAN_POINT('Ctrl Pts',(-1.73369672350818,22.9723317685688,
12.));
#245678=CARTESIAN_POINT('Ctrl Pts',(-1.73555436162771,22.9579761301062,
12.));
#245679=CARTESIAN_POINT('Ctrl Pts',(-1.73734756100038,22.9437717457825,
12.));
#245680=CARTESIAN_POINT('Ctrl Pts',(-1.73907688511664,22.9297205792587,
12.));
#245681=CARTESIAN_POINT('Ctrl Pts',(-1.74074291231057,22.9158246373365,
12.));
#245682=CARTESIAN_POINT('Ctrl Pts',(-1.74234623630079,22.9020859716144,
12.));
#245683=CARTESIAN_POINT('Ctrl Pts',(-1.74388746677702,22.8885066803351,
12.));
#245684=CARTESIAN_POINT('Ctrl Pts',(-1.745367229982,22.8750889101696,12.));
#245685=CARTESIAN_POINT('Ctrl Pts',(-1.74678616930663,22.8618348580234,
12.));
#245686=CARTESIAN_POINT('Ctrl Pts',(-1.74814494588492,22.8487467728075,
12.));
#245687=CARTESIAN_POINT('Ctrl Pts',(-1.74944423940117,22.8358269579854,
12.));
#245688=CARTESIAN_POINT('Ctrl Pts',(-1.75068474890884,22.8230777741285,
12.));
#245689=CARTESIAN_POINT('Ctrl Pts',(-1.7518671936559,22.8105016414712,12.));
#245690=CARTESIAN_POINT('Ctrl Pts',(-1.75299231391461,22.7981010424312,
12.));
#245691=CARTESIAN_POINT('Ctrl Pts',(-1.7540608718293,22.7858785242358,12.));
#245692=CARTESIAN_POINT('Ctrl Pts',(-1.75507365227127,22.7738367016115,
12.));
#245693=CARTESIAN_POINT('Ctrl Pts',(-1.7560314637164,22.7619782595013,12.));
#245694=CARTESIAN_POINT('Ctrl Pts',(-1.75693513908911,22.7503059556455,
12.));
#245695=CARTESIAN_POINT('Ctrl Pts',(-1.75778553673249,22.7388226235565,
12.));
#245696=CARTESIAN_POINT('Ctrl Pts',(-1.75858354204635,22.7275311777305,
12.));
#245697=CARTESIAN_POINT('Ctrl Pts',(-1.75933006905924,22.7164346186007,
12.));
#245698=CARTESIAN_POINT('Ctrl Pts',(-1.76002606202399,22.7055360375481,
12.));
#245699=CARTESIAN_POINT('Ctrl Pts',(-1.76067249704884,22.6948386219843,
12.));
#245700=CARTESIAN_POINT('Ctrl Pts',(-1.76127038310613,22.6843456585245,
12.));
#245701=CARTESIAN_POINT('Ctrl Pts',(-1.76182076289525,22.6740605356699,
12.));
#245702=CARTESIAN_POINT('Ctrl Pts',(-1.76232471392567,22.6639867471756,
12.));
#245703=CARTESIAN_POINT('Ctrl Pts',(-1.76278334912559,22.6541278938413,
12.));
#245704=CARTESIAN_POINT('Ctrl Pts',(-1.76319782013914,22.6444876940425,
12.));
#245705=CARTESIAN_POINT('Ctrl Pts',(-1.76356932176272,22.635069997936,12.));
#245706=CARTESIAN_POINT('Ctrl Pts',(-1.76389909571402,22.6258787994847,
12.));
#245707=CARTESIAN_POINT('Ctrl Pts',(-1.76418843543739,22.6169182517693,
12.));
#245708=CARTESIAN_POINT('Ctrl Pts',(-1.76443868648015,22.6081926681342,
12.));
#245709=CARTESIAN_POINT('Ctrl Pts',(-1.76465124413556,22.5997065145638,
12.));
#245710=CARTESIAN_POINT('Ctrl Pts',(-1.76482755288411,22.5914644078106,
12.));
#245711=CARTESIAN_POINT('Ctrl Pts',(-1.76496910283088,22.5834711038024,
12.));
#245712=CARTESIAN_POINT('Ctrl Pts',(-1.76507744026747,22.5757315316355,
12.));
#245713=CARTESIAN_POINT('Ctrl Pts',(-1.76515418518829,22.5682508499873,
12.));
#245714=CARTESIAN_POINT('Ctrl Pts',(-1.76520104500449,22.5610344912501,
12.));
#245715=CARTESIAN_POINT('Ctrl Pts',(-1.76521983384063,22.5540882235837,
12.));
#245716=CARTESIAN_POINT('Ctrl Pts',(-1.76521245524047,22.5474180954006,
12.));
#245717=CARTESIAN_POINT('Ctrl Pts',(-1.76518087841493,22.5410303590891,
12.));
#245718=CARTESIAN_POINT('Ctrl Pts',(-1.7651271156325,22.5349313983571,12.));
#245719=CARTESIAN_POINT('Ctrl Pts',(-1.76505320262752,22.529127665298,12.));
#245720=CARTESIAN_POINT('Ctrl Pts',(-1.76496128643369,22.5236259635515,
12.));
#245721=CARTESIAN_POINT('Ctrl Pts',(-1.76485369319896,22.5184336670207,
12.));
#245722=CARTESIAN_POINT('Ctrl Pts',(-1.76473303281159,22.5135590569554,
12.));
#245723=CARTESIAN_POINT('Ctrl Pts',(-1.76460218257323,22.5090112700212,
12.));
#245724=CARTESIAN_POINT('Ctrl Pts',(-1.76446408210366,22.5047996391978,
12.));
#245725=CARTESIAN_POINT('Ctrl Pts',(-1.76432160068725,22.5009332677316,
12.));
#245726=CARTESIAN_POINT('Ctrl Pts',(-1.76417731243462,22.4974203063191,
12.));
#245727=CARTESIAN_POINT('Ctrl Pts',(-1.76403393880301,22.4942693792449,
12.));
#245728=CARTESIAN_POINT('Ctrl Pts',(-1.76389475965724,22.4914909094908,
12.));
#245729=CARTESIAN_POINT('Ctrl Pts',(-1.76376424879505,22.4890991659478,
12.));
#245730=CARTESIAN_POINT('Ctrl Pts',(-1.76364784232963,22.4871115206571,
12.));
#245731=CARTESIAN_POINT('Ctrl Pts',(-1.76355076045546,22.4855446605991,
12.));
#245732=CARTESIAN_POINT('Ctrl Pts',(-1.76347698284792,22.4844112933129,
12.));
#245733=CARTESIAN_POINT('Ctrl Pts',(-1.76343813434565,22.483856251707,12.));
#245734=CARTESIAN_POINT('Ctrl Pts',(-1.7634206426357,22.4836387052232,12.));
#245735=CARTESIAN_POINT('Ctrl Pts',(-1.76341415538764,22.483581992979,12.));
#245736=CARTESIAN_POINT('Ctrl Pts',(-1.76341220531179,22.4835757167854,
12.));
#245737=CARTESIAN_POINT('',(-0.661312440730891,25.991588367311,0.));
#245738=CARTESIAN_POINT('Origin',(3.92374859571501,21.1389261070099,0.));
#245739=CARTESIAN_POINT('',(4.11585220600461,22.1738711152697,12.));
#245740=CARTESIAN_POINT('',(1.96187429785751,10.5694630535049,12.));
#245741=CARTESIAN_POINT('',(4.11585220600461,22.1738711152697,0.));
#245742=CARTESIAN_POINT('',(4.11585220600461,22.1738711152697,0.));
#245743=CARTESIAN_POINT('',(1.96187429785751,10.5694630535049,0.));
#245744=CARTESIAN_POINT('Ctrl Pts',(0.661312440730901,25.991588367311,0.));
#245745=CARTESIAN_POINT('Ctrl Pts',(0.661312440730901,25.991588367311,12.));
#245746=CARTESIAN_POINT('Ctrl Pts',(0.664028313187627,25.9865613464773,
0.));
#245747=CARTESIAN_POINT('Ctrl Pts',(0.664028313187627,25.9865613464773,
12.));
#245748=CARTESIAN_POINT('Ctrl Pts',(0.669451306780825,25.9765104298071,
0.));
#245749=CARTESIAN_POINT('Ctrl Pts',(0.669451306780825,25.9765104298071,
12.));
#245750=CARTESIAN_POINT('Ctrl Pts',(0.677559543209725,25.9614434297919,
0.));
#245751=CARTESIAN_POINT('Ctrl Pts',(0.677559543209725,25.9614434297919,
12.));
#245752=CARTESIAN_POINT('Ctrl Pts',(0.688318015057729,25.9413728471909,
0.));
#245753=CARTESIAN_POINT('Ctrl Pts',(0.688318015057729,25.9413728471909,
12.));
#245754=CARTESIAN_POINT('Ctrl Pts',(0.701678575228756,25.9163158909426,
0.));
#245755=CARTESIAN_POINT('Ctrl Pts',(0.701678575228756,25.9163158909426,
12.));
#245756=CARTESIAN_POINT('Ctrl Pts',(0.714951588527638,25.891290261497,0.));
#245757=CARTESIAN_POINT('Ctrl Pts',(0.714951588527638,25.891290261497,12.));
#245758=CARTESIAN_POINT('Ctrl Pts',(0.728137036482335,25.8662960624185,
0.));
#245759=CARTESIAN_POINT('Ctrl Pts',(0.728137036482335,25.8662960624185,
12.));
#245760=CARTESIAN_POINT('Ctrl Pts',(0.741234902663807,25.8413334619055,
0.));
#245761=CARTESIAN_POINT('Ctrl Pts',(0.741234902663807,25.8413334619055,
12.));
#245762=CARTESIAN_POINT('Ctrl Pts',(0.754245175609524,25.8164027059984,
0.));
#245763=CARTESIAN_POINT('Ctrl Pts',(0.754245175609524,25.8164027059984,
12.));
#245764=CARTESIAN_POINT('Ctrl Pts',(0.767167852651168,25.7915041383376,
0.));
#245765=CARTESIAN_POINT('Ctrl Pts',(0.767167852651168,25.7915041383376,
12.));
#245766=CARTESIAN_POINT('Ctrl Pts',(0.780002940291965,25.7666381946955,
0.));
#245767=CARTESIAN_POINT('Ctrl Pts',(0.780002940291965,25.7666381946955,
12.));
#245768=CARTESIAN_POINT('Ctrl Pts',(0.792750451616127,25.7418053757746,
0.));
#245769=CARTESIAN_POINT('Ctrl Pts',(0.792750451616127,25.7418053757746,
12.));
#245770=CARTESIAN_POINT('Ctrl Pts',(0.805410404554352,25.7170062262525,
0.));
#245771=CARTESIAN_POINT('Ctrl Pts',(0.805410404554352,25.7170062262525,
12.));
#245772=CARTESIAN_POINT('Ctrl Pts',(0.817982819787464,25.6922413110194,
0.));
#245773=CARTESIAN_POINT('Ctrl Pts',(0.817982819787464,25.6922413110194,
12.));
#245774=CARTESIAN_POINT('Ctrl Pts',(0.830467718864205,25.6675111931952,
0.));
#245775=CARTESIAN_POINT('Ctrl Pts',(0.830467718864205,25.6675111931952,
12.));
#245776=CARTESIAN_POINT('Ctrl Pts',(0.842865122120758,25.6428164100055,
0.));
#245777=CARTESIAN_POINT('Ctrl Pts',(0.842865122120758,25.6428164100055,
12.));
#245778=CARTESIAN_POINT('Ctrl Pts',(0.855175047036549,25.6181574536049,
0.));
#245779=CARTESIAN_POINT('Ctrl Pts',(0.855175047036549,25.6181574536049,
12.));
#245780=CARTESIAN_POINT('Ctrl Pts',(0.867397509338431,25.5935347843585,
0.));
#245781=CARTESIAN_POINT('Ctrl Pts',(0.867397509338431,25.5935347843585,
12.));
#245782=CARTESIAN_POINT('Ctrl Pts',(0.879532523834294,25.5689488408156,
0.));
#245783=CARTESIAN_POINT('Ctrl Pts',(0.879532523834294,25.5689488408156,
12.));
#245784=CARTESIAN_POINT('Ctrl Pts',(0.89158010534904,25.5444000508211,0.));
#245785=CARTESIAN_POINT('Ctrl Pts',(0.89158010534904,25.5444000508211,12.));
#245786=CARTESIAN_POINT('Ctrl Pts',(0.903540269651106,25.5198888424194,
0.));
#245787=CARTESIAN_POINT('Ctrl Pts',(0.903540269651106,25.5198888424194,
12.));
#245788=CARTESIAN_POINT('Ctrl Pts',(0.915413034335613,25.4954156541795,
0.));
#245789=CARTESIAN_POINT('Ctrl Pts',(0.915413034335613,25.4954156541795,
12.));
#245790=CARTESIAN_POINT('Ctrl Pts',(0.927198419886094,25.4709809475009,
0.));
#245791=CARTESIAN_POINT('Ctrl Pts',(0.927198419886094,25.4709809475009,
12.));
#245792=CARTESIAN_POINT('Ctrl Pts',(0.938896449496192,25.4465852044849,
0.));
#245793=CARTESIAN_POINT('Ctrl Pts',(0.938896449496192,25.4465852044849,
12.));
#245794=CARTESIAN_POINT('Ctrl Pts',(0.950507148597468,25.4222289223167,
0.));
#245795=CARTESIAN_POINT('Ctrl Pts',(0.950507148597468,25.4222289223167,
12.));
#245796=CARTESIAN_POINT('Ctrl Pts',(0.962030544503142,25.3979126089163,
0.));
#245797=CARTESIAN_POINT('Ctrl Pts',(0.962030544503142,25.3979126089163,
12.));
#245798=CARTESIAN_POINT('Ctrl Pts',(0.973466666000163,25.3736367778845,
0.));
#245799=CARTESIAN_POINT('Ctrl Pts',(0.973466666000163,25.3736367778845,
12.));
#245800=CARTESIAN_POINT('Ctrl Pts',(0.984815543003973,25.3494019441441,
0.));
#245801=CARTESIAN_POINT('Ctrl Pts',(0.984815543003973,25.3494019441441,
12.));
#245802=CARTESIAN_POINT('Ctrl Pts',(0.996077206120624,25.3252086182968,
0.));
#245803=CARTESIAN_POINT('Ctrl Pts',(0.996077206120624,25.3252086182968,
12.));
#245804=CARTESIAN_POINT('Ctrl Pts',(1.00725168656896,25.3010573055547,0.));
#245805=CARTESIAN_POINT('Ctrl Pts',(1.00725168656896,25.3010573055547,12.));
#245806=CARTESIAN_POINT('Ctrl Pts',(1.01833901642237,25.276948508726,0.));
#245807=CARTESIAN_POINT('Ctrl Pts',(1.01833901642237,25.276948508726,12.));
#245808=CARTESIAN_POINT('Ctrl Pts',(1.02933922876806,25.2528827300422,0.));
#245809=CARTESIAN_POINT('Ctrl Pts',(1.02933922876806,25.2528827300422,12.));
#245810=CARTESIAN_POINT('Ctrl Pts',(1.04025235791507,25.2288604735086,0.));
#245811=CARTESIAN_POINT('Ctrl Pts',(1.04025235791507,25.2288604735086,12.));
#245812=CARTESIAN_POINT('Ctrl Pts',(1.05107843957931,25.2048822469028,0.));
#245813=CARTESIAN_POINT('Ctrl Pts',(1.05107843957931,25.2048822469028,12.));
#245814=CARTESIAN_POINT('Ctrl Pts',(1.06181751111768,25.1809485642192,0.));
#245815=CARTESIAN_POINT('Ctrl Pts',(1.06181751111768,25.1809485642192,12.));
#245816=CARTESIAN_POINT('Ctrl Pts',(1.07246961165475,25.157059946931,0.));
#245817=CARTESIAN_POINT('Ctrl Pts',(1.07246961165475,25.157059946931,12.));
#245818=CARTESIAN_POINT('Ctrl Pts',(1.08303478197187,25.1332169227413,0.));
#245819=CARTESIAN_POINT('Ctrl Pts',(1.08303478197187,25.1332169227413,12.));
#245820=CARTESIAN_POINT('Ctrl Pts',(1.09351306445308,25.1094200248446,0.));
#245821=CARTESIAN_POINT('Ctrl Pts',(1.09351306445308,25.1094200248446,12.));
#245822=CARTESIAN_POINT('Ctrl Pts',(1.10390450301745,25.0856697909679,0.));
#245823=CARTESIAN_POINT('Ctrl Pts',(1.10390450301745,25.0856697909679,12.));
#245824=CARTESIAN_POINT('Ctrl Pts',(1.11420914306889,25.0619667625336,0.));
#245825=CARTESIAN_POINT('Ctrl Pts',(1.11420914306889,25.0619667625336,12.));
#245826=CARTESIAN_POINT('Ctrl Pts',(1.12442703144451,25.0383114836899,0.));
#245827=CARTESIAN_POINT('Ctrl Pts',(1.12442703144451,25.0383114836899,12.));
#245828=CARTESIAN_POINT('Ctrl Pts',(1.1345582163853,25.0147045006196,0.));
#245829=CARTESIAN_POINT('Ctrl Pts',(1.1345582163853,25.0147045006196,12.));
#245830=CARTESIAN_POINT('Ctrl Pts',(1.144602747582,24.9911463621433,0.));
#245831=CARTESIAN_POINT('Ctrl Pts',(1.144602747582,24.9911463621433,12.));
#245832=CARTESIAN_POINT('Ctrl Pts',(1.15456067621889,24.9676376201502,0.));
#245833=CARTESIAN_POINT('Ctrl Pts',(1.15456067621889,24.9676376201502,12.));
#245834=CARTESIAN_POINT('Ctrl Pts',(1.16443205502849,24.9441788300932,0.));
#245835=CARTESIAN_POINT('Ctrl Pts',(1.16443205502849,24.9441788300932,12.));
#245836=CARTESIAN_POINT('Ctrl Pts',(1.17421693835041,24.9207705514449,0.));
#245837=CARTESIAN_POINT('Ctrl Pts',(1.17421693835041,24.9207705514449,12.));
#245838=CARTESIAN_POINT('Ctrl Pts',(1.18391538220103,24.8974133481829,0.));
#245839=CARTESIAN_POINT('Ctrl Pts',(1.18391538220103,24.8974133481829,12.));
#245840=CARTESIAN_POINT('Ctrl Pts',(1.19352744434064,24.8741077892075,0.));
#245841=CARTESIAN_POINT('Ctrl Pts',(1.19352744434064,24.8741077892075,12.));
#245842=CARTESIAN_POINT('Ctrl Pts',(1.2030531842602,24.8508544481974,0.));
#245843=CARTESIAN_POINT('Ctrl Pts',(1.2030531842602,24.8508544481974,12.));
#245844=CARTESIAN_POINT('Ctrl Pts',(1.21249266318208,24.8276539035092,0.));
#245845=CARTESIAN_POINT('Ctrl Pts',(1.21249266318208,24.8276539035092,12.));
#245846=CARTESIAN_POINT('Ctrl Pts',(1.22184594406528,24.8045067380536,0.));
#245847=CARTESIAN_POINT('Ctrl Pts',(1.22184594406528,24.8045067380536,12.));
#245848=CARTESIAN_POINT('Ctrl Pts',(1.23111309161843,24.7814135391799,0.));
#245849=CARTESIAN_POINT('Ctrl Pts',(1.23111309161843,24.7814135391799,12.));
#245850=CARTESIAN_POINT('Ctrl Pts',(1.24029417231989,24.7583748985438,0.));
#245851=CARTESIAN_POINT('Ctrl Pts',(1.24029417231989,24.7583748985438,12.));
#245852=CARTESIAN_POINT('Ctrl Pts',(1.24938925444325,24.7353914120011,0.));
#245853=CARTESIAN_POINT('Ctrl Pts',(1.24938925444325,24.7353914120011,12.));
#245854=CARTESIAN_POINT('Ctrl Pts',(1.25839840807418,24.7124636797894,0.));
#245855=CARTESIAN_POINT('Ctrl Pts',(1.25839840807418,24.7124636797894,12.));
#245856=CARTESIAN_POINT('Ctrl Pts',(1.267321705135,24.6895923066836,0.));
#245857=CARTESIAN_POINT('Ctrl Pts',(1.267321705135,24.6895923066836,12.));
#245858=CARTESIAN_POINT('Ctrl Pts',(1.27615921941642,24.666777902156,0.));
#245859=CARTESIAN_POINT('Ctrl Pts',(1.27615921941642,24.666777902156,12.));
#245860=CARTESIAN_POINT('Ctrl Pts',(1.28491102661514,24.6440210805278,0.));
#245861=CARTESIAN_POINT('Ctrl Pts',(1.28491102661514,24.6440210805278,12.));
#245862=CARTESIAN_POINT('Ctrl Pts',(1.29357720438107,24.6213224611229,0.));
#245863=CARTESIAN_POINT('Ctrl Pts',(1.29357720438107,24.6213224611229,12.));
#245864=CARTESIAN_POINT('Ctrl Pts',(1.30215783236362,24.5986826684027,0.));
#245865=CARTESIAN_POINT('Ctrl Pts',(1.30215783236362,24.5986826684027,12.));
#245866=CARTESIAN_POINT('Ctrl Pts',(1.31065299222021,24.5761023320183,0.));
#245867=CARTESIAN_POINT('Ctrl Pts',(1.31065299222021,24.5761023320183,12.));
#245868=CARTESIAN_POINT('Ctrl Pts',(1.31906276763668,24.5535820868674,0.));
#245869=CARTESIAN_POINT('Ctrl Pts',(1.31906276763668,24.5535820868674,12.));
#245870=CARTESIAN_POINT('Ctrl Pts',(1.32738724435326,24.5311225731435,0.));
#245871=CARTESIAN_POINT('Ctrl Pts',(1.32738724435326,24.5311225731435,12.));
#245872=CARTESIAN_POINT('Ctrl Pts',(1.33562651019686,24.5087244363856,0.));
#245873=CARTESIAN_POINT('Ctrl Pts',(1.33562651019686,24.5087244363856,12.));
#245874=CARTESIAN_POINT('Ctrl Pts',(1.34378065512337,24.4863883275134,0.));
#245875=CARTESIAN_POINT('Ctrl Pts',(1.34378065512337,24.4863883275134,12.));
#245876=CARTESIAN_POINT('Ctrl Pts',(1.35184977125648,24.4641149028892,0.));
#245877=CARTESIAN_POINT('Ctrl Pts',(1.35184977125648,24.4641149028892,12.));
#245878=CARTESIAN_POINT('Ctrl Pts',(1.35983395290627,24.4419048244523,0.));
#245879=CARTESIAN_POINT('Ctrl Pts',(1.35983395290627,24.4419048244523,12.));
#245880=CARTESIAN_POINT('Ctrl Pts',(1.36773329659956,24.4197587598337,0.));
#245881=CARTESIAN_POINT('Ctrl Pts',(1.36773329659956,24.4197587598337,12.));
#245882=CARTESIAN_POINT('Ctrl Pts',(1.37554790111609,24.3976773824732,0.));
#245883=CARTESIAN_POINT('Ctrl Pts',(1.37554790111609,24.3976773824732,12.));
#245884=CARTESIAN_POINT('Ctrl Pts',(1.38327786752998,24.3756613717299,0.));
#245885=CARTESIAN_POINT('Ctrl Pts',(1.38327786752998,24.3756613717299,12.));
#245886=CARTESIAN_POINT('Ctrl Pts',(1.39092329926388,24.3537114129875,0.));
#245887=CARTESIAN_POINT('Ctrl Pts',(1.39092329926388,24.3537114129875,12.));
#245888=CARTESIAN_POINT('Ctrl Pts',(1.39848430212807,24.3318281977643,0.));
#245889=CARTESIAN_POINT('Ctrl Pts',(1.39848430212807,24.3318281977643,12.));
#245890=CARTESIAN_POINT('Ctrl Pts',(1.40596098434337,24.3100124238311,0.));
#245891=CARTESIAN_POINT('Ctrl Pts',(1.40596098434337,24.3100124238311,12.));
#245892=CARTESIAN_POINT('Ctrl Pts',(1.41335345657682,24.288264795321,0.));
#245893=CARTESIAN_POINT('Ctrl Pts',(1.41335345657682,24.288264795321,12.));
#245894=CARTESIAN_POINT('Ctrl Pts',(1.42066183198252,24.2665860228356,0.));
#245895=CARTESIAN_POINT('Ctrl Pts',(1.42066183198252,24.2665860228356,12.));
#245896=CARTESIAN_POINT('Ctrl Pts',(1.42788622624854,24.2449768235488,0.));
#245897=CARTESIAN_POINT('Ctrl Pts',(1.42788622624854,24.2449768235488,12.));
#245898=CARTESIAN_POINT('Ctrl Pts',(1.43502675765508,24.2234379212984,0.));
#245899=CARTESIAN_POINT('Ctrl Pts',(1.43502675765508,24.2234379212984,12.));
#245900=CARTESIAN_POINT('Ctrl Pts',(1.44208354711082,24.201970046722,0.));
#245901=CARTESIAN_POINT('Ctrl Pts',(1.44208354711082,24.201970046722,12.));
#245902=CARTESIAN_POINT('Ctrl Pts',(1.44905671818727,24.1805739374038,0.));
#245903=CARTESIAN_POINT('Ctrl Pts',(1.44905671818727,24.1805739374038,12.));
#245904=CARTESIAN_POINT('Ctrl Pts',(1.45594639716317,24.1592503380107,0.));
#245905=CARTESIAN_POINT('Ctrl Pts',(1.45594639716317,24.1592503380107,12.));
#245906=CARTESIAN_POINT('Ctrl Pts',(1.46275271307397,24.1380000004272,0.));
#245907=CARTESIAN_POINT('Ctrl Pts',(1.46275271307397,24.1380000004272,12.));
#245908=CARTESIAN_POINT('Ctrl Pts',(1.46947579776991,24.1168236838824,0.));
#245909=CARTESIAN_POINT('Ctrl Pts',(1.46947579776991,24.1168236838824,12.));
#245910=CARTESIAN_POINT('Ctrl Pts',(1.47611578597742,24.0957221550778,0.));
#245911=CARTESIAN_POINT('Ctrl Pts',(1.47611578597742,24.0957221550778,12.));
#245912=CARTESIAN_POINT('Ctrl Pts',(1.48267281533683,24.0746961883528,0.));
#245913=CARTESIAN_POINT('Ctrl Pts',(1.48267281533683,24.0746961883528,12.));
#245914=CARTESIAN_POINT('Ctrl Pts',(1.48914702644887,24.0537465658429,0.));
#245915=CARTESIAN_POINT('Ctrl Pts',(1.48914702644887,24.0537465658429,12.));
#245916=CARTESIAN_POINT('Ctrl Pts',(1.49553856292801,24.0328740776331,0.));
#245917=CARTESIAN_POINT('Ctrl Pts',(1.49553856292801,24.0328740776331,12.));
#245918=CARTESIAN_POINT('Ctrl Pts',(1.50184757146098,24.0120795219086,0.));
#245919=CARTESIAN_POINT('Ctrl Pts',(1.50184757146098,24.0120795219086,12.));
#245920=CARTESIAN_POINT('Ctrl Pts',(1.50807420187694,23.9913637050927,0.));
#245921=CARTESIAN_POINT('Ctrl Pts',(1.50807420187694,23.9913637050927,12.));
#245922=CARTESIAN_POINT('Ctrl Pts',(1.51421860720614,23.970727442014,0.));
#245923=CARTESIAN_POINT('Ctrl Pts',(1.51421860720614,23.970727442014,12.));
#245924=CARTESIAN_POINT('Ctrl Pts',(1.52028094372792,23.9501715561033,0.));
#245925=CARTESIAN_POINT('Ctrl Pts',(1.52028094372792,23.9501715561033,12.));
#245926=CARTESIAN_POINT('Ctrl Pts',(1.52626137103032,23.9296968795757,0.));
#245927=CARTESIAN_POINT('Ctrl Pts',(1.52626137103032,23.9296968795757,12.));
#245928=CARTESIAN_POINT('Ctrl Pts',(1.53216005207463,23.9093042536119,0.));
#245929=CARTESIAN_POINT('Ctrl Pts',(1.53216005207463,23.9093042536119,12.));
#245930=CARTESIAN_POINT('Ctrl Pts',(1.53797715326758,23.8889945285318,0.));
#245931=CARTESIAN_POINT('Ctrl Pts',(1.53797715326758,23.8889945285318,12.));
#245932=CARTESIAN_POINT('Ctrl Pts',(1.5437128445399,23.8687685639642,0.));
#245933=CARTESIAN_POINT('Ctrl Pts',(1.5437128445399,23.8687685639642,12.));
#245934=CARTESIAN_POINT('Ctrl Pts',(1.54936729940541,23.8486272290705,0.));
#245935=CARTESIAN_POINT('Ctrl Pts',(1.54936729940541,23.8486272290705,12.));
#245936=CARTESIAN_POINT('Ctrl Pts',(1.55494069502635,23.8285714027636,0.));
#245937=CARTESIAN_POINT('Ctrl Pts',(1.55494069502635,23.8285714027636,12.));
#245938=CARTESIAN_POINT('Ctrl Pts',(1.56043321228633,23.8086019739194,0.));
#245939=CARTESIAN_POINT('Ctrl Pts',(1.56043321228633,23.8086019739194,12.));
#245940=CARTESIAN_POINT('Ctrl Pts',(1.56584503586843,23.7887198415878,0.));
#245941=CARTESIAN_POINT('Ctrl Pts',(1.56584503586843,23.7887198415878,12.));
#245942=CARTESIAN_POINT('Ctrl Pts',(1.57117635434408,23.7689259151862,0.));
#245943=CARTESIAN_POINT('Ctrl Pts',(1.57117635434408,23.7689259151862,12.));
#245944=CARTESIAN_POINT('Ctrl Pts',(1.57642736025246,23.749221114736,0.));
#245945=CARTESIAN_POINT('Ctrl Pts',(1.57642736025246,23.749221114736,12.));
#245946=CARTESIAN_POINT('Ctrl Pts',(1.58159825017358,23.72960637113,0.));
#245947=CARTESIAN_POINT('Ctrl Pts',(1.58159825017358,23.72960637113,12.));
#245948=CARTESIAN_POINT('Ctrl Pts',(1.58668922481221,23.710082626383,0.));
#245949=CARTESIAN_POINT('Ctrl Pts',(1.58668922481221,23.710082626383,12.));
#245950=CARTESIAN_POINT('Ctrl Pts',(1.59170048908633,23.6906508338833,0.));
#245951=CARTESIAN_POINT('Ctrl Pts',(1.59170048908633,23.6906508338833,12.));
#245952=CARTESIAN_POINT('Ctrl Pts',(1.59663225222463,23.671311958631,0.));
#245953=CARTESIAN_POINT('Ctrl Pts',(1.59663225222463,23.671311958631,12.));
#245954=CARTESIAN_POINT('Ctrl Pts',(1.60148472786595,23.6520669774876,0.));
#245955=CARTESIAN_POINT('Ctrl Pts',(1.60148472786595,23.6520669774876,12.));
#245956=CARTESIAN_POINT('Ctrl Pts',(1.60625813414672,23.6329168794929,0.));
#245957=CARTESIAN_POINT('Ctrl Pts',(1.60625813414672,23.6329168794929,12.));
#245958=CARTESIAN_POINT('Ctrl Pts',(1.61095269379778,23.6138626661653,0.));
#245959=CARTESIAN_POINT('Ctrl Pts',(1.61095269379778,23.6138626661653,12.));
#245960=CARTESIAN_POINT('Ctrl Pts',(1.61556863424698,23.5949053517997,0.));
#245961=CARTESIAN_POINT('Ctrl Pts',(1.61556863424698,23.5949053517997,12.));
#245962=CARTESIAN_POINT('Ctrl Pts',(1.62010618772866,23.57604596376,0.));
#245963=CARTESIAN_POINT('Ctrl Pts',(1.62010618772866,23.57604596376,12.));
#245964=CARTESIAN_POINT('Ctrl Pts',(1.62456559140064,23.5572855427601,0.));
#245965=CARTESIAN_POINT('Ctrl Pts',(1.62456559140064,23.5572855427601,12.));
#245966=CARTESIAN_POINT('Ctrl Pts',(1.62894708745223,23.538625143226,0.));
#245967=CARTESIAN_POINT('Ctrl Pts',(1.62894708745223,23.538625143226,12.));
#245968=CARTESIAN_POINT('Ctrl Pts',(1.63325092321725,23.5200658336612,0.));
#245969=CARTESIAN_POINT('Ctrl Pts',(1.63325092321725,23.5200658336612,12.));
#245970=CARTESIAN_POINT('Ctrl Pts',(1.63747735129474,23.5016086970003,0.));
#245971=CARTESIAN_POINT('Ctrl Pts',(1.63747735129474,23.5016086970003,12.));
#245972=CARTESIAN_POINT('Ctrl Pts',(1.64162662967528,23.4832548309645,0.));
#245973=CARTESIAN_POINT('Ctrl Pts',(1.64162662967528,23.4832548309645,12.));
#245974=CARTESIAN_POINT('Ctrl Pts',(1.64569902187611,23.4650053483932,0.));
#245975=CARTESIAN_POINT('Ctrl Pts',(1.64569902187611,23.4650053483932,12.));
#245976=CARTESIAN_POINT('Ctrl Pts',(1.6496947970734,23.4468613776574,0.));
#245977=CARTESIAN_POINT('Ctrl Pts',(1.6496947970734,23.4468613776574,12.));
#245978=CARTESIAN_POINT('Ctrl Pts',(1.65361423023728,23.4288240631043,0.));
#245979=CARTESIAN_POINT('Ctrl Pts',(1.65361423023728,23.4288240631043,12.));
#245980=CARTESIAN_POINT('Ctrl Pts',(1.65745760227505,23.4108945654805,0.));
#245981=CARTESIAN_POINT('Ctrl Pts',(1.65745760227505,23.4108945654805,12.));
#245982=CARTESIAN_POINT('Ctrl Pts',(1.66122520018011,23.3930740623619,0.));
#245983=CARTESIAN_POINT('Ctrl Pts',(1.66122520018011,23.3930740623619,12.));
#245984=CARTESIAN_POINT('Ctrl Pts',(1.66491731718876,23.3753637485545,0.));
#245985=CARTESIAN_POINT('Ctrl Pts',(1.66491731718876,23.3753637485545,12.));
#245986=CARTESIAN_POINT('Ctrl Pts',(1.66853425293995,23.3577648365744,0.));
#245987=CARTESIAN_POINT('Ctrl Pts',(1.66853425293995,23.3577648365744,12.));
#245988=CARTESIAN_POINT('Ctrl Pts',(1.67207631363921,23.3402785571865,0.));
#245989=CARTESIAN_POINT('Ctrl Pts',(1.67207631363921,23.3402785571865,12.));
#245990=CARTESIAN_POINT('Ctrl Pts',(1.67554381222994,23.3229061599145,0.));
#245991=CARTESIAN_POINT('Ctrl Pts',(1.67554381222994,23.3229061599145,12.));
#245992=CARTESIAN_POINT('Ctrl Pts',(1.67893706857117,23.3056489135611,0.));
#245993=CARTESIAN_POINT('Ctrl Pts',(1.67893706857117,23.3056489135611,12.));
#245994=CARTESIAN_POINT('Ctrl Pts',(1.68225640962168,23.2885081066951,0.));
#245995=CARTESIAN_POINT('Ctrl Pts',(1.68225640962168,23.2885081066951,12.));
#245996=CARTESIAN_POINT('Ctrl Pts',(1.68550216963258,23.2714850482246,0.));
#245997=CARTESIAN_POINT('Ctrl Pts',(1.68550216963258,23.2714850482246,12.));
#245998=CARTESIAN_POINT('Ctrl Pts',(1.68867469034896,23.2545810680537,0.));
#245999=CARTESIAN_POINT('Ctrl Pts',(1.68867469034896,23.2545810680537,12.));
#246000=CARTESIAN_POINT('Ctrl Pts',(1.69177432121711,23.2377975177013,0.));
#246001=CARTESIAN_POINT('Ctrl Pts',(1.69177432121711,23.2377975177013,12.));
#246002=CARTESIAN_POINT('Ctrl Pts',(1.69480141959953,23.2211357709374,0.));
#246003=CARTESIAN_POINT('Ctrl Pts',(1.69480141959953,23.2211357709374,12.));
#246004=CARTESIAN_POINT('Ctrl Pts',(1.69775635099443,23.2045972243767,0.));
#246005=CARTESIAN_POINT('Ctrl Pts',(1.69775635099443,23.2045972243767,12.));
#246006=CARTESIAN_POINT('Ctrl Pts',(1.7006394892701,23.1881832981851,0.));
#246007=CARTESIAN_POINT('Ctrl Pts',(1.7006394892701,23.1881832981851,12.));
#246008=CARTESIAN_POINT('Ctrl Pts',(1.70345121691276,23.1718954368751,0.));
#246009=CARTESIAN_POINT('Ctrl Pts',(1.70345121691276,23.1718954368751,12.));
#246010=CARTESIAN_POINT('Ctrl Pts',(1.70619192527852,23.1557351100614,0.));
#246011=CARTESIAN_POINT('Ctrl Pts',(1.70619192527852,23.1557351100614,12.));
#246012=CARTESIAN_POINT('Ctrl Pts',(1.70886201485452,23.1397038132356,0.));
#246013=CARTESIAN_POINT('Ctrl Pts',(1.70886201485452,23.1397038132356,12.));
#246014=CARTESIAN_POINT('Ctrl Pts',(1.71146189552174,23.1238030684925,0.));
#246015=CARTESIAN_POINT('Ctrl Pts',(1.71146189552174,23.1238030684925,12.));
#246016=CARTESIAN_POINT('Ctrl Pts',(1.71399198684704,23.1080344254286,0.));
#246017=CARTESIAN_POINT('Ctrl Pts',(1.71399198684704,23.1080344254286,12.));
#246018=CARTESIAN_POINT('Ctrl Pts',(1.71645271839296,23.0923994621213,0.));
#246019=CARTESIAN_POINT('Ctrl Pts',(1.71645271839296,23.0923994621213,12.));
#246020=CARTESIAN_POINT('Ctrl Pts',(1.71884453003027,23.0768997860709,0.));
#246021=CARTESIAN_POINT('Ctrl Pts',(1.71884453003027,23.0768997860709,12.));
#246022=CARTESIAN_POINT('Ctrl Pts',(1.72116787225991,23.0615370351562,0.));
#246023=CARTESIAN_POINT('Ctrl Pts',(1.72116787225991,23.0615370351562,12.));
#246024=CARTESIAN_POINT('Ctrl Pts',(1.72342320653746,23.0463128785531,0.));
#246025=CARTESIAN_POINT('Ctrl Pts',(1.72342320653746,23.0463128785531,12.));
#246026=CARTESIAN_POINT('Ctrl Pts',(1.72561100564045,23.0312290178883,0.));
#246027=CARTESIAN_POINT('Ctrl Pts',(1.72561100564045,23.0312290178883,12.));
#246028=CARTESIAN_POINT('Ctrl Pts',(1.72773175404708,23.0162871884168,0.));
#246029=CARTESIAN_POINT('Ctrl Pts',(1.72773175404708,23.0162871884168,12.));
#246030=CARTESIAN_POINT('Ctrl Pts',(1.72978594832136,23.001489160189,0.));
#246031=CARTESIAN_POINT('Ctrl Pts',(1.72978594832136,23.001489160189,12.));
#246032=CARTESIAN_POINT('Ctrl Pts',(1.7317740975019,22.9868367391978,0.));
#246033=CARTESIAN_POINT('Ctrl Pts',(1.7317740975019,22.9868367391978,12.));
#246034=CARTESIAN_POINT('Ctrl Pts',(1.73369672350814,22.9723317685688,0.));
#246035=CARTESIAN_POINT('Ctrl Pts',(1.73369672350814,22.9723317685688,12.));
#246036=CARTESIAN_POINT('Ctrl Pts',(1.73555436162769,22.9579761301063,0.));
#246037=CARTESIAN_POINT('Ctrl Pts',(1.73555436162769,22.9579761301063,12.));
#246038=CARTESIAN_POINT('Ctrl Pts',(1.73734756100039,22.9437717457826,0.));
#246039=CARTESIAN_POINT('Ctrl Pts',(1.73734756100039,22.9437717457826,12.));
#246040=CARTESIAN_POINT('Ctrl Pts',(1.73907688511666,22.9297205792586,0.));
#246041=CARTESIAN_POINT('Ctrl Pts',(1.73907688511666,22.9297205792586,12.));
#246042=CARTESIAN_POINT('Ctrl Pts',(1.74074291231058,22.9158246373363,0.));
#246043=CARTESIAN_POINT('Ctrl Pts',(1.74074291231058,22.9158246373363,12.));
#246044=CARTESIAN_POINT('Ctrl Pts',(1.7423462363008,22.9020859716141,0.));
#246045=CARTESIAN_POINT('Ctrl Pts',(1.7423462363008,22.9020859716141,12.));
#246046=CARTESIAN_POINT('Ctrl Pts',(1.74388746677702,22.888506680335,0.));
#246047=CARTESIAN_POINT('Ctrl Pts',(1.74388746677702,22.888506680335,12.));
#246048=CARTESIAN_POINT('Ctrl Pts',(1.74536722998201,22.8750889101696,0.));
#246049=CARTESIAN_POINT('Ctrl Pts',(1.74536722998201,22.8750889101696,12.));
#246050=CARTESIAN_POINT('Ctrl Pts',(1.74678616930664,22.8618348580235,0.));
#246051=CARTESIAN_POINT('Ctrl Pts',(1.74678616930664,22.8618348580235,12.));
#246052=CARTESIAN_POINT('Ctrl Pts',(1.74814494588492,22.8487467728076,0.));
#246053=CARTESIAN_POINT('Ctrl Pts',(1.74814494588492,22.8487467728076,12.));
#246054=CARTESIAN_POINT('Ctrl Pts',(1.74944423940115,22.8358269579853,0.));
#246055=CARTESIAN_POINT('Ctrl Pts',(1.74944423940115,22.8358269579853,12.));
#246056=CARTESIAN_POINT('Ctrl Pts',(1.75068474890883,22.8230777741284,0.));
#246057=CARTESIAN_POINT('Ctrl Pts',(1.75068474890883,22.8230777741284,12.));
#246058=CARTESIAN_POINT('Ctrl Pts',(1.75186719365592,22.8105016414713,0.));
#246059=CARTESIAN_POINT('Ctrl Pts',(1.75186719365592,22.8105016414713,12.));
#246060=CARTESIAN_POINT('Ctrl Pts',(1.75299231391466,22.7981010424314,0.));
#246061=CARTESIAN_POINT('Ctrl Pts',(1.75299231391466,22.7981010424314,12.));
#246062=CARTESIAN_POINT('Ctrl Pts',(1.75406087182936,22.7858785242361,0.));
#246063=CARTESIAN_POINT('Ctrl Pts',(1.75406087182936,22.7858785242361,12.));
#246064=CARTESIAN_POINT('Ctrl Pts',(1.75507365227131,22.7738367016118,0.));
#246065=CARTESIAN_POINT('Ctrl Pts',(1.75507365227131,22.7738367016118,12.));
#246066=CARTESIAN_POINT('Ctrl Pts',(1.75603146371641,22.7619782595013,0.));
#246067=CARTESIAN_POINT('Ctrl Pts',(1.75603146371641,22.7619782595013,12.));
#246068=CARTESIAN_POINT('Ctrl Pts',(1.75693513908907,22.750305955645,0.));
#246069=CARTESIAN_POINT('Ctrl Pts',(1.75693513908907,22.750305955645,12.));
#246070=CARTESIAN_POINT('Ctrl Pts',(1.75778553673244,22.7388226235559,0.));
#246071=CARTESIAN_POINT('Ctrl Pts',(1.75778553673244,22.7388226235559,12.));
#246072=CARTESIAN_POINT('Ctrl Pts',(1.75858354204633,22.72753117773,0.));
#246073=CARTESIAN_POINT('Ctrl Pts',(1.75858354204633,22.72753117773,12.));
#246074=CARTESIAN_POINT('Ctrl Pts',(1.75933006905925,22.7164346186006,0.));
#246075=CARTESIAN_POINT('Ctrl Pts',(1.75933006905925,22.7164346186006,12.));
#246076=CARTESIAN_POINT('Ctrl Pts',(1.76002606202401,22.7055360375485,0.));
#246077=CARTESIAN_POINT('Ctrl Pts',(1.76002606202401,22.7055360375485,12.));
#246078=CARTESIAN_POINT('Ctrl Pts',(1.76067249704886,22.6948386219851,0.));
#246079=CARTESIAN_POINT('Ctrl Pts',(1.76067249704886,22.6948386219851,12.));
#246080=CARTESIAN_POINT('Ctrl Pts',(1.76127038310614,22.684345658525,0.));
#246081=CARTESIAN_POINT('Ctrl Pts',(1.76127038310614,22.684345658525,12.));
#246082=CARTESIAN_POINT('Ctrl Pts',(1.76182076289525,22.67406053567,0.));
#246083=CARTESIAN_POINT('Ctrl Pts',(1.76182076289525,22.67406053567,12.));
#246084=CARTESIAN_POINT('Ctrl Pts',(1.76232471392568,22.6639867471753,0.));
#246085=CARTESIAN_POINT('Ctrl Pts',(1.76232471392568,22.6639867471753,12.));
#246086=CARTESIAN_POINT('Ctrl Pts',(1.76278334912561,22.6541278938409,0.));
#246087=CARTESIAN_POINT('Ctrl Pts',(1.76278334912561,22.6541278938409,12.));
#246088=CARTESIAN_POINT('Ctrl Pts',(1.76319782013916,22.6444876940423,0.));
#246089=CARTESIAN_POINT('Ctrl Pts',(1.76319782013916,22.6444876940423,12.));
#246090=CARTESIAN_POINT('Ctrl Pts',(1.76356932176273,22.6350699979359,0.));
#246091=CARTESIAN_POINT('Ctrl Pts',(1.76356932176273,22.6350699979359,12.));
#246092=CARTESIAN_POINT('Ctrl Pts',(1.76389909571403,22.6258787994848,0.));
#246093=CARTESIAN_POINT('Ctrl Pts',(1.76389909571403,22.6258787994848,12.));
#246094=CARTESIAN_POINT('Ctrl Pts',(1.76418843543739,22.6169182517694,0.));
#246095=CARTESIAN_POINT('Ctrl Pts',(1.76418843543739,22.6169182517694,12.));
#246096=CARTESIAN_POINT('Ctrl Pts',(1.76443868648015,22.6081926681343,0.));
#246097=CARTESIAN_POINT('Ctrl Pts',(1.76443868648015,22.6081926681343,12.));
#246098=CARTESIAN_POINT('Ctrl Pts',(1.76465124413557,22.5997065145638,0.));
#246099=CARTESIAN_POINT('Ctrl Pts',(1.76465124413557,22.5997065145638,12.));
#246100=CARTESIAN_POINT('Ctrl Pts',(1.76482755288411,22.5914644078106,0.));
#246101=CARTESIAN_POINT('Ctrl Pts',(1.76482755288411,22.5914644078106,12.));
#246102=CARTESIAN_POINT('Ctrl Pts',(1.76496910283088,22.5834711038022,0.));
#246103=CARTESIAN_POINT('Ctrl Pts',(1.76496910283088,22.5834711038022,12.));
#246104=CARTESIAN_POINT('Ctrl Pts',(1.76507744026746,22.5757315316353,0.));
#246105=CARTESIAN_POINT('Ctrl Pts',(1.76507744026746,22.5757315316353,12.));
#246106=CARTESIAN_POINT('Ctrl Pts',(1.76515418518831,22.5682508499873,0.));
#246107=CARTESIAN_POINT('Ctrl Pts',(1.76515418518831,22.5682508499873,12.));
#246108=CARTESIAN_POINT('Ctrl Pts',(1.7652010450045,22.5610344912501,0.));
#246109=CARTESIAN_POINT('Ctrl Pts',(1.7652010450045,22.5610344912501,12.));
#246110=CARTESIAN_POINT('Ctrl Pts',(1.76521983384062,22.5540882235837,0.));
#246111=CARTESIAN_POINT('Ctrl Pts',(1.76521983384062,22.5540882235837,12.));
#246112=CARTESIAN_POINT('Ctrl Pts',(1.76521245524047,22.5474180954006,0.));
#246113=CARTESIAN_POINT('Ctrl Pts',(1.76521245524047,22.5474180954006,12.));
#246114=CARTESIAN_POINT('Ctrl Pts',(1.76518087841493,22.5410303590892,0.));
#246115=CARTESIAN_POINT('Ctrl Pts',(1.76518087841493,22.5410303590892,12.));
#246116=CARTESIAN_POINT('Ctrl Pts',(1.76512711563254,22.5349313983571,0.));
#246117=CARTESIAN_POINT('Ctrl Pts',(1.76512711563254,22.5349313983571,12.));
#246118=CARTESIAN_POINT('Ctrl Pts',(1.76505320262759,22.529127665298,0.));
#246119=CARTESIAN_POINT('Ctrl Pts',(1.76505320262759,22.529127665298,12.));
#246120=CARTESIAN_POINT('Ctrl Pts',(1.76496128643375,22.5236259635515,0.));
#246121=CARTESIAN_POINT('Ctrl Pts',(1.76496128643375,22.5236259635515,12.));
#246122=CARTESIAN_POINT('Ctrl Pts',(1.76485369319895,22.5184336670207,0.));
#246123=CARTESIAN_POINT('Ctrl Pts',(1.76485369319895,22.5184336670207,12.));
#246124=CARTESIAN_POINT('Ctrl Pts',(1.76473303281149,22.5135590569554,0.));
#246125=CARTESIAN_POINT('Ctrl Pts',(1.76473303281149,22.5135590569554,12.));
#246126=CARTESIAN_POINT('Ctrl Pts',(1.76460218257313,22.5090112700212,0.));
#246127=CARTESIAN_POINT('Ctrl Pts',(1.76460218257313,22.5090112700212,12.));
#246128=CARTESIAN_POINT('Ctrl Pts',(1.76446408210364,22.5047996391978,0.));
#246129=CARTESIAN_POINT('Ctrl Pts',(1.76446408210364,22.5047996391978,12.));
#246130=CARTESIAN_POINT('Ctrl Pts',(1.76432160068737,22.5009332677316,0.));
#246131=CARTESIAN_POINT('Ctrl Pts',(1.76432160068737,22.5009332677316,12.));
#246132=CARTESIAN_POINT('Ctrl Pts',(1.76417731243483,22.4974203063191,0.));
#246133=CARTESIAN_POINT('Ctrl Pts',(1.76417731243483,22.4974203063191,12.));
#246134=CARTESIAN_POINT('Ctrl Pts',(1.76403393880316,22.4942693792449,0.));
#246135=CARTESIAN_POINT('Ctrl Pts',(1.76403393880316,22.4942693792449,12.));
#246136=CARTESIAN_POINT('Ctrl Pts',(1.76389475965714,22.4914909094908,0.));
#246137=CARTESIAN_POINT('Ctrl Pts',(1.76389475965714,22.4914909094908,12.));
#246138=CARTESIAN_POINT('Ctrl Pts',(1.76376424879468,22.4890991659479,0.));
#246139=CARTESIAN_POINT('Ctrl Pts',(1.76376424879468,22.4890991659479,12.));
#246140=CARTESIAN_POINT('Ctrl Pts',(1.76364784232925,22.4871115206572,0.));
#246141=CARTESIAN_POINT('Ctrl Pts',(1.76364784232925,22.4871115206572,12.));
#246142=CARTESIAN_POINT('Ctrl Pts',(1.76355076045549,22.4855446605991,0.));
#246143=CARTESIAN_POINT('Ctrl Pts',(1.76355076045549,22.4855446605991,12.));
#246144=CARTESIAN_POINT('Ctrl Pts',(1.76347698284861,22.4844112933125,0.));
#246145=CARTESIAN_POINT('Ctrl Pts',(1.76347698284861,22.4844112933125,12.));
#246146=CARTESIAN_POINT('Ctrl Pts',(1.76343813434659,22.4838562517064,0.));
#246147=CARTESIAN_POINT('Ctrl Pts',(1.76343813434659,22.4838562517064,12.));
#246148=CARTESIAN_POINT('Ctrl Pts',(1.76342064263637,22.4836387052228,0.));
#246149=CARTESIAN_POINT('Ctrl Pts',(1.76342064263637,22.4836387052228,12.));
#246150=CARTESIAN_POINT('Ctrl Pts',(1.7634141553879,22.4835819929788,0.));
#246151=CARTESIAN_POINT('Ctrl Pts',(1.7634141553879,22.4835819929788,12.));
#246152=CARTESIAN_POINT('Ctrl Pts',(1.7634122053118,22.4835757167854,0.));
#246153=CARTESIAN_POINT('Ctrl Pts',(1.7634122053118,22.4835757167854,12.));
#246154=CARTESIAN_POINT('',(0.661312440730901,25.991588367311,0.));
#246155=CARTESIAN_POINT('Ctrl Pts',(0.661312440730901,25.991588367311,0.));
#246156=CARTESIAN_POINT('Ctrl Pts',(0.664028313187627,25.9865613464773,
0.));
#246157=CARTESIAN_POINT('Ctrl Pts',(0.669451306780825,25.9765104298071,
0.));
#246158=CARTESIAN_POINT('Ctrl Pts',(0.677559543209725,25.9614434297919,
0.));
#246159=CARTESIAN_POINT('Ctrl Pts',(0.688318015057729,25.9413728471909,
0.));
#246160=CARTESIAN_POINT('Ctrl Pts',(0.701678575228756,25.9163158909426,
0.));
#246161=CARTESIAN_POINT('Ctrl Pts',(0.714951588527638,25.891290261497,0.));
#246162=CARTESIAN_POINT('Ctrl Pts',(0.728137036482335,25.8662960624185,
0.));
#246163=CARTESIAN_POINT('Ctrl Pts',(0.741234902663807,25.8413334619055,
0.));
#246164=CARTESIAN_POINT('Ctrl Pts',(0.754245175609524,25.8164027059984,
0.));
#246165=CARTESIAN_POINT('Ctrl Pts',(0.767167852651168,25.7915041383376,
0.));
#246166=CARTESIAN_POINT('Ctrl Pts',(0.780002940291965,25.7666381946955,
0.));
#246167=CARTESIAN_POINT('Ctrl Pts',(0.792750451616127,25.7418053757746,
0.));
#246168=CARTESIAN_POINT('Ctrl Pts',(0.805410404554352,25.7170062262525,
0.));
#246169=CARTESIAN_POINT('Ctrl Pts',(0.817982819787464,25.6922413110194,
0.));
#246170=CARTESIAN_POINT('Ctrl Pts',(0.830467718864205,25.6675111931952,
0.));
#246171=CARTESIAN_POINT('Ctrl Pts',(0.842865122120758,25.6428164100055,
0.));
#246172=CARTESIAN_POINT('Ctrl Pts',(0.855175047036549,25.6181574536049,
0.));
#246173=CARTESIAN_POINT('Ctrl Pts',(0.867397509338431,25.5935347843585,
0.));
#246174=CARTESIAN_POINT('Ctrl Pts',(0.879532523834294,25.5689488408156,
0.));
#246175=CARTESIAN_POINT('Ctrl Pts',(0.89158010534904,25.5444000508211,0.));
#246176=CARTESIAN_POINT('Ctrl Pts',(0.903540269651106,25.5198888424194,
0.));
#246177=CARTESIAN_POINT('Ctrl Pts',(0.915413034335613,25.4954156541795,
0.));
#246178=CARTESIAN_POINT('Ctrl Pts',(0.927198419886094,25.4709809475009,
0.));
#246179=CARTESIAN_POINT('Ctrl Pts',(0.938896449496192,25.4465852044849,
0.));
#246180=CARTESIAN_POINT('Ctrl Pts',(0.950507148597468,25.4222289223167,
0.));
#246181=CARTESIAN_POINT('Ctrl Pts',(0.962030544503142,25.3979126089163,
0.));
#246182=CARTESIAN_POINT('Ctrl Pts',(0.973466666000163,25.3736367778845,
0.));
#246183=CARTESIAN_POINT('Ctrl Pts',(0.984815543003973,25.3494019441441,
0.));
#246184=CARTESIAN_POINT('Ctrl Pts',(0.996077206120624,25.3252086182968,
0.));
#246185=CARTESIAN_POINT('Ctrl Pts',(1.00725168656896,25.3010573055547,0.));
#246186=CARTESIAN_POINT('Ctrl Pts',(1.01833901642237,25.276948508726,0.));
#246187=CARTESIAN_POINT('Ctrl Pts',(1.02933922876806,25.2528827300422,0.));
#246188=CARTESIAN_POINT('Ctrl Pts',(1.04025235791507,25.2288604735086,0.));
#246189=CARTESIAN_POINT('Ctrl Pts',(1.05107843957931,25.2048822469028,0.));
#246190=CARTESIAN_POINT('Ctrl Pts',(1.06181751111768,25.1809485642192,0.));
#246191=CARTESIAN_POINT('Ctrl Pts',(1.07246961165475,25.157059946931,0.));
#246192=CARTESIAN_POINT('Ctrl Pts',(1.08303478197187,25.1332169227413,0.));
#246193=CARTESIAN_POINT('Ctrl Pts',(1.09351306445308,25.1094200248446,0.));
#246194=CARTESIAN_POINT('Ctrl Pts',(1.10390450301745,25.0856697909679,0.));
#246195=CARTESIAN_POINT('Ctrl Pts',(1.11420914306889,25.0619667625336,0.));
#246196=CARTESIAN_POINT('Ctrl Pts',(1.12442703144451,25.0383114836899,0.));
#246197=CARTESIAN_POINT('Ctrl Pts',(1.1345582163853,25.0147045006196,0.));
#246198=CARTESIAN_POINT('Ctrl Pts',(1.144602747582,24.9911463621433,0.));
#246199=CARTESIAN_POINT('Ctrl Pts',(1.15456067621889,24.9676376201502,0.));
#246200=CARTESIAN_POINT('Ctrl Pts',(1.16443205502849,24.9441788300932,0.));
#246201=CARTESIAN_POINT('Ctrl Pts',(1.17421693835041,24.9207705514449,0.));
#246202=CARTESIAN_POINT('Ctrl Pts',(1.18391538220103,24.8974133481829,0.));
#246203=CARTESIAN_POINT('Ctrl Pts',(1.19352744434064,24.8741077892075,0.));
#246204=CARTESIAN_POINT('Ctrl Pts',(1.2030531842602,24.8508544481974,0.));
#246205=CARTESIAN_POINT('Ctrl Pts',(1.21249266318208,24.8276539035092,0.));
#246206=CARTESIAN_POINT('Ctrl Pts',(1.22184594406528,24.8045067380536,0.));
#246207=CARTESIAN_POINT('Ctrl Pts',(1.23111309161843,24.7814135391799,0.));
#246208=CARTESIAN_POINT('Ctrl Pts',(1.24029417231989,24.7583748985438,0.));
#246209=CARTESIAN_POINT('Ctrl Pts',(1.24938925444325,24.7353914120011,0.));
#246210=CARTESIAN_POINT('Ctrl Pts',(1.25839840807418,24.7124636797894,0.));
#246211=CARTESIAN_POINT('Ctrl Pts',(1.267321705135,24.6895923066836,0.));
#246212=CARTESIAN_POINT('Ctrl Pts',(1.27615921941642,24.666777902156,0.));
#246213=CARTESIAN_POINT('Ctrl Pts',(1.28491102661514,24.6440210805278,0.));
#246214=CARTESIAN_POINT('Ctrl Pts',(1.29357720438107,24.6213224611229,0.));
#246215=CARTESIAN_POINT('Ctrl Pts',(1.30215783236362,24.5986826684027,0.));
#246216=CARTESIAN_POINT('Ctrl Pts',(1.31065299222021,24.5761023320183,0.));
#246217=CARTESIAN_POINT('Ctrl Pts',(1.31906276763668,24.5535820868674,0.));
#246218=CARTESIAN_POINT('Ctrl Pts',(1.32738724435326,24.5311225731435,0.));
#246219=CARTESIAN_POINT('Ctrl Pts',(1.33562651019686,24.5087244363856,0.));
#246220=CARTESIAN_POINT('Ctrl Pts',(1.34378065512337,24.4863883275134,0.));
#246221=CARTESIAN_POINT('Ctrl Pts',(1.35184977125648,24.4641149028892,0.));
#246222=CARTESIAN_POINT('Ctrl Pts',(1.35983395290627,24.4419048244523,0.));
#246223=CARTESIAN_POINT('Ctrl Pts',(1.36773329659956,24.4197587598337,0.));
#246224=CARTESIAN_POINT('Ctrl Pts',(1.37554790111609,24.3976773824732,0.));
#246225=CARTESIAN_POINT('Ctrl Pts',(1.38327786752998,24.3756613717299,0.));
#246226=CARTESIAN_POINT('Ctrl Pts',(1.39092329926388,24.3537114129875,0.));
#246227=CARTESIAN_POINT('Ctrl Pts',(1.39848430212807,24.3318281977643,0.));
#246228=CARTESIAN_POINT('Ctrl Pts',(1.40596098434337,24.3100124238311,0.));
#246229=CARTESIAN_POINT('Ctrl Pts',(1.41335345657682,24.288264795321,0.));
#246230=CARTESIAN_POINT('Ctrl Pts',(1.42066183198252,24.2665860228356,0.));
#246231=CARTESIAN_POINT('Ctrl Pts',(1.42788622624854,24.2449768235488,0.));
#246232=CARTESIAN_POINT('Ctrl Pts',(1.43502675765508,24.2234379212984,0.));
#246233=CARTESIAN_POINT('Ctrl Pts',(1.44208354711082,24.201970046722,0.));
#246234=CARTESIAN_POINT('Ctrl Pts',(1.44905671818727,24.1805739374038,0.));
#246235=CARTESIAN_POINT('Ctrl Pts',(1.45594639716317,24.1592503380107,0.));
#246236=CARTESIAN_POINT('Ctrl Pts',(1.46275271307397,24.1380000004272,0.));
#246237=CARTESIAN_POINT('Ctrl Pts',(1.46947579776991,24.1168236838824,0.));
#246238=CARTESIAN_POINT('Ctrl Pts',(1.47611578597742,24.0957221550778,0.));
#246239=CARTESIAN_POINT('Ctrl Pts',(1.48267281533683,24.0746961883528,0.));
#246240=CARTESIAN_POINT('Ctrl Pts',(1.48914702644887,24.0537465658429,0.));
#246241=CARTESIAN_POINT('Ctrl Pts',(1.49553856292801,24.0328740776331,0.));
#246242=CARTESIAN_POINT('Ctrl Pts',(1.50184757146098,24.0120795219086,0.));
#246243=CARTESIAN_POINT('Ctrl Pts',(1.50807420187694,23.9913637050927,0.));
#246244=CARTESIAN_POINT('Ctrl Pts',(1.51421860720614,23.970727442014,0.));
#246245=CARTESIAN_POINT('Ctrl Pts',(1.52028094372792,23.9501715561033,0.));
#246246=CARTESIAN_POINT('Ctrl Pts',(1.52626137103032,23.9296968795757,0.));
#246247=CARTESIAN_POINT('Ctrl Pts',(1.53216005207463,23.9093042536119,0.));
#246248=CARTESIAN_POINT('Ctrl Pts',(1.53797715326758,23.8889945285318,0.));
#246249=CARTESIAN_POINT('Ctrl Pts',(1.5437128445399,23.8687685639642,0.));
#246250=CARTESIAN_POINT('Ctrl Pts',(1.54936729940541,23.8486272290705,0.));
#246251=CARTESIAN_POINT('Ctrl Pts',(1.55494069502635,23.8285714027636,0.));
#246252=CARTESIAN_POINT('Ctrl Pts',(1.56043321228633,23.8086019739194,0.));
#246253=CARTESIAN_POINT('Ctrl Pts',(1.56584503586843,23.7887198415878,0.));
#246254=CARTESIAN_POINT('Ctrl Pts',(1.57117635434408,23.7689259151862,0.));
#246255=CARTESIAN_POINT('Ctrl Pts',(1.57642736025246,23.749221114736,0.));
#246256=CARTESIAN_POINT('Ctrl Pts',(1.58159825017358,23.72960637113,0.));
#246257=CARTESIAN_POINT('Ctrl Pts',(1.58668922481221,23.710082626383,0.));
#246258=CARTESIAN_POINT('Ctrl Pts',(1.59170048908633,23.6906508338833,0.));
#246259=CARTESIAN_POINT('Ctrl Pts',(1.59663225222463,23.671311958631,0.));
#246260=CARTESIAN_POINT('Ctrl Pts',(1.60148472786595,23.6520669774876,0.));
#246261=CARTESIAN_POINT('Ctrl Pts',(1.60625813414672,23.6329168794929,0.));
#246262=CARTESIAN_POINT('Ctrl Pts',(1.61095269379778,23.6138626661653,0.));
#246263=CARTESIAN_POINT('Ctrl Pts',(1.61556863424698,23.5949053517997,0.));
#246264=CARTESIAN_POINT('Ctrl Pts',(1.62010618772866,23.57604596376,0.));
#246265=CARTESIAN_POINT('Ctrl Pts',(1.62456559140064,23.5572855427601,0.));
#246266=CARTESIAN_POINT('Ctrl Pts',(1.62894708745223,23.538625143226,0.));
#246267=CARTESIAN_POINT('Ctrl Pts',(1.63325092321725,23.5200658336612,0.));
#246268=CARTESIAN_POINT('Ctrl Pts',(1.63747735129474,23.5016086970003,0.));
#246269=CARTESIAN_POINT('Ctrl Pts',(1.64162662967528,23.4832548309645,0.));
#246270=CARTESIAN_POINT('Ctrl Pts',(1.64569902187611,23.4650053483932,0.));
#246271=CARTESIAN_POINT('Ctrl Pts',(1.6496947970734,23.4468613776574,0.));
#246272=CARTESIAN_POINT('Ctrl Pts',(1.65361423023728,23.4288240631043,0.));
#246273=CARTESIAN_POINT('Ctrl Pts',(1.65745760227505,23.4108945654805,0.));
#246274=CARTESIAN_POINT('Ctrl Pts',(1.66122520018011,23.3930740623619,0.));
#246275=CARTESIAN_POINT('Ctrl Pts',(1.66491731718876,23.3753637485545,0.));
#246276=CARTESIAN_POINT('Ctrl Pts',(1.66853425293995,23.3577648365744,0.));
#246277=CARTESIAN_POINT('Ctrl Pts',(1.67207631363921,23.3402785571865,0.));
#246278=CARTESIAN_POINT('Ctrl Pts',(1.67554381222994,23.3229061599145,0.));
#246279=CARTESIAN_POINT('Ctrl Pts',(1.67893706857117,23.3056489135611,0.));
#246280=CARTESIAN_POINT('Ctrl Pts',(1.68225640962168,23.2885081066951,0.));
#246281=CARTESIAN_POINT('Ctrl Pts',(1.68550216963258,23.2714850482246,0.));
#246282=CARTESIAN_POINT('Ctrl Pts',(1.68867469034896,23.2545810680537,0.));
#246283=CARTESIAN_POINT('Ctrl Pts',(1.69177432121711,23.2377975177013,0.));
#246284=CARTESIAN_POINT('Ctrl Pts',(1.69480141959953,23.2211357709374,0.));
#246285=CARTESIAN_POINT('Ctrl Pts',(1.69775635099443,23.2045972243767,0.));
#246286=CARTESIAN_POINT('Ctrl Pts',(1.7006394892701,23.1881832981851,0.));
#246287=CARTESIAN_POINT('Ctrl Pts',(1.70345121691276,23.1718954368751,0.));
#246288=CARTESIAN_POINT('Ctrl Pts',(1.70619192527852,23.1557351100614,0.));
#246289=CARTESIAN_POINT('Ctrl Pts',(1.70886201485452,23.1397038132356,0.));
#246290=CARTESIAN_POINT('Ctrl Pts',(1.71146189552174,23.1238030684925,0.));
#246291=CARTESIAN_POINT('Ctrl Pts',(1.71399198684704,23.1080344254286,0.));
#246292=CARTESIAN_POINT('Ctrl Pts',(1.71645271839296,23.0923994621213,0.));
#246293=CARTESIAN_POINT('Ctrl Pts',(1.71884453003027,23.0768997860709,0.));
#246294=CARTESIAN_POINT('Ctrl Pts',(1.72116787225991,23.0615370351562,0.));
#246295=CARTESIAN_POINT('Ctrl Pts',(1.72342320653746,23.0463128785531,0.));
#246296=CARTESIAN_POINT('Ctrl Pts',(1.72561100564045,23.0312290178883,0.));
#246297=CARTESIAN_POINT('Ctrl Pts',(1.72773175404708,23.0162871884168,0.));
#246298=CARTESIAN_POINT('Ctrl Pts',(1.72978594832136,23.001489160189,0.));
#246299=CARTESIAN_POINT('Ctrl Pts',(1.7317740975019,22.9868367391978,0.));
#246300=CARTESIAN_POINT('Ctrl Pts',(1.73369672350814,22.9723317685688,0.));
#246301=CARTESIAN_POINT('Ctrl Pts',(1.73555436162769,22.9579761301063,0.));
#246302=CARTESIAN_POINT('Ctrl Pts',(1.73734756100039,22.9437717457826,0.));
#246303=CARTESIAN_POINT('Ctrl Pts',(1.73907688511666,22.9297205792586,0.));
#246304=CARTESIAN_POINT('Ctrl Pts',(1.74074291231058,22.9158246373363,0.));
#246305=CARTESIAN_POINT('Ctrl Pts',(1.7423462363008,22.9020859716141,0.));
#246306=CARTESIAN_POINT('Ctrl Pts',(1.74388746677702,22.888506680335,0.));
#246307=CARTESIAN_POINT('Ctrl Pts',(1.74536722998201,22.8750889101696,0.));
#246308=CARTESIAN_POINT('Ctrl Pts',(1.74678616930664,22.8618348580235,0.));
#246309=CARTESIAN_POINT('Ctrl Pts',(1.74814494588492,22.8487467728076,0.));
#246310=CARTESIAN_POINT('Ctrl Pts',(1.74944423940115,22.8358269579853,0.));
#246311=CARTESIAN_POINT('Ctrl Pts',(1.75068474890883,22.8230777741284,0.));
#246312=CARTESIAN_POINT('Ctrl Pts',(1.75186719365592,22.8105016414713,0.));
#246313=CARTESIAN_POINT('Ctrl Pts',(1.75299231391466,22.7981010424314,0.));
#246314=CARTESIAN_POINT('Ctrl Pts',(1.75406087182936,22.7858785242361,0.));
#246315=CARTESIAN_POINT('Ctrl Pts',(1.75507365227131,22.7738367016118,0.));
#246316=CARTESIAN_POINT('Ctrl Pts',(1.75603146371641,22.7619782595013,0.));
#246317=CARTESIAN_POINT('Ctrl Pts',(1.75693513908907,22.750305955645,0.));
#246318=CARTESIAN_POINT('Ctrl Pts',(1.75778553673244,22.7388226235559,0.));
#246319=CARTESIAN_POINT('Ctrl Pts',(1.75858354204633,22.72753117773,0.));
#246320=CARTESIAN_POINT('Ctrl Pts',(1.75933006905925,22.7164346186006,0.));
#246321=CARTESIAN_POINT('Ctrl Pts',(1.76002606202401,22.7055360375485,0.));
#246322=CARTESIAN_POINT('Ctrl Pts',(1.76067249704886,22.6948386219851,0.));
#246323=CARTESIAN_POINT('Ctrl Pts',(1.76127038310614,22.684345658525,0.));
#246324=CARTESIAN_POINT('Ctrl Pts',(1.76182076289525,22.67406053567,0.));
#246325=CARTESIAN_POINT('Ctrl Pts',(1.76232471392568,22.6639867471753,0.));
#246326=CARTESIAN_POINT('Ctrl Pts',(1.76278334912561,22.6541278938409,0.));
#246327=CARTESIAN_POINT('Ctrl Pts',(1.76319782013916,22.6444876940423,0.));
#246328=CARTESIAN_POINT('Ctrl Pts',(1.76356932176273,22.6350699979359,0.));
#246329=CARTESIAN_POINT('Ctrl Pts',(1.76389909571403,22.6258787994848,0.));
#246330=CARTESIAN_POINT('Ctrl Pts',(1.76418843543739,22.6169182517694,0.));
#246331=CARTESIAN_POINT('Ctrl Pts',(1.76443868648015,22.6081926681343,0.));
#246332=CARTESIAN_POINT('Ctrl Pts',(1.76465124413557,22.5997065145638,0.));
#246333=CARTESIAN_POINT('Ctrl Pts',(1.76482755288411,22.5914644078106,0.));
#246334=CARTESIAN_POINT('Ctrl Pts',(1.76496910283088,22.5834711038022,0.));
#246335=CARTESIAN_POINT('Ctrl Pts',(1.76507744026746,22.5757315316353,0.));
#246336=CARTESIAN_POINT('Ctrl Pts',(1.76515418518831,22.5682508499873,0.));
#246337=CARTESIAN_POINT('Ctrl Pts',(1.7652010450045,22.5610344912501,0.));
#246338=CARTESIAN_POINT('Ctrl Pts',(1.76521983384062,22.5540882235837,0.));
#246339=CARTESIAN_POINT('Ctrl Pts',(1.76521245524047,22.5474180954006,0.));
#246340=CARTESIAN_POINT('Ctrl Pts',(1.76518087841493,22.5410303590892,0.));
#246341=CARTESIAN_POINT('Ctrl Pts',(1.76512711563254,22.5349313983571,0.));
#246342=CARTESIAN_POINT('Ctrl Pts',(1.76505320262759,22.529127665298,0.));
#246343=CARTESIAN_POINT('Ctrl Pts',(1.76496128643375,22.5236259635515,0.));
#246344=CARTESIAN_POINT('Ctrl Pts',(1.76485369319895,22.5184336670207,0.));
#246345=CARTESIAN_POINT('Ctrl Pts',(1.76473303281149,22.5135590569554,0.));
#246346=CARTESIAN_POINT('Ctrl Pts',(1.76460218257313,22.5090112700212,0.));
#246347=CARTESIAN_POINT('Ctrl Pts',(1.76446408210364,22.5047996391978,0.));
#246348=CARTESIAN_POINT('Ctrl Pts',(1.76432160068737,22.5009332677316,0.));
#246349=CARTESIAN_POINT('Ctrl Pts',(1.76417731243483,22.4974203063191,0.));
#246350=CARTESIAN_POINT('Ctrl Pts',(1.76403393880316,22.4942693792449,0.));
#246351=CARTESIAN_POINT('Ctrl Pts',(1.76389475965714,22.4914909094908,0.));
#246352=CARTESIAN_POINT('Ctrl Pts',(1.76376424879468,22.4890991659479,0.));
#246353=CARTESIAN_POINT('Ctrl Pts',(1.76364784232925,22.4871115206572,0.));
#246354=CARTESIAN_POINT('Ctrl Pts',(1.76355076045549,22.4855446605991,0.));
#246355=CARTESIAN_POINT('Ctrl Pts',(1.76347698284861,22.4844112933125,0.));
#246356=CARTESIAN_POINT('Ctrl Pts',(1.76343813434659,22.4838562517064,0.));
#246357=CARTESIAN_POINT('Ctrl Pts',(1.76342064263637,22.4836387052228,0.));
#246358=CARTESIAN_POINT('Ctrl Pts',(1.7634141553879,22.4835819929788,0.));
#246359=CARTESIAN_POINT('Ctrl Pts',(1.7634122053118,22.4835757167854,0.));
#246360=CARTESIAN_POINT('',(0.661312440730901,25.991588367311,12.));
#246361=CARTESIAN_POINT('',(0.661312440730901,25.991588367311,0.));
#246362=CARTESIAN_POINT('Ctrl Pts',(1.7634122053118,22.4835757167854,12.));
#246363=CARTESIAN_POINT('Ctrl Pts',(1.7634141553879,22.4835819929788,12.));
#246364=CARTESIAN_POINT('Ctrl Pts',(1.76342064263637,22.4836387052228,12.));
#246365=CARTESIAN_POINT('Ctrl Pts',(1.76343813434659,22.4838562517064,12.));
#246366=CARTESIAN_POINT('Ctrl Pts',(1.76347698284861,22.4844112933125,12.));
#246367=CARTESIAN_POINT('Ctrl Pts',(1.76355076045549,22.4855446605991,12.));
#246368=CARTESIAN_POINT('Ctrl Pts',(1.76364784232925,22.4871115206572,12.));
#246369=CARTESIAN_POINT('Ctrl Pts',(1.76376424879468,22.4890991659479,12.));
#246370=CARTESIAN_POINT('Ctrl Pts',(1.76389475965714,22.4914909094908,12.));
#246371=CARTESIAN_POINT('Ctrl Pts',(1.76403393880316,22.4942693792449,12.));
#246372=CARTESIAN_POINT('Ctrl Pts',(1.76417731243483,22.4974203063191,12.));
#246373=CARTESIAN_POINT('Ctrl Pts',(1.76432160068737,22.5009332677316,12.));
#246374=CARTESIAN_POINT('Ctrl Pts',(1.76446408210364,22.5047996391978,12.));
#246375=CARTESIAN_POINT('Ctrl Pts',(1.76460218257313,22.5090112700212,12.));
#246376=CARTESIAN_POINT('Ctrl Pts',(1.76473303281149,22.5135590569554,12.));
#246377=CARTESIAN_POINT('Ctrl Pts',(1.76485369319895,22.5184336670207,12.));
#246378=CARTESIAN_POINT('Ctrl Pts',(1.76496128643375,22.5236259635515,12.));
#246379=CARTESIAN_POINT('Ctrl Pts',(1.76505320262759,22.529127665298,12.));
#246380=CARTESIAN_POINT('Ctrl Pts',(1.76512711563254,22.5349313983571,12.));
#246381=CARTESIAN_POINT('Ctrl Pts',(1.76518087841493,22.5410303590892,12.));
#246382=CARTESIAN_POINT('Ctrl Pts',(1.76521245524047,22.5474180954006,12.));
#246383=CARTESIAN_POINT('Ctrl Pts',(1.76521983384062,22.5540882235837,12.));
#246384=CARTESIAN_POINT('Ctrl Pts',(1.7652010450045,22.5610344912501,12.));
#246385=CARTESIAN_POINT('Ctrl Pts',(1.76515418518831,22.5682508499873,12.));
#246386=CARTESIAN_POINT('Ctrl Pts',(1.76507744026746,22.5757315316353,12.));
#246387=CARTESIAN_POINT('Ctrl Pts',(1.76496910283088,22.5834711038022,12.));
#246388=CARTESIAN_POINT('Ctrl Pts',(1.76482755288411,22.5914644078106,12.));
#246389=CARTESIAN_POINT('Ctrl Pts',(1.76465124413557,22.5997065145638,12.));
#246390=CARTESIAN_POINT('Ctrl Pts',(1.76443868648015,22.6081926681343,12.));
#246391=CARTESIAN_POINT('Ctrl Pts',(1.76418843543739,22.6169182517694,12.));
#246392=CARTESIAN_POINT('Ctrl Pts',(1.76389909571403,22.6258787994848,12.));
#246393=CARTESIAN_POINT('Ctrl Pts',(1.76356932176273,22.6350699979359,12.));
#246394=CARTESIAN_POINT('Ctrl Pts',(1.76319782013916,22.6444876940423,12.));
#246395=CARTESIAN_POINT('Ctrl Pts',(1.76278334912561,22.6541278938409,12.));
#246396=CARTESIAN_POINT('Ctrl Pts',(1.76232471392568,22.6639867471753,12.));
#246397=CARTESIAN_POINT('Ctrl Pts',(1.76182076289525,22.67406053567,12.));
#246398=CARTESIAN_POINT('Ctrl Pts',(1.76127038310614,22.684345658525,12.));
#246399=CARTESIAN_POINT('Ctrl Pts',(1.76067249704886,22.6948386219851,12.));
#246400=CARTESIAN_POINT('Ctrl Pts',(1.76002606202401,22.7055360375485,12.));
#246401=CARTESIAN_POINT('Ctrl Pts',(1.75933006905925,22.7164346186006,12.));
#246402=CARTESIAN_POINT('Ctrl Pts',(1.75858354204633,22.72753117773,12.));
#246403=CARTESIAN_POINT('Ctrl Pts',(1.75778553673244,22.7388226235559,12.));
#246404=CARTESIAN_POINT('Ctrl Pts',(1.75693513908907,22.750305955645,12.));
#246405=CARTESIAN_POINT('Ctrl Pts',(1.75603146371641,22.7619782595013,12.));
#246406=CARTESIAN_POINT('Ctrl Pts',(1.75507365227131,22.7738367016118,12.));
#246407=CARTESIAN_POINT('Ctrl Pts',(1.75406087182936,22.7858785242361,12.));
#246408=CARTESIAN_POINT('Ctrl Pts',(1.75299231391466,22.7981010424314,12.));
#246409=CARTESIAN_POINT('Ctrl Pts',(1.75186719365592,22.8105016414713,12.));
#246410=CARTESIAN_POINT('Ctrl Pts',(1.75068474890883,22.8230777741284,12.));
#246411=CARTESIAN_POINT('Ctrl Pts',(1.74944423940115,22.8358269579853,12.));
#246412=CARTESIAN_POINT('Ctrl Pts',(1.74814494588492,22.8487467728076,12.));
#246413=CARTESIAN_POINT('Ctrl Pts',(1.74678616930664,22.8618348580235,12.));
#246414=CARTESIAN_POINT('Ctrl Pts',(1.74536722998201,22.8750889101696,12.));
#246415=CARTESIAN_POINT('Ctrl Pts',(1.74388746677702,22.888506680335,12.));
#246416=CARTESIAN_POINT('Ctrl Pts',(1.7423462363008,22.9020859716141,12.));
#246417=CARTESIAN_POINT('Ctrl Pts',(1.74074291231058,22.9158246373363,12.));
#246418=CARTESIAN_POINT('Ctrl Pts',(1.73907688511666,22.9297205792586,12.));
#246419=CARTESIAN_POINT('Ctrl Pts',(1.73734756100039,22.9437717457826,12.));
#246420=CARTESIAN_POINT('Ctrl Pts',(1.73555436162769,22.9579761301063,12.));
#246421=CARTESIAN_POINT('Ctrl Pts',(1.73369672350814,22.9723317685688,12.));
#246422=CARTESIAN_POINT('Ctrl Pts',(1.7317740975019,22.9868367391978,12.));
#246423=CARTESIAN_POINT('Ctrl Pts',(1.72978594832136,23.001489160189,12.));
#246424=CARTESIAN_POINT('Ctrl Pts',(1.72773175404708,23.0162871884168,12.));
#246425=CARTESIAN_POINT('Ctrl Pts',(1.72561100564045,23.0312290178883,12.));
#246426=CARTESIAN_POINT('Ctrl Pts',(1.72342320653746,23.0463128785531,12.));
#246427=CARTESIAN_POINT('Ctrl Pts',(1.72116787225991,23.0615370351562,12.));
#246428=CARTESIAN_POINT('Ctrl Pts',(1.71884453003027,23.0768997860709,12.));
#246429=CARTESIAN_POINT('Ctrl Pts',(1.71645271839296,23.0923994621213,12.));
#246430=CARTESIAN_POINT('Ctrl Pts',(1.71399198684704,23.1080344254286,12.));
#246431=CARTESIAN_POINT('Ctrl Pts',(1.71146189552174,23.1238030684925,12.));
#246432=CARTESIAN_POINT('Ctrl Pts',(1.70886201485452,23.1397038132356,12.));
#246433=CARTESIAN_POINT('Ctrl Pts',(1.70619192527852,23.1557351100614,12.));
#246434=CARTESIAN_POINT('Ctrl Pts',(1.70345121691276,23.1718954368751,12.));
#246435=CARTESIAN_POINT('Ctrl Pts',(1.7006394892701,23.1881832981851,12.));
#246436=CARTESIAN_POINT('Ctrl Pts',(1.69775635099443,23.2045972243767,12.));
#246437=CARTESIAN_POINT('Ctrl Pts',(1.69480141959953,23.2211357709374,12.));
#246438=CARTESIAN_POINT('Ctrl Pts',(1.69177432121711,23.2377975177013,12.));
#246439=CARTESIAN_POINT('Ctrl Pts',(1.68867469034896,23.2545810680537,12.));
#246440=CARTESIAN_POINT('Ctrl Pts',(1.68550216963258,23.2714850482246,12.));
#246441=CARTESIAN_POINT('Ctrl Pts',(1.68225640962168,23.2885081066951,12.));
#246442=CARTESIAN_POINT('Ctrl Pts',(1.67893706857117,23.3056489135611,12.));
#246443=CARTESIAN_POINT('Ctrl Pts',(1.67554381222994,23.3229061599145,12.));
#246444=CARTESIAN_POINT('Ctrl Pts',(1.67207631363921,23.3402785571865,12.));
#246445=CARTESIAN_POINT('Ctrl Pts',(1.66853425293995,23.3577648365744,12.));
#246446=CARTESIAN_POINT('Ctrl Pts',(1.66491731718876,23.3753637485545,12.));
#246447=CARTESIAN_POINT('Ctrl Pts',(1.66122520018011,23.3930740623619,12.));
#246448=CARTESIAN_POINT('Ctrl Pts',(1.65745760227505,23.4108945654805,12.));
#246449=CARTESIAN_POINT('Ctrl Pts',(1.65361423023728,23.4288240631043,12.));
#246450=CARTESIAN_POINT('Ctrl Pts',(1.6496947970734,23.4468613776574,12.));
#246451=CARTESIAN_POINT('Ctrl Pts',(1.64569902187611,23.4650053483932,12.));
#246452=CARTESIAN_POINT('Ctrl Pts',(1.64162662967528,23.4832548309645,12.));
#246453=CARTESIAN_POINT('Ctrl Pts',(1.63747735129474,23.5016086970003,12.));
#246454=CARTESIAN_POINT('Ctrl Pts',(1.63325092321725,23.5200658336612,12.));
#246455=CARTESIAN_POINT('Ctrl Pts',(1.62894708745223,23.538625143226,12.));
#246456=CARTESIAN_POINT('Ctrl Pts',(1.62456559140064,23.5572855427601,12.));
#246457=CARTESIAN_POINT('Ctrl Pts',(1.62010618772866,23.57604596376,12.));
#246458=CARTESIAN_POINT('Ctrl Pts',(1.61556863424698,23.5949053517997,12.));
#246459=CARTESIAN_POINT('Ctrl Pts',(1.61095269379778,23.6138626661653,12.));
#246460=CARTESIAN_POINT('Ctrl Pts',(1.60625813414672,23.6329168794929,12.));
#246461=CARTESIAN_POINT('Ctrl Pts',(1.60148472786595,23.6520669774876,12.));
#246462=CARTESIAN_POINT('Ctrl Pts',(1.59663225222463,23.671311958631,12.));
#246463=CARTESIAN_POINT('Ctrl Pts',(1.59170048908633,23.6906508338833,12.));
#246464=CARTESIAN_POINT('Ctrl Pts',(1.58668922481221,23.710082626383,12.));
#246465=CARTESIAN_POINT('Ctrl Pts',(1.58159825017358,23.72960637113,12.));
#246466=CARTESIAN_POINT('Ctrl Pts',(1.57642736025246,23.749221114736,12.));
#246467=CARTESIAN_POINT('Ctrl Pts',(1.57117635434408,23.7689259151862,12.));
#246468=CARTESIAN_POINT('Ctrl Pts',(1.56584503586843,23.7887198415878,12.));
#246469=CARTESIAN_POINT('Ctrl Pts',(1.56043321228633,23.8086019739194,12.));
#246470=CARTESIAN_POINT('Ctrl Pts',(1.55494069502635,23.8285714027636,12.));
#246471=CARTESIAN_POINT('Ctrl Pts',(1.54936729940541,23.8486272290705,12.));
#246472=CARTESIAN_POINT('Ctrl Pts',(1.5437128445399,23.8687685639642,12.));
#246473=CARTESIAN_POINT('Ctrl Pts',(1.53797715326758,23.8889945285318,12.));
#246474=CARTESIAN_POINT('Ctrl Pts',(1.53216005207463,23.9093042536119,12.));
#246475=CARTESIAN_POINT('Ctrl Pts',(1.52626137103032,23.9296968795757,12.));
#246476=CARTESIAN_POINT('Ctrl Pts',(1.52028094372792,23.9501715561033,12.));
#246477=CARTESIAN_POINT('Ctrl Pts',(1.51421860720614,23.970727442014,12.));
#246478=CARTESIAN_POINT('Ctrl Pts',(1.50807420187694,23.9913637050927,12.));
#246479=CARTESIAN_POINT('Ctrl Pts',(1.50184757146098,24.0120795219086,12.));
#246480=CARTESIAN_POINT('Ctrl Pts',(1.49553856292801,24.0328740776331,12.));
#246481=CARTESIAN_POINT('Ctrl Pts',(1.48914702644887,24.0537465658429,12.));
#246482=CARTESIAN_POINT('Ctrl Pts',(1.48267281533683,24.0746961883528,12.));
#246483=CARTESIAN_POINT('Ctrl Pts',(1.47611578597742,24.0957221550778,12.));
#246484=CARTESIAN_POINT('Ctrl Pts',(1.46947579776991,24.1168236838824,12.));
#246485=CARTESIAN_POINT('Ctrl Pts',(1.46275271307397,24.1380000004272,12.));
#246486=CARTESIAN_POINT('Ctrl Pts',(1.45594639716317,24.1592503380107,12.));
#246487=CARTESIAN_POINT('Ctrl Pts',(1.44905671818727,24.1805739374038,12.));
#246488=CARTESIAN_POINT('Ctrl Pts',(1.44208354711082,24.201970046722,12.));
#246489=CARTESIAN_POINT('Ctrl Pts',(1.43502675765508,24.2234379212984,12.));
#246490=CARTESIAN_POINT('Ctrl Pts',(1.42788622624854,24.2449768235488,12.));
#246491=CARTESIAN_POINT('Ctrl Pts',(1.42066183198252,24.2665860228356,12.));
#246492=CARTESIAN_POINT('Ctrl Pts',(1.41335345657682,24.288264795321,12.));
#246493=CARTESIAN_POINT('Ctrl Pts',(1.40596098434337,24.3100124238311,12.));
#246494=CARTESIAN_POINT('Ctrl Pts',(1.39848430212807,24.3318281977643,12.));
#246495=CARTESIAN_POINT('Ctrl Pts',(1.39092329926388,24.3537114129875,12.));
#246496=CARTESIAN_POINT('Ctrl Pts',(1.38327786752998,24.3756613717299,12.));
#246497=CARTESIAN_POINT('Ctrl Pts',(1.37554790111609,24.3976773824732,12.));
#246498=CARTESIAN_POINT('Ctrl Pts',(1.36773329659956,24.4197587598337,12.));
#246499=CARTESIAN_POINT('Ctrl Pts',(1.35983395290627,24.4419048244523,12.));
#246500=CARTESIAN_POINT('Ctrl Pts',(1.35184977125648,24.4641149028892,12.));
#246501=CARTESIAN_POINT('Ctrl Pts',(1.34378065512337,24.4863883275134,12.));
#246502=CARTESIAN_POINT('Ctrl Pts',(1.33562651019686,24.5087244363856,12.));
#246503=CARTESIAN_POINT('Ctrl Pts',(1.32738724435326,24.5311225731435,12.));
#246504=CARTESIAN_POINT('Ctrl Pts',(1.31906276763668,24.5535820868674,12.));
#246505=CARTESIAN_POINT('Ctrl Pts',(1.31065299222021,24.5761023320183,12.));
#246506=CARTESIAN_POINT('Ctrl Pts',(1.30215783236362,24.5986826684027,12.));
#246507=CARTESIAN_POINT('Ctrl Pts',(1.29357720438107,24.6213224611229,12.));
#246508=CARTESIAN_POINT('Ctrl Pts',(1.28491102661514,24.6440210805278,12.));
#246509=CARTESIAN_POINT('Ctrl Pts',(1.27615921941642,24.666777902156,12.));
#246510=CARTESIAN_POINT('Ctrl Pts',(1.267321705135,24.6895923066836,12.));
#246511=CARTESIAN_POINT('Ctrl Pts',(1.25839840807418,24.7124636797894,12.));
#246512=CARTESIAN_POINT('Ctrl Pts',(1.24938925444325,24.7353914120011,12.));
#246513=CARTESIAN_POINT('Ctrl Pts',(1.24029417231989,24.7583748985438,12.));
#246514=CARTESIAN_POINT('Ctrl Pts',(1.23111309161843,24.7814135391799,12.));
#246515=CARTESIAN_POINT('Ctrl Pts',(1.22184594406528,24.8045067380536,12.));
#246516=CARTESIAN_POINT('Ctrl Pts',(1.21249266318208,24.8276539035092,12.));
#246517=CARTESIAN_POINT('Ctrl Pts',(1.2030531842602,24.8508544481974,12.));
#246518=CARTESIAN_POINT('Ctrl Pts',(1.19352744434064,24.8741077892075,12.));
#246519=CARTESIAN_POINT('Ctrl Pts',(1.18391538220103,24.8974133481829,12.));
#246520=CARTESIAN_POINT('Ctrl Pts',(1.17421693835041,24.9207705514449,12.));
#246521=CARTESIAN_POINT('Ctrl Pts',(1.16443205502849,24.9441788300932,12.));
#246522=CARTESIAN_POINT('Ctrl Pts',(1.15456067621889,24.9676376201502,12.));
#246523=CARTESIAN_POINT('Ctrl Pts',(1.144602747582,24.9911463621433,12.));
#246524=CARTESIAN_POINT('Ctrl Pts',(1.1345582163853,25.0147045006196,12.));
#246525=CARTESIAN_POINT('Ctrl Pts',(1.12442703144451,25.0383114836899,12.));
#246526=CARTESIAN_POINT('Ctrl Pts',(1.11420914306889,25.0619667625336,12.));
#246527=CARTESIAN_POINT('Ctrl Pts',(1.10390450301745,25.0856697909679,12.));
#246528=CARTESIAN_POINT('Ctrl Pts',(1.09351306445308,25.1094200248446,12.));
#246529=CARTESIAN_POINT('Ctrl Pts',(1.08303478197187,25.1332169227413,12.));
#246530=CARTESIAN_POINT('Ctrl Pts',(1.07246961165475,25.157059946931,12.));
#246531=CARTESIAN_POINT('Ctrl Pts',(1.06181751111768,25.1809485642192,12.));
#246532=CARTESIAN_POINT('Ctrl Pts',(1.05107843957931,25.2048822469028,12.));
#246533=CARTESIAN_POINT('Ctrl Pts',(1.04025235791507,25.2288604735086,12.));
#246534=CARTESIAN_POINT('Ctrl Pts',(1.02933922876806,25.2528827300422,12.));
#246535=CARTESIAN_POINT('Ctrl Pts',(1.01833901642237,25.276948508726,12.));
#246536=CARTESIAN_POINT('Ctrl Pts',(1.00725168656896,25.3010573055547,12.));
#246537=CARTESIAN_POINT('Ctrl Pts',(0.996077206120624,25.3252086182968,
12.));
#246538=CARTESIAN_POINT('Ctrl Pts',(0.984815543003973,25.3494019441441,
12.));
#246539=CARTESIAN_POINT('Ctrl Pts',(0.973466666000163,25.3736367778845,
12.));
#246540=CARTESIAN_POINT('Ctrl Pts',(0.962030544503142,25.3979126089163,
12.));
#246541=CARTESIAN_POINT('Ctrl Pts',(0.950507148597468,25.4222289223167,
12.));
#246542=CARTESIAN_POINT('Ctrl Pts',(0.938896449496192,25.4465852044849,
12.));
#246543=CARTESIAN_POINT('Ctrl Pts',(0.927198419886094,25.4709809475009,
12.));
#246544=CARTESIAN_POINT('Ctrl Pts',(0.915413034335613,25.4954156541795,
12.));
#246545=CARTESIAN_POINT('Ctrl Pts',(0.903540269651106,25.5198888424194,
12.));
#246546=CARTESIAN_POINT('Ctrl Pts',(0.89158010534904,25.5444000508211,12.));
#246547=CARTESIAN_POINT('Ctrl Pts',(0.879532523834294,25.5689488408156,
12.));
#246548=CARTESIAN_POINT('Ctrl Pts',(0.867397509338431,25.5935347843585,
12.));
#246549=CARTESIAN_POINT('Ctrl Pts',(0.855175047036549,25.6181574536049,
12.));
#246550=CARTESIAN_POINT('Ctrl Pts',(0.842865122120758,25.6428164100055,
12.));
#246551=CARTESIAN_POINT('Ctrl Pts',(0.830467718864205,25.6675111931952,
12.));
#246552=CARTESIAN_POINT('Ctrl Pts',(0.817982819787464,25.6922413110194,
12.));
#246553=CARTESIAN_POINT('Ctrl Pts',(0.805410404554352,25.7170062262525,
12.));
#246554=CARTESIAN_POINT('Ctrl Pts',(0.792750451616127,25.7418053757746,
12.));
#246555=CARTESIAN_POINT('Ctrl Pts',(0.780002940291965,25.7666381946955,
12.));
#246556=CARTESIAN_POINT('Ctrl Pts',(0.767167852651168,25.7915041383376,
12.));
#246557=CARTESIAN_POINT('Ctrl Pts',(0.754245175609524,25.8164027059984,
12.));
#246558=CARTESIAN_POINT('Ctrl Pts',(0.741234902663807,25.8413334619055,
12.));
#246559=CARTESIAN_POINT('Ctrl Pts',(0.728137036482335,25.8662960624185,
12.));
#246560=CARTESIAN_POINT('Ctrl Pts',(0.714951588527638,25.891290261497,12.));
#246561=CARTESIAN_POINT('Ctrl Pts',(0.701678575228756,25.9163158909426,
12.));
#246562=CARTESIAN_POINT('Ctrl Pts',(0.688318015057729,25.9413728471909,
12.));
#246563=CARTESIAN_POINT('Ctrl Pts',(0.677559543209725,25.9614434297919,
12.));
#246564=CARTESIAN_POINT('Ctrl Pts',(0.669451306780825,25.9765104298071,
12.));
#246565=CARTESIAN_POINT('Ctrl Pts',(0.664028313187627,25.9865613464773,
12.));
#246566=CARTESIAN_POINT('Ctrl Pts',(0.661312440730901,25.991588367311,12.));
#246567=CARTESIAN_POINT('Ctrl Pts',(4.11585220600461,22.1738711152697,0.));
#246568=CARTESIAN_POINT('Ctrl Pts',(4.11585220600461,22.1738711152697,12.));
#246569=CARTESIAN_POINT('Ctrl Pts',(4.11585194677442,22.173877682324,0.));
#246570=CARTESIAN_POINT('Ctrl Pts',(4.11585194677442,22.173877682324,12.));
#246571=CARTESIAN_POINT('Ctrl Pts',(4.11586035878287,22.1739341411687,0.));
#246572=CARTESIAN_POINT('Ctrl Pts',(4.11586035878287,22.1739341411687,12.));
#246573=CARTESIAN_POINT('Ctrl Pts',(4.11589976826166,22.1741488021234,0.));
#246574=CARTESIAN_POINT('Ctrl Pts',(4.11589976826166,22.1741488021234,12.));
#246575=CARTESIAN_POINT('Ctrl Pts',(4.11600589882845,22.1746949858775,0.));
#246576=CARTESIAN_POINT('Ctrl Pts',(4.11600589882845,22.1746949858775,12.));
#246577=CARTESIAN_POINT('Ctrl Pts',(4.11622797217068,22.1758088296598,0.));
#246578=CARTESIAN_POINT('Ctrl Pts',(4.11622797217068,22.1758088296598,12.));
#246579=CARTESIAN_POINT('Ctrl Pts',(4.11653973150518,22.177347426894,0.));
#246580=CARTESIAN_POINT('Ctrl Pts',(4.11653973150518,22.177347426894,12.));
#246581=CARTESIAN_POINT('Ctrl Pts',(4.11694173195003,22.179297473024,0.));
#246582=CARTESIAN_POINT('Ctrl Pts',(4.11694173195003,22.179297473024,12.));
#246583=CARTESIAN_POINT('Ctrl Pts',(4.11743469691756,22.1816414985788,0.));
#246584=CARTESIAN_POINT('Ctrl Pts',(4.11743469691756,22.1816414985788,12.));
#246585=CARTESIAN_POINT('Ctrl Pts',(4.11801938107479,22.1843613164855,0.));
#246586=CARTESIAN_POINT('Ctrl Pts',(4.11801938107479,22.1843613164855,12.));
#246587=CARTESIAN_POINT('Ctrl Pts',(4.11869641271773,22.1874419861496,0.));
#246588=CARTESIAN_POINT('Ctrl Pts',(4.11869641271773,22.1874419861496,12.));
#246589=CARTESIAN_POINT('Ctrl Pts',(4.11946626228636,22.1908725908525,0.));
#246590=CARTESIAN_POINT('Ctrl Pts',(4.11946626228636,22.1908725908525,12.));
#246591=CARTESIAN_POINT('Ctrl Pts',(4.12032932637736,22.1946440958098,0.));
#246592=CARTESIAN_POINT('Ctrl Pts',(4.12032932637736,22.1946440958098,12.));
#246593=CARTESIAN_POINT('Ctrl Pts',(4.12128598183522,22.1987479618246,0.));
#246594=CARTESIAN_POINT('Ctrl Pts',(4.12128598183522,22.1987479618246,12.));
#246595=CARTESIAN_POINT('Ctrl Pts',(4.12233664408227,22.2031746532106,0.));
#246596=CARTESIAN_POINT('Ctrl Pts',(4.12233664408227,22.2031746532106,12.));
#246597=CARTESIAN_POINT('Ctrl Pts',(4.12348173702023,22.2079143941719,0.));
#246598=CARTESIAN_POINT('Ctrl Pts',(4.12348173702023,22.2079143941719,12.));
#246599=CARTESIAN_POINT('Ctrl Pts',(4.12472167516607,22.2129576146671,0.));
#246600=CARTESIAN_POINT('Ctrl Pts',(4.12472167516607,22.2129576146671,12.));
#246601=CARTESIAN_POINT('Ctrl Pts',(4.12605683613307,22.2182956401341,0.));
#246602=CARTESIAN_POINT('Ctrl Pts',(4.12605683613307,22.2182956401341,12.));
#246603=CARTESIAN_POINT('Ctrl Pts',(4.12748755830104,22.2239207458781,0.));
#246604=CARTESIAN_POINT('Ctrl Pts',(4.12748755830104,22.2239207458781,12.));
#246605=CARTESIAN_POINT('Ctrl Pts',(4.12901415463379,22.2298258043947,0.));
#246606=CARTESIAN_POINT('Ctrl Pts',(4.12901415463379,22.2298258043947,12.));
#246607=CARTESIAN_POINT('Ctrl Pts',(4.13063692157498,22.2360040565533,0.));
#246608=CARTESIAN_POINT('Ctrl Pts',(4.13063692157498,22.2360040565533,12.));
#246609=CARTESIAN_POINT('Ctrl Pts',(4.1323561506016,22.2424488153523,0.));
#246610=CARTESIAN_POINT('Ctrl Pts',(4.1323561506016,22.2424488153523,12.));
#246611=CARTESIAN_POINT('Ctrl Pts',(4.1341721255881,22.249153531779,0.));
#246612=CARTESIAN_POINT('Ctrl Pts',(4.1341721255881,22.249153531779,12.));
#246613=CARTESIAN_POINT('Ctrl Pts',(4.13608511977225,22.2561118708421,0.));
#246614=CARTESIAN_POINT('Ctrl Pts',(4.13608511977225,22.2561118708421,12.));
#246615=CARTESIAN_POINT('Ctrl Pts',(4.13809539255421,22.2633177913972,0.));
#246616=CARTESIAN_POINT('Ctrl Pts',(4.13809539255421,22.2633177913972,12.));
#246617=CARTESIAN_POINT('Ctrl Pts',(4.14020318715991,22.2707656042457,0.));
#246618=CARTESIAN_POINT('Ctrl Pts',(4.14020318715991,22.2707656042457,12.));
#246619=CARTESIAN_POINT('Ctrl Pts',(4.14240873321984,22.2784499072027,0.));
#246620=CARTESIAN_POINT('Ctrl Pts',(4.14240873321984,22.2784499072027,12.));
#246621=CARTESIAN_POINT('Ctrl Pts',(4.14471224859295,22.2863655389166,0.));
#246622=CARTESIAN_POINT('Ctrl Pts',(4.14471224859295,22.2863655389166,12.));
#246623=CARTESIAN_POINT('Ctrl Pts',(4.14711394168556,22.2945075198467,0.));
#246624=CARTESIAN_POINT('Ctrl Pts',(4.14711394168556,22.2945075198467,12.));
#246625=CARTESIAN_POINT('Ctrl Pts',(4.14961401285522,22.3028710166933,0.));
#246626=CARTESIAN_POINT('Ctrl Pts',(4.14961401285522,22.3028710166933,12.));
#246627=CARTESIAN_POINT('Ctrl Pts',(4.1522126539699,22.3114513545185,0.));
#246628=CARTESIAN_POINT('Ctrl Pts',(4.1522126539699,22.3114513545185,12.));
#246629=CARTESIAN_POINT('Ctrl Pts',(4.15491004835281,22.3202440186979,0.));
#246630=CARTESIAN_POINT('Ctrl Pts',(4.15491004835281,22.3202440186979,12.));
#246631=CARTESIAN_POINT('Ctrl Pts',(4.15770637047889,22.3292446628959,0.));
#246632=CARTESIAN_POINT('Ctrl Pts',(4.15770637047889,22.3292446628959,12.));
#246633=CARTESIAN_POINT('Ctrl Pts',(4.16060178604164,22.3384491078602,0.));
#246634=CARTESIAN_POINT('Ctrl Pts',(4.16060178604164,22.3384491078602,12.));
#246635=CARTESIAN_POINT('Ctrl Pts',(4.16359645263187,22.3478533253889,0.));
#246636=CARTESIAN_POINT('Ctrl Pts',(4.16359645263187,22.3478533253889,12.));
#246637=CARTESIAN_POINT('Ctrl Pts',(4.166690520266,22.3574534257396,0.));
#246638=CARTESIAN_POINT('Ctrl Pts',(4.166690520266,22.3574534257396,12.));
#246639=CARTESIAN_POINT('Ctrl Pts',(4.16988413199457,22.36724564276,0.));
#246640=CARTESIAN_POINT('Ctrl Pts',(4.16988413199457,22.36724564276,12.));
#246641=CARTESIAN_POINT('Ctrl Pts',(4.17317742436145,22.3772263228617,0.));
#246642=CARTESIAN_POINT('Ctrl Pts',(4.17317742436145,22.3772263228617,12.));
#246643=CARTESIAN_POINT('Ctrl Pts',(4.17657052752825,22.3873919231334,0.));
#246644=CARTESIAN_POINT('Ctrl Pts',(4.17657052752825,22.3873919231334,12.));
#246645=CARTESIAN_POINT('Ctrl Pts',(4.18006356544882,22.3977390078075,0.));
#246646=CARTESIAN_POINT('Ctrl Pts',(4.18006356544882,22.3977390078075,12.));
#246647=CARTESIAN_POINT('Ctrl Pts',(4.1836566560085,22.4082642454453,0.));
#246648=CARTESIAN_POINT('Ctrl Pts',(4.1836566560085,22.4082642454453,12.));
#246649=CARTESIAN_POINT('Ctrl Pts',(4.1873499111772,22.4189644056115,0.));
#246650=CARTESIAN_POINT('Ctrl Pts',(4.1873499111772,22.4189644056115,12.));
#246651=CARTESIAN_POINT('Ctrl Pts',(4.19114343726941,22.4298363535421,0.));
#246652=CARTESIAN_POINT('Ctrl Pts',(4.19114343726941,22.4298363535421,12.));
#246653=CARTESIAN_POINT('Ctrl Pts',(4.1950373351886,22.4408770448917,0.));
#246654=CARTESIAN_POINT('Ctrl Pts',(4.1950373351886,22.4408770448917,12.));
#246655=CARTESIAN_POINT('Ctrl Pts',(4.19903170066354,22.4520835205419,0.));
#246656=CARTESIAN_POINT('Ctrl Pts',(4.19903170066354,22.4520835205419,12.));
#246657=CARTESIAN_POINT('Ctrl Pts',(4.2031266244817,22.4634529011433,0.));
#246658=CARTESIAN_POINT('Ctrl Pts',(4.2031266244817,22.4634529011433,12.));
#246659=CARTESIAN_POINT('Ctrl Pts',(4.20732219265648,22.4749823839915,0.));
#246660=CARTESIAN_POINT('Ctrl Pts',(4.20732219265648,22.4749823839915,12.));
#246661=CARTESIAN_POINT('Ctrl Pts',(4.21161848657428,22.4866692403147,0.));
#246662=CARTESIAN_POINT('Ctrl Pts',(4.21161848657428,22.4866692403147,12.));
#246663=CARTESIAN_POINT('Ctrl Pts',(4.21601558313908,22.4985108124229,0.));
#246664=CARTESIAN_POINT('Ctrl Pts',(4.21601558313908,22.4985108124229,12.));
#246665=CARTESIAN_POINT('Ctrl Pts',(4.22051355490196,22.5105045108882,0.));
#246666=CARTESIAN_POINT('Ctrl Pts',(4.22051355490196,22.5105045108882,12.));
#246667=CARTESIAN_POINT('Ctrl Pts',(4.2251124702004,22.5226478117885,0.));
#246668=CARTESIAN_POINT('Ctrl Pts',(4.2251124702004,22.5226478117885,12.));
#246669=CARTESIAN_POINT('Ctrl Pts',(4.22981239330731,22.5349382540587,0.));
#246670=CARTESIAN_POINT('Ctrl Pts',(4.22981239330731,22.5349382540587,12.));
#246671=CARTESIAN_POINT('Ctrl Pts',(4.23461338456713,22.5473734368086,0.));
#246672=CARTESIAN_POINT('Ctrl Pts',(4.23461338456713,22.5473734368086,12.));
#246673=CARTESIAN_POINT('Ctrl Pts',(4.23951550052526,22.559951016643,0.));
#246674=CARTESIAN_POINT('Ctrl Pts',(4.23951550052526,22.559951016643,12.));
#246675=CARTESIAN_POINT('Ctrl Pts',(4.24451879404858,22.5726687049922,0.));
#246676=CARTESIAN_POINT('Ctrl Pts',(4.24451879404858,22.5726687049922,12.));
#246677=CARTESIAN_POINT('Ctrl Pts',(4.24962331444184,22.5855242662479,0.));
#246678=CARTESIAN_POINT('Ctrl Pts',(4.24962331444184,22.5855242662479,12.));
#246679=CARTESIAN_POINT('Ctrl Pts',(4.25482910755485,22.5985155158637,0.));
#246680=CARTESIAN_POINT('Ctrl Pts',(4.25482910755485,22.5985155158637,12.));
#246681=CARTESIAN_POINT('Ctrl Pts',(4.26013621588303,22.611640318482,0.));
#246682=CARTESIAN_POINT('Ctrl Pts',(4.26013621588303,22.611640318482,12.));
#246683=CARTESIAN_POINT('Ctrl Pts',(4.26554467865571,22.6248965859975,0.));
#246684=CARTESIAN_POINT('Ctrl Pts',(4.26554467865571,22.6248965859975,12.));
#246685=CARTESIAN_POINT('Ctrl Pts',(4.27105453192999,22.6382822758171,0.));
#246686=CARTESIAN_POINT('Ctrl Pts',(4.27105453192999,22.6382822758171,12.));
#246687=CARTESIAN_POINT('Ctrl Pts',(4.27666580869117,22.6517953893303,0.));
#246688=CARTESIAN_POINT('Ctrl Pts',(4.27666580869117,22.6517953893303,12.));
#246689=CARTESIAN_POINT('Ctrl Pts',(4.28237853894059,22.665433970311,0.));
#246690=CARTESIAN_POINT('Ctrl Pts',(4.28237853894059,22.665433970311,12.));
#246691=CARTESIAN_POINT('Ctrl Pts',(4.28819274977766,22.6791961033537,0.));
#246692=CARTESIAN_POINT('Ctrl Pts',(4.28819274977766,22.6791961033537,12.));
#246693=CARTESIAN_POINT('Ctrl Pts',(4.29410846547061,22.6930799122545,0.));
#246694=CARTESIAN_POINT('Ctrl Pts',(4.29410846547061,22.6930799122545,12.));
#246695=CARTESIAN_POINT('Ctrl Pts',(4.30012570754066,22.707083558756,0.));
#246696=CARTESIAN_POINT('Ctrl Pts',(4.30012570754066,22.707083558756,12.));
#246697=CARTESIAN_POINT('Ctrl Pts',(4.30624449484074,22.7212052413384,0.));
#246698=CARTESIAN_POINT('Ctrl Pts',(4.30624449484074,22.7212052413384,12.));
#246699=CARTESIAN_POINT('Ctrl Pts',(4.3124648436255,22.7354431939927,0.));
#246700=CARTESIAN_POINT('Ctrl Pts',(4.3124648436255,22.7354431939927,12.));
#246701=CARTESIAN_POINT('Ctrl Pts',(4.3187867676123,22.7497956849852,0.));
#246702=CARTESIAN_POINT('Ctrl Pts',(4.3187867676123,22.7497956849852,12.));
#246703=CARTESIAN_POINT('Ctrl Pts',(4.32521027803747,22.764261015648,0.));
#246704=CARTESIAN_POINT('Ctrl Pts',(4.32521027803747,22.764261015648,12.));
#246705=CARTESIAN_POINT('Ctrl Pts',(4.33173538373182,22.7788375194081,0.));
#246706=CARTESIAN_POINT('Ctrl Pts',(4.33173538373182,22.7788375194081,12.));
#246707=CARTESIAN_POINT('Ctrl Pts',(4.33836209118442,22.7935235607807,0.));
#246708=CARTESIAN_POINT('Ctrl Pts',(4.33836209118442,22.7935235607807,12.));
#246709=CARTESIAN_POINT('Ctrl Pts',(4.34509040460065,22.808317534379,0.));
#246710=CARTESIAN_POINT('Ctrl Pts',(4.34509040460065,22.808317534379,12.));
#246711=CARTESIAN_POINT('Ctrl Pts',(4.35192032594801,22.8232178638873,0.));
#246712=CARTESIAN_POINT('Ctrl Pts',(4.35192032594801,22.8232178638873,12.));
#246713=CARTESIAN_POINT('Ctrl Pts',(4.35885185500559,22.838223001118,0.));
#246714=CARTESIAN_POINT('Ctrl Pts',(4.35885185500559,22.838223001118,12.));
#246715=CARTESIAN_POINT('Ctrl Pts',(4.36588498943009,22.8533314252419,0.));
#246716=CARTESIAN_POINT('Ctrl Pts',(4.36588498943009,22.8533314252419,12.));
#246717=CARTESIAN_POINT('Ctrl Pts',(4.37301972480752,22.8685416419725,0.));
#246718=CARTESIAN_POINT('Ctrl Pts',(4.37301972480752,22.8685416419725,12.));
#246719=CARTESIAN_POINT('Ctrl Pts',(4.38025605470089,22.8838521827702,0.));
#246720=CARTESIAN_POINT('Ctrl Pts',(4.38025605470089,22.8838521827702,12.));
#246721=CARTESIAN_POINT('Ctrl Pts',(4.38759397068391,22.8992616040108,0.));
#246722=CARTESIAN_POINT('Ctrl Pts',(4.38759397068391,22.8992616040108,12.));
#246723=CARTESIAN_POINT('Ctrl Pts',(4.39503346238454,22.9147684862425,0.));
#246724=CARTESIAN_POINT('Ctrl Pts',(4.39503346238454,22.9147684862425,12.));
#246725=CARTESIAN_POINT('Ctrl Pts',(4.40257451754307,22.9303714335549,0.));
#246726=CARTESIAN_POINT('Ctrl Pts',(4.40257451754307,22.9303714335549,12.));
#246727=CARTESIAN_POINT('Ctrl Pts',(4.41021712205547,22.9460690729093,0.));
#246728=CARTESIAN_POINT('Ctrl Pts',(4.41021712205547,22.9460690729093,12.));
#246729=CARTESIAN_POINT('Ctrl Pts',(4.41796126001309,22.9618600534866,0.));
#246730=CARTESIAN_POINT('Ctrl Pts',(4.41796126001309,22.9618600534866,12.));
#246731=CARTESIAN_POINT('Ctrl Pts',(4.42580691372771,22.9777430460021,0.));
#246732=CARTESIAN_POINT('Ctrl Pts',(4.42580691372771,22.9777430460021,12.));
#246733=CARTESIAN_POINT('Ctrl Pts',(4.43375406376904,22.9937167421009,0.));
#246734=CARTESIAN_POINT('Ctrl Pts',(4.43375406376904,22.9937167421009,12.));
#246735=CARTESIAN_POINT('Ctrl Pts',(4.44180268901666,23.0097798538399,0.));
#246736=CARTESIAN_POINT('Ctrl Pts',(4.44180268901666,23.0097798538399,12.));
#246737=CARTESIAN_POINT('Ctrl Pts',(4.44995276669698,23.0259311131395,0.));
#246738=CARTESIAN_POINT('Ctrl Pts',(4.44995276669698,23.0259311131395,12.));
#246739=CARTESIAN_POINT('Ctrl Pts',(4.45820427241676,23.0421692712466,0.));
#246740=CARTESIAN_POINT('Ctrl Pts',(4.45820427241676,23.0421692712466,12.));
#246741=CARTESIAN_POINT('Ctrl Pts',(4.46655718018205,23.0584930981723,0.));
#246742=CARTESIAN_POINT('Ctrl Pts',(4.46655718018205,23.0584930981723,12.));
#246743=CARTESIAN_POINT('Ctrl Pts',(4.47501146242821,23.0749013821868,0.));
#246744=CARTESIAN_POINT('Ctrl Pts',(4.47501146242821,23.0749013821868,12.));
#246745=CARTESIAN_POINT('Ctrl Pts',(4.48356709006756,23.0913929293909,0.));
#246746=CARTESIAN_POINT('Ctrl Pts',(4.48356709006756,23.0913929293909,12.));
#246747=CARTESIAN_POINT('Ctrl Pts',(4.49222403252201,23.1079665632629,0.));
#246748=CARTESIAN_POINT('Ctrl Pts',(4.49222403252201,23.1079665632629,12.));
#246749=CARTESIAN_POINT('Ctrl Pts',(4.50098225775178,23.1246211242117,0.));
#246750=CARTESIAN_POINT('Ctrl Pts',(4.50098225775178,23.1246211242117,12.));
#246751=CARTESIAN_POINT('Ctrl Pts',(4.50984173227087,23.1413554691136,0.));
#246752=CARTESIAN_POINT('Ctrl Pts',(4.50984173227087,23.1413554691136,12.));
#246753=CARTESIAN_POINT('Ctrl Pts',(4.51880242116785,23.1581684708778,0.));
#246754=CARTESIAN_POINT('Ctrl Pts',(4.51880242116785,23.1581684708778,12.));
#246755=CARTESIAN_POINT('Ctrl Pts',(4.52786428815047,23.1750590180923,0.));
#246756=CARTESIAN_POINT('Ctrl Pts',(4.52786428815047,23.1750590180923,12.));
#246757=CARTESIAN_POINT('Ctrl Pts',(4.53702729557585,23.1920260146474,0.));
#246758=CARTESIAN_POINT('Ctrl Pts',(4.53702729557585,23.1920260146474,12.));
#246759=CARTESIAN_POINT('Ctrl Pts',(4.54629140447542,23.2090683793627,0.));
#246760=CARTESIAN_POINT('Ctrl Pts',(4.54629140447542,23.2090683793627,12.));
#246761=CARTESIAN_POINT('Ctrl Pts',(4.55565657456956,23.2261850456055,0.));
#246762=CARTESIAN_POINT('Ctrl Pts',(4.55565657456956,23.2261850456055,12.));
#246763=CARTESIAN_POINT('Ctrl Pts',(4.5651227642781,23.2433749609117,0.));
#246764=CARTESIAN_POINT('Ctrl Pts',(4.5651227642781,23.2433749609117,12.));
#246765=CARTESIAN_POINT('Ctrl Pts',(4.5746899307607,23.2606370866853,0.));
#246766=CARTESIAN_POINT('Ctrl Pts',(4.5746899307607,23.2606370866853,12.));
#246767=CARTESIAN_POINT('Ctrl Pts',(4.58435802994674,23.2779703978868,0.));
#246768=CARTESIAN_POINT('Ctrl Pts',(4.58435802994674,23.2779703978868,12.));
#246769=CARTESIAN_POINT('Ctrl Pts',(4.59412701655749,23.295373882719,0.));
#246770=CARTESIAN_POINT('Ctrl Pts',(4.59412701655749,23.295373882719,12.));
#246771=CARTESIAN_POINT('Ctrl Pts',(4.60399684412174,23.3128465423119,0.));
#246772=CARTESIAN_POINT('Ctrl Pts',(4.60399684412174,23.3128465423119,12.));
#246773=CARTESIAN_POINT('Ctrl Pts',(4.61396746497848,23.3303873903947,0.));
#246774=CARTESIAN_POINT('Ctrl Pts',(4.61396746497848,23.3303873903947,12.));
#246775=CARTESIAN_POINT('Ctrl Pts',(4.62403883030823,23.3479954530281,0.));
#246776=CARTESIAN_POINT('Ctrl Pts',(4.62403883030823,23.3479954530281,12.));
#246777=CARTESIAN_POINT('Ctrl Pts',(4.63421089016554,23.3656697683496,0.));
#246778=CARTESIAN_POINT('Ctrl Pts',(4.63421089016554,23.3656697683496,12.));
#246779=CARTESIAN_POINT('Ctrl Pts',(4.64448359349935,23.383409386307,0.));
#246780=CARTESIAN_POINT('Ctrl Pts',(4.64448359349935,23.383409386307,12.));
#246781=CARTESIAN_POINT('Ctrl Pts',(4.65485688816921,23.4012133683957,0.));
#246782=CARTESIAN_POINT('Ctrl Pts',(4.65485688816921,23.4012133683957,12.));
#246783=CARTESIAN_POINT('Ctrl Pts',(4.66533072094663,23.4190807873798,0.));
#246784=CARTESIAN_POINT('Ctrl Pts',(4.66533072094663,23.4190807873798,12.));
#246785=CARTESIAN_POINT('Ctrl Pts',(4.6759050375305,23.4370107270444,0.));
#246786=CARTESIAN_POINT('Ctrl Pts',(4.6759050375305,23.4370107270444,12.));
#246787=CARTESIAN_POINT('Ctrl Pts',(4.68657978258297,23.4550022819853,0.));
#246788=CARTESIAN_POINT('Ctrl Pts',(4.68657978258297,23.4550022819853,12.));
#246789=CARTESIAN_POINT('Ctrl Pts',(4.69735489975023,23.4730545573849,0.));
#246790=CARTESIAN_POINT('Ctrl Pts',(4.69735489975023,23.4730545573849,12.));
#246791=CARTESIAN_POINT('Ctrl Pts',(4.7082303316782,23.491166668789,0.));
#246792=CARTESIAN_POINT('Ctrl Pts',(4.7082303316782,23.491166668789,12.));
#246793=CARTESIAN_POINT('Ctrl Pts',(4.71920602001904,23.5093377418784,0.));
#246794=CARTESIAN_POINT('Ctrl Pts',(4.71920602001904,23.5093377418784,12.));
#246795=CARTESIAN_POINT('Ctrl Pts',(4.73028190543031,23.5275669122378,0.));
#246796=CARTESIAN_POINT('Ctrl Pts',(4.73028190543031,23.5275669122378,12.));
#246797=CARTESIAN_POINT('Ctrl Pts',(4.74145792760698,23.5458533251715,0.));
#246798=CARTESIAN_POINT('Ctrl Pts',(4.74145792760698,23.5458533251715,12.));
#246799=CARTESIAN_POINT('Ctrl Pts',(4.75273402530615,23.564196135517,0.));
#246800=CARTESIAN_POINT('Ctrl Pts',(4.75273402530615,23.564196135517,12.));
#246801=CARTESIAN_POINT('Ctrl Pts',(4.7641101363625,23.5825945074535,0.));
#246802=CARTESIAN_POINT('Ctrl Pts',(4.7641101363625,23.5825945074535,12.));
#246803=CARTESIAN_POINT('Ctrl Pts',(4.77558619769875,23.6010476143099,0.));
#246804=CARTESIAN_POINT('Ctrl Pts',(4.77558619769875,23.6010476143099,12.));
#246805=CARTESIAN_POINT('Ctrl Pts',(4.78716214532104,23.6195546383625,0.));
#246806=CARTESIAN_POINT('Ctrl Pts',(4.78716214532104,23.6195546383625,12.));
#246807=CARTESIAN_POINT('Ctrl Pts',(4.79883791433229,23.6381147706581,0.));
#246808=CARTESIAN_POINT('Ctrl Pts',(4.79883791433229,23.6381147706581,12.));
#246809=CARTESIAN_POINT('Ctrl Pts',(4.81061343896442,23.6567272108631,0.));
#246810=CARTESIAN_POINT('Ctrl Pts',(4.81061343896442,23.6567272108631,12.));
#246811=CARTESIAN_POINT('Ctrl Pts',(4.82248865259569,23.6753911671023,0.));
#246812=CARTESIAN_POINT('Ctrl Pts',(4.82248865259569,23.6753911671023,12.));
#246813=CARTESIAN_POINT('Ctrl Pts',(4.83446348776267,23.6941058557971,0.));
#246814=CARTESIAN_POINT('Ctrl Pts',(4.83446348776267,23.6941058557971,12.));
#246815=CARTESIAN_POINT('Ctrl Pts',(4.84653787616422,23.7128705015014,0.));
#246816=CARTESIAN_POINT('Ctrl Pts',(4.84653787616422,23.7128705015014,12.));
#246817=CARTESIAN_POINT('Ctrl Pts',(4.85871174865491,23.7316843367308,0.));
#246818=CARTESIAN_POINT('Ctrl Pts',(4.85871174865491,23.7316843367308,12.));
#246819=CARTESIAN_POINT('Ctrl Pts',(4.87098503527142,23.7505466018239,0.));
#246820=CARTESIAN_POINT('Ctrl Pts',(4.87098503527142,23.7505466018239,12.));
#246821=CARTESIAN_POINT('Ctrl Pts',(4.88335766525565,23.7694565448044,0.));
#246822=CARTESIAN_POINT('Ctrl Pts',(4.88335766525565,23.7694565448044,12.));
#246823=CARTESIAN_POINT('Ctrl Pts',(4.89582956706771,23.7884134212381,0.));
#246824=CARTESIAN_POINT('Ctrl Pts',(4.89582956706771,23.7884134212381,12.));
#246825=CARTESIAN_POINT('Ctrl Pts',(4.90840066839346,23.8074164940897,0.));
#246826=CARTESIAN_POINT('Ctrl Pts',(4.90840066839346,23.8074164940897,12.));
#246827=CARTESIAN_POINT('Ctrl Pts',(4.92107089613976,23.8264650335721,0.));
#246828=CARTESIAN_POINT('Ctrl Pts',(4.92107089613976,23.8264650335721,12.));
#246829=CARTESIAN_POINT('Ctrl Pts',(4.93384017643441,23.8455583170062,0.));
#246830=CARTESIAN_POINT('Ctrl Pts',(4.93384017643441,23.8455583170062,12.));
#246831=CARTESIAN_POINT('Ctrl Pts',(4.94670843465868,23.8646956287172,0.));
#246832=CARTESIAN_POINT('Ctrl Pts',(4.94670843465868,23.8646956287172,12.));
#246833=CARTESIAN_POINT('Ctrl Pts',(4.95967559546565,23.883876259922,0.));
#246834=CARTESIAN_POINT('Ctrl Pts',(4.95967559546565,23.883876259922,12.));
#246835=CARTESIAN_POINT('Ctrl Pts',(4.97274158279228,23.9030995086164,0.));
#246836=CARTESIAN_POINT('Ctrl Pts',(4.97274158279228,23.9030995086164,12.));
#246837=CARTESIAN_POINT('Ctrl Pts',(4.98590631986532,23.9223646794591,0.));
#246838=CARTESIAN_POINT('Ctrl Pts',(4.98590631986532,23.9223646794591,12.));
#246839=CARTESIAN_POINT('Ctrl Pts',(4.99916972919309,23.9416710836529,0.));
#246840=CARTESIAN_POINT('Ctrl Pts',(4.99916972919309,23.9416710836529,12.));
#246841=CARTESIAN_POINT('Ctrl Pts',(5.01253173257458,23.9610180388271,0.));
#246842=CARTESIAN_POINT('Ctrl Pts',(5.01253173257458,23.9610180388271,12.));
#246843=CARTESIAN_POINT('Ctrl Pts',(5.02599225112461,23.9804048689228,0.));
#246844=CARTESIAN_POINT('Ctrl Pts',(5.02599225112461,23.9804048689228,12.));
#246845=CARTESIAN_POINT('Ctrl Pts',(5.03955120528527,23.9998309040747,0.));
#246846=CARTESIAN_POINT('Ctrl Pts',(5.03955120528527,23.9998309040747,12.));
#246847=CARTESIAN_POINT('Ctrl Pts',(5.05320851483068,24.0192954804896,0.));
#246848=CARTESIAN_POINT('Ctrl Pts',(5.05320851483068,24.0192954804896,12.));
#246849=CARTESIAN_POINT('Ctrl Pts',(5.06696409886639,24.0387979403268,0.));
#246850=CARTESIAN_POINT('Ctrl Pts',(5.06696409886639,24.0387979403268,12.));
#246851=CARTESIAN_POINT('Ctrl Pts',(5.0808178758127,24.0583376315636,0.));
#246852=CARTESIAN_POINT('Ctrl Pts',(5.0808178758127,24.0583376315636,12.));
#246853=CARTESIAN_POINT('Ctrl Pts',(5.09476976342616,24.0779139079264,0.));
#246854=CARTESIAN_POINT('Ctrl Pts',(5.09476976342616,24.0779139079264,12.));
#246855=CARTESIAN_POINT('Ctrl Pts',(5.10881967883124,24.0975261288444,0.));
#246856=CARTESIAN_POINT('Ctrl Pts',(5.10881967883124,24.0975261288444,12.));
#246857=CARTESIAN_POINT('Ctrl Pts',(5.12296753853857,24.117173659394,0.));
#246858=CARTESIAN_POINT('Ctrl Pts',(5.12296753853857,24.117173659394,12.));
#246859=CARTESIAN_POINT('Ctrl Pts',(5.13721325845745,24.1368558702443,0.));
#246860=CARTESIAN_POINT('Ctrl Pts',(5.13721325845745,24.1368558702443,12.));
#246861=CARTESIAN_POINT('Ctrl Pts',(5.15155675390079,24.1565721375971,0.));
#246862=CARTESIAN_POINT('Ctrl Pts',(5.15155675390079,24.1565721375971,12.));
#246863=CARTESIAN_POINT('Ctrl Pts',(5.16599793957985,24.1763218431344,0.));
#246864=CARTESIAN_POINT('Ctrl Pts',(5.16599793957985,24.1763218431344,12.));
#246865=CARTESIAN_POINT('Ctrl Pts',(5.18053672961398,24.1961043738756,0.));
#246866=CARTESIAN_POINT('Ctrl Pts',(5.18053672961398,24.1961043738756,12.));
#246867=CARTESIAN_POINT('Ctrl Pts',(5.19517303753647,24.2159191220171,0.));
#246868=CARTESIAN_POINT('Ctrl Pts',(5.19517303753647,24.2159191220171,12.));
#246869=CARTESIAN_POINT('Ctrl Pts',(5.20990677629176,24.2357654847766,0.));
#246870=CARTESIAN_POINT('Ctrl Pts',(5.20990677629176,24.2357654847766,12.));
#246871=CARTESIAN_POINT('Ctrl Pts',(5.22473785822442,24.2556428642294,0.));
#246872=CARTESIAN_POINT('Ctrl Pts',(5.22473785822442,24.2556428642294,12.));
#246873=CARTESIAN_POINT('Ctrl Pts',(5.23966619506289,24.2755506671525,0.));
#246874=CARTESIAN_POINT('Ctrl Pts',(5.23966619506289,24.2755506671525,12.));
#246875=CARTESIAN_POINT('Ctrl Pts',(5.25469169788856,24.2954883048447,0.));
#246876=CARTESIAN_POINT('Ctrl Pts',(5.25469169788856,24.2954883048447,12.));
#246877=CARTESIAN_POINT('Ctrl Pts',(5.26981427718798,24.3154551932221,0.));
#246878=CARTESIAN_POINT('Ctrl Pts',(5.26981427718798,24.3154551932221,12.));
#246879=CARTESIAN_POINT('Ctrl Pts',(5.28503384290648,24.3354507529414,0.));
#246880=CARTESIAN_POINT('Ctrl Pts',(5.28503384290648,24.3354507529414,12.));
#246881=CARTESIAN_POINT('Ctrl Pts',(5.30035030449063,24.3554744095075,0.));
#246882=CARTESIAN_POINT('Ctrl Pts',(5.30035030449063,24.3554744095075,12.));
#246883=CARTESIAN_POINT('Ctrl Pts',(5.31576357092526,24.3755255933917,0.));
#246884=CARTESIAN_POINT('Ctrl Pts',(5.31576357092526,24.3755255933917,12.));
#246885=CARTESIAN_POINT('Ctrl Pts',(5.33127355076033,24.3956037401293,0.));
#246886=CARTESIAN_POINT('Ctrl Pts',(5.33127355076033,24.3956037401293,12.));
#246887=CARTESIAN_POINT('Ctrl Pts',(5.34688015213537,24.4157082904614,0.));
#246888=CARTESIAN_POINT('Ctrl Pts',(5.34688015213537,24.4157082904614,12.));
#246889=CARTESIAN_POINT('Ctrl Pts',(5.36258328273627,24.435838689915,0.));
#246890=CARTESIAN_POINT('Ctrl Pts',(5.36258328273627,24.435838689915,12.));
#246891=CARTESIAN_POINT('Ctrl Pts',(5.37838284973695,24.4559943883157,0.));
#246892=CARTESIAN_POINT('Ctrl Pts',(5.37838284973695,24.4559943883157,12.));
#246893=CARTESIAN_POINT('Ctrl Pts',(5.39427875973824,24.4761748393321,0.));
#246894=CARTESIAN_POINT('Ctrl Pts',(5.39427875973824,24.4761748393321,12.));
#246895=CARTESIAN_POINT('Ctrl Pts',(5.41027091869241,24.4963794999831,0.));
#246896=CARTESIAN_POINT('Ctrl Pts',(5.41027091869241,24.4963794999831,12.));
#246897=CARTESIAN_POINT('Ctrl Pts',(5.42635923183419,24.5166078302108,0.));
#246898=CARTESIAN_POINT('Ctrl Pts',(5.42635923183419,24.5166078302108,12.));
#246899=CARTESIAN_POINT('Ctrl Pts',(5.4425436035688,24.5368592922863,0.));
#246900=CARTESIAN_POINT('Ctrl Pts',(5.4425436035688,24.5368592922863,12.));
#246901=CARTESIAN_POINT('Ctrl Pts',(5.45882393762261,24.5571333514842,0.));
#246902=CARTESIAN_POINT('Ctrl Pts',(5.45882393762261,24.5571333514842,12.));
#246903=CARTESIAN_POINT('Ctrl Pts',(5.47520013724419,24.5774294770329,0.));
#246904=CARTESIAN_POINT('Ctrl Pts',(5.47520013724419,24.5774294770329,12.));
#246905=CARTESIAN_POINT('Ctrl Pts',(5.49167210537246,24.5977471429364,0.));
#246906=CARTESIAN_POINT('Ctrl Pts',(5.49167210537246,24.5977471429364,12.));
#246907=CARTESIAN_POINT('Ctrl Pts',(5.50823974481962,24.6180858289179,0.));
#246908=CARTESIAN_POINT('Ctrl Pts',(5.50823974481962,24.6180858289179,12.));
#246909=CARTESIAN_POINT('Ctrl Pts',(5.52490295840991,24.6384450211467,0.));
#246910=CARTESIAN_POINT('Ctrl Pts',(5.52490295840991,24.6384450211467,12.));
#246911=CARTESIAN_POINT('Ctrl Pts',(5.54166164919583,24.6588242134738,0.));
#246912=CARTESIAN_POINT('Ctrl Pts',(5.54166164919583,24.6588242134738,12.));
#246913=CARTESIAN_POINT('Ctrl Pts',(5.55851572025376,24.6792229061794,0.));
#246914=CARTESIAN_POINT('Ctrl Pts',(5.55851572025376,24.6792229061794,12.));
#246915=CARTESIAN_POINT('Ctrl Pts',(5.57546507427754,24.6996406035517,0.));
#246916=CARTESIAN_POINT('Ctrl Pts',(5.57546507427754,24.6996406035517,12.));
#246917=CARTESIAN_POINT('Ctrl Pts',(5.59250961323987,24.7200768119088,0.));
#246918=CARTESIAN_POINT('Ctrl Pts',(5.59250961323987,24.7200768119088,12.));
#246919=CARTESIAN_POINT('Ctrl Pts',(5.60964923798491,24.7405310372739,0.));
#246920=CARTESIAN_POINT('Ctrl Pts',(5.60964923798491,24.7405310372739,12.));
#246921=CARTESIAN_POINT('Ctrl Pts',(5.62688384790923,24.7610027835697,0.));
#246922=CARTESIAN_POINT('Ctrl Pts',(5.62688384790923,24.7610027835697,12.));
#246923=CARTESIAN_POINT('Ctrl Pts',(5.6442133404226,24.781491549672,0.));
#246924=CARTESIAN_POINT('Ctrl Pts',(5.6442133404226,24.781491549672,12.));
#246925=CARTESIAN_POINT('Ctrl Pts',(5.66163761114921,24.8019968304605,0.));
#246926=CARTESIAN_POINT('Ctrl Pts',(5.66163761114921,24.8019968304605,12.));
#246927=CARTESIAN_POINT('Ctrl Pts',(5.67915655496542,24.8225181223845,0.));
#246928=CARTESIAN_POINT('Ctrl Pts',(5.67915655496542,24.8225181223845,12.));
#246929=CARTESIAN_POINT('Ctrl Pts',(5.69677006679444,24.8430549277621,0.));
#246930=CARTESIAN_POINT('Ctrl Pts',(5.69677006679444,24.8430549277621,12.));
#246931=CARTESIAN_POINT('Ctrl Pts',(5.71447804252027,24.8636067597669,0.));
#246932=CARTESIAN_POINT('Ctrl Pts',(5.71447804252027,24.8636067597669,12.));
#246933=CARTESIAN_POINT('Ctrl Pts',(5.73228037976926,24.884173146722,0.));
#246934=CARTESIAN_POINT('Ctrl Pts',(5.73228037976926,24.884173146722,12.));
#246935=CARTESIAN_POINT('Ctrl Pts',(5.75017697890804,24.904753637648,0.));
#246936=CARTESIAN_POINT('Ctrl Pts',(5.75017697890804,24.904753637648,12.));
#246937=CARTESIAN_POINT('Ctrl Pts',(5.76816774342219,24.9253478043656,0.));
#246938=CARTESIAN_POINT('Ctrl Pts',(5.76816774342219,24.9253478043656,12.));
#246939=CARTESIAN_POINT('Ctrl Pts',(5.78625257775681,24.945955229334,0.));
#246940=CARTESIAN_POINT('Ctrl Pts',(5.78625257775681,24.945955229334,12.));
#246941=CARTESIAN_POINT('Ctrl Pts',(5.80443138549726,24.9665754954496,0.));
#246942=CARTESIAN_POINT('Ctrl Pts',(5.80443138549726,24.9665754954496,12.));
#246943=CARTESIAN_POINT('Ctrl Pts',(5.82270406744198,24.9872081752734,0.));
#246944=CARTESIAN_POINT('Ctrl Pts',(5.82270406744198,24.9872081752734,12.));
#246945=CARTESIAN_POINT('Ctrl Pts',(5.84107051963071,25.0078528200564,0.));
#246946=CARTESIAN_POINT('Ctrl Pts',(5.84107051963071,25.0078528200564,12.));
#246947=CARTESIAN_POINT('Ctrl Pts',(5.85953063156826,25.0285089498899,0.));
#246948=CARTESIAN_POINT('Ctrl Pts',(5.85953063156826,25.0285089498899,12.));
#246949=CARTESIAN_POINT('Ctrl Pts',(5.87808428385365,25.0491760405911,0.));
#246950=CARTESIAN_POINT('Ctrl Pts',(5.87808428385365,25.0491760405911,12.));
#246951=CARTESIAN_POINT('Ctrl Pts',(5.89673135155514,25.0698535426514,0.));
#246952=CARTESIAN_POINT('Ctrl Pts',(5.89673135155514,25.0698535426514,12.));
#246953=CARTESIAN_POINT('Ctrl Pts',(5.91547170844447,25.0905409050773,0.));
#246954=CARTESIAN_POINT('Ctrl Pts',(5.91547170844447,25.0905409050773,12.));
#246955=CARTESIAN_POINT('Ctrl Pts',(5.93430523086834,25.1112375971106,0.));
#246956=CARTESIAN_POINT('Ctrl Pts',(5.93430523086834,25.1112375971106,12.));
#246957=CARTESIAN_POINT('Ctrl Pts',(5.95323180187378,25.1319431317237,0.));
#246958=CARTESIAN_POINT('Ctrl Pts',(5.95323180187378,25.1319431317237,12.));
#246959=CARTESIAN_POINT('Ctrl Pts',(5.97225131495616,25.1526570863092,0.));
#246960=CARTESIAN_POINT('Ctrl Pts',(5.97225131495616,25.1526570863092,12.));
#246961=CARTESIAN_POINT('Ctrl Pts',(5.99136367859754,25.1733791296259,0.));
#246962=CARTESIAN_POINT('Ctrl Pts',(5.99136367859754,25.1733791296259,12.));
#246963=CARTESIAN_POINT('Ctrl Pts',(6.01056881804612,25.1941090269819,0.));
#246964=CARTESIAN_POINT('Ctrl Pts',(6.01056881804612,25.1941090269819,12.));
#246965=CARTESIAN_POINT('Ctrl Pts',(6.02986667389996,25.21484662016,0.));
#246966=CARTESIAN_POINT('Ctrl Pts',(6.02986667389996,25.21484662016,12.));
#246967=CARTESIAN_POINT('Ctrl Pts',(6.04925720151218,25.2355918139032,0.));
#246968=CARTESIAN_POINT('Ctrl Pts',(6.04925720151218,25.2355918139032,12.));
#246969=CARTESIAN_POINT('Ctrl Pts',(6.06484373634546,25.2521940105705,0.));
#246970=CARTESIAN_POINT('Ctrl Pts',(6.06484373634546,25.2521940105705,12.));
#246971=CARTESIAN_POINT('Ctrl Pts',(6.0765753178749,25.2646490489923,0.));
#246972=CARTESIAN_POINT('Ctrl Pts',(6.0765753178749,25.2646490489923,12.));
#246973=CARTESIAN_POINT('Ctrl Pts',(6.08441489609793,25.2729539149517,0.));
#246974=CARTESIAN_POINT('Ctrl Pts',(6.08441489609793,25.2729539149517,12.));
#246975=CARTESIAN_POINT('Ctrl Pts',(6.08833931617699,25.2771067246846,0.));
#246976=CARTESIAN_POINT('Ctrl Pts',(6.08833931617699,25.2771067246846,12.));
#246977=CARTESIAN_POINT('',(6.08833931617699,25.2771067246846,0.));
#246978=CARTESIAN_POINT('Ctrl Pts',(4.11585220600461,22.1738711152697,0.));
#246979=CARTESIAN_POINT('Ctrl Pts',(4.11585194677442,22.173877682324,0.));
#246980=CARTESIAN_POINT('Ctrl Pts',(4.11586035878287,22.1739341411687,0.));
#246981=CARTESIAN_POINT('Ctrl Pts',(4.11589976826166,22.1741488021234,0.));
#246982=CARTESIAN_POINT('Ctrl Pts',(4.11600589882845,22.1746949858775,0.));
#246983=CARTESIAN_POINT('Ctrl Pts',(4.11622797217068,22.1758088296598,0.));
#246984=CARTESIAN_POINT('Ctrl Pts',(4.11653973150518,22.177347426894,0.));
#246985=CARTESIAN_POINT('Ctrl Pts',(4.11694173195003,22.179297473024,0.));
#246986=CARTESIAN_POINT('Ctrl Pts',(4.11743469691756,22.1816414985788,0.));
#246987=CARTESIAN_POINT('Ctrl Pts',(4.11801938107479,22.1843613164855,0.));
#246988=CARTESIAN_POINT('Ctrl Pts',(4.11869641271773,22.1874419861496,0.));
#246989=CARTESIAN_POINT('Ctrl Pts',(4.11946626228636,22.1908725908525,0.));
#246990=CARTESIAN_POINT('Ctrl Pts',(4.12032932637736,22.1946440958098,0.));
#246991=CARTESIAN_POINT('Ctrl Pts',(4.12128598183522,22.1987479618246,0.));
#246992=CARTESIAN_POINT('Ctrl Pts',(4.12233664408227,22.2031746532106,0.));
#246993=CARTESIAN_POINT('Ctrl Pts',(4.12348173702023,22.2079143941719,0.));
#246994=CARTESIAN_POINT('Ctrl Pts',(4.12472167516607,22.2129576146671,0.));
#246995=CARTESIAN_POINT('Ctrl Pts',(4.12605683613307,22.2182956401341,0.));
#246996=CARTESIAN_POINT('Ctrl Pts',(4.12748755830104,22.2239207458781,0.));
#246997=CARTESIAN_POINT('Ctrl Pts',(4.12901415463379,22.2298258043947,0.));
#246998=CARTESIAN_POINT('Ctrl Pts',(4.13063692157498,22.2360040565533,0.));
#246999=CARTESIAN_POINT('Ctrl Pts',(4.1323561506016,22.2424488153523,0.));
#247000=CARTESIAN_POINT('Ctrl Pts',(4.1341721255881,22.249153531779,0.));
#247001=CARTESIAN_POINT('Ctrl Pts',(4.13608511977225,22.2561118708421,0.));
#247002=CARTESIAN_POINT('Ctrl Pts',(4.13809539255421,22.2633177913972,0.));
#247003=CARTESIAN_POINT('Ctrl Pts',(4.14020318715991,22.2707656042457,0.));
#247004=CARTESIAN_POINT('Ctrl Pts',(4.14240873321984,22.2784499072027,0.));
#247005=CARTESIAN_POINT('Ctrl Pts',(4.14471224859295,22.2863655389166,0.));
#247006=CARTESIAN_POINT('Ctrl Pts',(4.14711394168556,22.2945075198467,0.));
#247007=CARTESIAN_POINT('Ctrl Pts',(4.14961401285522,22.3028710166933,0.));
#247008=CARTESIAN_POINT('Ctrl Pts',(4.1522126539699,22.3114513545185,0.));
#247009=CARTESIAN_POINT('Ctrl Pts',(4.15491004835281,22.3202440186979,0.));
#247010=CARTESIAN_POINT('Ctrl Pts',(4.15770637047889,22.3292446628959,0.));
#247011=CARTESIAN_POINT('Ctrl Pts',(4.16060178604164,22.3384491078602,0.));
#247012=CARTESIAN_POINT('Ctrl Pts',(4.16359645263187,22.3478533253889,0.));
#247013=CARTESIAN_POINT('Ctrl Pts',(4.166690520266,22.3574534257396,0.));
#247014=CARTESIAN_POINT('Ctrl Pts',(4.16988413199457,22.36724564276,0.));
#247015=CARTESIAN_POINT('Ctrl Pts',(4.17317742436145,22.3772263228617,0.));
#247016=CARTESIAN_POINT('Ctrl Pts',(4.17657052752825,22.3873919231334,0.));
#247017=CARTESIAN_POINT('Ctrl Pts',(4.18006356544882,22.3977390078075,0.));
#247018=CARTESIAN_POINT('Ctrl Pts',(4.1836566560085,22.4082642454453,0.));
#247019=CARTESIAN_POINT('Ctrl Pts',(4.1873499111772,22.4189644056115,0.));
#247020=CARTESIAN_POINT('Ctrl Pts',(4.19114343726941,22.4298363535421,0.));
#247021=CARTESIAN_POINT('Ctrl Pts',(4.1950373351886,22.4408770448917,0.));
#247022=CARTESIAN_POINT('Ctrl Pts',(4.19903170066354,22.4520835205419,0.));
#247023=CARTESIAN_POINT('Ctrl Pts',(4.2031266244817,22.4634529011433,0.));
#247024=CARTESIAN_POINT('Ctrl Pts',(4.20732219265648,22.4749823839915,0.));
#247025=CARTESIAN_POINT('Ctrl Pts',(4.21161848657428,22.4866692403147,0.));
#247026=CARTESIAN_POINT('Ctrl Pts',(4.21601558313908,22.4985108124229,0.));
#247027=CARTESIAN_POINT('Ctrl Pts',(4.22051355490196,22.5105045108882,0.));
#247028=CARTESIAN_POINT('Ctrl Pts',(4.2251124702004,22.5226478117885,0.));
#247029=CARTESIAN_POINT('Ctrl Pts',(4.22981239330731,22.5349382540587,0.));
#247030=CARTESIAN_POINT('Ctrl Pts',(4.23461338456713,22.5473734368086,0.));
#247031=CARTESIAN_POINT('Ctrl Pts',(4.23951550052526,22.559951016643,0.));
#247032=CARTESIAN_POINT('Ctrl Pts',(4.24451879404858,22.5726687049922,0.));
#247033=CARTESIAN_POINT('Ctrl Pts',(4.24962331444184,22.5855242662479,0.));
#247034=CARTESIAN_POINT('Ctrl Pts',(4.25482910755485,22.5985155158637,0.));
#247035=CARTESIAN_POINT('Ctrl Pts',(4.26013621588303,22.611640318482,0.));
#247036=CARTESIAN_POINT('Ctrl Pts',(4.26554467865571,22.6248965859975,0.));
#247037=CARTESIAN_POINT('Ctrl Pts',(4.27105453192999,22.6382822758171,0.));
#247038=CARTESIAN_POINT('Ctrl Pts',(4.27666580869117,22.6517953893303,0.));
#247039=CARTESIAN_POINT('Ctrl Pts',(4.28237853894059,22.665433970311,0.));
#247040=CARTESIAN_POINT('Ctrl Pts',(4.28819274977766,22.6791961033537,0.));
#247041=CARTESIAN_POINT('Ctrl Pts',(4.29410846547061,22.6930799122545,0.));
#247042=CARTESIAN_POINT('Ctrl Pts',(4.30012570754066,22.707083558756,0.));
#247043=CARTESIAN_POINT('Ctrl Pts',(4.30624449484074,22.7212052413384,0.));
#247044=CARTESIAN_POINT('Ctrl Pts',(4.3124648436255,22.7354431939927,0.));
#247045=CARTESIAN_POINT('Ctrl Pts',(4.3187867676123,22.7497956849852,0.));
#247046=CARTESIAN_POINT('Ctrl Pts',(4.32521027803747,22.764261015648,0.));
#247047=CARTESIAN_POINT('Ctrl Pts',(4.33173538373182,22.7788375194081,0.));
#247048=CARTESIAN_POINT('Ctrl Pts',(4.33836209118442,22.7935235607807,0.));
#247049=CARTESIAN_POINT('Ctrl Pts',(4.34509040460065,22.808317534379,0.));
#247050=CARTESIAN_POINT('Ctrl Pts',(4.35192032594801,22.8232178638873,0.));
#247051=CARTESIAN_POINT('Ctrl Pts',(4.35885185500559,22.838223001118,0.));
#247052=CARTESIAN_POINT('Ctrl Pts',(4.36588498943009,22.8533314252419,0.));
#247053=CARTESIAN_POINT('Ctrl Pts',(4.37301972480752,22.8685416419725,0.));
#247054=CARTESIAN_POINT('Ctrl Pts',(4.38025605470089,22.8838521827702,0.));
#247055=CARTESIAN_POINT('Ctrl Pts',(4.38759397068391,22.8992616040108,0.));
#247056=CARTESIAN_POINT('Ctrl Pts',(4.39503346238454,22.9147684862425,0.));
#247057=CARTESIAN_POINT('Ctrl Pts',(4.40257451754307,22.9303714335549,0.));
#247058=CARTESIAN_POINT('Ctrl Pts',(4.41021712205547,22.9460690729093,0.));
#247059=CARTESIAN_POINT('Ctrl Pts',(4.41796126001309,22.9618600534866,0.));
#247060=CARTESIAN_POINT('Ctrl Pts',(4.42580691372771,22.9777430460021,0.));
#247061=CARTESIAN_POINT('Ctrl Pts',(4.43375406376904,22.9937167421009,0.));
#247062=CARTESIAN_POINT('Ctrl Pts',(4.44180268901666,23.0097798538399,0.));
#247063=CARTESIAN_POINT('Ctrl Pts',(4.44995276669698,23.0259311131395,0.));
#247064=CARTESIAN_POINT('Ctrl Pts',(4.45820427241676,23.0421692712466,0.));
#247065=CARTESIAN_POINT('Ctrl Pts',(4.46655718018205,23.0584930981723,0.));
#247066=CARTESIAN_POINT('Ctrl Pts',(4.47501146242821,23.0749013821868,0.));
#247067=CARTESIAN_POINT('Ctrl Pts',(4.48356709006756,23.0913929293909,0.));
#247068=CARTESIAN_POINT('Ctrl Pts',(4.49222403252201,23.1079665632629,0.));
#247069=CARTESIAN_POINT('Ctrl Pts',(4.50098225775178,23.1246211242117,0.));
#247070=CARTESIAN_POINT('Ctrl Pts',(4.50984173227087,23.1413554691136,0.));
#247071=CARTESIAN_POINT('Ctrl Pts',(4.51880242116785,23.1581684708778,0.));
#247072=CARTESIAN_POINT('Ctrl Pts',(4.52786428815047,23.1750590180923,0.));
#247073=CARTESIAN_POINT('Ctrl Pts',(4.53702729557585,23.1920260146474,0.));
#247074=CARTESIAN_POINT('Ctrl Pts',(4.54629140447542,23.2090683793627,0.));
#247075=CARTESIAN_POINT('Ctrl Pts',(4.55565657456956,23.2261850456055,0.));
#247076=CARTESIAN_POINT('Ctrl Pts',(4.5651227642781,23.2433749609117,0.));
#247077=CARTESIAN_POINT('Ctrl Pts',(4.5746899307607,23.2606370866853,0.));
#247078=CARTESIAN_POINT('Ctrl Pts',(4.58435802994674,23.2779703978868,0.));
#247079=CARTESIAN_POINT('Ctrl Pts',(4.59412701655749,23.295373882719,0.));
#247080=CARTESIAN_POINT('Ctrl Pts',(4.60399684412174,23.3128465423119,0.));
#247081=CARTESIAN_POINT('Ctrl Pts',(4.61396746497848,23.3303873903947,0.));
#247082=CARTESIAN_POINT('Ctrl Pts',(4.62403883030823,23.3479954530281,0.));
#247083=CARTESIAN_POINT('Ctrl Pts',(4.63421089016554,23.3656697683496,0.));
#247084=CARTESIAN_POINT('Ctrl Pts',(4.64448359349935,23.383409386307,0.));
#247085=CARTESIAN_POINT('Ctrl Pts',(4.65485688816921,23.4012133683957,0.));
#247086=CARTESIAN_POINT('Ctrl Pts',(4.66533072094663,23.4190807873798,0.));
#247087=CARTESIAN_POINT('Ctrl Pts',(4.6759050375305,23.4370107270444,0.));
#247088=CARTESIAN_POINT('Ctrl Pts',(4.68657978258297,23.4550022819853,0.));
#247089=CARTESIAN_POINT('Ctrl Pts',(4.69735489975023,23.4730545573849,0.));
#247090=CARTESIAN_POINT('Ctrl Pts',(4.7082303316782,23.491166668789,0.));
#247091=CARTESIAN_POINT('Ctrl Pts',(4.71920602001904,23.5093377418784,0.));
#247092=CARTESIAN_POINT('Ctrl Pts',(4.73028190543031,23.5275669122378,0.));
#247093=CARTESIAN_POINT('Ctrl Pts',(4.74145792760698,23.5458533251715,0.));
#247094=CARTESIAN_POINT('Ctrl Pts',(4.75273402530615,23.564196135517,0.));
#247095=CARTESIAN_POINT('Ctrl Pts',(4.7641101363625,23.5825945074535,0.));
#247096=CARTESIAN_POINT('Ctrl Pts',(4.77558619769875,23.6010476143099,0.));
#247097=CARTESIAN_POINT('Ctrl Pts',(4.78716214532104,23.6195546383625,0.));
#247098=CARTESIAN_POINT('Ctrl Pts',(4.79883791433229,23.6381147706581,0.));
#247099=CARTESIAN_POINT('Ctrl Pts',(4.81061343896442,23.6567272108631,0.));
#247100=CARTESIAN_POINT('Ctrl Pts',(4.82248865259569,23.6753911671023,0.));
#247101=CARTESIAN_POINT('Ctrl Pts',(4.83446348776267,23.6941058557971,0.));
#247102=CARTESIAN_POINT('Ctrl Pts',(4.84653787616422,23.7128705015014,0.));
#247103=CARTESIAN_POINT('Ctrl Pts',(4.85871174865491,23.7316843367308,0.));
#247104=CARTESIAN_POINT('Ctrl Pts',(4.87098503527142,23.7505466018239,0.));
#247105=CARTESIAN_POINT('Ctrl Pts',(4.88335766525565,23.7694565448044,0.));
#247106=CARTESIAN_POINT('Ctrl Pts',(4.89582956706771,23.7884134212381,0.));
#247107=CARTESIAN_POINT('Ctrl Pts',(4.90840066839346,23.8074164940897,0.));
#247108=CARTESIAN_POINT('Ctrl Pts',(4.92107089613976,23.8264650335721,0.));
#247109=CARTESIAN_POINT('Ctrl Pts',(4.93384017643441,23.8455583170062,0.));
#247110=CARTESIAN_POINT('Ctrl Pts',(4.94670843465868,23.8646956287172,0.));
#247111=CARTESIAN_POINT('Ctrl Pts',(4.95967559546565,23.883876259922,0.));
#247112=CARTESIAN_POINT('Ctrl Pts',(4.97274158279228,23.9030995086164,0.));
#247113=CARTESIAN_POINT('Ctrl Pts',(4.98590631986532,23.9223646794591,0.));
#247114=CARTESIAN_POINT('Ctrl Pts',(4.99916972919309,23.9416710836529,0.));
#247115=CARTESIAN_POINT('Ctrl Pts',(5.01253173257458,23.9610180388271,0.));
#247116=CARTESIAN_POINT('Ctrl Pts',(5.02599225112461,23.9804048689228,0.));
#247117=CARTESIAN_POINT('Ctrl Pts',(5.03955120528527,23.9998309040747,0.));
#247118=CARTESIAN_POINT('Ctrl Pts',(5.05320851483068,24.0192954804896,0.));
#247119=CARTESIAN_POINT('Ctrl Pts',(5.06696409886639,24.0387979403268,0.));
#247120=CARTESIAN_POINT('Ctrl Pts',(5.0808178758127,24.0583376315636,0.));
#247121=CARTESIAN_POINT('Ctrl Pts',(5.09476976342616,24.0779139079264,0.));
#247122=CARTESIAN_POINT('Ctrl Pts',(5.10881967883124,24.0975261288444,0.));
#247123=CARTESIAN_POINT('Ctrl Pts',(5.12296753853857,24.117173659394,0.));
#247124=CARTESIAN_POINT('Ctrl Pts',(5.13721325845745,24.1368558702443,0.));
#247125=CARTESIAN_POINT('Ctrl Pts',(5.15155675390079,24.1565721375971,0.));
#247126=CARTESIAN_POINT('Ctrl Pts',(5.16599793957985,24.1763218431344,0.));
#247127=CARTESIAN_POINT('Ctrl Pts',(5.18053672961398,24.1961043738756,0.));
#247128=CARTESIAN_POINT('Ctrl Pts',(5.19517303753647,24.2159191220171,0.));
#247129=CARTESIAN_POINT('Ctrl Pts',(5.20990677629176,24.2357654847766,0.));
#247130=CARTESIAN_POINT('Ctrl Pts',(5.22473785822442,24.2556428642294,0.));
#247131=CARTESIAN_POINT('Ctrl Pts',(5.23966619506289,24.2755506671525,0.));
#247132=CARTESIAN_POINT('Ctrl Pts',(5.25469169788856,24.2954883048447,0.));
#247133=CARTESIAN_POINT('Ctrl Pts',(5.26981427718798,24.3154551932221,0.));
#247134=CARTESIAN_POINT('Ctrl Pts',(5.28503384290648,24.3354507529414,0.));
#247135=CARTESIAN_POINT('Ctrl Pts',(5.30035030449063,24.3554744095075,0.));
#247136=CARTESIAN_POINT('Ctrl Pts',(5.31576357092526,24.3755255933917,0.));
#247137=CARTESIAN_POINT('Ctrl Pts',(5.33127355076033,24.3956037401293,0.));
#247138=CARTESIAN_POINT('Ctrl Pts',(5.34688015213537,24.4157082904614,0.));
#247139=CARTESIAN_POINT('Ctrl Pts',(5.36258328273627,24.435838689915,0.));
#247140=CARTESIAN_POINT('Ctrl Pts',(5.37838284973695,24.4559943883157,0.));
#247141=CARTESIAN_POINT('Ctrl Pts',(5.39427875973824,24.4761748393321,0.));
#247142=CARTESIAN_POINT('Ctrl Pts',(5.41027091869241,24.4963794999831,0.));
#247143=CARTESIAN_POINT('Ctrl Pts',(5.42635923183419,24.5166078302108,0.));
#247144=CARTESIAN_POINT('Ctrl Pts',(5.4425436035688,24.5368592922863,0.));
#247145=CARTESIAN_POINT('Ctrl Pts',(5.45882393762261,24.5571333514842,0.));
#247146=CARTESIAN_POINT('Ctrl Pts',(5.47520013724419,24.5774294770329,0.));
#247147=CARTESIAN_POINT('Ctrl Pts',(5.49167210537246,24.5977471429364,0.));
#247148=CARTESIAN_POINT('Ctrl Pts',(5.50823974481962,24.6180858289179,0.));
#247149=CARTESIAN_POINT('Ctrl Pts',(5.52490295840991,24.6384450211467,0.));
#247150=CARTESIAN_POINT('Ctrl Pts',(5.54166164919583,24.6588242134738,0.));
#247151=CARTESIAN_POINT('Ctrl Pts',(5.55851572025376,24.6792229061794,0.));
#247152=CARTESIAN_POINT('Ctrl Pts',(5.57546507427754,24.6996406035517,0.));
#247153=CARTESIAN_POINT('Ctrl Pts',(5.59250961323987,24.7200768119088,0.));
#247154=CARTESIAN_POINT('Ctrl Pts',(5.60964923798491,24.7405310372739,0.));
#247155=CARTESIAN_POINT('Ctrl Pts',(5.62688384790923,24.7610027835697,0.));
#247156=CARTESIAN_POINT('Ctrl Pts',(5.6442133404226,24.781491549672,0.));
#247157=CARTESIAN_POINT('Ctrl Pts',(5.66163761114921,24.8019968304605,0.));
#247158=CARTESIAN_POINT('Ctrl Pts',(5.67915655496542,24.8225181223845,0.));
#247159=CARTESIAN_POINT('Ctrl Pts',(5.69677006679444,24.8430549277621,0.));
#247160=CARTESIAN_POINT('Ctrl Pts',(5.71447804252027,24.8636067597669,0.));
#247161=CARTESIAN_POINT('Ctrl Pts',(5.73228037976926,24.884173146722,0.));
#247162=CARTESIAN_POINT('Ctrl Pts',(5.75017697890804,24.904753637648,0.));
#247163=CARTESIAN_POINT('Ctrl Pts',(5.76816774342219,24.9253478043656,0.));
#247164=CARTESIAN_POINT('Ctrl Pts',(5.78625257775681,24.945955229334,0.));
#247165=CARTESIAN_POINT('Ctrl Pts',(5.80443138549726,24.9665754954496,0.));
#247166=CARTESIAN_POINT('Ctrl Pts',(5.82270406744198,24.9872081752734,0.));
#247167=CARTESIAN_POINT('Ctrl Pts',(5.84107051963071,25.0078528200564,0.));
#247168=CARTESIAN_POINT('Ctrl Pts',(5.85953063156826,25.0285089498899,0.));
#247169=CARTESIAN_POINT('Ctrl Pts',(5.87808428385365,25.0491760405911,0.));
#247170=CARTESIAN_POINT('Ctrl Pts',(5.89673135155514,25.0698535426514,0.));
#247171=CARTESIAN_POINT('Ctrl Pts',(5.91547170844447,25.0905409050773,0.));
#247172=CARTESIAN_POINT('Ctrl Pts',(5.93430523086834,25.1112375971106,0.));
#247173=CARTESIAN_POINT('Ctrl Pts',(5.95323180187378,25.1319431317237,0.));
#247174=CARTESIAN_POINT('Ctrl Pts',(5.97225131495616,25.1526570863092,0.));
#247175=CARTESIAN_POINT('Ctrl Pts',(5.99136367859754,25.1733791296259,0.));
#247176=CARTESIAN_POINT('Ctrl Pts',(6.01056881804612,25.1941090269819,0.));
#247177=CARTESIAN_POINT('Ctrl Pts',(6.02986667389996,25.21484662016,0.));
#247178=CARTESIAN_POINT('Ctrl Pts',(6.04925720151218,25.2355918139032,0.));
#247179=CARTESIAN_POINT('Ctrl Pts',(6.06484373634546,25.2521940105705,0.));
#247180=CARTESIAN_POINT('Ctrl Pts',(6.0765753178749,25.2646490489923,0.));
#247181=CARTESIAN_POINT('Ctrl Pts',(6.08441489609793,25.2729539149517,0.));
#247182=CARTESIAN_POINT('Ctrl Pts',(6.08833931617699,25.2771067246846,0.));
#247183=CARTESIAN_POINT('',(6.08833931617699,25.2771067246846,12.));
#247184=CARTESIAN_POINT('Ctrl Pts',(6.08833931617699,25.2771067246846,12.));
#247185=CARTESIAN_POINT('Ctrl Pts',(6.08441489609793,25.2729539149517,12.));
#247186=CARTESIAN_POINT('Ctrl Pts',(6.0765753178749,25.2646490489923,12.));
#247187=CARTESIAN_POINT('Ctrl Pts',(6.06484373634546,25.2521940105705,12.));
#247188=CARTESIAN_POINT('Ctrl Pts',(6.04925720151218,25.2355918139032,12.));
#247189=CARTESIAN_POINT('Ctrl Pts',(6.02986667389996,25.21484662016,12.));
#247190=CARTESIAN_POINT('Ctrl Pts',(6.01056881804612,25.1941090269819,12.));
#247191=CARTESIAN_POINT('Ctrl Pts',(5.99136367859754,25.1733791296259,12.));
#247192=CARTESIAN_POINT('Ctrl Pts',(5.97225131495616,25.1526570863092,12.));
#247193=CARTESIAN_POINT('Ctrl Pts',(5.95323180187378,25.1319431317237,12.));
#247194=CARTESIAN_POINT('Ctrl Pts',(5.93430523086834,25.1112375971106,12.));
#247195=CARTESIAN_POINT('Ctrl Pts',(5.91547170844447,25.0905409050773,12.));
#247196=CARTESIAN_POINT('Ctrl Pts',(5.89673135155514,25.0698535426514,12.));
#247197=CARTESIAN_POINT('Ctrl Pts',(5.87808428385365,25.0491760405911,12.));
#247198=CARTESIAN_POINT('Ctrl Pts',(5.85953063156826,25.0285089498899,12.));
#247199=CARTESIAN_POINT('Ctrl Pts',(5.84107051963071,25.0078528200564,12.));
#247200=CARTESIAN_POINT('Ctrl Pts',(5.82270406744198,24.9872081752734,12.));
#247201=CARTESIAN_POINT('Ctrl Pts',(5.80443138549726,24.9665754954496,12.));
#247202=CARTESIAN_POINT('Ctrl Pts',(5.78625257775681,24.945955229334,12.));
#247203=CARTESIAN_POINT('Ctrl Pts',(5.76816774342219,24.9253478043656,12.));
#247204=CARTESIAN_POINT('Ctrl Pts',(5.75017697890804,24.904753637648,12.));
#247205=CARTESIAN_POINT('Ctrl Pts',(5.73228037976926,24.884173146722,12.));
#247206=CARTESIAN_POINT('Ctrl Pts',(5.71447804252027,24.8636067597669,12.));
#247207=CARTESIAN_POINT('Ctrl Pts',(5.69677006679444,24.8430549277621,12.));
#247208=CARTESIAN_POINT('Ctrl Pts',(5.67915655496542,24.8225181223845,12.));
#247209=CARTESIAN_POINT('Ctrl Pts',(5.66163761114921,24.8019968304605,12.));
#247210=CARTESIAN_POINT('Ctrl Pts',(5.6442133404226,24.781491549672,12.));
#247211=CARTESIAN_POINT('Ctrl Pts',(5.62688384790923,24.7610027835697,12.));
#247212=CARTESIAN_POINT('Ctrl Pts',(5.60964923798491,24.7405310372739,12.));
#247213=CARTESIAN_POINT('Ctrl Pts',(5.59250961323987,24.7200768119088,12.));
#247214=CARTESIAN_POINT('Ctrl Pts',(5.57546507427754,24.6996406035517,12.));
#247215=CARTESIAN_POINT('Ctrl Pts',(5.55851572025376,24.6792229061794,12.));
#247216=CARTESIAN_POINT('Ctrl Pts',(5.54166164919583,24.6588242134738,12.));
#247217=CARTESIAN_POINT('Ctrl Pts',(5.52490295840991,24.6384450211467,12.));
#247218=CARTESIAN_POINT('Ctrl Pts',(5.50823974481962,24.6180858289179,12.));
#247219=CARTESIAN_POINT('Ctrl Pts',(5.49167210537246,24.5977471429364,12.));
#247220=CARTESIAN_POINT('Ctrl Pts',(5.47520013724419,24.5774294770329,12.));
#247221=CARTESIAN_POINT('Ctrl Pts',(5.45882393762261,24.5571333514842,12.));
#247222=CARTESIAN_POINT('Ctrl Pts',(5.4425436035688,24.5368592922863,12.));
#247223=CARTESIAN_POINT('Ctrl Pts',(5.42635923183419,24.5166078302108,12.));
#247224=CARTESIAN_POINT('Ctrl Pts',(5.41027091869241,24.4963794999831,12.));
#247225=CARTESIAN_POINT('Ctrl Pts',(5.39427875973824,24.4761748393321,12.));
#247226=CARTESIAN_POINT('Ctrl Pts',(5.37838284973695,24.4559943883157,12.));
#247227=CARTESIAN_POINT('Ctrl Pts',(5.36258328273627,24.435838689915,12.));
#247228=CARTESIAN_POINT('Ctrl Pts',(5.34688015213537,24.4157082904614,12.));
#247229=CARTESIAN_POINT('Ctrl Pts',(5.33127355076033,24.3956037401293,12.));
#247230=CARTESIAN_POINT('Ctrl Pts',(5.31576357092526,24.3755255933917,12.));
#247231=CARTESIAN_POINT('Ctrl Pts',(5.30035030449063,24.3554744095075,12.));
#247232=CARTESIAN_POINT('Ctrl Pts',(5.28503384290648,24.3354507529414,12.));
#247233=CARTESIAN_POINT('Ctrl Pts',(5.26981427718798,24.3154551932221,12.));
#247234=CARTESIAN_POINT('Ctrl Pts',(5.25469169788856,24.2954883048447,12.));
#247235=CARTESIAN_POINT('Ctrl Pts',(5.23966619506289,24.2755506671525,12.));
#247236=CARTESIAN_POINT('Ctrl Pts',(5.22473785822442,24.2556428642294,12.));
#247237=CARTESIAN_POINT('Ctrl Pts',(5.20990677629176,24.2357654847766,12.));
#247238=CARTESIAN_POINT('Ctrl Pts',(5.19517303753647,24.2159191220171,12.));
#247239=CARTESIAN_POINT('Ctrl Pts',(5.18053672961398,24.1961043738756,12.));
#247240=CARTESIAN_POINT('Ctrl Pts',(5.16599793957985,24.1763218431344,12.));
#247241=CARTESIAN_POINT('Ctrl Pts',(5.15155675390079,24.1565721375971,12.));
#247242=CARTESIAN_POINT('Ctrl Pts',(5.13721325845745,24.1368558702443,12.));
#247243=CARTESIAN_POINT('Ctrl Pts',(5.12296753853857,24.117173659394,12.));
#247244=CARTESIAN_POINT('Ctrl Pts',(5.10881967883124,24.0975261288444,12.));
#247245=CARTESIAN_POINT('Ctrl Pts',(5.09476976342616,24.0779139079264,12.));
#247246=CARTESIAN_POINT('Ctrl Pts',(5.0808178758127,24.0583376315636,12.));
#247247=CARTESIAN_POINT('Ctrl Pts',(5.06696409886639,24.0387979403268,12.));
#247248=CARTESIAN_POINT('Ctrl Pts',(5.05320851483068,24.0192954804896,12.));
#247249=CARTESIAN_POINT('Ctrl Pts',(5.03955120528527,23.9998309040747,12.));
#247250=CARTESIAN_POINT('Ctrl Pts',(5.02599225112461,23.9804048689228,12.));
#247251=CARTESIAN_POINT('Ctrl Pts',(5.01253173257458,23.9610180388271,12.));
#247252=CARTESIAN_POINT('Ctrl Pts',(4.99916972919309,23.9416710836529,12.));
#247253=CARTESIAN_POINT('Ctrl Pts',(4.98590631986532,23.9223646794591,12.));
#247254=CARTESIAN_POINT('Ctrl Pts',(4.97274158279228,23.9030995086164,12.));
#247255=CARTESIAN_POINT('Ctrl Pts',(4.95967559546565,23.883876259922,12.));
#247256=CARTESIAN_POINT('Ctrl Pts',(4.94670843465868,23.8646956287172,12.));
#247257=CARTESIAN_POINT('Ctrl Pts',(4.93384017643441,23.8455583170062,12.));
#247258=CARTESIAN_POINT('Ctrl Pts',(4.92107089613976,23.8264650335721,12.));
#247259=CARTESIAN_POINT('Ctrl Pts',(4.90840066839346,23.8074164940897,12.));
#247260=CARTESIAN_POINT('Ctrl Pts',(4.89582956706771,23.7884134212381,12.));
#247261=CARTESIAN_POINT('Ctrl Pts',(4.88335766525565,23.7694565448044,12.));
#247262=CARTESIAN_POINT('Ctrl Pts',(4.87098503527142,23.7505466018239,12.));
#247263=CARTESIAN_POINT('Ctrl Pts',(4.85871174865491,23.7316843367308,12.));
#247264=CARTESIAN_POINT('Ctrl Pts',(4.84653787616422,23.7128705015014,12.));
#247265=CARTESIAN_POINT('Ctrl Pts',(4.83446348776267,23.6941058557971,12.));
#247266=CARTESIAN_POINT('Ctrl Pts',(4.82248865259569,23.6753911671023,12.));
#247267=CARTESIAN_POINT('Ctrl Pts',(4.81061343896442,23.6567272108631,12.));
#247268=CARTESIAN_POINT('Ctrl Pts',(4.79883791433229,23.6381147706581,12.));
#247269=CARTESIAN_POINT('Ctrl Pts',(4.78716214532104,23.6195546383625,12.));
#247270=CARTESIAN_POINT('Ctrl Pts',(4.77558619769875,23.6010476143099,12.));
#247271=CARTESIAN_POINT('Ctrl Pts',(4.7641101363625,23.5825945074535,12.));
#247272=CARTESIAN_POINT('Ctrl Pts',(4.75273402530615,23.564196135517,12.));
#247273=CARTESIAN_POINT('Ctrl Pts',(4.74145792760698,23.5458533251715,12.));
#247274=CARTESIAN_POINT('Ctrl Pts',(4.73028190543031,23.5275669122378,12.));
#247275=CARTESIAN_POINT('Ctrl Pts',(4.71920602001904,23.5093377418784,12.));
#247276=CARTESIAN_POINT('Ctrl Pts',(4.7082303316782,23.491166668789,12.));
#247277=CARTESIAN_POINT('Ctrl Pts',(4.69735489975023,23.4730545573849,12.));
#247278=CARTESIAN_POINT('Ctrl Pts',(4.68657978258297,23.4550022819853,12.));
#247279=CARTESIAN_POINT('Ctrl Pts',(4.6759050375305,23.4370107270444,12.));
#247280=CARTESIAN_POINT('Ctrl Pts',(4.66533072094663,23.4190807873798,12.));
#247281=CARTESIAN_POINT('Ctrl Pts',(4.65485688816921,23.4012133683957,12.));
#247282=CARTESIAN_POINT('Ctrl Pts',(4.64448359349935,23.383409386307,12.));
#247283=CARTESIAN_POINT('Ctrl Pts',(4.63421089016554,23.3656697683496,12.));
#247284=CARTESIAN_POINT('Ctrl Pts',(4.62403883030823,23.3479954530281,12.));
#247285=CARTESIAN_POINT('Ctrl Pts',(4.61396746497848,23.3303873903947,12.));
#247286=CARTESIAN_POINT('Ctrl Pts',(4.60399684412174,23.3128465423119,12.));
#247287=CARTESIAN_POINT('Ctrl Pts',(4.59412701655749,23.295373882719,12.));
#247288=CARTESIAN_POINT('Ctrl Pts',(4.58435802994674,23.2779703978868,12.));
#247289=CARTESIAN_POINT('Ctrl Pts',(4.5746899307607,23.2606370866853,12.));
#247290=CARTESIAN_POINT('Ctrl Pts',(4.5651227642781,23.2433749609117,12.));
#247291=CARTESIAN_POINT('Ctrl Pts',(4.55565657456956,23.2261850456055,12.));
#247292=CARTESIAN_POINT('Ctrl Pts',(4.54629140447542,23.2090683793627,12.));
#247293=CARTESIAN_POINT('Ctrl Pts',(4.53702729557585,23.1920260146474,12.));
#247294=CARTESIAN_POINT('Ctrl Pts',(4.52786428815047,23.1750590180923,12.));
#247295=CARTESIAN_POINT('Ctrl Pts',(4.51880242116785,23.1581684708778,12.));
#247296=CARTESIAN_POINT('Ctrl Pts',(4.50984173227087,23.1413554691136,12.));
#247297=CARTESIAN_POINT('Ctrl Pts',(4.50098225775178,23.1246211242117,12.));
#247298=CARTESIAN_POINT('Ctrl Pts',(4.49222403252201,23.1079665632629,12.));
#247299=CARTESIAN_POINT('Ctrl Pts',(4.48356709006756,23.0913929293909,12.));
#247300=CARTESIAN_POINT('Ctrl Pts',(4.47501146242821,23.0749013821868,12.));
#247301=CARTESIAN_POINT('Ctrl Pts',(4.46655718018205,23.0584930981723,12.));
#247302=CARTESIAN_POINT('Ctrl Pts',(4.45820427241676,23.0421692712466,12.));
#247303=CARTESIAN_POINT('Ctrl Pts',(4.44995276669698,23.0259311131395,12.));
#247304=CARTESIAN_POINT('Ctrl Pts',(4.44180268901666,23.0097798538399,12.));
#247305=CARTESIAN_POINT('Ctrl Pts',(4.43375406376904,22.9937167421009,12.));
#247306=CARTESIAN_POINT('Ctrl Pts',(4.42580691372771,22.9777430460021,12.));
#247307=CARTESIAN_POINT('Ctrl Pts',(4.41796126001309,22.9618600534866,12.));
#247308=CARTESIAN_POINT('Ctrl Pts',(4.41021712205547,22.9460690729093,12.));
#247309=CARTESIAN_POINT('Ctrl Pts',(4.40257451754307,22.9303714335549,12.));
#247310=CARTESIAN_POINT('Ctrl Pts',(4.39503346238454,22.9147684862425,12.));
#247311=CARTESIAN_POINT('Ctrl Pts',(4.38759397068391,22.8992616040108,12.));
#247312=CARTESIAN_POINT('Ctrl Pts',(4.38025605470089,22.8838521827702,12.));
#247313=CARTESIAN_POINT('Ctrl Pts',(4.37301972480752,22.8685416419725,12.));
#247314=CARTESIAN_POINT('Ctrl Pts',(4.36588498943009,22.8533314252419,12.));
#247315=CARTESIAN_POINT('Ctrl Pts',(4.35885185500559,22.838223001118,12.));
#247316=CARTESIAN_POINT('Ctrl Pts',(4.35192032594801,22.8232178638873,12.));
#247317=CARTESIAN_POINT('Ctrl Pts',(4.34509040460065,22.808317534379,12.));
#247318=CARTESIAN_POINT('Ctrl Pts',(4.33836209118442,22.7935235607807,12.));
#247319=CARTESIAN_POINT('Ctrl Pts',(4.33173538373182,22.7788375194081,12.));
#247320=CARTESIAN_POINT('Ctrl Pts',(4.32521027803747,22.764261015648,12.));
#247321=CARTESIAN_POINT('Ctrl Pts',(4.3187867676123,22.7497956849852,12.));
#247322=CARTESIAN_POINT('Ctrl Pts',(4.3124648436255,22.7354431939927,12.));
#247323=CARTESIAN_POINT('Ctrl Pts',(4.30624449484074,22.7212052413384,12.));
#247324=CARTESIAN_POINT('Ctrl Pts',(4.30012570754066,22.707083558756,12.));
#247325=CARTESIAN_POINT('Ctrl Pts',(4.29410846547061,22.6930799122545,12.));
#247326=CARTESIAN_POINT('Ctrl Pts',(4.28819274977766,22.6791961033537,12.));
#247327=CARTESIAN_POINT('Ctrl Pts',(4.28237853894059,22.665433970311,12.));
#247328=CARTESIAN_POINT('Ctrl Pts',(4.27666580869117,22.6517953893303,12.));
#247329=CARTESIAN_POINT('Ctrl Pts',(4.27105453192999,22.6382822758171,12.));
#247330=CARTESIAN_POINT('Ctrl Pts',(4.26554467865571,22.6248965859975,12.));
#247331=CARTESIAN_POINT('Ctrl Pts',(4.26013621588303,22.611640318482,12.));
#247332=CARTESIAN_POINT('Ctrl Pts',(4.25482910755485,22.5985155158637,12.));
#247333=CARTESIAN_POINT('Ctrl Pts',(4.24962331444184,22.5855242662479,12.));
#247334=CARTESIAN_POINT('Ctrl Pts',(4.24451879404858,22.5726687049922,12.));
#247335=CARTESIAN_POINT('Ctrl Pts',(4.23951550052526,22.559951016643,12.));
#247336=CARTESIAN_POINT('Ctrl Pts',(4.23461338456713,22.5473734368086,12.));
#247337=CARTESIAN_POINT('Ctrl Pts',(4.22981239330731,22.5349382540587,12.));
#247338=CARTESIAN_POINT('Ctrl Pts',(4.2251124702004,22.5226478117885,12.));
#247339=CARTESIAN_POINT('Ctrl Pts',(4.22051355490196,22.5105045108882,12.));
#247340=CARTESIAN_POINT('Ctrl Pts',(4.21601558313908,22.4985108124229,12.));
#247341=CARTESIAN_POINT('Ctrl Pts',(4.21161848657428,22.4866692403147,12.));
#247342=CARTESIAN_POINT('Ctrl Pts',(4.20732219265648,22.4749823839915,12.));
#247343=CARTESIAN_POINT('Ctrl Pts',(4.2031266244817,22.4634529011433,12.));
#247344=CARTESIAN_POINT('Ctrl Pts',(4.19903170066354,22.4520835205419,12.));
#247345=CARTESIAN_POINT('Ctrl Pts',(4.1950373351886,22.4408770448917,12.));
#247346=CARTESIAN_POINT('Ctrl Pts',(4.19114343726941,22.4298363535421,12.));
#247347=CARTESIAN_POINT('Ctrl Pts',(4.1873499111772,22.4189644056115,12.));
#247348=CARTESIAN_POINT('Ctrl Pts',(4.1836566560085,22.4082642454453,12.));
#247349=CARTESIAN_POINT('Ctrl Pts',(4.18006356544882,22.3977390078075,12.));
#247350=CARTESIAN_POINT('Ctrl Pts',(4.17657052752825,22.3873919231334,12.));
#247351=CARTESIAN_POINT('Ctrl Pts',(4.17317742436145,22.3772263228617,12.));
#247352=CARTESIAN_POINT('Ctrl Pts',(4.16988413199457,22.36724564276,12.));
#247353=CARTESIAN_POINT('Ctrl Pts',(4.166690520266,22.3574534257396,12.));
#247354=CARTESIAN_POINT('Ctrl Pts',(4.16359645263187,22.3478533253889,12.));
#247355=CARTESIAN_POINT('Ctrl Pts',(4.16060178604164,22.3384491078602,12.));
#247356=CARTESIAN_POINT('Ctrl Pts',(4.15770637047889,22.3292446628959,12.));
#247357=CARTESIAN_POINT('Ctrl Pts',(4.15491004835281,22.3202440186979,12.));
#247358=CARTESIAN_POINT('Ctrl Pts',(4.1522126539699,22.3114513545185,12.));
#247359=CARTESIAN_POINT('Ctrl Pts',(4.14961401285522,22.3028710166933,12.));
#247360=CARTESIAN_POINT('Ctrl Pts',(4.14711394168556,22.2945075198467,12.));
#247361=CARTESIAN_POINT('Ctrl Pts',(4.14471224859295,22.2863655389166,12.));
#247362=CARTESIAN_POINT('Ctrl Pts',(4.14240873321984,22.2784499072027,12.));
#247363=CARTESIAN_POINT('Ctrl Pts',(4.14020318715991,22.2707656042457,12.));
#247364=CARTESIAN_POINT('Ctrl Pts',(4.13809539255421,22.2633177913972,12.));
#247365=CARTESIAN_POINT('Ctrl Pts',(4.13608511977225,22.2561118708421,12.));
#247366=CARTESIAN_POINT('Ctrl Pts',(4.1341721255881,22.249153531779,12.));
#247367=CARTESIAN_POINT('Ctrl Pts',(4.1323561506016,22.2424488153523,12.));
#247368=CARTESIAN_POINT('Ctrl Pts',(4.13063692157498,22.2360040565533,12.));
#247369=CARTESIAN_POINT('Ctrl Pts',(4.12901415463379,22.2298258043947,12.));
#247370=CARTESIAN_POINT('Ctrl Pts',(4.12748755830104,22.2239207458781,12.));
#247371=CARTESIAN_POINT('Ctrl Pts',(4.12605683613307,22.2182956401341,12.));
#247372=CARTESIAN_POINT('Ctrl Pts',(4.12472167516607,22.2129576146671,12.));
#247373=CARTESIAN_POINT('Ctrl Pts',(4.12348173702023,22.2079143941719,12.));
#247374=CARTESIAN_POINT('Ctrl Pts',(4.12233664408227,22.2031746532106,12.));
#247375=CARTESIAN_POINT('Ctrl Pts',(4.12128598183522,22.1987479618246,12.));
#247376=CARTESIAN_POINT('Ctrl Pts',(4.12032932637736,22.1946440958098,12.));
#247377=CARTESIAN_POINT('Ctrl Pts',(4.11946626228636,22.1908725908525,12.));
#247378=CARTESIAN_POINT('Ctrl Pts',(4.11869641271773,22.1874419861496,12.));
#247379=CARTESIAN_POINT('Ctrl Pts',(4.11801938107479,22.1843613164855,12.));
#247380=CARTESIAN_POINT('Ctrl Pts',(4.11743469691756,22.1816414985788,12.));
#247381=CARTESIAN_POINT('Ctrl Pts',(4.11694173195003,22.179297473024,12.));
#247382=CARTESIAN_POINT('Ctrl Pts',(4.11653973150518,22.177347426894,12.));
#247383=CARTESIAN_POINT('Ctrl Pts',(4.11622797217068,22.1758088296598,12.));
#247384=CARTESIAN_POINT('Ctrl Pts',(4.11600589882845,22.1746949858775,12.));
#247385=CARTESIAN_POINT('Ctrl Pts',(4.11589976826166,22.1741488021234,12.));
#247386=CARTESIAN_POINT('Ctrl Pts',(4.11586035878287,22.1739341411687,12.));
#247387=CARTESIAN_POINT('Ctrl Pts',(4.11585194677442,22.173877682324,12.));
#247388=CARTESIAN_POINT('Ctrl Pts',(4.11585220600461,22.1738711152697,12.));
#247389=CARTESIAN_POINT('',(6.08833931617699,25.2771067246846,0.));
#247390=CARTESIAN_POINT('Origin',(9.26120677397564,19.4030938020118,0.));
#247391=CARTESIAN_POINT('',(9.71462809124917,20.353053841303,12.));
#247392=CARTESIAN_POINT('',(4.63060338698782,9.70154690100589,12.));
#247393=CARTESIAN_POINT('',(9.71462809124917,20.353053841303,0.));
#247394=CARTESIAN_POINT('',(9.71462809124917,20.353053841303,0.));
#247395=CARTESIAN_POINT('',(4.63060338698782,9.70154690100589,0.));
#247396=CARTESIAN_POINT('Ctrl Pts',(7.36589684767344,24.9347862158358,0.));
#247397=CARTESIAN_POINT('Ctrl Pts',(7.36589684767344,24.9347862158358,12.));
#247398=CARTESIAN_POINT('Ctrl Pts',(7.36721909028842,24.9292275670674,0.));
#247399=CARTESIAN_POINT('Ctrl Pts',(7.36721909028842,24.9292275670674,12.));
#247400=CARTESIAN_POINT('Ctrl Pts',(7.3698559312009,24.9181155530543,0.));
#247401=CARTESIAN_POINT('Ctrl Pts',(7.3698559312009,24.9181155530543,12.));
#247402=CARTESIAN_POINT('Ctrl Pts',(7.37378825961676,24.901463382605,0.));
#247403=CARTESIAN_POINT('Ctrl Pts',(7.37378825961676,24.901463382605,12.));
#247404=CARTESIAN_POINT('Ctrl Pts',(7.37898549640269,24.8792921911115,0.));
#247405=CARTESIAN_POINT('Ctrl Pts',(7.37898549640269,24.8792921911115,12.));
#247406=CARTESIAN_POINT('Ctrl Pts',(7.3854055890362,24.8516310625176,0.));
#247407=CARTESIAN_POINT('Ctrl Pts',(7.3854055890362,24.8516310625176,12.));
#247408=CARTESIAN_POINT('Ctrl Pts',(7.39174922585808,24.8240228520893,0.));
#247409=CARTESIAN_POINT('Ctrl Pts',(7.39174922585808,24.8240228520893,12.));
#247410=CARTESIAN_POINT('Ctrl Pts',(7.39801641583012,24.7964676646431,0.));
#247411=CARTESIAN_POINT('Ctrl Pts',(7.39801641583012,24.7964676646431,12.));
#247412=CARTESIAN_POINT('Ctrl Pts',(7.40420718661602,24.7689656668983,0.));
#247413=CARTESIAN_POINT('Ctrl Pts',(7.40420718661602,24.7689656668983,12.));
#247414=CARTESIAN_POINT('Ctrl Pts',(7.41032159082381,24.7415170994784,0.));
#247415=CARTESIAN_POINT('Ctrl Pts',(7.41032159082381,24.7415170994784,12.));
#247416=CARTESIAN_POINT('Ctrl Pts',(7.41635971481674,24.7141222950051,0.));
#247417=CARTESIAN_POINT('Ctrl Pts',(7.41635971481674,24.7141222950051,12.));
#247418=CARTESIAN_POINT('Ctrl Pts',(7.42232167766265,24.6867816727192,0.));
#247419=CARTESIAN_POINT('Ctrl Pts',(7.42232167766265,24.6867816727192,12.));
#247420=CARTESIAN_POINT('Ctrl Pts',(7.42820762159125,24.6594957128756,0.));
#247421=CARTESIAN_POINT('Ctrl Pts',(7.42820762159125,24.6594957128756,12.));
#247422=CARTESIAN_POINT('Ctrl Pts',(7.43401770489523,24.6322649369517,0.));
#247423=CARTESIAN_POINT('Ctrl Pts',(7.43401770489523,24.6322649369517,12.));
#247424=CARTESIAN_POINT('Ctrl Pts',(7.43975209375503,24.6050898852368,0.));
#247425=CARTESIAN_POINT('Ctrl Pts',(7.43975209375503,24.6050898852368,12.));
#247426=CARTESIAN_POINT('Ctrl Pts',(7.44541095473134,24.577971096086,0.));
#247427=CARTESIAN_POINT('Ctrl Pts',(7.44541095473134,24.577971096086,12.));
#247428=CARTESIAN_POINT('Ctrl Pts',(7.4509944465116,24.5509090831559,0.));
#247429=CARTESIAN_POINT('Ctrl Pts',(7.4509944465116,24.5509090831559,12.));
#247430=CARTESIAN_POINT('Ctrl Pts',(7.45650271335861,24.5239043173072,0.));
#247431=CARTESIAN_POINT('Ctrl Pts',(7.45650271335861,24.5239043173072,12.));
#247432=CARTESIAN_POINT('Ctrl Pts',(7.46193588961463,24.4969572391483,0.));
#247433=CARTESIAN_POINT('Ctrl Pts',(7.46193588961463,24.4969572391483,12.));
#247434=CARTESIAN_POINT('Ctrl Pts',(7.46729410308786,24.4700682684524,0.));
#247435=CARTESIAN_POINT('Ctrl Pts',(7.46729410308786,24.4700682684524,12.));
#247436=CARTESIAN_POINT('Ctrl Pts',(7.47257747883246,24.443237814649,0.));
#247437=CARTESIAN_POINT('Ctrl Pts',(7.47257747883246,24.443237814649,12.));
#247438=CARTESIAN_POINT('Ctrl Pts',(7.47778614286564,24.4164662871163,0.));
#247439=CARTESIAN_POINT('Ctrl Pts',(7.47778614286564,24.4164662871163,12.));
#247440=CARTESIAN_POINT('Ctrl Pts',(7.482920225693,24.3897541049254,0.));
#247441=CARTESIAN_POINT('Ctrl Pts',(7.482920225693,24.3897541049254,12.));
#247442=CARTESIAN_POINT('Ctrl Pts',(7.48797986651908,24.3631017084524,0.));
#247443=CARTESIAN_POINT('Ctrl Pts',(7.48797986651908,24.3631017084524,12.));
#247444=CARTESIAN_POINT('Ctrl Pts',(7.4929652125242,24.3365095573685,0.));
#247445=CARTESIAN_POINT('Ctrl Pts',(7.4929652125242,24.3365095573685,12.));
#247446=CARTESIAN_POINT('Ctrl Pts',(7.49787641695438,24.3099781253355,0.));
#247447=CARTESIAN_POINT('Ctrl Pts',(7.49787641695438,24.3099781253355,12.));
#247448=CARTESIAN_POINT('Ctrl Pts',(7.50271363765151,24.2835078958973,0.));
#247449=CARTESIAN_POINT('Ctrl Pts',(7.50271363765151,24.2835078958973,12.));
#247450=CARTESIAN_POINT('Ctrl Pts',(7.50747703535133,24.2570993577034,0.));
#247451=CARTESIAN_POINT('Ctrl Pts',(7.50747703535133,24.2570993577034,12.));
#247452=CARTESIAN_POINT('Ctrl Pts',(7.5121667722218,24.2307530003887,0.));
#247453=CARTESIAN_POINT('Ctrl Pts',(7.5121667722218,24.2307530003887,12.));
#247454=CARTESIAN_POINT('Ctrl Pts',(7.51678300997949,24.2044693092349,0.));
#247455=CARTESIAN_POINT('Ctrl Pts',(7.51678300997949,24.2044693092349,12.));
#247456=CARTESIAN_POINT('Ctrl Pts',(7.52132590953801,24.1782487641594,0.));
#247457=CARTESIAN_POINT('Ctrl Pts',(7.52132590953801,24.1782487641594,12.));
#247458=CARTESIAN_POINT('Ctrl Pts',(7.52579563201423,24.1520918425364,0.));
#247459=CARTESIAN_POINT('Ctrl Pts',(7.52579563201423,24.1520918425364,12.));
#247460=CARTESIAN_POINT('Ctrl Pts',(7.53019233935501,24.1259990209207,0.));
#247461=CARTESIAN_POINT('Ctrl Pts',(7.53019233935501,24.1259990209207,12.));
#247462=CARTESIAN_POINT('Ctrl Pts',(7.53451619514649,24.0999707772642,0.));
#247463=CARTESIAN_POINT('Ctrl Pts',(7.53451619514649,24.0999707772642,12.));
#247464=CARTESIAN_POINT('Ctrl Pts',(7.53876736531013,24.0740075927985,0.));
#247465=CARTESIAN_POINT('Ctrl Pts',(7.53876736531013,24.0740075927985,12.));
#247466=CARTESIAN_POINT('Ctrl Pts',(7.54294601896144,24.0481099543353,0.));
#247467=CARTESIAN_POINT('Ctrl Pts',(7.54294601896144,24.0481099543353,12.));
#247468=CARTESIAN_POINT('Ctrl Pts',(7.5470523288591,24.022278355453,0.));
#247469=CARTESIAN_POINT('Ctrl Pts',(7.5470523288591,24.022278355453,12.));
#247470=CARTESIAN_POINT('Ctrl Pts',(7.5510864709744,23.9965132953185,0.));
#247471=CARTESIAN_POINT('Ctrl Pts',(7.5510864709744,23.9965132953185,12.));
#247472=CARTESIAN_POINT('Ctrl Pts',(7.55504862424811,23.9708152779884,0.));
#247473=CARTESIAN_POINT('Ctrl Pts',(7.55504862424811,23.9708152779884,12.));
#247474=CARTESIAN_POINT('Ctrl Pts',(7.55893897027682,23.9451848115,0.));
#247475=CARTESIAN_POINT('Ctrl Pts',(7.55893897027682,23.9451848115,12.));
#247476=CARTESIAN_POINT('Ctrl Pts',(7.56275769304773,23.9196224070759,0.));
#247477=CARTESIAN_POINT('Ctrl Pts',(7.56275769304773,23.9196224070759,12.));
#247478=CARTESIAN_POINT('Ctrl Pts',(7.56650497863791,23.8941285782003,0.));
#247479=CARTESIAN_POINT('Ctrl Pts',(7.56650497863791,23.8941285782003,12.));
#247480=CARTESIAN_POINT('Ctrl Pts',(7.5701810150071,23.8687038399598,0.));
#247481=CARTESIAN_POINT('Ctrl Pts',(7.5701810150071,23.8687038399598,12.));
#247482=CARTESIAN_POINT('Ctrl Pts',(7.57378599219816,23.8433487096134,0.));
#247483=CARTESIAN_POINT('Ctrl Pts',(7.57378599219816,23.8433487096134,12.));
#247484=CARTESIAN_POINT('Ctrl Pts',(7.57732010249065,23.8180637069977,0.));
#247485=CARTESIAN_POINT('Ctrl Pts',(7.57732010249065,23.8180637069977,12.));
#247486=CARTESIAN_POINT('Ctrl Pts',(7.58078354058211,23.7928493549908,0.));
#247487=CARTESIAN_POINT('Ctrl Pts',(7.58078354058211,23.7928493549908,12.));
#247488=CARTESIAN_POINT('Ctrl Pts',(7.58417650376271,23.7677061799376,0.));
#247489=CARTESIAN_POINT('Ctrl Pts',(7.58417650376271,23.7677061799376,12.));
#247490=CARTESIAN_POINT('Ctrl Pts',(7.58749919210831,23.7426347121006,0.));
#247491=CARTESIAN_POINT('Ctrl Pts',(7.58749919210831,23.7426347121006,12.));
#247492=CARTESIAN_POINT('Ctrl Pts',(7.59075180865326,23.7176354860457,0.));
#247493=CARTESIAN_POINT('Ctrl Pts',(7.59075180865326,23.7176354860457,12.));
#247494=CARTESIAN_POINT('Ctrl Pts',(7.59393455934041,23.6927090405067,0.));
#247495=CARTESIAN_POINT('Ctrl Pts',(7.59393455934041,23.6927090405067,12.));
#247496=CARTESIAN_POINT('Ctrl Pts',(7.59704765299572,23.6678559182876,0.));
#247497=CARTESIAN_POINT('Ctrl Pts',(7.59704765299572,23.6678559182876,12.));
#247498=CARTESIAN_POINT('Ctrl Pts',(7.60009130130129,23.6430766661419,0.));
#247499=CARTESIAN_POINT('Ctrl Pts',(7.60009130130129,23.6430766661419,12.));
#247500=CARTESIAN_POINT('Ctrl Pts',(7.60306571877806,23.6183718346576,0.));
#247501=CARTESIAN_POINT('Ctrl Pts',(7.60306571877806,23.6183718346576,12.));
#247502=CARTESIAN_POINT('Ctrl Pts',(7.60597112277094,23.5937419781244,0.));
#247503=CARTESIAN_POINT('Ctrl Pts',(7.60597112277094,23.5937419781244,12.));
#247504=CARTESIAN_POINT('Ctrl Pts',(7.60880773344599,23.5691876544243,0.));
#247505=CARTESIAN_POINT('Ctrl Pts',(7.60880773344599,23.5691876544243,12.));
#247506=CARTESIAN_POINT('Ctrl Pts',(7.61157577385371,23.5447094252029,0.));
#247507=CARTESIAN_POINT('Ctrl Pts',(7.61157577385371,23.5447094252029,12.));
#247508=CARTESIAN_POINT('Ctrl Pts',(7.61427546999298,23.5203078560128,0.));
#247509=CARTESIAN_POINT('Ctrl Pts',(7.61427546999298,23.5203078560128,12.));
#247510=CARTESIAN_POINT('Ctrl Pts',(7.61690705088318,23.4959835164608,0.));
#247511=CARTESIAN_POINT('Ctrl Pts',(7.61690705088318,23.4959835164608,12.));
#247512=CARTESIAN_POINT('Ctrl Pts',(7.61947074863977,23.4717369803438,0.));
#247513=CARTESIAN_POINT('Ctrl Pts',(7.61947074863977,23.4717369803438,12.));
#247514=CARTESIAN_POINT('Ctrl Pts',(7.62196679855957,23.4475688257855,0.));
#247515=CARTESIAN_POINT('Ctrl Pts',(7.62196679855957,23.4475688257855,12.));
#247516=CARTESIAN_POINT('Ctrl Pts',(7.62439543920053,23.4234796353544,0.));
#247517=CARTESIAN_POINT('Ctrl Pts',(7.62439543920053,23.4234796353544,12.));
#247518=CARTESIAN_POINT('Ctrl Pts',(7.62675691240334,23.3994699961122,0.));
#247519=CARTESIAN_POINT('Ctrl Pts',(7.62675691240334,23.3994699961122,12.));
#247520=CARTESIAN_POINT('Ctrl Pts',(7.62905146332597,23.3755404996638,0.));
#247521=CARTESIAN_POINT('Ctrl Pts',(7.62905146332597,23.3755404996638,12.));
#247522=CARTESIAN_POINT('Ctrl Pts',(7.63127934048138,23.3516917421973,0.));
#247523=CARTESIAN_POINT('Ctrl Pts',(7.63127934048138,23.3516917421973,12.));
#247524=CARTESIAN_POINT('Ctrl Pts',(7.63344079578162,23.3279243245241,0.));
#247525=CARTESIAN_POINT('Ctrl Pts',(7.63344079578162,23.3279243245241,12.));
#247526=CARTESIAN_POINT('Ctrl Pts',(7.63553608458783,23.3042388521021,0.));
#247527=CARTESIAN_POINT('Ctrl Pts',(7.63553608458783,23.3042388521021,12.));
#247528=CARTESIAN_POINT('Ctrl Pts',(7.63756546576374,23.2806359350853,0.));
#247529=CARTESIAN_POINT('Ctrl Pts',(7.63756546576374,23.2806359350853,12.));
#247530=CARTESIAN_POINT('Ctrl Pts',(7.63952920172837,23.2571161884487,0.));
#247531=CARTESIAN_POINT('Ctrl Pts',(7.63952920172837,23.2571161884487,12.));
#247532=CARTESIAN_POINT('Ctrl Pts',(7.64142755851507,23.2336802320912,0.));
#247533=CARTESIAN_POINT('Ctrl Pts',(7.64142755851507,23.2336802320912,12.));
#247534=CARTESIAN_POINT('Ctrl Pts',(7.64326080583683,23.2103286909399,0.));
#247535=CARTESIAN_POINT('Ctrl Pts',(7.64326080583683,23.2103286909399,12.));
#247536=CARTESIAN_POINT('Ctrl Pts',(7.64502921715482,23.1870621950452,0.));
#247537=CARTESIAN_POINT('Ctrl Pts',(7.64502921715482,23.1870621950452,12.));
#247538=CARTESIAN_POINT('Ctrl Pts',(7.64673306975796,23.1638813796691,0.));
#247539=CARTESIAN_POINT('Ctrl Pts',(7.64673306975796,23.1638813796691,12.));
#247540=CARTESIAN_POINT('Ctrl Pts',(7.64837264482929,23.1407868853815,0.));
#247541=CARTESIAN_POINT('Ctrl Pts',(7.64837264482929,23.1407868853815,12.));
#247542=CARTESIAN_POINT('Ctrl Pts',(7.64994822749844,23.1177793581674,0.));
#247543=CARTESIAN_POINT('Ctrl Pts',(7.64994822749844,23.1177793581674,12.));
#247544=CARTESIAN_POINT('Ctrl Pts',(7.65146010690464,23.0948594495246,0.));
#247545=CARTESIAN_POINT('Ctrl Pts',(7.65146010690464,23.0948594495246,12.));
#247546=CARTESIAN_POINT('Ctrl Pts',(7.65290857626356,23.072027816555,0.));
#247547=CARTESIAN_POINT('Ctrl Pts',(7.65290857626356,23.072027816555,12.));
#247548=CARTESIAN_POINT('Ctrl Pts',(7.65429393293955,23.049285122053,0.));
#247549=CARTESIAN_POINT('Ctrl Pts',(7.65429393293955,23.049285122053,12.));
#247550=CARTESIAN_POINT('Ctrl Pts',(7.65561647852554,23.0266320345792,0.));
#247551=CARTESIAN_POINT('Ctrl Pts',(7.65561647852554,23.0266320345792,12.));
#247552=CARTESIAN_POINT('Ctrl Pts',(7.6568765189133,23.004069228582,0.));
#247553=CARTESIAN_POINT('Ctrl Pts',(7.6568765189133,23.004069228582,12.));
#247554=CARTESIAN_POINT('Ctrl Pts',(7.65807436436452,22.9815973845301,0.));
#247555=CARTESIAN_POINT('Ctrl Pts',(7.65807436436452,22.9815973845301,12.));
#247556=CARTESIAN_POINT('Ctrl Pts',(7.65921032958911,22.9592171890332,0.));
#247557=CARTESIAN_POINT('Ctrl Pts',(7.65921032958911,22.9592171890332,12.));
#247558=CARTESIAN_POINT('Ctrl Pts',(7.66028473382776,22.9369293349592,0.));
#247559=CARTESIAN_POINT('Ctrl Pts',(7.66028473382776,22.9369293349592,12.));
#247560=CARTESIAN_POINT('Ctrl Pts',(7.66129790094099,22.9147345215418,0.));
#247561=CARTESIAN_POINT('Ctrl Pts',(7.66129790094099,22.9147345215418,12.));
#247562=CARTESIAN_POINT('Ctrl Pts',(7.66225015950147,22.8926334544879,0.));
#247563=CARTESIAN_POINT('Ctrl Pts',(7.66225015950147,22.8926334544879,12.));
#247564=CARTESIAN_POINT('Ctrl Pts',(7.66314184287333,22.870626846128,0.));
#247565=CARTESIAN_POINT('Ctrl Pts',(7.66314184287333,22.870626846128,12.));
#247566=CARTESIAN_POINT('Ctrl Pts',(7.66397328929805,22.8487154155569,0.));
#247567=CARTESIAN_POINT('Ctrl Pts',(7.66397328929805,22.8487154155569,12.));
#247568=CARTESIAN_POINT('Ctrl Pts',(7.66474484198552,22.8268998887679,0.));
#247569=CARTESIAN_POINT('Ctrl Pts',(7.66474484198552,22.8268998887679,12.));
#247570=CARTESIAN_POINT('Ctrl Pts',(7.66545684920987,22.8051809987834,0.));
#247571=CARTESIAN_POINT('Ctrl Pts',(7.66545684920987,22.8051809987834,12.));
#247572=CARTESIAN_POINT('Ctrl Pts',(7.66610966441259,22.7835594857697,0.));
#247573=CARTESIAN_POINT('Ctrl Pts',(7.66610966441259,22.7835594857697,12.));
#247574=CARTESIAN_POINT('Ctrl Pts',(7.66670364630273,22.7620360971839,0.));
#247575=CARTESIAN_POINT('Ctrl Pts',(7.66670364630273,22.7620360971839,12.));
#247576=CARTESIAN_POINT('Ctrl Pts',(7.66723915895412,22.7406115879508,0.));
#247577=CARTESIAN_POINT('Ctrl Pts',(7.66723915895412,22.7406115879508,12.));
#247578=CARTESIAN_POINT('Ctrl Pts',(7.6677165719101,22.7192867206242,0.));
#247579=CARTESIAN_POINT('Ctrl Pts',(7.6677165719101,22.7192867206242,12.));
#247580=CARTESIAN_POINT('Ctrl Pts',(7.66813626029276,22.6980622655446,0.));
#247581=CARTESIAN_POINT('Ctrl Pts',(7.66813626029276,22.6980622655446,12.));
#247582=CARTESIAN_POINT('Ctrl Pts',(7.66849860491762,22.6769390009889,0.));
#247583=CARTESIAN_POINT('Ctrl Pts',(7.66849860491762,22.6769390009889,12.));
#247584=CARTESIAN_POINT('Ctrl Pts',(7.66880399241353,22.6559177133133,0.));
#247585=CARTESIAN_POINT('Ctrl Pts',(7.66880399241353,22.6559177133133,12.));
#247586=CARTESIAN_POINT('Ctrl Pts',(7.66905281533744,22.6349991971548,0.));
#247587=CARTESIAN_POINT('Ctrl Pts',(7.66905281533744,22.6349991971548,12.));
#247588=CARTESIAN_POINT('Ctrl Pts',(7.66924547229434,22.6141842556248,0.));
#247589=CARTESIAN_POINT('Ctrl Pts',(7.66924547229434,22.6141842556248,12.));
#247590=CARTESIAN_POINT('Ctrl Pts',(7.6693823680624,22.5934737004955,0.));
#247591=CARTESIAN_POINT('Ctrl Pts',(7.6693823680624,22.5934737004955,12.));
#247592=CARTESIAN_POINT('Ctrl Pts',(7.66946391372299,22.5728683523829,0.));
#247593=CARTESIAN_POINT('Ctrl Pts',(7.66946391372299,22.5728683523829,12.));
#247594=CARTESIAN_POINT('Ctrl Pts',(7.66949052679671,22.5523690409109,0.));
#247595=CARTESIAN_POINT('Ctrl Pts',(7.66949052679671,22.5523690409109,12.));
#247596=CARTESIAN_POINT('Ctrl Pts',(7.66946263138115,22.5319766049191,0.));
#247597=CARTESIAN_POINT('Ctrl Pts',(7.66946263138115,22.5319766049191,12.));
#247598=CARTESIAN_POINT('Ctrl Pts',(7.66938065829082,22.5116918927023,0.));
#247599=CARTESIAN_POINT('Ctrl Pts',(7.66938065829082,22.5116918927023,12.));
#247600=CARTESIAN_POINT('Ctrl Pts',(7.66924504520301,22.4915157622308,0.));
#247601=CARTESIAN_POINT('Ctrl Pts',(7.66924504520301,22.4915157622308,12.));
#247602=CARTESIAN_POINT('Ctrl Pts',(7.66905623680835,22.47144908137,0.));
#247603=CARTESIAN_POINT('Ctrl Pts',(7.66905623680835,22.47144908137,12.));
#247604=CARTESIAN_POINT('Ctrl Pts',(7.66881468496659,22.4514927280863,0.));
#247605=CARTESIAN_POINT('Ctrl Pts',(7.66881468496659,22.4514927280863,12.));
#247606=CARTESIAN_POINT('Ctrl Pts',(7.66852084886745,22.4316475906616,0.));
#247607=CARTESIAN_POINT('Ctrl Pts',(7.66852084886745,22.4316475906616,12.));
#247608=CARTESIAN_POINT('Ctrl Pts',(7.66817519519681,22.411914567977,0.));
#247609=CARTESIAN_POINT('Ctrl Pts',(7.66817519519681,22.411914567977,12.));
#247610=CARTESIAN_POINT('Ctrl Pts',(7.66777819830819,22.3922945697782,0.));
#247611=CARTESIAN_POINT('Ctrl Pts',(7.66777819830819,22.3922945697782,12.));
#247612=CARTESIAN_POINT('Ctrl Pts',(7.66733034039887,22.3727885169361,0.));
#247613=CARTESIAN_POINT('Ctrl Pts',(7.66733034039887,22.3727885169361,12.));
#247614=CARTESIAN_POINT('Ctrl Pts',(7.66683211169133,22.3533973417013,0.));
#247615=CARTESIAN_POINT('Ctrl Pts',(7.66683211169133,22.3533973417013,12.));
#247616=CARTESIAN_POINT('Ctrl Pts',(7.66628401061905,22.3341219879454,0.));
#247617=CARTESIAN_POINT('Ctrl Pts',(7.66628401061905,22.3341219879454,12.));
#247618=CARTESIAN_POINT('Ctrl Pts',(7.66568654402441,22.3149634114823,0.));
#247619=CARTESIAN_POINT('Ctrl Pts',(7.66568654402441,22.3149634114823,12.));
#247620=CARTESIAN_POINT('Ctrl Pts',(7.66504022736262,22.2959225803925,0.));
#247621=CARTESIAN_POINT('Ctrl Pts',(7.66504022736262,22.2959225803925,12.));
#247622=CARTESIAN_POINT('Ctrl Pts',(7.66434558490972,22.2770004753332,0.));
#247623=CARTESIAN_POINT('Ctrl Pts',(7.66434558490972,22.2770004753332,12.));
#247624=CARTESIAN_POINT('Ctrl Pts',(7.66360314997661,22.2581980898487,0.));
#247625=CARTESIAN_POINT('Ctrl Pts',(7.66360314997661,22.2581980898487,12.));
#247626=CARTESIAN_POINT('Ctrl Pts',(7.66281346512545,22.239516430656,0.));
#247627=CARTESIAN_POINT('Ctrl Pts',(7.66281346512545,22.239516430656,12.));
#247628=CARTESIAN_POINT('Ctrl Pts',(7.66197708240435,22.2209565180098,0.));
#247629=CARTESIAN_POINT('Ctrl Pts',(7.66197708240435,22.2209565180098,12.));
#247630=CARTESIAN_POINT('Ctrl Pts',(7.66109456359292,22.2025193860972,0.));
#247631=CARTESIAN_POINT('Ctrl Pts',(7.66109456359292,22.2025193860972,12.));
#247632=CARTESIAN_POINT('Ctrl Pts',(7.66016648045007,22.1842060834093,0.));
#247633=CARTESIAN_POINT('Ctrl Pts',(7.66016648045007,22.1842060834093,12.));
#247634=CARTESIAN_POINT('Ctrl Pts',(7.65919341496925,22.1660176731174,0.));
#247635=CARTESIAN_POINT('Ctrl Pts',(7.65919341496925,22.1660176731174,12.));
#247636=CARTESIAN_POINT('Ctrl Pts',(7.6581759596335,22.1479552334206,0.));
#247637=CARTESIAN_POINT('Ctrl Pts',(7.6581759596335,22.1479552334206,12.));
#247638=CARTESIAN_POINT('Ctrl Pts',(7.65711471769406,22.1300198579671,0.));
#247639=CARTESIAN_POINT('Ctrl Pts',(7.65711471769406,22.1300198579671,12.));
#247640=CARTESIAN_POINT('Ctrl Pts',(7.65601030346818,22.1122126563327,0.));
#247641=CARTESIAN_POINT('Ctrl Pts',(7.65601030346818,22.1122126563327,12.));
#247642=CARTESIAN_POINT('Ctrl Pts',(7.6548633426365,22.094534754469,0.));
#247643=CARTESIAN_POINT('Ctrl Pts',(7.6548633426365,22.094534754469,12.));
#247644=CARTESIAN_POINT('Ctrl Pts',(7.65367447254944,22.0769872951596,0.));
#247645=CARTESIAN_POINT('Ctrl Pts',(7.65367447254944,22.0769872951596,12.));
#247646=CARTESIAN_POINT('Ctrl Pts',(7.65244434253103,22.0595714384432,0.));
#247647=CARTESIAN_POINT('Ctrl Pts',(7.65244434253103,22.0595714384432,12.));
#247648=CARTESIAN_POINT('Ctrl Pts',(7.65117361421346,22.0422883621176,0.));
#247649=CARTESIAN_POINT('Ctrl Pts',(7.65117361421346,22.0422883621176,12.));
#247650=CARTESIAN_POINT('Ctrl Pts',(7.64986296190156,22.025139262321,0.));
#247651=CARTESIAN_POINT('Ctrl Pts',(7.64986296190156,22.025139262321,12.));
#247652=CARTESIAN_POINT('Ctrl Pts',(7.64851307293345,22.0081253540774,0.));
#247653=CARTESIAN_POINT('Ctrl Pts',(7.64851307293345,22.0081253540774,12.));
#247654=CARTESIAN_POINT('Ctrl Pts',(7.64712464805257,21.9912478718542,0.));
#247655=CARTESIAN_POINT('Ctrl Pts',(7.64712464805257,21.9912478718542,12.));
#247656=CARTESIAN_POINT('Ctrl Pts',(7.64569840177359,21.97450807008,0.));
#247657=CARTESIAN_POINT('Ctrl Pts',(7.64569840177359,21.97450807008,12.));
#247658=CARTESIAN_POINT('Ctrl Pts',(7.64423506279153,21.9579072237653,0.));
#247659=CARTESIAN_POINT('Ctrl Pts',(7.64423506279153,21.9579072237653,12.));
#247660=CARTESIAN_POINT('Ctrl Pts',(7.64273537442706,21.9414466292074,0.));
#247661=CARTESIAN_POINT('Ctrl Pts',(7.64273537442706,21.9414466292074,12.));
#247662=CARTESIAN_POINT('Ctrl Pts',(7.64120009506539,21.9251276046546,0.));
#247663=CARTESIAN_POINT('Ctrl Pts',(7.64120009506539,21.9251276046546,12.));
#247664=CARTESIAN_POINT('Ctrl Pts',(7.63962999860916,21.9089514909873,0.));
#247665=CARTESIAN_POINT('Ctrl Pts',(7.63962999860916,21.9089514909873,12.));
#247666=CARTESIAN_POINT('Ctrl Pts',(7.63802587492007,21.8929196523511,0.));
#247667=CARTESIAN_POINT('Ctrl Pts',(7.63802587492007,21.8929196523511,12.));
#247668=CARTESIAN_POINT('Ctrl Pts',(7.63638853033367,21.8770334769492,0.));
#247669=CARTESIAN_POINT('Ctrl Pts',(7.63638853033367,21.8770334769492,12.));
#247670=CARTESIAN_POINT('Ctrl Pts',(7.63471878821203,21.8612943779086,0.));
#247671=CARTESIAN_POINT('Ctrl Pts',(7.63471878821203,21.8612943779086,12.));
#247672=CARTESIAN_POINT('Ctrl Pts',(7.63301748948936,21.8457037941084,0.));
#247673=CARTESIAN_POINT('Ctrl Pts',(7.63301748948936,21.8457037941084,12.));
#247674=CARTESIAN_POINT('Ctrl Pts',(7.6312854932304,21.8302631910197,0.));
#247675=CARTESIAN_POINT('Ctrl Pts',(7.6312854932304,21.8302631910197,12.));
#247676=CARTESIAN_POINT('Ctrl Pts',(7.62952367718151,21.8149740615093,0.));
#247677=CARTESIAN_POINT('Ctrl Pts',(7.62952367718151,21.8149740615093,12.));
#247678=CARTESIAN_POINT('Ctrl Pts',(7.62773293842409,21.7998379268583,0.));
#247679=CARTESIAN_POINT('Ctrl Pts',(7.62773293842409,21.7998379268583,12.));
#247680=CARTESIAN_POINT('Ctrl Pts',(7.6259141940452,21.7848563378022,0.));
#247681=CARTESIAN_POINT('Ctrl Pts',(7.6259141940452,21.7848563378022,12.));
#247682=CARTESIAN_POINT('Ctrl Pts',(7.62406838181164,21.7700308755584,0.));
#247683=CARTESIAN_POINT('Ctrl Pts',(7.62406838181164,21.7700308755584,12.));
#247684=CARTESIAN_POINT('Ctrl Pts',(7.62219646084225,21.7553631528329,0.));
#247685=CARTESIAN_POINT('Ctrl Pts',(7.62219646084225,21.7553631528329,12.));
#247686=CARTESIAN_POINT('Ctrl Pts',(7.62029941230854,21.7408548148657,0.));
#247687=CARTESIAN_POINT('Ctrl Pts',(7.62029941230854,21.7408548148657,12.));
#247688=CARTESIAN_POINT('Ctrl Pts',(7.61837824030541,21.7265075407977,0.));
#247689=CARTESIAN_POINT('Ctrl Pts',(7.61837824030541,21.7265075407977,12.));
#247690=CARTESIAN_POINT('Ctrl Pts',(7.61643397270424,21.7123230449835,0.));
#247691=CARTESIAN_POINT('Ctrl Pts',(7.61643397270424,21.7123230449835,12.));
#247692=CARTESIAN_POINT('Ctrl Pts',(7.61446766202786,21.6983030783321,0.));
#247693=CARTESIAN_POINT('Ctrl Pts',(7.61446766202786,21.6983030783321,12.));
#247694=CARTESIAN_POINT('Ctrl Pts',(7.61248038630264,21.6844494295813,0.));
#247695=CARTESIAN_POINT('Ctrl Pts',(7.61248038630264,21.6844494295813,12.));
#247696=CARTESIAN_POINT('Ctrl Pts',(7.61047325000949,21.6707639267573,0.));
#247697=CARTESIAN_POINT('Ctrl Pts',(7.61047325000949,21.6707639267573,12.));
#247698=CARTESIAN_POINT('Ctrl Pts',(7.60844738512871,21.6572484388079,0.));
#247699=CARTESIAN_POINT('Ctrl Pts',(7.60844738512871,21.6572484388079,12.));
#247700=CARTESIAN_POINT('Ctrl Pts',(7.60640395216358,21.6439048771743,0.));
#247701=CARTESIAN_POINT('Ctrl Pts',(7.60640395216358,21.6439048771743,12.));
#247702=CARTESIAN_POINT('Ctrl Pts',(7.60434414118299,21.6307351973823,0.));
#247703=CARTESIAN_POINT('Ctrl Pts',(7.60434414118299,21.6307351973823,12.));
#247704=CARTESIAN_POINT('Ctrl Pts',(7.60226917285431,21.6177414005991,0.));
#247705=CARTESIAN_POINT('Ctrl Pts',(7.60226917285431,21.6177414005991,12.));
#247706=CARTESIAN_POINT('Ctrl Pts',(7.60018029988238,21.6049255358843,0.));
#247707=CARTESIAN_POINT('Ctrl Pts',(7.60018029988238,21.6049255358843,12.));
#247708=CARTESIAN_POINT('Ctrl Pts',(7.59807880846192,21.5922897024466,0.));
#247709=CARTESIAN_POINT('Ctrl Pts',(7.59807880846192,21.5922897024466,12.));
#247710=CARTESIAN_POINT('Ctrl Pts',(7.59596601973588,21.5798360518978,0.));
#247711=CARTESIAN_POINT('Ctrl Pts',(7.59596601973588,21.5798360518978,12.));
#247712=CARTESIAN_POINT('Ctrl Pts',(7.59384329124929,21.5675667904728,0.));
#247713=CARTESIAN_POINT('Ctrl Pts',(7.59384329124929,21.5675667904728,12.));
#247714=CARTESIAN_POINT('Ctrl Pts',(7.59171201844792,21.5554841813466,0.));
#247715=CARTESIAN_POINT('Ctrl Pts',(7.59171201844792,21.5554841813466,12.));
#247716=CARTESIAN_POINT('Ctrl Pts',(7.58957363620026,21.5435905470113,0.));
#247717=CARTESIAN_POINT('Ctrl Pts',(7.58957363620026,21.5435905470113,12.));
#247718=CARTESIAN_POINT('Ctrl Pts',(7.58742962034834,21.5318882716736,0.));
#247719=CARTESIAN_POINT('Ctrl Pts',(7.58742962034834,21.5318882716736,12.));
#247720=CARTESIAN_POINT('Ctrl Pts',(7.58528148919113,21.5203798035294,0.));
#247721=CARTESIAN_POINT('Ctrl Pts',(7.58528148919113,21.5203798035294,12.));
#247722=CARTESIAN_POINT('Ctrl Pts',(7.58313080519158,21.5090676573866,0.));
#247723=CARTESIAN_POINT('Ctrl Pts',(7.58313080519158,21.5090676573866,12.));
#247724=CARTESIAN_POINT('Ctrl Pts',(7.58097917790729,21.497954419274,0.));
#247725=CARTESIAN_POINT('Ctrl Pts',(7.58097917790729,21.497954419274,12.));
#247726=CARTESIAN_POINT('Ctrl Pts',(7.57882826679131,21.4870427508193,0.));
#247727=CARTESIAN_POINT('Ctrl Pts',(7.57882826679131,21.4870427508193,12.));
#247728=CARTESIAN_POINT('Ctrl Pts',(7.57667978403001,21.4763353936766,0.));
#247729=CARTESIAN_POINT('Ctrl Pts',(7.57667978403001,21.4763353936766,12.));
#247730=CARTESIAN_POINT('Ctrl Pts',(7.57453549743434,21.4658351740135,0.));
#247731=CARTESIAN_POINT('Ctrl Pts',(7.57453549743434,21.4658351740135,12.));
#247732=CARTESIAN_POINT('Ctrl Pts',(7.57239723223521,21.4555450053147,0.));
#247733=CARTESIAN_POINT('Ctrl Pts',(7.57239723223521,21.4555450053147,12.));
#247734=CARTESIAN_POINT('Ctrl Pts',(7.57026687261169,21.445467890751,0.));
#247735=CARTESIAN_POINT('Ctrl Pts',(7.57026687261169,21.445467890751,12.));
#247736=CARTESIAN_POINT('Ctrl Pts',(7.56814636360841,21.435606926151,0.));
#247737=CARTESIAN_POINT('Ctrl Pts',(7.56814636360841,21.435606926151,12.));
#247738=CARTESIAN_POINT('Ctrl Pts',(7.56603771218706,21.4259653015732,0.));
#247739=CARTESIAN_POINT('Ctrl Pts',(7.56603771218706,21.4259653015732,12.));
#247740=CARTESIAN_POINT('Ctrl Pts',(7.56394299313682,21.4165463106252,0.));
#247741=CARTESIAN_POINT('Ctrl Pts',(7.56394299313682,21.4165463106252,12.));
#247742=CARTESIAN_POINT('Ctrl Pts',(7.56186435703622,21.4073533630364,0.));
#247743=CARTESIAN_POINT('Ctrl Pts',(7.56186435703622,21.4073533630364,12.));
#247744=CARTESIAN_POINT('Ctrl Pts',(7.55980403700614,21.3983899952988,0.));
#247745=CARTESIAN_POINT('Ctrl Pts',(7.55980403700614,21.3983899952988,12.));
#247746=CARTESIAN_POINT('Ctrl Pts',(7.55776435731421,21.3896598842119,0.));
#247747=CARTESIAN_POINT('Ctrl Pts',(7.55776435731421,21.3896598842119,12.));
#247748=CARTESIAN_POINT('Ctrl Pts',(7.55574773403507,21.3811668478933,0.));
#247749=CARTESIAN_POINT('Ctrl Pts',(7.55574773403507,21.3811668478933,12.));
#247750=CARTESIAN_POINT('Ctrl Pts',(7.55375667080031,21.3729148390244,0.));
#247751=CARTESIAN_POINT('Ctrl Pts',(7.55375667080031,21.3729148390244,12.));
#247752=CARTESIAN_POINT('Ctrl Pts',(7.55179375777441,21.3649079431864,0.));
#247753=CARTESIAN_POINT('Ctrl Pts',(7.55179375777441,21.3649079431864,12.));
#247754=CARTESIAN_POINT('Ctrl Pts',(7.54986166521306,21.3571503685853,0.));
#247755=CARTESIAN_POINT('Ctrl Pts',(7.54986166521306,21.3571503685853,12.));
#247756=CARTESIAN_POINT('Ctrl Pts',(7.54796316246326,21.349646476153,0.));
#247757=CARTESIAN_POINT('Ctrl Pts',(7.54796316246326,21.349646476153,12.));
#247758=CARTESIAN_POINT('Ctrl Pts',(7.5461011494835,21.3424008295038,0.));
#247759=CARTESIAN_POINT('Ctrl Pts',(7.5461011494835,21.3424008295038,12.));
#247760=CARTESIAN_POINT('Ctrl Pts',(7.54427868151268,21.3354182340149,0.));
#247761=CARTESIAN_POINT('Ctrl Pts',(7.54427868151268,21.3354182340149,12.));
#247762=CARTESIAN_POINT('Ctrl Pts',(7.54249900377031,21.328703791771,0.));
#247763=CARTESIAN_POINT('Ctrl Pts',(7.54249900377031,21.328703791771,12.));
#247764=CARTESIAN_POINT('Ctrl Pts',(7.54076552038279,21.3222628524165,0.));
#247765=CARTESIAN_POINT('Ctrl Pts',(7.54076552038279,21.3222628524165,12.));
#247766=CARTESIAN_POINT('Ctrl Pts',(7.53908175169898,21.3161009456256,0.));
#247767=CARTESIAN_POINT('Ctrl Pts',(7.53908175169898,21.3161009456256,12.));
#247768=CARTESIAN_POINT('Ctrl Pts',(7.53745129364619,21.3102237167729,0.));
#247769=CARTESIAN_POINT('Ctrl Pts',(7.53745129364619,21.3102237167729,12.));
#247770=CARTESIAN_POINT('Ctrl Pts',(7.53587778251743,21.3046368712157,0.));
#247771=CARTESIAN_POINT('Ctrl Pts',(7.53587778251743,21.3046368712157,12.));
#247772=CARTESIAN_POINT('Ctrl Pts',(7.53436505309948,21.2993464250717,0.));
#247773=CARTESIAN_POINT('Ctrl Pts',(7.53436505309948,21.2993464250717,12.));
#247774=CARTESIAN_POINT('Ctrl Pts',(7.53291726078526,21.2943588989331,0.));
#247775=CARTESIAN_POINT('Ctrl Pts',(7.53291726078526,21.2943588989331,12.));
#247776=CARTESIAN_POINT('Ctrl Pts',(7.53153906987846,21.2896816163843,0.));
#247777=CARTESIAN_POINT('Ctrl Pts',(7.53153906987846,21.2896816163843,12.));
#247778=CARTESIAN_POINT('Ctrl Pts',(7.5302356243822,21.2853226580658,0.));
#247779=CARTESIAN_POINT('Ctrl Pts',(7.5302356243822,21.2853226580658,12.));
#247780=CARTESIAN_POINT('Ctrl Pts',(7.52901217930407,21.2812902781143,0.));
#247781=CARTESIAN_POINT('Ctrl Pts',(7.52901217930407,21.2812902781143,12.));
#247782=CARTESIAN_POINT('Ctrl Pts',(7.52787386225343,21.2775925269652,0.));
#247783=CARTESIAN_POINT('Ctrl Pts',(7.52787386225343,21.2775925269652,12.));
#247784=CARTESIAN_POINT('Ctrl Pts',(7.5268252691856,21.2742366113578,0.));
#247785=CARTESIAN_POINT('Ctrl Pts',(7.5268252691856,21.2742366113578,12.));
#247786=CARTESIAN_POINT('Ctrl Pts',(7.52587126095544,21.2712301573465,0.));
#247787=CARTESIAN_POINT('Ctrl Pts',(7.52587126095544,21.2712301573465,12.));
#247788=CARTESIAN_POINT('Ctrl Pts',(7.52501770333521,21.2685823838672,0.));
#247789=CARTESIAN_POINT('Ctrl Pts',(7.52501770333521,21.2685823838672,12.));
#247790=CARTESIAN_POINT('Ctrl Pts',(7.52427261074263,21.266305915706,0.));
#247791=CARTESIAN_POINT('Ctrl Pts',(7.52427261074263,21.266305915706,12.));
#247792=CARTESIAN_POINT('Ctrl Pts',(7.52364573027521,21.2644161259965,0.));
#247793=CARTESIAN_POINT('Ctrl Pts',(7.52364573027521,21.2644161259965,12.));
#247794=CARTESIAN_POINT('Ctrl Pts',(7.52314642316202,21.262927782038,0.));
#247795=CARTESIAN_POINT('Ctrl Pts',(7.52314642316202,21.262927782038,12.));
#247796=CARTESIAN_POINT('Ctrl Pts',(7.52278182242727,21.261852128355,0.));
#247797=CARTESIAN_POINT('Ctrl Pts',(7.52278182242727,21.261852128355,12.));
#247798=CARTESIAN_POINT('Ctrl Pts',(7.52260064231736,21.2613260540651,0.));
#247799=CARTESIAN_POINT('Ctrl Pts',(7.52260064231736,21.2613260540651,12.));
#247800=CARTESIAN_POINT('Ctrl Pts',(7.52252744144957,21.261120447486,0.));
#247801=CARTESIAN_POINT('Ctrl Pts',(7.52252744144957,21.261120447486,12.));
#247802=CARTESIAN_POINT('Ctrl Pts',(7.52250649703991,21.2610673466883,0.));
#247803=CARTESIAN_POINT('Ctrl Pts',(7.52250649703991,21.2610673466883,12.));
#247804=CARTESIAN_POINT('Ctrl Pts',(7.52250298901265,21.2610617890679,0.));
#247805=CARTESIAN_POINT('Ctrl Pts',(7.52250298901265,21.2610617890679,12.));
#247806=CARTESIAN_POINT('',(7.36589684767344,24.9347862158358,0.));
#247807=CARTESIAN_POINT('Ctrl Pts',(7.36589684767344,24.9347862158358,0.));
#247808=CARTESIAN_POINT('Ctrl Pts',(7.36721909028842,24.9292275670674,0.));
#247809=CARTESIAN_POINT('Ctrl Pts',(7.3698559312009,24.9181155530543,0.));
#247810=CARTESIAN_POINT('Ctrl Pts',(7.37378825961676,24.901463382605,0.));
#247811=CARTESIAN_POINT('Ctrl Pts',(7.37898549640269,24.8792921911115,0.));
#247812=CARTESIAN_POINT('Ctrl Pts',(7.3854055890362,24.8516310625176,0.));
#247813=CARTESIAN_POINT('Ctrl Pts',(7.39174922585808,24.8240228520893,0.));
#247814=CARTESIAN_POINT('Ctrl Pts',(7.39801641583012,24.7964676646431,0.));
#247815=CARTESIAN_POINT('Ctrl Pts',(7.40420718661602,24.7689656668983,0.));
#247816=CARTESIAN_POINT('Ctrl Pts',(7.41032159082381,24.7415170994784,0.));
#247817=CARTESIAN_POINT('Ctrl Pts',(7.41635971481674,24.7141222950051,0.));
#247818=CARTESIAN_POINT('Ctrl Pts',(7.42232167766265,24.6867816727192,0.));
#247819=CARTESIAN_POINT('Ctrl Pts',(7.42820762159125,24.6594957128756,0.));
#247820=CARTESIAN_POINT('Ctrl Pts',(7.43401770489523,24.6322649369517,0.));
#247821=CARTESIAN_POINT('Ctrl Pts',(7.43975209375503,24.6050898852368,0.));
#247822=CARTESIAN_POINT('Ctrl Pts',(7.44541095473134,24.577971096086,0.));
#247823=CARTESIAN_POINT('Ctrl Pts',(7.4509944465116,24.5509090831559,0.));
#247824=CARTESIAN_POINT('Ctrl Pts',(7.45650271335861,24.5239043173072,0.));
#247825=CARTESIAN_POINT('Ctrl Pts',(7.46193588961463,24.4969572391483,0.));
#247826=CARTESIAN_POINT('Ctrl Pts',(7.46729410308786,24.4700682684524,0.));
#247827=CARTESIAN_POINT('Ctrl Pts',(7.47257747883246,24.443237814649,0.));
#247828=CARTESIAN_POINT('Ctrl Pts',(7.47778614286564,24.4164662871163,0.));
#247829=CARTESIAN_POINT('Ctrl Pts',(7.482920225693,24.3897541049254,0.));
#247830=CARTESIAN_POINT('Ctrl Pts',(7.48797986651908,24.3631017084524,0.));
#247831=CARTESIAN_POINT('Ctrl Pts',(7.4929652125242,24.3365095573685,0.));
#247832=CARTESIAN_POINT('Ctrl Pts',(7.49787641695438,24.3099781253355,0.));
#247833=CARTESIAN_POINT('Ctrl Pts',(7.50271363765151,24.2835078958973,0.));
#247834=CARTESIAN_POINT('Ctrl Pts',(7.50747703535133,24.2570993577034,0.));
#247835=CARTESIAN_POINT('Ctrl Pts',(7.5121667722218,24.2307530003887,0.));
#247836=CARTESIAN_POINT('Ctrl Pts',(7.51678300997949,24.2044693092349,0.));
#247837=CARTESIAN_POINT('Ctrl Pts',(7.52132590953801,24.1782487641594,0.));
#247838=CARTESIAN_POINT('Ctrl Pts',(7.52579563201423,24.1520918425364,0.));
#247839=CARTESIAN_POINT('Ctrl Pts',(7.53019233935501,24.1259990209207,0.));
#247840=CARTESIAN_POINT('Ctrl Pts',(7.53451619514649,24.0999707772642,0.));
#247841=CARTESIAN_POINT('Ctrl Pts',(7.53876736531013,24.0740075927985,0.));
#247842=CARTESIAN_POINT('Ctrl Pts',(7.54294601896144,24.0481099543353,0.));
#247843=CARTESIAN_POINT('Ctrl Pts',(7.5470523288591,24.022278355453,0.));
#247844=CARTESIAN_POINT('Ctrl Pts',(7.5510864709744,23.9965132953185,0.));
#247845=CARTESIAN_POINT('Ctrl Pts',(7.55504862424811,23.9708152779884,0.));
#247846=CARTESIAN_POINT('Ctrl Pts',(7.55893897027682,23.9451848115,0.));
#247847=CARTESIAN_POINT('Ctrl Pts',(7.56275769304773,23.9196224070759,0.));
#247848=CARTESIAN_POINT('Ctrl Pts',(7.56650497863791,23.8941285782003,0.));
#247849=CARTESIAN_POINT('Ctrl Pts',(7.5701810150071,23.8687038399598,0.));
#247850=CARTESIAN_POINT('Ctrl Pts',(7.57378599219816,23.8433487096134,0.));
#247851=CARTESIAN_POINT('Ctrl Pts',(7.57732010249065,23.8180637069977,0.));
#247852=CARTESIAN_POINT('Ctrl Pts',(7.58078354058211,23.7928493549908,0.));
#247853=CARTESIAN_POINT('Ctrl Pts',(7.58417650376271,23.7677061799376,0.));
#247854=CARTESIAN_POINT('Ctrl Pts',(7.58749919210831,23.7426347121006,0.));
#247855=CARTESIAN_POINT('Ctrl Pts',(7.59075180865326,23.7176354860457,0.));
#247856=CARTESIAN_POINT('Ctrl Pts',(7.59393455934041,23.6927090405067,0.));
#247857=CARTESIAN_POINT('Ctrl Pts',(7.59704765299572,23.6678559182876,0.));
#247858=CARTESIAN_POINT('Ctrl Pts',(7.60009130130129,23.6430766661419,0.));
#247859=CARTESIAN_POINT('Ctrl Pts',(7.60306571877806,23.6183718346576,0.));
#247860=CARTESIAN_POINT('Ctrl Pts',(7.60597112277094,23.5937419781244,0.));
#247861=CARTESIAN_POINT('Ctrl Pts',(7.60880773344599,23.5691876544243,0.));
#247862=CARTESIAN_POINT('Ctrl Pts',(7.61157577385371,23.5447094252029,0.));
#247863=CARTESIAN_POINT('Ctrl Pts',(7.61427546999298,23.5203078560128,0.));
#247864=CARTESIAN_POINT('Ctrl Pts',(7.61690705088318,23.4959835164608,0.));
#247865=CARTESIAN_POINT('Ctrl Pts',(7.61947074863977,23.4717369803438,0.));
#247866=CARTESIAN_POINT('Ctrl Pts',(7.62196679855957,23.4475688257855,0.));
#247867=CARTESIAN_POINT('Ctrl Pts',(7.62439543920053,23.4234796353544,0.));
#247868=CARTESIAN_POINT('Ctrl Pts',(7.62675691240334,23.3994699961122,0.));
#247869=CARTESIAN_POINT('Ctrl Pts',(7.62905146332597,23.3755404996638,0.));
#247870=CARTESIAN_POINT('Ctrl Pts',(7.63127934048138,23.3516917421973,0.));
#247871=CARTESIAN_POINT('Ctrl Pts',(7.63344079578162,23.3279243245241,0.));
#247872=CARTESIAN_POINT('Ctrl Pts',(7.63553608458783,23.3042388521021,0.));
#247873=CARTESIAN_POINT('Ctrl Pts',(7.63756546576374,23.2806359350853,0.));
#247874=CARTESIAN_POINT('Ctrl Pts',(7.63952920172837,23.2571161884487,0.));
#247875=CARTESIAN_POINT('Ctrl Pts',(7.64142755851507,23.2336802320912,0.));
#247876=CARTESIAN_POINT('Ctrl Pts',(7.64326080583683,23.2103286909399,0.));
#247877=CARTESIAN_POINT('Ctrl Pts',(7.64502921715482,23.1870621950452,0.));
#247878=CARTESIAN_POINT('Ctrl Pts',(7.64673306975796,23.1638813796691,0.));
#247879=CARTESIAN_POINT('Ctrl Pts',(7.64837264482929,23.1407868853815,0.));
#247880=CARTESIAN_POINT('Ctrl Pts',(7.64994822749844,23.1177793581674,0.));
#247881=CARTESIAN_POINT('Ctrl Pts',(7.65146010690464,23.0948594495246,0.));
#247882=CARTESIAN_POINT('Ctrl Pts',(7.65290857626356,23.072027816555,0.));
#247883=CARTESIAN_POINT('Ctrl Pts',(7.65429393293955,23.049285122053,0.));
#247884=CARTESIAN_POINT('Ctrl Pts',(7.65561647852554,23.0266320345792,0.));
#247885=CARTESIAN_POINT('Ctrl Pts',(7.6568765189133,23.004069228582,0.));
#247886=CARTESIAN_POINT('Ctrl Pts',(7.65807436436452,22.9815973845301,0.));
#247887=CARTESIAN_POINT('Ctrl Pts',(7.65921032958911,22.9592171890332,0.));
#247888=CARTESIAN_POINT('Ctrl Pts',(7.66028473382776,22.9369293349592,0.));
#247889=CARTESIAN_POINT('Ctrl Pts',(7.66129790094099,22.9147345215418,0.));
#247890=CARTESIAN_POINT('Ctrl Pts',(7.66225015950147,22.8926334544879,0.));
#247891=CARTESIAN_POINT('Ctrl Pts',(7.66314184287333,22.870626846128,0.));
#247892=CARTESIAN_POINT('Ctrl Pts',(7.66397328929805,22.8487154155569,0.));
#247893=CARTESIAN_POINT('Ctrl Pts',(7.66474484198552,22.8268998887679,0.));
#247894=CARTESIAN_POINT('Ctrl Pts',(7.66545684920987,22.8051809987834,0.));
#247895=CARTESIAN_POINT('Ctrl Pts',(7.66610966441259,22.7835594857697,0.));
#247896=CARTESIAN_POINT('Ctrl Pts',(7.66670364630273,22.7620360971839,0.));
#247897=CARTESIAN_POINT('Ctrl Pts',(7.66723915895412,22.7406115879508,0.));
#247898=CARTESIAN_POINT('Ctrl Pts',(7.6677165719101,22.7192867206242,0.));
#247899=CARTESIAN_POINT('Ctrl Pts',(7.66813626029276,22.6980622655446,0.));
#247900=CARTESIAN_POINT('Ctrl Pts',(7.66849860491762,22.6769390009889,0.));
#247901=CARTESIAN_POINT('Ctrl Pts',(7.66880399241353,22.6559177133133,0.));
#247902=CARTESIAN_POINT('Ctrl Pts',(7.66905281533744,22.6349991971548,0.));
#247903=CARTESIAN_POINT('Ctrl Pts',(7.66924547229434,22.6141842556248,0.));
#247904=CARTESIAN_POINT('Ctrl Pts',(7.6693823680624,22.5934737004955,0.));
#247905=CARTESIAN_POINT('Ctrl Pts',(7.66946391372299,22.5728683523829,0.));
#247906=CARTESIAN_POINT('Ctrl Pts',(7.66949052679671,22.5523690409109,0.));
#247907=CARTESIAN_POINT('Ctrl Pts',(7.66946263138115,22.5319766049191,0.));
#247908=CARTESIAN_POINT('Ctrl Pts',(7.66938065829082,22.5116918927023,0.));
#247909=CARTESIAN_POINT('Ctrl Pts',(7.66924504520301,22.4915157622308,0.));
#247910=CARTESIAN_POINT('Ctrl Pts',(7.66905623680835,22.47144908137,0.));
#247911=CARTESIAN_POINT('Ctrl Pts',(7.66881468496659,22.4514927280863,0.));
#247912=CARTESIAN_POINT('Ctrl Pts',(7.66852084886745,22.4316475906616,0.));
#247913=CARTESIAN_POINT('Ctrl Pts',(7.66817519519681,22.411914567977,0.));
#247914=CARTESIAN_POINT('Ctrl Pts',(7.66777819830819,22.3922945697782,0.));
#247915=CARTESIAN_POINT('Ctrl Pts',(7.66733034039887,22.3727885169361,0.));
#247916=CARTESIAN_POINT('Ctrl Pts',(7.66683211169133,22.3533973417013,0.));
#247917=CARTESIAN_POINT('Ctrl Pts',(7.66628401061905,22.3341219879454,0.));
#247918=CARTESIAN_POINT('Ctrl Pts',(7.66568654402441,22.3149634114823,0.));
#247919=CARTESIAN_POINT('Ctrl Pts',(7.66504022736262,22.2959225803925,0.));
#247920=CARTESIAN_POINT('Ctrl Pts',(7.66434558490972,22.2770004753332,0.));
#247921=CARTESIAN_POINT('Ctrl Pts',(7.66360314997661,22.2581980898487,0.));
#247922=CARTESIAN_POINT('Ctrl Pts',(7.66281346512545,22.239516430656,0.));
#247923=CARTESIAN_POINT('Ctrl Pts',(7.66197708240435,22.2209565180098,0.));
#247924=CARTESIAN_POINT('Ctrl Pts',(7.66109456359292,22.2025193860972,0.));
#247925=CARTESIAN_POINT('Ctrl Pts',(7.66016648045007,22.1842060834093,0.));
#247926=CARTESIAN_POINT('Ctrl Pts',(7.65919341496925,22.1660176731174,0.));
#247927=CARTESIAN_POINT('Ctrl Pts',(7.6581759596335,22.1479552334206,0.));
#247928=CARTESIAN_POINT('Ctrl Pts',(7.65711471769406,22.1300198579671,0.));
#247929=CARTESIAN_POINT('Ctrl Pts',(7.65601030346818,22.1122126563327,0.));
#247930=CARTESIAN_POINT('Ctrl Pts',(7.6548633426365,22.094534754469,0.));
#247931=CARTESIAN_POINT('Ctrl Pts',(7.65367447254944,22.0769872951596,0.));
#247932=CARTESIAN_POINT('Ctrl Pts',(7.65244434253103,22.0595714384432,0.));
#247933=CARTESIAN_POINT('Ctrl Pts',(7.65117361421346,22.0422883621176,0.));
#247934=CARTESIAN_POINT('Ctrl Pts',(7.64986296190156,22.025139262321,0.));
#247935=CARTESIAN_POINT('Ctrl Pts',(7.64851307293345,22.0081253540774,0.));
#247936=CARTESIAN_POINT('Ctrl Pts',(7.64712464805257,21.9912478718542,0.));
#247937=CARTESIAN_POINT('Ctrl Pts',(7.64569840177359,21.97450807008,0.));
#247938=CARTESIAN_POINT('Ctrl Pts',(7.64423506279153,21.9579072237653,0.));
#247939=CARTESIAN_POINT('Ctrl Pts',(7.64273537442706,21.9414466292074,0.));
#247940=CARTESIAN_POINT('Ctrl Pts',(7.64120009506539,21.9251276046546,0.));
#247941=CARTESIAN_POINT('Ctrl Pts',(7.63962999860916,21.9089514909873,0.));
#247942=CARTESIAN_POINT('Ctrl Pts',(7.63802587492007,21.8929196523511,0.));
#247943=CARTESIAN_POINT('Ctrl Pts',(7.63638853033367,21.8770334769492,0.));
#247944=CARTESIAN_POINT('Ctrl Pts',(7.63471878821203,21.8612943779086,0.));
#247945=CARTESIAN_POINT('Ctrl Pts',(7.63301748948936,21.8457037941084,0.));
#247946=CARTESIAN_POINT('Ctrl Pts',(7.6312854932304,21.8302631910197,0.));
#247947=CARTESIAN_POINT('Ctrl Pts',(7.62952367718151,21.8149740615093,0.));
#247948=CARTESIAN_POINT('Ctrl Pts',(7.62773293842409,21.7998379268583,0.));
#247949=CARTESIAN_POINT('Ctrl Pts',(7.6259141940452,21.7848563378022,0.));
#247950=CARTESIAN_POINT('Ctrl Pts',(7.62406838181164,21.7700308755584,0.));
#247951=CARTESIAN_POINT('Ctrl Pts',(7.62219646084225,21.7553631528329,0.));
#247952=CARTESIAN_POINT('Ctrl Pts',(7.62029941230854,21.7408548148657,0.));
#247953=CARTESIAN_POINT('Ctrl Pts',(7.61837824030541,21.7265075407977,0.));
#247954=CARTESIAN_POINT('Ctrl Pts',(7.61643397270424,21.7123230449835,0.));
#247955=CARTESIAN_POINT('Ctrl Pts',(7.61446766202786,21.6983030783321,0.));
#247956=CARTESIAN_POINT('Ctrl Pts',(7.61248038630264,21.6844494295813,0.));
#247957=CARTESIAN_POINT('Ctrl Pts',(7.61047325000949,21.6707639267573,0.));
#247958=CARTESIAN_POINT('Ctrl Pts',(7.60844738512871,21.6572484388079,0.));
#247959=CARTESIAN_POINT('Ctrl Pts',(7.60640395216358,21.6439048771743,0.));
#247960=CARTESIAN_POINT('Ctrl Pts',(7.60434414118299,21.6307351973823,0.));
#247961=CARTESIAN_POINT('Ctrl Pts',(7.60226917285431,21.6177414005991,0.));
#247962=CARTESIAN_POINT('Ctrl Pts',(7.60018029988238,21.6049255358843,0.));
#247963=CARTESIAN_POINT('Ctrl Pts',(7.59807880846192,21.5922897024466,0.));
#247964=CARTESIAN_POINT('Ctrl Pts',(7.59596601973588,21.5798360518978,0.));
#247965=CARTESIAN_POINT('Ctrl Pts',(7.59384329124929,21.5675667904728,0.));
#247966=CARTESIAN_POINT('Ctrl Pts',(7.59171201844792,21.5554841813466,0.));
#247967=CARTESIAN_POINT('Ctrl Pts',(7.58957363620026,21.5435905470113,0.));
#247968=CARTESIAN_POINT('Ctrl Pts',(7.58742962034834,21.5318882716736,0.));
#247969=CARTESIAN_POINT('Ctrl Pts',(7.58528148919113,21.5203798035294,0.));
#247970=CARTESIAN_POINT('Ctrl Pts',(7.58313080519158,21.5090676573866,0.));
#247971=CARTESIAN_POINT('Ctrl Pts',(7.58097917790729,21.497954419274,0.));
#247972=CARTESIAN_POINT('Ctrl Pts',(7.57882826679131,21.4870427508193,0.));
#247973=CARTESIAN_POINT('Ctrl Pts',(7.57667978403001,21.4763353936766,0.));
#247974=CARTESIAN_POINT('Ctrl Pts',(7.57453549743434,21.4658351740135,0.));
#247975=CARTESIAN_POINT('Ctrl Pts',(7.57239723223521,21.4555450053147,0.));
#247976=CARTESIAN_POINT('Ctrl Pts',(7.57026687261169,21.445467890751,0.));
#247977=CARTESIAN_POINT('Ctrl Pts',(7.56814636360841,21.435606926151,0.));
#247978=CARTESIAN_POINT('Ctrl Pts',(7.56603771218706,21.4259653015732,0.));
#247979=CARTESIAN_POINT('Ctrl Pts',(7.56394299313682,21.4165463106252,0.));
#247980=CARTESIAN_POINT('Ctrl Pts',(7.56186435703622,21.4073533630364,0.));
#247981=CARTESIAN_POINT('Ctrl Pts',(7.55980403700614,21.3983899952988,0.));
#247982=CARTESIAN_POINT('Ctrl Pts',(7.55776435731421,21.3896598842119,0.));
#247983=CARTESIAN_POINT('Ctrl Pts',(7.55574773403507,21.3811668478933,0.));
#247984=CARTESIAN_POINT('Ctrl Pts',(7.55375667080031,21.3729148390244,0.));
#247985=CARTESIAN_POINT('Ctrl Pts',(7.55179375777441,21.3649079431864,0.));
#247986=CARTESIAN_POINT('Ctrl Pts',(7.54986166521306,21.3571503685853,0.));
#247987=CARTESIAN_POINT('Ctrl Pts',(7.54796316246326,21.349646476153,0.));
#247988=CARTESIAN_POINT('Ctrl Pts',(7.5461011494835,21.3424008295038,0.));
#247989=CARTESIAN_POINT('Ctrl Pts',(7.54427868151268,21.3354182340149,0.));
#247990=CARTESIAN_POINT('Ctrl Pts',(7.54249900377031,21.328703791771,0.));
#247991=CARTESIAN_POINT('Ctrl Pts',(7.54076552038279,21.3222628524165,0.));
#247992=CARTESIAN_POINT('Ctrl Pts',(7.53908175169898,21.3161009456256,0.));
#247993=CARTESIAN_POINT('Ctrl Pts',(7.53745129364619,21.3102237167729,0.));
#247994=CARTESIAN_POINT('Ctrl Pts',(7.53587778251743,21.3046368712157,0.));
#247995=CARTESIAN_POINT('Ctrl Pts',(7.53436505309948,21.2993464250717,0.));
#247996=CARTESIAN_POINT('Ctrl Pts',(7.53291726078526,21.2943588989331,0.));
#247997=CARTESIAN_POINT('Ctrl Pts',(7.53153906987846,21.2896816163843,0.));
#247998=CARTESIAN_POINT('Ctrl Pts',(7.5302356243822,21.2853226580658,0.));
#247999=CARTESIAN_POINT('Ctrl Pts',(7.52901217930407,21.2812902781143,0.));
#248000=CARTESIAN_POINT('Ctrl Pts',(7.52787386225343,21.2775925269652,0.));
#248001=CARTESIAN_POINT('Ctrl Pts',(7.5268252691856,21.2742366113578,0.));
#248002=CARTESIAN_POINT('Ctrl Pts',(7.52587126095544,21.2712301573465,0.));
#248003=CARTESIAN_POINT('Ctrl Pts',(7.52501770333521,21.2685823838672,0.));
#248004=CARTESIAN_POINT('Ctrl Pts',(7.52427261074263,21.266305915706,0.));
#248005=CARTESIAN_POINT('Ctrl Pts',(7.52364573027521,21.2644161259965,0.));
#248006=CARTESIAN_POINT('Ctrl Pts',(7.52314642316202,21.262927782038,0.));
#248007=CARTESIAN_POINT('Ctrl Pts',(7.52278182242727,21.261852128355,0.));
#248008=CARTESIAN_POINT('Ctrl Pts',(7.52260064231736,21.2613260540651,0.));
#248009=CARTESIAN_POINT('Ctrl Pts',(7.52252744144957,21.261120447486,0.));
#248010=CARTESIAN_POINT('Ctrl Pts',(7.52250649703991,21.2610673466883,0.));
#248011=CARTESIAN_POINT('Ctrl Pts',(7.52250298901265,21.2610617890679,0.));
#248012=CARTESIAN_POINT('',(7.36589684767344,24.9347862158358,12.));
#248013=CARTESIAN_POINT('',(7.36589684767344,24.9347862158358,0.));
#248014=CARTESIAN_POINT('Ctrl Pts',(7.52250298901265,21.2610617890679,12.));
#248015=CARTESIAN_POINT('Ctrl Pts',(7.52250649703991,21.2610673466883,12.));
#248016=CARTESIAN_POINT('Ctrl Pts',(7.52252744144957,21.261120447486,12.));
#248017=CARTESIAN_POINT('Ctrl Pts',(7.52260064231736,21.2613260540651,12.));
#248018=CARTESIAN_POINT('Ctrl Pts',(7.52278182242727,21.261852128355,12.));
#248019=CARTESIAN_POINT('Ctrl Pts',(7.52314642316202,21.262927782038,12.));
#248020=CARTESIAN_POINT('Ctrl Pts',(7.52364573027521,21.2644161259965,12.));
#248021=CARTESIAN_POINT('Ctrl Pts',(7.52427261074263,21.266305915706,12.));
#248022=CARTESIAN_POINT('Ctrl Pts',(7.52501770333521,21.2685823838672,12.));
#248023=CARTESIAN_POINT('Ctrl Pts',(7.52587126095544,21.2712301573465,12.));
#248024=CARTESIAN_POINT('Ctrl Pts',(7.5268252691856,21.2742366113578,12.));
#248025=CARTESIAN_POINT('Ctrl Pts',(7.52787386225343,21.2775925269652,12.));
#248026=CARTESIAN_POINT('Ctrl Pts',(7.52901217930407,21.2812902781143,12.));
#248027=CARTESIAN_POINT('Ctrl Pts',(7.5302356243822,21.2853226580658,12.));
#248028=CARTESIAN_POINT('Ctrl Pts',(7.53153906987846,21.2896816163843,12.));
#248029=CARTESIAN_POINT('Ctrl Pts',(7.53291726078526,21.2943588989331,12.));
#248030=CARTESIAN_POINT('Ctrl Pts',(7.53436505309948,21.2993464250717,12.));
#248031=CARTESIAN_POINT('Ctrl Pts',(7.53587778251743,21.3046368712157,12.));
#248032=CARTESIAN_POINT('Ctrl Pts',(7.53745129364619,21.3102237167729,12.));
#248033=CARTESIAN_POINT('Ctrl Pts',(7.53908175169898,21.3161009456256,12.));
#248034=CARTESIAN_POINT('Ctrl Pts',(7.54076552038279,21.3222628524165,12.));
#248035=CARTESIAN_POINT('Ctrl Pts',(7.54249900377031,21.328703791771,12.));
#248036=CARTESIAN_POINT('Ctrl Pts',(7.54427868151268,21.3354182340149,12.));
#248037=CARTESIAN_POINT('Ctrl Pts',(7.5461011494835,21.3424008295038,12.));
#248038=CARTESIAN_POINT('Ctrl Pts',(7.54796316246326,21.349646476153,12.));
#248039=CARTESIAN_POINT('Ctrl Pts',(7.54986166521306,21.3571503685853,12.));
#248040=CARTESIAN_POINT('Ctrl Pts',(7.55179375777441,21.3649079431864,12.));
#248041=CARTESIAN_POINT('Ctrl Pts',(7.55375667080031,21.3729148390244,12.));
#248042=CARTESIAN_POINT('Ctrl Pts',(7.55574773403507,21.3811668478933,12.));
#248043=CARTESIAN_POINT('Ctrl Pts',(7.55776435731421,21.3896598842119,12.));
#248044=CARTESIAN_POINT('Ctrl Pts',(7.55980403700614,21.3983899952988,12.));
#248045=CARTESIAN_POINT('Ctrl Pts',(7.56186435703622,21.4073533630364,12.));
#248046=CARTESIAN_POINT('Ctrl Pts',(7.56394299313682,21.4165463106252,12.));
#248047=CARTESIAN_POINT('Ctrl Pts',(7.56603771218706,21.4259653015732,12.));
#248048=CARTESIAN_POINT('Ctrl Pts',(7.56814636360841,21.435606926151,12.));
#248049=CARTESIAN_POINT('Ctrl Pts',(7.57026687261169,21.445467890751,12.));
#248050=CARTESIAN_POINT('Ctrl Pts',(7.57239723223521,21.4555450053147,12.));
#248051=CARTESIAN_POINT('Ctrl Pts',(7.57453549743434,21.4658351740135,12.));
#248052=CARTESIAN_POINT('Ctrl Pts',(7.57667978403001,21.4763353936766,12.));
#248053=CARTESIAN_POINT('Ctrl Pts',(7.57882826679131,21.4870427508193,12.));
#248054=CARTESIAN_POINT('Ctrl Pts',(7.58097917790729,21.497954419274,12.));
#248055=CARTESIAN_POINT('Ctrl Pts',(7.58313080519158,21.5090676573866,12.));
#248056=CARTESIAN_POINT('Ctrl Pts',(7.58528148919113,21.5203798035294,12.));
#248057=CARTESIAN_POINT('Ctrl Pts',(7.58742962034834,21.5318882716736,12.));
#248058=CARTESIAN_POINT('Ctrl Pts',(7.58957363620026,21.5435905470113,12.));
#248059=CARTESIAN_POINT('Ctrl Pts',(7.59171201844792,21.5554841813466,12.));
#248060=CARTESIAN_POINT('Ctrl Pts',(7.59384329124929,21.5675667904728,12.));
#248061=CARTESIAN_POINT('Ctrl Pts',(7.59596601973588,21.5798360518978,12.));
#248062=CARTESIAN_POINT('Ctrl Pts',(7.59807880846192,21.5922897024466,12.));
#248063=CARTESIAN_POINT('Ctrl Pts',(7.60018029988238,21.6049255358843,12.));
#248064=CARTESIAN_POINT('Ctrl Pts',(7.60226917285431,21.6177414005991,12.));
#248065=CARTESIAN_POINT('Ctrl Pts',(7.60434414118299,21.6307351973823,12.));
#248066=CARTESIAN_POINT('Ctrl Pts',(7.60640395216358,21.6439048771743,12.));
#248067=CARTESIAN_POINT('Ctrl Pts',(7.60844738512871,21.6572484388079,12.));
#248068=CARTESIAN_POINT('Ctrl Pts',(7.61047325000949,21.6707639267573,12.));
#248069=CARTESIAN_POINT('Ctrl Pts',(7.61248038630264,21.6844494295813,12.));
#248070=CARTESIAN_POINT('Ctrl Pts',(7.61446766202786,21.6983030783321,12.));
#248071=CARTESIAN_POINT('Ctrl Pts',(7.61643397270424,21.7123230449835,12.));
#248072=CARTESIAN_POINT('Ctrl Pts',(7.61837824030541,21.7265075407977,12.));
#248073=CARTESIAN_POINT('Ctrl Pts',(7.62029941230854,21.7408548148657,12.));
#248074=CARTESIAN_POINT('Ctrl Pts',(7.62219646084225,21.7553631528329,12.));
#248075=CARTESIAN_POINT('Ctrl Pts',(7.62406838181164,21.7700308755584,12.));
#248076=CARTESIAN_POINT('Ctrl Pts',(7.6259141940452,21.7848563378022,12.));
#248077=CARTESIAN_POINT('Ctrl Pts',(7.62773293842409,21.7998379268583,12.));
#248078=CARTESIAN_POINT('Ctrl Pts',(7.62952367718151,21.8149740615093,12.));
#248079=CARTESIAN_POINT('Ctrl Pts',(7.6312854932304,21.8302631910197,12.));
#248080=CARTESIAN_POINT('Ctrl Pts',(7.63301748948936,21.8457037941084,12.));
#248081=CARTESIAN_POINT('Ctrl Pts',(7.63471878821203,21.8612943779086,12.));
#248082=CARTESIAN_POINT('Ctrl Pts',(7.63638853033367,21.8770334769492,12.));
#248083=CARTESIAN_POINT('Ctrl Pts',(7.63802587492007,21.8929196523511,12.));
#248084=CARTESIAN_POINT('Ctrl Pts',(7.63962999860916,21.9089514909873,12.));
#248085=CARTESIAN_POINT('Ctrl Pts',(7.64120009506539,21.9251276046546,12.));
#248086=CARTESIAN_POINT('Ctrl Pts',(7.64273537442706,21.9414466292074,12.));
#248087=CARTESIAN_POINT('Ctrl Pts',(7.64423506279153,21.9579072237653,12.));
#248088=CARTESIAN_POINT('Ctrl Pts',(7.64569840177359,21.97450807008,12.));
#248089=CARTESIAN_POINT('Ctrl Pts',(7.64712464805257,21.9912478718542,12.));
#248090=CARTESIAN_POINT('Ctrl Pts',(7.64851307293345,22.0081253540774,12.));
#248091=CARTESIAN_POINT('Ctrl Pts',(7.64986296190156,22.025139262321,12.));
#248092=CARTESIAN_POINT('Ctrl Pts',(7.65117361421346,22.0422883621176,12.));
#248093=CARTESIAN_POINT('Ctrl Pts',(7.65244434253103,22.0595714384432,12.));
#248094=CARTESIAN_POINT('Ctrl Pts',(7.65367447254944,22.0769872951596,12.));
#248095=CARTESIAN_POINT('Ctrl Pts',(7.6548633426365,22.094534754469,12.));
#248096=CARTESIAN_POINT('Ctrl Pts',(7.65601030346818,22.1122126563327,12.));
#248097=CARTESIAN_POINT('Ctrl Pts',(7.65711471769406,22.1300198579671,12.));
#248098=CARTESIAN_POINT('Ctrl Pts',(7.6581759596335,22.1479552334206,12.));
#248099=CARTESIAN_POINT('Ctrl Pts',(7.65919341496925,22.1660176731174,12.));
#248100=CARTESIAN_POINT('Ctrl Pts',(7.66016648045007,22.1842060834093,12.));
#248101=CARTESIAN_POINT('Ctrl Pts',(7.66109456359292,22.2025193860972,12.));
#248102=CARTESIAN_POINT('Ctrl Pts',(7.66197708240435,22.2209565180098,12.));
#248103=CARTESIAN_POINT('Ctrl Pts',(7.66281346512545,22.239516430656,12.));
#248104=CARTESIAN_POINT('Ctrl Pts',(7.66360314997661,22.2581980898487,12.));
#248105=CARTESIAN_POINT('Ctrl Pts',(7.66434558490972,22.2770004753332,12.));
#248106=CARTESIAN_POINT('Ctrl Pts',(7.66504022736262,22.2959225803925,12.));
#248107=CARTESIAN_POINT('Ctrl Pts',(7.66568654402441,22.3149634114823,12.));
#248108=CARTESIAN_POINT('Ctrl Pts',(7.66628401061905,22.3341219879454,12.));
#248109=CARTESIAN_POINT('Ctrl Pts',(7.66683211169133,22.3533973417013,12.));
#248110=CARTESIAN_POINT('Ctrl Pts',(7.66733034039887,22.3727885169361,12.));
#248111=CARTESIAN_POINT('Ctrl Pts',(7.66777819830819,22.3922945697782,12.));
#248112=CARTESIAN_POINT('Ctrl Pts',(7.66817519519681,22.411914567977,12.));
#248113=CARTESIAN_POINT('Ctrl Pts',(7.66852084886745,22.4316475906616,12.));
#248114=CARTESIAN_POINT('Ctrl Pts',(7.66881468496659,22.4514927280863,12.));
#248115=CARTESIAN_POINT('Ctrl Pts',(7.66905623680835,22.47144908137,12.));
#248116=CARTESIAN_POINT('Ctrl Pts',(7.66924504520301,22.4915157622308,12.));
#248117=CARTESIAN_POINT('Ctrl Pts',(7.66938065829082,22.5116918927023,12.));
#248118=CARTESIAN_POINT('Ctrl Pts',(7.66946263138115,22.5319766049191,12.));
#248119=CARTESIAN_POINT('Ctrl Pts',(7.66949052679671,22.5523690409109,12.));
#248120=CARTESIAN_POINT('Ctrl Pts',(7.66946391372299,22.5728683523829,12.));
#248121=CARTESIAN_POINT('Ctrl Pts',(7.6693823680624,22.5934737004955,12.));
#248122=CARTESIAN_POINT('Ctrl Pts',(7.66924547229434,22.6141842556248,12.));
#248123=CARTESIAN_POINT('Ctrl Pts',(7.66905281533744,22.6349991971548,12.));
#248124=CARTESIAN_POINT('Ctrl Pts',(7.66880399241353,22.6559177133133,12.));
#248125=CARTESIAN_POINT('Ctrl Pts',(7.66849860491762,22.6769390009889,12.));
#248126=CARTESIAN_POINT('Ctrl Pts',(7.66813626029276,22.6980622655446,12.));
#248127=CARTESIAN_POINT('Ctrl Pts',(7.6677165719101,22.7192867206242,12.));
#248128=CARTESIAN_POINT('Ctrl Pts',(7.66723915895412,22.7406115879508,12.));
#248129=CARTESIAN_POINT('Ctrl Pts',(7.66670364630273,22.7620360971839,12.));
#248130=CARTESIAN_POINT('Ctrl Pts',(7.66610966441259,22.7835594857697,12.));
#248131=CARTESIAN_POINT('Ctrl Pts',(7.66545684920987,22.8051809987834,12.));
#248132=CARTESIAN_POINT('Ctrl Pts',(7.66474484198552,22.8268998887679,12.));
#248133=CARTESIAN_POINT('Ctrl Pts',(7.66397328929805,22.8487154155569,12.));
#248134=CARTESIAN_POINT('Ctrl Pts',(7.66314184287333,22.870626846128,12.));
#248135=CARTESIAN_POINT('Ctrl Pts',(7.66225015950147,22.8926334544879,12.));
#248136=CARTESIAN_POINT('Ctrl Pts',(7.66129790094099,22.9147345215418,12.));
#248137=CARTESIAN_POINT('Ctrl Pts',(7.66028473382776,22.9369293349592,12.));
#248138=CARTESIAN_POINT('Ctrl Pts',(7.65921032958911,22.9592171890332,12.));
#248139=CARTESIAN_POINT('Ctrl Pts',(7.65807436436452,22.9815973845301,12.));
#248140=CARTESIAN_POINT('Ctrl Pts',(7.6568765189133,23.004069228582,12.));
#248141=CARTESIAN_POINT('Ctrl Pts',(7.65561647852554,23.0266320345792,12.));
#248142=CARTESIAN_POINT('Ctrl Pts',(7.65429393293955,23.049285122053,12.));
#248143=CARTESIAN_POINT('Ctrl Pts',(7.65290857626356,23.072027816555,12.));
#248144=CARTESIAN_POINT('Ctrl Pts',(7.65146010690464,23.0948594495246,12.));
#248145=CARTESIAN_POINT('Ctrl Pts',(7.64994822749844,23.1177793581674,12.));
#248146=CARTESIAN_POINT('Ctrl Pts',(7.64837264482929,23.1407868853815,12.));
#248147=CARTESIAN_POINT('Ctrl Pts',(7.64673306975796,23.1638813796691,12.));
#248148=CARTESIAN_POINT('Ctrl Pts',(7.64502921715482,23.1870621950452,12.));
#248149=CARTESIAN_POINT('Ctrl Pts',(7.64326080583683,23.2103286909399,12.));
#248150=CARTESIAN_POINT('Ctrl Pts',(7.64142755851507,23.2336802320912,12.));
#248151=CARTESIAN_POINT('Ctrl Pts',(7.63952920172837,23.2571161884487,12.));
#248152=CARTESIAN_POINT('Ctrl Pts',(7.63756546576374,23.2806359350853,12.));
#248153=CARTESIAN_POINT('Ctrl Pts',(7.63553608458783,23.3042388521021,12.));
#248154=CARTESIAN_POINT('Ctrl Pts',(7.63344079578162,23.3279243245241,12.));
#248155=CARTESIAN_POINT('Ctrl Pts',(7.63127934048138,23.3516917421973,12.));
#248156=CARTESIAN_POINT('Ctrl Pts',(7.62905146332597,23.3755404996638,12.));
#248157=CARTESIAN_POINT('Ctrl Pts',(7.62675691240334,23.3994699961122,12.));
#248158=CARTESIAN_POINT('Ctrl Pts',(7.62439543920053,23.4234796353544,12.));
#248159=CARTESIAN_POINT('Ctrl Pts',(7.62196679855957,23.4475688257855,12.));
#248160=CARTESIAN_POINT('Ctrl Pts',(7.61947074863977,23.4717369803438,12.));
#248161=CARTESIAN_POINT('Ctrl Pts',(7.61690705088318,23.4959835164608,12.));
#248162=CARTESIAN_POINT('Ctrl Pts',(7.61427546999298,23.5203078560128,12.));
#248163=CARTESIAN_POINT('Ctrl Pts',(7.61157577385371,23.5447094252029,12.));
#248164=CARTESIAN_POINT('Ctrl Pts',(7.60880773344599,23.5691876544243,12.));
#248165=CARTESIAN_POINT('Ctrl Pts',(7.60597112277094,23.5937419781244,12.));
#248166=CARTESIAN_POINT('Ctrl Pts',(7.60306571877806,23.6183718346576,12.));
#248167=CARTESIAN_POINT('Ctrl Pts',(7.60009130130129,23.6430766661419,12.));
#248168=CARTESIAN_POINT('Ctrl Pts',(7.59704765299572,23.6678559182876,12.));
#248169=CARTESIAN_POINT('Ctrl Pts',(7.59393455934041,23.6927090405067,12.));
#248170=CARTESIAN_POINT('Ctrl Pts',(7.59075180865326,23.7176354860457,12.));
#248171=CARTESIAN_POINT('Ctrl Pts',(7.58749919210831,23.7426347121006,12.));
#248172=CARTESIAN_POINT('Ctrl Pts',(7.58417650376271,23.7677061799376,12.));
#248173=CARTESIAN_POINT('Ctrl Pts',(7.58078354058211,23.7928493549908,12.));
#248174=CARTESIAN_POINT('Ctrl Pts',(7.57732010249065,23.8180637069977,12.));
#248175=CARTESIAN_POINT('Ctrl Pts',(7.57378599219816,23.8433487096134,12.));
#248176=CARTESIAN_POINT('Ctrl Pts',(7.5701810150071,23.8687038399598,12.));
#248177=CARTESIAN_POINT('Ctrl Pts',(7.56650497863791,23.8941285782003,12.));
#248178=CARTESIAN_POINT('Ctrl Pts',(7.56275769304773,23.9196224070759,12.));
#248179=CARTESIAN_POINT('Ctrl Pts',(7.55893897027682,23.9451848115,12.));
#248180=CARTESIAN_POINT('Ctrl Pts',(7.55504862424811,23.9708152779884,12.));
#248181=CARTESIAN_POINT('Ctrl Pts',(7.5510864709744,23.9965132953185,12.));
#248182=CARTESIAN_POINT('Ctrl Pts',(7.5470523288591,24.022278355453,12.));
#248183=CARTESIAN_POINT('Ctrl Pts',(7.54294601896144,24.0481099543353,12.));
#248184=CARTESIAN_POINT('Ctrl Pts',(7.53876736531013,24.0740075927985,12.));
#248185=CARTESIAN_POINT('Ctrl Pts',(7.53451619514649,24.0999707772642,12.));
#248186=CARTESIAN_POINT('Ctrl Pts',(7.53019233935501,24.1259990209207,12.));
#248187=CARTESIAN_POINT('Ctrl Pts',(7.52579563201423,24.1520918425364,12.));
#248188=CARTESIAN_POINT('Ctrl Pts',(7.52132590953801,24.1782487641594,12.));
#248189=CARTESIAN_POINT('Ctrl Pts',(7.51678300997949,24.2044693092349,12.));
#248190=CARTESIAN_POINT('Ctrl Pts',(7.5121667722218,24.2307530003887,12.));
#248191=CARTESIAN_POINT('Ctrl Pts',(7.50747703535133,24.2570993577034,12.));
#248192=CARTESIAN_POINT('Ctrl Pts',(7.50271363765151,24.2835078958973,12.));
#248193=CARTESIAN_POINT('Ctrl Pts',(7.49787641695438,24.3099781253355,12.));
#248194=CARTESIAN_POINT('Ctrl Pts',(7.4929652125242,24.3365095573685,12.));
#248195=CARTESIAN_POINT('Ctrl Pts',(7.48797986651908,24.3631017084524,12.));
#248196=CARTESIAN_POINT('Ctrl Pts',(7.482920225693,24.3897541049254,12.));
#248197=CARTESIAN_POINT('Ctrl Pts',(7.47778614286564,24.4164662871163,12.));
#248198=CARTESIAN_POINT('Ctrl Pts',(7.47257747883246,24.443237814649,12.));
#248199=CARTESIAN_POINT('Ctrl Pts',(7.46729410308786,24.4700682684524,12.));
#248200=CARTESIAN_POINT('Ctrl Pts',(7.46193588961463,24.4969572391483,12.));
#248201=CARTESIAN_POINT('Ctrl Pts',(7.45650271335861,24.5239043173072,12.));
#248202=CARTESIAN_POINT('Ctrl Pts',(7.4509944465116,24.5509090831559,12.));
#248203=CARTESIAN_POINT('Ctrl Pts',(7.44541095473134,24.577971096086,12.));
#248204=CARTESIAN_POINT('Ctrl Pts',(7.43975209375503,24.6050898852368,12.));
#248205=CARTESIAN_POINT('Ctrl Pts',(7.43401770489523,24.6322649369517,12.));
#248206=CARTESIAN_POINT('Ctrl Pts',(7.42820762159125,24.6594957128756,12.));
#248207=CARTESIAN_POINT('Ctrl Pts',(7.42232167766265,24.6867816727192,12.));
#248208=CARTESIAN_POINT('Ctrl Pts',(7.41635971481674,24.7141222950051,12.));
#248209=CARTESIAN_POINT('Ctrl Pts',(7.41032159082381,24.7415170994784,12.));
#248210=CARTESIAN_POINT('Ctrl Pts',(7.40420718661602,24.7689656668983,12.));
#248211=CARTESIAN_POINT('Ctrl Pts',(7.39801641583012,24.7964676646431,12.));
#248212=CARTESIAN_POINT('Ctrl Pts',(7.39174922585808,24.8240228520893,12.));
#248213=CARTESIAN_POINT('Ctrl Pts',(7.3854055890362,24.8516310625176,12.));
#248214=CARTESIAN_POINT('Ctrl Pts',(7.37898549640269,24.8792921911115,12.));
#248215=CARTESIAN_POINT('Ctrl Pts',(7.37378825961676,24.901463382605,12.));
#248216=CARTESIAN_POINT('Ctrl Pts',(7.3698559312009,24.9181155530543,12.));
#248217=CARTESIAN_POINT('Ctrl Pts',(7.36721909028842,24.9292275670674,12.));
#248218=CARTESIAN_POINT('Ctrl Pts',(7.36589684767344,24.9347862158358,12.));
#248219=CARTESIAN_POINT('Ctrl Pts',(9.71462809124917,20.353053841303,0.));
#248220=CARTESIAN_POINT('Ctrl Pts',(9.71462809124917,20.353053841303,12.));
#248221=CARTESIAN_POINT('Ctrl Pts',(9.71462954053074,20.353060251684,0.));
#248222=CARTESIAN_POINT('Ctrl Pts',(9.71462954053074,20.353060251684,12.));
#248223=CARTESIAN_POINT('Ctrl Pts',(9.71465227853122,20.3531126095522,0.));
#248224=CARTESIAN_POINT('Ctrl Pts',(9.71465227853122,20.3531126095522,12.));
#248225=CARTESIAN_POINT('Ctrl Pts',(9.71474590350791,20.3533097561886,0.));
#248226=CARTESIAN_POINT('Ctrl Pts',(9.71474590350791,20.3533097561886,12.));
#248227=CARTESIAN_POINT('Ctrl Pts',(9.714989780521,20.3538098605706,0.));
#248228=CARTESIAN_POINT('Ctrl Pts',(9.714989780521,20.3538098605706,12.));
#248229=CARTESIAN_POINT('Ctrl Pts',(9.71549257088174,20.3548282742361,0.));
#248230=CARTESIAN_POINT('Ctrl Pts',(9.71549257088174,20.3548282742361,12.));
#248231=CARTESIAN_POINT('Ctrl Pts',(9.71619192554146,20.3562337557875,0.));
#248232=CARTESIAN_POINT('Ctrl Pts',(9.71619192554146,20.3562337557875,12.));
#248233=CARTESIAN_POINT('Ctrl Pts',(9.71708493723061,20.3580133103357,0.));
#248234=CARTESIAN_POINT('Ctrl Pts',(9.71708493723061,20.3580133103357,12.));
#248235=CARTESIAN_POINT('Ctrl Pts',(9.71816778327998,20.3601498764344,0.));
#248236=CARTESIAN_POINT('Ctrl Pts',(9.71816778327998,20.3601498764344,12.));
#248237=CARTESIAN_POINT('Ctrl Pts',(9.71943648548114,20.362625691398,0.));
#248238=CARTESIAN_POINT('Ctrl Pts',(9.71943648548114,20.362625691398,12.));
#248239=CARTESIAN_POINT('Ctrl Pts',(9.72088778381101,20.3654261611055,0.));
#248240=CARTESIAN_POINT('Ctrl Pts',(9.72088778381101,20.3654261611055,12.));
#248241=CARTESIAN_POINT('Ctrl Pts',(9.72251930722503,20.3685406190576,0.));
#248242=CARTESIAN_POINT('Ctrl Pts',(9.72251930722503,20.3685406190576,12.));
#248243=CARTESIAN_POINT('Ctrl Pts',(9.72432910043192,20.371960235676,0.));
#248244=CARTESIAN_POINT('Ctrl Pts',(9.72432910043192,20.371960235676,12.));
#248245=CARTESIAN_POINT('Ctrl Pts',(9.7263153173287,20.3756766651952,0.));
#248246=CARTESIAN_POINT('Ctrl Pts',(9.7263153173287,20.3756766651952,12.));
#248247=CARTESIAN_POINT('Ctrl Pts',(9.72847589116532,20.3796805893304,0.));
#248248=CARTESIAN_POINT('Ctrl Pts',(9.72847589116532,20.3796805893304,12.));
#248249=CARTESIAN_POINT('Ctrl Pts',(9.73080870123726,20.3839624556742,0.));
#248250=CARTESIAN_POINT('Ctrl Pts',(9.73080870123726,20.3839624556742,12.));
#248251=CARTESIAN_POINT('Ctrl Pts',(9.73331167102812,20.3885129129912,0.));
#248252=CARTESIAN_POINT('Ctrl Pts',(9.73331167102812,20.3885129129912,12.));
#248253=CARTESIAN_POINT('Ctrl Pts',(9.73598292014249,20.3933234845646,0.));
#248254=CARTESIAN_POINT('Ctrl Pts',(9.73598292014249,20.3933234845646,12.));
#248255=CARTESIAN_POINT('Ctrl Pts',(9.73882077613206,20.3983866213331,0.));
#248256=CARTESIAN_POINT('Ctrl Pts',(9.73882077613206,20.3983866213331,12.));
#248257=CARTESIAN_POINT('Ctrl Pts',(9.74182369656272,20.4036953576549,0.));
#248258=CARTESIAN_POINT('Ctrl Pts',(9.74182369656272,20.4036953576549,12.));
#248259=CARTESIAN_POINT('Ctrl Pts',(9.74499021838536,20.4092430879861,0.));
#248260=CARTESIAN_POINT('Ctrl Pts',(9.74499021838536,20.4092430879861,12.));
#248261=CARTESIAN_POINT('Ctrl Pts',(9.74831889242174,20.4150232777393,0.));
#248262=CARTESIAN_POINT('Ctrl Pts',(9.74831889242174,20.4150232777393,12.));
#248263=CARTESIAN_POINT('Ctrl Pts',(9.75180829786433,20.4210295275818,0.));
#248264=CARTESIAN_POINT('Ctrl Pts',(9.75180829786433,20.4210295275818,12.));
#248265=CARTESIAN_POINT('Ctrl Pts',(9.75545705902416,20.4272556476629,0.));
#248266=CARTESIAN_POINT('Ctrl Pts',(9.75545705902416,20.4272556476629,12.));
#248267=CARTESIAN_POINT('Ctrl Pts',(9.75926386289929,20.4336957355474,0.));
#248268=CARTESIAN_POINT('Ctrl Pts',(9.75926386289929,20.4336957355474,12.));
#248269=CARTESIAN_POINT('Ctrl Pts',(9.76322747195502,20.4403442329401,0.));
#248270=CARTESIAN_POINT('Ctrl Pts',(9.76322747195502,20.4403442329401,12.));
#248271=CARTESIAN_POINT('Ctrl Pts',(9.76734670980896,20.447195862298,0.));
#248272=CARTESIAN_POINT('Ctrl Pts',(9.76734670980896,20.447195862298,12.));
#248273=CARTESIAN_POINT('Ctrl Pts',(9.77162045104069,20.4542455817527,0.));
#248274=CARTESIAN_POINT('Ctrl Pts',(9.77162045104069,20.4542455817527,12.));
#248275=CARTESIAN_POINT('Ctrl Pts',(9.77604760815522,20.4614885274973,0.));
#248276=CARTESIAN_POINT('Ctrl Pts',(9.77604760815522,20.4614885274973,12.));
#248277=CARTESIAN_POINT('Ctrl Pts',(9.78062712373313,20.4689199790668,0.));
#248278=CARTESIAN_POINT('Ctrl Pts',(9.78062712373313,20.4689199790668,12.));
#248279=CARTESIAN_POINT('Ctrl Pts',(9.78535797314162,20.4765353711585,0.));
#248280=CARTESIAN_POINT('Ctrl Pts',(9.78535797314162,20.4765353711585,12.));
#248281=CARTESIAN_POINT('Ctrl Pts',(9.79023916498659,20.4843302955329,0.));
#248282=CARTESIAN_POINT('Ctrl Pts',(9.79023916498659,20.4843302955329,12.));
#248283=CARTESIAN_POINT('Ctrl Pts',(9.79526974288343,20.4923005087945,0.));
#248284=CARTESIAN_POINT('Ctrl Pts',(9.79526974288343,20.4923005087945,12.));
#248285=CARTESIAN_POINT('Ctrl Pts',(9.80044878520967,20.500441931211,0.));
#248286=CARTESIAN_POINT('Ctrl Pts',(9.80044878520967,20.500441931211,12.));
#248287=CARTESIAN_POINT('Ctrl Pts',(9.80577540161102,20.5087506310507,0.));
#248288=CARTESIAN_POINT('Ctrl Pts',(9.80577540161102,20.5087506310507,12.));
#248289=CARTESIAN_POINT('Ctrl Pts',(9.81124873025278,20.5172228122839,0.));
#248290=CARTESIAN_POINT('Ctrl Pts',(9.81124873025278,20.5172228122839,12.));
#248291=CARTESIAN_POINT('Ctrl Pts',(9.81686793455918,20.5258548000625,0.));
#248292=CARTESIAN_POINT('Ctrl Pts',(9.81686793455918,20.5258548000625,12.));
#248293=CARTESIAN_POINT('Ctrl Pts',(9.82263220080327,20.534643029951,0.));
#248294=CARTESIAN_POINT('Ctrl Pts',(9.82263220080327,20.534643029951,12.));
#248295=CARTESIAN_POINT('Ctrl Pts',(9.82854073773857,20.5435840460717,0.));
#248296=CARTESIAN_POINT('Ctrl Pts',(9.82854073773857,20.5435840460717,12.));
#248297=CARTESIAN_POINT('Ctrl Pts',(9.8345927758532,20.5526744976461,0.));
#248298=CARTESIAN_POINT('Ctrl Pts',(9.8345927758532,20.5526744976461,12.));
#248299=CARTESIAN_POINT('Ctrl Pts',(9.84078756677589,20.5619111362406,0.));
#248300=CARTESIAN_POINT('Ctrl Pts',(9.84078756677589,20.5619111362406,12.));
#248301=CARTESIAN_POINT('Ctrl Pts',(9.84712438256308,20.5712908125145,0.));
#248302=CARTESIAN_POINT('Ctrl Pts',(9.84712438256308,20.5712908125145,12.));
#248303=CARTESIAN_POINT('Ctrl Pts',(9.85360251457004,20.580810471002,0.));
#248304=CARTESIAN_POINT('Ctrl Pts',(9.85360251457004,20.580810471002,12.));
#248305=CARTESIAN_POINT('Ctrl Pts',(9.86022127232749,20.5904671449755,0.));
#248306=CARTESIAN_POINT('Ctrl Pts',(9.86022127232749,20.5904671449755,12.));
#248307=CARTESIAN_POINT('Ctrl Pts',(9.86697998242612,20.6002579513696,0.));
#248308=CARTESIAN_POINT('Ctrl Pts',(9.86697998242612,20.6002579513696,12.));
#248309=CARTESIAN_POINT('Ctrl Pts',(9.87387798732943,20.6101800854491,0.));
#248310=CARTESIAN_POINT('Ctrl Pts',(9.87387798732943,20.6101800854491,12.));
#248311=CARTESIAN_POINT('Ctrl Pts',(9.88091464472669,20.6202308177472,0.));
#248312=CARTESIAN_POINT('Ctrl Pts',(9.88091464472669,20.6202308177472,12.));
#248313=CARTESIAN_POINT('Ctrl Pts',(9.88808932697304,20.6304074914086,0.));
#248314=CARTESIAN_POINT('Ctrl Pts',(9.88808932697304,20.6304074914086,12.));
#248315=CARTESIAN_POINT('Ctrl Pts',(9.89540142049123,20.6407075193977,0.));
#248316=CARTESIAN_POINT('Ctrl Pts',(9.89540142049123,20.6407075193977,12.));
#248317=CARTESIAN_POINT('Ctrl Pts',(9.90285032516695,20.6511283817415,0.));
#248318=CARTESIAN_POINT('Ctrl Pts',(9.90285032516695,20.6511283817415,12.));
#248319=CARTESIAN_POINT('Ctrl Pts',(9.91043545377004,20.6616676228315,0.));
#248320=CARTESIAN_POINT('Ctrl Pts',(9.91043545377004,20.6616676228315,12.));
#248321=CARTESIAN_POINT('Ctrl Pts',(9.91815623141284,20.6723228488262,0.));
#248322=CARTESIAN_POINT('Ctrl Pts',(9.91815623141284,20.6723228488262,12.));
#248323=CARTESIAN_POINT('Ctrl Pts',(9.9260120949875,20.6830917250255,0.));
#248324=CARTESIAN_POINT('Ctrl Pts',(9.9260120949875,20.6830917250255,12.));
#248325=CARTESIAN_POINT('Ctrl Pts',(9.93400249259736,20.6939719732485,0.));
#248326=CARTESIAN_POINT('Ctrl Pts',(9.93400249259736,20.6939719732485,12.));
#248327=CARTESIAN_POINT('Ctrl Pts',(9.9421268829825,20.7049613692237,0.));
#248328=CARTESIAN_POINT('Ctrl Pts',(9.9421268829825,20.7049613692237,12.));
#248329=CARTESIAN_POINT('Ctrl Pts',(9.95038473514962,20.7160577407581,0.));
#248330=CARTESIAN_POINT('Ctrl Pts',(9.95038473514962,20.7160577407581,12.));
#248331=CARTESIAN_POINT('Ctrl Pts',(9.95877552798403,20.7272589658752,0.));
#248332=CARTESIAN_POINT('Ctrl Pts',(9.95877552798403,20.7272589658752,12.));
#248333=CARTESIAN_POINT('Ctrl Pts',(9.96729874986198,20.7385629709795,0.));
#248334=CARTESIAN_POINT('Ctrl Pts',(9.96729874986198,20.7385629709795,12.));
#248335=CARTESIAN_POINT('Ctrl Pts',(9.97595389823461,20.7499677289626,0.));
#248336=CARTESIAN_POINT('Ctrl Pts',(9.97595389823461,20.7499677289626,12.));
#248337=CARTESIAN_POINT('Ctrl Pts',(9.98474047926846,20.7614712574989,0.));
#248338=CARTESIAN_POINT('Ctrl Pts',(9.98474047926846,20.7614712574989,12.));
#248339=CARTESIAN_POINT('Ctrl Pts',(9.99365800754637,20.7730716175417,0.));
#248340=CARTESIAN_POINT('Ctrl Pts',(9.99365800754637,20.7730716175417,12.));
#248341=CARTESIAN_POINT('Ctrl Pts',(10.0027060057389,20.7847669117568,0.));
#248342=CARTESIAN_POINT('Ctrl Pts',(10.0027060057389,20.7847669117568,12.));
#248343=CARTESIAN_POINT('Ctrl Pts',(10.0118840042786,20.7965552829907,0.));
#248344=CARTESIAN_POINT('Ctrl Pts',(10.0118840042786,20.7965552829907,12.));
#248345=CARTESIAN_POINT('Ctrl Pts',(10.0211915410095,20.8084349126885,0.));
#248346=CARTESIAN_POINT('Ctrl Pts',(10.0211915410095,20.8084349126885,12.));
#248347=CARTESIAN_POINT('Ctrl Pts',(10.0306281609435,20.8204040196599,0.));
#248348=CARTESIAN_POINT('Ctrl Pts',(10.0306281609435,20.8204040196599,12.));
#248349=CARTESIAN_POINT('Ctrl Pts',(10.0401934160234,20.8324608588906,0.));
#248350=CARTESIAN_POINT('Ctrl Pts',(10.0401934160234,20.8324608588906,12.));
#248351=CARTESIAN_POINT('Ctrl Pts',(10.0498868648733,20.8446037203402,0.));
#248352=CARTESIAN_POINT('Ctrl Pts',(10.0498868648733,20.8446037203402,12.));
#248353=CARTESIAN_POINT('Ctrl Pts',(10.0597080725375,20.856830927732,0.));
#248354=CARTESIAN_POINT('Ctrl Pts',(10.0597080725375,20.856830927732,12.));
#248355=CARTESIAN_POINT('Ctrl Pts',(10.0696566102219,20.8691408373705,0.));
#248356=CARTESIAN_POINT('Ctrl Pts',(10.0696566102219,20.8691408373705,12.));
#248357=CARTESIAN_POINT('Ctrl Pts',(10.0797320551154,20.8815318371844,0.));
#248358=CARTESIAN_POINT('Ctrl Pts',(10.0797320551154,20.8815318371844,12.));
#248359=CARTESIAN_POINT('Ctrl Pts',(10.0899339901916,20.8940023457371,0.));
#248360=CARTESIAN_POINT('Ctrl Pts',(10.0899339901916,20.8940023457371,12.));
#248361=CARTESIAN_POINT('Ctrl Pts',(10.1002620040076,20.9065508112556,0.));
#248362=CARTESIAN_POINT('Ctrl Pts',(10.1002620040076,20.9065508112556,12.));
#248363=CARTESIAN_POINT('Ctrl Pts',(10.1107156904836,20.9191757106266,0.));
#248364=CARTESIAN_POINT('Ctrl Pts',(10.1107156904836,20.9191757106266,12.));
#248365=CARTESIAN_POINT('Ctrl Pts',(10.1212946487057,20.931875548473,0.));
#248366=CARTESIAN_POINT('Ctrl Pts',(10.1212946487057,20.931875548473,12.));
#248367=CARTESIAN_POINT('Ctrl Pts',(10.1319984827909,20.944648856393,0.));
#248368=CARTESIAN_POINT('Ctrl Pts',(10.1319984827909,20.944648856393,12.));
#248369=CARTESIAN_POINT('Ctrl Pts',(10.1428268017257,20.9574941921591,0.));
#248370=CARTESIAN_POINT('Ctrl Pts',(10.1428268017257,20.9574941921591,12.));
#248371=CARTESIAN_POINT('Ctrl Pts',(10.1537792192065,20.970410138937,0.));
#248372=CARTESIAN_POINT('Ctrl Pts',(10.1537792192065,20.970410138937,12.));
#248373=CARTESIAN_POINT('Ctrl Pts',(10.1648553534567,20.9833953044737,0.));
#248374=CARTESIAN_POINT('Ctrl Pts',(10.1648553534567,20.9833953044737,12.));
#248375=CARTESIAN_POINT('Ctrl Pts',(10.1760548270765,20.9964483203685,0.));
#248376=CARTESIAN_POINT('Ctrl Pts',(10.1760548270765,20.9964483203685,12.));
#248377=CARTESIAN_POINT('Ctrl Pts',(10.1873772669358,21.0095678414486,0.));
#248378=CARTESIAN_POINT('Ctrl Pts',(10.1873772669358,21.0095678414486,12.));
#248379=CARTESIAN_POINT('Ctrl Pts',(10.1988223040425,21.0227525451107,0.));
#248380=CARTESIAN_POINT('Ctrl Pts',(10.1988223040425,21.0227525451107,12.));
#248381=CARTESIAN_POINT('Ctrl Pts',(10.2103895734123,21.0360011306814,0.));
#248382=CARTESIAN_POINT('Ctrl Pts',(10.2103895734123,21.0360011306814,12.));
#248383=CARTESIAN_POINT('Ctrl Pts',(10.2220787139157,21.0493123187484,0.));
#248384=CARTESIAN_POINT('Ctrl Pts',(10.2220787139157,21.0493123187484,12.));
#248385=CARTESIAN_POINT('Ctrl Pts',(10.233889368157,21.0626848505665,0.));
#248386=CARTESIAN_POINT('Ctrl Pts',(10.233889368157,21.0626848505665,12.));
#248387=CARTESIAN_POINT('Ctrl Pts',(10.2458211823915,21.0761174875448,0.));
#248388=CARTESIAN_POINT('Ctrl Pts',(10.2458211823915,21.0761174875448,12.));
#248389=CARTESIAN_POINT('Ctrl Pts',(10.2578738064183,21.0896090107066,0.));
#248390=CARTESIAN_POINT('Ctrl Pts',(10.2578738064183,21.0896090107066,12.));
#248391=CARTESIAN_POINT('Ctrl Pts',(10.2700468934743,21.1031582201625,0.));
#248392=CARTESIAN_POINT('Ctrl Pts',(10.2700468934743,21.1031582201625,12.));
#248393=CARTESIAN_POINT('Ctrl Pts',(10.2823401001067,21.1167639345623,0.));
#248394=CARTESIAN_POINT('Ctrl Pts',(10.2823401001067,21.1167639345623,12.));
#248395=CARTESIAN_POINT('Ctrl Pts',(10.2947530860714,21.130424990599,0.));
#248396=CARTESIAN_POINT('Ctrl Pts',(10.2947530860714,21.130424990599,12.));
#248397=CARTESIAN_POINT('Ctrl Pts',(10.307285514268,21.1441402425831,0.));
#248398=CARTESIAN_POINT('Ctrl Pts',(10.307285514268,21.1441402425831,12.));
#248399=CARTESIAN_POINT('Ctrl Pts',(10.3199370506541,21.1579085619959,0.));
#248400=CARTESIAN_POINT('Ctrl Pts',(10.3199370506541,21.1579085619959,12.));
#248401=CARTESIAN_POINT('Ctrl Pts',(10.3327073641574,21.1717288370512,0.));
#248402=CARTESIAN_POINT('Ctrl Pts',(10.3327073641574,21.1717288370512,12.));
#248403=CARTESIAN_POINT('Ctrl Pts',(10.3455961265706,21.1855999722427,0.));
#248404=CARTESIAN_POINT('Ctrl Pts',(10.3455961265706,21.1855999722427,12.));
#248405=CARTESIAN_POINT('Ctrl Pts',(10.3586030124595,21.1995208879205,0.));
#248406=CARTESIAN_POINT('Ctrl Pts',(10.3586030124595,21.1995208879205,12.));
#248407=CARTESIAN_POINT('Ctrl Pts',(10.3717276991137,21.2134905199359,0.));
#248408=CARTESIAN_POINT('Ctrl Pts',(10.3717276991137,21.2134905199359,12.));
#248409=CARTESIAN_POINT('Ctrl Pts',(10.384969866479,21.2275078192708,0.));
#248410=CARTESIAN_POINT('Ctrl Pts',(10.384969866479,21.2275078192708,12.));
#248411=CARTESIAN_POINT('Ctrl Pts',(10.3983291970846,21.2415717516713,0.));
#248412=CARTESIAN_POINT('Ctrl Pts',(10.3983291970846,21.2415717516713,12.));
#248413=CARTESIAN_POINT('Ctrl Pts',(10.4118053759584,21.2556812972741,0.));
#248414=CARTESIAN_POINT('Ctrl Pts',(10.4118053759584,21.2556812972741,12.));
#248415=CARTESIAN_POINT('Ctrl Pts',(10.4253980905394,21.2698354502391,0.));
#248416=CARTESIAN_POINT('Ctrl Pts',(10.4253980905394,21.2698354502391,12.));
#248417=CARTESIAN_POINT('Ctrl Pts',(10.4391070306385,21.2840332184471,0.));
#248418=CARTESIAN_POINT('Ctrl Pts',(10.4391070306385,21.2840332184471,12.));
#248419=CARTESIAN_POINT('Ctrl Pts',(10.452931888387,21.2982736231924,0.));
#248420=CARTESIAN_POINT('Ctrl Pts',(10.452931888387,21.2982736231924,12.));
#248421=CARTESIAN_POINT('Ctrl Pts',(10.4668723581768,21.312555698873,0.));
#248422=CARTESIAN_POINT('Ctrl Pts',(10.4668723581768,21.312555698873,12.));
#248423=CARTESIAN_POINT('Ctrl Pts',(10.4809281365933,21.3268784926823,0.));
#248424=CARTESIAN_POINT('Ctrl Pts',(10.4809281365933,21.3268784926823,12.));
#248425=CARTESIAN_POINT('Ctrl Pts',(10.4950989223341,21.3412410642912,0.));
#248426=CARTESIAN_POINT('Ctrl Pts',(10.4950989223341,21.3412410642912,12.));
#248427=CARTESIAN_POINT('Ctrl Pts',(10.5093844161689,21.3556424855822,0.));
#248428=CARTESIAN_POINT('Ctrl Pts',(10.5093844161689,21.3556424855822,12.));
#248429=CARTESIAN_POINT('Ctrl Pts',(10.523784320906,21.3700818403942,0.));
#248430=CARTESIAN_POINT('Ctrl Pts',(10.523784320906,21.3700818403942,12.));
#248431=CARTESIAN_POINT('Ctrl Pts',(10.5382983413422,21.3845582242604,0.));
#248432=CARTESIAN_POINT('Ctrl Pts',(10.5382983413422,21.3845582242604,12.));
#248433=CARTESIAN_POINT('Ctrl Pts',(10.5529261842107,21.3990707441495,0.));
#248434=CARTESIAN_POINT('Ctrl Pts',(10.5529261842107,21.3990707441495,12.));
#248435=CARTESIAN_POINT('Ctrl Pts',(10.5676675581106,21.4136185181974,0.));
#248436=CARTESIAN_POINT('Ctrl Pts',(10.5676675581106,21.4136185181974,12.));
#248437=CARTESIAN_POINT('Ctrl Pts',(10.582522173457,21.4282006754624,0.));
#248438=CARTESIAN_POINT('Ctrl Pts',(10.582522173457,21.4282006754624,12.));
#248439=CARTESIAN_POINT('Ctrl Pts',(10.597489742462,21.4428163557137,0.));
#248440=CARTESIAN_POINT('Ctrl Pts',(10.597489742462,21.4428163557137,12.));
#248441=CARTESIAN_POINT('Ctrl Pts',(10.612569979096,21.4574647092093,0.));
#248442=CARTESIAN_POINT('Ctrl Pts',(10.612569979096,21.4574647092093,12.));
#248443=CARTESIAN_POINT('Ctrl Pts',(10.6277625990456,21.4721448964766,0.));
#248444=CARTESIAN_POINT('Ctrl Pts',(10.6277625990456,21.4721448964766,12.));
#248445=CARTESIAN_POINT('Ctrl Pts',(10.6430673196609,21.4868560880893,0.));
#248446=CARTESIAN_POINT('Ctrl Pts',(10.6430673196609,21.4868560880893,12.));
#248447=CARTESIAN_POINT('Ctrl Pts',(10.658483859894,21.5015974644454,0.));
#248448=CARTESIAN_POINT('Ctrl Pts',(10.658483859894,21.5015974644454,12.));
#248449=CARTESIAN_POINT('Ctrl Pts',(10.6740119402835,21.5163682155805,0.));
#248450=CARTESIAN_POINT('Ctrl Pts',(10.6740119402835,21.5163682155805,12.));
#248451=CARTESIAN_POINT('Ctrl Pts',(10.689651282929,21.531167540981,0.));
#248452=CARTESIAN_POINT('Ctrl Pts',(10.689651282929,21.531167540981,12.));
#248453=CARTESIAN_POINT('Ctrl Pts',(10.7054016114571,21.5459946493955,0.));
#248454=CARTESIAN_POINT('Ctrl Pts',(10.7054016114571,21.5459946493955,12.));
#248455=CARTESIAN_POINT('Ctrl Pts',(10.7212626509816,21.5608487586467,0.));
#248456=CARTESIAN_POINT('Ctrl Pts',(10.7212626509816,21.5608487586467,12.));
#248457=CARTESIAN_POINT('Ctrl Pts',(10.7372341280468,21.5757290954372,0.));
#248458=CARTESIAN_POINT('Ctrl Pts',(10.7372341280468,21.5757290954372,12.));
#248459=CARTESIAN_POINT('Ctrl Pts',(10.7533157705943,21.5906348951745,0.));
#248460=CARTESIAN_POINT('Ctrl Pts',(10.7533157705943,21.5906348951745,12.));
#248461=CARTESIAN_POINT('Ctrl Pts',(10.7695073079554,21.6055654018179,0.));
#248462=CARTESIAN_POINT('Ctrl Pts',(10.7695073079554,21.6055654018179,12.));
#248463=CARTESIAN_POINT('Ctrl Pts',(10.7858084708262,21.6205198677176,0.));
#248464=CARTESIAN_POINT('Ctrl Pts',(10.7858084708262,21.6205198677176,12.));
#248465=CARTESIAN_POINT('Ctrl Pts',(10.8022189912369,21.6354975534558,0.));
#248466=CARTESIAN_POINT('Ctrl Pts',(10.8022189912369,21.6354975534558,12.));
#248467=CARTESIAN_POINT('Ctrl Pts',(10.8187386025135,21.6504977276864,0.));
#248468=CARTESIAN_POINT('Ctrl Pts',(10.8187386025135,21.6504977276864,12.));
#248469=CARTESIAN_POINT('Ctrl Pts',(10.835367039227,21.6655196669727,0.));
#248470=CARTESIAN_POINT('Ctrl Pts',(10.835367039227,21.6655196669727,12.));
#248471=CARTESIAN_POINT('Ctrl Pts',(10.8521040371832,21.6805626556461,0.));
#248472=CARTESIAN_POINT('Ctrl Pts',(10.8521040371832,21.6805626556461,12.));
#248473=CARTESIAN_POINT('Ctrl Pts',(10.8689493334093,21.6956259856667,0.));
#248474=CARTESIAN_POINT('Ctrl Pts',(10.8689493334093,21.6956259856667,12.));
#248475=CARTESIAN_POINT('Ctrl Pts',(10.8859026661292,21.7107089564822,0.));
#248476=CARTESIAN_POINT('Ctrl Pts',(10.8859026661292,21.7107089564822,12.));
#248477=CARTESIAN_POINT('Ctrl Pts',(10.9029637747341,21.7258108748874,0.));
#248478=CARTESIAN_POINT('Ctrl Pts',(10.9029637747341,21.7258108748874,12.));
#248479=CARTESIAN_POINT('Ctrl Pts',(10.9201323997386,21.74093105488,0.));
#248480=CARTESIAN_POINT('Ctrl Pts',(10.9201323997386,21.74093105488,12.));
#248481=CARTESIAN_POINT('Ctrl Pts',(10.9374082827446,21.7560688175252,0.));
#248482=CARTESIAN_POINT('Ctrl Pts',(10.9374082827446,21.7560688175252,12.));
#248483=CARTESIAN_POINT('Ctrl Pts',(10.9547911664457,21.7712234908468,0.));
#248484=CARTESIAN_POINT('Ctrl Pts',(10.9547911664457,21.7712234908468,12.));
#248485=CARTESIAN_POINT('Ctrl Pts',(10.9722807946157,21.7863944097143,0.));
#248486=CARTESIAN_POINT('Ctrl Pts',(10.9722807946157,21.7863944097143,12.));
#248487=CARTESIAN_POINT('Ctrl Pts',(10.9898769120913,21.8015809157302,0.));
#248488=CARTESIAN_POINT('Ctrl Pts',(10.9898769120913,21.8015809157302,12.));
#248489=CARTESIAN_POINT('Ctrl Pts',(11.0075792647477,21.8167823571168,0.));
#248490=CARTESIAN_POINT('Ctrl Pts',(11.0075792647477,21.8167823571168,12.));
#248491=CARTESIAN_POINT('Ctrl Pts',(11.0253875994598,21.8319980886033,0.));
#248492=CARTESIAN_POINT('Ctrl Pts',(11.0253875994598,21.8319980886033,12.));
#248493=CARTESIAN_POINT('Ctrl Pts',(11.0433016640808,21.8472274713103,0.));
#248494=CARTESIAN_POINT('Ctrl Pts',(11.0433016640808,21.8472274713103,12.));
#248495=CARTESIAN_POINT('Ctrl Pts',(11.0613212074364,21.8624698726319,0.));
#248496=CARTESIAN_POINT('Ctrl Pts',(11.0613212074364,21.8624698726319,12.));
#248497=CARTESIAN_POINT('Ctrl Pts',(11.0794459793058,21.8777246661191,0.));
#248498=CARTESIAN_POINT('Ctrl Pts',(11.0794459793058,21.8777246661191,12.));
#248499=CARTESIAN_POINT('Ctrl Pts',(11.0976757303944,21.8929912313608,0.));
#248500=CARTESIAN_POINT('Ctrl Pts',(11.0976757303944,21.8929912313608,12.));
#248501=CARTESIAN_POINT('Ctrl Pts',(11.1160102123024,21.9082689538687,0.));
#248502=CARTESIAN_POINT('Ctrl Pts',(11.1160102123024,21.9082689538687,12.));
#248503=CARTESIAN_POINT('Ctrl Pts',(11.134449177474,21.9235572249518,0.));
#248504=CARTESIAN_POINT('Ctrl Pts',(11.134449177474,21.9235572249518,12.));
#248505=CARTESIAN_POINT('Ctrl Pts',(11.1529923792002,21.9388554416437,0.));
#248506=CARTESIAN_POINT('Ctrl Pts',(11.1529923792002,21.9388554416437,12.));
#248507=CARTESIAN_POINT('Ctrl Pts',(11.1716395716375,21.9541630066504,0.));
#248508=CARTESIAN_POINT('Ctrl Pts',(11.1716395716375,21.9541630066504,12.));
#248509=CARTESIAN_POINT('Ctrl Pts',(11.1903905098109,21.9694793282913,0.));
#248510=CARTESIAN_POINT('Ctrl Pts',(11.1903905098109,21.9694793282913,12.));
#248511=CARTESIAN_POINT('Ctrl Pts',(11.2092449496125,21.9848038204439,0.));
#248512=CARTESIAN_POINT('Ctrl Pts',(11.2092449496125,21.9848038204439,12.));
#248513=CARTESIAN_POINT('Ctrl Pts',(11.2282026477897,22.000135902484,0.));
#248514=CARTESIAN_POINT('Ctrl Pts',(11.2282026477897,22.000135902484,12.));
#248515=CARTESIAN_POINT('Ctrl Pts',(11.2472633619276,22.0154749992364,0.));
#248516=CARTESIAN_POINT('Ctrl Pts',(11.2472633619276,22.0154749992364,12.));
#248517=CARTESIAN_POINT('Ctrl Pts',(11.2664268504207,22.0308205408351,0.));
#248518=CARTESIAN_POINT('Ctrl Pts',(11.2664268504207,22.0308205408351,12.));
#248519=CARTESIAN_POINT('Ctrl Pts',(11.2856928724374,22.0461719625661,0.));
#248520=CARTESIAN_POINT('Ctrl Pts',(11.2856928724374,22.0461719625661,12.));
#248521=CARTESIAN_POINT('Ctrl Pts',(11.3050611878771,22.0615287047179,0.));
#248522=CARTESIAN_POINT('Ctrl Pts',(11.3050611878771,22.0615287047179,12.));
#248523=CARTESIAN_POINT('Ctrl Pts',(11.3245315573168,22.0768902124267,0.));
#248524=CARTESIAN_POINT('Ctrl Pts',(11.3245315573168,22.0768902124267,12.));
#248525=CARTESIAN_POINT('Ctrl Pts',(11.3441037419553,22.0922559355293,0.));
#248526=CARTESIAN_POINT('Ctrl Pts',(11.3441037419553,22.0922559355293,12.));
#248527=CARTESIAN_POINT('Ctrl Pts',(11.3637775035367,22.1076253283978,0.));
#248528=CARTESIAN_POINT('Ctrl Pts',(11.3637775035367,22.1076253283978,12.));
#248529=CARTESIAN_POINT('Ctrl Pts',(11.3835526044256,22.1229978500185,0.));
#248530=CARTESIAN_POINT('Ctrl Pts',(11.3835526044256,22.1229978500185,12.));
#248531=CARTESIAN_POINT('Ctrl Pts',(11.4034288076908,22.1383729640963,0.));
#248532=CARTESIAN_POINT('Ctrl Pts',(11.4034288076908,22.1383729640963,12.));
#248533=CARTESIAN_POINT('Ctrl Pts',(11.4234058771742,22.1537501391486,0.));
#248534=CARTESIAN_POINT('Ctrl Pts',(11.4234058771742,22.1537501391486,12.));
#248535=CARTESIAN_POINT('Ctrl Pts',(11.443483577557,22.1691288486096,0.));
#248536=CARTESIAN_POINT('Ctrl Pts',(11.443483577557,22.1691288486096,12.));
#248537=CARTESIAN_POINT('Ctrl Pts',(11.463661674411,22.184508570917,0.));
#248538=CARTESIAN_POINT('Ctrl Pts',(11.463661674411,22.184508570917,12.));
#248539=CARTESIAN_POINT('Ctrl Pts',(11.4839399342589,22.1998887896435,0.));
#248540=CARTESIAN_POINT('Ctrl Pts',(11.4839399342589,22.1998887896435,12.));
#248541=CARTESIAN_POINT('Ctrl Pts',(11.504318124424,22.215268993102,0.));
#248542=CARTESIAN_POINT('Ctrl Pts',(11.504318124424,22.215268993102,12.));
#248543=CARTESIAN_POINT('Ctrl Pts',(11.5247960128476,22.2306486738899,0.));
#248544=CARTESIAN_POINT('Ctrl Pts',(11.5247960128476,22.2306486738899,12.));
#248545=CARTESIAN_POINT('Ctrl Pts',(11.545373367912,22.2460273284653,0.));
#248546=CARTESIAN_POINT('Ctrl Pts',(11.545373367912,22.2460273284653,12.));
#248547=CARTESIAN_POINT('Ctrl Pts',(11.5660499582403,22.2614044566898,0.));
#248548=CARTESIAN_POINT('Ctrl Pts',(11.5660499582403,22.2614044566898,12.));
#248549=CARTESIAN_POINT('Ctrl Pts',(11.5868255525189,22.2767795614349,0.));
#248550=CARTESIAN_POINT('Ctrl Pts',(11.5868255525189,22.2767795614349,12.));
#248551=CARTESIAN_POINT('Ctrl Pts',(11.6076999192359,22.2921521480358,0.));
#248552=CARTESIAN_POINT('Ctrl Pts',(11.6076999192359,22.2921521480358,12.));
#248553=CARTESIAN_POINT('Ctrl Pts',(11.6286728270011,22.3075217249049,0.));
#248554=CARTESIAN_POINT('Ctrl Pts',(11.6286728270011,22.3075217249049,12.));
#248555=CARTESIAN_POINT('Ctrl Pts',(11.6497440449858,22.3228878043976,0.));
#248556=CARTESIAN_POINT('Ctrl Pts',(11.6497440449858,22.3228878043976,12.));
#248557=CARTESIAN_POINT('Ctrl Pts',(11.6709133432986,22.3382499035618,0.));
#248558=CARTESIAN_POINT('Ctrl Pts',(11.6709133432986,22.3382499035618,12.));
#248559=CARTESIAN_POINT('Ctrl Pts',(11.6921804934056,22.3536075450028,0.));
#248560=CARTESIAN_POINT('Ctrl Pts',(11.6921804934056,22.3536075450028,12.));
#248561=CARTESIAN_POINT('Ctrl Pts',(11.7135452684532,22.3689602575492,0.));
#248562=CARTESIAN_POINT('Ctrl Pts',(11.7135452684532,22.3689602575492,12.));
#248563=CARTESIAN_POINT('Ctrl Pts',(11.7350074437961,22.3843075773905,0.));
#248564=CARTESIAN_POINT('Ctrl Pts',(11.7350074437961,22.3843075773905,12.));
#248565=CARTESIAN_POINT('Ctrl Pts',(11.7565667964765,22.39964904692,0.));
#248566=CARTESIAN_POINT('Ctrl Pts',(11.7565667964765,22.39964904692,12.));
#248567=CARTESIAN_POINT('Ctrl Pts',(11.7782231042041,22.4149842125018,0.));
#248568=CARTESIAN_POINT('Ctrl Pts',(11.7782231042041,22.4149842125018,12.));
#248569=CARTESIAN_POINT('Ctrl Pts',(11.7999761445175,22.4303126226468,0.));
#248570=CARTESIAN_POINT('Ctrl Pts',(11.7999761445175,22.4303126226468,12.));
#248571=CARTESIAN_POINT('Ctrl Pts',(11.8218256937889,22.4456338258738,0.));
#248572=CARTESIAN_POINT('Ctrl Pts',(11.8218256937889,22.4456338258738,12.));
#248573=CARTESIAN_POINT('Ctrl Pts',(11.8437715264487,22.4609473690469,0.));
#248574=CARTESIAN_POINT('Ctrl Pts',(11.8437715264487,22.4609473690469,12.));
#248575=CARTESIAN_POINT('Ctrl Pts',(11.8658134137018,22.4762527946694,0.));
#248576=CARTESIAN_POINT('Ctrl Pts',(11.8658134137018,22.4762527946694,12.));
#248577=CARTESIAN_POINT('Ctrl Pts',(11.8879511239941,22.4915496418472,0.));
#248578=CARTESIAN_POINT('Ctrl Pts',(11.8879511239941,22.4915496418472,12.));
#248579=CARTESIAN_POINT('Ctrl Pts',(11.9101844254555,22.5068374513958,0.));
#248580=CARTESIAN_POINT('Ctrl Pts',(11.9101844254555,22.5068374513958,12.));
#248581=CARTESIAN_POINT('Ctrl Pts',(11.9325130877801,22.5221157697869,0.));
#248582=CARTESIAN_POINT('Ctrl Pts',(11.9325130877801,22.5221157697869,12.));
#248583=CARTESIAN_POINT('Ctrl Pts',(11.9549368843996,22.5373841537299,0.));
#248584=CARTESIAN_POINT('Ctrl Pts',(11.9549368843996,22.5373841537299,12.));
#248585=CARTESIAN_POINT('Ctrl Pts',(11.9774555943496,22.5526421741159,0.));
#248586=CARTESIAN_POINT('Ctrl Pts',(11.9774555943496,22.5526421741159,12.));
#248587=CARTESIAN_POINT('Ctrl Pts',(12.0000690046697,22.5678894211194,0.));
#248588=CARTESIAN_POINT('Ctrl Pts',(12.0000690046697,22.5678894211194,12.));
#248589=CARTESIAN_POINT('Ctrl Pts',(12.0227769113132,22.5831255061306,0.));
#248590=CARTESIAN_POINT('Ctrl Pts',(12.0227769113132,22.5831255061306,12.));
#248591=CARTESIAN_POINT('Ctrl Pts',(12.0455791139135,22.5983500505675,0.));
#248592=CARTESIAN_POINT('Ctrl Pts',(12.0455791139135,22.5983500505675,12.));
#248593=CARTESIAN_POINT('Ctrl Pts',(12.0684754113869,22.613562676493,0.));
#248594=CARTESIAN_POINT('Ctrl Pts',(12.0684754113869,22.613562676493,12.));
#248595=CARTESIAN_POINT('Ctrl Pts',(12.0914655972828,22.628762996708,0.));
#248596=CARTESIAN_POINT('Ctrl Pts',(12.0914655972828,22.628762996708,12.));
#248597=CARTESIAN_POINT('Ctrl Pts',(12.1145494550384,22.6439506046611,0.));
#248598=CARTESIAN_POINT('Ctrl Pts',(12.1145494550384,22.6439506046611,12.));
#248599=CARTESIAN_POINT('Ctrl Pts',(12.1377267537141,22.6591250653942,0.));
#248600=CARTESIAN_POINT('Ctrl Pts',(12.1377267537141,22.6591250653942,12.));
#248601=CARTESIAN_POINT('Ctrl Pts',(12.1609972423088,22.6742859034891,0.));
#248602=CARTESIAN_POINT('Ctrl Pts',(12.1609972423088,22.6742859034891,12.));
#248603=CARTESIAN_POINT('Ctrl Pts',(12.1843606579246,22.6894326204959,0.));
#248604=CARTESIAN_POINT('Ctrl Pts',(12.1843606579246,22.6894326204959,12.));
#248605=CARTESIAN_POINT('Ctrl Pts',(12.2078167360267,22.7045647168659,0.));
#248606=CARTESIAN_POINT('Ctrl Pts',(12.2078167360267,22.7045647168659,12.));
#248607=CARTESIAN_POINT('Ctrl Pts',(12.2313652198047,22.7196817119299,0.));
#248608=CARTESIAN_POINT('Ctrl Pts',(12.2313652198047,22.7196817119299,12.));
#248609=CARTESIAN_POINT('Ctrl Pts',(12.2550058702389,22.7347831655251,0.));
#248610=CARTESIAN_POINT('Ctrl Pts',(12.2550058702389,22.7347831655251,12.));
#248611=CARTESIAN_POINT('Ctrl Pts',(12.2787384750747,22.7498686970096,0.));
#248612=CARTESIAN_POINT('Ctrl Pts',(12.2787384750747,22.7498686970096,12.));
#248613=CARTESIAN_POINT('Ctrl Pts',(12.3025628601811,22.7649380101154,0.));
#248614=CARTESIAN_POINT('Ctrl Pts',(12.3025628601811,22.7649380101154,12.));
#248615=CARTESIAN_POINT('Ctrl Pts',(12.3264788926108,22.7799908974947,0.));
#248616=CARTESIAN_POINT('Ctrl Pts',(12.3264788926108,22.7799908974947,12.));
#248617=CARTESIAN_POINT('Ctrl Pts',(12.3504864740361,22.7950272216959,0.));
#248618=CARTESIAN_POINT('Ctrl Pts',(12.3504864740361,22.7950272216959,12.));
#248619=CARTESIAN_POINT('Ctrl Pts',(12.3745855366772,22.8100469022632,0.));
#248620=CARTESIAN_POINT('Ctrl Pts',(12.3745855366772,22.8100469022632,12.));
#248621=CARTESIAN_POINT('Ctrl Pts',(12.393937937903,22.8220493007353,0.));
#248622=CARTESIAN_POINT('Ctrl Pts',(12.393937937903,22.8220493007353,12.));
#248623=CARTESIAN_POINT('Ctrl Pts',(12.4084933766366,22.8310435872852,0.));
#248624=CARTESIAN_POINT('Ctrl Pts',(12.4084933766366,22.8310435872852,12.));
#248625=CARTESIAN_POINT('Ctrl Pts',(12.4182152851867,22.8370364396497,0.));
#248626=CARTESIAN_POINT('Ctrl Pts',(12.4182152851867,22.8370364396497,12.));
#248627=CARTESIAN_POINT('Ctrl Pts',(12.4230808101438,22.8400320311648,0.));
#248628=CARTESIAN_POINT('Ctrl Pts',(12.4230808101438,22.8400320311648,12.));
#248629=CARTESIAN_POINT('',(12.4230808101438,22.8400320311648,0.));
#248630=CARTESIAN_POINT('Ctrl Pts',(9.71462809124917,20.353053841303,0.));
#248631=CARTESIAN_POINT('Ctrl Pts',(9.71462954053074,20.353060251684,0.));
#248632=CARTESIAN_POINT('Ctrl Pts',(9.71465227853122,20.3531126095522,0.));
#248633=CARTESIAN_POINT('Ctrl Pts',(9.71474590350791,20.3533097561886,0.));
#248634=CARTESIAN_POINT('Ctrl Pts',(9.714989780521,20.3538098605706,0.));
#248635=CARTESIAN_POINT('Ctrl Pts',(9.71549257088174,20.3548282742361,0.));
#248636=CARTESIAN_POINT('Ctrl Pts',(9.71619192554146,20.3562337557875,0.));
#248637=CARTESIAN_POINT('Ctrl Pts',(9.71708493723061,20.3580133103357,0.));
#248638=CARTESIAN_POINT('Ctrl Pts',(9.71816778327998,20.3601498764344,0.));
#248639=CARTESIAN_POINT('Ctrl Pts',(9.71943648548114,20.362625691398,0.));
#248640=CARTESIAN_POINT('Ctrl Pts',(9.72088778381101,20.3654261611055,0.));
#248641=CARTESIAN_POINT('Ctrl Pts',(9.72251930722503,20.3685406190576,0.));
#248642=CARTESIAN_POINT('Ctrl Pts',(9.72432910043192,20.371960235676,0.));
#248643=CARTESIAN_POINT('Ctrl Pts',(9.7263153173287,20.3756766651952,0.));
#248644=CARTESIAN_POINT('Ctrl Pts',(9.72847589116532,20.3796805893304,0.));
#248645=CARTESIAN_POINT('Ctrl Pts',(9.73080870123726,20.3839624556742,0.));
#248646=CARTESIAN_POINT('Ctrl Pts',(9.73331167102812,20.3885129129912,0.));
#248647=CARTESIAN_POINT('Ctrl Pts',(9.73598292014249,20.3933234845646,0.));
#248648=CARTESIAN_POINT('Ctrl Pts',(9.73882077613206,20.3983866213331,0.));
#248649=CARTESIAN_POINT('Ctrl Pts',(9.74182369656272,20.4036953576549,0.));
#248650=CARTESIAN_POINT('Ctrl Pts',(9.74499021838536,20.4092430879861,0.));
#248651=CARTESIAN_POINT('Ctrl Pts',(9.74831889242174,20.4150232777393,0.));
#248652=CARTESIAN_POINT('Ctrl Pts',(9.75180829786433,20.4210295275818,0.));
#248653=CARTESIAN_POINT('Ctrl Pts',(9.75545705902416,20.4272556476629,0.));
#248654=CARTESIAN_POINT('Ctrl Pts',(9.75926386289929,20.4336957355474,0.));
#248655=CARTESIAN_POINT('Ctrl Pts',(9.76322747195502,20.4403442329401,0.));
#248656=CARTESIAN_POINT('Ctrl Pts',(9.76734670980896,20.447195862298,0.));
#248657=CARTESIAN_POINT('Ctrl Pts',(9.77162045104069,20.4542455817527,0.));
#248658=CARTESIAN_POINT('Ctrl Pts',(9.77604760815522,20.4614885274973,0.));
#248659=CARTESIAN_POINT('Ctrl Pts',(9.78062712373313,20.4689199790668,0.));
#248660=CARTESIAN_POINT('Ctrl Pts',(9.78535797314162,20.4765353711585,0.));
#248661=CARTESIAN_POINT('Ctrl Pts',(9.79023916498659,20.4843302955329,0.));
#248662=CARTESIAN_POINT('Ctrl Pts',(9.79526974288343,20.4923005087945,0.));
#248663=CARTESIAN_POINT('Ctrl Pts',(9.80044878520967,20.500441931211,0.));
#248664=CARTESIAN_POINT('Ctrl Pts',(9.80577540161102,20.5087506310507,0.));
#248665=CARTESIAN_POINT('Ctrl Pts',(9.81124873025278,20.5172228122839,0.));
#248666=CARTESIAN_POINT('Ctrl Pts',(9.81686793455918,20.5258548000625,0.));
#248667=CARTESIAN_POINT('Ctrl Pts',(9.82263220080327,20.534643029951,0.));
#248668=CARTESIAN_POINT('Ctrl Pts',(9.82854073773857,20.5435840460717,0.));
#248669=CARTESIAN_POINT('Ctrl Pts',(9.8345927758532,20.5526744976461,0.));
#248670=CARTESIAN_POINT('Ctrl Pts',(9.84078756677589,20.5619111362406,0.));
#248671=CARTESIAN_POINT('Ctrl Pts',(9.84712438256308,20.5712908125145,0.));
#248672=CARTESIAN_POINT('Ctrl Pts',(9.85360251457004,20.580810471002,0.));
#248673=CARTESIAN_POINT('Ctrl Pts',(9.86022127232749,20.5904671449755,0.));
#248674=CARTESIAN_POINT('Ctrl Pts',(9.86697998242612,20.6002579513696,0.));
#248675=CARTESIAN_POINT('Ctrl Pts',(9.87387798732943,20.6101800854491,0.));
#248676=CARTESIAN_POINT('Ctrl Pts',(9.88091464472669,20.6202308177472,0.));
#248677=CARTESIAN_POINT('Ctrl Pts',(9.88808932697304,20.6304074914086,0.));
#248678=CARTESIAN_POINT('Ctrl Pts',(9.89540142049123,20.6407075193977,0.));
#248679=CARTESIAN_POINT('Ctrl Pts',(9.90285032516695,20.6511283817415,0.));
#248680=CARTESIAN_POINT('Ctrl Pts',(9.91043545377004,20.6616676228315,0.));
#248681=CARTESIAN_POINT('Ctrl Pts',(9.91815623141284,20.6723228488262,0.));
#248682=CARTESIAN_POINT('Ctrl Pts',(9.9260120949875,20.6830917250255,0.));
#248683=CARTESIAN_POINT('Ctrl Pts',(9.93400249259736,20.6939719732485,0.));
#248684=CARTESIAN_POINT('Ctrl Pts',(9.9421268829825,20.7049613692237,0.));
#248685=CARTESIAN_POINT('Ctrl Pts',(9.95038473514962,20.7160577407581,0.));
#248686=CARTESIAN_POINT('Ctrl Pts',(9.95877552798403,20.7272589658752,0.));
#248687=CARTESIAN_POINT('Ctrl Pts',(9.96729874986198,20.7385629709795,0.));
#248688=CARTESIAN_POINT('Ctrl Pts',(9.97595389823461,20.7499677289626,0.));
#248689=CARTESIAN_POINT('Ctrl Pts',(9.98474047926846,20.7614712574989,0.));
#248690=CARTESIAN_POINT('Ctrl Pts',(9.99365800754637,20.7730716175417,0.));
#248691=CARTESIAN_POINT('Ctrl Pts',(10.0027060057389,20.7847669117568,0.));
#248692=CARTESIAN_POINT('Ctrl Pts',(10.0118840042786,20.7965552829907,0.));
#248693=CARTESIAN_POINT('Ctrl Pts',(10.0211915410095,20.8084349126885,0.));
#248694=CARTESIAN_POINT('Ctrl Pts',(10.0306281609435,20.8204040196599,0.));
#248695=CARTESIAN_POINT('Ctrl Pts',(10.0401934160234,20.8324608588906,0.));
#248696=CARTESIAN_POINT('Ctrl Pts',(10.0498868648733,20.8446037203402,0.));
#248697=CARTESIAN_POINT('Ctrl Pts',(10.0597080725375,20.856830927732,0.));
#248698=CARTESIAN_POINT('Ctrl Pts',(10.0696566102219,20.8691408373705,0.));
#248699=CARTESIAN_POINT('Ctrl Pts',(10.0797320551154,20.8815318371844,0.));
#248700=CARTESIAN_POINT('Ctrl Pts',(10.0899339901916,20.8940023457371,0.));
#248701=CARTESIAN_POINT('Ctrl Pts',(10.1002620040076,20.9065508112556,0.));
#248702=CARTESIAN_POINT('Ctrl Pts',(10.1107156904836,20.9191757106266,0.));
#248703=CARTESIAN_POINT('Ctrl Pts',(10.1212946487057,20.931875548473,0.));
#248704=CARTESIAN_POINT('Ctrl Pts',(10.1319984827909,20.944648856393,0.));
#248705=CARTESIAN_POINT('Ctrl Pts',(10.1428268017257,20.9574941921591,0.));
#248706=CARTESIAN_POINT('Ctrl Pts',(10.1537792192065,20.970410138937,0.));
#248707=CARTESIAN_POINT('Ctrl Pts',(10.1648553534567,20.9833953044737,0.));
#248708=CARTESIAN_POINT('Ctrl Pts',(10.1760548270765,20.9964483203685,0.));
#248709=CARTESIAN_POINT('Ctrl Pts',(10.1873772669358,21.0095678414486,0.));
#248710=CARTESIAN_POINT('Ctrl Pts',(10.1988223040425,21.0227525451107,0.));
#248711=CARTESIAN_POINT('Ctrl Pts',(10.2103895734123,21.0360011306814,0.));
#248712=CARTESIAN_POINT('Ctrl Pts',(10.2220787139157,21.0493123187484,0.));
#248713=CARTESIAN_POINT('Ctrl Pts',(10.233889368157,21.0626848505665,0.));
#248714=CARTESIAN_POINT('Ctrl Pts',(10.2458211823915,21.0761174875448,0.));
#248715=CARTESIAN_POINT('Ctrl Pts',(10.2578738064183,21.0896090107066,0.));
#248716=CARTESIAN_POINT('Ctrl Pts',(10.2700468934743,21.1031582201625,0.));
#248717=CARTESIAN_POINT('Ctrl Pts',(10.2823401001067,21.1167639345623,0.));
#248718=CARTESIAN_POINT('Ctrl Pts',(10.2947530860714,21.130424990599,0.));
#248719=CARTESIAN_POINT('Ctrl Pts',(10.307285514268,21.1441402425831,0.));
#248720=CARTESIAN_POINT('Ctrl Pts',(10.3199370506541,21.1579085619959,0.));
#248721=CARTESIAN_POINT('Ctrl Pts',(10.3327073641574,21.1717288370512,0.));
#248722=CARTESIAN_POINT('Ctrl Pts',(10.3455961265706,21.1855999722427,0.));
#248723=CARTESIAN_POINT('Ctrl Pts',(10.3586030124595,21.1995208879205,0.));
#248724=CARTESIAN_POINT('Ctrl Pts',(10.3717276991137,21.2134905199359,0.));
#248725=CARTESIAN_POINT('Ctrl Pts',(10.384969866479,21.2275078192708,0.));
#248726=CARTESIAN_POINT('Ctrl Pts',(10.3983291970846,21.2415717516713,0.));
#248727=CARTESIAN_POINT('Ctrl Pts',(10.4118053759584,21.2556812972741,0.));
#248728=CARTESIAN_POINT('Ctrl Pts',(10.4253980905394,21.2698354502391,0.));
#248729=CARTESIAN_POINT('Ctrl Pts',(10.4391070306385,21.2840332184471,0.));
#248730=CARTESIAN_POINT('Ctrl Pts',(10.452931888387,21.2982736231924,0.));
#248731=CARTESIAN_POINT('Ctrl Pts',(10.4668723581768,21.312555698873,0.));
#248732=CARTESIAN_POINT('Ctrl Pts',(10.4809281365933,21.3268784926823,0.));
#248733=CARTESIAN_POINT('Ctrl Pts',(10.4950989223341,21.3412410642912,0.));
#248734=CARTESIAN_POINT('Ctrl Pts',(10.5093844161689,21.3556424855822,0.));
#248735=CARTESIAN_POINT('Ctrl Pts',(10.523784320906,21.3700818403942,0.));
#248736=CARTESIAN_POINT('Ctrl Pts',(10.5382983413422,21.3845582242604,0.));
#248737=CARTESIAN_POINT('Ctrl Pts',(10.5529261842107,21.3990707441495,0.));
#248738=CARTESIAN_POINT('Ctrl Pts',(10.5676675581106,21.4136185181974,0.));
#248739=CARTESIAN_POINT('Ctrl Pts',(10.582522173457,21.4282006754624,0.));
#248740=CARTESIAN_POINT('Ctrl Pts',(10.597489742462,21.4428163557137,0.));
#248741=CARTESIAN_POINT('Ctrl Pts',(10.612569979096,21.4574647092093,0.));
#248742=CARTESIAN_POINT('Ctrl Pts',(10.6277625990456,21.4721448964766,0.));
#248743=CARTESIAN_POINT('Ctrl Pts',(10.6430673196609,21.4868560880893,0.));
#248744=CARTESIAN_POINT('Ctrl Pts',(10.658483859894,21.5015974644454,0.));
#248745=CARTESIAN_POINT('Ctrl Pts',(10.6740119402835,21.5163682155805,0.));
#248746=CARTESIAN_POINT('Ctrl Pts',(10.689651282929,21.531167540981,0.));
#248747=CARTESIAN_POINT('Ctrl Pts',(10.7054016114571,21.5459946493955,0.));
#248748=CARTESIAN_POINT('Ctrl Pts',(10.7212626509816,21.5608487586467,0.));
#248749=CARTESIAN_POINT('Ctrl Pts',(10.7372341280468,21.5757290954372,0.));
#248750=CARTESIAN_POINT('Ctrl Pts',(10.7533157705943,21.5906348951745,0.));
#248751=CARTESIAN_POINT('Ctrl Pts',(10.7695073079554,21.6055654018179,0.));
#248752=CARTESIAN_POINT('Ctrl Pts',(10.7858084708262,21.6205198677176,0.));
#248753=CARTESIAN_POINT('Ctrl Pts',(10.8022189912369,21.6354975534558,0.));
#248754=CARTESIAN_POINT('Ctrl Pts',(10.8187386025135,21.6504977276864,0.));
#248755=CARTESIAN_POINT('Ctrl Pts',(10.835367039227,21.6655196669727,0.));
#248756=CARTESIAN_POINT('Ctrl Pts',(10.8521040371832,21.6805626556461,0.));
#248757=CARTESIAN_POINT('Ctrl Pts',(10.8689493334093,21.6956259856667,0.));
#248758=CARTESIAN_POINT('Ctrl Pts',(10.8859026661292,21.7107089564822,0.));
#248759=CARTESIAN_POINT('Ctrl Pts',(10.9029637747341,21.7258108748874,0.));
#248760=CARTESIAN_POINT('Ctrl Pts',(10.9201323997386,21.74093105488,0.));
#248761=CARTESIAN_POINT('Ctrl Pts',(10.9374082827446,21.7560688175252,0.));
#248762=CARTESIAN_POINT('Ctrl Pts',(10.9547911664457,21.7712234908468,0.));
#248763=CARTESIAN_POINT('Ctrl Pts',(10.9722807946157,21.7863944097143,0.));
#248764=CARTESIAN_POINT('Ctrl Pts',(10.9898769120913,21.8015809157302,0.));
#248765=CARTESIAN_POINT('Ctrl Pts',(11.0075792647477,21.8167823571168,0.));
#248766=CARTESIAN_POINT('Ctrl Pts',(11.0253875994598,21.8319980886033,0.));
#248767=CARTESIAN_POINT('Ctrl Pts',(11.0433016640808,21.8472274713103,0.));
#248768=CARTESIAN_POINT('Ctrl Pts',(11.0613212074364,21.8624698726319,0.));
#248769=CARTESIAN_POINT('Ctrl Pts',(11.0794459793058,21.8777246661191,0.));
#248770=CARTESIAN_POINT('Ctrl Pts',(11.0976757303944,21.8929912313608,0.));
#248771=CARTESIAN_POINT('Ctrl Pts',(11.1160102123024,21.9082689538687,0.));
#248772=CARTESIAN_POINT('Ctrl Pts',(11.134449177474,21.9235572249518,0.));
#248773=CARTESIAN_POINT('Ctrl Pts',(11.1529923792002,21.9388554416437,0.));
#248774=CARTESIAN_POINT('Ctrl Pts',(11.1716395716375,21.9541630066504,0.));
#248775=CARTESIAN_POINT('Ctrl Pts',(11.1903905098109,21.9694793282913,0.));
#248776=CARTESIAN_POINT('Ctrl Pts',(11.2092449496125,21.9848038204439,0.));
#248777=CARTESIAN_POINT('Ctrl Pts',(11.2282026477897,22.000135902484,0.));
#248778=CARTESIAN_POINT('Ctrl Pts',(11.2472633619276,22.0154749992364,0.));
#248779=CARTESIAN_POINT('Ctrl Pts',(11.2664268504207,22.0308205408351,0.));
#248780=CARTESIAN_POINT('Ctrl Pts',(11.2856928724374,22.0461719625661,0.));
#248781=CARTESIAN_POINT('Ctrl Pts',(11.3050611878771,22.0615287047179,0.));
#248782=CARTESIAN_POINT('Ctrl Pts',(11.3245315573168,22.0768902124267,0.));
#248783=CARTESIAN_POINT('Ctrl Pts',(11.3441037419553,22.0922559355293,0.));
#248784=CARTESIAN_POINT('Ctrl Pts',(11.3637775035367,22.1076253283978,0.));
#248785=CARTESIAN_POINT('Ctrl Pts',(11.3835526044256,22.1229978500185,0.));
#248786=CARTESIAN_POINT('Ctrl Pts',(11.4034288076908,22.1383729640963,0.));
#248787=CARTESIAN_POINT('Ctrl Pts',(11.4234058771742,22.1537501391486,0.));
#248788=CARTESIAN_POINT('Ctrl Pts',(11.443483577557,22.1691288486096,0.));
#248789=CARTESIAN_POINT('Ctrl Pts',(11.463661674411,22.184508570917,0.));
#248790=CARTESIAN_POINT('Ctrl Pts',(11.4839399342589,22.1998887896435,0.));
#248791=CARTESIAN_POINT('Ctrl Pts',(11.504318124424,22.215268993102,0.));
#248792=CARTESIAN_POINT('Ctrl Pts',(11.5247960128476,22.2306486738899,0.));
#248793=CARTESIAN_POINT('Ctrl Pts',(11.545373367912,22.2460273284653,0.));
#248794=CARTESIAN_POINT('Ctrl Pts',(11.5660499582403,22.2614044566898,0.));
#248795=CARTESIAN_POINT('Ctrl Pts',(11.5868255525189,22.2767795614349,0.));
#248796=CARTESIAN_POINT('Ctrl Pts',(11.6076999192359,22.2921521480358,0.));
#248797=CARTESIAN_POINT('Ctrl Pts',(11.6286728270011,22.3075217249049,0.));
#248798=CARTESIAN_POINT('Ctrl Pts',(11.6497440449858,22.3228878043976,0.));
#248799=CARTESIAN_POINT('Ctrl Pts',(11.6709133432986,22.3382499035618,0.));
#248800=CARTESIAN_POINT('Ctrl Pts',(11.6921804934056,22.3536075450028,0.));
#248801=CARTESIAN_POINT('Ctrl Pts',(11.7135452684532,22.3689602575492,0.));
#248802=CARTESIAN_POINT('Ctrl Pts',(11.7350074437961,22.3843075773905,0.));
#248803=CARTESIAN_POINT('Ctrl Pts',(11.7565667964765,22.39964904692,0.));
#248804=CARTESIAN_POINT('Ctrl Pts',(11.7782231042041,22.4149842125018,0.));
#248805=CARTESIAN_POINT('Ctrl Pts',(11.7999761445175,22.4303126226468,0.));
#248806=CARTESIAN_POINT('Ctrl Pts',(11.8218256937889,22.4456338258738,0.));
#248807=CARTESIAN_POINT('Ctrl Pts',(11.8437715264487,22.4609473690469,0.));
#248808=CARTESIAN_POINT('Ctrl Pts',(11.8658134137018,22.4762527946694,0.));
#248809=CARTESIAN_POINT('Ctrl Pts',(11.8879511239941,22.4915496418472,0.));
#248810=CARTESIAN_POINT('Ctrl Pts',(11.9101844254555,22.5068374513958,0.));
#248811=CARTESIAN_POINT('Ctrl Pts',(11.9325130877801,22.5221157697869,0.));
#248812=CARTESIAN_POINT('Ctrl Pts',(11.9549368843996,22.5373841537299,0.));
#248813=CARTESIAN_POINT('Ctrl Pts',(11.9774555943496,22.5526421741159,0.));
#248814=CARTESIAN_POINT('Ctrl Pts',(12.0000690046697,22.5678894211194,0.));
#248815=CARTESIAN_POINT('Ctrl Pts',(12.0227769113132,22.5831255061306,0.));
#248816=CARTESIAN_POINT('Ctrl Pts',(12.0455791139135,22.5983500505675,0.));
#248817=CARTESIAN_POINT('Ctrl Pts',(12.0684754113869,22.613562676493,0.));
#248818=CARTESIAN_POINT('Ctrl Pts',(12.0914655972828,22.628762996708,0.));
#248819=CARTESIAN_POINT('Ctrl Pts',(12.1145494550384,22.6439506046611,0.));
#248820=CARTESIAN_POINT('Ctrl Pts',(12.1377267537141,22.6591250653942,0.));
#248821=CARTESIAN_POINT('Ctrl Pts',(12.1609972423088,22.6742859034891,0.));
#248822=CARTESIAN_POINT('Ctrl Pts',(12.1843606579246,22.6894326204959,0.));
#248823=CARTESIAN_POINT('Ctrl Pts',(12.2078167360267,22.7045647168659,0.));
#248824=CARTESIAN_POINT('Ctrl Pts',(12.2313652198047,22.7196817119299,0.));
#248825=CARTESIAN_POINT('Ctrl Pts',(12.2550058702389,22.7347831655251,0.));
#248826=CARTESIAN_POINT('Ctrl Pts',(12.2787384750747,22.7498686970096,0.));
#248827=CARTESIAN_POINT('Ctrl Pts',(12.3025628601811,22.7649380101154,0.));
#248828=CARTESIAN_POINT('Ctrl Pts',(12.3264788926108,22.7799908974947,0.));
#248829=CARTESIAN_POINT('Ctrl Pts',(12.3504864740361,22.7950272216959,0.));
#248830=CARTESIAN_POINT('Ctrl Pts',(12.3745855366772,22.8100469022632,0.));
#248831=CARTESIAN_POINT('Ctrl Pts',(12.393937937903,22.8220493007353,0.));
#248832=CARTESIAN_POINT('Ctrl Pts',(12.4084933766366,22.8310435872852,0.));
#248833=CARTESIAN_POINT('Ctrl Pts',(12.4182152851867,22.8370364396497,0.));
#248834=CARTESIAN_POINT('Ctrl Pts',(12.4230808101438,22.8400320311648,0.));
#248835=CARTESIAN_POINT('',(12.4230808101438,22.8400320311648,12.));
#248836=CARTESIAN_POINT('Ctrl Pts',(12.4230808101438,22.8400320311648,12.));
#248837=CARTESIAN_POINT('Ctrl Pts',(12.4182152851867,22.8370364396497,12.));
#248838=CARTESIAN_POINT('Ctrl Pts',(12.4084933766366,22.8310435872852,12.));
#248839=CARTESIAN_POINT('Ctrl Pts',(12.393937937903,22.8220493007353,12.));
#248840=CARTESIAN_POINT('Ctrl Pts',(12.3745855366772,22.8100469022632,12.));
#248841=CARTESIAN_POINT('Ctrl Pts',(12.3504864740361,22.7950272216959,12.));
#248842=CARTESIAN_POINT('Ctrl Pts',(12.3264788926108,22.7799908974947,12.));
#248843=CARTESIAN_POINT('Ctrl Pts',(12.3025628601811,22.7649380101154,12.));
#248844=CARTESIAN_POINT('Ctrl Pts',(12.2787384750747,22.7498686970096,12.));
#248845=CARTESIAN_POINT('Ctrl Pts',(12.2550058702389,22.7347831655251,12.));
#248846=CARTESIAN_POINT('Ctrl Pts',(12.2313652198047,22.7196817119299,12.));
#248847=CARTESIAN_POINT('Ctrl Pts',(12.2078167360267,22.7045647168659,12.));
#248848=CARTESIAN_POINT('Ctrl Pts',(12.1843606579246,22.6894326204959,12.));
#248849=CARTESIAN_POINT('Ctrl Pts',(12.1609972423088,22.6742859034891,12.));
#248850=CARTESIAN_POINT('Ctrl Pts',(12.1377267537141,22.6591250653942,12.));
#248851=CARTESIAN_POINT('Ctrl Pts',(12.1145494550384,22.6439506046611,12.));
#248852=CARTESIAN_POINT('Ctrl Pts',(12.0914655972828,22.628762996708,12.));
#248853=CARTESIAN_POINT('Ctrl Pts',(12.0684754113869,22.613562676493,12.));
#248854=CARTESIAN_POINT('Ctrl Pts',(12.0455791139135,22.5983500505675,12.));
#248855=CARTESIAN_POINT('Ctrl Pts',(12.0227769113132,22.5831255061306,12.));
#248856=CARTESIAN_POINT('Ctrl Pts',(12.0000690046697,22.5678894211194,12.));
#248857=CARTESIAN_POINT('Ctrl Pts',(11.9774555943496,22.5526421741159,12.));
#248858=CARTESIAN_POINT('Ctrl Pts',(11.9549368843996,22.5373841537299,12.));
#248859=CARTESIAN_POINT('Ctrl Pts',(11.9325130877801,22.5221157697869,12.));
#248860=CARTESIAN_POINT('Ctrl Pts',(11.9101844254555,22.5068374513958,12.));
#248861=CARTESIAN_POINT('Ctrl Pts',(11.8879511239941,22.4915496418472,12.));
#248862=CARTESIAN_POINT('Ctrl Pts',(11.8658134137018,22.4762527946694,12.));
#248863=CARTESIAN_POINT('Ctrl Pts',(11.8437715264487,22.4609473690469,12.));
#248864=CARTESIAN_POINT('Ctrl Pts',(11.8218256937889,22.4456338258738,12.));
#248865=CARTESIAN_POINT('Ctrl Pts',(11.7999761445175,22.4303126226468,12.));
#248866=CARTESIAN_POINT('Ctrl Pts',(11.7782231042041,22.4149842125018,12.));
#248867=CARTESIAN_POINT('Ctrl Pts',(11.7565667964765,22.39964904692,12.));
#248868=CARTESIAN_POINT('Ctrl Pts',(11.7350074437961,22.3843075773905,12.));
#248869=CARTESIAN_POINT('Ctrl Pts',(11.7135452684532,22.3689602575492,12.));
#248870=CARTESIAN_POINT('Ctrl Pts',(11.6921804934056,22.3536075450028,12.));
#248871=CARTESIAN_POINT('Ctrl Pts',(11.6709133432986,22.3382499035618,12.));
#248872=CARTESIAN_POINT('Ctrl Pts',(11.6497440449858,22.3228878043976,12.));
#248873=CARTESIAN_POINT('Ctrl Pts',(11.6286728270011,22.3075217249049,12.));
#248874=CARTESIAN_POINT('Ctrl Pts',(11.6076999192359,22.2921521480358,12.));
#248875=CARTESIAN_POINT('Ctrl Pts',(11.5868255525189,22.2767795614349,12.));
#248876=CARTESIAN_POINT('Ctrl Pts',(11.5660499582403,22.2614044566898,12.));
#248877=CARTESIAN_POINT('Ctrl Pts',(11.545373367912,22.2460273284653,12.));
#248878=CARTESIAN_POINT('Ctrl Pts',(11.5247960128476,22.2306486738899,12.));
#248879=CARTESIAN_POINT('Ctrl Pts',(11.504318124424,22.215268993102,12.));
#248880=CARTESIAN_POINT('Ctrl Pts',(11.4839399342589,22.1998887896435,12.));
#248881=CARTESIAN_POINT('Ctrl Pts',(11.463661674411,22.184508570917,12.));
#248882=CARTESIAN_POINT('Ctrl Pts',(11.443483577557,22.1691288486096,12.));
#248883=CARTESIAN_POINT('Ctrl Pts',(11.4234058771742,22.1537501391486,12.));
#248884=CARTESIAN_POINT('Ctrl Pts',(11.4034288076908,22.1383729640963,12.));
#248885=CARTESIAN_POINT('Ctrl Pts',(11.3835526044256,22.1229978500185,12.));
#248886=CARTESIAN_POINT('Ctrl Pts',(11.3637775035367,22.1076253283978,12.));
#248887=CARTESIAN_POINT('Ctrl Pts',(11.3441037419553,22.0922559355293,12.));
#248888=CARTESIAN_POINT('Ctrl Pts',(11.3245315573168,22.0768902124267,12.));
#248889=CARTESIAN_POINT('Ctrl Pts',(11.3050611878771,22.0615287047179,12.));
#248890=CARTESIAN_POINT('Ctrl Pts',(11.2856928724374,22.0461719625661,12.));
#248891=CARTESIAN_POINT('Ctrl Pts',(11.2664268504207,22.0308205408351,12.));
#248892=CARTESIAN_POINT('Ctrl Pts',(11.2472633619276,22.0154749992364,12.));
#248893=CARTESIAN_POINT('Ctrl Pts',(11.2282026477897,22.000135902484,12.));
#248894=CARTESIAN_POINT('Ctrl Pts',(11.2092449496125,21.9848038204439,12.));
#248895=CARTESIAN_POINT('Ctrl Pts',(11.1903905098109,21.9694793282913,12.));
#248896=CARTESIAN_POINT('Ctrl Pts',(11.1716395716375,21.9541630066504,12.));
#248897=CARTESIAN_POINT('Ctrl Pts',(11.1529923792002,21.9388554416437,12.));
#248898=CARTESIAN_POINT('Ctrl Pts',(11.134449177474,21.9235572249518,12.));
#248899=CARTESIAN_POINT('Ctrl Pts',(11.1160102123024,21.9082689538687,12.));
#248900=CARTESIAN_POINT('Ctrl Pts',(11.0976757303944,21.8929912313608,12.));
#248901=CARTESIAN_POINT('Ctrl Pts',(11.0794459793058,21.8777246661191,12.));
#248902=CARTESIAN_POINT('Ctrl Pts',(11.0613212074364,21.8624698726319,12.));
#248903=CARTESIAN_POINT('Ctrl Pts',(11.0433016640808,21.8472274713103,12.));
#248904=CARTESIAN_POINT('Ctrl Pts',(11.0253875994598,21.8319980886033,12.));
#248905=CARTESIAN_POINT('Ctrl Pts',(11.0075792647477,21.8167823571168,12.));
#248906=CARTESIAN_POINT('Ctrl Pts',(10.9898769120913,21.8015809157302,12.));
#248907=CARTESIAN_POINT('Ctrl Pts',(10.9722807946157,21.7863944097143,12.));
#248908=CARTESIAN_POINT('Ctrl Pts',(10.9547911664457,21.7712234908468,12.));
#248909=CARTESIAN_POINT('Ctrl Pts',(10.9374082827446,21.7560688175252,12.));
#248910=CARTESIAN_POINT('Ctrl Pts',(10.9201323997386,21.74093105488,12.));
#248911=CARTESIAN_POINT('Ctrl Pts',(10.9029637747341,21.7258108748874,12.));
#248912=CARTESIAN_POINT('Ctrl Pts',(10.8859026661292,21.7107089564822,12.));
#248913=CARTESIAN_POINT('Ctrl Pts',(10.8689493334093,21.6956259856667,12.));
#248914=CARTESIAN_POINT('Ctrl Pts',(10.8521040371832,21.6805626556461,12.));
#248915=CARTESIAN_POINT('Ctrl Pts',(10.835367039227,21.6655196669727,12.));
#248916=CARTESIAN_POINT('Ctrl Pts',(10.8187386025135,21.6504977276864,12.));
#248917=CARTESIAN_POINT('Ctrl Pts',(10.8022189912369,21.6354975534558,12.));
#248918=CARTESIAN_POINT('Ctrl Pts',(10.7858084708262,21.6205198677176,12.));
#248919=CARTESIAN_POINT('Ctrl Pts',(10.7695073079554,21.6055654018179,12.));
#248920=CARTESIAN_POINT('Ctrl Pts',(10.7533157705943,21.5906348951745,12.));
#248921=CARTESIAN_POINT('Ctrl Pts',(10.7372341280468,21.5757290954372,12.));
#248922=CARTESIAN_POINT('Ctrl Pts',(10.7212626509816,21.5608487586467,12.));
#248923=CARTESIAN_POINT('Ctrl Pts',(10.7054016114571,21.5459946493955,12.));
#248924=CARTESIAN_POINT('Ctrl Pts',(10.689651282929,21.531167540981,12.));
#248925=CARTESIAN_POINT('Ctrl Pts',(10.6740119402835,21.5163682155805,12.));
#248926=CARTESIAN_POINT('Ctrl Pts',(10.658483859894,21.5015974644454,12.));
#248927=CARTESIAN_POINT('Ctrl Pts',(10.6430673196609,21.4868560880893,12.));
#248928=CARTESIAN_POINT('Ctrl Pts',(10.6277625990456,21.4721448964766,12.));
#248929=CARTESIAN_POINT('Ctrl Pts',(10.612569979096,21.4574647092093,12.));
#248930=CARTESIAN_POINT('Ctrl Pts',(10.597489742462,21.4428163557137,12.));
#248931=CARTESIAN_POINT('Ctrl Pts',(10.582522173457,21.4282006754624,12.));
#248932=CARTESIAN_POINT('Ctrl Pts',(10.5676675581106,21.4136185181974,12.));
#248933=CARTESIAN_POINT('Ctrl Pts',(10.5529261842107,21.3990707441495,12.));
#248934=CARTESIAN_POINT('Ctrl Pts',(10.5382983413422,21.3845582242604,12.));
#248935=CARTESIAN_POINT('Ctrl Pts',(10.523784320906,21.3700818403942,12.));
#248936=CARTESIAN_POINT('Ctrl Pts',(10.5093844161689,21.3556424855822,12.));
#248937=CARTESIAN_POINT('Ctrl Pts',(10.4950989223341,21.3412410642912,12.));
#248938=CARTESIAN_POINT('Ctrl Pts',(10.4809281365933,21.3268784926823,12.));
#248939=CARTESIAN_POINT('Ctrl Pts',(10.4668723581768,21.312555698873,12.));
#248940=CARTESIAN_POINT('Ctrl Pts',(10.452931888387,21.2982736231924,12.));
#248941=CARTESIAN_POINT('Ctrl Pts',(10.4391070306385,21.2840332184471,12.));
#248942=CARTESIAN_POINT('Ctrl Pts',(10.4253980905394,21.2698354502391,12.));
#248943=CARTESIAN_POINT('Ctrl Pts',(10.4118053759584,21.2556812972741,12.));
#248944=CARTESIAN_POINT('Ctrl Pts',(10.3983291970846,21.2415717516713,12.));
#248945=CARTESIAN_POINT('Ctrl Pts',(10.384969866479,21.2275078192708,12.));
#248946=CARTESIAN_POINT('Ctrl Pts',(10.3717276991137,21.2134905199359,12.));
#248947=CARTESIAN_POINT('Ctrl Pts',(10.3586030124595,21.1995208879205,12.));
#248948=CARTESIAN_POINT('Ctrl Pts',(10.3455961265706,21.1855999722427,12.));
#248949=CARTESIAN_POINT('Ctrl Pts',(10.3327073641574,21.1717288370512,12.));
#248950=CARTESIAN_POINT('Ctrl Pts',(10.3199370506541,21.1579085619959,12.));
#248951=CARTESIAN_POINT('Ctrl Pts',(10.307285514268,21.1441402425831,12.));
#248952=CARTESIAN_POINT('Ctrl Pts',(10.2947530860714,21.130424990599,12.));
#248953=CARTESIAN_POINT('Ctrl Pts',(10.2823401001067,21.1167639345623,12.));
#248954=CARTESIAN_POINT('Ctrl Pts',(10.2700468934743,21.1031582201625,12.));
#248955=CARTESIAN_POINT('Ctrl Pts',(10.2578738064183,21.0896090107066,12.));
#248956=CARTESIAN_POINT('Ctrl Pts',(10.2458211823915,21.0761174875448,12.));
#248957=CARTESIAN_POINT('Ctrl Pts',(10.233889368157,21.0626848505665,12.));
#248958=CARTESIAN_POINT('Ctrl Pts',(10.2220787139157,21.0493123187484,12.));
#248959=CARTESIAN_POINT('Ctrl Pts',(10.2103895734123,21.0360011306814,12.));
#248960=CARTESIAN_POINT('Ctrl Pts',(10.1988223040425,21.0227525451107,12.));
#248961=CARTESIAN_POINT('Ctrl Pts',(10.1873772669358,21.0095678414486,12.));
#248962=CARTESIAN_POINT('Ctrl Pts',(10.1760548270765,20.9964483203685,12.));
#248963=CARTESIAN_POINT('Ctrl Pts',(10.1648553534567,20.9833953044737,12.));
#248964=CARTESIAN_POINT('Ctrl Pts',(10.1537792192065,20.970410138937,12.));
#248965=CARTESIAN_POINT('Ctrl Pts',(10.1428268017257,20.9574941921591,12.));
#248966=CARTESIAN_POINT('Ctrl Pts',(10.1319984827909,20.944648856393,12.));
#248967=CARTESIAN_POINT('Ctrl Pts',(10.1212946487057,20.931875548473,12.));
#248968=CARTESIAN_POINT('Ctrl Pts',(10.1107156904836,20.9191757106266,12.));
#248969=CARTESIAN_POINT('Ctrl Pts',(10.1002620040076,20.9065508112556,12.));
#248970=CARTESIAN_POINT('Ctrl Pts',(10.0899339901916,20.8940023457371,12.));
#248971=CARTESIAN_POINT('Ctrl Pts',(10.0797320551154,20.8815318371844,12.));
#248972=CARTESIAN_POINT('Ctrl Pts',(10.0696566102219,20.8691408373705,12.));
#248973=CARTESIAN_POINT('Ctrl Pts',(10.0597080725375,20.856830927732,12.));
#248974=CARTESIAN_POINT('Ctrl Pts',(10.0498868648733,20.8446037203402,12.));
#248975=CARTESIAN_POINT('Ctrl Pts',(10.0401934160234,20.8324608588906,12.));
#248976=CARTESIAN_POINT('Ctrl Pts',(10.0306281609435,20.8204040196599,12.));
#248977=CARTESIAN_POINT('Ctrl Pts',(10.0211915410095,20.8084349126885,12.));
#248978=CARTESIAN_POINT('Ctrl Pts',(10.0118840042786,20.7965552829907,12.));
#248979=CARTESIAN_POINT('Ctrl Pts',(10.0027060057389,20.7847669117568,12.));
#248980=CARTESIAN_POINT('Ctrl Pts',(9.99365800754637,20.7730716175417,12.));
#248981=CARTESIAN_POINT('Ctrl Pts',(9.98474047926846,20.7614712574989,12.));
#248982=CARTESIAN_POINT('Ctrl Pts',(9.97595389823461,20.7499677289626,12.));
#248983=CARTESIAN_POINT('Ctrl Pts',(9.96729874986198,20.7385629709795,12.));
#248984=CARTESIAN_POINT('Ctrl Pts',(9.95877552798403,20.7272589658752,12.));
#248985=CARTESIAN_POINT('Ctrl Pts',(9.95038473514962,20.7160577407581,12.));
#248986=CARTESIAN_POINT('Ctrl Pts',(9.9421268829825,20.7049613692237,12.));
#248987=CARTESIAN_POINT('Ctrl Pts',(9.93400249259736,20.6939719732485,12.));
#248988=CARTESIAN_POINT('Ctrl Pts',(9.9260120949875,20.6830917250255,12.));
#248989=CARTESIAN_POINT('Ctrl Pts',(9.91815623141284,20.6723228488262,12.));
#248990=CARTESIAN_POINT('Ctrl Pts',(9.91043545377004,20.6616676228315,12.));
#248991=CARTESIAN_POINT('Ctrl Pts',(9.90285032516695,20.6511283817415,12.));
#248992=CARTESIAN_POINT('Ctrl Pts',(9.89540142049123,20.6407075193977,12.));
#248993=CARTESIAN_POINT('Ctrl Pts',(9.88808932697304,20.6304074914086,12.));
#248994=CARTESIAN_POINT('Ctrl Pts',(9.88091464472669,20.6202308177472,12.));
#248995=CARTESIAN_POINT('Ctrl Pts',(9.87387798732943,20.6101800854491,12.));
#248996=CARTESIAN_POINT('Ctrl Pts',(9.86697998242612,20.6002579513696,12.));
#248997=CARTESIAN_POINT('Ctrl Pts',(9.86022127232749,20.5904671449755,12.));
#248998=CARTESIAN_POINT('Ctrl Pts',(9.85360251457004,20.580810471002,12.));
#248999=CARTESIAN_POINT('Ctrl Pts',(9.84712438256308,20.5712908125145,12.));
#249000=CARTESIAN_POINT('Ctrl Pts',(9.84078756677589,20.5619111362406,12.));
#249001=CARTESIAN_POINT('Ctrl Pts',(9.8345927758532,20.5526744976461,12.));
#249002=CARTESIAN_POINT('Ctrl Pts',(9.82854073773857,20.5435840460717,12.));
#249003=CARTESIAN_POINT('Ctrl Pts',(9.82263220080327,20.534643029951,12.));
#249004=CARTESIAN_POINT('Ctrl Pts',(9.81686793455918,20.5258548000625,12.));
#249005=CARTESIAN_POINT('Ctrl Pts',(9.81124873025278,20.5172228122839,12.));
#249006=CARTESIAN_POINT('Ctrl Pts',(9.80577540161102,20.5087506310507,12.));
#249007=CARTESIAN_POINT('Ctrl Pts',(9.80044878520967,20.500441931211,12.));
#249008=CARTESIAN_POINT('Ctrl Pts',(9.79526974288343,20.4923005087945,12.));
#249009=CARTESIAN_POINT('Ctrl Pts',(9.79023916498659,20.4843302955329,12.));
#249010=CARTESIAN_POINT('Ctrl Pts',(9.78535797314162,20.4765353711585,12.));
#249011=CARTESIAN_POINT('Ctrl Pts',(9.78062712373313,20.4689199790668,12.));
#249012=CARTESIAN_POINT('Ctrl Pts',(9.77604760815522,20.4614885274973,12.));
#249013=CARTESIAN_POINT('Ctrl Pts',(9.77162045104069,20.4542455817527,12.));
#249014=CARTESIAN_POINT('Ctrl Pts',(9.76734670980896,20.447195862298,12.));
#249015=CARTESIAN_POINT('Ctrl Pts',(9.76322747195502,20.4403442329401,12.));
#249016=CARTESIAN_POINT('Ctrl Pts',(9.75926386289929,20.4336957355474,12.));
#249017=CARTESIAN_POINT('Ctrl Pts',(9.75545705902416,20.4272556476629,12.));
#249018=CARTESIAN_POINT('Ctrl Pts',(9.75180829786433,20.4210295275818,12.));
#249019=CARTESIAN_POINT('Ctrl Pts',(9.74831889242174,20.4150232777393,12.));
#249020=CARTESIAN_POINT('Ctrl Pts',(9.74499021838536,20.4092430879861,12.));
#249021=CARTESIAN_POINT('Ctrl Pts',(9.74182369656272,20.4036953576549,12.));
#249022=CARTESIAN_POINT('Ctrl Pts',(9.73882077613206,20.3983866213331,12.));
#249023=CARTESIAN_POINT('Ctrl Pts',(9.73598292014249,20.3933234845646,12.));
#249024=CARTESIAN_POINT('Ctrl Pts',(9.73331167102812,20.3885129129912,12.));
#249025=CARTESIAN_POINT('Ctrl Pts',(9.73080870123726,20.3839624556742,12.));
#249026=CARTESIAN_POINT('Ctrl Pts',(9.72847589116532,20.3796805893304,12.));
#249027=CARTESIAN_POINT('Ctrl Pts',(9.7263153173287,20.3756766651952,12.));
#249028=CARTESIAN_POINT('Ctrl Pts',(9.72432910043192,20.371960235676,12.));
#249029=CARTESIAN_POINT('Ctrl Pts',(9.72251930722503,20.3685406190576,12.));
#249030=CARTESIAN_POINT('Ctrl Pts',(9.72088778381101,20.3654261611055,12.));
#249031=CARTESIAN_POINT('Ctrl Pts',(9.71943648548114,20.362625691398,12.));
#249032=CARTESIAN_POINT('Ctrl Pts',(9.71816778327998,20.3601498764344,12.));
#249033=CARTESIAN_POINT('Ctrl Pts',(9.71708493723061,20.3580133103357,12.));
#249034=CARTESIAN_POINT('Ctrl Pts',(9.71619192554146,20.3562337557875,12.));
#249035=CARTESIAN_POINT('Ctrl Pts',(9.71549257088174,20.3548282742361,12.));
#249036=CARTESIAN_POINT('Ctrl Pts',(9.714989780521,20.3538098605706,12.));
#249037=CARTESIAN_POINT('Ctrl Pts',(9.71474590350791,20.3533097561886,12.));
#249038=CARTESIAN_POINT('Ctrl Pts',(9.71465227853122,20.3531126095522,12.));
#249039=CARTESIAN_POINT('Ctrl Pts',(9.71462954053074,20.353060251684,12.));
#249040=CARTESIAN_POINT('Ctrl Pts',(9.71462809124917,20.353053841303,12.));
#249041=CARTESIAN_POINT('',(12.4230808101438,22.8400320311648,0.));
#249042=CARTESIAN_POINT('Origin',(13.9675290154577,16.3449727195352,0.));
#249043=CARTESIAN_POINT('',(14.6513681262571,17.1452095830633,12.));
#249044=CARTESIAN_POINT('',(6.98376450772883,8.17248635976757,12.));
#249045=CARTESIAN_POINT('',(14.6513681262571,17.1452095830633,0.));
#249046=CARTESIAN_POINT('',(14.6513681262571,17.1452095830633,0.));
#249047=CARTESIAN_POINT('',(6.98376450772883,8.17248635976757,0.));
#249048=CARTESIAN_POINT('Ctrl Pts',(13.5685075571671,22.1787195904339,0.));
#249049=CARTESIAN_POINT('Ctrl Pts',(13.5685075571671,22.1787195904339,12.));
#249050=CARTESIAN_POINT('Ctrl Pts',(13.5683460612913,22.1730081264583,0.));
#249051=CARTESIAN_POINT('Ctrl Pts',(13.5683460612913,22.1730081264583,12.));
#249052=CARTESIAN_POINT('Ctrl Pts',(13.5680170531724,22.1615922804939,0.));
#249053=CARTESIAN_POINT('Ctrl Pts',(13.5680170531724,22.1615922804939,12.));
#249054=CARTESIAN_POINT('Ctrl Pts',(13.5675054918922,22.1444897575076,0.));
#249055=CARTESIAN_POINT('Ctrl Pts',(13.5675054918922,22.1444897575076,12.));
#249056=CARTESIAN_POINT('Ctrl Pts',(13.5667873105179,22.1217288871823,0.));
#249057=CARTESIAN_POINT('Ctrl Pts',(13.5667873105179,22.1217288871823,12.));
#249058=CARTESIAN_POINT('Ctrl Pts',(13.5658294169106,22.0933486464442,0.));
#249059=CARTESIAN_POINT('Ctrl Pts',(13.5658294169106,22.0933486464442,12.));
#249060=CARTESIAN_POINT('Ctrl Pts',(13.5648113688894,22.0650393089492,0.));
#249061=CARTESIAN_POINT('Ctrl Pts',(13.5648113688894,22.0650393089492,12.));
#249062=CARTESIAN_POINT('Ctrl Pts',(13.5637332022393,22.0368009736227,0.));
#249063=CARTESIAN_POINT('Ctrl Pts',(13.5637332022393,22.0368009736227,12.));
#249064=CARTESIAN_POINT('Ctrl Pts',(13.5625949868313,22.0086337943431,0.));
#249065=CARTESIAN_POINT('Ctrl Pts',(13.5625949868313,22.0086337943431,12.));
#249066=CARTESIAN_POINT('Ctrl Pts',(13.5613968357589,21.9805379899192,0.));
#249067=CARTESIAN_POINT('Ctrl Pts',(13.5613968357589,21.9805379899192,12.));
#249068=CARTESIAN_POINT('Ctrl Pts',(13.5601389185315,21.9525138592862,0.));
#249069=CARTESIAN_POINT('Ctrl Pts',(13.5601389185315,21.9525138592862,12.));
#249070=CARTESIAN_POINT('Ctrl Pts',(13.5588214586672,21.9245617765827,0.));
#249071=CARTESIAN_POINT('Ctrl Pts',(13.5588214586672,21.9245617765827,12.));
#249072=CARTESIAN_POINT('Ctrl Pts',(13.5574447178484,21.8966821688876,0.));
#249073=CARTESIAN_POINT('Ctrl Pts',(13.5574447178484,21.8966821688876,12.));
#249074=CARTESIAN_POINT('Ctrl Pts',(13.5560089839426,21.8688754989401,0.));
#249075=CARTESIAN_POINT('Ctrl Pts',(13.5560089839426,21.8688754989401,12.));
#249076=CARTESIAN_POINT('Ctrl Pts',(13.5545145573048,21.841142245609,0.));
#249077=CARTESIAN_POINT('Ctrl Pts',(13.5545145573048,21.841142245609,12.));
#249078=CARTESIAN_POINT('Ctrl Pts',(13.5529617381569,21.8134828857963,0.));
#249079=CARTESIAN_POINT('Ctrl Pts',(13.5529617381569,21.8134828857963,12.));
#249080=CARTESIAN_POINT('Ctrl Pts',(13.5513508127232,21.7858978745848,0.));
#249081=CARTESIAN_POINT('Ctrl Pts',(13.5513508127232,21.7858978745848,12.));
#249082=CARTESIAN_POINT('Ctrl Pts',(13.5496820422186,21.7583876294532,0.));
#249083=CARTESIAN_POINT('Ctrl Pts',(13.5496820422186,21.7583876294532,12.));
#249084=CARTESIAN_POINT('Ctrl Pts',(13.5479556704457,21.730952541226,0.));
#249085=CARTESIAN_POINT('Ctrl Pts',(13.5479556704457,21.730952541226,12.));
#249086=CARTESIAN_POINT('Ctrl Pts',(13.546171929503,21.7035929822939,0.));
#249087=CARTESIAN_POINT('Ctrl Pts',(13.546171929503,21.7035929822939,12.));
#249088=CARTESIAN_POINT('Ctrl Pts',(13.5443310461516,21.676309315769,0.));
#249089=CARTESIAN_POINT('Ctrl Pts',(13.5443310461516,21.676309315769,12.));
#249090=CARTESIAN_POINT('Ctrl Pts',(13.5424332480698,21.6491019044647,0.));
#249091=CARTESIAN_POINT('Ctrl Pts',(13.5424332480698,21.6491019044647,12.));
#249092=CARTESIAN_POINT('Ctrl Pts',(13.5404787697798,21.6219711193951,0.));
#249093=CARTESIAN_POINT('Ctrl Pts',(13.5404787697798,21.6219711193951,12.));
#249094=CARTESIAN_POINT('Ctrl Pts',(13.5384678597206,21.5949173499022,0.));
#249095=CARTESIAN_POINT('Ctrl Pts',(13.5384678597206,21.5949173499022,12.));
#249096=CARTESIAN_POINT('Ctrl Pts',(13.5364007790292,21.5679410019011,0.));
#249097=CARTESIAN_POINT('Ctrl Pts',(13.5364007790292,21.5679410019011,12.));
#249098=CARTESIAN_POINT('Ctrl Pts',(13.5342777983225,21.5410424932511,0.));
#249099=CARTESIAN_POINT('Ctrl Pts',(13.5342777983225,21.5410424932511,12.));
#249100=CARTESIAN_POINT('Ctrl Pts',(13.5320991952145,21.5142222501671,0.));
#249101=CARTESIAN_POINT('Ctrl Pts',(13.5320991952145,21.5142222501671,12.));
#249102=CARTESIAN_POINT('Ctrl Pts',(13.5298652514357,21.487480703047,0.));
#249103=CARTESIAN_POINT('Ctrl Pts',(13.5298652514357,21.487480703047,12.));
#249104=CARTESIAN_POINT('Ctrl Pts',(13.5275762503553,21.4608182828695,0.));
#249105=CARTESIAN_POINT('Ctrl Pts',(13.5275762503553,21.4608182828695,12.));
#249106=CARTESIAN_POINT('Ctrl Pts',(13.5252324737795,21.4342354165254,0.));
#249107=CARTESIAN_POINT('Ctrl Pts',(13.5252324737795,21.4342354165254,12.));
#249108=CARTESIAN_POINT('Ctrl Pts',(13.5228342013508,21.4077325259318,0.));
#249109=CARTESIAN_POINT('Ctrl Pts',(13.5228342013508,21.4077325259318,12.));
#249110=CARTESIAN_POINT('Ctrl Pts',(13.5203817122496,21.3813100304967,0.));
#249111=CARTESIAN_POINT('Ctrl Pts',(13.5203817122496,21.3813100304967,12.));
#249112=CARTESIAN_POINT('Ctrl Pts',(13.5178752862461,21.3549683486219,0.));
#249113=CARTESIAN_POINT('Ctrl Pts',(13.5178752862461,21.3549683486219,12.));
#249114=CARTESIAN_POINT('Ctrl Pts',(13.5153152050554,21.328707899634,0.));
#249115=CARTESIAN_POINT('Ctrl Pts',(13.5153152050554,21.328707899634,12.));
#249116=CARTESIAN_POINT('Ctrl Pts',(13.5127017534972,21.3025291054236,0.));
#249117=CARTESIAN_POINT('Ctrl Pts',(13.5127017534972,21.3025291054236,12.));
#249118=CARTESIAN_POINT('Ctrl Pts',(13.5100352209207,21.2764323924442,0.));
#249119=CARTESIAN_POINT('Ctrl Pts',(13.5100352209207,21.2764323924442,12.));
#249120=CARTESIAN_POINT('Ctrl Pts',(13.5073159019454,21.2504181927429,0.));
#249121=CARTESIAN_POINT('Ctrl Pts',(13.5073159019454,21.2504181927429,12.));
#249122=CARTESIAN_POINT('Ctrl Pts',(13.5045440957404,21.224486942933,0.));
#249123=CARTESIAN_POINT('Ctrl Pts',(13.5045440957404,21.224486942933,12.));
#249124=CARTESIAN_POINT('Ctrl Pts',(13.5017201056088,21.1986390835825,0.));
#249125=CARTESIAN_POINT('Ctrl Pts',(13.5017201056088,21.1986390835825,12.));
#249126=CARTESIAN_POINT('Ctrl Pts',(13.4988442384491,21.1728750584173,0.));
#249127=CARTESIAN_POINT('Ctrl Pts',(13.4988442384491,21.1728750584173,12.));
#249128=CARTESIAN_POINT('Ctrl Pts',(13.4959168042934,21.1471953136209,0.));
#249129=CARTESIAN_POINT('Ctrl Pts',(13.4959168042934,21.1471953136209,12.));
#249130=CARTESIAN_POINT('Ctrl Pts',(13.4929381157778,21.1216002970209,0.));
#249131=CARTESIAN_POINT('Ctrl Pts',(13.4929381157778,21.1216002970209,12.));
#249132=CARTESIAN_POINT('Ctrl Pts',(13.4899084877718,21.0960904575048,0.));
#249133=CARTESIAN_POINT('Ctrl Pts',(13.4899084877718,21.0960904575048,12.));
#249134=CARTESIAN_POINT('Ctrl Pts',(13.4868282377191,21.0706662455202,0.));
#249135=CARTESIAN_POINT('Ctrl Pts',(13.4868282377191,21.0706662455202,12.));
#249136=CARTESIAN_POINT('Ctrl Pts',(13.4836976858912,21.0453281134247,0.));
#249137=CARTESIAN_POINT('Ctrl Pts',(13.4836976858912,21.0453281134247,12.));
#249138=CARTESIAN_POINT('Ctrl Pts',(13.4805171556822,21.0200765158885,0.));
#249139=CARTESIAN_POINT('Ctrl Pts',(13.4805171556822,21.0200765158885,12.));
#249140=CARTESIAN_POINT('Ctrl Pts',(13.4772869738879,20.9949119102592,0.));
#249141=CARTESIAN_POINT('Ctrl Pts',(13.4772869738879,20.9949119102592,12.));
#249142=CARTESIAN_POINT('Ctrl Pts',(13.4740074710087,20.9698347569476,0.));
#249143=CARTESIAN_POINT('Ctrl Pts',(13.4740074710087,20.9698347569476,12.));
#249144=CARTESIAN_POINT('Ctrl Pts',(13.4706789815166,20.9448455197557,0.));
#249145=CARTESIAN_POINT('Ctrl Pts',(13.4706789815166,20.9448455197557,12.));
#249146=CARTESIAN_POINT('Ctrl Pts',(13.4673018437718,20.9199446657584,0.));
#249147=CARTESIAN_POINT('Ctrl Pts',(13.4673018437718,20.9199446657584,12.));
#249148=CARTESIAN_POINT('Ctrl Pts',(13.4638763999725,20.8951326652158,0.));
#249149=CARTESIAN_POINT('Ctrl Pts',(13.4638763999725,20.8951326652158,12.));
#249150=CARTESIAN_POINT('Ctrl Pts',(13.4604029960983,20.8704099914641,0.));
#249151=CARTESIAN_POINT('Ctrl Pts',(13.4604029960983,20.8704099914641,12.));
#249152=CARTESIAN_POINT('Ctrl Pts',(13.4568819818631,20.8457771208082,0.));
#249153=CARTESIAN_POINT('Ctrl Pts',(13.4568819818631,20.8457771208082,12.));
#249154=CARTESIAN_POINT('Ctrl Pts',(13.4533137106667,20.821234532398,0.));
#249155=CARTESIAN_POINT('Ctrl Pts',(13.4533137106667,20.821234532398,12.));
#249156=CARTESIAN_POINT('Ctrl Pts',(13.4496985395637,20.7967827081227,0.));
#249157=CARTESIAN_POINT('Ctrl Pts',(13.4496985395637,20.7967827081227,12.));
#249158=CARTESIAN_POINT('Ctrl Pts',(13.4460368293688,20.7724221327608,0.));
#249159=CARTESIAN_POINT('Ctrl Pts',(13.4460368293688,20.7724221327608,12.));
#249160=CARTESIAN_POINT('Ctrl Pts',(13.4423289447561,20.7481532941013,0.));
#249161=CARTESIAN_POINT('Ctrl Pts',(13.4423289447561,20.7481532941013,12.));
#249162=CARTESIAN_POINT('Ctrl Pts',(13.4385752543663,20.7239766830675,0.));
#249163=CARTESIAN_POINT('Ctrl Pts',(13.4385752543663,20.7239766830675,12.));
#249164=CARTESIAN_POINT('Ctrl Pts',(13.4347761309154,20.6998927938288,0.));
#249165=CARTESIAN_POINT('Ctrl Pts',(13.4347761309154,20.6998927938288,12.));
#249166=CARTESIAN_POINT('Ctrl Pts',(13.4309319513119,20.6759021239103,0.));
#249167=CARTESIAN_POINT('Ctrl Pts',(13.4309319513119,20.6759021239103,12.));
#249168=CARTESIAN_POINT('Ctrl Pts',(13.4270430967651,20.6520051742869,0.));
#249169=CARTESIAN_POINT('Ctrl Pts',(13.4270430967651,20.6520051742869,12.));
#249170=CARTESIAN_POINT('Ctrl Pts',(13.4231099528179,20.6282024494237,0.));
#249171=CARTESIAN_POINT('Ctrl Pts',(13.4231099528179,20.6282024494237,12.));
#249172=CARTESIAN_POINT('Ctrl Pts',(13.4191329093932,20.6044944573153,0.));
#249173=CARTESIAN_POINT('Ctrl Pts',(13.4191329093932,20.6044944573153,12.));
#249174=CARTESIAN_POINT('Ctrl Pts',(13.4151123608411,20.5808817095155,0.));
#249175=CARTESIAN_POINT('Ctrl Pts',(13.4151123608411,20.5808817095155,12.));
#249176=CARTESIAN_POINT('Ctrl Pts',(13.4110487059912,20.5573647211639,0.));
#249177=CARTESIAN_POINT('Ctrl Pts',(13.4110487059912,20.5573647211639,12.));
#249178=CARTESIAN_POINT('Ctrl Pts',(13.4069423482076,20.5339440109956,0.));
#249179=CARTESIAN_POINT('Ctrl Pts',(13.4069423482076,20.5339440109956,12.));
#249180=CARTESIAN_POINT('Ctrl Pts',(13.4027936954529,20.5106201013753,0.));
#249181=CARTESIAN_POINT('Ctrl Pts',(13.4027936954529,20.5106201013753,12.));
#249182=CARTESIAN_POINT('Ctrl Pts',(13.3986031603716,20.487393518404,0.));
#249183=CARTESIAN_POINT('Ctrl Pts',(13.3986031603716,20.487393518404,12.));
#249184=CARTESIAN_POINT('Ctrl Pts',(13.3943711603739,20.4642647920038,0.));
#249185=CARTESIAN_POINT('Ctrl Pts',(13.3943711603739,20.4642647920038,12.));
#249186=CARTESIAN_POINT('Ctrl Pts',(13.3900981177255,20.4412344560008,0.));
#249187=CARTESIAN_POINT('Ctrl Pts',(13.3900981177255,20.4412344560008,12.));
#249188=CARTESIAN_POINT('Ctrl Pts',(13.3857844596387,20.4183030482002,0.));
#249189=CARTESIAN_POINT('Ctrl Pts',(13.3857844596387,20.4183030482002,12.));
#249190=CARTESIAN_POINT('Ctrl Pts',(13.3814306183719,20.3954711104502,0.));
#249191=CARTESIAN_POINT('Ctrl Pts',(13.3814306183719,20.3954711104502,12.));
#249192=CARTESIAN_POINT('Ctrl Pts',(13.3770370313188,20.3727391887184,0.));
#249193=CARTESIAN_POINT('Ctrl Pts',(13.3770370313188,20.3727391887184,12.));
#249194=CARTESIAN_POINT('Ctrl Pts',(13.3726041410867,20.3501078331814,0.));
#249195=CARTESIAN_POINT('Ctrl Pts',(13.3726041410867,20.3501078331814,12.));
#249196=CARTESIAN_POINT('Ctrl Pts',(13.3681323955826,20.3275775983029,0.));
#249197=CARTESIAN_POINT('Ctrl Pts',(13.3681323955826,20.3275775983029,12.));
#249198=CARTESIAN_POINT('Ctrl Pts',(13.3636222481016,20.3051490429048,0.));
#249199=CARTESIAN_POINT('Ctrl Pts',(13.3636222481016,20.3051490429048,12.));
#249200=CARTESIAN_POINT('Ctrl Pts',(13.3590741574195,20.2828227302339,0.));
#249201=CARTESIAN_POINT('Ctrl Pts',(13.3590741574195,20.2828227302339,12.));
#249202=CARTESIAN_POINT('Ctrl Pts',(13.3544885878889,20.2605992280122,0.));
#249203=CARTESIAN_POINT('Ctrl Pts',(13.3544885878889,20.2605992280122,12.));
#249204=CARTESIAN_POINT('Ctrl Pts',(13.3498660095386,20.2384791085359,0.));
#249205=CARTESIAN_POINT('Ctrl Pts',(13.3498660095386,20.2384791085359,12.));
#249206=CARTESIAN_POINT('Ctrl Pts',(13.3452068981766,20.216462948786,0.));
#249207=CARTESIAN_POINT('Ctrl Pts',(13.3452068981766,20.216462948786,12.));
#249208=CARTESIAN_POINT('Ctrl Pts',(13.3405117354971,20.1945513305235,0.));
#249209=CARTESIAN_POINT('Ctrl Pts',(13.3405117354971,20.1945513305235,12.));
#249210=CARTESIAN_POINT('Ctrl Pts',(13.3357810091903,20.1727448403817,0.));
#249211=CARTESIAN_POINT('Ctrl Pts',(13.3357810091903,20.1727448403817,12.));
#249212=CARTESIAN_POINT('Ctrl Pts',(13.3310152130564,20.1510440699474,0.));
#249213=CARTESIAN_POINT('Ctrl Pts',(13.3310152130564,20.1510440699474,12.));
#249214=CARTESIAN_POINT('Ctrl Pts',(13.3262148471226,20.1294496158402,0.));
#249215=CARTESIAN_POINT('Ctrl Pts',(13.3262148471226,20.1294496158402,12.));
#249216=CARTESIAN_POINT('Ctrl Pts',(13.3213804177587,20.1079620798375,0.));
#249217=CARTESIAN_POINT('Ctrl Pts',(13.3213804177587,20.1079620798375,12.));
#249218=CARTESIAN_POINT('Ctrl Pts',(13.3165124377962,20.0865820689883,0.));
#249219=CARTESIAN_POINT('Ctrl Pts',(13.3165124377962,20.0865820689883,12.));
#249220=CARTESIAN_POINT('Ctrl Pts',(13.3116114266515,20.0653101957188,0.));
#249221=CARTESIAN_POINT('Ctrl Pts',(13.3116114266515,20.0653101957188,12.));
#249222=CARTESIAN_POINT('Ctrl Pts',(13.3066779104515,20.0441470779345,0.));
#249223=CARTESIAN_POINT('Ctrl Pts',(13.3066779104515,20.0441470779345,12.));
#249224=CARTESIAN_POINT('Ctrl Pts',(13.3017124221637,20.0230933391038,0.));
#249225=CARTESIAN_POINT('Ctrl Pts',(13.3017124221637,20.0230933391038,12.));
#249226=CARTESIAN_POINT('Ctrl Pts',(13.2967155017306,20.0021496083738,0.));
#249227=CARTESIAN_POINT('Ctrl Pts',(13.2967155017306,20.0021496083738,12.));
#249228=CARTESIAN_POINT('Ctrl Pts',(13.2916876962094,19.981316520717,0.));
#249229=CARTESIAN_POINT('Ctrl Pts',(13.2916876962094,19.981316520717,12.));
#249230=CARTESIAN_POINT('Ctrl Pts',(13.286629559915,19.9605947170586,0.));
#249231=CARTESIAN_POINT('Ctrl Pts',(13.286629559915,19.9605947170586,12.));
#249232=CARTESIAN_POINT('Ctrl Pts',(13.2815416545663,19.9399848444019,0.));
#249233=CARTESIAN_POINT('Ctrl Pts',(13.2815416545663,19.9399848444019,12.));
#249234=CARTESIAN_POINT('Ctrl Pts',(13.2764245494357,19.9194875559422,0.));
#249235=CARTESIAN_POINT('Ctrl Pts',(13.2764245494357,19.9194875559422,12.));
#249236=CARTESIAN_POINT('Ctrl Pts',(13.271278821502,19.8991035111745,0.));
#249237=CARTESIAN_POINT('Ctrl Pts',(13.271278821502,19.8991035111745,12.));
#249238=CARTESIAN_POINT('Ctrl Pts',(13.2661050556132,19.8788333760577,0.));
#249239=CARTESIAN_POINT('Ctrl Pts',(13.2661050556132,19.8788333760577,12.));
#249240=CARTESIAN_POINT('Ctrl Pts',(13.2609038446529,19.8586778231715,0.));
#249241=CARTESIAN_POINT('Ctrl Pts',(13.2609038446529,19.8586778231715,12.));
#249242=CARTESIAN_POINT('Ctrl Pts',(13.2556757897086,19.8386375318634,0.));
#249243=CARTESIAN_POINT('Ctrl Pts',(13.2556757897086,19.8386375318634,12.));
#249244=CARTESIAN_POINT('Ctrl Pts',(13.2504215002457,19.8187131883917,0.));
#249245=CARTESIAN_POINT('Ctrl Pts',(13.2504215002457,19.8187131883917,12.));
#249246=CARTESIAN_POINT('Ctrl Pts',(13.2451415942805,19.7989054860495,0.));
#249247=CARTESIAN_POINT('Ctrl Pts',(13.2451415942805,19.7989054860495,12.));
#249248=CARTESIAN_POINT('Ctrl Pts',(13.2398366985675,19.7792151253289,0.));
#249249=CARTESIAN_POINT('Ctrl Pts',(13.2398366985675,19.7792151253289,12.));
#249250=CARTESIAN_POINT('Ctrl Pts',(13.2345074487963,19.7596428141168,0.));
#249251=CARTESIAN_POINT('Ctrl Pts',(13.2345074487963,19.7596428141168,12.));
#249252=CARTESIAN_POINT('Ctrl Pts',(13.2291544897899,19.7401892678697,0.));
#249253=CARTESIAN_POINT('Ctrl Pts',(13.2291544897899,19.7401892678697,12.));
#249254=CARTESIAN_POINT('Ctrl Pts',(13.2237784757065,19.7208552097868,0.));
#249255=CARTESIAN_POINT('Ctrl Pts',(13.2237784757065,19.7208552097868,12.));
#249256=CARTESIAN_POINT('Ctrl Pts',(13.2183800702436,19.7016413709685,0.));
#249257=CARTESIAN_POINT('Ctrl Pts',(13.2183800702436,19.7016413709685,12.));
#249258=CARTESIAN_POINT('Ctrl Pts',(13.2129599468485,19.6825484905823,0.));
#249259=CARTESIAN_POINT('Ctrl Pts',(13.2129599468485,19.6825484905823,12.));
#249260=CARTESIAN_POINT('Ctrl Pts',(13.2075187889529,19.6635773160936,0.));
#249261=CARTESIAN_POINT('Ctrl Pts',(13.2075187889529,19.6635773160936,12.));
#249262=CARTESIAN_POINT('Ctrl Pts',(13.2020572902065,19.6447286034772,0.));
#249263=CARTESIAN_POINT('Ctrl Pts',(13.2020572902065,19.6447286034772,12.));
#249264=CARTESIAN_POINT('Ctrl Pts',(13.1965761547151,19.6260031174244,0.));
#249265=CARTESIAN_POINT('Ctrl Pts',(13.1965761547151,19.6260031174244,12.));
#249266=CARTESIAN_POINT('Ctrl Pts',(13.1910760972814,19.6074016315414,0.));
#249267=CARTESIAN_POINT('Ctrl Pts',(13.1910760972814,19.6074016315414,12.));
#249268=CARTESIAN_POINT('Ctrl Pts',(13.1855578436471,19.5889249285338,0.));
#249269=CARTESIAN_POINT('Ctrl Pts',(13.1855578436471,19.5889249285338,12.));
#249270=CARTESIAN_POINT('Ctrl Pts',(13.1800221307673,19.5705738004667,0.));
#249271=CARTESIAN_POINT('Ctrl Pts',(13.1800221307673,19.5705738004667,12.));
#249272=CARTESIAN_POINT('Ctrl Pts',(13.1744697070911,19.5523490490244,0.));
#249273=CARTESIAN_POINT('Ctrl Pts',(13.1744697070911,19.5523490490244,12.));
#249274=CARTESIAN_POINT('Ctrl Pts',(13.168901332843,19.5342514857562,0.));
#249275=CARTESIAN_POINT('Ctrl Pts',(13.168901332843,19.5342514857562,12.));
#249276=CARTESIAN_POINT('Ctrl Pts',(13.1633177803101,19.5162819323213,0.));
#249277=CARTESIAN_POINT('Ctrl Pts',(13.1633177803101,19.5162819323213,12.));
#249278=CARTESIAN_POINT('Ctrl Pts',(13.1577198341245,19.4984412207082,0.));
#249279=CARTESIAN_POINT('Ctrl Pts',(13.1577198341245,19.4984412207082,12.));
#249280=CARTESIAN_POINT('Ctrl Pts',(13.1521082915853,19.4807301935268,0.));
#249281=CARTESIAN_POINT('Ctrl Pts',(13.1521082915853,19.4807301935268,12.));
#249282=CARTESIAN_POINT('Ctrl Pts',(13.1464839629971,19.4631497043258,0.));
#249283=CARTESIAN_POINT('Ctrl Pts',(13.1464839629971,19.4631497043258,12.));
#249284=CARTESIAN_POINT('Ctrl Pts',(13.1408476720061,19.4457006178876,0.));
#249285=CARTESIAN_POINT('Ctrl Pts',(13.1408476720061,19.4457006178876,12.));
#249286=CARTESIAN_POINT('Ctrl Pts',(13.1352002559438,19.4283838105262,0.));
#249287=CARTESIAN_POINT('Ctrl Pts',(13.1352002559438,19.4283838105262,12.));
#249288=CARTESIAN_POINT('Ctrl Pts',(13.1295425661634,19.4112001703557,0.));
#249289=CARTESIAN_POINT('Ctrl Pts',(13.1295425661634,19.4112001703557,12.));
#249290=CARTESIAN_POINT('Ctrl Pts',(13.1238754684177,19.3941505976263,0.));
#249291=CARTESIAN_POINT('Ctrl Pts',(13.1238754684177,19.3941505976263,12.));
#249292=CARTESIAN_POINT('Ctrl Pts',(13.118199843271,19.3772360051091,0.));
#249293=CARTESIAN_POINT('Ctrl Pts',(13.118199843271,19.3772360051091,12.));
#249294=CARTESIAN_POINT('Ctrl Pts',(13.1125165865022,19.3604573184515,0.));
#249295=CARTESIAN_POINT('Ctrl Pts',(13.1125165865022,19.3604573184515,12.));
#249296=CARTESIAN_POINT('Ctrl Pts',(13.1068266095186,19.3438154765395,0.));
#249297=CARTESIAN_POINT('Ctrl Pts',(13.1068266095186,19.3438154765395,12.));
#249298=CARTESIAN_POINT('Ctrl Pts',(13.1011308397591,19.3273114318269,0.));
#249299=CARTESIAN_POINT('Ctrl Pts',(13.1011308397591,19.3273114318269,12.));
#249300=CARTESIAN_POINT('Ctrl Pts',(13.0954302211479,19.310946150736,0.));
#249301=CARTESIAN_POINT('Ctrl Pts',(13.0954302211479,19.310946150736,12.));
#249302=CARTESIAN_POINT('Ctrl Pts',(13.0897257145968,19.2947206141247,0.));
#249303=CARTESIAN_POINT('Ctrl Pts',(13.0897257145968,19.2947206141247,12.));
#249304=CARTESIAN_POINT('Ctrl Pts',(13.0840182984949,19.2786358177198,0.));
#249305=CARTESIAN_POINT('Ctrl Pts',(13.0840182984949,19.2786358177198,12.));
#249306=CARTESIAN_POINT('Ctrl Pts',(13.0783089692118,19.2626927725596,0.));
#249307=CARTESIAN_POINT('Ctrl Pts',(13.0783089692118,19.2626927725596,12.));
#249308=CARTESIAN_POINT('Ctrl Pts',(13.0725987415859,19.2468925053989,0.));
#249309=CARTESIAN_POINT('Ctrl Pts',(13.0725987415859,19.2468925053989,12.));
#249310=CARTESIAN_POINT('Ctrl Pts',(13.0668886494795,19.2312360592033,0.));
#249311=CARTESIAN_POINT('Ctrl Pts',(13.0668886494795,19.2312360592033,12.));
#249312=CARTESIAN_POINT('Ctrl Pts',(13.0611797463915,19.2157244937142,0.));
#249313=CARTESIAN_POINT('Ctrl Pts',(13.0611797463915,19.2157244937142,12.));
#249314=CARTESIAN_POINT('Ctrl Pts',(13.0554731060538,19.2003588859772,0.));
#249315=CARTESIAN_POINT('Ctrl Pts',(13.0554731060538,19.2003588859772,12.));
#249316=CARTESIAN_POINT('Ctrl Pts',(13.0497698230441,19.1851403308825,0.));
#249317=CARTESIAN_POINT('Ctrl Pts',(13.0497698230441,19.1851403308825,12.));
#249318=CARTESIAN_POINT('Ctrl Pts',(13.0440710133772,19.1700699416622,0.));
#249319=CARTESIAN_POINT('Ctrl Pts',(13.0440710133772,19.1700699416622,12.));
#249320=CARTESIAN_POINT('Ctrl Pts',(13.0383778152068,19.155148850523,0.));
#249321=CARTESIAN_POINT('Ctrl Pts',(13.0383778152068,19.155148850523,12.));
#249322=CARTESIAN_POINT('Ctrl Pts',(13.0326913895838,19.1403782093386,0.));
#249323=CARTESIAN_POINT('Ctrl Pts',(13.0326913895838,19.1403782093386,12.));
#249324=CARTESIAN_POINT('Ctrl Pts',(13.0270129211976,19.1257591903099,0.));
#249325=CARTESIAN_POINT('Ctrl Pts',(13.0270129211976,19.1257591903099,12.));
#249326=CARTESIAN_POINT('Ctrl Pts',(13.0213436191328,19.111292986631,0.));
#249327=CARTESIAN_POINT('Ctrl Pts',(13.0213436191328,19.111292986631,12.));
#249328=CARTESIAN_POINT('Ctrl Pts',(13.0156847176096,19.0969808131228,0.));
#249329=CARTESIAN_POINT('Ctrl Pts',(13.0156847176096,19.0969808131228,12.));
#249330=CARTESIAN_POINT('Ctrl Pts',(13.0100374768788,19.0828239070484,0.));
#249331=CARTESIAN_POINT('Ctrl Pts',(13.0100374768788,19.0828239070484,12.));
#249332=CARTESIAN_POINT('Ctrl Pts',(13.0044031841382,19.0688235289437,0.));
#249333=CARTESIAN_POINT('Ctrl Pts',(13.0044031841382,19.0688235289437,12.));
#249334=CARTESIAN_POINT('Ctrl Pts',(12.9987831544502,19.0549809634354,0.));
#249335=CARTESIAN_POINT('Ctrl Pts',(12.9987831544502,19.0549809634354,12.));
#249336=CARTESIAN_POINT('Ctrl Pts',(12.9931787316514,19.0412975200398,0.));
#249337=CARTESIAN_POINT('Ctrl Pts',(12.9931787316514,19.0412975200398,12.));
#249338=CARTESIAN_POINT('Ctrl Pts',(12.9875912893003,19.0277745339909,0.));
#249339=CARTESIAN_POINT('Ctrl Pts',(12.9875912893003,19.0277745339909,12.));
#249340=CARTESIAN_POINT('Ctrl Pts',(12.9820222318716,19.014413367335,0.));
#249341=CARTESIAN_POINT('Ctrl Pts',(12.9820222318716,19.014413367335,12.));
#249342=CARTESIAN_POINT('Ctrl Pts',(12.9764729959206,19.0012154099792,0.));
#249343=CARTESIAN_POINT('Ctrl Pts',(12.9764729959206,19.0012154099792,12.));
#249344=CARTESIAN_POINT('Ctrl Pts',(12.9709450512747,18.9881820807585,0.));
#249345=CARTESIAN_POINT('Ctrl Pts',(12.9709450512747,18.9881820807585,12.));
#249346=CARTESIAN_POINT('Ctrl Pts',(12.9654399021868,18.9753148284473,0.));
#249347=CARTESIAN_POINT('Ctrl Pts',(12.9654399021868,18.9753148284473,12.));
#249348=CARTESIAN_POINT('Ctrl Pts',(12.9599590886317,18.9626151329226,0.));
#249349=CARTESIAN_POINT('Ctrl Pts',(12.9599590886317,18.9626151329226,12.));
#249350=CARTESIAN_POINT('Ctrl Pts',(12.9545041877377,18.9500845064714,0.));
#249351=CARTESIAN_POINT('Ctrl Pts',(12.9545041877377,18.9500845064714,12.));
#249352=CARTESIAN_POINT('Ctrl Pts',(12.9490768151821,18.9377244950435,0.));
#249353=CARTESIAN_POINT('Ctrl Pts',(12.9490768151821,18.9377244950435,12.));
#249354=CARTESIAN_POINT('Ctrl Pts',(12.9436786266106,18.9255366795196,0.));
#249355=CARTESIAN_POINT('Ctrl Pts',(12.9436786266106,18.9255366795196,12.));
#249356=CARTESIAN_POINT('Ctrl Pts',(12.9383113190375,18.9135226769466,0.));
#249357=CARTESIAN_POINT('Ctrl Pts',(12.9383113190375,18.9135226769466,12.));
#249358=CARTESIAN_POINT('Ctrl Pts',(12.9329766328184,18.9016841423402,0.));
#249359=CARTESIAN_POINT('Ctrl Pts',(12.9329766328184,18.9016841423402,12.));
#249360=CARTESIAN_POINT('Ctrl Pts',(12.9276763536372,18.8900227704888,0.));
#249361=CARTESIAN_POINT('Ctrl Pts',(12.9276763536372,18.8900227704888,12.));
#249362=CARTESIAN_POINT('Ctrl Pts',(12.9224123144982,18.8785402977528,0.));
#249363=CARTESIAN_POINT('Ctrl Pts',(12.9224123144982,18.8785402977528,12.));
#249364=CARTESIAN_POINT('Ctrl Pts',(12.9171863977047,18.8672385038328,0.));
#249365=CARTESIAN_POINT('Ctrl Pts',(12.9171863977047,18.8672385038328,12.));
#249366=CARTESIAN_POINT('Ctrl Pts',(12.9120005369066,18.8561192136201,0.));
#249367=CARTESIAN_POINT('Ctrl Pts',(12.9120005369066,18.8561192136201,12.));
#249368=CARTESIAN_POINT('Ctrl Pts',(12.9068567191856,18.8451842990986,0.));
#249369=CARTESIAN_POINT('Ctrl Pts',(12.9068567191856,18.8451842990986,12.));
#249370=CARTESIAN_POINT('Ctrl Pts',(12.9017569871738,18.834435681259,0.));
#249371=CARTESIAN_POINT('Ctrl Pts',(12.9017569871738,18.834435681259,12.));
#249372=CARTESIAN_POINT('Ctrl Pts',(12.8967034410752,18.8238753319124,0.));
#249373=CARTESIAN_POINT('Ctrl Pts',(12.8967034410752,18.8238753319124,12.));
#249374=CARTESIAN_POINT('Ctrl Pts',(12.8916982409931,18.8135052757815,0.));
#249375=CARTESIAN_POINT('Ctrl Pts',(12.8916982409931,18.8135052757815,12.));
#249376=CARTESIAN_POINT('Ctrl Pts',(12.8867436109543,18.8033275941939,0.));
#249377=CARTESIAN_POINT('Ctrl Pts',(12.8867436109543,18.8033275941939,12.));
#249378=CARTESIAN_POINT('Ctrl Pts',(12.8818418427474,18.7933444285867,0.));
#249379=CARTESIAN_POINT('Ctrl Pts',(12.8818418427474,18.7933444285867,12.));
#249380=CARTESIAN_POINT('Ctrl Pts',(12.8769952998097,18.7835579840481,0.));
#249381=CARTESIAN_POINT('Ctrl Pts',(12.8769952998097,18.7835579840481,12.));
#249382=CARTESIAN_POINT('Ctrl Pts',(12.8722064211814,18.7739705329029,0.));
#249383=CARTESIAN_POINT('Ctrl Pts',(12.8722064211814,18.7739705329029,12.));
#249384=CARTESIAN_POINT('Ctrl Pts',(12.8674777239656,18.7645844169568,0.));
#249385=CARTESIAN_POINT('Ctrl Pts',(12.8674777239656,18.7645844169568,12.));
#249386=CARTESIAN_POINT('Ctrl Pts',(12.8628118054172,18.7554020493888,0.));
#249387=CARTESIAN_POINT('Ctrl Pts',(12.8628118054172,18.7554020493888,12.));
#249388=CARTESIAN_POINT('Ctrl Pts',(12.8582113455644,18.7464259171248,0.));
#249389=CARTESIAN_POINT('Ctrl Pts',(12.8582113455644,18.7464259171248,12.));
#249390=CARTESIAN_POINT('Ctrl Pts',(12.8536791086315,18.7376585820851,0.));
#249391=CARTESIAN_POINT('Ctrl Pts',(12.8536791086315,18.7376585820851,12.));
#249392=CARTESIAN_POINT('Ctrl Pts',(12.849217951159,18.7291026886552,0.));
#249393=CARTESIAN_POINT('Ctrl Pts',(12.849217951159,18.7291026886552,12.));
#249394=CARTESIAN_POINT('Ctrl Pts',(12.8448308329494,18.7207609737701,0.));
#249395=CARTESIAN_POINT('Ctrl Pts',(12.8448308329494,18.7207609737701,12.));
#249396=CARTESIAN_POINT('Ctrl Pts',(12.8405208263432,18.7126362754446,0.));
#249397=CARTESIAN_POINT('Ctrl Pts',(12.8405208263432,18.7126362754446,12.));
#249398=CARTESIAN_POINT('Ctrl Pts',(12.8362911280362,18.7047315436296,0.));
#249399=CARTESIAN_POINT('Ctrl Pts',(12.8362911280362,18.7047315436296,12.));
#249400=CARTESIAN_POINT('Ctrl Pts',(12.832145059979,18.6970498410173,0.));
#249401=CARTESIAN_POINT('Ctrl Pts',(12.832145059979,18.6970498410173,12.));
#249402=CARTESIAN_POINT('Ctrl Pts',(12.8280860635231,18.6895943376172,0.));
#249403=CARTESIAN_POINT('Ctrl Pts',(12.8280860635231,18.6895943376172,12.));
#249404=CARTESIAN_POINT('Ctrl Pts',(12.8241176980016,18.6823683094139,0.));
#249405=CARTESIAN_POINT('Ctrl Pts',(12.8241176980016,18.6823683094139,12.));
#249406=CARTESIAN_POINT('Ctrl Pts',(12.8202436318473,18.6753751301091,0.));
#249407=CARTESIAN_POINT('Ctrl Pts',(12.8202436318473,18.6753751301091,12.));
#249408=CARTESIAN_POINT('Ctrl Pts',(12.8164676687361,18.6686182952798,0.));
#249409=CARTESIAN_POINT('Ctrl Pts',(12.8164676687361,18.6686182952798,12.));
#249410=CARTESIAN_POINT('Ctrl Pts',(12.8127937909632,18.6621014624746,0.));
#249411=CARTESIAN_POINT('Ctrl Pts',(12.8127937909632,18.6621014624746,12.));
#249412=CARTESIAN_POINT('Ctrl Pts',(12.8092261933858,18.6558284825772,0.));
#249413=CARTESIAN_POINT('Ctrl Pts',(12.8092261933858,18.6558284825772,12.));
#249414=CARTESIAN_POINT('Ctrl Pts',(12.805769331162,18.6498034438986,0.));
#249415=CARTESIAN_POINT('Ctrl Pts',(12.805769331162,18.6498034438986,12.));
#249416=CARTESIAN_POINT('Ctrl Pts',(12.8024278770153,18.6440306327457,0.));
#249417=CARTESIAN_POINT('Ctrl Pts',(12.8024278770153,18.6440306327457,12.));
#249418=CARTESIAN_POINT('Ctrl Pts',(12.7992066625264,18.63851447924,0.));
#249419=CARTESIAN_POINT('Ctrl Pts',(12.7992066625264,18.63851447924,12.));
#249420=CARTESIAN_POINT('Ctrl Pts',(12.7961106222251,18.6332595057005,0.));
#249421=CARTESIAN_POINT('Ctrl Pts',(12.7961106222251,18.6332595057005,12.));
#249422=CARTESIAN_POINT('Ctrl Pts',(12.7931447451556,18.6282702819371,0.));
#249423=CARTESIAN_POINT('Ctrl Pts',(12.7931447451556,18.6282702819371,12.));
#249424=CARTESIAN_POINT('Ctrl Pts',(12.7903142925234,18.6235516265575,0.));
#249425=CARTESIAN_POINT('Ctrl Pts',(12.7903142925234,18.6235516265575,12.));
#249426=CARTESIAN_POINT('Ctrl Pts',(12.7876249657834,18.6191087624752,0.));
#249427=CARTESIAN_POINT('Ctrl Pts',(12.7876249657834,18.6191087624752,12.));
#249428=CARTESIAN_POINT('Ctrl Pts',(12.78508316579,18.6149475565189,0.));
#249429=CARTESIAN_POINT('Ctrl Pts',(12.78508316579,18.6149475565189,12.));
#249430=CARTESIAN_POINT('Ctrl Pts',(12.7826959526924,18.611074482622,0.));
#249431=CARTESIAN_POINT('Ctrl Pts',(12.7826959526924,18.611074482622,12.));
#249432=CARTESIAN_POINT('Ctrl Pts',(12.7804705387658,18.6074961535723,0.));
#249433=CARTESIAN_POINT('Ctrl Pts',(12.7804705387658,18.6074961535723,12.));
#249434=CARTESIAN_POINT('Ctrl Pts',(12.7784139605067,18.6042190183703,0.));
#249435=CARTESIAN_POINT('Ctrl Pts',(12.7784139605067,18.6042190183703,12.));
#249436=CARTESIAN_POINT('Ctrl Pts',(12.7765325225082,18.6012488486708,0.));
#249437=CARTESIAN_POINT('Ctrl Pts',(12.7765325225082,18.6012488486708,12.));
#249438=CARTESIAN_POINT('Ctrl Pts',(12.7748328937639,18.5985917525949,0.));
#249439=CARTESIAN_POINT('Ctrl Pts',(12.7748328937639,18.5985917525949,12.));
#249440=CARTESIAN_POINT('Ctrl Pts',(12.7733231262107,18.5962551167772,0.));
#249441=CARTESIAN_POINT('Ctrl Pts',(12.7733231262107,18.5962551167772,12.));
#249442=CARTESIAN_POINT('Ctrl Pts',(12.7720142287169,18.5942490615409,0.));
#249443=CARTESIAN_POINT('Ctrl Pts',(12.7720142287169,18.5942490615409,12.));
#249444=CARTESIAN_POINT('Ctrl Pts',(12.7709195951153,18.5925859134582,0.));
#249445=CARTESIAN_POINT('Ctrl Pts',(12.7709195951153,18.5925859134582,12.));
#249446=CARTESIAN_POINT('Ctrl Pts',(12.7700520897174,18.5912775137806,0.));
#249447=CARTESIAN_POINT('Ctrl Pts',(12.7700520897174,18.5912775137806,12.));
#249448=CARTESIAN_POINT('Ctrl Pts',(12.7694215127923,18.590332877722,0.));
#249449=CARTESIAN_POINT('Ctrl Pts',(12.7694215127923,18.590332877722,12.));
#249450=CARTESIAN_POINT('Ctrl Pts',(12.7691103481996,18.589871621842,0.));
#249451=CARTESIAN_POINT('Ctrl Pts',(12.7691103481996,18.589871621842,12.));
#249452=CARTESIAN_POINT('Ctrl Pts',(12.7689864266924,18.5896919669158,0.));
#249453=CARTESIAN_POINT('Ctrl Pts',(12.7689864266924,18.5896919669158,12.));
#249454=CARTESIAN_POINT('Ctrl Pts',(12.7689524524484,18.5896460962961,0.));
#249455=CARTESIAN_POINT('Ctrl Pts',(12.7689524524484,18.5896460962961,12.));
#249456=CARTESIAN_POINT('Ctrl Pts',(12.7689476255363,18.5896416359912,0.));
#249457=CARTESIAN_POINT('Ctrl Pts',(12.7689476255363,18.5896416359912,12.));
#249458=CARTESIAN_POINT('',(13.5685075571671,22.1787195904339,0.));
#249459=CARTESIAN_POINT('Ctrl Pts',(13.5685075571671,22.1787195904339,0.));
#249460=CARTESIAN_POINT('Ctrl Pts',(13.5683460612913,22.1730081264583,0.));
#249461=CARTESIAN_POINT('Ctrl Pts',(13.5680170531724,22.1615922804939,0.));
#249462=CARTESIAN_POINT('Ctrl Pts',(13.5675054918922,22.1444897575076,0.));
#249463=CARTESIAN_POINT('Ctrl Pts',(13.5667873105179,22.1217288871823,0.));
#249464=CARTESIAN_POINT('Ctrl Pts',(13.5658294169106,22.0933486464442,0.));
#249465=CARTESIAN_POINT('Ctrl Pts',(13.5648113688894,22.0650393089492,0.));
#249466=CARTESIAN_POINT('Ctrl Pts',(13.5637332022393,22.0368009736227,0.));
#249467=CARTESIAN_POINT('Ctrl Pts',(13.5625949868313,22.0086337943431,0.));
#249468=CARTESIAN_POINT('Ctrl Pts',(13.5613968357589,21.9805379899192,0.));
#249469=CARTESIAN_POINT('Ctrl Pts',(13.5601389185315,21.9525138592862,0.));
#249470=CARTESIAN_POINT('Ctrl Pts',(13.5588214586672,21.9245617765827,0.));
#249471=CARTESIAN_POINT('Ctrl Pts',(13.5574447178484,21.8966821688876,0.));
#249472=CARTESIAN_POINT('Ctrl Pts',(13.5560089839426,21.8688754989401,0.));
#249473=CARTESIAN_POINT('Ctrl Pts',(13.5545145573048,21.841142245609,0.));
#249474=CARTESIAN_POINT('Ctrl Pts',(13.5529617381569,21.8134828857963,0.));
#249475=CARTESIAN_POINT('Ctrl Pts',(13.5513508127232,21.7858978745848,0.));
#249476=CARTESIAN_POINT('Ctrl Pts',(13.5496820422186,21.7583876294532,0.));
#249477=CARTESIAN_POINT('Ctrl Pts',(13.5479556704457,21.730952541226,0.));
#249478=CARTESIAN_POINT('Ctrl Pts',(13.546171929503,21.7035929822939,0.));
#249479=CARTESIAN_POINT('Ctrl Pts',(13.5443310461516,21.676309315769,0.));
#249480=CARTESIAN_POINT('Ctrl Pts',(13.5424332480698,21.6491019044647,0.));
#249481=CARTESIAN_POINT('Ctrl Pts',(13.5404787697798,21.6219711193951,0.));
#249482=CARTESIAN_POINT('Ctrl Pts',(13.5384678597206,21.5949173499022,0.));
#249483=CARTESIAN_POINT('Ctrl Pts',(13.5364007790292,21.5679410019011,0.));
#249484=CARTESIAN_POINT('Ctrl Pts',(13.5342777983225,21.5410424932511,0.));
#249485=CARTESIAN_POINT('Ctrl Pts',(13.5320991952145,21.5142222501671,0.));
#249486=CARTESIAN_POINT('Ctrl Pts',(13.5298652514357,21.487480703047,0.));
#249487=CARTESIAN_POINT('Ctrl Pts',(13.5275762503553,21.4608182828695,0.));
#249488=CARTESIAN_POINT('Ctrl Pts',(13.5252324737795,21.4342354165254,0.));
#249489=CARTESIAN_POINT('Ctrl Pts',(13.5228342013508,21.4077325259318,0.));
#249490=CARTESIAN_POINT('Ctrl Pts',(13.5203817122496,21.3813100304967,0.));
#249491=CARTESIAN_POINT('Ctrl Pts',(13.5178752862461,21.3549683486219,0.));
#249492=CARTESIAN_POINT('Ctrl Pts',(13.5153152050554,21.328707899634,0.));
#249493=CARTESIAN_POINT('Ctrl Pts',(13.5127017534972,21.3025291054236,0.));
#249494=CARTESIAN_POINT('Ctrl Pts',(13.5100352209207,21.2764323924442,0.));
#249495=CARTESIAN_POINT('Ctrl Pts',(13.5073159019454,21.2504181927429,0.));
#249496=CARTESIAN_POINT('Ctrl Pts',(13.5045440957404,21.224486942933,0.));
#249497=CARTESIAN_POINT('Ctrl Pts',(13.5017201056088,21.1986390835825,0.));
#249498=CARTESIAN_POINT('Ctrl Pts',(13.4988442384491,21.1728750584173,0.));
#249499=CARTESIAN_POINT('Ctrl Pts',(13.4959168042934,21.1471953136209,0.));
#249500=CARTESIAN_POINT('Ctrl Pts',(13.4929381157778,21.1216002970209,0.));
#249501=CARTESIAN_POINT('Ctrl Pts',(13.4899084877718,21.0960904575048,0.));
#249502=CARTESIAN_POINT('Ctrl Pts',(13.4868282377191,21.0706662455202,0.));
#249503=CARTESIAN_POINT('Ctrl Pts',(13.4836976858912,21.0453281134247,0.));
#249504=CARTESIAN_POINT('Ctrl Pts',(13.4805171556822,21.0200765158885,0.));
#249505=CARTESIAN_POINT('Ctrl Pts',(13.4772869738879,20.9949119102592,0.));
#249506=CARTESIAN_POINT('Ctrl Pts',(13.4740074710087,20.9698347569476,0.));
#249507=CARTESIAN_POINT('Ctrl Pts',(13.4706789815166,20.9448455197557,0.));
#249508=CARTESIAN_POINT('Ctrl Pts',(13.4673018437718,20.9199446657584,0.));
#249509=CARTESIAN_POINT('Ctrl Pts',(13.4638763999725,20.8951326652158,0.));
#249510=CARTESIAN_POINT('Ctrl Pts',(13.4604029960983,20.8704099914641,0.));
#249511=CARTESIAN_POINT('Ctrl Pts',(13.4568819818631,20.8457771208082,0.));
#249512=CARTESIAN_POINT('Ctrl Pts',(13.4533137106667,20.821234532398,0.));
#249513=CARTESIAN_POINT('Ctrl Pts',(13.4496985395637,20.7967827081227,0.));
#249514=CARTESIAN_POINT('Ctrl Pts',(13.4460368293688,20.7724221327608,0.));
#249515=CARTESIAN_POINT('Ctrl Pts',(13.4423289447561,20.7481532941013,0.));
#249516=CARTESIAN_POINT('Ctrl Pts',(13.4385752543663,20.7239766830675,0.));
#249517=CARTESIAN_POINT('Ctrl Pts',(13.4347761309154,20.6998927938288,0.));
#249518=CARTESIAN_POINT('Ctrl Pts',(13.4309319513119,20.6759021239103,0.));
#249519=CARTESIAN_POINT('Ctrl Pts',(13.4270430967651,20.6520051742869,0.));
#249520=CARTESIAN_POINT('Ctrl Pts',(13.4231099528179,20.6282024494237,0.));
#249521=CARTESIAN_POINT('Ctrl Pts',(13.4191329093932,20.6044944573153,0.));
#249522=CARTESIAN_POINT('Ctrl Pts',(13.4151123608411,20.5808817095155,0.));
#249523=CARTESIAN_POINT('Ctrl Pts',(13.4110487059912,20.5573647211639,0.));
#249524=CARTESIAN_POINT('Ctrl Pts',(13.4069423482076,20.5339440109956,0.));
#249525=CARTESIAN_POINT('Ctrl Pts',(13.4027936954529,20.5106201013753,0.));
#249526=CARTESIAN_POINT('Ctrl Pts',(13.3986031603716,20.487393518404,0.));
#249527=CARTESIAN_POINT('Ctrl Pts',(13.3943711603739,20.4642647920038,0.));
#249528=CARTESIAN_POINT('Ctrl Pts',(13.3900981177255,20.4412344560008,0.));
#249529=CARTESIAN_POINT('Ctrl Pts',(13.3857844596387,20.4183030482002,0.));
#249530=CARTESIAN_POINT('Ctrl Pts',(13.3814306183719,20.3954711104502,0.));
#249531=CARTESIAN_POINT('Ctrl Pts',(13.3770370313188,20.3727391887184,0.));
#249532=CARTESIAN_POINT('Ctrl Pts',(13.3726041410867,20.3501078331814,0.));
#249533=CARTESIAN_POINT('Ctrl Pts',(13.3681323955826,20.3275775983029,0.));
#249534=CARTESIAN_POINT('Ctrl Pts',(13.3636222481016,20.3051490429048,0.));
#249535=CARTESIAN_POINT('Ctrl Pts',(13.3590741574195,20.2828227302339,0.));
#249536=CARTESIAN_POINT('Ctrl Pts',(13.3544885878889,20.2605992280122,0.));
#249537=CARTESIAN_POINT('Ctrl Pts',(13.3498660095386,20.2384791085359,0.));
#249538=CARTESIAN_POINT('Ctrl Pts',(13.3452068981766,20.216462948786,0.));
#249539=CARTESIAN_POINT('Ctrl Pts',(13.3405117354971,20.1945513305235,0.));
#249540=CARTESIAN_POINT('Ctrl Pts',(13.3357810091903,20.1727448403817,0.));
#249541=CARTESIAN_POINT('Ctrl Pts',(13.3310152130564,20.1510440699474,0.));
#249542=CARTESIAN_POINT('Ctrl Pts',(13.3262148471226,20.1294496158402,0.));
#249543=CARTESIAN_POINT('Ctrl Pts',(13.3213804177587,20.1079620798375,0.));
#249544=CARTESIAN_POINT('Ctrl Pts',(13.3165124377962,20.0865820689883,0.));
#249545=CARTESIAN_POINT('Ctrl Pts',(13.3116114266515,20.0653101957188,0.));
#249546=CARTESIAN_POINT('Ctrl Pts',(13.3066779104515,20.0441470779345,0.));
#249547=CARTESIAN_POINT('Ctrl Pts',(13.3017124221637,20.0230933391038,0.));
#249548=CARTESIAN_POINT('Ctrl Pts',(13.2967155017306,20.0021496083738,0.));
#249549=CARTESIAN_POINT('Ctrl Pts',(13.2916876962094,19.981316520717,0.));
#249550=CARTESIAN_POINT('Ctrl Pts',(13.286629559915,19.9605947170586,0.));
#249551=CARTESIAN_POINT('Ctrl Pts',(13.2815416545663,19.9399848444019,0.));
#249552=CARTESIAN_POINT('Ctrl Pts',(13.2764245494357,19.9194875559422,0.));
#249553=CARTESIAN_POINT('Ctrl Pts',(13.271278821502,19.8991035111745,0.));
#249554=CARTESIAN_POINT('Ctrl Pts',(13.2661050556132,19.8788333760577,0.));
#249555=CARTESIAN_POINT('Ctrl Pts',(13.2609038446529,19.8586778231715,0.));
#249556=CARTESIAN_POINT('Ctrl Pts',(13.2556757897086,19.8386375318634,0.));
#249557=CARTESIAN_POINT('Ctrl Pts',(13.2504215002457,19.8187131883917,0.));
#249558=CARTESIAN_POINT('Ctrl Pts',(13.2451415942805,19.7989054860495,0.));
#249559=CARTESIAN_POINT('Ctrl Pts',(13.2398366985675,19.7792151253289,0.));
#249560=CARTESIAN_POINT('Ctrl Pts',(13.2345074487963,19.7596428141168,0.));
#249561=CARTESIAN_POINT('Ctrl Pts',(13.2291544897899,19.7401892678697,0.));
#249562=CARTESIAN_POINT('Ctrl Pts',(13.2237784757065,19.7208552097868,0.));
#249563=CARTESIAN_POINT('Ctrl Pts',(13.2183800702436,19.7016413709685,0.));
#249564=CARTESIAN_POINT('Ctrl Pts',(13.2129599468485,19.6825484905823,0.));
#249565=CARTESIAN_POINT('Ctrl Pts',(13.2075187889529,19.6635773160936,0.));
#249566=CARTESIAN_POINT('Ctrl Pts',(13.2020572902065,19.6447286034772,0.));
#249567=CARTESIAN_POINT('Ctrl Pts',(13.1965761547151,19.6260031174244,0.));
#249568=CARTESIAN_POINT('Ctrl Pts',(13.1910760972814,19.6074016315414,0.));
#249569=CARTESIAN_POINT('Ctrl Pts',(13.1855578436471,19.5889249285338,0.));
#249570=CARTESIAN_POINT('Ctrl Pts',(13.1800221307673,19.5705738004667,0.));
#249571=CARTESIAN_POINT('Ctrl Pts',(13.1744697070911,19.5523490490244,0.));
#249572=CARTESIAN_POINT('Ctrl Pts',(13.168901332843,19.5342514857562,0.));
#249573=CARTESIAN_POINT('Ctrl Pts',(13.1633177803101,19.5162819323213,0.));
#249574=CARTESIAN_POINT('Ctrl Pts',(13.1577198341245,19.4984412207082,0.));
#249575=CARTESIAN_POINT('Ctrl Pts',(13.1521082915853,19.4807301935268,0.));
#249576=CARTESIAN_POINT('Ctrl Pts',(13.1464839629971,19.4631497043258,0.));
#249577=CARTESIAN_POINT('Ctrl Pts',(13.1408476720061,19.4457006178876,0.));
#249578=CARTESIAN_POINT('Ctrl Pts',(13.1352002559438,19.4283838105262,0.));
#249579=CARTESIAN_POINT('Ctrl Pts',(13.1295425661634,19.4112001703557,0.));
#249580=CARTESIAN_POINT('Ctrl Pts',(13.1238754684177,19.3941505976263,0.));
#249581=CARTESIAN_POINT('Ctrl Pts',(13.118199843271,19.3772360051091,0.));
#249582=CARTESIAN_POINT('Ctrl Pts',(13.1125165865022,19.3604573184515,0.));
#249583=CARTESIAN_POINT('Ctrl Pts',(13.1068266095186,19.3438154765395,0.));
#249584=CARTESIAN_POINT('Ctrl Pts',(13.1011308397591,19.3273114318269,0.));
#249585=CARTESIAN_POINT('Ctrl Pts',(13.0954302211479,19.310946150736,0.));
#249586=CARTESIAN_POINT('Ctrl Pts',(13.0897257145968,19.2947206141247,0.));
#249587=CARTESIAN_POINT('Ctrl Pts',(13.0840182984949,19.2786358177198,0.));
#249588=CARTESIAN_POINT('Ctrl Pts',(13.0783089692118,19.2626927725596,0.));
#249589=CARTESIAN_POINT('Ctrl Pts',(13.0725987415859,19.2468925053989,0.));
#249590=CARTESIAN_POINT('Ctrl Pts',(13.0668886494795,19.2312360592033,0.));
#249591=CARTESIAN_POINT('Ctrl Pts',(13.0611797463915,19.2157244937142,0.));
#249592=CARTESIAN_POINT('Ctrl Pts',(13.0554731060538,19.2003588859772,0.));
#249593=CARTESIAN_POINT('Ctrl Pts',(13.0497698230441,19.1851403308825,0.));
#249594=CARTESIAN_POINT('Ctrl Pts',(13.0440710133772,19.1700699416622,0.));
#249595=CARTESIAN_POINT('Ctrl Pts',(13.0383778152068,19.155148850523,0.));
#249596=CARTESIAN_POINT('Ctrl Pts',(13.0326913895838,19.1403782093386,0.));
#249597=CARTESIAN_POINT('Ctrl Pts',(13.0270129211976,19.1257591903099,0.));
#249598=CARTESIAN_POINT('Ctrl Pts',(13.0213436191328,19.111292986631,0.));
#249599=CARTESIAN_POINT('Ctrl Pts',(13.0156847176096,19.0969808131228,0.));
#249600=CARTESIAN_POINT('Ctrl Pts',(13.0100374768788,19.0828239070484,0.));
#249601=CARTESIAN_POINT('Ctrl Pts',(13.0044031841382,19.0688235289437,0.));
#249602=CARTESIAN_POINT('Ctrl Pts',(12.9987831544502,19.0549809634354,0.));
#249603=CARTESIAN_POINT('Ctrl Pts',(12.9931787316514,19.0412975200398,0.));
#249604=CARTESIAN_POINT('Ctrl Pts',(12.9875912893003,19.0277745339909,0.));
#249605=CARTESIAN_POINT('Ctrl Pts',(12.9820222318716,19.014413367335,0.));
#249606=CARTESIAN_POINT('Ctrl Pts',(12.9764729959206,19.0012154099792,0.));
#249607=CARTESIAN_POINT('Ctrl Pts',(12.9709450512747,18.9881820807585,0.));
#249608=CARTESIAN_POINT('Ctrl Pts',(12.9654399021868,18.9753148284473,0.));
#249609=CARTESIAN_POINT('Ctrl Pts',(12.9599590886317,18.9626151329226,0.));
#249610=CARTESIAN_POINT('Ctrl Pts',(12.9545041877377,18.9500845064714,0.));
#249611=CARTESIAN_POINT('Ctrl Pts',(12.9490768151821,18.9377244950435,0.));
#249612=CARTESIAN_POINT('Ctrl Pts',(12.9436786266106,18.9255366795196,0.));
#249613=CARTESIAN_POINT('Ctrl Pts',(12.9383113190375,18.9135226769466,0.));
#249614=CARTESIAN_POINT('Ctrl Pts',(12.9329766328184,18.9016841423402,0.));
#249615=CARTESIAN_POINT('Ctrl Pts',(12.9276763536372,18.8900227704888,0.));
#249616=CARTESIAN_POINT('Ctrl Pts',(12.9224123144982,18.8785402977528,0.));
#249617=CARTESIAN_POINT('Ctrl Pts',(12.9171863977047,18.8672385038328,0.));
#249618=CARTESIAN_POINT('Ctrl Pts',(12.9120005369066,18.8561192136201,0.));
#249619=CARTESIAN_POINT('Ctrl Pts',(12.9068567191856,18.8451842990986,0.));
#249620=CARTESIAN_POINT('Ctrl Pts',(12.9017569871738,18.834435681259,0.));
#249621=CARTESIAN_POINT('Ctrl Pts',(12.8967034410752,18.8238753319124,0.));
#249622=CARTESIAN_POINT('Ctrl Pts',(12.8916982409931,18.8135052757815,0.));
#249623=CARTESIAN_POINT('Ctrl Pts',(12.8867436109543,18.8033275941939,0.));
#249624=CARTESIAN_POINT('Ctrl Pts',(12.8818418427474,18.7933444285867,0.));
#249625=CARTESIAN_POINT('Ctrl Pts',(12.8769952998097,18.7835579840481,0.));
#249626=CARTESIAN_POINT('Ctrl Pts',(12.8722064211814,18.7739705329029,0.));
#249627=CARTESIAN_POINT('Ctrl Pts',(12.8674777239656,18.7645844169568,0.));
#249628=CARTESIAN_POINT('Ctrl Pts',(12.8628118054172,18.7554020493888,0.));
#249629=CARTESIAN_POINT('Ctrl Pts',(12.8582113455644,18.7464259171248,0.));
#249630=CARTESIAN_POINT('Ctrl Pts',(12.8536791086315,18.7376585820851,0.));
#249631=CARTESIAN_POINT('Ctrl Pts',(12.849217951159,18.7291026886552,0.));
#249632=CARTESIAN_POINT('Ctrl Pts',(12.8448308329494,18.7207609737701,0.));
#249633=CARTESIAN_POINT('Ctrl Pts',(12.8405208263432,18.7126362754446,0.));
#249634=CARTESIAN_POINT('Ctrl Pts',(12.8362911280362,18.7047315436296,0.));
#249635=CARTESIAN_POINT('Ctrl Pts',(12.832145059979,18.6970498410173,0.));
#249636=CARTESIAN_POINT('Ctrl Pts',(12.8280860635231,18.6895943376172,0.));
#249637=CARTESIAN_POINT('Ctrl Pts',(12.8241176980016,18.6823683094139,0.));
#249638=CARTESIAN_POINT('Ctrl Pts',(12.8202436318473,18.6753751301091,0.));
#249639=CARTESIAN_POINT('Ctrl Pts',(12.8164676687361,18.6686182952798,0.));
#249640=CARTESIAN_POINT('Ctrl Pts',(12.8127937909632,18.6621014624746,0.));
#249641=CARTESIAN_POINT('Ctrl Pts',(12.8092261933858,18.6558284825772,0.));
#249642=CARTESIAN_POINT('Ctrl Pts',(12.805769331162,18.6498034438986,0.));
#249643=CARTESIAN_POINT('Ctrl Pts',(12.8024278770153,18.6440306327457,0.));
#249644=CARTESIAN_POINT('Ctrl Pts',(12.7992066625264,18.63851447924,0.));
#249645=CARTESIAN_POINT('Ctrl Pts',(12.7961106222251,18.6332595057005,0.));
#249646=CARTESIAN_POINT('Ctrl Pts',(12.7931447451556,18.6282702819371,0.));
#249647=CARTESIAN_POINT('Ctrl Pts',(12.7903142925234,18.6235516265575,0.));
#249648=CARTESIAN_POINT('Ctrl Pts',(12.7876249657834,18.6191087624752,0.));
#249649=CARTESIAN_POINT('Ctrl Pts',(12.78508316579,18.6149475565189,0.));
#249650=CARTESIAN_POINT('Ctrl Pts',(12.7826959526924,18.611074482622,0.));
#249651=CARTESIAN_POINT('Ctrl Pts',(12.7804705387658,18.6074961535723,0.));
#249652=CARTESIAN_POINT('Ctrl Pts',(12.7784139605067,18.6042190183703,0.));
#249653=CARTESIAN_POINT('Ctrl Pts',(12.7765325225082,18.6012488486708,0.));
#249654=CARTESIAN_POINT('Ctrl Pts',(12.7748328937639,18.5985917525949,0.));
#249655=CARTESIAN_POINT('Ctrl Pts',(12.7733231262107,18.5962551167772,0.));
#249656=CARTESIAN_POINT('Ctrl Pts',(12.7720142287169,18.5942490615409,0.));
#249657=CARTESIAN_POINT('Ctrl Pts',(12.7709195951153,18.5925859134582,0.));
#249658=CARTESIAN_POINT('Ctrl Pts',(12.7700520897174,18.5912775137806,0.));
#249659=CARTESIAN_POINT('Ctrl Pts',(12.7694215127923,18.590332877722,0.));
#249660=CARTESIAN_POINT('Ctrl Pts',(12.7691103481996,18.589871621842,0.));
#249661=CARTESIAN_POINT('Ctrl Pts',(12.7689864266924,18.5896919669158,0.));
#249662=CARTESIAN_POINT('Ctrl Pts',(12.7689524524484,18.5896460962961,0.));
#249663=CARTESIAN_POINT('Ctrl Pts',(12.7689476255363,18.5896416359912,0.));
#249664=CARTESIAN_POINT('',(13.5685075571671,22.1787195904339,12.));
#249665=CARTESIAN_POINT('',(13.5685075571671,22.1787195904339,0.));
#249666=CARTESIAN_POINT('Ctrl Pts',(12.7689476255363,18.5896416359912,12.));
#249667=CARTESIAN_POINT('Ctrl Pts',(12.7689524524484,18.5896460962961,12.));
#249668=CARTESIAN_POINT('Ctrl Pts',(12.7689864266924,18.5896919669158,12.));
#249669=CARTESIAN_POINT('Ctrl Pts',(12.7691103481996,18.589871621842,12.));
#249670=CARTESIAN_POINT('Ctrl Pts',(12.7694215127923,18.590332877722,12.));
#249671=CARTESIAN_POINT('Ctrl Pts',(12.7700520897174,18.5912775137806,12.));
#249672=CARTESIAN_POINT('Ctrl Pts',(12.7709195951153,18.5925859134582,12.));
#249673=CARTESIAN_POINT('Ctrl Pts',(12.7720142287169,18.5942490615409,12.));
#249674=CARTESIAN_POINT('Ctrl Pts',(12.7733231262107,18.5962551167772,12.));
#249675=CARTESIAN_POINT('Ctrl Pts',(12.7748328937639,18.5985917525949,12.));
#249676=CARTESIAN_POINT('Ctrl Pts',(12.7765325225082,18.6012488486708,12.));
#249677=CARTESIAN_POINT('Ctrl Pts',(12.7784139605067,18.6042190183703,12.));
#249678=CARTESIAN_POINT('Ctrl Pts',(12.7804705387658,18.6074961535723,12.));
#249679=CARTESIAN_POINT('Ctrl Pts',(12.7826959526924,18.611074482622,12.));
#249680=CARTESIAN_POINT('Ctrl Pts',(12.78508316579,18.6149475565189,12.));
#249681=CARTESIAN_POINT('Ctrl Pts',(12.7876249657834,18.6191087624752,12.));
#249682=CARTESIAN_POINT('Ctrl Pts',(12.7903142925234,18.6235516265575,12.));
#249683=CARTESIAN_POINT('Ctrl Pts',(12.7931447451556,18.6282702819371,12.));
#249684=CARTESIAN_POINT('Ctrl Pts',(12.7961106222251,18.6332595057005,12.));
#249685=CARTESIAN_POINT('Ctrl Pts',(12.7992066625264,18.63851447924,12.));
#249686=CARTESIAN_POINT('Ctrl Pts',(12.8024278770153,18.6440306327457,12.));
#249687=CARTESIAN_POINT('Ctrl Pts',(12.805769331162,18.6498034438986,12.));
#249688=CARTESIAN_POINT('Ctrl Pts',(12.8092261933858,18.6558284825772,12.));
#249689=CARTESIAN_POINT('Ctrl Pts',(12.8127937909632,18.6621014624746,12.));
#249690=CARTESIAN_POINT('Ctrl Pts',(12.8164676687361,18.6686182952798,12.));
#249691=CARTESIAN_POINT('Ctrl Pts',(12.8202436318473,18.6753751301091,12.));
#249692=CARTESIAN_POINT('Ctrl Pts',(12.8241176980016,18.6823683094139,12.));
#249693=CARTESIAN_POINT('Ctrl Pts',(12.8280860635231,18.6895943376172,12.));
#249694=CARTESIAN_POINT('Ctrl Pts',(12.832145059979,18.6970498410173,12.));
#249695=CARTESIAN_POINT('Ctrl Pts',(12.8362911280362,18.7047315436296,12.));
#249696=CARTESIAN_POINT('Ctrl Pts',(12.8405208263432,18.7126362754446,12.));
#249697=CARTESIAN_POINT('Ctrl Pts',(12.8448308329494,18.7207609737701,12.));
#249698=CARTESIAN_POINT('Ctrl Pts',(12.849217951159,18.7291026886552,12.));
#249699=CARTESIAN_POINT('Ctrl Pts',(12.8536791086315,18.7376585820851,12.));
#249700=CARTESIAN_POINT('Ctrl Pts',(12.8582113455644,18.7464259171248,12.));
#249701=CARTESIAN_POINT('Ctrl Pts',(12.8628118054172,18.7554020493888,12.));
#249702=CARTESIAN_POINT('Ctrl Pts',(12.8674777239656,18.7645844169568,12.));
#249703=CARTESIAN_POINT('Ctrl Pts',(12.8722064211814,18.7739705329029,12.));
#249704=CARTESIAN_POINT('Ctrl Pts',(12.8769952998097,18.7835579840481,12.));
#249705=CARTESIAN_POINT('Ctrl Pts',(12.8818418427474,18.7933444285867,12.));
#249706=CARTESIAN_POINT('Ctrl Pts',(12.8867436109543,18.8033275941939,12.));
#249707=CARTESIAN_POINT('Ctrl Pts',(12.8916982409931,18.8135052757815,12.));
#249708=CARTESIAN_POINT('Ctrl Pts',(12.8967034410752,18.8238753319124,12.));
#249709=CARTESIAN_POINT('Ctrl Pts',(12.9017569871738,18.834435681259,12.));
#249710=CARTESIAN_POINT('Ctrl Pts',(12.9068567191856,18.8451842990986,12.));
#249711=CARTESIAN_POINT('Ctrl Pts',(12.9120005369066,18.8561192136201,12.));
#249712=CARTESIAN_POINT('Ctrl Pts',(12.9171863977047,18.8672385038328,12.));
#249713=CARTESIAN_POINT('Ctrl Pts',(12.9224123144982,18.8785402977528,12.));
#249714=CARTESIAN_POINT('Ctrl Pts',(12.9276763536372,18.8900227704888,12.));
#249715=CARTESIAN_POINT('Ctrl Pts',(12.9329766328184,18.9016841423402,12.));
#249716=CARTESIAN_POINT('Ctrl Pts',(12.9383113190375,18.9135226769466,12.));
#249717=CARTESIAN_POINT('Ctrl Pts',(12.9436786266106,18.9255366795196,12.));
#249718=CARTESIAN_POINT('Ctrl Pts',(12.9490768151821,18.9377244950435,12.));
#249719=CARTESIAN_POINT('Ctrl Pts',(12.9545041877377,18.9500845064714,12.));
#249720=CARTESIAN_POINT('Ctrl Pts',(12.9599590886317,18.9626151329226,12.));
#249721=CARTESIAN_POINT('Ctrl Pts',(12.9654399021868,18.9753148284473,12.));
#249722=CARTESIAN_POINT('Ctrl Pts',(12.9709450512747,18.9881820807585,12.));
#249723=CARTESIAN_POINT('Ctrl Pts',(12.9764729959206,19.0012154099792,12.));
#249724=CARTESIAN_POINT('Ctrl Pts',(12.9820222318716,19.014413367335,12.));
#249725=CARTESIAN_POINT('Ctrl Pts',(12.9875912893003,19.0277745339909,12.));
#249726=CARTESIAN_POINT('Ctrl Pts',(12.9931787316514,19.0412975200398,12.));
#249727=CARTESIAN_POINT('Ctrl Pts',(12.9987831544502,19.0549809634354,12.));
#249728=CARTESIAN_POINT('Ctrl Pts',(13.0044031841382,19.0688235289437,12.));
#249729=CARTESIAN_POINT('Ctrl Pts',(13.0100374768788,19.0828239070484,12.));
#249730=CARTESIAN_POINT('Ctrl Pts',(13.0156847176096,19.0969808131228,12.));
#249731=CARTESIAN_POINT('Ctrl Pts',(13.0213436191328,19.111292986631,12.));
#249732=CARTESIAN_POINT('Ctrl Pts',(13.0270129211976,19.1257591903099,12.));
#249733=CARTESIAN_POINT('Ctrl Pts',(13.0326913895838,19.1403782093386,12.));
#249734=CARTESIAN_POINT('Ctrl Pts',(13.0383778152068,19.155148850523,12.));
#249735=CARTESIAN_POINT('Ctrl Pts',(13.0440710133772,19.1700699416622,12.));
#249736=CARTESIAN_POINT('Ctrl Pts',(13.0497698230441,19.1851403308825,12.));
#249737=CARTESIAN_POINT('Ctrl Pts',(13.0554731060538,19.2003588859772,12.));
#249738=CARTESIAN_POINT('Ctrl Pts',(13.0611797463915,19.2157244937142,12.));
#249739=CARTESIAN_POINT('Ctrl Pts',(13.0668886494795,19.2312360592033,12.));
#249740=CARTESIAN_POINT('Ctrl Pts',(13.0725987415859,19.2468925053989,12.));
#249741=CARTESIAN_POINT('Ctrl Pts',(13.0783089692118,19.2626927725596,12.));
#249742=CARTESIAN_POINT('Ctrl Pts',(13.0840182984949,19.2786358177198,12.));
#249743=CARTESIAN_POINT('Ctrl Pts',(13.0897257145968,19.2947206141247,12.));
#249744=CARTESIAN_POINT('Ctrl Pts',(13.0954302211479,19.310946150736,12.));
#249745=CARTESIAN_POINT('Ctrl Pts',(13.1011308397591,19.3273114318269,12.));
#249746=CARTESIAN_POINT('Ctrl Pts',(13.1068266095186,19.3438154765395,12.));
#249747=CARTESIAN_POINT('Ctrl Pts',(13.1125165865022,19.3604573184515,12.));
#249748=CARTESIAN_POINT('Ctrl Pts',(13.118199843271,19.3772360051091,12.));
#249749=CARTESIAN_POINT('Ctrl Pts',(13.1238754684177,19.3941505976263,12.));
#249750=CARTESIAN_POINT('Ctrl Pts',(13.1295425661634,19.4112001703557,12.));
#249751=CARTESIAN_POINT('Ctrl Pts',(13.1352002559438,19.4283838105262,12.));
#249752=CARTESIAN_POINT('Ctrl Pts',(13.1408476720061,19.4457006178876,12.));
#249753=CARTESIAN_POINT('Ctrl Pts',(13.1464839629971,19.4631497043258,12.));
#249754=CARTESIAN_POINT('Ctrl Pts',(13.1521082915853,19.4807301935268,12.));
#249755=CARTESIAN_POINT('Ctrl Pts',(13.1577198341245,19.4984412207082,12.));
#249756=CARTESIAN_POINT('Ctrl Pts',(13.1633177803101,19.5162819323213,12.));
#249757=CARTESIAN_POINT('Ctrl Pts',(13.168901332843,19.5342514857562,12.));
#249758=CARTESIAN_POINT('Ctrl Pts',(13.1744697070911,19.5523490490244,12.));
#249759=CARTESIAN_POINT('Ctrl Pts',(13.1800221307673,19.5705738004667,12.));
#249760=CARTESIAN_POINT('Ctrl Pts',(13.1855578436471,19.5889249285338,12.));
#249761=CARTESIAN_POINT('Ctrl Pts',(13.1910760972814,19.6074016315414,12.));
#249762=CARTESIAN_POINT('Ctrl Pts',(13.1965761547151,19.6260031174244,12.));
#249763=CARTESIAN_POINT('Ctrl Pts',(13.2020572902065,19.6447286034772,12.));
#249764=CARTESIAN_POINT('Ctrl Pts',(13.2075187889529,19.6635773160936,12.));
#249765=CARTESIAN_POINT('Ctrl Pts',(13.2129599468485,19.6825484905823,12.));
#249766=CARTESIAN_POINT('Ctrl Pts',(13.2183800702436,19.7016413709685,12.));
#249767=CARTESIAN_POINT('Ctrl Pts',(13.2237784757065,19.7208552097868,12.));
#249768=CARTESIAN_POINT('Ctrl Pts',(13.2291544897899,19.7401892678697,12.));
#249769=CARTESIAN_POINT('Ctrl Pts',(13.2345074487963,19.7596428141168,12.));
#249770=CARTESIAN_POINT('Ctrl Pts',(13.2398366985675,19.7792151253289,12.));
#249771=CARTESIAN_POINT('Ctrl Pts',(13.2451415942805,19.7989054860495,12.));
#249772=CARTESIAN_POINT('Ctrl Pts',(13.2504215002457,19.8187131883917,12.));
#249773=CARTESIAN_POINT('Ctrl Pts',(13.2556757897086,19.8386375318634,12.));
#249774=CARTESIAN_POINT('Ctrl Pts',(13.2609038446529,19.8586778231715,12.));
#249775=CARTESIAN_POINT('Ctrl Pts',(13.2661050556132,19.8788333760577,12.));
#249776=CARTESIAN_POINT('Ctrl Pts',(13.271278821502,19.8991035111745,12.));
#249777=CARTESIAN_POINT('Ctrl Pts',(13.2764245494357,19.9194875559422,12.));
#249778=CARTESIAN_POINT('Ctrl Pts',(13.2815416545663,19.9399848444019,12.));
#249779=CARTESIAN_POINT('Ctrl Pts',(13.286629559915,19.9605947170586,12.));
#249780=CARTESIAN_POINT('Ctrl Pts',(13.2916876962094,19.981316520717,12.));
#249781=CARTESIAN_POINT('Ctrl Pts',(13.2967155017306,20.0021496083738,12.));
#249782=CARTESIAN_POINT('Ctrl Pts',(13.3017124221637,20.0230933391038,12.));
#249783=CARTESIAN_POINT('Ctrl Pts',(13.3066779104515,20.0441470779345,12.));
#249784=CARTESIAN_POINT('Ctrl Pts',(13.3116114266515,20.0653101957188,12.));
#249785=CARTESIAN_POINT('Ctrl Pts',(13.3165124377962,20.0865820689883,12.));
#249786=CARTESIAN_POINT('Ctrl Pts',(13.3213804177587,20.1079620798375,12.));
#249787=CARTESIAN_POINT('Ctrl Pts',(13.3262148471226,20.1294496158402,12.));
#249788=CARTESIAN_POINT('Ctrl Pts',(13.3310152130564,20.1510440699474,12.));
#249789=CARTESIAN_POINT('Ctrl Pts',(13.3357810091903,20.1727448403817,12.));
#249790=CARTESIAN_POINT('Ctrl Pts',(13.3405117354971,20.1945513305235,12.));
#249791=CARTESIAN_POINT('Ctrl Pts',(13.3452068981766,20.216462948786,12.));
#249792=CARTESIAN_POINT('Ctrl Pts',(13.3498660095386,20.2384791085359,12.));
#249793=CARTESIAN_POINT('Ctrl Pts',(13.3544885878889,20.2605992280122,12.));
#249794=CARTESIAN_POINT('Ctrl Pts',(13.3590741574195,20.2828227302339,12.));
#249795=CARTESIAN_POINT('Ctrl Pts',(13.3636222481016,20.3051490429048,12.));
#249796=CARTESIAN_POINT('Ctrl Pts',(13.3681323955826,20.3275775983029,12.));
#249797=CARTESIAN_POINT('Ctrl Pts',(13.3726041410867,20.3501078331814,12.));
#249798=CARTESIAN_POINT('Ctrl Pts',(13.3770370313188,20.3727391887184,12.));
#249799=CARTESIAN_POINT('Ctrl Pts',(13.3814306183719,20.3954711104502,12.));
#249800=CARTESIAN_POINT('Ctrl Pts',(13.3857844596387,20.4183030482002,12.));
#249801=CARTESIAN_POINT('Ctrl Pts',(13.3900981177255,20.4412344560008,12.));
#249802=CARTESIAN_POINT('Ctrl Pts',(13.3943711603739,20.4642647920038,12.));
#249803=CARTESIAN_POINT('Ctrl Pts',(13.3986031603716,20.487393518404,12.));
#249804=CARTESIAN_POINT('Ctrl Pts',(13.4027936954529,20.5106201013753,12.));
#249805=CARTESIAN_POINT('Ctrl Pts',(13.4069423482076,20.5339440109956,12.));
#249806=CARTESIAN_POINT('Ctrl Pts',(13.4110487059912,20.5573647211639,12.));
#249807=CARTESIAN_POINT('Ctrl Pts',(13.4151123608411,20.5808817095155,12.));
#249808=CARTESIAN_POINT('Ctrl Pts',(13.4191329093932,20.6044944573153,12.));
#249809=CARTESIAN_POINT('Ctrl Pts',(13.4231099528179,20.6282024494237,12.));
#249810=CARTESIAN_POINT('Ctrl Pts',(13.4270430967651,20.6520051742869,12.));
#249811=CARTESIAN_POINT('Ctrl Pts',(13.4309319513119,20.6759021239103,12.));
#249812=CARTESIAN_POINT('Ctrl Pts',(13.4347761309154,20.6998927938288,12.));
#249813=CARTESIAN_POINT('Ctrl Pts',(13.4385752543663,20.7239766830675,12.));
#249814=CARTESIAN_POINT('Ctrl Pts',(13.4423289447561,20.7481532941013,12.));
#249815=CARTESIAN_POINT('Ctrl Pts',(13.4460368293688,20.7724221327608,12.));
#249816=CARTESIAN_POINT('Ctrl Pts',(13.4496985395637,20.7967827081227,12.));
#249817=CARTESIAN_POINT('Ctrl Pts',(13.4533137106667,20.821234532398,12.));
#249818=CARTESIAN_POINT('Ctrl Pts',(13.4568819818631,20.8457771208082,12.));
#249819=CARTESIAN_POINT('Ctrl Pts',(13.4604029960983,20.8704099914641,12.));
#249820=CARTESIAN_POINT('Ctrl Pts',(13.4638763999725,20.8951326652158,12.));
#249821=CARTESIAN_POINT('Ctrl Pts',(13.4673018437718,20.9199446657584,12.));
#249822=CARTESIAN_POINT('Ctrl Pts',(13.4706789815166,20.9448455197557,12.));
#249823=CARTESIAN_POINT('Ctrl Pts',(13.4740074710087,20.9698347569476,12.));
#249824=CARTESIAN_POINT('Ctrl Pts',(13.4772869738879,20.9949119102592,12.));
#249825=CARTESIAN_POINT('Ctrl Pts',(13.4805171556822,21.0200765158885,12.));
#249826=CARTESIAN_POINT('Ctrl Pts',(13.4836976858912,21.0453281134247,12.));
#249827=CARTESIAN_POINT('Ctrl Pts',(13.4868282377191,21.0706662455202,12.));
#249828=CARTESIAN_POINT('Ctrl Pts',(13.4899084877718,21.0960904575048,12.));
#249829=CARTESIAN_POINT('Ctrl Pts',(13.4929381157778,21.1216002970209,12.));
#249830=CARTESIAN_POINT('Ctrl Pts',(13.4959168042934,21.1471953136209,12.));
#249831=CARTESIAN_POINT('Ctrl Pts',(13.4988442384491,21.1728750584173,12.));
#249832=CARTESIAN_POINT('Ctrl Pts',(13.5017201056088,21.1986390835825,12.));
#249833=CARTESIAN_POINT('Ctrl Pts',(13.5045440957404,21.224486942933,12.));
#249834=CARTESIAN_POINT('Ctrl Pts',(13.5073159019454,21.2504181927429,12.));
#249835=CARTESIAN_POINT('Ctrl Pts',(13.5100352209207,21.2764323924442,12.));
#249836=CARTESIAN_POINT('Ctrl Pts',(13.5127017534972,21.3025291054236,12.));
#249837=CARTESIAN_POINT('Ctrl Pts',(13.5153152050554,21.328707899634,12.));
#249838=CARTESIAN_POINT('Ctrl Pts',(13.5178752862461,21.3549683486219,12.));
#249839=CARTESIAN_POINT('Ctrl Pts',(13.5203817122496,21.3813100304967,12.));
#249840=CARTESIAN_POINT('Ctrl Pts',(13.5228342013508,21.4077325259318,12.));
#249841=CARTESIAN_POINT('Ctrl Pts',(13.5252324737795,21.4342354165254,12.));
#249842=CARTESIAN_POINT('Ctrl Pts',(13.5275762503553,21.4608182828695,12.));
#249843=CARTESIAN_POINT('Ctrl Pts',(13.5298652514357,21.487480703047,12.));
#249844=CARTESIAN_POINT('Ctrl Pts',(13.5320991952145,21.5142222501671,12.));
#249845=CARTESIAN_POINT('Ctrl Pts',(13.5342777983225,21.5410424932511,12.));
#249846=CARTESIAN_POINT('Ctrl Pts',(13.5364007790292,21.5679410019011,12.));
#249847=CARTESIAN_POINT('Ctrl Pts',(13.5384678597206,21.5949173499022,12.));
#249848=CARTESIAN_POINT('Ctrl Pts',(13.5404787697798,21.6219711193951,12.));
#249849=CARTESIAN_POINT('Ctrl Pts',(13.5424332480698,21.6491019044647,12.));
#249850=CARTESIAN_POINT('Ctrl Pts',(13.5443310461516,21.676309315769,12.));
#249851=CARTESIAN_POINT('Ctrl Pts',(13.546171929503,21.7035929822939,12.));
#249852=CARTESIAN_POINT('Ctrl Pts',(13.5479556704457,21.730952541226,12.));
#249853=CARTESIAN_POINT('Ctrl Pts',(13.5496820422186,21.7583876294532,12.));
#249854=CARTESIAN_POINT('Ctrl Pts',(13.5513508127232,21.7858978745848,12.));
#249855=CARTESIAN_POINT('Ctrl Pts',(13.5529617381569,21.8134828857963,12.));
#249856=CARTESIAN_POINT('Ctrl Pts',(13.5545145573048,21.841142245609,12.));
#249857=CARTESIAN_POINT('Ctrl Pts',(13.5560089839426,21.8688754989401,12.));
#249858=CARTESIAN_POINT('Ctrl Pts',(13.5574447178484,21.8966821688876,12.));
#249859=CARTESIAN_POINT('Ctrl Pts',(13.5588214586672,21.9245617765827,12.));
#249860=CARTESIAN_POINT('Ctrl Pts',(13.5601389185315,21.9525138592862,12.));
#249861=CARTESIAN_POINT('Ctrl Pts',(13.5613968357589,21.9805379899192,12.));
#249862=CARTESIAN_POINT('Ctrl Pts',(13.5625949868313,22.0086337943431,12.));
#249863=CARTESIAN_POINT('Ctrl Pts',(13.5637332022393,22.0368009736227,12.));
#249864=CARTESIAN_POINT('Ctrl Pts',(13.5648113688894,22.0650393089492,12.));
#249865=CARTESIAN_POINT('Ctrl Pts',(13.5658294169106,22.0933486464442,12.));
#249866=CARTESIAN_POINT('Ctrl Pts',(13.5667873105179,22.1217288871823,12.));
#249867=CARTESIAN_POINT('Ctrl Pts',(13.5675054918922,22.1444897575076,12.));
#249868=CARTESIAN_POINT('Ctrl Pts',(13.5680170531724,22.1615922804939,12.));
#249869=CARTESIAN_POINT('Ctrl Pts',(13.5683460612913,22.1730081264583,12.));
#249870=CARTESIAN_POINT('Ctrl Pts',(13.5685075571671,22.1787195904339,12.));
#249871=CARTESIAN_POINT('Ctrl Pts',(14.6513681262571,17.1452095830633,0.));
#249872=CARTESIAN_POINT('Ctrl Pts',(14.6513681262571,17.1452095830633,12.));
#249873=CARTESIAN_POINT('Ctrl Pts',(14.6513711852843,17.1452153999142,0.));
#249874=CARTESIAN_POINT('Ctrl Pts',(14.6513711852843,17.1452153999142,12.));
#249875=CARTESIAN_POINT('Ctrl Pts',(14.6514066997196,17.1452600887037,0.));
#249876=CARTESIAN_POINT('Ctrl Pts',(14.6514066997196,17.1452600887037,12.));
#249877=CARTESIAN_POINT('Ctrl Pts',(14.6515481598068,17.1454262858043,0.));
#249878=CARTESIAN_POINT('Ctrl Pts',(14.6515481598068,17.1454262858043,12.));
#249879=CARTESIAN_POINT('Ctrl Pts',(14.6519131634508,17.1458462295271,0.));
#249880=CARTESIAN_POINT('Ctrl Pts',(14.6519131634508,17.1458462295271,12.));
#249881=CARTESIAN_POINT('Ctrl Pts',(14.6526624064978,17.1466998098673,0.));
#249882=CARTESIAN_POINT('Ctrl Pts',(14.6526624064978,17.1466998098673,12.));
#249883=CARTESIAN_POINT('Ctrl Pts',(14.6537016966184,17.147876394491,0.));
#249884=CARTESIAN_POINT('Ctrl Pts',(14.6537016966184,17.147876394491,12.));
#249885=CARTESIAN_POINT('Ctrl Pts',(14.655024862281,17.1493641837558,0.));
#249886=CARTESIAN_POINT('Ctrl Pts',(14.655024862281,17.1493641837558,12.));
#249887=CARTESIAN_POINT('Ctrl Pts',(14.6566237952435,17.1511476869496,0.));
#249888=CARTESIAN_POINT('Ctrl Pts',(14.6566237952435,17.1511476869496,12.));
#249889=CARTESIAN_POINT('Ctrl Pts',(14.6584900555302,17.1532107762718,0.));
#249890=CARTESIAN_POINT('Ctrl Pts',(14.6584900555302,17.1532107762718,12.));
#249891=CARTESIAN_POINT('Ctrl Pts',(14.6606167169642,17.1555401986401,0.));
#249892=CARTESIAN_POINT('Ctrl Pts',(14.6606167169642,17.1555401986401,12.));
#249893=CARTESIAN_POINT('Ctrl Pts',(14.6629987285992,17.1581262646789,0.));
#249894=CARTESIAN_POINT('Ctrl Pts',(14.6629987285992,17.1581262646789,12.));
#249895=CARTESIAN_POINT('Ctrl Pts',(14.6656319165057,17.1609609517369,0.));
#249896=CARTESIAN_POINT('Ctrl Pts',(14.6656319165057,17.1609609517369,12.));
#249897=CARTESIAN_POINT('Ctrl Pts',(14.6685123374423,17.1640366762305,0.));
#249898=CARTESIAN_POINT('Ctrl Pts',(14.6685123374423,17.1640366762305,12.));
#249899=CARTESIAN_POINT('Ctrl Pts',(14.671635583332,17.167344972302,0.));
#249900=CARTESIAN_POINT('Ctrl Pts',(14.671635583332,17.167344972302,12.));
#249901=CARTESIAN_POINT('Ctrl Pts',(14.6749971333867,17.1708771619129,0.));
#249902=CARTESIAN_POINT('Ctrl Pts',(14.6749971333867,17.1708771619129,12.));
#249903=CARTESIAN_POINT('Ctrl Pts',(14.6785925615677,17.1746247499057,0.));
#249904=CARTESIAN_POINT('Ctrl Pts',(14.6785925615677,17.1746247499057,12.));
#249905=CARTESIAN_POINT('Ctrl Pts',(14.6824178576167,17.1785800350826,0.));
#249906=CARTESIAN_POINT('Ctrl Pts',(14.6824178576167,17.1785800350826,12.));
#249907=CARTESIAN_POINT('Ctrl Pts',(14.686469452232,17.182736158472,0.));
#249908=CARTESIAN_POINT('Ctrl Pts',(14.686469452232,17.182736158472,12.));
#249909=CARTESIAN_POINT('Ctrl Pts',(14.6907440526958,17.1870867909918,0.));
#249910=CARTESIAN_POINT('Ctrl Pts',(14.6907440526958,17.1870867909918,12.));
#249911=CARTESIAN_POINT('Ctrl Pts',(14.6952385361705,17.1916259308415,0.));
#249912=CARTESIAN_POINT('Ctrl Pts',(14.6952385361705,17.1916259308415,12.));
#249913=CARTESIAN_POINT('Ctrl Pts',(14.699949811582,17.1963476411694,0.));
#249914=CARTESIAN_POINT('Ctrl Pts',(14.699949811582,17.1963476411694,12.));
#249915=CARTESIAN_POINT('Ctrl Pts',(14.7048748502663,17.2012461084268,0.));
#249916=CARTESIAN_POINT('Ctrl Pts',(14.7048748502663,17.2012461084268,12.));
#249917=CARTESIAN_POINT('Ctrl Pts',(14.7100107213586,17.2063157097315,0.));
#249918=CARTESIAN_POINT('Ctrl Pts',(14.7100107213586,17.2063157097315,12.));
#249919=CARTESIAN_POINT('Ctrl Pts',(14.7153546289339,17.2115510835989,0.));
#249920=CARTESIAN_POINT('Ctrl Pts',(14.7153546289339,17.2115510835989,12.));
#249921=CARTESIAN_POINT('Ctrl Pts',(14.7209039390327,17.2169471814256,0.));
#249922=CARTESIAN_POINT('Ctrl Pts',(14.7209039390327,17.2169471814256,12.));
#249923=CARTESIAN_POINT('Ctrl Pts',(14.7266561494282,17.2224992099667,0.));
#249924=CARTESIAN_POINT('Ctrl Pts',(14.7266561494282,17.2224992099667,12.));
#249925=CARTESIAN_POINT('Ctrl Pts',(14.7326088681163,17.2282025904314,0.));
#249926=CARTESIAN_POINT('Ctrl Pts',(14.7326088681163,17.2282025904314,12.));
#249927=CARTESIAN_POINT('Ctrl Pts',(14.7387597858116,17.2340529062076,0.));
#249928=CARTESIAN_POINT('Ctrl Pts',(14.7387597858116,17.2340529062076,12.));
#249929=CARTESIAN_POINT('Ctrl Pts',(14.7451066593792,17.2400458713565,0.));
#249930=CARTESIAN_POINT('Ctrl Pts',(14.7451066593792,17.2400458713565,12.));
#249931=CARTESIAN_POINT('Ctrl Pts',(14.7516473175124,17.2461773413288,0.));
#249932=CARTESIAN_POINT('Ctrl Pts',(14.7516473175124,17.2461773413288,12.));
#249933=CARTESIAN_POINT('Ctrl Pts',(14.7583796616617,17.2524433146837,0.));
#249934=CARTESIAN_POINT('Ctrl Pts',(14.7583796616617,17.2524433146837,12.));
#249935=CARTESIAN_POINT('Ctrl Pts',(14.7653016697591,17.2588399401465,0.));
#249936=CARTESIAN_POINT('Ctrl Pts',(14.7653016697591,17.2588399401465,12.));
#249937=CARTESIAN_POINT('Ctrl Pts',(14.7724113956731,17.2653635155319,0.));
#249938=CARTESIAN_POINT('Ctrl Pts',(14.7724113956731,17.2653635155319,12.));
#249939=CARTESIAN_POINT('Ctrl Pts',(14.7797069617804,17.2720104735194,0.));
#249940=CARTESIAN_POINT('Ctrl Pts',(14.7797069617804,17.2720104735194,12.));
#249941=CARTESIAN_POINT('Ctrl Pts',(14.787186553128,17.2787773704849,0.));
#249942=CARTESIAN_POINT('Ctrl Pts',(14.787186553128,17.2787773704849,12.));
#249943=CARTESIAN_POINT('Ctrl Pts',(14.7948484105249,17.2856608733196,0.));
#249944=CARTESIAN_POINT('Ctrl Pts',(14.7948484105249,17.2856608733196,12.));
#249945=CARTESIAN_POINT('Ctrl Pts',(14.8026908254276,17.2926577496513,0.));
#249946=CARTESIAN_POINT('Ctrl Pts',(14.8026908254276,17.2926577496513,12.));
#249947=CARTESIAN_POINT('Ctrl Pts',(14.8107121391035,17.299764866148,0.));
#249948=CARTESIAN_POINT('Ctrl Pts',(14.8107121391035,17.299764866148,12.));
#249949=CARTESIAN_POINT('Ctrl Pts',(14.8189107410162,17.3069791853706,0.));
#249950=CARTESIAN_POINT('Ctrl Pts',(14.8189107410162,17.3069791853706,12.));
#249951=CARTESIAN_POINT('Ctrl Pts',(14.8272850675379,17.3142977632659,0.));
#249952=CARTESIAN_POINT('Ctrl Pts',(14.8272850675379,17.3142977632659,12.));
#249953=CARTESIAN_POINT('Ctrl Pts',(14.8358336004197,17.3217177462101,0.));
#249954=CARTESIAN_POINT('Ctrl Pts',(14.8358336004197,17.3217177462101,12.));
#249955=CARTESIAN_POINT('Ctrl Pts',(14.8445548643508,17.3292363662605,0.));
#249956=CARTESIAN_POINT('Ctrl Pts',(14.8445548643508,17.3292363662605,12.));
#249957=CARTESIAN_POINT('Ctrl Pts',(14.8534474245433,17.336850936485,0.));
#249958=CARTESIAN_POINT('Ctrl Pts',(14.8534474245433,17.336850936485,12.));
#249959=CARTESIAN_POINT('Ctrl Pts',(14.8625098843417,17.3445588463475,0.));
#249960=CARTESIAN_POINT('Ctrl Pts',(14.8625098843417,17.3445588463475,12.));
#249961=CARTESIAN_POINT('Ctrl Pts',(14.8717408826955,17.3523575568645,0.));
#249962=CARTESIAN_POINT('Ctrl Pts',(14.8717408826955,17.3523575568645,12.));
#249963=CARTESIAN_POINT('Ctrl Pts',(14.8811390927423,17.3602445978161,0.));
#249964=CARTESIAN_POINT('Ctrl Pts',(14.8811390927423,17.3602445978161,12.));
#249965=CARTESIAN_POINT('Ctrl Pts',(14.8907032205788,17.3682175653235,0.));
#249966=CARTESIAN_POINT('Ctrl Pts',(14.8907032205788,17.3682175653235,12.));
#249967=CARTESIAN_POINT('Ctrl Pts',(14.900432003961,17.3762741193076,0.));
#249968=CARTESIAN_POINT('Ctrl Pts',(14.900432003961,17.3762741193076,12.));
#249969=CARTESIAN_POINT('Ctrl Pts',(14.9103242110057,17.3844119809824,0.));
#249970=CARTESIAN_POINT('Ctrl Pts',(14.9103242110057,17.3844119809824,12.));
#249971=CARTESIAN_POINT('Ctrl Pts',(14.9203786389342,17.3926289303986,0.));
#249972=CARTESIAN_POINT('Ctrl Pts',(14.9203786389342,17.3926289303986,12.));
#249973=CARTESIAN_POINT('Ctrl Pts',(14.9305941128757,17.4009228040749,0.));
#249974=CARTESIAN_POINT('Ctrl Pts',(14.9305941128757,17.4009228040749,12.));
#249975=CARTESIAN_POINT('Ctrl Pts',(14.940969484645,17.4092914926071,0.));
#249976=CARTESIAN_POINT('Ctrl Pts',(14.940969484645,17.4092914926071,12.));
#249977=CARTESIAN_POINT('Ctrl Pts',(14.9515036315143,17.4177329382828,0.));
#249978=CARTESIAN_POINT('Ctrl Pts',(14.9515036315143,17.4177329382828,12.));
#249979=CARTESIAN_POINT('Ctrl Pts',(14.9621954549827,17.426245132709,0.));
#249980=CARTESIAN_POINT('Ctrl Pts',(14.9621954549827,17.426245132709,12.));
#249981=CARTESIAN_POINT('Ctrl Pts',(14.9730438799452,17.4348261151396,0.));
#249982=CARTESIAN_POINT('Ctrl Pts',(14.9730438799452,17.4348261151396,12.));
#249983=CARTESIAN_POINT('Ctrl Pts',(14.9840478538358,17.4434739707773,0.));
#249984=CARTESIAN_POINT('Ctrl Pts',(14.9840478538358,17.4434739707773,12.));
#249985=CARTESIAN_POINT('Ctrl Pts',(14.9952063457778,17.4521868291004,0.));
#249986=CARTESIAN_POINT('Ctrl Pts',(14.9952063457778,17.4521868291004,12.));
#249987=CARTESIAN_POINT('Ctrl Pts',(15.0065183456921,17.4609628621418,0.));
#249988=CARTESIAN_POINT('Ctrl Pts',(15.0065183456921,17.4609628621418,12.));
#249989=CARTESIAN_POINT('Ctrl Pts',(15.0179828635086,17.4698002829357,0.));
#249990=CARTESIAN_POINT('Ctrl Pts',(15.0179828635086,17.4698002829357,12.));
#249991=CARTESIAN_POINT('Ctrl Pts',(15.029598928488,17.4786973441417,0.));
#249992=CARTESIAN_POINT('Ctrl Pts',(15.029598928488,17.4786973441417,12.));
#249993=CARTESIAN_POINT('Ctrl Pts',(15.0413655884993,17.4876523366178,0.));
#249994=CARTESIAN_POINT('Ctrl Pts',(15.0413655884993,17.4876523366178,12.));
#249995=CARTESIAN_POINT('Ctrl Pts',(15.0532819093085,17.4966635880245,0.));
#249996=CARTESIAN_POINT('Ctrl Pts',(15.0532819093085,17.4966635880245,12.));
#249997=CARTESIAN_POINT('Ctrl Pts',(15.0653469738306,17.5057294613874,0.));
#249998=CARTESIAN_POINT('Ctrl Pts',(15.0653469738306,17.5057294613874,12.));
#249999=CARTESIAN_POINT('Ctrl Pts',(15.0775598815748,17.5148483539684,0.));
#250000=CARTESIAN_POINT('Ctrl Pts',(15.0775598815748,17.5148483539684,12.));
#250001=CARTESIAN_POINT('Ctrl Pts',(15.0899197481082,17.5240186961788,0.));
#250002=CARTESIAN_POINT('Ctrl Pts',(15.0899197481082,17.5240186961788,12.));
#250003=CARTESIAN_POINT('Ctrl Pts',(15.1024257045033,17.5332389504829,0.));
#250004=CARTESIAN_POINT('Ctrl Pts',(15.1024257045033,17.5332389504829,12.));
#250005=CARTESIAN_POINT('Ctrl Pts',(15.1150768967729,17.5425076102966,0.));
#250006=CARTESIAN_POINT('Ctrl Pts',(15.1150768967729,17.5425076102966,12.));
#250007=CARTESIAN_POINT('Ctrl Pts',(15.127872485314,17.5518231989122,0.));
#250008=CARTESIAN_POINT('Ctrl Pts',(15.127872485314,17.5518231989122,12.));
#250009=CARTESIAN_POINT('Ctrl Pts',(15.1408116444877,17.5611842686196,0.));
#250010=CARTESIAN_POINT('Ctrl Pts',(15.1408116444877,17.5611842686196,12.));
#250011=CARTESIAN_POINT('Ctrl Pts',(15.1538935621714,17.570589399803,0.));
#250012=CARTESIAN_POINT('Ctrl Pts',(15.1538935621714,17.570589399803,12.));
#250013=CARTESIAN_POINT('Ctrl Pts',(15.1671174393136,17.5800372000539,0.));
#250014=CARTESIAN_POINT('Ctrl Pts',(15.1671174393136,17.5800372000539,12.));
#250015=CARTESIAN_POINT('Ctrl Pts',(15.1804824894605,17.5895263032592,0.));
#250016=CARTESIAN_POINT('Ctrl Pts',(15.1804824894605,17.5895263032592,12.));
#250017=CARTESIAN_POINT('Ctrl Pts',(15.1939879383268,17.5990553687595,0.));
#250018=CARTESIAN_POINT('Ctrl Pts',(15.1939879383268,17.5990553687595,12.));
#250019=CARTESIAN_POINT('Ctrl Pts',(15.2076330234686,17.6086230806497,0.));
#250020=CARTESIAN_POINT('Ctrl Pts',(15.2076330234686,17.6086230806497,12.));
#250021=CARTESIAN_POINT('Ctrl Pts',(15.22141699392,17.6182281470467,0.));
#250022=CARTESIAN_POINT('Ctrl Pts',(15.22141699392,17.6182281470467,12.));
#250023=CARTESIAN_POINT('Ctrl Pts',(15.2353391098367,17.6278692993765,0.));
#250024=CARTESIAN_POINT('Ctrl Pts',(15.2353391098367,17.6278692993765,12.));
#250025=CARTESIAN_POINT('Ctrl Pts',(15.2493986421091,17.637545291637,0.));
#250026=CARTESIAN_POINT('Ctrl Pts',(15.2493986421091,17.637545291637,12.));
#250027=CARTESIAN_POINT('Ctrl Pts',(15.263594872029,17.6472548997329,0.));
#250028=CARTESIAN_POINT('Ctrl Pts',(15.263594872029,17.6472548997329,12.));
#250029=CARTESIAN_POINT('Ctrl Pts',(15.2779270910238,17.6569969209,0.));
#250030=CARTESIAN_POINT('Ctrl Pts',(15.2779270910238,17.6569969209,12.));
#250031=CARTESIAN_POINT('Ctrl Pts',(15.2923946003598,17.6667701731041,0.));
#250032=CARTESIAN_POINT('Ctrl Pts',(15.2923946003598,17.6667701731041,12.));
#250033=CARTESIAN_POINT('Ctrl Pts',(15.3069967108501,17.6765734944559,0.));
#250034=CARTESIAN_POINT('Ctrl Pts',(15.3069967108501,17.6765734944559,12.));
#250035=CARTESIAN_POINT('Ctrl Pts',(15.3217327425341,17.6864057426052,0.));
#250036=CARTESIAN_POINT('Ctrl Pts',(15.3217327425341,17.6864057426052,12.));
#250037=CARTESIAN_POINT('Ctrl Pts',(15.3366020244069,17.6962657941984,0.));
#250038=CARTESIAN_POINT('Ctrl Pts',(15.3366020244069,17.6962657941984,12.));
#250039=CARTESIAN_POINT('Ctrl Pts',(15.3516038942064,17.7061525444044,0.));
#250040=CARTESIAN_POINT('Ctrl Pts',(15.3516038942064,17.7061525444044,12.));
#250041=CARTESIAN_POINT('Ctrl Pts',(15.3667376981702,17.7160649064208,0.));
#250042=CARTESIAN_POINT('Ctrl Pts',(15.3667376981702,17.7160649064208,12.));
#250043=CARTESIAN_POINT('Ctrl Pts',(15.3820027907965,17.7260018109923,0.));
#250044=CARTESIAN_POINT('Ctrl Pts',(15.3820027907965,17.7260018109923,12.));
#250045=CARTESIAN_POINT('Ctrl Pts',(15.3973985345796,17.7359622059143,0.));
#250046=CARTESIAN_POINT('Ctrl Pts',(15.3973985345796,17.7359622059143,12.));
#250047=CARTESIAN_POINT('Ctrl Pts',(15.4129242997828,17.7459450555803,0.));
#250048=CARTESIAN_POINT('Ctrl Pts',(15.4129242997828,17.7459450555803,12.));
#250049=CARTESIAN_POINT('Ctrl Pts',(15.4285794642658,17.7559493405871,0.));
#250050=CARTESIAN_POINT('Ctrl Pts',(15.4285794642658,17.7559493405871,12.));
#250051=CARTESIAN_POINT('Ctrl Pts',(15.4443634132865,17.765974057326,0.));
#250052=CARTESIAN_POINT('Ctrl Pts',(15.4443634132865,17.765974057326,12.));
#250053=CARTESIAN_POINT('Ctrl Pts',(15.4602755393019,17.7760182175817,0.));
#250054=CARTESIAN_POINT('Ctrl Pts',(15.4602755393019,17.7760182175817,12.));
#250055=CARTESIAN_POINT('Ctrl Pts',(15.4763152417506,17.7860808481229,0.));
#250056=CARTESIAN_POINT('Ctrl Pts',(15.4763152417506,17.7860808481229,12.));
#250057=CARTESIAN_POINT('Ctrl Pts',(15.4924819268529,17.7961609903161,0.));
#250058=CARTESIAN_POINT('Ctrl Pts',(15.4924819268529,17.7961609903161,12.));
#250059=CARTESIAN_POINT('Ctrl Pts',(15.5087750074728,17.8062576997964,0.));
#250060=CARTESIAN_POINT('Ctrl Pts',(15.5087750074728,17.8062576997964,12.));
#250061=CARTESIAN_POINT('Ctrl Pts',(15.5251939029558,17.8163700461263,0.));
#250062=CARTESIAN_POINT('Ctrl Pts',(15.5251939029558,17.8163700461263,12.));
#250063=CARTESIAN_POINT('Ctrl Pts',(15.5417380389639,17.8264971124606,0.));
#250064=CARTESIAN_POINT('Ctrl Pts',(15.5417380389639,17.8264971124606,12.));
#250065=CARTESIAN_POINT('Ctrl Pts',(15.5584068472976,17.8366379952078,0.));
#250066=CARTESIAN_POINT('Ctrl Pts',(15.5584068472976,17.8366379952078,12.));
#250067=CARTESIAN_POINT('Ctrl Pts',(15.5751997657153,17.8467918036977,0.));
#250068=CARTESIAN_POINT('Ctrl Pts',(15.5751997657153,17.8467918036977,12.));
#250069=CARTESIAN_POINT('Ctrl Pts',(15.5921162378183,17.8569576598996,0.));
#250070=CARTESIAN_POINT('Ctrl Pts',(15.5921162378183,17.8569576598996,12.));
#250071=CARTESIAN_POINT('Ctrl Pts',(15.6091557129205,17.8671346981388,0.));
#250072=CARTESIAN_POINT('Ctrl Pts',(15.6091557129205,17.8671346981388,12.));
#250073=CARTESIAN_POINT('Ctrl Pts',(15.6263176459107,17.8773220648125,0.));
#250074=CARTESIAN_POINT('Ctrl Pts',(15.6263176459107,17.8773220648125,12.));
#250075=CARTESIAN_POINT('Ctrl Pts',(15.6436014971088,17.8875189181095,0.));
#250076=CARTESIAN_POINT('Ctrl Pts',(15.6436014971088,17.8875189181095,12.));
#250077=CARTESIAN_POINT('Ctrl Pts',(15.6610067321036,17.8977244277247,0.));
#250078=CARTESIAN_POINT('Ctrl Pts',(15.6610067321036,17.8977244277247,12.));
#250079=CARTESIAN_POINT('Ctrl Pts',(15.6785328216467,17.9079377746118,0.));
#250080=CARTESIAN_POINT('Ctrl Pts',(15.6785328216467,17.9079377746118,12.));
#250081=CARTESIAN_POINT('Ctrl Pts',(15.6961792415526,17.918158150746,0.));
#250082=CARTESIAN_POINT('Ctrl Pts',(15.6961792415526,17.918158150746,12.));
#250083=CARTESIAN_POINT('Ctrl Pts',(15.713945472584,17.9283847588837,0.));
#250084=CARTESIAN_POINT('Ctrl Pts',(15.713945472584,17.9283847588837,12.));
#250085=CARTESIAN_POINT('Ctrl Pts',(15.7318310003334,17.9386168123261,0.));
#250086=CARTESIAN_POINT('Ctrl Pts',(15.7318310003334,17.9386168123261,12.));
#250087=CARTESIAN_POINT('Ctrl Pts',(15.7498353150856,17.9488535346776,0.));
#250088=CARTESIAN_POINT('Ctrl Pts',(15.7498353150856,17.9488535346776,12.));
#250089=CARTESIAN_POINT('Ctrl Pts',(15.7679579117072,17.9590941596236,0.));
#250090=CARTESIAN_POINT('Ctrl Pts',(15.7679579117072,17.9590941596236,12.));
#250091=CARTESIAN_POINT('Ctrl Pts',(15.786198289572,17.9693379307297,0.));
#250092=CARTESIAN_POINT('Ctrl Pts',(15.786198289572,17.9693379307297,12.));
#250093=CARTESIAN_POINT('Ctrl Pts',(15.8045559524674,17.9795841012383,0.));
#250094=CARTESIAN_POINT('Ctrl Pts',(15.8045559524674,17.9795841012383,12.));
#250095=CARTESIAN_POINT('Ctrl Pts',(15.8230304084963,17.9898319338664,0.));
#250096=CARTESIAN_POINT('Ctrl Pts',(15.8230304084963,17.9898319338664,12.));
#250097=CARTESIAN_POINT('Ctrl Pts',(15.8416211699681,18.0000807006055,0.));
#250098=CARTESIAN_POINT('Ctrl Pts',(15.8416211699681,18.0000807006055,12.));
#250099=CARTESIAN_POINT('Ctrl Pts',(15.8603277532834,18.010329682521,0.));
#250100=CARTESIAN_POINT('Ctrl Pts',(15.8603277532834,18.010329682521,12.));
#250101=CARTESIAN_POINT('Ctrl Pts',(15.8791496788685,18.0205781695773,0.));
#250102=CARTESIAN_POINT('Ctrl Pts',(15.8791496788685,18.0205781695773,12.));
#250103=CARTESIAN_POINT('Ctrl Pts',(15.8980864711043,18.0308254604638,0.));
#250104=CARTESIAN_POINT('Ctrl Pts',(15.8980864711043,18.0308254604638,12.));
#250105=CARTESIAN_POINT('Ctrl Pts',(15.9171376582436,18.0410708624208,0.));
#250106=CARTESIAN_POINT('Ctrl Pts',(15.9171376582436,18.0410708624208,12.));
#250107=CARTESIAN_POINT('Ctrl Pts',(15.9363027723244,18.0513136910691,0.));
#250108=CARTESIAN_POINT('Ctrl Pts',(15.9363027723244,18.0513136910691,12.));
#250109=CARTESIAN_POINT('Ctrl Pts',(15.9555813490645,18.061553270236,0.));
#250110=CARTESIAN_POINT('Ctrl Pts',(15.9555813490645,18.061553270236,12.));
#250111=CARTESIAN_POINT('Ctrl Pts',(15.9749729277848,18.071788931796,0.));
#250112=CARTESIAN_POINT('Ctrl Pts',(15.9749729277848,18.071788931796,12.));
#250113=CARTESIAN_POINT('Ctrl Pts',(15.9944770513616,18.0820200155239,0.));
#250114=CARTESIAN_POINT('Ctrl Pts',(15.9944770513616,18.0820200155239,12.));
#250115=CARTESIAN_POINT('Ctrl Pts',(16.0140932661612,18.0922458689464,0.));
#250116=CARTESIAN_POINT('Ctrl Pts',(16.0140932661612,18.0922458689464,12.));
#250117=CARTESIAN_POINT('Ctrl Pts',(16.0338211219693,18.1024658471966,0.));
#250118=CARTESIAN_POINT('Ctrl Pts',(16.0338211219693,18.1024658471966,12.));
#250119=CARTESIAN_POINT('Ctrl Pts',(16.0536601719124,18.1126793128688,0.));
#250120=CARTESIAN_POINT('Ctrl Pts',(16.0536601719124,18.1126793128688,12.));
#250121=CARTESIAN_POINT('Ctrl Pts',(16.0736099723664,18.1228856358746,0.));
#250122=CARTESIAN_POINT('Ctrl Pts',(16.0736099723664,18.1228856358746,12.));
#250123=CARTESIAN_POINT('Ctrl Pts',(16.0936700829108,18.1330841933099,0.));
#250124=CARTESIAN_POINT('Ctrl Pts',(16.0936700829108,18.1330841933099,12.));
#250125=CARTESIAN_POINT('Ctrl Pts',(16.113840066279,18.1432743693231,0.));
#250126=CARTESIAN_POINT('Ctrl Pts',(16.113840066279,18.1432743693231,12.));
#250127=CARTESIAN_POINT('Ctrl Pts',(16.1341194882987,18.1534555549851,0.));
#250128=CARTESIAN_POINT('Ctrl Pts',(16.1341194882987,18.1534555549851,12.));
#250129=CARTESIAN_POINT('Ctrl Pts',(16.1545079178261,18.1636271481616,0.));
#250130=CARTESIAN_POINT('Ctrl Pts',(16.1545079178261,18.1636271481616,12.));
#250131=CARTESIAN_POINT('Ctrl Pts',(16.1750049266673,18.1737885533852,0.));
#250132=CARTESIAN_POINT('Ctrl Pts',(16.1750049266673,18.1737885533852,12.));
#250133=CARTESIAN_POINT('Ctrl Pts',(16.1956100895076,18.1839391817335,0.));
#250134=CARTESIAN_POINT('Ctrl Pts',(16.1956100895076,18.1839391817335,12.));
#250135=CARTESIAN_POINT('Ctrl Pts',(16.2163229838878,18.1940784507232,0.));
#250136=CARTESIAN_POINT('Ctrl Pts',(16.2163229838878,18.1940784507232,12.));
#250137=CARTESIAN_POINT('Ctrl Pts',(16.237143190164,18.2042057842037,0.));
#250138=CARTESIAN_POINT('Ctrl Pts',(16.237143190164,18.2042057842037,12.));
#250139=CARTESIAN_POINT('Ctrl Pts',(16.2580702914615,18.214320612253,0.));
#250140=CARTESIAN_POINT('Ctrl Pts',(16.2580702914615,18.214320612253,12.));
#250141=CARTESIAN_POINT('Ctrl Pts',(16.2791038736223,18.2244223710745,0.));
#250142=CARTESIAN_POINT('Ctrl Pts',(16.2791038736223,18.2244223710745,12.));
#250143=CARTESIAN_POINT('Ctrl Pts',(16.3002435251378,18.2345105028981,0.));
#250144=CARTESIAN_POINT('Ctrl Pts',(16.3002435251378,18.2345105028981,12.));
#250145=CARTESIAN_POINT('Ctrl Pts',(16.3214888370988,18.2445844558742,0.));
#250146=CARTESIAN_POINT('Ctrl Pts',(16.3214888370988,18.2445844558742,12.));
#250147=CARTESIAN_POINT('Ctrl Pts',(16.342839403159,18.2546436839609,0.));
#250148=CARTESIAN_POINT('Ctrl Pts',(16.342839403159,18.2546436839609,12.));
#250149=CARTESIAN_POINT('Ctrl Pts',(16.3642948194869,18.2646876468169,0.));
#250150=CARTESIAN_POINT('Ctrl Pts',(16.3642948194869,18.2646876468169,12.));
#250151=CARTESIAN_POINT('Ctrl Pts',(16.385854684708,18.2747158096934,0.));
#250152=CARTESIAN_POINT('Ctrl Pts',(16.385854684708,18.2747158096934,12.));
#250153=CARTESIAN_POINT('Ctrl Pts',(16.4075185998454,18.2847276433308,0.));
#250154=CARTESIAN_POINT('Ctrl Pts',(16.4075185998454,18.2847276433308,12.));
#250155=CARTESIAN_POINT('Ctrl Pts',(16.4292861682377,18.2947226238509,0.));
#250156=CARTESIAN_POINT('Ctrl Pts',(16.4292861682377,18.2947226238509,12.));
#250157=CARTESIAN_POINT('Ctrl Pts',(16.4511569955231,18.3047002326858,0.));
#250158=CARTESIAN_POINT('Ctrl Pts',(16.4511569955231,18.3047002326858,12.));
#250159=CARTESIAN_POINT('Ctrl Pts',(16.4731306896439,18.3146599565229,0.));
#250160=CARTESIAN_POINT('Ctrl Pts',(16.4731306896439,18.3146599565229,12.));
#250161=CARTESIAN_POINT('Ctrl Pts',(16.4952068608344,18.3246012872468,0.));
#250162=CARTESIAN_POINT('Ctrl Pts',(16.4952068608344,18.3246012872468,12.));
#250163=CARTESIAN_POINT('Ctrl Pts',(16.5173851216045,18.3345237218864,0.));
#250164=CARTESIAN_POINT('Ctrl Pts',(16.5173851216045,18.3345237218864,12.));
#250165=CARTESIAN_POINT('Ctrl Pts',(16.5396650867139,18.3444267625601,0.));
#250166=CARTESIAN_POINT('Ctrl Pts',(16.5396650867139,18.3444267625601,12.));
#250167=CARTESIAN_POINT('Ctrl Pts',(16.5620463731414,18.3543099164331,0.));
#250168=CARTESIAN_POINT('Ctrl Pts',(16.5620463731414,18.3543099164331,12.));
#250169=CARTESIAN_POINT('Ctrl Pts',(16.5845286000218,18.364172695589,0.));
#250170=CARTESIAN_POINT('Ctrl Pts',(16.5845286000218,18.364172695589,12.));
#250171=CARTESIAN_POINT('Ctrl Pts',(16.6071113885711,18.3740146168879,0.));
#250172=CARTESIAN_POINT('Ctrl Pts',(16.6071113885711,18.3740146168879,12.));
#250173=CARTESIAN_POINT('Ctrl Pts',(16.6297943620056,18.3838352018327,0.));
#250174=CARTESIAN_POINT('Ctrl Pts',(16.6297943620056,18.3838352018327,12.));
#250175=CARTESIAN_POINT('Ctrl Pts',(16.6525771454513,18.3936339764332,0.));
#250176=CARTESIAN_POINT('Ctrl Pts',(16.6525771454513,18.3936339764332,12.));
#250177=CARTESIAN_POINT('Ctrl Pts',(16.6754593658513,18.4034104710789,0.));
#250178=CARTESIAN_POINT('Ctrl Pts',(16.6754593658513,18.4034104710789,12.));
#250179=CARTESIAN_POINT('Ctrl Pts',(16.698440651849,18.413164220399,0.));
#250180=CARTESIAN_POINT('Ctrl Pts',(16.698440651849,18.413164220399,12.));
#250181=CARTESIAN_POINT('Ctrl Pts',(16.7215206338818,18.4228947633186,0.));
#250182=CARTESIAN_POINT('Ctrl Pts',(16.7215206338818,18.4228947633186,12.));
#250183=CARTESIAN_POINT('Ctrl Pts',(16.7446989442882,18.4326016431392,0.));
#250184=CARTESIAN_POINT('Ctrl Pts',(16.7446989442882,18.4326016431392,12.));
#250185=CARTESIAN_POINT('Ctrl Pts',(16.7679752173992,18.4422844076099,0.));
#250186=CARTESIAN_POINT('Ctrl Pts',(16.7679752173992,18.4422844076099,12.));
#250187=CARTESIAN_POINT('Ctrl Pts',(16.791349089629,18.4519426090124,0.));
#250188=CARTESIAN_POINT('Ctrl Pts',(16.791349089629,18.4519426090124,12.));
#250189=CARTESIAN_POINT('Ctrl Pts',(16.8148201995472,18.4615758042305,0.));
#250190=CARTESIAN_POINT('Ctrl Pts',(16.8148201995472,18.4615758042305,12.));
#250191=CARTESIAN_POINT('Ctrl Pts',(16.8383881879707,18.4711835548622,0.));
#250192=CARTESIAN_POINT('Ctrl Pts',(16.8383881879707,18.4711835548622,12.));
#250193=CARTESIAN_POINT('Ctrl Pts',(16.8620526977169,18.4807654268769,0.));
#250194=CARTESIAN_POINT('Ctrl Pts',(16.8620526977169,18.4807654268769,12.));
#250195=CARTESIAN_POINT('Ctrl Pts',(16.8858133733086,18.4903209902226,0.));
#250196=CARTESIAN_POINT('Ctrl Pts',(16.8858133733086,18.4903209902226,12.));
#250197=CARTESIAN_POINT('Ctrl Pts',(16.9096698606942,18.4998498184619,0.));
#250198=CARTESIAN_POINT('Ctrl Pts',(16.9096698606942,18.4998498184619,12.));
#250199=CARTESIAN_POINT('Ctrl Pts',(16.9336218069353,18.5093514883835,0.));
#250200=CARTESIAN_POINT('Ctrl Pts',(16.9336218069353,18.5093514883835,12.));
#250201=CARTESIAN_POINT('Ctrl Pts',(16.957668859934,18.518825579666,0.));
#250202=CARTESIAN_POINT('Ctrl Pts',(16.957668859934,18.518825579666,12.));
#250203=CARTESIAN_POINT('Ctrl Pts',(16.9818106680382,18.5282716744198,0.));
#250204=CARTESIAN_POINT('Ctrl Pts',(16.9818106680382,18.5282716744198,12.));
#250205=CARTESIAN_POINT('Ctrl Pts',(17.0060468805099,18.5376893576961,0.));
#250206=CARTESIAN_POINT('Ctrl Pts',(17.0060468805099,18.5376893576961,12.));
#250207=CARTESIAN_POINT('Ctrl Pts',(17.030377148174,18.5470782182089,0.));
#250208=CARTESIAN_POINT('Ctrl Pts',(17.030377148174,18.5470782182089,12.));
#250209=CARTESIAN_POINT('Ctrl Pts',(17.0548011239751,18.5564378489628,0.));
#250210=CARTESIAN_POINT('Ctrl Pts',(17.0548011239751,18.5564378489628,12.));
#250211=CARTESIAN_POINT('Ctrl Pts',(17.0793184636079,18.5657678479788,0.));
#250212=CARTESIAN_POINT('Ctrl Pts',(17.0793184636079,18.5657678479788,12.));
#250213=CARTESIAN_POINT('Ctrl Pts',(17.1039288260001,18.5750678188543,0.));
#250214=CARTESIAN_POINT('Ctrl Pts',(17.1039288260001,18.5750678188543,12.));
#250215=CARTESIAN_POINT('Ctrl Pts',(17.1286318741185,18.5843373717253,0.));
#250216=CARTESIAN_POINT('Ctrl Pts',(17.1286318741185,18.5843373717253,12.));
#250217=CARTESIAN_POINT('Ctrl Pts',(17.1534272741646,18.5935761222833,0.));
#250218=CARTESIAN_POINT('Ctrl Pts',(17.1534272741646,18.5935761222833,12.));
#250219=CARTESIAN_POINT('Ctrl Pts',(17.1783146940131,18.6027836898826,0.));
#250220=CARTESIAN_POINT('Ctrl Pts',(17.1783146940131,18.6027836898826,12.));
#250221=CARTESIAN_POINT('Ctrl Pts',(17.2032938019288,18.6119596959957,0.));
#250222=CARTESIAN_POINT('Ctrl Pts',(17.2032938019288,18.6119596959957,12.));
#250223=CARTESIAN_POINT('Ctrl Pts',(17.2283642650519,18.6211037624041,0.));
#250224=CARTESIAN_POINT('Ctrl Pts',(17.2283642650519,18.6211037624041,12.));
#250225=CARTESIAN_POINT('Ctrl Pts',(17.2535257482186,18.630215509794,0.));
#250226=CARTESIAN_POINT('Ctrl Pts',(17.2535257482186,18.630215509794,12.));
#250227=CARTESIAN_POINT('Ctrl Pts',(17.278777912021,18.639294555474,0.));
#250228=CARTESIAN_POINT('Ctrl Pts',(17.278777912021,18.639294555474,12.));
#250229=CARTESIAN_POINT('Ctrl Pts',(17.3041204135069,18.6483405141853,0.));
#250230=CARTESIAN_POINT('Ctrl Pts',(17.3041204135069,18.6483405141853,12.));
#250231=CARTESIAN_POINT('Ctrl Pts',(17.3295529098612,18.6573530024019,0.));
#250232=CARTESIAN_POINT('Ctrl Pts',(17.3295529098612,18.6573530024019,12.));
#250233=CARTESIAN_POINT('Ctrl Pts',(17.3550750612438,18.6663316416569,0.));
#250234=CARTESIAN_POINT('Ctrl Pts',(17.3550750612438,18.6663316416569,12.));
#250235=CARTESIAN_POINT('Ctrl Pts',(17.3806865340744,18.6752760624045,0.));
#250236=CARTESIAN_POINT('Ctrl Pts',(17.3806865340744,18.6752760624045,12.));
#250237=CARTESIAN_POINT('Ctrl Pts',(17.4063870038563,18.6841859073472,0.));
#250238=CARTESIAN_POINT('Ctrl Pts',(17.4063870038563,18.6841859073472,12.));
#250239=CARTESIAN_POINT('Ctrl Pts',(17.4321761588148,18.6930608357421,0.));
#250240=CARTESIAN_POINT('Ctrl Pts',(17.4321761588148,18.6930608357421,12.));
#250241=CARTESIAN_POINT('Ctrl Pts',(17.4580537012764,18.7019005250322,0.));
#250242=CARTESIAN_POINT('Ctrl Pts',(17.4580537012764,18.7019005250322,12.));
#250243=CARTESIAN_POINT('Ctrl Pts',(17.4840193397176,18.7107046613941,0.));
#250244=CARTESIAN_POINT('Ctrl Pts',(17.4840193397176,18.7107046613941,12.));
#250245=CARTESIAN_POINT('Ctrl Pts',(17.5100727820891,18.7194729318128,0.));
#250246=CARTESIAN_POINT('Ctrl Pts',(17.5100727820891,18.7194729318128,12.));
#250247=CARTESIAN_POINT('Ctrl Pts',(17.5362137287604,18.728205015716,0.));
#250248=CARTESIAN_POINT('Ctrl Pts',(17.5362137287604,18.728205015716,12.));
#250249=CARTESIAN_POINT('Ctrl Pts',(17.5624418653248,18.7369005764558,0.));
#250250=CARTESIAN_POINT('Ctrl Pts',(17.5624418653248,18.7369005764558,12.));
#250251=CARTESIAN_POINT('Ctrl Pts',(17.5887568561361,18.7455592536667,0.));
#250252=CARTESIAN_POINT('Ctrl Pts',(17.5887568561361,18.7455592536667,12.));
#250253=CARTESIAN_POINT('Ctrl Pts',(17.6151583356988,18.7541806530935,0.));
#250254=CARTESIAN_POINT('Ctrl Pts',(17.6151583356988,18.7541806530935,12.));
#250255=CARTESIAN_POINT('Ctrl Pts',(17.6416459210646,18.7627643613139,0.));
#250256=CARTESIAN_POINT('Ctrl Pts',(17.6416459210646,18.7627643613139,12.));
#250257=CARTESIAN_POINT('Ctrl Pts',(17.6682192274197,18.7713099642673,0.));
#250258=CARTESIAN_POINT('Ctrl Pts',(17.6682192274197,18.7713099642673,12.));
#250259=CARTESIAN_POINT('Ctrl Pts',(17.6948778822981,18.7798170641305,0.));
#250260=CARTESIAN_POINT('Ctrl Pts',(17.6948778822981,18.7798170641305,12.));
#250261=CARTESIAN_POINT('Ctrl Pts',(17.7216215409019,18.7882852976016,0.));
#250262=CARTESIAN_POINT('Ctrl Pts',(17.7216215409019,18.7882852976016,12.));
#250263=CARTESIAN_POINT('Ctrl Pts',(17.7484498996916,18.7967143519444,0.));
#250264=CARTESIAN_POINT('Ctrl Pts',(17.7484498996916,18.7967143519444,12.));
#250265=CARTESIAN_POINT('Ctrl Pts',(17.7753627137898,18.8051039860543,0.));
#250266=CARTESIAN_POINT('Ctrl Pts',(17.7753627137898,18.8051039860543,12.));
#250267=CARTESIAN_POINT('Ctrl Pts',(17.8023598011135,18.8134540340581,0.));
#250268=CARTESIAN_POINT('Ctrl Pts',(17.8023598011135,18.8134540340581,12.));
#250269=CARTESIAN_POINT('Ctrl Pts',(17.8294410311105,18.8217643886368,0.));
#250270=CARTESIAN_POINT('Ctrl Pts',(17.8294410311105,18.8217643886368,12.));
#250271=CARTESIAN_POINT('Ctrl Pts',(17.8566063174871,18.8300349896187,0.));
#250272=CARTESIAN_POINT('Ctrl Pts',(17.8566063174871,18.8300349896187,12.));
#250273=CARTESIAN_POINT('Ctrl Pts',(17.8784057509434,18.8366196462746,0.));
#250274=CARTESIAN_POINT('Ctrl Pts',(17.8784057509434,18.8366196462746,12.));
#250275=CARTESIAN_POINT('Ctrl Pts',(17.8947931177853,18.8415402351882,0.));
#250276=CARTESIAN_POINT('Ctrl Pts',(17.8947931177853,18.8415402351882,12.));
#250277=CARTESIAN_POINT('Ctrl Pts',(17.9057348246611,18.8448126709726,0.));
#250278=CARTESIAN_POINT('Ctrl Pts',(17.9057348246611,18.8448126709726,12.));
#250279=CARTESIAN_POINT('Ctrl Pts',(17.9112098770111,18.8464468996588,0.));
#250280=CARTESIAN_POINT('Ctrl Pts',(17.9112098770111,18.8464468996588,12.));
#250281=CARTESIAN_POINT('',(17.9112098770111,18.8464468996588,0.));
#250282=CARTESIAN_POINT('Ctrl Pts',(14.6513681262571,17.1452095830633,0.));
#250283=CARTESIAN_POINT('Ctrl Pts',(14.6513711852843,17.1452153999142,0.));
#250284=CARTESIAN_POINT('Ctrl Pts',(14.6514066997196,17.1452600887037,0.));
#250285=CARTESIAN_POINT('Ctrl Pts',(14.6515481598068,17.1454262858043,0.));
#250286=CARTESIAN_POINT('Ctrl Pts',(14.6519131634508,17.1458462295271,0.));
#250287=CARTESIAN_POINT('Ctrl Pts',(14.6526624064978,17.1466998098673,0.));
#250288=CARTESIAN_POINT('Ctrl Pts',(14.6537016966184,17.147876394491,0.));
#250289=CARTESIAN_POINT('Ctrl Pts',(14.655024862281,17.1493641837558,0.));
#250290=CARTESIAN_POINT('Ctrl Pts',(14.6566237952435,17.1511476869496,0.));
#250291=CARTESIAN_POINT('Ctrl Pts',(14.6584900555302,17.1532107762718,0.));
#250292=CARTESIAN_POINT('Ctrl Pts',(14.6606167169642,17.1555401986401,0.));
#250293=CARTESIAN_POINT('Ctrl Pts',(14.6629987285992,17.1581262646789,0.));
#250294=CARTESIAN_POINT('Ctrl Pts',(14.6656319165057,17.1609609517369,0.));
#250295=CARTESIAN_POINT('Ctrl Pts',(14.6685123374423,17.1640366762305,0.));
#250296=CARTESIAN_POINT('Ctrl Pts',(14.671635583332,17.167344972302,0.));
#250297=CARTESIAN_POINT('Ctrl Pts',(14.6749971333867,17.1708771619129,0.));
#250298=CARTESIAN_POINT('Ctrl Pts',(14.6785925615677,17.1746247499057,0.));
#250299=CARTESIAN_POINT('Ctrl Pts',(14.6824178576167,17.1785800350826,0.));
#250300=CARTESIAN_POINT('Ctrl Pts',(14.686469452232,17.182736158472,0.));
#250301=CARTESIAN_POINT('Ctrl Pts',(14.6907440526958,17.1870867909918,0.));
#250302=CARTESIAN_POINT('Ctrl Pts',(14.6952385361705,17.1916259308415,0.));
#250303=CARTESIAN_POINT('Ctrl Pts',(14.699949811582,17.1963476411694,0.));
#250304=CARTESIAN_POINT('Ctrl Pts',(14.7048748502663,17.2012461084268,0.));
#250305=CARTESIAN_POINT('Ctrl Pts',(14.7100107213586,17.2063157097315,0.));
#250306=CARTESIAN_POINT('Ctrl Pts',(14.7153546289339,17.2115510835989,0.));
#250307=CARTESIAN_POINT('Ctrl Pts',(14.7209039390327,17.2169471814256,0.));
#250308=CARTESIAN_POINT('Ctrl Pts',(14.7266561494282,17.2224992099667,0.));
#250309=CARTESIAN_POINT('Ctrl Pts',(14.7326088681163,17.2282025904314,0.));
#250310=CARTESIAN_POINT('Ctrl Pts',(14.7387597858116,17.2340529062076,0.));
#250311=CARTESIAN_POINT('Ctrl Pts',(14.7451066593792,17.2400458713565,0.));
#250312=CARTESIAN_POINT('Ctrl Pts',(14.7516473175124,17.2461773413288,0.));
#250313=CARTESIAN_POINT('Ctrl Pts',(14.7583796616617,17.2524433146837,0.));
#250314=CARTESIAN_POINT('Ctrl Pts',(14.7653016697591,17.2588399401465,0.));
#250315=CARTESIAN_POINT('Ctrl Pts',(14.7724113956731,17.2653635155319,0.));
#250316=CARTESIAN_POINT('Ctrl Pts',(14.7797069617804,17.2720104735194,0.));
#250317=CARTESIAN_POINT('Ctrl Pts',(14.787186553128,17.2787773704849,0.));
#250318=CARTESIAN_POINT('Ctrl Pts',(14.7948484105249,17.2856608733196,0.));
#250319=CARTESIAN_POINT('Ctrl Pts',(14.8026908254276,17.2926577496513,0.));
#250320=CARTESIAN_POINT('Ctrl Pts',(14.8107121391035,17.299764866148,0.));
#250321=CARTESIAN_POINT('Ctrl Pts',(14.8189107410162,17.3069791853706,0.));
#250322=CARTESIAN_POINT('Ctrl Pts',(14.8272850675379,17.3142977632659,0.));
#250323=CARTESIAN_POINT('Ctrl Pts',(14.8358336004197,17.3217177462101,0.));
#250324=CARTESIAN_POINT('Ctrl Pts',(14.8445548643508,17.3292363662605,0.));
#250325=CARTESIAN_POINT('Ctrl Pts',(14.8534474245433,17.336850936485,0.));
#250326=CARTESIAN_POINT('Ctrl Pts',(14.8625098843417,17.3445588463475,0.));
#250327=CARTESIAN_POINT('Ctrl Pts',(14.8717408826955,17.3523575568645,0.));
#250328=CARTESIAN_POINT('Ctrl Pts',(14.8811390927423,17.3602445978161,0.));
#250329=CARTESIAN_POINT('Ctrl Pts',(14.8907032205788,17.3682175653235,0.));
#250330=CARTESIAN_POINT('Ctrl Pts',(14.900432003961,17.3762741193076,0.));
#250331=CARTESIAN_POINT('Ctrl Pts',(14.9103242110057,17.3844119809824,0.));
#250332=CARTESIAN_POINT('Ctrl Pts',(14.9203786389342,17.3926289303986,0.));
#250333=CARTESIAN_POINT('Ctrl Pts',(14.9305941128757,17.4009228040749,0.));
#250334=CARTESIAN_POINT('Ctrl Pts',(14.940969484645,17.4092914926071,0.));
#250335=CARTESIAN_POINT('Ctrl Pts',(14.9515036315143,17.4177329382828,0.));
#250336=CARTESIAN_POINT('Ctrl Pts',(14.9621954549827,17.426245132709,0.));
#250337=CARTESIAN_POINT('Ctrl Pts',(14.9730438799452,17.4348261151396,0.));
#250338=CARTESIAN_POINT('Ctrl Pts',(14.9840478538358,17.4434739707773,0.));
#250339=CARTESIAN_POINT('Ctrl Pts',(14.9952063457778,17.4521868291004,0.));
#250340=CARTESIAN_POINT('Ctrl Pts',(15.0065183456921,17.4609628621418,0.));
#250341=CARTESIAN_POINT('Ctrl Pts',(15.0179828635086,17.4698002829357,0.));
#250342=CARTESIAN_POINT('Ctrl Pts',(15.029598928488,17.4786973441417,0.));
#250343=CARTESIAN_POINT('Ctrl Pts',(15.0413655884993,17.4876523366178,0.));
#250344=CARTESIAN_POINT('Ctrl Pts',(15.0532819093085,17.4966635880245,0.));
#250345=CARTESIAN_POINT('Ctrl Pts',(15.0653469738306,17.5057294613874,0.));
#250346=CARTESIAN_POINT('Ctrl Pts',(15.0775598815748,17.5148483539684,0.));
#250347=CARTESIAN_POINT('Ctrl Pts',(15.0899197481082,17.5240186961788,0.));
#250348=CARTESIAN_POINT('Ctrl Pts',(15.1024257045033,17.5332389504829,0.));
#250349=CARTESIAN_POINT('Ctrl Pts',(15.1150768967729,17.5425076102966,0.));
#250350=CARTESIAN_POINT('Ctrl Pts',(15.127872485314,17.5518231989122,0.));
#250351=CARTESIAN_POINT('Ctrl Pts',(15.1408116444877,17.5611842686196,0.));
#250352=CARTESIAN_POINT('Ctrl Pts',(15.1538935621714,17.570589399803,0.));
#250353=CARTESIAN_POINT('Ctrl Pts',(15.1671174393136,17.5800372000539,0.));
#250354=CARTESIAN_POINT('Ctrl Pts',(15.1804824894605,17.5895263032592,0.));
#250355=CARTESIAN_POINT('Ctrl Pts',(15.1939879383268,17.5990553687595,0.));
#250356=CARTESIAN_POINT('Ctrl Pts',(15.2076330234686,17.6086230806497,0.));
#250357=CARTESIAN_POINT('Ctrl Pts',(15.22141699392,17.6182281470467,0.));
#250358=CARTESIAN_POINT('Ctrl Pts',(15.2353391098367,17.6278692993765,0.));
#250359=CARTESIAN_POINT('Ctrl Pts',(15.2493986421091,17.637545291637,0.));
#250360=CARTESIAN_POINT('Ctrl Pts',(15.263594872029,17.6472548997329,0.));
#250361=CARTESIAN_POINT('Ctrl Pts',(15.2779270910238,17.6569969209,0.));
#250362=CARTESIAN_POINT('Ctrl Pts',(15.2923946003598,17.6667701731041,0.));
#250363=CARTESIAN_POINT('Ctrl Pts',(15.3069967108501,17.6765734944559,0.));
#250364=CARTESIAN_POINT('Ctrl Pts',(15.3217327425341,17.6864057426052,0.));
#250365=CARTESIAN_POINT('Ctrl Pts',(15.3366020244069,17.6962657941984,0.));
#250366=CARTESIAN_POINT('Ctrl Pts',(15.3516038942064,17.7061525444044,0.));
#250367=CARTESIAN_POINT('Ctrl Pts',(15.3667376981702,17.7160649064208,0.));
#250368=CARTESIAN_POINT('Ctrl Pts',(15.3820027907965,17.7260018109923,0.));
#250369=CARTESIAN_POINT('Ctrl Pts',(15.3973985345796,17.7359622059143,0.));
#250370=CARTESIAN_POINT('Ctrl Pts',(15.4129242997828,17.7459450555803,0.));
#250371=CARTESIAN_POINT('Ctrl Pts',(15.4285794642658,17.7559493405871,0.));
#250372=CARTESIAN_POINT('Ctrl Pts',(15.4443634132865,17.765974057326,0.));
#250373=CARTESIAN_POINT('Ctrl Pts',(15.4602755393019,17.7760182175817,0.));
#250374=CARTESIAN_POINT('Ctrl Pts',(15.4763152417506,17.7860808481229,0.));
#250375=CARTESIAN_POINT('Ctrl Pts',(15.4924819268529,17.7961609903161,0.));
#250376=CARTESIAN_POINT('Ctrl Pts',(15.5087750074728,17.8062576997964,0.));
#250377=CARTESIAN_POINT('Ctrl Pts',(15.5251939029558,17.8163700461263,0.));
#250378=CARTESIAN_POINT('Ctrl Pts',(15.5417380389639,17.8264971124606,0.));
#250379=CARTESIAN_POINT('Ctrl Pts',(15.5584068472976,17.8366379952078,0.));
#250380=CARTESIAN_POINT('Ctrl Pts',(15.5751997657153,17.8467918036977,0.));
#250381=CARTESIAN_POINT('Ctrl Pts',(15.5921162378183,17.8569576598996,0.));
#250382=CARTESIAN_POINT('Ctrl Pts',(15.6091557129205,17.8671346981388,0.));
#250383=CARTESIAN_POINT('Ctrl Pts',(15.6263176459107,17.8773220648125,0.));
#250384=CARTESIAN_POINT('Ctrl Pts',(15.6436014971088,17.8875189181095,0.));
#250385=CARTESIAN_POINT('Ctrl Pts',(15.6610067321036,17.8977244277247,0.));
#250386=CARTESIAN_POINT('Ctrl Pts',(15.6785328216467,17.9079377746118,0.));
#250387=CARTESIAN_POINT('Ctrl Pts',(15.6961792415526,17.918158150746,0.));
#250388=CARTESIAN_POINT('Ctrl Pts',(15.713945472584,17.9283847588837,0.));
#250389=CARTESIAN_POINT('Ctrl Pts',(15.7318310003334,17.9386168123261,0.));
#250390=CARTESIAN_POINT('Ctrl Pts',(15.7498353150856,17.9488535346776,0.));
#250391=CARTESIAN_POINT('Ctrl Pts',(15.7679579117072,17.9590941596236,0.));
#250392=CARTESIAN_POINT('Ctrl Pts',(15.786198289572,17.9693379307297,0.));
#250393=CARTESIAN_POINT('Ctrl Pts',(15.8045559524674,17.9795841012383,0.));
#250394=CARTESIAN_POINT('Ctrl Pts',(15.8230304084963,17.9898319338664,0.));
#250395=CARTESIAN_POINT('Ctrl Pts',(15.8416211699681,18.0000807006055,0.));
#250396=CARTESIAN_POINT('Ctrl Pts',(15.8603277532834,18.010329682521,0.));
#250397=CARTESIAN_POINT('Ctrl Pts',(15.8791496788685,18.0205781695773,0.));
#250398=CARTESIAN_POINT('Ctrl Pts',(15.8980864711043,18.0308254604638,0.));
#250399=CARTESIAN_POINT('Ctrl Pts',(15.9171376582436,18.0410708624208,0.));
#250400=CARTESIAN_POINT('Ctrl Pts',(15.9363027723244,18.0513136910691,0.));
#250401=CARTESIAN_POINT('Ctrl Pts',(15.9555813490645,18.061553270236,0.));
#250402=CARTESIAN_POINT('Ctrl Pts',(15.9749729277848,18.071788931796,0.));
#250403=CARTESIAN_POINT('Ctrl Pts',(15.9944770513616,18.0820200155239,0.));
#250404=CARTESIAN_POINT('Ctrl Pts',(16.0140932661612,18.0922458689464,0.));
#250405=CARTESIAN_POINT('Ctrl Pts',(16.0338211219693,18.1024658471966,0.));
#250406=CARTESIAN_POINT('Ctrl Pts',(16.0536601719124,18.1126793128688,0.));
#250407=CARTESIAN_POINT('Ctrl Pts',(16.0736099723664,18.1228856358746,0.));
#250408=CARTESIAN_POINT('Ctrl Pts',(16.0936700829108,18.1330841933099,0.));
#250409=CARTESIAN_POINT('Ctrl Pts',(16.113840066279,18.1432743693231,0.));
#250410=CARTESIAN_POINT('Ctrl Pts',(16.1341194882987,18.1534555549851,0.));
#250411=CARTESIAN_POINT('Ctrl Pts',(16.1545079178261,18.1636271481616,0.));
#250412=CARTESIAN_POINT('Ctrl Pts',(16.1750049266673,18.1737885533852,0.));
#250413=CARTESIAN_POINT('Ctrl Pts',(16.1956100895076,18.1839391817335,0.));
#250414=CARTESIAN_POINT('Ctrl Pts',(16.2163229838878,18.1940784507232,0.));
#250415=CARTESIAN_POINT('Ctrl Pts',(16.237143190164,18.2042057842037,0.));
#250416=CARTESIAN_POINT('Ctrl Pts',(16.2580702914615,18.214320612253,0.));
#250417=CARTESIAN_POINT('Ctrl Pts',(16.2791038736223,18.2244223710745,0.));
#250418=CARTESIAN_POINT('Ctrl Pts',(16.3002435251378,18.2345105028981,0.));
#250419=CARTESIAN_POINT('Ctrl Pts',(16.3214888370988,18.2445844558742,0.));
#250420=CARTESIAN_POINT('Ctrl Pts',(16.342839403159,18.2546436839609,0.));
#250421=CARTESIAN_POINT('Ctrl Pts',(16.3642948194869,18.2646876468169,0.));
#250422=CARTESIAN_POINT('Ctrl Pts',(16.385854684708,18.2747158096934,0.));
#250423=CARTESIAN_POINT('Ctrl Pts',(16.4075185998454,18.2847276433308,0.));
#250424=CARTESIAN_POINT('Ctrl Pts',(16.4292861682377,18.2947226238509,0.));
#250425=CARTESIAN_POINT('Ctrl Pts',(16.4511569955231,18.3047002326858,0.));
#250426=CARTESIAN_POINT('Ctrl Pts',(16.4731306896439,18.3146599565229,0.));
#250427=CARTESIAN_POINT('Ctrl Pts',(16.4952068608344,18.3246012872468,0.));
#250428=CARTESIAN_POINT('Ctrl Pts',(16.5173851216045,18.3345237218864,0.));
#250429=CARTESIAN_POINT('Ctrl Pts',(16.5396650867139,18.3444267625601,0.));
#250430=CARTESIAN_POINT('Ctrl Pts',(16.5620463731414,18.3543099164331,0.));
#250431=CARTESIAN_POINT('Ctrl Pts',(16.5845286000218,18.364172695589,0.));
#250432=CARTESIAN_POINT('Ctrl Pts',(16.6071113885711,18.3740146168879,0.));
#250433=CARTESIAN_POINT('Ctrl Pts',(16.6297943620056,18.3838352018327,0.));
#250434=CARTESIAN_POINT('Ctrl Pts',(16.6525771454513,18.3936339764332,0.));
#250435=CARTESIAN_POINT('Ctrl Pts',(16.6754593658513,18.4034104710789,0.));
#250436=CARTESIAN_POINT('Ctrl Pts',(16.698440651849,18.413164220399,0.));
#250437=CARTESIAN_POINT('Ctrl Pts',(16.7215206338818,18.4228947633186,0.));
#250438=CARTESIAN_POINT('Ctrl Pts',(16.7446989442882,18.4326016431392,0.));
#250439=CARTESIAN_POINT('Ctrl Pts',(16.7679752173992,18.4422844076099,0.));
#250440=CARTESIAN_POINT('Ctrl Pts',(16.791349089629,18.4519426090124,0.));
#250441=CARTESIAN_POINT('Ctrl Pts',(16.8148201995472,18.4615758042305,0.));
#250442=CARTESIAN_POINT('Ctrl Pts',(16.8383881879707,18.4711835548622,0.));
#250443=CARTESIAN_POINT('Ctrl Pts',(16.8620526977169,18.4807654268769,0.));
#250444=CARTESIAN_POINT('Ctrl Pts',(16.8858133733086,18.4903209902226,0.));
#250445=CARTESIAN_POINT('Ctrl Pts',(16.9096698606942,18.4998498184619,0.));
#250446=CARTESIAN_POINT('Ctrl Pts',(16.9336218069353,18.5093514883835,0.));
#250447=CARTESIAN_POINT('Ctrl Pts',(16.957668859934,18.518825579666,0.));
#250448=CARTESIAN_POINT('Ctrl Pts',(16.9818106680382,18.5282716744198,0.));
#250449=CARTESIAN_POINT('Ctrl Pts',(17.0060468805099,18.5376893576961,0.));
#250450=CARTESIAN_POINT('Ctrl Pts',(17.030377148174,18.5470782182089,0.));
#250451=CARTESIAN_POINT('Ctrl Pts',(17.0548011239751,18.5564378489628,0.));
#250452=CARTESIAN_POINT('Ctrl Pts',(17.0793184636079,18.5657678479788,0.));
#250453=CARTESIAN_POINT('Ctrl Pts',(17.1039288260001,18.5750678188543,0.));
#250454=CARTESIAN_POINT('Ctrl Pts',(17.1286318741185,18.5843373717253,0.));
#250455=CARTESIAN_POINT('Ctrl Pts',(17.1534272741646,18.5935761222833,0.));
#250456=CARTESIAN_POINT('Ctrl Pts',(17.1783146940131,18.6027836898826,0.));
#250457=CARTESIAN_POINT('Ctrl Pts',(17.2032938019288,18.6119596959957,0.));
#250458=CARTESIAN_POINT('Ctrl Pts',(17.2283642650519,18.6211037624041,0.));
#250459=CARTESIAN_POINT('Ctrl Pts',(17.2535257482186,18.630215509794,0.));
#250460=CARTESIAN_POINT('Ctrl Pts',(17.278777912021,18.639294555474,0.));
#250461=CARTESIAN_POINT('Ctrl Pts',(17.3041204135069,18.6483405141853,0.));
#250462=CARTESIAN_POINT('Ctrl Pts',(17.3295529098612,18.6573530024019,0.));
#250463=CARTESIAN_POINT('Ctrl Pts',(17.3550750612438,18.6663316416569,0.));
#250464=CARTESIAN_POINT('Ctrl Pts',(17.3806865340744,18.6752760624045,0.));
#250465=CARTESIAN_POINT('Ctrl Pts',(17.4063870038563,18.6841859073472,0.));
#250466=CARTESIAN_POINT('Ctrl Pts',(17.4321761588148,18.6930608357421,0.));
#250467=CARTESIAN_POINT('Ctrl Pts',(17.4580537012764,18.7019005250322,0.));
#250468=CARTESIAN_POINT('Ctrl Pts',(17.4840193397176,18.7107046613941,0.));
#250469=CARTESIAN_POINT('Ctrl Pts',(17.5100727820891,18.7194729318128,0.));
#250470=CARTESIAN_POINT('Ctrl Pts',(17.5362137287604,18.728205015716,0.));
#250471=CARTESIAN_POINT('Ctrl Pts',(17.5624418653248,18.7369005764558,0.));
#250472=CARTESIAN_POINT('Ctrl Pts',(17.5887568561361,18.7455592536667,0.));
#250473=CARTESIAN_POINT('Ctrl Pts',(17.6151583356988,18.7541806530935,0.));
#250474=CARTESIAN_POINT('Ctrl Pts',(17.6416459210646,18.7627643613139,0.));
#250475=CARTESIAN_POINT('Ctrl Pts',(17.6682192274197,18.7713099642673,0.));
#250476=CARTESIAN_POINT('Ctrl Pts',(17.6948778822981,18.7798170641305,0.));
#250477=CARTESIAN_POINT('Ctrl Pts',(17.7216215409019,18.7882852976016,0.));
#250478=CARTESIAN_POINT('Ctrl Pts',(17.7484498996916,18.7967143519444,0.));
#250479=CARTESIAN_POINT('Ctrl Pts',(17.7753627137898,18.8051039860543,0.));
#250480=CARTESIAN_POINT('Ctrl Pts',(17.8023598011135,18.8134540340581,0.));
#250481=CARTESIAN_POINT('Ctrl Pts',(17.8294410311105,18.8217643886368,0.));
#250482=CARTESIAN_POINT('Ctrl Pts',(17.8566063174871,18.8300349896187,0.));
#250483=CARTESIAN_POINT('Ctrl Pts',(17.8784057509434,18.8366196462746,0.));
#250484=CARTESIAN_POINT('Ctrl Pts',(17.8947931177853,18.8415402351882,0.));
#250485=CARTESIAN_POINT('Ctrl Pts',(17.9057348246611,18.8448126709726,0.));
#250486=CARTESIAN_POINT('Ctrl Pts',(17.9112098770111,18.8464468996588,0.));
#250487=CARTESIAN_POINT('',(17.9112098770111,18.8464468996588,12.));
#250488=CARTESIAN_POINT('Ctrl Pts',(17.9112098770111,18.8464468996588,12.));
#250489=CARTESIAN_POINT('Ctrl Pts',(17.9057348246611,18.8448126709726,12.));
#250490=CARTESIAN_POINT('Ctrl Pts',(17.8947931177853,18.8415402351882,12.));
#250491=CARTESIAN_POINT('Ctrl Pts',(17.8784057509434,18.8366196462746,12.));
#250492=CARTESIAN_POINT('Ctrl Pts',(17.8566063174871,18.8300349896187,12.));
#250493=CARTESIAN_POINT('Ctrl Pts',(17.8294410311105,18.8217643886368,12.));
#250494=CARTESIAN_POINT('Ctrl Pts',(17.8023598011135,18.8134540340581,12.));
#250495=CARTESIAN_POINT('Ctrl Pts',(17.7753627137898,18.8051039860543,12.));
#250496=CARTESIAN_POINT('Ctrl Pts',(17.7484498996916,18.7967143519444,12.));
#250497=CARTESIAN_POINT('Ctrl Pts',(17.7216215409019,18.7882852976016,12.));
#250498=CARTESIAN_POINT('Ctrl Pts',(17.6948778822981,18.7798170641305,12.));
#250499=CARTESIAN_POINT('Ctrl Pts',(17.6682192274197,18.7713099642673,12.));
#250500=CARTESIAN_POINT('Ctrl Pts',(17.6416459210646,18.7627643613139,12.));
#250501=CARTESIAN_POINT('Ctrl Pts',(17.6151583356988,18.7541806530935,12.));
#250502=CARTESIAN_POINT('Ctrl Pts',(17.5887568561361,18.7455592536667,12.));
#250503=CARTESIAN_POINT('Ctrl Pts',(17.5624418653248,18.7369005764558,12.));
#250504=CARTESIAN_POINT('Ctrl Pts',(17.5362137287604,18.728205015716,12.));
#250505=CARTESIAN_POINT('Ctrl Pts',(17.5100727820891,18.7194729318128,12.));
#250506=CARTESIAN_POINT('Ctrl Pts',(17.4840193397176,18.7107046613941,12.));
#250507=CARTESIAN_POINT('Ctrl Pts',(17.4580537012764,18.7019005250322,12.));
#250508=CARTESIAN_POINT('Ctrl Pts',(17.4321761588148,18.6930608357421,12.));
#250509=CARTESIAN_POINT('Ctrl Pts',(17.4063870038563,18.6841859073472,12.));
#250510=CARTESIAN_POINT('Ctrl Pts',(17.3806865340744,18.6752760624045,12.));
#250511=CARTESIAN_POINT('Ctrl Pts',(17.3550750612438,18.6663316416569,12.));
#250512=CARTESIAN_POINT('Ctrl Pts',(17.3295529098612,18.6573530024019,12.));
#250513=CARTESIAN_POINT('Ctrl Pts',(17.3041204135069,18.6483405141853,12.));
#250514=CARTESIAN_POINT('Ctrl Pts',(17.278777912021,18.639294555474,12.));
#250515=CARTESIAN_POINT('Ctrl Pts',(17.2535257482186,18.630215509794,12.));
#250516=CARTESIAN_POINT('Ctrl Pts',(17.2283642650519,18.6211037624041,12.));
#250517=CARTESIAN_POINT('Ctrl Pts',(17.2032938019288,18.6119596959957,12.));
#250518=CARTESIAN_POINT('Ctrl Pts',(17.1783146940131,18.6027836898826,12.));
#250519=CARTESIAN_POINT('Ctrl Pts',(17.1534272741646,18.5935761222833,12.));
#250520=CARTESIAN_POINT('Ctrl Pts',(17.1286318741185,18.5843373717253,12.));
#250521=CARTESIAN_POINT('Ctrl Pts',(17.1039288260001,18.5750678188543,12.));
#250522=CARTESIAN_POINT('Ctrl Pts',(17.0793184636079,18.5657678479788,12.));
#250523=CARTESIAN_POINT('Ctrl Pts',(17.0548011239751,18.5564378489628,12.));
#250524=CARTESIAN_POINT('Ctrl Pts',(17.030377148174,18.5470782182089,12.));
#250525=CARTESIAN_POINT('Ctrl Pts',(17.0060468805099,18.5376893576961,12.));
#250526=CARTESIAN_POINT('Ctrl Pts',(16.9818106680382,18.5282716744198,12.));
#250527=CARTESIAN_POINT('Ctrl Pts',(16.957668859934,18.518825579666,12.));
#250528=CARTESIAN_POINT('Ctrl Pts',(16.9336218069353,18.5093514883835,12.));
#250529=CARTESIAN_POINT('Ctrl Pts',(16.9096698606942,18.4998498184619,12.));
#250530=CARTESIAN_POINT('Ctrl Pts',(16.8858133733086,18.4903209902226,12.));
#250531=CARTESIAN_POINT('Ctrl Pts',(16.8620526977169,18.4807654268769,12.));
#250532=CARTESIAN_POINT('Ctrl Pts',(16.8383881879707,18.4711835548622,12.));
#250533=CARTESIAN_POINT('Ctrl Pts',(16.8148201995472,18.4615758042305,12.));
#250534=CARTESIAN_POINT('Ctrl Pts',(16.791349089629,18.4519426090124,12.));
#250535=CARTESIAN_POINT('Ctrl Pts',(16.7679752173992,18.4422844076099,12.));
#250536=CARTESIAN_POINT('Ctrl Pts',(16.7446989442882,18.4326016431392,12.));
#250537=CARTESIAN_POINT('Ctrl Pts',(16.7215206338818,18.4228947633186,12.));
#250538=CARTESIAN_POINT('Ctrl Pts',(16.698440651849,18.413164220399,12.));
#250539=CARTESIAN_POINT('Ctrl Pts',(16.6754593658513,18.4034104710789,12.));
#250540=CARTESIAN_POINT('Ctrl Pts',(16.6525771454513,18.3936339764332,12.));
#250541=CARTESIAN_POINT('Ctrl Pts',(16.6297943620056,18.3838352018327,12.));
#250542=CARTESIAN_POINT('Ctrl Pts',(16.6071113885711,18.3740146168879,12.));
#250543=CARTESIAN_POINT('Ctrl Pts',(16.5845286000218,18.364172695589,12.));
#250544=CARTESIAN_POINT('Ctrl Pts',(16.5620463731414,18.3543099164331,12.));
#250545=CARTESIAN_POINT('Ctrl Pts',(16.5396650867139,18.3444267625601,12.));
#250546=CARTESIAN_POINT('Ctrl Pts',(16.5173851216045,18.3345237218864,12.));
#250547=CARTESIAN_POINT('Ctrl Pts',(16.4952068608344,18.3246012872468,12.));
#250548=CARTESIAN_POINT('Ctrl Pts',(16.4731306896439,18.3146599565229,12.));
#250549=CARTESIAN_POINT('Ctrl Pts',(16.4511569955231,18.3047002326858,12.));
#250550=CARTESIAN_POINT('Ctrl Pts',(16.4292861682377,18.2947226238509,12.));
#250551=CARTESIAN_POINT('Ctrl Pts',(16.4075185998454,18.2847276433308,12.));
#250552=CARTESIAN_POINT('Ctrl Pts',(16.385854684708,18.2747158096934,12.));
#250553=CARTESIAN_POINT('Ctrl Pts',(16.3642948194869,18.2646876468169,12.));
#250554=CARTESIAN_POINT('Ctrl Pts',(16.342839403159,18.2546436839609,12.));
#250555=CARTESIAN_POINT('Ctrl Pts',(16.3214888370988,18.2445844558742,12.));
#250556=CARTESIAN_POINT('Ctrl Pts',(16.3002435251378,18.2345105028981,12.));
#250557=CARTESIAN_POINT('Ctrl Pts',(16.2791038736223,18.2244223710745,12.));
#250558=CARTESIAN_POINT('Ctrl Pts',(16.2580702914615,18.214320612253,12.));
#250559=CARTESIAN_POINT('Ctrl Pts',(16.237143190164,18.2042057842037,12.));
#250560=CARTESIAN_POINT('Ctrl Pts',(16.2163229838878,18.1940784507232,12.));
#250561=CARTESIAN_POINT('Ctrl Pts',(16.1956100895076,18.1839391817335,12.));
#250562=CARTESIAN_POINT('Ctrl Pts',(16.1750049266673,18.1737885533852,12.));
#250563=CARTESIAN_POINT('Ctrl Pts',(16.1545079178261,18.1636271481616,12.));
#250564=CARTESIAN_POINT('Ctrl Pts',(16.1341194882987,18.1534555549851,12.));
#250565=CARTESIAN_POINT('Ctrl Pts',(16.113840066279,18.1432743693231,12.));
#250566=CARTESIAN_POINT('Ctrl Pts',(16.0936700829108,18.1330841933099,12.));
#250567=CARTESIAN_POINT('Ctrl Pts',(16.0736099723664,18.1228856358746,12.));
#250568=CARTESIAN_POINT('Ctrl Pts',(16.0536601719124,18.1126793128688,12.));
#250569=CARTESIAN_POINT('Ctrl Pts',(16.0338211219693,18.1024658471966,12.));
#250570=CARTESIAN_POINT('Ctrl Pts',(16.0140932661612,18.0922458689464,12.));
#250571=CARTESIAN_POINT('Ctrl Pts',(15.9944770513616,18.0820200155239,12.));
#250572=CARTESIAN_POINT('Ctrl Pts',(15.9749729277848,18.071788931796,12.));
#250573=CARTESIAN_POINT('Ctrl Pts',(15.9555813490645,18.061553270236,12.));
#250574=CARTESIAN_POINT('Ctrl Pts',(15.9363027723244,18.0513136910691,12.));
#250575=CARTESIAN_POINT('Ctrl Pts',(15.9171376582436,18.0410708624208,12.));
#250576=CARTESIAN_POINT('Ctrl Pts',(15.8980864711043,18.0308254604638,12.));
#250577=CARTESIAN_POINT('Ctrl Pts',(15.8791496788685,18.0205781695773,12.));
#250578=CARTESIAN_POINT('Ctrl Pts',(15.8603277532834,18.010329682521,12.));
#250579=CARTESIAN_POINT('Ctrl Pts',(15.8416211699681,18.0000807006055,12.));
#250580=CARTESIAN_POINT('Ctrl Pts',(15.8230304084963,17.9898319338664,12.));
#250581=CARTESIAN_POINT('Ctrl Pts',(15.8045559524674,17.9795841012383,12.));
#250582=CARTESIAN_POINT('Ctrl Pts',(15.786198289572,17.9693379307297,12.));
#250583=CARTESIAN_POINT('Ctrl Pts',(15.7679579117072,17.9590941596236,12.));
#250584=CARTESIAN_POINT('Ctrl Pts',(15.7498353150856,17.9488535346776,12.));
#250585=CARTESIAN_POINT('Ctrl Pts',(15.7318310003334,17.9386168123261,12.));
#250586=CARTESIAN_POINT('Ctrl Pts',(15.713945472584,17.9283847588837,12.));
#250587=CARTESIAN_POINT('Ctrl Pts',(15.6961792415526,17.918158150746,12.));
#250588=CARTESIAN_POINT('Ctrl Pts',(15.6785328216467,17.9079377746118,12.));
#250589=CARTESIAN_POINT('Ctrl Pts',(15.6610067321036,17.8977244277247,12.));
#250590=CARTESIAN_POINT('Ctrl Pts',(15.6436014971088,17.8875189181095,12.));
#250591=CARTESIAN_POINT('Ctrl Pts',(15.6263176459107,17.8773220648125,12.));
#250592=CARTESIAN_POINT('Ctrl Pts',(15.6091557129205,17.8671346981388,12.));
#250593=CARTESIAN_POINT('Ctrl Pts',(15.5921162378183,17.8569576598996,12.));
#250594=CARTESIAN_POINT('Ctrl Pts',(15.5751997657153,17.8467918036977,12.));
#250595=CARTESIAN_POINT('Ctrl Pts',(15.5584068472976,17.8366379952078,12.));
#250596=CARTESIAN_POINT('Ctrl Pts',(15.5417380389639,17.8264971124606,12.));
#250597=CARTESIAN_POINT('Ctrl Pts',(15.5251939029558,17.8163700461263,12.));
#250598=CARTESIAN_POINT('Ctrl Pts',(15.5087750074728,17.8062576997964,12.));
#250599=CARTESIAN_POINT('Ctrl Pts',(15.4924819268529,17.7961609903161,12.));
#250600=CARTESIAN_POINT('Ctrl Pts',(15.4763152417506,17.7860808481229,12.));
#250601=CARTESIAN_POINT('Ctrl Pts',(15.4602755393019,17.7760182175817,12.));
#250602=CARTESIAN_POINT('Ctrl Pts',(15.4443634132865,17.765974057326,12.));
#250603=CARTESIAN_POINT('Ctrl Pts',(15.4285794642658,17.7559493405871,12.));
#250604=CARTESIAN_POINT('Ctrl Pts',(15.4129242997828,17.7459450555803,12.));
#250605=CARTESIAN_POINT('Ctrl Pts',(15.3973985345796,17.7359622059143,12.));
#250606=CARTESIAN_POINT('Ctrl Pts',(15.3820027907965,17.7260018109923,12.));
#250607=CARTESIAN_POINT('Ctrl Pts',(15.3667376981702,17.7160649064208,12.));
#250608=CARTESIAN_POINT('Ctrl Pts',(15.3516038942064,17.7061525444044,12.));
#250609=CARTESIAN_POINT('Ctrl Pts',(15.3366020244069,17.6962657941984,12.));
#250610=CARTESIAN_POINT('Ctrl Pts',(15.3217327425341,17.6864057426052,12.));
#250611=CARTESIAN_POINT('Ctrl Pts',(15.3069967108501,17.6765734944559,12.));
#250612=CARTESIAN_POINT('Ctrl Pts',(15.2923946003598,17.6667701731041,12.));
#250613=CARTESIAN_POINT('Ctrl Pts',(15.2779270910238,17.6569969209,12.));
#250614=CARTESIAN_POINT('Ctrl Pts',(15.263594872029,17.6472548997329,12.));
#250615=CARTESIAN_POINT('Ctrl Pts',(15.2493986421091,17.637545291637,12.));
#250616=CARTESIAN_POINT('Ctrl Pts',(15.2353391098367,17.6278692993765,12.));
#250617=CARTESIAN_POINT('Ctrl Pts',(15.22141699392,17.6182281470467,12.));
#250618=CARTESIAN_POINT('Ctrl Pts',(15.2076330234686,17.6086230806497,12.));
#250619=CARTESIAN_POINT('Ctrl Pts',(15.1939879383268,17.5990553687595,12.));
#250620=CARTESIAN_POINT('Ctrl Pts',(15.1804824894605,17.5895263032592,12.));
#250621=CARTESIAN_POINT('Ctrl Pts',(15.1671174393136,17.5800372000539,12.));
#250622=CARTESIAN_POINT('Ctrl Pts',(15.1538935621714,17.570589399803,12.));
#250623=CARTESIAN_POINT('Ctrl Pts',(15.1408116444877,17.5611842686196,12.));
#250624=CARTESIAN_POINT('Ctrl Pts',(15.127872485314,17.5518231989122,12.));
#250625=CARTESIAN_POINT('Ctrl Pts',(15.1150768967729,17.5425076102966,12.));
#250626=CARTESIAN_POINT('Ctrl Pts',(15.1024257045033,17.5332389504829,12.));
#250627=CARTESIAN_POINT('Ctrl Pts',(15.0899197481082,17.5240186961788,12.));
#250628=CARTESIAN_POINT('Ctrl Pts',(15.0775598815748,17.5148483539684,12.));
#250629=CARTESIAN_POINT('Ctrl Pts',(15.0653469738306,17.5057294613874,12.));
#250630=CARTESIAN_POINT('Ctrl Pts',(15.0532819093085,17.4966635880245,12.));
#250631=CARTESIAN_POINT('Ctrl Pts',(15.0413655884993,17.4876523366178,12.));
#250632=CARTESIAN_POINT('Ctrl Pts',(15.029598928488,17.4786973441417,12.));
#250633=CARTESIAN_POINT('Ctrl Pts',(15.0179828635086,17.4698002829357,12.));
#250634=CARTESIAN_POINT('Ctrl Pts',(15.0065183456921,17.4609628621418,12.));
#250635=CARTESIAN_POINT('Ctrl Pts',(14.9952063457778,17.4521868291004,12.));
#250636=CARTESIAN_POINT('Ctrl Pts',(14.9840478538358,17.4434739707773,12.));
#250637=CARTESIAN_POINT('Ctrl Pts',(14.9730438799452,17.4348261151396,12.));
#250638=CARTESIAN_POINT('Ctrl Pts',(14.9621954549827,17.426245132709,12.));
#250639=CARTESIAN_POINT('Ctrl Pts',(14.9515036315143,17.4177329382828,12.));
#250640=CARTESIAN_POINT('Ctrl Pts',(14.940969484645,17.4092914926071,12.));
#250641=CARTESIAN_POINT('Ctrl Pts',(14.9305941128757,17.4009228040749,12.));
#250642=CARTESIAN_POINT('Ctrl Pts',(14.9203786389342,17.3926289303986,12.));
#250643=CARTESIAN_POINT('Ctrl Pts',(14.9103242110057,17.3844119809824,12.));
#250644=CARTESIAN_POINT('Ctrl Pts',(14.900432003961,17.3762741193076,12.));
#250645=CARTESIAN_POINT('Ctrl Pts',(14.8907032205788,17.3682175653235,12.));
#250646=CARTESIAN_POINT('Ctrl Pts',(14.8811390927423,17.3602445978161,12.));
#250647=CARTESIAN_POINT('Ctrl Pts',(14.8717408826955,17.3523575568645,12.));
#250648=CARTESIAN_POINT('Ctrl Pts',(14.8625098843417,17.3445588463475,12.));
#250649=CARTESIAN_POINT('Ctrl Pts',(14.8534474245433,17.336850936485,12.));
#250650=CARTESIAN_POINT('Ctrl Pts',(14.8445548643508,17.3292363662605,12.));
#250651=CARTESIAN_POINT('Ctrl Pts',(14.8358336004197,17.3217177462101,12.));
#250652=CARTESIAN_POINT('Ctrl Pts',(14.8272850675379,17.3142977632659,12.));
#250653=CARTESIAN_POINT('Ctrl Pts',(14.8189107410162,17.3069791853706,12.));
#250654=CARTESIAN_POINT('Ctrl Pts',(14.8107121391035,17.299764866148,12.));
#250655=CARTESIAN_POINT('Ctrl Pts',(14.8026908254276,17.2926577496513,12.));
#250656=CARTESIAN_POINT('Ctrl Pts',(14.7948484105249,17.2856608733196,12.));
#250657=CARTESIAN_POINT('Ctrl Pts',(14.787186553128,17.2787773704849,12.));
#250658=CARTESIAN_POINT('Ctrl Pts',(14.7797069617804,17.2720104735194,12.));
#250659=CARTESIAN_POINT('Ctrl Pts',(14.7724113956731,17.2653635155319,12.));
#250660=CARTESIAN_POINT('Ctrl Pts',(14.7653016697591,17.2588399401465,12.));
#250661=CARTESIAN_POINT('Ctrl Pts',(14.7583796616617,17.2524433146837,12.));
#250662=CARTESIAN_POINT('Ctrl Pts',(14.7516473175124,17.2461773413288,12.));
#250663=CARTESIAN_POINT('Ctrl Pts',(14.7451066593792,17.2400458713565,12.));
#250664=CARTESIAN_POINT('Ctrl Pts',(14.7387597858116,17.2340529062076,12.));
#250665=CARTESIAN_POINT('Ctrl Pts',(14.7326088681163,17.2282025904314,12.));
#250666=CARTESIAN_POINT('Ctrl Pts',(14.7266561494282,17.2224992099667,12.));
#250667=CARTESIAN_POINT('Ctrl Pts',(14.7209039390327,17.2169471814256,12.));
#250668=CARTESIAN_POINT('Ctrl Pts',(14.7153546289339,17.2115510835989,12.));
#250669=CARTESIAN_POINT('Ctrl Pts',(14.7100107213586,17.2063157097315,12.));
#250670=CARTESIAN_POINT('Ctrl Pts',(14.7048748502663,17.2012461084268,12.));
#250671=CARTESIAN_POINT('Ctrl Pts',(14.699949811582,17.1963476411694,12.));
#250672=CARTESIAN_POINT('Ctrl Pts',(14.6952385361705,17.1916259308415,12.));
#250673=CARTESIAN_POINT('Ctrl Pts',(14.6907440526958,17.1870867909918,12.));
#250674=CARTESIAN_POINT('Ctrl Pts',(14.686469452232,17.182736158472,12.));
#250675=CARTESIAN_POINT('Ctrl Pts',(14.6824178576167,17.1785800350826,12.));
#250676=CARTESIAN_POINT('Ctrl Pts',(14.6785925615677,17.1746247499057,12.));
#250677=CARTESIAN_POINT('Ctrl Pts',(14.6749971333867,17.1708771619129,12.));
#250678=CARTESIAN_POINT('Ctrl Pts',(14.671635583332,17.167344972302,12.));
#250679=CARTESIAN_POINT('Ctrl Pts',(14.6685123374423,17.1640366762305,12.));
#250680=CARTESIAN_POINT('Ctrl Pts',(14.6656319165057,17.1609609517369,12.));
#250681=CARTESIAN_POINT('Ctrl Pts',(14.6629987285992,17.1581262646789,12.));
#250682=CARTESIAN_POINT('Ctrl Pts',(14.6606167169642,17.1555401986401,12.));
#250683=CARTESIAN_POINT('Ctrl Pts',(14.6584900555302,17.1532107762718,12.));
#250684=CARTESIAN_POINT('Ctrl Pts',(14.6566237952435,17.1511476869496,12.));
#250685=CARTESIAN_POINT('Ctrl Pts',(14.655024862281,17.1493641837558,12.));
#250686=CARTESIAN_POINT('Ctrl Pts',(14.6537016966184,17.147876394491,12.));
#250687=CARTESIAN_POINT('Ctrl Pts',(14.6526624064978,17.1466998098673,12.));
#250688=CARTESIAN_POINT('Ctrl Pts',(14.6519131634508,17.1458462295271,12.));
#250689=CARTESIAN_POINT('Ctrl Pts',(14.6515481598068,17.1454262858043,12.));
#250690=CARTESIAN_POINT('Ctrl Pts',(14.6514066997196,17.1452600887037,12.));
#250691=CARTESIAN_POINT('Ctrl Pts',(14.6513711852843,17.1452153999142,12.));
#250692=CARTESIAN_POINT('Ctrl Pts',(14.6513681262571,17.1452095830633,12.));
#250693=CARTESIAN_POINT('',(17.9112098770111,18.8464468996588,0.));
#250694=CARTESIAN_POINT('Origin',(17.7219872369693,12.1729687575668,0.));
#250695=CARTESIAN_POINT('',(18.5896416359912,12.7689476255363,12.));
#250696=CARTESIAN_POINT('',(8.86099361848466,6.08648437878338,12.));
#250697=CARTESIAN_POINT('',(18.5896416359912,12.7689476255363,0.));
#250698=CARTESIAN_POINT('',(18.5896416359912,12.7689476255363,0.));
#250699=CARTESIAN_POINT('',(8.86099361848466,6.08648437878338,0.));
#250700=CARTESIAN_POINT('Ctrl Pts',(18.8464468996588,17.9112098770111,0.));
#250701=CARTESIAN_POINT('Ctrl Pts',(18.8464468996588,17.9112098770111,12.));
#250702=CARTESIAN_POINT('Ctrl Pts',(18.8448126709691,17.9057348246595,0.));
#250703=CARTESIAN_POINT('Ctrl Pts',(18.8448126709691,17.9057348246595,12.));
#250704=CARTESIAN_POINT('Ctrl Pts',(18.8415402351786,17.8947931177807,0.));
#250705=CARTESIAN_POINT('Ctrl Pts',(18.8415402351786,17.8947931177807,12.));
#250706=CARTESIAN_POINT('Ctrl Pts',(18.8366196462581,17.8784057509356,0.));
#250707=CARTESIAN_POINT('Ctrl Pts',(18.8366196462581,17.8784057509356,12.));
#250708=CARTESIAN_POINT('Ctrl Pts',(18.8300349895974,17.8566063174771,0.));
#250709=CARTESIAN_POINT('Ctrl Pts',(18.8300349895974,17.8566063174771,12.));
#250710=CARTESIAN_POINT('Ctrl Pts',(18.8217643886157,17.8294410311006,0.));
#250711=CARTESIAN_POINT('Ctrl Pts',(18.8217643886157,17.8294410311006,12.));
#250712=CARTESIAN_POINT('Ctrl Pts',(18.8134540340417,17.8023598011057,0.));
#250713=CARTESIAN_POINT('Ctrl Pts',(18.8134540340417,17.8023598011057,12.));
#250714=CARTESIAN_POINT('Ctrl Pts',(18.8051039860448,17.7753627137853,0.));
#250715=CARTESIAN_POINT('Ctrl Pts',(18.8051039860448,17.7753627137853,12.));
#250716=CARTESIAN_POINT('Ctrl Pts',(18.7967143519419,17.7484498996905,0.));
#250717=CARTESIAN_POINT('Ctrl Pts',(18.7967143519419,17.7484498996905,12.));
#250718=CARTESIAN_POINT('Ctrl Pts',(18.7882852976049,17.7216215409035,0.));
#250719=CARTESIAN_POINT('Ctrl Pts',(18.7882852976049,17.7216215409035,12.));
#250720=CARTESIAN_POINT('Ctrl Pts',(18.7798170641374,17.6948778823014,0.));
#250721=CARTESIAN_POINT('Ctrl Pts',(18.7798170641374,17.6948778823014,12.));
#250722=CARTESIAN_POINT('Ctrl Pts',(18.7713099642754,17.6682192274236,0.));
#250723=CARTESIAN_POINT('Ctrl Pts',(18.7713099642754,17.6682192274236,12.));
#250724=CARTESIAN_POINT('Ctrl Pts',(18.762764361321,17.6416459210681,0.));
#250725=CARTESIAN_POINT('Ctrl Pts',(18.762764361321,17.6416459210681,12.));
#250726=CARTESIAN_POINT('Ctrl Pts',(18.7541806530984,17.6151583357012,0.));
#250727=CARTESIAN_POINT('Ctrl Pts',(18.7541806530984,17.6151583357012,12.));
#250728=CARTESIAN_POINT('Ctrl Pts',(18.7455592536687,17.5887568561371,0.));
#250729=CARTESIAN_POINT('Ctrl Pts',(18.7455592536687,17.5887568561371,12.));
#250730=CARTESIAN_POINT('Ctrl Pts',(18.7369005764553,17.5624418653245,0.));
#250731=CARTESIAN_POINT('Ctrl Pts',(18.7369005764553,17.5624418653245,12.));
#250732=CARTESIAN_POINT('Ctrl Pts',(18.7282050157138,17.5362137287593,0.));
#250733=CARTESIAN_POINT('Ctrl Pts',(18.7282050157138,17.5362137287593,12.));
#250734=CARTESIAN_POINT('Ctrl Pts',(18.7194729318098,17.5100727820876,0.));
#250735=CARTESIAN_POINT('Ctrl Pts',(18.7194729318098,17.5100727820876,12.));
#250736=CARTESIAN_POINT('Ctrl Pts',(18.7107046613912,17.4840193397162,0.));
#250737=CARTESIAN_POINT('Ctrl Pts',(18.7107046613912,17.4840193397162,12.));
#250738=CARTESIAN_POINT('Ctrl Pts',(18.70190052503,17.4580537012753,0.));
#250739=CARTESIAN_POINT('Ctrl Pts',(18.70190052503,17.4580537012753,12.));
#250740=CARTESIAN_POINT('Ctrl Pts',(18.6930608357409,17.4321761588142,0.));
#250741=CARTESIAN_POINT('Ctrl Pts',(18.6930608357409,17.4321761588142,12.));
#250742=CARTESIAN_POINT('Ctrl Pts',(18.6841859073471,17.4063870038562,0.));
#250743=CARTESIAN_POINT('Ctrl Pts',(18.6841859073471,17.4063870038562,12.));
#250744=CARTESIAN_POINT('Ctrl Pts',(18.6752760624052,17.3806865340747,0.));
#250745=CARTESIAN_POINT('Ctrl Pts',(18.6752760624052,17.3806865340747,12.));
#250746=CARTESIAN_POINT('Ctrl Pts',(18.6663316416582,17.3550750612443,0.));
#250747=CARTESIAN_POINT('Ctrl Pts',(18.6663316416582,17.3550750612443,12.));
#250748=CARTESIAN_POINT('Ctrl Pts',(18.6573530024033,17.3295529098618,0.));
#250749=CARTESIAN_POINT('Ctrl Pts',(18.6573530024033,17.3295529098618,12.));
#250750=CARTESIAN_POINT('Ctrl Pts',(18.6483405141865,17.3041204135074,0.));
#250751=CARTESIAN_POINT('Ctrl Pts',(18.6483405141865,17.3041204135074,12.));
#250752=CARTESIAN_POINT('Ctrl Pts',(18.6392945554748,17.2787779120213,0.));
#250753=CARTESIAN_POINT('Ctrl Pts',(18.6392945554748,17.2787779120213,12.));
#250754=CARTESIAN_POINT('Ctrl Pts',(18.6302155097943,17.2535257482187,0.));
#250755=CARTESIAN_POINT('Ctrl Pts',(18.6302155097943,17.2535257482187,12.));
#250756=CARTESIAN_POINT('Ctrl Pts',(18.6211037624038,17.2283642650518,0.));
#250757=CARTESIAN_POINT('Ctrl Pts',(18.6211037624038,17.2283642650518,12.));
#250758=CARTESIAN_POINT('Ctrl Pts',(18.6119596959949,17.2032938019284,0.));
#250759=CARTESIAN_POINT('Ctrl Pts',(18.6119596959949,17.2032938019284,12.));
#250760=CARTESIAN_POINT('Ctrl Pts',(18.6027836898817,17.1783146940127,0.));
#250761=CARTESIAN_POINT('Ctrl Pts',(18.6027836898817,17.1783146940127,12.));
#250762=CARTESIAN_POINT('Ctrl Pts',(18.5935761222825,17.1534272741643,0.));
#250763=CARTESIAN_POINT('Ctrl Pts',(18.5935761222825,17.1534272741643,12.));
#250764=CARTESIAN_POINT('Ctrl Pts',(18.5843373717247,17.1286318741183,0.));
#250765=CARTESIAN_POINT('Ctrl Pts',(18.5843373717247,17.1286318741183,12.));
#250766=CARTESIAN_POINT('Ctrl Pts',(18.5750678188542,17.1039288260001,0.));
#250767=CARTESIAN_POINT('Ctrl Pts',(18.5750678188542,17.1039288260001,12.));
#250768=CARTESIAN_POINT('Ctrl Pts',(18.5657678479789,17.0793184636079,0.));
#250769=CARTESIAN_POINT('Ctrl Pts',(18.5657678479789,17.0793184636079,12.));
#250770=CARTESIAN_POINT('Ctrl Pts',(18.556437848963,17.0548011239751,0.));
#250771=CARTESIAN_POINT('Ctrl Pts',(18.556437848963,17.0548011239751,12.));
#250772=CARTESIAN_POINT('Ctrl Pts',(18.547078218209,17.0303771481738,0.));
#250773=CARTESIAN_POINT('Ctrl Pts',(18.547078218209,17.0303771481738,12.));
#250774=CARTESIAN_POINT('Ctrl Pts',(18.5376893576961,17.0060468805097,0.));
#250775=CARTESIAN_POINT('Ctrl Pts',(18.5376893576961,17.0060468805097,12.));
#250776=CARTESIAN_POINT('Ctrl Pts',(18.5282716744197,16.981810668038,0.));
#250777=CARTESIAN_POINT('Ctrl Pts',(18.5282716744197,16.981810668038,12.));
#250778=CARTESIAN_POINT('Ctrl Pts',(18.5188255796659,16.9576688599339,0.));
#250779=CARTESIAN_POINT('Ctrl Pts',(18.5188255796659,16.9576688599339,12.));
#250780=CARTESIAN_POINT('Ctrl Pts',(18.5093514883835,16.9336218069353,0.));
#250781=CARTESIAN_POINT('Ctrl Pts',(18.5093514883835,16.9336218069353,12.));
#250782=CARTESIAN_POINT('Ctrl Pts',(18.499849818462,16.9096698606943,0.));
#250783=CARTESIAN_POINT('Ctrl Pts',(18.499849818462,16.9096698606943,12.));
#250784=CARTESIAN_POINT('Ctrl Pts',(18.4903209902227,16.8858133733088,0.));
#250785=CARTESIAN_POINT('Ctrl Pts',(18.4903209902227,16.8858133733088,12.));
#250786=CARTESIAN_POINT('Ctrl Pts',(18.4807654268771,16.8620526977171,0.));
#250787=CARTESIAN_POINT('Ctrl Pts',(18.4807654268771,16.8620526977171,12.));
#250788=CARTESIAN_POINT('Ctrl Pts',(18.4711835548623,16.8383881879709,0.));
#250789=CARTESIAN_POINT('Ctrl Pts',(18.4711835548623,16.8383881879709,12.));
#250790=CARTESIAN_POINT('Ctrl Pts',(18.4615758042305,16.8148201995472,0.));
#250791=CARTESIAN_POINT('Ctrl Pts',(18.4615758042305,16.8148201995472,12.));
#250792=CARTESIAN_POINT('Ctrl Pts',(18.4519426090123,16.791349089629,0.));
#250793=CARTESIAN_POINT('Ctrl Pts',(18.4519426090123,16.791349089629,12.));
#250794=CARTESIAN_POINT('Ctrl Pts',(18.44228440761,16.7679752173992,0.));
#250795=CARTESIAN_POINT('Ctrl Pts',(18.44228440761,16.7679752173992,12.));
#250796=CARTESIAN_POINT('Ctrl Pts',(18.4326016431392,16.7446989442882,0.));
#250797=CARTESIAN_POINT('Ctrl Pts',(18.4326016431392,16.7446989442882,12.));
#250798=CARTESIAN_POINT('Ctrl Pts',(18.4228947633187,16.7215206338818,0.));
#250799=CARTESIAN_POINT('Ctrl Pts',(18.4228947633187,16.7215206338818,12.));
#250800=CARTESIAN_POINT('Ctrl Pts',(18.413164220399,16.6984406518491,0.));
#250801=CARTESIAN_POINT('Ctrl Pts',(18.413164220399,16.6984406518491,12.));
#250802=CARTESIAN_POINT('Ctrl Pts',(18.403410471079,16.6754593658513,0.));
#250803=CARTESIAN_POINT('Ctrl Pts',(18.403410471079,16.6754593658513,12.));
#250804=CARTESIAN_POINT('Ctrl Pts',(18.3936339764332,16.6525771454513,0.));
#250805=CARTESIAN_POINT('Ctrl Pts',(18.3936339764332,16.6525771454513,12.));
#250806=CARTESIAN_POINT('Ctrl Pts',(18.3838352018327,16.6297943620056,0.));
#250807=CARTESIAN_POINT('Ctrl Pts',(18.3838352018327,16.6297943620056,12.));
#250808=CARTESIAN_POINT('Ctrl Pts',(18.3740146168879,16.607111388571,0.));
#250809=CARTESIAN_POINT('Ctrl Pts',(18.3740146168879,16.607111388571,12.));
#250810=CARTESIAN_POINT('Ctrl Pts',(18.3641726955889,16.5845286000217,0.));
#250811=CARTESIAN_POINT('Ctrl Pts',(18.3641726955889,16.5845286000217,12.));
#250812=CARTESIAN_POINT('Ctrl Pts',(18.354309916433,16.5620463731413,0.));
#250813=CARTESIAN_POINT('Ctrl Pts',(18.354309916433,16.5620463731413,12.));
#250814=CARTESIAN_POINT('Ctrl Pts',(18.34442676256,16.5396650867139,0.));
#250815=CARTESIAN_POINT('Ctrl Pts',(18.34442676256,16.5396650867139,12.));
#250816=CARTESIAN_POINT('Ctrl Pts',(18.3345237218864,16.5173851216045,0.));
#250817=CARTESIAN_POINT('Ctrl Pts',(18.3345237218864,16.5173851216045,12.));
#250818=CARTESIAN_POINT('Ctrl Pts',(18.3246012872469,16.4952068608345,0.));
#250819=CARTESIAN_POINT('Ctrl Pts',(18.3246012872469,16.4952068608345,12.));
#250820=CARTESIAN_POINT('Ctrl Pts',(18.3146599565231,16.4731306896441,0.));
#250821=CARTESIAN_POINT('Ctrl Pts',(18.3146599565231,16.4731306896441,12.));
#250822=CARTESIAN_POINT('Ctrl Pts',(18.304700232686,16.4511569955233,0.));
#250823=CARTESIAN_POINT('Ctrl Pts',(18.304700232686,16.4511569955233,12.));
#250824=CARTESIAN_POINT('Ctrl Pts',(18.294722623851,16.4292861682379,0.));
#250825=CARTESIAN_POINT('Ctrl Pts',(18.294722623851,16.4292861682379,12.));
#250826=CARTESIAN_POINT('Ctrl Pts',(18.2847276433309,16.4075185998455,0.));
#250827=CARTESIAN_POINT('Ctrl Pts',(18.2847276433309,16.4075185998455,12.));
#250828=CARTESIAN_POINT('Ctrl Pts',(18.2747158096934,16.385854684708,0.));
#250829=CARTESIAN_POINT('Ctrl Pts',(18.2747158096934,16.385854684708,12.));
#250830=CARTESIAN_POINT('Ctrl Pts',(18.2646876468169,16.3642948194868,0.));
#250831=CARTESIAN_POINT('Ctrl Pts',(18.2646876468169,16.3642948194868,12.));
#250832=CARTESIAN_POINT('Ctrl Pts',(18.2546436839608,16.3428394031589,0.));
#250833=CARTESIAN_POINT('Ctrl Pts',(18.2546436839608,16.3428394031589,12.));
#250834=CARTESIAN_POINT('Ctrl Pts',(18.2445844558742,16.3214888370987,0.));
#250835=CARTESIAN_POINT('Ctrl Pts',(18.2445844558742,16.3214888370987,12.));
#250836=CARTESIAN_POINT('Ctrl Pts',(18.2345105028982,16.3002435251378,0.));
#250837=CARTESIAN_POINT('Ctrl Pts',(18.2345105028982,16.3002435251378,12.));
#250838=CARTESIAN_POINT('Ctrl Pts',(18.2244223710745,16.2791038736223,0.));
#250839=CARTESIAN_POINT('Ctrl Pts',(18.2244223710745,16.2791038736223,12.));
#250840=CARTESIAN_POINT('Ctrl Pts',(18.2143206122529,16.2580702914615,0.));
#250841=CARTESIAN_POINT('Ctrl Pts',(18.2143206122529,16.2580702914615,12.));
#250842=CARTESIAN_POINT('Ctrl Pts',(18.2042057842035,16.2371431901638,0.));
#250843=CARTESIAN_POINT('Ctrl Pts',(18.2042057842035,16.2371431901638,12.));
#250844=CARTESIAN_POINT('Ctrl Pts',(18.1940784507229,16.2163229838875,0.));
#250845=CARTESIAN_POINT('Ctrl Pts',(18.1940784507229,16.2163229838875,12.));
#250846=CARTESIAN_POINT('Ctrl Pts',(18.1839391817331,16.1956100895073,0.));
#250847=CARTESIAN_POINT('Ctrl Pts',(18.1839391817331,16.1956100895073,12.));
#250848=CARTESIAN_POINT('Ctrl Pts',(18.1737885533849,16.1750049266671,0.));
#250849=CARTESIAN_POINT('Ctrl Pts',(18.1737885533849,16.1750049266671,12.));
#250850=CARTESIAN_POINT('Ctrl Pts',(18.1636271481615,16.154507917826,0.));
#250851=CARTESIAN_POINT('Ctrl Pts',(18.1636271481615,16.154507917826,12.));
#250852=CARTESIAN_POINT('Ctrl Pts',(18.1534555549852,16.1341194882988,0.));
#250853=CARTESIAN_POINT('Ctrl Pts',(18.1534555549852,16.1341194882988,12.));
#250854=CARTESIAN_POINT('Ctrl Pts',(18.1432743693235,16.1138400662794,0.));
#250855=CARTESIAN_POINT('Ctrl Pts',(18.1432743693235,16.1138400662794,12.));
#250856=CARTESIAN_POINT('Ctrl Pts',(18.1330841933105,16.0936700829112,0.));
#250857=CARTESIAN_POINT('Ctrl Pts',(18.1330841933105,16.0936700829112,12.));
#250858=CARTESIAN_POINT('Ctrl Pts',(18.1228856358751,16.0736099723668,0.));
#250859=CARTESIAN_POINT('Ctrl Pts',(18.1228856358751,16.0736099723668,12.));
#250860=CARTESIAN_POINT('Ctrl Pts',(18.112679312869,16.0536601719126,0.));
#250861=CARTESIAN_POINT('Ctrl Pts',(18.112679312869,16.0536601719126,12.));
#250862=CARTESIAN_POINT('Ctrl Pts',(18.1024658471966,16.0338211219693,0.));
#250863=CARTESIAN_POINT('Ctrl Pts',(18.1024658471966,16.0338211219693,12.));
#250864=CARTESIAN_POINT('Ctrl Pts',(18.0922458689462,16.014093266161,0.));
#250865=CARTESIAN_POINT('Ctrl Pts',(18.0922458689462,16.014093266161,12.));
#250866=CARTESIAN_POINT('Ctrl Pts',(18.0820200155236,15.9944770513613,0.));
#250867=CARTESIAN_POINT('Ctrl Pts',(18.0820200155236,15.9944770513613,12.));
#250868=CARTESIAN_POINT('Ctrl Pts',(18.0717889317958,15.9749729277846,0.));
#250869=CARTESIAN_POINT('Ctrl Pts',(18.0717889317958,15.9749729277846,12.));
#250870=CARTESIAN_POINT('Ctrl Pts',(18.061553270236,15.9555813490644,0.));
#250871=CARTESIAN_POINT('Ctrl Pts',(18.061553270236,15.9555813490644,12.));
#250872=CARTESIAN_POINT('Ctrl Pts',(18.0513136910691,15.9363027723244,0.));
#250873=CARTESIAN_POINT('Ctrl Pts',(18.0513136910691,15.9363027723244,12.));
#250874=CARTESIAN_POINT('Ctrl Pts',(18.0410708624208,15.9171376582436,0.));
#250875=CARTESIAN_POINT('Ctrl Pts',(18.0410708624208,15.9171376582436,12.));
#250876=CARTESIAN_POINT('Ctrl Pts',(18.0308254604636,15.8980864711042,0.));
#250877=CARTESIAN_POINT('Ctrl Pts',(18.0308254604636,15.8980864711042,12.));
#250878=CARTESIAN_POINT('Ctrl Pts',(18.0205781695769,15.8791496788683,0.));
#250879=CARTESIAN_POINT('Ctrl Pts',(18.0205781695769,15.8791496788683,12.));
#250880=CARTESIAN_POINT('Ctrl Pts',(18.0103296825205,15.8603277532831,0.));
#250881=CARTESIAN_POINT('Ctrl Pts',(18.0103296825205,15.8603277532831,12.));
#250882=CARTESIAN_POINT('Ctrl Pts',(18.0000807006052,15.8416211699679,0.));
#250883=CARTESIAN_POINT('Ctrl Pts',(18.0000807006052,15.8416211699679,12.));
#250884=CARTESIAN_POINT('Ctrl Pts',(17.9898319338664,15.8230304084962,0.));
#250885=CARTESIAN_POINT('Ctrl Pts',(17.9898319338664,15.8230304084962,12.));
#250886=CARTESIAN_POINT('Ctrl Pts',(17.9795841012386,15.8045559524677,0.));
#250887=CARTESIAN_POINT('Ctrl Pts',(17.9795841012386,15.8045559524677,12.));
#250888=CARTESIAN_POINT('Ctrl Pts',(17.9693379307303,15.7861982895724,0.));
#250889=CARTESIAN_POINT('Ctrl Pts',(17.9693379307303,15.7861982895724,12.));
#250890=CARTESIAN_POINT('Ctrl Pts',(17.9590941596242,15.7679579117077,0.));
#250891=CARTESIAN_POINT('Ctrl Pts',(17.9590941596242,15.7679579117077,12.));
#250892=CARTESIAN_POINT('Ctrl Pts',(17.9488535346781,15.749835315086,0.));
#250893=CARTESIAN_POINT('Ctrl Pts',(17.9488535346781,15.749835315086,12.));
#250894=CARTESIAN_POINT('Ctrl Pts',(17.9386168123262,15.7318310003335,0.));
#250895=CARTESIAN_POINT('Ctrl Pts',(17.9386168123262,15.7318310003335,12.));
#250896=CARTESIAN_POINT('Ctrl Pts',(17.9283847588836,15.7139454725839,0.));
#250897=CARTESIAN_POINT('Ctrl Pts',(17.9283847588836,15.7139454725839,12.));
#250898=CARTESIAN_POINT('Ctrl Pts',(17.9181581507455,15.6961792415522,0.));
#250899=CARTESIAN_POINT('Ctrl Pts',(17.9181581507455,15.6961792415522,12.));
#250900=CARTESIAN_POINT('Ctrl Pts',(17.9079377746111,15.6785328216461,0.));
#250901=CARTESIAN_POINT('Ctrl Pts',(17.9079377746111,15.6785328216461,12.));
#250902=CARTESIAN_POINT('Ctrl Pts',(17.897724427724,15.661006732103,0.));
#250903=CARTESIAN_POINT('Ctrl Pts',(17.897724427724,15.661006732103,12.));
#250904=CARTESIAN_POINT('Ctrl Pts',(17.8875189181091,15.6436014971085,0.));
#250905=CARTESIAN_POINT('Ctrl Pts',(17.8875189181091,15.6436014971085,12.));
#250906=CARTESIAN_POINT('Ctrl Pts',(17.8773220648125,15.6263176459108,0.));
#250907=CARTESIAN_POINT('Ctrl Pts',(17.8773220648125,15.6263176459108,12.));
#250908=CARTESIAN_POINT('Ctrl Pts',(17.8671346981394,15.609155712921,0.));
#250909=CARTESIAN_POINT('Ctrl Pts',(17.8671346981394,15.609155712921,12.));
#250910=CARTESIAN_POINT('Ctrl Pts',(17.8569576599006,15.5921162378192,0.));
#250911=CARTESIAN_POINT('Ctrl Pts',(17.8569576599006,15.5921162378192,12.));
#250912=CARTESIAN_POINT('Ctrl Pts',(17.8467918036987,15.5751997657163,0.));
#250913=CARTESIAN_POINT('Ctrl Pts',(17.8467918036987,15.5751997657163,12.));
#250914=CARTESIAN_POINT('Ctrl Pts',(17.8366379952085,15.5584068472982,0.));
#250915=CARTESIAN_POINT('Ctrl Pts',(17.8366379952085,15.5584068472982,12.));
#250916=CARTESIAN_POINT('Ctrl Pts',(17.8264971124606,15.541738038964,0.));
#250917=CARTESIAN_POINT('Ctrl Pts',(17.8264971124606,15.541738038964,12.));
#250918=CARTESIAN_POINT('Ctrl Pts',(17.8163700461256,15.5251939029552,0.));
#250919=CARTESIAN_POINT('Ctrl Pts',(17.8163700461256,15.5251939029552,12.));
#250920=CARTESIAN_POINT('Ctrl Pts',(17.8062576997952,15.5087750074718,0.));
#250921=CARTESIAN_POINT('Ctrl Pts',(17.8062576997952,15.5087750074718,12.));
#250922=CARTESIAN_POINT('Ctrl Pts',(17.7961609903148,15.4924819268517,0.));
#250923=CARTESIAN_POINT('Ctrl Pts',(17.7961609903148,15.4924819268517,12.));
#250924=CARTESIAN_POINT('Ctrl Pts',(17.7860808481219,15.4763152417497,0.));
#250925=CARTESIAN_POINT('Ctrl Pts',(17.7860808481219,15.4763152417497,12.));
#250926=CARTESIAN_POINT('Ctrl Pts',(17.7760182175815,15.4602755393018,0.));
#250927=CARTESIAN_POINT('Ctrl Pts',(17.7760182175815,15.4602755393018,12.));
#250928=CARTESIAN_POINT('Ctrl Pts',(17.7659740573265,15.4443634132869,0.));
#250929=CARTESIAN_POINT('Ctrl Pts',(17.7659740573265,15.4443634132869,12.));
#250930=CARTESIAN_POINT('Ctrl Pts',(17.7559493405881,15.4285794642668,0.));
#250931=CARTESIAN_POINT('Ctrl Pts',(17.7559493405881,15.4285794642668,12.));
#250932=CARTESIAN_POINT('Ctrl Pts',(17.7459450555812,15.4129242997837,0.));
#250933=CARTESIAN_POINT('Ctrl Pts',(17.7459450555812,15.4129242997837,12.));
#250934=CARTESIAN_POINT('Ctrl Pts',(17.7359622059149,15.3973985345802,0.));
#250935=CARTESIAN_POINT('Ctrl Pts',(17.7359622059149,15.3973985345802,12.));
#250936=CARTESIAN_POINT('Ctrl Pts',(17.7260018109924,15.3820027907967,0.));
#250937=CARTESIAN_POINT('Ctrl Pts',(17.7260018109924,15.3820027907967,12.));
#250938=CARTESIAN_POINT('Ctrl Pts',(17.7160649064206,15.3667376981699,0.));
#250939=CARTESIAN_POINT('Ctrl Pts',(17.7160649064206,15.3667376981699,12.));
#250940=CARTESIAN_POINT('Ctrl Pts',(17.7061525444042,15.351603894206,0.));
#250941=CARTESIAN_POINT('Ctrl Pts',(17.7061525444042,15.351603894206,12.));
#250942=CARTESIAN_POINT('Ctrl Pts',(17.6962657941983,15.3366020244066,0.));
#250943=CARTESIAN_POINT('Ctrl Pts',(17.6962657941983,15.3366020244066,12.));
#250944=CARTESIAN_POINT('Ctrl Pts',(17.6864057426052,15.3217327425338,0.));
#250945=CARTESIAN_POINT('Ctrl Pts',(17.6864057426052,15.3217327425338,12.));
#250946=CARTESIAN_POINT('Ctrl Pts',(17.676573494456,15.3069967108501,0.));
#250947=CARTESIAN_POINT('Ctrl Pts',(17.676573494456,15.3069967108501,12.));
#250948=CARTESIAN_POINT('Ctrl Pts',(17.6667701731041,15.2923946003598,0.));
#250949=CARTESIAN_POINT('Ctrl Pts',(17.6667701731041,15.2923946003598,12.));
#250950=CARTESIAN_POINT('Ctrl Pts',(17.6569969209,15.2779270910239,0.));
#250951=CARTESIAN_POINT('Ctrl Pts',(17.6569969209,15.2779270910239,12.));
#250952=CARTESIAN_POINT('Ctrl Pts',(17.6472548997328,15.2635948720292,0.));
#250953=CARTESIAN_POINT('Ctrl Pts',(17.6472548997328,15.2635948720292,12.));
#250954=CARTESIAN_POINT('Ctrl Pts',(17.6375452916369,15.2493986421092,0.));
#250955=CARTESIAN_POINT('Ctrl Pts',(17.6375452916369,15.2493986421092,12.));
#250956=CARTESIAN_POINT('Ctrl Pts',(17.6278692993764,15.2353391098367,0.));
#250957=CARTESIAN_POINT('Ctrl Pts',(17.6278692993764,15.2353391098367,12.));
#250958=CARTESIAN_POINT('Ctrl Pts',(17.6182281470468,15.22141699392,0.));
#250959=CARTESIAN_POINT('Ctrl Pts',(17.6182281470468,15.22141699392,12.));
#250960=CARTESIAN_POINT('Ctrl Pts',(17.60862308065,15.2076330234686,0.));
#250961=CARTESIAN_POINT('Ctrl Pts',(17.60862308065,15.2076330234686,12.));
#250962=CARTESIAN_POINT('Ctrl Pts',(17.5990553687599,15.1939879383268,0.));
#250963=CARTESIAN_POINT('Ctrl Pts',(17.5990553687599,15.1939879383268,12.));
#250964=CARTESIAN_POINT('Ctrl Pts',(17.5895263032595,15.1804824894605,0.));
#250965=CARTESIAN_POINT('Ctrl Pts',(17.5895263032595,15.1804824894605,12.));
#250966=CARTESIAN_POINT('Ctrl Pts',(17.580037200054,15.1671174393137,0.));
#250967=CARTESIAN_POINT('Ctrl Pts',(17.580037200054,15.1671174393137,12.));
#250968=CARTESIAN_POINT('Ctrl Pts',(17.5705893998029,15.1538935621714,0.));
#250969=CARTESIAN_POINT('Ctrl Pts',(17.5705893998029,15.1538935621714,12.));
#250970=CARTESIAN_POINT('Ctrl Pts',(17.5611842686192,15.1408116444876,0.));
#250971=CARTESIAN_POINT('Ctrl Pts',(17.5611842686192,15.1408116444876,12.));
#250972=CARTESIAN_POINT('Ctrl Pts',(17.5518231989117,15.1278724853138,0.));
#250973=CARTESIAN_POINT('Ctrl Pts',(17.5518231989117,15.1278724853138,12.));
#250974=CARTESIAN_POINT('Ctrl Pts',(17.5425076102963,15.1150768967728,0.));
#250975=CARTESIAN_POINT('Ctrl Pts',(17.5425076102963,15.1150768967728,12.));
#250976=CARTESIAN_POINT('Ctrl Pts',(17.5332389504829,15.1024257045033,0.));
#250977=CARTESIAN_POINT('Ctrl Pts',(17.5332389504829,15.1024257045033,12.));
#250978=CARTESIAN_POINT('Ctrl Pts',(17.524018696179,15.0899197481082,0.));
#250979=CARTESIAN_POINT('Ctrl Pts',(17.524018696179,15.0899197481082,12.));
#250980=CARTESIAN_POINT('Ctrl Pts',(17.5148483539687,15.0775598815749,0.));
#250981=CARTESIAN_POINT('Ctrl Pts',(17.5148483539687,15.0775598815749,12.));
#250982=CARTESIAN_POINT('Ctrl Pts',(17.5057294613877,15.0653469738307,0.));
#250983=CARTESIAN_POINT('Ctrl Pts',(17.5057294613877,15.0653469738307,12.));
#250984=CARTESIAN_POINT('Ctrl Pts',(17.4966635880246,15.0532819093085,0.));
#250985=CARTESIAN_POINT('Ctrl Pts',(17.4966635880246,15.0532819093085,12.));
#250986=CARTESIAN_POINT('Ctrl Pts',(17.4876523366178,15.0413655884993,0.));
#250987=CARTESIAN_POINT('Ctrl Pts',(17.4876523366178,15.0413655884993,12.));
#250988=CARTESIAN_POINT('Ctrl Pts',(17.4786973441417,15.029598928488,0.));
#250989=CARTESIAN_POINT('Ctrl Pts',(17.4786973441417,15.029598928488,12.));
#250990=CARTESIAN_POINT('Ctrl Pts',(17.4698002829357,15.0179828635087,0.));
#250991=CARTESIAN_POINT('Ctrl Pts',(17.4698002829357,15.0179828635087,12.));
#250992=CARTESIAN_POINT('Ctrl Pts',(17.4609628621419,15.0065183456923,0.));
#250993=CARTESIAN_POINT('Ctrl Pts',(17.4609628621419,15.0065183456923,12.));
#250994=CARTESIAN_POINT('Ctrl Pts',(17.4521868291005,14.9952063457779,0.));
#250995=CARTESIAN_POINT('Ctrl Pts',(17.4521868291005,14.9952063457779,12.));
#250996=CARTESIAN_POINT('Ctrl Pts',(17.4434739707773,14.9840478538357,0.));
#250997=CARTESIAN_POINT('Ctrl Pts',(17.4434739707773,14.9840478538357,12.));
#250998=CARTESIAN_POINT('Ctrl Pts',(17.4348261151395,14.973043879945,0.));
#250999=CARTESIAN_POINT('Ctrl Pts',(17.4348261151395,14.973043879945,12.));
#251000=CARTESIAN_POINT('Ctrl Pts',(17.4262451327088,14.9621954549825,0.));
#251001=CARTESIAN_POINT('Ctrl Pts',(17.4262451327088,14.9621954549825,12.));
#251002=CARTESIAN_POINT('Ctrl Pts',(17.4177329382827,14.9515036315142,0.));
#251003=CARTESIAN_POINT('Ctrl Pts',(17.4177329382827,14.9515036315142,12.));
#251004=CARTESIAN_POINT('Ctrl Pts',(17.4092914926071,14.940969484645,0.));
#251005=CARTESIAN_POINT('Ctrl Pts',(17.4092914926071,14.940969484645,12.));
#251006=CARTESIAN_POINT('Ctrl Pts',(17.400922804075,14.9305941128758,0.));
#251007=CARTESIAN_POINT('Ctrl Pts',(17.400922804075,14.9305941128758,12.));
#251008=CARTESIAN_POINT('Ctrl Pts',(17.3926289303987,14.9203786389343,0.));
#251009=CARTESIAN_POINT('Ctrl Pts',(17.3926289303987,14.9203786389343,12.));
#251010=CARTESIAN_POINT('Ctrl Pts',(17.3844119809823,14.9103242110057,0.));
#251011=CARTESIAN_POINT('Ctrl Pts',(17.3844119809823,14.9103242110057,12.));
#251012=CARTESIAN_POINT('Ctrl Pts',(17.3762741193075,14.9004320039609,0.));
#251013=CARTESIAN_POINT('Ctrl Pts',(17.3762741193075,14.9004320039609,12.));
#251014=CARTESIAN_POINT('Ctrl Pts',(17.3682175653236,14.8907032205789,0.));
#251015=CARTESIAN_POINT('Ctrl Pts',(17.3682175653236,14.8907032205789,12.));
#251016=CARTESIAN_POINT('Ctrl Pts',(17.3602445978163,14.8811390927424,0.));
#251017=CARTESIAN_POINT('Ctrl Pts',(17.3602445978163,14.8811390927424,12.));
#251018=CARTESIAN_POINT('Ctrl Pts',(17.3523575568648,14.8717408826958,0.));
#251019=CARTESIAN_POINT('Ctrl Pts',(17.3523575568648,14.8717408826958,12.));
#251020=CARTESIAN_POINT('Ctrl Pts',(17.3445588463477,14.8625098843419,0.));
#251021=CARTESIAN_POINT('Ctrl Pts',(17.3445588463477,14.8625098843419,12.));
#251022=CARTESIAN_POINT('Ctrl Pts',(17.336850936485,14.8534474245433,0.));
#251023=CARTESIAN_POINT('Ctrl Pts',(17.336850936485,14.8534474245433,12.));
#251024=CARTESIAN_POINT('Ctrl Pts',(17.3292363662601,14.8445548643505,0.));
#251025=CARTESIAN_POINT('Ctrl Pts',(17.3292363662601,14.8445548643505,12.));
#251026=CARTESIAN_POINT('Ctrl Pts',(17.3217177462096,14.8358336004193,0.));
#251027=CARTESIAN_POINT('Ctrl Pts',(17.3217177462096,14.8358336004193,12.));
#251028=CARTESIAN_POINT('Ctrl Pts',(17.3142977632656,14.8272850675375,0.));
#251029=CARTESIAN_POINT('Ctrl Pts',(17.3142977632656,14.8272850675375,12.));
#251030=CARTESIAN_POINT('Ctrl Pts',(17.3069791853705,14.8189107410161,0.));
#251031=CARTESIAN_POINT('Ctrl Pts',(17.3069791853705,14.8189107410161,12.));
#251032=CARTESIAN_POINT('Ctrl Pts',(17.2997648661483,14.8107121391038,0.));
#251033=CARTESIAN_POINT('Ctrl Pts',(17.2997648661483,14.8107121391038,12.));
#251034=CARTESIAN_POINT('Ctrl Pts',(17.2926577496519,14.8026908254281,0.));
#251035=CARTESIAN_POINT('Ctrl Pts',(17.2926577496519,14.8026908254281,12.));
#251036=CARTESIAN_POINT('Ctrl Pts',(17.28566087332,14.7948484105253,0.));
#251037=CARTESIAN_POINT('Ctrl Pts',(17.28566087332,14.7948484105253,12.));
#251038=CARTESIAN_POINT('Ctrl Pts',(17.278777370485,14.787186553128,0.));
#251039=CARTESIAN_POINT('Ctrl Pts',(17.278777370485,14.787186553128,12.));
#251040=CARTESIAN_POINT('Ctrl Pts',(17.2720104735192,14.7797069617802,0.));
#251041=CARTESIAN_POINT('Ctrl Pts',(17.2720104735192,14.7797069617802,12.));
#251042=CARTESIAN_POINT('Ctrl Pts',(17.2653635155317,14.7724113956728,0.));
#251043=CARTESIAN_POINT('Ctrl Pts',(17.2653635155317,14.7724113956728,12.));
#251044=CARTESIAN_POINT('Ctrl Pts',(17.2588399401464,14.7653016697589,0.));
#251045=CARTESIAN_POINT('Ctrl Pts',(17.2588399401464,14.7653016697589,12.));
#251046=CARTESIAN_POINT('Ctrl Pts',(17.2524433146837,14.7583796616617,0.));
#251047=CARTESIAN_POINT('Ctrl Pts',(17.2524433146837,14.7583796616617,12.));
#251048=CARTESIAN_POINT('Ctrl Pts',(17.2461773413289,14.7516473175125,0.));
#251049=CARTESIAN_POINT('Ctrl Pts',(17.2461773413289,14.7516473175125,12.));
#251050=CARTESIAN_POINT('Ctrl Pts',(17.2400458713566,14.7451066593793,0.));
#251051=CARTESIAN_POINT('Ctrl Pts',(17.2400458713566,14.7451066593793,12.));
#251052=CARTESIAN_POINT('Ctrl Pts',(17.2340529062077,14.7387597858117,0.));
#251053=CARTESIAN_POINT('Ctrl Pts',(17.2340529062077,14.7387597858117,12.));
#251054=CARTESIAN_POINT('Ctrl Pts',(17.2282025904314,14.7326088681163,0.));
#251055=CARTESIAN_POINT('Ctrl Pts',(17.2282025904314,14.7326088681163,12.));
#251056=CARTESIAN_POINT('Ctrl Pts',(17.2224992099666,14.7266561494282,0.));
#251057=CARTESIAN_POINT('Ctrl Pts',(17.2224992099666,14.7266561494282,12.));
#251058=CARTESIAN_POINT('Ctrl Pts',(17.2169471814255,14.7209039390326,0.));
#251059=CARTESIAN_POINT('Ctrl Pts',(17.2169471814255,14.7209039390326,12.));
#251060=CARTESIAN_POINT('Ctrl Pts',(17.2115510835988,14.7153546289338,0.));
#251061=CARTESIAN_POINT('Ctrl Pts',(17.2115510835988,14.7153546289338,12.));
#251062=CARTESIAN_POINT('Ctrl Pts',(17.2063157097316,14.7100107213587,0.));
#251063=CARTESIAN_POINT('Ctrl Pts',(17.2063157097316,14.7100107213587,12.));
#251064=CARTESIAN_POINT('Ctrl Pts',(17.2012461084268,14.7048748502663,0.));
#251065=CARTESIAN_POINT('Ctrl Pts',(17.2012461084268,14.7048748502663,12.));
#251066=CARTESIAN_POINT('Ctrl Pts',(17.1963476411694,14.699949811582,0.));
#251067=CARTESIAN_POINT('Ctrl Pts',(17.1963476411694,14.699949811582,12.));
#251068=CARTESIAN_POINT('Ctrl Pts',(17.1916259308415,14.6952385361706,0.));
#251069=CARTESIAN_POINT('Ctrl Pts',(17.1916259308415,14.6952385361706,12.));
#251070=CARTESIAN_POINT('Ctrl Pts',(17.1870867909918,14.6907440526958,0.));
#251071=CARTESIAN_POINT('Ctrl Pts',(17.1870867909918,14.6907440526958,12.));
#251072=CARTESIAN_POINT('Ctrl Pts',(17.182736158472,14.6864694522319,0.));
#251073=CARTESIAN_POINT('Ctrl Pts',(17.182736158472,14.6864694522319,12.));
#251074=CARTESIAN_POINT('Ctrl Pts',(17.1785800350827,14.6824178576167,0.));
#251075=CARTESIAN_POINT('Ctrl Pts',(17.1785800350827,14.6824178576167,12.));
#251076=CARTESIAN_POINT('Ctrl Pts',(17.1746247499057,14.6785925615676,0.));
#251077=CARTESIAN_POINT('Ctrl Pts',(17.1746247499057,14.6785925615676,12.));
#251078=CARTESIAN_POINT('Ctrl Pts',(17.1708771619129,14.6749971333867,0.));
#251079=CARTESIAN_POINT('Ctrl Pts',(17.1708771619129,14.6749971333867,12.));
#251080=CARTESIAN_POINT('Ctrl Pts',(17.1673449723019,14.6716355833321,0.));
#251081=CARTESIAN_POINT('Ctrl Pts',(17.1673449723019,14.6716355833321,12.));
#251082=CARTESIAN_POINT('Ctrl Pts',(17.1640366762304,14.6685123374424,0.));
#251083=CARTESIAN_POINT('Ctrl Pts',(17.1640366762304,14.6685123374424,12.));
#251084=CARTESIAN_POINT('Ctrl Pts',(17.1609609517369,14.6656319165057,0.));
#251085=CARTESIAN_POINT('Ctrl Pts',(17.1609609517369,14.6656319165057,12.));
#251086=CARTESIAN_POINT('Ctrl Pts',(17.1581262646789,14.662998728599,0.));
#251087=CARTESIAN_POINT('Ctrl Pts',(17.1581262646789,14.662998728599,12.));
#251088=CARTESIAN_POINT('Ctrl Pts',(17.1555401986403,14.660616716964,0.));
#251089=CARTESIAN_POINT('Ctrl Pts',(17.1555401986403,14.660616716964,12.));
#251090=CARTESIAN_POINT('Ctrl Pts',(17.1532107762719,14.6584900555301,0.));
#251091=CARTESIAN_POINT('Ctrl Pts',(17.1532107762719,14.6584900555301,12.));
#251092=CARTESIAN_POINT('Ctrl Pts',(17.1511476869495,14.6566237952435,0.));
#251093=CARTESIAN_POINT('Ctrl Pts',(17.1511476869495,14.6566237952435,12.));
#251094=CARTESIAN_POINT('Ctrl Pts',(17.1493641837556,14.6550248622813,0.));
#251095=CARTESIAN_POINT('Ctrl Pts',(17.1493641837556,14.6550248622813,12.));
#251096=CARTESIAN_POINT('Ctrl Pts',(17.1478763944909,14.6537016966188,0.));
#251097=CARTESIAN_POINT('Ctrl Pts',(17.1478763944909,14.6537016966188,12.));
#251098=CARTESIAN_POINT('Ctrl Pts',(17.1466998098673,14.6526624064978,0.));
#251099=CARTESIAN_POINT('Ctrl Pts',(17.1466998098673,14.6526624064978,12.));
#251100=CARTESIAN_POINT('Ctrl Pts',(17.1458462295273,14.65191316345,0.));
#251101=CARTESIAN_POINT('Ctrl Pts',(17.1458462295273,14.65191316345,12.));
#251102=CARTESIAN_POINT('Ctrl Pts',(17.1454262858045,14.6515481598057,0.));
#251103=CARTESIAN_POINT('Ctrl Pts',(17.1454262858045,14.6515481598057,12.));
#251104=CARTESIAN_POINT('Ctrl Pts',(17.1452600887039,14.6514066997188,0.));
#251105=CARTESIAN_POINT('Ctrl Pts',(17.1452600887039,14.6514066997188,12.));
#251106=CARTESIAN_POINT('Ctrl Pts',(17.1452153999142,14.651371185284,0.));
#251107=CARTESIAN_POINT('Ctrl Pts',(17.1452153999142,14.651371185284,12.));
#251108=CARTESIAN_POINT('Ctrl Pts',(17.1452095830633,14.6513681262571,0.));
#251109=CARTESIAN_POINT('Ctrl Pts',(17.1452095830633,14.6513681262571,12.));
#251110=CARTESIAN_POINT('',(18.8464468996588,17.9112098770111,0.));
#251111=CARTESIAN_POINT('Ctrl Pts',(18.8464468996588,17.9112098770111,0.));
#251112=CARTESIAN_POINT('Ctrl Pts',(18.8448126709691,17.9057348246595,0.));
#251113=CARTESIAN_POINT('Ctrl Pts',(18.8415402351786,17.8947931177807,0.));
#251114=CARTESIAN_POINT('Ctrl Pts',(18.8366196462581,17.8784057509356,0.));
#251115=CARTESIAN_POINT('Ctrl Pts',(18.8300349895974,17.8566063174771,0.));
#251116=CARTESIAN_POINT('Ctrl Pts',(18.8217643886157,17.8294410311006,0.));
#251117=CARTESIAN_POINT('Ctrl Pts',(18.8134540340417,17.8023598011057,0.));
#251118=CARTESIAN_POINT('Ctrl Pts',(18.8051039860448,17.7753627137853,0.));
#251119=CARTESIAN_POINT('Ctrl Pts',(18.7967143519419,17.7484498996905,0.));
#251120=CARTESIAN_POINT('Ctrl Pts',(18.7882852976049,17.7216215409035,0.));
#251121=CARTESIAN_POINT('Ctrl Pts',(18.7798170641374,17.6948778823014,0.));
#251122=CARTESIAN_POINT('Ctrl Pts',(18.7713099642754,17.6682192274236,0.));
#251123=CARTESIAN_POINT('Ctrl Pts',(18.762764361321,17.6416459210681,0.));
#251124=CARTESIAN_POINT('Ctrl Pts',(18.7541806530984,17.6151583357012,0.));
#251125=CARTESIAN_POINT('Ctrl Pts',(18.7455592536687,17.5887568561371,0.));
#251126=CARTESIAN_POINT('Ctrl Pts',(18.7369005764553,17.5624418653245,0.));
#251127=CARTESIAN_POINT('Ctrl Pts',(18.7282050157138,17.5362137287593,0.));
#251128=CARTESIAN_POINT('Ctrl Pts',(18.7194729318098,17.5100727820876,0.));
#251129=CARTESIAN_POINT('Ctrl Pts',(18.7107046613912,17.4840193397162,0.));
#251130=CARTESIAN_POINT('Ctrl Pts',(18.70190052503,17.4580537012753,0.));
#251131=CARTESIAN_POINT('Ctrl Pts',(18.6930608357409,17.4321761588142,0.));
#251132=CARTESIAN_POINT('Ctrl Pts',(18.6841859073471,17.4063870038562,0.));
#251133=CARTESIAN_POINT('Ctrl Pts',(18.6752760624052,17.3806865340747,0.));
#251134=CARTESIAN_POINT('Ctrl Pts',(18.6663316416582,17.3550750612443,0.));
#251135=CARTESIAN_POINT('Ctrl Pts',(18.6573530024033,17.3295529098618,0.));
#251136=CARTESIAN_POINT('Ctrl Pts',(18.6483405141865,17.3041204135074,0.));
#251137=CARTESIAN_POINT('Ctrl Pts',(18.6392945554748,17.2787779120213,0.));
#251138=CARTESIAN_POINT('Ctrl Pts',(18.6302155097943,17.2535257482187,0.));
#251139=CARTESIAN_POINT('Ctrl Pts',(18.6211037624038,17.2283642650518,0.));
#251140=CARTESIAN_POINT('Ctrl Pts',(18.6119596959949,17.2032938019284,0.));
#251141=CARTESIAN_POINT('Ctrl Pts',(18.6027836898817,17.1783146940127,0.));
#251142=CARTESIAN_POINT('Ctrl Pts',(18.5935761222825,17.1534272741643,0.));
#251143=CARTESIAN_POINT('Ctrl Pts',(18.5843373717247,17.1286318741183,0.));
#251144=CARTESIAN_POINT('Ctrl Pts',(18.5750678188542,17.1039288260001,0.));
#251145=CARTESIAN_POINT('Ctrl Pts',(18.5657678479789,17.0793184636079,0.));
#251146=CARTESIAN_POINT('Ctrl Pts',(18.556437848963,17.0548011239751,0.));
#251147=CARTESIAN_POINT('Ctrl Pts',(18.547078218209,17.0303771481738,0.));
#251148=CARTESIAN_POINT('Ctrl Pts',(18.5376893576961,17.0060468805097,0.));
#251149=CARTESIAN_POINT('Ctrl Pts',(18.5282716744197,16.981810668038,0.));
#251150=CARTESIAN_POINT('Ctrl Pts',(18.5188255796659,16.9576688599339,0.));
#251151=CARTESIAN_POINT('Ctrl Pts',(18.5093514883835,16.9336218069353,0.));
#251152=CARTESIAN_POINT('Ctrl Pts',(18.499849818462,16.9096698606943,0.));
#251153=CARTESIAN_POINT('Ctrl Pts',(18.4903209902227,16.8858133733088,0.));
#251154=CARTESIAN_POINT('Ctrl Pts',(18.4807654268771,16.8620526977171,0.));
#251155=CARTESIAN_POINT('Ctrl Pts',(18.4711835548623,16.8383881879709,0.));
#251156=CARTESIAN_POINT('Ctrl Pts',(18.4615758042305,16.8148201995472,0.));
#251157=CARTESIAN_POINT('Ctrl Pts',(18.4519426090123,16.791349089629,0.));
#251158=CARTESIAN_POINT('Ctrl Pts',(18.44228440761,16.7679752173992,0.));
#251159=CARTESIAN_POINT('Ctrl Pts',(18.4326016431392,16.7446989442882,0.));
#251160=CARTESIAN_POINT('Ctrl Pts',(18.4228947633187,16.7215206338818,0.));
#251161=CARTESIAN_POINT('Ctrl Pts',(18.413164220399,16.6984406518491,0.));
#251162=CARTESIAN_POINT('Ctrl Pts',(18.403410471079,16.6754593658513,0.));
#251163=CARTESIAN_POINT('Ctrl Pts',(18.3936339764332,16.6525771454513,0.));
#251164=CARTESIAN_POINT('Ctrl Pts',(18.3838352018327,16.6297943620056,0.));
#251165=CARTESIAN_POINT('Ctrl Pts',(18.3740146168879,16.607111388571,0.));
#251166=CARTESIAN_POINT('Ctrl Pts',(18.3641726955889,16.5845286000217,0.));
#251167=CARTESIAN_POINT('Ctrl Pts',(18.354309916433,16.5620463731413,0.));
#251168=CARTESIAN_POINT('Ctrl Pts',(18.34442676256,16.5396650867139,0.));
#251169=CARTESIAN_POINT('Ctrl Pts',(18.3345237218864,16.5173851216045,0.));
#251170=CARTESIAN_POINT('Ctrl Pts',(18.3246012872469,16.4952068608345,0.));
#251171=CARTESIAN_POINT('Ctrl Pts',(18.3146599565231,16.4731306896441,0.));
#251172=CARTESIAN_POINT('Ctrl Pts',(18.304700232686,16.4511569955233,0.));
#251173=CARTESIAN_POINT('Ctrl Pts',(18.294722623851,16.4292861682379,0.));
#251174=CARTESIAN_POINT('Ctrl Pts',(18.2847276433309,16.4075185998455,0.));
#251175=CARTESIAN_POINT('Ctrl Pts',(18.2747158096934,16.385854684708,0.));
#251176=CARTESIAN_POINT('Ctrl Pts',(18.2646876468169,16.3642948194868,0.));
#251177=CARTESIAN_POINT('Ctrl Pts',(18.2546436839608,16.3428394031589,0.));
#251178=CARTESIAN_POINT('Ctrl Pts',(18.2445844558742,16.3214888370987,0.));
#251179=CARTESIAN_POINT('Ctrl Pts',(18.2345105028982,16.3002435251378,0.));
#251180=CARTESIAN_POINT('Ctrl Pts',(18.2244223710745,16.2791038736223,0.));
#251181=CARTESIAN_POINT('Ctrl Pts',(18.2143206122529,16.2580702914615,0.));
#251182=CARTESIAN_POINT('Ctrl Pts',(18.2042057842035,16.2371431901638,0.));
#251183=CARTESIAN_POINT('Ctrl Pts',(18.1940784507229,16.2163229838875,0.));
#251184=CARTESIAN_POINT('Ctrl Pts',(18.1839391817331,16.1956100895073,0.));
#251185=CARTESIAN_POINT('Ctrl Pts',(18.1737885533849,16.1750049266671,0.));
#251186=CARTESIAN_POINT('Ctrl Pts',(18.1636271481615,16.154507917826,0.));
#251187=CARTESIAN_POINT('Ctrl Pts',(18.1534555549852,16.1341194882988,0.));
#251188=CARTESIAN_POINT('Ctrl Pts',(18.1432743693235,16.1138400662794,0.));
#251189=CARTESIAN_POINT('Ctrl Pts',(18.1330841933105,16.0936700829112,0.));
#251190=CARTESIAN_POINT('Ctrl Pts',(18.1228856358751,16.0736099723668,0.));
#251191=CARTESIAN_POINT('Ctrl Pts',(18.112679312869,16.0536601719126,0.));
#251192=CARTESIAN_POINT('Ctrl Pts',(18.1024658471966,16.0338211219693,0.));
#251193=CARTESIAN_POINT('Ctrl Pts',(18.0922458689462,16.014093266161,0.));
#251194=CARTESIAN_POINT('Ctrl Pts',(18.0820200155236,15.9944770513613,0.));
#251195=CARTESIAN_POINT('Ctrl Pts',(18.0717889317958,15.9749729277846,0.));
#251196=CARTESIAN_POINT('Ctrl Pts',(18.061553270236,15.9555813490644,0.));
#251197=CARTESIAN_POINT('Ctrl Pts',(18.0513136910691,15.9363027723244,0.));
#251198=CARTESIAN_POINT('Ctrl Pts',(18.0410708624208,15.9171376582436,0.));
#251199=CARTESIAN_POINT('Ctrl Pts',(18.0308254604636,15.8980864711042,0.));
#251200=CARTESIAN_POINT('Ctrl Pts',(18.0205781695769,15.8791496788683,0.));
#251201=CARTESIAN_POINT('Ctrl Pts',(18.0103296825205,15.8603277532831,0.));
#251202=CARTESIAN_POINT('Ctrl Pts',(18.0000807006052,15.8416211699679,0.));
#251203=CARTESIAN_POINT('Ctrl Pts',(17.9898319338664,15.8230304084962,0.));
#251204=CARTESIAN_POINT('Ctrl Pts',(17.9795841012386,15.8045559524677,0.));
#251205=CARTESIAN_POINT('Ctrl Pts',(17.9693379307303,15.7861982895724,0.));
#251206=CARTESIAN_POINT('Ctrl Pts',(17.9590941596242,15.7679579117077,0.));
#251207=CARTESIAN_POINT('Ctrl Pts',(17.9488535346781,15.749835315086,0.));
#251208=CARTESIAN_POINT('Ctrl Pts',(17.9386168123262,15.7318310003335,0.));
#251209=CARTESIAN_POINT('Ctrl Pts',(17.9283847588836,15.7139454725839,0.));
#251210=CARTESIAN_POINT('Ctrl Pts',(17.9181581507455,15.6961792415522,0.));
#251211=CARTESIAN_POINT('Ctrl Pts',(17.9079377746111,15.6785328216461,0.));
#251212=CARTESIAN_POINT('Ctrl Pts',(17.897724427724,15.661006732103,0.));
#251213=CARTESIAN_POINT('Ctrl Pts',(17.8875189181091,15.6436014971085,0.));
#251214=CARTESIAN_POINT('Ctrl Pts',(17.8773220648125,15.6263176459108,0.));
#251215=CARTESIAN_POINT('Ctrl Pts',(17.8671346981394,15.609155712921,0.));
#251216=CARTESIAN_POINT('Ctrl Pts',(17.8569576599006,15.5921162378192,0.));
#251217=CARTESIAN_POINT('Ctrl Pts',(17.8467918036987,15.5751997657163,0.));
#251218=CARTESIAN_POINT('Ctrl Pts',(17.8366379952085,15.5584068472982,0.));
#251219=CARTESIAN_POINT('Ctrl Pts',(17.8264971124606,15.541738038964,0.));
#251220=CARTESIAN_POINT('Ctrl Pts',(17.8163700461256,15.5251939029552,0.));
#251221=CARTESIAN_POINT('Ctrl Pts',(17.8062576997952,15.5087750074718,0.));
#251222=CARTESIAN_POINT('Ctrl Pts',(17.7961609903148,15.4924819268517,0.));
#251223=CARTESIAN_POINT('Ctrl Pts',(17.7860808481219,15.4763152417497,0.));
#251224=CARTESIAN_POINT('Ctrl Pts',(17.7760182175815,15.4602755393018,0.));
#251225=CARTESIAN_POINT('Ctrl Pts',(17.7659740573265,15.4443634132869,0.));
#251226=CARTESIAN_POINT('Ctrl Pts',(17.7559493405881,15.4285794642668,0.));
#251227=CARTESIAN_POINT('Ctrl Pts',(17.7459450555812,15.4129242997837,0.));
#251228=CARTESIAN_POINT('Ctrl Pts',(17.7359622059149,15.3973985345802,0.));
#251229=CARTESIAN_POINT('Ctrl Pts',(17.7260018109924,15.3820027907967,0.));
#251230=CARTESIAN_POINT('Ctrl Pts',(17.7160649064206,15.3667376981699,0.));
#251231=CARTESIAN_POINT('Ctrl Pts',(17.7061525444042,15.351603894206,0.));
#251232=CARTESIAN_POINT('Ctrl Pts',(17.6962657941983,15.3366020244066,0.));
#251233=CARTESIAN_POINT('Ctrl Pts',(17.6864057426052,15.3217327425338,0.));
#251234=CARTESIAN_POINT('Ctrl Pts',(17.676573494456,15.3069967108501,0.));
#251235=CARTESIAN_POINT('Ctrl Pts',(17.6667701731041,15.2923946003598,0.));
#251236=CARTESIAN_POINT('Ctrl Pts',(17.6569969209,15.2779270910239,0.));
#251237=CARTESIAN_POINT('Ctrl Pts',(17.6472548997328,15.2635948720292,0.));
#251238=CARTESIAN_POINT('Ctrl Pts',(17.6375452916369,15.2493986421092,0.));
#251239=CARTESIAN_POINT('Ctrl Pts',(17.6278692993764,15.2353391098367,0.));
#251240=CARTESIAN_POINT('Ctrl Pts',(17.6182281470468,15.22141699392,0.));
#251241=CARTESIAN_POINT('Ctrl Pts',(17.60862308065,15.2076330234686,0.));
#251242=CARTESIAN_POINT('Ctrl Pts',(17.5990553687599,15.1939879383268,0.));
#251243=CARTESIAN_POINT('Ctrl Pts',(17.5895263032595,15.1804824894605,0.));
#251244=CARTESIAN_POINT('Ctrl Pts',(17.580037200054,15.1671174393137,0.));
#251245=CARTESIAN_POINT('Ctrl Pts',(17.5705893998029,15.1538935621714,0.));
#251246=CARTESIAN_POINT('Ctrl Pts',(17.5611842686192,15.1408116444876,0.));
#251247=CARTESIAN_POINT('Ctrl Pts',(17.5518231989117,15.1278724853138,0.));
#251248=CARTESIAN_POINT('Ctrl Pts',(17.5425076102963,15.1150768967728,0.));
#251249=CARTESIAN_POINT('Ctrl Pts',(17.5332389504829,15.1024257045033,0.));
#251250=CARTESIAN_POINT('Ctrl Pts',(17.524018696179,15.0899197481082,0.));
#251251=CARTESIAN_POINT('Ctrl Pts',(17.5148483539687,15.0775598815749,0.));
#251252=CARTESIAN_POINT('Ctrl Pts',(17.5057294613877,15.0653469738307,0.));
#251253=CARTESIAN_POINT('Ctrl Pts',(17.4966635880246,15.0532819093085,0.));
#251254=CARTESIAN_POINT('Ctrl Pts',(17.4876523366178,15.0413655884993,0.));
#251255=CARTESIAN_POINT('Ctrl Pts',(17.4786973441417,15.029598928488,0.));
#251256=CARTESIAN_POINT('Ctrl Pts',(17.4698002829357,15.0179828635087,0.));
#251257=CARTESIAN_POINT('Ctrl Pts',(17.4609628621419,15.0065183456923,0.));
#251258=CARTESIAN_POINT('Ctrl Pts',(17.4521868291005,14.9952063457779,0.));
#251259=CARTESIAN_POINT('Ctrl Pts',(17.4434739707773,14.9840478538357,0.));
#251260=CARTESIAN_POINT('Ctrl Pts',(17.4348261151395,14.973043879945,0.));
#251261=CARTESIAN_POINT('Ctrl Pts',(17.4262451327088,14.9621954549825,0.));
#251262=CARTESIAN_POINT('Ctrl Pts',(17.4177329382827,14.9515036315142,0.));
#251263=CARTESIAN_POINT('Ctrl Pts',(17.4092914926071,14.940969484645,0.));
#251264=CARTESIAN_POINT('Ctrl Pts',(17.400922804075,14.9305941128758,0.));
#251265=CARTESIAN_POINT('Ctrl Pts',(17.3926289303987,14.9203786389343,0.));
#251266=CARTESIAN_POINT('Ctrl Pts',(17.3844119809823,14.9103242110057,0.));
#251267=CARTESIAN_POINT('Ctrl Pts',(17.3762741193075,14.9004320039609,0.));
#251268=CARTESIAN_POINT('Ctrl Pts',(17.3682175653236,14.8907032205789,0.));
#251269=CARTESIAN_POINT('Ctrl Pts',(17.3602445978163,14.8811390927424,0.));
#251270=CARTESIAN_POINT('Ctrl Pts',(17.3523575568648,14.8717408826958,0.));
#251271=CARTESIAN_POINT('Ctrl Pts',(17.3445588463477,14.8625098843419,0.));
#251272=CARTESIAN_POINT('Ctrl Pts',(17.336850936485,14.8534474245433,0.));
#251273=CARTESIAN_POINT('Ctrl Pts',(17.3292363662601,14.8445548643505,0.));
#251274=CARTESIAN_POINT('Ctrl Pts',(17.3217177462096,14.8358336004193,0.));
#251275=CARTESIAN_POINT('Ctrl Pts',(17.3142977632656,14.8272850675375,0.));
#251276=CARTESIAN_POINT('Ctrl Pts',(17.3069791853705,14.8189107410161,0.));
#251277=CARTESIAN_POINT('Ctrl Pts',(17.2997648661483,14.8107121391038,0.));
#251278=CARTESIAN_POINT('Ctrl Pts',(17.2926577496519,14.8026908254281,0.));
#251279=CARTESIAN_POINT('Ctrl Pts',(17.28566087332,14.7948484105253,0.));
#251280=CARTESIAN_POINT('Ctrl Pts',(17.278777370485,14.787186553128,0.));
#251281=CARTESIAN_POINT('Ctrl Pts',(17.2720104735192,14.7797069617802,0.));
#251282=CARTESIAN_POINT('Ctrl Pts',(17.2653635155317,14.7724113956728,0.));
#251283=CARTESIAN_POINT('Ctrl Pts',(17.2588399401464,14.7653016697589,0.));
#251284=CARTESIAN_POINT('Ctrl Pts',(17.2524433146837,14.7583796616617,0.));
#251285=CARTESIAN_POINT('Ctrl Pts',(17.2461773413289,14.7516473175125,0.));
#251286=CARTESIAN_POINT('Ctrl Pts',(17.2400458713566,14.7451066593793,0.));
#251287=CARTESIAN_POINT('Ctrl Pts',(17.2340529062077,14.7387597858117,0.));
#251288=CARTESIAN_POINT('Ctrl Pts',(17.2282025904314,14.7326088681163,0.));
#251289=CARTESIAN_POINT('Ctrl Pts',(17.2224992099666,14.7266561494282,0.));
#251290=CARTESIAN_POINT('Ctrl Pts',(17.2169471814255,14.7209039390326,0.));
#251291=CARTESIAN_POINT('Ctrl Pts',(17.2115510835988,14.7153546289338,0.));
#251292=CARTESIAN_POINT('Ctrl Pts',(17.2063157097316,14.7100107213587,0.));
#251293=CARTESIAN_POINT('Ctrl Pts',(17.2012461084268,14.7048748502663,0.));
#251294=CARTESIAN_POINT('Ctrl Pts',(17.1963476411694,14.699949811582,0.));
#251295=CARTESIAN_POINT('Ctrl Pts',(17.1916259308415,14.6952385361706,0.));
#251296=CARTESIAN_POINT('Ctrl Pts',(17.1870867909918,14.6907440526958,0.));
#251297=CARTESIAN_POINT('Ctrl Pts',(17.182736158472,14.6864694522319,0.));
#251298=CARTESIAN_POINT('Ctrl Pts',(17.1785800350827,14.6824178576167,0.));
#251299=CARTESIAN_POINT('Ctrl Pts',(17.1746247499057,14.6785925615676,0.));
#251300=CARTESIAN_POINT('Ctrl Pts',(17.1708771619129,14.6749971333867,0.));
#251301=CARTESIAN_POINT('Ctrl Pts',(17.1673449723019,14.6716355833321,0.));
#251302=CARTESIAN_POINT('Ctrl Pts',(17.1640366762304,14.6685123374424,0.));
#251303=CARTESIAN_POINT('Ctrl Pts',(17.1609609517369,14.6656319165057,0.));
#251304=CARTESIAN_POINT('Ctrl Pts',(17.1581262646789,14.662998728599,0.));
#251305=CARTESIAN_POINT('Ctrl Pts',(17.1555401986403,14.660616716964,0.));
#251306=CARTESIAN_POINT('Ctrl Pts',(17.1532107762719,14.6584900555301,0.));
#251307=CARTESIAN_POINT('Ctrl Pts',(17.1511476869495,14.6566237952435,0.));
#251308=CARTESIAN_POINT('Ctrl Pts',(17.1493641837556,14.6550248622813,0.));
#251309=CARTESIAN_POINT('Ctrl Pts',(17.1478763944909,14.6537016966188,0.));
#251310=CARTESIAN_POINT('Ctrl Pts',(17.1466998098673,14.6526624064978,0.));
#251311=CARTESIAN_POINT('Ctrl Pts',(17.1458462295273,14.65191316345,0.));
#251312=CARTESIAN_POINT('Ctrl Pts',(17.1454262858045,14.6515481598057,0.));
#251313=CARTESIAN_POINT('Ctrl Pts',(17.1452600887039,14.6514066997188,0.));
#251314=CARTESIAN_POINT('Ctrl Pts',(17.1452153999142,14.651371185284,0.));
#251315=CARTESIAN_POINT('Ctrl Pts',(17.1452095830633,14.6513681262571,0.));
#251316=CARTESIAN_POINT('',(18.8464468996588,17.9112098770111,12.));
#251317=CARTESIAN_POINT('',(18.8464468996588,17.9112098770111,0.));
#251318=CARTESIAN_POINT('Ctrl Pts',(17.1452095830633,14.6513681262571,12.));
#251319=CARTESIAN_POINT('Ctrl Pts',(17.1452153999142,14.651371185284,12.));
#251320=CARTESIAN_POINT('Ctrl Pts',(17.1452600887039,14.6514066997188,12.));
#251321=CARTESIAN_POINT('Ctrl Pts',(17.1454262858045,14.6515481598057,12.));
#251322=CARTESIAN_POINT('Ctrl Pts',(17.1458462295273,14.65191316345,12.));
#251323=CARTESIAN_POINT('Ctrl Pts',(17.1466998098673,14.6526624064978,12.));
#251324=CARTESIAN_POINT('Ctrl Pts',(17.1478763944909,14.6537016966188,12.));
#251325=CARTESIAN_POINT('Ctrl Pts',(17.1493641837556,14.6550248622813,12.));
#251326=CARTESIAN_POINT('Ctrl Pts',(17.1511476869495,14.6566237952435,12.));
#251327=CARTESIAN_POINT('Ctrl Pts',(17.1532107762719,14.6584900555301,12.));
#251328=CARTESIAN_POINT('Ctrl Pts',(17.1555401986403,14.660616716964,12.));
#251329=CARTESIAN_POINT('Ctrl Pts',(17.1581262646789,14.662998728599,12.));
#251330=CARTESIAN_POINT('Ctrl Pts',(17.1609609517369,14.6656319165057,12.));
#251331=CARTESIAN_POINT('Ctrl Pts',(17.1640366762304,14.6685123374424,12.));
#251332=CARTESIAN_POINT('Ctrl Pts',(17.1673449723019,14.6716355833321,12.));
#251333=CARTESIAN_POINT('Ctrl Pts',(17.1708771619129,14.6749971333867,12.));
#251334=CARTESIAN_POINT('Ctrl Pts',(17.1746247499057,14.6785925615676,12.));
#251335=CARTESIAN_POINT('Ctrl Pts',(17.1785800350827,14.6824178576167,12.));
#251336=CARTESIAN_POINT('Ctrl Pts',(17.182736158472,14.6864694522319,12.));
#251337=CARTESIAN_POINT('Ctrl Pts',(17.1870867909918,14.6907440526958,12.));
#251338=CARTESIAN_POINT('Ctrl Pts',(17.1916259308415,14.6952385361706,12.));
#251339=CARTESIAN_POINT('Ctrl Pts',(17.1963476411694,14.699949811582,12.));
#251340=CARTESIAN_POINT('Ctrl Pts',(17.2012461084268,14.7048748502663,12.));
#251341=CARTESIAN_POINT('Ctrl Pts',(17.2063157097316,14.7100107213587,12.));
#251342=CARTESIAN_POINT('Ctrl Pts',(17.2115510835988,14.7153546289338,12.));
#251343=CARTESIAN_POINT('Ctrl Pts',(17.2169471814255,14.7209039390326,12.));
#251344=CARTESIAN_POINT('Ctrl Pts',(17.2224992099666,14.7266561494282,12.));
#251345=CARTESIAN_POINT('Ctrl Pts',(17.2282025904314,14.7326088681163,12.));
#251346=CARTESIAN_POINT('Ctrl Pts',(17.2340529062077,14.7387597858117,12.));
#251347=CARTESIAN_POINT('Ctrl Pts',(17.2400458713566,14.7451066593793,12.));
#251348=CARTESIAN_POINT('Ctrl Pts',(17.2461773413289,14.7516473175125,12.));
#251349=CARTESIAN_POINT('Ctrl Pts',(17.2524433146837,14.7583796616617,12.));
#251350=CARTESIAN_POINT('Ctrl Pts',(17.2588399401464,14.7653016697589,12.));
#251351=CARTESIAN_POINT('Ctrl Pts',(17.2653635155317,14.7724113956728,12.));
#251352=CARTESIAN_POINT('Ctrl Pts',(17.2720104735192,14.7797069617802,12.));
#251353=CARTESIAN_POINT('Ctrl Pts',(17.278777370485,14.787186553128,12.));
#251354=CARTESIAN_POINT('Ctrl Pts',(17.28566087332,14.7948484105253,12.));
#251355=CARTESIAN_POINT('Ctrl Pts',(17.2926577496519,14.8026908254281,12.));
#251356=CARTESIAN_POINT('Ctrl Pts',(17.2997648661483,14.8107121391038,12.));
#251357=CARTESIAN_POINT('Ctrl Pts',(17.3069791853705,14.8189107410161,12.));
#251358=CARTESIAN_POINT('Ctrl Pts',(17.3142977632656,14.8272850675375,12.));
#251359=CARTESIAN_POINT('Ctrl Pts',(17.3217177462096,14.8358336004193,12.));
#251360=CARTESIAN_POINT('Ctrl Pts',(17.3292363662601,14.8445548643505,12.));
#251361=CARTESIAN_POINT('Ctrl Pts',(17.336850936485,14.8534474245433,12.));
#251362=CARTESIAN_POINT('Ctrl Pts',(17.3445588463477,14.8625098843419,12.));
#251363=CARTESIAN_POINT('Ctrl Pts',(17.3523575568648,14.8717408826958,12.));
#251364=CARTESIAN_POINT('Ctrl Pts',(17.3602445978163,14.8811390927424,12.));
#251365=CARTESIAN_POINT('Ctrl Pts',(17.3682175653236,14.8907032205789,12.));
#251366=CARTESIAN_POINT('Ctrl Pts',(17.3762741193075,14.9004320039609,12.));
#251367=CARTESIAN_POINT('Ctrl Pts',(17.3844119809823,14.9103242110057,12.));
#251368=CARTESIAN_POINT('Ctrl Pts',(17.3926289303987,14.9203786389343,12.));
#251369=CARTESIAN_POINT('Ctrl Pts',(17.400922804075,14.9305941128758,12.));
#251370=CARTESIAN_POINT('Ctrl Pts',(17.4092914926071,14.940969484645,12.));
#251371=CARTESIAN_POINT('Ctrl Pts',(17.4177329382827,14.9515036315142,12.));
#251372=CARTESIAN_POINT('Ctrl Pts',(17.4262451327088,14.9621954549825,12.));
#251373=CARTESIAN_POINT('Ctrl Pts',(17.4348261151395,14.973043879945,12.));
#251374=CARTESIAN_POINT('Ctrl Pts',(17.4434739707773,14.9840478538357,12.));
#251375=CARTESIAN_POINT('Ctrl Pts',(17.4521868291005,14.9952063457779,12.));
#251376=CARTESIAN_POINT('Ctrl Pts',(17.4609628621419,15.0065183456923,12.));
#251377=CARTESIAN_POINT('Ctrl Pts',(17.4698002829357,15.0179828635087,12.));
#251378=CARTESIAN_POINT('Ctrl Pts',(17.4786973441417,15.029598928488,12.));
#251379=CARTESIAN_POINT('Ctrl Pts',(17.4876523366178,15.0413655884993,12.));
#251380=CARTESIAN_POINT('Ctrl Pts',(17.4966635880246,15.0532819093085,12.));
#251381=CARTESIAN_POINT('Ctrl Pts',(17.5057294613877,15.0653469738307,12.));
#251382=CARTESIAN_POINT('Ctrl Pts',(17.5148483539687,15.0775598815749,12.));
#251383=CARTESIAN_POINT('Ctrl Pts',(17.524018696179,15.0899197481082,12.));
#251384=CARTESIAN_POINT('Ctrl Pts',(17.5332389504829,15.1024257045033,12.));
#251385=CARTESIAN_POINT('Ctrl Pts',(17.5425076102963,15.1150768967728,12.));
#251386=CARTESIAN_POINT('Ctrl Pts',(17.5518231989117,15.1278724853138,12.));
#251387=CARTESIAN_POINT('Ctrl Pts',(17.5611842686192,15.1408116444876,12.));
#251388=CARTESIAN_POINT('Ctrl Pts',(17.5705893998029,15.1538935621714,12.));
#251389=CARTESIAN_POINT('Ctrl Pts',(17.580037200054,15.1671174393137,12.));
#251390=CARTESIAN_POINT('Ctrl Pts',(17.5895263032595,15.1804824894605,12.));
#251391=CARTESIAN_POINT('Ctrl Pts',(17.5990553687599,15.1939879383268,12.));
#251392=CARTESIAN_POINT('Ctrl Pts',(17.60862308065,15.2076330234686,12.));
#251393=CARTESIAN_POINT('Ctrl Pts',(17.6182281470468,15.22141699392,12.));
#251394=CARTESIAN_POINT('Ctrl Pts',(17.6278692993764,15.2353391098367,12.));
#251395=CARTESIAN_POINT('Ctrl Pts',(17.6375452916369,15.2493986421092,12.));
#251396=CARTESIAN_POINT('Ctrl Pts',(17.6472548997328,15.2635948720292,12.));
#251397=CARTESIAN_POINT('Ctrl Pts',(17.6569969209,15.2779270910239,12.));
#251398=CARTESIAN_POINT('Ctrl Pts',(17.6667701731041,15.2923946003598,12.));
#251399=CARTESIAN_POINT('Ctrl Pts',(17.676573494456,15.3069967108501,12.));
#251400=CARTESIAN_POINT('Ctrl Pts',(17.6864057426052,15.3217327425338,12.));
#251401=CARTESIAN_POINT('Ctrl Pts',(17.6962657941983,15.3366020244066,12.));
#251402=CARTESIAN_POINT('Ctrl Pts',(17.7061525444042,15.351603894206,12.));
#251403=CARTESIAN_POINT('Ctrl Pts',(17.7160649064206,15.3667376981699,12.));
#251404=CARTESIAN_POINT('Ctrl Pts',(17.7260018109924,15.3820027907967,12.));
#251405=CARTESIAN_POINT('Ctrl Pts',(17.7359622059149,15.3973985345802,12.));
#251406=CARTESIAN_POINT('Ctrl Pts',(17.7459450555812,15.4129242997837,12.));
#251407=CARTESIAN_POINT('Ctrl Pts',(17.7559493405881,15.4285794642668,12.));
#251408=CARTESIAN_POINT('Ctrl Pts',(17.7659740573265,15.4443634132869,12.));
#251409=CARTESIAN_POINT('Ctrl Pts',(17.7760182175815,15.4602755393018,12.));
#251410=CARTESIAN_POINT('Ctrl Pts',(17.7860808481219,15.4763152417497,12.));
#251411=CARTESIAN_POINT('Ctrl Pts',(17.7961609903148,15.4924819268517,12.));
#251412=CARTESIAN_POINT('Ctrl Pts',(17.8062576997952,15.5087750074718,12.));
#251413=CARTESIAN_POINT('Ctrl Pts',(17.8163700461256,15.5251939029552,12.));
#251414=CARTESIAN_POINT('Ctrl Pts',(17.8264971124606,15.541738038964,12.));
#251415=CARTESIAN_POINT('Ctrl Pts',(17.8366379952085,15.5584068472982,12.));
#251416=CARTESIAN_POINT('Ctrl Pts',(17.8467918036987,15.5751997657163,12.));
#251417=CARTESIAN_POINT('Ctrl Pts',(17.8569576599006,15.5921162378192,12.));
#251418=CARTESIAN_POINT('Ctrl Pts',(17.8671346981394,15.609155712921,12.));
#251419=CARTESIAN_POINT('Ctrl Pts',(17.8773220648125,15.6263176459108,12.));
#251420=CARTESIAN_POINT('Ctrl Pts',(17.8875189181091,15.6436014971085,12.));
#251421=CARTESIAN_POINT('Ctrl Pts',(17.897724427724,15.661006732103,12.));
#251422=CARTESIAN_POINT('Ctrl Pts',(17.9079377746111,15.6785328216461,12.));
#251423=CARTESIAN_POINT('Ctrl Pts',(17.9181581507455,15.6961792415522,12.));
#251424=CARTESIAN_POINT('Ctrl Pts',(17.9283847588836,15.7139454725839,12.));
#251425=CARTESIAN_POINT('Ctrl Pts',(17.9386168123262,15.7318310003335,12.));
#251426=CARTESIAN_POINT('Ctrl Pts',(17.9488535346781,15.749835315086,12.));
#251427=CARTESIAN_POINT('Ctrl Pts',(17.9590941596242,15.7679579117077,12.));
#251428=CARTESIAN_POINT('Ctrl Pts',(17.9693379307303,15.7861982895724,12.));
#251429=CARTESIAN_POINT('Ctrl Pts',(17.9795841012386,15.8045559524677,12.));
#251430=CARTESIAN_POINT('Ctrl Pts',(17.9898319338664,15.8230304084962,12.));
#251431=CARTESIAN_POINT('Ctrl Pts',(18.0000807006052,15.8416211699679,12.));
#251432=CARTESIAN_POINT('Ctrl Pts',(18.0103296825205,15.8603277532831,12.));
#251433=CARTESIAN_POINT('Ctrl Pts',(18.0205781695769,15.8791496788683,12.));
#251434=CARTESIAN_POINT('Ctrl Pts',(18.0308254604636,15.8980864711042,12.));
#251435=CARTESIAN_POINT('Ctrl Pts',(18.0410708624208,15.9171376582436,12.));
#251436=CARTESIAN_POINT('Ctrl Pts',(18.0513136910691,15.9363027723244,12.));
#251437=CARTESIAN_POINT('Ctrl Pts',(18.061553270236,15.9555813490644,12.));
#251438=CARTESIAN_POINT('Ctrl Pts',(18.0717889317958,15.9749729277846,12.));
#251439=CARTESIAN_POINT('Ctrl Pts',(18.0820200155236,15.9944770513613,12.));
#251440=CARTESIAN_POINT('Ctrl Pts',(18.0922458689462,16.014093266161,12.));
#251441=CARTESIAN_POINT('Ctrl Pts',(18.1024658471966,16.0338211219693,12.));
#251442=CARTESIAN_POINT('Ctrl Pts',(18.112679312869,16.0536601719126,12.));
#251443=CARTESIAN_POINT('Ctrl Pts',(18.1228856358751,16.0736099723668,12.));
#251444=CARTESIAN_POINT('Ctrl Pts',(18.1330841933105,16.0936700829112,12.));
#251445=CARTESIAN_POINT('Ctrl Pts',(18.1432743693235,16.1138400662794,12.));
#251446=CARTESIAN_POINT('Ctrl Pts',(18.1534555549852,16.1341194882988,12.));
#251447=CARTESIAN_POINT('Ctrl Pts',(18.1636271481615,16.154507917826,12.));
#251448=CARTESIAN_POINT('Ctrl Pts',(18.1737885533849,16.1750049266671,12.));
#251449=CARTESIAN_POINT('Ctrl Pts',(18.1839391817331,16.1956100895073,12.));
#251450=CARTESIAN_POINT('Ctrl Pts',(18.1940784507229,16.2163229838875,12.));
#251451=CARTESIAN_POINT('Ctrl Pts',(18.2042057842035,16.2371431901638,12.));
#251452=CARTESIAN_POINT('Ctrl Pts',(18.2143206122529,16.2580702914615,12.));
#251453=CARTESIAN_POINT('Ctrl Pts',(18.2244223710745,16.2791038736223,12.));
#251454=CARTESIAN_POINT('Ctrl Pts',(18.2345105028982,16.3002435251378,12.));
#251455=CARTESIAN_POINT('Ctrl Pts',(18.2445844558742,16.3214888370987,12.));
#251456=CARTESIAN_POINT('Ctrl Pts',(18.2546436839608,16.3428394031589,12.));
#251457=CARTESIAN_POINT('Ctrl Pts',(18.2646876468169,16.3642948194868,12.));
#251458=CARTESIAN_POINT('Ctrl Pts',(18.2747158096934,16.385854684708,12.));
#251459=CARTESIAN_POINT('Ctrl Pts',(18.2847276433309,16.4075185998455,12.));
#251460=CARTESIAN_POINT('Ctrl Pts',(18.294722623851,16.4292861682379,12.));
#251461=CARTESIAN_POINT('Ctrl Pts',(18.304700232686,16.4511569955233,12.));
#251462=CARTESIAN_POINT('Ctrl Pts',(18.3146599565231,16.4731306896441,12.));
#251463=CARTESIAN_POINT('Ctrl Pts',(18.3246012872469,16.4952068608345,12.));
#251464=CARTESIAN_POINT('Ctrl Pts',(18.3345237218864,16.5173851216045,12.));
#251465=CARTESIAN_POINT('Ctrl Pts',(18.34442676256,16.5396650867139,12.));
#251466=CARTESIAN_POINT('Ctrl Pts',(18.354309916433,16.5620463731413,12.));
#251467=CARTESIAN_POINT('Ctrl Pts',(18.3641726955889,16.5845286000217,12.));
#251468=CARTESIAN_POINT('Ctrl Pts',(18.3740146168879,16.607111388571,12.));
#251469=CARTESIAN_POINT('Ctrl Pts',(18.3838352018327,16.6297943620056,12.));
#251470=CARTESIAN_POINT('Ctrl Pts',(18.3936339764332,16.6525771454513,12.));
#251471=CARTESIAN_POINT('Ctrl Pts',(18.403410471079,16.6754593658513,12.));
#251472=CARTESIAN_POINT('Ctrl Pts',(18.413164220399,16.6984406518491,12.));
#251473=CARTESIAN_POINT('Ctrl Pts',(18.4228947633187,16.7215206338818,12.));
#251474=CARTESIAN_POINT('Ctrl Pts',(18.4326016431392,16.7446989442882,12.));
#251475=CARTESIAN_POINT('Ctrl Pts',(18.44228440761,16.7679752173992,12.));
#251476=CARTESIAN_POINT('Ctrl Pts',(18.4519426090123,16.791349089629,12.));
#251477=CARTESIAN_POINT('Ctrl Pts',(18.4615758042305,16.8148201995472,12.));
#251478=CARTESIAN_POINT('Ctrl Pts',(18.4711835548623,16.8383881879709,12.));
#251479=CARTESIAN_POINT('Ctrl Pts',(18.4807654268771,16.8620526977171,12.));
#251480=CARTESIAN_POINT('Ctrl Pts',(18.4903209902227,16.8858133733088,12.));
#251481=CARTESIAN_POINT('Ctrl Pts',(18.499849818462,16.9096698606943,12.));
#251482=CARTESIAN_POINT('Ctrl Pts',(18.5093514883835,16.9336218069353,12.));
#251483=CARTESIAN_POINT('Ctrl Pts',(18.5188255796659,16.9576688599339,12.));
#251484=CARTESIAN_POINT('Ctrl Pts',(18.5282716744197,16.981810668038,12.));
#251485=CARTESIAN_POINT('Ctrl Pts',(18.5376893576961,17.0060468805097,12.));
#251486=CARTESIAN_POINT('Ctrl Pts',(18.547078218209,17.0303771481738,12.));
#251487=CARTESIAN_POINT('Ctrl Pts',(18.556437848963,17.0548011239751,12.));
#251488=CARTESIAN_POINT('Ctrl Pts',(18.5657678479789,17.0793184636079,12.));
#251489=CARTESIAN_POINT('Ctrl Pts',(18.5750678188542,17.1039288260001,12.));
#251490=CARTESIAN_POINT('Ctrl Pts',(18.5843373717247,17.1286318741183,12.));
#251491=CARTESIAN_POINT('Ctrl Pts',(18.5935761222825,17.1534272741643,12.));
#251492=CARTESIAN_POINT('Ctrl Pts',(18.6027836898817,17.1783146940127,12.));
#251493=CARTESIAN_POINT('Ctrl Pts',(18.6119596959949,17.2032938019284,12.));
#251494=CARTESIAN_POINT('Ctrl Pts',(18.6211037624038,17.2283642650518,12.));
#251495=CARTESIAN_POINT('Ctrl Pts',(18.6302155097943,17.2535257482187,12.));
#251496=CARTESIAN_POINT('Ctrl Pts',(18.6392945554748,17.2787779120213,12.));
#251497=CARTESIAN_POINT('Ctrl Pts',(18.6483405141865,17.3041204135074,12.));
#251498=CARTESIAN_POINT('Ctrl Pts',(18.6573530024033,17.3295529098618,12.));
#251499=CARTESIAN_POINT('Ctrl Pts',(18.6663316416582,17.3550750612443,12.));
#251500=CARTESIAN_POINT('Ctrl Pts',(18.6752760624052,17.3806865340747,12.));
#251501=CARTESIAN_POINT('Ctrl Pts',(18.6841859073471,17.4063870038562,12.));
#251502=CARTESIAN_POINT('Ctrl Pts',(18.6930608357409,17.4321761588142,12.));
#251503=CARTESIAN_POINT('Ctrl Pts',(18.70190052503,17.4580537012753,12.));
#251504=CARTESIAN_POINT('Ctrl Pts',(18.7107046613912,17.4840193397162,12.));
#251505=CARTESIAN_POINT('Ctrl Pts',(18.7194729318098,17.5100727820876,12.));
#251506=CARTESIAN_POINT('Ctrl Pts',(18.7282050157138,17.5362137287593,12.));
#251507=CARTESIAN_POINT('Ctrl Pts',(18.7369005764553,17.5624418653245,12.));
#251508=CARTESIAN_POINT('Ctrl Pts',(18.7455592536687,17.5887568561371,12.));
#251509=CARTESIAN_POINT('Ctrl Pts',(18.7541806530984,17.6151583357012,12.));
#251510=CARTESIAN_POINT('Ctrl Pts',(18.762764361321,17.6416459210681,12.));
#251511=CARTESIAN_POINT('Ctrl Pts',(18.7713099642754,17.6682192274236,12.));
#251512=CARTESIAN_POINT('Ctrl Pts',(18.7798170641374,17.6948778823014,12.));
#251513=CARTESIAN_POINT('Ctrl Pts',(18.7882852976049,17.7216215409035,12.));
#251514=CARTESIAN_POINT('Ctrl Pts',(18.7967143519419,17.7484498996905,12.));
#251515=CARTESIAN_POINT('Ctrl Pts',(18.8051039860448,17.7753627137853,12.));
#251516=CARTESIAN_POINT('Ctrl Pts',(18.8134540340417,17.8023598011057,12.));
#251517=CARTESIAN_POINT('Ctrl Pts',(18.8217643886157,17.8294410311006,12.));
#251518=CARTESIAN_POINT('Ctrl Pts',(18.8300349895974,17.8566063174771,12.));
#251519=CARTESIAN_POINT('Ctrl Pts',(18.8366196462581,17.8784057509356,12.));
#251520=CARTESIAN_POINT('Ctrl Pts',(18.8415402351786,17.8947931177807,12.));
#251521=CARTESIAN_POINT('Ctrl Pts',(18.8448126709691,17.9057348246595,12.));
#251522=CARTESIAN_POINT('Ctrl Pts',(18.8464468996588,17.9112098770111,12.));
#251523=CARTESIAN_POINT('Ctrl Pts',(18.5896416359912,12.7689476255363,0.));
#251524=CARTESIAN_POINT('Ctrl Pts',(18.5896416359912,12.7689476255363,12.));
#251525=CARTESIAN_POINT('Ctrl Pts',(18.5896460962964,12.7689524524483,0.));
#251526=CARTESIAN_POINT('Ctrl Pts',(18.5896460962964,12.7689524524483,12.));
#251527=CARTESIAN_POINT('Ctrl Pts',(18.5896919669165,12.768986426692,0.));
#251528=CARTESIAN_POINT('Ctrl Pts',(18.5896919669165,12.768986426692,12.));
#251529=CARTESIAN_POINT('Ctrl Pts',(18.589871621843,12.769110348199,0.));
#251530=CARTESIAN_POINT('Ctrl Pts',(18.589871621843,12.769110348199,12.));
#251531=CARTESIAN_POINT('Ctrl Pts',(18.5903328777227,12.7694215127919,0.));
#251532=CARTESIAN_POINT('Ctrl Pts',(18.5903328777227,12.7694215127919,12.));
#251533=CARTESIAN_POINT('Ctrl Pts',(18.5912775137806,12.7700520897173,0.));
#251534=CARTESIAN_POINT('Ctrl Pts',(18.5912775137806,12.7700520897173,12.));
#251535=CARTESIAN_POINT('Ctrl Pts',(18.5925859134579,12.7709195951156,0.));
#251536=CARTESIAN_POINT('Ctrl Pts',(18.5925859134579,12.7709195951156,12.));
#251537=CARTESIAN_POINT('Ctrl Pts',(18.5942490615407,12.7720142287172,0.));
#251538=CARTESIAN_POINT('Ctrl Pts',(18.5942490615407,12.7720142287172,12.));
#251539=CARTESIAN_POINT('Ctrl Pts',(18.5962551167772,12.7733231262108,0.));
#251540=CARTESIAN_POINT('Ctrl Pts',(18.5962551167772,12.7733231262108,12.));
#251541=CARTESIAN_POINT('Ctrl Pts',(18.598591752595,12.7748328937638,0.));
#251542=CARTESIAN_POINT('Ctrl Pts',(18.598591752595,12.7748328937638,12.));
#251543=CARTESIAN_POINT('Ctrl Pts',(18.6012488486709,12.7765325225081,0.));
#251544=CARTESIAN_POINT('Ctrl Pts',(18.6012488486709,12.7765325225081,12.));
#251545=CARTESIAN_POINT('Ctrl Pts',(18.6042190183704,12.7784139605066,0.));
#251546=CARTESIAN_POINT('Ctrl Pts',(18.6042190183704,12.7784139605066,12.));
#251547=CARTESIAN_POINT('Ctrl Pts',(18.6074961535723,12.7804705387658,0.));
#251548=CARTESIAN_POINT('Ctrl Pts',(18.6074961535723,12.7804705387658,12.));
#251549=CARTESIAN_POINT('Ctrl Pts',(18.6110744826219,12.7826959526925,0.));
#251550=CARTESIAN_POINT('Ctrl Pts',(18.6110744826219,12.7826959526925,12.));
#251551=CARTESIAN_POINT('Ctrl Pts',(18.6149475565188,12.7850831657901,0.));
#251552=CARTESIAN_POINT('Ctrl Pts',(18.6149475565188,12.7850831657901,12.));
#251553=CARTESIAN_POINT('Ctrl Pts',(18.6191087624752,12.7876249657834,0.));
#251554=CARTESIAN_POINT('Ctrl Pts',(18.6191087624752,12.7876249657834,12.));
#251555=CARTESIAN_POINT('Ctrl Pts',(18.6235516265575,12.7903142925234,0.));
#251556=CARTESIAN_POINT('Ctrl Pts',(18.6235516265575,12.7903142925234,12.));
#251557=CARTESIAN_POINT('Ctrl Pts',(18.6282702819371,12.7931447451555,0.));
#251558=CARTESIAN_POINT('Ctrl Pts',(18.6282702819371,12.7931447451555,12.));
#251559=CARTESIAN_POINT('Ctrl Pts',(18.6332595057006,12.7961106222251,0.));
#251560=CARTESIAN_POINT('Ctrl Pts',(18.6332595057006,12.7961106222251,12.));
#251561=CARTESIAN_POINT('Ctrl Pts',(18.63851447924,12.7992066625264,0.));
#251562=CARTESIAN_POINT('Ctrl Pts',(18.63851447924,12.7992066625264,12.));
#251563=CARTESIAN_POINT('Ctrl Pts',(18.6440306327456,12.8024278770153,0.));
#251564=CARTESIAN_POINT('Ctrl Pts',(18.6440306327456,12.8024278770153,12.));
#251565=CARTESIAN_POINT('Ctrl Pts',(18.6498034438987,12.805769331162,0.));
#251566=CARTESIAN_POINT('Ctrl Pts',(18.6498034438987,12.805769331162,12.));
#251567=CARTESIAN_POINT('Ctrl Pts',(18.6558284825773,12.8092261933858,0.));
#251568=CARTESIAN_POINT('Ctrl Pts',(18.6558284825773,12.8092261933858,12.));
#251569=CARTESIAN_POINT('Ctrl Pts',(18.6621014624746,12.8127937909631,0.));
#251570=CARTESIAN_POINT('Ctrl Pts',(18.6621014624746,12.8127937909631,12.));
#251571=CARTESIAN_POINT('Ctrl Pts',(18.6686182952799,12.8164676687362,0.));
#251572=CARTESIAN_POINT('Ctrl Pts',(18.6686182952799,12.8164676687362,12.));
#251573=CARTESIAN_POINT('Ctrl Pts',(18.6753751301092,12.8202436318474,0.));
#251574=CARTESIAN_POINT('Ctrl Pts',(18.6753751301092,12.8202436318474,12.));
#251575=CARTESIAN_POINT('Ctrl Pts',(18.6823683094139,12.8241176980017,0.));
#251576=CARTESIAN_POINT('Ctrl Pts',(18.6823683094139,12.8241176980017,12.));
#251577=CARTESIAN_POINT('Ctrl Pts',(18.6895943376171,12.8280860635231,0.));
#251578=CARTESIAN_POINT('Ctrl Pts',(18.6895943376171,12.8280860635231,12.));
#251579=CARTESIAN_POINT('Ctrl Pts',(18.6970498410172,12.8321450599789,0.));
#251580=CARTESIAN_POINT('Ctrl Pts',(18.6970498410172,12.8321450599789,12.));
#251581=CARTESIAN_POINT('Ctrl Pts',(18.7047315436294,12.8362911280361,0.));
#251582=CARTESIAN_POINT('Ctrl Pts',(18.7047315436294,12.8362911280361,12.));
#251583=CARTESIAN_POINT('Ctrl Pts',(18.7126362754445,12.8405208263431,0.));
#251584=CARTESIAN_POINT('Ctrl Pts',(18.7126362754445,12.8405208263431,12.));
#251585=CARTESIAN_POINT('Ctrl Pts',(18.7207609737702,12.8448308329494,0.));
#251586=CARTESIAN_POINT('Ctrl Pts',(18.7207609737702,12.8448308329494,12.));
#251587=CARTESIAN_POINT('Ctrl Pts',(18.7291026886554,12.8492179511591,0.));
#251588=CARTESIAN_POINT('Ctrl Pts',(18.7291026886554,12.8492179511591,12.));
#251589=CARTESIAN_POINT('Ctrl Pts',(18.7376585820854,12.8536791086316,0.));
#251590=CARTESIAN_POINT('Ctrl Pts',(18.7376585820854,12.8536791086316,12.));
#251591=CARTESIAN_POINT('Ctrl Pts',(18.7464259171251,12.8582113455646,0.));
#251592=CARTESIAN_POINT('Ctrl Pts',(18.7464259171251,12.8582113455646,12.));
#251593=CARTESIAN_POINT('Ctrl Pts',(18.7554020493887,12.8628118054171,0.));
#251594=CARTESIAN_POINT('Ctrl Pts',(18.7554020493887,12.8628118054171,12.));
#251595=CARTESIAN_POINT('Ctrl Pts',(18.7645844169564,12.8674777239653,0.));
#251596=CARTESIAN_POINT('Ctrl Pts',(18.7645844169564,12.8674777239653,12.));
#251597=CARTESIAN_POINT('Ctrl Pts',(18.7739705329022,12.872206421181,0.));
#251598=CARTESIAN_POINT('Ctrl Pts',(18.7739705329022,12.872206421181,12.));
#251599=CARTESIAN_POINT('Ctrl Pts',(18.7835579840477,12.8769952998095,0.));
#251600=CARTESIAN_POINT('Ctrl Pts',(18.7835579840477,12.8769952998095,12.));
#251601=CARTESIAN_POINT('Ctrl Pts',(18.7933444285868,12.8818418427475,0.));
#251602=CARTESIAN_POINT('Ctrl Pts',(18.7933444285868,12.8818418427475,12.));
#251603=CARTESIAN_POINT('Ctrl Pts',(18.8033275941943,12.8867436109546,0.));
#251604=CARTESIAN_POINT('Ctrl Pts',(18.8033275941943,12.8867436109546,12.));
#251605=CARTESIAN_POINT('Ctrl Pts',(18.813505275782,12.8916982409935,0.));
#251606=CARTESIAN_POINT('Ctrl Pts',(18.813505275782,12.8916982409935,12.));
#251607=CARTESIAN_POINT('Ctrl Pts',(18.8238753319129,12.8967034410755,0.));
#251608=CARTESIAN_POINT('Ctrl Pts',(18.8238753319129,12.8967034410755,12.));
#251609=CARTESIAN_POINT('Ctrl Pts',(18.834435681259,12.9017569871738,0.));
#251610=CARTESIAN_POINT('Ctrl Pts',(18.834435681259,12.9017569871738,12.));
#251611=CARTESIAN_POINT('Ctrl Pts',(18.8451842990984,12.9068567191854,0.));
#251612=CARTESIAN_POINT('Ctrl Pts',(18.8451842990984,12.9068567191854,12.));
#251613=CARTESIAN_POINT('Ctrl Pts',(18.8561192136198,12.9120005369063,0.));
#251614=CARTESIAN_POINT('Ctrl Pts',(18.8561192136198,12.9120005369063,12.));
#251615=CARTESIAN_POINT('Ctrl Pts',(18.8672385038326,12.9171863977045,0.));
#251616=CARTESIAN_POINT('Ctrl Pts',(18.8672385038326,12.9171863977045,12.));
#251617=CARTESIAN_POINT('Ctrl Pts',(18.8785402977527,12.9224123144982,0.));
#251618=CARTESIAN_POINT('Ctrl Pts',(18.8785402977527,12.9224123144982,12.));
#251619=CARTESIAN_POINT('Ctrl Pts',(18.8900227704889,12.9276763536373,0.));
#251620=CARTESIAN_POINT('Ctrl Pts',(18.8900227704889,12.9276763536373,12.));
#251621=CARTESIAN_POINT('Ctrl Pts',(18.9016841423403,12.9329766328185,0.));
#251622=CARTESIAN_POINT('Ctrl Pts',(18.9016841423403,12.9329766328185,12.));
#251623=CARTESIAN_POINT('Ctrl Pts',(18.9135226769465,12.9383113190375,0.));
#251624=CARTESIAN_POINT('Ctrl Pts',(18.9135226769465,12.9383113190375,12.));
#251625=CARTESIAN_POINT('Ctrl Pts',(18.9255366795195,12.9436786266105,0.));
#251626=CARTESIAN_POINT('Ctrl Pts',(18.9255366795195,12.9436786266105,12.));
#251627=CARTESIAN_POINT('Ctrl Pts',(18.9377244950435,12.9490768151821,0.));
#251628=CARTESIAN_POINT('Ctrl Pts',(18.9377244950435,12.9490768151821,12.));
#251629=CARTESIAN_POINT('Ctrl Pts',(18.9500845064715,12.9545041877377,0.));
#251630=CARTESIAN_POINT('Ctrl Pts',(18.9500845064715,12.9545041877377,12.));
#251631=CARTESIAN_POINT('Ctrl Pts',(18.9626151329229,12.9599590886319,0.));
#251632=CARTESIAN_POINT('Ctrl Pts',(18.9626151329229,12.9599590886319,12.));
#251633=CARTESIAN_POINT('Ctrl Pts',(18.9753148284475,12.9654399021869,0.));
#251634=CARTESIAN_POINT('Ctrl Pts',(18.9753148284475,12.9654399021869,12.));
#251635=CARTESIAN_POINT('Ctrl Pts',(18.9881820807585,12.9709450512747,0.));
#251636=CARTESIAN_POINT('Ctrl Pts',(18.9881820807585,12.9709450512747,12.));
#251637=CARTESIAN_POINT('Ctrl Pts',(19.0012154099791,12.9764729959205,0.));
#251638=CARTESIAN_POINT('Ctrl Pts',(19.0012154099791,12.9764729959205,12.));
#251639=CARTESIAN_POINT('Ctrl Pts',(19.0144133673348,12.9820222318716,0.));
#251640=CARTESIAN_POINT('Ctrl Pts',(19.0144133673348,12.9820222318716,12.));
#251641=CARTESIAN_POINT('Ctrl Pts',(19.0277745339908,12.9875912893003,0.));
#251642=CARTESIAN_POINT('Ctrl Pts',(19.0277745339908,12.9875912893003,12.));
#251643=CARTESIAN_POINT('Ctrl Pts',(19.0412975200398,12.9931787316515,0.));
#251644=CARTESIAN_POINT('Ctrl Pts',(19.0412975200398,12.9931787316515,12.));
#251645=CARTESIAN_POINT('Ctrl Pts',(19.0549809634355,12.9987831544502,0.));
#251646=CARTESIAN_POINT('Ctrl Pts',(19.0549809634355,12.9987831544502,12.));
#251647=CARTESIAN_POINT('Ctrl Pts',(19.0688235289437,13.0044031841381,0.));
#251648=CARTESIAN_POINT('Ctrl Pts',(19.0688235289437,13.0044031841381,12.));
#251649=CARTESIAN_POINT('Ctrl Pts',(19.0828239070482,13.0100374768786,0.));
#251650=CARTESIAN_POINT('Ctrl Pts',(19.0828239070482,13.0100374768786,12.));
#251651=CARTESIAN_POINT('Ctrl Pts',(19.0969808131226,13.0156847176094,0.));
#251652=CARTESIAN_POINT('Ctrl Pts',(19.0969808131226,13.0156847176094,12.));
#251653=CARTESIAN_POINT('Ctrl Pts',(19.1112929866308,13.0213436191326,0.));
#251654=CARTESIAN_POINT('Ctrl Pts',(19.1112929866308,13.0213436191326,12.));
#251655=CARTESIAN_POINT('Ctrl Pts',(19.1257591903099,13.0270129211976,0.));
#251656=CARTESIAN_POINT('Ctrl Pts',(19.1257591903099,13.0270129211976,12.));
#251657=CARTESIAN_POINT('Ctrl Pts',(19.1403782093389,13.0326913895841,0.));
#251658=CARTESIAN_POINT('Ctrl Pts',(19.1403782093389,13.0326913895841,12.));
#251659=CARTESIAN_POINT('Ctrl Pts',(19.1551488505233,13.0383778152072,0.));
#251660=CARTESIAN_POINT('Ctrl Pts',(19.1551488505233,13.0383778152072,12.));
#251661=CARTESIAN_POINT('Ctrl Pts',(19.1700699416625,13.0440710133775,0.));
#251662=CARTESIAN_POINT('Ctrl Pts',(19.1700699416625,13.0440710133775,12.));
#251663=CARTESIAN_POINT('Ctrl Pts',(19.1851403308825,13.0497698230442,0.));
#251664=CARTESIAN_POINT('Ctrl Pts',(19.1851403308825,13.0497698230442,12.));
#251665=CARTESIAN_POINT('Ctrl Pts',(19.2003588859771,13.0554731060537,0.));
#251666=CARTESIAN_POINT('Ctrl Pts',(19.2003588859771,13.0554731060537,12.));
#251667=CARTESIAN_POINT('Ctrl Pts',(19.2157244937141,13.0611797463913,0.));
#251668=CARTESIAN_POINT('Ctrl Pts',(19.2157244937141,13.0611797463913,12.));
#251669=CARTESIAN_POINT('Ctrl Pts',(19.2312360592031,13.0668886494791,0.));
#251670=CARTESIAN_POINT('Ctrl Pts',(19.2312360592031,13.0668886494791,12.));
#251671=CARTESIAN_POINT('Ctrl Pts',(19.2468925053988,13.0725987415856,0.));
#251672=CARTESIAN_POINT('Ctrl Pts',(19.2468925053988,13.0725987415856,12.));
#251673=CARTESIAN_POINT('Ctrl Pts',(19.2626927725596,13.0783089692118,0.));
#251674=CARTESIAN_POINT('Ctrl Pts',(19.2626927725596,13.0783089692118,12.));
#251675=CARTESIAN_POINT('Ctrl Pts',(19.2786358177198,13.0840182984949,0.));
#251676=CARTESIAN_POINT('Ctrl Pts',(19.2786358177198,13.0840182984949,12.));
#251677=CARTESIAN_POINT('Ctrl Pts',(19.2947206141246,13.089725714597,0.));
#251678=CARTESIAN_POINT('Ctrl Pts',(19.2947206141246,13.089725714597,12.));
#251679=CARTESIAN_POINT('Ctrl Pts',(19.3109461507358,13.095430221148,0.));
#251680=CARTESIAN_POINT('Ctrl Pts',(19.3109461507358,13.095430221148,12.));
#251681=CARTESIAN_POINT('Ctrl Pts',(19.3273114318268,13.1011308397592,0.));
#251682=CARTESIAN_POINT('Ctrl Pts',(19.3273114318268,13.1011308397592,12.));
#251683=CARTESIAN_POINT('Ctrl Pts',(19.3438154765395,13.1068266095186,0.));
#251684=CARTESIAN_POINT('Ctrl Pts',(19.3438154765395,13.1068266095186,12.));
#251685=CARTESIAN_POINT('Ctrl Pts',(19.3604573184516,13.1125165865021,0.));
#251686=CARTESIAN_POINT('Ctrl Pts',(19.3604573184516,13.1125165865021,12.));
#251687=CARTESIAN_POINT('Ctrl Pts',(19.3772360051093,13.118199843271,0.));
#251688=CARTESIAN_POINT('Ctrl Pts',(19.3772360051093,13.118199843271,12.));
#251689=CARTESIAN_POINT('Ctrl Pts',(19.3941505976267,13.1238754684177,0.));
#251690=CARTESIAN_POINT('Ctrl Pts',(19.3941505976267,13.1238754684177,12.));
#251691=CARTESIAN_POINT('Ctrl Pts',(19.4112001703561,13.1295425661635,0.));
#251692=CARTESIAN_POINT('Ctrl Pts',(19.4112001703561,13.1295425661635,12.));
#251693=CARTESIAN_POINT('Ctrl Pts',(19.4283838105265,13.135200255944,0.));
#251694=CARTESIAN_POINT('Ctrl Pts',(19.4283838105265,13.135200255944,12.));
#251695=CARTESIAN_POINT('Ctrl Pts',(19.4457006178875,13.140847672006,0.));
#251696=CARTESIAN_POINT('Ctrl Pts',(19.4457006178875,13.140847672006,12.));
#251697=CARTESIAN_POINT('Ctrl Pts',(19.463149704325,13.1464839629966,0.));
#251698=CARTESIAN_POINT('Ctrl Pts',(19.463149704325,13.1464839629966,12.));
#251699=CARTESIAN_POINT('Ctrl Pts',(19.4807301935256,13.1521082915846,0.));
#251700=CARTESIAN_POINT('Ctrl Pts',(19.4807301935256,13.1521082915846,12.));
#251701=CARTESIAN_POINT('Ctrl Pts',(19.498441220707,13.1577198341238,0.));
#251702=CARTESIAN_POINT('Ctrl Pts',(19.498441220707,13.1577198341238,12.));
#251703=CARTESIAN_POINT('Ctrl Pts',(19.5162819323207,13.1633177803097,0.));
#251704=CARTESIAN_POINT('Ctrl Pts',(19.5162819323207,13.1633177803097,12.));
#251705=CARTESIAN_POINT('Ctrl Pts',(19.5342514857564,13.1689013328432,0.));
#251706=CARTESIAN_POINT('Ctrl Pts',(19.5342514857564,13.1689013328432,12.));
#251707=CARTESIAN_POINT('Ctrl Pts',(19.5523490490254,13.1744697070918,0.));
#251708=CARTESIAN_POINT('Ctrl Pts',(19.5523490490254,13.1744697070918,12.));
#251709=CARTESIAN_POINT('Ctrl Pts',(19.5705738004682,13.1800221307683,0.));
#251710=CARTESIAN_POINT('Ctrl Pts',(19.5705738004682,13.1800221307683,12.));
#251711=CARTESIAN_POINT('Ctrl Pts',(19.5889249285352,13.185557843648,0.));
#251712=CARTESIAN_POINT('Ctrl Pts',(19.5889249285352,13.185557843648,12.));
#251713=CARTESIAN_POINT('Ctrl Pts',(19.6074016315421,13.1910760972818,0.));
#251714=CARTESIAN_POINT('Ctrl Pts',(19.6074016315421,13.1910760972818,12.));
#251715=CARTESIAN_POINT('Ctrl Pts',(19.6260031174244,13.196576154715,0.));
#251716=CARTESIAN_POINT('Ctrl Pts',(19.6260031174244,13.196576154715,12.));
#251717=CARTESIAN_POINT('Ctrl Pts',(19.6447286034764,13.202057290206,0.));
#251718=CARTESIAN_POINT('Ctrl Pts',(19.6447286034764,13.202057290206,12.));
#251719=CARTESIAN_POINT('Ctrl Pts',(19.6635773160924,13.2075187889522,0.));
#251720=CARTESIAN_POINT('Ctrl Pts',(19.6635773160924,13.2075187889522,12.));
#251721=CARTESIAN_POINT('Ctrl Pts',(19.6825484905812,13.2129599468478,0.));
#251722=CARTESIAN_POINT('Ctrl Pts',(19.6825484905812,13.2129599468478,12.));
#251723=CARTESIAN_POINT('Ctrl Pts',(19.7016413709678,13.2183800702431,0.));
#251724=CARTESIAN_POINT('Ctrl Pts',(19.7016413709678,13.2183800702431,12.));
#251725=CARTESIAN_POINT('Ctrl Pts',(19.7208552097867,13.2237784757065,0.));
#251726=CARTESIAN_POINT('Ctrl Pts',(19.7208552097867,13.2237784757065,12.));
#251727=CARTESIAN_POINT('Ctrl Pts',(19.7401892678701,13.2291544897902,0.));
#251728=CARTESIAN_POINT('Ctrl Pts',(19.7401892678701,13.2291544897902,12.));
#251729=CARTESIAN_POINT('Ctrl Pts',(19.7596428141176,13.2345074487968,0.));
#251730=CARTESIAN_POINT('Ctrl Pts',(19.7596428141176,13.2345074487968,12.));
#251731=CARTESIAN_POINT('Ctrl Pts',(19.7792151253297,13.239836698568,0.));
#251732=CARTESIAN_POINT('Ctrl Pts',(19.7792151253297,13.239836698568,12.));
#251733=CARTESIAN_POINT('Ctrl Pts',(19.7989054860501,13.2451415942809,0.));
#251734=CARTESIAN_POINT('Ctrl Pts',(19.7989054860501,13.2451415942809,12.));
#251735=CARTESIAN_POINT('Ctrl Pts',(19.8187131883919,13.2504215002458,0.));
#251736=CARTESIAN_POINT('Ctrl Pts',(19.8187131883919,13.2504215002458,12.));
#251737=CARTESIAN_POINT('Ctrl Pts',(19.8386375318632,13.2556757897085,0.));
#251738=CARTESIAN_POINT('Ctrl Pts',(19.8386375318632,13.2556757897085,12.));
#251739=CARTESIAN_POINT('Ctrl Pts',(19.8586778231711,13.2609038446525,0.));
#251740=CARTESIAN_POINT('Ctrl Pts',(19.8586778231711,13.2609038446525,12.));
#251741=CARTESIAN_POINT('Ctrl Pts',(19.8788333760571,13.2661050556128,0.));
#251742=CARTESIAN_POINT('Ctrl Pts',(19.8788333760571,13.2661050556128,12.));
#251743=CARTESIAN_POINT('Ctrl Pts',(19.8991035111739,13.2712788215015,0.));
#251744=CARTESIAN_POINT('Ctrl Pts',(19.8991035111739,13.2712788215015,12.));
#251745=CARTESIAN_POINT('Ctrl Pts',(19.9194875559419,13.2764245494354,0.));
#251746=CARTESIAN_POINT('Ctrl Pts',(19.9194875559419,13.2764245494354,12.));
#251747=CARTESIAN_POINT('Ctrl Pts',(19.9399848444019,13.2815416545663,0.));
#251748=CARTESIAN_POINT('Ctrl Pts',(19.9399848444019,13.2815416545663,12.));
#251749=CARTESIAN_POINT('Ctrl Pts',(19.9605947170589,13.2866295599152,0.));
#251750=CARTESIAN_POINT('Ctrl Pts',(19.9605947170589,13.2866295599152,12.));
#251751=CARTESIAN_POINT('Ctrl Pts',(19.9813165207174,13.2916876962098,0.));
#251752=CARTESIAN_POINT('Ctrl Pts',(19.9813165207174,13.2916876962098,12.));
#251753=CARTESIAN_POINT('Ctrl Pts',(20.0021496083742,13.296715501731,0.));
#251754=CARTESIAN_POINT('Ctrl Pts',(20.0021496083742,13.296715501731,12.));
#251755=CARTESIAN_POINT('Ctrl Pts',(20.0230933391039,13.3017124221639,0.));
#251756=CARTESIAN_POINT('Ctrl Pts',(20.0230933391039,13.3017124221639,12.));
#251757=CARTESIAN_POINT('Ctrl Pts',(20.0441470779345,13.3066779104515,0.));
#251758=CARTESIAN_POINT('Ctrl Pts',(20.0441470779345,13.3066779104515,12.));
#251759=CARTESIAN_POINT('Ctrl Pts',(20.0653101957188,13.3116114266514,0.));
#251760=CARTESIAN_POINT('Ctrl Pts',(20.0653101957188,13.3116114266514,12.));
#251761=CARTESIAN_POINT('Ctrl Pts',(20.0865820689883,13.3165124377963,0.));
#251762=CARTESIAN_POINT('Ctrl Pts',(20.0865820689883,13.3165124377963,12.));
#251763=CARTESIAN_POINT('Ctrl Pts',(20.1079620798377,13.3213804177588,0.));
#251764=CARTESIAN_POINT('Ctrl Pts',(20.1079620798377,13.3213804177588,12.));
#251765=CARTESIAN_POINT('Ctrl Pts',(20.1294496158405,13.3262148471228,0.));
#251766=CARTESIAN_POINT('Ctrl Pts',(20.1294496158405,13.3262148471228,12.));
#251767=CARTESIAN_POINT('Ctrl Pts',(20.1510440699477,13.3310152130565,0.));
#251768=CARTESIAN_POINT('Ctrl Pts',(20.1510440699477,13.3310152130565,12.));
#251769=CARTESIAN_POINT('Ctrl Pts',(20.1727448403818,13.3357810091903,0.));
#251770=CARTESIAN_POINT('Ctrl Pts',(20.1727448403818,13.3357810091903,12.));
#251771=CARTESIAN_POINT('Ctrl Pts',(20.1945513305233,13.3405117354969,0.));
#251772=CARTESIAN_POINT('Ctrl Pts',(20.1945513305233,13.3405117354969,12.));
#251773=CARTESIAN_POINT('Ctrl Pts',(20.2164629487855,13.3452068981763,0.));
#251774=CARTESIAN_POINT('Ctrl Pts',(20.2164629487855,13.3452068981763,12.));
#251775=CARTESIAN_POINT('Ctrl Pts',(20.2384791085354,13.3498660095382,0.));
#251776=CARTESIAN_POINT('Ctrl Pts',(20.2384791085354,13.3498660095382,12.));
#251777=CARTESIAN_POINT('Ctrl Pts',(20.2605992280117,13.3544885878886,0.));
#251778=CARTESIAN_POINT('Ctrl Pts',(20.2605992280117,13.3544885878886,12.));
#251779=CARTESIAN_POINT('Ctrl Pts',(20.2828227302337,13.3590741574194,0.));
#251780=CARTESIAN_POINT('Ctrl Pts',(20.2828227302337,13.3590741574194,12.));
#251781=CARTESIAN_POINT('Ctrl Pts',(20.3051490429049,13.3636222481017,0.));
#251782=CARTESIAN_POINT('Ctrl Pts',(20.3051490429049,13.3636222481017,12.));
#251783=CARTESIAN_POINT('Ctrl Pts',(20.3275775983032,13.3681323955828,0.));
#251784=CARTESIAN_POINT('Ctrl Pts',(20.3275775983032,13.3681323955828,12.));
#251785=CARTESIAN_POINT('Ctrl Pts',(20.3501078331818,13.372604141087,0.));
#251786=CARTESIAN_POINT('Ctrl Pts',(20.3501078331818,13.372604141087,12.));
#251787=CARTESIAN_POINT('Ctrl Pts',(20.3727391887187,13.377037031319,0.));
#251788=CARTESIAN_POINT('Ctrl Pts',(20.3727391887187,13.377037031319,12.));
#251789=CARTESIAN_POINT('Ctrl Pts',(20.3954711104504,13.3814306183721,0.));
#251790=CARTESIAN_POINT('Ctrl Pts',(20.3954711104504,13.3814306183721,12.));
#251791=CARTESIAN_POINT('Ctrl Pts',(20.4183030482002,13.3857844596387,0.));
#251792=CARTESIAN_POINT('Ctrl Pts',(20.4183030482002,13.3857844596387,12.));
#251793=CARTESIAN_POINT('Ctrl Pts',(20.4412344560007,13.3900981177254,0.));
#251794=CARTESIAN_POINT('Ctrl Pts',(20.4412344560007,13.3900981177254,12.));
#251795=CARTESIAN_POINT('Ctrl Pts',(20.4642647920038,13.3943711603739,0.));
#251796=CARTESIAN_POINT('Ctrl Pts',(20.4642647920038,13.3943711603739,12.));
#251797=CARTESIAN_POINT('Ctrl Pts',(20.4873935184041,13.3986031603716,0.));
#251798=CARTESIAN_POINT('Ctrl Pts',(20.4873935184041,13.3986031603716,12.));
#251799=CARTESIAN_POINT('Ctrl Pts',(20.5106201013755,13.4027936954529,0.));
#251800=CARTESIAN_POINT('Ctrl Pts',(20.5106201013755,13.4027936954529,12.));
#251801=CARTESIAN_POINT('Ctrl Pts',(20.5339440109957,13.4069423482077,0.));
#251802=CARTESIAN_POINT('Ctrl Pts',(20.5339440109957,13.4069423482077,12.));
#251803=CARTESIAN_POINT('Ctrl Pts',(20.557364721164,13.4110487059912,0.));
#251804=CARTESIAN_POINT('Ctrl Pts',(20.557364721164,13.4110487059912,12.));
#251805=CARTESIAN_POINT('Ctrl Pts',(20.5808817095155,13.4151123608411,0.));
#251806=CARTESIAN_POINT('Ctrl Pts',(20.5808817095155,13.4151123608411,12.));
#251807=CARTESIAN_POINT('Ctrl Pts',(20.6044944573151,13.4191329093932,0.));
#251808=CARTESIAN_POINT('Ctrl Pts',(20.6044944573151,13.4191329093932,12.));
#251809=CARTESIAN_POINT('Ctrl Pts',(20.6282024494234,13.4231099528178,0.));
#251810=CARTESIAN_POINT('Ctrl Pts',(20.6282024494234,13.4231099528178,12.));
#251811=CARTESIAN_POINT('Ctrl Pts',(20.6520051742867,13.4270430967651,0.));
#251812=CARTESIAN_POINT('Ctrl Pts',(20.6520051742867,13.4270430967651,12.));
#251813=CARTESIAN_POINT('Ctrl Pts',(20.6759021239102,13.4309319513119,0.));
#251814=CARTESIAN_POINT('Ctrl Pts',(20.6759021239102,13.4309319513119,12.));
#251815=CARTESIAN_POINT('Ctrl Pts',(20.6998927938288,13.4347761309154,0.));
#251816=CARTESIAN_POINT('Ctrl Pts',(20.6998927938288,13.4347761309154,12.));
#251817=CARTESIAN_POINT('Ctrl Pts',(20.7239766830675,13.4385752543663,0.));
#251818=CARTESIAN_POINT('Ctrl Pts',(20.7239766830675,13.4385752543663,12.));
#251819=CARTESIAN_POINT('Ctrl Pts',(20.7481532941014,13.4423289447561,0.));
#251820=CARTESIAN_POINT('Ctrl Pts',(20.7481532941014,13.4423289447561,12.));
#251821=CARTESIAN_POINT('Ctrl Pts',(20.7724221327609,13.4460368293689,0.));
#251822=CARTESIAN_POINT('Ctrl Pts',(20.7724221327609,13.4460368293689,12.));
#251823=CARTESIAN_POINT('Ctrl Pts',(20.7967827081228,13.4496985395637,0.));
#251824=CARTESIAN_POINT('Ctrl Pts',(20.7967827081228,13.4496985395637,12.));
#251825=CARTESIAN_POINT('Ctrl Pts',(20.821234532398,13.4533137106667,0.));
#251826=CARTESIAN_POINT('Ctrl Pts',(20.821234532398,13.4533137106667,12.));
#251827=CARTESIAN_POINT('Ctrl Pts',(20.8457771208083,13.4568819818631,0.));
#251828=CARTESIAN_POINT('Ctrl Pts',(20.8457771208083,13.4568819818631,12.));
#251829=CARTESIAN_POINT('Ctrl Pts',(20.8704099914641,13.4604029960983,0.));
#251830=CARTESIAN_POINT('Ctrl Pts',(20.8704099914641,13.4604029960983,12.));
#251831=CARTESIAN_POINT('Ctrl Pts',(20.8951326652158,13.4638763999725,0.));
#251832=CARTESIAN_POINT('Ctrl Pts',(20.8951326652158,13.4638763999725,12.));
#251833=CARTESIAN_POINT('Ctrl Pts',(20.9199446657583,13.4673018437717,0.));
#251834=CARTESIAN_POINT('Ctrl Pts',(20.9199446657583,13.4673018437717,12.));
#251835=CARTESIAN_POINT('Ctrl Pts',(20.9448455197557,13.4706789815166,0.));
#251836=CARTESIAN_POINT('Ctrl Pts',(20.9448455197557,13.4706789815166,12.));
#251837=CARTESIAN_POINT('Ctrl Pts',(20.9698347569477,13.4740074710086,0.));
#251838=CARTESIAN_POINT('Ctrl Pts',(20.9698347569477,13.4740074710086,12.));
#251839=CARTESIAN_POINT('Ctrl Pts',(20.9949119102592,13.4772869738879,0.));
#251840=CARTESIAN_POINT('Ctrl Pts',(20.9949119102592,13.4772869738879,12.));
#251841=CARTESIAN_POINT('Ctrl Pts',(21.0200765158884,13.4805171556822,0.));
#251842=CARTESIAN_POINT('Ctrl Pts',(21.0200765158884,13.4805171556822,12.));
#251843=CARTESIAN_POINT('Ctrl Pts',(21.0453281134245,13.4836976858912,0.));
#251844=CARTESIAN_POINT('Ctrl Pts',(21.0453281134245,13.4836976858912,12.));
#251845=CARTESIAN_POINT('Ctrl Pts',(21.0706662455199,13.4868282377191,0.));
#251846=CARTESIAN_POINT('Ctrl Pts',(21.0706662455199,13.4868282377191,12.));
#251847=CARTESIAN_POINT('Ctrl Pts',(21.0960904575046,13.4899084877717,0.));
#251848=CARTESIAN_POINT('Ctrl Pts',(21.0960904575046,13.4899084877717,12.));
#251849=CARTESIAN_POINT('Ctrl Pts',(21.1216002970207,13.4929381157778,0.));
#251850=CARTESIAN_POINT('Ctrl Pts',(21.1216002970207,13.4929381157778,12.));
#251851=CARTESIAN_POINT('Ctrl Pts',(21.1471953136209,13.4959168042934,0.));
#251852=CARTESIAN_POINT('Ctrl Pts',(21.1471953136209,13.4959168042934,12.));
#251853=CARTESIAN_POINT('Ctrl Pts',(21.1728750584175,13.4988442384491,0.));
#251854=CARTESIAN_POINT('Ctrl Pts',(21.1728750584175,13.4988442384491,12.));
#251855=CARTESIAN_POINT('Ctrl Pts',(21.1986390835828,13.5017201056088,0.));
#251856=CARTESIAN_POINT('Ctrl Pts',(21.1986390835828,13.5017201056088,12.));
#251857=CARTESIAN_POINT('Ctrl Pts',(21.2244869429332,13.5045440957404,0.));
#251858=CARTESIAN_POINT('Ctrl Pts',(21.2244869429332,13.5045440957404,12.));
#251859=CARTESIAN_POINT('Ctrl Pts',(21.250418192743,13.5073159019452,0.));
#251860=CARTESIAN_POINT('Ctrl Pts',(21.250418192743,13.5073159019452,12.));
#251861=CARTESIAN_POINT('Ctrl Pts',(21.2764323924442,13.5100352209205,0.));
#251862=CARTESIAN_POINT('Ctrl Pts',(21.2764323924442,13.5100352209205,12.));
#251863=CARTESIAN_POINT('Ctrl Pts',(21.3025291054235,13.5127017534971,0.));
#251864=CARTESIAN_POINT('Ctrl Pts',(21.3025291054235,13.5127017534971,12.));
#251865=CARTESIAN_POINT('Ctrl Pts',(21.3287078996341,13.5153152050555,0.));
#251866=CARTESIAN_POINT('Ctrl Pts',(21.3287078996341,13.5153152050555,12.));
#251867=CARTESIAN_POINT('Ctrl Pts',(21.3549683486222,13.5178752862466,0.));
#251868=CARTESIAN_POINT('Ctrl Pts',(21.3549683486222,13.5178752862466,12.));
#251869=CARTESIAN_POINT('Ctrl Pts',(21.3813100304973,13.5203817122504,0.));
#251870=CARTESIAN_POINT('Ctrl Pts',(21.3813100304973,13.5203817122504,12.));
#251871=CARTESIAN_POINT('Ctrl Pts',(21.4077325259324,13.5228342013516,0.));
#251872=CARTESIAN_POINT('Ctrl Pts',(21.4077325259324,13.5228342013516,12.));
#251873=CARTESIAN_POINT('Ctrl Pts',(21.4342354165259,13.5252324737802,0.));
#251874=CARTESIAN_POINT('Ctrl Pts',(21.4342354165259,13.5252324737802,12.));
#251875=CARTESIAN_POINT('Ctrl Pts',(21.4608182828697,13.5275762503555,0.));
#251876=CARTESIAN_POINT('Ctrl Pts',(21.4608182828697,13.5275762503555,12.));
#251877=CARTESIAN_POINT('Ctrl Pts',(21.4874807030468,13.5298652514355,0.));
#251878=CARTESIAN_POINT('Ctrl Pts',(21.4874807030468,13.5298652514355,12.));
#251879=CARTESIAN_POINT('Ctrl Pts',(21.5142222501666,13.5320991952138,0.));
#251880=CARTESIAN_POINT('Ctrl Pts',(21.5142222501666,13.5320991952138,12.));
#251881=CARTESIAN_POINT('Ctrl Pts',(21.5410424932503,13.5342777983215,0.));
#251882=CARTESIAN_POINT('Ctrl Pts',(21.5410424932503,13.5342777983215,12.));
#251883=CARTESIAN_POINT('Ctrl Pts',(21.5679410019001,13.536400779028,0.));
#251884=CARTESIAN_POINT('Ctrl Pts',(21.5679410019001,13.536400779028,12.));
#251885=CARTESIAN_POINT('Ctrl Pts',(21.5949173499013,13.5384678597195,0.));
#251886=CARTESIAN_POINT('Ctrl Pts',(21.5949173499013,13.5384678597195,12.));
#251887=CARTESIAN_POINT('Ctrl Pts',(21.6219711193946,13.5404787697792,0.));
#251888=CARTESIAN_POINT('Ctrl Pts',(21.6219711193946,13.5404787697792,12.));
#251889=CARTESIAN_POINT('Ctrl Pts',(21.6491019044648,13.5424332480699,0.));
#251890=CARTESIAN_POINT('Ctrl Pts',(21.6491019044648,13.5424332480699,12.));
#251891=CARTESIAN_POINT('Ctrl Pts',(21.6763093157699,13.5443310461526,0.));
#251892=CARTESIAN_POINT('Ctrl Pts',(21.6763093157699,13.5443310461526,12.));
#251893=CARTESIAN_POINT('Ctrl Pts',(21.7035929822955,13.5461719295048,0.));
#251894=CARTESIAN_POINT('Ctrl Pts',(21.7035929822955,13.5461719295048,12.));
#251895=CARTESIAN_POINT('Ctrl Pts',(21.7309525412281,13.5479556704481,0.));
#251896=CARTESIAN_POINT('Ctrl Pts',(21.7309525412281,13.5479556704481,12.));
#251897=CARTESIAN_POINT('Ctrl Pts',(21.7583876294554,13.5496820422211,0.));
#251898=CARTESIAN_POINT('Ctrl Pts',(21.7583876294554,13.5496820422211,12.));
#251899=CARTESIAN_POINT('Ctrl Pts',(21.7858978745865,13.551350812725,0.));
#251900=CARTESIAN_POINT('Ctrl Pts',(21.7858978745865,13.551350812725,12.));
#251901=CARTESIAN_POINT('Ctrl Pts',(21.8134828857967,13.5529617381573,0.));
#251902=CARTESIAN_POINT('Ctrl Pts',(21.8134828857967,13.5529617381573,12.));
#251903=CARTESIAN_POINT('Ctrl Pts',(21.8411422456075,13.5545145573031,0.));
#251904=CARTESIAN_POINT('Ctrl Pts',(21.8411422456075,13.5545145573031,12.));
#251905=CARTESIAN_POINT('Ctrl Pts',(21.8688754989365,13.5560089839385,0.));
#251906=CARTESIAN_POINT('Ctrl Pts',(21.8688754989365,13.5560089839385,12.));
#251907=CARTESIAN_POINT('Ctrl Pts',(21.8966821688824,13.5574447178425,0.));
#251908=CARTESIAN_POINT('Ctrl Pts',(21.8966821688824,13.5574447178425,12.));
#251909=CARTESIAN_POINT('Ctrl Pts',(21.9245617765769,13.5588214586604,0.));
#251910=CARTESIAN_POINT('Ctrl Pts',(21.9245617765769,13.5588214586604,12.));
#251911=CARTESIAN_POINT('Ctrl Pts',(21.9525138592813,13.5601389185257,0.));
#251912=CARTESIAN_POINT('Ctrl Pts',(21.9525138592813,13.5601389185257,12.));
#251913=CARTESIAN_POINT('Ctrl Pts',(21.9805379899168,13.5613968357561,0.));
#251914=CARTESIAN_POINT('Ctrl Pts',(21.9805379899168,13.5613968357561,12.));
#251915=CARTESIAN_POINT('Ctrl Pts',(22.0086337943449,13.5625949868333,0.));
#251916=CARTESIAN_POINT('Ctrl Pts',(22.0086337943449,13.5625949868333,12.));
#251917=CARTESIAN_POINT('Ctrl Pts',(22.0368009736295,13.5637332022473,0.));
#251918=CARTESIAN_POINT('Ctrl Pts',(22.0368009736295,13.5637332022473,12.));
#251919=CARTESIAN_POINT('Ctrl Pts',(22.0650393089609,13.5648113689033,0.));
#251920=CARTESIAN_POINT('Ctrl Pts',(22.0650393089609,13.5648113689033,12.));
#251921=CARTESIAN_POINT('Ctrl Pts',(22.0933486464593,13.5658294169284,0.));
#251922=CARTESIAN_POINT('Ctrl Pts',(22.0933486464593,13.5658294169284,12.));
#251923=CARTESIAN_POINT('Ctrl Pts',(22.1217288871975,13.5667873105359,0.));
#251924=CARTESIAN_POINT('Ctrl Pts',(22.1217288871975,13.5667873105359,12.));
#251925=CARTESIAN_POINT('Ctrl Pts',(22.1444897575194,13.5675054919061,0.));
#251926=CARTESIAN_POINT('Ctrl Pts',(22.1444897575194,13.5675054919061,12.));
#251927=CARTESIAN_POINT('Ctrl Pts',(22.1615922805008,13.5680170531805,0.));
#251928=CARTESIAN_POINT('Ctrl Pts',(22.1615922805008,13.5680170531805,12.));
#251929=CARTESIAN_POINT('Ctrl Pts',(22.1730081264608,13.5683460612942,0.));
#251930=CARTESIAN_POINT('Ctrl Pts',(22.1730081264608,13.5683460612942,12.));
#251931=CARTESIAN_POINT('Ctrl Pts',(22.1787195904339,13.5685075571671,0.));
#251932=CARTESIAN_POINT('Ctrl Pts',(22.1787195904339,13.5685075571671,12.));
#251933=CARTESIAN_POINT('',(22.1787195904339,13.5685075571671,0.));
#251934=CARTESIAN_POINT('Ctrl Pts',(18.5896416359912,12.7689476255363,0.));
#251935=CARTESIAN_POINT('Ctrl Pts',(18.5896460962964,12.7689524524483,0.));
#251936=CARTESIAN_POINT('Ctrl Pts',(18.5896919669165,12.768986426692,0.));
#251937=CARTESIAN_POINT('Ctrl Pts',(18.589871621843,12.769110348199,0.));
#251938=CARTESIAN_POINT('Ctrl Pts',(18.5903328777227,12.7694215127919,0.));
#251939=CARTESIAN_POINT('Ctrl Pts',(18.5912775137806,12.7700520897173,0.));
#251940=CARTESIAN_POINT('Ctrl Pts',(18.5925859134579,12.7709195951156,0.));
#251941=CARTESIAN_POINT('Ctrl Pts',(18.5942490615407,12.7720142287172,0.));
#251942=CARTESIAN_POINT('Ctrl Pts',(18.5962551167772,12.7733231262108,0.));
#251943=CARTESIAN_POINT('Ctrl Pts',(18.598591752595,12.7748328937638,0.));
#251944=CARTESIAN_POINT('Ctrl Pts',(18.6012488486709,12.7765325225081,0.));
#251945=CARTESIAN_POINT('Ctrl Pts',(18.6042190183704,12.7784139605066,0.));
#251946=CARTESIAN_POINT('Ctrl Pts',(18.6074961535723,12.7804705387658,0.));
#251947=CARTESIAN_POINT('Ctrl Pts',(18.6110744826219,12.7826959526925,0.));
#251948=CARTESIAN_POINT('Ctrl Pts',(18.6149475565188,12.7850831657901,0.));
#251949=CARTESIAN_POINT('Ctrl Pts',(18.6191087624752,12.7876249657834,0.));
#251950=CARTESIAN_POINT('Ctrl Pts',(18.6235516265575,12.7903142925234,0.));
#251951=CARTESIAN_POINT('Ctrl Pts',(18.6282702819371,12.7931447451555,0.));
#251952=CARTESIAN_POINT('Ctrl Pts',(18.6332595057006,12.7961106222251,0.));
#251953=CARTESIAN_POINT('Ctrl Pts',(18.63851447924,12.7992066625264,0.));
#251954=CARTESIAN_POINT('Ctrl Pts',(18.6440306327456,12.8024278770153,0.));
#251955=CARTESIAN_POINT('Ctrl Pts',(18.6498034438987,12.805769331162,0.));
#251956=CARTESIAN_POINT('Ctrl Pts',(18.6558284825773,12.8092261933858,0.));
#251957=CARTESIAN_POINT('Ctrl Pts',(18.6621014624746,12.8127937909631,0.));
#251958=CARTESIAN_POINT('Ctrl Pts',(18.6686182952799,12.8164676687362,0.));
#251959=CARTESIAN_POINT('Ctrl Pts',(18.6753751301092,12.8202436318474,0.));
#251960=CARTESIAN_POINT('Ctrl Pts',(18.6823683094139,12.8241176980017,0.));
#251961=CARTESIAN_POINT('Ctrl Pts',(18.6895943376171,12.8280860635231,0.));
#251962=CARTESIAN_POINT('Ctrl Pts',(18.6970498410172,12.8321450599789,0.));
#251963=CARTESIAN_POINT('Ctrl Pts',(18.7047315436294,12.8362911280361,0.));
#251964=CARTESIAN_POINT('Ctrl Pts',(18.7126362754445,12.8405208263431,0.));
#251965=CARTESIAN_POINT('Ctrl Pts',(18.7207609737702,12.8448308329494,0.));
#251966=CARTESIAN_POINT('Ctrl Pts',(18.7291026886554,12.8492179511591,0.));
#251967=CARTESIAN_POINT('Ctrl Pts',(18.7376585820854,12.8536791086316,0.));
#251968=CARTESIAN_POINT('Ctrl Pts',(18.7464259171251,12.8582113455646,0.));
#251969=CARTESIAN_POINT('Ctrl Pts',(18.7554020493887,12.8628118054171,0.));
#251970=CARTESIAN_POINT('Ctrl Pts',(18.7645844169564,12.8674777239653,0.));
#251971=CARTESIAN_POINT('Ctrl Pts',(18.7739705329022,12.872206421181,0.));
#251972=CARTESIAN_POINT('Ctrl Pts',(18.7835579840477,12.8769952998095,0.));
#251973=CARTESIAN_POINT('Ctrl Pts',(18.7933444285868,12.8818418427475,0.));
#251974=CARTESIAN_POINT('Ctrl Pts',(18.8033275941943,12.8867436109546,0.));
#251975=CARTESIAN_POINT('Ctrl Pts',(18.813505275782,12.8916982409935,0.));
#251976=CARTESIAN_POINT('Ctrl Pts',(18.8238753319129,12.8967034410755,0.));
#251977=CARTESIAN_POINT('Ctrl Pts',(18.834435681259,12.9017569871738,0.));
#251978=CARTESIAN_POINT('Ctrl Pts',(18.8451842990984,12.9068567191854,0.));
#251979=CARTESIAN_POINT('Ctrl Pts',(18.8561192136198,12.9120005369063,0.));
#251980=CARTESIAN_POINT('Ctrl Pts',(18.8672385038326,12.9171863977045,0.));
#251981=CARTESIAN_POINT('Ctrl Pts',(18.8785402977527,12.9224123144982,0.));
#251982=CARTESIAN_POINT('Ctrl Pts',(18.8900227704889,12.9276763536373,0.));
#251983=CARTESIAN_POINT('Ctrl Pts',(18.9016841423403,12.9329766328185,0.));
#251984=CARTESIAN_POINT('Ctrl Pts',(18.9135226769465,12.9383113190375,0.));
#251985=CARTESIAN_POINT('Ctrl Pts',(18.9255366795195,12.9436786266105,0.));
#251986=CARTESIAN_POINT('Ctrl Pts',(18.9377244950435,12.9490768151821,0.));
#251987=CARTESIAN_POINT('Ctrl Pts',(18.9500845064715,12.9545041877377,0.));
#251988=CARTESIAN_POINT('Ctrl Pts',(18.9626151329229,12.9599590886319,0.));
#251989=CARTESIAN_POINT('Ctrl Pts',(18.9753148284475,12.9654399021869,0.));
#251990=CARTESIAN_POINT('Ctrl Pts',(18.9881820807585,12.9709450512747,0.));
#251991=CARTESIAN_POINT('Ctrl Pts',(19.0012154099791,12.9764729959205,0.));
#251992=CARTESIAN_POINT('Ctrl Pts',(19.0144133673348,12.9820222318716,0.));
#251993=CARTESIAN_POINT('Ctrl Pts',(19.0277745339908,12.9875912893003,0.));
#251994=CARTESIAN_POINT('Ctrl Pts',(19.0412975200398,12.9931787316515,0.));
#251995=CARTESIAN_POINT('Ctrl Pts',(19.0549809634355,12.9987831544502,0.));
#251996=CARTESIAN_POINT('Ctrl Pts',(19.0688235289437,13.0044031841381,0.));
#251997=CARTESIAN_POINT('Ctrl Pts',(19.0828239070482,13.0100374768786,0.));
#251998=CARTESIAN_POINT('Ctrl Pts',(19.0969808131226,13.0156847176094,0.));
#251999=CARTESIAN_POINT('Ctrl Pts',(19.1112929866308,13.0213436191326,0.));
#252000=CARTESIAN_POINT('Ctrl Pts',(19.1257591903099,13.0270129211976,0.));
#252001=CARTESIAN_POINT('Ctrl Pts',(19.1403782093389,13.0326913895841,0.));
#252002=CARTESIAN_POINT('Ctrl Pts',(19.1551488505233,13.0383778152072,0.));
#252003=CARTESIAN_POINT('Ctrl Pts',(19.1700699416625,13.0440710133775,0.));
#252004=CARTESIAN_POINT('Ctrl Pts',(19.1851403308825,13.0497698230442,0.));
#252005=CARTESIAN_POINT('Ctrl Pts',(19.2003588859771,13.0554731060537,0.));
#252006=CARTESIAN_POINT('Ctrl Pts',(19.2157244937141,13.0611797463913,0.));
#252007=CARTESIAN_POINT('Ctrl Pts',(19.2312360592031,13.0668886494791,0.));
#252008=CARTESIAN_POINT('Ctrl Pts',(19.2468925053988,13.0725987415856,0.));
#252009=CARTESIAN_POINT('Ctrl Pts',(19.2626927725596,13.0783089692118,0.));
#252010=CARTESIAN_POINT('Ctrl Pts',(19.2786358177198,13.0840182984949,0.));
#252011=CARTESIAN_POINT('Ctrl Pts',(19.2947206141246,13.089725714597,0.));
#252012=CARTESIAN_POINT('Ctrl Pts',(19.3109461507358,13.095430221148,0.));
#252013=CARTESIAN_POINT('Ctrl Pts',(19.3273114318268,13.1011308397592,0.));
#252014=CARTESIAN_POINT('Ctrl Pts',(19.3438154765395,13.1068266095186,0.));
#252015=CARTESIAN_POINT('Ctrl Pts',(19.3604573184516,13.1125165865021,0.));
#252016=CARTESIAN_POINT('Ctrl Pts',(19.3772360051093,13.118199843271,0.));
#252017=CARTESIAN_POINT('Ctrl Pts',(19.3941505976267,13.1238754684177,0.));
#252018=CARTESIAN_POINT('Ctrl Pts',(19.4112001703561,13.1295425661635,0.));
#252019=CARTESIAN_POINT('Ctrl Pts',(19.4283838105265,13.135200255944,0.));
#252020=CARTESIAN_POINT('Ctrl Pts',(19.4457006178875,13.140847672006,0.));
#252021=CARTESIAN_POINT('Ctrl Pts',(19.463149704325,13.1464839629966,0.));
#252022=CARTESIAN_POINT('Ctrl Pts',(19.4807301935256,13.1521082915846,0.));
#252023=CARTESIAN_POINT('Ctrl Pts',(19.498441220707,13.1577198341238,0.));
#252024=CARTESIAN_POINT('Ctrl Pts',(19.5162819323207,13.1633177803097,0.));
#252025=CARTESIAN_POINT('Ctrl Pts',(19.5342514857564,13.1689013328432,0.));
#252026=CARTESIAN_POINT('Ctrl Pts',(19.5523490490254,13.1744697070918,0.));
#252027=CARTESIAN_POINT('Ctrl Pts',(19.5705738004682,13.1800221307683,0.));
#252028=CARTESIAN_POINT('Ctrl Pts',(19.5889249285352,13.185557843648,0.));
#252029=CARTESIAN_POINT('Ctrl Pts',(19.6074016315421,13.1910760972818,0.));
#252030=CARTESIAN_POINT('Ctrl Pts',(19.6260031174244,13.196576154715,0.));
#252031=CARTESIAN_POINT('Ctrl Pts',(19.6447286034764,13.202057290206,0.));
#252032=CARTESIAN_POINT('Ctrl Pts',(19.6635773160924,13.2075187889522,0.));
#252033=CARTESIAN_POINT('Ctrl Pts',(19.6825484905812,13.2129599468478,0.));
#252034=CARTESIAN_POINT('Ctrl Pts',(19.7016413709678,13.2183800702431,0.));
#252035=CARTESIAN_POINT('Ctrl Pts',(19.7208552097867,13.2237784757065,0.));
#252036=CARTESIAN_POINT('Ctrl Pts',(19.7401892678701,13.2291544897902,0.));
#252037=CARTESIAN_POINT('Ctrl Pts',(19.7596428141176,13.2345074487968,0.));
#252038=CARTESIAN_POINT('Ctrl Pts',(19.7792151253297,13.239836698568,0.));
#252039=CARTESIAN_POINT('Ctrl Pts',(19.7989054860501,13.2451415942809,0.));
#252040=CARTESIAN_POINT('Ctrl Pts',(19.8187131883919,13.2504215002458,0.));
#252041=CARTESIAN_POINT('Ctrl Pts',(19.8386375318632,13.2556757897085,0.));
#252042=CARTESIAN_POINT('Ctrl Pts',(19.8586778231711,13.2609038446525,0.));
#252043=CARTESIAN_POINT('Ctrl Pts',(19.8788333760571,13.2661050556128,0.));
#252044=CARTESIAN_POINT('Ctrl Pts',(19.8991035111739,13.2712788215015,0.));
#252045=CARTESIAN_POINT('Ctrl Pts',(19.9194875559419,13.2764245494354,0.));
#252046=CARTESIAN_POINT('Ctrl Pts',(19.9399848444019,13.2815416545663,0.));
#252047=CARTESIAN_POINT('Ctrl Pts',(19.9605947170589,13.2866295599152,0.));
#252048=CARTESIAN_POINT('Ctrl Pts',(19.9813165207174,13.2916876962098,0.));
#252049=CARTESIAN_POINT('Ctrl Pts',(20.0021496083742,13.296715501731,0.));
#252050=CARTESIAN_POINT('Ctrl Pts',(20.0230933391039,13.3017124221639,0.));
#252051=CARTESIAN_POINT('Ctrl Pts',(20.0441470779345,13.3066779104515,0.));
#252052=CARTESIAN_POINT('Ctrl Pts',(20.0653101957188,13.3116114266514,0.));
#252053=CARTESIAN_POINT('Ctrl Pts',(20.0865820689883,13.3165124377963,0.));
#252054=CARTESIAN_POINT('Ctrl Pts',(20.1079620798377,13.3213804177588,0.));
#252055=CARTESIAN_POINT('Ctrl Pts',(20.1294496158405,13.3262148471228,0.));
#252056=CARTESIAN_POINT('Ctrl Pts',(20.1510440699477,13.3310152130565,0.));
#252057=CARTESIAN_POINT('Ctrl Pts',(20.1727448403818,13.3357810091903,0.));
#252058=CARTESIAN_POINT('Ctrl Pts',(20.1945513305233,13.3405117354969,0.));
#252059=CARTESIAN_POINT('Ctrl Pts',(20.2164629487855,13.3452068981763,0.));
#252060=CARTESIAN_POINT('Ctrl Pts',(20.2384791085354,13.3498660095382,0.));
#252061=CARTESIAN_POINT('Ctrl Pts',(20.2605992280117,13.3544885878886,0.));
#252062=CARTESIAN_POINT('Ctrl Pts',(20.2828227302337,13.3590741574194,0.));
#252063=CARTESIAN_POINT('Ctrl Pts',(20.3051490429049,13.3636222481017,0.));
#252064=CARTESIAN_POINT('Ctrl Pts',(20.3275775983032,13.3681323955828,0.));
#252065=CARTESIAN_POINT('Ctrl Pts',(20.3501078331818,13.372604141087,0.));
#252066=CARTESIAN_POINT('Ctrl Pts',(20.3727391887187,13.377037031319,0.));
#252067=CARTESIAN_POINT('Ctrl Pts',(20.3954711104504,13.3814306183721,0.));
#252068=CARTESIAN_POINT('Ctrl Pts',(20.4183030482002,13.3857844596387,0.));
#252069=CARTESIAN_POINT('Ctrl Pts',(20.4412344560007,13.3900981177254,0.));
#252070=CARTESIAN_POINT('Ctrl Pts',(20.4642647920038,13.3943711603739,0.));
#252071=CARTESIAN_POINT('Ctrl Pts',(20.4873935184041,13.3986031603716,0.));
#252072=CARTESIAN_POINT('Ctrl Pts',(20.5106201013755,13.4027936954529,0.));
#252073=CARTESIAN_POINT('Ctrl Pts',(20.5339440109957,13.4069423482077,0.));
#252074=CARTESIAN_POINT('Ctrl Pts',(20.557364721164,13.4110487059912,0.));
#252075=CARTESIAN_POINT('Ctrl Pts',(20.5808817095155,13.4151123608411,0.));
#252076=CARTESIAN_POINT('Ctrl Pts',(20.6044944573151,13.4191329093932,0.));
#252077=CARTESIAN_POINT('Ctrl Pts',(20.6282024494234,13.4231099528178,0.));
#252078=CARTESIAN_POINT('Ctrl Pts',(20.6520051742867,13.4270430967651,0.));
#252079=CARTESIAN_POINT('Ctrl Pts',(20.6759021239102,13.4309319513119,0.));
#252080=CARTESIAN_POINT('Ctrl Pts',(20.6998927938288,13.4347761309154,0.));
#252081=CARTESIAN_POINT('Ctrl Pts',(20.7239766830675,13.4385752543663,0.));
#252082=CARTESIAN_POINT('Ctrl Pts',(20.7481532941014,13.4423289447561,0.));
#252083=CARTESIAN_POINT('Ctrl Pts',(20.7724221327609,13.4460368293689,0.));
#252084=CARTESIAN_POINT('Ctrl Pts',(20.7967827081228,13.4496985395637,0.));
#252085=CARTESIAN_POINT('Ctrl Pts',(20.821234532398,13.4533137106667,0.));
#252086=CARTESIAN_POINT('Ctrl Pts',(20.8457771208083,13.4568819818631,0.));
#252087=CARTESIAN_POINT('Ctrl Pts',(20.8704099914641,13.4604029960983,0.));
#252088=CARTESIAN_POINT('Ctrl Pts',(20.8951326652158,13.4638763999725,0.));
#252089=CARTESIAN_POINT('Ctrl Pts',(20.9199446657583,13.4673018437717,0.));
#252090=CARTESIAN_POINT('Ctrl Pts',(20.9448455197557,13.4706789815166,0.));
#252091=CARTESIAN_POINT('Ctrl Pts',(20.9698347569477,13.4740074710086,0.));
#252092=CARTESIAN_POINT('Ctrl Pts',(20.9949119102592,13.4772869738879,0.));
#252093=CARTESIAN_POINT('Ctrl Pts',(21.0200765158884,13.4805171556822,0.));
#252094=CARTESIAN_POINT('Ctrl Pts',(21.0453281134245,13.4836976858912,0.));
#252095=CARTESIAN_POINT('Ctrl Pts',(21.0706662455199,13.4868282377191,0.));
#252096=CARTESIAN_POINT('Ctrl Pts',(21.0960904575046,13.4899084877717,0.));
#252097=CARTESIAN_POINT('Ctrl Pts',(21.1216002970207,13.4929381157778,0.));
#252098=CARTESIAN_POINT('Ctrl Pts',(21.1471953136209,13.4959168042934,0.));
#252099=CARTESIAN_POINT('Ctrl Pts',(21.1728750584175,13.4988442384491,0.));
#252100=CARTESIAN_POINT('Ctrl Pts',(21.1986390835828,13.5017201056088,0.));
#252101=CARTESIAN_POINT('Ctrl Pts',(21.2244869429332,13.5045440957404,0.));
#252102=CARTESIAN_POINT('Ctrl Pts',(21.250418192743,13.5073159019452,0.));
#252103=CARTESIAN_POINT('Ctrl Pts',(21.2764323924442,13.5100352209205,0.));
#252104=CARTESIAN_POINT('Ctrl Pts',(21.3025291054235,13.5127017534971,0.));
#252105=CARTESIAN_POINT('Ctrl Pts',(21.3287078996341,13.5153152050555,0.));
#252106=CARTESIAN_POINT('Ctrl Pts',(21.3549683486222,13.5178752862466,0.));
#252107=CARTESIAN_POINT('Ctrl Pts',(21.3813100304973,13.5203817122504,0.));
#252108=CARTESIAN_POINT('Ctrl Pts',(21.4077325259324,13.5228342013516,0.));
#252109=CARTESIAN_POINT('Ctrl Pts',(21.4342354165259,13.5252324737802,0.));
#252110=CARTESIAN_POINT('Ctrl Pts',(21.4608182828697,13.5275762503555,0.));
#252111=CARTESIAN_POINT('Ctrl Pts',(21.4874807030468,13.5298652514355,0.));
#252112=CARTESIAN_POINT('Ctrl Pts',(21.5142222501666,13.5320991952138,0.));
#252113=CARTESIAN_POINT('Ctrl Pts',(21.5410424932503,13.5342777983215,0.));
#252114=CARTESIAN_POINT('Ctrl Pts',(21.5679410019001,13.536400779028,0.));
#252115=CARTESIAN_POINT('Ctrl Pts',(21.5949173499013,13.5384678597195,0.));
#252116=CARTESIAN_POINT('Ctrl Pts',(21.6219711193946,13.5404787697792,0.));
#252117=CARTESIAN_POINT('Ctrl Pts',(21.6491019044648,13.5424332480699,0.));
#252118=CARTESIAN_POINT('Ctrl Pts',(21.6763093157699,13.5443310461526,0.));
#252119=CARTESIAN_POINT('Ctrl Pts',(21.7035929822955,13.5461719295048,0.));
#252120=CARTESIAN_POINT('Ctrl Pts',(21.7309525412281,13.5479556704481,0.));
#252121=CARTESIAN_POINT('Ctrl Pts',(21.7583876294554,13.5496820422211,0.));
#252122=CARTESIAN_POINT('Ctrl Pts',(21.7858978745865,13.551350812725,0.));
#252123=CARTESIAN_POINT('Ctrl Pts',(21.8134828857967,13.5529617381573,0.));
#252124=CARTESIAN_POINT('Ctrl Pts',(21.8411422456075,13.5545145573031,0.));
#252125=CARTESIAN_POINT('Ctrl Pts',(21.8688754989365,13.5560089839385,0.));
#252126=CARTESIAN_POINT('Ctrl Pts',(21.8966821688824,13.5574447178425,0.));
#252127=CARTESIAN_POINT('Ctrl Pts',(21.9245617765769,13.5588214586604,0.));
#252128=CARTESIAN_POINT('Ctrl Pts',(21.9525138592813,13.5601389185257,0.));
#252129=CARTESIAN_POINT('Ctrl Pts',(21.9805379899168,13.5613968357561,0.));
#252130=CARTESIAN_POINT('Ctrl Pts',(22.0086337943449,13.5625949868333,0.));
#252131=CARTESIAN_POINT('Ctrl Pts',(22.0368009736295,13.5637332022473,0.));
#252132=CARTESIAN_POINT('Ctrl Pts',(22.0650393089609,13.5648113689033,0.));
#252133=CARTESIAN_POINT('Ctrl Pts',(22.0933486464593,13.5658294169284,0.));
#252134=CARTESIAN_POINT('Ctrl Pts',(22.1217288871975,13.5667873105359,0.));
#252135=CARTESIAN_POINT('Ctrl Pts',(22.1444897575194,13.5675054919061,0.));
#252136=CARTESIAN_POINT('Ctrl Pts',(22.1615922805008,13.5680170531805,0.));
#252137=CARTESIAN_POINT('Ctrl Pts',(22.1730081264608,13.5683460612942,0.));
#252138=CARTESIAN_POINT('Ctrl Pts',(22.1787195904339,13.5685075571671,0.));
#252139=CARTESIAN_POINT('',(22.1787195904339,13.5685075571671,12.));
#252140=CARTESIAN_POINT('Ctrl Pts',(22.1787195904339,13.5685075571671,12.));
#252141=CARTESIAN_POINT('Ctrl Pts',(22.1730081264608,13.5683460612942,12.));
#252142=CARTESIAN_POINT('Ctrl Pts',(22.1615922805008,13.5680170531805,12.));
#252143=CARTESIAN_POINT('Ctrl Pts',(22.1444897575194,13.5675054919061,12.));
#252144=CARTESIAN_POINT('Ctrl Pts',(22.1217288871975,13.5667873105359,12.));
#252145=CARTESIAN_POINT('Ctrl Pts',(22.0933486464593,13.5658294169284,12.));
#252146=CARTESIAN_POINT('Ctrl Pts',(22.0650393089609,13.5648113689033,12.));
#252147=CARTESIAN_POINT('Ctrl Pts',(22.0368009736295,13.5637332022473,12.));
#252148=CARTESIAN_POINT('Ctrl Pts',(22.0086337943449,13.5625949868333,12.));
#252149=CARTESIAN_POINT('Ctrl Pts',(21.9805379899168,13.5613968357561,12.));
#252150=CARTESIAN_POINT('Ctrl Pts',(21.9525138592813,13.5601389185257,12.));
#252151=CARTESIAN_POINT('Ctrl Pts',(21.9245617765769,13.5588214586604,12.));
#252152=CARTESIAN_POINT('Ctrl Pts',(21.8966821688824,13.5574447178425,12.));
#252153=CARTESIAN_POINT('Ctrl Pts',(21.8688754989365,13.5560089839385,12.));
#252154=CARTESIAN_POINT('Ctrl Pts',(21.8411422456075,13.5545145573031,12.));
#252155=CARTESIAN_POINT('Ctrl Pts',(21.8134828857967,13.5529617381573,12.));
#252156=CARTESIAN_POINT('Ctrl Pts',(21.7858978745865,13.551350812725,12.));
#252157=CARTESIAN_POINT('Ctrl Pts',(21.7583876294554,13.5496820422211,12.));
#252158=CARTESIAN_POINT('Ctrl Pts',(21.7309525412281,13.5479556704481,12.));
#252159=CARTESIAN_POINT('Ctrl Pts',(21.7035929822955,13.5461719295048,12.));
#252160=CARTESIAN_POINT('Ctrl Pts',(21.6763093157699,13.5443310461526,12.));
#252161=CARTESIAN_POINT('Ctrl Pts',(21.6491019044648,13.5424332480699,12.));
#252162=CARTESIAN_POINT('Ctrl Pts',(21.6219711193946,13.5404787697792,12.));
#252163=CARTESIAN_POINT('Ctrl Pts',(21.5949173499013,13.5384678597195,12.));
#252164=CARTESIAN_POINT('Ctrl Pts',(21.5679410019001,13.536400779028,12.));
#252165=CARTESIAN_POINT('Ctrl Pts',(21.5410424932503,13.5342777983215,12.));
#252166=CARTESIAN_POINT('Ctrl Pts',(21.5142222501666,13.5320991952138,12.));
#252167=CARTESIAN_POINT('Ctrl Pts',(21.4874807030468,13.5298652514355,12.));
#252168=CARTESIAN_POINT('Ctrl Pts',(21.4608182828697,13.5275762503555,12.));
#252169=CARTESIAN_POINT('Ctrl Pts',(21.4342354165259,13.5252324737802,12.));
#252170=CARTESIAN_POINT('Ctrl Pts',(21.4077325259324,13.5228342013516,12.));
#252171=CARTESIAN_POINT('Ctrl Pts',(21.3813100304973,13.5203817122504,12.));
#252172=CARTESIAN_POINT('Ctrl Pts',(21.3549683486222,13.5178752862466,12.));
#252173=CARTESIAN_POINT('Ctrl Pts',(21.3287078996341,13.5153152050555,12.));
#252174=CARTESIAN_POINT('Ctrl Pts',(21.3025291054235,13.5127017534971,12.));
#252175=CARTESIAN_POINT('Ctrl Pts',(21.2764323924442,13.5100352209205,12.));
#252176=CARTESIAN_POINT('Ctrl Pts',(21.250418192743,13.5073159019452,12.));
#252177=CARTESIAN_POINT('Ctrl Pts',(21.2244869429332,13.5045440957404,12.));
#252178=CARTESIAN_POINT('Ctrl Pts',(21.1986390835828,13.5017201056088,12.));
#252179=CARTESIAN_POINT('Ctrl Pts',(21.1728750584175,13.4988442384491,12.));
#252180=CARTESIAN_POINT('Ctrl Pts',(21.1471953136209,13.4959168042934,12.));
#252181=CARTESIAN_POINT('Ctrl Pts',(21.1216002970207,13.4929381157778,12.));
#252182=CARTESIAN_POINT('Ctrl Pts',(21.0960904575046,13.4899084877717,12.));
#252183=CARTESIAN_POINT('Ctrl Pts',(21.0706662455199,13.4868282377191,12.));
#252184=CARTESIAN_POINT('Ctrl Pts',(21.0453281134245,13.4836976858912,12.));
#252185=CARTESIAN_POINT('Ctrl Pts',(21.0200765158884,13.4805171556822,12.));
#252186=CARTESIAN_POINT('Ctrl Pts',(20.9949119102592,13.4772869738879,12.));
#252187=CARTESIAN_POINT('Ctrl Pts',(20.9698347569477,13.4740074710086,12.));
#252188=CARTESIAN_POINT('Ctrl Pts',(20.9448455197557,13.4706789815166,12.));
#252189=CARTESIAN_POINT('Ctrl Pts',(20.9199446657583,13.4673018437717,12.));
#252190=CARTESIAN_POINT('Ctrl Pts',(20.8951326652158,13.4638763999725,12.));
#252191=CARTESIAN_POINT('Ctrl Pts',(20.8704099914641,13.4604029960983,12.));
#252192=CARTESIAN_POINT('Ctrl Pts',(20.8457771208083,13.4568819818631,12.));
#252193=CARTESIAN_POINT('Ctrl Pts',(20.821234532398,13.4533137106667,12.));
#252194=CARTESIAN_POINT('Ctrl Pts',(20.7967827081228,13.4496985395637,12.));
#252195=CARTESIAN_POINT('Ctrl Pts',(20.7724221327609,13.4460368293689,12.));
#252196=CARTESIAN_POINT('Ctrl Pts',(20.7481532941014,13.4423289447561,12.));
#252197=CARTESIAN_POINT('Ctrl Pts',(20.7239766830675,13.4385752543663,12.));
#252198=CARTESIAN_POINT('Ctrl Pts',(20.6998927938288,13.4347761309154,12.));
#252199=CARTESIAN_POINT('Ctrl Pts',(20.6759021239102,13.4309319513119,12.));
#252200=CARTESIAN_POINT('Ctrl Pts',(20.6520051742867,13.4270430967651,12.));
#252201=CARTESIAN_POINT('Ctrl Pts',(20.6282024494234,13.4231099528178,12.));
#252202=CARTESIAN_POINT('Ctrl Pts',(20.6044944573151,13.4191329093932,12.));
#252203=CARTESIAN_POINT('Ctrl Pts',(20.5808817095155,13.4151123608411,12.));
#252204=CARTESIAN_POINT('Ctrl Pts',(20.557364721164,13.4110487059912,12.));
#252205=CARTESIAN_POINT('Ctrl Pts',(20.5339440109957,13.4069423482077,12.));
#252206=CARTESIAN_POINT('Ctrl Pts',(20.5106201013755,13.4027936954529,12.));
#252207=CARTESIAN_POINT('Ctrl Pts',(20.4873935184041,13.3986031603716,12.));
#252208=CARTESIAN_POINT('Ctrl Pts',(20.4642647920038,13.3943711603739,12.));
#252209=CARTESIAN_POINT('Ctrl Pts',(20.4412344560007,13.3900981177254,12.));
#252210=CARTESIAN_POINT('Ctrl Pts',(20.4183030482002,13.3857844596387,12.));
#252211=CARTESIAN_POINT('Ctrl Pts',(20.3954711104504,13.3814306183721,12.));
#252212=CARTESIAN_POINT('Ctrl Pts',(20.3727391887187,13.377037031319,12.));
#252213=CARTESIAN_POINT('Ctrl Pts',(20.3501078331818,13.372604141087,12.));
#252214=CARTESIAN_POINT('Ctrl Pts',(20.3275775983032,13.3681323955828,12.));
#252215=CARTESIAN_POINT('Ctrl Pts',(20.3051490429049,13.3636222481017,12.));
#252216=CARTESIAN_POINT('Ctrl Pts',(20.2828227302337,13.3590741574194,12.));
#252217=CARTESIAN_POINT('Ctrl Pts',(20.2605992280117,13.3544885878886,12.));
#252218=CARTESIAN_POINT('Ctrl Pts',(20.2384791085354,13.3498660095382,12.));
#252219=CARTESIAN_POINT('Ctrl Pts',(20.2164629487855,13.3452068981763,12.));
#252220=CARTESIAN_POINT('Ctrl Pts',(20.1945513305233,13.3405117354969,12.));
#252221=CARTESIAN_POINT('Ctrl Pts',(20.1727448403818,13.3357810091903,12.));
#252222=CARTESIAN_POINT('Ctrl Pts',(20.1510440699477,13.3310152130565,12.));
#252223=CARTESIAN_POINT('Ctrl Pts',(20.1294496158405,13.3262148471228,12.));
#252224=CARTESIAN_POINT('Ctrl Pts',(20.1079620798377,13.3213804177588,12.));
#252225=CARTESIAN_POINT('Ctrl Pts',(20.0865820689883,13.3165124377963,12.));
#252226=CARTESIAN_POINT('Ctrl Pts',(20.0653101957188,13.3116114266514,12.));
#252227=CARTESIAN_POINT('Ctrl Pts',(20.0441470779345,13.3066779104515,12.));
#252228=CARTESIAN_POINT('Ctrl Pts',(20.0230933391039,13.3017124221639,12.));
#252229=CARTESIAN_POINT('Ctrl Pts',(20.0021496083742,13.296715501731,12.));
#252230=CARTESIAN_POINT('Ctrl Pts',(19.9813165207174,13.2916876962098,12.));
#252231=CARTESIAN_POINT('Ctrl Pts',(19.9605947170589,13.2866295599152,12.));
#252232=CARTESIAN_POINT('Ctrl Pts',(19.9399848444019,13.2815416545663,12.));
#252233=CARTESIAN_POINT('Ctrl Pts',(19.9194875559419,13.2764245494354,12.));
#252234=CARTESIAN_POINT('Ctrl Pts',(19.8991035111739,13.2712788215015,12.));
#252235=CARTESIAN_POINT('Ctrl Pts',(19.8788333760571,13.2661050556128,12.));
#252236=CARTESIAN_POINT('Ctrl Pts',(19.8586778231711,13.2609038446525,12.));
#252237=CARTESIAN_POINT('Ctrl Pts',(19.8386375318632,13.2556757897085,12.));
#252238=CARTESIAN_POINT('Ctrl Pts',(19.8187131883919,13.2504215002458,12.));
#252239=CARTESIAN_POINT('Ctrl Pts',(19.7989054860501,13.2451415942809,12.));
#252240=CARTESIAN_POINT('Ctrl Pts',(19.7792151253297,13.239836698568,12.));
#252241=CARTESIAN_POINT('Ctrl Pts',(19.7596428141176,13.2345074487968,12.));
#252242=CARTESIAN_POINT('Ctrl Pts',(19.7401892678701,13.2291544897902,12.));
#252243=CARTESIAN_POINT('Ctrl Pts',(19.7208552097867,13.2237784757065,12.));
#252244=CARTESIAN_POINT('Ctrl Pts',(19.7016413709678,13.2183800702431,12.));
#252245=CARTESIAN_POINT('Ctrl Pts',(19.6825484905812,13.2129599468478,12.));
#252246=CARTESIAN_POINT('Ctrl Pts',(19.6635773160924,13.2075187889522,12.));
#252247=CARTESIAN_POINT('Ctrl Pts',(19.6447286034764,13.202057290206,12.));
#252248=CARTESIAN_POINT('Ctrl Pts',(19.6260031174244,13.196576154715,12.));
#252249=CARTESIAN_POINT('Ctrl Pts',(19.6074016315421,13.1910760972818,12.));
#252250=CARTESIAN_POINT('Ctrl Pts',(19.5889249285352,13.185557843648,12.));
#252251=CARTESIAN_POINT('Ctrl Pts',(19.5705738004682,13.1800221307683,12.));
#252252=CARTESIAN_POINT('Ctrl Pts',(19.5523490490254,13.1744697070918,12.));
#252253=CARTESIAN_POINT('Ctrl Pts',(19.5342514857564,13.1689013328432,12.));
#252254=CARTESIAN_POINT('Ctrl Pts',(19.5162819323207,13.1633177803097,12.));
#252255=CARTESIAN_POINT('Ctrl Pts',(19.498441220707,13.1577198341238,12.));
#252256=CARTESIAN_POINT('Ctrl Pts',(19.4807301935256,13.1521082915846,12.));
#252257=CARTESIAN_POINT('Ctrl Pts',(19.463149704325,13.1464839629966,12.));
#252258=CARTESIAN_POINT('Ctrl Pts',(19.4457006178875,13.140847672006,12.));
#252259=CARTESIAN_POINT('Ctrl Pts',(19.4283838105265,13.135200255944,12.));
#252260=CARTESIAN_POINT('Ctrl Pts',(19.4112001703561,13.1295425661635,12.));
#252261=CARTESIAN_POINT('Ctrl Pts',(19.3941505976267,13.1238754684177,12.));
#252262=CARTESIAN_POINT('Ctrl Pts',(19.3772360051093,13.118199843271,12.));
#252263=CARTESIAN_POINT('Ctrl Pts',(19.3604573184516,13.1125165865021,12.));
#252264=CARTESIAN_POINT('Ctrl Pts',(19.3438154765395,13.1068266095186,12.));
#252265=CARTESIAN_POINT('Ctrl Pts',(19.3273114318268,13.1011308397592,12.));
#252266=CARTESIAN_POINT('Ctrl Pts',(19.3109461507358,13.095430221148,12.));
#252267=CARTESIAN_POINT('Ctrl Pts',(19.2947206141246,13.089725714597,12.));
#252268=CARTESIAN_POINT('Ctrl Pts',(19.2786358177198,13.0840182984949,12.));
#252269=CARTESIAN_POINT('Ctrl Pts',(19.2626927725596,13.0783089692118,12.));
#252270=CARTESIAN_POINT('Ctrl Pts',(19.2468925053988,13.0725987415856,12.));
#252271=CARTESIAN_POINT('Ctrl Pts',(19.2312360592031,13.0668886494791,12.));
#252272=CARTESIAN_POINT('Ctrl Pts',(19.2157244937141,13.0611797463913,12.));
#252273=CARTESIAN_POINT('Ctrl Pts',(19.2003588859771,13.0554731060537,12.));
#252274=CARTESIAN_POINT('Ctrl Pts',(19.1851403308825,13.0497698230442,12.));
#252275=CARTESIAN_POINT('Ctrl Pts',(19.1700699416625,13.0440710133775,12.));
#252276=CARTESIAN_POINT('Ctrl Pts',(19.1551488505233,13.0383778152072,12.));
#252277=CARTESIAN_POINT('Ctrl Pts',(19.1403782093389,13.0326913895841,12.));
#252278=CARTESIAN_POINT('Ctrl Pts',(19.1257591903099,13.0270129211976,12.));
#252279=CARTESIAN_POINT('Ctrl Pts',(19.1112929866308,13.0213436191326,12.));
#252280=CARTESIAN_POINT('Ctrl Pts',(19.0969808131226,13.0156847176094,12.));
#252281=CARTESIAN_POINT('Ctrl Pts',(19.0828239070482,13.0100374768786,12.));
#252282=CARTESIAN_POINT('Ctrl Pts',(19.0688235289437,13.0044031841381,12.));
#252283=CARTESIAN_POINT('Ctrl Pts',(19.0549809634355,12.9987831544502,12.));
#252284=CARTESIAN_POINT('Ctrl Pts',(19.0412975200398,12.9931787316515,12.));
#252285=CARTESIAN_POINT('Ctrl Pts',(19.0277745339908,12.9875912893003,12.));
#252286=CARTESIAN_POINT('Ctrl Pts',(19.0144133673348,12.9820222318716,12.));
#252287=CARTESIAN_POINT('Ctrl Pts',(19.0012154099791,12.9764729959205,12.));
#252288=CARTESIAN_POINT('Ctrl Pts',(18.9881820807585,12.9709450512747,12.));
#252289=CARTESIAN_POINT('Ctrl Pts',(18.9753148284475,12.9654399021869,12.));
#252290=CARTESIAN_POINT('Ctrl Pts',(18.9626151329229,12.9599590886319,12.));
#252291=CARTESIAN_POINT('Ctrl Pts',(18.9500845064715,12.9545041877377,12.));
#252292=CARTESIAN_POINT('Ctrl Pts',(18.9377244950435,12.9490768151821,12.));
#252293=CARTESIAN_POINT('Ctrl Pts',(18.9255366795195,12.9436786266105,12.));
#252294=CARTESIAN_POINT('Ctrl Pts',(18.9135226769465,12.9383113190375,12.));
#252295=CARTESIAN_POINT('Ctrl Pts',(18.9016841423403,12.9329766328185,12.));
#252296=CARTESIAN_POINT('Ctrl Pts',(18.8900227704889,12.9276763536373,12.));
#252297=CARTESIAN_POINT('Ctrl Pts',(18.8785402977527,12.9224123144982,12.));
#252298=CARTESIAN_POINT('Ctrl Pts',(18.8672385038326,12.9171863977045,12.));
#252299=CARTESIAN_POINT('Ctrl Pts',(18.8561192136198,12.9120005369063,12.));
#252300=CARTESIAN_POINT('Ctrl Pts',(18.8451842990984,12.9068567191854,12.));
#252301=CARTESIAN_POINT('Ctrl Pts',(18.834435681259,12.9017569871738,12.));
#252302=CARTESIAN_POINT('Ctrl Pts',(18.8238753319129,12.8967034410755,12.));
#252303=CARTESIAN_POINT('Ctrl Pts',(18.813505275782,12.8916982409935,12.));
#252304=CARTESIAN_POINT('Ctrl Pts',(18.8033275941943,12.8867436109546,12.));
#252305=CARTESIAN_POINT('Ctrl Pts',(18.7933444285868,12.8818418427475,12.));
#252306=CARTESIAN_POINT('Ctrl Pts',(18.7835579840477,12.8769952998095,12.));
#252307=CARTESIAN_POINT('Ctrl Pts',(18.7739705329022,12.872206421181,12.));
#252308=CARTESIAN_POINT('Ctrl Pts',(18.7645844169564,12.8674777239653,12.));
#252309=CARTESIAN_POINT('Ctrl Pts',(18.7554020493887,12.8628118054171,12.));
#252310=CARTESIAN_POINT('Ctrl Pts',(18.7464259171251,12.8582113455646,12.));
#252311=CARTESIAN_POINT('Ctrl Pts',(18.7376585820854,12.8536791086316,12.));
#252312=CARTESIAN_POINT('Ctrl Pts',(18.7291026886554,12.8492179511591,12.));
#252313=CARTESIAN_POINT('Ctrl Pts',(18.7207609737702,12.8448308329494,12.));
#252314=CARTESIAN_POINT('Ctrl Pts',(18.7126362754445,12.8405208263431,12.));
#252315=CARTESIAN_POINT('Ctrl Pts',(18.7047315436294,12.8362911280361,12.));
#252316=CARTESIAN_POINT('Ctrl Pts',(18.6970498410172,12.8321450599789,12.));
#252317=CARTESIAN_POINT('Ctrl Pts',(18.6895943376171,12.8280860635231,12.));
#252318=CARTESIAN_POINT('Ctrl Pts',(18.6823683094139,12.8241176980017,12.));
#252319=CARTESIAN_POINT('Ctrl Pts',(18.6753751301092,12.8202436318474,12.));
#252320=CARTESIAN_POINT('Ctrl Pts',(18.6686182952799,12.8164676687362,12.));
#252321=CARTESIAN_POINT('Ctrl Pts',(18.6621014624746,12.8127937909631,12.));
#252322=CARTESIAN_POINT('Ctrl Pts',(18.6558284825773,12.8092261933858,12.));
#252323=CARTESIAN_POINT('Ctrl Pts',(18.6498034438987,12.805769331162,12.));
#252324=CARTESIAN_POINT('Ctrl Pts',(18.6440306327456,12.8024278770153,12.));
#252325=CARTESIAN_POINT('Ctrl Pts',(18.63851447924,12.7992066625264,12.));
#252326=CARTESIAN_POINT('Ctrl Pts',(18.6332595057006,12.7961106222251,12.));
#252327=CARTESIAN_POINT('Ctrl Pts',(18.6282702819371,12.7931447451555,12.));
#252328=CARTESIAN_POINT('Ctrl Pts',(18.6235516265575,12.7903142925234,12.));
#252329=CARTESIAN_POINT('Ctrl Pts',(18.6191087624752,12.7876249657834,12.));
#252330=CARTESIAN_POINT('Ctrl Pts',(18.6149475565188,12.7850831657901,12.));
#252331=CARTESIAN_POINT('Ctrl Pts',(18.6110744826219,12.7826959526925,12.));
#252332=CARTESIAN_POINT('Ctrl Pts',(18.6074961535723,12.7804705387658,12.));
#252333=CARTESIAN_POINT('Ctrl Pts',(18.6042190183704,12.7784139605066,12.));
#252334=CARTESIAN_POINT('Ctrl Pts',(18.6012488486709,12.7765325225081,12.));
#252335=CARTESIAN_POINT('Ctrl Pts',(18.598591752595,12.7748328937638,12.));
#252336=CARTESIAN_POINT('Ctrl Pts',(18.5962551167772,12.7733231262108,12.));
#252337=CARTESIAN_POINT('Ctrl Pts',(18.5942490615407,12.7720142287172,12.));
#252338=CARTESIAN_POINT('Ctrl Pts',(18.5925859134579,12.7709195951156,12.));
#252339=CARTESIAN_POINT('Ctrl Pts',(18.5912775137806,12.7700520897173,12.));
#252340=CARTESIAN_POINT('Ctrl Pts',(18.5903328777227,12.7694215127919,12.));
#252341=CARTESIAN_POINT('Ctrl Pts',(18.589871621843,12.769110348199,12.));
#252342=CARTESIAN_POINT('Ctrl Pts',(18.5896919669165,12.768986426692,12.));
#252343=CARTESIAN_POINT('Ctrl Pts',(18.5896460962964,12.7689524524483,12.));
#252344=CARTESIAN_POINT('Ctrl Pts',(18.5896416359912,12.7689476255363,12.));
#252345=CARTESIAN_POINT('',(22.1787195904339,13.5685075571671,0.));
#252346=CARTESIAN_POINT('Origin',(20.2687213152502,7.17139709155223,0.));
#252347=CARTESIAN_POINT('',(21.2610617890679,7.52250298901264,12.));
#252348=CARTESIAN_POINT('',(10.1343606576251,3.58569854577611,12.));
#252349=CARTESIAN_POINT('',(21.2610617890679,7.52250298901264,0.));
#252350=CARTESIAN_POINT('',(21.2610617890679,7.52250298901264,0.));
#252351=CARTESIAN_POINT('',(10.1343606576251,3.58569854577611,0.));
#252352=CARTESIAN_POINT('Ctrl Pts',(22.8400320311648,12.4230808101438,0.));
#252353=CARTESIAN_POINT('Ctrl Pts',(22.8400320311648,12.4230808101438,12.));
#252354=CARTESIAN_POINT('Ctrl Pts',(22.8370364396459,12.418215285186,0.));
#252355=CARTESIAN_POINT('Ctrl Pts',(22.8370364396459,12.418215285186,12.));
#252356=CARTESIAN_POINT('Ctrl Pts',(22.8310435872747,12.4084933766347,0.));
#252357=CARTESIAN_POINT('Ctrl Pts',(22.8310435872747,12.4084933766347,12.));
#252358=CARTESIAN_POINT('Ctrl Pts',(22.8220493007173,12.3939379378998,0.));
#252359=CARTESIAN_POINT('Ctrl Pts',(22.8220493007173,12.3939379378998,12.));
#252360=CARTESIAN_POINT('Ctrl Pts',(22.81004690224,12.374585536673,0.));
#252361=CARTESIAN_POINT('Ctrl Pts',(22.81004690224,12.374585536673,12.));
#252362=CARTESIAN_POINT('Ctrl Pts',(22.795027221673,12.3504864740319,0.));
#252363=CARTESIAN_POINT('Ctrl Pts',(22.795027221673,12.3504864740319,12.));
#252364=CARTESIAN_POINT('Ctrl Pts',(22.7799908974768,12.3264788926075,0.));
#252365=CARTESIAN_POINT('Ctrl Pts',(22.7799908974768,12.3264788926075,12.));
#252366=CARTESIAN_POINT('Ctrl Pts',(22.764938010105,12.3025628601792,0.));
#252367=CARTESIAN_POINT('Ctrl Pts',(22.764938010105,12.3025628601792,12.));
#252368=CARTESIAN_POINT('Ctrl Pts',(22.7498686970069,12.2787384750742,0.));
#252369=CARTESIAN_POINT('Ctrl Pts',(22.7498686970069,12.2787384750742,12.));
#252370=CARTESIAN_POINT('Ctrl Pts',(22.7347831655287,12.2550058702395,0.));
#252371=CARTESIAN_POINT('Ctrl Pts',(22.7347831655287,12.2550058702395,12.));
#252372=CARTESIAN_POINT('Ctrl Pts',(22.7196817119374,12.2313652198061,0.));
#252373=CARTESIAN_POINT('Ctrl Pts',(22.7196817119374,12.2313652198061,12.));
#252374=CARTESIAN_POINT('Ctrl Pts',(22.7045647168747,12.2078167360284,0.));
#252375=CARTESIAN_POINT('Ctrl Pts',(22.7045647168747,12.2078167360284,12.));
#252376=CARTESIAN_POINT('Ctrl Pts',(22.6894326205037,12.1843606579262,0.));
#252377=CARTESIAN_POINT('Ctrl Pts',(22.6894326205037,12.1843606579262,12.));
#252378=CARTESIAN_POINT('Ctrl Pts',(22.6742859034944,12.1609972423099,0.));
#252379=CARTESIAN_POINT('Ctrl Pts',(22.6742859034944,12.1609972423099,12.));
#252380=CARTESIAN_POINT('Ctrl Pts',(22.6591250653965,12.1377267537145,0.));
#252381=CARTESIAN_POINT('Ctrl Pts',(22.6591250653965,12.1377267537145,12.));
#252382=CARTESIAN_POINT('Ctrl Pts',(22.6439506046605,12.1145494550383,0.));
#252383=CARTESIAN_POINT('Ctrl Pts',(22.6439506046605,12.1145494550383,12.));
#252384=CARTESIAN_POINT('Ctrl Pts',(22.6287629967056,12.0914655972823,0.));
#252385=CARTESIAN_POINT('Ctrl Pts',(22.6287629967056,12.0914655972823,12.));
#252386=CARTESIAN_POINT('Ctrl Pts',(22.6135626764898,12.0684754113862,0.));
#252387=CARTESIAN_POINT('Ctrl Pts',(22.6135626764898,12.0684754113862,12.));
#252388=CARTESIAN_POINT('Ctrl Pts',(22.5983500505644,12.0455791139128,0.));
#252389=CARTESIAN_POINT('Ctrl Pts',(22.5983500505644,12.0455791139128,12.));
#252390=CARTESIAN_POINT('Ctrl Pts',(22.5831255061282,12.0227769113127,0.));
#252391=CARTESIAN_POINT('Ctrl Pts',(22.5831255061282,12.0227769113127,12.));
#252392=CARTESIAN_POINT('Ctrl Pts',(22.5678894211181,12.0000690046695,0.));
#252393=CARTESIAN_POINT('Ctrl Pts',(22.5678894211181,12.0000690046695,12.));
#252394=CARTESIAN_POINT('Ctrl Pts',(22.5526421741158,11.9774555943496,0.));
#252395=CARTESIAN_POINT('Ctrl Pts',(22.5526421741158,11.9774555943496,12.));
#252396=CARTESIAN_POINT('Ctrl Pts',(22.5373841537307,11.9549368843997,0.));
#252397=CARTESIAN_POINT('Ctrl Pts',(22.5373841537307,11.9549368843997,12.));
#252398=CARTESIAN_POINT('Ctrl Pts',(22.5221157697883,11.9325130877803,0.));
#252399=CARTESIAN_POINT('Ctrl Pts',(22.5221157697883,11.9325130877803,12.));
#252400=CARTESIAN_POINT('Ctrl Pts',(22.5068374513973,11.9101844254557,0.));
#252401=CARTESIAN_POINT('Ctrl Pts',(22.5068374513973,11.9101844254557,12.));
#252402=CARTESIAN_POINT('Ctrl Pts',(22.4915496418485,11.8879511239943,0.));
#252403=CARTESIAN_POINT('Ctrl Pts',(22.4915496418485,11.8879511239943,12.));
#252404=CARTESIAN_POINT('Ctrl Pts',(22.4762527946702,11.8658134137019,0.));
#252405=CARTESIAN_POINT('Ctrl Pts',(22.4762527946702,11.8658134137019,12.));
#252406=CARTESIAN_POINT('Ctrl Pts',(22.4609473690471,11.8437715264487,0.));
#252407=CARTESIAN_POINT('Ctrl Pts',(22.4609473690471,11.8437715264487,12.));
#252408=CARTESIAN_POINT('Ctrl Pts',(22.4456338258735,11.8218256937889,0.));
#252409=CARTESIAN_POINT('Ctrl Pts',(22.4456338258735,11.8218256937889,12.));
#252410=CARTESIAN_POINT('Ctrl Pts',(22.430312622646,11.7999761445173,0.));
#252411=CARTESIAN_POINT('Ctrl Pts',(22.430312622646,11.7999761445173,12.));
#252412=CARTESIAN_POINT('Ctrl Pts',(22.4149842125008,11.7782231042039,0.));
#252413=CARTESIAN_POINT('Ctrl Pts',(22.4149842125008,11.7782231042039,12.));
#252414=CARTESIAN_POINT('Ctrl Pts',(22.3996490469191,11.7565667964764,0.));
#252415=CARTESIAN_POINT('Ctrl Pts',(22.3996490469191,11.7565667964764,12.));
#252416=CARTESIAN_POINT('Ctrl Pts',(22.3843075773899,11.7350074437961,0.));
#252417=CARTESIAN_POINT('Ctrl Pts',(22.3843075773899,11.7350074437961,12.));
#252418=CARTESIAN_POINT('Ctrl Pts',(22.3689602575491,11.7135452684532,0.));
#252419=CARTESIAN_POINT('Ctrl Pts',(22.3689602575491,11.7135452684532,12.));
#252420=CARTESIAN_POINT('Ctrl Pts',(22.3536075450029,11.6921804934056,0.));
#252421=CARTESIAN_POINT('Ctrl Pts',(22.3536075450029,11.6921804934056,12.));
#252422=CARTESIAN_POINT('Ctrl Pts',(22.3382499035619,11.6709133432985,0.));
#252423=CARTESIAN_POINT('Ctrl Pts',(22.3382499035619,11.6709133432985,12.));
#252424=CARTESIAN_POINT('Ctrl Pts',(22.3228878043976,11.6497440449857,0.));
#252425=CARTESIAN_POINT('Ctrl Pts',(22.3228878043976,11.6497440449857,12.));
#252426=CARTESIAN_POINT('Ctrl Pts',(22.3075217249049,11.6286728270009,0.));
#252427=CARTESIAN_POINT('Ctrl Pts',(22.3075217249049,11.6286728270009,12.));
#252428=CARTESIAN_POINT('Ctrl Pts',(22.2921521480356,11.6076999192357,0.));
#252429=CARTESIAN_POINT('Ctrl Pts',(22.2921521480356,11.6076999192357,12.));
#252430=CARTESIAN_POINT('Ctrl Pts',(22.2767795614348,11.5868255525188,0.));
#252431=CARTESIAN_POINT('Ctrl Pts',(22.2767795614348,11.5868255525188,12.));
#252432=CARTESIAN_POINT('Ctrl Pts',(22.2614044566898,11.5660499582403,0.));
#252433=CARTESIAN_POINT('Ctrl Pts',(22.2614044566898,11.5660499582403,12.));
#252434=CARTESIAN_POINT('Ctrl Pts',(22.2460273284654,11.5453733679121,0.));
#252435=CARTESIAN_POINT('Ctrl Pts',(22.2460273284654,11.5453733679121,12.));
#252436=CARTESIAN_POINT('Ctrl Pts',(22.2306486738901,11.5247960128477,0.));
#252437=CARTESIAN_POINT('Ctrl Pts',(22.2306486738901,11.5247960128477,12.));
#252438=CARTESIAN_POINT('Ctrl Pts',(22.2152689931022,11.5043181244242,0.));
#252439=CARTESIAN_POINT('Ctrl Pts',(22.2152689931022,11.5043181244242,12.));
#252440=CARTESIAN_POINT('Ctrl Pts',(22.1998887896436,11.483939934259,0.));
#252441=CARTESIAN_POINT('Ctrl Pts',(22.1998887896436,11.483939934259,12.));
#252442=CARTESIAN_POINT('Ctrl Pts',(22.184508570917,11.463661674411,0.));
#252443=CARTESIAN_POINT('Ctrl Pts',(22.184508570917,11.463661674411,12.));
#252444=CARTESIAN_POINT('Ctrl Pts',(22.1691288486096,11.443483577557,0.));
#252445=CARTESIAN_POINT('Ctrl Pts',(22.1691288486096,11.443483577557,12.));
#252446=CARTESIAN_POINT('Ctrl Pts',(22.1537501391487,11.4234058771742,0.));
#252447=CARTESIAN_POINT('Ctrl Pts',(22.1537501391487,11.4234058771742,12.));
#252448=CARTESIAN_POINT('Ctrl Pts',(22.1383729640964,11.4034288076908,0.));
#252449=CARTESIAN_POINT('Ctrl Pts',(22.1383729640964,11.4034288076908,12.));
#252450=CARTESIAN_POINT('Ctrl Pts',(22.1229978500186,11.3835526044256,0.));
#252451=CARTESIAN_POINT('Ctrl Pts',(22.1229978500186,11.3835526044256,12.));
#252452=CARTESIAN_POINT('Ctrl Pts',(22.1076253283979,11.3637775035367,0.));
#252453=CARTESIAN_POINT('Ctrl Pts',(22.1076253283979,11.3637775035367,12.));
#252454=CARTESIAN_POINT('Ctrl Pts',(22.0922559355294,11.3441037419553,0.));
#252455=CARTESIAN_POINT('Ctrl Pts',(22.0922559355294,11.3441037419553,12.));
#252456=CARTESIAN_POINT('Ctrl Pts',(22.0768902124267,11.3245315573168,0.));
#252457=CARTESIAN_POINT('Ctrl Pts',(22.0768902124267,11.3245315573168,12.));
#252458=CARTESIAN_POINT('Ctrl Pts',(22.0615287047179,11.3050611878771,0.));
#252459=CARTESIAN_POINT('Ctrl Pts',(22.0615287047179,11.3050611878771,12.));
#252460=CARTESIAN_POINT('Ctrl Pts',(22.046171962566,11.2856928724374,0.));
#252461=CARTESIAN_POINT('Ctrl Pts',(22.046171962566,11.2856928724374,12.));
#252462=CARTESIAN_POINT('Ctrl Pts',(22.030820540835,11.2664268504206,0.));
#252463=CARTESIAN_POINT('Ctrl Pts',(22.030820540835,11.2664268504206,12.));
#252464=CARTESIAN_POINT('Ctrl Pts',(22.0154749992363,11.2472633619275,0.));
#252465=CARTESIAN_POINT('Ctrl Pts',(22.0154749992363,11.2472633619275,12.));
#252466=CARTESIAN_POINT('Ctrl Pts',(22.0001359024839,11.2282026477896,0.));
#252467=CARTESIAN_POINT('Ctrl Pts',(22.0001359024839,11.2282026477896,12.));
#252468=CARTESIAN_POINT('Ctrl Pts',(21.9848038204439,11.2092449496125,0.));
#252469=CARTESIAN_POINT('Ctrl Pts',(21.9848038204439,11.2092449496125,12.));
#252470=CARTESIAN_POINT('Ctrl Pts',(21.9694793282914,11.190390509811,0.));
#252471=CARTESIAN_POINT('Ctrl Pts',(21.9694793282914,11.190390509811,12.));
#252472=CARTESIAN_POINT('Ctrl Pts',(21.9541630066506,11.1716395716376,0.));
#252473=CARTESIAN_POINT('Ctrl Pts',(21.9541630066506,11.1716395716376,12.));
#252474=CARTESIAN_POINT('Ctrl Pts',(21.9388554416439,11.1529923792003,0.));
#252475=CARTESIAN_POINT('Ctrl Pts',(21.9388554416439,11.1529923792003,12.));
#252476=CARTESIAN_POINT('Ctrl Pts',(21.923557224952,11.1344491774741,0.));
#252477=CARTESIAN_POINT('Ctrl Pts',(21.923557224952,11.1344491774741,12.));
#252478=CARTESIAN_POINT('Ctrl Pts',(21.9082689538688,11.1160102123024,0.));
#252479=CARTESIAN_POINT('Ctrl Pts',(21.9082689538688,11.1160102123024,12.));
#252480=CARTESIAN_POINT('Ctrl Pts',(21.8929912313608,11.0976757303944,0.));
#252481=CARTESIAN_POINT('Ctrl Pts',(21.8929912313608,11.0976757303944,12.));
#252482=CARTESIAN_POINT('Ctrl Pts',(21.877724666119,11.0794459793057,0.));
#252483=CARTESIAN_POINT('Ctrl Pts',(21.877724666119,11.0794459793057,12.));
#252484=CARTESIAN_POINT('Ctrl Pts',(21.8624698726318,11.0613212074363,0.));
#252485=CARTESIAN_POINT('Ctrl Pts',(21.8624698726318,11.0613212074363,12.));
#252486=CARTESIAN_POINT('Ctrl Pts',(21.8472274713103,11.0433016640807,0.));
#252487=CARTESIAN_POINT('Ctrl Pts',(21.8472274713103,11.0433016640807,12.));
#252488=CARTESIAN_POINT('Ctrl Pts',(21.8319980886033,11.0253875994598,0.));
#252489=CARTESIAN_POINT('Ctrl Pts',(21.8319980886033,11.0253875994598,12.));
#252490=CARTESIAN_POINT('Ctrl Pts',(21.8167823571168,11.0075792647477,0.));
#252491=CARTESIAN_POINT('Ctrl Pts',(21.8167823571168,11.0075792647477,12.));
#252492=CARTESIAN_POINT('Ctrl Pts',(21.8015809157301,10.9898769120912,0.));
#252493=CARTESIAN_POINT('Ctrl Pts',(21.8015809157301,10.9898769120912,12.));
#252494=CARTESIAN_POINT('Ctrl Pts',(21.7863944097141,10.9722807946156,0.));
#252495=CARTESIAN_POINT('Ctrl Pts',(21.7863944097141,10.9722807946156,12.));
#252496=CARTESIAN_POINT('Ctrl Pts',(21.7712234908464,10.9547911664455,0.));
#252497=CARTESIAN_POINT('Ctrl Pts',(21.7712234908464,10.9547911664455,12.));
#252498=CARTESIAN_POINT('Ctrl Pts',(21.7560688175247,10.9374082827444,0.));
#252499=CARTESIAN_POINT('Ctrl Pts',(21.7560688175247,10.9374082827444,12.));
#252500=CARTESIAN_POINT('Ctrl Pts',(21.7409310548797,10.9201323997384,0.));
#252501=CARTESIAN_POINT('Ctrl Pts',(21.7409310548797,10.9201323997384,12.));
#252502=CARTESIAN_POINT('Ctrl Pts',(21.7258108748873,10.902963774734,0.));
#252503=CARTESIAN_POINT('Ctrl Pts',(21.7258108748873,10.902963774734,12.));
#252504=CARTESIAN_POINT('Ctrl Pts',(21.7107089564825,10.8859026661293,0.));
#252505=CARTESIAN_POINT('Ctrl Pts',(21.7107089564825,10.8859026661293,12.));
#252506=CARTESIAN_POINT('Ctrl Pts',(21.6956259856672,10.8689493334095,0.));
#252507=CARTESIAN_POINT('Ctrl Pts',(21.6956259856672,10.8689493334095,12.));
#252508=CARTESIAN_POINT('Ctrl Pts',(21.6805626556467,10.8521040371835,0.));
#252509=CARTESIAN_POINT('Ctrl Pts',(21.6805626556467,10.8521040371835,12.));
#252510=CARTESIAN_POINT('Ctrl Pts',(21.6655196669732,10.8353670392272,0.));
#252511=CARTESIAN_POINT('Ctrl Pts',(21.6655196669732,10.8353670392272,12.));
#252512=CARTESIAN_POINT('Ctrl Pts',(21.6504977276866,10.8187386025136,0.));
#252513=CARTESIAN_POINT('Ctrl Pts',(21.6504977276866,10.8187386025136,12.));
#252514=CARTESIAN_POINT('Ctrl Pts',(21.6354975534557,10.8022189912369,0.));
#252515=CARTESIAN_POINT('Ctrl Pts',(21.6354975534557,10.8022189912369,12.));
#252516=CARTESIAN_POINT('Ctrl Pts',(21.6205198677173,10.7858084708261,0.));
#252517=CARTESIAN_POINT('Ctrl Pts',(21.6205198677173,10.7858084708261,12.));
#252518=CARTESIAN_POINT('Ctrl Pts',(21.6055654018176,10.7695073079552,0.));
#252519=CARTESIAN_POINT('Ctrl Pts',(21.6055654018176,10.7695073079552,12.));
#252520=CARTESIAN_POINT('Ctrl Pts',(21.5906348951743,10.7533157705941,0.));
#252521=CARTESIAN_POINT('Ctrl Pts',(21.5906348951743,10.7533157705941,12.));
#252522=CARTESIAN_POINT('Ctrl Pts',(21.5757290954371,10.7372341280467,0.));
#252523=CARTESIAN_POINT('Ctrl Pts',(21.5757290954371,10.7372341280467,12.));
#252524=CARTESIAN_POINT('Ctrl Pts',(21.5608487586468,10.7212626509816,0.));
#252525=CARTESIAN_POINT('Ctrl Pts',(21.5608487586468,10.7212626509816,12.));
#252526=CARTESIAN_POINT('Ctrl Pts',(21.5459946493955,10.7054016114571,0.));
#252527=CARTESIAN_POINT('Ctrl Pts',(21.5459946493955,10.7054016114571,12.));
#252528=CARTESIAN_POINT('Ctrl Pts',(21.5311675409807,10.689651282929,0.));
#252529=CARTESIAN_POINT('Ctrl Pts',(21.5311675409807,10.689651282929,12.));
#252530=CARTESIAN_POINT('Ctrl Pts',(21.51636821558,10.6740119402834,0.));
#252531=CARTESIAN_POINT('Ctrl Pts',(21.51636821558,10.6740119402834,12.));
#252532=CARTESIAN_POINT('Ctrl Pts',(21.5015974644449,10.6584838598939,0.));
#252533=CARTESIAN_POINT('Ctrl Pts',(21.5015974644449,10.6584838598939,12.));
#252534=CARTESIAN_POINT('Ctrl Pts',(21.4868560880889,10.6430673196607,0.));
#252535=CARTESIAN_POINT('Ctrl Pts',(21.4868560880889,10.6430673196607,12.));
#252536=CARTESIAN_POINT('Ctrl Pts',(21.4721448964766,10.6277625990456,0.));
#252537=CARTESIAN_POINT('Ctrl Pts',(21.4721448964766,10.6277625990456,12.));
#252538=CARTESIAN_POINT('Ctrl Pts',(21.4574647092097,10.6125699790961,0.));
#252539=CARTESIAN_POINT('Ctrl Pts',(21.4574647092097,10.6125699790961,12.));
#252540=CARTESIAN_POINT('Ctrl Pts',(21.4428163557144,10.5974897424622,0.));
#252541=CARTESIAN_POINT('Ctrl Pts',(21.4428163557144,10.5974897424622,12.));
#252542=CARTESIAN_POINT('Ctrl Pts',(21.4282006754631,10.5825221734573,0.));
#252543=CARTESIAN_POINT('Ctrl Pts',(21.4282006754631,10.5825221734573,12.));
#252544=CARTESIAN_POINT('Ctrl Pts',(21.4136185181979,10.5676675581108,0.));
#252545=CARTESIAN_POINT('Ctrl Pts',(21.4136185181979,10.5676675581108,12.));
#252546=CARTESIAN_POINT('Ctrl Pts',(21.3990707441497,10.5529261842108,0.));
#252547=CARTESIAN_POINT('Ctrl Pts',(21.3990707441497,10.5529261842108,12.));
#252548=CARTESIAN_POINT('Ctrl Pts',(21.3845582242602,10.5382983413421,0.));
#252549=CARTESIAN_POINT('Ctrl Pts',(21.3845582242602,10.5382983413421,12.));
#252550=CARTESIAN_POINT('Ctrl Pts',(21.3700818403936,10.5237843209057,0.));
#252551=CARTESIAN_POINT('Ctrl Pts',(21.3700818403936,10.5237843209057,12.));
#252552=CARTESIAN_POINT('Ctrl Pts',(21.3556424855814,10.5093844161685,0.));
#252553=CARTESIAN_POINT('Ctrl Pts',(21.3556424855814,10.5093844161685,12.));
#252554=CARTESIAN_POINT('Ctrl Pts',(21.3412410642904,10.4950989223337,0.));
#252555=CARTESIAN_POINT('Ctrl Pts',(21.3412410642904,10.4950989223337,12.));
#252556=CARTESIAN_POINT('Ctrl Pts',(21.3268784926819,10.4809281365931,0.));
#252557=CARTESIAN_POINT('Ctrl Pts',(21.3268784926819,10.4809281365931,12.));
#252558=CARTESIAN_POINT('Ctrl Pts',(21.3125556988731,10.4668723581768,0.));
#252559=CARTESIAN_POINT('Ctrl Pts',(21.3125556988731,10.4668723581768,12.));
#252560=CARTESIAN_POINT('Ctrl Pts',(21.2982736231931,10.4529318883874,0.));
#252561=CARTESIAN_POINT('Ctrl Pts',(21.2982736231931,10.4529318883874,12.));
#252562=CARTESIAN_POINT('Ctrl Pts',(21.2840332184483,10.4391070306391,0.));
#252563=CARTESIAN_POINT('Ctrl Pts',(21.2840332184483,10.4391070306391,12.));
#252564=CARTESIAN_POINT('Ctrl Pts',(21.2698354502403,10.42539809054,0.));
#252565=CARTESIAN_POINT('Ctrl Pts',(21.2698354502403,10.42539809054,12.));
#252566=CARTESIAN_POINT('Ctrl Pts',(21.255681297275,10.4118053759588,0.));
#252567=CARTESIAN_POINT('Ctrl Pts',(21.255681297275,10.4118053759588,12.));
#252568=CARTESIAN_POINT('Ctrl Pts',(21.2415717516714,10.3983291970846,0.));
#252569=CARTESIAN_POINT('Ctrl Pts',(21.2415717516714,10.3983291970846,12.));
#252570=CARTESIAN_POINT('Ctrl Pts',(21.22750781927,10.3849698664786,0.));
#252571=CARTESIAN_POINT('Ctrl Pts',(21.22750781927,10.3849698664786,12.));
#252572=CARTESIAN_POINT('Ctrl Pts',(21.2134905199345,10.371727699113,0.));
#252573=CARTESIAN_POINT('Ctrl Pts',(21.2134905199345,10.371727699113,12.));
#252574=CARTESIAN_POINT('Ctrl Pts',(21.199520887919,10.3586030124587,0.));
#252575=CARTESIAN_POINT('Ctrl Pts',(21.199520887919,10.3586030124587,12.));
#252576=CARTESIAN_POINT('Ctrl Pts',(21.1855999722416,10.3455961265701,0.));
#252577=CARTESIAN_POINT('Ctrl Pts',(21.1855999722416,10.3455961265701,12.));
#252578=CARTESIAN_POINT('Ctrl Pts',(21.1717288370509,10.3327073641572,0.));
#252579=CARTESIAN_POINT('Ctrl Pts',(21.1717288370509,10.3327073641572,12.));
#252580=CARTESIAN_POINT('Ctrl Pts',(21.1579085619965,10.3199370506544,0.));
#252581=CARTESIAN_POINT('Ctrl Pts',(21.1579085619965,10.3199370506544,12.));
#252582=CARTESIAN_POINT('Ctrl Pts',(21.1441402425843,10.3072855142687,0.));
#252583=CARTESIAN_POINT('Ctrl Pts',(21.1441402425843,10.3072855142687,12.));
#252584=CARTESIAN_POINT('Ctrl Pts',(21.1304249906002,10.2947530860721,0.));
#252585=CARTESIAN_POINT('Ctrl Pts',(21.1304249906002,10.2947530860721,12.));
#252586=CARTESIAN_POINT('Ctrl Pts',(21.1167639345631,10.2823401001072,0.));
#252587=CARTESIAN_POINT('Ctrl Pts',(21.1167639345631,10.2823401001072,12.));
#252588=CARTESIAN_POINT('Ctrl Pts',(21.1031582201627,10.2700468934744,0.));
#252589=CARTESIAN_POINT('Ctrl Pts',(21.1031582201627,10.2700468934744,12.));
#252590=CARTESIAN_POINT('Ctrl Pts',(21.0896090107063,10.2578738064181,0.));
#252591=CARTESIAN_POINT('Ctrl Pts',(21.0896090107063,10.2578738064181,12.));
#252592=CARTESIAN_POINT('Ctrl Pts',(21.0761174875444,10.2458211823912,0.));
#252593=CARTESIAN_POINT('Ctrl Pts',(21.0761174875444,10.2458211823912,12.));
#252594=CARTESIAN_POINT('Ctrl Pts',(21.0626848505663,10.2338893681567,0.));
#252595=CARTESIAN_POINT('Ctrl Pts',(21.0626848505663,10.2338893681567,12.));
#252596=CARTESIAN_POINT('Ctrl Pts',(21.0493123187483,10.2220787139155,0.));
#252597=CARTESIAN_POINT('Ctrl Pts',(21.0493123187483,10.2220787139155,12.));
#252598=CARTESIAN_POINT('Ctrl Pts',(21.0360011306815,10.2103895734123,0.));
#252599=CARTESIAN_POINT('Ctrl Pts',(21.0360011306815,10.2103895734123,12.));
#252600=CARTESIAN_POINT('Ctrl Pts',(21.0227525451107,10.1988223040425,0.));
#252601=CARTESIAN_POINT('Ctrl Pts',(21.0227525451107,10.1988223040425,12.));
#252602=CARTESIAN_POINT('Ctrl Pts',(21.0095678414486,10.187377266936,0.));
#252603=CARTESIAN_POINT('Ctrl Pts',(21.0095678414486,10.187377266936,12.));
#252604=CARTESIAN_POINT('Ctrl Pts',(20.9964483203686,10.1760548270767,0.));
#252605=CARTESIAN_POINT('Ctrl Pts',(20.9964483203686,10.1760548270767,12.));
#252606=CARTESIAN_POINT('Ctrl Pts',(20.9833953044736,10.1648553534568,0.));
#252607=CARTESIAN_POINT('Ctrl Pts',(20.9833953044736,10.1648553534568,12.));
#252608=CARTESIAN_POINT('Ctrl Pts',(20.9704101389369,10.1537792192065,0.));
#252609=CARTESIAN_POINT('Ctrl Pts',(20.9704101389369,10.1537792192065,12.));
#252610=CARTESIAN_POINT('Ctrl Pts',(20.9574941921591,10.1428268017256,0.));
#252611=CARTESIAN_POINT('Ctrl Pts',(20.9574941921591,10.1428268017256,12.));
#252612=CARTESIAN_POINT('Ctrl Pts',(20.9446488563933,10.1319984827908,0.));
#252613=CARTESIAN_POINT('Ctrl Pts',(20.9446488563933,10.1319984827908,12.));
#252614=CARTESIAN_POINT('Ctrl Pts',(20.9318755484734,10.1212946487057,0.));
#252615=CARTESIAN_POINT('Ctrl Pts',(20.9318755484734,10.1212946487057,12.));
#252616=CARTESIAN_POINT('Ctrl Pts',(20.919175710627,10.1107156904836,0.));
#252617=CARTESIAN_POINT('Ctrl Pts',(20.919175710627,10.1107156904836,12.));
#252618=CARTESIAN_POINT('Ctrl Pts',(20.9065508112557,10.1002620040076,0.));
#252619=CARTESIAN_POINT('Ctrl Pts',(20.9065508112557,10.1002620040076,12.));
#252620=CARTESIAN_POINT('Ctrl Pts',(20.894002345737,10.0899339901916,0.));
#252621=CARTESIAN_POINT('Ctrl Pts',(20.894002345737,10.0899339901916,12.));
#252622=CARTESIAN_POINT('Ctrl Pts',(20.881531837184,10.0797320551154,0.));
#252623=CARTESIAN_POINT('Ctrl Pts',(20.881531837184,10.0797320551154,12.));
#252624=CARTESIAN_POINT('Ctrl Pts',(20.86914083737,10.0696566102218,0.));
#252625=CARTESIAN_POINT('Ctrl Pts',(20.86914083737,10.0696566102218,12.));
#252626=CARTESIAN_POINT('Ctrl Pts',(20.8568309277316,10.0597080725375,0.));
#252627=CARTESIAN_POINT('Ctrl Pts',(20.8568309277316,10.0597080725375,12.));
#252628=CARTESIAN_POINT('Ctrl Pts',(20.8446037203402,10.0498868648733,0.));
#252629=CARTESIAN_POINT('Ctrl Pts',(20.8446037203402,10.0498868648733,12.));
#252630=CARTESIAN_POINT('Ctrl Pts',(20.8324608588909,10.0401934160234,0.));
#252631=CARTESIAN_POINT('Ctrl Pts',(20.8324608588909,10.0401934160234,12.));
#252632=CARTESIAN_POINT('Ctrl Pts',(20.8204040196602,10.0306281609435,0.));
#252633=CARTESIAN_POINT('Ctrl Pts',(20.8204040196602,10.0306281609435,12.));
#252634=CARTESIAN_POINT('Ctrl Pts',(20.8084349126888,10.0211915410095,0.));
#252635=CARTESIAN_POINT('Ctrl Pts',(20.8084349126888,10.0211915410095,12.));
#252636=CARTESIAN_POINT('Ctrl Pts',(20.7965552829908,10.0118840042786,0.));
#252637=CARTESIAN_POINT('Ctrl Pts',(20.7965552829908,10.0118840042786,12.));
#252638=CARTESIAN_POINT('Ctrl Pts',(20.7847669117568,10.0027060057389,0.));
#252639=CARTESIAN_POINT('Ctrl Pts',(20.7847669117568,10.0027060057389,12.));
#252640=CARTESIAN_POINT('Ctrl Pts',(20.7730716175417,9.9936580075464,0.));
#252641=CARTESIAN_POINT('Ctrl Pts',(20.7730716175417,9.9936580075464,12.));
#252642=CARTESIAN_POINT('Ctrl Pts',(20.761471257499,9.98474047926853,0.));
#252643=CARTESIAN_POINT('Ctrl Pts',(20.761471257499,9.98474047926853,12.));
#252644=CARTESIAN_POINT('Ctrl Pts',(20.7499677289627,9.9759538982347,0.));
#252645=CARTESIAN_POINT('Ctrl Pts',(20.7499677289627,9.9759538982347,12.));
#252646=CARTESIAN_POINT('Ctrl Pts',(20.7385629709795,9.96729874986202,0.));
#252647=CARTESIAN_POINT('Ctrl Pts',(20.7385629709795,9.96729874986202,12.));
#252648=CARTESIAN_POINT('Ctrl Pts',(20.7272589658751,9.95877552798398,0.));
#252649=CARTESIAN_POINT('Ctrl Pts',(20.7272589658751,9.95877552798398,12.));
#252650=CARTESIAN_POINT('Ctrl Pts',(20.7160577407579,9.95038473514949,0.));
#252651=CARTESIAN_POINT('Ctrl Pts',(20.7160577407579,9.95038473514949,12.));
#252652=CARTESIAN_POINT('Ctrl Pts',(20.7049613692234,9.94212688298236,0.));
#252653=CARTESIAN_POINT('Ctrl Pts',(20.7049613692234,9.94212688298236,12.));
#252654=CARTESIAN_POINT('Ctrl Pts',(20.6939719732484,9.9340024925973,0.));
#252655=CARTESIAN_POINT('Ctrl Pts',(20.6939719732484,9.9340024925973,12.));
#252656=CARTESIAN_POINT('Ctrl Pts',(20.6830917250255,9.92601209498749,0.));
#252657=CARTESIAN_POINT('Ctrl Pts',(20.6830917250255,9.92601209498749,12.));
#252658=CARTESIAN_POINT('Ctrl Pts',(20.6723228488263,9.91815623141289,0.));
#252659=CARTESIAN_POINT('Ctrl Pts',(20.6723228488263,9.91815623141289,12.));
#252660=CARTESIAN_POINT('Ctrl Pts',(20.6616676228315,9.91043545377008,0.));
#252661=CARTESIAN_POINT('Ctrl Pts',(20.6616676228315,9.91043545377008,12.));
#252662=CARTESIAN_POINT('Ctrl Pts',(20.6511283817414,9.90285032516693,0.));
#252663=CARTESIAN_POINT('Ctrl Pts',(20.6511283817414,9.90285032516693,12.));
#252664=CARTESIAN_POINT('Ctrl Pts',(20.6407075193976,9.8954014204912,0.));
#252665=CARTESIAN_POINT('Ctrl Pts',(20.6407075193976,9.8954014204912,12.));
#252666=CARTESIAN_POINT('Ctrl Pts',(20.6304074914087,9.88808932697306,0.));
#252667=CARTESIAN_POINT('Ctrl Pts',(20.6304074914087,9.88808932697306,12.));
#252668=CARTESIAN_POINT('Ctrl Pts',(20.6202308177474,9.88091464472676,0.));
#252669=CARTESIAN_POINT('Ctrl Pts',(20.6202308177474,9.88091464472676,12.));
#252670=CARTESIAN_POINT('Ctrl Pts',(20.6101800854494,9.87387798732956,0.));
#252671=CARTESIAN_POINT('Ctrl Pts',(20.6101800854494,9.87387798732956,12.));
#252672=CARTESIAN_POINT('Ctrl Pts',(20.6002579513699,9.86697998242623,0.));
#252673=CARTESIAN_POINT('Ctrl Pts',(20.6002579513699,9.86697998242623,12.));
#252674=CARTESIAN_POINT('Ctrl Pts',(20.5904671449754,9.86022127232748,0.));
#252675=CARTESIAN_POINT('Ctrl Pts',(20.5904671449754,9.86022127232748,12.));
#252676=CARTESIAN_POINT('Ctrl Pts',(20.5808104710015,9.85360251456981,0.));
#252677=CARTESIAN_POINT('Ctrl Pts',(20.5808104710015,9.85360251456981,12.));
#252678=CARTESIAN_POINT('Ctrl Pts',(20.5712908125139,9.84712438256278,0.));
#252679=CARTESIAN_POINT('Ctrl Pts',(20.5712908125139,9.84712438256278,12.));
#252680=CARTESIAN_POINT('Ctrl Pts',(20.5619111362402,9.84078756677565,0.));
#252681=CARTESIAN_POINT('Ctrl Pts',(20.5619111362402,9.84078756677565,12.));
#252682=CARTESIAN_POINT('Ctrl Pts',(20.552674497646,9.83459277585315,0.));
#252683=CARTESIAN_POINT('Ctrl Pts',(20.552674497646,9.83459277585315,12.));
#252684=CARTESIAN_POINT('Ctrl Pts',(20.5435840460721,9.82854073773878,0.));
#252685=CARTESIAN_POINT('Ctrl Pts',(20.5435840460721,9.82854073773878,12.));
#252686=CARTESIAN_POINT('Ctrl Pts',(20.5346430299517,9.82263220080363,0.));
#252687=CARTESIAN_POINT('Ctrl Pts',(20.5346430299517,9.82263220080363,12.));
#252688=CARTESIAN_POINT('Ctrl Pts',(20.5258548000629,9.81686793455943,0.));
#252689=CARTESIAN_POINT('Ctrl Pts',(20.5258548000629,9.81686793455943,12.));
#252690=CARTESIAN_POINT('Ctrl Pts',(20.517222812284,9.81124873025282,0.));
#252691=CARTESIAN_POINT('Ctrl Pts',(20.517222812284,9.81124873025282,12.));
#252692=CARTESIAN_POINT('Ctrl Pts',(20.5087506310505,9.80577540161088,0.));
#252693=CARTESIAN_POINT('Ctrl Pts',(20.5087506310505,9.80577540161088,12.));
#252694=CARTESIAN_POINT('Ctrl Pts',(20.5004419312107,9.80044878520949,0.));
#252695=CARTESIAN_POINT('Ctrl Pts',(20.5004419312107,9.80044878520949,12.));
#252696=CARTESIAN_POINT('Ctrl Pts',(20.4923005087943,9.79526974288331,0.));
#252697=CARTESIAN_POINT('Ctrl Pts',(20.4923005087943,9.79526974288331,12.));
#252698=CARTESIAN_POINT('Ctrl Pts',(20.4843302955329,9.79023916498656,0.));
#252699=CARTESIAN_POINT('Ctrl Pts',(20.4843302955329,9.79023916498656,12.));
#252700=CARTESIAN_POINT('Ctrl Pts',(20.4765353711586,9.78535797314167,0.));
#252701=CARTESIAN_POINT('Ctrl Pts',(20.4765353711586,9.78535797314167,12.));
#252702=CARTESIAN_POINT('Ctrl Pts',(20.4689199790669,9.78062712373321,0.));
#252703=CARTESIAN_POINT('Ctrl Pts',(20.4689199790669,9.78062712373321,12.));
#252704=CARTESIAN_POINT('Ctrl Pts',(20.4614885274975,9.77604760815529,0.));
#252705=CARTESIAN_POINT('Ctrl Pts',(20.4614885274975,9.77604760815529,12.));
#252706=CARTESIAN_POINT('Ctrl Pts',(20.4542455817527,9.7716204510407,0.));
#252707=CARTESIAN_POINT('Ctrl Pts',(20.4542455817527,9.7716204510407,12.));
#252708=CARTESIAN_POINT('Ctrl Pts',(20.447195862298,9.76734670980892,0.));
#252709=CARTESIAN_POINT('Ctrl Pts',(20.447195862298,9.76734670980892,12.));
#252710=CARTESIAN_POINT('Ctrl Pts',(20.44034423294,9.76322747195495,0.));
#252711=CARTESIAN_POINT('Ctrl Pts',(20.44034423294,9.76322747195495,12.));
#252712=CARTESIAN_POINT('Ctrl Pts',(20.4336957355473,9.75926386289923,0.));
#252713=CARTESIAN_POINT('Ctrl Pts',(20.4336957355473,9.75926386289923,12.));
#252714=CARTESIAN_POINT('Ctrl Pts',(20.4272556476629,9.75545705902418,0.));
#252715=CARTESIAN_POINT('Ctrl Pts',(20.4272556476629,9.75545705902418,12.));
#252716=CARTESIAN_POINT('Ctrl Pts',(20.4210295275817,9.7518082978643,0.));
#252717=CARTESIAN_POINT('Ctrl Pts',(20.4210295275817,9.7518082978643,12.));
#252718=CARTESIAN_POINT('Ctrl Pts',(20.4150232777393,9.74831889242174,0.));
#252719=CARTESIAN_POINT('Ctrl Pts',(20.4150232777393,9.74831889242174,12.));
#252720=CARTESIAN_POINT('Ctrl Pts',(20.4092430879861,9.74499021838538,0.));
#252721=CARTESIAN_POINT('Ctrl Pts',(20.4092430879861,9.74499021838538,12.));
#252722=CARTESIAN_POINT('Ctrl Pts',(20.4036953576549,9.74182369656272,0.));
#252723=CARTESIAN_POINT('Ctrl Pts',(20.4036953576549,9.74182369656272,12.));
#252724=CARTESIAN_POINT('Ctrl Pts',(20.3983866213331,9.73882077613201,0.));
#252725=CARTESIAN_POINT('Ctrl Pts',(20.3983866213331,9.73882077613201,12.));
#252726=CARTESIAN_POINT('Ctrl Pts',(20.3933234845647,9.73598292014243,0.));
#252727=CARTESIAN_POINT('Ctrl Pts',(20.3933234845647,9.73598292014243,12.));
#252728=CARTESIAN_POINT('Ctrl Pts',(20.3885129129912,9.73331167102808,0.));
#252729=CARTESIAN_POINT('Ctrl Pts',(20.3885129129912,9.73331167102808,12.));
#252730=CARTESIAN_POINT('Ctrl Pts',(20.3839624556742,9.73080870123727,0.));
#252731=CARTESIAN_POINT('Ctrl Pts',(20.3839624556742,9.73080870123727,12.));
#252732=CARTESIAN_POINT('Ctrl Pts',(20.3796805893304,9.72847589116542,0.));
#252733=CARTESIAN_POINT('Ctrl Pts',(20.3796805893304,9.72847589116542,12.));
#252734=CARTESIAN_POINT('Ctrl Pts',(20.3756766651951,9.72631531732881,0.));
#252735=CARTESIAN_POINT('Ctrl Pts',(20.3756766651951,9.72631531732881,12.));
#252736=CARTESIAN_POINT('Ctrl Pts',(20.371960235676,9.72432910043194,0.));
#252737=CARTESIAN_POINT('Ctrl Pts',(20.371960235676,9.72432910043194,12.));
#252738=CARTESIAN_POINT('Ctrl Pts',(20.3685406190576,9.7225193072249,0.));
#252739=CARTESIAN_POINT('Ctrl Pts',(20.3685406190576,9.7225193072249,12.));
#252740=CARTESIAN_POINT('Ctrl Pts',(20.3654261611056,9.72088778381081,0.));
#252741=CARTESIAN_POINT('Ctrl Pts',(20.3654261611056,9.72088778381081,12.));
#252742=CARTESIAN_POINT('Ctrl Pts',(20.3626256913981,9.71943648548099,0.));
#252743=CARTESIAN_POINT('Ctrl Pts',(20.3626256913981,9.71943648548099,12.));
#252744=CARTESIAN_POINT('Ctrl Pts',(20.3601498764344,9.71816778328007,0.));
#252745=CARTESIAN_POINT('Ctrl Pts',(20.3601498764344,9.71816778328007,12.));
#252746=CARTESIAN_POINT('Ctrl Pts',(20.3580133103356,9.71708493723096,0.));
#252747=CARTESIAN_POINT('Ctrl Pts',(20.3580133103356,9.71708493723096,12.));
#252748=CARTESIAN_POINT('Ctrl Pts',(20.3562337557875,9.71619192554186,0.));
#252749=CARTESIAN_POINT('Ctrl Pts',(20.3562337557875,9.71619192554186,12.));
#252750=CARTESIAN_POINT('Ctrl Pts',(20.3548282742361,9.71549257088173,0.));
#252751=CARTESIAN_POINT('Ctrl Pts',(20.3548282742361,9.71549257088173,12.));
#252752=CARTESIAN_POINT('Ctrl Pts',(20.3538098605706,9.71498978052021,0.));
#252753=CARTESIAN_POINT('Ctrl Pts',(20.3538098605706,9.71498978052021,12.));
#252754=CARTESIAN_POINT('Ctrl Pts',(20.3533097561886,9.71474590350681,0.));
#252755=CARTESIAN_POINT('Ctrl Pts',(20.3533097561886,9.71474590350681,12.));
#252756=CARTESIAN_POINT('Ctrl Pts',(20.3531126095522,9.71465227853042,0.));
#252757=CARTESIAN_POINT('Ctrl Pts',(20.3531126095522,9.71465227853042,12.));
#252758=CARTESIAN_POINT('Ctrl Pts',(20.353060251684,9.71462954053042,0.));
#252759=CARTESIAN_POINT('Ctrl Pts',(20.353060251684,9.71462954053042,12.));
#252760=CARTESIAN_POINT('Ctrl Pts',(20.353053841303,9.71462809124916,0.));
#252761=CARTESIAN_POINT('Ctrl Pts',(20.353053841303,9.71462809124916,12.));
#252762=CARTESIAN_POINT('',(22.8400320311648,12.4230808101438,0.));
#252763=CARTESIAN_POINT('Ctrl Pts',(22.8400320311648,12.4230808101438,0.));
#252764=CARTESIAN_POINT('Ctrl Pts',(22.8370364396459,12.418215285186,0.));
#252765=CARTESIAN_POINT('Ctrl Pts',(22.8310435872747,12.4084933766347,0.));
#252766=CARTESIAN_POINT('Ctrl Pts',(22.8220493007173,12.3939379378998,0.));
#252767=CARTESIAN_POINT('Ctrl Pts',(22.81004690224,12.374585536673,0.));
#252768=CARTESIAN_POINT('Ctrl Pts',(22.795027221673,12.3504864740319,0.));
#252769=CARTESIAN_POINT('Ctrl Pts',(22.7799908974768,12.3264788926075,0.));
#252770=CARTESIAN_POINT('Ctrl Pts',(22.764938010105,12.3025628601792,0.));
#252771=CARTESIAN_POINT('Ctrl Pts',(22.7498686970069,12.2787384750742,0.));
#252772=CARTESIAN_POINT('Ctrl Pts',(22.7347831655287,12.2550058702395,0.));
#252773=CARTESIAN_POINT('Ctrl Pts',(22.7196817119374,12.2313652198061,0.));
#252774=CARTESIAN_POINT('Ctrl Pts',(22.7045647168747,12.2078167360284,0.));
#252775=CARTESIAN_POINT('Ctrl Pts',(22.6894326205037,12.1843606579262,0.));
#252776=CARTESIAN_POINT('Ctrl Pts',(22.6742859034944,12.1609972423099,0.));
#252777=CARTESIAN_POINT('Ctrl Pts',(22.6591250653965,12.1377267537145,0.));
#252778=CARTESIAN_POINT('Ctrl Pts',(22.6439506046605,12.1145494550383,0.));
#252779=CARTESIAN_POINT('Ctrl Pts',(22.6287629967056,12.0914655972823,0.));
#252780=CARTESIAN_POINT('Ctrl Pts',(22.6135626764898,12.0684754113862,0.));
#252781=CARTESIAN_POINT('Ctrl Pts',(22.5983500505644,12.0455791139128,0.));
#252782=CARTESIAN_POINT('Ctrl Pts',(22.5831255061282,12.0227769113127,0.));
#252783=CARTESIAN_POINT('Ctrl Pts',(22.5678894211181,12.0000690046695,0.));
#252784=CARTESIAN_POINT('Ctrl Pts',(22.5526421741158,11.9774555943496,0.));
#252785=CARTESIAN_POINT('Ctrl Pts',(22.5373841537307,11.9549368843997,0.));
#252786=CARTESIAN_POINT('Ctrl Pts',(22.5221157697883,11.9325130877803,0.));
#252787=CARTESIAN_POINT('Ctrl Pts',(22.5068374513973,11.9101844254557,0.));
#252788=CARTESIAN_POINT('Ctrl Pts',(22.4915496418485,11.8879511239943,0.));
#252789=CARTESIAN_POINT('Ctrl Pts',(22.4762527946702,11.8658134137019,0.));
#252790=CARTESIAN_POINT('Ctrl Pts',(22.4609473690471,11.8437715264487,0.));
#252791=CARTESIAN_POINT('Ctrl Pts',(22.4456338258735,11.8218256937889,0.));
#252792=CARTESIAN_POINT('Ctrl Pts',(22.430312622646,11.7999761445173,0.));
#252793=CARTESIAN_POINT('Ctrl Pts',(22.4149842125008,11.7782231042039,0.));
#252794=CARTESIAN_POINT('Ctrl Pts',(22.3996490469191,11.7565667964764,0.));
#252795=CARTESIAN_POINT('Ctrl Pts',(22.3843075773899,11.7350074437961,0.));
#252796=CARTESIAN_POINT('Ctrl Pts',(22.3689602575491,11.7135452684532,0.));
#252797=CARTESIAN_POINT('Ctrl Pts',(22.3536075450029,11.6921804934056,0.));
#252798=CARTESIAN_POINT('Ctrl Pts',(22.3382499035619,11.6709133432985,0.));
#252799=CARTESIAN_POINT('Ctrl Pts',(22.3228878043976,11.6497440449857,0.));
#252800=CARTESIAN_POINT('Ctrl Pts',(22.3075217249049,11.6286728270009,0.));
#252801=CARTESIAN_POINT('Ctrl Pts',(22.2921521480356,11.6076999192357,0.));
#252802=CARTESIAN_POINT('Ctrl Pts',(22.2767795614348,11.5868255525188,0.));
#252803=CARTESIAN_POINT('Ctrl Pts',(22.2614044566898,11.5660499582403,0.));
#252804=CARTESIAN_POINT('Ctrl Pts',(22.2460273284654,11.5453733679121,0.));
#252805=CARTESIAN_POINT('Ctrl Pts',(22.2306486738901,11.5247960128477,0.));
#252806=CARTESIAN_POINT('Ctrl Pts',(22.2152689931022,11.5043181244242,0.));
#252807=CARTESIAN_POINT('Ctrl Pts',(22.1998887896436,11.483939934259,0.));
#252808=CARTESIAN_POINT('Ctrl Pts',(22.184508570917,11.463661674411,0.));
#252809=CARTESIAN_POINT('Ctrl Pts',(22.1691288486096,11.443483577557,0.));
#252810=CARTESIAN_POINT('Ctrl Pts',(22.1537501391487,11.4234058771742,0.));
#252811=CARTESIAN_POINT('Ctrl Pts',(22.1383729640964,11.4034288076908,0.));
#252812=CARTESIAN_POINT('Ctrl Pts',(22.1229978500186,11.3835526044256,0.));
#252813=CARTESIAN_POINT('Ctrl Pts',(22.1076253283979,11.3637775035367,0.));
#252814=CARTESIAN_POINT('Ctrl Pts',(22.0922559355294,11.3441037419553,0.));
#252815=CARTESIAN_POINT('Ctrl Pts',(22.0768902124267,11.3245315573168,0.));
#252816=CARTESIAN_POINT('Ctrl Pts',(22.0615287047179,11.3050611878771,0.));
#252817=CARTESIAN_POINT('Ctrl Pts',(22.046171962566,11.2856928724374,0.));
#252818=CARTESIAN_POINT('Ctrl Pts',(22.030820540835,11.2664268504206,0.));
#252819=CARTESIAN_POINT('Ctrl Pts',(22.0154749992363,11.2472633619275,0.));
#252820=CARTESIAN_POINT('Ctrl Pts',(22.0001359024839,11.2282026477896,0.));
#252821=CARTESIAN_POINT('Ctrl Pts',(21.9848038204439,11.2092449496125,0.));
#252822=CARTESIAN_POINT('Ctrl Pts',(21.9694793282914,11.190390509811,0.));
#252823=CARTESIAN_POINT('Ctrl Pts',(21.9541630066506,11.1716395716376,0.));
#252824=CARTESIAN_POINT('Ctrl Pts',(21.9388554416439,11.1529923792003,0.));
#252825=CARTESIAN_POINT('Ctrl Pts',(21.923557224952,11.1344491774741,0.));
#252826=CARTESIAN_POINT('Ctrl Pts',(21.9082689538688,11.1160102123024,0.));
#252827=CARTESIAN_POINT('Ctrl Pts',(21.8929912313608,11.0976757303944,0.));
#252828=CARTESIAN_POINT('Ctrl Pts',(21.877724666119,11.0794459793057,0.));
#252829=CARTESIAN_POINT('Ctrl Pts',(21.8624698726318,11.0613212074363,0.));
#252830=CARTESIAN_POINT('Ctrl Pts',(21.8472274713103,11.0433016640807,0.));
#252831=CARTESIAN_POINT('Ctrl Pts',(21.8319980886033,11.0253875994598,0.));
#252832=CARTESIAN_POINT('Ctrl Pts',(21.8167823571168,11.0075792647477,0.));
#252833=CARTESIAN_POINT('Ctrl Pts',(21.8015809157301,10.9898769120912,0.));
#252834=CARTESIAN_POINT('Ctrl Pts',(21.7863944097141,10.9722807946156,0.));
#252835=CARTESIAN_POINT('Ctrl Pts',(21.7712234908464,10.9547911664455,0.));
#252836=CARTESIAN_POINT('Ctrl Pts',(21.7560688175247,10.9374082827444,0.));
#252837=CARTESIAN_POINT('Ctrl Pts',(21.7409310548797,10.9201323997384,0.));
#252838=CARTESIAN_POINT('Ctrl Pts',(21.7258108748873,10.902963774734,0.));
#252839=CARTESIAN_POINT('Ctrl Pts',(21.7107089564825,10.8859026661293,0.));
#252840=CARTESIAN_POINT('Ctrl Pts',(21.6956259856672,10.8689493334095,0.));
#252841=CARTESIAN_POINT('Ctrl Pts',(21.6805626556467,10.8521040371835,0.));
#252842=CARTESIAN_POINT('Ctrl Pts',(21.6655196669732,10.8353670392272,0.));
#252843=CARTESIAN_POINT('Ctrl Pts',(21.6504977276866,10.8187386025136,0.));
#252844=CARTESIAN_POINT('Ctrl Pts',(21.6354975534557,10.8022189912369,0.));
#252845=CARTESIAN_POINT('Ctrl Pts',(21.6205198677173,10.7858084708261,0.));
#252846=CARTESIAN_POINT('Ctrl Pts',(21.6055654018176,10.7695073079552,0.));
#252847=CARTESIAN_POINT('Ctrl Pts',(21.5906348951743,10.7533157705941,0.));
#252848=CARTESIAN_POINT('Ctrl Pts',(21.5757290954371,10.7372341280467,0.));
#252849=CARTESIAN_POINT('Ctrl Pts',(21.5608487586468,10.7212626509816,0.));
#252850=CARTESIAN_POINT('Ctrl Pts',(21.5459946493955,10.7054016114571,0.));
#252851=CARTESIAN_POINT('Ctrl Pts',(21.5311675409807,10.689651282929,0.));
#252852=CARTESIAN_POINT('Ctrl Pts',(21.51636821558,10.6740119402834,0.));
#252853=CARTESIAN_POINT('Ctrl Pts',(21.5015974644449,10.6584838598939,0.));
#252854=CARTESIAN_POINT('Ctrl Pts',(21.4868560880889,10.6430673196607,0.));
#252855=CARTESIAN_POINT('Ctrl Pts',(21.4721448964766,10.6277625990456,0.));
#252856=CARTESIAN_POINT('Ctrl Pts',(21.4574647092097,10.6125699790961,0.));
#252857=CARTESIAN_POINT('Ctrl Pts',(21.4428163557144,10.5974897424622,0.));
#252858=CARTESIAN_POINT('Ctrl Pts',(21.4282006754631,10.5825221734573,0.));
#252859=CARTESIAN_POINT('Ctrl Pts',(21.4136185181979,10.5676675581108,0.));
#252860=CARTESIAN_POINT('Ctrl Pts',(21.3990707441497,10.5529261842108,0.));
#252861=CARTESIAN_POINT('Ctrl Pts',(21.3845582242602,10.5382983413421,0.));
#252862=CARTESIAN_POINT('Ctrl Pts',(21.3700818403936,10.5237843209057,0.));
#252863=CARTESIAN_POINT('Ctrl Pts',(21.3556424855814,10.5093844161685,0.));
#252864=CARTESIAN_POINT('Ctrl Pts',(21.3412410642904,10.4950989223337,0.));
#252865=CARTESIAN_POINT('Ctrl Pts',(21.3268784926819,10.4809281365931,0.));
#252866=CARTESIAN_POINT('Ctrl Pts',(21.3125556988731,10.4668723581768,0.));
#252867=CARTESIAN_POINT('Ctrl Pts',(21.2982736231931,10.4529318883874,0.));
#252868=CARTESIAN_POINT('Ctrl Pts',(21.2840332184483,10.4391070306391,0.));
#252869=CARTESIAN_POINT('Ctrl Pts',(21.2698354502403,10.42539809054,0.));
#252870=CARTESIAN_POINT('Ctrl Pts',(21.255681297275,10.4118053759588,0.));
#252871=CARTESIAN_POINT('Ctrl Pts',(21.2415717516714,10.3983291970846,0.));
#252872=CARTESIAN_POINT('Ctrl Pts',(21.22750781927,10.3849698664786,0.));
#252873=CARTESIAN_POINT('Ctrl Pts',(21.2134905199345,10.371727699113,0.));
#252874=CARTESIAN_POINT('Ctrl Pts',(21.199520887919,10.3586030124587,0.));
#252875=CARTESIAN_POINT('Ctrl Pts',(21.1855999722416,10.3455961265701,0.));
#252876=CARTESIAN_POINT('Ctrl Pts',(21.1717288370509,10.3327073641572,0.));
#252877=CARTESIAN_POINT('Ctrl Pts',(21.1579085619965,10.3199370506544,0.));
#252878=CARTESIAN_POINT('Ctrl Pts',(21.1441402425843,10.3072855142687,0.));
#252879=CARTESIAN_POINT('Ctrl Pts',(21.1304249906002,10.2947530860721,0.));
#252880=CARTESIAN_POINT('Ctrl Pts',(21.1167639345631,10.2823401001072,0.));
#252881=CARTESIAN_POINT('Ctrl Pts',(21.1031582201627,10.2700468934744,0.));
#252882=CARTESIAN_POINT('Ctrl Pts',(21.0896090107063,10.2578738064181,0.));
#252883=CARTESIAN_POINT('Ctrl Pts',(21.0761174875444,10.2458211823912,0.));
#252884=CARTESIAN_POINT('Ctrl Pts',(21.0626848505663,10.2338893681567,0.));
#252885=CARTESIAN_POINT('Ctrl Pts',(21.0493123187483,10.2220787139155,0.));
#252886=CARTESIAN_POINT('Ctrl Pts',(21.0360011306815,10.2103895734123,0.));
#252887=CARTESIAN_POINT('Ctrl Pts',(21.0227525451107,10.1988223040425,0.));
#252888=CARTESIAN_POINT('Ctrl Pts',(21.0095678414486,10.187377266936,0.));
#252889=CARTESIAN_POINT('Ctrl Pts',(20.9964483203686,10.1760548270767,0.));
#252890=CARTESIAN_POINT('Ctrl Pts',(20.9833953044736,10.1648553534568,0.));
#252891=CARTESIAN_POINT('Ctrl Pts',(20.9704101389369,10.1537792192065,0.));
#252892=CARTESIAN_POINT('Ctrl Pts',(20.9574941921591,10.1428268017256,0.));
#252893=CARTESIAN_POINT('Ctrl Pts',(20.9446488563933,10.1319984827908,0.));
#252894=CARTESIAN_POINT('Ctrl Pts',(20.9318755484734,10.1212946487057,0.));
#252895=CARTESIAN_POINT('Ctrl Pts',(20.919175710627,10.1107156904836,0.));
#252896=CARTESIAN_POINT('Ctrl Pts',(20.9065508112557,10.1002620040076,0.));
#252897=CARTESIAN_POINT('Ctrl Pts',(20.894002345737,10.0899339901916,0.));
#252898=CARTESIAN_POINT('Ctrl Pts',(20.881531837184,10.0797320551154,0.));
#252899=CARTESIAN_POINT('Ctrl Pts',(20.86914083737,10.0696566102218,0.));
#252900=CARTESIAN_POINT('Ctrl Pts',(20.8568309277316,10.0597080725375,0.));
#252901=CARTESIAN_POINT('Ctrl Pts',(20.8446037203402,10.0498868648733,0.));
#252902=CARTESIAN_POINT('Ctrl Pts',(20.8324608588909,10.0401934160234,0.));
#252903=CARTESIAN_POINT('Ctrl Pts',(20.8204040196602,10.0306281609435,0.));
#252904=CARTESIAN_POINT('Ctrl Pts',(20.8084349126888,10.0211915410095,0.));
#252905=CARTESIAN_POINT('Ctrl Pts',(20.7965552829908,10.0118840042786,0.));
#252906=CARTESIAN_POINT('Ctrl Pts',(20.7847669117568,10.0027060057389,0.));
#252907=CARTESIAN_POINT('Ctrl Pts',(20.7730716175417,9.9936580075464,0.));
#252908=CARTESIAN_POINT('Ctrl Pts',(20.761471257499,9.98474047926853,0.));
#252909=CARTESIAN_POINT('Ctrl Pts',(20.7499677289627,9.9759538982347,0.));
#252910=CARTESIAN_POINT('Ctrl Pts',(20.7385629709795,9.96729874986202,0.));
#252911=CARTESIAN_POINT('Ctrl Pts',(20.7272589658751,9.95877552798398,0.));
#252912=CARTESIAN_POINT('Ctrl Pts',(20.7160577407579,9.95038473514949,0.));
#252913=CARTESIAN_POINT('Ctrl Pts',(20.7049613692234,9.94212688298236,0.));
#252914=CARTESIAN_POINT('Ctrl Pts',(20.6939719732484,9.9340024925973,0.));
#252915=CARTESIAN_POINT('Ctrl Pts',(20.6830917250255,9.92601209498749,0.));
#252916=CARTESIAN_POINT('Ctrl Pts',(20.6723228488263,9.91815623141289,0.));
#252917=CARTESIAN_POINT('Ctrl Pts',(20.6616676228315,9.91043545377008,0.));
#252918=CARTESIAN_POINT('Ctrl Pts',(20.6511283817414,9.90285032516693,0.));
#252919=CARTESIAN_POINT('Ctrl Pts',(20.6407075193976,9.8954014204912,0.));
#252920=CARTESIAN_POINT('Ctrl Pts',(20.6304074914087,9.88808932697306,0.));
#252921=CARTESIAN_POINT('Ctrl Pts',(20.6202308177474,9.88091464472676,0.));
#252922=CARTESIAN_POINT('Ctrl Pts',(20.6101800854494,9.87387798732956,0.));
#252923=CARTESIAN_POINT('Ctrl Pts',(20.6002579513699,9.86697998242623,0.));
#252924=CARTESIAN_POINT('Ctrl Pts',(20.5904671449754,9.86022127232748,0.));
#252925=CARTESIAN_POINT('Ctrl Pts',(20.5808104710015,9.85360251456981,0.));
#252926=CARTESIAN_POINT('Ctrl Pts',(20.5712908125139,9.84712438256278,0.));
#252927=CARTESIAN_POINT('Ctrl Pts',(20.5619111362402,9.84078756677565,0.));
#252928=CARTESIAN_POINT('Ctrl Pts',(20.552674497646,9.83459277585315,0.));
#252929=CARTESIAN_POINT('Ctrl Pts',(20.5435840460721,9.82854073773878,0.));
#252930=CARTESIAN_POINT('Ctrl Pts',(20.5346430299517,9.82263220080363,0.));
#252931=CARTESIAN_POINT('Ctrl Pts',(20.5258548000629,9.81686793455943,0.));
#252932=CARTESIAN_POINT('Ctrl Pts',(20.517222812284,9.81124873025282,0.));
#252933=CARTESIAN_POINT('Ctrl Pts',(20.5087506310505,9.80577540161088,0.));
#252934=CARTESIAN_POINT('Ctrl Pts',(20.5004419312107,9.80044878520949,0.));
#252935=CARTESIAN_POINT('Ctrl Pts',(20.4923005087943,9.79526974288331,0.));
#252936=CARTESIAN_POINT('Ctrl Pts',(20.4843302955329,9.79023916498656,0.));
#252937=CARTESIAN_POINT('Ctrl Pts',(20.4765353711586,9.78535797314167,0.));
#252938=CARTESIAN_POINT('Ctrl Pts',(20.4689199790669,9.78062712373321,0.));
#252939=CARTESIAN_POINT('Ctrl Pts',(20.4614885274975,9.77604760815529,0.));
#252940=CARTESIAN_POINT('Ctrl Pts',(20.4542455817527,9.7716204510407,0.));
#252941=CARTESIAN_POINT('Ctrl Pts',(20.447195862298,9.76734670980892,0.));
#252942=CARTESIAN_POINT('Ctrl Pts',(20.44034423294,9.76322747195495,0.));
#252943=CARTESIAN_POINT('Ctrl Pts',(20.4336957355473,9.75926386289923,0.));
#252944=CARTESIAN_POINT('Ctrl Pts',(20.4272556476629,9.75545705902418,0.));
#252945=CARTESIAN_POINT('Ctrl Pts',(20.4210295275817,9.7518082978643,0.));
#252946=CARTESIAN_POINT('Ctrl Pts',(20.4150232777393,9.74831889242174,0.));
#252947=CARTESIAN_POINT('Ctrl Pts',(20.4092430879861,9.74499021838538,0.));
#252948=CARTESIAN_POINT('Ctrl Pts',(20.4036953576549,9.74182369656272,0.));
#252949=CARTESIAN_POINT('Ctrl Pts',(20.3983866213331,9.73882077613201,0.));
#252950=CARTESIAN_POINT('Ctrl Pts',(20.3933234845647,9.73598292014243,0.));
#252951=CARTESIAN_POINT('Ctrl Pts',(20.3885129129912,9.73331167102808,0.));
#252952=CARTESIAN_POINT('Ctrl Pts',(20.3839624556742,9.73080870123727,0.));
#252953=CARTESIAN_POINT('Ctrl Pts',(20.3796805893304,9.72847589116542,0.));
#252954=CARTESIAN_POINT('Ctrl Pts',(20.3756766651951,9.72631531732881,0.));
#252955=CARTESIAN_POINT('Ctrl Pts',(20.371960235676,9.72432910043194,0.));
#252956=CARTESIAN_POINT('Ctrl Pts',(20.3685406190576,9.7225193072249,0.));
#252957=CARTESIAN_POINT('Ctrl Pts',(20.3654261611056,9.72088778381081,0.));
#252958=CARTESIAN_POINT('Ctrl Pts',(20.3626256913981,9.71943648548099,0.));
#252959=CARTESIAN_POINT('Ctrl Pts',(20.3601498764344,9.71816778328007,0.));
#252960=CARTESIAN_POINT('Ctrl Pts',(20.3580133103356,9.71708493723096,0.));
#252961=CARTESIAN_POINT('Ctrl Pts',(20.3562337557875,9.71619192554186,0.));
#252962=CARTESIAN_POINT('Ctrl Pts',(20.3548282742361,9.71549257088173,0.));
#252963=CARTESIAN_POINT('Ctrl Pts',(20.3538098605706,9.71498978052021,0.));
#252964=CARTESIAN_POINT('Ctrl Pts',(20.3533097561886,9.71474590350681,0.));
#252965=CARTESIAN_POINT('Ctrl Pts',(20.3531126095522,9.71465227853042,0.));
#252966=CARTESIAN_POINT('Ctrl Pts',(20.353060251684,9.71462954053042,0.));
#252967=CARTESIAN_POINT('Ctrl Pts',(20.353053841303,9.71462809124916,0.));
#252968=CARTESIAN_POINT('',(22.8400320311648,12.4230808101438,12.));
#252969=CARTESIAN_POINT('',(22.8400320311648,12.4230808101438,0.));
#252970=CARTESIAN_POINT('Ctrl Pts',(20.353053841303,9.71462809124916,12.));
#252971=CARTESIAN_POINT('Ctrl Pts',(20.353060251684,9.71462954053042,12.));
#252972=CARTESIAN_POINT('Ctrl Pts',(20.3531126095522,9.71465227853042,12.));
#252973=CARTESIAN_POINT('Ctrl Pts',(20.3533097561886,9.71474590350681,12.));
#252974=CARTESIAN_POINT('Ctrl Pts',(20.3538098605706,9.71498978052021,12.));
#252975=CARTESIAN_POINT('Ctrl Pts',(20.3548282742361,9.71549257088173,12.));
#252976=CARTESIAN_POINT('Ctrl Pts',(20.3562337557875,9.71619192554186,12.));
#252977=CARTESIAN_POINT('Ctrl Pts',(20.3580133103356,9.71708493723096,12.));
#252978=CARTESIAN_POINT('Ctrl Pts',(20.3601498764344,9.71816778328007,12.));
#252979=CARTESIAN_POINT('Ctrl Pts',(20.3626256913981,9.71943648548099,12.));
#252980=CARTESIAN_POINT('Ctrl Pts',(20.3654261611056,9.72088778381081,12.));
#252981=CARTESIAN_POINT('Ctrl Pts',(20.3685406190576,9.7225193072249,12.));
#252982=CARTESIAN_POINT('Ctrl Pts',(20.371960235676,9.72432910043194,12.));
#252983=CARTESIAN_POINT('Ctrl Pts',(20.3756766651951,9.72631531732881,12.));
#252984=CARTESIAN_POINT('Ctrl Pts',(20.3796805893304,9.72847589116542,12.));
#252985=CARTESIAN_POINT('Ctrl Pts',(20.3839624556742,9.73080870123727,12.));
#252986=CARTESIAN_POINT('Ctrl Pts',(20.3885129129912,9.73331167102808,12.));
#252987=CARTESIAN_POINT('Ctrl Pts',(20.3933234845647,9.73598292014243,12.));
#252988=CARTESIAN_POINT('Ctrl Pts',(20.3983866213331,9.73882077613201,12.));
#252989=CARTESIAN_POINT('Ctrl Pts',(20.4036953576549,9.74182369656272,12.));
#252990=CARTESIAN_POINT('Ctrl Pts',(20.4092430879861,9.74499021838538,12.));
#252991=CARTESIAN_POINT('Ctrl Pts',(20.4150232777393,9.74831889242174,12.));
#252992=CARTESIAN_POINT('Ctrl Pts',(20.4210295275817,9.7518082978643,12.));
#252993=CARTESIAN_POINT('Ctrl Pts',(20.4272556476629,9.75545705902418,12.));
#252994=CARTESIAN_POINT('Ctrl Pts',(20.4336957355473,9.75926386289923,12.));
#252995=CARTESIAN_POINT('Ctrl Pts',(20.44034423294,9.76322747195495,12.));
#252996=CARTESIAN_POINT('Ctrl Pts',(20.447195862298,9.76734670980892,12.));
#252997=CARTESIAN_POINT('Ctrl Pts',(20.4542455817527,9.7716204510407,12.));
#252998=CARTESIAN_POINT('Ctrl Pts',(20.4614885274975,9.77604760815529,12.));
#252999=CARTESIAN_POINT('Ctrl Pts',(20.4689199790669,9.78062712373321,12.));
#253000=CARTESIAN_POINT('Ctrl Pts',(20.4765353711586,9.78535797314167,12.));
#253001=CARTESIAN_POINT('Ctrl Pts',(20.4843302955329,9.79023916498656,12.));
#253002=CARTESIAN_POINT('Ctrl Pts',(20.4923005087943,9.79526974288331,12.));
#253003=CARTESIAN_POINT('Ctrl Pts',(20.5004419312107,9.80044878520949,12.));
#253004=CARTESIAN_POINT('Ctrl Pts',(20.5087506310505,9.80577540161088,12.));
#253005=CARTESIAN_POINT('Ctrl Pts',(20.517222812284,9.81124873025282,12.));
#253006=CARTESIAN_POINT('Ctrl Pts',(20.5258548000629,9.81686793455943,12.));
#253007=CARTESIAN_POINT('Ctrl Pts',(20.5346430299517,9.82263220080363,12.));
#253008=CARTESIAN_POINT('Ctrl Pts',(20.5435840460721,9.82854073773878,12.));
#253009=CARTESIAN_POINT('Ctrl Pts',(20.552674497646,9.83459277585315,12.));
#253010=CARTESIAN_POINT('Ctrl Pts',(20.5619111362402,9.84078756677565,12.));
#253011=CARTESIAN_POINT('Ctrl Pts',(20.5712908125139,9.84712438256278,12.));
#253012=CARTESIAN_POINT('Ctrl Pts',(20.5808104710015,9.85360251456981,12.));
#253013=CARTESIAN_POINT('Ctrl Pts',(20.5904671449754,9.86022127232748,12.));
#253014=CARTESIAN_POINT('Ctrl Pts',(20.6002579513699,9.86697998242623,12.));
#253015=CARTESIAN_POINT('Ctrl Pts',(20.6101800854494,9.87387798732956,12.));
#253016=CARTESIAN_POINT('Ctrl Pts',(20.6202308177474,9.88091464472676,12.));
#253017=CARTESIAN_POINT('Ctrl Pts',(20.6304074914087,9.88808932697306,12.));
#253018=CARTESIAN_POINT('Ctrl Pts',(20.6407075193976,9.8954014204912,12.));
#253019=CARTESIAN_POINT('Ctrl Pts',(20.6511283817414,9.90285032516693,12.));
#253020=CARTESIAN_POINT('Ctrl Pts',(20.6616676228315,9.91043545377008,12.));
#253021=CARTESIAN_POINT('Ctrl Pts',(20.6723228488263,9.91815623141289,12.));
#253022=CARTESIAN_POINT('Ctrl Pts',(20.6830917250255,9.92601209498749,12.));
#253023=CARTESIAN_POINT('Ctrl Pts',(20.6939719732484,9.9340024925973,12.));
#253024=CARTESIAN_POINT('Ctrl Pts',(20.7049613692234,9.94212688298236,12.));
#253025=CARTESIAN_POINT('Ctrl Pts',(20.7160577407579,9.95038473514949,12.));
#253026=CARTESIAN_POINT('Ctrl Pts',(20.7272589658751,9.95877552798398,12.));
#253027=CARTESIAN_POINT('Ctrl Pts',(20.7385629709795,9.96729874986202,12.));
#253028=CARTESIAN_POINT('Ctrl Pts',(20.7499677289627,9.9759538982347,12.));
#253029=CARTESIAN_POINT('Ctrl Pts',(20.761471257499,9.98474047926853,12.));
#253030=CARTESIAN_POINT('Ctrl Pts',(20.7730716175417,9.9936580075464,12.));
#253031=CARTESIAN_POINT('Ctrl Pts',(20.7847669117568,10.0027060057389,12.));
#253032=CARTESIAN_POINT('Ctrl Pts',(20.7965552829908,10.0118840042786,12.));
#253033=CARTESIAN_POINT('Ctrl Pts',(20.8084349126888,10.0211915410095,12.));
#253034=CARTESIAN_POINT('Ctrl Pts',(20.8204040196602,10.0306281609435,12.));
#253035=CARTESIAN_POINT('Ctrl Pts',(20.8324608588909,10.0401934160234,12.));
#253036=CARTESIAN_POINT('Ctrl Pts',(20.8446037203402,10.0498868648733,12.));
#253037=CARTESIAN_POINT('Ctrl Pts',(20.8568309277316,10.0597080725375,12.));
#253038=CARTESIAN_POINT('Ctrl Pts',(20.86914083737,10.0696566102218,12.));
#253039=CARTESIAN_POINT('Ctrl Pts',(20.881531837184,10.0797320551154,12.));
#253040=CARTESIAN_POINT('Ctrl Pts',(20.894002345737,10.0899339901916,12.));
#253041=CARTESIAN_POINT('Ctrl Pts',(20.9065508112557,10.1002620040076,12.));
#253042=CARTESIAN_POINT('Ctrl Pts',(20.919175710627,10.1107156904836,12.));
#253043=CARTESIAN_POINT('Ctrl Pts',(20.9318755484734,10.1212946487057,12.));
#253044=CARTESIAN_POINT('Ctrl Pts',(20.9446488563933,10.1319984827908,12.));
#253045=CARTESIAN_POINT('Ctrl Pts',(20.9574941921591,10.1428268017256,12.));
#253046=CARTESIAN_POINT('Ctrl Pts',(20.9704101389369,10.1537792192065,12.));
#253047=CARTESIAN_POINT('Ctrl Pts',(20.9833953044736,10.1648553534568,12.));
#253048=CARTESIAN_POINT('Ctrl Pts',(20.9964483203686,10.1760548270767,12.));
#253049=CARTESIAN_POINT('Ctrl Pts',(21.0095678414486,10.187377266936,12.));
#253050=CARTESIAN_POINT('Ctrl Pts',(21.0227525451107,10.1988223040425,12.));
#253051=CARTESIAN_POINT('Ctrl Pts',(21.0360011306815,10.2103895734123,12.));
#253052=CARTESIAN_POINT('Ctrl Pts',(21.0493123187483,10.2220787139155,12.));
#253053=CARTESIAN_POINT('Ctrl Pts',(21.0626848505663,10.2338893681567,12.));
#253054=CARTESIAN_POINT('Ctrl Pts',(21.0761174875444,10.2458211823912,12.));
#253055=CARTESIAN_POINT('Ctrl Pts',(21.0896090107063,10.2578738064181,12.));
#253056=CARTESIAN_POINT('Ctrl Pts',(21.1031582201627,10.2700468934744,12.));
#253057=CARTESIAN_POINT('Ctrl Pts',(21.1167639345631,10.2823401001072,12.));
#253058=CARTESIAN_POINT('Ctrl Pts',(21.1304249906002,10.2947530860721,12.));
#253059=CARTESIAN_POINT('Ctrl Pts',(21.1441402425843,10.3072855142687,12.));
#253060=CARTESIAN_POINT('Ctrl Pts',(21.1579085619965,10.3199370506544,12.));
#253061=CARTESIAN_POINT('Ctrl Pts',(21.1717288370509,10.3327073641572,12.));
#253062=CARTESIAN_POINT('Ctrl Pts',(21.1855999722416,10.3455961265701,12.));
#253063=CARTESIAN_POINT('Ctrl Pts',(21.199520887919,10.3586030124587,12.));
#253064=CARTESIAN_POINT('Ctrl Pts',(21.2134905199345,10.371727699113,12.));
#253065=CARTESIAN_POINT('Ctrl Pts',(21.22750781927,10.3849698664786,12.));
#253066=CARTESIAN_POINT('Ctrl Pts',(21.2415717516714,10.3983291970846,12.));
#253067=CARTESIAN_POINT('Ctrl Pts',(21.255681297275,10.4118053759588,12.));
#253068=CARTESIAN_POINT('Ctrl Pts',(21.2698354502403,10.42539809054,12.));
#253069=CARTESIAN_POINT('Ctrl Pts',(21.2840332184483,10.4391070306391,12.));
#253070=CARTESIAN_POINT('Ctrl Pts',(21.2982736231931,10.4529318883874,12.));
#253071=CARTESIAN_POINT('Ctrl Pts',(21.3125556988731,10.4668723581768,12.));
#253072=CARTESIAN_POINT('Ctrl Pts',(21.3268784926819,10.4809281365931,12.));
#253073=CARTESIAN_POINT('Ctrl Pts',(21.3412410642904,10.4950989223337,12.));
#253074=CARTESIAN_POINT('Ctrl Pts',(21.3556424855814,10.5093844161685,12.));
#253075=CARTESIAN_POINT('Ctrl Pts',(21.3700818403936,10.5237843209057,12.));
#253076=CARTESIAN_POINT('Ctrl Pts',(21.3845582242602,10.5382983413421,12.));
#253077=CARTESIAN_POINT('Ctrl Pts',(21.3990707441497,10.5529261842108,12.));
#253078=CARTESIAN_POINT('Ctrl Pts',(21.4136185181979,10.5676675581108,12.));
#253079=CARTESIAN_POINT('Ctrl Pts',(21.4282006754631,10.5825221734573,12.));
#253080=CARTESIAN_POINT('Ctrl Pts',(21.4428163557144,10.5974897424622,12.));
#253081=CARTESIAN_POINT('Ctrl Pts',(21.4574647092097,10.6125699790961,12.));
#253082=CARTESIAN_POINT('Ctrl Pts',(21.4721448964766,10.6277625990456,12.));
#253083=CARTESIAN_POINT('Ctrl Pts',(21.4868560880889,10.6430673196607,12.));
#253084=CARTESIAN_POINT('Ctrl Pts',(21.5015974644449,10.6584838598939,12.));
#253085=CARTESIAN_POINT('Ctrl Pts',(21.51636821558,10.6740119402834,12.));
#253086=CARTESIAN_POINT('Ctrl Pts',(21.5311675409807,10.689651282929,12.));
#253087=CARTESIAN_POINT('Ctrl Pts',(21.5459946493955,10.7054016114571,12.));
#253088=CARTESIAN_POINT('Ctrl Pts',(21.5608487586468,10.7212626509816,12.));
#253089=CARTESIAN_POINT('Ctrl Pts',(21.5757290954371,10.7372341280467,12.));
#253090=CARTESIAN_POINT('Ctrl Pts',(21.5906348951743,10.7533157705941,12.));
#253091=CARTESIAN_POINT('Ctrl Pts',(21.6055654018176,10.7695073079552,12.));
#253092=CARTESIAN_POINT('Ctrl Pts',(21.6205198677173,10.7858084708261,12.));
#253093=CARTESIAN_POINT('Ctrl Pts',(21.6354975534557,10.8022189912369,12.));
#253094=CARTESIAN_POINT('Ctrl Pts',(21.6504977276866,10.8187386025136,12.));
#253095=CARTESIAN_POINT('Ctrl Pts',(21.6655196669732,10.8353670392272,12.));
#253096=CARTESIAN_POINT('Ctrl Pts',(21.6805626556467,10.8521040371835,12.));
#253097=CARTESIAN_POINT('Ctrl Pts',(21.6956259856672,10.8689493334095,12.));
#253098=CARTESIAN_POINT('Ctrl Pts',(21.7107089564825,10.8859026661293,12.));
#253099=CARTESIAN_POINT('Ctrl Pts',(21.7258108748873,10.902963774734,12.));
#253100=CARTESIAN_POINT('Ctrl Pts',(21.7409310548797,10.9201323997384,12.));
#253101=CARTESIAN_POINT('Ctrl Pts',(21.7560688175247,10.9374082827444,12.));
#253102=CARTESIAN_POINT('Ctrl Pts',(21.7712234908464,10.9547911664455,12.));
#253103=CARTESIAN_POINT('Ctrl Pts',(21.7863944097141,10.9722807946156,12.));
#253104=CARTESIAN_POINT('Ctrl Pts',(21.8015809157301,10.9898769120912,12.));
#253105=CARTESIAN_POINT('Ctrl Pts',(21.8167823571168,11.0075792647477,12.));
#253106=CARTESIAN_POINT('Ctrl Pts',(21.8319980886033,11.0253875994598,12.));
#253107=CARTESIAN_POINT('Ctrl Pts',(21.8472274713103,11.0433016640807,12.));
#253108=CARTESIAN_POINT('Ctrl Pts',(21.8624698726318,11.0613212074363,12.));
#253109=CARTESIAN_POINT('Ctrl Pts',(21.877724666119,11.0794459793057,12.));
#253110=CARTESIAN_POINT('Ctrl Pts',(21.8929912313608,11.0976757303944,12.));
#253111=CARTESIAN_POINT('Ctrl Pts',(21.9082689538688,11.1160102123024,12.));
#253112=CARTESIAN_POINT('Ctrl Pts',(21.923557224952,11.1344491774741,12.));
#253113=CARTESIAN_POINT('Ctrl Pts',(21.9388554416439,11.1529923792003,12.));
#253114=CARTESIAN_POINT('Ctrl Pts',(21.9541630066506,11.1716395716376,12.));
#253115=CARTESIAN_POINT('Ctrl Pts',(21.9694793282914,11.190390509811,12.));
#253116=CARTESIAN_POINT('Ctrl Pts',(21.9848038204439,11.2092449496125,12.));
#253117=CARTESIAN_POINT('Ctrl Pts',(22.0001359024839,11.2282026477896,12.));
#253118=CARTESIAN_POINT('Ctrl Pts',(22.0154749992363,11.2472633619275,12.));
#253119=CARTESIAN_POINT('Ctrl Pts',(22.030820540835,11.2664268504206,12.));
#253120=CARTESIAN_POINT('Ctrl Pts',(22.046171962566,11.2856928724374,12.));
#253121=CARTESIAN_POINT('Ctrl Pts',(22.0615287047179,11.3050611878771,12.));
#253122=CARTESIAN_POINT('Ctrl Pts',(22.0768902124267,11.3245315573168,12.));
#253123=CARTESIAN_POINT('Ctrl Pts',(22.0922559355294,11.3441037419553,12.));
#253124=CARTESIAN_POINT('Ctrl Pts',(22.1076253283979,11.3637775035367,12.));
#253125=CARTESIAN_POINT('Ctrl Pts',(22.1229978500186,11.3835526044256,12.));
#253126=CARTESIAN_POINT('Ctrl Pts',(22.1383729640964,11.4034288076908,12.));
#253127=CARTESIAN_POINT('Ctrl Pts',(22.1537501391487,11.4234058771742,12.));
#253128=CARTESIAN_POINT('Ctrl Pts',(22.1691288486096,11.443483577557,12.));
#253129=CARTESIAN_POINT('Ctrl Pts',(22.184508570917,11.463661674411,12.));
#253130=CARTESIAN_POINT('Ctrl Pts',(22.1998887896436,11.483939934259,12.));
#253131=CARTESIAN_POINT('Ctrl Pts',(22.2152689931022,11.5043181244242,12.));
#253132=CARTESIAN_POINT('Ctrl Pts',(22.2306486738901,11.5247960128477,12.));
#253133=CARTESIAN_POINT('Ctrl Pts',(22.2460273284654,11.5453733679121,12.));
#253134=CARTESIAN_POINT('Ctrl Pts',(22.2614044566898,11.5660499582403,12.));
#253135=CARTESIAN_POINT('Ctrl Pts',(22.2767795614348,11.5868255525188,12.));
#253136=CARTESIAN_POINT('Ctrl Pts',(22.2921521480356,11.6076999192357,12.));
#253137=CARTESIAN_POINT('Ctrl Pts',(22.3075217249049,11.6286728270009,12.));
#253138=CARTESIAN_POINT('Ctrl Pts',(22.3228878043976,11.6497440449857,12.));
#253139=CARTESIAN_POINT('Ctrl Pts',(22.3382499035619,11.6709133432985,12.));
#253140=CARTESIAN_POINT('Ctrl Pts',(22.3536075450029,11.6921804934056,12.));
#253141=CARTESIAN_POINT('Ctrl Pts',(22.3689602575491,11.7135452684532,12.));
#253142=CARTESIAN_POINT('Ctrl Pts',(22.3843075773899,11.7350074437961,12.));
#253143=CARTESIAN_POINT('Ctrl Pts',(22.3996490469191,11.7565667964764,12.));
#253144=CARTESIAN_POINT('Ctrl Pts',(22.4149842125008,11.7782231042039,12.));
#253145=CARTESIAN_POINT('Ctrl Pts',(22.430312622646,11.7999761445173,12.));
#253146=CARTESIAN_POINT('Ctrl Pts',(22.4456338258735,11.8218256937889,12.));
#253147=CARTESIAN_POINT('Ctrl Pts',(22.4609473690471,11.8437715264487,12.));
#253148=CARTESIAN_POINT('Ctrl Pts',(22.4762527946702,11.8658134137019,12.));
#253149=CARTESIAN_POINT('Ctrl Pts',(22.4915496418485,11.8879511239943,12.));
#253150=CARTESIAN_POINT('Ctrl Pts',(22.5068374513973,11.9101844254557,12.));
#253151=CARTESIAN_POINT('Ctrl Pts',(22.5221157697883,11.9325130877803,12.));
#253152=CARTESIAN_POINT('Ctrl Pts',(22.5373841537307,11.9549368843997,12.));
#253153=CARTESIAN_POINT('Ctrl Pts',(22.5526421741158,11.9774555943496,12.));
#253154=CARTESIAN_POINT('Ctrl Pts',(22.5678894211181,12.0000690046695,12.));
#253155=CARTESIAN_POINT('Ctrl Pts',(22.5831255061282,12.0227769113127,12.));
#253156=CARTESIAN_POINT('Ctrl Pts',(22.5983500505644,12.0455791139128,12.));
#253157=CARTESIAN_POINT('Ctrl Pts',(22.6135626764898,12.0684754113862,12.));
#253158=CARTESIAN_POINT('Ctrl Pts',(22.6287629967056,12.0914655972823,12.));
#253159=CARTESIAN_POINT('Ctrl Pts',(22.6439506046605,12.1145494550383,12.));
#253160=CARTESIAN_POINT('Ctrl Pts',(22.6591250653965,12.1377267537145,12.));
#253161=CARTESIAN_POINT('Ctrl Pts',(22.6742859034944,12.1609972423099,12.));
#253162=CARTESIAN_POINT('Ctrl Pts',(22.6894326205037,12.1843606579262,12.));
#253163=CARTESIAN_POINT('Ctrl Pts',(22.7045647168747,12.2078167360284,12.));
#253164=CARTESIAN_POINT('Ctrl Pts',(22.7196817119374,12.2313652198061,12.));
#253165=CARTESIAN_POINT('Ctrl Pts',(22.7347831655287,12.2550058702395,12.));
#253166=CARTESIAN_POINT('Ctrl Pts',(22.7498686970069,12.2787384750742,12.));
#253167=CARTESIAN_POINT('Ctrl Pts',(22.764938010105,12.3025628601792,12.));
#253168=CARTESIAN_POINT('Ctrl Pts',(22.7799908974768,12.3264788926075,12.));
#253169=CARTESIAN_POINT('Ctrl Pts',(22.795027221673,12.3504864740319,12.));
#253170=CARTESIAN_POINT('Ctrl Pts',(22.81004690224,12.374585536673,12.));
#253171=CARTESIAN_POINT('Ctrl Pts',(22.8220493007173,12.3939379378998,12.));
#253172=CARTESIAN_POINT('Ctrl Pts',(22.8310435872747,12.4084933766347,12.));
#253173=CARTESIAN_POINT('Ctrl Pts',(22.8370364396459,12.418215285186,12.));
#253174=CARTESIAN_POINT('Ctrl Pts',(22.8400320311648,12.4230808101438,12.));
#253175=CARTESIAN_POINT('Ctrl Pts',(21.2610617890679,7.52250298901264,0.));
#253176=CARTESIAN_POINT('Ctrl Pts',(21.2610617890679,7.52250298901264,12.));
#253177=CARTESIAN_POINT('Ctrl Pts',(21.2610673466886,7.5225064970397,0.));
#253178=CARTESIAN_POINT('Ctrl Pts',(21.2610673466886,7.5225064970397,12.));
#253179=CARTESIAN_POINT('Ctrl Pts',(21.2611204474866,7.52252744144904,0.));
#253180=CARTESIAN_POINT('Ctrl Pts',(21.2611204474866,7.52252744144904,12.));
#253181=CARTESIAN_POINT('Ctrl Pts',(21.261326054066,7.52260064231661,0.));
#253182=CARTESIAN_POINT('Ctrl Pts',(21.261326054066,7.52260064231661,12.));
#253183=CARTESIAN_POINT('Ctrl Pts',(21.2618521283555,7.5227818224267,0.));
#253184=CARTESIAN_POINT('Ctrl Pts',(21.2618521283555,7.5227818224267,12.));
#253185=CARTESIAN_POINT('Ctrl Pts',(21.262927782038,7.52314642316199,0.));
#253186=CARTESIAN_POINT('Ctrl Pts',(21.262927782038,7.52314642316199,12.));
#253187=CARTESIAN_POINT('Ctrl Pts',(21.2644161259962,7.52364573027553,0.));
#253188=CARTESIAN_POINT('Ctrl Pts',(21.2644161259962,7.52364573027553,12.));
#253189=CARTESIAN_POINT('Ctrl Pts',(21.2663059157058,7.52427261074298,0.));
#253190=CARTESIAN_POINT('Ctrl Pts',(21.2663059157058,7.52427261074298,12.));
#253191=CARTESIAN_POINT('Ctrl Pts',(21.2685823838671,7.52501770333531,0.));
#253192=CARTESIAN_POINT('Ctrl Pts',(21.2685823838671,7.52501770333531,12.));
#253193=CARTESIAN_POINT('Ctrl Pts',(21.2712301573466,7.5258712609553,0.));
#253194=CARTESIAN_POINT('Ctrl Pts',(21.2712301573466,7.5258712609553,12.));
#253195=CARTESIAN_POINT('Ctrl Pts',(21.2742366113579,7.52682526918541,0.));
#253196=CARTESIAN_POINT('Ctrl Pts',(21.2742366113579,7.52682526918541,12.));
#253197=CARTESIAN_POINT('Ctrl Pts',(21.2775925269652,7.52787386225333,0.));
#253198=CARTESIAN_POINT('Ctrl Pts',(21.2775925269652,7.52787386225333,12.));
#253199=CARTESIAN_POINT('Ctrl Pts',(21.2812902781143,7.52901217930408,0.));
#253200=CARTESIAN_POINT('Ctrl Pts',(21.2812902781143,7.52901217930408,12.));
#253201=CARTESIAN_POINT('Ctrl Pts',(21.2853226580657,7.5302356243823,0.));
#253202=CARTESIAN_POINT('Ctrl Pts',(21.2853226580657,7.5302356243823,12.));
#253203=CARTESIAN_POINT('Ctrl Pts',(21.2896816163842,7.53153906987856,0.));
#253204=CARTESIAN_POINT('Ctrl Pts',(21.2896816163842,7.53153906987856,12.));
#253205=CARTESIAN_POINT('Ctrl Pts',(21.2943588989331,7.53291726078527,0.));
#253206=CARTESIAN_POINT('Ctrl Pts',(21.2943588989331,7.53291726078527,12.));
#253207=CARTESIAN_POINT('Ctrl Pts',(21.2993464250717,7.53436505309943,0.));
#253208=CARTESIAN_POINT('Ctrl Pts',(21.2993464250717,7.53436505309943,12.));
#253209=CARTESIAN_POINT('Ctrl Pts',(21.3046368712157,7.53587778251736,0.));
#253210=CARTESIAN_POINT('Ctrl Pts',(21.3046368712157,7.53587778251736,12.));
#253211=CARTESIAN_POINT('Ctrl Pts',(21.310223716773,7.53745129364616,0.));
#253212=CARTESIAN_POINT('Ctrl Pts',(21.310223716773,7.53745129364616,12.));
#253213=CARTESIAN_POINT('Ctrl Pts',(21.3161009456256,7.53908175169899,0.));
#253214=CARTESIAN_POINT('Ctrl Pts',(21.3161009456256,7.53908175169899,12.));
#253215=CARTESIAN_POINT('Ctrl Pts',(21.3222628524165,7.54076552038279,0.));
#253216=CARTESIAN_POINT('Ctrl Pts',(21.3222628524165,7.54076552038279,12.));
#253217=CARTESIAN_POINT('Ctrl Pts',(21.328703791771,7.54249900377031,0.));
#253218=CARTESIAN_POINT('Ctrl Pts',(21.328703791771,7.54249900377031,12.));
#253219=CARTESIAN_POINT('Ctrl Pts',(21.3354182340149,7.54427868151268,0.));
#253220=CARTESIAN_POINT('Ctrl Pts',(21.3354182340149,7.54427868151268,12.));
#253221=CARTESIAN_POINT('Ctrl Pts',(21.3424008295038,7.54610114948347,0.));
#253222=CARTESIAN_POINT('Ctrl Pts',(21.3424008295038,7.54610114948347,12.));
#253223=CARTESIAN_POINT('Ctrl Pts',(21.3496464761531,7.54796316246331,0.));
#253224=CARTESIAN_POINT('Ctrl Pts',(21.3496464761531,7.54796316246331,12.));
#253225=CARTESIAN_POINT('Ctrl Pts',(21.3571503685855,7.5498616652131,0.));
#253226=CARTESIAN_POINT('Ctrl Pts',(21.3571503685855,7.5498616652131,12.));
#253227=CARTESIAN_POINT('Ctrl Pts',(21.3649079431865,7.55179375777444,0.));
#253228=CARTESIAN_POINT('Ctrl Pts',(21.3649079431865,7.55179375777444,12.));
#253229=CARTESIAN_POINT('Ctrl Pts',(21.3729148390243,7.55375667080029,0.));
#253230=CARTESIAN_POINT('Ctrl Pts',(21.3729148390243,7.55375667080029,12.));
#253231=CARTESIAN_POINT('Ctrl Pts',(21.3811668478932,7.55574773403503,0.));
#253232=CARTESIAN_POINT('Ctrl Pts',(21.3811668478932,7.55574773403503,12.));
#253233=CARTESIAN_POINT('Ctrl Pts',(21.3896598842117,7.55776435731417,0.));
#253234=CARTESIAN_POINT('Ctrl Pts',(21.3896598842117,7.55776435731417,12.));
#253235=CARTESIAN_POINT('Ctrl Pts',(21.3983899952987,7.55980403700611,0.));
#253236=CARTESIAN_POINT('Ctrl Pts',(21.3983899952987,7.55980403700611,12.));
#253237=CARTESIAN_POINT('Ctrl Pts',(21.4073533630365,7.56186435703622,0.));
#253238=CARTESIAN_POINT('Ctrl Pts',(21.4073533630365,7.56186435703622,12.));
#253239=CARTESIAN_POINT('Ctrl Pts',(21.4165463106254,7.56394299313685,0.));
#253240=CARTESIAN_POINT('Ctrl Pts',(21.4165463106254,7.56394299313685,12.));
#253241=CARTESIAN_POINT('Ctrl Pts',(21.4259653015736,7.56603771218712,0.));
#253242=CARTESIAN_POINT('Ctrl Pts',(21.4259653015736,7.56603771218712,12.));
#253243=CARTESIAN_POINT('Ctrl Pts',(21.4356069261513,7.56814636360848,0.));
#253244=CARTESIAN_POINT('Ctrl Pts',(21.4356069261513,7.56814636360848,12.));
#253245=CARTESIAN_POINT('Ctrl Pts',(21.4454678907509,7.57026687261166,0.));
#253246=CARTESIAN_POINT('Ctrl Pts',(21.4454678907509,7.57026687261166,12.));
#253247=CARTESIAN_POINT('Ctrl Pts',(21.4555450053142,7.57239723223506,0.));
#253248=CARTESIAN_POINT('Ctrl Pts',(21.4555450053142,7.57239723223506,12.));
#253249=CARTESIAN_POINT('Ctrl Pts',(21.4658351740128,7.57453549743412,0.));
#253250=CARTESIAN_POINT('Ctrl Pts',(21.4658351740128,7.57453549743412,12.));
#253251=CARTESIAN_POINT('Ctrl Pts',(21.4763353936762,7.57667978402987,0.));
#253252=CARTESIAN_POINT('Ctrl Pts',(21.4763353936762,7.57667978402987,12.));
#253253=CARTESIAN_POINT('Ctrl Pts',(21.4870427508194,7.57882826679132,0.));
#253254=CARTESIAN_POINT('Ctrl Pts',(21.4870427508194,7.57882826679132,12.));
#253255=CARTESIAN_POINT('Ctrl Pts',(21.4979544192744,7.58097917790744,0.));
#253256=CARTESIAN_POINT('Ctrl Pts',(21.4979544192744,7.58097917790744,12.));
#253257=CARTESIAN_POINT('Ctrl Pts',(21.5090676573873,7.5831308051918,0.));
#253258=CARTESIAN_POINT('Ctrl Pts',(21.5090676573873,7.5831308051918,12.));
#253259=CARTESIAN_POINT('Ctrl Pts',(21.5203798035299,7.5852814891913,0.));
#253260=CARTESIAN_POINT('Ctrl Pts',(21.5203798035299,7.5852814891913,12.));
#253261=CARTESIAN_POINT('Ctrl Pts',(21.5318882716736,7.58742962034834,0.));
#253262=CARTESIAN_POINT('Ctrl Pts',(21.5318882716736,7.58742962034834,12.));
#253263=CARTESIAN_POINT('Ctrl Pts',(21.543590547011,7.58957363620014,0.));
#253264=CARTESIAN_POINT('Ctrl Pts',(21.543590547011,7.58957363620014,12.));
#253265=CARTESIAN_POINT('Ctrl Pts',(21.5554841813462,7.59171201844777,0.));
#253266=CARTESIAN_POINT('Ctrl Pts',(21.5554841813462,7.59171201844777,12.));
#253267=CARTESIAN_POINT('Ctrl Pts',(21.5675667904726,7.59384329124918,0.));
#253268=CARTESIAN_POINT('Ctrl Pts',(21.5675667904726,7.59384329124918,12.));
#253269=CARTESIAN_POINT('Ctrl Pts',(21.5798360518978,7.59596601973584,0.));
#253270=CARTESIAN_POINT('Ctrl Pts',(21.5798360518978,7.59596601973584,12.));
#253271=CARTESIAN_POINT('Ctrl Pts',(21.5922897024466,7.59807880846195,0.));
#253272=CARTESIAN_POINT('Ctrl Pts',(21.5922897024466,7.59807880846195,12.));
#253273=CARTESIAN_POINT('Ctrl Pts',(21.6049255358843,7.60018029988241,0.));
#253274=CARTESIAN_POINT('Ctrl Pts',(21.6049255358843,7.60018029988241,12.));
#253275=CARTESIAN_POINT('Ctrl Pts',(21.617741400599,7.60226917285429,0.));
#253276=CARTESIAN_POINT('Ctrl Pts',(21.617741400599,7.60226917285429,12.));
#253277=CARTESIAN_POINT('Ctrl Pts',(21.6307351973822,7.60434414118296,0.));
#253278=CARTESIAN_POINT('Ctrl Pts',(21.6307351973822,7.60434414118296,12.));
#253279=CARTESIAN_POINT('Ctrl Pts',(21.6439048771743,7.60640395216357,0.));
#253280=CARTESIAN_POINT('Ctrl Pts',(21.6439048771743,7.60640395216357,12.));
#253281=CARTESIAN_POINT('Ctrl Pts',(21.6572484388081,7.60844738512874,0.));
#253282=CARTESIAN_POINT('Ctrl Pts',(21.6572484388081,7.60844738512874,12.));
#253283=CARTESIAN_POINT('Ctrl Pts',(21.6707639267576,7.61047325000956,0.));
#253284=CARTESIAN_POINT('Ctrl Pts',(21.6707639267576,7.61047325000956,12.));
#253285=CARTESIAN_POINT('Ctrl Pts',(21.6844494295815,7.61248038630269,0.));
#253286=CARTESIAN_POINT('Ctrl Pts',(21.6844494295815,7.61248038630269,12.));
#253287=CARTESIAN_POINT('Ctrl Pts',(21.6983030783322,7.61446766202787,0.));
#253288=CARTESIAN_POINT('Ctrl Pts',(21.6983030783322,7.61446766202787,12.));
#253289=CARTESIAN_POINT('Ctrl Pts',(21.7123230449834,7.61643397270421,0.));
#253290=CARTESIAN_POINT('Ctrl Pts',(21.7123230449834,7.61643397270421,12.));
#253291=CARTESIAN_POINT('Ctrl Pts',(21.7265075407975,7.61837824030538,0.));
#253292=CARTESIAN_POINT('Ctrl Pts',(21.7265075407975,7.61837824030538,12.));
#253293=CARTESIAN_POINT('Ctrl Pts',(21.7408548148656,7.62029941230855,0.));
#253294=CARTESIAN_POINT('Ctrl Pts',(21.7408548148656,7.62029941230855,12.));
#253295=CARTESIAN_POINT('Ctrl Pts',(21.7553631528328,7.62219646084229,0.));
#253296=CARTESIAN_POINT('Ctrl Pts',(21.7553631528328,7.62219646084229,12.));
#253297=CARTESIAN_POINT('Ctrl Pts',(21.7700308755584,7.62406838181166,0.));
#253298=CARTESIAN_POINT('Ctrl Pts',(21.7700308755584,7.62406838181166,12.));
#253299=CARTESIAN_POINT('Ctrl Pts',(21.7848563378021,7.62591419404513,0.));
#253300=CARTESIAN_POINT('Ctrl Pts',(21.7848563378021,7.62591419404513,12.));
#253301=CARTESIAN_POINT('Ctrl Pts',(21.799837926858,7.62773293842389,0.));
#253302=CARTESIAN_POINT('Ctrl Pts',(21.799837926858,7.62773293842389,12.));
#253303=CARTESIAN_POINT('Ctrl Pts',(21.814974061509,7.62952367718127,0.));
#253304=CARTESIAN_POINT('Ctrl Pts',(21.814974061509,7.62952367718127,12.));
#253305=CARTESIAN_POINT('Ctrl Pts',(21.8302631910195,7.63128549323023,0.));
#253306=CARTESIAN_POINT('Ctrl Pts',(21.8302631910195,7.63128549323023,12.));
#253307=CARTESIAN_POINT('Ctrl Pts',(21.8457037941084,7.63301748948936,0.));
#253308=CARTESIAN_POINT('Ctrl Pts',(21.8457037941084,7.63301748948936,12.));
#253309=CARTESIAN_POINT('Ctrl Pts',(21.8612943779089,7.63471878821226,0.));
#253310=CARTESIAN_POINT('Ctrl Pts',(21.8612943779089,7.63471878821226,12.));
#253311=CARTESIAN_POINT('Ctrl Pts',(21.8770334769496,7.636388530334,0.));
#253312=CARTESIAN_POINT('Ctrl Pts',(21.8770334769496,7.636388530334,12.));
#253313=CARTESIAN_POINT('Ctrl Pts',(21.8929196523514,7.63802587492035,0.));
#253314=CARTESIAN_POINT('Ctrl Pts',(21.8929196523514,7.63802587492035,12.));
#253315=CARTESIAN_POINT('Ctrl Pts',(21.9089514909874,7.63962999860927,0.));
#253316=CARTESIAN_POINT('Ctrl Pts',(21.9089514909874,7.63962999860927,12.));
#253317=CARTESIAN_POINT('Ctrl Pts',(21.9251276046545,7.64120009506532,0.));
#253318=CARTESIAN_POINT('Ctrl Pts',(21.9251276046545,7.64120009506532,12.));
#253319=CARTESIAN_POINT('Ctrl Pts',(21.9414466292072,7.64273537442682,0.));
#253320=CARTESIAN_POINT('Ctrl Pts',(21.9414466292072,7.64273537442682,12.));
#253321=CARTESIAN_POINT('Ctrl Pts',(21.9579072237651,7.64423506279123,0.));
#253322=CARTESIAN_POINT('Ctrl Pts',(21.9579072237651,7.64423506279123,12.));
#253323=CARTESIAN_POINT('Ctrl Pts',(21.9745080700798,7.64569840177336,0.));
#253324=CARTESIAN_POINT('Ctrl Pts',(21.9745080700798,7.64569840177336,12.));
#253325=CARTESIAN_POINT('Ctrl Pts',(21.9912478718542,7.6471246480525,0.));
#253326=CARTESIAN_POINT('Ctrl Pts',(21.9912478718542,7.6471246480525,12.));
#253327=CARTESIAN_POINT('Ctrl Pts',(22.0081253540774,7.64851307293352,0.));
#253328=CARTESIAN_POINT('Ctrl Pts',(22.0081253540774,7.64851307293352,12.));
#253329=CARTESIAN_POINT('Ctrl Pts',(22.0251392623209,7.64986296190169,0.));
#253330=CARTESIAN_POINT('Ctrl Pts',(22.0251392623209,7.64986296190169,12.));
#253331=CARTESIAN_POINT('Ctrl Pts',(22.0422883621174,7.65117361421359,0.));
#253332=CARTESIAN_POINT('Ctrl Pts',(22.0422883621174,7.65117361421359,12.));
#253333=CARTESIAN_POINT('Ctrl Pts',(22.0595714384431,7.65244434253113,0.));
#253334=CARTESIAN_POINT('Ctrl Pts',(22.0595714384431,7.65244434253113,12.));
#253335=CARTESIAN_POINT('Ctrl Pts',(22.0769872951596,7.65367447254949,0.));
#253336=CARTESIAN_POINT('Ctrl Pts',(22.0769872951596,7.65367447254949,12.));
#253337=CARTESIAN_POINT('Ctrl Pts',(22.094534754469,7.65486334263644,0.));
#253338=CARTESIAN_POINT('Ctrl Pts',(22.094534754469,7.65486334263644,12.));
#253339=CARTESIAN_POINT('Ctrl Pts',(22.1122126563329,7.65601030346807,0.));
#253340=CARTESIAN_POINT('Ctrl Pts',(22.1122126563329,7.65601030346807,12.));
#253341=CARTESIAN_POINT('Ctrl Pts',(22.1300198579675,7.65711471769397,0.));
#253342=CARTESIAN_POINT('Ctrl Pts',(22.1300198579675,7.65711471769397,12.));
#253343=CARTESIAN_POINT('Ctrl Pts',(22.1479552334211,7.65817595963349,0.));
#253344=CARTESIAN_POINT('Ctrl Pts',(22.1479552334211,7.65817595963349,12.));
#253345=CARTESIAN_POINT('Ctrl Pts',(22.1660176731178,7.65919341496931,0.));
#253346=CARTESIAN_POINT('Ctrl Pts',(22.1660176731178,7.65919341496931,12.));
#253347=CARTESIAN_POINT('Ctrl Pts',(22.1842060834091,7.66016648045005,0.));
#253348=CARTESIAN_POINT('Ctrl Pts',(22.1842060834091,7.66016648045005,12.));
#253349=CARTESIAN_POINT('Ctrl Pts',(22.2025193860964,7.66109456359271,0.));
#253350=CARTESIAN_POINT('Ctrl Pts',(22.2025193860964,7.66109456359271,12.));
#253351=CARTESIAN_POINT('Ctrl Pts',(22.2209565180085,7.661977082404,0.));
#253352=CARTESIAN_POINT('Ctrl Pts',(22.2209565180085,7.661977082404,12.));
#253353=CARTESIAN_POINT('Ctrl Pts',(22.2395164306547,7.66281346512509,0.));
#253354=CARTESIAN_POINT('Ctrl Pts',(22.2395164306547,7.66281346512509,12.));
#253355=CARTESIAN_POINT('Ctrl Pts',(22.258198089848,7.66360314997641,0.));
#253356=CARTESIAN_POINT('Ctrl Pts',(22.258198089848,7.66360314997641,12.));
#253357=CARTESIAN_POINT('Ctrl Pts',(22.2770004753335,7.66434558490979,0.));
#253358=CARTESIAN_POINT('Ctrl Pts',(22.2770004753335,7.66434558490979,12.));
#253359=CARTESIAN_POINT('Ctrl Pts',(22.2959225803937,7.66504022736299,0.));
#253360=CARTESIAN_POINT('Ctrl Pts',(22.2959225803937,7.66504022736299,12.));
#253361=CARTESIAN_POINT('Ctrl Pts',(22.314963411484,7.66568654402494,0.));
#253362=CARTESIAN_POINT('Ctrl Pts',(22.314963411484,7.66568654402494,12.));
#253363=CARTESIAN_POINT('Ctrl Pts',(22.3341219879469,7.66628401061952,0.));
#253364=CARTESIAN_POINT('Ctrl Pts',(22.3341219879469,7.66628401061952,12.));
#253365=CARTESIAN_POINT('Ctrl Pts',(22.3533973417021,7.66683211169159,0.));
#253366=CARTESIAN_POINT('Ctrl Pts',(22.3533973417021,7.66683211169159,12.));
#253367=CARTESIAN_POINT('Ctrl Pts',(22.372788516936,7.66733034039883,0.));
#253368=CARTESIAN_POINT('Ctrl Pts',(22.372788516936,7.66733034039883,12.));
#253369=CARTESIAN_POINT('Ctrl Pts',(22.3922945697773,7.6677781983079,0.));
#253370=CARTESIAN_POINT('Ctrl Pts',(22.3922945697773,7.6677781983079,12.));
#253371=CARTESIAN_POINT('Ctrl Pts',(22.4119145679758,7.6681751951964,0.));
#253372=CARTESIAN_POINT('Ctrl Pts',(22.4119145679758,7.6681751951964,12.));
#253373=CARTESIAN_POINT('Ctrl Pts',(22.4316475906603,7.66852084886704,0.));
#253374=CARTESIAN_POINT('Ctrl Pts',(22.4316475906603,7.66852084886704,12.));
#253375=CARTESIAN_POINT('Ctrl Pts',(22.4514927280855,7.66881468496635,0.));
#253376=CARTESIAN_POINT('Ctrl Pts',(22.4514927280855,7.66881468496635,12.));
#253377=CARTESIAN_POINT('Ctrl Pts',(22.4714490813699,7.66905623680831,0.));
#253378=CARTESIAN_POINT('Ctrl Pts',(22.4714490813699,7.66905623680831,12.));
#253379=CARTESIAN_POINT('Ctrl Pts',(22.4915157622312,7.66924504520315,0.));
#253380=CARTESIAN_POINT('Ctrl Pts',(22.4915157622312,7.66924504520315,12.));
#253381=CARTESIAN_POINT('Ctrl Pts',(22.5116918927031,7.66938065829108,0.));
#253382=CARTESIAN_POINT('Ctrl Pts',(22.5116918927031,7.66938065829108,12.));
#253383=CARTESIAN_POINT('Ctrl Pts',(22.53197660492,7.66946263138144,0.));
#253384=CARTESIAN_POINT('Ctrl Pts',(22.53197660492,7.66946263138144,12.));
#253385=CARTESIAN_POINT('Ctrl Pts',(22.5523690409116,7.66949052679693,0.));
#253386=CARTESIAN_POINT('Ctrl Pts',(22.5523690409116,7.66949052679693,12.));
#253387=CARTESIAN_POINT('Ctrl Pts',(22.5728683523831,7.66946391372306,0.));
#253388=CARTESIAN_POINT('Ctrl Pts',(22.5728683523831,7.66946391372306,12.));
#253389=CARTESIAN_POINT('Ctrl Pts',(22.5934737004953,7.66938236806233,0.));
#253390=CARTESIAN_POINT('Ctrl Pts',(22.5934737004953,7.66938236806233,12.));
#253391=CARTESIAN_POINT('Ctrl Pts',(22.6141842556243,7.66924547229414,0.));
#253392=CARTESIAN_POINT('Ctrl Pts',(22.6141842556243,7.66924547229414,12.));
#253393=CARTESIAN_POINT('Ctrl Pts',(22.6349991971541,7.66905281533715,0.));
#253394=CARTESIAN_POINT('Ctrl Pts',(22.6349991971541,7.66905281533715,12.));
#253395=CARTESIAN_POINT('Ctrl Pts',(22.6559177133127,7.66880399241323,0.));
#253396=CARTESIAN_POINT('Ctrl Pts',(22.6559177133127,7.66880399241323,12.));
#253397=CARTESIAN_POINT('Ctrl Pts',(22.6769390009885,7.66849860491743,0.));
#253398=CARTESIAN_POINT('Ctrl Pts',(22.6769390009885,7.66849860491743,12.));
#253399=CARTESIAN_POINT('Ctrl Pts',(22.6980622655446,7.66813626029275,0.));
#253400=CARTESIAN_POINT('Ctrl Pts',(22.6980622655446,7.66813626029275,12.));
#253401=CARTESIAN_POINT('Ctrl Pts',(22.7192867206245,7.66771657191028,0.));
#253402=CARTESIAN_POINT('Ctrl Pts',(22.7192867206245,7.66771657191028,12.));
#253403=CARTESIAN_POINT('Ctrl Pts',(22.7406115879513,7.6672391589544,0.));
#253404=CARTESIAN_POINT('Ctrl Pts',(22.7406115879513,7.6672391589544,12.));
#253405=CARTESIAN_POINT('Ctrl Pts',(22.7620360971843,7.66670364630299,0.));
#253406=CARTESIAN_POINT('Ctrl Pts',(22.7620360971843,7.66670364630299,12.));
#253407=CARTESIAN_POINT('Ctrl Pts',(22.7835594857699,7.66610966441273,0.));
#253408=CARTESIAN_POINT('Ctrl Pts',(22.7835594857699,7.66610966441273,12.));
#253409=CARTESIAN_POINT('Ctrl Pts',(22.8051809987833,7.66545684920987,0.));
#253410=CARTESIAN_POINT('Ctrl Pts',(22.8051809987833,7.66545684920987,12.));
#253411=CARTESIAN_POINT('Ctrl Pts',(22.8268998887678,7.66474484198549,0.));
#253412=CARTESIAN_POINT('Ctrl Pts',(22.8268998887678,7.66474484198549,12.));
#253413=CARTESIAN_POINT('Ctrl Pts',(22.848715415557,7.66397328929803,0.));
#253414=CARTESIAN_POINT('Ctrl Pts',(22.848715415557,7.66397328929803,12.));
#253415=CARTESIAN_POINT('Ctrl Pts',(22.8706268461283,7.66314184287337,0.));
#253416=CARTESIAN_POINT('Ctrl Pts',(22.8706268461283,7.66314184287337,12.));
#253417=CARTESIAN_POINT('Ctrl Pts',(22.8926334544883,7.66225015950156,0.));
#253418=CARTESIAN_POINT('Ctrl Pts',(22.8926334544883,7.66225015950156,12.));
#253419=CARTESIAN_POINT('Ctrl Pts',(22.9147345215421,7.66129790094108,0.));
#253420=CARTESIAN_POINT('Ctrl Pts',(22.9147345215421,7.66129790094108,12.));
#253421=CARTESIAN_POINT('Ctrl Pts',(22.9369293349593,7.66028473382778,0.));
#253422=CARTESIAN_POINT('Ctrl Pts',(22.9369293349593,7.66028473382778,12.));
#253423=CARTESIAN_POINT('Ctrl Pts',(22.959217189033,7.65921032958902,0.));
#253424=CARTESIAN_POINT('Ctrl Pts',(22.959217189033,7.65921032958902,12.));
#253425=CARTESIAN_POINT('Ctrl Pts',(22.9815973845296,7.65807436436432,0.));
#253426=CARTESIAN_POINT('Ctrl Pts',(22.9815973845296,7.65807436436432,12.));
#253427=CARTESIAN_POINT('Ctrl Pts',(23.0040692285814,7.65687651891305,0.));
#253428=CARTESIAN_POINT('Ctrl Pts',(23.0040692285814,7.65687651891305,12.));
#253429=CARTESIAN_POINT('Ctrl Pts',(23.0266320345787,7.65561647852534,0.));
#253430=CARTESIAN_POINT('Ctrl Pts',(23.0266320345787,7.65561647852534,12.));
#253431=CARTESIAN_POINT('Ctrl Pts',(23.0492851220528,7.65429393293946,0.));
#253432=CARTESIAN_POINT('Ctrl Pts',(23.0492851220528,7.65429393293946,12.));
#253433=CARTESIAN_POINT('Ctrl Pts',(23.072027816555,7.65290857626358,0.));
#253434=CARTESIAN_POINT('Ctrl Pts',(23.072027816555,7.65290857626358,12.));
#253435=CARTESIAN_POINT('Ctrl Pts',(23.094859449525,7.65146010690476,0.));
#253436=CARTESIAN_POINT('Ctrl Pts',(23.094859449525,7.65146010690476,12.));
#253437=CARTESIAN_POINT('Ctrl Pts',(23.1177793581679,7.6499482274986,0.));
#253438=CARTESIAN_POINT('Ctrl Pts',(23.1177793581679,7.6499482274986,12.));
#253439=CARTESIAN_POINT('Ctrl Pts',(23.1407868853819,7.64837264482943,0.));
#253440=CARTESIAN_POINT('Ctrl Pts',(23.1407868853819,7.64837264482943,12.));
#253441=CARTESIAN_POINT('Ctrl Pts',(23.1638813796694,7.64673306975805,0.));
#253442=CARTESIAN_POINT('Ctrl Pts',(23.1638813796694,7.64673306975805,12.));
#253443=CARTESIAN_POINT('Ctrl Pts',(23.1870621950452,7.64502921715483,0.));
#253444=CARTESIAN_POINT('Ctrl Pts',(23.1870621950452,7.64502921715483,12.));
#253445=CARTESIAN_POINT('Ctrl Pts',(23.2103286909398,7.6432608058368,0.));
#253446=CARTESIAN_POINT('Ctrl Pts',(23.2103286909398,7.6432608058368,12.));
#253447=CARTESIAN_POINT('Ctrl Pts',(23.2336802320912,7.64142755851505,0.));
#253448=CARTESIAN_POINT('Ctrl Pts',(23.2336802320912,7.64142755851505,12.));
#253449=CARTESIAN_POINT('Ctrl Pts',(23.2571161884488,7.63952920172835,0.));
#253450=CARTESIAN_POINT('Ctrl Pts',(23.2571161884488,7.63952920172835,12.));
#253451=CARTESIAN_POINT('Ctrl Pts',(23.2806359350855,7.63756546576374,0.));
#253452=CARTESIAN_POINT('Ctrl Pts',(23.2806359350855,7.63756546576374,12.));
#253453=CARTESIAN_POINT('Ctrl Pts',(23.3042388521022,7.63553608458783,0.));
#253454=CARTESIAN_POINT('Ctrl Pts',(23.3042388521022,7.63553608458783,12.));
#253455=CARTESIAN_POINT('Ctrl Pts',(23.3279243245241,7.63344079578162,0.));
#253456=CARTESIAN_POINT('Ctrl Pts',(23.3279243245241,7.63344079578162,12.));
#253457=CARTESIAN_POINT('Ctrl Pts',(23.3516917421972,7.63127934048137,0.));
#253458=CARTESIAN_POINT('Ctrl Pts',(23.3516917421972,7.63127934048137,12.));
#253459=CARTESIAN_POINT('Ctrl Pts',(23.3755404996636,7.62905146332593,0.));
#253460=CARTESIAN_POINT('Ctrl Pts',(23.3755404996636,7.62905146332593,12.));
#253461=CARTESIAN_POINT('Ctrl Pts',(23.399469996112,7.62675691240329,0.));
#253462=CARTESIAN_POINT('Ctrl Pts',(23.399469996112,7.62675691240329,12.));
#253463=CARTESIAN_POINT('Ctrl Pts',(23.4234796353542,7.6243954392005,0.));
#253464=CARTESIAN_POINT('Ctrl Pts',(23.4234796353542,7.6243954392005,12.));
#253465=CARTESIAN_POINT('Ctrl Pts',(23.4475688257854,7.62196679855955,0.));
#253466=CARTESIAN_POINT('Ctrl Pts',(23.4475688257854,7.62196679855955,12.));
#253467=CARTESIAN_POINT('Ctrl Pts',(23.4717369803438,7.61947074863977,0.));
#253468=CARTESIAN_POINT('Ctrl Pts',(23.4717369803438,7.61947074863977,12.));
#253469=CARTESIAN_POINT('Ctrl Pts',(23.4959835164609,7.61690705088319,0.));
#253470=CARTESIAN_POINT('Ctrl Pts',(23.4959835164609,7.61690705088319,12.));
#253471=CARTESIAN_POINT('Ctrl Pts',(23.5203078560129,7.61427546999298,0.));
#253472=CARTESIAN_POINT('Ctrl Pts',(23.5203078560129,7.61427546999298,12.));
#253473=CARTESIAN_POINT('Ctrl Pts',(23.544709425203,7.61157577385372,0.));
#253474=CARTESIAN_POINT('Ctrl Pts',(23.544709425203,7.61157577385372,12.));
#253475=CARTESIAN_POINT('Ctrl Pts',(23.5691876544244,7.608807733446,0.));
#253476=CARTESIAN_POINT('Ctrl Pts',(23.5691876544244,7.608807733446,12.));
#253477=CARTESIAN_POINT('Ctrl Pts',(23.5937419781245,7.60597112277094,0.));
#253478=CARTESIAN_POINT('Ctrl Pts',(23.5937419781245,7.60597112277094,12.));
#253479=CARTESIAN_POINT('Ctrl Pts',(23.6183718346576,7.60306571877806,0.));
#253480=CARTESIAN_POINT('Ctrl Pts',(23.6183718346576,7.60306571877806,12.));
#253481=CARTESIAN_POINT('Ctrl Pts',(23.6430766661418,7.60009130130126,0.));
#253482=CARTESIAN_POINT('Ctrl Pts',(23.6430766661418,7.60009130130126,12.));
#253483=CARTESIAN_POINT('Ctrl Pts',(23.6678559182875,7.59704765299567,0.));
#253484=CARTESIAN_POINT('Ctrl Pts',(23.6678559182875,7.59704765299567,12.));
#253485=CARTESIAN_POINT('Ctrl Pts',(23.6927090405066,7.59393455934035,0.));
#253486=CARTESIAN_POINT('Ctrl Pts',(23.6927090405066,7.59393455934035,12.));
#253487=CARTESIAN_POINT('Ctrl Pts',(23.7176354860456,7.59075180865321,0.));
#253488=CARTESIAN_POINT('Ctrl Pts',(23.7176354860456,7.59075180865321,12.));
#253489=CARTESIAN_POINT('Ctrl Pts',(23.7426347121006,7.58749919210826,0.));
#253490=CARTESIAN_POINT('Ctrl Pts',(23.7426347121006,7.58749919210826,12.));
#253491=CARTESIAN_POINT('Ctrl Pts',(23.7677061799376,7.58417650376271,0.));
#253492=CARTESIAN_POINT('Ctrl Pts',(23.7677061799376,7.58417650376271,12.));
#253493=CARTESIAN_POINT('Ctrl Pts',(23.7928493549908,7.58078354058213,0.));
#253494=CARTESIAN_POINT('Ctrl Pts',(23.7928493549908,7.58078354058213,12.));
#253495=CARTESIAN_POINT('Ctrl Pts',(23.8180637069976,7.57732010249066,0.));
#253496=CARTESIAN_POINT('Ctrl Pts',(23.8180637069976,7.57732010249066,12.));
#253497=CARTESIAN_POINT('Ctrl Pts',(23.8433487096132,7.57378599219814,0.));
#253498=CARTESIAN_POINT('Ctrl Pts',(23.8433487096132,7.57378599219814,12.));
#253499=CARTESIAN_POINT('Ctrl Pts',(23.8687038399595,7.57018101500709,0.));
#253500=CARTESIAN_POINT('Ctrl Pts',(23.8687038399595,7.57018101500709,12.));
#253501=CARTESIAN_POINT('Ctrl Pts',(23.8941285782002,7.56650497863791,0.));
#253502=CARTESIAN_POINT('Ctrl Pts',(23.8941285782002,7.56650497863791,12.));
#253503=CARTESIAN_POINT('Ctrl Pts',(23.9196224070759,7.56275769304773,0.));
#253504=CARTESIAN_POINT('Ctrl Pts',(23.9196224070759,7.56275769304773,12.));
#253505=CARTESIAN_POINT('Ctrl Pts',(23.9451848115002,7.5589389702768,0.));
#253506=CARTESIAN_POINT('Ctrl Pts',(23.9451848115002,7.5589389702768,12.));
#253507=CARTESIAN_POINT('Ctrl Pts',(23.9708152779886,7.55504862424808,0.));
#253508=CARTESIAN_POINT('Ctrl Pts',(23.9708152779886,7.55504862424808,12.));
#253509=CARTESIAN_POINT('Ctrl Pts',(23.9965132953187,7.55108647097432,0.));
#253510=CARTESIAN_POINT('Ctrl Pts',(23.9965132953187,7.55108647097432,12.));
#253511=CARTESIAN_POINT('Ctrl Pts',(24.0222783554531,7.54705232885895,0.));
#253512=CARTESIAN_POINT('Ctrl Pts',(24.0222783554531,7.54705232885895,12.));
#253513=CARTESIAN_POINT('Ctrl Pts',(24.0481099543353,7.54294601896128,0.));
#253514=CARTESIAN_POINT('Ctrl Pts',(24.0481099543353,7.54294601896128,12.));
#253515=CARTESIAN_POINT('Ctrl Pts',(24.0740075927984,7.53876736531005,0.));
#253516=CARTESIAN_POINT('Ctrl Pts',(24.0740075927984,7.53876736531005,12.));
#253517=CARTESIAN_POINT('Ctrl Pts',(24.0999707772642,7.53451619514659,0.));
#253518=CARTESIAN_POINT('Ctrl Pts',(24.0999707772642,7.53451619514659,12.));
#253519=CARTESIAN_POINT('Ctrl Pts',(24.1259990209211,7.53019233935537,0.));
#253520=CARTESIAN_POINT('Ctrl Pts',(24.1259990209211,7.53019233935537,12.));
#253521=CARTESIAN_POINT('Ctrl Pts',(24.152091842537,7.52579563201479,0.));
#253522=CARTESIAN_POINT('Ctrl Pts',(24.152091842537,7.52579563201479,12.));
#253523=CARTESIAN_POINT('Ctrl Pts',(24.1782487641602,7.52132590953863,0.));
#253524=CARTESIAN_POINT('Ctrl Pts',(24.1782487641602,7.52132590953863,12.));
#253525=CARTESIAN_POINT('Ctrl Pts',(24.2044693092356,7.51678300997998,0.));
#253526=CARTESIAN_POINT('Ctrl Pts',(24.2044693092356,7.51678300997998,12.));
#253527=CARTESIAN_POINT('Ctrl Pts',(24.230753000389,7.51216677222199,0.));
#253528=CARTESIAN_POINT('Ctrl Pts',(24.230753000389,7.51216677222199,12.));
#253529=CARTESIAN_POINT('Ctrl Pts',(24.2570993577032,7.50747703535115,0.));
#253530=CARTESIAN_POINT('Ctrl Pts',(24.2570993577032,7.50747703535115,12.));
#253531=CARTESIAN_POINT('Ctrl Pts',(24.2835078958966,7.50271363765099,0.));
#253532=CARTESIAN_POINT('Ctrl Pts',(24.2835078958966,7.50271363765099,12.));
#253533=CARTESIAN_POINT('Ctrl Pts',(24.3099781253345,7.49787641695359,0.));
#253534=CARTESIAN_POINT('Ctrl Pts',(24.3099781253345,7.49787641695359,12.));
#253535=CARTESIAN_POINT('Ctrl Pts',(24.3365095573673,7.4929652125233,0.));
#253536=CARTESIAN_POINT('Ctrl Pts',(24.3365095573673,7.4929652125233,12.));
#253537=CARTESIAN_POINT('Ctrl Pts',(24.3631017084513,7.48797986651828,0.));
#253538=CARTESIAN_POINT('Ctrl Pts',(24.3631017084513,7.48797986651828,12.));
#253539=CARTESIAN_POINT('Ctrl Pts',(24.3897541049248,7.48292022569254,0.));
#253540=CARTESIAN_POINT('Ctrl Pts',(24.3897541049248,7.48292022569254,12.));
#253541=CARTESIAN_POINT('Ctrl Pts',(24.4164662871165,7.47778614286574,0.));
#253542=CARTESIAN_POINT('Ctrl Pts',(24.4164662871165,7.47778614286574,12.));
#253543=CARTESIAN_POINT('Ctrl Pts',(24.4432378146501,7.47257747883319,0.));
#253544=CARTESIAN_POINT('Ctrl Pts',(24.4432378146501,7.47257747883319,12.));
#253545=CARTESIAN_POINT('Ctrl Pts',(24.4700682684544,7.46729410308923,0.));
#253546=CARTESIAN_POINT('Ctrl Pts',(24.4700682684544,7.46729410308923,12.));
#253547=CARTESIAN_POINT('Ctrl Pts',(24.4969572391509,7.46193588961642,0.));
#253548=CARTESIAN_POINT('Ctrl Pts',(24.4969572391509,7.46193588961642,12.));
#253549=CARTESIAN_POINT('Ctrl Pts',(24.52390431731,7.45650271336046,0.));
#253550=CARTESIAN_POINT('Ctrl Pts',(24.52390431731,7.45650271336046,12.));
#253551=CARTESIAN_POINT('Ctrl Pts',(24.5509090831579,7.45099444651296,0.));
#253552=CARTESIAN_POINT('Ctrl Pts',(24.5509090831579,7.45099444651296,12.));
#253553=CARTESIAN_POINT('Ctrl Pts',(24.5779710960865,7.44541095473163,0.));
#253554=CARTESIAN_POINT('Ctrl Pts',(24.5779710960865,7.44541095473163,12.));
#253555=CARTESIAN_POINT('Ctrl Pts',(24.6050898852349,7.43975209375375,0.));
#253556=CARTESIAN_POINT('Ctrl Pts',(24.6050898852349,7.43975209375375,12.));
#253557=CARTESIAN_POINT('Ctrl Pts',(24.6322649369472,7.43401770489221,0.));
#253558=CARTESIAN_POINT('Ctrl Pts',(24.6322649369472,7.43401770489221,12.));
#253559=CARTESIAN_POINT('Ctrl Pts',(24.659495712869,7.42820762158681,0.));
#253560=CARTESIAN_POINT('Ctrl Pts',(24.659495712869,7.42820762158681,12.));
#253561=CARTESIAN_POINT('Ctrl Pts',(24.6867816727118,7.42232167765763,0.));
#253562=CARTESIAN_POINT('Ctrl Pts',(24.6867816727118,7.42232167765763,12.));
#253563=CARTESIAN_POINT('Ctrl Pts',(24.7141222949988,7.41635971481243,0.));
#253564=CARTESIAN_POINT('Ctrl Pts',(24.7141222949988,7.41635971481243,12.));
#253565=CARTESIAN_POINT('Ctrl Pts',(24.7415170994754,7.41032159082173,0.));
#253566=CARTESIAN_POINT('Ctrl Pts',(24.7415170994754,7.41032159082173,12.));
#253567=CARTESIAN_POINT('Ctrl Pts',(24.7689656669005,7.40420718661755,0.));
#253568=CARTESIAN_POINT('Ctrl Pts',(24.7689656669005,7.40420718661755,12.));
#253569=CARTESIAN_POINT('Ctrl Pts',(24.7964676646518,7.39801641583613,0.));
#253570=CARTESIAN_POINT('Ctrl Pts',(24.7964676646518,7.39801641583613,12.));
#253571=CARTESIAN_POINT('Ctrl Pts',(24.8240228521042,7.39174922586841,0.));
#253572=CARTESIAN_POINT('Ctrl Pts',(24.8240228521042,7.39174922586841,12.));
#253573=CARTESIAN_POINT('Ctrl Pts',(24.8516310625367,7.38540558904946,0.));
#253574=CARTESIAN_POINT('Ctrl Pts',(24.8516310625367,7.38540558904946,12.));
#253575=CARTESIAN_POINT('Ctrl Pts',(24.8792921911309,7.3789854964161,0.));
#253576=CARTESIAN_POINT('Ctrl Pts',(24.8792921911309,7.3789854964161,12.));
#253577=CARTESIAN_POINT('Ctrl Pts',(24.9014633826201,7.37378825962718,0.));
#253578=CARTESIAN_POINT('Ctrl Pts',(24.9014633826201,7.37378825962718,12.));
#253579=CARTESIAN_POINT('Ctrl Pts',(24.9181155530631,7.36985593120697,0.));
#253580=CARTESIAN_POINT('Ctrl Pts',(24.9181155530631,7.36985593120697,12.));
#253581=CARTESIAN_POINT('Ctrl Pts',(24.9292275670705,7.3672190902906,0.));
#253582=CARTESIAN_POINT('Ctrl Pts',(24.9292275670705,7.3672190902906,12.));
#253583=CARTESIAN_POINT('Ctrl Pts',(24.9347862158358,7.36589684767344,0.));
#253584=CARTESIAN_POINT('Ctrl Pts',(24.9347862158358,7.36589684767344,12.));
#253585=CARTESIAN_POINT('',(24.9347862158358,7.36589684767344,0.));
#253586=CARTESIAN_POINT('Ctrl Pts',(21.2610617890679,7.52250298901264,0.));
#253587=CARTESIAN_POINT('Ctrl Pts',(21.2610673466886,7.5225064970397,0.));
#253588=CARTESIAN_POINT('Ctrl Pts',(21.2611204474866,7.52252744144904,0.));
#253589=CARTESIAN_POINT('Ctrl Pts',(21.261326054066,7.52260064231661,0.));
#253590=CARTESIAN_POINT('Ctrl Pts',(21.2618521283555,7.5227818224267,0.));
#253591=CARTESIAN_POINT('Ctrl Pts',(21.262927782038,7.52314642316199,0.));
#253592=CARTESIAN_POINT('Ctrl Pts',(21.2644161259962,7.52364573027553,0.));
#253593=CARTESIAN_POINT('Ctrl Pts',(21.2663059157058,7.52427261074298,0.));
#253594=CARTESIAN_POINT('Ctrl Pts',(21.2685823838671,7.52501770333531,0.));
#253595=CARTESIAN_POINT('Ctrl Pts',(21.2712301573466,7.5258712609553,0.));
#253596=CARTESIAN_POINT('Ctrl Pts',(21.2742366113579,7.52682526918541,0.));
#253597=CARTESIAN_POINT('Ctrl Pts',(21.2775925269652,7.52787386225333,0.));
#253598=CARTESIAN_POINT('Ctrl Pts',(21.2812902781143,7.52901217930408,0.));
#253599=CARTESIAN_POINT('Ctrl Pts',(21.2853226580657,7.5302356243823,0.));
#253600=CARTESIAN_POINT('Ctrl Pts',(21.2896816163842,7.53153906987856,0.));
#253601=CARTESIAN_POINT('Ctrl Pts',(21.2943588989331,7.53291726078527,0.));
#253602=CARTESIAN_POINT('Ctrl Pts',(21.2993464250717,7.53436505309943,0.));
#253603=CARTESIAN_POINT('Ctrl Pts',(21.3046368712157,7.53587778251736,0.));
#253604=CARTESIAN_POINT('Ctrl Pts',(21.310223716773,7.53745129364616,0.));
#253605=CARTESIAN_POINT('Ctrl Pts',(21.3161009456256,7.53908175169899,0.));
#253606=CARTESIAN_POINT('Ctrl Pts',(21.3222628524165,7.54076552038279,0.));
#253607=CARTESIAN_POINT('Ctrl Pts',(21.328703791771,7.54249900377031,0.));
#253608=CARTESIAN_POINT('Ctrl Pts',(21.3354182340149,7.54427868151268,0.));
#253609=CARTESIAN_POINT('Ctrl Pts',(21.3424008295038,7.54610114948347,0.));
#253610=CARTESIAN_POINT('Ctrl Pts',(21.3496464761531,7.54796316246331,0.));
#253611=CARTESIAN_POINT('Ctrl Pts',(21.3571503685855,7.5498616652131,0.));
#253612=CARTESIAN_POINT('Ctrl Pts',(21.3649079431865,7.55179375777444,0.));
#253613=CARTESIAN_POINT('Ctrl Pts',(21.3729148390243,7.55375667080029,0.));
#253614=CARTESIAN_POINT('Ctrl Pts',(21.3811668478932,7.55574773403503,0.));
#253615=CARTESIAN_POINT('Ctrl Pts',(21.3896598842117,7.55776435731417,0.));
#253616=CARTESIAN_POINT('Ctrl Pts',(21.3983899952987,7.55980403700611,0.));
#253617=CARTESIAN_POINT('Ctrl Pts',(21.4073533630365,7.56186435703622,0.));
#253618=CARTESIAN_POINT('Ctrl Pts',(21.4165463106254,7.56394299313685,0.));
#253619=CARTESIAN_POINT('Ctrl Pts',(21.4259653015736,7.56603771218712,0.));
#253620=CARTESIAN_POINT('Ctrl Pts',(21.4356069261513,7.56814636360848,0.));
#253621=CARTESIAN_POINT('Ctrl Pts',(21.4454678907509,7.57026687261166,0.));
#253622=CARTESIAN_POINT('Ctrl Pts',(21.4555450053142,7.57239723223506,0.));
#253623=CARTESIAN_POINT('Ctrl Pts',(21.4658351740128,7.57453549743412,0.));
#253624=CARTESIAN_POINT('Ctrl Pts',(21.4763353936762,7.57667978402987,0.));
#253625=CARTESIAN_POINT('Ctrl Pts',(21.4870427508194,7.57882826679132,0.));
#253626=CARTESIAN_POINT('Ctrl Pts',(21.4979544192744,7.58097917790744,0.));
#253627=CARTESIAN_POINT('Ctrl Pts',(21.5090676573873,7.5831308051918,0.));
#253628=CARTESIAN_POINT('Ctrl Pts',(21.5203798035299,7.5852814891913,0.));
#253629=CARTESIAN_POINT('Ctrl Pts',(21.5318882716736,7.58742962034834,0.));
#253630=CARTESIAN_POINT('Ctrl Pts',(21.543590547011,7.58957363620014,0.));
#253631=CARTESIAN_POINT('Ctrl Pts',(21.5554841813462,7.59171201844777,0.));
#253632=CARTESIAN_POINT('Ctrl Pts',(21.5675667904726,7.59384329124918,0.));
#253633=CARTESIAN_POINT('Ctrl Pts',(21.5798360518978,7.59596601973584,0.));
#253634=CARTESIAN_POINT('Ctrl Pts',(21.5922897024466,7.59807880846195,0.));
#253635=CARTESIAN_POINT('Ctrl Pts',(21.6049255358843,7.60018029988241,0.));
#253636=CARTESIAN_POINT('Ctrl Pts',(21.617741400599,7.60226917285429,0.));
#253637=CARTESIAN_POINT('Ctrl Pts',(21.6307351973822,7.60434414118296,0.));
#253638=CARTESIAN_POINT('Ctrl Pts',(21.6439048771743,7.60640395216357,0.));
#253639=CARTESIAN_POINT('Ctrl Pts',(21.6572484388081,7.60844738512874,0.));
#253640=CARTESIAN_POINT('Ctrl Pts',(21.6707639267576,7.61047325000956,0.));
#253641=CARTESIAN_POINT('Ctrl Pts',(21.6844494295815,7.61248038630269,0.));
#253642=CARTESIAN_POINT('Ctrl Pts',(21.6983030783322,7.61446766202787,0.));
#253643=CARTESIAN_POINT('Ctrl Pts',(21.7123230449834,7.61643397270421,0.));
#253644=CARTESIAN_POINT('Ctrl Pts',(21.7265075407975,7.61837824030538,0.));
#253645=CARTESIAN_POINT('Ctrl Pts',(21.7408548148656,7.62029941230855,0.));
#253646=CARTESIAN_POINT('Ctrl Pts',(21.7553631528328,7.62219646084229,0.));
#253647=CARTESIAN_POINT('Ctrl Pts',(21.7700308755584,7.62406838181166,0.));
#253648=CARTESIAN_POINT('Ctrl Pts',(21.7848563378021,7.62591419404513,0.));
#253649=CARTESIAN_POINT('Ctrl Pts',(21.799837926858,7.62773293842389,0.));
#253650=CARTESIAN_POINT('Ctrl Pts',(21.814974061509,7.62952367718127,0.));
#253651=CARTESIAN_POINT('Ctrl Pts',(21.8302631910195,7.63128549323023,0.));
#253652=CARTESIAN_POINT('Ctrl Pts',(21.8457037941084,7.63301748948936,0.));
#253653=CARTESIAN_POINT('Ctrl Pts',(21.8612943779089,7.63471878821226,0.));
#253654=CARTESIAN_POINT('Ctrl Pts',(21.8770334769496,7.636388530334,0.));
#253655=CARTESIAN_POINT('Ctrl Pts',(21.8929196523514,7.63802587492035,0.));
#253656=CARTESIAN_POINT('Ctrl Pts',(21.9089514909874,7.63962999860927,0.));
#253657=CARTESIAN_POINT('Ctrl Pts',(21.9251276046545,7.64120009506532,0.));
#253658=CARTESIAN_POINT('Ctrl Pts',(21.9414466292072,7.64273537442682,0.));
#253659=CARTESIAN_POINT('Ctrl Pts',(21.9579072237651,7.64423506279123,0.));
#253660=CARTESIAN_POINT('Ctrl Pts',(21.9745080700798,7.64569840177336,0.));
#253661=CARTESIAN_POINT('Ctrl Pts',(21.9912478718542,7.6471246480525,0.));
#253662=CARTESIAN_POINT('Ctrl Pts',(22.0081253540774,7.64851307293352,0.));
#253663=CARTESIAN_POINT('Ctrl Pts',(22.0251392623209,7.64986296190169,0.));
#253664=CARTESIAN_POINT('Ctrl Pts',(22.0422883621174,7.65117361421359,0.));
#253665=CARTESIAN_POINT('Ctrl Pts',(22.0595714384431,7.65244434253113,0.));
#253666=CARTESIAN_POINT('Ctrl Pts',(22.0769872951596,7.65367447254949,0.));
#253667=CARTESIAN_POINT('Ctrl Pts',(22.094534754469,7.65486334263644,0.));
#253668=CARTESIAN_POINT('Ctrl Pts',(22.1122126563329,7.65601030346807,0.));
#253669=CARTESIAN_POINT('Ctrl Pts',(22.1300198579675,7.65711471769397,0.));
#253670=CARTESIAN_POINT('Ctrl Pts',(22.1479552334211,7.65817595963349,0.));
#253671=CARTESIAN_POINT('Ctrl Pts',(22.1660176731178,7.65919341496931,0.));
#253672=CARTESIAN_POINT('Ctrl Pts',(22.1842060834091,7.66016648045005,0.));
#253673=CARTESIAN_POINT('Ctrl Pts',(22.2025193860964,7.66109456359271,0.));
#253674=CARTESIAN_POINT('Ctrl Pts',(22.2209565180085,7.661977082404,0.));
#253675=CARTESIAN_POINT('Ctrl Pts',(22.2395164306547,7.66281346512509,0.));
#253676=CARTESIAN_POINT('Ctrl Pts',(22.258198089848,7.66360314997641,0.));
#253677=CARTESIAN_POINT('Ctrl Pts',(22.2770004753335,7.66434558490979,0.));
#253678=CARTESIAN_POINT('Ctrl Pts',(22.2959225803937,7.66504022736299,0.));
#253679=CARTESIAN_POINT('Ctrl Pts',(22.314963411484,7.66568654402494,0.));
#253680=CARTESIAN_POINT('Ctrl Pts',(22.3341219879469,7.66628401061952,0.));
#253681=CARTESIAN_POINT('Ctrl Pts',(22.3533973417021,7.66683211169159,0.));
#253682=CARTESIAN_POINT('Ctrl Pts',(22.372788516936,7.66733034039883,0.));
#253683=CARTESIAN_POINT('Ctrl Pts',(22.3922945697773,7.6677781983079,0.));
#253684=CARTESIAN_POINT('Ctrl Pts',(22.4119145679758,7.6681751951964,0.));
#253685=CARTESIAN_POINT('Ctrl Pts',(22.4316475906603,7.66852084886704,0.));
#253686=CARTESIAN_POINT('Ctrl Pts',(22.4514927280855,7.66881468496635,0.));
#253687=CARTESIAN_POINT('Ctrl Pts',(22.4714490813699,7.66905623680831,0.));
#253688=CARTESIAN_POINT('Ctrl Pts',(22.4915157622312,7.66924504520315,0.));
#253689=CARTESIAN_POINT('Ctrl Pts',(22.5116918927031,7.66938065829108,0.));
#253690=CARTESIAN_POINT('Ctrl Pts',(22.53197660492,7.66946263138144,0.));
#253691=CARTESIAN_POINT('Ctrl Pts',(22.5523690409116,7.66949052679693,0.));
#253692=CARTESIAN_POINT('Ctrl Pts',(22.5728683523831,7.66946391372306,0.));
#253693=CARTESIAN_POINT('Ctrl Pts',(22.5934737004953,7.66938236806233,0.));
#253694=CARTESIAN_POINT('Ctrl Pts',(22.6141842556243,7.66924547229414,0.));
#253695=CARTESIAN_POINT('Ctrl Pts',(22.6349991971541,7.66905281533715,0.));
#253696=CARTESIAN_POINT('Ctrl Pts',(22.6559177133127,7.66880399241323,0.));
#253697=CARTESIAN_POINT('Ctrl Pts',(22.6769390009885,7.66849860491743,0.));
#253698=CARTESIAN_POINT('Ctrl Pts',(22.6980622655446,7.66813626029275,0.));
#253699=CARTESIAN_POINT('Ctrl Pts',(22.7192867206245,7.66771657191028,0.));
#253700=CARTESIAN_POINT('Ctrl Pts',(22.7406115879513,7.6672391589544,0.));
#253701=CARTESIAN_POINT('Ctrl Pts',(22.7620360971843,7.66670364630299,0.));
#253702=CARTESIAN_POINT('Ctrl Pts',(22.7835594857699,7.66610966441273,0.));
#253703=CARTESIAN_POINT('Ctrl Pts',(22.8051809987833,7.66545684920987,0.));
#253704=CARTESIAN_POINT('Ctrl Pts',(22.8268998887678,7.66474484198549,0.));
#253705=CARTESIAN_POINT('Ctrl Pts',(22.848715415557,7.66397328929803,0.));
#253706=CARTESIAN_POINT('Ctrl Pts',(22.8706268461283,7.66314184287337,0.));
#253707=CARTESIAN_POINT('Ctrl Pts',(22.8926334544883,7.66225015950156,0.));
#253708=CARTESIAN_POINT('Ctrl Pts',(22.9147345215421,7.66129790094108,0.));
#253709=CARTESIAN_POINT('Ctrl Pts',(22.9369293349593,7.66028473382778,0.));
#253710=CARTESIAN_POINT('Ctrl Pts',(22.959217189033,7.65921032958902,0.));
#253711=CARTESIAN_POINT('Ctrl Pts',(22.9815973845296,7.65807436436432,0.));
#253712=CARTESIAN_POINT('Ctrl Pts',(23.0040692285814,7.65687651891305,0.));
#253713=CARTESIAN_POINT('Ctrl Pts',(23.0266320345787,7.65561647852534,0.));
#253714=CARTESIAN_POINT('Ctrl Pts',(23.0492851220528,7.65429393293946,0.));
#253715=CARTESIAN_POINT('Ctrl Pts',(23.072027816555,7.65290857626358,0.));
#253716=CARTESIAN_POINT('Ctrl Pts',(23.094859449525,7.65146010690476,0.));
#253717=CARTESIAN_POINT('Ctrl Pts',(23.1177793581679,7.6499482274986,0.));
#253718=CARTESIAN_POINT('Ctrl Pts',(23.1407868853819,7.64837264482943,0.));
#253719=CARTESIAN_POINT('Ctrl Pts',(23.1638813796694,7.64673306975805,0.));
#253720=CARTESIAN_POINT('Ctrl Pts',(23.1870621950452,7.64502921715483,0.));
#253721=CARTESIAN_POINT('Ctrl Pts',(23.2103286909398,7.6432608058368,0.));
#253722=CARTESIAN_POINT('Ctrl Pts',(23.2336802320912,7.64142755851505,0.));
#253723=CARTESIAN_POINT('Ctrl Pts',(23.2571161884488,7.63952920172835,0.));
#253724=CARTESIAN_POINT('Ctrl Pts',(23.2806359350855,7.63756546576374,0.));
#253725=CARTESIAN_POINT('Ctrl Pts',(23.3042388521022,7.63553608458783,0.));
#253726=CARTESIAN_POINT('Ctrl Pts',(23.3279243245241,7.63344079578162,0.));
#253727=CARTESIAN_POINT('Ctrl Pts',(23.3516917421972,7.63127934048137,0.));
#253728=CARTESIAN_POINT('Ctrl Pts',(23.3755404996636,7.62905146332593,0.));
#253729=CARTESIAN_POINT('Ctrl Pts',(23.399469996112,7.62675691240329,0.));
#253730=CARTESIAN_POINT('Ctrl Pts',(23.4234796353542,7.6243954392005,0.));
#253731=CARTESIAN_POINT('Ctrl Pts',(23.4475688257854,7.62196679855955,0.));
#253732=CARTESIAN_POINT('Ctrl Pts',(23.4717369803438,7.61947074863977,0.));
#253733=CARTESIAN_POINT('Ctrl Pts',(23.4959835164609,7.61690705088319,0.));
#253734=CARTESIAN_POINT('Ctrl Pts',(23.5203078560129,7.61427546999298,0.));
#253735=CARTESIAN_POINT('Ctrl Pts',(23.544709425203,7.61157577385372,0.));
#253736=CARTESIAN_POINT('Ctrl Pts',(23.5691876544244,7.608807733446,0.));
#253737=CARTESIAN_POINT('Ctrl Pts',(23.5937419781245,7.60597112277094,0.));
#253738=CARTESIAN_POINT('Ctrl Pts',(23.6183718346576,7.60306571877806,0.));
#253739=CARTESIAN_POINT('Ctrl Pts',(23.6430766661418,7.60009130130126,0.));
#253740=CARTESIAN_POINT('Ctrl Pts',(23.6678559182875,7.59704765299567,0.));
#253741=CARTESIAN_POINT('Ctrl Pts',(23.6927090405066,7.59393455934035,0.));
#253742=CARTESIAN_POINT('Ctrl Pts',(23.7176354860456,7.59075180865321,0.));
#253743=CARTESIAN_POINT('Ctrl Pts',(23.7426347121006,7.58749919210826,0.));
#253744=CARTESIAN_POINT('Ctrl Pts',(23.7677061799376,7.58417650376271,0.));
#253745=CARTESIAN_POINT('Ctrl Pts',(23.7928493549908,7.58078354058213,0.));
#253746=CARTESIAN_POINT('Ctrl Pts',(23.8180637069976,7.57732010249066,0.));
#253747=CARTESIAN_POINT('Ctrl Pts',(23.8433487096132,7.57378599219814,0.));
#253748=CARTESIAN_POINT('Ctrl Pts',(23.8687038399595,7.57018101500709,0.));
#253749=CARTESIAN_POINT('Ctrl Pts',(23.8941285782002,7.56650497863791,0.));
#253750=CARTESIAN_POINT('Ctrl Pts',(23.9196224070759,7.56275769304773,0.));
#253751=CARTESIAN_POINT('Ctrl Pts',(23.9451848115002,7.5589389702768,0.));
#253752=CARTESIAN_POINT('Ctrl Pts',(23.9708152779886,7.55504862424808,0.));
#253753=CARTESIAN_POINT('Ctrl Pts',(23.9965132953187,7.55108647097432,0.));
#253754=CARTESIAN_POINT('Ctrl Pts',(24.0222783554531,7.54705232885895,0.));
#253755=CARTESIAN_POINT('Ctrl Pts',(24.0481099543353,7.54294601896128,0.));
#253756=CARTESIAN_POINT('Ctrl Pts',(24.0740075927984,7.53876736531005,0.));
#253757=CARTESIAN_POINT('Ctrl Pts',(24.0999707772642,7.53451619514659,0.));
#253758=CARTESIAN_POINT('Ctrl Pts',(24.1259990209211,7.53019233935537,0.));
#253759=CARTESIAN_POINT('Ctrl Pts',(24.152091842537,7.52579563201479,0.));
#253760=CARTESIAN_POINT('Ctrl Pts',(24.1782487641602,7.52132590953863,0.));
#253761=CARTESIAN_POINT('Ctrl Pts',(24.2044693092356,7.51678300997998,0.));
#253762=CARTESIAN_POINT('Ctrl Pts',(24.230753000389,7.51216677222199,0.));
#253763=CARTESIAN_POINT('Ctrl Pts',(24.2570993577032,7.50747703535115,0.));
#253764=CARTESIAN_POINT('Ctrl Pts',(24.2835078958966,7.50271363765099,0.));
#253765=CARTESIAN_POINT('Ctrl Pts',(24.3099781253345,7.49787641695359,0.));
#253766=CARTESIAN_POINT('Ctrl Pts',(24.3365095573673,7.4929652125233,0.));
#253767=CARTESIAN_POINT('Ctrl Pts',(24.3631017084513,7.48797986651828,0.));
#253768=CARTESIAN_POINT('Ctrl Pts',(24.3897541049248,7.48292022569254,0.));
#253769=CARTESIAN_POINT('Ctrl Pts',(24.4164662871165,7.47778614286574,0.));
#253770=CARTESIAN_POINT('Ctrl Pts',(24.4432378146501,7.47257747883319,0.));
#253771=CARTESIAN_POINT('Ctrl Pts',(24.4700682684544,7.46729410308923,0.));
#253772=CARTESIAN_POINT('Ctrl Pts',(24.4969572391509,7.46193588961642,0.));
#253773=CARTESIAN_POINT('Ctrl Pts',(24.52390431731,7.45650271336046,0.));
#253774=CARTESIAN_POINT('Ctrl Pts',(24.5509090831579,7.45099444651296,0.));
#253775=CARTESIAN_POINT('Ctrl Pts',(24.5779710960865,7.44541095473163,0.));
#253776=CARTESIAN_POINT('Ctrl Pts',(24.6050898852349,7.43975209375375,0.));
#253777=CARTESIAN_POINT('Ctrl Pts',(24.6322649369472,7.43401770489221,0.));
#253778=CARTESIAN_POINT('Ctrl Pts',(24.659495712869,7.42820762158681,0.));
#253779=CARTESIAN_POINT('Ctrl Pts',(24.6867816727118,7.42232167765763,0.));
#253780=CARTESIAN_POINT('Ctrl Pts',(24.7141222949988,7.41635971481243,0.));
#253781=CARTESIAN_POINT('Ctrl Pts',(24.7415170994754,7.41032159082173,0.));
#253782=CARTESIAN_POINT('Ctrl Pts',(24.7689656669005,7.40420718661755,0.));
#253783=CARTESIAN_POINT('Ctrl Pts',(24.7964676646518,7.39801641583613,0.));
#253784=CARTESIAN_POINT('Ctrl Pts',(24.8240228521042,7.39174922586841,0.));
#253785=CARTESIAN_POINT('Ctrl Pts',(24.8516310625367,7.38540558904946,0.));
#253786=CARTESIAN_POINT('Ctrl Pts',(24.8792921911309,7.3789854964161,0.));
#253787=CARTESIAN_POINT('Ctrl Pts',(24.9014633826201,7.37378825962718,0.));
#253788=CARTESIAN_POINT('Ctrl Pts',(24.9181155530631,7.36985593120697,0.));
#253789=CARTESIAN_POINT('Ctrl Pts',(24.9292275670705,7.3672190902906,0.));
#253790=CARTESIAN_POINT('Ctrl Pts',(24.9347862158358,7.36589684767344,0.));
#253791=CARTESIAN_POINT('',(24.9347862158358,7.36589684767344,12.));
#253792=CARTESIAN_POINT('Ctrl Pts',(24.9347862158358,7.36589684767344,12.));
#253793=CARTESIAN_POINT('Ctrl Pts',(24.9292275670705,7.3672190902906,12.));
#253794=CARTESIAN_POINT('Ctrl Pts',(24.9181155530631,7.36985593120697,12.));
#253795=CARTESIAN_POINT('Ctrl Pts',(24.9014633826201,7.37378825962718,12.));
#253796=CARTESIAN_POINT('Ctrl Pts',(24.8792921911309,7.3789854964161,12.));
#253797=CARTESIAN_POINT('Ctrl Pts',(24.8516310625367,7.38540558904946,12.));
#253798=CARTESIAN_POINT('Ctrl Pts',(24.8240228521042,7.39174922586841,12.));
#253799=CARTESIAN_POINT('Ctrl Pts',(24.7964676646518,7.39801641583613,12.));
#253800=CARTESIAN_POINT('Ctrl Pts',(24.7689656669005,7.40420718661755,12.));
#253801=CARTESIAN_POINT('Ctrl Pts',(24.7415170994754,7.41032159082173,12.));
#253802=CARTESIAN_POINT('Ctrl Pts',(24.7141222949988,7.41635971481243,12.));
#253803=CARTESIAN_POINT('Ctrl Pts',(24.6867816727118,7.42232167765763,12.));
#253804=CARTESIAN_POINT('Ctrl Pts',(24.659495712869,7.42820762158681,12.));
#253805=CARTESIAN_POINT('Ctrl Pts',(24.6322649369472,7.43401770489221,12.));
#253806=CARTESIAN_POINT('Ctrl Pts',(24.6050898852349,7.43975209375375,12.));
#253807=CARTESIAN_POINT('Ctrl Pts',(24.5779710960865,7.44541095473163,12.));
#253808=CARTESIAN_POINT('Ctrl Pts',(24.5509090831579,7.45099444651296,12.));
#253809=CARTESIAN_POINT('Ctrl Pts',(24.52390431731,7.45650271336046,12.));
#253810=CARTESIAN_POINT('Ctrl Pts',(24.4969572391509,7.46193588961642,12.));
#253811=CARTESIAN_POINT('Ctrl Pts',(24.4700682684544,7.46729410308923,12.));
#253812=CARTESIAN_POINT('Ctrl Pts',(24.4432378146501,7.47257747883319,12.));
#253813=CARTESIAN_POINT('Ctrl Pts',(24.4164662871165,7.47778614286574,12.));
#253814=CARTESIAN_POINT('Ctrl Pts',(24.3897541049248,7.48292022569254,12.));
#253815=CARTESIAN_POINT('Ctrl Pts',(24.3631017084513,7.48797986651828,12.));
#253816=CARTESIAN_POINT('Ctrl Pts',(24.3365095573673,7.4929652125233,12.));
#253817=CARTESIAN_POINT('Ctrl Pts',(24.3099781253345,7.49787641695359,12.));
#253818=CARTESIAN_POINT('Ctrl Pts',(24.2835078958966,7.50271363765099,12.));
#253819=CARTESIAN_POINT('Ctrl Pts',(24.2570993577032,7.50747703535115,12.));
#253820=CARTESIAN_POINT('Ctrl Pts',(24.230753000389,7.51216677222199,12.));
#253821=CARTESIAN_POINT('Ctrl Pts',(24.2044693092356,7.51678300997998,12.));
#253822=CARTESIAN_POINT('Ctrl Pts',(24.1782487641602,7.52132590953863,12.));
#253823=CARTESIAN_POINT('Ctrl Pts',(24.152091842537,7.52579563201479,12.));
#253824=CARTESIAN_POINT('Ctrl Pts',(24.1259990209211,7.53019233935537,12.));
#253825=CARTESIAN_POINT('Ctrl Pts',(24.0999707772642,7.53451619514659,12.));
#253826=CARTESIAN_POINT('Ctrl Pts',(24.0740075927984,7.53876736531005,12.));
#253827=CARTESIAN_POINT('Ctrl Pts',(24.0481099543353,7.54294601896128,12.));
#253828=CARTESIAN_POINT('Ctrl Pts',(24.0222783554531,7.54705232885895,12.));
#253829=CARTESIAN_POINT('Ctrl Pts',(23.9965132953187,7.55108647097432,12.));
#253830=CARTESIAN_POINT('Ctrl Pts',(23.9708152779886,7.55504862424808,12.));
#253831=CARTESIAN_POINT('Ctrl Pts',(23.9451848115002,7.5589389702768,12.));
#253832=CARTESIAN_POINT('Ctrl Pts',(23.9196224070759,7.56275769304773,12.));
#253833=CARTESIAN_POINT('Ctrl Pts',(23.8941285782002,7.56650497863791,12.));
#253834=CARTESIAN_POINT('Ctrl Pts',(23.8687038399595,7.57018101500709,12.));
#253835=CARTESIAN_POINT('Ctrl Pts',(23.8433487096132,7.57378599219814,12.));
#253836=CARTESIAN_POINT('Ctrl Pts',(23.8180637069976,7.57732010249066,12.));
#253837=CARTESIAN_POINT('Ctrl Pts',(23.7928493549908,7.58078354058213,12.));
#253838=CARTESIAN_POINT('Ctrl Pts',(23.7677061799376,7.58417650376271,12.));
#253839=CARTESIAN_POINT('Ctrl Pts',(23.7426347121006,7.58749919210826,12.));
#253840=CARTESIAN_POINT('Ctrl Pts',(23.7176354860456,7.59075180865321,12.));
#253841=CARTESIAN_POINT('Ctrl Pts',(23.6927090405066,7.59393455934035,12.));
#253842=CARTESIAN_POINT('Ctrl Pts',(23.6678559182875,7.59704765299567,12.));
#253843=CARTESIAN_POINT('Ctrl Pts',(23.6430766661418,7.60009130130126,12.));
#253844=CARTESIAN_POINT('Ctrl Pts',(23.6183718346576,7.60306571877806,12.));
#253845=CARTESIAN_POINT('Ctrl Pts',(23.5937419781245,7.60597112277094,12.));
#253846=CARTESIAN_POINT('Ctrl Pts',(23.5691876544244,7.608807733446,12.));
#253847=CARTESIAN_POINT('Ctrl Pts',(23.544709425203,7.61157577385372,12.));
#253848=CARTESIAN_POINT('Ctrl Pts',(23.5203078560129,7.61427546999298,12.));
#253849=CARTESIAN_POINT('Ctrl Pts',(23.4959835164609,7.61690705088319,12.));
#253850=CARTESIAN_POINT('Ctrl Pts',(23.4717369803438,7.61947074863977,12.));
#253851=CARTESIAN_POINT('Ctrl Pts',(23.4475688257854,7.62196679855955,12.));
#253852=CARTESIAN_POINT('Ctrl Pts',(23.4234796353542,7.6243954392005,12.));
#253853=CARTESIAN_POINT('Ctrl Pts',(23.399469996112,7.62675691240329,12.));
#253854=CARTESIAN_POINT('Ctrl Pts',(23.3755404996636,7.62905146332593,12.));
#253855=CARTESIAN_POINT('Ctrl Pts',(23.3516917421972,7.63127934048137,12.));
#253856=CARTESIAN_POINT('Ctrl Pts',(23.3279243245241,7.63344079578162,12.));
#253857=CARTESIAN_POINT('Ctrl Pts',(23.3042388521022,7.63553608458783,12.));
#253858=CARTESIAN_POINT('Ctrl Pts',(23.2806359350855,7.63756546576374,12.));
#253859=CARTESIAN_POINT('Ctrl Pts',(23.2571161884488,7.63952920172835,12.));
#253860=CARTESIAN_POINT('Ctrl Pts',(23.2336802320912,7.64142755851505,12.));
#253861=CARTESIAN_POINT('Ctrl Pts',(23.2103286909398,7.6432608058368,12.));
#253862=CARTESIAN_POINT('Ctrl Pts',(23.1870621950452,7.64502921715483,12.));
#253863=CARTESIAN_POINT('Ctrl Pts',(23.1638813796694,7.64673306975805,12.));
#253864=CARTESIAN_POINT('Ctrl Pts',(23.1407868853819,7.64837264482943,12.));
#253865=CARTESIAN_POINT('Ctrl Pts',(23.1177793581679,7.6499482274986,12.));
#253866=CARTESIAN_POINT('Ctrl Pts',(23.094859449525,7.65146010690476,12.));
#253867=CARTESIAN_POINT('Ctrl Pts',(23.072027816555,7.65290857626358,12.));
#253868=CARTESIAN_POINT('Ctrl Pts',(23.0492851220528,7.65429393293946,12.));
#253869=CARTESIAN_POINT('Ctrl Pts',(23.0266320345787,7.65561647852534,12.));
#253870=CARTESIAN_POINT('Ctrl Pts',(23.0040692285814,7.65687651891305,12.));
#253871=CARTESIAN_POINT('Ctrl Pts',(22.9815973845296,7.65807436436432,12.));
#253872=CARTESIAN_POINT('Ctrl Pts',(22.959217189033,7.65921032958902,12.));
#253873=CARTESIAN_POINT('Ctrl Pts',(22.9369293349593,7.66028473382778,12.));
#253874=CARTESIAN_POINT('Ctrl Pts',(22.9147345215421,7.66129790094108,12.));
#253875=CARTESIAN_POINT('Ctrl Pts',(22.8926334544883,7.66225015950156,12.));
#253876=CARTESIAN_POINT('Ctrl Pts',(22.8706268461283,7.66314184287337,12.));
#253877=CARTESIAN_POINT('Ctrl Pts',(22.848715415557,7.66397328929803,12.));
#253878=CARTESIAN_POINT('Ctrl Pts',(22.8268998887678,7.66474484198549,12.));
#253879=CARTESIAN_POINT('Ctrl Pts',(22.8051809987833,7.66545684920987,12.));
#253880=CARTESIAN_POINT('Ctrl Pts',(22.7835594857699,7.66610966441273,12.));
#253881=CARTESIAN_POINT('Ctrl Pts',(22.7620360971843,7.66670364630299,12.));
#253882=CARTESIAN_POINT('Ctrl Pts',(22.7406115879513,7.6672391589544,12.));
#253883=CARTESIAN_POINT('Ctrl Pts',(22.7192867206245,7.66771657191028,12.));
#253884=CARTESIAN_POINT('Ctrl Pts',(22.6980622655446,7.66813626029275,12.));
#253885=CARTESIAN_POINT('Ctrl Pts',(22.6769390009885,7.66849860491743,12.));
#253886=CARTESIAN_POINT('Ctrl Pts',(22.6559177133127,7.66880399241323,12.));
#253887=CARTESIAN_POINT('Ctrl Pts',(22.6349991971541,7.66905281533715,12.));
#253888=CARTESIAN_POINT('Ctrl Pts',(22.6141842556243,7.66924547229414,12.));
#253889=CARTESIAN_POINT('Ctrl Pts',(22.5934737004953,7.66938236806233,12.));
#253890=CARTESIAN_POINT('Ctrl Pts',(22.5728683523831,7.66946391372306,12.));
#253891=CARTESIAN_POINT('Ctrl Pts',(22.5523690409116,7.66949052679693,12.));
#253892=CARTESIAN_POINT('Ctrl Pts',(22.53197660492,7.66946263138144,12.));
#253893=CARTESIAN_POINT('Ctrl Pts',(22.5116918927031,7.66938065829108,12.));
#253894=CARTESIAN_POINT('Ctrl Pts',(22.4915157622312,7.66924504520315,12.));
#253895=CARTESIAN_POINT('Ctrl Pts',(22.4714490813699,7.66905623680831,12.));
#253896=CARTESIAN_POINT('Ctrl Pts',(22.4514927280855,7.66881468496635,12.));
#253897=CARTESIAN_POINT('Ctrl Pts',(22.4316475906603,7.66852084886704,12.));
#253898=CARTESIAN_POINT('Ctrl Pts',(22.4119145679758,7.6681751951964,12.));
#253899=CARTESIAN_POINT('Ctrl Pts',(22.3922945697773,7.6677781983079,12.));
#253900=CARTESIAN_POINT('Ctrl Pts',(22.372788516936,7.66733034039883,12.));
#253901=CARTESIAN_POINT('Ctrl Pts',(22.3533973417021,7.66683211169159,12.));
#253902=CARTESIAN_POINT('Ctrl Pts',(22.3341219879469,7.66628401061952,12.));
#253903=CARTESIAN_POINT('Ctrl Pts',(22.314963411484,7.66568654402494,12.));
#253904=CARTESIAN_POINT('Ctrl Pts',(22.2959225803937,7.66504022736299,12.));
#253905=CARTESIAN_POINT('Ctrl Pts',(22.2770004753335,7.66434558490979,12.));
#253906=CARTESIAN_POINT('Ctrl Pts',(22.258198089848,7.66360314997641,12.));
#253907=CARTESIAN_POINT('Ctrl Pts',(22.2395164306547,7.66281346512509,12.));
#253908=CARTESIAN_POINT('Ctrl Pts',(22.2209565180085,7.661977082404,12.));
#253909=CARTESIAN_POINT('Ctrl Pts',(22.2025193860964,7.66109456359271,12.));
#253910=CARTESIAN_POINT('Ctrl Pts',(22.1842060834091,7.66016648045005,12.));
#253911=CARTESIAN_POINT('Ctrl Pts',(22.1660176731178,7.65919341496931,12.));
#253912=CARTESIAN_POINT('Ctrl Pts',(22.1479552334211,7.65817595963349,12.));
#253913=CARTESIAN_POINT('Ctrl Pts',(22.1300198579675,7.65711471769397,12.));
#253914=CARTESIAN_POINT('Ctrl Pts',(22.1122126563329,7.65601030346807,12.));
#253915=CARTESIAN_POINT('Ctrl Pts',(22.094534754469,7.65486334263644,12.));
#253916=CARTESIAN_POINT('Ctrl Pts',(22.0769872951596,7.65367447254949,12.));
#253917=CARTESIAN_POINT('Ctrl Pts',(22.0595714384431,7.65244434253113,12.));
#253918=CARTESIAN_POINT('Ctrl Pts',(22.0422883621174,7.65117361421359,12.));
#253919=CARTESIAN_POINT('Ctrl Pts',(22.0251392623209,7.64986296190169,12.));
#253920=CARTESIAN_POINT('Ctrl Pts',(22.0081253540774,7.64851307293352,12.));
#253921=CARTESIAN_POINT('Ctrl Pts',(21.9912478718542,7.6471246480525,12.));
#253922=CARTESIAN_POINT('Ctrl Pts',(21.9745080700798,7.64569840177336,12.));
#253923=CARTESIAN_POINT('Ctrl Pts',(21.9579072237651,7.64423506279123,12.));
#253924=CARTESIAN_POINT('Ctrl Pts',(21.9414466292072,7.64273537442682,12.));
#253925=CARTESIAN_POINT('Ctrl Pts',(21.9251276046545,7.64120009506532,12.));
#253926=CARTESIAN_POINT('Ctrl Pts',(21.9089514909874,7.63962999860927,12.));
#253927=CARTESIAN_POINT('Ctrl Pts',(21.8929196523514,7.63802587492035,12.));
#253928=CARTESIAN_POINT('Ctrl Pts',(21.8770334769496,7.636388530334,12.));
#253929=CARTESIAN_POINT('Ctrl Pts',(21.8612943779089,7.63471878821226,12.));
#253930=CARTESIAN_POINT('Ctrl Pts',(21.8457037941084,7.63301748948936,12.));
#253931=CARTESIAN_POINT('Ctrl Pts',(21.8302631910195,7.63128549323023,12.));
#253932=CARTESIAN_POINT('Ctrl Pts',(21.814974061509,7.62952367718127,12.));
#253933=CARTESIAN_POINT('Ctrl Pts',(21.799837926858,7.62773293842389,12.));
#253934=CARTESIAN_POINT('Ctrl Pts',(21.7848563378021,7.62591419404513,12.));
#253935=CARTESIAN_POINT('Ctrl Pts',(21.7700308755584,7.62406838181166,12.));
#253936=CARTESIAN_POINT('Ctrl Pts',(21.7553631528328,7.62219646084229,12.));
#253937=CARTESIAN_POINT('Ctrl Pts',(21.7408548148656,7.62029941230855,12.));
#253938=CARTESIAN_POINT('Ctrl Pts',(21.7265075407975,7.61837824030538,12.));
#253939=CARTESIAN_POINT('Ctrl Pts',(21.7123230449834,7.61643397270421,12.));
#253940=CARTESIAN_POINT('Ctrl Pts',(21.6983030783322,7.61446766202787,12.));
#253941=CARTESIAN_POINT('Ctrl Pts',(21.6844494295815,7.61248038630269,12.));
#253942=CARTESIAN_POINT('Ctrl Pts',(21.6707639267576,7.61047325000956,12.));
#253943=CARTESIAN_POINT('Ctrl Pts',(21.6572484388081,7.60844738512874,12.));
#253944=CARTESIAN_POINT('Ctrl Pts',(21.6439048771743,7.60640395216357,12.));
#253945=CARTESIAN_POINT('Ctrl Pts',(21.6307351973822,7.60434414118296,12.));
#253946=CARTESIAN_POINT('Ctrl Pts',(21.617741400599,7.60226917285429,12.));
#253947=CARTESIAN_POINT('Ctrl Pts',(21.6049255358843,7.60018029988241,12.));
#253948=CARTESIAN_POINT('Ctrl Pts',(21.5922897024466,7.59807880846195,12.));
#253949=CARTESIAN_POINT('Ctrl Pts',(21.5798360518978,7.59596601973584,12.));
#253950=CARTESIAN_POINT('Ctrl Pts',(21.5675667904726,7.59384329124918,12.));
#253951=CARTESIAN_POINT('Ctrl Pts',(21.5554841813462,7.59171201844777,12.));
#253952=CARTESIAN_POINT('Ctrl Pts',(21.543590547011,7.58957363620014,12.));
#253953=CARTESIAN_POINT('Ctrl Pts',(21.5318882716736,7.58742962034834,12.));
#253954=CARTESIAN_POINT('Ctrl Pts',(21.5203798035299,7.5852814891913,12.));
#253955=CARTESIAN_POINT('Ctrl Pts',(21.5090676573873,7.5831308051918,12.));
#253956=CARTESIAN_POINT('Ctrl Pts',(21.4979544192744,7.58097917790744,12.));
#253957=CARTESIAN_POINT('Ctrl Pts',(21.4870427508194,7.57882826679132,12.));
#253958=CARTESIAN_POINT('Ctrl Pts',(21.4763353936762,7.57667978402987,12.));
#253959=CARTESIAN_POINT('Ctrl Pts',(21.4658351740128,7.57453549743412,12.));
#253960=CARTESIAN_POINT('Ctrl Pts',(21.4555450053142,7.57239723223506,12.));
#253961=CARTESIAN_POINT('Ctrl Pts',(21.4454678907509,7.57026687261166,12.));
#253962=CARTESIAN_POINT('Ctrl Pts',(21.4356069261513,7.56814636360848,12.));
#253963=CARTESIAN_POINT('Ctrl Pts',(21.4259653015736,7.56603771218712,12.));
#253964=CARTESIAN_POINT('Ctrl Pts',(21.4165463106254,7.56394299313685,12.));
#253965=CARTESIAN_POINT('Ctrl Pts',(21.4073533630365,7.56186435703622,12.));
#253966=CARTESIAN_POINT('Ctrl Pts',(21.3983899952987,7.55980403700611,12.));
#253967=CARTESIAN_POINT('Ctrl Pts',(21.3896598842117,7.55776435731417,12.));
#253968=CARTESIAN_POINT('Ctrl Pts',(21.3811668478932,7.55574773403503,12.));
#253969=CARTESIAN_POINT('Ctrl Pts',(21.3729148390243,7.55375667080029,12.));
#253970=CARTESIAN_POINT('Ctrl Pts',(21.3649079431865,7.55179375777444,12.));
#253971=CARTESIAN_POINT('Ctrl Pts',(21.3571503685855,7.5498616652131,12.));
#253972=CARTESIAN_POINT('Ctrl Pts',(21.3496464761531,7.54796316246331,12.));
#253973=CARTESIAN_POINT('Ctrl Pts',(21.3424008295038,7.54610114948347,12.));
#253974=CARTESIAN_POINT('Ctrl Pts',(21.3354182340149,7.54427868151268,12.));
#253975=CARTESIAN_POINT('Ctrl Pts',(21.328703791771,7.54249900377031,12.));
#253976=CARTESIAN_POINT('Ctrl Pts',(21.3222628524165,7.54076552038279,12.));
#253977=CARTESIAN_POINT('Ctrl Pts',(21.3161009456256,7.53908175169899,12.));
#253978=CARTESIAN_POINT('Ctrl Pts',(21.310223716773,7.53745129364616,12.));
#253979=CARTESIAN_POINT('Ctrl Pts',(21.3046368712157,7.53587778251736,12.));
#253980=CARTESIAN_POINT('Ctrl Pts',(21.2993464250717,7.53436505309943,12.));
#253981=CARTESIAN_POINT('Ctrl Pts',(21.2943588989331,7.53291726078527,12.));
#253982=CARTESIAN_POINT('Ctrl Pts',(21.2896816163842,7.53153906987856,12.));
#253983=CARTESIAN_POINT('Ctrl Pts',(21.2853226580657,7.5302356243823,12.));
#253984=CARTESIAN_POINT('Ctrl Pts',(21.2812902781143,7.52901217930408,12.));
#253985=CARTESIAN_POINT('Ctrl Pts',(21.2775925269652,7.52787386225333,12.));
#253986=CARTESIAN_POINT('Ctrl Pts',(21.2742366113579,7.52682526918541,12.));
#253987=CARTESIAN_POINT('Ctrl Pts',(21.2712301573466,7.5258712609553,12.));
#253988=CARTESIAN_POINT('Ctrl Pts',(21.2685823838671,7.52501770333531,12.));
#253989=CARTESIAN_POINT('Ctrl Pts',(21.2663059157058,7.52427261074298,12.));
#253990=CARTESIAN_POINT('Ctrl Pts',(21.2644161259962,7.52364573027553,12.));
#253991=CARTESIAN_POINT('Ctrl Pts',(21.262927782038,7.52314642316199,12.));
#253992=CARTESIAN_POINT('Ctrl Pts',(21.2618521283555,7.5227818224267,12.));
#253993=CARTESIAN_POINT('Ctrl Pts',(21.261326054066,7.52260064231661,12.));
#253994=CARTESIAN_POINT('Ctrl Pts',(21.2611204474866,7.52252744144904,12.));
#253995=CARTESIAN_POINT('Ctrl Pts',(21.2610673466886,7.5225064970397,12.));
#253996=CARTESIAN_POINT('Ctrl Pts',(21.2610617890679,7.52250298901264,12.));
#253997=CARTESIAN_POINT('',(24.9347862158358,7.36589684767344,0.));
#253998=CARTESIAN_POINT('Origin',(0.,0.,0.));
#253999=CARTESIAN_POINT('Origin',(0.,0.,0.));
#254000=CARTESIAN_POINT('Origin',(0.,0.,0.));
#254001=CARTESIAN_POINT('Origin',(0.,0.,0.));
#254002=CARTESIAN_POINT('Origin',(0.,0.,0.));
#254003=CARTESIAN_POINT('Origin',(0.,0.,0.));
#254004=CARTESIAN_POINT('Origin',(0.,0.,0.));
#254005=CARTESIAN_POINT('Origin',(0.,0.,0.));
#254006=CARTESIAN_POINT('Origin',(0.,0.,0.));
#254007=CARTESIAN_POINT('Origin',(0.,0.,0.));
#254008=CARTESIAN_POINT('Origin',(0.,0.,0.));
#254009=CARTESIAN_POINT('Origin',(0.,0.,0.));
#254010=CARTESIAN_POINT('Origin',(0.,0.,0.));
#254011=CARTESIAN_POINT('Origin',(0.,0.,0.));
#254012=CARTESIAN_POINT('Origin',(0.,0.,0.));
#254013=CARTESIAN_POINT('Origin',(0.,0.,0.));
#254014=CARTESIAN_POINT('Origin',(0.,0.,0.));
#254015=CARTESIAN_POINT('Origin',(0.,0.,0.));
#254016=CARTESIAN_POINT('Origin',(0.,0.,0.));
#254017=CARTESIAN_POINT('Origin',(0.,0.,0.));
#254018=CARTESIAN_POINT('Origin',(0.,0.,0.));
#254019=CARTESIAN_POINT('Origin',(0.,0.,0.));
#254020=CARTESIAN_POINT('Origin',(0.,0.,0.));
#254021=CARTESIAN_POINT('',(25.2771067246846,6.08833931617698,0.));
#254022=CARTESIAN_POINT('Origin',(0.,0.,0.));
#254023=CARTESIAN_POINT('',(22.1738711152697,4.11585220600461,0.));
#254024=CARTESIAN_POINT('Ctrl Pts',(25.2771067246846,6.08833931617698,0.));
#254025=CARTESIAN_POINT('Ctrl Pts',(25.2729539149479,6.08441489609824,0.));
#254026=CARTESIAN_POINT('Ctrl Pts',(25.2646490489816,6.07657531787578,0.));
#254027=CARTESIAN_POINT('Ctrl Pts',(25.2521940105523,6.06484373634697,0.));
#254028=CARTESIAN_POINT('Ctrl Pts',(25.2355918138798,6.04925720151412,0.));
#254029=CARTESIAN_POINT('Ctrl Pts',(25.2148466201368,6.02986667390187,0.));
#254030=CARTESIAN_POINT('Ctrl Pts',(25.1941090269638,6.0105688180476,0.));
#254031=CARTESIAN_POINT('Ctrl Pts',(25.1733791296154,5.99136367859839,0.));
#254032=CARTESIAN_POINT('Ctrl Pts',(25.1526570863065,5.97225131495636,0.));
#254033=CARTESIAN_POINT('Ctrl Pts',(25.1319431317273,5.95323180187348,0.));
#254034=CARTESIAN_POINT('Ctrl Pts',(25.1112375971182,5.93430523086776,0.));
#254035=CARTESIAN_POINT('Ctrl Pts',(25.0905409050863,5.91547170844382,0.));
#254036=CARTESIAN_POINT('Ctrl Pts',(25.0698535426593,5.89673135155459,0.));
#254037=CARTESIAN_POINT('Ctrl Pts',(25.0491760405965,5.87808428385329,0.));
#254038=CARTESIAN_POINT('Ctrl Pts',(25.0285089498922,5.8595306315681,0.));
#254039=CARTESIAN_POINT('Ctrl Pts',(25.0078528200558,5.84107051963074,0.));
#254040=CARTESIAN_POINT('Ctrl Pts',(24.9872081752709,5.82270406744214,0.));
#254041=CARTESIAN_POINT('Ctrl Pts',(24.9665754954462,5.80443138549747,0.));
#254042=CARTESIAN_POINT('Ctrl Pts',(24.9459552293308,5.78625257775703,0.));
#254043=CARTESIAN_POINT('Ctrl Pts',(24.9253478043632,5.76816774342236,0.));
#254044=CARTESIAN_POINT('Ctrl Pts',(24.9047536376467,5.75017697890813,0.));
#254045=CARTESIAN_POINT('Ctrl Pts',(24.8841731467219,5.73228037976927,0.));
#254046=CARTESIAN_POINT('Ctrl Pts',(24.8636067597677,5.71447804252019,0.));
#254047=CARTESIAN_POINT('Ctrl Pts',(24.8430549277634,5.6967700667943,0.));
#254048=CARTESIAN_POINT('Ctrl Pts',(24.822518122386,5.67915655496524,0.));
#254049=CARTESIAN_POINT('Ctrl Pts',(24.8019968304618,5.66163761114903,0.));
#254050=CARTESIAN_POINT('Ctrl Pts',(24.7814915496728,5.64421334042248,0.));
#254051=CARTESIAN_POINT('Ctrl Pts',(24.76100278357,5.62688384790919,0.));
#254052=CARTESIAN_POINT('Ctrl Pts',(24.7405310372736,5.60964923798495,0.));
#254053=CARTESIAN_POINT('Ctrl Pts',(24.7200768119079,5.59250961323995,0.));
#254054=CARTESIAN_POINT('Ctrl Pts',(24.6996406035507,5.57546507427767,0.));
#254055=CARTESIAN_POINT('Ctrl Pts',(24.6792229061785,5.55851572025389,0.));
#254056=CARTESIAN_POINT('Ctrl Pts',(24.6588242134733,5.54166164919593,0.));
#254057=CARTESIAN_POINT('Ctrl Pts',(24.6384450211466,5.52490295840996,0.));
#254058=CARTESIAN_POINT('Ctrl Pts',(24.618085828918,5.50823974481959,0.));
#254059=CARTESIAN_POINT('Ctrl Pts',(24.5977471429365,5.49167210537235,0.));
#254060=CARTESIAN_POINT('Ctrl Pts',(24.5774294770329,5.47520013724403,0.));
#254061=CARTESIAN_POINT('Ctrl Pts',(24.5571333514841,5.45882393762244,0.));
#254062=CARTESIAN_POINT('Ctrl Pts',(24.5368592922861,5.44254360356866,0.));
#254063=CARTESIAN_POINT('Ctrl Pts',(24.5166078302107,5.42635923183411,0.));
#254064=CARTESIAN_POINT('Ctrl Pts',(24.4963794999831,5.41027091869242,0.));
#254065=CARTESIAN_POINT('Ctrl Pts',(24.4761748393322,5.39427875973831,0.));
#254066=CARTESIAN_POINT('Ctrl Pts',(24.4559943883159,5.37838284973706,0.));
#254067=CARTESIAN_POINT('Ctrl Pts',(24.4358386899152,5.36258328273639,0.));
#254068=CARTESIAN_POINT('Ctrl Pts',(24.4157082904615,5.34688015213546,0.));
#254069=CARTESIAN_POINT('Ctrl Pts',(24.3956037401293,5.33127355076037,0.));
#254070=CARTESIAN_POINT('Ctrl Pts',(24.3755255933917,5.31576357092525,0.));
#254071=CARTESIAN_POINT('Ctrl Pts',(24.3554744095075,5.30035030449059,0.));
#254072=CARTESIAN_POINT('Ctrl Pts',(24.3354507529415,5.28503384290644,0.));
#254073=CARTESIAN_POINT('Ctrl Pts',(24.3154551932222,5.26981427718796,0.));
#254074=CARTESIAN_POINT('Ctrl Pts',(24.2954883048448,5.25469169788856,0.));
#254075=CARTESIAN_POINT('Ctrl Pts',(24.2755506671526,5.23966619506289,0.));
#254076=CARTESIAN_POINT('Ctrl Pts',(24.2556428642294,5.22473785822441,0.));
#254077=CARTESIAN_POINT('Ctrl Pts',(24.2357654847765,5.20990677629173,0.));
#254078=CARTESIAN_POINT('Ctrl Pts',(24.215919122017,5.19517303753643,0.));
#254079=CARTESIAN_POINT('Ctrl Pts',(24.1961043738754,5.18053672961392,0.));
#254080=CARTESIAN_POINT('Ctrl Pts',(24.1763218431343,5.16599793957979,0.));
#254081=CARTESIAN_POINT('Ctrl Pts',(24.156572137597,5.15155675390075,0.));
#254082=CARTESIAN_POINT('Ctrl Pts',(24.1368558702443,5.13721325845745,0.));
#254083=CARTESIAN_POINT('Ctrl Pts',(24.117173659394,5.1229675385386,0.));
#254084=CARTESIAN_POINT('Ctrl Pts',(24.0975261288446,5.10881967883132,0.));
#254085=CARTESIAN_POINT('Ctrl Pts',(24.0779139079266,5.09476976342625,0.));
#254086=CARTESIAN_POINT('Ctrl Pts',(24.0583376315638,5.08081787581277,0.));
#254087=CARTESIAN_POINT('Ctrl Pts',(24.0387979403268,5.06696409886641,0.));
#254088=CARTESIAN_POINT('Ctrl Pts',(24.0192954804896,5.05320851483065,0.));
#254089=CARTESIAN_POINT('Ctrl Pts',(23.9998309040746,5.03955120528521,0.));
#254090=CARTESIAN_POINT('Ctrl Pts',(23.9804048689227,5.02599225112454,0.));
#254091=CARTESIAN_POINT('Ctrl Pts',(23.961018038827,5.01253173257453,0.));
#254092=CARTESIAN_POINT('Ctrl Pts',(23.9416710836529,4.99916972919307,0.));
#254093=CARTESIAN_POINT('Ctrl Pts',(23.9223646794592,4.98590631986533,0.));
#254094=CARTESIAN_POINT('Ctrl Pts',(23.9030995086163,4.97274158279227,0.));
#254095=CARTESIAN_POINT('Ctrl Pts',(23.8838762599218,4.95967559546561,0.));
#254096=CARTESIAN_POINT('Ctrl Pts',(23.8646956287168,4.9467084346586,0.));
#254097=CARTESIAN_POINT('Ctrl Pts',(23.8455583170057,4.93384017643432,0.));
#254098=CARTESIAN_POINT('Ctrl Pts',(23.8264650335717,4.92107089613969,0.));
#254099=CARTESIAN_POINT('Ctrl Pts',(23.8074164940896,4.90840066839344,0.));
#254100=CARTESIAN_POINT('Ctrl Pts',(23.7884134212384,4.89582956706775,0.));
#254101=CARTESIAN_POINT('Ctrl Pts',(23.7694565448049,4.88335766525573,0.));
#254102=CARTESIAN_POINT('Ctrl Pts',(23.7505466018245,4.87098503527152,0.));
#254103=CARTESIAN_POINT('Ctrl Pts',(23.7316843367313,4.85871174865499,0.));
#254104=CARTESIAN_POINT('Ctrl Pts',(23.7128705015017,4.84653787616426,0.));
#254105=CARTESIAN_POINT('Ctrl Pts',(23.6941058557971,4.83446348776266,0.));
#254106=CARTESIAN_POINT('Ctrl Pts',(23.675391167102,4.82248865259562,0.));
#254107=CARTESIAN_POINT('Ctrl Pts',(23.6567272108628,4.81061343896432,0.));
#254108=CARTESIAN_POINT('Ctrl Pts',(23.6381147706579,4.7988379143322,0.));
#254109=CARTESIAN_POINT('Ctrl Pts',(23.6195546383624,4.78716214532098,0.));
#254110=CARTESIAN_POINT('Ctrl Pts',(23.6010476143099,4.77558619769872,0.));
#254111=CARTESIAN_POINT('Ctrl Pts',(23.5825945074535,4.76411013636251,0.));
#254112=CARTESIAN_POINT('Ctrl Pts',(23.5641961355168,4.75273402530617,0.));
#254113=CARTESIAN_POINT('Ctrl Pts',(23.545853325171,4.74145792760699,0.));
#254114=CARTESIAN_POINT('Ctrl Pts',(23.5275669122372,4.7302819054303,0.));
#254115=CARTESIAN_POINT('Ctrl Pts',(23.509337741878,4.71920602001902,0.));
#254116=CARTESIAN_POINT('Ctrl Pts',(23.491166668789,4.70823033167819,0.));
#254117=CARTESIAN_POINT('Ctrl Pts',(23.4730545573853,4.69735489975024,0.));
#254118=CARTESIAN_POINT('Ctrl Pts',(23.455002281986,4.68657978258303,0.));
#254119=CARTESIAN_POINT('Ctrl Pts',(23.4370107270451,4.67590503753059,0.));
#254120=CARTESIAN_POINT('Ctrl Pts',(23.4190807873803,4.6653307209467,0.));
#254121=CARTESIAN_POINT('Ctrl Pts',(23.4012133683959,4.65485688816924,0.));
#254122=CARTESIAN_POINT('Ctrl Pts',(23.3834093863068,4.6444835934993,0.));
#254123=CARTESIAN_POINT('Ctrl Pts',(23.3656697683489,4.63421089016541,0.));
#254124=CARTESIAN_POINT('Ctrl Pts',(23.3479954530272,4.62403883030805,0.));
#254125=CARTESIAN_POINT('Ctrl Pts',(23.3303873903938,4.6139674649783,0.));
#254126=CARTESIAN_POINT('Ctrl Pts',(23.3128465423115,4.60399684412163,0.));
#254127=CARTESIAN_POINT('Ctrl Pts',(23.2953738827191,4.5941270165575,0.));
#254128=CARTESIAN_POINT('Ctrl Pts',(23.2779703978876,4.5843580299469,0.));
#254129=CARTESIAN_POINT('Ctrl Pts',(23.2606370866866,4.57468993076097,0.));
#254130=CARTESIAN_POINT('Ctrl Pts',(23.2433749609131,4.56512276427839,0.));
#254131=CARTESIAN_POINT('Ctrl Pts',(23.2261850456064,4.55565657456975,0.));
#254132=CARTESIAN_POINT('Ctrl Pts',(23.2090683793629,4.54629140447544,0.));
#254133=CARTESIAN_POINT('Ctrl Pts',(23.1920260146465,4.53702729557566,0.));
#254134=CARTESIAN_POINT('Ctrl Pts',(23.1750590180908,4.52786428815015,0.));
#254135=CARTESIAN_POINT('Ctrl Pts',(23.1581684708761,4.51880242116748,0.));
#254136=CARTESIAN_POINT('Ctrl Pts',(23.1413554691123,4.5098417322706,0.));
#254137=CARTESIAN_POINT('Ctrl Pts',(23.1246211242115,4.50098225775171,0.));
#254138=CARTESIAN_POINT('Ctrl Pts',(23.1079665632636,4.49222403252216,0.));
#254139=CARTESIAN_POINT('Ctrl Pts',(23.0913929293922,4.48356709006788,0.));
#254140=CARTESIAN_POINT('Ctrl Pts',(23.0749013821881,4.47501146242856,0.));
#254141=CARTESIAN_POINT('Ctrl Pts',(23.0584930981732,4.46655718018231,0.));
#254142=CARTESIAN_POINT('Ctrl Pts',(23.0421692712467,4.45820427241683,0.));
#254143=CARTESIAN_POINT('Ctrl Pts',(23.0259311131392,4.44995276669687,0.));
#254144=CARTESIAN_POINT('Ctrl Pts',(23.0097798538395,4.44180268901643,0.));
#254145=CARTESIAN_POINT('Ctrl Pts',(22.9937167421006,4.43375406376879,0.));
#254146=CARTESIAN_POINT('Ctrl Pts',(22.977743046002,4.42580691372752,0.));
#254147=CARTESIAN_POINT('Ctrl Pts',(22.9618600534866,4.41796126001302,0.));
#254148=CARTESIAN_POINT('Ctrl Pts',(22.9460690729093,4.41021712205554,0.));
#254149=CARTESIAN_POINT('Ctrl Pts',(22.930371433555,4.40257451754324,0.));
#254150=CARTESIAN_POINT('Ctrl Pts',(22.9147684862426,4.39503346238473,0.));
#254151=CARTESIAN_POINT('Ctrl Pts',(22.8992616040108,4.38759397068406,0.));
#254152=CARTESIAN_POINT('Ctrl Pts',(22.8838521827701,4.38025605470093,0.));
#254153=CARTESIAN_POINT('Ctrl Pts',(22.8685416419725,4.37301972480746,0.));
#254154=CARTESIAN_POINT('Ctrl Pts',(22.8533314252422,4.36588498942997,0.));
#254155=CARTESIAN_POINT('Ctrl Pts',(22.8382230011184,4.35885185500546,0.));
#254156=CARTESIAN_POINT('Ctrl Pts',(22.8232178638876,4.35192032594791,0.));
#254157=CARTESIAN_POINT('Ctrl Pts',(22.8083175343791,4.34509040460062,0.));
#254158=CARTESIAN_POINT('Ctrl Pts',(22.7935235607806,4.33836209118446,0.));
#254159=CARTESIAN_POINT('Ctrl Pts',(22.7788375194076,4.3317353837319,0.));
#254160=CARTESIAN_POINT('Ctrl Pts',(22.7642610156475,4.32521027803754,0.));
#254161=CARTESIAN_POINT('Ctrl Pts',(22.7497956849848,4.31878676761235,0.));
#254162=CARTESIAN_POINT('Ctrl Pts',(22.7354431939926,4.31246484362549,0.));
#254163=CARTESIAN_POINT('Ctrl Pts',(22.7212052413386,4.30624449484069,0.));
#254164=CARTESIAN_POINT('Ctrl Pts',(22.7070835587564,4.3001257075406,0.));
#254165=CARTESIAN_POINT('Ctrl Pts',(22.6930799122548,4.29410846547056,0.));
#254166=CARTESIAN_POINT('Ctrl Pts',(22.6791961033537,4.28819274977763,0.));
#254167=CARTESIAN_POINT('Ctrl Pts',(22.6654339703109,4.28237853894059,0.));
#254168=CARTESIAN_POINT('Ctrl Pts',(22.6517953893303,4.2766658086912,0.));
#254169=CARTESIAN_POINT('Ctrl Pts',(22.6382822758172,4.27105453193004,0.));
#254170=CARTESIAN_POINT('Ctrl Pts',(22.6248965859977,4.26554467865576,0.));
#254171=CARTESIAN_POINT('Ctrl Pts',(22.6116403184821,4.26013621588305,0.));
#254172=CARTESIAN_POINT('Ctrl Pts',(22.5985155158636,4.25482910755481,0.));
#254173=CARTESIAN_POINT('Ctrl Pts',(22.5855242662477,4.24962331444177,0.));
#254174=CARTESIAN_POINT('Ctrl Pts',(22.572668704992,4.24451879404851,0.));
#254175=CARTESIAN_POINT('Ctrl Pts',(22.5599510166429,4.23951550052523,0.));
#254176=CARTESIAN_POINT('Ctrl Pts',(22.5473734368086,4.23461338456712,0.));
#254177=CARTESIAN_POINT('Ctrl Pts',(22.5349382540588,4.22981239330733,0.));
#254178=CARTESIAN_POINT('Ctrl Pts',(22.5226478117886,4.22511247020041,0.));
#254179=CARTESIAN_POINT('Ctrl Pts',(22.5105045108881,4.22051355490196,0.));
#254180=CARTESIAN_POINT('Ctrl Pts',(22.4985108124228,4.21601558313906,0.));
#254181=CARTESIAN_POINT('Ctrl Pts',(22.4866692403147,4.21161848657428,0.));
#254182=CARTESIAN_POINT('Ctrl Pts',(22.4749823839917,4.20732219265649,0.));
#254183=CARTESIAN_POINT('Ctrl Pts',(22.4634529011437,4.20312662448174,0.));
#254184=CARTESIAN_POINT('Ctrl Pts',(22.4520835205422,4.19903170066358,0.));
#254185=CARTESIAN_POINT('Ctrl Pts',(22.4408770448917,4.1950373351886,0.));
#254186=CARTESIAN_POINT('Ctrl Pts',(22.4298363535416,4.19114343726932,0.));
#254187=CARTESIAN_POINT('Ctrl Pts',(22.4189644056109,4.18734991117707,0.));
#254188=CARTESIAN_POINT('Ctrl Pts',(22.4082642454448,4.18365665600839,0.));
#254189=CARTESIAN_POINT('Ctrl Pts',(22.3977390078074,4.18006356544879,0.));
#254190=CARTESIAN_POINT('Ctrl Pts',(22.3873919231339,4.17657052752834,0.));
#254191=CARTESIAN_POINT('Ctrl Pts',(22.3772263228624,4.17317742436162,0.));
#254192=CARTESIAN_POINT('Ctrl Pts',(22.3672456427605,4.1698841319947,0.));
#254193=CARTESIAN_POINT('Ctrl Pts',(22.3574534257397,4.16669052026602,0.));
#254194=CARTESIAN_POINT('Ctrl Pts',(22.3478533253886,4.1635964526318,0.));
#254195=CARTESIAN_POINT('Ctrl Pts',(22.3384491078599,4.16060178604154,0.));
#254196=CARTESIAN_POINT('Ctrl Pts',(22.3292446628957,4.15770637047882,0.));
#254197=CARTESIAN_POINT('Ctrl Pts',(22.3202440186979,4.15491004835278,0.));
#254198=CARTESIAN_POINT('Ctrl Pts',(22.3114513545186,4.15221265396993,0.));
#254199=CARTESIAN_POINT('Ctrl Pts',(22.3028710166935,4.14961401285526,0.));
#254200=CARTESIAN_POINT('Ctrl Pts',(22.2945075198468,4.14711394168559,0.));
#254201=CARTESIAN_POINT('Ctrl Pts',(22.2863655389167,4.14471224859295,0.));
#254202=CARTESIAN_POINT('Ctrl Pts',(22.2784499072026,4.14240873321982,0.));
#254203=CARTESIAN_POINT('Ctrl Pts',(22.2707656042456,4.14020318715988,0.));
#254204=CARTESIAN_POINT('Ctrl Pts',(22.263317791397,4.13809539255419,0.));
#254205=CARTESIAN_POINT('Ctrl Pts',(22.2561118708422,4.13608511977226,0.));
#254206=CARTESIAN_POINT('Ctrl Pts',(22.2491535317789,4.13417212558809,0.));
#254207=CARTESIAN_POINT('Ctrl Pts',(22.2424488153523,4.1323561506016,0.));
#254208=CARTESIAN_POINT('Ctrl Pts',(22.2360040565534,4.13063692157499,0.));
#254209=CARTESIAN_POINT('Ctrl Pts',(22.2298258043947,4.12901415463379,0.));
#254210=CARTESIAN_POINT('Ctrl Pts',(22.2239207458781,4.127487558301,0.));
#254211=CARTESIAN_POINT('Ctrl Pts',(22.2182956401341,4.126056836133,0.));
#254212=CARTESIAN_POINT('Ctrl Pts',(22.2129576146671,4.12472167516602,0.));
#254213=CARTESIAN_POINT('Ctrl Pts',(22.2079143941719,4.12348173702025,0.));
#254214=CARTESIAN_POINT('Ctrl Pts',(22.2031746532106,4.12233664408237,0.));
#254215=CARTESIAN_POINT('Ctrl Pts',(22.1987479618246,4.12128598183533,0.));
#254216=CARTESIAN_POINT('Ctrl Pts',(22.1946440958098,4.12032932637738,0.));
#254217=CARTESIAN_POINT('Ctrl Pts',(22.1908725908525,4.11946626228623,0.));
#254218=CARTESIAN_POINT('Ctrl Pts',(22.1874419861496,4.11869641271752,0.));
#254219=CARTESIAN_POINT('Ctrl Pts',(22.1843613164855,4.11801938107464,0.));
#254220=CARTESIAN_POINT('Ctrl Pts',(22.1816414985788,4.11743469691765,0.));
#254221=CARTESIAN_POINT('Ctrl Pts',(22.179297473024,4.11694173195041,0.));
#254222=CARTESIAN_POINT('Ctrl Pts',(22.177347426894,4.11653973150558,0.));
#254223=CARTESIAN_POINT('Ctrl Pts',(22.1758088296598,4.11622797217066,0.));
#254224=CARTESIAN_POINT('Ctrl Pts',(22.1746949858773,4.11600589882768,0.));
#254225=CARTESIAN_POINT('Ctrl Pts',(22.174148802123,4.11589976826061,0.));
#254226=CARTESIAN_POINT('Ctrl Pts',(22.1739341411684,4.1158603587821,0.));
#254227=CARTESIAN_POINT('Ctrl Pts',(22.1738776823239,4.11585194677412,0.));
#254228=CARTESIAN_POINT('Ctrl Pts',(22.1738711152697,4.11585220600461,0.));
#254229=CARTESIAN_POINT('',(21.624941921198,4.01396149767428,0.));
#254230=CARTESIAN_POINT('',(11.0869355576349,2.05792610300232,0.));
#254231=CARTESIAN_POINT('',(21.2226420728916,3.44230496120419,0.));
#254232=CARTESIAN_POINT('Origin',(21.7161918885402,3.52235856495312,0.));
#254233=CARTESIAN_POINT('',(21.3904321633055,2.16781269186828,0.));
#254234=CARTESIAN_POINT('Origin',(7.7715611723761E-13,7.16093850883226E-14,
0.));
#254235=CARTESIAN_POINT('',(21.9269795755927,1.71975774210841,0.));
#254236=CARTESIAN_POINT('Origin',(21.8878840740801,2.21822694051638,0.));
#254237=CARTESIAN_POINT('',(22.4835757167854,1.76341220531179,0.));
#254238=CARTESIAN_POINT('',(10.7170877657712,0.840553282521227,0.));
#254239=CARTESIAN_POINT('',(25.991588367311,0.661312440730894,0.));
#254240=CARTESIAN_POINT('Ctrl Pts',(22.4835757167854,1.76341220531179,0.));
#254241=CARTESIAN_POINT('Ctrl Pts',(22.483581992979,1.76341415538764,0.));
#254242=CARTESIAN_POINT('Ctrl Pts',(22.4836387052232,1.7634206426357,0.));
#254243=CARTESIAN_POINT('Ctrl Pts',(22.4838562517069,1.76343813434565,0.));
#254244=CARTESIAN_POINT('Ctrl Pts',(22.4844112933129,1.76347698284792,0.));
#254245=CARTESIAN_POINT('Ctrl Pts',(22.4855446605991,1.76355076045546,0.));
#254246=CARTESIAN_POINT('Ctrl Pts',(22.4871115206571,1.76364784232963,0.));
#254247=CARTESIAN_POINT('Ctrl Pts',(22.4890991659478,1.76376424879505,0.));
#254248=CARTESIAN_POINT('Ctrl Pts',(22.4914909094908,1.76389475965724,0.));
#254249=CARTESIAN_POINT('Ctrl Pts',(22.4942693792449,1.76403393880301,0.));
#254250=CARTESIAN_POINT('Ctrl Pts',(22.4974203063191,1.76417731243462,0.));
#254251=CARTESIAN_POINT('Ctrl Pts',(22.5009332677316,1.76432160068726,0.));
#254252=CARTESIAN_POINT('Ctrl Pts',(22.5047996391978,1.76446408210366,0.));
#254253=CARTESIAN_POINT('Ctrl Pts',(22.5090112700212,1.76460218257323,0.));
#254254=CARTESIAN_POINT('Ctrl Pts',(22.5135590569554,1.76473303281159,0.));
#254255=CARTESIAN_POINT('Ctrl Pts',(22.5184336670207,1.76485369319896,0.));
#254256=CARTESIAN_POINT('Ctrl Pts',(22.5236259635515,1.76496128643369,0.));
#254257=CARTESIAN_POINT('Ctrl Pts',(22.529127665298,1.76505320262752,0.));
#254258=CARTESIAN_POINT('Ctrl Pts',(22.5349313983571,1.7651271156325,0.));
#254259=CARTESIAN_POINT('Ctrl Pts',(22.5410303590891,1.76518087841493,0.));
#254260=CARTESIAN_POINT('Ctrl Pts',(22.5474180954006,1.76521245524047,0.));
#254261=CARTESIAN_POINT('Ctrl Pts',(22.5540882235837,1.76521983384063,0.));
#254262=CARTESIAN_POINT('Ctrl Pts',(22.5610344912501,1.7652010450045,0.));
#254263=CARTESIAN_POINT('Ctrl Pts',(22.5682508499873,1.76515418518829,0.));
#254264=CARTESIAN_POINT('Ctrl Pts',(22.5757315316355,1.76507744026747,0.));
#254265=CARTESIAN_POINT('Ctrl Pts',(22.5834711038024,1.76496910283089,0.));
#254266=CARTESIAN_POINT('Ctrl Pts',(22.5914644078106,1.76482755288411,0.));
#254267=CARTESIAN_POINT('Ctrl Pts',(22.5997065145638,1.76465124413556,0.));
#254268=CARTESIAN_POINT('Ctrl Pts',(22.6081926681342,1.76443868648015,0.));
#254269=CARTESIAN_POINT('Ctrl Pts',(22.6169182517693,1.76418843543739,0.));
#254270=CARTESIAN_POINT('Ctrl Pts',(22.6258787994847,1.76389909571402,0.));
#254271=CARTESIAN_POINT('Ctrl Pts',(22.635069997936,1.76356932176272,0.));
#254272=CARTESIAN_POINT('Ctrl Pts',(22.6444876940425,1.76319782013914,0.));
#254273=CARTESIAN_POINT('Ctrl Pts',(22.6541278938413,1.76278334912559,0.));
#254274=CARTESIAN_POINT('Ctrl Pts',(22.6639867471756,1.76232471392568,0.));
#254275=CARTESIAN_POINT('Ctrl Pts',(22.6740605356699,1.76182076289525,0.));
#254276=CARTESIAN_POINT('Ctrl Pts',(22.6843456585245,1.76127038310613,0.));
#254277=CARTESIAN_POINT('Ctrl Pts',(22.6948386219843,1.76067249704884,0.));
#254278=CARTESIAN_POINT('Ctrl Pts',(22.7055360375481,1.76002606202399,0.));
#254279=CARTESIAN_POINT('Ctrl Pts',(22.7164346186007,1.75933006905924,0.));
#254280=CARTESIAN_POINT('Ctrl Pts',(22.7275311777305,1.75858354204635,0.));
#254281=CARTESIAN_POINT('Ctrl Pts',(22.7388226235565,1.75778553673249,0.));
#254282=CARTESIAN_POINT('Ctrl Pts',(22.7503059556455,1.75693513908911,0.));
#254283=CARTESIAN_POINT('Ctrl Pts',(22.7619782595013,1.75603146371641,0.));
#254284=CARTESIAN_POINT('Ctrl Pts',(22.7738367016115,1.75507365227127,0.));
#254285=CARTESIAN_POINT('Ctrl Pts',(22.7858785242358,1.7540608718293,0.));
#254286=CARTESIAN_POINT('Ctrl Pts',(22.7981010424312,1.75299231391461,0.));
#254287=CARTESIAN_POINT('Ctrl Pts',(22.8105016414712,1.7518671936559,0.));
#254288=CARTESIAN_POINT('Ctrl Pts',(22.8230777741285,1.75068474890884,0.));
#254289=CARTESIAN_POINT('Ctrl Pts',(22.8358269579854,1.74944423940117,0.));
#254290=CARTESIAN_POINT('Ctrl Pts',(22.8487467728075,1.74814494588492,0.));
#254291=CARTESIAN_POINT('Ctrl Pts',(22.8618348580234,1.74678616930663,0.));
#254292=CARTESIAN_POINT('Ctrl Pts',(22.8750889101696,1.745367229982,0.));
#254293=CARTESIAN_POINT('Ctrl Pts',(22.8885066803351,1.74388746677702,0.));
#254294=CARTESIAN_POINT('Ctrl Pts',(22.9020859716144,1.74234623630079,0.));
#254295=CARTESIAN_POINT('Ctrl Pts',(22.9158246373365,1.74074291231057,0.));
#254296=CARTESIAN_POINT('Ctrl Pts',(22.9297205792587,1.73907688511665,0.));
#254297=CARTESIAN_POINT('Ctrl Pts',(22.9437717457825,1.73734756100038,0.));
#254298=CARTESIAN_POINT('Ctrl Pts',(22.9579761301062,1.73555436162771,0.));
#254299=CARTESIAN_POINT('Ctrl Pts',(22.9723317685688,1.73369672350818,0.));
#254300=CARTESIAN_POINT('Ctrl Pts',(22.9868367391978,1.73177409750194,0.));
#254301=CARTESIAN_POINT('Ctrl Pts',(23.0014891601891,1.72978594832137,0.));
#254302=CARTESIAN_POINT('Ctrl Pts',(23.0162871884167,1.72773175404703,0.));
#254303=CARTESIAN_POINT('Ctrl Pts',(23.031229017888,1.72561100564033,0.));
#254304=CARTESIAN_POINT('Ctrl Pts',(23.0463128785528,1.72342320653731,0.));
#254305=CARTESIAN_POINT('Ctrl Pts',(23.0615370351559,1.72116787225981,0.));
#254306=CARTESIAN_POINT('Ctrl Pts',(23.0768997860709,1.71884453003027,0.));
#254307=CARTESIAN_POINT('Ctrl Pts',(23.0923994621216,1.71645271839311,0.));
#254308=CARTESIAN_POINT('Ctrl Pts',(23.1080344254291,1.71399198684725,0.));
#254309=CARTESIAN_POINT('Ctrl Pts',(23.1238030684929,1.71146189552192,0.));
#254310=CARTESIAN_POINT('Ctrl Pts',(23.1397038132358,1.7088620148546,0.));
#254311=CARTESIAN_POINT('Ctrl Pts',(23.1557351100613,1.70619192527847,0.));
#254312=CARTESIAN_POINT('Ctrl Pts',(23.1718954368749,1.70345121691259,0.));
#254313=CARTESIAN_POINT('Ctrl Pts',(23.1881832981848,1.70063948926988,0.));
#254314=CARTESIAN_POINT('Ctrl Pts',(23.2045972243765,1.69775635099425,0.));
#254315=CARTESIAN_POINT('Ctrl Pts',(23.2211357709374,1.69480141959946,0.));
#254316=CARTESIAN_POINT('Ctrl Pts',(23.2377975177014,1.69177432121716,0.));
#254317=CARTESIAN_POINT('Ctrl Pts',(23.2545810680536,1.6886746903491,0.));
#254318=CARTESIAN_POINT('Ctrl Pts',(23.2714850482245,1.68550216963275,0.));
#254319=CARTESIAN_POINT('Ctrl Pts',(23.2885081066949,1.68225640962181,0.));
#254320=CARTESIAN_POINT('Ctrl Pts',(23.3056489135611,1.67893706857123,0.));
#254321=CARTESIAN_POINT('Ctrl Pts',(23.3229061599145,1.67554381222988,0.));
#254322=CARTESIAN_POINT('Ctrl Pts',(23.3402785571866,1.67207631363905,0.));
#254323=CARTESIAN_POINT('Ctrl Pts',(23.3577648365747,1.66853425293978,0.));
#254324=CARTESIAN_POINT('Ctrl Pts',(23.375363748555,1.66491731718864,0.));
#254325=CARTESIAN_POINT('Ctrl Pts',(23.3930740623622,1.66122520018008,0.));
#254326=CARTESIAN_POINT('Ctrl Pts',(23.4108945654803,1.65745760227507,0.));
#254327=CARTESIAN_POINT('Ctrl Pts',(23.4288240631034,1.6536142302373,0.));
#254328=CARTESIAN_POINT('Ctrl Pts',(23.446861377656,1.6496947970734,0.));
#254329=CARTESIAN_POINT('Ctrl Pts',(23.4650053483919,1.64569902187608,0.));
#254330=CARTESIAN_POINT('Ctrl Pts',(23.4832548309638,1.64162662967525,0.));
#254331=CARTESIAN_POINT('Ctrl Pts',(23.5016086970006,1.63747735129474,0.));
#254332=CARTESIAN_POINT('Ctrl Pts',(23.5200658336624,1.63325092321731,0.));
#254333=CARTESIAN_POINT('Ctrl Pts',(23.5386251432278,1.62894708745231,0.));
#254334=CARTESIAN_POINT('Ctrl Pts',(23.5572855427617,1.62456559140072,0.));
#254335=CARTESIAN_POINT('Ctrl Pts',(23.5760459637608,1.62010618772869,0.));
#254336=CARTESIAN_POINT('Ctrl Pts',(23.5949053517996,1.61556863424697,0.));
#254337=CARTESIAN_POINT('Ctrl Pts',(23.6138626661644,1.61095269379773,0.));
#254338=CARTESIAN_POINT('Ctrl Pts',(23.6329168794916,1.60625813414666,0.));
#254339=CARTESIAN_POINT('Ctrl Pts',(23.6520669774863,1.60148472786588,0.));
#254340=CARTESIAN_POINT('Ctrl Pts',(23.6713119586302,1.59663225222459,0.));
#254341=CARTESIAN_POINT('Ctrl Pts',(23.6906508338832,1.59170048908631,0.));
#254342=CARTESIAN_POINT('Ctrl Pts',(23.7100826263835,1.58668922481222,0.));
#254343=CARTESIAN_POINT('Ctrl Pts',(23.7296063711308,1.58159825017362,0.));
#254344=CARTESIAN_POINT('Ctrl Pts',(23.7492211147369,1.57642736025251,0.));
#254345=CARTESIAN_POINT('Ctrl Pts',(23.7689259151869,1.57117635434412,0.));
#254346=CARTESIAN_POINT('Ctrl Pts',(23.788719841588,1.56584503586844,0.));
#254347=CARTESIAN_POINT('Ctrl Pts',(23.8086019739192,1.56043321228631,0.));
#254348=CARTESIAN_POINT('Ctrl Pts',(23.8285714027631,1.55494069502628,0.));
#254349=CARTESIAN_POINT('Ctrl Pts',(23.8486272290698,1.5493672994053,0.));
#254350=CARTESIAN_POINT('Ctrl Pts',(23.8687685639635,1.54371284453978,0.));
#254351=CARTESIAN_POINT('Ctrl Pts',(23.8889945285313,1.53797715326748,0.));
#254352=CARTESIAN_POINT('Ctrl Pts',(23.9093042536119,1.53216005207462,0.));
#254353=CARTESIAN_POINT('Ctrl Pts',(23.9296968795761,1.5262613710304,0.));
#254354=CARTESIAN_POINT('Ctrl Pts',(23.9501715561038,1.52028094372806,0.));
#254355=CARTESIAN_POINT('Ctrl Pts',(23.9707274420145,1.51421860720628,0.));
#254356=CARTESIAN_POINT('Ctrl Pts',(23.991363705093,1.50807420187703,0.));
#254357=CARTESIAN_POINT('Ctrl Pts',(24.0120795219086,1.50184757146099,0.));
#254358=CARTESIAN_POINT('Ctrl Pts',(24.0328740776331,1.49553856292798,0.));
#254359=CARTESIAN_POINT('Ctrl Pts',(24.053746565843,1.48914702644883,0.));
#254360=CARTESIAN_POINT('Ctrl Pts',(24.074696188353,1.4826728153368,0.));
#254361=CARTESIAN_POINT('Ctrl Pts',(24.0957221550782,1.47611578597742,0.));
#254362=CARTESIAN_POINT('Ctrl Pts',(24.1168236838827,1.46947579776992,0.));
#254363=CARTESIAN_POINT('Ctrl Pts',(24.1380000004272,1.46275271307398,0.));
#254364=CARTESIAN_POINT('Ctrl Pts',(24.1592503380105,1.45594639716314,0.));
#254365=CARTESIAN_POINT('Ctrl Pts',(24.1805739374033,1.44905671818721,0.));
#254366=CARTESIAN_POINT('Ctrl Pts',(24.2019700467214,1.44208354711074,0.));
#254367=CARTESIAN_POINT('Ctrl Pts',(24.2234379212978,1.43502675765502,0.));
#254368=CARTESIAN_POINT('Ctrl Pts',(24.2449768235485,1.42788622624851,0.));
#254369=CARTESIAN_POINT('Ctrl Pts',(24.2665860228357,1.42066183198252,0.));
#254370=CARTESIAN_POINT('Ctrl Pts',(24.2882647953214,1.41335345657685,0.));
#254371=CARTESIAN_POINT('Ctrl Pts',(24.3100124238316,1.40596098434341,0.));
#254372=CARTESIAN_POINT('Ctrl Pts',(24.3318281977647,1.3984843021281,0.));
#254373=CARTESIAN_POINT('Ctrl Pts',(24.3537114129877,1.3909232992639,0.));
#254374=CARTESIAN_POINT('Ctrl Pts',(24.37566137173,1.38327786752998,0.));
#254375=CARTESIAN_POINT('Ctrl Pts',(24.3976773824731,1.37554790111608,0.));
#254376=CARTESIAN_POINT('Ctrl Pts',(24.4197587598337,1.36773329659954,0.));
#254377=CARTESIAN_POINT('Ctrl Pts',(24.4419048244524,1.35983395290624,0.));
#254378=CARTESIAN_POINT('Ctrl Pts',(24.4641149028894,1.35184977125645,0.));
#254379=CARTESIAN_POINT('Ctrl Pts',(24.4863883275135,1.34378065512335,0.));
#254380=CARTESIAN_POINT('Ctrl Pts',(24.5087244363856,1.33562651019684,0.));
#254381=CARTESIAN_POINT('Ctrl Pts',(24.5311225731434,1.32738724435326,0.));
#254382=CARTESIAN_POINT('Ctrl Pts',(24.5535820868671,1.31906276763669,0.));
#254383=CARTESIAN_POINT('Ctrl Pts',(24.576102332018,1.31065299222023,0.));
#254384=CARTESIAN_POINT('Ctrl Pts',(24.5986826684025,1.30215783236364,0.));
#254385=CARTESIAN_POINT('Ctrl Pts',(24.6213224611228,1.29357720438108,0.));
#254386=CARTESIAN_POINT('Ctrl Pts',(24.6440210805278,1.28491102661514,0.));
#254387=CARTESIAN_POINT('Ctrl Pts',(24.666777902156,1.2761592194164,0.));
#254388=CARTESIAN_POINT('Ctrl Pts',(24.6895923066837,1.26732170513497,0.));
#254389=CARTESIAN_POINT('Ctrl Pts',(24.7124636797895,1.25839840807415,0.));
#254390=CARTESIAN_POINT('Ctrl Pts',(24.7353914120012,1.24938925444324,0.));
#254391=CARTESIAN_POINT('Ctrl Pts',(24.7583748985439,1.24029417231988,0.));
#254392=CARTESIAN_POINT('Ctrl Pts',(24.78141353918,1.23111309161843,0.));
#254393=CARTESIAN_POINT('Ctrl Pts',(24.8045067380536,1.22184594406527,0.));
#254394=CARTESIAN_POINT('Ctrl Pts',(24.8276539035092,1.21249266318205,0.));
#254395=CARTESIAN_POINT('Ctrl Pts',(24.8508544481973,1.20305318426016,0.));
#254396=CARTESIAN_POINT('Ctrl Pts',(24.8741077892074,1.19352744434059,0.));
#254397=CARTESIAN_POINT('Ctrl Pts',(24.8974133481829,1.18391538220098,0.));
#254398=CARTESIAN_POINT('Ctrl Pts',(24.9207705514449,1.1742169383504,0.));
#254399=CARTESIAN_POINT('Ctrl Pts',(24.9441788300932,1.16443205502852,0.));
#254400=CARTESIAN_POINT('Ctrl Pts',(24.9676376201501,1.15456067621894,0.));
#254401=CARTESIAN_POINT('Ctrl Pts',(24.9911463621431,1.14460274758206,0.));
#254402=CARTESIAN_POINT('Ctrl Pts',(25.0147045006193,1.13455821638536,0.));
#254403=CARTESIAN_POINT('Ctrl Pts',(25.0383114836898,1.12442703144455,0.));
#254404=CARTESIAN_POINT('Ctrl Pts',(25.0619667625336,1.1142091430689,0.));
#254405=CARTESIAN_POINT('Ctrl Pts',(25.085669790968,1.10390450301741,0.));
#254406=CARTESIAN_POINT('Ctrl Pts',(25.1094200248448,1.09351306445299,0.));
#254407=CARTESIAN_POINT('Ctrl Pts',(25.1332169227415,1.08303478197174,0.));
#254408=CARTESIAN_POINT('Ctrl Pts',(25.1570599469311,1.0724696116546,0.));
#254409=CARTESIAN_POINT('Ctrl Pts',(25.1809485642191,1.06181751111754,0.));
#254410=CARTESIAN_POINT('Ctrl Pts',(25.2048822469027,1.05107843957926,0.));
#254411=CARTESIAN_POINT('Ctrl Pts',(25.2288604735087,1.04025235791515,0.));
#254412=CARTESIAN_POINT('Ctrl Pts',(25.2528827300427,1.0293392287683,0.));
#254413=CARTESIAN_POINT('Ctrl Pts',(25.2769485087268,1.01833901642273,0.));
#254414=CARTESIAN_POINT('Ctrl Pts',(25.3010573055557,1.00725168656934,0.));
#254415=CARTESIAN_POINT('Ctrl Pts',(25.3252086182976,0.996077206120921,
0.));
#254416=CARTESIAN_POINT('Ctrl Pts',(25.3494019441444,0.984815543004091,
0.));
#254417=CARTESIAN_POINT('Ctrl Pts',(25.3736367778842,0.97346666600005,0.));
#254418=CARTESIAN_POINT('Ctrl Pts',(25.3979126089155,0.962030544502806,
0.));
#254419=CARTESIAN_POINT('Ctrl Pts',(25.4222289223155,0.950507148596971,
0.));
#254420=CARTESIAN_POINT('Ctrl Pts',(25.4465852044835,0.938896449495636,
0.));
#254421=CARTESIAN_POINT('Ctrl Pts',(25.4709809474996,0.927198419885607,
0.));
#254422=CARTESIAN_POINT('Ctrl Pts',(25.4954156541787,0.915413034335334,
0.));
#254423=CARTESIAN_POINT('Ctrl Pts',(25.5198888424195,0.903540269651155,
0.));
#254424=CARTESIAN_POINT('Ctrl Pts',(25.5444000508223,0.891580105349469,
0.));
#254425=CARTESIAN_POINT('Ctrl Pts',(25.568948840818,0.879532523835094,0.));
#254426=CARTESIAN_POINT('Ctrl Pts',(25.5935347843616,0.867397509339473,
0.));
#254427=CARTESIAN_POINT('Ctrl Pts',(25.618157453608,0.855175047037618,0.));
#254428=CARTESIAN_POINT('Ctrl Pts',(25.6428164100078,0.842865122121547,
0.));
#254429=CARTESIAN_POINT('Ctrl Pts',(25.6675111931957,0.83046771886437,0.));
#254430=CARTESIAN_POINT('Ctrl Pts',(25.6922413110172,0.817982819786722,
0.));
#254431=CARTESIAN_POINT('Ctrl Pts',(25.7170062262474,0.805410404552597,
0.));
#254432=CARTESIAN_POINT('Ctrl Pts',(25.7418053757671,0.792750451613538,
0.));
#254433=CARTESIAN_POINT('Ctrl Pts',(25.7666381946871,0.780002940289028,
0.));
#254434=CARTESIAN_POINT('Ctrl Pts',(25.7915041383304,0.767167852648643,
0.));
#254435=CARTESIAN_POINT('Ctrl Pts',(25.816402705995,0.754245175608291,0.));
#254436=CARTESIAN_POINT('Ctrl Pts',(25.841333461908,0.741234902664698,0.));
#254437=CARTESIAN_POINT('Ctrl Pts',(25.8662960624285,0.728137036485881,
0.));
#254438=CARTESIAN_POINT('Ctrl Pts',(25.8912902615141,0.714951588533756,
0.));
#254439=CARTESIAN_POINT('Ctrl Pts',(25.9163158909645,0.701678575236605,
0.));
#254440=CARTESIAN_POINT('Ctrl Pts',(25.941372847213,0.68831801506568,0.));
#254441=CARTESIAN_POINT('Ctrl Pts',(25.9614434298092,0.677559543215907,
0.));
#254442=CARTESIAN_POINT('Ctrl Pts',(25.9765104298171,0.669451306784419,
0.));
#254443=CARTESIAN_POINT('Ctrl Pts',(25.9865613464809,0.664028313188916,
0.));
#254444=CARTESIAN_POINT('Ctrl Pts',(25.991588367311,0.661312440730894,0.));
#254445=CARTESIAN_POINT('Origin',(0.,0.,0.));
#254446=CARTESIAN_POINT('',(-7.,-8.57252759403147E-16,0.));
#254447=CARTESIAN_POINT('Origin',(0.,0.,0.));
#254448=CARTESIAN_POINT('Origin',(0.,0.,12.));
#254449=CARTESIAN_POINT('',(25.991588367311,0.661312440730894,12.));
#254450=CARTESIAN_POINT('Origin',(0.,0.,12.));
#254451=CARTESIAN_POINT('',(22.4835757167854,1.76341220531179,12.));
#254452=CARTESIAN_POINT('Ctrl Pts',(25.991588367311,0.661312440730894,12.));
#254453=CARTESIAN_POINT('Ctrl Pts',(25.9865613464809,0.664028313188916,
12.));
#254454=CARTESIAN_POINT('Ctrl Pts',(25.9765104298171,0.669451306784419,
12.));
#254455=CARTESIAN_POINT('Ctrl Pts',(25.9614434298092,0.677559543215907,
12.));
#254456=CARTESIAN_POINT('Ctrl Pts',(25.941372847213,0.68831801506568,12.));
#254457=CARTESIAN_POINT('Ctrl Pts',(25.9163158909645,0.701678575236605,
12.));
#254458=CARTESIAN_POINT('Ctrl Pts',(25.8912902615141,0.714951588533756,
12.));
#254459=CARTESIAN_POINT('Ctrl Pts',(25.8662960624285,0.728137036485881,
12.));
#254460=CARTESIAN_POINT('Ctrl Pts',(25.841333461908,0.741234902664698,12.));
#254461=CARTESIAN_POINT('Ctrl Pts',(25.816402705995,0.754245175608291,12.));
#254462=CARTESIAN_POINT('Ctrl Pts',(25.7915041383304,0.767167852648643,
12.));
#254463=CARTESIAN_POINT('Ctrl Pts',(25.7666381946871,0.780002940289028,
12.));
#254464=CARTESIAN_POINT('Ctrl Pts',(25.7418053757671,0.792750451613538,
12.));
#254465=CARTESIAN_POINT('Ctrl Pts',(25.7170062262474,0.805410404552597,
12.));
#254466=CARTESIAN_POINT('Ctrl Pts',(25.6922413110172,0.817982819786722,
12.));
#254467=CARTESIAN_POINT('Ctrl Pts',(25.6675111931957,0.83046771886437,12.));
#254468=CARTESIAN_POINT('Ctrl Pts',(25.6428164100078,0.842865122121547,
12.));
#254469=CARTESIAN_POINT('Ctrl Pts',(25.618157453608,0.855175047037618,12.));
#254470=CARTESIAN_POINT('Ctrl Pts',(25.5935347843616,0.867397509339473,
12.));
#254471=CARTESIAN_POINT('Ctrl Pts',(25.568948840818,0.879532523835094,12.));
#254472=CARTESIAN_POINT('Ctrl Pts',(25.5444000508223,0.891580105349469,
12.));
#254473=CARTESIAN_POINT('Ctrl Pts',(25.5198888424195,0.903540269651155,
12.));
#254474=CARTESIAN_POINT('Ctrl Pts',(25.4954156541787,0.915413034335334,
12.));
#254475=CARTESIAN_POINT('Ctrl Pts',(25.4709809474996,0.927198419885607,
12.));
#254476=CARTESIAN_POINT('Ctrl Pts',(25.4465852044835,0.938896449495636,
12.));
#254477=CARTESIAN_POINT('Ctrl Pts',(25.4222289223155,0.950507148596971,
12.));
#254478=CARTESIAN_POINT('Ctrl Pts',(25.3979126089155,0.962030544502806,
12.));
#254479=CARTESIAN_POINT('Ctrl Pts',(25.3736367778842,0.97346666600005,12.));
#254480=CARTESIAN_POINT('Ctrl Pts',(25.3494019441444,0.984815543004091,
12.));
#254481=CARTESIAN_POINT('Ctrl Pts',(25.3252086182976,0.996077206120921,
12.));
#254482=CARTESIAN_POINT('Ctrl Pts',(25.3010573055557,1.00725168656934,12.));
#254483=CARTESIAN_POINT('Ctrl Pts',(25.2769485087268,1.01833901642273,12.));
#254484=CARTESIAN_POINT('Ctrl Pts',(25.2528827300427,1.0293392287683,12.));
#254485=CARTESIAN_POINT('Ctrl Pts',(25.2288604735087,1.04025235791515,12.));
#254486=CARTESIAN_POINT('Ctrl Pts',(25.2048822469027,1.05107843957926,12.));
#254487=CARTESIAN_POINT('Ctrl Pts',(25.1809485642191,1.06181751111754,12.));
#254488=CARTESIAN_POINT('Ctrl Pts',(25.1570599469311,1.0724696116546,12.));
#254489=CARTESIAN_POINT('Ctrl Pts',(25.1332169227415,1.08303478197174,12.));
#254490=CARTESIAN_POINT('Ctrl Pts',(25.1094200248448,1.09351306445299,12.));
#254491=CARTESIAN_POINT('Ctrl Pts',(25.085669790968,1.10390450301741,12.));
#254492=CARTESIAN_POINT('Ctrl Pts',(25.0619667625336,1.1142091430689,12.));
#254493=CARTESIAN_POINT('Ctrl Pts',(25.0383114836898,1.12442703144455,12.));
#254494=CARTESIAN_POINT('Ctrl Pts',(25.0147045006193,1.13455821638536,12.));
#254495=CARTESIAN_POINT('Ctrl Pts',(24.9911463621431,1.14460274758206,12.));
#254496=CARTESIAN_POINT('Ctrl Pts',(24.9676376201501,1.15456067621894,12.));
#254497=CARTESIAN_POINT('Ctrl Pts',(24.9441788300932,1.16443205502852,12.));
#254498=CARTESIAN_POINT('Ctrl Pts',(24.9207705514449,1.1742169383504,12.));
#254499=CARTESIAN_POINT('Ctrl Pts',(24.8974133481829,1.18391538220098,12.));
#254500=CARTESIAN_POINT('Ctrl Pts',(24.8741077892074,1.19352744434059,12.));
#254501=CARTESIAN_POINT('Ctrl Pts',(24.8508544481973,1.20305318426016,12.));
#254502=CARTESIAN_POINT('Ctrl Pts',(24.8276539035092,1.21249266318205,12.));
#254503=CARTESIAN_POINT('Ctrl Pts',(24.8045067380536,1.22184594406527,12.));
#254504=CARTESIAN_POINT('Ctrl Pts',(24.78141353918,1.23111309161843,12.));
#254505=CARTESIAN_POINT('Ctrl Pts',(24.7583748985439,1.24029417231988,12.));
#254506=CARTESIAN_POINT('Ctrl Pts',(24.7353914120012,1.24938925444324,12.));
#254507=CARTESIAN_POINT('Ctrl Pts',(24.7124636797895,1.25839840807415,12.));
#254508=CARTESIAN_POINT('Ctrl Pts',(24.6895923066837,1.26732170513497,12.));
#254509=CARTESIAN_POINT('Ctrl Pts',(24.666777902156,1.2761592194164,12.));
#254510=CARTESIAN_POINT('Ctrl Pts',(24.6440210805278,1.28491102661514,12.));
#254511=CARTESIAN_POINT('Ctrl Pts',(24.6213224611228,1.29357720438108,12.));
#254512=CARTESIAN_POINT('Ctrl Pts',(24.5986826684025,1.30215783236364,12.));
#254513=CARTESIAN_POINT('Ctrl Pts',(24.576102332018,1.31065299222023,12.));
#254514=CARTESIAN_POINT('Ctrl Pts',(24.5535820868671,1.31906276763669,12.));
#254515=CARTESIAN_POINT('Ctrl Pts',(24.5311225731434,1.32738724435326,12.));
#254516=CARTESIAN_POINT('Ctrl Pts',(24.5087244363856,1.33562651019684,12.));
#254517=CARTESIAN_POINT('Ctrl Pts',(24.4863883275135,1.34378065512335,12.));
#254518=CARTESIAN_POINT('Ctrl Pts',(24.4641149028894,1.35184977125645,12.));
#254519=CARTESIAN_POINT('Ctrl Pts',(24.4419048244524,1.35983395290624,12.));
#254520=CARTESIAN_POINT('Ctrl Pts',(24.4197587598337,1.36773329659954,12.));
#254521=CARTESIAN_POINT('Ctrl Pts',(24.3976773824731,1.37554790111608,12.));
#254522=CARTESIAN_POINT('Ctrl Pts',(24.37566137173,1.38327786752998,12.));
#254523=CARTESIAN_POINT('Ctrl Pts',(24.3537114129877,1.3909232992639,12.));
#254524=CARTESIAN_POINT('Ctrl Pts',(24.3318281977647,1.3984843021281,12.));
#254525=CARTESIAN_POINT('Ctrl Pts',(24.3100124238316,1.40596098434341,12.));
#254526=CARTESIAN_POINT('Ctrl Pts',(24.2882647953214,1.41335345657685,12.));
#254527=CARTESIAN_POINT('Ctrl Pts',(24.2665860228357,1.42066183198252,12.));
#254528=CARTESIAN_POINT('Ctrl Pts',(24.2449768235485,1.42788622624851,12.));
#254529=CARTESIAN_POINT('Ctrl Pts',(24.2234379212978,1.43502675765502,12.));
#254530=CARTESIAN_POINT('Ctrl Pts',(24.2019700467214,1.44208354711074,12.));
#254531=CARTESIAN_POINT('Ctrl Pts',(24.1805739374033,1.44905671818721,12.));
#254532=CARTESIAN_POINT('Ctrl Pts',(24.1592503380105,1.45594639716314,12.));
#254533=CARTESIAN_POINT('Ctrl Pts',(24.1380000004272,1.46275271307398,12.));
#254534=CARTESIAN_POINT('Ctrl Pts',(24.1168236838827,1.46947579776992,12.));
#254535=CARTESIAN_POINT('Ctrl Pts',(24.0957221550782,1.47611578597742,12.));
#254536=CARTESIAN_POINT('Ctrl Pts',(24.074696188353,1.4826728153368,12.));
#254537=CARTESIAN_POINT('Ctrl Pts',(24.053746565843,1.48914702644883,12.));
#254538=CARTESIAN_POINT('Ctrl Pts',(24.0328740776331,1.49553856292798,12.));
#254539=CARTESIAN_POINT('Ctrl Pts',(24.0120795219086,1.50184757146099,12.));
#254540=CARTESIAN_POINT('Ctrl Pts',(23.991363705093,1.50807420187703,12.));
#254541=CARTESIAN_POINT('Ctrl Pts',(23.9707274420145,1.51421860720628,12.));
#254542=CARTESIAN_POINT('Ctrl Pts',(23.9501715561038,1.52028094372806,12.));
#254543=CARTESIAN_POINT('Ctrl Pts',(23.9296968795761,1.5262613710304,12.));
#254544=CARTESIAN_POINT('Ctrl Pts',(23.9093042536119,1.53216005207462,12.));
#254545=CARTESIAN_POINT('Ctrl Pts',(23.8889945285313,1.53797715326748,12.));
#254546=CARTESIAN_POINT('Ctrl Pts',(23.8687685639635,1.54371284453978,12.));
#254547=CARTESIAN_POINT('Ctrl Pts',(23.8486272290698,1.5493672994053,12.));
#254548=CARTESIAN_POINT('Ctrl Pts',(23.8285714027631,1.55494069502628,12.));
#254549=CARTESIAN_POINT('Ctrl Pts',(23.8086019739192,1.56043321228631,12.));
#254550=CARTESIAN_POINT('Ctrl Pts',(23.788719841588,1.56584503586844,12.));
#254551=CARTESIAN_POINT('Ctrl Pts',(23.7689259151869,1.57117635434412,12.));
#254552=CARTESIAN_POINT('Ctrl Pts',(23.7492211147369,1.57642736025251,12.));
#254553=CARTESIAN_POINT('Ctrl Pts',(23.7296063711308,1.58159825017362,12.));
#254554=CARTESIAN_POINT('Ctrl Pts',(23.7100826263835,1.58668922481222,12.));
#254555=CARTESIAN_POINT('Ctrl Pts',(23.6906508338832,1.59170048908631,12.));
#254556=CARTESIAN_POINT('Ctrl Pts',(23.6713119586302,1.59663225222459,12.));
#254557=CARTESIAN_POINT('Ctrl Pts',(23.6520669774863,1.60148472786588,12.));
#254558=CARTESIAN_POINT('Ctrl Pts',(23.6329168794916,1.60625813414666,12.));
#254559=CARTESIAN_POINT('Ctrl Pts',(23.6138626661644,1.61095269379773,12.));
#254560=CARTESIAN_POINT('Ctrl Pts',(23.5949053517996,1.61556863424697,12.));
#254561=CARTESIAN_POINT('Ctrl Pts',(23.5760459637608,1.62010618772869,12.));
#254562=CARTESIAN_POINT('Ctrl Pts',(23.5572855427617,1.62456559140072,12.));
#254563=CARTESIAN_POINT('Ctrl Pts',(23.5386251432278,1.62894708745231,12.));
#254564=CARTESIAN_POINT('Ctrl Pts',(23.5200658336624,1.63325092321731,12.));
#254565=CARTESIAN_POINT('Ctrl Pts',(23.5016086970006,1.63747735129474,12.));
#254566=CARTESIAN_POINT('Ctrl Pts',(23.4832548309638,1.64162662967525,12.));
#254567=CARTESIAN_POINT('Ctrl Pts',(23.4650053483919,1.64569902187608,12.));
#254568=CARTESIAN_POINT('Ctrl Pts',(23.446861377656,1.6496947970734,12.));
#254569=CARTESIAN_POINT('Ctrl Pts',(23.4288240631034,1.6536142302373,12.));
#254570=CARTESIAN_POINT('Ctrl Pts',(23.4108945654803,1.65745760227507,12.));
#254571=CARTESIAN_POINT('Ctrl Pts',(23.3930740623622,1.66122520018008,12.));
#254572=CARTESIAN_POINT('Ctrl Pts',(23.375363748555,1.66491731718864,12.));
#254573=CARTESIAN_POINT('Ctrl Pts',(23.3577648365747,1.66853425293978,12.));
#254574=CARTESIAN_POINT('Ctrl Pts',(23.3402785571866,1.67207631363905,12.));
#254575=CARTESIAN_POINT('Ctrl Pts',(23.3229061599145,1.67554381222988,12.));
#254576=CARTESIAN_POINT('Ctrl Pts',(23.3056489135611,1.67893706857123,12.));
#254577=CARTESIAN_POINT('Ctrl Pts',(23.2885081066949,1.68225640962181,12.));
#254578=CARTESIAN_POINT('Ctrl Pts',(23.2714850482245,1.68550216963275,12.));
#254579=CARTESIAN_POINT('Ctrl Pts',(23.2545810680536,1.6886746903491,12.));
#254580=CARTESIAN_POINT('Ctrl Pts',(23.2377975177014,1.69177432121716,12.));
#254581=CARTESIAN_POINT('Ctrl Pts',(23.2211357709374,1.69480141959946,12.));
#254582=CARTESIAN_POINT('Ctrl Pts',(23.2045972243765,1.69775635099425,12.));
#254583=CARTESIAN_POINT('Ctrl Pts',(23.1881832981848,1.70063948926988,12.));
#254584=CARTESIAN_POINT('Ctrl Pts',(23.1718954368749,1.70345121691259,12.));
#254585=CARTESIAN_POINT('Ctrl Pts',(23.1557351100613,1.70619192527847,12.));
#254586=CARTESIAN_POINT('Ctrl Pts',(23.1397038132358,1.7088620148546,12.));
#254587=CARTESIAN_POINT('Ctrl Pts',(23.1238030684929,1.71146189552192,12.));
#254588=CARTESIAN_POINT('Ctrl Pts',(23.1080344254291,1.71399198684725,12.));
#254589=CARTESIAN_POINT('Ctrl Pts',(23.0923994621216,1.71645271839311,12.));
#254590=CARTESIAN_POINT('Ctrl Pts',(23.0768997860709,1.71884453003027,12.));
#254591=CARTESIAN_POINT('Ctrl Pts',(23.0615370351559,1.72116787225981,12.));
#254592=CARTESIAN_POINT('Ctrl Pts',(23.0463128785528,1.72342320653731,12.));
#254593=CARTESIAN_POINT('Ctrl Pts',(23.031229017888,1.72561100564033,12.));
#254594=CARTESIAN_POINT('Ctrl Pts',(23.0162871884167,1.72773175404703,12.));
#254595=CARTESIAN_POINT('Ctrl Pts',(23.0014891601891,1.72978594832137,12.));
#254596=CARTESIAN_POINT('Ctrl Pts',(22.9868367391978,1.73177409750194,12.));
#254597=CARTESIAN_POINT('Ctrl Pts',(22.9723317685688,1.73369672350818,12.));
#254598=CARTESIAN_POINT('Ctrl Pts',(22.9579761301062,1.73555436162771,12.));
#254599=CARTESIAN_POINT('Ctrl Pts',(22.9437717457825,1.73734756100038,12.));
#254600=CARTESIAN_POINT('Ctrl Pts',(22.9297205792587,1.73907688511665,12.));
#254601=CARTESIAN_POINT('Ctrl Pts',(22.9158246373365,1.74074291231057,12.));
#254602=CARTESIAN_POINT('Ctrl Pts',(22.9020859716144,1.74234623630079,12.));
#254603=CARTESIAN_POINT('Ctrl Pts',(22.8885066803351,1.74388746677702,12.));
#254604=CARTESIAN_POINT('Ctrl Pts',(22.8750889101696,1.745367229982,12.));
#254605=CARTESIAN_POINT('Ctrl Pts',(22.8618348580234,1.74678616930663,12.));
#254606=CARTESIAN_POINT('Ctrl Pts',(22.8487467728075,1.74814494588492,12.));
#254607=CARTESIAN_POINT('Ctrl Pts',(22.8358269579854,1.74944423940117,12.));
#254608=CARTESIAN_POINT('Ctrl Pts',(22.8230777741285,1.75068474890884,12.));
#254609=CARTESIAN_POINT('Ctrl Pts',(22.8105016414712,1.7518671936559,12.));
#254610=CARTESIAN_POINT('Ctrl Pts',(22.7981010424312,1.75299231391461,12.));
#254611=CARTESIAN_POINT('Ctrl Pts',(22.7858785242358,1.7540608718293,12.));
#254612=CARTESIAN_POINT('Ctrl Pts',(22.7738367016115,1.75507365227127,12.));
#254613=CARTESIAN_POINT('Ctrl Pts',(22.7619782595013,1.75603146371641,12.));
#254614=CARTESIAN_POINT('Ctrl Pts',(22.7503059556455,1.75693513908911,12.));
#254615=CARTESIAN_POINT('Ctrl Pts',(22.7388226235565,1.75778553673249,12.));
#254616=CARTESIAN_POINT('Ctrl Pts',(22.7275311777305,1.75858354204635,12.));
#254617=CARTESIAN_POINT('Ctrl Pts',(22.7164346186007,1.75933006905924,12.));
#254618=CARTESIAN_POINT('Ctrl Pts',(22.7055360375481,1.76002606202399,12.));
#254619=CARTESIAN_POINT('Ctrl Pts',(22.6948386219843,1.76067249704884,12.));
#254620=CARTESIAN_POINT('Ctrl Pts',(22.6843456585245,1.76127038310613,12.));
#254621=CARTESIAN_POINT('Ctrl Pts',(22.6740605356699,1.76182076289525,12.));
#254622=CARTESIAN_POINT('Ctrl Pts',(22.6639867471756,1.76232471392568,12.));
#254623=CARTESIAN_POINT('Ctrl Pts',(22.6541278938413,1.76278334912559,12.));
#254624=CARTESIAN_POINT('Ctrl Pts',(22.6444876940425,1.76319782013914,12.));
#254625=CARTESIAN_POINT('Ctrl Pts',(22.635069997936,1.76356932176272,12.));
#254626=CARTESIAN_POINT('Ctrl Pts',(22.6258787994847,1.76389909571402,12.));
#254627=CARTESIAN_POINT('Ctrl Pts',(22.6169182517693,1.76418843543739,12.));
#254628=CARTESIAN_POINT('Ctrl Pts',(22.6081926681342,1.76443868648015,12.));
#254629=CARTESIAN_POINT('Ctrl Pts',(22.5997065145638,1.76465124413556,12.));
#254630=CARTESIAN_POINT('Ctrl Pts',(22.5914644078106,1.76482755288411,12.));
#254631=CARTESIAN_POINT('Ctrl Pts',(22.5834711038024,1.76496910283089,12.));
#254632=CARTESIAN_POINT('Ctrl Pts',(22.5757315316355,1.76507744026747,12.));
#254633=CARTESIAN_POINT('Ctrl Pts',(22.5682508499873,1.76515418518829,12.));
#254634=CARTESIAN_POINT('Ctrl Pts',(22.5610344912501,1.7652010450045,12.));
#254635=CARTESIAN_POINT('Ctrl Pts',(22.5540882235837,1.76521983384063,12.));
#254636=CARTESIAN_POINT('Ctrl Pts',(22.5474180954006,1.76521245524047,12.));
#254637=CARTESIAN_POINT('Ctrl Pts',(22.5410303590891,1.76518087841493,12.));
#254638=CARTESIAN_POINT('Ctrl Pts',(22.5349313983571,1.7651271156325,12.));
#254639=CARTESIAN_POINT('Ctrl Pts',(22.529127665298,1.76505320262752,12.));
#254640=CARTESIAN_POINT('Ctrl Pts',(22.5236259635515,1.76496128643369,12.));
#254641=CARTESIAN_POINT('Ctrl Pts',(22.5184336670207,1.76485369319896,12.));
#254642=CARTESIAN_POINT('Ctrl Pts',(22.5135590569554,1.76473303281159,12.));
#254643=CARTESIAN_POINT('Ctrl Pts',(22.5090112700212,1.76460218257323,12.));
#254644=CARTESIAN_POINT('Ctrl Pts',(22.5047996391978,1.76446408210366,12.));
#254645=CARTESIAN_POINT('Ctrl Pts',(22.5009332677316,1.76432160068726,12.));
#254646=CARTESIAN_POINT('Ctrl Pts',(22.4974203063191,1.76417731243462,12.));
#254647=CARTESIAN_POINT('Ctrl Pts',(22.4942693792449,1.76403393880301,12.));
#254648=CARTESIAN_POINT('Ctrl Pts',(22.4914909094908,1.76389475965724,12.));
#254649=CARTESIAN_POINT('Ctrl Pts',(22.4890991659478,1.76376424879505,12.));
#254650=CARTESIAN_POINT('Ctrl Pts',(22.4871115206571,1.76364784232963,12.));
#254651=CARTESIAN_POINT('Ctrl Pts',(22.4855446605991,1.76355076045546,12.));
#254652=CARTESIAN_POINT('Ctrl Pts',(22.4844112933129,1.76347698284792,12.));
#254653=CARTESIAN_POINT('Ctrl Pts',(22.4838562517069,1.76343813434565,12.));
#254654=CARTESIAN_POINT('Ctrl Pts',(22.4836387052232,1.7634206426357,12.));
#254655=CARTESIAN_POINT('Ctrl Pts',(22.483581992979,1.76341415538764,12.));
#254656=CARTESIAN_POINT('Ctrl Pts',(22.4835757167854,1.76341220531179,12.));
#254657=CARTESIAN_POINT('',(21.9269795755927,1.71975774210841,12.));
#254658=CARTESIAN_POINT('',(10.7170877657712,0.840553282521227,12.));
#254659=CARTESIAN_POINT('',(21.3904321633055,2.16781269186828,12.));
#254660=CARTESIAN_POINT('Origin',(21.8878840740801,2.21822694051638,12.));
#254661=CARTESIAN_POINT('',(21.2226420728916,3.44230496120419,12.));
#254662=CARTESIAN_POINT('Origin',(7.7715611723761E-13,7.16093850883226E-14,
12.));
#254663=CARTESIAN_POINT('',(21.624941921198,4.01396149767428,12.));
#254664=CARTESIAN_POINT('Origin',(21.7161918885402,3.52235856495312,12.));
#254665=CARTESIAN_POINT('',(22.1738711152697,4.11585220600461,12.));
#254666=CARTESIAN_POINT('',(11.0869355576349,2.05792610300232,12.));
#254667=CARTESIAN_POINT('',(25.2771067246846,6.08833931617698,12.));
#254668=CARTESIAN_POINT('Ctrl Pts',(22.1738711152697,4.11585220600461,12.));
#254669=CARTESIAN_POINT('Ctrl Pts',(22.1738776823239,4.11585194677412,12.));
#254670=CARTESIAN_POINT('Ctrl Pts',(22.1739341411684,4.1158603587821,12.));
#254671=CARTESIAN_POINT('Ctrl Pts',(22.174148802123,4.11589976826061,12.));
#254672=CARTESIAN_POINT('Ctrl Pts',(22.1746949858773,4.11600589882768,12.));
#254673=CARTESIAN_POINT('Ctrl Pts',(22.1758088296598,4.11622797217066,12.));
#254674=CARTESIAN_POINT('Ctrl Pts',(22.177347426894,4.11653973150558,12.));
#254675=CARTESIAN_POINT('Ctrl Pts',(22.179297473024,4.11694173195041,12.));
#254676=CARTESIAN_POINT('Ctrl Pts',(22.1816414985788,4.11743469691765,12.));
#254677=CARTESIAN_POINT('Ctrl Pts',(22.1843613164855,4.11801938107464,12.));
#254678=CARTESIAN_POINT('Ctrl Pts',(22.1874419861496,4.11869641271752,12.));
#254679=CARTESIAN_POINT('Ctrl Pts',(22.1908725908525,4.11946626228623,12.));
#254680=CARTESIAN_POINT('Ctrl Pts',(22.1946440958098,4.12032932637738,12.));
#254681=CARTESIAN_POINT('Ctrl Pts',(22.1987479618246,4.12128598183533,12.));
#254682=CARTESIAN_POINT('Ctrl Pts',(22.2031746532106,4.12233664408237,12.));
#254683=CARTESIAN_POINT('Ctrl Pts',(22.2079143941719,4.12348173702025,12.));
#254684=CARTESIAN_POINT('Ctrl Pts',(22.2129576146671,4.12472167516602,12.));
#254685=CARTESIAN_POINT('Ctrl Pts',(22.2182956401341,4.126056836133,12.));
#254686=CARTESIAN_POINT('Ctrl Pts',(22.2239207458781,4.127487558301,12.));
#254687=CARTESIAN_POINT('Ctrl Pts',(22.2298258043947,4.12901415463379,12.));
#254688=CARTESIAN_POINT('Ctrl Pts',(22.2360040565534,4.13063692157499,12.));
#254689=CARTESIAN_POINT('Ctrl Pts',(22.2424488153523,4.1323561506016,12.));
#254690=CARTESIAN_POINT('Ctrl Pts',(22.2491535317789,4.13417212558809,12.));
#254691=CARTESIAN_POINT('Ctrl Pts',(22.2561118708422,4.13608511977226,12.));
#254692=CARTESIAN_POINT('Ctrl Pts',(22.263317791397,4.13809539255419,12.));
#254693=CARTESIAN_POINT('Ctrl Pts',(22.2707656042456,4.14020318715988,12.));
#254694=CARTESIAN_POINT('Ctrl Pts',(22.2784499072026,4.14240873321982,12.));
#254695=CARTESIAN_POINT('Ctrl Pts',(22.2863655389167,4.14471224859295,12.));
#254696=CARTESIAN_POINT('Ctrl Pts',(22.2945075198468,4.14711394168559,12.));
#254697=CARTESIAN_POINT('Ctrl Pts',(22.3028710166935,4.14961401285526,12.));
#254698=CARTESIAN_POINT('Ctrl Pts',(22.3114513545186,4.15221265396993,12.));
#254699=CARTESIAN_POINT('Ctrl Pts',(22.3202440186979,4.15491004835278,12.));
#254700=CARTESIAN_POINT('Ctrl Pts',(22.3292446628957,4.15770637047882,12.));
#254701=CARTESIAN_POINT('Ctrl Pts',(22.3384491078599,4.16060178604154,12.));
#254702=CARTESIAN_POINT('Ctrl Pts',(22.3478533253886,4.1635964526318,12.));
#254703=CARTESIAN_POINT('Ctrl Pts',(22.3574534257397,4.16669052026602,12.));
#254704=CARTESIAN_POINT('Ctrl Pts',(22.3672456427605,4.1698841319947,12.));
#254705=CARTESIAN_POINT('Ctrl Pts',(22.3772263228624,4.17317742436162,12.));
#254706=CARTESIAN_POINT('Ctrl Pts',(22.3873919231339,4.17657052752834,12.));
#254707=CARTESIAN_POINT('Ctrl Pts',(22.3977390078074,4.18006356544879,12.));
#254708=CARTESIAN_POINT('Ctrl Pts',(22.4082642454448,4.18365665600839,12.));
#254709=CARTESIAN_POINT('Ctrl Pts',(22.4189644056109,4.18734991117707,12.));
#254710=CARTESIAN_POINT('Ctrl Pts',(22.4298363535416,4.19114343726932,12.));
#254711=CARTESIAN_POINT('Ctrl Pts',(22.4408770448917,4.1950373351886,12.));
#254712=CARTESIAN_POINT('Ctrl Pts',(22.4520835205422,4.19903170066358,12.));
#254713=CARTESIAN_POINT('Ctrl Pts',(22.4634529011437,4.20312662448174,12.));
#254714=CARTESIAN_POINT('Ctrl Pts',(22.4749823839917,4.20732219265649,12.));
#254715=CARTESIAN_POINT('Ctrl Pts',(22.4866692403147,4.21161848657428,12.));
#254716=CARTESIAN_POINT('Ctrl Pts',(22.4985108124228,4.21601558313906,12.));
#254717=CARTESIAN_POINT('Ctrl Pts',(22.5105045108881,4.22051355490196,12.));
#254718=CARTESIAN_POINT('Ctrl Pts',(22.5226478117886,4.22511247020041,12.));
#254719=CARTESIAN_POINT('Ctrl Pts',(22.5349382540588,4.22981239330733,12.));
#254720=CARTESIAN_POINT('Ctrl Pts',(22.5473734368086,4.23461338456712,12.));
#254721=CARTESIAN_POINT('Ctrl Pts',(22.5599510166429,4.23951550052523,12.));
#254722=CARTESIAN_POINT('Ctrl Pts',(22.572668704992,4.24451879404851,12.));
#254723=CARTESIAN_POINT('Ctrl Pts',(22.5855242662477,4.24962331444177,12.));
#254724=CARTESIAN_POINT('Ctrl Pts',(22.5985155158636,4.25482910755481,12.));
#254725=CARTESIAN_POINT('Ctrl Pts',(22.6116403184821,4.26013621588305,12.));
#254726=CARTESIAN_POINT('Ctrl Pts',(22.6248965859977,4.26554467865576,12.));
#254727=CARTESIAN_POINT('Ctrl Pts',(22.6382822758172,4.27105453193004,12.));
#254728=CARTESIAN_POINT('Ctrl Pts',(22.6517953893303,4.2766658086912,12.));
#254729=CARTESIAN_POINT('Ctrl Pts',(22.6654339703109,4.28237853894059,12.));
#254730=CARTESIAN_POINT('Ctrl Pts',(22.6791961033537,4.28819274977763,12.));
#254731=CARTESIAN_POINT('Ctrl Pts',(22.6930799122548,4.29410846547056,12.));
#254732=CARTESIAN_POINT('Ctrl Pts',(22.7070835587564,4.3001257075406,12.));
#254733=CARTESIAN_POINT('Ctrl Pts',(22.7212052413386,4.30624449484069,12.));
#254734=CARTESIAN_POINT('Ctrl Pts',(22.7354431939926,4.31246484362549,12.));
#254735=CARTESIAN_POINT('Ctrl Pts',(22.7497956849848,4.31878676761235,12.));
#254736=CARTESIAN_POINT('Ctrl Pts',(22.7642610156475,4.32521027803754,12.));
#254737=CARTESIAN_POINT('Ctrl Pts',(22.7788375194076,4.3317353837319,12.));
#254738=CARTESIAN_POINT('Ctrl Pts',(22.7935235607806,4.33836209118446,12.));
#254739=CARTESIAN_POINT('Ctrl Pts',(22.8083175343791,4.34509040460062,12.));
#254740=CARTESIAN_POINT('Ctrl Pts',(22.8232178638876,4.35192032594791,12.));
#254741=CARTESIAN_POINT('Ctrl Pts',(22.8382230011184,4.35885185500546,12.));
#254742=CARTESIAN_POINT('Ctrl Pts',(22.8533314252422,4.36588498942997,12.));
#254743=CARTESIAN_POINT('Ctrl Pts',(22.8685416419725,4.37301972480746,12.));
#254744=CARTESIAN_POINT('Ctrl Pts',(22.8838521827701,4.38025605470093,12.));
#254745=CARTESIAN_POINT('Ctrl Pts',(22.8992616040108,4.38759397068406,12.));
#254746=CARTESIAN_POINT('Ctrl Pts',(22.9147684862426,4.39503346238473,12.));
#254747=CARTESIAN_POINT('Ctrl Pts',(22.930371433555,4.40257451754324,12.));
#254748=CARTESIAN_POINT('Ctrl Pts',(22.9460690729093,4.41021712205554,12.));
#254749=CARTESIAN_POINT('Ctrl Pts',(22.9618600534866,4.41796126001302,12.));
#254750=CARTESIAN_POINT('Ctrl Pts',(22.977743046002,4.42580691372752,12.));
#254751=CARTESIAN_POINT('Ctrl Pts',(22.9937167421006,4.43375406376879,12.));
#254752=CARTESIAN_POINT('Ctrl Pts',(23.0097798538395,4.44180268901643,12.));
#254753=CARTESIAN_POINT('Ctrl Pts',(23.0259311131392,4.44995276669687,12.));
#254754=CARTESIAN_POINT('Ctrl Pts',(23.0421692712467,4.45820427241683,12.));
#254755=CARTESIAN_POINT('Ctrl Pts',(23.0584930981732,4.46655718018231,12.));
#254756=CARTESIAN_POINT('Ctrl Pts',(23.0749013821881,4.47501146242856,12.));
#254757=CARTESIAN_POINT('Ctrl Pts',(23.0913929293922,4.48356709006788,12.));
#254758=CARTESIAN_POINT('Ctrl Pts',(23.1079665632636,4.49222403252216,12.));
#254759=CARTESIAN_POINT('Ctrl Pts',(23.1246211242115,4.50098225775171,12.));
#254760=CARTESIAN_POINT('Ctrl Pts',(23.1413554691123,4.5098417322706,12.));
#254761=CARTESIAN_POINT('Ctrl Pts',(23.1581684708761,4.51880242116748,12.));
#254762=CARTESIAN_POINT('Ctrl Pts',(23.1750590180908,4.52786428815015,12.));
#254763=CARTESIAN_POINT('Ctrl Pts',(23.1920260146465,4.53702729557566,12.));
#254764=CARTESIAN_POINT('Ctrl Pts',(23.2090683793629,4.54629140447544,12.));
#254765=CARTESIAN_POINT('Ctrl Pts',(23.2261850456064,4.55565657456975,12.));
#254766=CARTESIAN_POINT('Ctrl Pts',(23.2433749609131,4.56512276427839,12.));
#254767=CARTESIAN_POINT('Ctrl Pts',(23.2606370866866,4.57468993076097,12.));
#254768=CARTESIAN_POINT('Ctrl Pts',(23.2779703978876,4.5843580299469,12.));
#254769=CARTESIAN_POINT('Ctrl Pts',(23.2953738827191,4.5941270165575,12.));
#254770=CARTESIAN_POINT('Ctrl Pts',(23.3128465423115,4.60399684412163,12.));
#254771=CARTESIAN_POINT('Ctrl Pts',(23.3303873903938,4.6139674649783,12.));
#254772=CARTESIAN_POINT('Ctrl Pts',(23.3479954530272,4.62403883030805,12.));
#254773=CARTESIAN_POINT('Ctrl Pts',(23.3656697683489,4.63421089016541,12.));
#254774=CARTESIAN_POINT('Ctrl Pts',(23.3834093863068,4.6444835934993,12.));
#254775=CARTESIAN_POINT('Ctrl Pts',(23.4012133683959,4.65485688816924,12.));
#254776=CARTESIAN_POINT('Ctrl Pts',(23.4190807873803,4.6653307209467,12.));
#254777=CARTESIAN_POINT('Ctrl Pts',(23.4370107270451,4.67590503753059,12.));
#254778=CARTESIAN_POINT('Ctrl Pts',(23.455002281986,4.68657978258303,12.));
#254779=CARTESIAN_POINT('Ctrl Pts',(23.4730545573853,4.69735489975024,12.));
#254780=CARTESIAN_POINT('Ctrl Pts',(23.491166668789,4.70823033167819,12.));
#254781=CARTESIAN_POINT('Ctrl Pts',(23.509337741878,4.71920602001902,12.));
#254782=CARTESIAN_POINT('Ctrl Pts',(23.5275669122372,4.7302819054303,12.));
#254783=CARTESIAN_POINT('Ctrl Pts',(23.545853325171,4.74145792760699,12.));
#254784=CARTESIAN_POINT('Ctrl Pts',(23.5641961355168,4.75273402530617,12.));
#254785=CARTESIAN_POINT('Ctrl Pts',(23.5825945074535,4.76411013636251,12.));
#254786=CARTESIAN_POINT('Ctrl Pts',(23.6010476143099,4.77558619769872,12.));
#254787=CARTESIAN_POINT('Ctrl Pts',(23.6195546383624,4.78716214532098,12.));
#254788=CARTESIAN_POINT('Ctrl Pts',(23.6381147706579,4.7988379143322,12.));
#254789=CARTESIAN_POINT('Ctrl Pts',(23.6567272108628,4.81061343896432,12.));
#254790=CARTESIAN_POINT('Ctrl Pts',(23.675391167102,4.82248865259562,12.));
#254791=CARTESIAN_POINT('Ctrl Pts',(23.6941058557971,4.83446348776266,12.));
#254792=CARTESIAN_POINT('Ctrl Pts',(23.7128705015017,4.84653787616426,12.));
#254793=CARTESIAN_POINT('Ctrl Pts',(23.7316843367313,4.85871174865499,12.));
#254794=CARTESIAN_POINT('Ctrl Pts',(23.7505466018245,4.87098503527152,12.));
#254795=CARTESIAN_POINT('Ctrl Pts',(23.7694565448049,4.88335766525573,12.));
#254796=CARTESIAN_POINT('Ctrl Pts',(23.7884134212384,4.89582956706775,12.));
#254797=CARTESIAN_POINT('Ctrl Pts',(23.8074164940896,4.90840066839344,12.));
#254798=CARTESIAN_POINT('Ctrl Pts',(23.8264650335717,4.92107089613969,12.));
#254799=CARTESIAN_POINT('Ctrl Pts',(23.8455583170057,4.93384017643432,12.));
#254800=CARTESIAN_POINT('Ctrl Pts',(23.8646956287168,4.9467084346586,12.));
#254801=CARTESIAN_POINT('Ctrl Pts',(23.8838762599218,4.95967559546561,12.));
#254802=CARTESIAN_POINT('Ctrl Pts',(23.9030995086163,4.97274158279227,12.));
#254803=CARTESIAN_POINT('Ctrl Pts',(23.9223646794592,4.98590631986533,12.));
#254804=CARTESIAN_POINT('Ctrl Pts',(23.9416710836529,4.99916972919307,12.));
#254805=CARTESIAN_POINT('Ctrl Pts',(23.961018038827,5.01253173257453,12.));
#254806=CARTESIAN_POINT('Ctrl Pts',(23.9804048689227,5.02599225112454,12.));
#254807=CARTESIAN_POINT('Ctrl Pts',(23.9998309040746,5.03955120528521,12.));
#254808=CARTESIAN_POINT('Ctrl Pts',(24.0192954804896,5.05320851483065,12.));
#254809=CARTESIAN_POINT('Ctrl Pts',(24.0387979403268,5.06696409886641,12.));
#254810=CARTESIAN_POINT('Ctrl Pts',(24.0583376315638,5.08081787581277,12.));
#254811=CARTESIAN_POINT('Ctrl Pts',(24.0779139079266,5.09476976342625,12.));
#254812=CARTESIAN_POINT('Ctrl Pts',(24.0975261288446,5.10881967883132,12.));
#254813=CARTESIAN_POINT('Ctrl Pts',(24.117173659394,5.1229675385386,12.));
#254814=CARTESIAN_POINT('Ctrl Pts',(24.1368558702443,5.13721325845745,12.));
#254815=CARTESIAN_POINT('Ctrl Pts',(24.156572137597,5.15155675390075,12.));
#254816=CARTESIAN_POINT('Ctrl Pts',(24.1763218431343,5.16599793957979,12.));
#254817=CARTESIAN_POINT('Ctrl Pts',(24.1961043738754,5.18053672961392,12.));
#254818=CARTESIAN_POINT('Ctrl Pts',(24.215919122017,5.19517303753643,12.));
#254819=CARTESIAN_POINT('Ctrl Pts',(24.2357654847765,5.20990677629173,12.));
#254820=CARTESIAN_POINT('Ctrl Pts',(24.2556428642294,5.22473785822441,12.));
#254821=CARTESIAN_POINT('Ctrl Pts',(24.2755506671526,5.23966619506289,12.));
#254822=CARTESIAN_POINT('Ctrl Pts',(24.2954883048448,5.25469169788856,12.));
#254823=CARTESIAN_POINT('Ctrl Pts',(24.3154551932222,5.26981427718796,12.));
#254824=CARTESIAN_POINT('Ctrl Pts',(24.3354507529415,5.28503384290644,12.));
#254825=CARTESIAN_POINT('Ctrl Pts',(24.3554744095075,5.30035030449059,12.));
#254826=CARTESIAN_POINT('Ctrl Pts',(24.3755255933917,5.31576357092525,12.));
#254827=CARTESIAN_POINT('Ctrl Pts',(24.3956037401293,5.33127355076037,12.));
#254828=CARTESIAN_POINT('Ctrl Pts',(24.4157082904615,5.34688015213546,12.));
#254829=CARTESIAN_POINT('Ctrl Pts',(24.4358386899152,5.36258328273639,12.));
#254830=CARTESIAN_POINT('Ctrl Pts',(24.4559943883159,5.37838284973706,12.));
#254831=CARTESIAN_POINT('Ctrl Pts',(24.4761748393322,5.39427875973831,12.));
#254832=CARTESIAN_POINT('Ctrl Pts',(24.4963794999831,5.41027091869242,12.));
#254833=CARTESIAN_POINT('Ctrl Pts',(24.5166078302107,5.42635923183411,12.));
#254834=CARTESIAN_POINT('Ctrl Pts',(24.5368592922861,5.44254360356866,12.));
#254835=CARTESIAN_POINT('Ctrl Pts',(24.5571333514841,5.45882393762244,12.));
#254836=CARTESIAN_POINT('Ctrl Pts',(24.5774294770329,5.47520013724403,12.));
#254837=CARTESIAN_POINT('Ctrl Pts',(24.5977471429365,5.49167210537235,12.));
#254838=CARTESIAN_POINT('Ctrl Pts',(24.618085828918,5.50823974481959,12.));
#254839=CARTESIAN_POINT('Ctrl Pts',(24.6384450211466,5.52490295840996,12.));
#254840=CARTESIAN_POINT('Ctrl Pts',(24.6588242134733,5.54166164919593,12.));
#254841=CARTESIAN_POINT('Ctrl Pts',(24.6792229061785,5.55851572025389,12.));
#254842=CARTESIAN_POINT('Ctrl Pts',(24.6996406035507,5.57546507427767,12.));
#254843=CARTESIAN_POINT('Ctrl Pts',(24.7200768119079,5.59250961323995,12.));
#254844=CARTESIAN_POINT('Ctrl Pts',(24.7405310372736,5.60964923798495,12.));
#254845=CARTESIAN_POINT('Ctrl Pts',(24.76100278357,5.62688384790919,12.));
#254846=CARTESIAN_POINT('Ctrl Pts',(24.7814915496728,5.64421334042248,12.));
#254847=CARTESIAN_POINT('Ctrl Pts',(24.8019968304618,5.66163761114903,12.));
#254848=CARTESIAN_POINT('Ctrl Pts',(24.822518122386,5.67915655496524,12.));
#254849=CARTESIAN_POINT('Ctrl Pts',(24.8430549277634,5.6967700667943,12.));
#254850=CARTESIAN_POINT('Ctrl Pts',(24.8636067597677,5.71447804252019,12.));
#254851=CARTESIAN_POINT('Ctrl Pts',(24.8841731467219,5.73228037976927,12.));
#254852=CARTESIAN_POINT('Ctrl Pts',(24.9047536376467,5.75017697890813,12.));
#254853=CARTESIAN_POINT('Ctrl Pts',(24.9253478043632,5.76816774342236,12.));
#254854=CARTESIAN_POINT('Ctrl Pts',(24.9459552293308,5.78625257775703,12.));
#254855=CARTESIAN_POINT('Ctrl Pts',(24.9665754954462,5.80443138549747,12.));
#254856=CARTESIAN_POINT('Ctrl Pts',(24.9872081752709,5.82270406744214,12.));
#254857=CARTESIAN_POINT('Ctrl Pts',(25.0078528200558,5.84107051963074,12.));
#254858=CARTESIAN_POINT('Ctrl Pts',(25.0285089498922,5.8595306315681,12.));
#254859=CARTESIAN_POINT('Ctrl Pts',(25.0491760405965,5.87808428385329,12.));
#254860=CARTESIAN_POINT('Ctrl Pts',(25.0698535426593,5.89673135155459,12.));
#254861=CARTESIAN_POINT('Ctrl Pts',(25.0905409050863,5.91547170844382,12.));
#254862=CARTESIAN_POINT('Ctrl Pts',(25.1112375971182,5.93430523086776,12.));
#254863=CARTESIAN_POINT('Ctrl Pts',(25.1319431317273,5.95323180187348,12.));
#254864=CARTESIAN_POINT('Ctrl Pts',(25.1526570863065,5.97225131495636,12.));
#254865=CARTESIAN_POINT('Ctrl Pts',(25.1733791296154,5.99136367859839,12.));
#254866=CARTESIAN_POINT('Ctrl Pts',(25.1941090269638,6.0105688180476,12.));
#254867=CARTESIAN_POINT('Ctrl Pts',(25.2148466201368,6.02986667390187,12.));
#254868=CARTESIAN_POINT('Ctrl Pts',(25.2355918138798,6.04925720151412,12.));
#254869=CARTESIAN_POINT('Ctrl Pts',(25.2521940105523,6.06484373634697,12.));
#254870=CARTESIAN_POINT('Ctrl Pts',(25.2646490489816,6.07657531787578,12.));
#254871=CARTESIAN_POINT('Ctrl Pts',(25.2729539149479,6.08441489609824,12.));
#254872=CARTESIAN_POINT('Ctrl Pts',(25.2771067246846,6.08833931617698,12.));
#254873=CARTESIAN_POINT('Origin',(0.,0.,12.));
#254874=CARTESIAN_POINT('Origin',(0.,0.,12.));
#254875=CARTESIAN_POINT('Origin',(0.,0.,12.));
#254876=CARTESIAN_POINT('Origin',(0.,0.,12.));
#254877=CARTESIAN_POINT('Origin',(0.,0.,12.));
#254878=CARTESIAN_POINT('Origin',(0.,0.,12.));
#254879=CARTESIAN_POINT('Origin',(0.,0.,12.));
#254880=CARTESIAN_POINT('Origin',(0.,0.,12.));
#254881=CARTESIAN_POINT('Origin',(0.,0.,12.));
#254882=CARTESIAN_POINT('Origin',(0.,0.,12.));
#254883=CARTESIAN_POINT('Origin',(0.,0.,12.));
#254884=CARTESIAN_POINT('Origin',(0.,0.,12.));
#254885=CARTESIAN_POINT('Origin',(0.,0.,12.));
#254886=CARTESIAN_POINT('Origin',(0.,0.,12.));
#254887=CARTESIAN_POINT('Origin',(0.,0.,12.));
#254888=CARTESIAN_POINT('Origin',(0.,0.,12.));
#254889=CARTESIAN_POINT('Origin',(0.,0.,12.));
#254890=CARTESIAN_POINT('Origin',(0.,0.,12.));
#254891=CARTESIAN_POINT('Origin',(0.,0.,12.));
#254892=CARTESIAN_POINT('Origin',(0.,0.,12.));
#254893=CARTESIAN_POINT('Origin',(0.,0.,12.));
#254894=CARTESIAN_POINT('Origin',(0.,0.,12.));
#254895=CARTESIAN_POINT('Origin',(0.,0.,12.));
#254896=CARTESIAN_POINT('',(-7.,-8.57252759403147E-16,12.));
#254897=CARTESIAN_POINT('Origin',(0.,0.,12.));
#254898=CARTESIAN_POINT('Origin',(0.,0.,0.));
#254899=CARTESIAN_POINT('',(25.2771067246846,6.08833931617698,0.));
#254900=CARTESIAN_POINT('Origin',(0.,0.,0.));
#254901=CARTESIAN_POINT('Origin',(0.,0.,0.));
#254902=CARTESIAN_POINT('Origin',(0.,0.,0.));
#254903=CARTESIAN_POINT('Origin',(0.,0.,0.));
#254904=CARTESIAN_POINT('Origin',(0.,0.,0.));
#254905=CARTESIAN_POINT('Origin',(0.,0.,0.));
#254906=CARTESIAN_POINT('Origin',(0.,0.,0.));
#254907=CARTESIAN_POINT('Origin',(0.,0.,0.));
#254908=CARTESIAN_POINT('Origin',(0.,0.,0.));
#254909=CARTESIAN_POINT('Origin',(0.,0.,0.));
#254910=CARTESIAN_POINT('Origin',(0.,0.,0.));
#254911=CARTESIAN_POINT('Origin',(0.,0.,0.));
#254912=CARTESIAN_POINT('Origin',(0.,0.,0.));
#254913=CARTESIAN_POINT('Origin',(0.,0.,0.));
#254914=CARTESIAN_POINT('Origin',(0.,0.,0.));
#254915=CARTESIAN_POINT('Origin',(0.,0.,0.));
#254916=CARTESIAN_POINT('Origin',(0.,0.,0.));
#254917=CARTESIAN_POINT('Origin',(0.,0.,0.));
#254918=CARTESIAN_POINT('Origin',(0.,0.,0.));
#254919=CARTESIAN_POINT('Origin',(0.,0.,0.));
#254920=CARTESIAN_POINT('Origin',(0.,0.,0.));
#254921=CARTESIAN_POINT('Origin',(0.,0.,0.));
#254922=CARTESIAN_POINT('Origin',(21.7161918885402,3.52235856495312,0.));
#254923=CARTESIAN_POINT('',(21.624941921198,4.01396149767428,0.));
#254924=CARTESIAN_POINT('',(21.2226420728916,3.44230496120418,0.));
#254925=CARTESIAN_POINT('Origin',(22.1738711152697,4.11585220600461,0.));
#254926=CARTESIAN_POINT('',(22.1738711152697,4.11585220600461,0.));
#254927=CARTESIAN_POINT('Origin',(21.8878840740801,2.21822694051638,0.));
#254928=CARTESIAN_POINT('',(21.3904321633055,2.16781269186828,0.));
#254929=CARTESIAN_POINT('',(21.9269795755927,1.71975774210841,0.));
#254930=CARTESIAN_POINT('Origin',(7.7715611723761E-13,7.16093850883226E-14,
0.));
#254931=CARTESIAN_POINT('Origin',(21.4341755315424,1.68110656504246,0.));
#254932=CARTESIAN_POINT('',(22.4835757167854,1.76341220531179,0.));
#254933=CARTESIAN_POINT('Ctrl Pts',(25.2771067246846,6.08833931617698,0.));
#254934=CARTESIAN_POINT('Ctrl Pts',(25.2771067246846,6.08833931617698,12.));
#254935=CARTESIAN_POINT('Ctrl Pts',(25.2729539149479,6.08441489609824,0.));
#254936=CARTESIAN_POINT('Ctrl Pts',(25.2729539149479,6.08441489609824,12.));
#254937=CARTESIAN_POINT('Ctrl Pts',(25.2646490489816,6.07657531787578,0.));
#254938=CARTESIAN_POINT('Ctrl Pts',(25.2646490489816,6.07657531787578,12.));
#254939=CARTESIAN_POINT('Ctrl Pts',(25.2521940105523,6.06484373634697,0.));
#254940=CARTESIAN_POINT('Ctrl Pts',(25.2521940105523,6.06484373634697,12.));
#254941=CARTESIAN_POINT('Ctrl Pts',(25.2355918138798,6.04925720151412,0.));
#254942=CARTESIAN_POINT('Ctrl Pts',(25.2355918138798,6.04925720151412,12.));
#254943=CARTESIAN_POINT('Ctrl Pts',(25.2148466201368,6.02986667390187,0.));
#254944=CARTESIAN_POINT('Ctrl Pts',(25.2148466201368,6.02986667390187,12.));
#254945=CARTESIAN_POINT('Ctrl Pts',(25.1941090269638,6.0105688180476,0.));
#254946=CARTESIAN_POINT('Ctrl Pts',(25.1941090269638,6.0105688180476,12.));
#254947=CARTESIAN_POINT('Ctrl Pts',(25.1733791296154,5.99136367859839,0.));
#254948=CARTESIAN_POINT('Ctrl Pts',(25.1733791296154,5.99136367859839,12.));
#254949=CARTESIAN_POINT('Ctrl Pts',(25.1526570863065,5.97225131495636,0.));
#254950=CARTESIAN_POINT('Ctrl Pts',(25.1526570863065,5.97225131495636,12.));
#254951=CARTESIAN_POINT('Ctrl Pts',(25.1319431317273,5.95323180187348,0.));
#254952=CARTESIAN_POINT('Ctrl Pts',(25.1319431317273,5.95323180187348,12.));
#254953=CARTESIAN_POINT('Ctrl Pts',(25.1112375971182,5.93430523086776,0.));
#254954=CARTESIAN_POINT('Ctrl Pts',(25.1112375971182,5.93430523086776,12.));
#254955=CARTESIAN_POINT('Ctrl Pts',(25.0905409050863,5.91547170844382,0.));
#254956=CARTESIAN_POINT('Ctrl Pts',(25.0905409050863,5.91547170844382,12.));
#254957=CARTESIAN_POINT('Ctrl Pts',(25.0698535426593,5.89673135155459,0.));
#254958=CARTESIAN_POINT('Ctrl Pts',(25.0698535426593,5.89673135155459,12.));
#254959=CARTESIAN_POINT('Ctrl Pts',(25.0491760405965,5.87808428385329,0.));
#254960=CARTESIAN_POINT('Ctrl Pts',(25.0491760405965,5.87808428385329,12.));
#254961=CARTESIAN_POINT('Ctrl Pts',(25.0285089498922,5.8595306315681,0.));
#254962=CARTESIAN_POINT('Ctrl Pts',(25.0285089498922,5.8595306315681,12.));
#254963=CARTESIAN_POINT('Ctrl Pts',(25.0078528200558,5.84107051963074,0.));
#254964=CARTESIAN_POINT('Ctrl Pts',(25.0078528200558,5.84107051963074,12.));
#254965=CARTESIAN_POINT('Ctrl Pts',(24.9872081752709,5.82270406744214,0.));
#254966=CARTESIAN_POINT('Ctrl Pts',(24.9872081752709,5.82270406744214,12.));
#254967=CARTESIAN_POINT('Ctrl Pts',(24.9665754954462,5.80443138549747,0.));
#254968=CARTESIAN_POINT('Ctrl Pts',(24.9665754954462,5.80443138549747,12.));
#254969=CARTESIAN_POINT('Ctrl Pts',(24.9459552293308,5.78625257775703,0.));
#254970=CARTESIAN_POINT('Ctrl Pts',(24.9459552293308,5.78625257775703,12.));
#254971=CARTESIAN_POINT('Ctrl Pts',(24.9253478043632,5.76816774342236,0.));
#254972=CARTESIAN_POINT('Ctrl Pts',(24.9253478043632,5.76816774342236,12.));
#254973=CARTESIAN_POINT('Ctrl Pts',(24.9047536376467,5.75017697890813,0.));
#254974=CARTESIAN_POINT('Ctrl Pts',(24.9047536376467,5.75017697890813,12.));
#254975=CARTESIAN_POINT('Ctrl Pts',(24.8841731467219,5.73228037976927,0.));
#254976=CARTESIAN_POINT('Ctrl Pts',(24.8841731467219,5.73228037976927,12.));
#254977=CARTESIAN_POINT('Ctrl Pts',(24.8636067597677,5.71447804252019,0.));
#254978=CARTESIAN_POINT('Ctrl Pts',(24.8636067597677,5.71447804252019,12.));
#254979=CARTESIAN_POINT('Ctrl Pts',(24.8430549277634,5.6967700667943,0.));
#254980=CARTESIAN_POINT('Ctrl Pts',(24.8430549277634,5.6967700667943,12.));
#254981=CARTESIAN_POINT('Ctrl Pts',(24.822518122386,5.67915655496524,0.));
#254982=CARTESIAN_POINT('Ctrl Pts',(24.822518122386,5.67915655496524,12.));
#254983=CARTESIAN_POINT('Ctrl Pts',(24.8019968304618,5.66163761114903,0.));
#254984=CARTESIAN_POINT('Ctrl Pts',(24.8019968304618,5.66163761114903,12.));
#254985=CARTESIAN_POINT('Ctrl Pts',(24.7814915496728,5.64421334042248,0.));
#254986=CARTESIAN_POINT('Ctrl Pts',(24.7814915496728,5.64421334042248,12.));
#254987=CARTESIAN_POINT('Ctrl Pts',(24.76100278357,5.62688384790919,0.));
#254988=CARTESIAN_POINT('Ctrl Pts',(24.76100278357,5.62688384790919,12.));
#254989=CARTESIAN_POINT('Ctrl Pts',(24.7405310372736,5.60964923798495,0.));
#254990=CARTESIAN_POINT('Ctrl Pts',(24.7405310372736,5.60964923798495,12.));
#254991=CARTESIAN_POINT('Ctrl Pts',(24.7200768119079,5.59250961323995,0.));
#254992=CARTESIAN_POINT('Ctrl Pts',(24.7200768119079,5.59250961323995,12.));
#254993=CARTESIAN_POINT('Ctrl Pts',(24.6996406035507,5.57546507427767,0.));
#254994=CARTESIAN_POINT('Ctrl Pts',(24.6996406035507,5.57546507427767,12.));
#254995=CARTESIAN_POINT('Ctrl Pts',(24.6792229061785,5.55851572025389,0.));
#254996=CARTESIAN_POINT('Ctrl Pts',(24.6792229061785,5.55851572025389,12.));
#254997=CARTESIAN_POINT('Ctrl Pts',(24.6588242134733,5.54166164919593,0.));
#254998=CARTESIAN_POINT('Ctrl Pts',(24.6588242134733,5.54166164919593,12.));
#254999=CARTESIAN_POINT('Ctrl Pts',(24.6384450211466,5.52490295840996,0.));
#255000=CARTESIAN_POINT('Ctrl Pts',(24.6384450211466,5.52490295840996,12.));
#255001=CARTESIAN_POINT('Ctrl Pts',(24.618085828918,5.50823974481959,0.));
#255002=CARTESIAN_POINT('Ctrl Pts',(24.618085828918,5.50823974481959,12.));
#255003=CARTESIAN_POINT('Ctrl Pts',(24.5977471429365,5.49167210537235,0.));
#255004=CARTESIAN_POINT('Ctrl Pts',(24.5977471429365,5.49167210537235,12.));
#255005=CARTESIAN_POINT('Ctrl Pts',(24.5774294770329,5.47520013724403,0.));
#255006=CARTESIAN_POINT('Ctrl Pts',(24.5774294770329,5.47520013724403,12.));
#255007=CARTESIAN_POINT('Ctrl Pts',(24.5571333514841,5.45882393762244,0.));
#255008=CARTESIAN_POINT('Ctrl Pts',(24.5571333514841,5.45882393762244,12.));
#255009=CARTESIAN_POINT('Ctrl Pts',(24.5368592922861,5.44254360356866,0.));
#255010=CARTESIAN_POINT('Ctrl Pts',(24.5368592922861,5.44254360356866,12.));
#255011=CARTESIAN_POINT('Ctrl Pts',(24.5166078302107,5.42635923183411,0.));
#255012=CARTESIAN_POINT('Ctrl Pts',(24.5166078302107,5.42635923183411,12.));
#255013=CARTESIAN_POINT('Ctrl Pts',(24.4963794999831,5.41027091869242,0.));
#255014=CARTESIAN_POINT('Ctrl Pts',(24.4963794999831,5.41027091869242,12.));
#255015=CARTESIAN_POINT('Ctrl Pts',(24.4761748393322,5.39427875973831,0.));
#255016=CARTESIAN_POINT('Ctrl Pts',(24.4761748393322,5.39427875973831,12.));
#255017=CARTESIAN_POINT('Ctrl Pts',(24.4559943883159,5.37838284973706,0.));
#255018=CARTESIAN_POINT('Ctrl Pts',(24.4559943883159,5.37838284973706,12.));
#255019=CARTESIAN_POINT('Ctrl Pts',(24.4358386899152,5.36258328273639,0.));
#255020=CARTESIAN_POINT('Ctrl Pts',(24.4358386899152,5.36258328273639,12.));
#255021=CARTESIAN_POINT('Ctrl Pts',(24.4157082904615,5.34688015213546,0.));
#255022=CARTESIAN_POINT('Ctrl Pts',(24.4157082904615,5.34688015213546,12.));
#255023=CARTESIAN_POINT('Ctrl Pts',(24.3956037401293,5.33127355076037,0.));
#255024=CARTESIAN_POINT('Ctrl Pts',(24.3956037401293,5.33127355076037,12.));
#255025=CARTESIAN_POINT('Ctrl Pts',(24.3755255933917,5.31576357092525,0.));
#255026=CARTESIAN_POINT('Ctrl Pts',(24.3755255933917,5.31576357092525,12.));
#255027=CARTESIAN_POINT('Ctrl Pts',(24.3554744095075,5.30035030449059,0.));
#255028=CARTESIAN_POINT('Ctrl Pts',(24.3554744095075,5.30035030449059,12.));
#255029=CARTESIAN_POINT('Ctrl Pts',(24.3354507529415,5.28503384290644,0.));
#255030=CARTESIAN_POINT('Ctrl Pts',(24.3354507529415,5.28503384290644,12.));
#255031=CARTESIAN_POINT('Ctrl Pts',(24.3154551932222,5.26981427718796,0.));
#255032=CARTESIAN_POINT('Ctrl Pts',(24.3154551932222,5.26981427718796,12.));
#255033=CARTESIAN_POINT('Ctrl Pts',(24.2954883048448,5.25469169788856,0.));
#255034=CARTESIAN_POINT('Ctrl Pts',(24.2954883048448,5.25469169788856,12.));
#255035=CARTESIAN_POINT('Ctrl Pts',(24.2755506671526,5.23966619506289,0.));
#255036=CARTESIAN_POINT('Ctrl Pts',(24.2755506671526,5.23966619506289,12.));
#255037=CARTESIAN_POINT('Ctrl Pts',(24.2556428642294,5.22473785822441,0.));
#255038=CARTESIAN_POINT('Ctrl Pts',(24.2556428642294,5.22473785822441,12.));
#255039=CARTESIAN_POINT('Ctrl Pts',(24.2357654847765,5.20990677629173,0.));
#255040=CARTESIAN_POINT('Ctrl Pts',(24.2357654847765,5.20990677629173,12.));
#255041=CARTESIAN_POINT('Ctrl Pts',(24.215919122017,5.19517303753643,0.));
#255042=CARTESIAN_POINT('Ctrl Pts',(24.215919122017,5.19517303753643,12.));
#255043=CARTESIAN_POINT('Ctrl Pts',(24.1961043738754,5.18053672961392,0.));
#255044=CARTESIAN_POINT('Ctrl Pts',(24.1961043738754,5.18053672961392,12.));
#255045=CARTESIAN_POINT('Ctrl Pts',(24.1763218431343,5.16599793957979,0.));
#255046=CARTESIAN_POINT('Ctrl Pts',(24.1763218431343,5.16599793957979,12.));
#255047=CARTESIAN_POINT('Ctrl Pts',(24.156572137597,5.15155675390075,0.));
#255048=CARTESIAN_POINT('Ctrl Pts',(24.156572137597,5.15155675390075,12.));
#255049=CARTESIAN_POINT('Ctrl Pts',(24.1368558702443,5.13721325845745,0.));
#255050=CARTESIAN_POINT('Ctrl Pts',(24.1368558702443,5.13721325845745,12.));
#255051=CARTESIAN_POINT('Ctrl Pts',(24.117173659394,5.1229675385386,0.));
#255052=CARTESIAN_POINT('Ctrl Pts',(24.117173659394,5.1229675385386,12.));
#255053=CARTESIAN_POINT('Ctrl Pts',(24.0975261288446,5.10881967883132,0.));
#255054=CARTESIAN_POINT('Ctrl Pts',(24.0975261288446,5.10881967883132,12.));
#255055=CARTESIAN_POINT('Ctrl Pts',(24.0779139079266,5.09476976342625,0.));
#255056=CARTESIAN_POINT('Ctrl Pts',(24.0779139079266,5.09476976342625,12.));
#255057=CARTESIAN_POINT('Ctrl Pts',(24.0583376315638,5.08081787581277,0.));
#255058=CARTESIAN_POINT('Ctrl Pts',(24.0583376315638,5.08081787581277,12.));
#255059=CARTESIAN_POINT('Ctrl Pts',(24.0387979403268,5.06696409886641,0.));
#255060=CARTESIAN_POINT('Ctrl Pts',(24.0387979403268,5.06696409886641,12.));
#255061=CARTESIAN_POINT('Ctrl Pts',(24.0192954804896,5.05320851483065,0.));
#255062=CARTESIAN_POINT('Ctrl Pts',(24.0192954804896,5.05320851483065,12.));
#255063=CARTESIAN_POINT('Ctrl Pts',(23.9998309040746,5.03955120528521,0.));
#255064=CARTESIAN_POINT('Ctrl Pts',(23.9998309040746,5.03955120528521,12.));
#255065=CARTESIAN_POINT('Ctrl Pts',(23.9804048689227,5.02599225112454,0.));
#255066=CARTESIAN_POINT('Ctrl Pts',(23.9804048689227,5.02599225112454,12.));
#255067=CARTESIAN_POINT('Ctrl Pts',(23.961018038827,5.01253173257453,0.));
#255068=CARTESIAN_POINT('Ctrl Pts',(23.961018038827,5.01253173257453,12.));
#255069=CARTESIAN_POINT('Ctrl Pts',(23.9416710836529,4.99916972919307,0.));
#255070=CARTESIAN_POINT('Ctrl Pts',(23.9416710836529,4.99916972919307,12.));
#255071=CARTESIAN_POINT('Ctrl Pts',(23.9223646794592,4.98590631986533,0.));
#255072=CARTESIAN_POINT('Ctrl Pts',(23.9223646794592,4.98590631986533,12.));
#255073=CARTESIAN_POINT('Ctrl Pts',(23.9030995086163,4.97274158279227,0.));
#255074=CARTESIAN_POINT('Ctrl Pts',(23.9030995086163,4.97274158279227,12.));
#255075=CARTESIAN_POINT('Ctrl Pts',(23.8838762599218,4.95967559546561,0.));
#255076=CARTESIAN_POINT('Ctrl Pts',(23.8838762599218,4.95967559546561,12.));
#255077=CARTESIAN_POINT('Ctrl Pts',(23.8646956287168,4.9467084346586,0.));
#255078=CARTESIAN_POINT('Ctrl Pts',(23.8646956287168,4.9467084346586,12.));
#255079=CARTESIAN_POINT('Ctrl Pts',(23.8455583170057,4.93384017643432,0.));
#255080=CARTESIAN_POINT('Ctrl Pts',(23.8455583170057,4.93384017643432,12.));
#255081=CARTESIAN_POINT('Ctrl Pts',(23.8264650335717,4.92107089613969,0.));
#255082=CARTESIAN_POINT('Ctrl Pts',(23.8264650335717,4.92107089613969,12.));
#255083=CARTESIAN_POINT('Ctrl Pts',(23.8074164940896,4.90840066839344,0.));
#255084=CARTESIAN_POINT('Ctrl Pts',(23.8074164940896,4.90840066839344,12.));
#255085=CARTESIAN_POINT('Ctrl Pts',(23.7884134212384,4.89582956706775,0.));
#255086=CARTESIAN_POINT('Ctrl Pts',(23.7884134212384,4.89582956706775,12.));
#255087=CARTESIAN_POINT('Ctrl Pts',(23.7694565448049,4.88335766525573,0.));
#255088=CARTESIAN_POINT('Ctrl Pts',(23.7694565448049,4.88335766525573,12.));
#255089=CARTESIAN_POINT('Ctrl Pts',(23.7505466018245,4.87098503527152,0.));
#255090=CARTESIAN_POINT('Ctrl Pts',(23.7505466018245,4.87098503527152,12.));
#255091=CARTESIAN_POINT('Ctrl Pts',(23.7316843367313,4.85871174865499,0.));
#255092=CARTESIAN_POINT('Ctrl Pts',(23.7316843367313,4.85871174865499,12.));
#255093=CARTESIAN_POINT('Ctrl Pts',(23.7128705015017,4.84653787616426,0.));
#255094=CARTESIAN_POINT('Ctrl Pts',(23.7128705015017,4.84653787616426,12.));
#255095=CARTESIAN_POINT('Ctrl Pts',(23.6941058557971,4.83446348776266,0.));
#255096=CARTESIAN_POINT('Ctrl Pts',(23.6941058557971,4.83446348776266,12.));
#255097=CARTESIAN_POINT('Ctrl Pts',(23.675391167102,4.82248865259562,0.));
#255098=CARTESIAN_POINT('Ctrl Pts',(23.675391167102,4.82248865259562,12.));
#255099=CARTESIAN_POINT('Ctrl Pts',(23.6567272108628,4.81061343896432,0.));
#255100=CARTESIAN_POINT('Ctrl Pts',(23.6567272108628,4.81061343896432,12.));
#255101=CARTESIAN_POINT('Ctrl Pts',(23.6381147706579,4.7988379143322,0.));
#255102=CARTESIAN_POINT('Ctrl Pts',(23.6381147706579,4.7988379143322,12.));
#255103=CARTESIAN_POINT('Ctrl Pts',(23.6195546383624,4.78716214532098,0.));
#255104=CARTESIAN_POINT('Ctrl Pts',(23.6195546383624,4.78716214532098,12.));
#255105=CARTESIAN_POINT('Ctrl Pts',(23.6010476143099,4.77558619769872,0.));
#255106=CARTESIAN_POINT('Ctrl Pts',(23.6010476143099,4.77558619769872,12.));
#255107=CARTESIAN_POINT('Ctrl Pts',(23.5825945074535,4.76411013636251,0.));
#255108=CARTESIAN_POINT('Ctrl Pts',(23.5825945074535,4.76411013636251,12.));
#255109=CARTESIAN_POINT('Ctrl Pts',(23.5641961355168,4.75273402530617,0.));
#255110=CARTESIAN_POINT('Ctrl Pts',(23.5641961355168,4.75273402530617,12.));
#255111=CARTESIAN_POINT('Ctrl Pts',(23.545853325171,4.74145792760699,0.));
#255112=CARTESIAN_POINT('Ctrl Pts',(23.545853325171,4.74145792760699,12.));
#255113=CARTESIAN_POINT('Ctrl Pts',(23.5275669122372,4.7302819054303,0.));
#255114=CARTESIAN_POINT('Ctrl Pts',(23.5275669122372,4.7302819054303,12.));
#255115=CARTESIAN_POINT('Ctrl Pts',(23.509337741878,4.71920602001902,0.));
#255116=CARTESIAN_POINT('Ctrl Pts',(23.509337741878,4.71920602001902,12.));
#255117=CARTESIAN_POINT('Ctrl Pts',(23.491166668789,4.70823033167819,0.));
#255118=CARTESIAN_POINT('Ctrl Pts',(23.491166668789,4.70823033167819,12.));
#255119=CARTESIAN_POINT('Ctrl Pts',(23.4730545573853,4.69735489975024,0.));
#255120=CARTESIAN_POINT('Ctrl Pts',(23.4730545573853,4.69735489975024,12.));
#255121=CARTESIAN_POINT('Ctrl Pts',(23.455002281986,4.68657978258303,0.));
#255122=CARTESIAN_POINT('Ctrl Pts',(23.455002281986,4.68657978258303,12.));
#255123=CARTESIAN_POINT('Ctrl Pts',(23.4370107270451,4.67590503753059,0.));
#255124=CARTESIAN_POINT('Ctrl Pts',(23.4370107270451,4.67590503753059,12.));
#255125=CARTESIAN_POINT('Ctrl Pts',(23.4190807873803,4.6653307209467,0.));
#255126=CARTESIAN_POINT('Ctrl Pts',(23.4190807873803,4.6653307209467,12.));
#255127=CARTESIAN_POINT('Ctrl Pts',(23.4012133683959,4.65485688816924,0.));
#255128=CARTESIAN_POINT('Ctrl Pts',(23.4012133683959,4.65485688816924,12.));
#255129=CARTESIAN_POINT('Ctrl Pts',(23.3834093863068,4.6444835934993,0.));
#255130=CARTESIAN_POINT('Ctrl Pts',(23.3834093863068,4.6444835934993,12.));
#255131=CARTESIAN_POINT('Ctrl Pts',(23.3656697683489,4.63421089016541,0.));
#255132=CARTESIAN_POINT('Ctrl Pts',(23.3656697683489,4.63421089016541,12.));
#255133=CARTESIAN_POINT('Ctrl Pts',(23.3479954530272,4.62403883030805,0.));
#255134=CARTESIAN_POINT('Ctrl Pts',(23.3479954530272,4.62403883030805,12.));
#255135=CARTESIAN_POINT('Ctrl Pts',(23.3303873903938,4.6139674649783,0.));
#255136=CARTESIAN_POINT('Ctrl Pts',(23.3303873903938,4.6139674649783,12.));
#255137=CARTESIAN_POINT('Ctrl Pts',(23.3128465423115,4.60399684412163,0.));
#255138=CARTESIAN_POINT('Ctrl Pts',(23.3128465423115,4.60399684412163,12.));
#255139=CARTESIAN_POINT('Ctrl Pts',(23.2953738827191,4.5941270165575,0.));
#255140=CARTESIAN_POINT('Ctrl Pts',(23.2953738827191,4.5941270165575,12.));
#255141=CARTESIAN_POINT('Ctrl Pts',(23.2779703978876,4.5843580299469,0.));
#255142=CARTESIAN_POINT('Ctrl Pts',(23.2779703978876,4.5843580299469,12.));
#255143=CARTESIAN_POINT('Ctrl Pts',(23.2606370866866,4.57468993076097,0.));
#255144=CARTESIAN_POINT('Ctrl Pts',(23.2606370866866,4.57468993076097,12.));
#255145=CARTESIAN_POINT('Ctrl Pts',(23.2433749609131,4.56512276427839,0.));
#255146=CARTESIAN_POINT('Ctrl Pts',(23.2433749609131,4.56512276427839,12.));
#255147=CARTESIAN_POINT('Ctrl Pts',(23.2261850456064,4.55565657456975,0.));
#255148=CARTESIAN_POINT('Ctrl Pts',(23.2261850456064,4.55565657456975,12.));
#255149=CARTESIAN_POINT('Ctrl Pts',(23.2090683793629,4.54629140447544,0.));
#255150=CARTESIAN_POINT('Ctrl Pts',(23.2090683793629,4.54629140447544,12.));
#255151=CARTESIAN_POINT('Ctrl Pts',(23.1920260146465,4.53702729557566,0.));
#255152=CARTESIAN_POINT('Ctrl Pts',(23.1920260146465,4.53702729557566,12.));
#255153=CARTESIAN_POINT('Ctrl Pts',(23.1750590180908,4.52786428815015,0.));
#255154=CARTESIAN_POINT('Ctrl Pts',(23.1750590180908,4.52786428815015,12.));
#255155=CARTESIAN_POINT('Ctrl Pts',(23.1581684708761,4.51880242116748,0.));
#255156=CARTESIAN_POINT('Ctrl Pts',(23.1581684708761,4.51880242116748,12.));
#255157=CARTESIAN_POINT('Ctrl Pts',(23.1413554691123,4.5098417322706,0.));
#255158=CARTESIAN_POINT('Ctrl Pts',(23.1413554691123,4.5098417322706,12.));
#255159=CARTESIAN_POINT('Ctrl Pts',(23.1246211242115,4.50098225775171,0.));
#255160=CARTESIAN_POINT('Ctrl Pts',(23.1246211242115,4.50098225775171,12.));
#255161=CARTESIAN_POINT('Ctrl Pts',(23.1079665632636,4.49222403252216,0.));
#255162=CARTESIAN_POINT('Ctrl Pts',(23.1079665632636,4.49222403252216,12.));
#255163=CARTESIAN_POINT('Ctrl Pts',(23.0913929293922,4.48356709006788,0.));
#255164=CARTESIAN_POINT('Ctrl Pts',(23.0913929293922,4.48356709006788,12.));
#255165=CARTESIAN_POINT('Ctrl Pts',(23.0749013821881,4.47501146242856,0.));
#255166=CARTESIAN_POINT('Ctrl Pts',(23.0749013821881,4.47501146242856,12.));
#255167=CARTESIAN_POINT('Ctrl Pts',(23.0584930981732,4.46655718018231,0.));
#255168=CARTESIAN_POINT('Ctrl Pts',(23.0584930981732,4.46655718018231,12.));
#255169=CARTESIAN_POINT('Ctrl Pts',(23.0421692712467,4.45820427241683,0.));
#255170=CARTESIAN_POINT('Ctrl Pts',(23.0421692712467,4.45820427241683,12.));
#255171=CARTESIAN_POINT('Ctrl Pts',(23.0259311131392,4.44995276669687,0.));
#255172=CARTESIAN_POINT('Ctrl Pts',(23.0259311131392,4.44995276669687,12.));
#255173=CARTESIAN_POINT('Ctrl Pts',(23.0097798538395,4.44180268901643,0.));
#255174=CARTESIAN_POINT('Ctrl Pts',(23.0097798538395,4.44180268901643,12.));
#255175=CARTESIAN_POINT('Ctrl Pts',(22.9937167421006,4.43375406376879,0.));
#255176=CARTESIAN_POINT('Ctrl Pts',(22.9937167421006,4.43375406376879,12.));
#255177=CARTESIAN_POINT('Ctrl Pts',(22.977743046002,4.42580691372752,0.));
#255178=CARTESIAN_POINT('Ctrl Pts',(22.977743046002,4.42580691372752,12.));
#255179=CARTESIAN_POINT('Ctrl Pts',(22.9618600534866,4.41796126001302,0.));
#255180=CARTESIAN_POINT('Ctrl Pts',(22.9618600534866,4.41796126001302,12.));
#255181=CARTESIAN_POINT('Ctrl Pts',(22.9460690729093,4.41021712205554,0.));
#255182=CARTESIAN_POINT('Ctrl Pts',(22.9460690729093,4.41021712205554,12.));
#255183=CARTESIAN_POINT('Ctrl Pts',(22.930371433555,4.40257451754324,0.));
#255184=CARTESIAN_POINT('Ctrl Pts',(22.930371433555,4.40257451754324,12.));
#255185=CARTESIAN_POINT('Ctrl Pts',(22.9147684862426,4.39503346238473,0.));
#255186=CARTESIAN_POINT('Ctrl Pts',(22.9147684862426,4.39503346238473,12.));
#255187=CARTESIAN_POINT('Ctrl Pts',(22.8992616040108,4.38759397068406,0.));
#255188=CARTESIAN_POINT('Ctrl Pts',(22.8992616040108,4.38759397068406,12.));
#255189=CARTESIAN_POINT('Ctrl Pts',(22.8838521827701,4.38025605470093,0.));
#255190=CARTESIAN_POINT('Ctrl Pts',(22.8838521827701,4.38025605470093,12.));
#255191=CARTESIAN_POINT('Ctrl Pts',(22.8685416419725,4.37301972480746,0.));
#255192=CARTESIAN_POINT('Ctrl Pts',(22.8685416419725,4.37301972480746,12.));
#255193=CARTESIAN_POINT('Ctrl Pts',(22.8533314252422,4.36588498942997,0.));
#255194=CARTESIAN_POINT('Ctrl Pts',(22.8533314252422,4.36588498942997,12.));
#255195=CARTESIAN_POINT('Ctrl Pts',(22.8382230011184,4.35885185500546,0.));
#255196=CARTESIAN_POINT('Ctrl Pts',(22.8382230011184,4.35885185500546,12.));
#255197=CARTESIAN_POINT('Ctrl Pts',(22.8232178638876,4.35192032594791,0.));
#255198=CARTESIAN_POINT('Ctrl Pts',(22.8232178638876,4.35192032594791,12.));
#255199=CARTESIAN_POINT('Ctrl Pts',(22.8083175343791,4.34509040460062,0.));
#255200=CARTESIAN_POINT('Ctrl Pts',(22.8083175343791,4.34509040460062,12.));
#255201=CARTESIAN_POINT('Ctrl Pts',(22.7935235607806,4.33836209118446,0.));
#255202=CARTESIAN_POINT('Ctrl Pts',(22.7935235607806,4.33836209118446,12.));
#255203=CARTESIAN_POINT('Ctrl Pts',(22.7788375194076,4.3317353837319,0.));
#255204=CARTESIAN_POINT('Ctrl Pts',(22.7788375194076,4.3317353837319,12.));
#255205=CARTESIAN_POINT('Ctrl Pts',(22.7642610156475,4.32521027803754,0.));
#255206=CARTESIAN_POINT('Ctrl Pts',(22.7642610156475,4.32521027803754,12.));
#255207=CARTESIAN_POINT('Ctrl Pts',(22.7497956849848,4.31878676761235,0.));
#255208=CARTESIAN_POINT('Ctrl Pts',(22.7497956849848,4.31878676761235,12.));
#255209=CARTESIAN_POINT('Ctrl Pts',(22.7354431939926,4.31246484362549,0.));
#255210=CARTESIAN_POINT('Ctrl Pts',(22.7354431939926,4.31246484362549,12.));
#255211=CARTESIAN_POINT('Ctrl Pts',(22.7212052413386,4.30624449484069,0.));
#255212=CARTESIAN_POINT('Ctrl Pts',(22.7212052413386,4.30624449484069,12.));
#255213=CARTESIAN_POINT('Ctrl Pts',(22.7070835587564,4.3001257075406,0.));
#255214=CARTESIAN_POINT('Ctrl Pts',(22.7070835587564,4.3001257075406,12.));
#255215=CARTESIAN_POINT('Ctrl Pts',(22.6930799122548,4.29410846547056,0.));
#255216=CARTESIAN_POINT('Ctrl Pts',(22.6930799122548,4.29410846547056,12.));
#255217=CARTESIAN_POINT('Ctrl Pts',(22.6791961033537,4.28819274977763,0.));
#255218=CARTESIAN_POINT('Ctrl Pts',(22.6791961033537,4.28819274977763,12.));
#255219=CARTESIAN_POINT('Ctrl Pts',(22.6654339703109,4.28237853894059,0.));
#255220=CARTESIAN_POINT('Ctrl Pts',(22.6654339703109,4.28237853894059,12.));
#255221=CARTESIAN_POINT('Ctrl Pts',(22.6517953893303,4.2766658086912,0.));
#255222=CARTESIAN_POINT('Ctrl Pts',(22.6517953893303,4.2766658086912,12.));
#255223=CARTESIAN_POINT('Ctrl Pts',(22.6382822758172,4.27105453193004,0.));
#255224=CARTESIAN_POINT('Ctrl Pts',(22.6382822758172,4.27105453193004,12.));
#255225=CARTESIAN_POINT('Ctrl Pts',(22.6248965859977,4.26554467865576,0.));
#255226=CARTESIAN_POINT('Ctrl Pts',(22.6248965859977,4.26554467865576,12.));
#255227=CARTESIAN_POINT('Ctrl Pts',(22.6116403184821,4.26013621588305,0.));
#255228=CARTESIAN_POINT('Ctrl Pts',(22.6116403184821,4.26013621588305,12.));
#255229=CARTESIAN_POINT('Ctrl Pts',(22.5985155158636,4.25482910755481,0.));
#255230=CARTESIAN_POINT('Ctrl Pts',(22.5985155158636,4.25482910755481,12.));
#255231=CARTESIAN_POINT('Ctrl Pts',(22.5855242662477,4.24962331444177,0.));
#255232=CARTESIAN_POINT('Ctrl Pts',(22.5855242662477,4.24962331444177,12.));
#255233=CARTESIAN_POINT('Ctrl Pts',(22.572668704992,4.24451879404851,0.));
#255234=CARTESIAN_POINT('Ctrl Pts',(22.572668704992,4.24451879404851,12.));
#255235=CARTESIAN_POINT('Ctrl Pts',(22.5599510166429,4.23951550052523,0.));
#255236=CARTESIAN_POINT('Ctrl Pts',(22.5599510166429,4.23951550052523,12.));
#255237=CARTESIAN_POINT('Ctrl Pts',(22.5473734368086,4.23461338456712,0.));
#255238=CARTESIAN_POINT('Ctrl Pts',(22.5473734368086,4.23461338456712,12.));
#255239=CARTESIAN_POINT('Ctrl Pts',(22.5349382540588,4.22981239330733,0.));
#255240=CARTESIAN_POINT('Ctrl Pts',(22.5349382540588,4.22981239330733,12.));
#255241=CARTESIAN_POINT('Ctrl Pts',(22.5226478117886,4.22511247020041,0.));
#255242=CARTESIAN_POINT('Ctrl Pts',(22.5226478117886,4.22511247020041,12.));
#255243=CARTESIAN_POINT('Ctrl Pts',(22.5105045108881,4.22051355490196,0.));
#255244=CARTESIAN_POINT('Ctrl Pts',(22.5105045108881,4.22051355490196,12.));
#255245=CARTESIAN_POINT('Ctrl Pts',(22.4985108124228,4.21601558313906,0.));
#255246=CARTESIAN_POINT('Ctrl Pts',(22.4985108124228,4.21601558313906,12.));
#255247=CARTESIAN_POINT('Ctrl Pts',(22.4866692403147,4.21161848657428,0.));
#255248=CARTESIAN_POINT('Ctrl Pts',(22.4866692403147,4.21161848657428,12.));
#255249=CARTESIAN_POINT('Ctrl Pts',(22.4749823839917,4.20732219265649,0.));
#255250=CARTESIAN_POINT('Ctrl Pts',(22.4749823839917,4.20732219265649,12.));
#255251=CARTESIAN_POINT('Ctrl Pts',(22.4634529011437,4.20312662448174,0.));
#255252=CARTESIAN_POINT('Ctrl Pts',(22.4634529011437,4.20312662448174,12.));
#255253=CARTESIAN_POINT('Ctrl Pts',(22.4520835205422,4.19903170066358,0.));
#255254=CARTESIAN_POINT('Ctrl Pts',(22.4520835205422,4.19903170066358,12.));
#255255=CARTESIAN_POINT('Ctrl Pts',(22.4408770448917,4.1950373351886,0.));
#255256=CARTESIAN_POINT('Ctrl Pts',(22.4408770448917,4.1950373351886,12.));
#255257=CARTESIAN_POINT('Ctrl Pts',(22.4298363535416,4.19114343726932,0.));
#255258=CARTESIAN_POINT('Ctrl Pts',(22.4298363535416,4.19114343726932,12.));
#255259=CARTESIAN_POINT('Ctrl Pts',(22.4189644056109,4.18734991117707,0.));
#255260=CARTESIAN_POINT('Ctrl Pts',(22.4189644056109,4.18734991117707,12.));
#255261=CARTESIAN_POINT('Ctrl Pts',(22.4082642454448,4.18365665600839,0.));
#255262=CARTESIAN_POINT('Ctrl Pts',(22.4082642454448,4.18365665600839,12.));
#255263=CARTESIAN_POINT('Ctrl Pts',(22.3977390078074,4.18006356544879,0.));
#255264=CARTESIAN_POINT('Ctrl Pts',(22.3977390078074,4.18006356544879,12.));
#255265=CARTESIAN_POINT('Ctrl Pts',(22.3873919231339,4.17657052752834,0.));
#255266=CARTESIAN_POINT('Ctrl Pts',(22.3873919231339,4.17657052752834,12.));
#255267=CARTESIAN_POINT('Ctrl Pts',(22.3772263228624,4.17317742436162,0.));
#255268=CARTESIAN_POINT('Ctrl Pts',(22.3772263228624,4.17317742436162,12.));
#255269=CARTESIAN_POINT('Ctrl Pts',(22.3672456427605,4.1698841319947,0.));
#255270=CARTESIAN_POINT('Ctrl Pts',(22.3672456427605,4.1698841319947,12.));
#255271=CARTESIAN_POINT('Ctrl Pts',(22.3574534257397,4.16669052026602,0.));
#255272=CARTESIAN_POINT('Ctrl Pts',(22.3574534257397,4.16669052026602,12.));
#255273=CARTESIAN_POINT('Ctrl Pts',(22.3478533253886,4.1635964526318,0.));
#255274=CARTESIAN_POINT('Ctrl Pts',(22.3478533253886,4.1635964526318,12.));
#255275=CARTESIAN_POINT('Ctrl Pts',(22.3384491078599,4.16060178604154,0.));
#255276=CARTESIAN_POINT('Ctrl Pts',(22.3384491078599,4.16060178604154,12.));
#255277=CARTESIAN_POINT('Ctrl Pts',(22.3292446628957,4.15770637047882,0.));
#255278=CARTESIAN_POINT('Ctrl Pts',(22.3292446628957,4.15770637047882,12.));
#255279=CARTESIAN_POINT('Ctrl Pts',(22.3202440186979,4.15491004835278,0.));
#255280=CARTESIAN_POINT('Ctrl Pts',(22.3202440186979,4.15491004835278,12.));
#255281=CARTESIAN_POINT('Ctrl Pts',(22.3114513545186,4.15221265396993,0.));
#255282=CARTESIAN_POINT('Ctrl Pts',(22.3114513545186,4.15221265396993,12.));
#255283=CARTESIAN_POINT('Ctrl Pts',(22.3028710166935,4.14961401285526,0.));
#255284=CARTESIAN_POINT('Ctrl Pts',(22.3028710166935,4.14961401285526,12.));
#255285=CARTESIAN_POINT('Ctrl Pts',(22.2945075198468,4.14711394168559,0.));
#255286=CARTESIAN_POINT('Ctrl Pts',(22.2945075198468,4.14711394168559,12.));
#255287=CARTESIAN_POINT('Ctrl Pts',(22.2863655389167,4.14471224859295,0.));
#255288=CARTESIAN_POINT('Ctrl Pts',(22.2863655389167,4.14471224859295,12.));
#255289=CARTESIAN_POINT('Ctrl Pts',(22.2784499072026,4.14240873321982,0.));
#255290=CARTESIAN_POINT('Ctrl Pts',(22.2784499072026,4.14240873321982,12.));
#255291=CARTESIAN_POINT('Ctrl Pts',(22.2707656042456,4.14020318715988,0.));
#255292=CARTESIAN_POINT('Ctrl Pts',(22.2707656042456,4.14020318715988,12.));
#255293=CARTESIAN_POINT('Ctrl Pts',(22.263317791397,4.13809539255419,0.));
#255294=CARTESIAN_POINT('Ctrl Pts',(22.263317791397,4.13809539255419,12.));
#255295=CARTESIAN_POINT('Ctrl Pts',(22.2561118708422,4.13608511977226,0.));
#255296=CARTESIAN_POINT('Ctrl Pts',(22.2561118708422,4.13608511977226,12.));
#255297=CARTESIAN_POINT('Ctrl Pts',(22.2491535317789,4.13417212558809,0.));
#255298=CARTESIAN_POINT('Ctrl Pts',(22.2491535317789,4.13417212558809,12.));
#255299=CARTESIAN_POINT('Ctrl Pts',(22.2424488153523,4.1323561506016,0.));
#255300=CARTESIAN_POINT('Ctrl Pts',(22.2424488153523,4.1323561506016,12.));
#255301=CARTESIAN_POINT('Ctrl Pts',(22.2360040565534,4.13063692157499,0.));
#255302=CARTESIAN_POINT('Ctrl Pts',(22.2360040565534,4.13063692157499,12.));
#255303=CARTESIAN_POINT('Ctrl Pts',(22.2298258043947,4.12901415463379,0.));
#255304=CARTESIAN_POINT('Ctrl Pts',(22.2298258043947,4.12901415463379,12.));
#255305=CARTESIAN_POINT('Ctrl Pts',(22.2239207458781,4.127487558301,0.));
#255306=CARTESIAN_POINT('Ctrl Pts',(22.2239207458781,4.127487558301,12.));
#255307=CARTESIAN_POINT('Ctrl Pts',(22.2182956401341,4.126056836133,0.));
#255308=CARTESIAN_POINT('Ctrl Pts',(22.2182956401341,4.126056836133,12.));
#255309=CARTESIAN_POINT('Ctrl Pts',(22.2129576146671,4.12472167516602,0.));
#255310=CARTESIAN_POINT('Ctrl Pts',(22.2129576146671,4.12472167516602,12.));
#255311=CARTESIAN_POINT('Ctrl Pts',(22.2079143941719,4.12348173702025,0.));
#255312=CARTESIAN_POINT('Ctrl Pts',(22.2079143941719,4.12348173702025,12.));
#255313=CARTESIAN_POINT('Ctrl Pts',(22.2031746532106,4.12233664408237,0.));
#255314=CARTESIAN_POINT('Ctrl Pts',(22.2031746532106,4.12233664408237,12.));
#255315=CARTESIAN_POINT('Ctrl Pts',(22.1987479618246,4.12128598183533,0.));
#255316=CARTESIAN_POINT('Ctrl Pts',(22.1987479618246,4.12128598183533,12.));
#255317=CARTESIAN_POINT('Ctrl Pts',(22.1946440958098,4.12032932637738,0.));
#255318=CARTESIAN_POINT('Ctrl Pts',(22.1946440958098,4.12032932637738,12.));
#255319=CARTESIAN_POINT('Ctrl Pts',(22.1908725908525,4.11946626228623,0.));
#255320=CARTESIAN_POINT('Ctrl Pts',(22.1908725908525,4.11946626228623,12.));
#255321=CARTESIAN_POINT('Ctrl Pts',(22.1874419861496,4.11869641271752,0.));
#255322=CARTESIAN_POINT('Ctrl Pts',(22.1874419861496,4.11869641271752,12.));
#255323=CARTESIAN_POINT('Ctrl Pts',(22.1843613164855,4.11801938107464,0.));
#255324=CARTESIAN_POINT('Ctrl Pts',(22.1843613164855,4.11801938107464,12.));
#255325=CARTESIAN_POINT('Ctrl Pts',(22.1816414985788,4.11743469691765,0.));
#255326=CARTESIAN_POINT('Ctrl Pts',(22.1816414985788,4.11743469691765,12.));
#255327=CARTESIAN_POINT('Ctrl Pts',(22.179297473024,4.11694173195041,0.));
#255328=CARTESIAN_POINT('Ctrl Pts',(22.179297473024,4.11694173195041,12.));
#255329=CARTESIAN_POINT('Ctrl Pts',(22.177347426894,4.11653973150558,0.));
#255330=CARTESIAN_POINT('Ctrl Pts',(22.177347426894,4.11653973150558,12.));
#255331=CARTESIAN_POINT('Ctrl Pts',(22.1758088296598,4.11622797217066,0.));
#255332=CARTESIAN_POINT('Ctrl Pts',(22.1758088296598,4.11622797217066,12.));
#255333=CARTESIAN_POINT('Ctrl Pts',(22.1746949858773,4.11600589882768,0.));
#255334=CARTESIAN_POINT('Ctrl Pts',(22.1746949858773,4.11600589882768,12.));
#255335=CARTESIAN_POINT('Ctrl Pts',(22.174148802123,4.11589976826061,0.));
#255336=CARTESIAN_POINT('Ctrl Pts',(22.174148802123,4.11589976826061,12.));
#255337=CARTESIAN_POINT('Ctrl Pts',(22.1739341411684,4.1158603587821,0.));
#255338=CARTESIAN_POINT('Ctrl Pts',(22.1739341411684,4.1158603587821,12.));
#255339=CARTESIAN_POINT('Ctrl Pts',(22.1738776823239,4.11585194677412,0.));
#255340=CARTESIAN_POINT('Ctrl Pts',(22.1738776823239,4.11585194677412,12.));
#255341=CARTESIAN_POINT('Ctrl Pts',(22.1738711152697,4.11585220600461,0.));
#255342=CARTESIAN_POINT('Ctrl Pts',(22.1738711152697,4.11585220600461,12.));
#255343=CARTESIAN_POINT('Ctrl Pts',(22.4835757167854,1.76341220531179,0.));
#255344=CARTESIAN_POINT('Ctrl Pts',(22.4835757167854,1.76341220531179,12.));
#255345=CARTESIAN_POINT('Ctrl Pts',(22.483581992979,1.76341415538764,0.));
#255346=CARTESIAN_POINT('Ctrl Pts',(22.483581992979,1.76341415538764,12.));
#255347=CARTESIAN_POINT('Ctrl Pts',(22.4836387052232,1.7634206426357,0.));
#255348=CARTESIAN_POINT('Ctrl Pts',(22.4836387052232,1.7634206426357,12.));
#255349=CARTESIAN_POINT('Ctrl Pts',(22.4838562517069,1.76343813434565,0.));
#255350=CARTESIAN_POINT('Ctrl Pts',(22.4838562517069,1.76343813434565,12.));
#255351=CARTESIAN_POINT('Ctrl Pts',(22.4844112933129,1.76347698284792,0.));
#255352=CARTESIAN_POINT('Ctrl Pts',(22.4844112933129,1.76347698284792,12.));
#255353=CARTESIAN_POINT('Ctrl Pts',(22.4855446605991,1.76355076045546,0.));
#255354=CARTESIAN_POINT('Ctrl Pts',(22.4855446605991,1.76355076045546,12.));
#255355=CARTESIAN_POINT('Ctrl Pts',(22.4871115206571,1.76364784232963,0.));
#255356=CARTESIAN_POINT('Ctrl Pts',(22.4871115206571,1.76364784232963,12.));
#255357=CARTESIAN_POINT('Ctrl Pts',(22.4890991659478,1.76376424879505,0.));
#255358=CARTESIAN_POINT('Ctrl Pts',(22.4890991659478,1.76376424879505,12.));
#255359=CARTESIAN_POINT('Ctrl Pts',(22.4914909094908,1.76389475965724,0.));
#255360=CARTESIAN_POINT('Ctrl Pts',(22.4914909094908,1.76389475965724,12.));
#255361=CARTESIAN_POINT('Ctrl Pts',(22.4942693792449,1.76403393880301,0.));
#255362=CARTESIAN_POINT('Ctrl Pts',(22.4942693792449,1.76403393880301,12.));
#255363=CARTESIAN_POINT('Ctrl Pts',(22.4974203063191,1.76417731243462,0.));
#255364=CARTESIAN_POINT('Ctrl Pts',(22.4974203063191,1.76417731243462,12.));
#255365=CARTESIAN_POINT('Ctrl Pts',(22.5009332677316,1.76432160068726,0.));
#255366=CARTESIAN_POINT('Ctrl Pts',(22.5009332677316,1.76432160068726,12.));
#255367=CARTESIAN_POINT('Ctrl Pts',(22.5047996391978,1.76446408210366,0.));
#255368=CARTESIAN_POINT('Ctrl Pts',(22.5047996391978,1.76446408210366,12.));
#255369=CARTESIAN_POINT('Ctrl Pts',(22.5090112700212,1.76460218257323,0.));
#255370=CARTESIAN_POINT('Ctrl Pts',(22.5090112700212,1.76460218257323,12.));
#255371=CARTESIAN_POINT('Ctrl Pts',(22.5135590569554,1.76473303281159,0.));
#255372=CARTESIAN_POINT('Ctrl Pts',(22.5135590569554,1.76473303281159,12.));
#255373=CARTESIAN_POINT('Ctrl Pts',(22.5184336670207,1.76485369319896,0.));
#255374=CARTESIAN_POINT('Ctrl Pts',(22.5184336670207,1.76485369319896,12.));
#255375=CARTESIAN_POINT('Ctrl Pts',(22.5236259635515,1.76496128643369,0.));
#255376=CARTESIAN_POINT('Ctrl Pts',(22.5236259635515,1.76496128643369,12.));
#255377=CARTESIAN_POINT('Ctrl Pts',(22.529127665298,1.76505320262752,0.));
#255378=CARTESIAN_POINT('Ctrl Pts',(22.529127665298,1.76505320262752,12.));
#255379=CARTESIAN_POINT('Ctrl Pts',(22.5349313983571,1.7651271156325,0.));
#255380=CARTESIAN_POINT('Ctrl Pts',(22.5349313983571,1.7651271156325,12.));
#255381=CARTESIAN_POINT('Ctrl Pts',(22.5410303590891,1.76518087841493,0.));
#255382=CARTESIAN_POINT('Ctrl Pts',(22.5410303590891,1.76518087841493,12.));
#255383=CARTESIAN_POINT('Ctrl Pts',(22.5474180954006,1.76521245524047,0.));
#255384=CARTESIAN_POINT('Ctrl Pts',(22.5474180954006,1.76521245524047,12.));
#255385=CARTESIAN_POINT('Ctrl Pts',(22.5540882235837,1.76521983384063,0.));
#255386=CARTESIAN_POINT('Ctrl Pts',(22.5540882235837,1.76521983384063,12.));
#255387=CARTESIAN_POINT('Ctrl Pts',(22.5610344912501,1.7652010450045,0.));
#255388=CARTESIAN_POINT('Ctrl Pts',(22.5610344912501,1.7652010450045,12.));
#255389=CARTESIAN_POINT('Ctrl Pts',(22.5682508499873,1.76515418518829,0.));
#255390=CARTESIAN_POINT('Ctrl Pts',(22.5682508499873,1.76515418518829,12.));
#255391=CARTESIAN_POINT('Ctrl Pts',(22.5757315316355,1.76507744026747,0.));
#255392=CARTESIAN_POINT('Ctrl Pts',(22.5757315316355,1.76507744026747,12.));
#255393=CARTESIAN_POINT('Ctrl Pts',(22.5834711038024,1.76496910283089,0.));
#255394=CARTESIAN_POINT('Ctrl Pts',(22.5834711038024,1.76496910283089,12.));
#255395=CARTESIAN_POINT('Ctrl Pts',(22.5914644078106,1.76482755288411,0.));
#255396=CARTESIAN_POINT('Ctrl Pts',(22.5914644078106,1.76482755288411,12.));
#255397=CARTESIAN_POINT('Ctrl Pts',(22.5997065145638,1.76465124413556,0.));
#255398=CARTESIAN_POINT('Ctrl Pts',(22.5997065145638,1.76465124413556,12.));
#255399=CARTESIAN_POINT('Ctrl Pts',(22.6081926681342,1.76443868648015,0.));
#255400=CARTESIAN_POINT('Ctrl Pts',(22.6081926681342,1.76443868648015,12.));
#255401=CARTESIAN_POINT('Ctrl Pts',(22.6169182517693,1.76418843543739,0.));
#255402=CARTESIAN_POINT('Ctrl Pts',(22.6169182517693,1.76418843543739,12.));
#255403=CARTESIAN_POINT('Ctrl Pts',(22.6258787994847,1.76389909571402,0.));
#255404=CARTESIAN_POINT('Ctrl Pts',(22.6258787994847,1.76389909571402,12.));
#255405=CARTESIAN_POINT('Ctrl Pts',(22.635069997936,1.76356932176272,0.));
#255406=CARTESIAN_POINT('Ctrl Pts',(22.635069997936,1.76356932176272,12.));
#255407=CARTESIAN_POINT('Ctrl Pts',(22.6444876940425,1.76319782013914,0.));
#255408=CARTESIAN_POINT('Ctrl Pts',(22.6444876940425,1.76319782013914,12.));
#255409=CARTESIAN_POINT('Ctrl Pts',(22.6541278938413,1.76278334912559,0.));
#255410=CARTESIAN_POINT('Ctrl Pts',(22.6541278938413,1.76278334912559,12.));
#255411=CARTESIAN_POINT('Ctrl Pts',(22.6639867471756,1.76232471392568,0.));
#255412=CARTESIAN_POINT('Ctrl Pts',(22.6639867471756,1.76232471392568,12.));
#255413=CARTESIAN_POINT('Ctrl Pts',(22.6740605356699,1.76182076289525,0.));
#255414=CARTESIAN_POINT('Ctrl Pts',(22.6740605356699,1.76182076289525,12.));
#255415=CARTESIAN_POINT('Ctrl Pts',(22.6843456585245,1.76127038310613,0.));
#255416=CARTESIAN_POINT('Ctrl Pts',(22.6843456585245,1.76127038310613,12.));
#255417=CARTESIAN_POINT('Ctrl Pts',(22.6948386219843,1.76067249704884,0.));
#255418=CARTESIAN_POINT('Ctrl Pts',(22.6948386219843,1.76067249704884,12.));
#255419=CARTESIAN_POINT('Ctrl Pts',(22.7055360375481,1.76002606202399,0.));
#255420=CARTESIAN_POINT('Ctrl Pts',(22.7055360375481,1.76002606202399,12.));
#255421=CARTESIAN_POINT('Ctrl Pts',(22.7164346186007,1.75933006905924,0.));
#255422=CARTESIAN_POINT('Ctrl Pts',(22.7164346186007,1.75933006905924,12.));
#255423=CARTESIAN_POINT('Ctrl Pts',(22.7275311777305,1.75858354204635,0.));
#255424=CARTESIAN_POINT('Ctrl Pts',(22.7275311777305,1.75858354204635,12.));
#255425=CARTESIAN_POINT('Ctrl Pts',(22.7388226235565,1.75778553673249,0.));
#255426=CARTESIAN_POINT('Ctrl Pts',(22.7388226235565,1.75778553673249,12.));
#255427=CARTESIAN_POINT('Ctrl Pts',(22.7503059556455,1.75693513908911,0.));
#255428=CARTESIAN_POINT('Ctrl Pts',(22.7503059556455,1.75693513908911,12.));
#255429=CARTESIAN_POINT('Ctrl Pts',(22.7619782595013,1.75603146371641,0.));
#255430=CARTESIAN_POINT('Ctrl Pts',(22.7619782595013,1.75603146371641,12.));
#255431=CARTESIAN_POINT('Ctrl Pts',(22.7738367016115,1.75507365227127,0.));
#255432=CARTESIAN_POINT('Ctrl Pts',(22.7738367016115,1.75507365227127,12.));
#255433=CARTESIAN_POINT('Ctrl Pts',(22.7858785242358,1.7540608718293,0.));
#255434=CARTESIAN_POINT('Ctrl Pts',(22.7858785242358,1.7540608718293,12.));
#255435=CARTESIAN_POINT('Ctrl Pts',(22.7981010424312,1.75299231391461,0.));
#255436=CARTESIAN_POINT('Ctrl Pts',(22.7981010424312,1.75299231391461,12.));
#255437=CARTESIAN_POINT('Ctrl Pts',(22.8105016414712,1.7518671936559,0.));
#255438=CARTESIAN_POINT('Ctrl Pts',(22.8105016414712,1.7518671936559,12.));
#255439=CARTESIAN_POINT('Ctrl Pts',(22.8230777741285,1.75068474890884,0.));
#255440=CARTESIAN_POINT('Ctrl Pts',(22.8230777741285,1.75068474890884,12.));
#255441=CARTESIAN_POINT('Ctrl Pts',(22.8358269579854,1.74944423940117,0.));
#255442=CARTESIAN_POINT('Ctrl Pts',(22.8358269579854,1.74944423940117,12.));
#255443=CARTESIAN_POINT('Ctrl Pts',(22.8487467728075,1.74814494588492,0.));
#255444=CARTESIAN_POINT('Ctrl Pts',(22.8487467728075,1.74814494588492,12.));
#255445=CARTESIAN_POINT('Ctrl Pts',(22.8618348580234,1.74678616930663,0.));
#255446=CARTESIAN_POINT('Ctrl Pts',(22.8618348580234,1.74678616930663,12.));
#255447=CARTESIAN_POINT('Ctrl Pts',(22.8750889101696,1.745367229982,0.));
#255448=CARTESIAN_POINT('Ctrl Pts',(22.8750889101696,1.745367229982,12.));
#255449=CARTESIAN_POINT('Ctrl Pts',(22.8885066803351,1.74388746677702,0.));
#255450=CARTESIAN_POINT('Ctrl Pts',(22.8885066803351,1.74388746677702,12.));
#255451=CARTESIAN_POINT('Ctrl Pts',(22.9020859716144,1.74234623630079,0.));
#255452=CARTESIAN_POINT('Ctrl Pts',(22.9020859716144,1.74234623630079,12.));
#255453=CARTESIAN_POINT('Ctrl Pts',(22.9158246373365,1.74074291231057,0.));
#255454=CARTESIAN_POINT('Ctrl Pts',(22.9158246373365,1.74074291231057,12.));
#255455=CARTESIAN_POINT('Ctrl Pts',(22.9297205792587,1.73907688511665,0.));
#255456=CARTESIAN_POINT('Ctrl Pts',(22.9297205792587,1.73907688511665,12.));
#255457=CARTESIAN_POINT('Ctrl Pts',(22.9437717457825,1.73734756100038,0.));
#255458=CARTESIAN_POINT('Ctrl Pts',(22.9437717457825,1.73734756100038,12.));
#255459=CARTESIAN_POINT('Ctrl Pts',(22.9579761301062,1.73555436162771,0.));
#255460=CARTESIAN_POINT('Ctrl Pts',(22.9579761301062,1.73555436162771,12.));
#255461=CARTESIAN_POINT('Ctrl Pts',(22.9723317685688,1.73369672350818,0.));
#255462=CARTESIAN_POINT('Ctrl Pts',(22.9723317685688,1.73369672350818,12.));
#255463=CARTESIAN_POINT('Ctrl Pts',(22.9868367391978,1.73177409750194,0.));
#255464=CARTESIAN_POINT('Ctrl Pts',(22.9868367391978,1.73177409750194,12.));
#255465=CARTESIAN_POINT('Ctrl Pts',(23.0014891601891,1.72978594832137,0.));
#255466=CARTESIAN_POINT('Ctrl Pts',(23.0014891601891,1.72978594832137,12.));
#255467=CARTESIAN_POINT('Ctrl Pts',(23.0162871884167,1.72773175404703,0.));
#255468=CARTESIAN_POINT('Ctrl Pts',(23.0162871884167,1.72773175404703,12.));
#255469=CARTESIAN_POINT('Ctrl Pts',(23.031229017888,1.72561100564033,0.));
#255470=CARTESIAN_POINT('Ctrl Pts',(23.031229017888,1.72561100564033,12.));
#255471=CARTESIAN_POINT('Ctrl Pts',(23.0463128785528,1.72342320653731,0.));
#255472=CARTESIAN_POINT('Ctrl Pts',(23.0463128785528,1.72342320653731,12.));
#255473=CARTESIAN_POINT('Ctrl Pts',(23.0615370351559,1.72116787225981,0.));
#255474=CARTESIAN_POINT('Ctrl Pts',(23.0615370351559,1.72116787225981,12.));
#255475=CARTESIAN_POINT('Ctrl Pts',(23.0768997860709,1.71884453003027,0.));
#255476=CARTESIAN_POINT('Ctrl Pts',(23.0768997860709,1.71884453003027,12.));
#255477=CARTESIAN_POINT('Ctrl Pts',(23.0923994621216,1.71645271839311,0.));
#255478=CARTESIAN_POINT('Ctrl Pts',(23.0923994621216,1.71645271839311,12.));
#255479=CARTESIAN_POINT('Ctrl Pts',(23.1080344254291,1.71399198684725,0.));
#255480=CARTESIAN_POINT('Ctrl Pts',(23.1080344254291,1.71399198684725,12.));
#255481=CARTESIAN_POINT('Ctrl Pts',(23.1238030684929,1.71146189552192,0.));
#255482=CARTESIAN_POINT('Ctrl Pts',(23.1238030684929,1.71146189552192,12.));
#255483=CARTESIAN_POINT('Ctrl Pts',(23.1397038132358,1.7088620148546,0.));
#255484=CARTESIAN_POINT('Ctrl Pts',(23.1397038132358,1.7088620148546,12.));
#255485=CARTESIAN_POINT('Ctrl Pts',(23.1557351100613,1.70619192527847,0.));
#255486=CARTESIAN_POINT('Ctrl Pts',(23.1557351100613,1.70619192527847,12.));
#255487=CARTESIAN_POINT('Ctrl Pts',(23.1718954368749,1.70345121691259,0.));
#255488=CARTESIAN_POINT('Ctrl Pts',(23.1718954368749,1.70345121691259,12.));
#255489=CARTESIAN_POINT('Ctrl Pts',(23.1881832981848,1.70063948926988,0.));
#255490=CARTESIAN_POINT('Ctrl Pts',(23.1881832981848,1.70063948926988,12.));
#255491=CARTESIAN_POINT('Ctrl Pts',(23.2045972243765,1.69775635099425,0.));
#255492=CARTESIAN_POINT('Ctrl Pts',(23.2045972243765,1.69775635099425,12.));
#255493=CARTESIAN_POINT('Ctrl Pts',(23.2211357709374,1.69480141959946,0.));
#255494=CARTESIAN_POINT('Ctrl Pts',(23.2211357709374,1.69480141959946,12.));
#255495=CARTESIAN_POINT('Ctrl Pts',(23.2377975177014,1.69177432121716,0.));
#255496=CARTESIAN_POINT('Ctrl Pts',(23.2377975177014,1.69177432121716,12.));
#255497=CARTESIAN_POINT('Ctrl Pts',(23.2545810680536,1.6886746903491,0.));
#255498=CARTESIAN_POINT('Ctrl Pts',(23.2545810680536,1.6886746903491,12.));
#255499=CARTESIAN_POINT('Ctrl Pts',(23.2714850482245,1.68550216963275,0.));
#255500=CARTESIAN_POINT('Ctrl Pts',(23.2714850482245,1.68550216963275,12.));
#255501=CARTESIAN_POINT('Ctrl Pts',(23.2885081066949,1.68225640962181,0.));
#255502=CARTESIAN_POINT('Ctrl Pts',(23.2885081066949,1.68225640962181,12.));
#255503=CARTESIAN_POINT('Ctrl Pts',(23.3056489135611,1.67893706857123,0.));
#255504=CARTESIAN_POINT('Ctrl Pts',(23.3056489135611,1.67893706857123,12.));
#255505=CARTESIAN_POINT('Ctrl Pts',(23.3229061599145,1.67554381222988,0.));
#255506=CARTESIAN_POINT('Ctrl Pts',(23.3229061599145,1.67554381222988,12.));
#255507=CARTESIAN_POINT('Ctrl Pts',(23.3402785571866,1.67207631363905,0.));
#255508=CARTESIAN_POINT('Ctrl Pts',(23.3402785571866,1.67207631363905,12.));
#255509=CARTESIAN_POINT('Ctrl Pts',(23.3577648365747,1.66853425293978,0.));
#255510=CARTESIAN_POINT('Ctrl Pts',(23.3577648365747,1.66853425293978,12.));
#255511=CARTESIAN_POINT('Ctrl Pts',(23.375363748555,1.66491731718864,0.));
#255512=CARTESIAN_POINT('Ctrl Pts',(23.375363748555,1.66491731718864,12.));
#255513=CARTESIAN_POINT('Ctrl Pts',(23.3930740623622,1.66122520018008,0.));
#255514=CARTESIAN_POINT('Ctrl Pts',(23.3930740623622,1.66122520018008,12.));
#255515=CARTESIAN_POINT('Ctrl Pts',(23.4108945654803,1.65745760227507,0.));
#255516=CARTESIAN_POINT('Ctrl Pts',(23.4108945654803,1.65745760227507,12.));
#255517=CARTESIAN_POINT('Ctrl Pts',(23.4288240631034,1.6536142302373,0.));
#255518=CARTESIAN_POINT('Ctrl Pts',(23.4288240631034,1.6536142302373,12.));
#255519=CARTESIAN_POINT('Ctrl Pts',(23.446861377656,1.6496947970734,0.));
#255520=CARTESIAN_POINT('Ctrl Pts',(23.446861377656,1.6496947970734,12.));
#255521=CARTESIAN_POINT('Ctrl Pts',(23.4650053483919,1.64569902187608,0.));
#255522=CARTESIAN_POINT('Ctrl Pts',(23.4650053483919,1.64569902187608,12.));
#255523=CARTESIAN_POINT('Ctrl Pts',(23.4832548309638,1.64162662967525,0.));
#255524=CARTESIAN_POINT('Ctrl Pts',(23.4832548309638,1.64162662967525,12.));
#255525=CARTESIAN_POINT('Ctrl Pts',(23.5016086970006,1.63747735129474,0.));
#255526=CARTESIAN_POINT('Ctrl Pts',(23.5016086970006,1.63747735129474,12.));
#255527=CARTESIAN_POINT('Ctrl Pts',(23.5200658336624,1.63325092321731,0.));
#255528=CARTESIAN_POINT('Ctrl Pts',(23.5200658336624,1.63325092321731,12.));
#255529=CARTESIAN_POINT('Ctrl Pts',(23.5386251432278,1.62894708745231,0.));
#255530=CARTESIAN_POINT('Ctrl Pts',(23.5386251432278,1.62894708745231,12.));
#255531=CARTESIAN_POINT('Ctrl Pts',(23.5572855427617,1.62456559140072,0.));
#255532=CARTESIAN_POINT('Ctrl Pts',(23.5572855427617,1.62456559140072,12.));
#255533=CARTESIAN_POINT('Ctrl Pts',(23.5760459637608,1.62010618772869,0.));
#255534=CARTESIAN_POINT('Ctrl Pts',(23.5760459637608,1.62010618772869,12.));
#255535=CARTESIAN_POINT('Ctrl Pts',(23.5949053517996,1.61556863424697,0.));
#255536=CARTESIAN_POINT('Ctrl Pts',(23.5949053517996,1.61556863424697,12.));
#255537=CARTESIAN_POINT('Ctrl Pts',(23.6138626661644,1.61095269379773,0.));
#255538=CARTESIAN_POINT('Ctrl Pts',(23.6138626661644,1.61095269379773,12.));
#255539=CARTESIAN_POINT('Ctrl Pts',(23.6329168794916,1.60625813414666,0.));
#255540=CARTESIAN_POINT('Ctrl Pts',(23.6329168794916,1.60625813414666,12.));
#255541=CARTESIAN_POINT('Ctrl Pts',(23.6520669774863,1.60148472786588,0.));
#255542=CARTESIAN_POINT('Ctrl Pts',(23.6520669774863,1.60148472786588,12.));
#255543=CARTESIAN_POINT('Ctrl Pts',(23.6713119586302,1.59663225222459,0.));
#255544=CARTESIAN_POINT('Ctrl Pts',(23.6713119586302,1.59663225222459,12.));
#255545=CARTESIAN_POINT('Ctrl Pts',(23.6906508338832,1.59170048908631,0.));
#255546=CARTESIAN_POINT('Ctrl Pts',(23.6906508338832,1.59170048908631,12.));
#255547=CARTESIAN_POINT('Ctrl Pts',(23.7100826263835,1.58668922481222,0.));
#255548=CARTESIAN_POINT('Ctrl Pts',(23.7100826263835,1.58668922481222,12.));
#255549=CARTESIAN_POINT('Ctrl Pts',(23.7296063711308,1.58159825017362,0.));
#255550=CARTESIAN_POINT('Ctrl Pts',(23.7296063711308,1.58159825017362,12.));
#255551=CARTESIAN_POINT('Ctrl Pts',(23.7492211147369,1.57642736025251,0.));
#255552=CARTESIAN_POINT('Ctrl Pts',(23.7492211147369,1.57642736025251,12.));
#255553=CARTESIAN_POINT('Ctrl Pts',(23.7689259151869,1.57117635434412,0.));
#255554=CARTESIAN_POINT('Ctrl Pts',(23.7689259151869,1.57117635434412,12.));
#255555=CARTESIAN_POINT('Ctrl Pts',(23.788719841588,1.56584503586844,0.));
#255556=CARTESIAN_POINT('Ctrl Pts',(23.788719841588,1.56584503586844,12.));
#255557=CARTESIAN_POINT('Ctrl Pts',(23.8086019739192,1.56043321228631,0.));
#255558=CARTESIAN_POINT('Ctrl Pts',(23.8086019739192,1.56043321228631,12.));
#255559=CARTESIAN_POINT('Ctrl Pts',(23.8285714027631,1.55494069502628,0.));
#255560=CARTESIAN_POINT('Ctrl Pts',(23.8285714027631,1.55494069502628,12.));
#255561=CARTESIAN_POINT('Ctrl Pts',(23.8486272290698,1.5493672994053,0.));
#255562=CARTESIAN_POINT('Ctrl Pts',(23.8486272290698,1.5493672994053,12.));
#255563=CARTESIAN_POINT('Ctrl Pts',(23.8687685639635,1.54371284453978,0.));
#255564=CARTESIAN_POINT('Ctrl Pts',(23.8687685639635,1.54371284453978,12.));
#255565=CARTESIAN_POINT('Ctrl Pts',(23.8889945285313,1.53797715326748,0.));
#255566=CARTESIAN_POINT('Ctrl Pts',(23.8889945285313,1.53797715326748,12.));
#255567=CARTESIAN_POINT('Ctrl Pts',(23.9093042536119,1.53216005207462,0.));
#255568=CARTESIAN_POINT('Ctrl Pts',(23.9093042536119,1.53216005207462,12.));
#255569=CARTESIAN_POINT('Ctrl Pts',(23.9296968795761,1.5262613710304,0.));
#255570=CARTESIAN_POINT('Ctrl Pts',(23.9296968795761,1.5262613710304,12.));
#255571=CARTESIAN_POINT('Ctrl Pts',(23.9501715561038,1.52028094372806,0.));
#255572=CARTESIAN_POINT('Ctrl Pts',(23.9501715561038,1.52028094372806,12.));
#255573=CARTESIAN_POINT('Ctrl Pts',(23.9707274420145,1.51421860720628,0.));
#255574=CARTESIAN_POINT('Ctrl Pts',(23.9707274420145,1.51421860720628,12.));
#255575=CARTESIAN_POINT('Ctrl Pts',(23.991363705093,1.50807420187703,0.));
#255576=CARTESIAN_POINT('Ctrl Pts',(23.991363705093,1.50807420187703,12.));
#255577=CARTESIAN_POINT('Ctrl Pts',(24.0120795219086,1.50184757146099,0.));
#255578=CARTESIAN_POINT('Ctrl Pts',(24.0120795219086,1.50184757146099,12.));
#255579=CARTESIAN_POINT('Ctrl Pts',(24.0328740776331,1.49553856292798,0.));
#255580=CARTESIAN_POINT('Ctrl Pts',(24.0328740776331,1.49553856292798,12.));
#255581=CARTESIAN_POINT('Ctrl Pts',(24.053746565843,1.48914702644883,0.));
#255582=CARTESIAN_POINT('Ctrl Pts',(24.053746565843,1.48914702644883,12.));
#255583=CARTESIAN_POINT('Ctrl Pts',(24.074696188353,1.4826728153368,0.));
#255584=CARTESIAN_POINT('Ctrl Pts',(24.074696188353,1.4826728153368,12.));
#255585=CARTESIAN_POINT('Ctrl Pts',(24.0957221550782,1.47611578597742,0.));
#255586=CARTESIAN_POINT('Ctrl Pts',(24.0957221550782,1.47611578597742,12.));
#255587=CARTESIAN_POINT('Ctrl Pts',(24.1168236838827,1.46947579776992,0.));
#255588=CARTESIAN_POINT('Ctrl Pts',(24.1168236838827,1.46947579776992,12.));
#255589=CARTESIAN_POINT('Ctrl Pts',(24.1380000004272,1.46275271307398,0.));
#255590=CARTESIAN_POINT('Ctrl Pts',(24.1380000004272,1.46275271307398,12.));
#255591=CARTESIAN_POINT('Ctrl Pts',(24.1592503380105,1.45594639716314,0.));
#255592=CARTESIAN_POINT('Ctrl Pts',(24.1592503380105,1.45594639716314,12.));
#255593=CARTESIAN_POINT('Ctrl Pts',(24.1805739374033,1.44905671818721,0.));
#255594=CARTESIAN_POINT('Ctrl Pts',(24.1805739374033,1.44905671818721,12.));
#255595=CARTESIAN_POINT('Ctrl Pts',(24.2019700467214,1.44208354711074,0.));
#255596=CARTESIAN_POINT('Ctrl Pts',(24.2019700467214,1.44208354711074,12.));
#255597=CARTESIAN_POINT('Ctrl Pts',(24.2234379212978,1.43502675765502,0.));
#255598=CARTESIAN_POINT('Ctrl Pts',(24.2234379212978,1.43502675765502,12.));
#255599=CARTESIAN_POINT('Ctrl Pts',(24.2449768235485,1.42788622624851,0.));
#255600=CARTESIAN_POINT('Ctrl Pts',(24.2449768235485,1.42788622624851,12.));
#255601=CARTESIAN_POINT('Ctrl Pts',(24.2665860228357,1.42066183198252,0.));
#255602=CARTESIAN_POINT('Ctrl Pts',(24.2665860228357,1.42066183198252,12.));
#255603=CARTESIAN_POINT('Ctrl Pts',(24.2882647953214,1.41335345657685,0.));
#255604=CARTESIAN_POINT('Ctrl Pts',(24.2882647953214,1.41335345657685,12.));
#255605=CARTESIAN_POINT('Ctrl Pts',(24.3100124238316,1.40596098434341,0.));
#255606=CARTESIAN_POINT('Ctrl Pts',(24.3100124238316,1.40596098434341,12.));
#255607=CARTESIAN_POINT('Ctrl Pts',(24.3318281977647,1.3984843021281,0.));
#255608=CARTESIAN_POINT('Ctrl Pts',(24.3318281977647,1.3984843021281,12.));
#255609=CARTESIAN_POINT('Ctrl Pts',(24.3537114129877,1.3909232992639,0.));
#255610=CARTESIAN_POINT('Ctrl Pts',(24.3537114129877,1.3909232992639,12.));
#255611=CARTESIAN_POINT('Ctrl Pts',(24.37566137173,1.38327786752998,0.));
#255612=CARTESIAN_POINT('Ctrl Pts',(24.37566137173,1.38327786752998,12.));
#255613=CARTESIAN_POINT('Ctrl Pts',(24.3976773824731,1.37554790111608,0.));
#255614=CARTESIAN_POINT('Ctrl Pts',(24.3976773824731,1.37554790111608,12.));
#255615=CARTESIAN_POINT('Ctrl Pts',(24.4197587598337,1.36773329659954,0.));
#255616=CARTESIAN_POINT('Ctrl Pts',(24.4197587598337,1.36773329659954,12.));
#255617=CARTESIAN_POINT('Ctrl Pts',(24.4419048244524,1.35983395290624,0.));
#255618=CARTESIAN_POINT('Ctrl Pts',(24.4419048244524,1.35983395290624,12.));
#255619=CARTESIAN_POINT('Ctrl Pts',(24.4641149028894,1.35184977125645,0.));
#255620=CARTESIAN_POINT('Ctrl Pts',(24.4641149028894,1.35184977125645,12.));
#255621=CARTESIAN_POINT('Ctrl Pts',(24.4863883275135,1.34378065512335,0.));
#255622=CARTESIAN_POINT('Ctrl Pts',(24.4863883275135,1.34378065512335,12.));
#255623=CARTESIAN_POINT('Ctrl Pts',(24.5087244363856,1.33562651019684,0.));
#255624=CARTESIAN_POINT('Ctrl Pts',(24.5087244363856,1.33562651019684,12.));
#255625=CARTESIAN_POINT('Ctrl Pts',(24.5311225731434,1.32738724435326,0.));
#255626=CARTESIAN_POINT('Ctrl Pts',(24.5311225731434,1.32738724435326,12.));
#255627=CARTESIAN_POINT('Ctrl Pts',(24.5535820868671,1.31906276763669,0.));
#255628=CARTESIAN_POINT('Ctrl Pts',(24.5535820868671,1.31906276763669,12.));
#255629=CARTESIAN_POINT('Ctrl Pts',(24.576102332018,1.31065299222023,0.));
#255630=CARTESIAN_POINT('Ctrl Pts',(24.576102332018,1.31065299222023,12.));
#255631=CARTESIAN_POINT('Ctrl Pts',(24.5986826684025,1.30215783236364,0.));
#255632=CARTESIAN_POINT('Ctrl Pts',(24.5986826684025,1.30215783236364,12.));
#255633=CARTESIAN_POINT('Ctrl Pts',(24.6213224611228,1.29357720438108,0.));
#255634=CARTESIAN_POINT('Ctrl Pts',(24.6213224611228,1.29357720438108,12.));
#255635=CARTESIAN_POINT('Ctrl Pts',(24.6440210805278,1.28491102661514,0.));
#255636=CARTESIAN_POINT('Ctrl Pts',(24.6440210805278,1.28491102661514,12.));
#255637=CARTESIAN_POINT('Ctrl Pts',(24.666777902156,1.2761592194164,0.));
#255638=CARTESIAN_POINT('Ctrl Pts',(24.666777902156,1.2761592194164,12.));
#255639=CARTESIAN_POINT('Ctrl Pts',(24.6895923066837,1.26732170513497,0.));
#255640=CARTESIAN_POINT('Ctrl Pts',(24.6895923066837,1.26732170513497,12.));
#255641=CARTESIAN_POINT('Ctrl Pts',(24.7124636797895,1.25839840807415,0.));
#255642=CARTESIAN_POINT('Ctrl Pts',(24.7124636797895,1.25839840807415,12.));
#255643=CARTESIAN_POINT('Ctrl Pts',(24.7353914120012,1.24938925444324,0.));
#255644=CARTESIAN_POINT('Ctrl Pts',(24.7353914120012,1.24938925444324,12.));
#255645=CARTESIAN_POINT('Ctrl Pts',(24.7583748985439,1.24029417231988,0.));
#255646=CARTESIAN_POINT('Ctrl Pts',(24.7583748985439,1.24029417231988,12.));
#255647=CARTESIAN_POINT('Ctrl Pts',(24.78141353918,1.23111309161843,0.));
#255648=CARTESIAN_POINT('Ctrl Pts',(24.78141353918,1.23111309161843,12.));
#255649=CARTESIAN_POINT('Ctrl Pts',(24.8045067380536,1.22184594406527,0.));
#255650=CARTESIAN_POINT('Ctrl Pts',(24.8045067380536,1.22184594406527,12.));
#255651=CARTESIAN_POINT('Ctrl Pts',(24.8276539035092,1.21249266318205,0.));
#255652=CARTESIAN_POINT('Ctrl Pts',(24.8276539035092,1.21249266318205,12.));
#255653=CARTESIAN_POINT('Ctrl Pts',(24.8508544481973,1.20305318426016,0.));
#255654=CARTESIAN_POINT('Ctrl Pts',(24.8508544481973,1.20305318426016,12.));
#255655=CARTESIAN_POINT('Ctrl Pts',(24.8741077892074,1.19352744434059,0.));
#255656=CARTESIAN_POINT('Ctrl Pts',(24.8741077892074,1.19352744434059,12.));
#255657=CARTESIAN_POINT('Ctrl Pts',(24.8974133481829,1.18391538220098,0.));
#255658=CARTESIAN_POINT('Ctrl Pts',(24.8974133481829,1.18391538220098,12.));
#255659=CARTESIAN_POINT('Ctrl Pts',(24.9207705514449,1.1742169383504,0.));
#255660=CARTESIAN_POINT('Ctrl Pts',(24.9207705514449,1.1742169383504,12.));
#255661=CARTESIAN_POINT('Ctrl Pts',(24.9441788300932,1.16443205502852,0.));
#255662=CARTESIAN_POINT('Ctrl Pts',(24.9441788300932,1.16443205502852,12.));
#255663=CARTESIAN_POINT('Ctrl Pts',(24.9676376201501,1.15456067621894,0.));
#255664=CARTESIAN_POINT('Ctrl Pts',(24.9676376201501,1.15456067621894,12.));
#255665=CARTESIAN_POINT('Ctrl Pts',(24.9911463621431,1.14460274758206,0.));
#255666=CARTESIAN_POINT('Ctrl Pts',(24.9911463621431,1.14460274758206,12.));
#255667=CARTESIAN_POINT('Ctrl Pts',(25.0147045006193,1.13455821638536,0.));
#255668=CARTESIAN_POINT('Ctrl Pts',(25.0147045006193,1.13455821638536,12.));
#255669=CARTESIAN_POINT('Ctrl Pts',(25.0383114836898,1.12442703144455,0.));
#255670=CARTESIAN_POINT('Ctrl Pts',(25.0383114836898,1.12442703144455,12.));
#255671=CARTESIAN_POINT('Ctrl Pts',(25.0619667625336,1.1142091430689,0.));
#255672=CARTESIAN_POINT('Ctrl Pts',(25.0619667625336,1.1142091430689,12.));
#255673=CARTESIAN_POINT('Ctrl Pts',(25.085669790968,1.10390450301741,0.));
#255674=CARTESIAN_POINT('Ctrl Pts',(25.085669790968,1.10390450301741,12.));
#255675=CARTESIAN_POINT('Ctrl Pts',(25.1094200248448,1.09351306445299,0.));
#255676=CARTESIAN_POINT('Ctrl Pts',(25.1094200248448,1.09351306445299,12.));
#255677=CARTESIAN_POINT('Ctrl Pts',(25.1332169227415,1.08303478197174,0.));
#255678=CARTESIAN_POINT('Ctrl Pts',(25.1332169227415,1.08303478197174,12.));
#255679=CARTESIAN_POINT('Ctrl Pts',(25.1570599469311,1.0724696116546,0.));
#255680=CARTESIAN_POINT('Ctrl Pts',(25.1570599469311,1.0724696116546,12.));
#255681=CARTESIAN_POINT('Ctrl Pts',(25.1809485642191,1.06181751111754,0.));
#255682=CARTESIAN_POINT('Ctrl Pts',(25.1809485642191,1.06181751111754,12.));
#255683=CARTESIAN_POINT('Ctrl Pts',(25.2048822469027,1.05107843957926,0.));
#255684=CARTESIAN_POINT('Ctrl Pts',(25.2048822469027,1.05107843957926,12.));
#255685=CARTESIAN_POINT('Ctrl Pts',(25.2288604735087,1.04025235791515,0.));
#255686=CARTESIAN_POINT('Ctrl Pts',(25.2288604735087,1.04025235791515,12.));
#255687=CARTESIAN_POINT('Ctrl Pts',(25.2528827300427,1.0293392287683,0.));
#255688=CARTESIAN_POINT('Ctrl Pts',(25.2528827300427,1.0293392287683,12.));
#255689=CARTESIAN_POINT('Ctrl Pts',(25.2769485087268,1.01833901642273,0.));
#255690=CARTESIAN_POINT('Ctrl Pts',(25.2769485087268,1.01833901642273,12.));
#255691=CARTESIAN_POINT('Ctrl Pts',(25.3010573055557,1.00725168656934,0.));
#255692=CARTESIAN_POINT('Ctrl Pts',(25.3010573055557,1.00725168656934,12.));
#255693=CARTESIAN_POINT('Ctrl Pts',(25.3252086182976,0.996077206120921,
0.));
#255694=CARTESIAN_POINT('Ctrl Pts',(25.3252086182976,0.996077206120921,
12.));
#255695=CARTESIAN_POINT('Ctrl Pts',(25.3494019441444,0.984815543004091,
0.));
#255696=CARTESIAN_POINT('Ctrl Pts',(25.3494019441444,0.984815543004091,
12.));
#255697=CARTESIAN_POINT('Ctrl Pts',(25.3736367778842,0.97346666600005,0.));
#255698=CARTESIAN_POINT('Ctrl Pts',(25.3736367778842,0.97346666600005,12.));
#255699=CARTESIAN_POINT('Ctrl Pts',(25.3979126089155,0.962030544502806,
0.));
#255700=CARTESIAN_POINT('Ctrl Pts',(25.3979126089155,0.962030544502806,
12.));
#255701=CARTESIAN_POINT('Ctrl Pts',(25.4222289223155,0.950507148596971,
0.));
#255702=CARTESIAN_POINT('Ctrl Pts',(25.4222289223155,0.950507148596971,
12.));
#255703=CARTESIAN_POINT('Ctrl Pts',(25.4465852044835,0.938896449495636,
0.));
#255704=CARTESIAN_POINT('Ctrl Pts',(25.4465852044835,0.938896449495636,
12.));
#255705=CARTESIAN_POINT('Ctrl Pts',(25.4709809474996,0.927198419885607,
0.));
#255706=CARTESIAN_POINT('Ctrl Pts',(25.4709809474996,0.927198419885607,
12.));
#255707=CARTESIAN_POINT('Ctrl Pts',(25.4954156541787,0.915413034335334,
0.));
#255708=CARTESIAN_POINT('Ctrl Pts',(25.4954156541787,0.915413034335334,
12.));
#255709=CARTESIAN_POINT('Ctrl Pts',(25.5198888424195,0.903540269651155,
0.));
#255710=CARTESIAN_POINT('Ctrl Pts',(25.5198888424195,0.903540269651155,
12.));
#255711=CARTESIAN_POINT('Ctrl Pts',(25.5444000508223,0.891580105349469,
0.));
#255712=CARTESIAN_POINT('Ctrl Pts',(25.5444000508223,0.891580105349469,
12.));
#255713=CARTESIAN_POINT('Ctrl Pts',(25.568948840818,0.879532523835094,0.));
#255714=CARTESIAN_POINT('Ctrl Pts',(25.568948840818,0.879532523835094,12.));
#255715=CARTESIAN_POINT('Ctrl Pts',(25.5935347843616,0.867397509339473,
0.));
#255716=CARTESIAN_POINT('Ctrl Pts',(25.5935347843616,0.867397509339473,
12.));
#255717=CARTESIAN_POINT('Ctrl Pts',(25.618157453608,0.855175047037618,0.));
#255718=CARTESIAN_POINT('Ctrl Pts',(25.618157453608,0.855175047037618,12.));
#255719=CARTESIAN_POINT('Ctrl Pts',(25.6428164100078,0.842865122121547,
0.));
#255720=CARTESIAN_POINT('Ctrl Pts',(25.6428164100078,0.842865122121547,
12.));
#255721=CARTESIAN_POINT('Ctrl Pts',(25.6675111931957,0.83046771886437,0.));
#255722=CARTESIAN_POINT('Ctrl Pts',(25.6675111931957,0.83046771886437,12.));
#255723=CARTESIAN_POINT('Ctrl Pts',(25.6922413110172,0.817982819786722,
0.));
#255724=CARTESIAN_POINT('Ctrl Pts',(25.6922413110172,0.817982819786722,
12.));
#255725=CARTESIAN_POINT('Ctrl Pts',(25.7170062262474,0.805410404552597,
0.));
#255726=CARTESIAN_POINT('Ctrl Pts',(25.7170062262474,0.805410404552597,
12.));
#255727=CARTESIAN_POINT('Ctrl Pts',(25.7418053757671,0.792750451613538,
0.));
#255728=CARTESIAN_POINT('Ctrl Pts',(25.7418053757671,0.792750451613538,
12.));
#255729=CARTESIAN_POINT('Ctrl Pts',(25.7666381946871,0.780002940289028,
0.));
#255730=CARTESIAN_POINT('Ctrl Pts',(25.7666381946871,0.780002940289028,
12.));
#255731=CARTESIAN_POINT('Ctrl Pts',(25.7915041383304,0.767167852648643,
0.));
#255732=CARTESIAN_POINT('Ctrl Pts',(25.7915041383304,0.767167852648643,
12.));
#255733=CARTESIAN_POINT('Ctrl Pts',(25.816402705995,0.754245175608291,0.));
#255734=CARTESIAN_POINT('Ctrl Pts',(25.816402705995,0.754245175608291,12.));
#255735=CARTESIAN_POINT('Ctrl Pts',(25.841333461908,0.741234902664698,0.));
#255736=CARTESIAN_POINT('Ctrl Pts',(25.841333461908,0.741234902664698,12.));
#255737=CARTESIAN_POINT('Ctrl Pts',(25.8662960624285,0.728137036485881,
0.));
#255738=CARTESIAN_POINT('Ctrl Pts',(25.8662960624285,0.728137036485881,
12.));
#255739=CARTESIAN_POINT('Ctrl Pts',(25.8912902615141,0.714951588533756,
0.));
#255740=CARTESIAN_POINT('Ctrl Pts',(25.8912902615141,0.714951588533756,
12.));
#255741=CARTESIAN_POINT('Ctrl Pts',(25.9163158909645,0.701678575236605,
0.));
#255742=CARTESIAN_POINT('Ctrl Pts',(25.9163158909645,0.701678575236605,
12.));
#255743=CARTESIAN_POINT('Ctrl Pts',(25.941372847213,0.68831801506568,0.));
#255744=CARTESIAN_POINT('Ctrl Pts',(25.941372847213,0.68831801506568,12.));
#255745=CARTESIAN_POINT('Ctrl Pts',(25.9614434298092,0.677559543215907,
0.));
#255746=CARTESIAN_POINT('Ctrl Pts',(25.9614434298092,0.677559543215907,
12.));
#255747=CARTESIAN_POINT('Ctrl Pts',(25.9765104298171,0.669451306784419,
0.));
#255748=CARTESIAN_POINT('Ctrl Pts',(25.9765104298171,0.669451306784419,
12.));
#255749=CARTESIAN_POINT('Ctrl Pts',(25.9865613464809,0.664028313188916,
0.));
#255750=CARTESIAN_POINT('Ctrl Pts',(25.9865613464809,0.664028313188916,
12.));
#255751=CARTESIAN_POINT('Ctrl Pts',(25.991588367311,0.661312440730894,0.));
#255752=CARTESIAN_POINT('Ctrl Pts',(25.991588367311,0.661312440730894,12.));
#255753=CARTESIAN_POINT('',(25.991588367311,0.661312440730894,0.));
#255754=CARTESIAN_POINT('Origin',(0.,0.,0.));
#255755=CARTESIAN_POINT('',(-7.,-8.57252759403147E-16,0.));
#255756=CARTESIAN_POINT('Origin',(0.,0.,0.));
#255757=CARTESIAN_POINT('',(0.,0.,0.));
#255758=CARTESIAN_POINT('Origin',(0.,0.,0.));
#255759=CARTESIAN_POINT('',(-16.,-1.95943487863577E-15,8.));
#255760=CARTESIAN_POINT('Origin',(0.,0.,8.));
#255761=CARTESIAN_POINT('',(-16.,-1.95943487863577E-15,0.));
#255762=CARTESIAN_POINT('',(-16.,-1.95943487863577E-15,0.));
#255763=CARTESIAN_POINT('Origin',(0.,0.,0.));
#255764=CARTESIAN_POINT('Origin',(0.,0.,0.));
#255765=CARTESIAN_POINT('',(-18.,-2.20436423846524E-15,8.));
#255766=CARTESIAN_POINT('Origin',(0.,0.,8.));
#255767=CARTESIAN_POINT('',(-18.,-2.20436423846524E-15,0.));
#255768=CARTESIAN_POINT('',(-18.,-2.20436423846524E-15,0.));
#255769=CARTESIAN_POINT('Origin',(0.,0.,0.));
#255770=CARTESIAN_POINT('Origin',(0.,0.,8.));
#255771=CARTESIAN_POINT('Origin',(0.,0.,0.));
#255772=CARTESIAN_POINT('',(0.,0.,0.));
#255773=CARTESIAN_POINT('Origin',(11.,-3.,98.));
#255774=CARTESIAN_POINT('',(7.41619848709566,-3.,86.));
#255775=CARTESIAN_POINT('',(7.41619848709566,-3.,98.));
#255776=CARTESIAN_POINT('',(7.41619848709566,-3.,78.));
#255777=CARTESIAN_POINT('',(5.,-3.,86.));
#255778=CARTESIAN_POINT('',(5.,-3.,86.));
#255779=CARTESIAN_POINT('',(5.,-3.,98.));
#255780=CARTESIAN_POINT('',(5.,-3.,98.));
#255781=CARTESIAN_POINT('',(5.,-3.,98.));
#255782=CARTESIAN_POINT('Origin',(8.,0.,98.));
#255783=CARTESIAN_POINT('',(7.41619848709566,3.,98.));
#255784=CARTESIAN_POINT('Origin',(0.,0.,98.));
#255785=CARTESIAN_POINT('',(5.,3.,98.));
#255786=CARTESIAN_POINT('',(5.,3.,98.));
#255787=CARTESIAN_POINT('',(11.,3.,98.));
#255788=CARTESIAN_POINT('Origin',(5.,3.,98.));
#255789=CARTESIAN_POINT('',(7.41619848709566,3.,86.));
#255790=CARTESIAN_POINT('',(7.41619848709566,3.,78.));
#255791=CARTESIAN_POINT('',(5.,3.,86.));
#255792=CARTESIAN_POINT('',(5.,3.,98.));
#255793=CARTESIAN_POINT('',(11.,3.,86.));
#255794=CARTESIAN_POINT('Origin',(5.,-3.,98.));
#255795=CARTESIAN_POINT('',(5.,3.,86.));
#255796=CARTESIAN_POINT('Origin',(8.,0.,86.));
#255797=CARTESIAN_POINT('Origin',(0.,0.,86.));
#255798=CARTESIAN_POINT('Origin',(0.,0.,100.5));
#255799=CARTESIAN_POINT('',(-7.,-8.57252759403147E-16,100.));
#255800=CARTESIAN_POINT('Origin',(0.,0.,100.));
#255801=CARTESIAN_POINT('',(-7.,-8.57252759403147E-16,101.));
#255802=CARTESIAN_POINT('',(-7.,-8.57252759403147E-16,100.5));
#255803=CARTESIAN_POINT('Origin',(0.,0.,101.));
#255804=CARTESIAN_POINT('Origin',(11.,0.,100.));
#255805=CARTESIAN_POINT('',(-8.,9.79717439317883E-16,100.));
#255806=CARTESIAN_POINT('Origin',(0.,0.,100.));
#255807=CARTESIAN_POINT('Origin',(7.,0.,101.));
#255808=CARTESIAN_POINT('',(-8.,-9.79717439317883E-16,101.));
#255809=CARTESIAN_POINT('Origin',(0.,0.,101.));
#255810=CARTESIAN_POINT('Origin',(0.,0.,78.));
#255811=CARTESIAN_POINT('',(-8.,-9.79717439317883E-16,113.));
#255812=CARTESIAN_POINT('Origin',(0.,0.,113.));
#255813=CARTESIAN_POINT('',(-8.,-9.79717439317883E-16,78.));
#255814=CARTESIAN_POINT('Origin',(0.,0.,76.5));
#255815=CARTESIAN_POINT('',(-15.,-1.83697019872103E-15,76.));
#255816=CARTESIAN_POINT('Origin',(0.,0.,76.));
#255817=CARTESIAN_POINT('',(-15.,-1.83697019872103E-15,77.));
#255818=CARTESIAN_POINT('',(-15.,-1.83697019872103E-15,76.5));
#255819=CARTESIAN_POINT('Origin',(0.,0.,77.));
#255820=CARTESIAN_POINT('Origin',(19.,0.,76.));
#255821=CARTESIAN_POINT('',(-16.,1.95943487863577E-15,76.));
#255822=CARTESIAN_POINT('Origin',(0.,0.,76.));
#255823=CARTESIAN_POINT('Origin',(15.,0.,77.));
#255824=CARTESIAN_POINT('',(-16.,-1.95943487863577E-15,77.));
#255825=CARTESIAN_POINT('Origin',(0.,0.,77.));
#255826=CARTESIAN_POINT('Origin',(0.,0.,54.));
#255827=CARTESIAN_POINT('',(-16.,-1.95943487863577E-15,78.));
#255828=CARTESIAN_POINT('Origin',(0.,0.,78.));
#255829=CARTESIAN_POINT('',(-16.,-1.95943487863577E-15,54.));
#255830=CARTESIAN_POINT('Origin',(-24.,41.5692193816531,50.));
#255831=CARTESIAN_POINT('',(-29.,41.5692193816531,54.));
#255832=CARTESIAN_POINT('Origin',(-24.,41.5692193816531,54.));
#255833=CARTESIAN_POINT('',(-29.,41.5692193816531,46.));
#255834=CARTESIAN_POINT('',(-29.,41.5692193816531,50.));
#255835=CARTESIAN_POINT('Origin',(-24.,41.5692193816531,46.));
#255836=CARTESIAN_POINT('Origin',(48.,0.,50.));
#255837=CARTESIAN_POINT('',(43.,6.12323399573677E-16,54.));
#255838=CARTESIAN_POINT('Origin',(48.,0.,54.));
#255839=CARTESIAN_POINT('',(43.,6.12323399573677E-16,46.));
#255840=CARTESIAN_POINT('',(43.,6.12323399573677E-16,50.));
#255841=CARTESIAN_POINT('Origin',(48.,0.,46.));
#255842=CARTESIAN_POINT('Origin',(-24.,-41.569219381653,50.));
#255843=CARTESIAN_POINT('',(-29.,-41.569219381653,54.));
#255844=CARTESIAN_POINT('Origin',(-24.,-41.569219381653,54.));
#255845=CARTESIAN_POINT('',(-29.,-41.569219381653,46.));
#255846=CARTESIAN_POINT('',(-29.,-41.569219381653,50.));
#255847=CARTESIAN_POINT('Origin',(-24.,-41.569219381653,46.));
#255848=CARTESIAN_POINT('Origin',(0.,0.,84.));
#255849=CARTESIAN_POINT('',(-11.,-1.34711147906209E-15,84.));
#255850=CARTESIAN_POINT('Origin',(0.,0.,84.));
#255851=CARTESIAN_POINT('',(-8.,-9.79717439317883E-16,84.));
#255852=CARTESIAN_POINT('Origin',(0.,0.,84.));
#255853=CARTESIAN_POINT('Origin',(0.,0.,82.));
#255854=CARTESIAN_POINT('',(-11.,-1.34711147906209E-15,82.));
#255855=CARTESIAN_POINT('Origin',(0.,0.,82.));
#255856=CARTESIAN_POINT('',(-8.,9.79717439317883E-16,82.));
#255857=CARTESIAN_POINT('Origin',(0.,0.,82.));
#255858=CARTESIAN_POINT('Origin',(0.,0.,82.));
#255859=CARTESIAN_POINT('',(-11.,-1.34711147906209E-15,82.));
#255860=CARTESIAN_POINT('Origin',(0.,0.,78.));
#255861=CARTESIAN_POINT('',(-8.,-9.79717439317883E-16,78.));
#255862=CARTESIAN_POINT('',(-8.,-9.79717439317883E-16,78.));
#255863=CARTESIAN_POINT('Origin',(0.,0.,78.));
#255864=CARTESIAN_POINT('Origin',(0.,0.,78.));
#255865=CARTESIAN_POINT('',(-8.,-9.79717439317883E-16,78.));
#255866=CARTESIAN_POINT('Origin',(0.,0.,113.));
#255867=CARTESIAN_POINT('Origin',(0.,0.,64.));
#255868=CARTESIAN_POINT('',(-20.,-2.44929359829471E-15,64.));
#255869=CARTESIAN_POINT('Origin',(0.,0.,64.));
#255870=CARTESIAN_POINT('',(-16.,-1.95943487863577E-15,64.));
#255871=CARTESIAN_POINT('Origin',(0.,0.,64.));
#255872=CARTESIAN_POINT('Origin',(0.,0.,62.));
#255873=CARTESIAN_POINT('',(-20.,-2.44929359829471E-15,62.));
#255874=CARTESIAN_POINT('Origin',(0.,0.,62.));
#255875=CARTESIAN_POINT('',(-16.,1.95943487863577E-15,62.));
#255876=CARTESIAN_POINT('Origin',(0.,0.,62.));
#255877=CARTESIAN_POINT('Origin',(0.,0.,62.));
#255878=CARTESIAN_POINT('',(-20.,-2.44929359829471E-15,62.));
#255879=CARTESIAN_POINT('Origin',(0.,0.,54.));
#255880=CARTESIAN_POINT('',(-16.,-1.95943487863577E-15,54.));
#255881=CARTESIAN_POINT('',(-16.,-1.95943487863577E-15,54.));
#255882=CARTESIAN_POINT('Origin',(0.,0.,54.));
#255883=CARTESIAN_POINT('Origin',(0.,0.,54.));
#255884=CARTESIAN_POINT('',(-12.,-1.46957615897682E-15,54.));
#255885=CARTESIAN_POINT('Origin',(0.,0.,54.));
#255886=CARTESIAN_POINT('Origin',(0.,0.,54.));
#255887=CARTESIAN_POINT('',(-16.,-1.95943487863577E-15,54.));
#255888=CARTESIAN_POINT('Origin',(0.,0.,78.));
#255889=CARTESIAN_POINT('Origin',(0.,0.,46.));
#255890=CARTESIAN_POINT('',(-12.,-1.46957615897682E-15,46.));
#255891=CARTESIAN_POINT('',(-12.,-1.46957615897682E-15,46.));
#255892=CARTESIAN_POINT('Origin',(0.,0.,46.));
#255893=CARTESIAN_POINT('Origin',(0.,0.,46.));
#255894=CARTESIAN_POINT('',(-70.,-8.57252759403147E-15,54.));
#255895=CARTESIAN_POINT('Origin',(0.,0.,54.));
#255896=CARTESIAN_POINT('',(-70.,-8.57252759403147E-15,46.));
#255897=CARTESIAN_POINT('',(-70.,-8.57252759403147E-15,46.));
#255898=CARTESIAN_POINT('Origin',(0.,0.,46.));
#255899=CARTESIAN_POINT('Origin',(0.,0.,54.));
#255900=CARTESIAN_POINT('Origin',(0.,0.,46.));
#255901=CARTESIAN_POINT('',(0.,0.,0.));
#255902=CARTESIAN_POINT('Origin',(11.,3.,0.));
#255903=CARTESIAN_POINT('',(11.,3.,0.));
#255904=CARTESIAN_POINT('',(5.,3.,0.));
#255905=CARTESIAN_POINT('',(11.,3.,0.));
#255906=CARTESIAN_POINT('',(5.,3.,12.));
#255907=CARTESIAN_POINT('',(5.,3.,0.));
#255908=CARTESIAN_POINT('',(11.,3.,12.));
#255909=CARTESIAN_POINT('',(11.,3.,12.));
#255910=CARTESIAN_POINT('',(11.,3.,0.));
#255911=CARTESIAN_POINT('Origin',(11.,-3.,0.));
#255912=CARTESIAN_POINT('',(11.,-3.,0.));
#255913=CARTESIAN_POINT('',(11.,-3.,0.));
#255914=CARTESIAN_POINT('',(11.,-3.,12.));
#255915=CARTESIAN_POINT('',(11.,-3.,12.));
#255916=CARTESIAN_POINT('',(11.,-3.,0.));
#255917=CARTESIAN_POINT('Origin',(5.,-3.,0.));
#255918=CARTESIAN_POINT('',(5.,-3.,0.));
#255919=CARTESIAN_POINT('',(5.,-3.,0.));
#255920=CARTESIAN_POINT('',(5.,-3.,12.));
#255921=CARTESIAN_POINT('',(5.,-3.,12.));
#255922=CARTESIAN_POINT('',(5.,-3.,0.));
#255923=CARTESIAN_POINT('Origin',(5.,3.,0.));
#255924=CARTESIAN_POINT('',(5.,3.,0.));
#255925=CARTESIAN_POINT('',(5.,3.,12.));
#255926=CARTESIAN_POINT('Origin',(8.,0.,12.));
#255927=CARTESIAN_POINT('Origin',(8.,0.,0.));
#255928=CARTESIAN_POINT('',(0.,0.,0.));
#255929=CARTESIAN_POINT('Origin',(0.,0.,0.));
#255930=CARTESIAN_POINT('',(-5.,-6.12323399573677E-16,12.));
#255931=CARTESIAN_POINT('Origin',(0.,0.,12.));
#255932=CARTESIAN_POINT('',(-5.,-6.12323399573677E-16,0.));
#255933=CARTESIAN_POINT('',(-5.,-6.12323399573677E-16,0.));
#255934=CARTESIAN_POINT('Origin',(0.,0.,0.));
#255935=CARTESIAN_POINT('Origin',(0.,0.,0.));
#255936=CARTESIAN_POINT('',(-7.,-8.57252759403147E-16,12.));
#255937=CARTESIAN_POINT('Origin',(0.,0.,12.));
#255938=CARTESIAN_POINT('',(-7.,-8.57252759403147E-16,0.));
#255939=CARTESIAN_POINT('',(-7.,-8.57252759403147E-16,0.));
#255940=CARTESIAN_POINT('Origin',(0.,0.,0.));
#255941=CARTESIAN_POINT('Origin',(0.,0.,12.));
#255942=CARTESIAN_POINT('Origin',(0.,0.,0.));
#255943=CARTESIAN_POINT('',(0.,0.,0.));
#255944=CARTESIAN_POINT('Origin',(0.,0.,28.5));
#255945=CARTESIAN_POINT('',(-4.,-4.89858719658941E-16,28.));
#255946=CARTESIAN_POINT('Origin',(0.,0.,28.));
#255947=CARTESIAN_POINT('',(-4.,-4.89858719658941E-16,29.));
#255948=CARTESIAN_POINT('',(-4.,-4.89858719658941E-16,28.5));
#255949=CARTESIAN_POINT('Origin',(0.,0.,29.));
#255950=CARTESIAN_POINT('Origin',(8.,0.,28.));
#255951=CARTESIAN_POINT('',(-5.,6.12323399573677E-16,28.));
#255952=CARTESIAN_POINT('Origin',(0.,0.,28.));
#255953=CARTESIAN_POINT('Origin',(4.,0.,29.));
#255954=CARTESIAN_POINT('',(-5.,-6.12323399573677E-16,29.));
#255955=CARTESIAN_POINT('Origin',(0.,0.,29.));
#255956=CARTESIAN_POINT('Origin',(0.,0.,0.));
#255957=CARTESIAN_POINT('',(-5.,-6.12323399573677E-16,30.));
#255958=CARTESIAN_POINT('Origin',(0.,0.,30.));
#255959=CARTESIAN_POINT('',(-5.,-6.12323399573677E-16,0.));
#255960=CARTESIAN_POINT('Origin',(0.,0.,0.));
#255961=CARTESIAN_POINT('',(-8.,-9.79717439317883E-16,0.));
#255962=CARTESIAN_POINT('Origin',(0.,0.,0.));
#255963=CARTESIAN_POINT('',(-5.,-6.12323399573677E-16,0.));
#255964=CARTESIAN_POINT('Origin',(0.,0.,0.));
#255965=CARTESIAN_POINT('Origin',(0.,0.,-2.));
#255966=CARTESIAN_POINT('',(-8.,-9.79717439317883E-16,-2.));
#255967=CARTESIAN_POINT('',(-8.,-9.79717439317883E-16,-2.));
#255968=CARTESIAN_POINT('Origin',(0.,0.,-2.));
#255969=CARTESIAN_POINT('Origin',(0.,0.,-2.));
#255970=CARTESIAN_POINT('Origin',(0.,0.,0.));
#255971=CARTESIAN_POINT('',(-5.,-6.12323399573677E-16,0.));
#255972=CARTESIAN_POINT('Origin',(0.,0.,30.));
#255973=CARTESIAN_POINT('',(0.,0.,0.));
#255974=CARTESIAN_POINT('Origin',(-1.,0.,1.));
#255975=CARTESIAN_POINT('',(-1.,3.87298334620742,0.));
#255976=CARTESIAN_POINT('',(-1.,3.87298334620742,1.));
#255977=CARTESIAN_POINT('',(-1.,3.87298334620742,0.));
#255978=CARTESIAN_POINT('',(-1.,7.93725393319377,0.));
#255979=CARTESIAN_POINT('',(-1.,0.,0.));
#255980=CARTESIAN_POINT('',(-1.,7.93725393319377,1.));
#255981=CARTESIAN_POINT('',(-1.,7.93725393319377,0.));
#255982=CARTESIAN_POINT('',(-1.,0.,1.));
#255983=CARTESIAN_POINT('Origin',(1.,16.,1.));
#255984=CARTESIAN_POINT('',(1.,3.87298334620742,1.));
#255985=CARTESIAN_POINT('',(1.,3.87298334620742,0.));
#255986=CARTESIAN_POINT('',(1.,3.87298334620742,0.));
#255987=CARTESIAN_POINT('',(1.,7.93725393319377,1.));
#255988=CARTESIAN_POINT('',(1.,8.,1.));
#255989=CARTESIAN_POINT('',(1.,7.93725393319377,0.));
#255990=CARTESIAN_POINT('',(1.,7.93725393319377,0.));
#255991=CARTESIAN_POINT('',(1.,8.,0.));
#255992=CARTESIAN_POINT('Origin',(0.,0.,0.));
#255993=CARTESIAN_POINT('Origin',(0.,0.,0.));
#255994=CARTESIAN_POINT('Origin',(0.,0.,0.));
#255995=CARTESIAN_POINT('Origin',(0.,0.,0.));
#255996=CARTESIAN_POINT('Origin',(0.,0.,1.));
#255997=CARTESIAN_POINT('Origin',(0.,0.,0.));
#255998=CARTESIAN_POINT('Origin',(0.,0.,1.));
#255999=CARTESIAN_POINT('Origin',(0.,0.,1.));
#256000=CARTESIAN_POINT('',(0.,0.,0.));
#256001=CARTESIAN_POINT('Origin',(0.,0.,0.));
#256002=CARTESIAN_POINT('',(-5.,-6.12323399573677E-16,2.));
#256003=CARTESIAN_POINT('Origin',(0.,0.,2.));
#256004=CARTESIAN_POINT('',(-5.,-6.12323399573677E-16,0.));
#256005=CARTESIAN_POINT('',(-5.,-6.12323399573677E-16,0.));
#256006=CARTESIAN_POINT('Origin',(0.,0.,0.));
#256007=CARTESIAN_POINT('Origin',(0.,0.,0.));
#256008=CARTESIAN_POINT('',(-10.,-1.22464679914735E-15,2.));
#256009=CARTESIAN_POINT('Origin',(0.,0.,2.));
#256010=CARTESIAN_POINT('',(-10.,-1.22464679914735E-15,0.));
#256011=CARTESIAN_POINT('',(-10.,-1.22464679914735E-15,0.));
#256012=CARTESIAN_POINT('Origin',(0.,0.,0.));
#256013=CARTESIAN_POINT('Origin',(0.,0.,2.));
#256014=CARTESIAN_POINT('Origin',(0.,0.,0.));
#256015=CARTESIAN_POINT('',(0.,0.,0.));
#256016=CARTESIAN_POINT('Origin',(0.,0.,0.));
#256017=CARTESIAN_POINT('',(-8.,-9.79717439317883E-16,2.));
#256018=CARTESIAN_POINT('Origin',(0.,0.,2.));
#256019=CARTESIAN_POINT('',(-8.,-9.79717439317883E-16,0.));
#256020=CARTESIAN_POINT('',(-8.,-9.79717439317883E-16,0.));
#256021=CARTESIAN_POINT('Origin',(0.,0.,0.));
#256022=CARTESIAN_POINT('Origin',(0.,0.,0.));
#256023=CARTESIAN_POINT('',(-11.,-1.34711147906209E-15,2.));
#256024=CARTESIAN_POINT('Origin',(0.,0.,2.));
#256025=CARTESIAN_POINT('',(-11.,-1.34711147906209E-15,0.));
#256026=CARTESIAN_POINT('',(-11.,-1.34711147906209E-15,0.));
#256027=CARTESIAN_POINT('Origin',(0.,0.,0.));
#256028=CARTESIAN_POINT('Origin',(0.,0.,2.));
#256029=CARTESIAN_POINT('Origin',(0.,0.,0.));
#256030=CARTESIAN_POINT('',(0.,0.,0.));
#256031=CARTESIAN_POINT('Origin',(0.,0.,0.));
#256032=CARTESIAN_POINT('',(-16.,-1.95943487863577E-15,2.));
#256033=CARTESIAN_POINT('Origin',(0.,0.,2.));
#256034=CARTESIAN_POINT('',(-16.,-1.95943487863577E-15,0.));
#256035=CARTESIAN_POINT('',(-16.,-1.95943487863577E-15,0.));
#256036=CARTESIAN_POINT('Origin',(0.,0.,0.));
#256037=CARTESIAN_POINT('Origin',(0.,0.,0.));
#256038=CARTESIAN_POINT('',(-20.,-2.44929359829471E-15,2.));
#256039=CARTESIAN_POINT('Origin',(0.,0.,2.));
#256040=CARTESIAN_POINT('',(-20.,-2.44929359829471E-15,0.));
#256041=CARTESIAN_POINT('',(-20.,-2.44929359829471E-15,0.));
#256042=CARTESIAN_POINT('Origin',(0.,0.,0.));
#256043=CARTESIAN_POINT('Origin',(0.,0.,2.));
#256044=CARTESIAN_POINT('Origin',(0.,0.,0.));
#256045=CARTESIAN_POINT('',(0.,0.,0.));
#256046=CARTESIAN_POINT('Origin',(-1.,0.,1.));
#256047=CARTESIAN_POINT('',(-1.,6.92820323027551,0.));
#256048=CARTESIAN_POINT('',(-1.,6.92820323027551,1.));
#256049=CARTESIAN_POINT('',(-1.,6.92820323027551,0.));
#256050=CARTESIAN_POINT('',(-1.,10.9544511501033,0.));
#256051=CARTESIAN_POINT('',(-1.,0.,0.));
#256052=CARTESIAN_POINT('',(-1.,10.9544511501033,1.));
#256053=CARTESIAN_POINT('',(-1.,10.9544511501033,0.));
#256054=CARTESIAN_POINT('',(-1.,0.,1.));
#256055=CARTESIAN_POINT('Origin',(1.,22.,1.));
#256056=CARTESIAN_POINT('',(1.,6.92820323027551,1.));
#256057=CARTESIAN_POINT('',(1.,6.92820323027551,0.));
#256058=CARTESIAN_POINT('',(1.,6.92820323027551,0.));
#256059=CARTESIAN_POINT('',(1.,10.9544511501033,1.));
#256060=CARTESIAN_POINT('',(1.,11.,1.));
#256061=CARTESIAN_POINT('',(1.,10.9544511501033,0.));
#256062=CARTESIAN_POINT('',(1.,10.9544511501033,0.));
#256063=CARTESIAN_POINT('',(1.,11.,0.));
#256064=CARTESIAN_POINT('Origin',(0.,0.,0.));
#256065=CARTESIAN_POINT('Origin',(0.,0.,0.));
#256066=CARTESIAN_POINT('Origin',(0.,0.,0.));
#256067=CARTESIAN_POINT('Origin',(0.,0.,0.));
#256068=CARTESIAN_POINT('Origin',(0.,0.,1.));
#256069=CARTESIAN_POINT('Origin',(0.,0.,0.));
#256070=CARTESIAN_POINT('Origin',(0.,0.,1.));
#256071=CARTESIAN_POINT('Origin',(0.,0.,1.));
#256072=CARTESIAN_POINT('',(0.,0.,0.));
#256073=CARTESIAN_POINT('Origin',(-1.,0.,1.));
#256074=CARTESIAN_POINT('',(-1.,14.9666295470958,0.));
#256075=CARTESIAN_POINT('',(-1.,14.9666295470958,1.));
#256076=CARTESIAN_POINT('',(-1.,14.9666295470958,0.));
#256077=CARTESIAN_POINT('',(-1.,19.9749843554382,0.));
#256078=CARTESIAN_POINT('',(-1.,0.,0.));
#256079=CARTESIAN_POINT('',(-1.,19.9749843554382,1.));
#256080=CARTESIAN_POINT('',(-1.,19.9749843554382,0.));
#256081=CARTESIAN_POINT('',(-1.,0.,1.));
#256082=CARTESIAN_POINT('Origin',(1.,40.,1.));
#256083=CARTESIAN_POINT('',(1.,14.9666295470958,1.));
#256084=CARTESIAN_POINT('',(1.,14.9666295470958,0.));
#256085=CARTESIAN_POINT('',(1.,14.9666295470958,0.));
#256086=CARTESIAN_POINT('',(1.,19.9749843554382,1.));
#256087=CARTESIAN_POINT('',(1.,20.,1.));
#256088=CARTESIAN_POINT('',(1.,19.9749843554382,0.));
#256089=CARTESIAN_POINT('',(1.,19.9749843554382,0.));
#256090=CARTESIAN_POINT('',(1.,20.,0.));
#256091=CARTESIAN_POINT('Origin',(0.,0.,0.));
#256092=CARTESIAN_POINT('Origin',(0.,0.,0.));
#256093=CARTESIAN_POINT('Origin',(0.,0.,0.));
#256094=CARTESIAN_POINT('Origin',(0.,0.,0.));
#256095=CARTESIAN_POINT('Origin',(0.,0.,1.));
#256096=CARTESIAN_POINT('Origin',(0.,0.,0.));
#256097=CARTESIAN_POINT('Origin',(0.,0.,1.));
#256098=CARTESIAN_POINT('Origin',(0.,0.,1.));
#256099=CARTESIAN_POINT('',(0.,0.,0.));
#256100=CARTESIAN_POINT('Origin',(0.,0.,0.));
#256101=CARTESIAN_POINT('',(-2.,-2.44929359829471E-16,18.));
#256102=CARTESIAN_POINT('Origin',(0.,0.,18.));
#256103=CARTESIAN_POINT('',(-2.,-2.44929359829471E-16,0.));
#256104=CARTESIAN_POINT('',(-2.,-2.44929359829471E-16,0.));
#256105=CARTESIAN_POINT('Origin',(0.,0.,0.));
#256106=CARTESIAN_POINT('Origin',(0.,0.,18.));
#256107=CARTESIAN_POINT('Origin',(0.,0.,0.));
#256108=CARTESIAN_POINT('',(0.,0.,0.));
#256109=CARTESIAN_POINT('Origin',(0.,0.,0.));
#256110=CARTESIAN_POINT('',(-2.94557004194935,0.00189169806540372,0.322176117089595));
#256111=CARTESIAN_POINT('',(-2.9447355781443,0.00314069784331926,0.177823882910384));
#256112=CARTESIAN_POINT('',(-2.942,-3.60291088309151E-16,0.));
#256113=CARTESIAN_POINT('',(1.28892185405323,2.64462557919717,0.));
#256114=CARTESIAN_POINT('Ctrl Pts',(-2.94557004194935,0.00189169806540372,
0.322176117089595));
#256115=CARTESIAN_POINT('Ctrl Pts',(-2.94624968390491,0.100877667946963,
0.316802268464241));
#256116=CARTESIAN_POINT('Ctrl Pts',(-2.94169413341334,0.199796244590278,
0.311428419838886));
#256117=CARTESIAN_POINT('Ctrl Pts',(-2.93169775767856,0.298156773010515,
0.306054571213531));
#256118=CARTESIAN_POINT('Ctrl Pts',(-2.8332180086401,1.26715998088469,0.253113857695288));
#256119=CARTESIAN_POINT('Ctrl Pts',(-2.20669014063059,2.18200296465327,
0.200173144177046));
#256120=CARTESIAN_POINT('Ctrl Pts',(-1.33882305771969,2.62485694228654,
0.147232430658803));
#256121=CARTESIAN_POINT('Ctrl Pts',(-0.534286740179597,3.03539458726557,
0.0981549537725353));
#256122=CARTESIAN_POINT('Ctrl Pts',(0.477651495878826,3.0403146643246,0.0490774768862676));
#256123=CARTESIAN_POINT('Ctrl Pts',(1.29201717055307,2.64849452802569,4.33680868994202E-18));
#256124=CARTESIAN_POINT('',(-1.28892185405326,2.64462557919716,0.));
#256125=CARTESIAN_POINT('Origin',(0.,0.,0.));
#256126=CARTESIAN_POINT('Ctrl Pts',(-1.28892185405326,2.64462557919716,
1.59594559789866E-15));
#256127=CARTESIAN_POINT('Ctrl Pts',(-2.16862035685409,2.21588336549516,
0.0529407135182443));
#256128=CARTESIAN_POINT('Ctrl Pts',(-2.80996338750092,1.31741950685156,
0.105881427036487));
#256129=CARTESIAN_POINT('Ctrl Pts',(-2.92551917741274,0.351793993740128,
0.15882214055473));
#256130=CARTESIAN_POINT('Ctrl Pts',(-2.93934446235059,0.236264967698149,
0.165156054673281));
#256131=CARTESIAN_POINT('Ctrl Pts',(-2.94564356378168,0.119774581438611,
0.171489968791833));
#256132=CARTESIAN_POINT('Ctrl Pts',(-2.9447355781443,0.00314069784331926,
0.177823882910384));
#256133=CARTESIAN_POINT('Origin',(0.,0.,0.));
#256134=CARTESIAN_POINT('',(-2.93798487825769,0.00155454897156224,1.3221761170896));
#256135=CARTESIAN_POINT('',(-2.93771757447194,0.00132355291632602,1.17782388291039));
#256136=CARTESIAN_POINT('',(-2.942,-3.60291088309151E-16,0.));
#256137=CARTESIAN_POINT('Ctrl Pts',(-2.93798487825769,0.00155454897156224,
1.3221761170896));
#256138=CARTESIAN_POINT('Ctrl Pts',(-2.93985103439238,0.392136713800161,
1.30111321624037));
#256139=CARTESIAN_POINT('Ctrl Pts',(-2.86747910744294,0.782054648384103,
1.28005031539114));
#256140=CARTESIAN_POINT('Ctrl Pts',(-2.71761372677595,1.13947848623566,
1.25898741454191));
#256141=CARTESIAN_POINT('Ctrl Pts',(-2.34093340904641,2.03784823785433,
1.20604670102367));
#256142=CARTESIAN_POINT('Ctrl Pts',(-1.47469049342653,2.73093749609884,
1.15310598750542));
#256143=CARTESIAN_POINT('Ctrl Pts',(-0.515567473276226,2.90137621497648,
1.10016527398718));
#256144=CARTESIAN_POINT('Ctrl Pts',(0.443555546874085,3.07181493385413,
1.04722456046894));
#256145=CARTESIAN_POINT('Ctrl Pts',(1.49555867155482,2.7196031133649,0.994283846950693));
#256146=CARTESIAN_POINT('Ctrl Pts',(2.15868031522846,2.00598891393562,0.94134313343245));
#256147=CARTESIAN_POINT('Ctrl Pts',(2.82180195890208,1.29237471450635,0.888402419914207));
#256148=CARTESIAN_POINT('Ctrl Pts',(3.09604212156861,0.217358136137037,
0.835461706395964));
#256149=CARTESIAN_POINT('Ctrl Pts',(2.85583072731624,-0.726685455261021,
0.782520992877721));
#256150=CARTESIAN_POINT('Ctrl Pts',(2.61561933306387,-1.67072904665908,
0.729580279359478));
#256151=CARTESIAN_POINT('Ctrl Pts',(1.86095638189261,-2.48379965108589,
0.676639565841234));
#256152=CARTESIAN_POINT('Ctrl Pts',(0.937402540044778,-2.79371879385104,
0.623698852322991));
#256153=CARTESIAN_POINT('Ctrl Pts',(0.0138486981969448,-3.1036379366162,
0.570758138804748));
#256154=CARTESIAN_POINT('Ctrl Pts',(-1.07859603432746,-2.91040561771969,
0.517817425286505));
#256155=CARTESIAN_POINT('Ctrl Pts',(-1.83960258555595,-2.30220774228156,
0.464876711768262));
#256156=CARTESIAN_POINT('Ctrl Pts',(-2.52336170777509,-1.75574615824684,
0.417309846875373));
#256157=CARTESIAN_POINT('Ctrl Pts',(-2.93955416034762,-0.874287104856683,
0.369742981982484));
#256158=CARTESIAN_POINT('Ctrl Pts',(-2.94557004194935,0.00189169806540372,
0.322176117089595));
#256159=CARTESIAN_POINT('Ctrl Pts',(-2.9447355781443,0.00314069784331926,
0.177823882910384));
#256160=CARTESIAN_POINT('Ctrl Pts',(-2.93805435328604,-0.85508565543347,
0.224430682310076));
#256161=CARTESIAN_POINT('Ctrl Pts',(-2.54114911827883,-1.72108159790374,
0.271037481709768));
#256162=CARTESIAN_POINT('Ctrl Pts',(-1.88115140643926,-2.26900155522438,
0.31764428110946));
#256163=CARTESIAN_POINT('Ctrl Pts',(-1.13145929637718,-2.89138442349815,
0.370584994627703));
#256164=CARTESIAN_POINT('Ctrl Pts',(-0.0423065270762356,-3.10336299246639,
0.423525708145946));
#256165=CARTESIAN_POINT('Ctrl Pts',(0.88679629592561,-2.80996731425714,
0.476466421664189));
#256166=CARTESIAN_POINT('Ctrl Pts',(1.81589911892745,-2.51657163604789,
0.529407135182432));
#256167=CARTESIAN_POINT('Ctrl Pts',(2.5849519956302,-1.71780171066114,0.582347848700675));
#256168=CARTESIAN_POINT('Ctrl Pts',(2.84215968009143,-0.778381688792158,
0.635288562218918));
#256169=CARTESIAN_POINT('Ctrl Pts',(3.09936736455265,0.161038333076827,
0.688229275737162));
#256170=CARTESIAN_POINT('Ctrl Pts',(2.84472985677235,1.24110845142804,0.741169989255405));
#256171=CARTESIAN_POINT('Ctrl Pts',(2.19465508113817,1.9666691917807,0.794110702773649));
#256172=CARTESIAN_POINT('Ctrl Pts',(1.54458030550399,2.69222993213336,0.847051416291892));
#256173=CARTESIAN_POINT('Ctrl Pts',(0.499068262015925,3.06328129448748,
0.899992129810135));
#256174=CARTESIAN_POINT('Ctrl Pts',(-0.462995013488164,2.91019332193529,
0.952932843328378));
#256175=CARTESIAN_POINT('Ctrl Pts',(-1.42505828899225,2.75710534938309,
1.00587355684662));
#256176=CARTESIAN_POINT('Ctrl Pts',(-2.30367279651237,2.0798780419246,1.05881427036486));
#256177=CARTESIAN_POINT('Ctrl Pts',(-2.69654137432937,1.18848910114619,
1.11175498388311));
#256178=CARTESIAN_POINT('Ctrl Pts',(-2.85997195339173,0.817677539756684,
1.13377795022553));
#256179=CARTESIAN_POINT('Ctrl Pts',(-2.93934411301125,0.409805269668763,
1.15580091656796));
#256180=CARTESIAN_POINT('Ctrl Pts',(-2.93771757447194,0.00132355291632602,
1.17782388291039));
#256181=CARTESIAN_POINT('Origin',(0.,0.,0.));
#256182=CARTESIAN_POINT('',(-2.93994176176976,-0.00248389711332564,2.32217611708959));
#256183=CARTESIAN_POINT('',(-2.94042627567403,-0.00258468312704599,2.17782388291038));
#256184=CARTESIAN_POINT('',(-2.942,-3.60291088309151E-16,0.));
#256185=CARTESIAN_POINT('Ctrl Pts',(-2.93994176176976,-0.00248389711332564,
2.32217611708959));
#256186=CARTESIAN_POINT('Ctrl Pts',(-2.93449635628973,0.677888284957744,
2.28542416401649));
#256187=CARTESIAN_POINT('Ctrl Pts',(-2.69945487914443,1.36165532324218,
2.24867221094339));
#256188=CARTESIAN_POINT('Ctrl Pts',(-2.26755203286641,1.88203058384677,
2.21192025787029));
#256189=CARTESIAN_POINT('Ctrl Pts',(-1.64540156355562,2.63162442281503,
2.15897954435204));
#256190=CARTESIAN_POINT('Ctrl Pts',(-0.61476315801349,3.04217982902399,
2.1060388308338));
#256191=CARTESIAN_POINT('Ctrl Pts',(0.352393429603434,2.92568781287356,
2.05309811731556));
#256192=CARTESIAN_POINT('Ctrl Pts',(1.31955001722035,2.80919579672313,2.00015740379731));
#256193=CARTESIAN_POINT('Ctrl Pts',(2.22322478691207,2.16565635821333,1.94721669027907));
#256194=CARTESIAN_POINT('Ctrl Pts',(2.64958937276608,1.28977060664693,1.89427597676083));
#256195=CARTESIAN_POINT('Ctrl Pts',(3.0759539586201,0.413884855080523,1.84133526324259));
#256196=CARTESIAN_POINT('Ctrl Pts',(3.02500836063641,-0.694347209542482,
1.78839454972434));
#256197=CARTESIAN_POINT('Ctrl Pts',(2.52008288608448,-1.52742084653071,
1.7354538362061));
#256198=CARTESIAN_POINT('Ctrl Pts',(2.01515741153255,-2.36049448351894,
1.68251312268785));
#256199=CARTESIAN_POINT('Ctrl Pts',(1.05625206041239,-2.91840969287239,
1.62957240916961));
#256200=CARTESIAN_POINT('Ctrl Pts',(0.0824866859396203,-2.94567843973959,
1.57663169565137));
#256201=CARTESIAN_POINT('Ctrl Pts',(-0.891278688533154,-2.9729471866068,
1.52369098213313));
#256202=CARTESIAN_POINT('Ctrl Pts',(-1.87990408635854,-2.46956947098774,
1.47075026861488));
#256203=CARTESIAN_POINT('Ctrl Pts',(-2.43065792535163,-1.66605549068179,
1.41780955509664));
#256204=CARTESIAN_POINT('Ctrl Pts',(-2.7622897931411,-1.18222619487337,
1.38593174242762));
#256205=CARTESIAN_POINT('Ctrl Pts',(-2.93516052960321,-0.589575095106889,
1.35405392975861));
#256206=CARTESIAN_POINT('Ctrl Pts',(-2.93798487825769,0.00155454897156224,
1.3221761170896));
#256207=CARTESIAN_POINT('Ctrl Pts',(-2.93771757447194,0.00132355291632602,
1.17782388291039));
#256208=CARTESIAN_POINT('Ctrl Pts',(-2.93543409882438,-0.572138452525019,
1.2087416300862));
#256209=CARTESIAN_POINT('Ctrl Pts',(-2.77351048623348,-1.14680161491326,
1.23965937726202));
#256210=CARTESIAN_POINT('Ctrl Pts',(-2.46041273051419,-1.62180832981924,
1.27057712443784));
#256211=CARTESIAN_POINT('Ctrl Pts',(-1.92429286076815,-2.43516624590794,
1.32351783795608));
#256212=CARTESIAN_POINT('Ctrl Pts',(-0.944930473162187,-2.95633150398703,
1.37645855147432));
#256213=CARTESIAN_POINT('Ctrl Pts',(0.029170826245073,-2.94668352979876,
1.42939926499257));
#256214=CARTESIAN_POINT('Ctrl Pts',(1.00327212565234,-2.93703555561049,
1.48233997851081));
#256215=CARTESIAN_POINT('Ctrl Pts',(1.9721123368609,-2.39657434915485,1.53528069202905));
#256216=CARTESIAN_POINT('Ctrl Pts',(2.49202933291632,-1.57277661940358,
1.5882214055473));
#256217=CARTESIAN_POINT('Ctrl Pts',(3.01194632897174,-0.74897888965232,
1.64116211906554));
#256218=CARTESIAN_POINT('Ctrl Pts',(3.08294010987402,0.358155363394565,
1.69410283258378));
#256219=CARTESIAN_POINT('Ctrl Pts',(2.67249570036986,1.24161446820423,1.74704354610203));
#256220=CARTESIAN_POINT('Ctrl Pts',(2.2620512908657,2.1250735730139,1.79998425962027));
#256221=CARTESIAN_POINT('Ctrl Pts',(1.37016869095509,2.78485752958635,1.85292497313851));
#256222=CARTESIAN_POINT('Ctrl Pts',(0.405278167142355,2.91883128448651,
1.90586568665676));
#256223=CARTESIAN_POINT('Ctrl Pts',(-0.559612356670371,3.05280503938667,
1.958806400175));
#256224=CARTESIAN_POINT('Ctrl Pts',(-1.59751080438521,2.66096859261455,
2.01174711369324));
#256225=CARTESIAN_POINT('Ctrl Pts',(-2.23312380973047,1.92275613721379,
2.06468782721148));
#256226=CARTESIAN_POINT('Ctrl Pts',(-2.6858991477565,1.39689465983959,2.10239984577778));
#256227=CARTESIAN_POINT('Ctrl Pts',(-2.9345409799455,0.695270051284926,
2.14011186434408));
#256228=CARTESIAN_POINT('Ctrl Pts',(-2.94042627567403,-0.00258468312704599,
2.17782388291038));
#256229=CARTESIAN_POINT('Origin',(0.,0.,0.));
#256230=CARTESIAN_POINT('',(-2.94682150487212,-0.000171940033828477,3.3221761170896));
#256231=CARTESIAN_POINT('',(-2.94682355286865,0.000158414420006351,3.17782388291039));
#256232=CARTESIAN_POINT('',(-2.942,-3.60291088309151E-16,0.));
#256233=CARTESIAN_POINT('Ctrl Pts',(-2.94682150487212,-0.000171940033828477,
3.3221761170896));
#256234=CARTESIAN_POINT('Ctrl Pts',(-2.9460050992064,0.964791128401366,
3.26973511179262));
#256235=CARTESIAN_POINT('Ctrl Pts',(-2.42654136012265,1.93050781252574,
3.21729410649564));
#256236=CARTESIAN_POINT('Ctrl Pts',(-1.62061705181913,2.46118498029747,
3.16485310119866));
#256237=CARTESIAN_POINT('Ctrl Pts',(-0.80701312333486,2.99691894936566,
3.11191238768042));
#256238=CARTESIAN_POINT('Ctrl Pts',(0.298536727682353,3.08928295206887,
3.05897167416218));
#256239=CARTESIAN_POINT('Ctrl Pts',(1.18975776670605,2.6959798904096,3.00603096064393));
#256240=CARTESIAN_POINT('Ctrl Pts',(2.08097880572974,2.30267682875033,2.95309024712569));
#256241=CARTESIAN_POINT('Ctrl Pts',(2.75787103275992,1.42370670272858,2.90014953360745));
#256242=CARTESIAN_POINT('Ctrl Pts',(2.91045888477416,0.461584467135937,
2.84720882008921));
#256243=CARTESIAN_POINT('Ctrl Pts',(3.0630467367884,-0.500537768456714,
2.79426810657096));
#256244=CARTESIAN_POINT('Ctrl Pts',(2.69133021378669,-1.54581211362026,
2.74132739305272));
#256245=CARTESIAN_POINT('Ctrl Pts',(1.96553293045783,-2.19556632026221,
2.68838667953447));
#256246=CARTESIAN_POINT('Ctrl Pts',(1.23973564712899,-2.84532052690416,
2.63544596601623));
#256247=CARTESIAN_POINT('Ctrl Pts',(0.159857603473006,-3.09955459502451,
2.58250525249799));
#256248=CARTESIAN_POINT('Ctrl Pts',(-0.779582606380496,-2.84184481832332,
2.52956453897975));
#256249=CARTESIAN_POINT('Ctrl Pts',(-1.719022816234,-2.58413504162213,2.4766238254615));
#256250=CARTESIAN_POINT('Ctrl Pts',(-2.51802519228503,-1.81448142009939,
2.42368311194326));
#256251=CARTESIAN_POINT('Ctrl Pts',(-2.81069511377083,-0.885338473474232,
2.37074239842502));
#256252=CARTESIAN_POINT('Ctrl Pts',(-2.90019075773866,-0.601215506808447,
2.35455363797988));
#256253=CARTESIAN_POINT('Ctrl Pts',(-2.94234039252192,-0.302179052012372,
2.33836487753473));
#256254=CARTESIAN_POINT('Ctrl Pts',(-2.93994176176976,-0.00248389711332564,
2.32217611708959));
#256255=CARTESIAN_POINT('Ctrl Pts',(-2.94042627567403,-0.00258468312704599,
2.17782388291038));
#256256=CARTESIAN_POINT('Ctrl Pts',(-2.94280284889284,-0.284389192011812,
2.19305257786233));
#256257=CARTESIAN_POINT('Ctrl Pts',(-2.90559386610683,-0.565578959204417,
2.20828127281427));
#256258=CARTESIAN_POINT('Ctrl Pts',(-2.82625604206022,-0.834331928330834,
2.22350996776621));
#256259=CARTESIAN_POINT('Ctrl Pts',(-2.55044770606905,-1.76861907444532,
2.27645068128446));
#256260=CARTESIAN_POINT('Ctrl Pts',(-1.76550347111102,-2.55260490264487,
2.3293913948027));
#256261=CARTESIAN_POINT('Ctrl Pts',(-0.830880469484507,-2.82727233874327,
2.38233210832095));
#256262=CARTESIAN_POINT('Ctrl Pts',(0.103742532142001,-3.10193977484166,
2.43527282183919));
#256263=CARTESIAN_POINT('Ctrl Pts',(1.188044300437,-2.8672888188389,2.48821353535743));
#256264=CARTESIAN_POINT('Ctrl Pts',(1.92548059413032,-2.23077491982669,
2.54115424887567));
#256265=CARTESIAN_POINT('Ctrl Pts',(2.66291688782364,-1.59426102081447,
2.59409496239392));
#256266=CARTESIAN_POINT('Ctrl Pts',(3.05348770691528,-0.555884178792804,
2.64703567591216));
#256267=CARTESIAN_POINT('Ctrl Pts',(2.91833523468123,0.408841796814555,
2.6999763894304));
#256268=CARTESIAN_POINT('Ctrl Pts',(2.78318276244717,1.37356777242192,2.75291710294865));
#256269=CARTESIAN_POINT('Ctrl Pts',(2.1223069988874,2.26464288161497,2.80585781646689));
#256270=CARTESIAN_POINT('Ctrl Pts',(1.23834897999233,2.67400892624479,2.85879852998513));
#256271=CARTESIAN_POINT('Ctrl Pts',(0.354390961097264,3.08337497087461,
2.91173924350338));
#256272=CARTESIAN_POINT('Ctrl Pts',(-0.752649313133101,3.0110319509412,
2.96467995702162));
#256273=CARTESIAN_POINT('Ctrl Pts',(-1.57581460636975,2.49010851479218,
3.01762067053986));
#256274=CARTESIAN_POINT('Ctrl Pts',(-2.39897989960641,1.96918507864315,
3.07056138405811));
#256275=CARTESIAN_POINT('Ctrl Pts',(-2.93827021184934,0.999681226278506,
3.12350209757635));
#256276=CARTESIAN_POINT('Ctrl Pts',(-2.94672329720919,0.0255709168879045,
3.17644281109459));
#256277=CARTESIAN_POINT('Ctrl Pts',(-2.94679680281682,0.0171003328177383,
3.17690316836652));
#256278=CARTESIAN_POINT('Ctrl Pts',(-2.94683016893847,0.00862940042833639,
3.17736352563846));
#256279=CARTESIAN_POINT('Ctrl Pts',(-2.94682355286865,0.000158414420006351,
3.17782388291039));
#256280=CARTESIAN_POINT('Origin',(0.,0.,0.));
#256281=CARTESIAN_POINT('',(-2.94044650265958,0.0025882162845009,4.3221761170896));
#256282=CARTESIAN_POINT('',(-2.9399612768956,0.00248864850571281,4.17782388291038));
#256283=CARTESIAN_POINT('',(-2.942,-3.60291088309151E-16,0.));
#256284=CARTESIAN_POINT('Ctrl Pts',(-2.94044650265958,0.0025882162845009,
4.3221761170896));
#256285=CARTESIAN_POINT('Ctrl Pts',(-2.94282130517145,0.283659464351577,
4.30698677308699));
#256286=CARTESIAN_POINT('Ctrl Pts',(-2.90580786785067,0.5641179787111,4.29179742908438));
#256287=CARTESIAN_POINT('Ctrl Pts',(-2.82687388743177,0.832235035317424,
4.27660808508177));
#256288=CARTESIAN_POINT('Ctrl Pts',(-2.55175856688243,1.76672623393097,
4.22366737156353));
#256289=CARTESIAN_POINT('Ctrl Pts',(-1.76739628630419,2.55129452175516,
4.17072665804528));
#256290=CARTESIAN_POINT('Ctrl Pts',(-0.832977367533957,2.82665523805142,
4.11778594452704));
#256291=CARTESIAN_POINT('Ctrl Pts',(0.101441551236281,3.10201595434767,
4.0648452310088));
#256292=CARTESIAN_POINT('Ctrl Pts',(1.18591710819853,2.86816909911599,4.01190451749056));
#256293=CARTESIAN_POINT('Ctrl Pts',(1.92382531476357,2.23220234016443,3.95896380397231));
#256294=CARTESIAN_POINT('Ctrl Pts',(2.6617335213286,1.59623558121286,3.90602309045407));
#256295=CARTESIAN_POINT('Ctrl Pts',(3.05307437749644,0.558148918541431,
3.85308237693583));
#256296=CARTESIAN_POINT('Ctrl Pts',(2.91863752141895,-0.406676957864641,
3.80014166341758));
#256297=CARTESIAN_POINT('Ctrl Pts',(2.78420066534145,-1.37150283427072,
3.74720094989934));
#256298=CARTESIAN_POINT('Ctrl Pts',(2.12398609701859,-2.26306792441144,
3.6942602363811));
#256299=CARTESIAN_POINT('Ctrl Pts',(1.24033202067288,-2.67308952506278,
3.64131952286285));
#256300=CARTESIAN_POINT('Ctrl Pts',(0.356677944327172,-3.08311112571411,
3.58837880934461));
#256301=CARTESIAN_POINT('Ctrl Pts',(-0.750415640041392,-3.01158923687608,
3.53543809582637));
#256302=CARTESIAN_POINT('Ctrl Pts',(-1.57396706019169,-2.49127654439024,
3.48249738230812));
#256303=CARTESIAN_POINT('Ctrl Pts',(-2.39751848034199,-1.97096385190439,
3.42955666878988));
#256304=CARTESIAN_POINT('Ctrl Pts',(-2.93752773627403,-1.00186035577074,
3.37661595527164));
#256305=CARTESIAN_POINT('Ctrl Pts',(-2.94670336126438,-0.0277566399873261,
3.3236752417534));
#256306=CARTESIAN_POINT('Ctrl Pts',(-2.94678997013189,-0.0185620598089631,
3.32317553353213));
#256307=CARTESIAN_POINT('Ctrl Pts',(-2.94682928436873,-0.00936703413595167,
3.32267582531086));
#256308=CARTESIAN_POINT('Ctrl Pts',(-2.94682150487212,-0.000171940033828477,
3.3221761170896));
#256309=CARTESIAN_POINT('Ctrl Pts',(-2.94682355286865,0.000158414420006351,
3.17782388291039));
#256310=CARTESIAN_POINT('Ctrl Pts',(-2.94606932626624,-0.965527131525665,
3.2303042391567));
#256311=CARTESIAN_POINT('Ctrl Pts',(-2.42571392052528,-1.93190949916178,
3.28278459540301));
#256312=CARTESIAN_POINT('Ctrl Pts',(-1.61879111254203,-2.46238651897324,
3.33526495164932));
#256313=CARTESIAN_POINT('Ctrl Pts',(-0.80478998403827,-2.99751687902722,
3.38820566516757));
#256314=CARTESIAN_POINT('Ctrl Pts',(0.300828131446,-3.08906083271863,3.44114637868581));
#256315=CARTESIAN_POINT('Ctrl Pts',(1.19175723997081,-2.6950967957953,3.49408709220405));
#256316=CARTESIAN_POINT('Ctrl Pts',(2.08268634849563,-2.30113275887196,
3.5470278057223));
#256317=CARTESIAN_POINT('Ctrl Pts',(2.75892645006097,-1.42166073133388,
3.59996851924054));
#256318=CARTESIAN_POINT('Ctrl Pts',(2.91080061718145,-0.459425531762414,
3.65290923275878));
#256319=CARTESIAN_POINT('Ctrl Pts',(3.06267478430194,0.502809667809053,
3.70584994627703));
#256320=CARTESIAN_POINT('Ctrl Pts',(2.69018301697755,1.54780803941391,3.75879065979527));
#256321=CARTESIAN_POINT('Ctrl Pts',(1.96390393916053,2.19702375199443,3.81173137331351));
#256322=CARTESIAN_POINT('Ctrl Pts',(1.23762486134351,2.84623946457495,3.86467208683175));
#256323=CARTESIAN_POINT('Ctrl Pts',(0.157558473033873,3.09967251813113,
3.91761280035));
#256324=CARTESIAN_POINT('Ctrl Pts',(-0.781690369275895,2.84126595357656,
3.97055351386824));
#256325=CARTESIAN_POINT('Ctrl Pts',(-1.72093921158567,2.58285938902198,
4.02349422738649));
#256326=CARTESIAN_POINT('Ctrl Pts',(-2.51937050789556,1.81261320635664,
4.07643494090473));
#256327=CARTESIAN_POINT('Ctrl Pts',(-2.81135118077459,0.883253411949605,
4.12937565442297));
#256328=CARTESIAN_POINT('Ctrl Pts',(-2.90041902927571,0.599754930508779,
4.14552506391878));
#256329=CARTESIAN_POINT('Ctrl Pts',(-2.94235976611751,0.301450336487282,
4.16167447341458));
#256330=CARTESIAN_POINT('Ctrl Pts',(-2.9399612768956,0.00248864850571281,
4.17782388291038));
#256331=CARTESIAN_POINT('Origin',(0.,0.,0.));
#256332=CARTESIAN_POINT('',(-2.93771571390321,-0.00129109254332599,5.3221761170896));
#256333=CARTESIAN_POINT('',(-2.93797409250287,-0.00154122909697584,5.17782388291039));
#256334=CARTESIAN_POINT('',(-2.942,-3.60291088309151E-16,0.));
#256335=CARTESIAN_POINT('Ctrl Pts',(-2.93771571390321,-0.00129109254332599,
5.3221761170896));
#256336=CARTESIAN_POINT('Ctrl Pts',(-2.93545056844751,0.571435936275613,
5.29129772086311));
#256337=CARTESIAN_POINT('Ctrl Pts',(-2.7739600267295,1.14534299189815,5.26041932463663));
#256338=CARTESIAN_POINT('Ctrl Pts',(-2.46161048164032,1.61997066829654,
5.22954092841015));
#256339=CARTESIAN_POINT('Ctrl Pts',(-1.92609018897895,2.4337152572233,5.17660021489191));
#256340=CARTESIAN_POINT('Ctrl Pts',(-0.947123281983236,2.95563036559962,
5.12365950137366));
#256341=CARTESIAN_POINT('Ctrl Pts',(0.0269828091199985,2.94671054864219,
5.07071878785542));
#256342=CARTESIAN_POINT('Ctrl Pts',(1.00108890022323,2.93779073168476,5.01777807433718));
#256343=CARTESIAN_POINT('Ctrl Pts',(1.97033417543399,2.39803598939359,4.96483736081894));
#256344=CARTESIAN_POINT('Ctrl Pts',(2.4908631218815,1.57462123620547,4.91189664730069));
#256345=CARTESIAN_POINT('Ctrl Pts',(3.01139206832902,0.751206483017347,
4.85895593378245));
#256346=CARTESIAN_POINT('Ctrl Pts',(3.08320468601329,-0.355868281067734,
4.8060152202642));
#256347=CARTESIAN_POINT('Ctrl Pts',(2.67341515431747,-1.23963000210775,
4.75307450674596));
#256348=CARTESIAN_POINT('Ctrl Pts',(2.26362562262165,-2.12339172314776,
4.70013379322772));
#256349=CARTESIAN_POINT('Ctrl Pts',(1.37223394154574,-2.78384040114272,
4.64719307970947));
#256350=CARTESIAN_POINT('Ctrl Pts',(0.407443402759136,-2.91853062396757,
4.59425236619123));
#256351=CARTESIAN_POINT('Ctrl Pts',(-0.55734713602746,-3.05322084679241,
4.54131165267299));
#256352=CARTESIAN_POINT('Ctrl Pts',(-1.59553653252474,-2.66215261444716,
4.48837093915474));
#256353=CARTESIAN_POINT('Ctrl Pts',(-2.23169705051315,-1.92441144357309,
4.4354302256365));
#256354=CARTESIAN_POINT('Ctrl Pts',(-2.68533526559998,-1.39833731842992,
4.39767885612087));
#256355=CARTESIAN_POINT('Ctrl Pts',(-2.93454420384162,-0.695982080377398,
4.35992748660523));
#256356=CARTESIAN_POINT('Ctrl Pts',(-2.94044650265958,0.0025882162845009,
4.3221761170896));
#256357=CARTESIAN_POINT('Ctrl Pts',(-2.9399612768956,0.00248864850571281,
4.17782388291038));
#256358=CARTESIAN_POINT('Ctrl Pts',(-2.93449708043811,-0.678600672837507,
4.21461518693282));
#256359=CARTESIAN_POINT('Ctrl Pts',(-2.69890715531692,-1.36310038808667,
4.25140649095526));
#256360=CARTESIAN_POINT('Ctrl Pts',(-2.26615555049358,-1.88371204593479,
4.2881977949777));
#256361=CARTESIAN_POINT('Ctrl Pts',(-1.64344919788537,-2.63284430326346,
4.34113850849594));
#256362=CARTESIAN_POINT('Ctrl Pts',(-0.612506443220769,-3.04263541177207,
4.39407922201419));
#256363=CARTESIAN_POINT('Ctrl Pts',(0.354563499507598,-2.92542591366007,
4.44701993553243));
#256364=CARTESIAN_POINT('Ctrl Pts',(1.32163344223596,-2.80821641554808,
4.49996064905067));
#256365=CARTESIAN_POINT('Ctrl Pts',(2.22483057302809,-2.16400631081546,
4.55290136256892));
#256366=CARTESIAN_POINT('Ctrl Pts',(2.65054542067995,-1.28780473063139,
4.60584207608716));
#256367=CARTESIAN_POINT('Ctrl Pts',(3.07626026833181,-0.411603150447325,
4.65878278960541));
#256368=CARTESIAN_POINT('Ctrl Pts',(3.02449283284339,0.696589905188196,
4.71172350312365));
#256369=CARTESIAN_POINT('Ctrl Pts',(2.51894945793883,1.52928927271612,4.76466421664189));
#256370=CARTESIAN_POINT('Ctrl Pts',(2.01340608303427,2.36198864024403,4.81760493016013));
#256371=CARTESIAN_POINT('Ctrl Pts',(1.05408676871357,2.91919431966434,4.87054564367837));
#256372=CARTESIAN_POINT('Ctrl Pts',(0.0803015401539713,2.94573992640351,
4.92348635719662));
#256373=CARTESIAN_POINT('Ctrl Pts',(-0.893483688405635,2.97228553314268,
4.97642707071486));
#256374=CARTESIAN_POINT('Ctrl Pts',(-1.88173483120415,2.46817106720069,
5.02936778423311));
#256375=CARTESIAN_POINT('Ctrl Pts',(-2.43189284146947,1.66425035945319,
5.08230849775135));
#256376=CARTESIAN_POINT('Ctrl Pts',(-2.76275700225513,1.18077371211907,
5.11414695947103));
#256377=CARTESIAN_POINT('Ctrl Pts',(-2.93517161021586,0.588863123642047,
5.14598542119071));
#256378=CARTESIAN_POINT('Ctrl Pts',(-2.93797409250287,-0.00154122909697584,
5.17782388291039));
#256379=CARTESIAN_POINT('Origin',(0.,0.,0.));
#256380=CARTESIAN_POINT('',(-2.94517248244385,-0.00193699951557325,6.3221761170896));
#256381=CARTESIAN_POINT('',(-2.94559088235875,-0.00170176706889942,6.17782388291039));
#256382=CARTESIAN_POINT('',(-2.942,-3.60291088309151E-16,0.));
#256383=CARTESIAN_POINT('Ctrl Pts',(-2.94517248244385,-0.00193699951557325,
6.3221761170896));
#256384=CARTESIAN_POINT('Ctrl Pts',(-2.9386420685114,0.856218115624555,
6.27560866863924));
#256385=CARTESIAN_POINT('Ctrl Pts',(-2.54183626857632,1.71963167034793,
6.22904122018889));
#256386=CARTESIAN_POINT('Ctrl Pts',(-1.88262592526034,2.26705773084874,
6.18247377173853));
#256387=CARTESIAN_POINT('Ctrl Pts',(-1.13319543045971,2.88940504009179,
6.12953305822029));
#256388=CARTESIAN_POINT('Ctrl Pts',(-0.0446194458096424,3.10335342402028,
6.07659234470204));
#256389=CARTESIAN_POINT('Ctrl Pts',(0.884600293036423,2.81092750725154,
6.0236516311838));
#256390=CARTESIAN_POINT('Ctrl Pts',(1.81382003188248,2.51850159048281,5.97071091766556));
#256391=CARTESIAN_POINT('Ctrl Pts',(2.58368352492452,1.71970137301683,5.91777020414732));
#256392=CARTESIAN_POINT('Ctrl Pts',(2.84164001510992,0.780328875532278,
5.86482949062907));
#256393=CARTESIAN_POINT('Ctrl Pts',(3.09959650529531,-0.159043621952279,
5.81188877711083));
#256394=CARTESIAN_POINT('Ctrl Pts',(2.84564599262406,-1.23898839945542,
5.75894806359258));
#256395=CARTESIAN_POINT('Ctrl Pts',(2.196082399727,-1.96495629037203,5.70600735007434));
#256396=CARTESIAN_POINT('Ctrl Pts',(1.54651880682993,-2.69092418128863,
5.65306663655609));
#256397=CARTESIAN_POINT('Ctrl Pts',(0.501342133707051,-3.06291518561871,
5.60012592303785));
#256398=CARTESIAN_POINT('Ctrl Pts',(-0.460820134777716,-2.91057999938971,
5.54718520951961));
#256399=CARTESIAN_POINT('Ctrl Pts',(-1.42298240326247,-2.75824481316072,
5.49424449600136));
#256400=CARTESIAN_POINT('Ctrl Pts',(-2.30213026710911,-2.08158343637267,
5.44130378248312));
#256401=CARTESIAN_POINT('Ctrl Pts',(-2.69566735986892,-1.19046571324005,
5.38836306896488));
#256402=CARTESIAN_POINT('Ctrl Pts',(-2.85966855345979,-0.819104606720612,
5.36630075167312));
#256403=CARTESIAN_POINT('Ctrl Pts',(-2.93933413855808,-0.41049904941688,
5.34423843438136));
#256404=CARTESIAN_POINT('Ctrl Pts',(-2.93771571390321,-0.00129109254332599,
5.3221761170896));
#256405=CARTESIAN_POINT('Ctrl Pts',(-2.93797409250287,-0.00154122909697584,
5.17782388291039));
#256406=CARTESIAN_POINT('Ctrl Pts',(-2.93983155306118,-0.39285603017501,
5.19892613470895));
#256407=CARTESIAN_POINT('Ctrl Pts',(-2.86717973724354,-0.783509153708209,
5.22002838650751));
#256408=CARTESIAN_POINT('Ctrl Pts',(-2.71676856184761,-1.14149053114142,
5.24113063830608));
#256409=CARTESIAN_POINT('Ctrl Pts',(-2.3394213942283,-2.03958376443549,
5.29407135182432));
#256410=CARTESIAN_POINT('Ctrl Pts',(-1.47266218125755,-2.7320432814706,
5.34701206534256));
#256411=CARTESIAN_POINT('Ctrl Pts',(-0.51341403914473,-2.90176464857968,
5.39995277886081));
#256412=CARTESIAN_POINT('Ctrl Pts',(0.445834102968095,-3.07148601568877,
5.45289349237905));
#256413=CARTESIAN_POINT('Ctrl Pts',(1.49757117422299,-2.71846923287181,
5.5058342058973));
#256414=CARTESIAN_POINT('Ctrl Pts',(2.16016542555926,-2.00437456218931,
5.55877491941554));
#256415=CARTESIAN_POINT('Ctrl Pts',(2.82275967689551,-1.29027989150683,
5.61171563293378));
#256416=CARTESIAN_POINT('Ctrl Pts',(3.09621110831315,-0.215107332958816,
5.66465634645202));
#256417=CARTESIAN_POINT('Ctrl Pts',(2.85529555990017,0.728779333507592,
5.71759705997026));
#256418=CARTESIAN_POINT('Ctrl Pts',(2.61438001148719,1.67266599997401,5.77053777348851));
#256419=CARTESIAN_POINT('Ctrl Pts',(1.85909748324357,2.48526677435882,5.82347848700676));
#256420=CARTESIAN_POINT('Ctrl Pts',(0.935321535258006,2.7944598184653,5.876419200525));
#256421=CARTESIAN_POINT('Ctrl Pts',(0.0115455872724497,3.10365286257177,
5.92935991404324));
#256422=CARTESIAN_POINT('Ctrl Pts',(-1.08072378045507,2.90943817639992,
5.98230062756148));
#256423=CARTESIAN_POINT('Ctrl Pts',(-1.84129348697169,2.30075429939171,
6.03524134107972));
#256424=CARTESIAN_POINT('Ctrl Pts',(-2.52409477409559,1.75430848237877,
6.08276885502328));
#256425=CARTESIAN_POINT('Ctrl Pts',(-2.93956117072973,0.873819286065656,
6.13029636896684));
#256426=CARTESIAN_POINT('Ctrl Pts',(-2.94559088235875,-0.00170176706889942,
6.17782388291039));
#256427=CARTESIAN_POINT('Origin',(0.,0.,0.));
#256428=CARTESIAN_POINT('',(-2.94368178595509,0.00247084038202318,7.3221761170896));
#256429=CARTESIAN_POINT('',(-2.94315318334351,0.00257818642023648,7.17782388291039));
#256430=CARTESIAN_POINT('',(-2.942,-3.60291088309151E-16,0.));
#256431=CARTESIAN_POINT('Ctrl Pts',(-2.94368178595509,0.00247084038202318,
7.3221761170896));
#256432=CARTESIAN_POINT('Ctrl Pts',(-2.94522564461956,0.17437048182408,
7.31286032993361));
#256433=CARTESIAN_POINT('Ctrl Pts',(-2.93146429530118,0.346023191581102,
7.30354454277762));
#256434=CARTESIAN_POINT('Ctrl Pts',(-2.90151816454975,0.51480430286788,
7.29422875562163));
#256435=CARTESIAN_POINT('Ctrl Pts',(-2.7313372123076,1.4739709637528,7.24128804210339));
#256436=CARTESIAN_POINT('Ctrl Pts',(-2.03846251298597,2.3403982465541,7.18834732858515));
#256437=CARTESIAN_POINT('Ctrl Pts',(-1.14018862853796,2.71731503893386,
7.13540661506691));
#256438=CARTESIAN_POINT('Ctrl Pts',(-0.241914744089952,3.09423183131363,
7.08246590154866));
#256439=CARTESIAN_POINT('Ctrl Pts',(0.861758325484441,2.98163813327185,
7.02952518803042));
#256440=CARTESIAN_POINT('Ctrl Pts',(1.6654152958735,2.43109502523739,6.97658447451217));
#256441=CARTESIAN_POINT('Ctrl Pts',(2.46907226626257,1.88055191720293,6.92364376099393));
#256442=CARTESIAN_POINT('Ctrl Pts',(2.97271313746631,0.892059399175779,
6.87070304747569));
#256443=CARTESIAN_POINT('Ctrl Pts',(2.94570095627119,-0.0817129468714171,
6.81776233395745));
#256444=CARTESIAN_POINT('Ctrl Pts',(2.91868877507608,-1.05548529291861,
6.76482162043921));
#256445=CARTESIAN_POINT('Ctrl Pts',(2.36102354148214,-2.01453746698584,
6.71188090692096));
#256446=CARTESIAN_POINT('Ctrl Pts',(1.5280820879569,-2.5196817779094,6.65894019340271));
#256447=CARTESIAN_POINT('Ctrl Pts',(0.695140634431661,-3.02482608883297,
6.60599947988447));
#256448=CARTESIAN_POINT('Ctrl Pts',(-0.413077039024869,-3.07606253661285,
6.55305876636623));
#256449=CARTESIAN_POINT('Ctrl Pts',(-1.28907449533346,-2.64992793768891,
6.50011805284799));
#256450=CARTESIAN_POINT('Ctrl Pts',(-2.16507195164203,-2.22379333876499,
6.44717733932974));
#256451=CARTESIAN_POINT('Ctrl Pts',(-2.80884919080268,-1.32028769313726,
6.3942366258115));
#256452=CARTESIAN_POINT('Ctrl Pts',(-2.92559530790742,-0.353161753044597,
6.34129591229326));
#256453=CARTESIAN_POINT('Ctrl Pts',(-2.939649783197,-0.236734346600298,
6.33492264722537));
#256454=CARTESIAN_POINT('Ctrl Pts',(-2.94606624107525,-0.119384920759988,
6.32854938215748));
#256455=CARTESIAN_POINT('Ctrl Pts',(-2.94517248244385,-0.00193699951557325,
6.3221761170896));
#256456=CARTESIAN_POINT('Ctrl Pts',(-2.94559088235875,-0.00170176706889942,
6.17782388291039));
#256457=CARTESIAN_POINT('Ctrl Pts',(-2.94627764313619,-0.101420220638511,
6.18323708248508));
#256458=CARTESIAN_POINT('Ctrl Pts',(-2.94165305741639,-0.201074225831034,
6.18865028205977));
#256459=CARTESIAN_POINT('Ctrl Pts',(-2.93150717012004,-0.300162893890445,
6.19406348163446));
#256460=CARTESIAN_POINT('Ctrl Pts',(-2.83228110144603,-1.26924314231981,
6.2470041951527));
#256461=CARTESIAN_POINT('Ctrl Pts',(-2.20495891879229,-2.18425057133397,
6.29994490867094));
#256462=CARTESIAN_POINT('Ctrl Pts',(-1.33681610983853,-2.62616730994242,
6.35288562218918));
#256463=CARTESIAN_POINT('Ctrl Pts',(-0.468673300884761,-3.06808404855088,
6.40582633570743));
#256464=CARTESIAN_POINT('Ctrl Pts',(0.640290134369015,-3.03691009675363,
6.45876704922568));
#256465=CARTESIAN_POINT('Ctrl Pts',(1.48223624520047,-2.54692123253703,
6.51170776274392));
#256466=CARTESIAN_POINT('Ctrl Pts',(2.32418235603191,-2.05693236832044,
6.56464847626216));
#256467=CARTESIAN_POINT('Ctrl Pts',(2.89911114244103,-1.1081285916845,6.6175891897804));
#256468=CARTESIAN_POINT('Ctrl Pts',(2.94374011249023,-0.135004449741251,
6.67052990329864));
#256469=CARTESIAN_POINT('Ctrl Pts',(2.98836908253944,0.838119692202002,
6.72347061681688));
#256470=CARTESIAN_POINT('Ctrl Pts',(2.50269823622873,1.83556419945258,6.77641133033513));
#256471=CARTESIAN_POINT('Ctrl Pts',(1.70913534596548,2.40056002226677,6.82935204385338));
#256472=CARTESIAN_POINT('Ctrl Pts',(0.915572455702211,2.96555584508097,
6.88229275737162));
#256473=CARTESIAN_POINT('Ctrl Pts',(-0.185882478513599,3.09810298345876,
6.93523347088986));
#256474=CARTESIAN_POINT('Ctrl Pts',(-1.09082994374658,2.7375028922651,6.9881741844081));
#256475=CARTESIAN_POINT('Ctrl Pts',(-1.99577740897954,2.37690280107145,
7.04111489792634));
#256476=CARTESIAN_POINT('Ctrl Pts',(-2.70421740522968,1.52315548030635,
7.0940556114446));
#256477=CARTESIAN_POINT('Ctrl Pts',(-2.89172740920335,0.567225389237848,
7.14699632496284));
#256478=CARTESIAN_POINT('Ctrl Pts',(-2.92812331403787,0.381678272360454,
7.15727217761202));
#256479=CARTESIAN_POINT('Ctrl Pts',(-2.94489305060584,0.19228139395339,
7.16754803026121));
#256480=CARTESIAN_POINT('Ctrl Pts',(-2.94315318334351,0.00257818642023648,
7.17782388291039));
#256481=CARTESIAN_POINT('Origin',(0.,0.,0.));
#256482=CARTESIAN_POINT('',(-2.93722985491238,0.00044505069937778,8.3221761170896));
#256483=CARTESIAN_POINT('',(-2.93717599790887,0.000154098632716083,8.17782388291039));
#256484=CARTESIAN_POINT('',(-2.942,-3.60291088309151E-16,0.));
#256485=CARTESIAN_POINT('Ctrl Pts',(-2.93722985491238,0.00044505069937778,
8.3221761170896));
#256486=CARTESIAN_POINT('Ctrl Pts',(-2.93785622278809,0.464421997225427,
8.29717127770974));
#256487=CARTESIAN_POINT('Ctrl Pts',(-2.83444790412075,0.928134993578535,
8.27216643832987));
#256488=CARTESIAN_POINT('Ctrl Pts',(-2.62552634776407,1.33807418578346,
8.24716159895001));
#256489=CARTESIAN_POINT('Ctrl Pts',(-2.18319372187359,2.20600510926297,
8.19422088543177));
#256490=CARTESIAN_POINT('Ctrl Pts',(-1.26788587165546,2.83288877045659,
8.14128017191352));
#256491=CARTESIAN_POINT('Ctrl Pts',(-0.298758242779041,2.9316504978996,
8.08833945839528));
#256492=CARTESIAN_POINT('Ctrl Pts',(0.670369386097388,3.03041222534262,
8.03539874487704));
#256493=CARTESIAN_POINT('Ctrl Pts',(1.6933167936321,2.60105201903501,7.9824580313588));
#256494=CARTESIAN_POINT('Ctrl Pts',(2.30163614951384,1.84019079573682,7.92951731784056));
#256495=CARTESIAN_POINT('Ctrl Pts',(2.90995550539557,1.07932957243865,7.87657660432231));
#256496=CARTESIAN_POINT('Ctrl Pts',(3.10364680962433,-0.0130326678500794,
7.82363589080407));
#256497=CARTESIAN_POINT('Ctrl Pts',(2.79401119992451,-0.936660314180018,
7.77069517728582));
#256498=CARTESIAN_POINT('Ctrl Pts',(2.48437559022469,-1.86028796050997,
7.71775446376758));
#256499=CARTESIAN_POINT('Ctrl Pts',(1.67141306659626,-2.61518101288112,
7.66481375024934));
#256500=CARTESIAN_POINT('Ctrl Pts',(0.727411126434527,-2.855644267517,7.61187303673109));
#256501=CARTESIAN_POINT('Ctrl Pts',(-0.21659081372719,-3.09610752215287,
7.55893232321285));
#256502=CARTESIAN_POINT('Ctrl Pts',(-1.29163217042221,-2.82214097905349,
7.50599160969461));
#256503=CARTESIAN_POINT('Ctrl Pts',(-2.00540924618839,-2.15920468801954,
7.45305089617636));
#256504=CARTESIAN_POINT('Ctrl Pts',(-2.59358553434202,-1.61292291436613,
7.40942596981411));
#256505=CARTESIAN_POINT('Ctrl Pts',(-2.93645204579212,-0.802518483014787,
7.36580104345185));
#256506=CARTESIAN_POINT('Ctrl Pts',(-2.94368178595509,0.00247084038202318,
7.3221761170896));
#256507=CARTESIAN_POINT('Ctrl Pts',(-2.94315318334351,0.00257818642023648,
7.17782388291039));
#256508=CARTESIAN_POINT('Ctrl Pts',(-2.93592933562868,-0.785060682307407,
7.22048874377945));
#256509=CARTESIAN_POINT('Ctrl Pts',(-2.60962367215334,-1.57798027204179,
7.2631536046485));
#256510=CARTESIAN_POINT('Ctrl Pts',(-2.04415356378889,-2.12256172088897,
7.30581846551756));
#256511=CARTESIAN_POINT('Ctrl Pts',(-1.34248970270355,-2.79830587857536,
7.3587591790358));
#256512=CARTESIAN_POINT('Ctrl Pts',(-0.272581968835661,-3.09168133257619,
7.41169989255405));
#256513=CARTESIAN_POINT('Ctrl Pts',(0.675616828049579,-2.86833992981832,
7.4646406060723));
#256514=CARTESIAN_POINT('Ctrl Pts',(1.62381562493482,-2.64499852706046,
7.51758131959054));
#256515=CARTESIAN_POINT('Ctrl Pts',(2.45030548483741,-1.90494026754388,
7.57052203310878));
#256516=CARTESIAN_POINT('Ctrl Pts',(2.77660421131805,-0.987066920236321,
7.62346274662702));
#256517=CARTESIAN_POINT('Ctrl Pts',(3.10290293779869,-0.0691935729287693,
7.67640346014526));
#256518=CARTESIAN_POINT('Ctrl Pts',(2.92901053085739,1.02649486216977,7.72934417366351));
#256519=CARTESIAN_POINT('Ctrl Pts',(2.33455915940062,1.79823957875268,7.78228488718175));
#256520=CARTESIAN_POINT('Ctrl Pts',(1.74010778794386,2.56998429533559,7.8352256007));
#256521=CARTESIAN_POINT('Ctrl Pts',(0.725097451971645,3.01778529340287,
7.88816631421824));
#256522=CARTESIAN_POINT('Ctrl Pts',(-0.245658715282151,2.9365768927341,
7.94110702773649));
#256523=CARTESIAN_POINT('Ctrl Pts',(-1.21641488253595,2.85536849206534,
7.99404774125473));
#256524=CARTESIAN_POINT('Ctrl Pts',(-2.14291688107131,2.24515069266052,
8.04698845477297));
#256525=CARTESIAN_POINT('Ctrl Pts',(-2.60088302465875,1.38536621273075,
8.09992916829121));
#256526=CARTESIAN_POINT('Ctrl Pts',(-2.82549366103092,0.963682771969861,
8.12589407316427));
#256527=CARTESIAN_POINT('Ctrl Pts',(-2.9374009741482,0.481967651729552,
8.15185897803733));
#256528=CARTESIAN_POINT('Ctrl Pts',(-2.93717599790887,0.000154098632716083,
8.17782388291039));
#256529=CARTESIAN_POINT('Origin',(0.,0.,0.));
#256530=CARTESIAN_POINT('',(-2.94204712377748,-0.00269013877321395,9.3221761170896));
#256531=CARTESIAN_POINT('',(-2.94258699139408,-0.00265391868664876,9.17782388291039));
#256532=CARTESIAN_POINT('',(-2.942,-3.60291088309151E-16,0.));
#256533=CARTESIAN_POINT('Ctrl Pts',(-2.94204712377748,-0.00269013877321395,
9.3221761170896));
#256534=CARTESIAN_POINT('Ctrl Pts',(-2.93512682590844,0.749287554217331,
9.28148222548586));
#256535=CARTESIAN_POINT('Ctrl Pts',(-2.6412639315254,1.50607184887019,9.24078833388212));
#256536=CARTESIAN_POINT('Ctrl Pts',(-2.12158192997297,2.04517022369181,
9.20009444227839));
#256537=CARTESIAN_POINT('Ctrl Pts',(-1.44550169088747,2.74651019130897,
9.14715372876014));
#256538=CARTESIAN_POINT('Ctrl Pts',(-0.387229252469055,3.07942314003042,
9.0942130152419));
#256539=CARTESIAN_POINT('Ctrl Pts',(0.56861083469072,2.89145514371842,9.04127230172366));
#256540=CARTESIAN_POINT('Ctrl Pts',(1.5244509218505,2.70348714740643,8.98833158820542));
#256541=CARTESIAN_POINT('Ctrl Pts',(2.37785865775163,1.99463820606099,8.93539087468717));
#256542=CARTESIAN_POINT('Ctrl Pts',(2.73802509238449,1.08951811501063,8.88245016116893));
#256543=CARTESIAN_POINT('Ctrl Pts',(3.09819152701736,0.184398023960259,
8.82950944765069));
#256544=CARTESIAN_POINT('Ctrl Pts',(2.96511666038193,-0.916993216795031,
8.77656873413245));
#256545=CARTESIAN_POINT('Ctrl Pts',(2.39974070512762,-1.71028526205923,
8.7236280206142));
#256546=CARTESIAN_POINT('Ctrl Pts',(1.83436474987331,-2.50357730732343,
8.67068730709596));
#256547=CARTESIAN_POINT('Ctrl Pts',(0.836687706000118,-2.98877015709654,
8.61774659357772));
#256548=CARTESIAN_POINT('Ctrl Pts',(-0.136414889087667,-2.94367493237596,
8.56480588005947));
#256549=CARTESIAN_POINT('Ctrl Pts',(-1.10951748417545,-2.89857970765538,
8.51186516654123));
#256550=CARTESIAN_POINT('Ctrl Pts',(-2.05804563047783,-2.32319640844112,
8.45892445302298));
#256551=CARTESIAN_POINT('Ctrl Pts',(-2.5476310028476,-1.48101566595129,
8.40598373950474));
#256552=CARTESIAN_POINT('Ctrl Pts',(-2.80597650734862,-1.03661184778483,
8.37804786536636));
#256553=CARTESIAN_POINT('Ctrl Pts',(-2.93653006500875,-0.517918670193003,
8.35011199122798));
#256554=CARTESIAN_POINT('Ctrl Pts',(-2.93722985491238,0.00044505069937778,
8.3221761170896));
#256555=CARTESIAN_POINT('Ctrl Pts',(-2.93717599790887,0.000154098632716083,
8.17782388291039));
#256556=CARTESIAN_POINT('Ctrl Pts',(-2.9369422625645,-0.500418126628262,
8.20479969155557));
#256557=CARTESIAN_POINT('Ctrl Pts',(-2.81567486845355,-1.00109659861654,
8.23177550020076));
#256558=CARTESIAN_POINT('Ctrl Pts',(-2.57401417690804,-1.43467176330002,
8.25875130884594));
#256559=CARTESIAN_POINT('Ctrl Pts',(-2.09974889693042,-2.28557409894624,
8.31169202236419));
#256560=CARTESIAN_POINT('Ctrl Pts',(-1.1617880483357,-2.87802760978395,
8.36463273588243));
#256561=CARTESIAN_POINT('Ctrl Pts',(-0.189660775246745,-2.94072454365702,
8.41757344940067));
#256562=CARTESIAN_POINT('Ctrl Pts',(0.782466497842209,-3.00342147753008,
8.47051416291892));
#256563=CARTESIAN_POINT('Ctrl Pts',(1.7887601954254,-2.53636183443847,8.52345487643716));
#256564=CARTESIAN_POINT('Ctrl Pts',(2.36839887564121,-1.75343058522299,
8.5763955899554));
#256565=CARTESIAN_POINT('Ctrl Pts',(2.94803755585702,-0.97049933600749,
8.62933630347364));
#256566=CARTESIAN_POINT('Ctrl Pts',(3.10102121870546,0.128303519331893,
8.68227701699189));
#256567=CARTESIAN_POINT('Ctrl Pts',(2.7572926311298,1.0397929590314,8.73521773051013));
#256568=CARTESIAN_POINT('Ctrl Pts',(2.41356404355414,1.9512823987309,8.78815844402838));
#256569=CARTESIAN_POINT('Ctrl Pts',(1.57312320555439,2.67545842279051,8.84109915754662));
#256570=CARTESIAN_POINT('Ctrl Pts',(0.620841014858106,2.88069236219419,
8.89403987106487));
#256571=CARTESIAN_POINT('Ctrl Pts',(-0.331441175838184,3.08592630159786,
8.94698058458311));
#256572=CARTESIAN_POINT('Ctrl Pts',(-1.395564719231,2.77221815634559,8.99992129810135));
#256573=CARTESIAN_POINT('Ctrl Pts',(-2.08422561375214,2.08322721811939,
9.05286201161959));
#256574=CARTESIAN_POINT('Ctrl Pts',(-2.62606665533224,1.54112649688225,
9.09451596871652));
#256575=CARTESIAN_POINT('Ctrl Pts',(-2.93547367882327,0.766703099201119,
9.13616992581345));
#256576=CARTESIAN_POINT('Ctrl Pts',(-2.94258699139408,-0.00265391868664876,
9.17782388291039));
#256577=CARTESIAN_POINT('Origin',(0.,0.,0.));
#256578=CARTESIAN_POINT('',(-2.946293830078,0.00114127199139325,10.3221761170896));
#256579=CARTESIAN_POINT('',(-2.94598056703706,0.00142614341313253,10.1778238829104));
#256580=CARTESIAN_POINT('',(-2.942,-3.60291088309151E-16,0.));
#256581=CARTESIAN_POINT('Ctrl Pts',(-2.946293830078,0.00114127199139325,
10.3221761170896));
#256582=CARTESIAN_POINT('Ctrl Pts',(-2.94660735229615,0.0645118181007279,
10.3187338867802));
#256583=CARTESIAN_POINT('Ctrl Pts',(-2.94474004527922,0.127863547905195,
10.3152916564709));
#256584=CARTESIAN_POINT('Ctrl Pts',(-2.94063317604738,0.19106976054023,
10.3118494261615));
#256585=CARTESIAN_POINT('Ctrl Pts',(-2.87747046817515,1.16316682986685,
10.2589087126433));
#256586=CARTESIAN_POINT('Ctrl Pts',(-2.28456764274864,2.10084365316138,
10.205967999125));
#256587=CARTESIAN_POINT('Ctrl Pts',(-1.43343821073695,2.57470115265106,
10.1530272856068));
#256588=CARTESIAN_POINT('Ctrl Pts',(-0.582308778725255,3.04855865214073,
10.1000865720885));
#256589=CARTESIAN_POINT('Ctrl Pts',(0.527047259871636,3.05859682782553,
10.0471458585703));
#256590=CARTESIAN_POINT('Ctrl Pts',(1.38661216582722,2.60021880445538,9.99420514505204));
#256591=CARTESIAN_POINT('Ctrl Pts',(2.24617707178282,2.14184078108523,9.9412644315338));
#256592=CARTESIAN_POINT('Ctrl Pts',(2.8559508450971,1.21504655866011,9.88832371801555));
#256593=CARTESIAN_POINT('Ctrl Pts',(2.93669410456063,0.244251644216089,
9.83538300449731));
#256594=CARTESIAN_POINT('Ctrl Pts',(3.01743736402416,-0.726543270227937,
9.78244229097906));
#256595=CARTESIAN_POINT('Ctrl Pts',(2.56915010963695,-1.74133887669088,
9.72950157746082));
#256596=CARTESIAN_POINT('Ctrl Pts',(1.79712069750322,-2.33542037502223,
9.67656086394258));
#256597=CARTESIAN_POINT('Ctrl Pts',(1.02509128536949,-2.92950187335358,
9.62362015042434));
#256598=CARTESIAN_POINT('Ctrl Pts',(-0.0706802845107621,-3.10286926355335,
9.57067943690609));
#256599=CARTESIAN_POINT('Ctrl Pts',(-0.988397135146327,-2.77613080251957,
9.51773872338785));
#256600=CARTESIAN_POINT('Ctrl Pts',(-1.90611398578189,-2.4493923414858,
9.4647980098696));
#256601=CARTESIAN_POINT('Ctrl Pts',(-2.64577611717277,-1.62254802921848,
9.41185729635136));
#256602=CARTESIAN_POINT('Ctrl Pts',(-2.86866316299192,-0.674242379828374,
9.35891658283312));
#256603=CARTESIAN_POINT('Ctrl Pts',(-2.92022381973027,-0.454869998218924,
9.34666976091862));
#256604=CARTESIAN_POINT('Ctrl Pts',(-2.94412978661107,-0.228997737451993,
9.33442293900411));
#256605=CARTESIAN_POINT('Ctrl Pts',(-2.94204712377748,-0.00269013877321395,
9.3221761170896));
#256606=CARTESIAN_POINT('Ctrl Pts',(-2.94258699139408,-0.00265391868664876,
9.17782388291039));
#256607=CARTESIAN_POINT('Ctrl Pts',(-2.94451444875782,-0.211122594104875,
9.1891106393317));
#256608=CARTESIAN_POINT('Ctrl Pts',(-2.92424691955225,-0.419219286159219,
9.20039739575301));
#256609=CARTESIAN_POINT('Ctrl Pts',(-2.88039456209096,-0.622221197011802,
9.21168415217432));
#256610=CARTESIAN_POINT('Ctrl Pts',(-2.67470437025918,-1.57440494271673,
9.26462486569256));
#256611=CARTESIAN_POINT('Ctrl Pts',(-1.95012574094615,-2.41449870292648,
9.3175655792108));
#256612=CARTESIAN_POINT('Ctrl Pts',(-1.03847171194,-2.75779052047728,9.37050629272905));
#256613=CARTESIAN_POINT('Ctrl Pts',(-0.126817682933869,-3.10108233802808,
9.42344700624729));
#256614=CARTESIAN_POINT('Ctrl Pts',(0.971911745765368,-2.94757221291993,
9.47638771976554));
#256615=CARTESIAN_POINT('Ctrl Pts',(1.7545651773389,-2.36755846597369,9.52932843328378));
#256616=CARTESIAN_POINT('Ctrl Pts',(2.53721860891243,-1.78754471902744,
9.58226914680202));
#256617=CARTESIAN_POINT('Ctrl Pts',(3.00379604336026,-0.781027350243069,
9.63520986032027));
#256618=CARTESIAN_POINT('Ctrl Pts',(2.94063333213535,0.191069770682194,
9.68815057383851));
#256619=CARTESIAN_POINT('Ctrl Pts',(2.87747062091044,1.16316689160746,9.74109128735675));
#256620=CARTESIAN_POINT('Ctrl Pts',(2.28456776401279,2.10084376467362,9.794032000875));
#256621=CARTESIAN_POINT('Ctrl Pts',(1.43343828682337,2.57470128931549,9.84697271439324));
#256622=CARTESIAN_POINT('Ctrl Pts',(0.582308809633943,3.04855881395736,
9.89991342791148));
#256623=CARTESIAN_POINT('Ctrl Pts',(-0.527047287847267,3.05859699017495,
9.95285414142973));
#256624=CARTESIAN_POINT('Ctrl Pts',(-1.3866122394283,2.60021894247419,10.005794854948));
#256625=CARTESIAN_POINT('Ctrl Pts',(-2.24617719100933,2.14184089477343,
10.0587355684662));
#256626=CARTESIAN_POINT('Ctrl Pts',(-2.85595099669019,1.21504662315432,
10.1116762819844));
#256627=CARTESIAN_POINT('Ctrl Pts',(-2.93669426043952,0.244251657180776,
10.1646169955027));
#256628=CARTESIAN_POINT('Ctrl Pts',(-2.94340848296254,0.163525004292322,
10.1690192913053));
#256629=CARTESIAN_POINT('Ctrl Pts',(-2.94646457151759,0.0824940959367936,
10.1734215871078));
#256630=CARTESIAN_POINT('Ctrl Pts',(-2.94598056703706,0.00142614341313253,
10.1778238829104));
#256631=CARTESIAN_POINT('Origin',(0.,0.,0.));
#256632=CARTESIAN_POINT('',(-2.93864369880353,0.00199559307489716,11.3221761170896));
#256633=CARTESIAN_POINT('',(-2.9382951498277,0.00178522549583758,11.1778238829104));
#256634=CARTESIAN_POINT('',(-2.942,-3.60291088309151E-16,0.));
#256635=CARTESIAN_POINT('Ctrl Pts',(-2.93864369880353,0.00199559307489716,
11.3221761170896));
#256636=CARTESIAN_POINT('Ctrl Pts',(-2.94085467865027,0.356558542189881,
11.3030448345564));
#256637=CARTESIAN_POINT('Ctrl Pts',(-2.88150630694549,0.71040631434159,
11.2839135520231));
#256638=CARTESIAN_POINT('Ctrl Pts',(-2.75729248477352,1.03979290383945,
11.2647822694899));
#256639=CARTESIAN_POINT('Ctrl Pts',(-2.4135639154429,1.95128229515734,11.2118415559716));
#256640=CARTESIAN_POINT('Ctrl Pts',(-1.57312312205356,2.6754582807779,11.1589008424534));
#256641=CARTESIAN_POINT('Ctrl Pts',(-0.620840981904164,2.88069220928785,
11.1059601289351));
#256642=CARTESIAN_POINT('Ctrl Pts',(0.331441158245256,3.0859261377978,11.0530194154169));
#256643=CARTESIAN_POINT('Ctrl Pts',(1.39556464515472,2.77221800919711,11.0000787018987));
#256644=CARTESIAN_POINT('Ctrl Pts',(2.08422550312197,2.08322710754239,10.9471379883804));
#256645=CARTESIAN_POINT('Ctrl Pts',(2.77288636108922,1.39423620588766,10.8941972748622));
#256646=CARTESIAN_POINT('Ctrl Pts',(3.08608459011425,0.329962531178855,
10.8412565613439));
#256647=CARTESIAN_POINT('Ctrl Pts',(2.88039440920046,-0.622221163984446,
10.7883158478257));
#256648=CARTESIAN_POINT('Ctrl Pts',(2.67470422828667,-1.57440485914773,
10.7353751343074));
#256649=CARTESIAN_POINT('Ctrl Pts',(1.95012563743409,-2.41449857476555,
10.6824344207892));
#256650=CARTESIAN_POINT('Ctrl Pts',(1.0384716568183,-2.75779037409454,10.629493707271));
#256651=CARTESIAN_POINT('Ctrl Pts',(0.12681767620249,-3.10108217342353,
10.5765529937527));
#256652=CARTESIAN_POINT('Ctrl Pts',(-0.971911694176526,-2.94757205646368,
10.5236122802345));
#256653=CARTESIAN_POINT('Ctrl Pts',(-1.75456508420706,-2.3675583403044,
10.4706715667162));
#256654=CARTESIAN_POINT('Ctrl Pts',(-2.48632997950726,-1.82525739114296,
10.4211730835074));
#256655=CARTESIAN_POINT('Ctrl Pts',(-2.94178545241125,-0.910112662410656,
10.3716746002985));
#256656=CARTESIAN_POINT('Ctrl Pts',(-2.946293830078,0.00114127199139325,
10.3221761170896));
#256657=CARTESIAN_POINT('Ctrl Pts',(-2.94598056703706,0.00142614341313253,
10.1778238829104));
#256658=CARTESIAN_POINT('Ctrl Pts',(-2.94064407610001,-0.892405238989152,
10.2263623006261));
#256659=CARTESIAN_POINT('Ctrl Pts',(-2.50495197977583,-1.79073993959316,
10.2749007183418));
#256660=CARTESIAN_POINT('Ctrl Pts',(-1.79712079289381,-2.33542049898572,
10.3234391360574));
#256661=CARTESIAN_POINT('Ctrl Pts',(-1.02509133978096,-2.92950202885072,
10.3763798495757));
#256662=CARTESIAN_POINT('Ctrl Pts',(0.0706802882625301,-3.10286942825275,
10.4293205630939));
#256663=CARTESIAN_POINT('Ctrl Pts',(0.988397187610237,-2.77613094987577,
10.4822612766122));
#256664=CARTESIAN_POINT('Ctrl Pts',(1.90611408695794,-2.44939247149879,
10.5352019901304));
#256665=CARTESIAN_POINT('Ctrl Pts',(2.64577625760985,-1.6225481153428,10.5881427036486));
#256666=CARTESIAN_POINT('Ctrl Pts',(2.86866331525975,-0.674242415616888,
10.6410834171669));
#256667=CARTESIAN_POINT('Ctrl Pts',(3.09155037290965,0.274063284109008,
10.6940241306851));
#256668=CARTESIAN_POINT('Ctrl Pts',(2.79766231755754,1.34383032740484,10.7469648442034));
#256669=CARTESIAN_POINT('Ctrl Pts',(2.12158204258587,2.04517033224891,10.7999055577216));
#256670=CARTESIAN_POINT('Ctrl Pts',(1.4455017676142,2.74651033709298,10.8528462712399));
#256671=CARTESIAN_POINT('Ctrl Pts',(0.387229273022993,3.07942330348533,
10.9057869847581));
#256672=CARTESIAN_POINT('Ctrl Pts',(-0.568610864872497,2.89145529719602,
10.9587276982763));
#256673=CARTESIAN_POINT('Ctrl Pts',(-1.524451002768,2.70348729090671,11.0116684117946));
#256674=CARTESIAN_POINT('Ctrl Pts',(-2.37785878396776,1.99463831193572,
11.0646091253128));
#256675=CARTESIAN_POINT('Ctrl Pts',(-2.73802523771812,1.08951817284182,
11.1175498388311));
#256676=CARTESIAN_POINT('Ctrl Pts',(-2.87471076930343,0.746019143233786,
11.1376411868575));
#256677=CARTESIAN_POINT('Ctrl Pts',(-2.94035710602654,0.374252114952768,
11.157732534884));
#256678=CARTESIAN_POINT('Ctrl Pts',(-2.9382951498277,0.00178522549583758,
11.1778238829104));
#256679=CARTESIAN_POINT('Origin',(0.,0.,0.));
#256680=CARTESIAN_POINT('',(-2.9390533811986,-0.0021916646264461,12.3221761170896));
#256681=CARTESIAN_POINT('',(-2.93947917419302,-0.0023511949260692,12.1778238829104));
#256682=CARTESIAN_POINT('',(-2.942,-3.60291088309151E-16,0.));
#256683=CARTESIAN_POINT('Ctrl Pts',(-2.9390533811986,-0.0021916646264461,
12.3221761170896));
#256684=CARTESIAN_POINT('Ctrl Pts',(-2.93459418397931,0.64291277294828,
12.2873557823325));
#256685=CARTESIAN_POINT('Ctrl Pts',(-2.7255434646052,1.29064511658111,12.2525354475754));
#256686=CARTESIAN_POINT('Ctrl Pts',(-2.33455903548297,1.79823948330255,
12.2177151128183));
#256687=CARTESIAN_POINT('Ctrl Pts',(-1.74010769557955,2.5699841589215,12.1647743993));
#256688=CARTESIAN_POINT('Ctrl Pts',(-0.725097413483787,3.01778513321968,
12.1118336857818));
#256689=CARTESIAN_POINT('Ctrl Pts',(0.245658702242558,2.93657673686146,
12.0588929722635));
#256690=CARTESIAN_POINT('Ctrl Pts',(1.21641481796892,2.85536834050325,12.0059522587453));
#256691=CARTESIAN_POINT('Ctrl Pts',(2.14291676732584,2.24515057348865,11.953011545227));
#256692=CARTESIAN_POINT('Ctrl Pts',(2.6008828866046,1.38536613919598,11.9000708317088));
#256693=CARTESIAN_POINT('Ctrl Pts',(3.05884900588334,0.525581704903325,
11.8471301181905));
#256694=CARTESIAN_POINT('Ctrl Pts',(3.0482792950839,-0.583769396667378,
11.7941894046723));
#256695=CARTESIAN_POINT('Ctrl Pts',(2.57401404028016,-1.43467168714797,
11.7412486911541));
#256696=CARTESIAN_POINT('Ctrl Pts',(2.09974878547643,-2.28557397762857,
11.6883079776358));
#256697=CARTESIAN_POINT('Ctrl Pts',(1.16178798666839,-2.87802745701906,
11.6353672641176));
#256698=CARTESIAN_POINT('Ctrl Pts',(0.189660765179664,-2.94072438756421,
11.5824265505993));
#256699=CARTESIAN_POINT('Ctrl Pts',(-0.782466456309061,-3.00342131810935,
11.5294858370811));
#256700=CARTESIAN_POINT('Ctrl Pts',(-1.78876010047849,-2.53636169980915,
11.4765451235628));
#256701=CARTESIAN_POINT('Ctrl Pts',(-2.36839874992726,-1.75343049215143,
11.4236044100446));
#256702=CARTESIAN_POINT('Ctrl Pts',(-2.73857231980224,-1.25342856788223,
11.3897949790596));
#256703=CARTESIAN_POINT('Ctrl Pts',(-2.93473638258426,-0.624599698542917,
11.3559855480746));
#256704=CARTESIAN_POINT('Ctrl Pts',(-2.93864369880353,0.00199559307489716,
11.3221761170896));
#256705=CARTESIAN_POINT('Ctrl Pts',(-2.9382951498277,0.00178522549583758,
11.1778238829104));
#256706=CARTESIAN_POINT('Ctrl Pts',(-2.93492385026559,-0.607198351378453,
11.2106732484022));
#256707=CARTESIAN_POINT('Ctrl Pts',(-2.75055292297376,-1.21805281595107,
11.243522613894));
#256708=CARTESIAN_POINT('Ctrl Pts',(-2.3997408325051,-1.71028535284078,
11.2763719793858));
#256709=CARTESIAN_POINT('Ctrl Pts',(-1.83436484724077,-2.50357744021265,
11.329312692904));
#256710=CARTESIAN_POINT('Ctrl Pts',(-0.836687750411167,-2.98877031573962,
11.3822534064223));
#256711=CARTESIAN_POINT('Ctrl Pts',(0.136414896328608,-2.94367508862538,
11.4351941199405));
#256712=CARTESIAN_POINT('Ctrl Pts',(1.10951754306841,-2.89857986151113,
11.4881348334588));
#256713=CARTESIAN_POINT('Ctrl Pts',(2.05804573971839,-2.32319653175565,
11.541075546977));
#256714=CARTESIAN_POINT('Ctrl Pts',(2.54763113807518,-1.48101574456307,
11.5940162604953));
#256715=CARTESIAN_POINT('Ctrl Pts',(3.03721653643197,-0.638834957370519,
11.6469569740135));
#256716=CARTESIAN_POINT('Ctrl Pts',(3.06785913649561,0.470143287259109,
11.6998976875318));
#256717=CARTESIAN_POINT('Ctrl Pts',(2.62552648712622,1.33807425680813,11.75283840105));
#256718=CARTESIAN_POINT('Ctrl Pts',(2.18319383775683,2.20600522635714,11.8057791145682));
#256719=CARTESIAN_POINT('Ctrl Pts',(1.2678859389544,2.83288892082555,11.8587198280865));
#256720=CARTESIAN_POINT('Ctrl Pts',(0.298758258636965,2.93165065351078,
11.9116605416047));
#256721=CARTESIAN_POINT('Ctrl Pts',(-0.670369421680497,3.03041238619601,
11.964601255123));
#256722=CARTESIAN_POINT('Ctrl Pts',(-1.69331688351297,2.60105215709804,
12.0175419686412));
#256723=CARTESIAN_POINT('Ctrl Pts',(-2.3016362716841,1.84019089341353,12.0704826821594));
#256724=CARTESIAN_POINT('Ctrl Pts',(-2.71277374495007,1.32595678623232,
12.1062630824098));
#256725=CARTESIAN_POINT('Ctrl Pts',(-2.93451578093251,0.66029833662526,
12.1420434826601));
#256726=CARTESIAN_POINT('Ctrl Pts',(-2.93947917419302,-0.00235119492606921,
12.1778238829104));
#256727=CARTESIAN_POINT('Origin',(0.,0.,0.));
#256728=CARTESIAN_POINT('',(-2.9465548750618,-0.00082129130520664,13.3221761170896));
#256729=CARTESIAN_POINT('',(-2.94672861832122,-0.000503025179204854,13.1778238829104));
#256730=CARTESIAN_POINT('',(-2.942,-3.60291088309151E-16,0.));
#256731=CARTESIAN_POINT('Ctrl Pts',(-2.9465548750618,-0.00082129130520664,
13.3221761170896));
#256732=CARTESIAN_POINT('Ctrl Pts',(-2.94311022400094,0.928823737220892,
13.2716667301086));
#256733=CARTESIAN_POINT('Ctrl Pts',(-2.46625336580265,1.86151179281048,
13.2211573431276));
#256734=CARTESIAN_POINT('Ctrl Pts',(-1.70913525524513,2.4005598948457,13.1706479561466));
#256735=CARTESIAN_POINT('Ctrl Pts',(-0.915572407103973,2.9655556876701,
13.1177072426284));
#256736=CARTESIAN_POINT('Ctrl Pts',(0.185882468646932,3.09810281901236,
13.0647665291101));
#256737=CARTESIAN_POINT('Ctrl Pts',(1.09082988584557,2.73750274695927,13.0118258155919));
#256738=CARTESIAN_POINT('Ctrl Pts',(1.99577730304421,2.37690267490618,12.9588851020737));
#256739=CARTESIAN_POINT('Ctrl Pts',(2.70421726169058,1.52315539945775,12.9059443885554));
#256740=CARTESIAN_POINT('Ctrl Pts',(2.8917272557113,0.567225359129726,12.8530036750372));
#256741=CARTESIAN_POINT('Ctrl Pts',(3.07923724973201,-0.388704681198295,
12.8000629615189));
#256742=CARTESIAN_POINT('Ctrl Pts',(2.74581727912706,-1.4468174864059,12.7471222480007));
#256743=CARTESIAN_POINT('Ctrl Pts',(2.04415345528584,-2.12256160822399,
12.6941815344824));
#256744=CARTESIAN_POINT('Ctrl Pts',(1.34248963144462,-2.79830573004207,
12.6412408209642));
#256745=CARTESIAN_POINT('Ctrl Pts',(0.272581954367126,-3.09168116847064,
12.588300107446));
#256746=CARTESIAN_POINT('Ctrl Pts',(-0.675616792187998,-2.86833977756768,
12.5353593939277));
#256747=CARTESIAN_POINT('Ctrl Pts',(-1.62381553874312,-2.64499838666472,
12.4824186804095));
#256748=CARTESIAN_POINT('Ctrl Pts',(-2.45030535477588,-1.90494016643023,
12.4294779668912));
#256749=CARTESIAN_POINT('Ctrl Pts',(-2.77660406393669,-0.98706686784313,
12.376537253373));
#256750=CARTESIAN_POINT('Ctrl Pts',(-2.88828854656504,-0.672900119421985,
12.3584168746119));
#256751=CARTESIAN_POINT('Ctrl Pts',(-2.94137393162258,-0.337901726889642,
12.3402964958507));
#256752=CARTESIAN_POINT('Ctrl Pts',(-2.9390533811986,-0.0021916646264461,
12.3221761170896));
#256753=CARTESIAN_POINT('Ctrl Pts',(-2.93947917419302,-0.00235119492606921,
12.1778238829104));
#256754=CARTESIAN_POINT('Ctrl Pts',(-2.94185962222118,-0.320158527116781,
12.1949841961783));
#256755=CARTESIAN_POINT('Ctrl Pts',(-2.89437728571495,-0.637273756843844,
12.2121445094463));
#256756=CARTESIAN_POINT('Ctrl Pts',(-2.79401134822979,-0.936660363897793,
12.2293048227142));
#256757=CARTESIAN_POINT('Ctrl Pts',(-2.48437572209456,-1.86028805925362,
12.2822455362324));
#256758=CARTESIAN_POINT('Ctrl Pts',(-1.67141315531429,-2.61518115169423,
12.3351862497507));
#256759=CARTESIAN_POINT('Ctrl Pts',(-0.727411165045203,-2.8556444190938,
12.3881269632689));
#256760=CARTESIAN_POINT('Ctrl Pts',(0.216590825223855,-3.09610768649335,
12.4410676767871));
#256761=CARTESIAN_POINT('Ctrl Pts',(1.29163223898172,-2.82214112885189,
12.4940083903054));
#256762=CARTESIAN_POINT('Ctrl Pts',(2.00540935263496,-2.15920480262948,
12.5469491038236));
#256763=CARTESIAN_POINT('Ctrl Pts',(2.71918646628823,-1.49626847640703,
12.5998898173419));
#256764=CARTESIAN_POINT('Ctrl Pts',(3.07169927983683,-0.444362381603572,
12.6528305308601));
#256765=CARTESIAN_POINT('Ctrl Pts',(2.90151831856148,0.514804330193662,
12.7057712443784));
#256766=CARTESIAN_POINT('Ctrl Pts',(2.73133735728613,1.47397104199087,12.7587119578966));
#256767=CARTESIAN_POINT('Ctrl Pts',(2.03846262118687,2.34039837078186,12.8116526714149));
#256768=CARTESIAN_POINT('Ctrl Pts',(1.14018868905871,2.71731518316822,12.8645933849331));
#256769=CARTESIAN_POINT('Ctrl Pts',(0.241914756930561,3.09423199555458,
12.9175340984513));
#256770=CARTESIAN_POINT('Ctrl Pts',(-0.861758371226483,2.9816382915363,
12.9704748119696));
#256771=CARTESIAN_POINT('Ctrl Pts',(-1.6654153842734,2.43109515427912,13.0234155254878));
#256772=CARTESIAN_POINT('Ctrl Pts',(-2.44673818273382,1.89585201237694,
13.074884977962));
#256773=CARTESIAN_POINT('Ctrl Pts',(-2.94448848959189,0.946663066484181,
13.1263544304362));
#256774=CARTESIAN_POINT('Ctrl Pts',(-2.94672861832122,-0.000503025179204854,
13.1778238829104));
#256775=CARTESIAN_POINT('Origin',(0.,0.,0.));
#256776=CARTESIAN_POINT('',(-2.94148383545301,0.00269085865063343,14.3221761170896));
#256777=CARTESIAN_POINT('',(-2.94096005475604,0.00265658997900563,14.1778238829104));
#256778=CARTESIAN_POINT('',(-2.942,-3.60291088309151E-16,0.));
#256779=CARTESIAN_POINT('Ctrl Pts',(-2.94148383545301,0.00269085865063343,
14.3221761170896));
#256780=CARTESIAN_POINT('Ctrl Pts',(-2.94370082512592,0.247798640329141,
14.308918391403));
#256781=CARTESIAN_POINT('Ctrl Pts',(-2.91562689752491,0.492405641969356,
14.2956606657164));
#256782=CARTESIAN_POINT('Ctrl Pts',(-2.85529540834193,0.728779294824118,
14.2824029400297));
#256783=CARTESIAN_POINT('Ctrl Pts',(-2.6143798727167,1.67266591118932,14.2294622265115));
#256784=CARTESIAN_POINT('Ctrl Pts',(-1.85909738456329,2.48526664244153,
14.1765215129932));
#256785=CARTESIAN_POINT('Ctrl Pts',(-0.935321485611485,2.79445967013616,
14.123580799475));
#256786=CARTESIAN_POINT('Ctrl Pts',(-0.0115455866596831,3.10365269783079,
14.0706400859568));
#256787=CARTESIAN_POINT('Ctrl Pts',(1.0807237230905,2.90943802196782,14.0176993724385));
#256788=CARTESIAN_POINT('Ctrl Pts',(1.84129338923632,2.30075417726838,13.9647586589203));
#256789=CARTESIAN_POINT('Ctrl Pts',(2.60186305538213,1.69207033256895,13.911817945402));
#256790=CARTESIAN_POINT('Ctrl Pts',(3.0307330779236,0.668917319033036,13.8588772318838));
#256791=CARTESIAN_POINT('Ctrl Pts',(2.9315070145165,-0.300162877957828,
13.8059365183655));
#256792=CARTESIAN_POINT('Ctrl Pts',(2.8322809511094,-1.26924307494871,13.7529958048473));
#256793=CARTESIAN_POINT('Ctrl Pts',(2.20495880175375,-2.18425045539455,
13.7000550913291));
#256794=CARTESIAN_POINT('Ctrl Pts',(1.33681603888075,-2.62616717054621,
13.6471143778108));
#256795=CARTESIAN_POINT('Ctrl Pts',(0.468673276007757,-3.06808388569787,
13.5941736642926));
#256796=CARTESIAN_POINT('Ctrl Pts',(-0.640290100382566,-3.03690993555533,
13.5412329507743));
#256797=CARTESIAN_POINT('Ctrl Pts',(-1.48223616652377,-2.54692109734721,
13.4882922372561));
#256798=CARTESIAN_POINT('Ctrl Pts',(-2.32418223266497,-2.05693225913909,
13.4353515237378));
#256799=CARTESIAN_POINT('Ctrl Pts',(-2.89911098855705,-1.10812853286539,
13.3824108102196));
#256800=CARTESIAN_POINT('Ctrl Pts',(-2.94373995623737,-0.135004442575269,
13.3294700967013));
#256801=CARTESIAN_POINT('Ctrl Pts',(-2.94578956203676,-0.0903132726320247,
13.3270387701641));
#256802=CARTESIAN_POINT('Ctrl Pts',(-2.9467206872412,-0.045570807448204,
13.3246074436268));
#256803=CARTESIAN_POINT('Ctrl Pts',(-2.9465548750618,-0.00082129130520664,
13.3221761170896));
#256804=CARTESIAN_POINT('Ctrl Pts',(-2.94672861832122,-0.000503025179204854,
13.1778238829104));
#256805=CARTESIAN_POINT('Ctrl Pts',(-2.94679265269451,-0.0275778920356812,
13.1792951439544));
#256806=CARTESIAN_POINT('Ctrl Pts',(-2.94645180088631,-0.0546511059983106,
13.1807664049985));
#256807=CARTESIAN_POINT('Ctrl Pts',(-2.94570111262815,-0.0817129512087959,
13.1822376660426));
#256808=CARTESIAN_POINT('Ctrl Pts',(-2.91868892999921,-1.05548534894355,
13.2351783795608));
#256809=CARTESIAN_POINT('Ctrl Pts',(-2.36102366680452,-2.01453757391699,
13.2881190930791));
#256810=CARTESIAN_POINT('Ctrl Pts',(-1.52808216906697,-2.51968191165344,
13.3410598065973));
#256811=CARTESIAN_POINT('Ctrl Pts',(-0.695140671329426,-3.02482624938989,
13.3940005201155));
#256812=CARTESIAN_POINT('Ctrl Pts',(0.413077060950985,-3.07606269988935,
13.4469412336338));
#256813=CARTESIAN_POINT('Ctrl Pts',(1.28907456375725,-2.64992807834628,
13.499881947152));
#256814=CARTESIAN_POINT('Ctrl Pts',(2.16507206656352,-2.22379345680322,
13.5528226606703));
#256815=CARTESIAN_POINT('Ctrl Pts',(2.80884933989565,-1.32028776321762,
13.6057633741885));
#256816=CARTESIAN_POINT('Ctrl Pts',(2.92559546319719,-0.35316177179018,
13.6587040877068));
#256817=CARTESIAN_POINT('Ctrl Pts',(3.04234158649873,0.613964219637249,
13.711644801225));
#256818=CARTESIAN_POINT('Ctrl Pts',(2.63205655976973,1.64471050890651,13.7645855147432));
#256819=CARTESIAN_POINT('Ctrl Pts',(1.88262602518954,2.26705785118355,13.8175262282615));
#256820=CARTESIAN_POINT('Ctrl Pts',(1.13319549060933,2.88940519346061,13.8704669417797));
#256821=CARTESIAN_POINT('Ctrl Pts',(0.0446194481779108,3.10335358874539,
13.923407655298));
#256822=CARTESIAN_POINT('Ctrl Pts',(-0.884600339990867,2.81092765645473,
13.9763483688162));
#256823=CARTESIAN_POINT('Ctrl Pts',(-1.81382012815963,2.51850172416407,
14.0292890823345));
#256824=CARTESIAN_POINT('Ctrl Pts',(-2.58368366206577,1.71970146429798,
14.0822297958527));
#256825=CARTESIAN_POINT('Ctrl Pts',(-2.84164016594338,0.780328916951795,
14.1351705093709));
#256826=CARTESIAN_POINT('Ctrl Pts',(-2.91091712618578,0.528050437297014,
14.1493883005507));
#256827=CARTESIAN_POINT('Ctrl Pts',(-2.94327288914735,0.265633208115812,
14.1636060917306));
#256828=CARTESIAN_POINT('Ctrl Pts',(-2.94096005475604,0.00265658997900563,
14.1778238829104));
#256829=CARTESIAN_POINT('Origin',(0.,0.,0.));
#256830=CARTESIAN_POINT('',(-2.9373430723748,-0.000745847102335828,15.3221761170896));
#256831=CARTESIAN_POINT('',(-2.93750327725234,-0.00102280351065573,15.1778238829104));
#256832=CARTESIAN_POINT('',(-2.942,-3.60291088309151E-16,0.));
#256833=CARTESIAN_POINT('Ctrl Pts',(-2.9373430723748,-0.000745847102335828,
15.3221761170896));
#256834=CARTESIAN_POINT('Ctrl Pts',(-2.93612524862381,0.536324027848074,
15.2932293391791));
#256835=CARTESIAN_POINT('Ctrl Pts',(-2.79536892737495,1.07398814293945,
15.2642825612686));
#256836=CARTESIAN_POINT('Ctrl Pts',(-2.51894932423377,1.52928919154174,
15.2353357833581));
#256837=CARTESIAN_POINT('Ctrl Pts',(-2.01340597616332,2.36198851487021,
15.1823950698399));
#256838=CARTESIAN_POINT('Ctrl Pts',(-1.05408671276304,2.91919416471434,
15.1294543563216));
#256839=CARTESIAN_POINT('Ctrl Pts',(-0.0803015358916538,2.94573977004452,
15.0765136428034));
#256840=CARTESIAN_POINT('Ctrl Pts',(0.893483640979715,2.97228537537469,
15.0235729292851));
#256841=CARTESIAN_POINT('Ctrl Pts',(1.88173473132218,2.46817093619092,14.9706322157669));
#256842=CARTESIAN_POINT('Ctrl Pts',(2.43189271238529,1.66425027111528,14.9176915022486));
#256843=CARTESIAN_POINT('Ctrl Pts',(2.9820506934484,0.860329606039647,14.8647507887304));
#256844=CARTESIAN_POINT('Ctrl Pts',(3.09411556523217,-0.243397284927852,
14.8118100752122));
#256845=CARTESIAN_POINT('Ctrl Pts',(2.71676841764234,-1.1414904705514,14.7588693616939));
#256846=CARTESIAN_POINT('Ctrl Pts',(2.33942127005251,-2.03958365617494,
14.7059286481757));
#256847=CARTESIAN_POINT('Ctrl Pts',(1.47266210308909,-2.73204313645453,
14.6529879346574));
#256848=CARTESIAN_POINT('Ctrl Pts',(0.513414011892879,-2.90176449455486,
14.6000472211392));
#256849=CARTESIAN_POINT('Ctrl Pts',(-0.445834079303328,-3.07148585265519,
14.5471065076209));
#256850=CARTESIAN_POINT('Ctrl Pts',(-1.49757109473232,-2.71846908857627,
14.4941657941027));
#256851=CARTESIAN_POINT('Ctrl Pts',(-2.16016531089828,-2.00437445579772,
14.4412250805845));
#256852=CARTESIAN_POINT('Ctrl Pts',(-2.65682877593363,-1.46910761219142,
14.4015420927528));
#256853=CARTESIAN_POINT('Ctrl Pts',(-2.93484794810006,-0.730965075081445,
14.3618591049212));
#256854=CARTESIAN_POINT('Ctrl Pts',(-2.94148383545301,0.00269085865063343,
14.3221761170896));
#256855=CARTESIAN_POINT('Ctrl Pts',(-2.94096005475604,0.00265658997900563,
14.1778238829104));
#256856=CARTESIAN_POINT('Ctrl Pts',(-2.93466092534955,-0.713574435792997,
14.2165468052488));
#256857=CARTESIAN_POINT('Ctrl Pts',(-2.67119892907313,-1.43395486703575,
14.2552697275872));
#256858=CARTESIAN_POINT('Ctrl Pts',(-2.19608251629437,-1.9649563946714,
14.2939926499257));
#256859=CARTESIAN_POINT('Ctrl Pts',(-1.54651888891863,-2.69092432412216,
14.3469333634439));
#256860=CARTESIAN_POINT('Ctrl Pts',(-0.501342160318069,-3.06291534819738,
14.3998740769621));
#256861=CARTESIAN_POINT('Ctrl Pts',(0.460820159237994,-2.91058015388245,
14.4528147904804));
#256862=CARTESIAN_POINT('Ctrl Pts',(1.42298247879406,-2.75824495956752,
14.5057555039986));
#256863=CARTESIAN_POINT('Ctrl Pts',(2.3021303893056,-2.08158354686245,14.5586962175169));
#256864=CARTESIAN_POINT('Ctrl Pts',(2.69566750295422,-1.19046577642952,
14.6116369310351));
#256865=CARTESIAN_POINT('Ctrl Pts',(3.08920461660283,-0.299348005996613,
14.6645776445534));
#256866=CARTESIAN_POINT('Ctrl Pts',(2.9971309333885,0.806226122164165,14.7175183580716));
#256867=CARTESIAN_POINT('Ctrl Pts',(2.46161061230183,1.61997075428422,14.7704590715898));
#256868=CARTESIAN_POINT('Ctrl Pts',(1.92609029121516,2.43371538640428,14.8233997851081));
#256869=CARTESIAN_POINT('Ctrl Pts',(0.947123332256163,2.95563052248365,
14.8763404986263));
#256870=CARTESIAN_POINT('Ctrl Pts',(-0.0269828105523374,2.94671070505273,
14.9292812121446));
#256871=CARTESIAN_POINT('Ctrl Pts',(-1.00108895336087,2.93779088762181,
14.9822219256628));
#256872=CARTESIAN_POINT('Ctrl Pts',(-1.97033428001888,2.39803611668058,
15.0351626391811));
#256873=CARTESIAN_POINT('Ctrl Pts',(-2.49086325409589,1.57462131978578,
15.0881033526993));
#256874=CARTESIAN_POINT('Ctrl Pts',(-2.78491630854596,1.10946443483882,
15.118010196103));
#256875=CARTESIAN_POINT('Ctrl Pts',(-2.93577251133268,0.553784388822177,
15.1479170395067));
#256876=CARTESIAN_POINT('Ctrl Pts',(-2.93750327725234,-0.00102280351065573,
15.1778238829104));
#256877=CARTESIAN_POINT('Origin',(0.,0.,0.));
#256878=CARTESIAN_POINT('',(-2.94422130955314,-0.00232131633852328,16.3221761170896));
#256879=CARTESIAN_POINT('',(-2.94470991062246,-0.00214590136519504,16.1778238829104));
#256880=CARTESIAN_POINT('',(-2.942,-3.60291088309151E-16,0.));
#256881=CARTESIAN_POINT('Ctrl Pts',(-2.94422130955314,-0.00232131633852328,
16.3221761170896));
#256882=CARTESIAN_POINT('Ctrl Pts',(-2.93710180263276,0.82093065071311,
16.2775402869552));
#256883=CARTESIAN_POINT('Ctrl Pts',(-2.57625047085104,1.64965132391019,
16.2329044568209));
#256884=CARTESIAN_POINT('Ctrl Pts',(-1.96390383491667,2.19702363537515,
16.1882686266865));
#256885=CARTESIAN_POINT('Ctrl Pts',(-1.23762479565001,2.846239313494,16.1353279131683));
#256886=CARTESIAN_POINT('Ctrl Pts',(-0.157558464670802,3.09967235360161,
16.08238719965));
#256887=CARTESIAN_POINT('Ctrl Pts',(0.781690327783711,2.84126580276401,
16.0294464861318));
#256888=CARTESIAN_POINT('Ctrl Pts',(1.72093912023825,2.5828592519264,15.9765057726135));
#256889=CARTESIAN_POINT('Ctrl Pts',(2.51937037416811,1.81261311014359,15.9235650590953));
#256890=CARTESIAN_POINT('Ctrl Pts',(2.81135103154901,0.883253365066257,
15.870624345577));
#256891=CARTESIAN_POINT('Ctrl Pts',(3.10333168892991,-0.0461063800110671,
15.8176836320588));
#256892=CARTESIAN_POINT('Ctrl Pts',(2.88886174976182,-1.1345797283829,15.7647429185406));
#256893=CARTESIAN_POINT('Ctrl Pts',(2.26615543020662,-1.8837119459476,15.7118022050223));
#256894=CARTESIAN_POINT('Ctrl Pts',(1.64344911065142,-2.63284416351231,
15.6588614915041));
#256895=CARTESIAN_POINT('Ctrl Pts',(0.612506410709106,-3.0426352502699,
15.6059207779858));
#256896=CARTESIAN_POINT('Ctrl Pts',(-0.354563480687433,-2.92542575837948,
15.5529800644676));
#256897=CARTESIAN_POINT('Ctrl Pts',(-1.32163337208394,-2.80821626648906,
15.5000393509493));
#256898=CARTESIAN_POINT('Ctrl Pts',(-2.22483045493469,-2.16400619595065,
15.4470986374311));
#256899=CARTESIAN_POINT('Ctrl Pts',(-2.65054527998976,-1.28780466227508,
15.3941579239129));
#256900=CARTESIAN_POINT('Ctrl Pts',(-2.84348892243074,-0.890690196275744,
15.3701639883051));
#256901=CARTESIAN_POINT('Ctrl Pts',(-2.93835252443724,-0.445922164696833,
15.3461700526974));
#256902=CARTESIAN_POINT('Ctrl Pts',(-2.9373430723748,-0.000745847102335828,
15.3221761170896));
#256903=CARTESIAN_POINT('Ctrl Pts',(-2.93750327725234,-0.00102280351065573,
15.1778238829104));
#256904=CARTESIAN_POINT('Ctrl Pts',(-2.93883629113328,-0.428328241075983,
15.2008577530249));
#256905=CARTESIAN_POINT('Ctrl Pts',(-2.8517098208156,-0.855115911932468,
15.2238916231395));
#256906=CARTESIAN_POINT('Ctrl Pts',(-2.67341529622153,-1.23963006790708,
15.246925493254));
#256907=CARTESIAN_POINT('Ctrl Pts',(-2.26362574277417,-2.12339183585687,
15.2998662067723));
#256908=CARTESIAN_POINT('Ctrl Pts',(-1.37223401438344,-2.78384054890816,
15.3528069202905));
#256909=CARTESIAN_POINT('Ctrl Pts',(-0.407443424386039,-2.91853077888232,
15.4057476338088));
#256910=CARTESIAN_POINT('Ctrl Pts',(0.557347165611373,-3.05322100885648,
15.458688347327));
#256911=CARTESIAN_POINT('Ctrl Pts',(1.59553661721545,-2.6621527557535,15.5116290608453));
#256912=CARTESIAN_POINT('Ctrl Pts',(2.23169716897106,-1.92441154572027,
15.5645697743635));
#256913=CARTESIAN_POINT('Ctrl Pts',(2.86785772072666,-1.18667033568704,
15.6175104878818));
#256914=CARTESIAN_POINT('Ctrl Pts',(3.1019893726338,-0.102256168723561,
15.6704512014));
#256915=CARTESIAN_POINT('Ctrl Pts',(2.82687403748138,0.832235079492427,
15.7233919149182));
#256916=CARTESIAN_POINT('Ctrl Pts',(2.55175870232897,1.76672632770841,15.7763326284365));
#256917=CARTESIAN_POINT('Ctrl Pts',(1.767396380117,2.55129465717691,15.8292733419547));
#256918=CARTESIAN_POINT('Ctrl Pts',(0.832977411748055,2.82665538808933,
15.882214055473));
#256919=CARTESIAN_POINT('Ctrl Pts',(-0.10144155662088,3.10201611900175,
15.9351547689912));
#256920=CARTESIAN_POINT('Ctrl Pts',(-1.18591717114679,2.8681692513581,15.9880954825095));
#256921=CARTESIAN_POINT('Ctrl Pts',(-1.92382541687975,2.23220245864934,
16.0410361960277));
#256922=CARTESIAN_POINT('Ctrl Pts',(-2.55935873555268,1.68446757606307,
16.0866320916553));
#256923=CARTESIAN_POINT('Ctrl Pts',(-2.93781720471667,0.838450372262618,
16.1322279872828));
#256924=CARTESIAN_POINT('Ctrl Pts',(-2.94470991062246,-0.00214590136519504,
16.1778238829104));
#256925=CARTESIAN_POINT('Origin',(0.,0.,0.));
#256926=CARTESIAN_POINT('',(-2.94469029704704,0.00215372812720598,17.3221761170896));
#256927=CARTESIAN_POINT('',(-2.94420089479508,0.00232782532028453,17.1778238829104));
#256928=CARTESIAN_POINT('',(-2.942,-3.60291088309151E-16,0.));
#256929=CARTESIAN_POINT('Ctrl Pts',(-2.94469029704704,0.00215372812720598,
17.3221761170896));
#256930=CARTESIAN_POINT('Ctrl Pts',(-2.94580943424373,0.138289047385046,
17.3147919482496));
#256931=CARTESIAN_POINT('Ctrl Pts',(-2.93718614082346,0.274281837578631,
17.3074077794096));
#256932=CARTESIAN_POINT('Ctrl Pts',(-2.91833507980263,0.408841775241091,
17.3000236105696));
#256933=CARTESIAN_POINT('Ctrl Pts',(-2.78318261475982,1.37356769973914,
17.2470828970514));
#256934=CARTESIAN_POINT('Ctrl Pts',(-2.12230688623147,2.26464276139239,
17.1941421835331));
#256935=CARTESIAN_POINT('Ctrl Pts',(-1.23834891424648,2.67400878423888,
17.1412014700149));
#256936=CARTESIAN_POINT('Ctrl Pts',(-0.354390942261467,3.08337480708537,
17.0882607564966));
#256937=CARTESIAN_POINT('Ctrl Pts',(0.752649273180203,3.01103179112507,
17.0353200429784));
#256938=CARTESIAN_POINT('Ctrl Pts',(1.57581452271761,2.49010838265651,16.9823793294601));
#256939=CARTESIAN_POINT('Ctrl Pts',(2.398979772255,1.96918497418795,16.9294386159419));
#256940=CARTESIAN_POINT('Ctrl Pts',(2.93827005588813,0.999681173211149,
16.8764979024236));
#256941=CARTESIAN_POINT('Ctrl Pts',(2.94672314080267,0.0255709155095142,
16.8235571889054));
#256942=CARTESIAN_POINT('Ctrl Pts',(2.95517622571722,-0.948539342192135,
16.7706164753872));
#256943=CARTESIAN_POINT('Ctrl Pts',(2.43279211191319,-1.92725605661859,
16.7176757618689));
#256944=CARTESIAN_POINT('Ctrl Pts',(1.61879102661444,-2.46238638825894,
16.6647350483507));
#256945=CARTESIAN_POINT('Ctrl Pts',(0.804789941315737,-2.99751671989926,
16.6117943348324));
#256946=CARTESIAN_POINT('Ctrl Pts',(-0.300828115477698,-3.08906066875349,
16.5588536213142));
#256947=CARTESIAN_POINT('Ctrl Pts',(-1.19175717671114,-2.69509665274667,
16.5059129077959));
#256948=CARTESIAN_POINT('Ctrl Pts',(-2.08268623794463,-2.30113263673982,
16.4529721942777));
#256949=CARTESIAN_POINT('Ctrl Pts',(-2.75892630361815,-1.42166065587188,
16.4000314807595));
#256950=CARTESIAN_POINT('Ctrl Pts',(-2.91080046267782,-0.459425507372839,
16.3470907672412));
#256951=CARTESIAN_POINT('Ctrl Pts',(-2.93462517330586,-0.30847834090911,
16.3387858838573));
#256952=CARTESIAN_POINT('Ctrl Pts',(-2.94554595557286,-0.155494485994484,
16.3304810004735));
#256953=CARTESIAN_POINT('Ctrl Pts',(-2.94422130955314,-0.00232131633852328,
16.3221761170896));
#256954=CARTESIAN_POINT('Ctrl Pts',(-2.94470991062246,-0.00214590136519504,
16.1778238829104));
#256955=CARTESIAN_POINT('Ctrl Pts',(-2.94582022261338,-0.137553408211996,
16.1851687008011));
#256956=CARTESIAN_POINT('Ctrl Pts',(-2.93728899802496,-0.272820250601191,
16.1925135186917));
#256957=CARTESIAN_POINT('Ctrl Pts',(-2.91863767633933,-0.40667697945158,
16.1998583365824));
#256958=CARTESIAN_POINT('Ctrl Pts',(-2.78420081312597,-1.3715029070699,
16.2527990501007));
#256959=CARTESIAN_POINT('Ctrl Pts',(-2.12398620975921,-2.26306804453264,
16.3057397636189));
#256960=CARTESIAN_POINT('Ctrl Pts',(-1.24033208650932,-2.67308966694861,
16.3586804771372));
#256961=CARTESIAN_POINT('Ctrl Pts',(-0.356677963259429,-3.08311128936457,
16.4116211906554));
#256962=CARTESIAN_POINT('Ctrl Pts',(0.75041567987361,-3.01158939673377,
16.4645619041736));
#256963=CARTESIAN_POINT('Ctrl Pts',(1.57396714373767,-2.49127667662831,
16.5175026176919));
#256964=CARTESIAN_POINT('Ctrl Pts',(2.39751860760173,-1.97096395652286,
16.5704433312101));
#256965=CARTESIAN_POINT('Ctrl Pts',(2.9375278921968,-1.00186040894278,16.6233840447284));
#256966=CARTESIAN_POINT('Ctrl Pts',(2.94670351767431,-0.0277566414570051,
16.6763247582466));
#256967=CARTESIAN_POINT('Ctrl Pts',(2.95587914315182,0.946347126028773,
16.7292654717649));
#256968=CARTESIAN_POINT('Ctrl Pts',(2.43422110951174,1.92545111342022,16.7822061852831));
#256969=CARTESIAN_POINT('Ctrl Pts',(1.62061713784133,2.46118511093008,16.8351468988013));
#256970=CARTESIAN_POINT('Ctrl Pts',(0.807013166170923,2.99691910843993,
16.8880876123196));
#256971=CARTESIAN_POINT('Ctrl Pts',(-0.298536743529821,3.0892831160682,
16.9410283258378));
#256972=CARTESIAN_POINT('Ctrl Pts',(-1.18975782985886,2.6959800335232,16.9939690393561));
#256973=CARTESIAN_POINT('Ctrl Pts',(-2.08097891618788,2.30267695097821,
17.0469097528743));
#256974=CARTESIAN_POINT('Ctrl Pts',(-2.75787117914521,1.42370677825997,
17.0998504663926));
#256975=CARTESIAN_POINT('Ctrl Pts',(-2.91045903925934,0.461584491615014,
17.1527911799108));
#256976=CARTESIAN_POINT('Ctrl Pts',(-2.93450912805829,0.309939882325946,
17.161135414244));
#256977=CARTESIAN_POINT('Ctrl Pts',(-2.94553424156564,0.156229575660569,
17.1694796485772));
#256978=CARTESIAN_POINT('Ctrl Pts',(-2.94420089479508,0.00232782532028453,
17.1778238829104));
#256979=CARTESIAN_POINT('Origin',(0.,0.,0.));
#256980=CARTESIAN_POINT('',(-2.93749488437707,0.00100976365607033,18.3221761170896));
#256981=CARTESIAN_POINT('',(-2.93733769429065,0.000733981079946969,18.1778238829104));
#256982=CARTESIAN_POINT('',(-2.942,-3.60291088309151E-16,0.));
#256983=CARTESIAN_POINT('Ctrl Pts',(-2.93749488437707,0.00100976365607033,
18.3221761170896));
#256984=CARTESIAN_POINT('Ctrl Pts',(-2.93881592843739,0.429049291744892,
18.2991028960257));
#256985=CARTESIAN_POINT('Ctrl Pts',(-2.85138007834119,0.856575277742226,
18.2760296749618));
#256986=CARTESIAN_POINT('Ctrl Pts',(-2.6724955590887,1.24161440663228,18.252956453898));
#256987=CARTESIAN_POINT('Ctrl Pts',(-2.26205117161561,2.12507346765581,
18.2000157403797));
#256988=CARTESIAN_POINT('Ctrl Pts',(-1.37016861804769,2.7848573811066,18.1470750268615));
#256989=CARTESIAN_POINT('Ctrl Pts',(-0.405278145270705,2.91883112712434,
18.0941343133433));
#256990=CARTESIAN_POINT('Ctrl Pts',(0.559612327506269,3.05280487314207,
18.041193599825));
#256991=CARTESIAN_POINT('Ctrl Pts',(1.59751071949234,2.66096845172673,17.9882528863068));
#256992=CARTESIAN_POINT('Ctrl Pts',(2.23312369097767,1.92275603651289,17.9353121727885));
#256993=CARTESIAN_POINT('Ctrl Pts',(2.868736662463,1.18454362129903,17.8823714592703));
#256994=CARTESIAN_POINT('Ctrl Pts',(3.10206421344762,0.0999552122866541,
17.829430745752));
#256995=CARTESIAN_POINT('Ctrl Pts',(2.82625589217435,-0.834331884800715,
17.7764900322338));
#256996=CARTESIAN_POINT('Ctrl Pts',(2.55044757090108,-1.76861898188808,
17.7235493187155));
#256997=CARTESIAN_POINT('Ctrl Pts',(1.76550337736993,-2.55260476705042,
17.6706086051973));
#256998=CARTESIAN_POINT('Ctrl Pts',(0.830880425304543,-2.82727218825324,
17.6176678916791));
#256999=CARTESIAN_POINT('Ctrl Pts',(-0.103742526760801,-3.10193960945605,
17.5647271781608));
#257000=CARTESIAN_POINT('Ctrl Pts',(-1.18804423736035,-2.86728866669937,
17.5117864646426));
#257001=CARTESIAN_POINT('Ctrl Pts',(-1.9254804918815,-2.23077480164964,
17.4588457511243));
#257002=CARTESIAN_POINT('Ctrl Pts',(-2.5600591638307,-1.68304186787519,
17.4132892064461));
#257003=CARTESIAN_POINT('Ctrl Pts',(-2.93778579299154,-0.837731557330954,
17.3677326617678));
#257004=CARTESIAN_POINT('Ctrl Pts',(-2.94469029704704,0.00215372812720598,
17.3221761170896));
#257005=CARTESIAN_POINT('Ctrl Pts',(-2.94420089479508,0.00232782532028453,
17.1778238829104));
#257006=CARTESIAN_POINT('Ctrl Pts',(-2.93707470812229,-0.820213336819081,
17.2224203620954));
#257007=CARTESIAN_POINT('Ctrl Pts',(-2.57693403423976,-1.64822301115232,
17.2670168412805));
#257008=CARTESIAN_POINT('Ctrl Pts',(-1.96553303478957,-2.19556643676288,
17.3116133204655));
#257009=CARTESIAN_POINT('Ctrl Pts',(-1.23973571293473,-2.84532067792415,
17.3645540339838));
#257010=CARTESIAN_POINT('Ctrl Pts',(-0.159857611954115,-3.09955475967498,
17.417494747502));
#257011=CARTESIAN_POINT('Ctrl Pts',(0.779582647763551,-2.84184496923932,
17.4704354610203));
#257012=CARTESIAN_POINT('Ctrl Pts',(1.71902290748122,-2.58413517880367,
17.5233761745385));
#257013=CARTESIAN_POINT('Ctrl Pts',(2.51802532593593,-1.81448151618153,
17.5763168880567));
#257014=CARTESIAN_POINT('Ctrl Pts',(2.81069526295745,-0.88533852033729,
17.629257601575));
#257015=CARTESIAN_POINT('Ctrl Pts',(3.10336519997896,0.04380447550691,17.6821983150932));
#257016=CARTESIAN_POINT('Ctrl Pts',(2.88970265556732,1.13243680457316,17.7351390286115));
#257017=CARTESIAN_POINT('Ctrl Pts',(2.26755215323326,1.88203068350848,17.7880797421297));
#257018=CARTESIAN_POINT('Ctrl Pts',(1.64540165089919,2.63162456244383,17.841020455648));
#257019=CARTESIAN_POINT('Ctrl Pts',(0.614763190642608,3.0421799912482,17.8939611691662));
#257020=CARTESIAN_POINT('Ctrl Pts',(-0.352393448315245,2.92568796859441,
17.9469018826845));
#257021=CARTESIAN_POINT('Ctrl Pts',(-1.3195500872731,2.80919594594063,17.9998425962027));
#257022=CARTESIAN_POINT('Ctrl Pts',(-2.22322490493229,2.16565647182868,
18.052783309721));
#257023=CARTESIAN_POINT('Ctrl Pts',(-2.6495895134013,1.2897706743402,18.1057240232392));
#257024=CARTESIAN_POINT('Ctrl Pts',(-2.84314457022158,0.892148259314461,
18.1297573097963));
#257025=CARTESIAN_POINT('Ctrl Pts',(-2.93833306961704,0.446642711850341,
18.1537905963533));
#257026=CARTESIAN_POINT('Ctrl Pts',(-2.93733769429065,0.000733981079946969,
18.1778238829104));
#257027=CARTESIAN_POINT('Origin',(0.,0.,0.));
#257028=CARTESIAN_POINT('',(-2.94091171156293,-0.00284992947760021,19.3221761170896));
#257029=CARTESIAN_POINT('',(-2.94150036975487,-0.00272063203504856,19.1778238829104));
#257030=CARTESIAN_POINT('',(-2.942,-3.60291088309151E-16,0.));
#257031=CARTESIAN_POINT('Ctrl Pts',(-2.94091171156293,-0.00284992947760021,
19.3221761170896));
#257032=CARTESIAN_POINT('Ctrl Pts',(-2.9346113934442,0.714133551483545,
19.2834138438019));
#257033=CARTESIAN_POINT('Ctrl Pts',(-2.67062843555962,1.43542617849289,
19.2446515705141));
#257034=CARTESIAN_POINT('Ctrl Pts',(-2.19465495964654,1.96666920693444,
19.2058892972264));
#257035=CARTESIAN_POINT('Ctrl Pts',(-1.54458020155545,2.69222998012506,
19.1529485837081));
#257036=CARTESIAN_POINT('Ctrl Pts',(-0.499068228844468,3.06328110544936,
19.1000078701899));
#257037=CARTESIAN_POINT('Ctrl Pts',(0.462994989182175,2.91019309689085,
19.0470671566716));
#257038=CARTESIAN_POINT('Ctrl Pts',(1.42505820720882,2.75710508833233,18.9941264431534));
#257039=CARTESIAN_POINT('Ctrl Pts',(2.3036726705511,2.07987794589101,18.9411857296351));
#257040=CARTESIAN_POINT('Ctrl Pts',(2.69654122955538,1.18848907915869,18.8882450161169));
#257041=CARTESIAN_POINT('Ctrl Pts',(3.08940978855965,0.297100212426381,
18.8353043025987));
#257042=CARTESIAN_POINT('Ctrl Pts',(2.99653244322591,-0.808450378596954,
18.7823635890804));
#257043=CARTESIAN_POINT('Ctrl Pts',(2.46041260156092,-1.62180826741871,
18.7294228755622));
#257044=CARTESIAN_POINT('Ctrl Pts',(1.92429275989593,-2.43516615624046,
18.6764821620439));
#257045=CARTESIAN_POINT('Ctrl Pts',(0.944930421899721,-2.95633134286067,
18.6235414485257));
#257046=CARTESIAN_POINT('Ctrl Pts',(-0.0291708259686788,-2.9466833598546,
18.5706007350074));
#257047=CARTESIAN_POINT('Ctrl Pts',(-1.00327207383711,-2.93703537684853,
18.5176600214892));
#257048=CARTESIAN_POINT('Ctrl Pts',(-1.97211223157771,-2.39657422421615,
18.464719307971));
#257049=CARTESIAN_POINT('Ctrl Pts',(-2.49202919975888,-1.57277654360183,
18.4117785944527));
#257050=CARTESIAN_POINT('Ctrl Pts',(-2.78535006931415,-1.10801569369011,
18.3819111019984));
#257051=CARTESIAN_POINT('Ctrl Pts',(-2.93578483819868,-0.553072708833093,
18.352043609544));
#257052=CARTESIAN_POINT('Ctrl Pts',(-2.93749488437707,0.00100976365607033,
18.3221761170896));
#257053=CARTESIAN_POINT('Ctrl Pts',(-2.93733769429065,0.000733981079946969,
18.1778238829104));
#257054=CARTESIAN_POINT('Ctrl Pts',(-2.93614044898348,-0.535608563477325,
18.2067313098716));
#257055=CARTESIAN_POINT('Ctrl Pts',(-2.79578948618625,-1.07253441221167,
18.2356387368327));
#257056=CARTESIAN_POINT('Ctrl Pts',(-2.52008301984148,-1.52742092622991,
18.2645461637939));
#257057=CARTESIAN_POINT('Ctrl Pts',(-2.01515751853378,-2.36049460844656,
18.3174868773121));
#257058=CARTESIAN_POINT('Ctrl Pts',(-1.05625211663952,-2.91840985201485,
18.3704275908304));
#257059=CARTESIAN_POINT('Ctrl Pts',(-0.0824866903648528,-2.94567859855282,
18.4233683043486));
#257060=CARTESIAN_POINT('Ctrl Pts',(0.891278735909814,-2.97294734509078,
18.4763090178669));
#257061=CARTESIAN_POINT('Ctrl Pts',(1.87990418656487,-2.46956959459843,
18.5292497313851));
#257062=CARTESIAN_POINT('Ctrl Pts',(2.43065805451983,-1.66605557474753,
18.5821904449034));
#257063=CARTESIAN_POINT('Ctrl Pts',(2.9814119224748,-0.862541554896619,
18.6351311584216));
#257064=CARTESIAN_POINT('Ctrl Pts',(3.09429420772964,0.24110873431293,18.6880718719398));
#257065=CARTESIAN_POINT('Ctrl Pts',(2.71761387062628,1.13947853899825,18.7410125854581));
#257066=CARTESIAN_POINT('Ctrl Pts',(2.34093353352292,2.03784834368356,18.7939532989763));
#257067=CARTESIAN_POINT('Ctrl Pts',(1.47469057406145,2.73093766384468,18.8468940124946));
#257068=CARTESIAN_POINT('Ctrl Pts',(0.515567501623733,2.90137638253994,
18.8998347260128));
#257069=CARTESIAN_POINT('Ctrl Pts',(-0.443555570813993,3.0718151012352,
18.9527754395311));
#257070=CARTESIAN_POINT('Ctrl Pts',(-1.49555875622791,2.71960321846454,
19.0057161530493));
#257071=CARTESIAN_POINT('Ctrl Pts',(-2.15868043210128,2.00598899678199,
19.0586568665676));
#257072=CARTESIAN_POINT('Ctrl Pts',(-2.65623216708033,1.47055182586423,
19.0983792053485));
#257073=CARTESIAN_POINT('Ctrl Pts',(-2.93485286441541,0.731653736584941,
19.1381015441295));
#257074=CARTESIAN_POINT('Ctrl Pts',(-2.94150036975487,-0.00272063203504856,
19.1778238829104));
#257075=CARTESIAN_POINT('Origin',(0.,0.,-1.84858989190501));
#257076=CARTESIAN_POINT('',(-2.3708726553023,-0.00229752557382901,19.651410108095));
#257077=CARTESIAN_POINT('',(-2.37527958827657,0.000195494738070845,19.848589891905));
#257078=CARTESIAN_POINT('',(-2.37175,-1.78696459712734E-13,-1.84858989190501));
#257079=CARTESIAN_POINT('',(1.37999437319995,-1.9337199838065,20.));
#257080=CARTESIAN_POINT('Ctrl Pts',(-2.3708726553023,-0.00229752557382881,
19.651410108095));
#257081=CARTESIAN_POINT('Ctrl Pts',(-2.37273049371058,-0.21372168288164,
19.6655885483255));
#257082=CARTESIAN_POINT('Ctrl Pts',(-2.24995196766579,-1.21237978931051,
19.7327077020742));
#257083=CARTESIAN_POINT('Ctrl Pts',(-0.889177232511419,-2.62573507798409,
19.8489043327092));
#257084=CARTESIAN_POINT('Ctrl Pts',(0.784688072628902,-2.35371694544778,
19.9509225231137));
#257085=CARTESIAN_POINT('Ctrl Pts',(1.38000112159638,-1.93372602389037,
20.));
#257086=CARTESIAN_POINT('',(-1.37702479013097,-1.93106208855768,20.));
#257087=CARTESIAN_POINT('Origin',(0.,0.,20.));
#257088=CARTESIAN_POINT('Ctrl Pts',(-2.37527958827657,0.000195494738070906,
19.848589891905));
#257089=CARTESIAN_POINT('Ctrl Pts',(-2.372659361562,-0.7471422980956,19.8990599279367));
#257090=CARTESIAN_POINT('Ctrl Pts',(-1.98938888825762,-1.49439019245293,
19.9495299639683));
#257091=CARTESIAN_POINT('Ctrl Pts',(-1.37702479013087,-1.93106208855776,
20.));
#257092=CARTESIAN_POINT('Origin',(0.,0.,-1.84858989190501));
#257093=CARTESIAN_POINT('',(-2.36811811421527,0.0008140404320815,18.651410108095));
#257094=CARTESIAN_POINT('',(-2.37134721344871,-0.00219328994902151,18.848589891905));
#257095=CARTESIAN_POINT('',(-2.37175,-1.78696459712734E-13,-1.84858989190501));
#257096=CARTESIAN_POINT('Ctrl Pts',(-2.36811811421527,0.00081404043208156,
18.651410108095));
#257097=CARTESIAN_POINT('Ctrl Pts',(-2.36673952753151,-0.44587022337695,
18.6812776005494));
#257098=CARTESIAN_POINT('Ctrl Pts',(-2.03049975964963,-1.68623441444512,
18.764085806522));
#257099=CARTESIAN_POINT('Ctrl Pts',(-0.0277579527538448,-2.80345084765341,
18.8998347260128));
#257100=CARTESIAN_POINT('Ctrl Pts',(2.3408375181597,-1.54300876944143,19.0586568665676));
#257101=CARTESIAN_POINT('Ctrl Pts',(2.56546210394684,1.13077397793403,19.2174790071223));
#257102=CARTESIAN_POINT('Ctrl Pts',(0.440526155511663,2.76865311636215,
19.376301147677));
#257103=CARTESIAN_POINT('Ctrl Pts',(-1.86232031433183,1.95137526934819,
19.5209448480012));
#257104=CARTESIAN_POINT('Ctrl Pts',(-2.36579353242733,0.57571252574142,
19.6126478348072));
#257105=CARTESIAN_POINT('Ctrl Pts',(-2.3708726553023,-0.00229752557382881,
19.651410108095));
#257106=CARTESIAN_POINT('Ctrl Pts',(-2.37134721344871,-0.00219328994902172,
18.848589891905));
#257107=CARTESIAN_POINT('Ctrl Pts',(-2.37313052894926,-0.199202713470517,
18.8618082666423));
#257108=CARTESIAN_POINT('Ctrl Pts',(-2.26053546724123,-1.1832303613783,
18.9279673548978));
#257109=CARTESIAN_POINT('Ctrl Pts',(-0.891859856974616,-2.65783582951041,
19.0470671566717));
#257110=CARTESIAN_POINT('Ctrl Pts',(1.75022653268834,-2.19050141850195,
19.2058892972263));
#257111=CARTESIAN_POINT('Ctrl Pts',(2.78914078757823,0.284026632862494,
19.3647114377811));
#257112=CARTESIAN_POINT('Ctrl Pts',(1.2738787066253,2.49658300563447,19.5235335783358));
#257113=CARTESIAN_POINT('Ctrl Pts',(-1.4087466563893,2.42611756744335,19.6823557188906));
#257114=CARTESIAN_POINT('Ctrl Pts',(-2.35782611185151,0.857292191480967,
19.7907078234136));
#257115=CARTESIAN_POINT('Ctrl Pts',(-2.37540785715971,0.0367801854735495,
19.8461192144184));
#257116=CARTESIAN_POINT('Ctrl Pts',(-2.37527958827657,0.000195494738070906,
19.848589891905));
#257117=CARTESIAN_POINT('Origin',(0.,0.,-1.84858989190501));
#257118=CARTESIAN_POINT('',(-2.3739188348135,0.00173626943759396,17.651410108095));
#257119=CARTESIAN_POINT('',(-2.36799139239764,0.000591712993054244,17.848589891905));
#257120=CARTESIAN_POINT('',(-2.37175,-1.78696459712734E-13,-1.84858989190501));
#257121=CARTESIAN_POINT('Ctrl Pts',(-2.3739188348135,0.00173626943759402,
17.651410108095));
#257122=CARTESIAN_POINT('Ctrl Pts',(-2.36835263580136,-0.675353440210703,
17.6969666527732));
#257123=CARTESIAN_POINT('Ctrl Pts',(-1.70997175802821,-2.14873683783659,
17.7954639109697));
#257124=CARTESIAN_POINT('Ctrl Pts',(0.790496683980206,-2.68985677845362,
17.9469018826844));
#257125=CARTESIAN_POINT('Ctrl Pts',(2.68889035258062,-0.793781027985773,
18.1057240232392));
#257126=CARTESIAN_POINT('Ctrl Pts',(2.1245858464136,1.82930451831788,18.2645461637939));
#257127=CARTESIAN_POINT('Ctrl Pts',(-0.385579528698175,2.7769639668139,
18.4233683043486));
#257128=CARTESIAN_POINT('Ctrl Pts',(-2.13696248834435,1.48135133436157,
18.552322952449));
#257129=CARTESIAN_POINT('Ctrl Pts',(-2.36918309934445,0.345886355437064,
18.6283368870311));
#257130=CARTESIAN_POINT('Ctrl Pts',(-2.36811811421527,0.00081404043208156,
18.651410108095));
#257131=CARTESIAN_POINT('Ctrl Pts',(-2.36799139239764,0.000591712993054314,
17.848589891905));
#257132=CARTESIAN_POINT('Ctrl Pts',(-2.36702621001918,-0.431791166019004,
17.8774973188662));
#257133=CARTESIAN_POINT('Ctrl Pts',(-2.04666419464228,-1.65736627843879,
17.9593454593456));
#257134=CARTESIAN_POINT('Ctrl Pts',(-0.0784779302164847,-2.80250647364015,
18.0941343133432));
#257135=CARTESIAN_POINT('Ctrl Pts',(2.31252045107973,-1.58508344876221,
18.252956453898));
#257136=CARTESIAN_POINT('Ctrl Pts',(2.58552714046087,1.08410340382027,18.4117785944527));
#257137=CARTESIAN_POINT('Ctrl Pts',(0.490511770879417,2.76034534307135,
18.5706007350074));
#257138=CARTESIAN_POINT('Ctrl Pts',(-1.84201218548248,1.97941362568811,
18.7162045008249));
#257139=CARTESIAN_POINT('Ctrl Pts',(-2.36598819890465,0.589836760620223,
18.8088675531241));
#257140=CARTESIAN_POINT('Ctrl Pts',(-2.37134721344871,-0.00219328994902172,
18.848589891905));
#257141=CARTESIAN_POINT('Origin',(0.,0.,-1.84858989190501));
#257142=CARTESIAN_POINT('',(-2.37354075150668,-0.00187137390417786,16.651410108095));
#257143=CARTESIAN_POINT('',(-2.37352429375602,0.00187662124489854,16.848589891905));
#257144=CARTESIAN_POINT('',(-2.37175,-1.78696459712734E-13,-1.84858989190501));
#257145=CARTESIAN_POINT('Ctrl Pts',(-2.37354075150668,-0.0018713739041778,
16.651410108095));
#257146=CARTESIAN_POINT('Ctrl Pts',(-2.37460864042485,-0.125354876668123,
16.6597149914789));
#257147=CARTESIAN_POINT('Ctrl Pts',(-2.30968224051476,-1.03487680478001,
16.720960588381));
#257148=CARTESIAN_POINT('Ctrl Pts',(-1.13383368765599,-2.56410571101671,
16.8351468988013));
#257149=CARTESIAN_POINT('Ctrl Pts',(1.54011222621193,-2.34270595503943,
16.9939690393561));
#257150=CARTESIAN_POINT('Ctrl Pts',(2.80350228934723,0.0243280702232952,
17.1527911799108));
#257151=CARTESIAN_POINT('Ctrl Pts',(1.49922452231095,2.36908059228316,17.3116133204655));
#257152=CARTESIAN_POINT('Ctrl Pts',(-1.17816089336587,2.54404274194716,
17.4704354610202));
#257153=CARTESIAN_POINT('Ctrl Pts',(-2.31802811947121,1.00713161791457,
17.5837010568967));
#257154=CARTESIAN_POINT('Ctrl Pts',(-2.37482104883331,0.111484380739378,
17.644025939255));
#257155=CARTESIAN_POINT('Ctrl Pts',(-2.3739188348135,0.00173626943759402,
17.651410108095));
#257156=CARTESIAN_POINT('Ctrl Pts',(-2.37352429375602,0.00187662124489858,
16.848589891905));
#257157=CARTESIAN_POINT('Ctrl Pts',(-2.3677793810295,-0.661230789123494,
16.8931863710901));
#257158=CARTESIAN_POINT('Ctrl Pts',(-1.73278761746912,-2.12115842707006,
16.9907235637934));
#257159=CARTESIAN_POINT('Ctrl Pts',(0.741692248419004,-2.70372151075853,
17.1412014700149));
#257160=CARTESIAN_POINT('Ctrl Pts',(2.67408584390158,-0.842308110700031,
17.3000236105696));
#257161=CARTESIAN_POINT('Ctrl Pts',(2.15734130986859,1.79055768786866,17.4588457511243));
#257162=CARTESIAN_POINT('Ctrl Pts',(-0.33526586359856,2.78348920207669,
17.6176678916791));
#257163=CARTESIAN_POINT('Ctrl Pts',(-2.12301662194415,1.51036732196377,
17.7475826052726));
#257164=CARTESIAN_POINT('Ctrl Pts',(-2.36879383340052,0.360069630125928,
17.8245566053479));
#257165=CARTESIAN_POINT('Ctrl Pts',(-2.36799139239764,0.000591712993054314,
17.848589891905));
#257166=CARTESIAN_POINT('Origin',(0.,0.,-1.84858989190501));
#257167=CARTESIAN_POINT('',(-2.36799572804382,-0.000601279016031824,15.651410108095));
#257168=CARTESIAN_POINT('',(-2.37393464667533,-0.00172995974292794,15.848589891905));
#257169=CARTESIAN_POINT('',(-2.37175,-1.78696459712734E-13,-1.84858989190501));
#257170=CARTESIAN_POINT('Ctrl Pts',(-2.36799572804382,-0.000601279016032089,
15.651410108095));
#257171=CARTESIAN_POINT('Ctrl Pts',(-2.36880951727872,-0.359488747151558,
15.6754040437027));
#257172=CARTESIAN_POINT('Ctrl Pts',(-2.12359490831044,-1.5091775280786,
15.7523386928287));
#257173=CARTESIAN_POINT('Ctrl Pts',(-0.33733047892205,-2.7832400288392,
15.882214055473));
#257174=CARTESIAN_POINT('Ctrl Pts',(2.15601250060359,-1.79215708184668,
16.0410361960277));
#257175=CARTESIAN_POINT('Ctrl Pts',(2.67470972516702,0.840324220669528,
16.1998583365824));
#257176=CARTESIAN_POINT('Ctrl Pts',(0.743697495552939,2.70317053621002,
16.3586804771371));
#257177=CARTESIAN_POINT('Ctrl Pts',(-1.7318608941197,2.12229113032217,16.509197734308));
#257178=CARTESIAN_POINT('Ctrl Pts',(-2.3678012237914,0.66180906554338,16.6067742779606));
#257179=CARTESIAN_POINT('Ctrl Pts',(-2.37354075150668,-0.0018713739041778,
16.651410108095));
#257180=CARTESIAN_POINT('Ctrl Pts',(-2.37393464667533,-0.00172995974292791,
15.848589891905));
#257181=CARTESIAN_POINT('Ctrl Pts',(-2.3748297460854,-0.110891331042623,
15.8559347097957));
#257182=CARTESIAN_POINT('Ctrl Pts',(-2.31837900116332,-1.00594618946061,
15.9162202412046));
#257183=CARTESIAN_POINT('Ctrl Pts',(-1.18004769118328,-2.54316833766063,
16.0294464861318));
#257184=CARTESIAN_POINT('Ctrl Pts',(1.49746693978282,-2.37019208118836,
16.1882686266865));
#257185=CARTESIAN_POINT('Ctrl Pts',(2.80348361626654,-0.0264075750974751,
16.3470907672412));
#257186=CARTESIAN_POINT('Ctrl Pts',(1.54184958368406,2.34156307285865,16.5059129077959));
#257187=CARTESIAN_POINT('Ctrl Pts',(-1.13193151590743,2.56494614739192,
16.6647350483507));
#257188=CARTESIAN_POINT('Ctrl Pts',(-2.30931972403911,1.03606308387966,
16.7789607097204));
#257189=CARTESIAN_POINT('Ctrl Pts',(-2.37459919695219,0.125947483369248,
16.8402456575718));
#257190=CARTESIAN_POINT('Ctrl Pts',(-2.37352429375602,0.00187662124489858,
16.848589891905));
#257191=CARTESIAN_POINT('Origin',(0.,0.,-1.84858989190501));
#257192=CARTESIAN_POINT('',(-2.37133388400261,0.00216928756102642,14.651410108095));
#257193=CARTESIAN_POINT('',(-2.36812488029342,-0.000824552762472563,14.848589891905));
#257194=CARTESIAN_POINT('',(-2.37175,-1.78696459712734E-13,-1.84858989190501));
#257195=CARTESIAN_POINT('Ctrl Pts',(-2.37133388400261,0.0021692875610264,
14.651410108095));
#257196=CARTESIAN_POINT('Ctrl Pts',(-2.36598423552219,-0.589281582877131,
14.6910930959266));
#257197=CARTESIAN_POINT('Ctrl Pts',(-1.84284323965632,-1.97822400345055,
14.7837167972765));
#257198=CARTESIAN_POINT('Ctrl Pts',(0.488460329284891,-2.7607287835619,
14.9292812121446));
#257199=CARTESIAN_POINT('Ctrl Pts',(2.58472415074527,-1.08601011698834,
15.0881033526993));
#257200=CARTESIAN_POINT('Ctrl Pts',(2.31369438223421,1.5833619975448,15.246925493254));
#257201=CARTESIAN_POINT('Ctrl Pts',(-0.0763986057193116,2.80256670978213,
15.4057476338088));
#257202=CARTESIAN_POINT('Ctrl Pts',(-2.04600918548686,1.65854908717202,
15.5405758387557));
#257203=CARTESIAN_POINT('Ctrl Pts',(-2.36701395595634,0.432367951410106,
15.6224633301845));
#257204=CARTESIAN_POINT('Ctrl Pts',(-2.36799572804382,-0.000601279016032089,
15.651410108095));
#257205=CARTESIAN_POINT('Ctrl Pts',(-2.36812488029342,-0.000824552762472806,
14.848589891905));
#257206=CARTESIAN_POINT('Ctrl Pts',(-2.36919951512415,-0.345305066544026,
14.8716237620196));
#257207=CARTESIAN_POINT('Ctrl Pts',(-2.13752525958051,-1.48015783356563,
14.9475983456523));
#257208=CARTESIAN_POINT('Ctrl Pts',(-0.387640275935778,-2.7766801689505,
15.0765136428034));
#257209=CARTESIAN_POINT('Ctrl Pts',(2.1232290291376,-1.8308785415232,15.2353357833581));
#257210=CARTESIAN_POINT('Ctrl Pts',(2.68947825967196,0.791785599022987,
15.3941579239129));
#257211=CARTESIAN_POINT('Ctrl Pts',(0.792491851405913,2.68927023744945,
15.5529800644676));
#257212=CARTESIAN_POINT('Ctrl Pts',(-1.70902747157913,2.14986441753538,
15.7044573871316));
#257213=CARTESIAN_POINT('Ctrl Pts',(-2.36837795896906,0.67593292672104,
15.8029939962775));
#257214=CARTESIAN_POINT('Ctrl Pts',(-2.37393464667533,-0.00172995974292791,
15.848589891905));
#257215=CARTESIAN_POINT('Origin',(0.,0.,-1.84858989190501));
#257216=CARTESIAN_POINT('',(-2.37542200031537,-0.00066209981418288,13.651410108095));
#257217=CARTESIAN_POINT('',(-2.37091162809913,0.0021416612107103,13.848589891905));
#257218=CARTESIAN_POINT('',(-2.37175,-1.78696459712734E-13,-1.84858989190501));
#257219=CARTESIAN_POINT('Ctrl Pts',(-2.37542200031537,-0.00066209981418278,
13.651410108095));
#257220=CARTESIAN_POINT('Ctrl Pts',(-2.37555567299943,-0.0367377846925378,
13.6538414346322));
#257221=CARTESIAN_POINT('Ctrl Pts',(-2.3584601828308,-0.858210955027421,
13.7092134746877));
#257222=CARTESIAN_POINT('Ctrl Pts',(-1.41019440296941,-2.42313199299893,
13.8175262282615));
#257223=CARTESIAN_POINT('Ctrl Pts',(1.27184219249669,-2.49852643513066,
13.9763483688162));
#257224=CARTESIAN_POINT('Ctrl Pts',(2.78902571499932,-0.285573932167581,
14.1351705093709));
#257225=CARTESIAN_POINT('Ctrl Pts',(1.75180021265799,2.18892962988587,14.2939926499257));
#257226=CARTESIAN_POINT('Ctrl Pts',(-0.889861652127881,2.65863934179406,
14.4528147904804));
#257227=CARTESIAN_POINT('Ctrl Pts',(-2.26011342652525,1.18439942316799,
14.5719539432035));
#257228=CARTESIAN_POINT('Ctrl Pts',(-2.37312115295459,0.199767649626288,
14.6381523824084));
#257229=CARTESIAN_POINT('Ctrl Pts',(-2.37133388400261,0.0021692875610264,
14.651410108095));
#257230=CARTESIAN_POINT('Ctrl Pts',(-2.37091162809913,0.0021416612107103,
13.848589891905));
#257231=CARTESIAN_POINT('Ctrl Pts',(-2.36583346352739,-0.575261783852008,
13.8873128142435));
#257232=CARTESIAN_POINT('Ctrl Pts',(-1.86305904372481,-1.94999080919174,
13.9789764501001));
#257233=CARTESIAN_POINT('Ctrl Pts',(0.438422718329072,-2.76911597159671,
14.123580799475));
#257234=CARTESIAN_POINT('Ctrl Pts',(2.56464881291346,-1.1326050549584,14.2824029400298));
#257235=CARTESIAN_POINT('Ctrl Pts',(2.34196789024492,1.54123461716797,14.4412250805845));
#257236=CARTESIAN_POINT('Ctrl Pts',(-0.0256713533761431,2.80349045400981,
14.6000472211392));
#257237=CARTESIAN_POINT('Ctrl Pts',(-2.02983150517857,1.68741078469057,
14.7358354915794));
#257238=CARTESIAN_POINT('Ctrl Pts',(-2.36672958999097,0.44644395791586,
14.8186830485013));
#257239=CARTESIAN_POINT('Ctrl Pts',(-2.36812488029342,-0.000824552762472806,
14.848589891905));
#257240=CARTESIAN_POINT('Origin',(0.,0.,-1.84858989190501));
#257241=CARTESIAN_POINT('',(-2.36937452646423,-0.00176685267772711,12.651410108095));
#257242=CARTESIAN_POINT('',(-2.37556206679244,-0.000405523443091083,12.848589891905));
#257243=CARTESIAN_POINT('',(-2.37175,-1.78696459712734E-13,-1.84858989190501));
#257244=CARTESIAN_POINT('Ctrl Pts',(-2.36937452646423,-0.00176685267772737,
12.651410108095));
#257245=CARTESIAN_POINT('Ctrl Pts',(-2.37124528291158,-0.272405989378181,
12.6695304868561));
#257246=CARTESIAN_POINT('Ctrl Pts',(-2.20341674148091,-1.33149770622952,
12.7405915791355));
#257247=CARTESIAN_POINT('Ctrl Pts',(-0.642779497905573,-2.7289286225062,
12.8645933849331));
#257248=CARTESIAN_POINT('Ctrl Pts',(1.94480058344235,-2.01939783111293,
13.0234155254878));
#257249=CARTESIAN_POINT('Ctrl Pts',(2.7511793889647,0.539656260407611,13.1822376660426));
#257250=CARTESIAN_POINT('Ctrl Pts',(1.03781181052871,2.60445072051449,13.3410598065973));
#257251=CARTESIAN_POINT('Ctrl Pts',(-1.58528548982049,2.28879183148743,
13.4974506206148));
#257252=CARTESIAN_POINT('Ctrl Pts',(-2.37264502847528,0.748789156612332,
13.600900721114));
#257253=CARTESIAN_POINT('Ctrl Pts',(-2.37542200031537,-0.00066209981418278,
13.651410108095));
#257254=CARTESIAN_POINT('Ctrl Pts',(-2.37556206679244,-0.000405523443090844,
12.848589891905));
#257255=CARTESIAN_POINT('Ctrl Pts',(-2.37561368933657,-0.0222324491625394,
12.8500611529491));
#257256=CARTESIAN_POINT('Ctrl Pts',(-2.36545128211817,-0.829413219156352,
12.9044731275114));
#257257=CARTESIAN_POINT('Ctrl Pts',(-1.45381213248182,-2.39721672519321,
13.0118258155919));
#257258=CARTESIAN_POINT('Ctrl Pts',(1.22642111687513,-2.52113248128301,
13.1706479561466));
#257259=CARTESIAN_POINT('Ctrl Pts',(2.7834014853579,-0.335996897909497,
13.3294700967014));
#257260=CARTESIAN_POINT('Ctrl Pts',(1.79112394068293,2.15687106086799,13.4882922372561));
#257261=CARTESIAN_POINT('Ctrl Pts',(-0.841605728219187,2.6743069274723,
13.6471143778108));
#257262=CARTESIAN_POINT('Ctrl Pts',(-2.24956593291735,1.21342596888521,
13.7672135960271));
#257263=CARTESIAN_POINT('Ctrl Pts',(-2.37277616411804,0.214145330165912,
13.8343721007252));
#257264=CARTESIAN_POINT('Ctrl Pts',(-2.37091162809913,0.0021416612107103,
13.848589891905));
#257265=CARTESIAN_POINT('Origin',(0.,0.,-1.84858989190501));
#257266=CARTESIAN_POINT('',(-2.3690442531058,0.00160878581760178,11.651410108095));
#257267=CARTESIAN_POINT('',(-2.36971778769283,-0.00189546110360289,11.848589891905));
#257268=CARTESIAN_POINT('',(-2.37175,-1.78696459712734E-13,-1.84858989190501));
#257269=CARTESIAN_POINT('Ctrl Pts',(-2.3690442531058,0.00160878581760195,
11.651410108095));
#257270=CARTESIAN_POINT('Ctrl Pts',(-2.36589429483149,-0.503533084642829,
11.68521953908));
#257271=CARTESIAN_POINT('Ctrl Pts',(-1.96012607113578,-1.80427476842366,
11.7719696835832));
#257272=CARTESIAN_POINT('Ctrl Pts',(0.180442601226353,-2.79779509209019,
11.9116605416047));
#257273=CARTESIAN_POINT('Ctrl Pts',(2.44890812594382,-1.36494172049492,
12.0704826821594));
#257274=CARTESIAN_POINT('Ctrl Pts',(2.47447105414424,1.31803259135108,12.2293048227142));
#257275=CARTESIAN_POINT('Ctrl Pts',(0.233718846407313,2.79384903144306,
12.3881269632689));
#257276=CARTESIAN_POINT('Ctrl Pts',(-1.94101657279419,1.83440196303656,
12.5288287250625));
#257277=CARTESIAN_POINT('Ctrl Pts',(-2.36577965868557,0.518296522515291,
12.6165897733379));
#257278=CARTESIAN_POINT('Ctrl Pts',(-2.36937452646423,-0.00176685267772737,
12.651410108095));
#257279=CARTESIAN_POINT('Ctrl Pts',(-2.36971778769283,-0.00189546110360261,
11.848589891905));
#257280=CARTESIAN_POINT('Ctrl Pts',(-2.37163683174812,-0.258101966923812,
11.8657502051729));
#257281=CARTESIAN_POINT('Ctrl Pts',(-2.21526537220026,-1.30244339925312,
11.9358512319591));
#257282=CARTESIAN_POINT('Ctrl Pts',(-0.692056486524632,-2.71685030201456,
12.0588929722635));
#257283=CARTESIAN_POINT('Ctrl Pts',(1.90793957711943,-2.05426004053984,
12.2177151128183));
#257284=CARTESIAN_POINT('Ctrl Pts',(2.7604945725652,0.489783073345279,12.376537253373));
#257285=CARTESIAN_POINT('Ctrl Pts',(1.08477160654539,2.58524434159141,12.5353593939277));
#257286=CARTESIAN_POINT('Ctrl Pts',(-1.55974375400603,2.31545814114733,
12.6927102734384));
#257287=CARTESIAN_POINT('Ctrl Pts',(-2.37375614384427,0.763170675708133,
12.7971204394308));
#257288=CARTESIAN_POINT('Ctrl Pts',(-2.37556206679244,-0.000405523443090844,
12.848589891905));
#257289=CARTESIAN_POINT('Origin',(0.,0.,-1.84858989190501));
#257290=CARTESIAN_POINT('',(-2.37521155387067,0.000920058411076374,10.651410108095));
#257291=CARTESIAN_POINT('',(-2.36876326363149,0.00143919393907455,10.848589891905));
#257292=CARTESIAN_POINT('',(-2.37175,-1.78696459712734E-13,-1.84858989190501));
#257293=CARTESIAN_POINT('Ctrl Pts',(-2.37521155387066,0.00092005841107628,
10.651410108095));
#257294=CARTESIAN_POINT('Ctrl Pts',(-2.37157703832641,-0.733704863043044,
10.7009085913039));
#257295=CARTESIAN_POINT('Ctrl Pts',(-1.6116945446461,-2.26053349925102,
10.803347788031));
#257296=CARTESIAN_POINT('Ctrl Pts',(0.987998371084236,-2.62375229935987,
10.9587276982763));
#257297=CARTESIAN_POINT('Ctrl Pts',(2.74039735767968,-0.591979080444202,
11.1175498388311));
#257298=CARTESIAN_POINT('Ctrl Pts',(1.98292499225804,1.98197512212938,11.2763719793858));
#257299=CARTESIAN_POINT('Ctrl Pts',(-0.590665979948808,2.74068068366097,
11.4351941199405));
#257300=CARTESIAN_POINT('Ctrl Pts',(-2.19058404802704,1.36209190860851,
11.5602068295102));
#257301=CARTESIAN_POINT('Ctrl Pts',(-2.37082667712059,0.287446540597829,
11.6322788255617));
#257302=CARTESIAN_POINT('Ctrl Pts',(-2.3690442531058,0.00160878581760195,
11.651410108095));
#257303=CARTESIAN_POINT('Ctrl Pts',(-2.36876326363149,0.00143919393907441,
10.848589891905));
#257304=CARTESIAN_POINT('Ctrl Pts',(-2.36604542551571,-0.489504653257154,
10.8814392573968));
#257305=CARTESIAN_POINT('Ctrl Pts',(-1.97786935145004,-1.7756026914142,
10.9672293364069));
#257306=CARTESIAN_POINT('Ctrl Pts',(0.129784664299144,-2.80060237895531,
11.1059601289351));
#257307=CARTESIAN_POINT('Ctrl Pts',(2.42380752331122,-1.40903329770356,
11.2647822694899));
#257308=CARTESIAN_POINT('Ctrl Pts',(2.49791689112318,1.27303925671557,11.4236044100446));
#257309=CARTESIAN_POINT('Ctrl Pts',(0.28423758216529,2.78916237264563,11.5824265505993));
#257310=CARTESIAN_POINT('Ctrl Pts',(-1.92245898347911,1.86294887847699,
11.7240883778862));
#257311=CARTESIAN_POINT('Ctrl Pts',(-2.36571645255842,0.532312229738396,
11.8128094916547));
#257312=CARTESIAN_POINT('Ctrl Pts',(-2.36971778769283,-0.00189546110360261,
11.848589891905));
#257313=CARTESIAN_POINT('Origin',(0.,0.,-1.84858989190501));
#257314=CARTESIAN_POINT('',(-2.37178798974141,-0.00216870721807306,9.65141010809499));
#257315=CARTESIAN_POINT('',(-2.37495901083281,0.00114971299769069,9.84858989190502));
#257316=CARTESIAN_POINT('',(-2.37175,-1.78696459712734E-13,-1.84858989190501));
#257317=CARTESIAN_POINT('Ctrl Pts',(-2.37178798974141,-0.00216870721807308,
9.65141010809499));
#257318=CARTESIAN_POINT('Ctrl Pts',(-2.37346696852305,-0.184610939429616,
9.66365693000949));
#257319=CARTESIAN_POINT('Ctrl Pts',(-2.27088436585652,-1.15384864042565,
9.72884446544225));
#257320=CARTESIAN_POINT('Ctrl Pts',(-0.940357642981567,-2.64120132003364,
9.84697271439322));
#257321=CARTESIAN_POINT('Ctrl Pts',(1.70977446530886,-2.22191093148198,
10.005794854948));
#257322=CARTESIAN_POINT('Ctrl Pts',(2.79396069466933,0.232380176228921,
10.1646169955027));
#257323=CARTESIAN_POINT('Ctrl Pts',(1.3192180568126,2.47383924866609,10.3234391360574));
#257324=CARTESIAN_POINT('Ctrl Pts',(-1.36376819526984,2.44956184229582,
10.4822612766122));
#257325=CARTESIAN_POINT('Ctrl Pts',(-2.35080676320134,0.88855867422785,
10.591584933958));
#257326=CARTESIAN_POINT('Ctrl Pts',(-2.37546430584922,0.0520074454725471,
10.6479678777856));
#257327=CARTESIAN_POINT('Ctrl Pts',(-2.37521155387066,0.00092005841107628,
10.651410108095));
#257328=CARTESIAN_POINT('Ctrl Pts',(-2.37495901083282,0.0011497129976905,
9.84858989190502));
#257329=CARTESIAN_POINT('Ctrl Pts',(-2.37065689581574,-0.719429682383803,
9.89712830962069));
#257330=CARTESIAN_POINT('Ctrl Pts',(-1.6363171272997,-2.23353310922339,
9.99860744085461));
#257331=CARTESIAN_POINT('Ctrl Pts',(0.940357692895628,-2.6412014602278,
10.1530272856068));
#257332=CARTESIAN_POINT('Ctrl Pts',(2.7292364351563,-0.6414719207516,10.3118494261615));
#257333=CARTESIAN_POINT('Ctrl Pts',(2.01846587572594,1.94576803669588,10.4706715667162));
#257334=CARTESIAN_POINT('Ctrl Pts',(-0.540974425817324,2.75092064856641,
10.6294937072709));
#257335=CARTESIAN_POINT('Ctrl Pts',(-2.17805383277753,1.3911462339404,10.7554664823339));
#257336=CARTESIAN_POINT('Ctrl Pts',(-2.37042554936049,0.301710555281621,
10.8284985438786));
#257337=CARTESIAN_POINT('Ctrl Pts',(-2.36876326363149,0.00143919393907441,
10.848589891905));
#257338=CARTESIAN_POINT('Origin',(0.,0.,-1.84858989190501));
#257339=CARTESIAN_POINT('',(-2.3679044556045,0.000358786198520854,8.65141010809499));
#257340=CARTESIAN_POINT('',(-2.37222321442519,-0.00213950769743509,8.84858989190502));
#257341=CARTESIAN_POINT('',(-2.37175,-1.78696459712734E-13,-1.84858989190501));
#257342=CARTESIAN_POINT('Ctrl Pts',(-2.3679044556045,0.000358786198520929,
8.65141010809499));
#257343=CARTESIAN_POINT('Ctrl Pts',(-2.3673403064869,-0.417530117617411,
8.67934598223336));
#257344=CARTESIAN_POINT('Ctrl Pts',(-2.06263816549048,-1.62812080978298,
8.76022256988998));
#257345=CARTESIAN_POINT('Ctrl Pts',(-0.129784657410042,-2.80060223030017,
8.89403987106487));
#257346=CARTESIAN_POINT('Ctrl Pts',(2.28310507284784,-1.62715952997786,
9.05286201161958));
#257347=CARTESIAN_POINT('Ctrl Pts',(2.60494767815974,1.03656379625737,9.21168415217432));
#257348=CARTESIAN_POINT('Ctrl Pts',(0.540974397102402,2.75092050254836,
9.37050629272904));
#257349=CARTESIAN_POINT('Ctrl Pts',(-1.82110658553714,2.00785348454621,
9.51708161136926));
#257350=CARTESIAN_POINT('Ctrl Pts',(-2.36620905824215,0.604052602554313,
9.61071621649125));
#257351=CARTESIAN_POINT('Ctrl Pts',(-2.37178798974141,-0.00216870721807308,
9.65141010809499));
#257352=CARTESIAN_POINT('Ctrl Pts',(-2.37222321442519,-0.00213950769743516,
8.84858989190502));
#257353=CARTESIAN_POINT('Ctrl Pts',(-2.37377707132607,-0.170200548119919,
8.85987664832633));
#257354=CARTESIAN_POINT('Ctrl Pts',(-2.28079939028199,-1.12484813559341,
8.92410411826587));
#257355=CARTESIAN_POINT('Ctrl Pts',(-0.987998423526767,-2.62375243862793,
9.04127230172366));
#257356=CARTESIAN_POINT('Ctrl Pts',(1.66928728944139,-2.2524870009407,9.2000944422784));
#257357=CARTESIAN_POINT('Ctrl Pts',(2.79770846226761,0.181783124226867,
9.35891658283312));
#257358=CARTESIAN_POINT('Ctrl Pts',(1.36376826765814,2.44956197231794,9.51773872338785));
#257359=CARTESIAN_POINT('Ctrl Pts',(-1.31921812683648,2.4738393799767,9.67656086394259));
#257360=CARTESIAN_POINT('Ctrl Pts',(-2.34325744778466,0.917403587350583,
9.78684458678164));
#257361=CARTESIAN_POINT('Ctrl Pts',(-2.37534920037284,0.066504205315249,
9.84418759610245));
#257362=CARTESIAN_POINT('Ctrl Pts',(-2.37495901083282,0.0011497129976905,
9.84858989190502));
#257363=CARTESIAN_POINT('Origin',(0.,0.,-1.84858989190501));
#257364=CARTESIAN_POINT('',(-2.37310580416009,0.00199191559344375,7.65141010809498));
#257365=CARTESIAN_POINT('',(-2.36786103774315,0.000124229582373903,7.84858989190502));
#257366=CARTESIAN_POINT('',(-2.37175,-1.78696459712734E-13,-1.84858989190501));
#257367=CARTESIAN_POINT('Ctrl Pts',(-2.37310580416009,0.00199191559344367,
7.65141010809498));
#257368=CARTESIAN_POINT('Ctrl Pts',(-2.36727740979178,-0.64696574170308,
7.69503503445724));
#257369=CARTESIAN_POINT('Ctrl Pts',(-1.75543549519818,-2.09312447203823,
7.79160067433773));
#257370=CARTESIAN_POINT('Ctrl Pts',(0.692056449790645,-2.71685015780489,
7.94110702773648));
#257371=CARTESIAN_POINT('Ctrl Pts',(2.65821266877332,-0.891135409034062,
8.0999291682912));
#257372=CARTESIAN_POINT('Ctrl Pts',(2.18976873525401,1.75075120898583,8.25875130884594));
#257373=CARTESIAN_POINT('Ctrl Pts',(-0.284237567078199,2.78916222459769,
8.41757344940066));
#257374=CARTESIAN_POINT('Ctrl Pts',(-2.10854369594215,1.53971625412154,
8.54845971581703));
#257375=CARTESIAN_POINT('Ctrl Pts',(-2.36840941413925,0.37440274368431,
8.62640526871512));
#257376=CARTESIAN_POINT('Ctrl Pts',(-2.3679044556045,0.000358786198520929,
8.65141010809499));
#257377=CARTESIAN_POINT('Ctrl Pts',(-2.36786103774315,0.000124229582374076,
7.84858989190502));
#257378=CARTESIAN_POINT('Ctrl Pts',(-2.36767260749056,-0.403421717141786,
7.8755657005502));
#257379=CARTESIAN_POINT('Ctrl Pts',(-2.07805004637786,-1.59919064096749,
7.95548222271362));
#257380=CARTESIAN_POINT('Ctrl Pts',(-0.180442610804054,-2.79779524059636,
8.08833945839529));
#257381=CARTESIAN_POINT('Ctrl Pts',(2.25328656381482,-1.66820784239526,
8.24716159895002));
#257382=CARTESIAN_POINT('Ctrl Pts',(2.62327874841108,0.989255453476115,
8.40598373950475));
#257383=CARTESIAN_POINT('Ctrl Pts',(0.59066601130102,2.74068082913556,8.56480588005947));
#257384=CARTESIAN_POINT('Ctrl Pts',(-1.80003185686014,2.03589293233909,
8.71234126419291));
#257385=CARTESIAN_POINT('Ctrl Pts',(-2.36648868040425,0.618092479785756,
8.80693593480808));
#257386=CARTESIAN_POINT('Ctrl Pts',(-2.37222321442519,-0.00213950769743516,
8.84858989190502));
#257387=CARTESIAN_POINT('Origin',(0.,0.,-1.84858989190501));
#257388=CARTESIAN_POINT('',(-2.37430755786411,-0.00156154949053819,6.65141010809498));
#257389=CARTESIAN_POINT('',(-2.37267966097722,0.00207845467076861,6.84858989190502));
#257390=CARTESIAN_POINT('',(-2.37175,-1.78696459712734E-13,-1.84858989190501));
#257391=CARTESIAN_POINT('Ctrl Pts',(-2.37430755786411,-0.00156154949053798,
6.65141010809498));
#257392=CARTESIAN_POINT('Ctrl Pts',(-2.37502807860986,-0.0962444547289554,
6.65778337316287));
#257393=CARTESIAN_POINT('Ctrl Pts',(-2.3268869061531,-0.97668956233699,
6.717097351749));
#257394=CARTESIAN_POINT('Ctrl Pts',(-1.2264210517769,-2.5211323474621,6.82935204385337));
#257395=CARTESIAN_POINT('Ctrl Pts',(1.45381205531404,-2.39721659794956,
6.9881741844081));
#257396=CARTESIAN_POINT('Ctrl Pts',(2.80252978248238,-0.0777414172792658,
7.14699632496283));
#257397=CARTESIAN_POINT('Ctrl Pts',(1.58447039810697,2.31293546541706,7.30581846551756));
#257398=CARTESIAN_POINT('Ctrl Pts',(-1.08477154896619,2.58524420436732,
7.46464060607229));
#257399=CARTESIAN_POINT('Ctrl Pts',(-2.30021044509958,1.06535984256429,
7.57983782026477));
#257400=CARTESIAN_POINT('Ctrl Pts',(-2.37435041557663,0.140572124495619,
7.642094320939));
#257401=CARTESIAN_POINT('Ctrl Pts',(-2.37310580416009,0.00199191559344367,
7.65141010809498));
#257402=CARTESIAN_POINT('Ctrl Pts',(-2.37267966097722,0.00207845467076865,
6.84858989190502));
#257403=CARTESIAN_POINT('Ctrl Pts',(-2.36685601691948,-0.632891799205702,
6.89125475277407));
#257404=CARTESIAN_POINT('Ctrl Pts',(-1.77738326645305,-2.06530485168304,
6.98686032716137));
#257405=CARTESIAN_POINT('Ctrl Pts',(0.64277953202424,-2.72892876735691,
7.13540661506691));
#257406=CARTESIAN_POINT('Ctrl Pts',(2.64165171954015,-0.939092081080438,
7.29422875562163));
#257407=CARTESIAN_POINT('Ctrl Pts',(2.2210915738946,1.71083896509047,7.45305089617638));
#257408=CARTESIAN_POINT('Ctrl Pts',(-0.233718858813212,2.79384917973975,
7.61187303673109));
#257409=CARTESIAN_POINT('Ctrl Pts',(-2.09388126411793,1.56869887105715,
7.74371936864065));
#257410=CARTESIAN_POINT('Ctrl Pts',(-2.36804240667441,0.388547511213119,
7.82262498703196));
#257411=CARTESIAN_POINT('Ctrl Pts',(-2.36786103774315,0.000124229582374076,
7.84858989190502));
#257412=CARTESIAN_POINT('Origin',(0.,0.,-1.84858989190501));
#257413=CARTESIAN_POINT('',(-2.36829614019373,-0.00104083913653463,5.65141010809498));
#257414=CARTESIAN_POINT('',(-2.37464485901916,-0.00137191232029432,5.84858989190501));
#257415=CARTESIAN_POINT('',(-2.37175,-1.78696459712734E-13,-1.84858989190501));
#257416=CARTESIAN_POINT('Ctrl Pts',(-2.36829614019373,-0.00104083913653439,
5.65141010809498));
#257417=CARTESIAN_POINT('Ctrl Pts',(-2.3696008644205,-0.330931720072927,
5.67347242538674));
#257418=CARTESIAN_POINT('Ctrl Pts',(-2.15126520202627,-1.45077744645276,
5.74847545619674));
#257419=CARTESIAN_POINT('Ctrl Pts',(-0.438422695057549,-2.76911582461286,
5.876419200525));
#257420=CARTESIAN_POINT('Ctrl Pts',(2.08934525988381,-1.86945267248516,
6.03524134107972));
#257421=CARTESIAN_POINT('Ctrl Pts',(2.7035265601163,0.742402214710351,6.19406348163445));
#257422=CARTESIAN_POINT('Ctrl Pts',(0.841605683546825,2.67430678552092,
6.35288562218919));
#257423=CARTESIAN_POINT('Ctrl Pts',(-1.68547684272582,2.17763477532239,
6.50533449767602));
#257424=CARTESIAN_POINT('Ctrl Pts',(-2.36904293881439,0.690256735463098,
6.60484265964462));
#257425=CARTESIAN_POINT('Ctrl Pts',(-2.37430755786411,-0.00156154949053798,
6.65141010809498));
#257426=CARTESIAN_POINT('Ctrl Pts',(-2.37464485901916,-0.00137191232029429,
5.84858989190501));
#257427=CARTESIAN_POINT('Ctrl Pts',(-2.37519850445556,-0.0817618654996098,
5.8540030914797));
#257428=CARTESIAN_POINT('Ctrl Pts',(-2.33500878081015,-0.94779985711636,
5.91235700457263));
#257429=CARTESIAN_POINT('Ctrl Pts',(-1.2718422600056,-2.49852656775178,
6.02365163118381));
#257430=CARTESIAN_POINT('Ctrl Pts',(1.41019447782222,-2.42313212161802,
6.18247377173853));
#257431=CARTESIAN_POINT('Ctrl Pts',(2.80066424243723,-0.128442770255383,
6.34129591229326));
#257432=CARTESIAN_POINT('Ctrl Pts',(1.62606550375187,2.28388456836278,6.50011805284799));
#257433=CARTESIAN_POINT('Ctrl Pts',(-1.0378118656156,2.60445085875792,6.65894019340272));
#257434=CARTESIAN_POINT('Ctrl Pts',(-2.29091251569842,1.09432815490155,
6.7750974730884));
#257435=CARTESIAN_POINT('Ctrl Pts',(-2.37408228850253,0.155011351498428,
6.83831403925583));
#257436=CARTESIAN_POINT('Ctrl Pts',(-2.37267966097722,0.00207845467076865,
6.84858989190502));
#257437=CARTESIAN_POINT('Origin',(0.,0.,-1.84858989190501));
#257438=CARTESIAN_POINT('',(-2.37049761817908,0.00208654043934857,4.65141010809498));
#257439=CARTESIAN_POINT('',(-2.36850443708147,-0.00124249154027839,4.84858989190502));
#257440=CARTESIAN_POINT('',(-2.37175,-1.78696459712734E-13,-1.84858989190501));
#257441=CARTESIAN_POINT('Ctrl Pts',(-2.37049761817908,0.00208654043934844,
4.65141010809498));
#257442=CARTESIAN_POINT('Ctrl Pts',(-2.3657393662343,-0.561079367483094,
4.68916147761062));
#257443=CARTESIAN_POINT('Ctrl Pts',(-1.88309579984035,-1.9213324922744,
4.7798535606445));
#257444=CARTESIAN_POINT('Ctrl Pts',(0.387640255360107,-2.77668002156518,
4.92348635719661));
#257445=CARTESIAN_POINT('Ctrl Pts',(2.54347800477387,-1.17937973057141,
5.08230849775135));
#257446=CARTESIAN_POINT('Ctrl Pts',(2.36979862748696,1.49808924126962,5.24113063830607));
#257447=CARTESIAN_POINT('Ctrl Pts',(0.0256713520133373,2.80349030520137,
5.3999527788608));
#257448=CARTESIAN_POINT('Ctrl Pts',(-2.01307404072613,1.71657713684027,
5.53671260212377));
#257449=CARTESIAN_POINT('Ctrl Pts',(-2.36647004952937,0.460674093086885,
5.6205317118685));
#257450=CARTESIAN_POINT('Ctrl Pts',(-2.36829614019373,-0.00104083913653439,
5.65141010809498));
#257451=CARTESIAN_POINT('Ctrl Pts',(-2.36850443708147,-0.00124249154027849,
4.84858989190502));
#257452=CARTESIAN_POINT('Ctrl Pts',(-2.37000186470862,-0.316708460084333,
4.86969214370357));
#257453=CARTESIAN_POINT('Ctrl Pts',(-2.16449434554539,-1.42173458182854,
4.94373510902037));
#257454=CARTESIAN_POINT('Ctrl Pts',(-0.488460355212123,-2.76072893010059,
5.07071878785543));
#257455=CARTESIAN_POINT('Ctrl Pts',(2.05517397389945,-1.90695508103928,
5.22954092841014));
#257456=CARTESIAN_POINT('Ctrl Pts',(2.7165183985746,0.693358157305003,5.3883630689649));
#257457=CARTESIAN_POINT('Ctrl Pts',(0.889861699361338,2.65863948291391,
5.5471852095196));
#257458=CARTESIAN_POINT('Ctrl Pts',(-1.66176346574157,2.20493905396228,
5.70059415049967));
#257459=CARTESIAN_POINT('Ctrl Pts',(-2.36978389078125,0.704446258234449,
5.80106237796146));
#257460=CARTESIAN_POINT('Ctrl Pts',(-2.37464485901916,-0.00137191232029429,
5.84858989190501));
#257461=CARTESIAN_POINT('Origin',(0.,0.,-1.84858989190501));
#257462=CARTESIAN_POINT('',(-2.37563694907561,-0.000138612772022241,3.65141010809498));
#257463=CARTESIAN_POINT('',(-2.37010644407789,0.0020062719553457,3.84858989190501));
#257464=CARTESIAN_POINT('',(-2.37175,-1.78696459712734E-13,-1.84858989190501));
#257465=CARTESIAN_POINT('Ctrl Pts',(-2.37563694907561,-0.00013861277202187,
3.65141010809498));
#257466=CARTESIAN_POINT('Ctrl Pts',(-2.37564322066674,-0.0075514150958584,
3.65190981631625));
#257467=CARTESIAN_POINT('Ctrl Pts',(-2.37225376878547,-0.800294695141046,
3.70535023805575));
#257468=CARTESIAN_POINT('Ctrl Pts',(-1.49746686029714,-2.37019195537365,
3.81173137331351));
#257469=CARTESIAN_POINT('Ctrl Pts',(1.18004762854664,-2.54316820267302,
3.97055351386824));
#257470=CARTESIAN_POINT('Ctrl Pts',(2.77678172346816,-0.3869110620803,4.12937565442297));
#257471=CARTESIAN_POINT('Ctrl Pts',(1.83032080339732,2.12370964715592,4.2881977949777));
#257472=CARTESIAN_POINT('Ctrl Pts',(-0.792491809340816,2.68927009470421,
4.44701993553242));
#257473=CARTESIAN_POINT('Ctrl Pts',(-2.23857227461137,1.24280982655239,
4.56809070657152));
#257474=CARTESIAN_POINT('Ctrl Pts',(-2.37241211099266,0.2286775440434,4.63622076409237));
#257475=CARTESIAN_POINT('Ctrl Pts',(-2.37049761817908,0.00208654043934844,
4.65141010809498));
#257476=CARTESIAN_POINT('Ctrl Pts',(-2.37010644407789,0.00200627195534563,
3.84858989190501));
#257477=CARTESIAN_POINT('Ctrl Pts',(-2.36570137679432,-0.547067010809973,
3.88538119592745));
#257478=CARTESIAN_POINT('Ctrl Pts',(-1.90248361218273,-1.89293283173512,
3.97511321346813));
#257479=CARTESIAN_POINT('Ctrl Pts',(0.337330496827683,-2.7832401765723,
4.11778594452705));
#257480=CARTESIAN_POINT('Ctrl Pts',(2.5217198186729,-1.22521300196359,4.27660808508177));
#257481=CARTESIAN_POINT('Ctrl Pts',(2.39651987123609,1.45496056673479,4.43543022563651));
#257482=CARTESIAN_POINT('Ctrl Pts',(0.0763986097743705,2.80256685854148,
4.59425236619123));
#257483=CARTESIAN_POINT('Ctrl Pts',(-1.99612954492781,1.74535439643512,
4.73197225494741));
#257484=CARTESIAN_POINT('Ctrl Pts',(-2.36624516197471,0.474723356049453,
4.81675143018533));
#257485=CARTESIAN_POINT('Ctrl Pts',(-2.36850443708147,-0.00124249154027849,
4.84858989190502));
#257486=CARTESIAN_POINT('Origin',(0.,0.,-1.84858989190501));
#257487=CARTESIAN_POINT('',(-2.37009071158309,-0.00200244152909902,2.65141010809498));
#257488=CARTESIAN_POINT('',(-2.37563860010749,0.000127708837501365,2.84858989190502));
#257489=CARTESIAN_POINT('',(-2.37175,-1.78696459712734E-13,-1.84858989190501));
#257490=CARTESIAN_POINT('Ctrl Pts',(-2.37009071158308,-0.00200244152909895,
2.65141010809498));
#257491=CARTESIAN_POINT('Ctrl Pts',(-2.37202441399179,-0.243607466556911,
2.66759886854012));
#257492=CARTESIAN_POINT('Ctrl Pts',(-2.22692364558065,-1.27304507845961,
2.7367283425035));
#257493=CARTESIAN_POINT('Ctrl Pts',(-0.741692209042783,-2.70372136703395,
2.85879852998513));
#257494=CARTESIAN_POINT('Ctrl Pts',(1.87000128182168,-2.08885428573093,
3.01762067053986));
#257495=CARTESIAN_POINT('Ctrl Pts',(2.76900059871079,0.439149889804403,
3.17644281109459));
#257496=CARTESIAN_POINT('Ctrl Pts',(1.13193145582276,2.56494601121031,3.33526495164932));
#257497=CARTESIAN_POINT('Ctrl Pts',(-1.53343688177706,2.34226578732656,
3.49358738398278));
#257498=CARTESIAN_POINT('Ctrl Pts',(-2.37497878791394,0.77778496219778,
3.598969102798));
#257499=CARTESIAN_POINT('Ctrl Pts',(-2.37563694907561,-0.00013861277202187,
3.65141010809498));
#257500=CARTESIAN_POINT('Ctrl Pts',(-2.37563860010749,0.000127708837501165,
2.84858989190502));
#257501=CARTESIAN_POINT('Ctrl Pts',(-2.37503056579596,-0.778378305301327,
2.90107024815132));
#257502=CARTESIAN_POINT('Ctrl Pts',(-1.53236168511894,-2.34334782239945,
3.00649131791588));
#257503=CARTESIAN_POINT('Ctrl Pts',(1.13383374784398,-2.56410584709992,
3.16485310119866));
#257504=CARTESIAN_POINT('Ctrl Pts',(2.76932572019706,-0.437095872952947,
3.3236752417534));
#257505=CARTESIAN_POINT('Ctrl Pts',(1.86845146885275,2.09024085837316,3.48249738230812));
#257506=CARTESIAN_POINT('Ctrl Pts',(-0.743697535029044,2.70317067969047,
3.64131952286286));
#257507=CARTESIAN_POINT('Ctrl Pts',(-2.22738897388365,1.27185445710156,
3.76335035939515));
#257508=CARTESIAN_POINT('Ctrl Pts',(-2.37204003238928,0.243019998491892,
3.8324404824092));
#257509=CARTESIAN_POINT('Ctrl Pts',(-2.37010644407789,0.00200627195534563,
3.84858989190501));
#257510=CARTESIAN_POINT('Origin',(0.,0.,-1.84858989190501));
#257511=CARTESIAN_POINT('',(-2.36851313222558,0.00125322961359671,1.65141010809498));
#257512=CARTESIAN_POINT('',(-2.37048131180486,-0.00208369211671167,1.84858989190502));
#257513=CARTESIAN_POINT('',(-2.37175,-1.78696459712734E-13,-1.84858989190501));
#257514=CARTESIAN_POINT('Ctrl Pts',(-2.36851313222558,0.0012532296135967,
1.65141010809498));
#257515=CARTESIAN_POINT('Ctrl Pts',(-2.36623622912522,-0.475297325567596,
1.68328792076399));
#257516=CARTESIAN_POINT('Ctrl Pts',(-1.99542751577998,-1.74653730674971,
1.76810644695125));
#257517=CARTESIAN_POINT('Ctrl Pts',(0.078477925820518,-2.80250631776144,
1.90586568665675));
#257518=CARTESIAN_POINT('Ctrl Pts',(2.39759801404543,-1.4531840222644,2.06468782721148));
#257519=CARTESIAN_POINT('Ctrl Pts',(2.520810341052,1.22708388997517,2.22350996776621));
#257520=CARTESIAN_POINT('Ctrl Pts',(0.335265845793994,2.78348905308081,
2.38233210832094));
#257521=CARTESIAN_POINT('Ctrl Pts',(-1.90326945111716,1.89176722009415,
2.52496548843053));
#257522=CARTESIAN_POINT('Ctrl Pts',(-2.36570079300822,0.546492705590905,
2.61465815502187));
#257523=CARTESIAN_POINT('Ctrl Pts',(-2.37009071158308,-0.00200244152909895,
2.65141010809498));
#257524=CARTESIAN_POINT('Ctrl Pts',(-2.37048131180486,-0.00208369211671135,
1.84858989190502));
#257525=CARTESIAN_POINT('Ctrl Pts',(-2.37239723210793,-0.229265828060701,
1.86381858685695));
#257526=CARTESIAN_POINT('Ctrl Pts',(-2.23812046499434,-1.24400071348261,
1.93198799532714));
#257527=CARTESIAN_POINT('Ctrl Pts',(-0.79049672615424,-2.68985692246101,
2.05309811731556));
#257528=CARTESIAN_POINT('Ctrl Pts',(1.83189557733352,-2.12235175091147,
2.21192025787029));
#257529=CARTESIAN_POINT('Ctrl Pts',(2.77649415671547,0.388970759351873,
2.37074239842502));
#257530=CARTESIAN_POINT('Ctrl Pts',(1.17816095594432,2.54404287719204,2.52956453897975));
#257531=CARTESIAN_POINT('Ctrl Pts',(-1.49922460191346,2.36908071791899,
2.68838667953448));
#257532=CARTESIAN_POINT('Ctrl Pts',(-2.37252370148548,0.799115854689114,
2.7947284638429));
#257533=CARTESIAN_POINT('Ctrl Pts',(-2.37564393377968,0.00695675746614235,
2.84812953463308));
#257534=CARTESIAN_POINT('Ctrl Pts',(-2.37563860010749,0.000127708837501165,
2.84858989190502));
#257535=CARTESIAN_POINT('Origin',(0.,0.,-1.84858989190501));
#257536=CARTESIAN_POINT('',(-2.37462805812147,0.00152502885334134,0.651410108094979));
#257537=CARTESIAN_POINT('',(-2.36829764012707,0.00106700769158252,0.848589891905016));
#257538=CARTESIAN_POINT('',(-2.37175,-1.78696459712734E-13,-1.84858989190501));
#257539=CARTESIAN_POINT('Ctrl Pts',(-2.37462805812147,0.00152502885334119,
0.651410108094978));
#257540=CARTESIAN_POINT('Ctrl Pts',(-2.36977823922653,-0.704823399369114,
0.698976972987868));
#257541=CARTESIAN_POINT('Ctrl Pts',(-1.66082968322975,-2.20631416213666,
0.799484551399001));
#257542=CARTESIAN_POINT('Ctrl Pts',(0.891859770330893,-2.65783549575534,
0.952932843328373));
#257543=CARTESIAN_POINT('Ctrl Pts',(2.71701801755088,-0.691417882516756,
1.11175498388311));
#257544=CARTESIAN_POINT('Ctrl Pts',(2.05376604018409,1.90851811654588,1.27057712443783));
#257545=CARTESIAN_POINT('Ctrl Pts',(-0.490511741217893,2.76034515792448,
1.42939926499256));
#257546=CARTESIAN_POINT('Ctrl Pts',(-2.16502830177281,1.42054841044669,
1.55634359287828));
#257547=CARTESIAN_POINT('Ctrl Pts',(-2.37001756995926,0.316128569325436,
1.63034720724575));
#257548=CARTESIAN_POINT('Ctrl Pts',(-2.36851313222558,0.0012532296135967,
1.65141010809498));
#257549=CARTESIAN_POINT('Ctrl Pts',(-2.36829764012707,0.00106700769158283,
0.848589891905016));
#257550=CARTESIAN_POINT('Ctrl Pts',(-2.36645677222522,-0.461240440100845,
0.879507639080828));
#257551=CARTESIAN_POINT('Ctrl Pts',(-2.01239790937726,-1.71778716938983,
0.963366099774883));
#257552=CARTESIAN_POINT('Ctrl Pts',(0.0277579514215299,-2.80345103515647,
1.10016527398718));
#257553=CARTESIAN_POINT('Ctrl Pts',(2.37090557643909,-1.49634138211991,
1.25898741454191));
#257554=CARTESIAN_POINT('Ctrl Pts',(2.54260459056719,1.18127146424035,1.41780955509664));
#257555=CARTESIAN_POINT('Ctrl Pts',(0.385579550113745,2.77696412127707,
1.57663169565137));
#257556=CARTESIAN_POINT('Ctrl Pts',(-1.88389820241982,1.92017114645465,
1.72022514125416));
#257557=CARTESIAN_POINT('Ctrl Pts',(-2.36573676722839,0.560505351507294,
1.81087787333871));
#257558=CARTESIAN_POINT('Ctrl Pts',(-2.37048131180486,-0.00208369211671135,
1.84858989190502));
#257559=CARTESIAN_POINT('Ctrl Pts',(-1.03908919352509,2.13201587949044,
-0.329233991005384));
#257560=CARTESIAN_POINT('Ctrl Pts',(-1.74827509563859,1.7863770809358,-0.276293277487141));
#257561=CARTESIAN_POINT('Ctrl Pts',(-2.78233718465057,0.337749170168978,
-0.170411850450654));
#257562=CARTESIAN_POINT('Ctrl Pts',(-1.79018921372264,-2.16005466875641,
-0.0115897098959247));
#257563=CARTESIAN_POINT('Ctrl Pts',(0.843935273622217,-2.67272649501447,
0.147232430658805));
#257564=CARTESIAN_POINT('Ctrl Pts',(2.70389566823784,-0.740895185834261,
0.306054571213535));
#257565=CARTESIAN_POINT('Ctrl Pts',(2.08805286496322,1.8712628391822,0.464876711768264));
#257566=CARTESIAN_POINT('Ctrl Pts',(-0.440526185828228,2.76865345984501,
0.623698852322994));
#257567=CARTESIAN_POINT('Ctrl Pts',(-2.56546224110779,1.13077392232151,
0.782520992877724));
#257568=CARTESIAN_POINT('Ctrl Pts',(-2.34083763947357,-1.54300878412073,
0.941343133432452));
#257569=CARTESIAN_POINT('Ctrl Pts',(0.0277579514215299,-2.80345103515647,
1.10016527398718));
#257570=CARTESIAN_POINT('Ctrl Pts',(2.37090557643909,-1.49634138211991,
1.25898741454191));
#257571=CARTESIAN_POINT('Ctrl Pts',(2.54260459056719,1.18127146424035,1.41780955509664));
#257572=CARTESIAN_POINT('Ctrl Pts',(0.385579550113745,2.77696412127707,
1.57663169565137));
#257573=CARTESIAN_POINT('Ctrl Pts',(-2.12458595977851,1.82930461145536,
1.7354538362061));
#257574=CARTESIAN_POINT('Ctrl Pts',(-2.68889049494592,-0.793781067907386,
1.89427597676083));
#257575=CARTESIAN_POINT('Ctrl Pts',(-0.79049672615424,-2.68985692246101,
2.05309811731556));
#257576=CARTESIAN_POINT('Ctrl Pts',(1.83189557733352,-2.12235175091147,
2.21192025787029));
#257577=CARTESIAN_POINT('Ctrl Pts',(2.77649415671547,0.388970759351873,
2.37074239842502));
#257578=CARTESIAN_POINT('Ctrl Pts',(1.17816095594432,2.54404287719204,2.52956453897975));
#257579=CARTESIAN_POINT('Ctrl Pts',(-1.49922460191346,2.36908071791899,
2.68838667953448));
#257580=CARTESIAN_POINT('Ctrl Pts',(-2.80350243814271,0.024328071577183,
2.84720882008921));
#257581=CARTESIAN_POINT('Ctrl Pts',(-1.54011230796823,-2.34270607942395,
3.00603096064394));
#257582=CARTESIAN_POINT('Ctrl Pts',(1.13383374784398,-2.56410584709992,
3.16485310119866));
#257583=CARTESIAN_POINT('Ctrl Pts',(2.76932572019706,-0.437095872952947,
3.3236752417534));
#257584=CARTESIAN_POINT('Ctrl Pts',(1.86845146885275,2.09024085837316,3.48249738230812));
#257585=CARTESIAN_POINT('Ctrl Pts',(-0.743697535029044,2.70317067969047,
3.64131952286286));
#257586=CARTESIAN_POINT('Ctrl Pts',(-2.67470986713947,0.840324265275232,
3.80014166341758));
#257587=CARTESIAN_POINT('Ctrl Pts',(-2.15601261504427,-1.79215717697482,
3.95896380397232));
#257588=CARTESIAN_POINT('Ctrl Pts',(0.337330496827683,-2.7832401765723,
4.11778594452705));
#257589=CARTESIAN_POINT('Ctrl Pts',(2.5217198186729,-1.22521300196359,4.27660808508177));
#257590=CARTESIAN_POINT('Ctrl Pts',(2.39651987123609,1.45496056673479,4.43543022563651));
#257591=CARTESIAN_POINT('Ctrl Pts',(0.0763986097743705,2.80256685854148,
4.59425236619123));
#257592=CARTESIAN_POINT('Ctrl Pts',(-2.31369450504449,1.58336208158914,
4.75307450674597));
#257593=CARTESIAN_POINT('Ctrl Pts',(-2.58472428794165,-1.08601017463356,
4.91189664730069));
#257594=CARTESIAN_POINT('Ctrl Pts',(-0.488460355212123,-2.76072893010059,
5.07071878785543));
#257595=CARTESIAN_POINT('Ctrl Pts',(2.05517397389945,-1.90695508103928,
5.22954092841014));
#257596=CARTESIAN_POINT('Ctrl Pts',(2.7165183985746,0.693358157305003,5.3883630689649));
#257597=CARTESIAN_POINT('Ctrl Pts',(0.889861699361338,2.65863948291391,
5.5471852095196));
#257598=CARTESIAN_POINT('Ctrl Pts',(-1.75180030564315,2.18892974607354,
5.70600735007435));
#257599=CARTESIAN_POINT('Ctrl Pts',(-2.78902586303999,-0.285573947325892,
5.86482949062906));
#257600=CARTESIAN_POINT('Ctrl Pts',(-1.2718422600056,-2.49852656775178,
6.02365163118381));
#257601=CARTESIAN_POINT('Ctrl Pts',(1.41019447782222,-2.42313212161802,
6.18247377173853));
#257602=CARTESIAN_POINT('Ctrl Pts',(2.80066424243723,-0.128442770255383,
6.34129591229326));
#257603=CARTESIAN_POINT('Ctrl Pts',(1.62606550375187,2.28388456836278,6.50011805284799));
#257604=CARTESIAN_POINT('Ctrl Pts',(-1.0378118656156,2.60445085875792,6.65894019340272));
#257605=CARTESIAN_POINT('Ctrl Pts',(-2.75117953499654,0.539656289052272,
6.81776233395745));
#257606=CARTESIAN_POINT('Ctrl Pts',(-1.94480068667171,-2.01939793830208,
6.97658447451218));
#257607=CARTESIAN_POINT('Ctrl Pts',(0.64277953202424,-2.72892876735691,
7.13540661506691));
#257608=CARTESIAN_POINT('Ctrl Pts',(2.64165171954015,-0.939092081080438,
7.29422875562163));
#257609=CARTESIAN_POINT('Ctrl Pts',(2.2210915738946,1.71083896509047,7.45305089617638));
#257610=CARTESIAN_POINT('Ctrl Pts',(-0.233718858813212,2.79384917973975,
7.61187303673109));
#257611=CARTESIAN_POINT('Ctrl Pts',(-2.47447118548852,1.31803266131172,
7.77069517728583));
#257612=CARTESIAN_POINT('Ctrl Pts',(-2.44890825593109,-1.36494179294576,
7.92951731784055));
#257613=CARTESIAN_POINT('Ctrl Pts',(-0.180442610804054,-2.79779524059636,
8.08833945839529));
#257614=CARTESIAN_POINT('Ctrl Pts',(2.25328656381482,-1.66820784239526,
8.24716159895002));
#257615=CARTESIAN_POINT('Ctrl Pts',(2.62327874841108,0.989255453476115,
8.40598373950475));
#257616=CARTESIAN_POINT('Ctrl Pts',(0.59066601130102,2.74068082913556,8.56480588005947));
#257617=CARTESIAN_POINT('Ctrl Pts',(-1.98292509751125,1.98197522733192,
8.72362802061421));
#257618=CARTESIAN_POINT('Ctrl Pts',(-2.74039750313914,-0.591979111866446,
8.88245016116893));
#257619=CARTESIAN_POINT('Ctrl Pts',(-0.987998423526767,-2.62375243862793,
9.04127230172366));
#257620=CARTESIAN_POINT('Ctrl Pts',(1.66928728944139,-2.2524870009407,9.2000944422784));
#257621=CARTESIAN_POINT('Ctrl Pts',(2.79770846226761,0.181783124226867,
9.35891658283312));
#257622=CARTESIAN_POINT('Ctrl Pts',(1.36376826765814,2.44956197231794,9.51773872338785));
#257623=CARTESIAN_POINT('Ctrl Pts',(-1.31921812683648,2.4738393799767,9.67656086394259));
#257624=CARTESIAN_POINT('Ctrl Pts',(-2.79396084297197,0.23238018856341,
9.83538300449731));
#257625=CARTESIAN_POINT('Ctrl Pts',(-1.70977455606306,-2.22191104942047,
9.99420514505205));
#257626=CARTESIAN_POINT('Ctrl Pts',(0.940357692895628,-2.6412014602278,
10.1530272856068));
#257627=CARTESIAN_POINT('Ctrl Pts',(2.7292364351563,-0.6414719207516,10.3118494261615));
#257628=CARTESIAN_POINT('Ctrl Pts',(2.01846587572594,1.94576803669588,10.4706715667162));
#257629=CARTESIAN_POINT('Ctrl Pts',(-0.540974425817324,2.75092064856641,
10.6294937072709));
#257630=CARTESIAN_POINT('Ctrl Pts',(-2.60494781642969,1.0365638512777,10.7883158478257));
#257631=CARTESIAN_POINT('Ctrl Pts',(-2.28310519403429,-1.62715961634717,
10.9471379883804));
#257632=CARTESIAN_POINT('Ctrl Pts',(0.129784664299144,-2.80060237895531,
11.1059601289351));
#257633=CARTESIAN_POINT('Ctrl Pts',(2.42380752331122,-1.40903329770356,
11.2647822694899));
#257634=CARTESIAN_POINT('Ctrl Pts',(2.49791689112318,1.27303925671557,11.4236044100446));
#257635=CARTESIAN_POINT('Ctrl Pts',(0.28423758216529,2.78916237264563,11.5824265505993));
#257636=CARTESIAN_POINT('Ctrl Pts',(-2.18976885148641,1.75075130191508,
11.7412486911541));
#257637=CARTESIAN_POINT('Ctrl Pts',(-2.65821280987044,-0.891135456335437,
11.9000708317088));
#257638=CARTESIAN_POINT('Ctrl Pts',(-0.692056486524632,-2.71685030201456,
12.0588929722635));
#257639=CARTESIAN_POINT('Ctrl Pts',(1.90793957711943,-2.05426004053984,
12.2177151128183));
#257640=CARTESIAN_POINT('Ctrl Pts',(2.7604945725652,0.489783073345279,12.376537253373));
#257641=CARTESIAN_POINT('Ctrl Pts',(1.08477160654539,2.58524434159141,12.5353593939277));
#257642=CARTESIAN_POINT('Ctrl Pts',(-1.58447048221035,2.31293558818691,
12.6941815344825));
#257643=CARTESIAN_POINT('Ctrl Pts',(-2.80252993123984,-0.0777414214059339,
12.8530036750372));
#257644=CARTESIAN_POINT('Ctrl Pts',(-1.45381213248182,-2.39721672519321,
13.0118258155919));
#257645=CARTESIAN_POINT('Ctrl Pts',(1.22642111687513,-2.52113248128301,
13.1706479561466));
#257646=CARTESIAN_POINT('Ctrl Pts',(2.7834014853579,-0.335996897909497,
13.3294700967014));
#257647=CARTESIAN_POINT('Ctrl Pts',(1.79112394068293,2.15687106086799,13.4882922372561));
#257648=CARTESIAN_POINT('Ctrl Pts',(-0.841605728219187,2.6743069274723,
13.6471143778108));
#257649=CARTESIAN_POINT('Ctrl Pts',(-2.70352670361876,0.742402254116675,
13.8059365183655));
#257650=CARTESIAN_POINT('Ctrl Pts',(-2.08934537078553,-1.8694527717153,
13.9647586589203));
#257651=CARTESIAN_POINT('Ctrl Pts',(0.438422718329072,-2.76911597159671,
14.123580799475));
#257652=CARTESIAN_POINT('Ctrl Pts',(2.56464881291346,-1.1326050549584,14.2824029400298));
#257653=CARTESIAN_POINT('Ctrl Pts',(2.34196789024492,1.54123461716797,14.4412250805845));
#257654=CARTESIAN_POINT('Ctrl Pts',(-0.0256713533761431,2.80349045400981,
14.6000472211392));
#257655=CARTESIAN_POINT('Ctrl Pts',(-2.3697987532753,1.49808932078764,14.7588693616939));
#257656=CARTESIAN_POINT('Ctrl Pts',(-2.54347813978087,-1.17937979317275,
14.9176915022486));
#257657=CARTESIAN_POINT('Ctrl Pts',(-0.387640275935778,-2.7766801689505,
15.0765136428034));
#257658=CARTESIAN_POINT('Ctrl Pts',(2.1232290291376,-1.8308785415232,15.2353357833581));
#257659=CARTESIAN_POINT('Ctrl Pts',(2.68947825967196,0.791785599022987,
15.3941579239129));
#257660=CARTESIAN_POINT('Ctrl Pts',(0.792491851405913,2.68927023744945,
15.5529800644676));
#257661=CARTESIAN_POINT('Ctrl Pts',(-1.83032090055044,2.12370975988261,
15.7118022050223));
#257662=CARTESIAN_POINT('Ctrl Pts',(-2.77678187085878,-0.386911082619306,
15.870624345577));
#257663=CARTESIAN_POINT('Ctrl Pts',(-1.18004769118328,-2.54316833766063,
16.0294464861318));
#257664=CARTESIAN_POINT('Ctrl Pts',(1.49746693978282,-2.37019208118836,
16.1882686266865));
#257665=CARTESIAN_POINT('Ctrl Pts',(2.80348361626654,-0.0264075750974751,
16.3470907672412));
#257666=CARTESIAN_POINT('Ctrl Pts',(1.54184958368406,2.34156307285865,16.5059129077959));
#257667=CARTESIAN_POINT('Ctrl Pts',(-1.13193151590743,2.56494614739192,
16.6647350483507));
#257668=CARTESIAN_POINT('Ctrl Pts',(-2.7690007456855,0.439149913050121,
16.8235571889054));
#257669=CARTESIAN_POINT('Ctrl Pts',(-1.87000138108549,-2.08885439649021,
16.9823793294602));
#257670=CARTESIAN_POINT('Ctrl Pts',(0.741692248419004,-2.70372151075853,
17.1412014700149));
#257671=CARTESIAN_POINT('Ctrl Pts',(2.67408584390158,-0.842308110700031,
17.3000236105696));
#257672=CARTESIAN_POINT('Ctrl Pts',(2.15734130986859,1.79055768786866,17.4588457511243));
#257673=CARTESIAN_POINT('Ctrl Pts',(-0.33526586359856,2.78348920207669,
17.6176678916791));
#257674=CARTESIAN_POINT('Ctrl Pts',(-2.52081047486617,1.22708395286699,
17.7764900322338));
#257675=CARTESIAN_POINT('Ctrl Pts',(-2.39759814123902,-1.45318409539433,
17.9353121727885));
#257676=CARTESIAN_POINT('Ctrl Pts',(-0.0784779302164847,-2.80250647364015,
18.0941343133432));
#257677=CARTESIAN_POINT('Ctrl Pts',(2.31252045107973,-1.58508344876221,
18.252956453898));
#257678=CARTESIAN_POINT('Ctrl Pts',(2.58552714046087,1.08410340382027,18.4117785944527));
#257679=CARTESIAN_POINT('Ctrl Pts',(0.490511770879417,2.76034534307135,
18.5706007350074));
#257680=CARTESIAN_POINT('Ctrl Pts',(-2.05376615740623,1.90851815106454,
18.7294228755622));
#257681=CARTESIAN_POINT('Ctrl Pts',(-2.71701814363985,-0.691417805009407,
18.8882450161169));
#257682=CARTESIAN_POINT('Ctrl Pts',(-0.891859856974616,-2.65783582951041,
19.0470671566717));
#257683=CARTESIAN_POINT('Ctrl Pts',(1.75022653268834,-2.19050141850195,
19.2058892972263));
#257684=CARTESIAN_POINT('Ctrl Pts',(2.78914078757823,0.284026632862494,
19.3647114377811));
#257685=CARTESIAN_POINT('Ctrl Pts',(1.2738787066253,2.49658300563447,19.5235335783358));
#257686=CARTESIAN_POINT('Ctrl Pts',(-1.4087466563893,2.42611756744335,19.6823557188906));
#257687=CARTESIAN_POINT('Ctrl Pts',(-2.79990404402391,0.126538750182127,
19.8411778594453));
#257688=CARTESIAN_POINT('Ctrl Pts',(-2.01936616407895,-1.47301363900539,
19.9470592864818));
#257689=CARTESIAN_POINT('Ctrl Pts',(-1.37702479013087,-1.93106208855776,
20.));
#257690=CARTESIAN_POINT('Ctrl Pts',(-1.12236674703447,2.30288577939268,
-0.219489327336923));
#257691=CARTESIAN_POINT('Ctrl Pts',(-1.88839018271042,1.92954584245559,
-0.16654861381868));
#257692=CARTESIAN_POINT('Ctrl Pts',(-3.00532692914963,0.364817996181975,
-0.060667186782193));
#257693=CARTESIAN_POINT('Ctrl Pts',(-1.9336634977078,-2.33317173068091,
0.0981549537725366));
#257694=CARTESIAN_POINT('Ctrl Pts',(0.911572263156383,-2.88693151715453,
0.256977094327266));
#257695=CARTESIAN_POINT('Ctrl Pts',(2.92059873626954,-0.800274052314299,
0.415799234881996));
#257696=CARTESIAN_POINT('Ctrl Pts',(2.2553993596395,2.02123474938121,0.574621375436725));
#257697=CARTESIAN_POINT('Ctrl Pts',(-0.475832051042864,2.99054652551054,
0.733443515991456));
#257698=CARTESIAN_POINT('Ctrl Pts',(-2.77107059541602,1.2213995263697,0.892265656546184));
#257699=CARTESIAN_POINT('Ctrl Pts',(-2.52844350910708,-1.66667285202344,
1.05108779710092));
#257700=CARTESIAN_POINT('Ctrl Pts',(0.0299826057622768,-3.02813294412635,
1.20990993765564));
#257701=CARTESIAN_POINT('Ctrl Pts',(2.56092123364921,-1.61626530231301,
1.36873207821037));
#257702=CARTESIAN_POINT('Ctrl Pts',(2.74638102397023,1.27594418164071,1.5275542187651));
#257703=CARTESIAN_POINT('Ctrl Pts',(0.416481730423991,2.99952324290431,
1.68637635931983));
#257704=CARTESIAN_POINT('Ctrl Pts',(-2.29486039055236,1.97591378958438,
1.84519849987456));
#257705=CARTESIAN_POINT('Ctrl Pts',(-2.90439097697297,-0.857398460686849,
2.00402064042929));
#257706=CARTESIAN_POINT('Ctrl Pts',(-0.853850896153828,-2.90543485858881,
2.16284278098402));
#257707=CARTESIAN_POINT('Ctrl Pts',(1.97871240779968,-2.29244712155302,
2.32166492153875));
#257708=CARTESIAN_POINT('Ctrl Pts',(2.99901561314596,0.420144727310875,
2.48048706209348));
#257709=CARTESIAN_POINT('Ctrl Pts',(1.27258438240543,2.7479345817307,2.63930920264821));
#257710=CARTESIAN_POINT('Ctrl Pts',(-1.61937959706346,2.55895012228193,
2.79813134320294));
#257711=CARTESIAN_POINT('Ctrl Pts',(-3.02818846679257,0.0262778390227437,
2.95695348375767));
#257712=CARTESIAN_POINT('Ctrl Pts',(-1.66354423848634,-2.53046169472791,
3.1157756243124));
#257713=CARTESIAN_POINT('Ctrl Pts',(1.22470458087275,-2.76960549353663,
3.27459776486713));
#257714=CARTESIAN_POINT('Ctrl Pts',(2.99127266400681,-0.472126816567234,
3.43341990542186));
#257715=CARTESIAN_POINT('Ctrl Pts',(2.01819806245289,2.25776270925503,3.59224204597659));
#257716=CARTESIAN_POINT('Ctrl Pts',(-0.803300995111289,2.91981564368942,
3.75106418653132));
#257717=CARTESIAN_POINT('Ctrl Pts',(-2.88907384616146,0.907671851413923,
3.90988632708605));
#257718=CARTESIAN_POINT('Ctrl Pts',(-2.32880572754616,-1.9357891829015,
4.06870846764077));
#257719=CARTESIAN_POINT('Ctrl Pts',(0.364365768366402,-3.00630229114176,
4.22753060819551));
#257720=CARTESIAN_POINT('Ctrl Pts',(2.72382244705534,-1.32340740333668,
4.38635274875023));
#257721=CARTESIAN_POINT('Ctrl Pts',(2.58858837994239,1.5715680314311,4.54517488930497));
#257722=CARTESIAN_POINT('Ctrl Pts',(0.0825215579805379,3.02717790538921,
4.70399702985969));
#257723=CARTESIAN_POINT('Ctrl Pts',(-2.49912499469722,1.71026025481233,
4.86281917041443));
#257724=CARTESIAN_POINT('Ctrl Pts',(-2.79187639436079,-1.17304819888917,
5.02164131096916));
#257725=CARTESIAN_POINT('Ctrl Pts',(-0.527607892903676,-2.98198688623563,
5.18046345152388));
#257726=CARTESIAN_POINT('Ctrl Pts',(2.21988539775892,-2.05978753737781,
5.33928559207862));
#257727=CARTESIAN_POINT('Ctrl Pts',(2.93423311229333,0.748927180066403,
5.49810773263335));
#257728=CARTESIAN_POINT('Ctrl Pts',(0.96117945124088,2.87171550485715,5.65692987318806));
#257729=CARTESIAN_POINT('Ctrl Pts',(-1.89219791982296,2.36436099412505,
5.81575201374282));
#257730=CARTESIAN_POINT('Ctrl Pts',(-3.01255167005992,-0.308461202652475,
5.97457415429752));
#257731=CARTESIAN_POINT('Ctrl Pts',(-1.37377375204991,-2.69877037861723,
6.13339629485228));
#257732=CARTESIAN_POINT('Ctrl Pts',(1.52321417508908,-2.6173334627308,6.29221843540698));
#257733=CARTESIAN_POINT('Ctrl Pts',(3.02512280457487,-0.138736785186446,
6.45104057596173));
#257734=CARTESIAN_POINT('Ctrl Pts',(1.75638613247392,2.46692594780958,6.60986271651646));
#257735=CARTESIAN_POINT('Ctrl Pts',(-1.12098704798687,2.8131839464508,6.76868485707117));
#257736=CARTESIAN_POINT('Ctrl Pts',(-2.97167215715763,0.582906912548589,
6.92750699762592));
#257737=CARTESIAN_POINT('Ctrl Pts',(-2.10066626997162,-2.18124210039289,
7.08632913818064));
#257738=CARTESIAN_POINT('Ctrl Pts',(0.694294943026906,-2.94763810709695,
7.24515127873538));
#257739=CARTESIAN_POINT('Ctrl Pts',(2.85336626127343,-1.01435539006273,
7.40397341929009));
#257740=CARTESIAN_POINT('Ctrl Pts',(2.39910042390177,1.84795374248307,7.56279555984483));
#257741=CARTESIAN_POINT('Ctrl Pts',(-0.25245020054233,3.01776155031655,
7.72161770039956));
#257742=CARTESIAN_POINT('Ctrl Pts',(-2.67278708352791,1.42366607195971,
7.8804398409543));
#257743=CARTESIAN_POINT('Ctrl Pts',(-2.64517541912911,-1.47433472466667,
8.03926198150901));
#257744=CARTESIAN_POINT('Ctrl Pts',(-0.194904140449694,-3.02202386727147,
8.19808412206375));
#257745=CARTESIAN_POINT('Ctrl Pts',(2.43387567354607,-1.80190595871246,
8.35690626261848));
#257746=CARTESIAN_POINT('Ctrl Pts',(2.83352079279202,1.0685390938745,8.5157284031732));
#257747=CARTESIAN_POINT('Ctrl Pts',(0.638004796718893,2.96033203504042,
8.67455054372795));
#257748=CARTESIAN_POINT('Ctrl Pts',(-2.14184615254877,2.14082015525238,
8.83337268428265));
#257749=CARTESIAN_POINT('Ctrl Pts',(-2.96002600195016,-0.639423135413294,
8.99219482483741));
#257750=CARTESIAN_POINT('Ctrl Pts',(-1.06718131956222,-2.83403244679736,
9.15101696539212));
#257751=CARTESIAN_POINT('Ctrl Pts',(1.80307191778247,-2.43301202989773,
9.30983910594686));
#257752=CARTESIAN_POINT('Ctrl Pts',(3.02193013411443,0.196352088998341,
9.46866124650158));
#257753=CARTESIAN_POINT('Ctrl Pts',(1.47306714747715,2.64588152745855,9.62748338705632));
#257754=CARTESIAN_POINT('Ctrl Pts',(-1.42494654633381,2.67210464211531,
9.78630552761105));
#257755=CARTESIAN_POINT('Ctrl Pts',(-3.01788216277166,0.251004242887347,
9.94512766816578));
#257756=CARTESIAN_POINT('Ctrl Pts',(-1.84680402665019,-2.39998557609655,
10.1039498087205));
#257757=CARTESIAN_POINT('Ctrl Pts',(1.01572243403243,-2.85287991603679,
10.2627719492752));
#257758=CARTESIAN_POINT('Ctrl Pts',(2.94797043285812,-0.692882533563333,
10.42159408983));
#257759=CARTESIAN_POINT('Ctrl Pts',(2.18023533788578,2.10171114803079,10.5804162303847));
#257760=CARTESIAN_POINT('Ctrl Pts',(-0.584330691067625,2.97139252233684,
10.7392383709394));
#257761=CARTESIAN_POINT('Ctrl Pts',(-2.81372073267564,1.11963901184004,
10.8980605114941));
#257762=CARTESIAN_POINT('Ctrl Pts',(-2.46608411071298,-1.75756793246,11.0568826520489));
#257763=CARTESIAN_POINT('Ctrl Pts',(0.140186225005578,-3.02505598305908,
11.2157047926036));
#257764=CARTESIAN_POINT('Ctrl Pts',(2.61806299433025,-1.5219599324691,11.3745269331583));
#257765=CARTESIAN_POINT('Ctrl Pts',(2.69811183960188,1.37506668177329,11.5333490737131));
#257766=CARTESIAN_POINT('Ctrl Pts',(0.307017734827514,3.01269912019508,
11.6921712142678));
#257767=CARTESIAN_POINT('Ctrl Pts',(-2.36526734943941,1.89106484394342,
11.8509933548225));
#257768=CARTESIAN_POINT('Ctrl Pts',(-2.87125463620523,-0.962555293161294,
12.0098154953773));
#257769=CARTESIAN_POINT('Ctrl Pts',(-0.747521187194434,-2.93459161605465,
12.168637635932));
#257770=CARTESIAN_POINT('Ctrl Pts',(2.06085093565951,-2.21889821743003,
12.3274597764867));
#257771=CARTESIAN_POINT('Ctrl Pts',(2.98173374617193,0.529036619963464,
12.4862819170415));
#257772=CARTESIAN_POINT('Ctrl Pts',(1.17171036605948,2.79243812758522,12.6451040575962));
#257773=CARTESIAN_POINT('Ctrl Pts',(-1.71145748793473,2.49830525463062,
12.8039261981509));
#257774=CARTESIAN_POINT('Ctrl Pts',(-3.02713801855786,-0.0839719889273276,
12.9627483387056));
#257775=CARTESIAN_POINT('Ctrl Pts',(-1.57032755619116,-2.58934108309229,
13.1215704792604));
#257776=CARTESIAN_POINT('Ctrl Pts',(1.32471234232721,-2.7231880376516,13.2803926198151));
#257777=CARTESIAN_POINT('Ctrl Pts',(3.00647652798119,-0.36292528848369,
13.4392147603698));
#257778=CARTESIAN_POINT('Ctrl Pts',(1.93467313813552,2.32973297330394,13.5980369009245));
#257779=CARTESIAN_POINT('Ctrl Pts',(-0.909056016897293,2.88863861299158,
13.7568590414793));
#257780=CARTESIAN_POINT('Ctrl Pts',(-2.9202002010698,0.801901904221753,
13.915681182034));
#257781=CARTESIAN_POINT('Ctrl Pts',(-2.25679545303008,-2.01927961449252,
14.0745033225888));
#257782=CARTESIAN_POINT('Ctrl Pts',(0.473560001646884,-2.99104610515534,
14.2333254631435));
#257783=CARTESIAN_POINT('Ctrl Pts',(2.77019197521469,-1.22337741469139,
14.3921476036982));
#257784=CARTESIAN_POINT('Ctrl Pts',(2.52966434355467,1.66475649488695,14.5509697442529));
#257785=CARTESIAN_POINT('Ctrl Pts',(-0.0277287778183823,3.02817552219422,
14.7097918848077));
#257786=CARTESIAN_POINT('Ctrl Pts',(-2.55972570440915,1.61815332910488,
14.8686140253624));
#257787=CARTESIAN_POINT('Ctrl Pts',(-2.74732458357555,-1.27390090305035,
15.0274361659171));
#257788=CARTESIAN_POINT('Ctrl Pts',(-0.418707612621415,-2.99921653328682,
15.1862583064718));
#257789=CARTESIAN_POINT('Ctrl Pts',(2.29339470903158,-1.97761386189897,
15.3450804470266));
#257790=CARTESIAN_POINT('Ctrl Pts',(2.90502584796162,0.855243065428628,
15.5039025875813));
#257791=CARTESIAN_POINT('Ctrl Pts',(0.856005920238958,2.9048011538481,15.6627247281361));
#257792=CARTESIAN_POINT('Ctrl Pts',(-1.97701152892453,2.29391396782655,
15.8215468686908));
#257793=CARTESIAN_POINT('Ctrl Pts',(-2.99932638607008,-0.417919978281937,
15.9803690092455));
#257794=CARTESIAN_POINT('Ctrl Pts',(-1.27462232958634,-2.74698995243888,
16.1391911498002));
#257795=CARTESIAN_POINT('Ctrl Pts',(1.61748106752409,-2.56015055549323,
16.298013290355));
#257796=CARTESIAN_POINT('Ctrl Pts',(3.02816813644166,-0.0285240038525372,
16.4568354309097));
#257797=CARTESIAN_POINT('Ctrl Pts',(1.66542074774659,2.52922708217632,16.6156575714644));
#257798=CARTESIAN_POINT('Ctrl Pts',(-1.22264989501513,2.77051313949344,
16.7744797120191));
#257799=CARTESIAN_POINT('Ctrl Pts',(-2.99092164449118,0.474345477213988,
16.9333018525739));
#257800=CARTESIAN_POINT('Ctrl Pts',(-2.01987219202877,-2.25626512971792,
17.0921239931286));
#257801=CARTESIAN_POINT('Ctrl Pts',(0.801134995288171,-2.92041062098095,
17.2509461336833));
#257802=CARTESIAN_POINT('Ctrl Pts',(2.88839981073126,-0.909814691653167,
17.4097682742381));
#257803=CARTESIAN_POINT('Ctrl Pts',(2.33024091029762,1.93406150312561,17.5685904147928));
#257804=CARTESIAN_POINT('Ctrl Pts',(-0.362135665603684,3.00657127473531,
17.7274125553475));
#257805=CARTESIAN_POINT('Ctrl Pts',(-2.72284022410792,1.32542830115026,
17.8862346959023));
#257806=CARTESIAN_POINT('Ctrl Pts',(-2.58975306763537,-1.56964918522231,
18.045056836457));
#257807=CARTESIAN_POINT('Ctrl Pts',(-0.0847675250594005,-3.02711268095448,
18.2038789770117));
#257808=CARTESIAN_POINT('Ctrl Pts',(2.49785684645981,-1.71211958054349,
18.3627011175664));
#257809=CARTESIAN_POINT('Ctrl Pts',(2.79274359130207,1.17098861038763,18.5215232581212));
#257810=CARTESIAN_POINT('Ctrl Pts',(0.529823718786248,2.98157255671619,
18.6803453986759));
#257811=CARTESIAN_POINT('Ctrl Pts',(-2.21836475215143,2.06147587927432,
18.8391675392306));
#257812=CARTESIAN_POINT('Ctrl Pts',(-2.93477290930665,-0.746831318702741,
18.9979896797854));
#257813=CARTESIAN_POINT('Ctrl Pts',(-0.963337750715509,-2.87084744284491,
19.1568118203401));
#257814=CARTESIAN_POINT('Ctrl Pts',(1.89049801721319,-2.36605862786224,
19.3156339608948));
#257815=CARTESIAN_POINT('Ctrl Pts',(3.01267580519764,0.306789879043543,
19.4744561014495));
#257816=CARTESIAN_POINT('Ctrl Pts',(1.37597340919417,2.69667105018146,19.6332782420043));
#257817=CARTESIAN_POINT('Ctrl Pts',(-1.52165031835563,2.62055817639379,
19.792100382559));
#257818=CARTESIAN_POINT('Ctrl Pts',(-3.02430168024254,0.136680167882348,
19.9509225231137));
#257819=CARTESIAN_POINT('Ctrl Pts',(-2.18120777963231,-1.59106796283699,
20.0568039501502));
#257820=CARTESIAN_POINT('Ctrl Pts',(-1.48738611075519,-2.08582659521599,
20.1097446636685));
#257821=CARTESIAN_POINT('Ctrl Pts',(-1.20564430054384,2.47375567929493,
-0.109744663668461));
#257822=CARTESIAN_POINT('Ctrl Pts',(-2.02850526978225,2.07271460397539,
-0.056803950150218));
#257823=CARTESIAN_POINT('Ctrl Pts',(-3.2283166736487,0.391886822194973,
0.0490774768862683));
#257824=CARTESIAN_POINT('Ctrl Pts',(-2.07713778169297,-2.5062887926054,
0.207899617440998));
#257825=CARTESIAN_POINT('Ctrl Pts',(0.979209252690544,-3.10113653929458,
0.366721757995727));
#257826=CARTESIAN_POINT('Ctrl Pts',(3.13730180430125,-0.85965291879434,
0.525543898550458));
#257827=CARTESIAN_POINT('Ctrl Pts',(2.42274585431577,2.17120665958024,0.684366039105187));
#257828=CARTESIAN_POINT('Ctrl Pts',(-0.511137916257496,3.21243959117606,
0.843188179659916));
#257829=CARTESIAN_POINT('Ctrl Pts',(-2.97667894972426,1.3120251304179,1.00201032021465));
#257830=CARTESIAN_POINT('Ctrl Pts',(-2.71604937874059,-1.79033691992615,
1.16083246076937));
#257831=CARTESIAN_POINT('Ctrl Pts',(0.0322072601030219,-3.25281485309624,
1.31965460132411));
#257832=CARTESIAN_POINT('Ctrl Pts',(2.75093689085934,-1.73618922250611,
1.47847674187883));
#257833=CARTESIAN_POINT('Ctrl Pts',(2.95015745737327,1.37061689904108,1.63729888243357));
#257834=CARTESIAN_POINT('Ctrl Pts',(0.44738391073424,3.22208236453155,1.79612102298829));
#257835=CARTESIAN_POINT('Ctrl Pts',(-2.46513482132621,2.1225229677134,1.95494316354302));
#257836=CARTESIAN_POINT('Ctrl Pts',(-3.11989145900001,-0.921015853466312,
2.11376530409775));
#257837=CARTESIAN_POINT('Ctrl Pts',(-0.91720506615342,-3.12101279471662,
2.27258744465248));
#257838=CARTESIAN_POINT('Ctrl Pts',(2.12552923826585,-2.46254249219458,
2.43140958520721));
#257839=CARTESIAN_POINT('Ctrl Pts',(3.22153706957644,0.451318695269874,
2.59023172576194));
#257840=CARTESIAN_POINT('Ctrl Pts',(1.36700780886653,2.95182628626936,2.74905386631667));
#257841=CARTESIAN_POINT('Ctrl Pts',(-1.73953459221347,2.74881952664486,
2.9078760068714));
#257842=CARTESIAN_POINT('Ctrl Pts',(-3.25287449544242,0.0282276064683039,
3.06669814742613));
#257843=CARTESIAN_POINT('Ctrl Pts',(-1.78697616900445,-2.71821731003186,
3.22552028798086));
#257844=CARTESIAN_POINT('Ctrl Pts',(1.31557541390151,-2.97510513997333,
3.38434242853558));
#257845=CARTESIAN_POINT('Ctrl Pts',(3.21321960781657,-0.507157760181518,
3.54316456909033));
#257846=CARTESIAN_POINT('Ctrl Pts',(2.16794465605303,2.4252845601369,3.70198670964504));
#257847=CARTESIAN_POINT('Ctrl Pts',(-0.862904455193533,3.13646060768837,
3.86080885019978));
#257848=CARTESIAN_POINT('Ctrl Pts',(-3.10343782518346,0.975019437552611,
4.01963099075451));
#257849=CARTESIAN_POINT('Ctrl Pts',(-2.50159884004805,-2.07942118882818,
4.17845313130924));
#257850=CARTESIAN_POINT('Ctrl Pts',(0.391401039905119,-3.22936440571122,
4.33727527186397));
#257851=CARTESIAN_POINT('Ctrl Pts',(2.92592507543778,-1.42160180470976,
4.4960974124187));
#257852=CARTESIAN_POINT('Ctrl Pts',(2.78065688864868,1.6881754961274,4.65491955297343));
#257853=CARTESIAN_POINT('Ctrl Pts',(0.0886445061867101,3.25178895223693,
4.81374169352816));
#257854=CARTESIAN_POINT('Ctrl Pts',(-2.68455548434994,1.83715842803552,
4.97256383408289));
#257855=CARTESIAN_POINT('Ctrl Pts',(-2.99902850077992,-1.26008622314477,
5.13138597463762));
#257856=CARTESIAN_POINT('Ctrl Pts',(-0.566755430595232,-3.20324484237067,
5.29020811519235));
#257857=CARTESIAN_POINT('Ctrl Pts',(2.38459682161839,-2.21261999371634,
5.44903025574707));
#257858=CARTESIAN_POINT('Ctrl Pts',(3.15194782601206,0.804496202827806,
5.60785239630181));
#257859=CARTESIAN_POINT('Ctrl Pts',(1.03249720312042,3.08479152680039,5.76667453685653));
#257860=CARTESIAN_POINT('Ctrl Pts',(-2.03259553400278,2.53979224217656,
5.92549667741127));
#257861=CARTESIAN_POINT('Ctrl Pts',(-3.23607747707985,-0.331348457979058,
6.08431881796598));
#257862=CARTESIAN_POINT('Ctrl Pts',(-1.47570524409423,-2.89901418948268,
6.24314095852073));
#257863=CARTESIAN_POINT('Ctrl Pts',(1.63623387235594,-2.81153480384359,
6.40196309907545));
#257864=CARTESIAN_POINT('Ctrl Pts',(3.24958136671251,-0.149030800117508,
6.56078523963019));
#257865=CARTESIAN_POINT('Ctrl Pts',(1.88670676119597,2.64996732725637,6.71960738018491));
#257866=CARTESIAN_POINT('Ctrl Pts',(-1.20416223035814,3.02191703414368,
6.87842952073964));
#257867=CARTESIAN_POINT('Ctrl Pts',(-3.19216477931873,0.626157536044905,
7.03725166129438));
#257868=CARTESIAN_POINT('Ctrl Pts',(-2.25653185327151,-2.3430862624837,
7.1960738018491));
#257869=CARTESIAN_POINT('Ctrl Pts',(0.745810354029566,-3.16634744683699,
7.35489594240383));
#257870=CARTESIAN_POINT('Ctrl Pts',(3.06508080300672,-1.08961869904501,
7.51371808295856));
#257871=CARTESIAN_POINT('Ctrl Pts',(2.57710927390893,1.98506851987568,7.67254022351329));
#257872=CARTESIAN_POINT('Ctrl Pts',(-0.271181542271447,3.24167392089336,
7.83136236406802));
#257873=CARTESIAN_POINT('Ctrl Pts',(-2.8711029815673,1.5292994826077,7.99018450462276));
#257874=CARTESIAN_POINT('Ctrl Pts',(-2.84144258232714,-1.58372765638758,
8.14900664517747));
#257875=CARTESIAN_POINT('Ctrl Pts',(-0.209365670095335,-3.24625249394657,
8.30782878573222));
#257876=CARTESIAN_POINT('Ctrl Pts',(2.61446478327733,-1.93560407502967,
8.46665092628693));
#257877=CARTESIAN_POINT('Ctrl Pts',(3.04376283717295,1.14782273427289,8.62547306684167));
#257878=CARTESIAN_POINT('Ctrl Pts',(0.685343582136768,3.17998324094527,
8.7842952073964));
#257879=CARTESIAN_POINT('Ctrl Pts',(-2.30076720758629,2.29966508317285,
8.94311734795113));
#257880=CARTESIAN_POINT('Ctrl Pts',(-3.17965450076118,-0.686867158960146,
9.10193948850586));
#257881=CARTESIAN_POINT('Ctrl Pts',(-1.14636421559767,-3.04431245496679,
9.2607616290606));
#257882=CARTESIAN_POINT('Ctrl Pts',(1.93685654612355,-2.61353705885476,
9.4195837696153));
#257883=CARTESIAN_POINT('Ctrl Pts',(3.24615180596125,0.210921053769822,
9.57840591017007));
#257884=CARTESIAN_POINT('Ctrl Pts',(1.58236602729615,2.84220108259916,9.73722805072475));
#257885=CARTESIAN_POINT('Ctrl Pts',(-1.53067496583115,2.87036990425393,
9.89605019127954));
#257886=CARTESIAN_POINT('Ctrl Pts',(-3.24180348257135,0.269628297211287,
10.0548723318342));
#257887=CARTESIAN_POINT('Ctrl Pts',(-1.98383349723732,-2.57806010277262,
10.213694472389));
#257888=CARTESIAN_POINT('Ctrl Pts',(1.09108717516923,-3.06455837184578,
10.3725166129437));
#257889=CARTESIAN_POINT('Ctrl Pts',(3.16670443055993,-0.744293146375072,
10.5313387534984));
#257890=CARTESIAN_POINT('Ctrl Pts',(2.34200480004562,2.2576542593657,10.6901608940532));
#257891=CARTESIAN_POINT('Ctrl Pts',(-0.62768695631793,3.19186439610727,
10.8489830346079));
#257892=CARTESIAN_POINT('Ctrl Pts',(-3.02249364892158,1.20271417240239,
11.0078051751626));
#257893=CARTESIAN_POINT('Ctrl Pts',(-2.64906302739169,-1.88797624857284,
11.1666273157173));
#257894=CARTESIAN_POINT('Ctrl Pts',(0.150587785712017,-3.24950958716283,
11.3254494562721));
#257895=CARTESIAN_POINT('Ctrl Pts',(2.81231846534928,-1.63488656723465,
11.4842715968268));
#257896=CARTESIAN_POINT('Ctrl Pts',(2.89830678808057,1.47709410683101,11.6430937373815));
#257897=CARTESIAN_POINT('Ctrl Pts',(0.329797887489733,3.23623586774451,
11.8019158779363));
#257898=CARTESIAN_POINT('Ctrl Pts',(-2.5407658473924,2.03137838597176,11.960738018491));
#257899=CARTESIAN_POINT('Ctrl Pts',(-3.08429646254003,-1.03397512998715,
12.1195601590457));
#257900=CARTESIAN_POINT('Ctrl Pts',(-0.802985887864231,-3.15233293009474,
12.2783822996005));
#257901=CARTESIAN_POINT('Ctrl Pts',(2.21376229419958,-2.38353639432022,
12.4372044401552));
#257902=CARTESIAN_POINT('Ctrl Pts',(3.20297291977867,0.568290166581644,
12.5960265807099));
#257903=CARTESIAN_POINT('Ctrl Pts',(1.25864912557356,2.99963191357903,12.7548487212647));
#257904=CARTESIAN_POINT('Ctrl Pts',(-1.8384444936591,2.68367492107434,12.9136708618194));
#257905=CARTESIAN_POINT('Ctrl Pts',(-3.25174610587588,-0.0902025564487242,
13.0724930023741));
#257906=CARTESIAN_POINT('Ctrl Pts',(-1.6868429799005,-2.78146544099136,
13.2313151429288));
#257907=CARTESIAN_POINT('Ctrl Pts',(1.42300356777929,-2.92524359402021,
13.3901372834835));
#257908=CARTESIAN_POINT('Ctrl Pts',(3.22955157060447,-0.389853679057881,
13.5489594240383));
#257909=CARTESIAN_POINT('Ctrl Pts',(2.07822233558811,2.50259488573989,13.707781564593));
#257910=CARTESIAN_POINT('Ctrl Pts',(-0.976506305575396,3.10297029851087,
13.8666037051478));
#257911=CARTESIAN_POINT('Ctrl Pts',(-3.13687369852085,0.86140155432683,
14.0254258457025));
#257912=CARTESIAN_POINT('Ctrl Pts',(-2.42424553527463,-2.16910645726973,
14.1842479862572));
#257913=CARTESIAN_POINT('Ctrl Pts',(0.508697284964691,-3.21297623871397,
14.3430701268119));
#257914=CARTESIAN_POINT('Ctrl Pts',(2.97573513751593,-1.31414977442438,
14.5018922673667));
#257915=CARTESIAN_POINT('Ctrl Pts',(2.71736079686443,1.78827837260592,14.6607144079214));
#257916=CARTESIAN_POINT('Ctrl Pts',(-0.0297862022606204,3.25286059037863,
14.8195365484761));
#257917=CARTESIAN_POINT('Ctrl Pts',(-2.749652655543,1.73821733742212,14.9783586890308));
#257918=CARTESIAN_POINT('Ctrl Pts',(-2.95117102737023,-1.36842201292796,
15.1371808295856));
#257919=CARTESIAN_POINT('Ctrl Pts',(-0.449774949307054,-3.22175289762314,
15.2960029701403));
#257920=CARTESIAN_POINT('Ctrl Pts',(2.46356038892555,-2.12434918227474,
15.4548251106951));
#257921=CARTESIAN_POINT('Ctrl Pts',(3.12057343625127,0.918700531834268,
15.6136472512498));
#257922=CARTESIAN_POINT('Ctrl Pts',(0.919519989072005,3.12033207024676,
15.7724693918045));
#257923=CARTESIAN_POINT('Ctrl Pts',(-2.12370215729863,2.46411817577049,
15.9312915323592));
#257924=CARTESIAN_POINT('Ctrl Pts',(-3.22187090128139,-0.448928873944568,
16.090113672914));
#257925=CARTESIAN_POINT('Ctrl Pts',(-1.3691969679894,-2.95081156721713,
16.2489358134687));
#257926=CARTESIAN_POINT('Ctrl Pts',(1.73749519526536,-2.7501090297981,16.4077579540234));
#257927=CARTESIAN_POINT('Ctrl Pts',(3.25285265661678,-0.0306404326076004,
16.5665800945781));
#257928=CARTESIAN_POINT('Ctrl Pts',(1.78899191180913,2.716891091494,16.7254022351329));
#257929=CARTESIAN_POINT('Ctrl Pts',(-1.31336827412284,2.97608013159495,
16.8842243756876));
#257930=CARTESIAN_POINT('Ctrl Pts',(-3.21284254329687,0.509541041377854,
17.0430465162423));
#257931=CARTESIAN_POINT('Ctrl Pts',(-2.16974300297203,-2.42367586294563,
17.2018686567971));
#257932=CARTESIAN_POINT('Ctrl Pts',(0.860577742157333,-3.13709973120337,
17.3606907973518));
#257933=CARTESIAN_POINT('Ctrl Pts',(3.10271377756093,-0.977321272606305,
17.5195129379065));
#257934=CARTESIAN_POINT('Ctrl Pts',(2.50314051072665,2.07756531838256,17.6783350784613));
#257935=CARTESIAN_POINT('Ctrl Pts',(-0.389005467608808,3.22965334739393,
17.837157219016));
#257936=CARTESIAN_POINT('Ctrl Pts',(-2.92486997334968,1.42377264943353,
17.9959793595707));
#257937=CARTESIAN_POINT('Ctrl Pts',(-2.78190799403171,-1.68611427505029,
18.1548015001254));
#257938=CARTESIAN_POINT('Ctrl Pts',(-0.091057119902321,-3.25171888826882,
18.3136236406802));
#257939=CARTESIAN_POINT('Ctrl Pts',(2.6831932418399,-1.83915571232477,18.4724457812349));
#257940=CARTESIAN_POINT('Ctrl Pts',(2.99996004214327,1.25787381695499,18.6312679217897));
#257941=CARTESIAN_POINT('Ctrl Pts',(0.569135666693086,3.20279977036102,
18.7900900623443));
#257942=CARTESIAN_POINT('Ctrl Pts',(-2.38296334689664,2.2144336074841,18.9489122028991));
#257943=CARTESIAN_POINT('Ctrl Pts',(-3.15252767497344,-0.802244832396076,
19.1077343434538));
#257944=CARTESIAN_POINT('Ctrl Pts',(-1.0348156444564,-3.0838590561794,19.2665564840085));
#257945=CARTESIAN_POINT('Ctrl Pts',(2.03076950173803,-2.54161583722253,
19.4253786245633));
#257946=CARTESIAN_POINT('Ctrl Pts',(3.23621082281705,0.329553125224593,
19.584200765118));
#257947=CARTESIAN_POINT('Ctrl Pts',(1.47806811176305,2.89675909472846,19.7430229056727));
#257948=CARTESIAN_POINT('Ctrl Pts',(-1.63455398032195,2.81499878534423,
19.9018450462275));
#257949=CARTESIAN_POINT('Ctrl Pts',(-3.24869931646117,0.146821585582566,
20.0606671867822));
#257950=CARTESIAN_POINT('Ctrl Pts',(-2.34304939518568,-1.70912228666858,
20.1665486138187));
#257951=CARTESIAN_POINT('Ctrl Pts',(-1.59774743137951,-2.24059110187423,
20.2194893273369));
#257952=CARTESIAN_POINT('Ctrl Pts',(-1.28892185405322,2.64462557919718,
0.));
#257953=CARTESIAN_POINT('Ctrl Pts',(-2.16862035685408,2.21588336549518,
0.0529407135182432));
#257954=CARTESIAN_POINT('Ctrl Pts',(-3.45130641814776,0.41895564820797,
0.15882214055473));
#257955=CARTESIAN_POINT('Ctrl Pts',(-2.22061206567813,-2.6794058545299,
0.317644281109459));
#257956=CARTESIAN_POINT('Ctrl Pts',(1.04684624222471,-3.31534156143464,
0.476466421664189));
#257957=CARTESIAN_POINT('Ctrl Pts',(3.35400487233295,-0.91903178527438,
0.635288562218918));
#257958=CARTESIAN_POINT('Ctrl Pts',(2.59009234899204,2.32117856977925,0.794110702773649));
#257959=CARTESIAN_POINT('Ctrl Pts',(-0.54644378147213,3.43433265684159,
0.952932843328378));
#257960=CARTESIAN_POINT('Ctrl Pts',(-3.1822873040325,1.4026507344661,1.11175498388311));
#257961=CARTESIAN_POINT('Ctrl Pts',(-2.9036552483741,-1.91400098782886,
1.27057712443784));
#257962=CARTESIAN_POINT('Ctrl Pts',(0.0344319144437711,-3.47749676206612,
1.42939926499257));
#257963=CARTESIAN_POINT('Ctrl Pts',(2.94095254806946,-1.85611314269922,
1.5882214055473));
#257964=CARTESIAN_POINT('Ctrl Pts',(3.15393389077631,1.46528961644145,1.74704354610203));
#257965=CARTESIAN_POINT('Ctrl Pts',(0.478286091044485,3.44464148615879,
1.90586568665676));
#257966=CARTESIAN_POINT('Ctrl Pts',(-2.63540925210006,2.26913214584243,
2.06468782721148));
#257967=CARTESIAN_POINT('Ctrl Pts',(-3.33539194102706,-0.984633246245777,
2.22350996776621));
#257968=CARTESIAN_POINT('Ctrl Pts',(-0.980559236153007,-3.33659073084442,
2.38233210832095));
#257969=CARTESIAN_POINT('Ctrl Pts',(2.272346068732,-2.63263786283614,2.54115424887567));
#257970=CARTESIAN_POINT('Ctrl Pts',(3.44405852600693,0.482492663228878,
2.6999763894304));
#257971=CARTESIAN_POINT('Ctrl Pts',(1.46143123532763,3.15571799080802,2.85879852998513));
#257972=CARTESIAN_POINT('Ctrl Pts',(-1.85968958736347,2.93868893100779,
3.01762067053986));
#257973=CARTESIAN_POINT('Ctrl Pts',(-3.47756052409227,0.0301773739138614,
3.17644281109459));
#257974=CARTESIAN_POINT('Ctrl Pts',(-1.91040809952256,-2.90597292533581,
3.33526495164932));
#257975=CARTESIAN_POINT('Ctrl Pts',(1.40644624693028,-3.18060478641004,
3.49408709220405));
#257976=CARTESIAN_POINT('Ctrl Pts',(3.43516655162632,-0.542188703795803,
3.65290923275879));
#257977=CARTESIAN_POINT('Ctrl Pts',(2.31769124965316,2.59280641101876,3.81173137331351));
#257978=CARTESIAN_POINT('Ctrl Pts',(-0.922507915275779,3.35310557168732,
3.97055351386824));
#257979=CARTESIAN_POINT('Ctrl Pts',(-3.31780180420545,1.0423670236913,4.12937565442297));
#257980=CARTESIAN_POINT('Ctrl Pts',(-2.67439195254995,-2.22305319475486,
4.2881977949777));
#257981=CARTESIAN_POINT('Ctrl Pts',(0.418436311443839,-3.45242652028068,
4.44701993553243));
#257982=CARTESIAN_POINT('Ctrl Pts',(3.12802770382022,-1.51979620608285,
4.60584207608716));
#257983=CARTESIAN_POINT('Ctrl Pts',(2.97272539735497,1.80478296082371,4.76466421664189));
#257984=CARTESIAN_POINT('Ctrl Pts',(0.0947674543928817,3.47639999908466,
4.92348635719661));
#257985=CARTESIAN_POINT('Ctrl Pts',(-2.86998597400267,1.96405660125871,
5.08230849775136));
#257986=CARTESIAN_POINT('Ctrl Pts',(-3.20618060719906,-1.34712424740037,
5.24113063830607));
#257987=CARTESIAN_POINT('Ctrl Pts',(-0.605902968286784,-3.42450279850571,
5.39995277886081));
#257988=CARTESIAN_POINT('Ctrl Pts',(2.54930824547785,-2.36545245005487,
5.55877491941554));
#257989=CARTESIAN_POINT('Ctrl Pts',(3.3696625397308,0.860065225589209,5.71759705997026));
#257990=CARTESIAN_POINT('Ctrl Pts',(1.10381495499996,3.29786754874362,5.87641920052501));
#257991=CARTESIAN_POINT('Ctrl Pts',(-2.17299314818259,2.71522349022807,
6.03524134107972));
#257992=CARTESIAN_POINT('Ctrl Pts',(-3.45960328409978,-0.354235713305642,
6.19406348163447));
#257993=CARTESIAN_POINT('Ctrl Pts',(-1.57763673613854,-3.09925800034814,
6.35288562218917));
#257994=CARTESIAN_POINT('Ctrl Pts',(1.7492535696228,-3.00573614495637,6.51170776274393));
#257995=CARTESIAN_POINT('Ctrl Pts',(3.47403992885015,-0.159324815048575,
6.67052990329863));
#257996=CARTESIAN_POINT('Ctrl Pts',(2.01702738991803,2.83300870670317,6.82935204385339));
#257997=CARTESIAN_POINT('Ctrl Pts',(-1.28733741272941,3.23065012183655,
6.98817418440809));
#257998=CARTESIAN_POINT('Ctrl Pts',(-3.41265740147983,0.669408159541225,
7.14699632496285));
#257999=CARTESIAN_POINT('Ctrl Pts',(-2.41239743657142,-2.50493042457452,
7.30581846551755));
#258000=CARTESIAN_POINT('Ctrl Pts',(0.797325765032234,-3.38505678657703,
7.4646406060723));
#258001=CARTESIAN_POINT('Ctrl Pts',(3.27679534473999,-1.16488200802731,
7.62346274662702));
#258002=CARTESIAN_POINT('Ctrl Pts',(2.75511812391609,2.12218329726829,7.78228488718175));
#258003=CARTESIAN_POINT('Ctrl Pts',(-0.289912884000569,3.46558629147016,
7.94110702773649));
#258004=CARTESIAN_POINT('Ctrl Pts',(-3.06941887960669,1.6349328932557,8.09992916829121));
#258005=CARTESIAN_POINT('Ctrl Pts',(-3.03770974552517,-1.6931205881085,
8.25875130884594));
#258006=CARTESIAN_POINT('Ctrl Pts',(-0.223827199740972,-3.47048112062168,
8.41757344940067));
#258007=CARTESIAN_POINT('Ctrl Pts',(2.79505389300859,-2.06930219134687,
8.5763955899554));
#258008=CARTESIAN_POINT('Ctrl Pts',(3.25400488155389,1.22710637467128,8.73521773051013));
#258009=CARTESIAN_POINT('Ctrl Pts',(0.73268236755464,3.39963444685013,8.89403987106487));
#258010=CARTESIAN_POINT('Ctrl Pts',(-2.45968826262381,2.45851001109332,
9.05286201161959));
#258011=CARTESIAN_POINT('Ctrl Pts',(-3.3992829995722,-0.734311182506995,
9.21168415217432));
#258012=CARTESIAN_POINT('Ctrl Pts',(-1.22554711163312,-3.25459246313622,
9.37050629272904));
#258013=CARTESIAN_POINT('Ctrl Pts',(2.07064117446462,-2.79406208781179,
9.52932843328378));
#258014=CARTESIAN_POINT('Ctrl Pts',(3.47037347780808,0.225490018541298,
9.68815057383851));
#258015=CARTESIAN_POINT('Ctrl Pts',(1.69166490711515,3.03852063773977,9.84697271439324));
#258016=CARTESIAN_POINT('Ctrl Pts',(-1.63640338532848,3.06863516639254,
10.005794854948));
#258017=CARTESIAN_POINT('Ctrl Pts',(-3.46572480237104,0.288252351535223,
10.1646169955027));
#258018=CARTESIAN_POINT('Ctrl Pts',(-2.12086296782444,-2.7561346294487,
10.3234391360574));
#258019=CARTESIAN_POINT('Ctrl Pts',(1.16645191630603,-3.27623682765478,
10.4822612766121));
#258020=CARTESIAN_POINT('Ctrl Pts',(3.38543842826175,-0.795703759186809,
10.6410834171669));
#258021=CARTESIAN_POINT('Ctrl Pts',(2.50377426220545,2.41359737070061,10.7999055577216));
#258022=CARTESIAN_POINT('Ctrl Pts',(-0.671043221568228,3.41233626987769,
10.9587276982764));
#258023=CARTESIAN_POINT('Ctrl Pts',(-3.23126656516753,1.28578933296473,
11.1175498388311));
#258024=CARTESIAN_POINT('Ctrl Pts',(-2.83204194407039,-2.01838456468568,
11.2763719793858));
#258025=CARTESIAN_POINT('Ctrl Pts',(0.160989346418449,-3.47396319126659,
11.4351941199405));
#258026=CARTESIAN_POINT('Ctrl Pts',(3.00657393636832,-1.7478132020002,11.5940162604952));
#258027=CARTESIAN_POINT('Ctrl Pts',(3.09850173655927,1.57912153188873,11.75283840105));
#258028=CARTESIAN_POINT('Ctrl Pts',(0.352578040151959,3.45977261529396,
11.9116605416047));
#258029=CARTESIAN_POINT('Ctrl Pts',(-2.7162643453454,2.1716919280001,12.0704826821594));
#258030=CARTESIAN_POINT('Ctrl Pts',(-3.29733828887482,-1.105394966813,12.2293048227142));
#258031=CARTESIAN_POINT('Ctrl Pts',(-0.858450588534032,-3.37007424413483,
12.3881269632689));
#258032=CARTESIAN_POINT('Ctrl Pts',(2.36667365273965,-2.54817457121041,
12.5469491038237));
#258033=CARTESIAN_POINT('Ctrl Pts',(3.4242120933854,0.607543713199829,12.7057712443784));
#258034=CARTESIAN_POINT('Ctrl Pts',(1.34558788508765,3.20682569957283,12.8645933849331));
#258035=CARTESIAN_POINT('Ctrl Pts',(-1.96543149938347,2.86904458751805,
13.0234155254878));
#258036=CARTESIAN_POINT('Ctrl Pts',(-3.4763541931939,-0.0964331239701206,
13.1822376660426));
#258037=CARTESIAN_POINT('Ctrl Pts',(-1.80335840360983,-2.97358979889043,
13.3410598065973));
#258038=CARTESIAN_POINT('Ctrl Pts',(1.52129479323137,-3.12729915038881,
13.499881947152));
#258039=CARTESIAN_POINT('Ctrl Pts',(3.45262661322776,-0.41678206963207,
13.6587040877068));
#258040=CARTESIAN_POINT('Ctrl Pts',(2.2217715330407,2.67545679817584,13.8175262282615));
#258041=CARTESIAN_POINT('Ctrl Pts',(-1.0439565942535,3.31730198403016,13.9763483688162));
#258042=CARTESIAN_POINT('Ctrl Pts',(-3.3535471959719,0.920901204431906,
14.1351705093709));
#258043=CARTESIAN_POINT('Ctrl Pts',(-2.59169561751918,-2.31893330004694,
14.2939926499257));
#258044=CARTESIAN_POINT('Ctrl Pts',(0.543834568282501,-3.4349063722726,
14.4528147904804));
#258045=CARTESIAN_POINT('Ctrl Pts',(3.18127829981716,-1.40492213415736,
14.6116369310352));
#258046=CARTESIAN_POINT('Ctrl Pts',(2.90505725017418,1.9118002503249,14.7704590715898));
#258047=CARTESIAN_POINT('Ctrl Pts',(-0.0318436267028579,3.47754565856303,
14.9292812121446));
#258048=CARTESIAN_POINT('Ctrl Pts',(-2.93957960667686,1.85828134573937,
15.0881033526993));
#258049=CARTESIAN_POINT('Ctrl Pts',(-3.15501747116491,-1.46294312280557,
15.2469254932541));
#258050=CARTESIAN_POINT('Ctrl Pts',(-0.480842285992692,-3.44428926195945,
15.4057476338088));
#258051=CARTESIAN_POINT('Ctrl Pts',(2.63372606881953,-2.27108450265052,
15.5645697743635));
#258052=CARTESIAN_POINT('Ctrl Pts',(3.33612102454093,0.982157998239916,
15.7233919149182));
#258053=CARTESIAN_POINT('Ctrl Pts',(0.98303405790505,3.3358629866454,15.882214055473));
#258054=CARTESIAN_POINT('Ctrl Pts',(-2.27039278567272,2.63432238371444,
16.0410361960277));
#258055=CARTESIAN_POINT('Ctrl Pts',(-3.44441541649269,-0.479937769607203,
16.1998583365824));
#258056=CARTESIAN_POINT('Ctrl Pts',(-1.46377160639246,-3.15463318199537,
16.3586804771372));
#258057=CARTESIAN_POINT('Ctrl Pts',(1.85750932300663,-2.94006750410297,
16.5175026176919));
#258058=CARTESIAN_POINT('Ctrl Pts',(3.47753717679189,-0.0327568613626608,
16.6763247582466));
#258059=CARTESIAN_POINT('Ctrl Pts',(1.91256307587166,2.90455510081167,16.8351468988013));
#258060=CARTESIAN_POINT('Ctrl Pts',(-1.40408665323054,3.18164712369646,
16.9939690393561));
#258061=CARTESIAN_POINT('Ctrl Pts',(-3.43476344210255,0.544736605541722,
17.1527911799108));
#258062=CARTESIAN_POINT('Ctrl Pts',(-2.3196138139153,-2.59108659617335,
17.3116133204655));
#258063=CARTESIAN_POINT('Ctrl Pts',(0.920020489026498,-3.35378884142579,
17.4704354610203));
#258064=CARTESIAN_POINT('Ctrl Pts',(3.31702774439061,-1.04482785355944,
17.629257601575));
#258065=CARTESIAN_POINT('Ctrl Pts',(2.67604011115567,2.22106913363951,17.7880797421297));
#258066=CARTESIAN_POINT('Ctrl Pts',(-0.415875269613933,3.45273542005255,
17.9469018826845));
#258067=CARTESIAN_POINT('Ctrl Pts',(-3.12689972259143,1.5221169977168,18.1057240232392));
#258068=CARTESIAN_POINT('Ctrl Pts',(-2.97406292042806,-1.80257936487827,
18.2645461637939));
#258069=CARTESIAN_POINT('Ctrl Pts',(-0.0973467147452378,-3.47632509558314,
18.4233683043487));
#258070=CARTESIAN_POINT('Ctrl Pts',(2.86852963721998,-1.96619184410605,
18.5821904449033));
#258071=CARTESIAN_POINT('Ctrl Pts',(3.20717649298447,1.34475902352235,18.7410125854581));
#258072=CARTESIAN_POINT('Ctrl Pts',(0.608447614599921,3.42402698400585,
18.8998347260128));
#258073=CARTESIAN_POINT('Ctrl Pts',(-2.54756194164184,2.36739133569388,
19.0586568665676));
#258074=CARTESIAN_POINT('Ctrl Pts',(-3.37028244064023,-0.85765834608941,
19.2174790071223));
#258075=CARTESIAN_POINT('Ctrl Pts',(-1.10629353819729,-3.2968706695139,
19.376301147677));
#258076=CARTESIAN_POINT('Ctrl Pts',(2.17104098626288,-2.71717304658282,
19.5351232882318));
#258077=CARTESIAN_POINT('Ctrl Pts',(3.45974584043646,0.352316371405642,
19.6939454287865));
#258078=CARTESIAN_POINT('Ctrl Pts',(1.58016281433192,3.09684713927545,19.8527675693412));
#258079=CARTESIAN_POINT('Ctrl Pts',(-1.74745764228828,3.00943939429467,
20.0115897098959));
#258080=CARTESIAN_POINT('Ctrl Pts',(-3.4730969526798,0.156963003282784,
20.1704118504506));
#258081=CARTESIAN_POINT('Ctrl Pts',(-2.50489101073904,-1.82717661050017,
20.2762932774871));
#258082=CARTESIAN_POINT('Ctrl Pts',(-1.70810875200383,-2.39535560853246,
20.3292339910054));
#258083=CARTESIAN_POINT('',(-1.28892185405321,2.64462557919718,20.));
#258084=CARTESIAN_POINT('Ctrl Pts',(-1.29201753387187,2.6484941502042,20.));
#258085=CARTESIAN_POINT('Ctrl Pts',(-1.35308056853875,2.61168945411392,
20.));
#258086=CARTESIAN_POINT('Ctrl Pts',(-1.41257524201938,2.57259309505077,
20.));
#258087=CARTESIAN_POINT('Ctrl Pts',(-1.47035924820557,2.53120495213521,
20.));
#258088=CARTESIAN_POINT('Ctrl Pts',(-1.54864379104185,2.47513317620905,
20.));
#258089=CARTESIAN_POINT('Ctrl Pts',(-1.62379024837904,2.41485613876148,
20.));
#258090=CARTESIAN_POINT('Ctrl Pts',(-1.6956508900262,2.35075252758899,20.));
#258091=CARTESIAN_POINT('Ctrl Pts',(-1.76862788507419,2.28565306830413,
20.));
#258092=CARTESIAN_POINT('Ctrl Pts',(-1.83821666035171,2.21660632168619,
20.));
#258093=CARTESIAN_POINT('Ctrl Pts',(-1.90421889121248,2.14397855279972,
20.));
#258094=CARTESIAN_POINT('Ctrl Pts',(-1.96614898753727,2.0758316937567,20.));
#258095=CARTESIAN_POINT('Ctrl Pts',(-2.02492131194806,2.00453113467257,
20.));
#258096=CARTESIAN_POINT('Ctrl Pts',(-2.08033244291902,1.93036652625872,
20.));
#258097=CARTESIAN_POINT('Ctrl Pts',(-2.08908421298837,1.91865278591904,
20.));
#258098=CARTESIAN_POINT('Ctrl Pts',(-2.09775205259584,1.90686758723073,
20.));
#258099=CARTESIAN_POINT('Ctrl Pts',(-2.10633506565414,1.89501206141369,
20.));
#258100=CARTESIAN_POINT('Ctrl Pts',(-2.1147494360715,1.883389477941,20.));
#258101=CARTESIAN_POINT('Ctrl Pts',(-2.12307703147204,1.87170653313929,
20.));
#258102=CARTESIAN_POINT('Ctrl Pts',(-2.131315873543,1.85996662408695,20.));
#258103=CARTESIAN_POINT('Ctrl Pts',(-2.18649728066684,1.78133607194937,
20.));
#258104=CARTESIAN_POINT('Ctrl Pts',(-2.2377236591346,1.70012099926416,20.));
#258105=CARTESIAN_POINT('Ctrl Pts',(-2.28483930387176,1.61668443511336,
20.));
#258106=CARTESIAN_POINT('Ctrl Pts',(-2.33175427875346,1.53360323494751,
20.));
#258107=CARTESIAN_POINT('Ctrl Pts',(-2.37459374927346,1.44831846308543,
20.));
#258108=CARTESIAN_POINT('Ctrl Pts',(-2.41315551737691,1.3611718656051,20.));
#258109=CARTESIAN_POINT('Ctrl Pts',(-2.45102518317753,1.27558936551363,
20.));
#258110=CARTESIAN_POINT('Ctrl Pts',(-2.48476946641423,1.18821040330778,
20.));
#258111=CARTESIAN_POINT('Ctrl Pts',(-2.51414698808105,1.09935608424961,
20.));
#258112=CARTESIAN_POINT('Ctrl Pts',(-2.52719508595624,1.05989122179956,
20.));
#258113=CARTESIAN_POINT('Ctrl Pts',(-2.53938106790202,1.02013535678853,
20.));
#258114=CARTESIAN_POINT('Ctrl Pts',(-2.55068042718563,0.980117124868435,
20.));
#258115=CARTESIAN_POINT('Ctrl Pts',(-2.55535533199412,0.963560307783975,
20.));
#258116=CARTESIAN_POINT('Ctrl Pts',(-2.55987844483971,0.946958586108546,
20.));
#258117=CARTESIAN_POINT('Ctrl Pts',(-2.56424792226785,0.930314016077816,
20.));
#258118=CARTESIAN_POINT('Ctrl Pts',(-2.56773342049482,0.917036771765441,
20.));
#258119=CARTESIAN_POINT('Ctrl Pts',(-2.57112065866752,0.903733935297233,
20.));
#258120=CARTESIAN_POINT('Ctrl Pts',(-2.574406132533,0.890417896529939,20.));
#258121=CARTESIAN_POINT('Ctrl Pts',(-2.59638017612545,0.801357009628399,
20.));
#258122=CARTESIAN_POINT('Ctrl Pts',(-2.61384334169276,0.711566154968481,
20.));
#258123=CARTESIAN_POINT('Ctrl Pts',(-2.62661790150812,0.621356934352257,
20.));
#258124=CARTESIAN_POINT('Ctrl Pts',(-2.63902788351211,0.5337222275113,20.));
#258125=CARTESIAN_POINT('Ctrl Pts',(-2.64701305177373,0.445691945839366,
20.));
#258126=CARTESIAN_POINT('Ctrl Pts',(-2.65036239442747,0.357554648287183,
20.));
#258127=CARTESIAN_POINT('Ctrl Pts',(-2.65333726456503,0.279271521835412,
20.));
#258128=CARTESIAN_POINT('Ctrl Pts',(-2.65265441549259,0.200903685880382,
20.));
#258129=CARTESIAN_POINT('Ctrl Pts',(-2.64813257022355,0.122662167407797,
20.));
#258130=CARTESIAN_POINT('Ctrl Pts',(-2.64512361303306,0.0705981613229452,
20.));
#258131=CARTESIAN_POINT('Ctrl Pts',(-2.64041394214298,0.018590270709511,
20.));
#258132=CARTESIAN_POINT('Ctrl Pts',(-2.63403298703025,-0.033295129085088,
20.));
#258133=CARTESIAN_POINT('Ctrl Pts',(-2.63152917116831,-0.0536543832584386,
20.));
#258134=CARTESIAN_POINT('Ctrl Pts',(-2.62876798190389,-0.0739947427382281,
20.));
#258135=CARTESIAN_POINT('Ctrl Pts',(-2.62575102113751,-0.09431205197893,
20.));
#258136=CARTESIAN_POINT('Ctrl Pts',(-2.62396534248827,-0.106337460371819,
20.));
#258137=CARTESIAN_POINT('Ctrl Pts',(-2.62209016838413,-0.118353727017597,
20.));
#258138=CARTESIAN_POINT('Ctrl Pts',(-2.62012761849013,-0.130350157446536,
20.));
#258139=CARTESIAN_POINT('Ctrl Pts',(-2.60589970539201,-0.217320771621497,
20.));
#258140=CARTESIAN_POINT('Ctrl Pts',(-2.58706315697293,-0.303391223847671,
20.));
#258141=CARTESIAN_POINT('Ctrl Pts',(-2.56384391335586,-0.38826985486937,
20.));
#258142=CARTESIAN_POINT('Ctrl Pts',(-2.54023125732743,-0.474586616583607,
20.));
#258143=CARTESIAN_POINT('Ctrl Pts',(-2.51208561519729,-0.559671701455797,
20.));
#258144=CARTESIAN_POINT('Ctrl Pts',(-2.47959660063743,-0.643195714463827,
20.));
#258145=CARTESIAN_POINT('Ctrl Pts',(-2.44745273696693,-0.725832400239446,
20.));
#258146=CARTESIAN_POINT('Ctrl Pts',(-2.41105660996257,-0.806941724285991,
20.));
#258147=CARTESIAN_POINT('Ctrl Pts',(-2.37055459062379,-0.886170933862585,
20.));
#258148=CARTESIAN_POINT('Ctrl Pts',(-2.35442910138672,-0.917715281209858,
20.));
#258149=CARTESIAN_POINT('Ctrl Pts',(-2.3376524018868,-0.948961164264044,
20.));
#258150=CARTESIAN_POINT('Ctrl Pts',(-2.32023242312333,-0.979884425452891,
20.));
#258151=CARTESIAN_POINT('Ctrl Pts',(-2.31191361326991,-0.994651649533392,
20.));
#258152=CARTESIAN_POINT('Ctrl Pts',(-2.30344809480684,-1.009345282903,20.));
#258153=CARTESIAN_POINT('Ctrl Pts',(-2.29483668091622,-1.02396259612013,
20.));
#258154=CARTESIAN_POINT('Ctrl Pts',(-2.28734968907845,-1.03667127626685,
20.));
#258155=CARTESIAN_POINT('Ctrl Pts',(-2.27975321692475,-1.04932077027146,
20.));
#258156=CARTESIAN_POINT('Ctrl Pts',(-2.27205422236239,-1.06189926689777,
20.));
#258157=CARTESIAN_POINT('Ctrl Pts',(-2.22635340848745,-1.13656454019917,
20.));
#258158=CARTESIAN_POINT('Ctrl Pts',(-2.17698444175376,-1.20883151645312,
20.));
#258159=CARTESIAN_POINT('Ctrl Pts',(-2.12411390333182,-1.27837441920937,
20.));
#258160=CARTESIAN_POINT('Ctrl Pts',(-2.07364971882218,-1.3447521407302,
20.));
#258161=CARTESIAN_POINT('Ctrl Pts',(-2.01999471848565,-1.4086484336108,
20.));
#258162=CARTESIAN_POINT('Ctrl Pts',(-1.9632684582212,-1.46974240857356,
20.));
#258163=CARTESIAN_POINT('Ctrl Pts',(-1.94362308304001,-1.49090040583722,
20.));
#258164=CARTESIAN_POINT('Ctrl Pts',(-1.92360916867631,-1.51172193809043,
20.));
#258165=CARTESIAN_POINT('Ctrl Pts',(-1.90323115841627,-1.53219245375308,
20.));
#258166=CARTESIAN_POINT('Ctrl Pts',(-1.88918447856243,-1.54630289811379,
20.));
#258167=CARTESIAN_POINT('Ctrl Pts',(-1.87496284084597,-1.56024823878356,
20.));
#258168=CARTESIAN_POINT('Ctrl Pts',(-1.86058497339293,-1.57400746720644,
20.));
#258169=CARTESIAN_POINT('Ctrl Pts',(-1.79998491988447,-1.63200007156065,
20.));
#258170=CARTESIAN_POINT('Ctrl Pts',(-1.73654958268729,-1.68675391438818,
20.));
#258171=CARTESIAN_POINT('Ctrl Pts',(-1.67041279855624,-1.73795012014107,
20.));
#258172=CARTESIAN_POINT('Ctrl Pts',(-1.60614828232035,-1.78769701121008,
20.));
#258173=CARTESIAN_POINT('Ctrl Pts',(-1.53933251541267,-1.83408516483458,
20.));
#258174=CARTESIAN_POINT('Ctrl Pts',(-1.47007091945726,-1.87677627180768,
20.));
#258175=CARTESIAN_POINT('Ctrl Pts',(-1.43952854209994,-1.8956018255794,
20.));
#258176=CARTESIAN_POINT('Ctrl Pts',(-1.40851038026661,-1.91370783080608,
20.));
#258177=CARTESIAN_POINT('Ctrl Pts',(-1.37702479013087,-1.93106208855776,
20.));
#258178=CARTESIAN_POINT('Ctrl Pts',(-2.94150036975487,-0.00272063203504856,
19.1778238829104));
#258179=CARTESIAN_POINT('Ctrl Pts',(-2.94371245543113,-0.247097874156059,
19.1910422576477));
#258180=CARTESIAN_POINT('Ctrl Pts',(-2.91580747959954,-0.490974180238699,
19.204260632385));
#258181=CARTESIAN_POINT('Ctrl Pts',(-2.85583087373334,-0.726685453029614,
19.2174790071223));
#258182=CARTESIAN_POINT('Ctrl Pts',(-2.61561947315925,-1.67072912056425,
19.2704197206405));
#258183=CARTESIAN_POINT('Ctrl Pts',(-1.86095650567826,-2.48379989503908,
19.3233604341588));
#258184=CARTESIAN_POINT('Ctrl Pts',(-0.937402601194396,-2.79371901178798,
19.376301147677));
#258185=CARTESIAN_POINT('Ctrl Pts',(-0.0138486967105547,-3.10363812853687,
19.4292418611953));
#258186=CARTESIAN_POINT('Ctrl Pts',(1.07859614477614,-2.91040558755985,
19.4821825747135));
#258187=CARTESIAN_POINT('Ctrl Pts',(1.83960270788176,-2.30220774740661,
19.5351232882317));
#258188=CARTESIAN_POINT('Ctrl Pts',(2.60060927098739,-1.69400990725336,
19.58806400175));
#258189=CARTESIAN_POINT('Ctrl Pts',(3.03017755571193,-0.670846767923846,
19.6410047152682));
#258190=CARTESIAN_POINT('Ctrl Pts',(2.9316978603901,0.298156596385862,19.6939454287865));
#258191=CARTESIAN_POINT('Ctrl Pts',(2.83321816506828,1.26715996069558,19.7468861423047));
#258192=CARTESIAN_POINT('Ctrl Pts',(2.2066904897001,2.18200354998551,19.7998268558229));
#258193=CARTESIAN_POINT('Ctrl Pts',(1.33882324257931,2.62485738713369,19.8527675693412));
#258194=CARTESIAN_POINT('Ctrl Pts',(0.534286772812256,3.03539490187918,
19.9018450462275));
#258195=CARTESIAN_POINT('Ctrl Pts',(-0.477651922143633,3.04031420760226,
19.9509225231137));
#258196=CARTESIAN_POINT('Ctrl Pts',(-1.29201753387187,2.6484941502042,20.));
#258197=CARTESIAN_POINT('',(-1.37702479013099,-1.93106208855767,0.));
#258198=CARTESIAN_POINT('Ctrl Pts',(-1.38000136014985,-1.93372567510039,
-5.3776427755281E-17));
#258199=CARTESIAN_POINT('Ctrl Pts',(-1.43101535044438,-1.90597970583003,
-6.22176958538883E-17));
#258200=CARTESIAN_POINT('Ctrl Pts',(-1.48084385890449,-1.87629002335049,
-1.38602792231131E-16));
#258201=CARTESIAN_POINT('Ctrl Pts',(-1.52936200486733,-1.84468127109107,
-1.61329283265843E-16));
#258202=CARTESIAN_POINT('Ctrl Pts',(-1.59766408851972,-1.800183617726,-1.92502189234508E-16));
#258203=CARTESIAN_POINT('Ctrl Pts',(-1.66337061633866,-1.75188515356435,
-7.54981138379841E-17));
#258204=CARTESIAN_POINT('Ctrl Pts',(-1.72639642843817,-1.70014539872556,
-3.12250225675825E-16));
#258205=CARTESIAN_POINT('Ctrl Pts',(-1.76317324629481,-1.6699542202819,
-4.50399802875828E-16));
#258206=CARTESIAN_POINT('Ctrl Pts',(-1.79903699951223,-1.63859032242655,
-3.1031875783162E-17));
#258207=CARTESIAN_POINT('Ctrl Pts',(-1.83396765709214,-1.60611776805061,
-1.38777878078145E-16));
#258208=CARTESIAN_POINT('Ctrl Pts',(-1.84847964786871,-1.59262699970429,
-1.83541106137601E-16));
#258209=CARTESIAN_POINT('Ctrl Pts',(-1.86283055532984,-1.57894481768837,
-1.98430142350905E-16));
#258210=CARTESIAN_POINT('Ctrl Pts',(-1.87701880215806,-1.56507557173329,
-1.87350135405495E-16));
#258211=CARTESIAN_POINT('Ctrl Pts',(-1.8884302860734,-1.55392065745456,
-1.78438581880232E-16));
#258212=CARTESIAN_POINT('Ctrl Pts',(-1.89973595998167,-1.54264518151194,
3.57342686513655E-16));
#258213=CARTESIAN_POINT('Ctrl Pts',(-1.91092588736256,-1.53126101376045,
3.12250225675825E-16));
#258214=CARTESIAN_POINT('Ctrl Pts',(-1.97083426275634,-1.47031271874583,
7.08352477809135E-17));
#258215=CARTESIAN_POINT('Ctrl Pts',(-2.02749743984676,-1.40618475518815,
-8.11534412475848E-16));
#258216=CARTESIAN_POINT('Ctrl Pts',(-2.08082093919753,-1.33926925427454,
-5.48172618408671E-16));
#258217=CARTESIAN_POINT('Ctrl Pts',(-2.12725152044828,-1.2810036558061,
-3.1885456301731E-16));
#258218=CARTESIAN_POINT('Ctrl Pts',(-2.17114995783034,-1.2206234746831,
9.75718645724583E-17));
#258219=CARTESIAN_POINT('Ctrl Pts',(-2.21243810966654,-1.15835938453353,
1.66533453693773E-16));
#258220=CARTESIAN_POINT('Ctrl Pts',(-2.23225460122457,-1.12847536788602,
1.99631974404344E-16));
#258221=CARTESIAN_POINT('Ctrl Pts',(-2.25146955036191,-1.09815702694957,
-1.08310280677544E-16));
#258222=CARTESIAN_POINT('Ctrl Pts',(-2.2700728366736,-1.06742810552577,
-9.71445146547012E-17));
#258223=CARTESIAN_POINT('Ctrl Pts',(-2.28179995764522,-1.04805723885056,
-9.01058502651499E-17));
#258224=CARTESIAN_POINT('Ctrl Pts',(-2.29328723219393,-1.02851724410871,
-1.76640528435757E-16));
#258225=CARTESIAN_POINT('Ctrl Pts',(-2.30451408383319,-1.00884594392475,
-1.80411241501588E-16));
#258226=CARTESIAN_POINT('Ctrl Pts',(-2.34846160948551,-0.931842613229072,
-1.95171702805683E-16));
#258227=CARTESIAN_POINT('Ctrl Pts',(-2.38846508399537,-0.852762706837416,
-1.08344740154023E-16));
#258228=CARTESIAN_POINT('Ctrl Pts',(-2.42442591717442,-0.772002953652072,
-1.38777878078145E-17));
#258229=CARTESIAN_POINT('Ctrl Pts',(-2.46263172560052,-0.686201502852074,
8.64865798909936E-17));
#258230=CARTESIAN_POINT('Ctrl Pts',(-2.49627541606281,-0.598503422002609,
-1.68069008667652E-16));
#258231=CARTESIAN_POINT('Ctrl Pts',(-2.52519947762592,-0.509336114470687,
-2.91433543964104E-16));
#258232=CARTESIAN_POINT('Ctrl Pts',(-2.54689252379825,-0.442460633821745,
-3.83956945436442E-16));
#258233=CARTESIAN_POINT('Ctrl Pts',(-2.56593002240835,-0.374757582045608,
2.75043757311674E-16));
#258234=CARTESIAN_POINT('Ctrl Pts',(-2.58222700004388,-0.306394258608983,
3.33066907387547E-16));
#258235=CARTESIAN_POINT('Ctrl Pts',(-2.59444973327053,-0.255121766031515,
3.76584269944452E-16));
#258236=CARTESIAN_POINT('Ctrl Pts',(-2.60513060989885,-0.203477624456378,
-3.29320581511714E-17));
#258237=CARTESIAN_POINT('Ctrl Pts',(-2.61422692989439,-0.151529773561905,
0.));
#258238=CARTESIAN_POINT('Ctrl Pts',(-2.61684954307657,-0.136552385056628,
9.49483415994306E-18));
#258239=CARTESIAN_POINT('Ctrl Pts',(-2.61934039841294,-0.121549739952084,
1.11903402599329E-17));
#258240=CARTESIAN_POINT('Ctrl Pts',(-2.62169837307482,-0.106523444586755,
0.));
#258241=CARTESIAN_POINT('Ctrl Pts',(-2.62406378639396,-0.0914497460567891,
-1.12256422108653E-17));
#258242=CARTESIAN_POINT('Ctrl Pts',(-2.62629415830334,-0.0763603840706239,
2.83678833725852E-16));
#258243=CARTESIAN_POINT('Ctrl Pts',(-2.62838787459448,-0.0612642678389218,
2.77555756156289E-16));
#258244=CARTESIAN_POINT('Ctrl Pts',(-2.64110515406688,0.0304298790130256,
2.40364046366038E-16));
#258245=CARTESIAN_POINT('Ctrl Pts',(-2.64879705700742,0.122452682837918,
1.35678568928957E-16));
#258246=CARTESIAN_POINT('Ctrl Pts',(-2.65132822859212,0.21441013312469,
1.38777878078145E-16));
#258247=CARTESIAN_POINT('Ctrl Pts',(-2.65228737650166,0.249255971606106,
1.39952312837697E-16));
#258248=CARTESIAN_POINT('Ctrl Pts',(-2.65250504989958,0.284092732465562,
-6.80384553331465E-17));
#258249=CARTESIAN_POINT('Ctrl Pts',(-2.65197217923219,0.318899937974375,
-5.55111512312578E-17));
#258250=CARTESIAN_POINT('Ctrl Pts',(-2.65061524597764,0.407535056292549,
-2.36108861841977E-17));
#258251=CARTESIAN_POINT('Ctrl Pts',(-2.64439528531828,0.495977946818749,
-1.03572650581825E-16));
#258252=CARTESIAN_POINT('Ctrl Pts',(-2.63355716179701,0.583967053320013,
-1.94289029309402E-16));
#258253=CARTESIAN_POINT('Ctrl Pts',(-2.62250057345816,0.673729762425441,
-2.868339844591E-16));
#258254=CARTESIAN_POINT('Ctrl Pts',(-2.60663767123318,0.763020939005978,
-7.23771563560485E-17));
#258255=CARTESIAN_POINT('Ctrl Pts',(-2.58617447009765,0.851566464826489,
-1.11022302462516E-16));
#258256=CARTESIAN_POINT('Ctrl Pts',(-2.58109483477611,0.873546358272459,
-1.20615290767153E-16));
#258257=CARTESIAN_POINT('Ctrl Pts',(-2.57573148044371,0.895480291325348,
2.39702298114726E-16));
#258258=CARTESIAN_POINT('Ctrl Pts',(-2.57008706945311,0.917364020427546,
2.4980018054066E-16));
#258259=CARTESIAN_POINT('Ctrl Pts',(-2.56640505109836,0.931639432398567,
2.56387331706348E-16));
#258260=CARTESIAN_POINT('Ctrl Pts',(-2.56260537556786,0.94588580938044,
4.94036337426619E-18));
#258261=CARTESIAN_POINT('Ctrl Pts',(-2.55869076374861,0.960096434692657,
0.));
#258262=CARTESIAN_POINT('Ctrl Pts',(-2.53409586674846,1.04937958254999,
-3.10395344274081E-17));
#258263=CARTESIAN_POINT('Ctrl Pts',(-2.50495054498212,1.13732018527145,
-2.59292046237921E-16));
#258264=CARTESIAN_POINT('Ctrl Pts',(-2.47154363309989,1.22363519951094,
-2.22044604925031E-16));
#258265=CARTESIAN_POINT('Ctrl Pts',(-2.43749715253502,1.31160269752815,
-1.84084068757516E-16));
#258266=CARTESIAN_POINT('Ctrl Pts',(-2.39902417803456,1.39788255512328,
1.18743150656401E-16));
#258267=CARTESIAN_POINT('Ctrl Pts',(-2.35637502831346,1.48217800192524,
1.38777878078145E-16));
#258268=CARTESIAN_POINT('Ctrl Pts',(-2.31337208634223,1.56717271415208,
1.58978801809585E-16));
#258269=CARTESIAN_POINT('Ctrl Pts',(-2.26612310346488,1.65015083103388,
-2.12641302436217E-17));
#258270=CARTESIAN_POINT('Ctrl Pts',(-2.21483250272833,1.73079835854605,
0.));
#258271=CARTESIAN_POINT('Ctrl Pts',(-2.18408162452443,1.77914995241235,
1.27487428465136E-17));
#258272=CARTESIAN_POINT('Ctrl Pts',(-2.15187700314947,1.82666356774367,
-1.93359933520376E-16));
#258273=CARTESIAN_POINT('Ctrl Pts',(-2.11825450271608,1.87326783752673,
-2.22044604925031E-16));
#258274=CARTESIAN_POINT('Ctrl Pts',(-2.10898884344645,1.88611100144236,
-2.29949501588597E-16));
#258275=CARTESIAN_POINT('Ctrl Pts',(-2.09961449121588,1.89888626983332,
-3.51687330639502E-16));
#258276=CARTESIAN_POINT('Ctrl Pts',(-2.09014358815089,1.9115771165726,-3.33066907387547E-16));
#258277=CARTESIAN_POINT('Ctrl Pts',(-2.03133347089822,1.99038165924946,
-2.17442318345972E-16));
#258278=CARTESIAN_POINT('Ctrl Pts',(-1.9687115216203,2.06606315861356,-3.78880423800246E-16));
#258279=CARTESIAN_POINT('Ctrl Pts',(-1.90254904260934,2.13831227552401,
-3.33066907387547E-16));
#258280=CARTESIAN_POINT('Ctrl Pts',(-1.83622830911578,2.21073420558757,
-2.87143809313996E-16));
#258281=CARTESIAN_POINT('Ctrl Pts',(-1.76634968788036,2.27970821505394,
1.19516948523233E-16));
#258282=CARTESIAN_POINT('Ctrl Pts',(-1.69313645008632,2.34490696177326,
1.66533453693773E-16));
#258283=CARTESIAN_POINT('Ctrl Pts',(-1.62134465410955,2.40883986876451,
2.12637129046033E-16));
#258284=CARTESIAN_POINT('Ctrl Pts',(-1.54634593780016,2.46914345344329,
3.88578058618805E-16));
#258285=CARTESIAN_POINT('Ctrl Pts',(-1.4683099737214,2.52548168087978,3.88578058618805E-16));
#258286=CARTESIAN_POINT('Ctrl Pts',(-1.4101809347186,2.56744806213316,3.88578058618805E-16));
#258287=CARTESIAN_POINT('Ctrl Pts',(-1.35036573192052,2.60721367515221,
1.51746623653549E-17));
#258288=CARTESIAN_POINT('Ctrl Pts',(-1.28892185405322,2.64462557919718,
0.));
#258289=CARTESIAN_POINT('Ctrl Pts',(-1.38000136014988,-1.93372567510037,
-2.60100101179273E-15));
#258290=CARTESIAN_POINT('Ctrl Pts',(-0.784688350722177,-2.35371652554116,
0.0490774768862665));
#258291=CARTESIAN_POINT('Ctrl Pts',(0.889177499330816,-2.62573605996334,
0.151095667290779));
#258292=CARTESIAN_POINT('Ctrl Pts',(2.70389566823784,-0.740895185834261,
0.306054571213535));
#258293=CARTESIAN_POINT('Ctrl Pts',(2.08805286496322,1.8712628391822,0.464876711768264));
#258294=CARTESIAN_POINT('Ctrl Pts',(-0.440526185828228,2.76865345984501,
0.623698852322994));
#258295=CARTESIAN_POINT('Ctrl Pts',(-2.15180306555184,1.44961829294084,
0.751603245701911));
#258296=CARTESIAN_POINT('Ctrl Pts',(-2.36960890551819,0.330372416157857,
0.826566925562585));
#258297=CARTESIAN_POINT('Ctrl Pts',(-2.36829764012707,0.00106700769158283,
0.848589891905016));
#258298=CARTESIAN_POINT('Origin',(0.,0.,-1.84858989190501));
#258299=CARTESIAN_POINT('',(1.37702479013102,-1.93106208855765,0.));
#258300=CARTESIAN_POINT('Origin',(0.,0.,0.));
#258301=CARTESIAN_POINT('Ctrl Pts',(1.37702479013101,-1.93106208855765,
-2.4980018054066E-15));
#258302=CARTESIAN_POINT('Ctrl Pts',(2.01936616407906,-1.47301363900524,
0.0529407135182407));
#258303=CARTESIAN_POINT('Ctrl Pts',(2.79990526463056,0.126536631817626,
0.158822140554727));
#258304=CARTESIAN_POINT('Ctrl Pts',(1.40874583290953,2.42611875140058,0.317644281109456));
#258305=CARTESIAN_POINT('Ctrl Pts',(-1.27387826991474,2.49658204560485,
0.476466421664188));
#258306=CARTESIAN_POINT('Ctrl Pts',(-2.33532317779642,0.946682230744997,
0.587721697326026));
#258307=CARTESIAN_POINT('Ctrl Pts',(-2.37517596458242,0.081324476190725,
0.646036259469624));
#258308=CARTESIAN_POINT('Ctrl Pts',(-2.37462805812147,0.00152502885334119,
0.651410108094978));
#258309=CARTESIAN_POINT('Ctrl Pts',(1.70810875200395,-2.39535560853238,
-0.329233991005387));
#258310=CARTESIAN_POINT('Ctrl Pts',(2.50489101073913,-1.82717661050005,
-0.276293277487143));
#258311=CARTESIAN_POINT('Ctrl Pts',(3.47309846676214,0.156960375590738,
-0.170411850450657));
#258312=CARTESIAN_POINT('Ctrl Pts',(1.74745662081582,3.00944086291576,-0.0115897098959277));
#258313=CARTESIAN_POINT('Ctrl Pts',(-1.58016227262108,3.09684594842185,
0.147232430658803));
#258314=CARTESIAN_POINT('Ctrl Pts',(-3.45974587664961,0.352316997116106,
0.306054571213531));
#258315=CARTESIAN_POINT('Ctrl Pts',(-2.17104076685187,-2.71717329882319,
0.464876711768262));
#258316=CARTESIAN_POINT('Ctrl Pts',(1.10629343072135,-3.2968702555127,0.62369885232299));
#258317=CARTESIAN_POINT('Ctrl Pts',(3.37028228423513,-0.857658442232281,
0.782520992877721));
#258318=CARTESIAN_POINT('Ctrl Pts',(2.54756179623556,2.36739129287567,0.941343133432451));
#258319=CARTESIAN_POINT('Ctrl Pts',(-0.608447577806647,3.42402675434335,
1.10016527398718));
#258320=CARTESIAN_POINT('Ctrl Pts',(-3.20717632466629,1.34475897960982,
1.25898741454191));
#258321=CARTESIAN_POINT('Ctrl Pts',(-2.86852948418392,-1.96619175536868,
1.41780955509664));
#258322=CARTESIAN_POINT('Ctrl Pts',(0.097346709292227,-3.47632490222585,
1.57663169565137));
#258323=CARTESIAN_POINT('Ctrl Pts',(2.97406276265272,-1.80257927416548,
1.7354538362061));
#258324=CARTESIAN_POINT('Ctrl Pts',(3.12689955660378,1.52211691970352,1.89427597676083));
#258325=CARTESIAN_POINT('Ctrl Pts',(0.415875247528641,3.45273523523294,
2.05309811731556));
#258326=CARTESIAN_POINT('Ctrl Pts',(-2.67603996909776,2.22106901660608,
2.21192025787029));
#258327=CARTESIAN_POINT('Ctrl Pts',(-3.31702756833606,-1.04482779857665,
2.37074239842501));
#258328=CARTESIAN_POINT('Ctrl Pts',(-0.92002044018298,-3.35378866314487,
2.52956453897975));
#258329=CARTESIAN_POINT('Ctrl Pts',(2.31961369078498,-2.5910864587838,2.68838667953447));
#258330=CARTESIAN_POINT('Ctrl Pts',(3.4347632597901,0.54473657670683,2.84720882008921));
#258331=CARTESIAN_POINT('Ctrl Pts',(1.40408657869956,3.18164695477209,3.00603096064393));
#258332=CARTESIAN_POINT('Ctrl Pts',(-1.91256297435207,2.90455494666245,
3.16485310119866));
#258333=CARTESIAN_POINT('Ctrl Pts',(-3.47753699220607,-0.0327568596370786,
3.3236752417534));
#258334=CARTESIAN_POINT('Ctrl Pts',(-1.85750922440995,-2.94006734803805,
3.48249738230812));
#258335=CARTESIAN_POINT('Ctrl Pts',(1.46377152869574,-3.15463301455215,
3.64131952286286));
#258336=CARTESIAN_POINT('Ctrl Pts',(3.4444152336643,-0.479937744130016,
3.80014166341758));
#258337=CARTESIAN_POINT('Ctrl Pts',(2.27039266516074,2.63432224388432,3.95896380397232));
#258338=CARTESIAN_POINT('Ctrl Pts',(-0.983034005725968,3.33586280957935,
4.11778594452704));
#258339=CARTESIAN_POINT('Ctrl Pts',(-3.33612084746066,0.982157946106786,
4.27660808508178));
#258340=CARTESIAN_POINT('Ctrl Pts',(-2.63372592902202,-2.27108438210191,
4.4354302256365));
#258341=CARTESIAN_POINT('Ctrl Pts',(0.480842260469829,-3.44428907913767,
4.59425236619123));
#258342=CARTESIAN_POINT('Ctrl Pts',(3.15501730369756,-1.46294304515281,
4.75307450674596));
#258343=CARTESIAN_POINT('Ctrl Pts',(2.93957945064476,1.8582812471024,4.9118966473007));
#258344=CARTESIAN_POINT('Ctrl Pts',(0.0318436250124843,3.47754547397594,
5.07071878785541));
#258345=CARTESIAN_POINT('Ctrl Pts',(-2.90505709597467,1.91180014884698,
5.22954092841015));
#258346=CARTESIAN_POINT('Ctrl Pts',(-3.18127813095577,-1.40492205958462,
5.38836306896487));
#258347=CARTESIAN_POINT('Ctrl Pts',(-0.543834539415804,-3.43490618994878,
5.54718520951961));
#258348=CARTESIAN_POINT('Ctrl Pts',(2.59169547995281,-2.31893317695855,
5.70600735007433));
#258349=CARTESIAN_POINT('Ctrl Pts',(3.35354701796656,0.920901155550854,
5.86482949062907));
#258350=CARTESIAN_POINT('Ctrl Pts',(1.04395653884046,3.31730180794877,6.0236516311838));
#258351=CARTESIAN_POINT('Ctrl Pts',(-2.22177141510979,2.6754566561633,6.18247377173853));
#258352=CARTESIAN_POINT('Ctrl Pts',(-3.45262642996333,-0.416782047509506,
6.34129591229325));
#258353=CARTESIAN_POINT('Ctrl Pts',(-1.52129471248139,-3.12729898439273,
6.50011805284799));
#258354=CARTESIAN_POINT('Ctrl Pts',(1.80335830788818,-2.97358964105309,
6.65894019340271));
#258355=CARTESIAN_POINT('Ctrl Pts',(3.47635400867004,-0.0964331188513625,
6.81776233395745));
#258356=CARTESIAN_POINT('Ctrl Pts',(1.96543139505884,2.86904443523007,6.97658447451217));
#258357=CARTESIAN_POINT('Ctrl Pts',(-1.34558781366435,3.20682552935541,
7.13540661506691));
#258358=CARTESIAN_POINT('Ctrl Pts',(-3.42421191162923,0.607543680951476,
7.29422875562163));
#258359=CARTESIAN_POINT('Ctrl Pts',(-2.36667352711723,-2.54817443595411,
7.45305089617636));
#258360=CARTESIAN_POINT('Ctrl Pts',(0.858450542967834,-3.37007406525225,
7.6118730367311));
#258361=CARTESIAN_POINT('Ctrl Pts',(3.29733811385309,-1.10539490813885,
7.77069517728582));
#258362=CARTESIAN_POINT('Ctrl Pts',(2.71626420116681,2.1716918127274,7.92951731784056));
#258363=CARTESIAN_POINT('Ctrl Pts',(-0.352578021437311,3.45977243165023,
8.08833945839528));
#258364=CARTESIAN_POINT('Ctrl Pts',(-3.09850157209174,1.57912144806933,
8.24716159895001));
#258365=CARTESIAN_POINT('Ctrl Pts',(-3.0065737767802,-1.74781310922686,
8.40598373950474));
#258366=CARTESIAN_POINT('Ctrl Pts',(-0.160989337873077,-3.47396300686965,
8.56480588005947));
#258367=CARTESIAN_POINT('Ctrl Pts',(2.83204179374651,-2.01838445755032,
8.72362802061421));
#258368=CARTESIAN_POINT('Ctrl Pts',(3.23126639365278,1.28578926471553,8.88245016116893));
#258369=CARTESIAN_POINT('Ctrl Pts',(0.671043185949358,3.41233608875187,
9.04127230172366));
#258370=CARTESIAN_POINT('Ctrl Pts',(-2.5037741293059,2.41359724258752,9.20009444227838));
#258371=CARTESIAN_POINT('Ctrl Pts',(-3.38543824856365,-0.795703716951166,
9.35891658283312));
#258372=CARTESIAN_POINT('Ctrl Pts',(-1.16645185439101,-3.27623665375311,
9.51773872338784));
#258373=CARTESIAN_POINT('Ctrl Pts',(2.12086285524974,-2.75613448315381,
9.67656086394259));
#258374=CARTESIAN_POINT('Ctrl Pts',(3.46572461841138,0.288252336235001,
9.8353830044973));
#258375=CARTESIAN_POINT('Ctrl Pts',(1.63640329846855,3.06863500351032,9.99420514505204));
#258376=CARTESIAN_POINT('Ctrl Pts',(-1.69166481732213,3.03852047645593,
10.1530272856068));
#258377=CARTESIAN_POINT('Ctrl Pts',(-3.47037329360166,0.225490006572311,
10.3118494261615));
#258378=CARTESIAN_POINT('Ctrl Pts',(-2.07064106455555,-2.79406193950383,
10.4706715667162));
#258379=CARTESIAN_POINT('Ctrl Pts',(1.22554704658151,-3.25459229038338,
10.629493707271));
#258380=CARTESIAN_POINT('Ctrl Pts',(3.39928281913928,-0.734311143529869,
10.7883158478257));
#258381=CARTESIAN_POINT('Ctrl Pts',(2.45968813206418,2.45850988059642,10.9471379883804));
#258382=CARTESIAN_POINT('Ctrl Pts',(-0.732682328664183,3.39963426639848,
11.1059601289351));
#258383=CARTESIAN_POINT('Ctrl Pts',(-3.25400470883227,1.22710630953676,
11.2647822694899));
#258384=CARTESIAN_POINT('Ctrl Pts',(-2.79505374464792,-2.06930208150895,
11.4236044100446));
#258385=CARTESIAN_POINT('Ctrl Pts',(0.223827187860361,-3.47048093640955,
11.5824265505993));
#258386=CARTESIAN_POINT('Ctrl Pts',(3.03770958428446,-1.69312049823808,
11.7412486911541));
#258387=CARTESIAN_POINT('Ctrl Pts',(3.06941871668279,1.63493280647403,11.9000708317088));
#258388=CARTESIAN_POINT('Ctrl Pts',(0.289912868611965,3.46558610751786,
12.0588929722635));
#258389=CARTESIAN_POINT('Ctrl Pts',(-2.75511797767527,2.12218318462333,
12.2177151128182));
#258390=CARTESIAN_POINT('Ctrl Pts',(-3.27679517080862,-1.16488194619576,
12.376537253373));
#258391=CARTESIAN_POINT('Ctrl Pts',(-0.797325722710365,-3.38505660689921,
12.5353593939277));
#258392=CARTESIAN_POINT('Ctrl Pts',(2.41239730852211,-2.50493029161351,
12.6941815344824));
#258393=CARTESIAN_POINT('Ctrl Pts',(3.41265722033696,0.669408124009311,
12.8530036750372));
#258394=CARTESIAN_POINT('Ctrl Pts',(1.28733734439784,3.23064995035462,13.0118258155919));
#258395=CARTESIAN_POINT('Ctrl Pts',(-2.01702728285485,2.83300855632784,
13.1706479561466));
#258396=CARTESIAN_POINT('Ctrl Pts',(-3.47403974444911,-0.159324806591705,
13.3294700967013));
#258397=CARTESIAN_POINT('Ctrl Pts',(-1.7492534767729,-3.0057359854128,13.4882922372561));
#258398=CARTESIAN_POINT('Ctrl Pts',(1.57763665239809,-3.0992578358404,13.6471143778108));
#258399=CARTESIAN_POINT('Ctrl Pts',(3.45960310046506,-0.354235694502853,
13.8059365183655));
#258400=CARTESIAN_POINT('Ctrl Pts',(2.17299303284069,2.71522334610484,13.9647586589203));
#258401=CARTESIAN_POINT('Ctrl Pts',(-1.10381489640987,3.29786737369376,
14.123580799475));
#258402=CARTESIAN_POINT('Ctrl Pts',(-3.36966236087009,0.860065179937116,
14.2824029400297));
#258403=CARTESIAN_POINT('Ctrl Pts',(-2.54930811016128,-2.36545232449735,
14.4412250805845));
#258404=CARTESIAN_POINT('Ctrl Pts',(0.605902936125663,-3.42450261673412,
14.6000472211392));
#258405=CARTESIAN_POINT('Ctrl Pts',(3.20618043701593,-1.34712417589535,
14.7588693616939));
#258406=CARTESIAN_POINT('Ctrl Pts',(2.86998582166464,1.96405649700715,14.9176915022486));
#258407=CARTESIAN_POINT('Ctrl Pts',(-0.0947674493627475,3.47639981455846,
15.0765136428034));
#258408=CARTESIAN_POINT('Ctrl Pts',(-2.97272523956357,1.80478286502611,
15.2353357833581));
#258409=CARTESIAN_POINT('Ctrl Pts',(-3.12802753778546,-1.51979612541224,
15.3941579239129));
#258410=CARTESIAN_POINT('Ctrl Pts',(-0.418436289233176,-3.45242633702748,
15.5529800644676));
#258411=CARTESIAN_POINT('Ctrl Pts',(2.67439181059374,-2.22305307675472,
15.7118022050223));
#258412=CARTESIAN_POINT('Ctrl Pts',(3.31780162809799,1.04236696836076,15.870624345577));
#258413=CARTESIAN_POINT('Ctrl Pts',(0.922507866308364,3.35310539370922,
16.0294464861318));
#258414=CARTESIAN_POINT('Ctrl Pts',(-2.31769112662919,2.59280627338641,
16.1882686266865));
#258415=CARTESIAN_POINT('Ctrl Pts',(-3.43516636929164,-0.542188675003985,
16.3470907672412));
#258416=CARTESIAN_POINT('Ctrl Pts',(-1.40644617227113,-3.18060461760772,
16.5059129077959));
#258417=CARTESIAN_POINT('Ctrl Pts',(1.91040799810916,-2.90597277104503,
16.6647350483507));
#258418=CARTESIAN_POINT('Ctrl Pts',(3.47756033952126,0.0301773722343488,
16.8235571889054));
#258419=CARTESIAN_POINT('Ctrl Pts',(1.85968948862187,2.93868877516475,16.9823793294602));
#258420=CARTESIAN_POINT('Ctrl Pts',(-1.46143115770309,3.15571782304568,
17.1412014700149));
#258421=CARTESIAN_POINT('Ctrl Pts',(-3.44405834328818,0.48249263808589,
17.3000236105696));
#258422=CARTESIAN_POINT('Ctrl Pts',(-2.27234594795998,-2.63263772394267,
17.4588457511243));
#258423=CARTESIAN_POINT('Ctrl Pts',(0.980559183838789,-3.33659055221275,
17.6176678916791));
#258424=CARTESIAN_POINT('Ctrl Pts',(3.33539176443223,-0.984633196725734,
17.7764900322338));
#258425=CARTESIAN_POINT('Ctrl Pts',(2.63540911147839,2.26913203031142,17.9353121727885));
#258426=CARTESIAN_POINT('Ctrl Pts',(-0.478286064479774,3.4446412945574,
18.0941343133433));
#258427=CARTESIAN_POINT('Ctrl Pts',(-3.15393372518352,1.46528955420501,
18.252956453898));
#258428=CARTESIAN_POINT('Ctrl Pts',(-2.94095238931831,-1.85611307158376,
18.4117785944527));
#258429=CARTESIAN_POINT('Ctrl Pts',(-0.0344319160965253,-3.4774965294809,
18.5706007350074));
#258430=CARTESIAN_POINT('Ctrl Pts',(2.90365509789218,-1.91400096962023,
18.7294228755622));
#258431=CARTESIAN_POINT('Ctrl Pts',(3.1822871338934,1.40265080344969,18.8882450161169));
#258432=CARTESIAN_POINT('Ctrl Pts',(0.546443743866525,3.43433223077365,
19.0470671566716));
#258433=CARTESIAN_POINT('Ctrl Pts',(-2.59009217426645,2.32117885480077,
19.2058892972263));
#258434=CARTESIAN_POINT('Ctrl Pts',(-3.35400480467998,-0.919032408370063,
19.3647114377811));
#258435=CARTESIAN_POINT('Ctrl Pts',(-1.04684590468812,-3.31534029745207,
19.5235335783358));
#258436=CARTESIAN_POINT('Ctrl Pts',(2.22061130085995,-2.6794074717208,19.6823557188906));
#258437=CARTESIAN_POINT('Ctrl Pts',(3.45130747732673,0.418958489924277,
19.8411778594453));
#258438=CARTESIAN_POINT('Ctrl Pts',(2.16862035685408,2.21588336549518,19.9470592864818));
#258439=CARTESIAN_POINT('Ctrl Pts',(1.28892185405323,2.64462557919718,20.));
#258440=CARTESIAN_POINT('Ctrl Pts',(1.59774743137964,-2.24059110187414,
-0.219489327336925));
#258441=CARTESIAN_POINT('Ctrl Pts',(2.34304939518577,-1.70912228666845,
-0.166548613818682));
#258442=CARTESIAN_POINT('Ctrl Pts',(3.24870073271828,0.146819127666371,
-0.0606671867821956));
#258443=CARTESIAN_POINT('Ctrl Pts',(1.63455302484706,2.81500015907737,0.0981549537725337));
#258444=CARTESIAN_POINT('Ctrl Pts',(-1.4780676050523,2.89675798081618,0.256977094327264));
#258445=CARTESIAN_POINT('Ctrl Pts',(-3.23621085669046,0.329553710507722,
0.415799234881993));
#258446=CARTESIAN_POINT('Ctrl Pts',(-2.0307692965032,-2.54161607316561,
0.574621375436723));
#258447=CARTESIAN_POINT('Ctrl Pts',(1.03481554392453,-3.08385866892691,
0.733443515991452));
#258448=CARTESIAN_POINT('Ctrl Pts',(3.15252752867372,-0.802244922327108,
0.892265656546182));
#258449=CARTESIAN_POINT('Ctrl Pts',(2.38296321088507,2.21443356743241,1.05108779710091));
#258450=CARTESIAN_POINT('Ctrl Pts',(-0.569135632277061,3.20279955553706,
1.20990993765564));
#258451=CARTESIAN_POINT('Ctrl Pts',(-2.99995988470017,1.25787377587964,
1.36873207821037));
#258452=CARTESIAN_POINT('Ctrl Pts',(-2.68319309869152,-1.83915562932077,
1.5275542187651));
#258453=CARTESIAN_POINT('Ctrl Pts',(0.0910571148016564,-3.25171870740438,
1.68637635931983));
#258454=CARTESIAN_POINT('Ctrl Pts',(2.78190784645029,-1.68611419019846,
1.84519849987456));
#258455=CARTESIAN_POINT('Ctrl Pts',(2.92486981808652,1.42377257646074,2.00402064042929));
#258456=CARTESIAN_POINT('Ctrl Pts',(0.389005446950427,3.22965317451556,
2.16284278098402));
#258457=CARTESIAN_POINT('Ctrl Pts',(-2.50314037784715,2.07756520891067,
2.32166492153875));
#258458=CARTESIAN_POINT('Ctrl Pts',(-3.1027136128813,-0.977321221175992,
2.48048706209348));
#258459=CARTESIAN_POINT('Ctrl Pts',(-0.860577696469583,-3.13709956444123,
2.63930920264821));
#258460=CARTESIAN_POINT('Ctrl Pts',(2.16974288779722,-2.42367573443284,
2.79813134320294));
#258461=CARTESIAN_POINT('Ctrl Pts',(3.21284237276366,0.509541014406022,
2.95695348375767));
#258462=CARTESIAN_POINT('Ctrl Pts',(1.31336820440729,2.97607997358482,3.1157756243124));
#258463=CARTESIAN_POINT('Ctrl Pts',(-1.78899181684877,2.71689094730438,
3.27459776486713));
#258464=CARTESIAN_POINT('Ctrl Pts',(-3.25285248395709,-0.0306404309935377,
3.43341990542185));
#258465=CARTESIAN_POINT('Ctrl Pts',(-1.73749510303901,-2.75010888381658,
3.59224204597659));
#258466=CARTESIAN_POINT('Ctrl Pts',(1.36919689531271,-2.95081141059244,
3.75106418653131));
#258467=CARTESIAN_POINT('Ctrl Pts',(3.22187073026558,-0.448928850113442,
3.90988632708604));
#258468=CARTESIAN_POINT('Ctrl Pts',(2.12370204457293,2.46411804497485,4.06870846764078));
#258469=CARTESIAN_POINT('Ctrl Pts',(-0.91951994026425,3.12033190462097,
4.2275306081955));
#258470=CARTESIAN_POINT('Ctrl Pts',(-3.12057327061221,0.918700483069451,
4.38635274875024));
#258471=CARTESIAN_POINT('Ctrl Pts',(-2.46356025816037,-2.12434906951483,
4.54517488930496));
#258472=CARTESIAN_POINT('Ctrl Pts',(0.449774925433255,-3.22175272661351,
4.70399702985969));
#258473=CARTESIAN_POINT('Ctrl Pts',(2.951170870723,-1.36842194029234,4.86281917041443));
#258474=CARTESIAN_POINT('Ctrl Pts',(2.74965250959216,1.73821724515814,5.02164131096915));
#258475=CARTESIAN_POINT('Ctrl Pts',(0.0297862006794342,3.25286041771775,
5.18046345152389));
#258476=CARTESIAN_POINT('Ctrl Pts',(-2.71736065262779,1.78827827768449,
5.33928559207861));
#258477=CARTESIAN_POINT('Ctrl Pts',(-2.9757349795647,-1.31414970466982,
5.49810773263333));
#258478=CARTESIAN_POINT('Ctrl Pts',(-0.50869725796305,-3.21297606817014,
5.65692987318808));
#258479=CARTESIAN_POINT('Ctrl Pts',(2.42424540659647,-2.16910634213409,
5.81575201374279));
#258480=CARTESIAN_POINT('Ctrl Pts',(3.13687353201647,0.86140150860402,5.97457415429754));
#258481=CARTESIAN_POINT('Ctrl Pts',(0.976506253742583,3.10297013380615,
6.13339629485226));
#258482=CARTESIAN_POINT('Ctrl Pts',(-2.07822222527677,2.5025947529028,6.29221843540699));
#258483=CARTESIAN_POINT('Ctrl Pts',(-3.2295513991808,-0.389853658364687,
6.45104057596172));
#258484=CARTESIAN_POINT('Ctrl Pts',(-1.42300349224656,-2.92524343874919,
6.60986271651644));
#258485=CARTESIAN_POINT('Ctrl Pts',(1.68684289036347,-2.78146529335191,
6.76868485707118));
#258486=CARTESIAN_POINT('Ctrl Pts',(3.25174593327414,-0.0902025516606631,
6.92750699762591));
#258487=CARTESIAN_POINT('Ctrl Pts',(1.83844439607489,2.68367477862573,7.08632913818064));
#258488=CARTESIAN_POINT('Ctrl Pts',(-1.25864905876497,2.99963175435938,
7.24515127873536));
#258489=CARTESIAN_POINT('Ctrl Pts',(-3.20297274976581,0.56829013641684,
7.4039734192901));
#258490=CARTESIAN_POINT('Ctrl Pts',(-2.21376217669363,-2.38353626780289,
7.56279555984482));
#258491=CARTESIAN_POINT('Ctrl Pts',(0.802985845242104,-3.1523327627698,
7.72161770039957));
#258492=CARTESIAN_POINT('Ctrl Pts',(3.0842962988265,-1.03397507510392,7.88043984095428));
#258493=CARTESIAN_POINT('Ctrl Pts',(2.54076571252921,2.03137827814687,8.03926198150902));
#258494=CARTESIAN_POINT('Ctrl Pts',(-0.329797869984274,3.23623569596605,
8.19808412206374));
#258495=CARTESIAN_POINT('Ctrl Pts',(-2.89830663423934,1.47709402842718,
8.35690626261848));
#258496=CARTESIAN_POINT('Ctrl Pts',(-2.81231831607218,-1.63488648045544,
8.5157284031732));
#258497=CARTESIAN_POINT('Ctrl Pts',(-0.15058777771873,-3.24950941467982,
8.67455054372794));
#258498=CARTESIAN_POINT('Ctrl Pts',(2.64906288678028,-1.8879761483595,8.83337268428267));
#258499=CARTESIAN_POINT('Ctrl Pts',(3.02249348848844,1.20271410856281,8.99219482483739));
#258500=CARTESIAN_POINT('Ctrl Pts',(0.627686923000373,3.19186422668404,
9.15101696539211));
#258501=CARTESIAN_POINT('Ctrl Pts',(-2.34200467573275,2.25765413953,9.30983910594686));
#258502=CARTESIAN_POINT('Ctrl Pts',(-3.16670426247216,-0.744293106868311,
9.46866124650158));
#258503=CARTESIAN_POINT('Ctrl Pts',(-1.09108711725453,-3.06455820917996,
9.62748338705631));
#258504=CARTESIAN_POINT('Ctrl Pts',(1.98383339193611,-2.57805996592987,
9.78630552761104));
#258505=CARTESIAN_POINT('Ctrl Pts',(3.24180331049736,0.269628282899643,
9.94512766816577));
#258506=CARTESIAN_POINT('Ctrl Pts',(1.53067488458323,2.87036975189557,10.1039498087205));
#258507=CARTESIAN_POINT('Ctrl Pts',(-1.5823659433047,2.8422009317359,10.2627719492752));
#258508=CARTESIAN_POINT('Ctrl Pts',(-3.24615163365646,0.210921042574126,
10.42159408983));
#258509=CARTESIAN_POINT('Ctrl Pts',(-1.9368564433157,-2.61353692012903,
10.5804162303847));
#258510=CARTESIAN_POINT('Ctrl Pts',(1.14636415474908,-3.04431229337554,
10.7392383709394));
#258511=CARTESIAN_POINT('Ctrl Pts',(3.17965433198608,-0.686867122501313,
10.8980605114941));
#258512=CARTESIAN_POINT('Ctrl Pts',(2.30076708546213,2.29966496110741,11.0568826520489));
#258513=CARTESIAN_POINT('Ctrl Pts',(-0.685343545759056,3.17998307215264,
11.2157047926036));
#258514=CARTESIAN_POINT('Ctrl Pts',(-3.04376267561093,1.1478226733467,11.3745269331583));
#258515=CARTESIAN_POINT('Ctrl Pts',(-2.61446464450226,-1.93560397228843,
11.5333490737131));
#258516=CARTESIAN_POINT('Ctrl Pts',(0.209365658982355,-3.24625232163643,
11.6921712142678));
#258517=CARTESIAN_POINT('Ctrl Pts',(2.84144243150425,-1.58372757232369,
11.8509933548225));
#258518=CARTESIAN_POINT('Ctrl Pts',(2.87110282916994,1.52929940143304,12.0098154953773));
#258519=CARTESIAN_POINT('Ctrl Pts',(0.271181527877081,3.24167374882626,
12.168637635932));
#258520=CARTESIAN_POINT('Ctrl Pts',(-2.57710913711678,1.98506841450872,
12.3274597764867));
#258521=CARTESIAN_POINT('Ctrl Pts',(-3.06508064031307,-1.08961864120845,
12.4862819170414));
#258522=CARTESIAN_POINT('Ctrl Pts',(-0.745810314442101,-3.16634727876821,
12.6451040575962));
#258523=CARTESIAN_POINT('Ctrl Pts',(2.25653173349553,-2.34308613811331,
12.8039261981509));
#258524=CARTESIAN_POINT('Ctrl Pts',(3.19216460987954,0.626157502808743,
12.9627483387057));
#258525=CARTESIAN_POINT('Ctrl Pts',(1.20416216644146,3.02191687374124,13.1215704792603));
#258526=CARTESIAN_POINT('Ctrl Pts',(-1.8867066610502,2.64996718659681,13.2803926198151));
#258527=CARTESIAN_POINT('Ctrl Pts',(-3.24958119422566,-0.149030792207068,
13.4392147603698));
#258528=CARTESIAN_POINT('Ctrl Pts',(-1.63623378550507,-2.81153465460818,
13.5980369009245));
#258529=CARTESIAN_POINT('Ctrl Pts',(1.47570516576429,-2.89901403560382,
13.7568590414793));
#258530=CARTESIAN_POINT('Ctrl Pts',(3.23607730530981,-0.331348440391097,
13.915681182034));
#258531=CARTESIAN_POINT('Ctrl Pts',(2.03259542611312,2.53979210736519,14.0745033225887));
#258532=CARTESIAN_POINT('Ctrl Pts',(-1.03249714831588,3.08479136306052,
14.2333254631435));
#258533=CARTESIAN_POINT('Ctrl Pts',(-3.1519476587076,0.804496160125281,
14.3921476036982));
#258534=CARTESIAN_POINT('Ctrl Pts',(-2.38459669504463,-2.21261987627114,
14.5509697442529));
#258535=CARTESIAN_POINT('Ctrl Pts',(0.56675540051207,-3.20324467234338,
14.7097918848077));
#258536=CARTESIAN_POINT('Ctrl Pts',(2.99902834159238,-1.26008615625968,
14.8686140253624));
#258537=CARTESIAN_POINT('Ctrl Pts',(2.68455534185449,1.8371583305197,15.0274361659171));
#258538=CARTESIAN_POINT('Ctrl Pts',(-0.0886445014816008,3.25178877963302,
15.1862583064719));
#258539=CARTESIAN_POINT('Ctrl Pts',(-2.78065674105224,1.68817540651928,
15.3450804470265));
#258540=CARTESIAN_POINT('Ctrl Pts',(-2.92592492013056,-1.42160172925132,
15.5039025875813));
#258541=CARTESIAN_POINT('Ctrl Pts',(-0.391401019129468,-3.22936423429805,
15.662724728136));
#258542=CARTESIAN_POINT('Ctrl Pts',(2.50159870726369,-2.07942107845204,
15.8215468686908));
#258543=CARTESIAN_POINT('Ctrl Pts',(3.10343766045434,0.975019385797018,
15.9803690092455));
#258544=CARTESIAN_POINT('Ctrl Pts',(0.862904409389887,3.13646044120949,
16.1391911498002));
#258545=CARTESIAN_POINT('Ctrl Pts',(-2.16794454097767,2.42528443139698,
16.298013290355));
#258546=CARTESIAN_POINT('Ctrl Pts',(-3.21321943726258,-0.507157733249974,
16.4568354309097));
#258547=CARTESIAN_POINT('Ctrl Pts',(-1.31557534406608,-2.97510498207739,
16.6156575714644));
#258548=CARTESIAN_POINT('Ctrl Pts',(1.78697607414341,-2.71821716570983,
16.7744797120191));
#258549=CARTESIAN_POINT('Ctrl Pts',(3.25287432279659,0.0282276048973285,
16.9333018525739));
#258550=CARTESIAN_POINT('Ctrl Pts',(1.73953449985156,2.74881938087089,17.0921239931286));
#258551=CARTESIAN_POINT('Ctrl Pts',(-1.36700773625735,2.95182612934618,
17.2509461336833));
#258552=CARTESIAN_POINT('Ctrl Pts',(-3.2215368986632,0.451318671751355,
17.4097682742381));
#258553=CARTESIAN_POINT('Ctrl Pts',(-2.12552912529691,-2.46254236227507,
17.5685904147928));
#258554=CARTESIAN_POINT('Ctrl Pts',(0.917205017219261,-3.12101262762637,
17.7274125553475));
#258555=CARTESIAN_POINT('Ctrl Pts',(3.11989129381503,-0.921015807145746,
17.8862346959023));
#258556=CARTESIAN_POINT('Ctrl Pts',(2.46513468979012,2.1225228596469,18.045056836457));
#258557=CARTESIAN_POINT('Ctrl Pts',(-0.447383885885906,3.22208218530956,
18.2038789770117));
#258558=CARTESIAN_POINT('Ctrl Pts',(-2.95015730247948,1.37061684082573,
18.3627011175664));
#258559=CARTESIAN_POINT('Ctrl Pts',(-2.75093674236513,-1.73618915598547,
18.5215232581212));
#258560=CARTESIAN_POINT('Ctrl Pts',(-0.032207261648967,-3.2528146355384,
18.6803453986759));
#258561=CARTESIAN_POINT('Ctrl Pts',(2.71604923798135,-1.79033690289397,
18.8391675392306));
#258562=CARTESIAN_POINT('Ctrl Pts',(2.97667879057788,1.31202519494447,18.9979896797854));
#258563=CARTESIAN_POINT('Ctrl Pts',(0.511137881081572,3.21243919263648,
19.1568118203401));
#258564=CARTESIAN_POINT('Ctrl Pts',(-2.42274569087925,2.17120692618642,
19.3156339608948));
#258565=CARTESIAN_POINT('Ctrl Pts',(-3.13730174101935,-0.859653501631685,
19.4744561014495));
#258566=CARTESIAN_POINT('Ctrl Pts',(-0.97920893696225,-3.10113535697825,
19.6332782420043));
#258567=CARTESIAN_POINT('Ctrl Pts',(2.07713706628989,-2.50629030530919,
19.792100382559));
#258568=CARTESIAN_POINT('Ctrl Pts',(3.22831766439385,0.391889480307326,
19.9509225231137));
#258569=CARTESIAN_POINT('Ctrl Pts',(2.02850526978224,2.0727146039754,20.0568039501502));
#258570=CARTESIAN_POINT('Ctrl Pts',(1.20564430054383,2.47375567929494,20.1097446636685));
#258571=CARTESIAN_POINT('Ctrl Pts',(1.48738611075532,-2.08582659521589,
-0.109744663668464));
#258572=CARTESIAN_POINT('Ctrl Pts',(2.18120777963242,-1.59106796283684,
-0.0568039501502205));
#258573=CARTESIAN_POINT('Ctrl Pts',(3.02430299867442,0.136677879741996,
0.049077476886266));
#258574=CARTESIAN_POINT('Ctrl Pts',(1.52164942887829,2.62055945523898,0.207899617440994));
#258575=CARTESIAN_POINT('Ctrl Pts',(-1.37597293748352,2.69667001321051,
0.366721757995726));
#258576=CARTESIAN_POINT('Ctrl Pts',(-3.01267583673131,0.306790423899341,
0.525543898550453));
#258577=CARTESIAN_POINT('Ctrl Pts',(-1.89049782615453,-2.36605884750802,
0.684366039105185));
#258578=CARTESIAN_POINT('Ctrl Pts',(0.963337657127712,-2.87084708234112,
0.843188179659912));
#258579=CARTESIAN_POINT('Ctrl Pts',(2.9347727731123,-0.746831402421932,
1.00201032021465));
#258580=CARTESIAN_POINT('Ctrl Pts',(2.21836462553458,2.06147584198914,1.16083246076937));
#258581=CARTESIAN_POINT('Ctrl Pts',(-0.529823686747478,2.98157235673077,
1.3196546013241));
#258582=CARTESIAN_POINT('Ctrl Pts',(-2.79274344473406,1.17098857214945,
1.47847674187883));
#258583=CARTESIAN_POINT('Ctrl Pts',(-2.49785671319912,-1.71211950327285,
1.63729888243356));
#258584=CARTESIAN_POINT('Ctrl Pts',(0.0847675203110875,-3.02711251258291,
1.79612102298829));
#258585=CARTESIAN_POINT('Ctrl Pts',(2.58975293024786,-1.56964910623143,
1.95494316354302));
#258586=CARTESIAN_POINT('Ctrl Pts',(2.72284007956926,1.32542823321795,2.11376530409775));
#258587=CARTESIAN_POINT('Ctrl Pts',(0.362135646372212,3.00657111379819,
2.27258744465248));
#258588=CARTESIAN_POINT('Ctrl Pts',(-2.33024078659653,1.93406140121526,
2.43140958520721));
#258589=CARTESIAN_POINT('Ctrl Pts',(-2.88839965742654,-0.909814643775332,
2.59023172576194));
#258590=CARTESIAN_POINT('Ctrl Pts',(-0.801134952756186,-2.92041046573759,
2.74905386631667));
#258591=CARTESIAN_POINT('Ctrl Pts',(2.01987208480945,-2.25626501008188,
2.9078760068714));
#258592=CARTESIAN_POINT('Ctrl Pts',(2.99092148573722,0.47434545210521,3.06669814742613));
#258593=CARTESIAN_POINT('Ctrl Pts',(1.22264983011503,2.77051299239757,3.22552028798086));
#258594=CARTESIAN_POINT('Ctrl Pts',(-1.66542065934546,2.52922694794631,
3.38434242853559));
#258595=CARTESIAN_POINT('Ctrl Pts',(-3.02816797570811,-0.0285240023499908,
3.54316456909032));
#258596=CARTESIAN_POINT('Ctrl Pts',(-1.61748098166808,-2.56015041959512,
3.70198670964505));
#258597=CARTESIAN_POINT('Ctrl Pts',(1.27462226192968,-2.74698980663272,
3.86080885019978));
#258598=CARTESIAN_POINT('Ctrl Pts',(2.99932622686687,-0.417919956096872,
4.01963099075451));
#258599=CARTESIAN_POINT('Ctrl Pts',(1.97701142398513,2.29391384606539,4.17845313130924));
#258600=CARTESIAN_POINT('Ctrl Pts',(-0.856005874802533,2.90480099966259,
4.33727527186396));
#258601=CARTESIAN_POINT('Ctrl Pts',(-2.90502569376376,0.855243020032118,
4.4960974124187));
#258602=CARTESIAN_POINT('Ctrl Pts',(-2.29339458729873,-1.97761375692776,
4.65491955297342));
#258603=CARTESIAN_POINT('Ctrl Pts',(0.418707590396682,-2.99921637408935,
4.81374169352815));
#258604=CARTESIAN_POINT('Ctrl Pts',(2.74732443774844,-1.27390083543187,
4.97256383408288));
#258605=CARTESIAN_POINT('Ctrl Pts',(2.55972556853956,1.61815324321388,5.13138597463761));
#258606=CARTESIAN_POINT('Ctrl Pts',(0.0277287763463851,3.02817536145956,
5.29020811519234));
#258607=CARTESIAN_POINT('Ctrl Pts',(-2.52966420928092,1.66475640652201,
5.44903025574707));
#258608=CARTESIAN_POINT('Ctrl Pts',(-2.77019182817363,-1.22337734975502,
5.6078523963018));
#258609=CARTESIAN_POINT('Ctrl Pts',(-0.4735599765103,-2.9910459463915,5.76667453685653));
#258610=CARTESIAN_POINT('Ctrl Pts',(2.25679533324014,-2.01927950730963,
5.92549667741126));
#258611=CARTESIAN_POINT('Ctrl Pts',(2.92020004606639,0.801901861657186,
6.084318817966));
#258612=CARTESIAN_POINT('Ctrl Pts',(0.909055968644706,2.88863845966353,
6.24314095852072));
#258613=CARTESIAN_POINT('Ctrl Pts',(-1.93467303544375,2.32973284964229,
6.40196309907545));
#258614=CARTESIAN_POINT('Ctrl Pts',(-3.00647636839827,-0.362925269219867,
6.56078523963017));
#258615=CARTESIAN_POINT('Ctrl Pts',(-1.32471227201173,-2.72318789310565,
6.71960738018491));
#258616=CARTESIAN_POINT('Ctrl Pts',(1.57032747283876,-2.58934094565073,
6.87842952073963));
#258617=CARTESIAN_POINT('Ctrl Pts',(3.02713785787826,-0.0839719844699643,
7.03725166129438));
#258618=CARTESIAN_POINT('Ctrl Pts',(1.71145739709093,2.4983051220214,7.19607380184909));
#258619=CARTESIAN_POINT('Ctrl Pts',(-1.17171030386558,2.79243797936335,
7.35489594240384));
#258620=CARTESIAN_POINT('Ctrl Pts',(-2.98173358790239,0.529036591882203,
7.51371808295854));
#258621=CARTESIAN_POINT('Ctrl Pts',(-2.06085082627003,-2.21889809965165,
7.67254022351329));
#258622=CARTESIAN_POINT('Ctrl Pts',(0.747521147516374,-2.93459146028735,
7.83136236406802));
#258623=CARTESIAN_POINT('Ctrl Pts',(2.87125448379991,-0.962555242068991,
7.99018450462274));
#258624=CARTESIAN_POINT('Ctrl Pts',(2.36526722389161,1.89106474356635,8.14900664517748));
#258625=CARTESIAN_POINT('Ctrl Pts',(-0.307017718531236,3.01269896028187,
8.3078287857322));
#258626=CARTESIAN_POINT('Ctrl Pts',(-2.69811169638694,1.37506660878503,
8.46665092628694));
#258627=CARTESIAN_POINT('Ctrl Pts',(-2.61806285536416,-1.52195985168403,
8.62547306684166));
#258628=CARTESIAN_POINT('Ctrl Pts',(-0.140186217564388,-3.02505582248999,
8.78429520739639));
#258629=CARTESIAN_POINT('Ctrl Pts',(2.46608397981406,-1.75756783916868,
8.94311734795112));
#258630=CARTESIAN_POINT('Ctrl Pts',(2.81372058332409,1.11963895241009,9.10193948850585));
#258631=CARTESIAN_POINT('Ctrl Pts',(0.584330660051387,2.9713923646162,9.26076162906059));
#258632=CARTESIAN_POINT('Ctrl Pts',(-2.1802352221596,2.10171103647249,9.41958376961531));
#258633=CARTESIAN_POINT('Ctrl Pts',(-2.94797027638068,-0.692882496785455,
9.57840591017004));
#258634=CARTESIAN_POINT('Ctrl Pts',(-1.01572238011805,-2.8528797646068,
9.73722805072478));
#258635=CARTESIAN_POINT('Ctrl Pts',(1.84680392862249,-2.39998544870592,
9.89605019127949));
#258636=CARTESIAN_POINT('Ctrl Pts',(3.01788200258335,0.25100422956428,10.0548723318342));
#258637=CARTESIAN_POINT('Ctrl Pts',(1.42494647069792,2.67210450028084,10.213694472389));
#258638=CARTESIAN_POINT('Ctrl Pts',(-1.47306706928727,2.64588138701586,
10.3725166129437));
#258639=CARTESIAN_POINT('Ctrl Pts',(-3.02192997371126,0.196352078575943,
10.5313387534984));
#258640=CARTESIAN_POINT('Ctrl Pts',(-1.80307182207585,-2.43301190075423,
10.6901608940532));
#258641=CARTESIAN_POINT('Ctrl Pts',(1.06718126291666,-2.83403229636771,
10.8489830346079));
#258642=CARTESIAN_POINT('Ctrl Pts',(2.96002584483288,-0.639423101472757,
11.0078051751626));
#258643=CARTESIAN_POINT('Ctrl Pts',(2.14184603886008,2.1408200416184,11.1666273157173));
#258644=CARTESIAN_POINT('Ctrl Pts',(-0.638004762853933,2.96033187790681,
11.3254494562721));
#258645=CARTESIAN_POINT('Ctrl Pts',(-2.83352064238958,1.06853903715664,
11.4842715968268));
#258646=CARTESIAN_POINT('Ctrl Pts',(-2.43387554435661,-1.8019058630679,
11.6430937373815));
#258647=CARTESIAN_POINT('Ctrl Pts',(0.194904130104354,-3.02202370686332,
11.8019158779362));
#258648=CARTESIAN_POINT('Ctrl Pts',(2.64517527872404,-1.4743346464093,11.960738018491));
#258649=CARTESIAN_POINT('Ctrl Pts',(2.67278694165709,1.42366599639206,12.1195601590457));
#258650=CARTESIAN_POINT('Ctrl Pts',(0.252450187142197,3.01776139013466,
12.2783822996004));
#258651=CARTESIAN_POINT('Ctrl Pts',(-2.39910029655829,1.84795364439411,
12.4372044401552));
#258652=CARTESIAN_POINT('Ctrl Pts',(-2.85336610981753,-1.01435533622114,
12.5960265807099));
#258653=CARTESIAN_POINT('Ctrl Pts',(-0.694294906173836,-2.9476379506372,
12.7548487212646));
#258654=CARTESIAN_POINT('Ctrl Pts',(2.10066615846894,-2.18124198461312,
12.9136708618194));
#258655=CARTESIAN_POINT('Ctrl Pts',(2.97167199942212,0.582906881608178,
13.0724930023741));
#258656=CARTESIAN_POINT('Ctrl Pts',(1.12098698848508,2.81318379712787,13.2313151429288));
#258657=CARTESIAN_POINT('Ctrl Pts',(-1.75638603924554,2.46692581686579,
13.3901372834835));
#258658=CARTESIAN_POINT('Ctrl Pts',(-3.02512264400222,-0.138736777822433,
13.5489594240383));
#258659=CARTESIAN_POINT('Ctrl Pts',(-1.52321409423724,-2.61733332380355,
13.707781564593));
#258660=CARTESIAN_POINT('Ctrl Pts',(1.37377367913049,-2.69877023536724,
13.8666037051478));
#258661=CARTESIAN_POINT('Ctrl Pts',(3.01255151015457,-0.30846118627934,
14.0254258457024));
#258662=CARTESIAN_POINT('Ctrl Pts',(1.89219781938555,2.36436086862553,14.1842479862572));
#258663=CARTESIAN_POINT('Ctrl Pts',(-0.961179400221878,2.87171535242729,
14.3430701268119));
#258664=CARTESIAN_POINT('Ctrl Pts',(-2.93423295654511,0.748927140313446,
14.5018922673667));
#258665=CARTESIAN_POINT('Ctrl Pts',(-2.21988527992798,-2.05978742804493,
14.6607144079214));
#258666=CARTESIAN_POINT('Ctrl Pts',(0.527607864898483,-2.98198672795264,
14.8195365484761));
#258667=CARTESIAN_POINT('Ctrl Pts',(2.79187624616883,-1.17304813662401,
14.9783586890308));
#258668=CARTESIAN_POINT('Ctrl Pts',(2.49912486204435,1.71026016403225,15.1371808295856));
#258669=CARTESIAN_POINT('Ctrl Pts',(-0.082521553600458,3.02717774470757,
15.2960029701403));
#258670=CARTESIAN_POINT('Ctrl Pts',(-2.5885882425409,1.57156794801246,15.454825110695));
#258671=CARTESIAN_POINT('Ctrl Pts',(-2.72382230247565,-1.32340733309041,
15.6136472512498));
#258672=CARTESIAN_POINT('Ctrl Pts',(-0.364365749025758,-3.00630213156863,
15.7724693918045));
#258673=CARTESIAN_POINT('Ctrl Pts',(2.32880560393364,-1.93578908014936,
15.9312915323592));
#258674=CARTESIAN_POINT('Ctrl Pts',(2.88907369281068,0.90767180323327,16.090113672914));
#258675=CARTESIAN_POINT('Ctrl Pts',(0.803300952471413,2.91981548870976,
16.2489358134687));
#258676=CARTESIAN_POINT('Ctrl Pts',(-2.01819795532617,2.25776258940755,
16.4077579540234));
#258677=CARTESIAN_POINT('Ctrl Pts',(-2.9912725052335,-0.472126791495962,
16.5665800945781));
#258678=CARTESIAN_POINT('Ctrl Pts',(-1.22470451586104,-2.76960534654705,
16.7254022351329));
#258679=CARTESIAN_POINT('Ctrl Pts',(1.66354415017768,-2.53046156037463,
16.8842243756876));
#258680=CARTESIAN_POINT('Ctrl Pts',(3.0281883060719,0.0262778375603132,
17.0430465162423));
#258681=CARTESIAN_POINT('Ctrl Pts',(1.61937951108125,2.55894998657703,17.2018686567971));
#258682=CARTESIAN_POINT('Ctrl Pts',(-1.27258431481161,2.74793443564667,
17.3606907973518));
#258683=CARTESIAN_POINT('Ctrl Pts',(-2.99901545403822,0.420144705416821,
17.5195129379065));
#258684=CARTESIAN_POINT('Ctrl Pts',(-1.97871230263384,-2.29244700060747,
17.6783350784613));
#258685=CARTESIAN_POINT('Ctrl Pts',(0.853850850599735,-2.90543470304,17.837157219016));
#258686=CARTESIAN_POINT('Ctrl Pts',(2.90439082319782,-0.857398417565761,
17.9959793595707));
#258687=CARTESIAN_POINT('Ctrl Pts',(2.29486026810186,1.97591368898239,18.1548015001254));
#258688=CARTESIAN_POINT('Ctrl Pts',(-0.416481707292041,2.99952307606173,
18.3136236406802));
#258689=CARTESIAN_POINT('Ctrl Pts',(-2.74638087977544,1.27594412744645,
18.4724457812349));
#258690=CARTESIAN_POINT('Ctrl Pts',(-2.56092109541194,-1.61626524038718,
18.6312679217896));
#258691=CARTESIAN_POINT('Ctrl Pts',(-0.0299826072014076,-3.0281327415959,
18.7900900623443));
#258692=CARTESIAN_POINT('Ctrl Pts',(2.52844337807053,-1.6666728361677,18.9489122028991));
#258693=CARTESIAN_POINT('Ctrl Pts',(2.77107044726236,1.22139958643925,19.1077343434538));
#258694=CARTESIAN_POINT('Ctrl Pts',(0.475832018296617,2.99054615449931,
19.2665564840086));
#258695=CARTESIAN_POINT('Ctrl Pts',(-2.25539920749206,2.02123499757207,
19.4253786245633));
#258696=CARTESIAN_POINT('Ctrl Pts',(-2.92059867735871,-0.80027459489331,
19.584200765118));
#258697=CARTESIAN_POINT('Ctrl Pts',(-0.911571969236381,-2.88693041650442,
19.7430229056727));
#258698=CARTESIAN_POINT('Ctrl Pts',(1.93366283171984,-2.33317313889758,
19.9018450462275));
#258699=CARTESIAN_POINT('Ctrl Pts',(3.00532785146098,0.364820470690377,
20.0606671867822));
#258700=CARTESIAN_POINT('Ctrl Pts',(1.88839018271039,1.92954584245562,20.1665486138187));
#258701=CARTESIAN_POINT('Ctrl Pts',(1.12236674703443,2.3028857793927,20.2194893273369));
#258702=CARTESIAN_POINT('Ctrl Pts',(1.37702479013101,-1.93106208855765,
-2.4980018054066E-15));
#258703=CARTESIAN_POINT('Ctrl Pts',(2.01936616407906,-1.47301363900524,
0.0529407135182407));
#258704=CARTESIAN_POINT('Ctrl Pts',(2.79990526463056,0.126536631817626,
0.158822140554727));
#258705=CARTESIAN_POINT('Ctrl Pts',(1.40874583290953,2.42611875140058,0.317644281109456));
#258706=CARTESIAN_POINT('Ctrl Pts',(-1.27387826991474,2.49658204560485,
0.476466421664188));
#258707=CARTESIAN_POINT('Ctrl Pts',(-2.78914081677217,0.284027137290959,
0.635288562218914));
#258708=CARTESIAN_POINT('Ctrl Pts',(-1.75022635580586,-2.19050162185044,
0.794110702773647));
#258709=CARTESIAN_POINT('Ctrl Pts',(0.891859770330893,-2.65783549575534,
0.952932843328373));
#258710=CARTESIAN_POINT('Ctrl Pts',(2.71701801755088,-0.691417882516756,
1.11175498388311));
#258711=CARTESIAN_POINT('Ctrl Pts',(2.05376604018409,1.90851811654588,1.27057712443783));
#258712=CARTESIAN_POINT('Ctrl Pts',(-0.490511741217893,2.76034515792448,
1.42939926499256));
#258713=CARTESIAN_POINT('Ctrl Pts',(-2.58552700476795,1.08410336841926,
1.58822140554729));
#258714=CARTESIAN_POINT('Ctrl Pts',(-2.31252032770672,-1.58508337722494,
1.74704354610202));
#258715=CARTESIAN_POINT('Ctrl Pts',(0.078477925820518,-2.80250631776144,
1.90586568665675));
#258716=CARTESIAN_POINT('Ctrl Pts',(2.39759801404543,-1.4531840222644,2.06468782721148));
#258717=CARTESIAN_POINT('Ctrl Pts',(2.520810341052,1.22708388997517,2.22350996776621));
#258718=CARTESIAN_POINT('Ctrl Pts',(0.335265845793994,2.78348905308081,
2.38233210832094));
#258719=CARTESIAN_POINT('Ctrl Pts',(-2.15734119534592,1.79055759351985,
2.54115424887567));
#258720=CARTESIAN_POINT('Ctrl Pts',(-2.67408570197179,-0.842308066374673,
2.6999763894304));
#258721=CARTESIAN_POINT('Ctrl Pts',(-0.741692209042783,-2.70372136703395,
2.85879852998513));
#258722=CARTESIAN_POINT('Ctrl Pts',(1.87000128182168,-2.08885428573093,
3.01762067053986));
#258723=CARTESIAN_POINT('Ctrl Pts',(2.76900059871079,0.439149889804403,
3.17644281109459));
#258724=CARTESIAN_POINT('Ctrl Pts',(1.13193145582276,2.56494601121031,3.33526495164932));
#258725=CARTESIAN_POINT('Ctrl Pts',(-1.54184950184215,2.34156294858825,
3.49408709220405));
#258726=CARTESIAN_POINT('Ctrl Pts',(-2.80348346745913,-0.0264075737064492,
3.65290923275878));
#258727=CARTESIAN_POINT('Ctrl Pts',(-1.49746686029714,-2.37019195537365,
3.81173137331351));
#258728=CARTESIAN_POINT('Ctrl Pts',(1.18004762854664,-2.54316820267302,
3.97055351386824));
#258729=CARTESIAN_POINT('Ctrl Pts',(2.77678172346816,-0.3869110620803,4.12937565442297));
#258730=CARTESIAN_POINT('Ctrl Pts',(1.83032080339732,2.12370964715592,4.2881977949777));
#258731=CARTESIAN_POINT('Ctrl Pts',(-0.792491809340816,2.68927009470421,
4.44701993553242));
#258732=CARTESIAN_POINT('Ctrl Pts',(-2.68947811691531,0.791785556994785,
4.60584207608716));
#258733=CARTESIAN_POINT('Ctrl Pts',(-2.12322891643708,-1.83087844434069,
4.76466421664189));
#258734=CARTESIAN_POINT('Ctrl Pts',(0.387640255360107,-2.77668002156518,
4.92348635719661));
#258735=CARTESIAN_POINT('Ctrl Pts',(2.54347800477387,-1.17937973057141,
5.08230849775135));
#258736=CARTESIAN_POINT('Ctrl Pts',(2.36979862748696,1.49808924126962,5.24113063830607));
#258737=CARTESIAN_POINT('Ctrl Pts',(0.0256713520133373,2.80349030520137,
5.3999527788608));
#258738=CARTESIAN_POINT('Ctrl Pts',(-2.34196776593405,1.54123453535952,
5.55877491941554));
#258739=CARTESIAN_POINT('Ctrl Pts',(-2.56464867678256,-1.13260499484022,
5.71759705997026));
#258740=CARTESIAN_POINT('Ctrl Pts',(-0.438422695057549,-2.76911582461286,
5.876419200525));
#258741=CARTESIAN_POINT('Ctrl Pts',(2.08934525988381,-1.86945267248516,
6.03524134107972));
#258742=CARTESIAN_POINT('Ctrl Pts',(2.7035265601163,0.742402214710351,6.19406348163445));
#258743=CARTESIAN_POINT('Ctrl Pts',(0.841605683546825,2.67430678552092,
6.35288562218919));
#258744=CARTESIAN_POINT('Ctrl Pts',(-1.79112384561072,2.15687094638179,
6.5117077627439));
#258745=CARTESIAN_POINT('Ctrl Pts',(-2.78340133761574,-0.335996880075048,
6.67052990329864));
#258746=CARTESIAN_POINT('Ctrl Pts',(-1.2264210517769,-2.5211323474621,6.82935204385337));
#258747=CARTESIAN_POINT('Ctrl Pts',(1.45381205531404,-2.39721659794956,
6.9881741844081));
#258748=CARTESIAN_POINT('Ctrl Pts',(2.80252978248238,-0.0777414172792658,
7.14699632496283));
#258749=CARTESIAN_POINT('Ctrl Pts',(1.58447039810697,2.31293546541706,7.30581846551756));
#258750=CARTESIAN_POINT('Ctrl Pts',(-1.08477154896619,2.58524420436732,
7.46464060607229));
#258751=CARTESIAN_POINT('Ctrl Pts',(-2.76049442603897,0.489783047347568,
7.62346274662702));
#258752=CARTESIAN_POINT('Ctrl Pts',(-1.90793947584643,-2.05425993150043,
7.78228488718174));
#258753=CARTESIAN_POINT('Ctrl Pts',(0.692056449790645,-2.71685015780489,
7.94110702773648));
#258754=CARTESIAN_POINT('Ctrl Pts',(2.65821266877332,-0.891135409034062,
8.0999291682912));
#258755=CARTESIAN_POINT('Ctrl Pts',(2.18976873525401,1.75075120898583,8.25875130884594));
#258756=CARTESIAN_POINT('Ctrl Pts',(-0.284237567078199,2.78916222459769,
8.41757344940066));
#258757=CARTESIAN_POINT('Ctrl Pts',(-2.49791675853455,1.27303918914287,
8.57639558995541));
#258758=CARTESIAN_POINT('Ctrl Pts',(-2.42380739465615,-1.40903322291262,
8.73521773051011));
#258759=CARTESIAN_POINT('Ctrl Pts',(-0.129784657410042,-2.80060223030017,
8.89403987106487));
#258760=CARTESIAN_POINT('Ctrl Pts',(2.28310507284784,-1.62715952997786,
9.05286201161958));
#258761=CARTESIAN_POINT('Ctrl Pts',(2.60494767815974,1.03656379625737,9.21168415217432));
#258762=CARTESIAN_POINT('Ctrl Pts',(0.540974397102402,2.75092050254836,
9.37050629272904));
#258763=CARTESIAN_POINT('Ctrl Pts',(-2.01846576858645,1.94576793341498,
9.52932843328377));
#258764=CARTESIAN_POINT('Ctrl Pts',(-2.7292362902892,-0.6414718867026,9.68815057383851));
#258765=CARTESIAN_POINT('Ctrl Pts',(-0.940357642981567,-2.64120132003364,
9.84697271439322));
#258766=CARTESIAN_POINT('Ctrl Pts',(1.70977446530886,-2.22191093148198,
10.005794854948));
#258767=CARTESIAN_POINT('Ctrl Pts',(2.79396069466933,0.232380176228921,
10.1646169955027));
#258768=CARTESIAN_POINT('Ctrl Pts',(1.3192180568126,2.47383924866609,10.3234391360574));
#258769=CARTESIAN_POINT('Ctrl Pts',(-1.36376819526984,2.44956184229582,
10.4822612766122));
#258770=CARTESIAN_POINT('Ctrl Pts',(-2.79770831376606,0.181783114577756,
10.6410834171669));
#258771=CARTESIAN_POINT('Ctrl Pts',(-1.66928720083601,-2.25248688137943,
10.7999055577216));
#258772=CARTESIAN_POINT('Ctrl Pts',(0.987998371084236,-2.62375229935987,
10.9587276982763));
#258773=CARTESIAN_POINT('Ctrl Pts',(2.74039735767968,-0.591979080444202,
11.1175498388311));
#258774=CARTESIAN_POINT('Ctrl Pts',(1.98292499225804,1.98197512212938,11.2763719793858));
#258775=CARTESIAN_POINT('Ctrl Pts',(-0.590665979948808,2.74068068366097,
11.4351941199405));
#258776=CARTESIAN_POINT('Ctrl Pts',(-2.62327860916824,0.989255400966587,
11.5940162604952));
#258777=CARTESIAN_POINT('Ctrl Pts',(-2.25328644421095,-1.66820775384737,
11.75283840105));
#258778=CARTESIAN_POINT('Ctrl Pts',(0.180442601226353,-2.79779509209019,
11.9116605416047));
#258779=CARTESIAN_POINT('Ctrl Pts',(2.44890812594382,-1.36494172049492,
12.0704826821594));
#258780=CARTESIAN_POINT('Ctrl Pts',(2.47447105414424,1.31803259135108,12.2293048227142));
#258781=CARTESIAN_POINT('Ctrl Pts',(0.233718846407313,2.79384903144306,
12.3881269632689));
#258782=CARTESIAN_POINT('Ctrl Pts',(-2.2210914559998,1.7108388742795,12.5469491038237));
#258783=CARTESIAN_POINT('Ctrl Pts',(-2.64165157932199,-0.939092031233823,
12.7057712443783));
#258784=CARTESIAN_POINT('Ctrl Pts',(-0.642779497905573,-2.7289286225062,
12.8645933849331));
#258785=CARTESIAN_POINT('Ctrl Pts',(1.94480058344235,-2.01939783111293,
13.0234155254878));
#258786=CARTESIAN_POINT('Ctrl Pts',(2.7511793889647,0.539656260407611,13.1822376660426));
#258787=CARTESIAN_POINT('Ctrl Pts',(1.03781181052871,2.60445072051449,13.3410598065973));
#258788=CARTESIAN_POINT('Ctrl Pts',(-1.62606541744088,2.28388444713476,
13.499881947152));
#258789=CARTESIAN_POINT('Ctrl Pts',(-2.80066409377878,-0.128442763437796,
13.6587040877067));
#258790=CARTESIAN_POINT('Ctrl Pts',(-1.41019440296941,-2.42313199299893,
13.8175262282615));
#258791=CARTESIAN_POINT('Ctrl Pts',(1.27184219249669,-2.49852643513066,
13.9763483688162));
#258792=CARTESIAN_POINT('Ctrl Pts',(2.78902571499932,-0.285573932167581,
14.1351705093709));
#258793=CARTESIAN_POINT('Ctrl Pts',(1.75180021265799,2.18892962988587,14.2939926499257));
#258794=CARTESIAN_POINT('Ctrl Pts',(-0.889861652127881,2.65863934179406,
14.4528147904804));
#258795=CARTESIAN_POINT('Ctrl Pts',(-2.71651825438262,0.693358120501612,
14.6116369310351));
#258796=CARTESIAN_POINT('Ctrl Pts',(-2.05517386481133,-1.90695497981872,
14.7704590715899));
#258797=CARTESIAN_POINT('Ctrl Pts',(0.488460329284891,-2.7607287835619,
14.9292812121446));
#258798=CARTESIAN_POINT('Ctrl Pts',(2.58472415074527,-1.08601011698834,
15.0881033526993));
#258799=CARTESIAN_POINT('Ctrl Pts',(2.31369438223421,1.5833619975448,15.246925493254));
#258800=CARTESIAN_POINT('Ctrl Pts',(-0.0763986057193116,2.80256670978213,
15.4057476338088));
#258801=CARTESIAN_POINT('Ctrl Pts',(-2.39651974402956,1.45496048950563,
15.5645697743635));
#258802=CARTESIAN_POINT('Ctrl Pts',(-2.52171968482074,-1.2252129369295,
15.7233919149182));
#258803=CARTESIAN_POINT('Ctrl Pts',(-0.33733047892205,-2.7832400288392,
15.882214055473));
#258804=CARTESIAN_POINT('Ctrl Pts',(2.15601250060359,-1.79215708184668,
16.0410361960277));
#258805=CARTESIAN_POINT('Ctrl Pts',(2.67470972516702,0.840324220669528,
16.1998583365824));
#258806=CARTESIAN_POINT('Ctrl Pts',(0.743697495552939,2.70317053621002,
16.3586804771371));
#258807=CARTESIAN_POINT('Ctrl Pts',(-1.86845136967466,2.09024074741813,
16.5175026176919));
#258808=CARTESIAN_POINT('Ctrl Pts',(-2.76932557320444,-0.437095849741951,
16.6763247582466));
#258809=CARTESIAN_POINT('Ctrl Pts',(-1.13383368765599,-2.56410571101671,
16.8351468988013));
#258810=CARTESIAN_POINT('Ctrl Pts',(1.54011222621193,-2.34270595503943,
16.9939690393561));
#258811=CARTESIAN_POINT('Ctrl Pts',(2.80350228934723,0.0243280702232952,
17.1527911799108));
#258812=CARTESIAN_POINT('Ctrl Pts',(1.49922452231095,2.36908059228316,17.3116133204655));
#258813=CARTESIAN_POINT('Ctrl Pts',(-1.17816089336587,2.54404274194716,
17.4704354610202));
#258814=CARTESIAN_POINT('Ctrl Pts',(-2.77649400941324,0.388970739082288,
17.629257601575));
#258815=CARTESIAN_POINT('Ctrl Pts',(-1.83189547997077,-2.12235163893987,
17.7880797421297));
#258816=CARTESIAN_POINT('Ctrl Pts',(0.790496683980206,-2.68985677845362,
17.9469018826844));
#258817=CARTESIAN_POINT('Ctrl Pts',(2.68889035258062,-0.793781027985773,
18.1057240232392));
#258818=CARTESIAN_POINT('Ctrl Pts',(2.1245858464136,1.82930451831788,18.2645461637939));
#258819=CARTESIAN_POINT('Ctrl Pts',(-0.385579528698175,2.7769639668139,
18.4233683043486));
#258820=CARTESIAN_POINT('Ctrl Pts',(-2.5426044570714,1.18127141406717,18.5821904449034));
#258821=CARTESIAN_POINT('Ctrl Pts',(-2.37090544845875,-1.49634132478888,
18.7410125854581));
#258822=CARTESIAN_POINT('Ctrl Pts',(-0.0277579527538448,-2.80345084765341,
18.8998347260128));
#258823=CARTESIAN_POINT('Ctrl Pts',(2.3408375181597,-1.54300876944143,19.0586568665676));
#258824=CARTESIAN_POINT('Ctrl Pts',(2.56546210394684,1.13077397793403,19.2174790071223));
#258825=CARTESIAN_POINT('Ctrl Pts',(0.440526155511663,2.76865311636215,
19.376301147677));
#258826=CARTESIAN_POINT('Ctrl Pts',(-2.08805272410487,1.87126306895772,
19.5351232882317));
#258827=CARTESIAN_POINT('Ctrl Pts',(-2.70389561369807,-0.740895688154933,
19.6939454287865));
#258828=CARTESIAN_POINT('Ctrl Pts',(-0.843935001510512,-2.67272547603058,
19.8527675693412));
#258829=CARTESIAN_POINT('Ctrl Pts',(1.79018859714979,-2.16005597248598,
20.0115897098959));
#258830=CARTESIAN_POINT('Ctrl Pts',(2.7823380385281,0.337751461073428,20.1704118504506));
#258831=CARTESIAN_POINT('Ctrl Pts',(1.74827509563854,1.78637708093585,20.2762932774871));
#258832=CARTESIAN_POINT('Ctrl Pts',(1.03908919352503,2.13201587949046,20.3292339910054));
#258833=CARTESIAN_POINT('',(1.28892185405323,2.64462557919718,20.));
#258834=CARTESIAN_POINT('Ctrl Pts',(1.38000112159638,-1.93372602389037,
20.));
#258835=CARTESIAN_POINT('Ctrl Pts',(1.43104039670144,-1.90596629917353,
20.));
#258836=CARTESIAN_POINT('Ctrl Pts',(1.48086808386216,-1.87627442504008,
20.));
#258837=CARTESIAN_POINT('Ctrl Pts',(1.52936177959298,-1.84468159128334,
20.));
#258838=CARTESIAN_POINT('Ctrl Pts',(1.59716821331816,-1.80050683091434,
20.));
#258839=CARTESIAN_POINT('Ctrl Pts',(1.66236782235411,-1.75261800820872,
20.));
#258840=CARTESIAN_POINT('Ctrl Pts',(1.72488638260891,-1.70138403719481,
20.));
#258841=CARTESIAN_POINT('Ctrl Pts',(1.78902316386727,-1.64882393378674,
20.));
#258842=CARTESIAN_POINT('Ctrl Pts',(1.8503388588045,-1.5927428737396,20.));
#258843=CARTESIAN_POINT('Ctrl Pts',(1.90873407605101,-1.53348793892088,
20.));
#258844=CARTESIAN_POINT('Ctrl Pts',(1.96836316935041,-1.47298096243615,
20.));
#258845=CARTESIAN_POINT('Ctrl Pts',(2.02494770374105,-1.40916401657361,
20.));
#258846=CARTESIAN_POINT('Ctrl Pts',(2.07835290128116,-1.34236124876648,
20.));
#258847=CARTESIAN_POINT('Ctrl Pts',(2.08686002520482,-1.33171997319116,
20.));
#258848=CARTESIAN_POINT('Ctrl Pts',(2.09528652032987,-1.32100257727076,
20.));
#258849=CARTESIAN_POINT('Ctrl Pts',(2.10362268727388,-1.31022238979363,
20.));
#258850=CARTESIAN_POINT('Ctrl Pts',(2.15664189201375,-1.2416588676349,20.));
#258851=CARTESIAN_POINT('Ctrl Pts',(2.20610243814027,-1.17044390820985,
20.));
#258852=CARTESIAN_POINT('Ctrl Pts',(2.25191648819796,-1.09697647600033,
20.));
#258853=CARTESIAN_POINT('Ctrl Pts',(2.29866887655797,-1.0220043240481,20.));
#258854=CARTESIAN_POINT('Ctrl Pts',(2.34162449612302,-0.944685869277743,
20.));
#258855=CARTESIAN_POINT('Ctrl Pts',(2.38066172624132,-0.86539794489534,
20.));
#258856=CARTESIAN_POINT('Ctrl Pts',(2.42000062340461,-0.785497309165861,
20.));
#258857=CARTESIAN_POINT('Ctrl Pts',(2.45536096486505,-0.703595853686508,
20.));
#258858=CARTESIAN_POINT('Ctrl Pts',(2.48658040767009,-0.62004268886668,
20.));
#258859=CARTESIAN_POINT('Ctrl Pts',(2.50067454461614,-0.582322292810884,
20.));
#258860=CARTESIAN_POINT('Ctrl Pts',(2.51392415514951,-0.544264842490704,
20.));
#258861=CARTESIAN_POINT('Ctrl Pts',(2.52631126586128,-0.505900729858203,
20.));
#258862=CARTESIAN_POINT('Ctrl Pts',(2.53056444695775,-0.492728205414998,
20.));
#258863=CARTESIAN_POINT('Ctrl Pts',(2.53471592773745,-0.479519520243206,
20.));
#258864=CARTESIAN_POINT('Ctrl Pts',(2.53876492381411,-0.46627588320346,
20.));
#258865=CARTESIAN_POINT('Ctrl Pts',(2.54272170769679,-0.453333857922437,
20.));
#258866=CARTESIAN_POINT('Ctrl Pts',(2.5465779933553,-0.44036701015714,20.));
#258867=CARTESIAN_POINT('Ctrl Pts',(2.55033280274283,-0.427378822049379,
20.));
#258868=CARTESIAN_POINT('Ctrl Pts',(2.57581353743285,-0.339238908375791,
20.));
#258869=CARTESIAN_POINT('Ctrl Pts',(2.59663392622878,-0.250087233771202,
20.));
#258870=CARTESIAN_POINT('Ctrl Pts',(2.61267173384564,-0.160322906932646,
20.));
#258871=CARTESIAN_POINT('Ctrl Pts',(2.62865972446749,-0.0708374080441688,
20.));
#258872=CARTESIAN_POINT('Ctrl Pts',(2.63989534171169,0.0192578513483404,
20.));
#258873=CARTESIAN_POINT('Ctrl Pts',(2.64621597035763,0.109597181710584,
20.));
#258874=CARTESIAN_POINT('Ctrl Pts',(2.65109085997397,0.179272887751659,
20.));
#258875=CARTESIAN_POINT('Ctrl Pts',(2.65304130476616,0.24909449849761,20.));
#258876=CARTESIAN_POINT('Ctrl Pts',(2.65197262376409,0.31890119631434,20.));
#258877=CARTESIAN_POINT('Ctrl Pts',(2.65108318146032,0.376999946086523,
20.));
#258878=CARTESIAN_POINT('Ctrl Pts',(2.64810211482615,0.435088533644068,
20.));
#258879=CARTESIAN_POINT('Ctrl Pts',(2.64308540245169,0.493094560823236,
20.));
#258880=CARTESIAN_POINT('Ctrl Pts',(2.64180721514896,0.507873675488013,
20.));
#258881=CARTESIAN_POINT('Ctrl Pts',(2.64039683402233,0.522647431607784,
20.));
#258882=CARTESIAN_POINT('Ctrl Pts',(2.63885508706822,0.537414630746964,
20.));
#258883=CARTESIAN_POINT('Ctrl Pts',(2.63731701688765,0.552146612922076,
20.));
#258884=CARTESIAN_POINT('Ctrl Pts',(2.63564900582864,0.566864075411001,
20.));
#258885=CARTESIAN_POINT('Ctrl Pts',(2.63385310696625,0.581559801841969,
20.));
#258886=CARTESIAN_POINT('Ctrl Pts',(2.62304356262524,0.67001361725719,20.));
#258887=CARTESIAN_POINT('Ctrl Pts',(2.6075979139829,0.757747286034274,20.));
#258888=CARTESIAN_POINT('Ctrl Pts',(2.58779888199941,0.844496593095176,
20.));
#258889=CARTESIAN_POINT('Ctrl Pts',(2.5668320373806,0.936362662277352,20.));
#258890=CARTESIAN_POINT('Ctrl Pts',(2.54098334417491,1.02712551913946,20.));
#258891=CARTESIAN_POINT('Ctrl Pts',(2.5105286039796,1.11648109850773,20.));
#258892=CARTESIAN_POINT('Ctrl Pts',(2.4838807063087,1.19466723045496,20.));
#258893=CARTESIAN_POINT('Ctrl Pts',(2.45370523303439,1.27177643242526,20.));
#258894=CARTESIAN_POINT('Ctrl Pts',(2.42015135515334,1.3476035881054,20.));
#258895=CARTESIAN_POINT('Ctrl Pts',(2.40261366909957,1.38723634993944,20.));
#258896=CARTESIAN_POINT('Ctrl Pts',(2.38415251762534,1.42651880651212,20.));
#258897=CARTESIAN_POINT('Ctrl Pts',(2.36478585672699,1.46542086170342,20.));
#258898=CARTESIAN_POINT('Ctrl Pts',(2.35510885575605,1.48485917519657,20.));
#258899=CARTESIAN_POINT('Ctrl Pts',(2.34520573857011,1.50420250113221,20.));
#258900=CARTESIAN_POINT('Ctrl Pts',(2.33507854188857,1.52344700440923,20.));
#258901=CARTESIAN_POINT('Ctrl Pts',(2.32609493115886,1.54051837485496,20.));
#258902=CARTESIAN_POINT('Ctrl Pts',(2.31693343742811,1.55751456940709,20.));
#258903=CARTESIAN_POINT('Ctrl Pts',(2.30760786718556,1.57441093843168,20.));
#258904=CARTESIAN_POINT('Ctrl Pts',(2.2610478988748,1.65876979112269,20.));
#258905=CARTESIAN_POINT('Ctrl Pts',(2.21034456355009,1.74075363192982,20.));
#258906=CARTESIAN_POINT('Ctrl Pts',(2.1557571209275,1.82005591564008,20.));
#258907=CARTESIAN_POINT('Ctrl Pts',(2.09879739664546,1.90280454789056,20.));
#258908=CARTESIAN_POINT('Ctrl Pts',(2.03760859153995,1.98263458419847,20.));
#258909=CARTESIAN_POINT('Ctrl Pts',(1.97242793240484,2.05918273337975,20.));
#258910=CARTESIAN_POINT('Ctrl Pts',(1.9514213230739,2.08385288992916,20.));
#258911=CARTESIAN_POINT('Ctrl Pts',(1.92999966961265,2.10818198519152,20.));
#258912=CARTESIAN_POINT('Ctrl Pts',(1.90816974030175,2.13215724040594,20.));
#258913=CARTESIAN_POINT('Ctrl Pts',(1.89233578867659,2.14954726608397,20.));
#258914=CARTESIAN_POINT('Ctrl Pts',(1.87628380519926,2.16675431787413,20.));
#258915=CARTESIAN_POINT('Ctrl Pts',(1.86003660437627,2.18375258633449,20.));
#258916=CARTESIAN_POINT('Ctrl Pts',(1.79159664630606,2.25535635324592,20.));
#258917=CARTESIAN_POINT('Ctrl Pts',(1.71963685016589,2.32332525945659,20.));
#258918=CARTESIAN_POINT('Ctrl Pts',(1.64439743292523,2.38733140490762,20.));
#258919=CARTESIAN_POINT('Ctrl Pts',(1.57010648122843,2.45053069105827,20.));
#258920=CARTESIAN_POINT('Ctrl Pts',(1.49261756777843,2.50986732158365,20.));
#258921=CARTESIAN_POINT('Ctrl Pts',(1.41211902868467,2.56499971753534,20.));
#258922=CARTESIAN_POINT('Ctrl Pts',(1.37180215812419,2.5926122145607,20.));
#258923=CARTESIAN_POINT('Ctrl Pts',(1.33072972222921,2.61916963457235,20.));
#258924=CARTESIAN_POINT('Ctrl Pts',(1.28892185405323,2.64462557919718,20.));
#258925=CARTESIAN_POINT('Ctrl Pts',(1.29201717055307,2.64849452802569,1.73472347597681E-18));
#258926=CARTESIAN_POINT('Ctrl Pts',(1.35304057255792,2.61171371626496,-4.41564112292885E-17));
#258927=CARTESIAN_POINT('Ctrl Pts',(1.41253786891839,2.57261997258187,-1.97337342542082E-16));
#258928=CARTESIAN_POINT('Ctrl Pts',(1.47035891216485,2.53120529245361,-2.74086309204336E-16));
#258929=CARTESIAN_POINT('Ctrl Pts',(1.54979852115497,2.47430618079598,-3.7714836491708E-16));
#258930=CARTESIAN_POINT('Ctrl Pts',(1.6260758814995,2.41302695688629,1.41787018262576E-18));
#258931=CARTESIAN_POINT('Ctrl Pts',(1.6990147092737,2.34774686778585,2.04697370165263E-16));
#258932=CARTESIAN_POINT('Ctrl Pts',(1.73774680310026,2.3130817297078,3.12643177722203E-16));
#258933=CARTESIAN_POINT('Ctrl Pts',(1.77553678566096,2.27728785079842,-9.65553741364963E-17));
#258934=CARTESIAN_POINT('Ctrl Pts',(1.81235319455274,2.24041903484712,-9.0205620750794E-17));
#258935=CARTESIAN_POINT('Ctrl Pts',(1.83051349989456,2.22223287885251,-8.70734994005395E-17));
#258936=CARTESIAN_POINT('Ctrl Pts',(1.84843686678461,2.20378515234822,-5.57779331647957E-16));
#258937=CARTESIAN_POINT('Ctrl Pts',(1.8661191808394,2.18508218765713,-5.62050406216485E-16));
#258938=CARTESIAN_POINT('Ctrl Pts',(1.8813003216564,2.16902476780864,-5.6571733489244E-16));
#258939=CARTESIAN_POINT('Ctrl Pts',(1.89630589148148,2.15277668641829,-8.7084074591344E-16));
#258940=CARTESIAN_POINT('Ctrl Pts',(1.91111646711286,2.13636094210903,-8.53483950180589E-16));
#258941=CARTESIAN_POINT('Ctrl Pts',(1.97625654995093,2.06416098373011,-7.77145046144621E-16));
#258942=CARTESIAN_POINT('Ctrl Pts',(2.03769603328323,1.98865039987372,-5.52894930421052E-17));
#258943=CARTESIAN_POINT('Ctrl Pts',(2.09526132380736,1.910204650615,-2.35922392732846E-16));
#258944=CARTESIAN_POINT('Ctrl Pts',(2.14247204912315,1.84586934218999,-3.84063922683431E-16));
#258945=CARTESIAN_POINT('Ctrl Pts',(2.18707626360589,1.77955897818102,-1.9456188113995E-16));
#258946=CARTESIAN_POINT('Ctrl Pts',(2.22895387699605,1.71147104687654,-1.2490009027033E-16));
#258947=CARTESIAN_POINT('Ctrl Pts',(2.24792551730372,1.68062545570191,-9.33415000695447E-17));
#258948=CARTESIAN_POINT('Ctrl Pts',(2.26633725889061,1.64941497047097,-2.71651496365891E-16));
#258949=CARTESIAN_POINT('Ctrl Pts',(2.28417633551315,1.61785769665074,-3.19189119579733E-16));
#258950=CARTESIAN_POINT('Ctrl Pts',(2.29466973440569,1.59929490502404,-3.47151959436352E-16));
#258951=CARTESIAN_POINT('Ctrl Pts',(2.3049649666982,1.58061211955791,-4.10929051741138E-16));
#258952=CARTESIAN_POINT('Ctrl Pts',(2.31505926524131,1.56181301987131,-4.16333634234434E-16));
#258953=CARTESIAN_POINT('Ctrl Pts',(2.32233104844966,1.54827042680759,-4.20227015439185E-16));
#258954=CARTESIAN_POINT('Ctrl Pts',(2.3294983759238,1.53466764779613,-6.49847629289258E-17));
#258955=CARTESIAN_POINT('Ctrl Pts',(2.33655394576526,1.52101860731817,-8.32667268468867E-17));
#258956=CARTESIAN_POINT('Ctrl Pts',(2.38021790436486,1.43655042802932,-1.96406123602879E-16));
#258957=CARTESIAN_POINT('Ctrl Pts',(2.41967121036231,1.3501913449407,6.88706256054415E-17));
#258958=CARTESIAN_POINT('Ctrl Pts',(2.45474928345663,1.26228765150751,4.16333634234434E-17));
#258959=CARTESIAN_POINT('Ctrl Pts',(2.49092308776736,1.1716381167998,1.35452928648742E-17));
#258960=CARTESIAN_POINT('Ctrl Pts',(2.52244468369081,1.07934497178013,-2.21712706299005E-16));
#258961=CARTESIAN_POINT('Ctrl Pts',(2.54907591826243,0.985777684531876,
-6.93889390390723E-17));
#258962=CARTESIAN_POINT('Ctrl Pts',(2.57381682909422,0.898851939337636,
7.21226658098787E-17));
#258963=CARTESIAN_POINT('Ctrl Pts',(2.59433663472327,0.810825740820981,
-9.80095638385124E-17));
#258964=CARTESIAN_POINT('Ctrl Pts',(2.61039511711921,0.721999381027909,
-2.77555756156289E-17));
#258965=CARTESIAN_POINT('Ctrl Pts',(2.6195878391639,0.671150489103632,1.24615115499021E-17));
#258966=CARTESIAN_POINT('Ctrl Pts',(2.62731768360901,0.620039518677072,
-3.00496852254879E-16));
#258967=CARTESIAN_POINT('Ctrl Pts',(2.63353210695095,0.568724824688507,
-3.60822483003176E-16));
#258968=CARTESIAN_POINT('Ctrl Pts',(2.63589786401921,0.549189930889105,
-3.8378773327462E-16));
#258969=CARTESIAN_POINT('Ctrl Pts',(2.63804436688365,0.529620027364891,
-4.11084434172389E-16));
#258970=CARTESIAN_POINT('Ctrl Pts',(2.63996573358163,0.510050166638142,
-4.16333634234434E-16));
#258971=CARTESIAN_POINT('Ctrl Pts',(2.64867955611758,0.421296523929082,
-4.40139916421116E-16));
#258972=CARTESIAN_POINT('Ctrl Pts',(2.65278205939108,0.332438665006606,
4.43189382769785E-16));
#258973=CARTESIAN_POINT('Ctrl Pts',(2.6520903038075,0.243767416134848,3.05311331771918E-16));
#258974=CARTESIAN_POINT('Ctrl Pts',(2.65177499678039,0.203350441505137,
2.4246555300958E-16));
#258975=CARTESIAN_POINT('Ctrl Pts',(2.65046293738114,0.162972281097136,
-4.01413413377188E-16));
#258976=CARTESIAN_POINT('Ctrl Pts',(2.6481332116628,0.122661008583792,-4.16333634234434E-16));
#258977=CARTESIAN_POINT('Ctrl Pts',(2.64291502376441,0.0323706397470573,
-4.48739692579806E-16));
#258978=CARTESIAN_POINT('Ctrl Pts',(2.63259442660143,-0.0575857021650941,
-6.13287208414012E-16));
#258979=CARTESIAN_POINT('Ctrl Pts',(2.61736772417562,-0.146875162641521,
-7.21644966006352E-16));
#258980=CARTESIAN_POINT('Ctrl Pts',(2.60171400810126,-0.238668633325112,
-8.33041480128173E-16));
#258981=CARTESIAN_POINT('Ctrl Pts',(2.5808746796005,-0.329758351676144,
-1.90458112270157E-16));
#258982=CARTESIAN_POINT('Ctrl Pts',(2.55501621449523,-0.419750916628513,
-2.4980018054066E-16));
#258983=CARTESIAN_POINT('Ctrl Pts',(2.55103891410019,-0.433592707418413,
-2.58927606728312E-16));
#258984=CARTESIAN_POINT('Ctrl Pts',(2.54694279346922,-0.447408464297446,
3.75767635899293E-16));
#258985=CARTESIAN_POINT('Ctrl Pts',(2.5427283753618,-0.461196666179357,
3.88578058618805E-16));
#258986=CARTESIAN_POINT('Ctrl Pts',(2.53849453512576,-0.475048410933263,
4.0144751811904E-16));
#258987=CARTESIAN_POINT('Ctrl Pts',(2.53414344842462,-0.488865206644749,
8.48754092844161E-17));
#258988=CARTESIAN_POINT('Ctrl Pts',(2.52967811492983,-0.502639383000654,
8.32667268468867E-17));
#258989=CARTESIAN_POINT('Ctrl Pts',(2.50231167638331,-0.58705640385971,
7.340768516079E-17));
#258990=CARTESIAN_POINT('Ctrl Pts',(2.47063498600197,-0.669950084265983,
4.22436203556581E-17));
#258991=CARTESIAN_POINT('Ctrl Pts',(2.43486046177467,-0.751017022735213,
-2.77555756156289E-17));
#258992=CARTESIAN_POINT('Ctrl Pts',(2.399141311881,-0.831958480075241,-9.76464218907314E-17));
#258993=CARTESIAN_POINT('Ctrl Pts',(2.3593363425435,-0.911079627280405,
2.35473293751788E-18));
#258994=CARTESIAN_POINT('Ctrl Pts',(2.31561489444494,-0.98804847264715,
5.55111512312578E-17));
#258995=CARTESIAN_POINT('Ctrl Pts',(2.27259325787788,-1.06378534405382,
1.0781674055859E-16));
#258996=CARTESIAN_POINT('Ctrl Pts',(2.22577883862421,-1.13743887886136,
-1.12290620317281E-16));
#258997=CARTESIAN_POINT('Ctrl Pts',(2.17530221885831,-1.20865349993215,
-1.66533453693773E-16));
#258998=CARTESIAN_POINT('Ctrl Pts',(2.15809729115553,-1.23292696381674,
-1.85022093205784E-16));
#258999=CARTESIAN_POINT('Ctrl Pts',(2.14046667353494,-1.25691669716042,
-1.35829105932757E-16));
#259000=CARTESIAN_POINT('Ctrl Pts',(2.12241491153992,-1.28060735992797,
-1.66533453693773E-16));
#259001=CARTESIAN_POINT('Ctrl Pts',(2.11071608335196,-1.29596059765916,
-1.8643205911404E-16));
#259002=CARTESIAN_POINT('Ctrl Pts',(2.09884037016556,-1.31118821315322,
-3.70177197692537E-16));
#259003=CARTESIAN_POINT('Ctrl Pts',(2.08678895088832,-1.32628587161512,
-3.88578058618805E-16));
#259004=CARTESIAN_POINT('Ctrl Pts',(2.07852306914528,-1.33664112161282,
-4.01198924003022E-16));
#259005=CARTESIAN_POINT('Ctrl Pts',(2.07018042347752,-1.34692783442558,
-1.72843886385882E-16));
#259006=CARTESIAN_POINT('Ctrl Pts',(2.06176261244685,-1.35714381216209,
-1.66533453693773E-16));
#259007=CARTESIAN_POINT('Ctrl Pts',(2.00753927090544,-1.42295004705715,
-1.25884792671121E-16));
#259008=CARTESIAN_POINT('Ctrl Pts',(1.95018700439859,-1.48584042548277,
6.40190105150689E-17));
#259009=CARTESIAN_POINT('Ctrl Pts',(1.88986384968284,-1.54551861016893,
5.55111512312578E-17));
#259010=CARTESIAN_POINT('Ctrl Pts',(1.83049021222098,-1.60425742975877,
4.71372099963581E-17));
#259011=CARTESIAN_POINT('Ctrl Pts',(1.76823783877865,-1.65988489840281,
6.01633408062021E-17));
#259012=CARTESIAN_POINT('Ctrl Pts',(1.70323154838963,-1.71207601348042,
5.55111512312578E-17));
#259013=CARTESIAN_POINT('Ctrl Pts',(1.64025200525105,-1.76263992912321,
5.10040062723506E-17));
#259014=CARTESIAN_POINT('Ctrl Pts',(1.57468702241033,-1.80997871266923,
3.69270603532203E-16));
#259015=CARTESIAN_POINT('Ctrl Pts',(1.50663444364591,-1.85375106403961,
4.44089209850063E-16));
#259016=CARTESIAN_POINT('Ctrl Pts',(1.46438318762361,-1.88092765099674,
4.90541234860173E-16));
#259017=CARTESIAN_POINT('Ctrl Pts',(1.42117276288613,-1.90672856661623,
5.10338476158255E-17));
#259018=CARTESIAN_POINT('Ctrl Pts',(1.37702479013104,-1.93106208855763,
5.55111512312578E-17));
#259019=CARTESIAN_POINT('Ctrl Pts',(1.28892185405323,2.64462557919718,20.));
#259020=CARTESIAN_POINT('Ctrl Pts',(2.16862035685408,2.21588336549518,19.9470592864818));
#259021=CARTESIAN_POINT('Ctrl Pts',(2.80996391709042,1.31742092770971,19.8941185729635));
#259022=CARTESIAN_POINT('Ctrl Pts',(2.92551966779744,0.35179538187613,19.8411778594453));
#259023=CARTESIAN_POINT('Ctrl Pts',(3.04107541850447,-0.613830163957432,
19.788237145927));
#259024=CARTESIAN_POINT('Ctrl Pts',(2.63084335968222,-1.6466188178391,19.7352964324088));
#259025=CARTESIAN_POINT('Ctrl Pts',(1.88115112934642,-2.26900194906848,
19.6823557188906));
#259026=CARTESIAN_POINT('Ctrl Pts',(1.13145889901062,-2.89138508029788,
19.6294150053723));
#259027=CARTESIAN_POINT('Ctrl Pts',(0.0423064971612432,-3.10336268887498,
19.576474291854));
#259028=CARTESIAN_POINT('Ctrl Pts',(-0.886796187095413,-2.80996684498319,
19.5235335783358));
#259029=CARTESIAN_POINT('Ctrl Pts',(-1.81589887135208,-2.5165710010914,
19.4705928648176));
#259030=CARTESIAN_POINT('Ctrl Pts',(-2.58495183801603,-1.71780170473074,
19.4176521512993));
#259031=CARTESIAN_POINT('Ctrl Pts',(-2.84215954961242,-0.778381846021926,
19.3647114377811));
#259032=CARTESIAN_POINT('Ctrl Pts',(-2.91104423067048,-0.526788933254545,
19.3505329975506));
#259033=CARTESIAN_POINT('Ctrl Pts',(-2.94321623800843,-0.265107701502241,
19.3363545573201));
#259034=CARTESIAN_POINT('Ctrl Pts',(-2.94091171156293,-0.00284992947760021,
19.3221761170896));
#259035=CARTESIAN_POINT('Origin',(0.,0.,0.));
#259036=CARTESIAN_POINT('Origin',(0.,0.,20.));
#259037=CARTESIAN_POINT('Origin',(-1.44337567297407,-2.5,-6.));
#259038=CARTESIAN_POINT('',(-1.44337567297407,-2.5,-6.));
#259039=CARTESIAN_POINT('',(1.44337567297406,-2.5,-6.));
#259040=CARTESIAN_POINT('',(-0.721687836487033,-2.5,-6.));
#259041=CARTESIAN_POINT('',(-1.44337567297407,-2.5,-3.));
#259042=CARTESIAN_POINT('',(-1.44337567297407,-2.5,-6.));
#259043=CARTESIAN_POINT('',(1.44337567297406,-2.5,-3.));
#259044=CARTESIAN_POINT('',(-1.44337567297407,-2.5,-3.));
#259045=CARTESIAN_POINT('',(1.44337567297406,-2.5,-6.));
#259046=CARTESIAN_POINT('Origin',(-2.88675134594813,3.53525079574969E-16,
-6.));
#259047=CARTESIAN_POINT('',(-2.88675134594813,3.53525079574969E-16,-6.));
#259048=CARTESIAN_POINT('',(-2.52590742770461,-0.625,-6.));
#259049=CARTESIAN_POINT('',(-2.88675134594813,5.55111512312578E-16,-3.));
#259050=CARTESIAN_POINT('',(-2.88675134594813,3.53525079574969E-16,-6.));
#259051=CARTESIAN_POINT('',(-2.88675134594813,3.53525079574969E-16,-3.));
#259052=CARTESIAN_POINT('Origin',(-1.44337567297406,2.5,-6.));
#259053=CARTESIAN_POINT('',(-1.44337567297406,2.5,-6.));
#259054=CARTESIAN_POINT('',(-1.80421959121758,1.875,-6.));
#259055=CARTESIAN_POINT('',(-1.44337567297406,2.5,-3.));
#259056=CARTESIAN_POINT('',(-1.44337567297406,2.5,-6.));
#259057=CARTESIAN_POINT('',(-1.44337567297406,2.5,-3.));
#259058=CARTESIAN_POINT('Origin',(1.44337567297406,2.5,-6.));
#259059=CARTESIAN_POINT('',(1.44337567297406,2.5,-6.));
#259060=CARTESIAN_POINT('',(0.721687836487033,2.5,-6.));
#259061=CARTESIAN_POINT('',(1.44337567297406,2.5,-3.));
#259062=CARTESIAN_POINT('',(1.44337567297406,2.5,-6.));
#259063=CARTESIAN_POINT('',(1.44337567297406,2.5,-3.));
#259064=CARTESIAN_POINT('Origin',(2.88675134594813,0.,-6.));
#259065=CARTESIAN_POINT('',(2.88675134594813,0.,-6.));
#259066=CARTESIAN_POINT('',(2.52590742770461,0.625,-6.));
#259067=CARTESIAN_POINT('',(2.88675134594813,0.,-3.));
#259068=CARTESIAN_POINT('',(2.88675134594813,0.,-6.));
#259069=CARTESIAN_POINT('',(2.88675134594813,0.,-3.));
#259070=CARTESIAN_POINT('Origin',(1.44337567297406,-2.5,-6.));
#259071=CARTESIAN_POINT('',(1.80421959121758,-1.875,-6.));
#259072=CARTESIAN_POINT('',(1.44337567297406,-2.5,-3.));
#259073=CARTESIAN_POINT('Origin',(0.,0.,-3.));
#259074=CARTESIAN_POINT('Origin',(0.,0.,0.));
#259075=CARTESIAN_POINT('',(-5.,-6.12323399573677E-16,0.));
#259076=CARTESIAN_POINT('Origin',(0.,0.,0.));
#259077=CARTESIAN_POINT('Origin',(0.,0.,-6.));
#259078=CARTESIAN_POINT('',(-5.,-6.12323399573677E-16,-6.));
#259079=CARTESIAN_POINT('',(-5.,-6.12323399573677E-16,-6.));
#259080=CARTESIAN_POINT('Origin',(0.,0.,-6.));
#259081=CARTESIAN_POINT('Origin',(0.,0.,-6.));
#259082=CARTESIAN_POINT('Origin',(0.,0.,20.));
#259083=CARTESIAN_POINT('',(0.,0.,30.));
#259084=CARTESIAN_POINT('',(48.,0.,30.));
#259085=CARTESIAN_POINT('',(0.,0.,30.));
#259086=CARTESIAN_POINT('',(-24.,41.5692193816531,30.));
#259087=CARTESIAN_POINT('',(-24.,-41.569219381653,30.));
#259088=CARTESIAN_POINT('',(0.,0.,0.));
#259089=CARTESIAN_POINT('',(0.,0.,66.));
#259090=CARTESIAN_POINT('',(0.,0.,122.));
#259091=CARTESIAN_POINT('',(0.,0.,2.));
#259092=CARTESIAN_POINT('',(0.,0.,0.));
#259093=CARTESIAN_POINT('',(0.,0.,0.));
#259094=CARTESIAN_POINT('',(0.,0.,30.));
#259095=CARTESIAN_POINT('',(48.,0.,30.));
#259096=CARTESIAN_POINT('',(0.,0.,86.));
#259097=CARTESIAN_POINT('',(0.,0.,86.));
#259098=CARTESIAN_POINT('',(48.,0.,86.));
#259099=CARTESIAN_POINT('',(-24.,41.5692193816531,86.));
#259100=CARTESIAN_POINT('',(-24.,-41.569219381653,86.));
#259101=CARTESIAN_POINT('',(0.,0.,66.));
#259102=CARTESIAN_POINT('',(0.,0.,122.));
#259103=CARTESIAN_POINT('',(0.,0.,56.));
#259104=CARTESIAN_POINT('',(0.,0.,86.));
#259105=CARTESIAN_POINT('',(48.,0.,28.));
#259106=CARTESIAN_POINT('',(48.,0.,28.));
#259107=CARTESIAN_POINT('',(48.,0.,56.));
#259108=CARTESIAN_POINT('',(-24.,41.5692193816531,30.));
#259109=CARTESIAN_POINT('',(-24.,-41.569219381653,30.));
#259110=CARTESIAN_POINT('',(48.,0.,86.));
#259111=CARTESIAN_POINT('',(-24.,41.5692193816531,86.));
#259112=CARTESIAN_POINT('',(-24.,-41.569219381653,86.));
#259113=CARTESIAN_POINT('',(0.,0.,28.));
#259114=CARTESIAN_POINT('',(0.,0.,-2.));
#259115=CARTESIAN_POINT('',(0.,0.,44.));
#259116=CARTESIAN_POINT('',(0.,0.,-3.));
#259117=CARTESIAN_POINT('',(100.,0.,36.));
#259118=CARTESIAN_POINT('',(87.7685555885722,36.3549260746835,130.));
#259119=CARTESIAN_POINT('',(48.,0.,42.));
#259120=CARTESIAN_POINT('',(48.,0.,44.));
#259121=CARTESIAN_POINT('',(48.,0.,54.));
#259122=CARTESIAN_POINT('',(-24.,41.5692193816531,28.));
#259123=CARTESIAN_POINT('',(-24.,41.5692193816531,56.));
#259124=CARTESIAN_POINT('',(-24.,41.5692193816531,28.));
#259125=CARTESIAN_POINT('',(-24.,41.5692193816531,42.));
#259126=CARTESIAN_POINT('',(-24.,41.5692193816531,44.));
#259127=CARTESIAN_POINT('',(-24.,41.5692193816531,54.));
#259128=CARTESIAN_POINT('',(-24.,-41.569219381653,28.));
#259129=CARTESIAN_POINT('',(-24.,-41.569219381653,56.));
#259130=CARTESIAN_POINT('',(-24.,-41.569219381653,28.));
#259131=CARTESIAN_POINT('',(-24.,-41.569219381653,42.));
#259132=CARTESIAN_POINT('',(-24.,-41.569219381653,44.));
#259133=CARTESIAN_POINT('',(-24.,-41.569219381653,54.));
#259134=CARTESIAN_POINT('',(48.,0.,84.));
#259135=CARTESIAN_POINT('',(48.,0.,112.));
#259136=CARTESIAN_POINT('',(48.,0.,84.));
#259137=CARTESIAN_POINT('',(48.,0.,98.));
#259138=CARTESIAN_POINT('',(48.,0.,100.));
#259139=CARTESIAN_POINT('',(48.,0.,110.));
#259140=CARTESIAN_POINT('',(-24.,41.5692193816531,84.));
#259141=CARTESIAN_POINT('',(-24.,41.5692193816531,112.));
#259142=CARTESIAN_POINT('',(-24.,41.5692193816531,84.));
#259143=CARTESIAN_POINT('',(-24.,41.5692193816531,98.));
#259144=CARTESIAN_POINT('',(-24.,41.5692193816531,100.));
#259145=CARTESIAN_POINT('',(-24.,41.5692193816531,110.));
#259146=CARTESIAN_POINT('',(-24.,-41.569219381653,84.));
#259147=CARTESIAN_POINT('',(-24.,-41.569219381653,112.));
#259148=CARTESIAN_POINT('',(-24.,-41.569219381653,84.));
#259149=CARTESIAN_POINT('',(-24.,-41.569219381653,98.));
#259150=CARTESIAN_POINT('',(-24.,-41.569219381653,100.));
#259151=CARTESIAN_POINT('',(-24.,-41.569219381653,110.));
#259152=CARTESIAN_POINT('',(0.,0.,42.));
#259153=CARTESIAN_POINT('',(0.,0.,84.));
#259154=CARTESIAN_POINT('',(0.,0.,98.));
#259155=CARTESIAN_POINT('',(0.,0.,10.));
#259156=CARTESIAN_POINT('',(0.,0.,64.));
#259157=CARTESIAN_POINT('',(0.,0.,74.));
#259158=CARTESIAN_POINT('',(0.,0.,120.));
#259159=CARTESIAN_POINT('',(0.,0.,130.));
#259160=CARTESIAN_POINT('',(0.,0.,100.));
#259161=CARTESIAN_POINT('',(0.,0.,76.));
#259162=CARTESIAN_POINT('',(0.,0.,132.));
#259163=CARTESIAN_POINT('',(-100.,0.,36.));
#259164=CARTESIAN_POINT('',(0.,100.,36.));
#259165=CARTESIAN_POINT('',(0.,-100.,36.));
#259166=CARTESIAN_POINT('',(100.,0.,70.));
#259167=CARTESIAN_POINT('',(-100.,0.,70.));
#259168=CARTESIAN_POINT('',(0.,100.,70.));
#259169=CARTESIAN_POINT('',(0.,-100.,70.));
#259170=CARTESIAN_POINT('',(100.,0.,92.));
#259171=CARTESIAN_POINT('',(-100.,0.,92.));
#259172=CARTESIAN_POINT('',(1.77635683940025E-14,100.,92.));
#259173=CARTESIAN_POINT('',(1.77635683940025E-14,-100.,92.));
#259174=CARTESIAN_POINT('',(36.3549260746835,87.7685555885722,130.));
#259175=CARTESIAN_POINT('',(-36.3549260746835,87.7685555885722,130.));
#259176=CARTESIAN_POINT('',(-87.7685555885722,36.3549260746835,130.));
#259177=CARTESIAN_POINT('',(-87.7685555885722,-36.3549260746835,130.));
#259178=CARTESIAN_POINT('',(-36.3549260746835,-87.7685555885722,130.));
#259179=CARTESIAN_POINT('',(36.3549260746835,-87.7685555885722,130.));
#259180=CARTESIAN_POINT('',(87.7685555885722,-36.3549260746835,130.));
#259181=UNCERTAINTY_MEASURE_WITH_UNIT(LENGTH_MEASURE(0.01),#259225,
'DISTANCE_ACCURACY_VALUE',
'Maximum model space distance between geometric entities at asserted c
onnectivities');
#259182=UNCERTAINTY_MEASURE_WITH_UNIT(LENGTH_MEASURE(0.01),#259225,
'DISTANCE_ACCURACY_VALUE',
'Maximum model space distance between geometric entities at asserted c
onnectivities');
#259183=UNCERTAINTY_MEASURE_WITH_UNIT(LENGTH_MEASURE(0.01),#259225,
'DISTANCE_ACCURACY_VALUE',
'Maximum model space distance between geometric entities at asserted c
onnectivities');
#259184=UNCERTAINTY_MEASURE_WITH_UNIT(LENGTH_MEASURE(0.01),#259225,
'DISTANCE_ACCURACY_VALUE',
'Maximum model space distance between geometric entities at asserted c
onnectivities');
#259185=UNCERTAINTY_MEASURE_WITH_UNIT(LENGTH_MEASURE(0.01),#259225,
'DISTANCE_ACCURACY_VALUE',
'Maximum model space distance between geometric entities at asserted c
onnectivities');
#259186=UNCERTAINTY_MEASURE_WITH_UNIT(LENGTH_MEASURE(0.01),#259225,
'DISTANCE_ACCURACY_VALUE',
'Maximum model space distance between geometric entities at asserted c
onnectivities');
#259187=UNCERTAINTY_MEASURE_WITH_UNIT(LENGTH_MEASURE(0.01),#259225,
'DISTANCE_ACCURACY_VALUE',
'Maximum model space distance between geometric entities at asserted c
onnectivities');
#259188=UNCERTAINTY_MEASURE_WITH_UNIT(LENGTH_MEASURE(0.01),#259225,
'DISTANCE_ACCURACY_VALUE',
'Maximum model space distance between geometric entities at asserted c
onnectivities');
#259189=UNCERTAINTY_MEASURE_WITH_UNIT(LENGTH_MEASURE(0.01),#259225,
'DISTANCE_ACCURACY_VALUE',
'Maximum model space distance between geometric entities at asserted c
onnectivities');
#259190=UNCERTAINTY_MEASURE_WITH_UNIT(LENGTH_MEASURE(0.01),#259225,
'DISTANCE_ACCURACY_VALUE',
'Maximum model space distance between geometric entities at asserted c
onnectivities');
#259191=UNCERTAINTY_MEASURE_WITH_UNIT(LENGTH_MEASURE(0.01),#259225,
'DISTANCE_ACCURACY_VALUE',
'Maximum model space distance between geometric entities at asserted c
onnectivities');
#259192=UNCERTAINTY_MEASURE_WITH_UNIT(LENGTH_MEASURE(0.01),#259225,
'DISTANCE_ACCURACY_VALUE',
'Maximum model space distance between geometric entities at asserted c
onnectivities');
#259193=UNCERTAINTY_MEASURE_WITH_UNIT(LENGTH_MEASURE(0.01),#259225,
'DISTANCE_ACCURACY_VALUE',
'Maximum model space distance between geometric entities at asserted c
onnectivities');
#259194=UNCERTAINTY_MEASURE_WITH_UNIT(LENGTH_MEASURE(0.01),#259225,
'DISTANCE_ACCURACY_VALUE',
'Maximum model space distance between geometric entities at asserted c
onnectivities');
#259195=UNCERTAINTY_MEASURE_WITH_UNIT(LENGTH_MEASURE(0.01),#259225,
'DISTANCE_ACCURACY_VALUE',
'Maximum model space distance between geometric entities at asserted c
onnectivities');
#259196=UNCERTAINTY_MEASURE_WITH_UNIT(LENGTH_MEASURE(0.01),#259225,
'DISTANCE_ACCURACY_VALUE',
'Maximum model space distance between geometric entities at asserted c
onnectivities');
#259197=UNCERTAINTY_MEASURE_WITH_UNIT(LENGTH_MEASURE(0.01),#259225,
'DISTANCE_ACCURACY_VALUE',
'Maximum model space distance between geometric entities at asserted c
onnectivities');
#259198=UNCERTAINTY_MEASURE_WITH_UNIT(LENGTH_MEASURE(0.01),#259225,
'DISTANCE_ACCURACY_VALUE',
'Maximum model space distance between geometric entities at asserted c
onnectivities');
#259199=UNCERTAINTY_MEASURE_WITH_UNIT(LENGTH_MEASURE(0.01),#259225,
'DISTANCE_ACCURACY_VALUE',
'Maximum model space distance between geometric entities at asserted c
onnectivities');
#259200=UNCERTAINTY_MEASURE_WITH_UNIT(LENGTH_MEASURE(0.01),#259225,
'DISTANCE_ACCURACY_VALUE',
'Maximum model space distance between geometric entities at asserted c
onnectivities');
#259201=UNCERTAINTY_MEASURE_WITH_UNIT(LENGTH_MEASURE(0.01),#259225,
'DISTANCE_ACCURACY_VALUE',
'Maximum model space distance between geometric entities at asserted c
onnectivities');
#259202=UNCERTAINTY_MEASURE_WITH_UNIT(LENGTH_MEASURE(0.01),#259225,
'DISTANCE_ACCURACY_VALUE',
'Maximum model space distance between geometric entities at asserted c
onnectivities');
#259203=(
GEOMETRIC_REPRESENTATION_CONTEXT(3)
GLOBAL_UNCERTAINTY_ASSIGNED_CONTEXT((#259181))
GLOBAL_UNIT_ASSIGNED_CONTEXT((#259225,#259227,#259228))
REPRESENTATION_CONTEXT('','3D')
);
#259204=(
GEOMETRIC_REPRESENTATION_CONTEXT(3)
GLOBAL_UNCERTAINTY_ASSIGNED_CONTEXT((#259182))
GLOBAL_UNIT_ASSIGNED_CONTEXT((#259225,#259227,#259228))
REPRESENTATION_CONTEXT('','3D')
);
#259205=(
GEOMETRIC_REPRESENTATION_CONTEXT(3)
GLOBAL_UNCERTAINTY_ASSIGNED_CONTEXT((#259183))
GLOBAL_UNIT_ASSIGNED_CONTEXT((#259225,#259227,#259228))
REPRESENTATION_CONTEXT('','3D')
);
#259206=(
GEOMETRIC_REPRESENTATION_CONTEXT(3)
GLOBAL_UNCERTAINTY_ASSIGNED_CONTEXT((#259184))
GLOBAL_UNIT_ASSIGNED_CONTEXT((#259225,#259227,#259228))
REPRESENTATION_CONTEXT('','3D')
);
#259207=(
GEOMETRIC_REPRESENTATION_CONTEXT(3)
GLOBAL_UNCERTAINTY_ASSIGNED_CONTEXT((#259185))
GLOBAL_UNIT_ASSIGNED_CONTEXT((#259225,#259227,#259228))
REPRESENTATION_CONTEXT('','3D')
);
#259208=(
GEOMETRIC_REPRESENTATION_CONTEXT(3)
GLOBAL_UNCERTAINTY_ASSIGNED_CONTEXT((#259186))
GLOBAL_UNIT_ASSIGNED_CONTEXT((#259225,#259227,#259228))
REPRESENTATION_CONTEXT('','3D')
);
#259209=(
GEOMETRIC_REPRESENTATION_CONTEXT(3)
GLOBAL_UNCERTAINTY_ASSIGNED_CONTEXT((#259187))
GLOBAL_UNIT_ASSIGNED_CONTEXT((#259225,#259227,#259228))
REPRESENTATION_CONTEXT('','3D')
);
#259210=(
GEOMETRIC_REPRESENTATION_CONTEXT(3)
GLOBAL_UNCERTAINTY_ASSIGNED_CONTEXT((#259188))
GLOBAL_UNIT_ASSIGNED_CONTEXT((#259225,#259227,#259228))
REPRESENTATION_CONTEXT('','3D')
);
#259211=(
GEOMETRIC_REPRESENTATION_CONTEXT(3)
GLOBAL_UNCERTAINTY_ASSIGNED_CONTEXT((#259189))
GLOBAL_UNIT_ASSIGNED_CONTEXT((#259225,#259227,#259228))
REPRESENTATION_CONTEXT('','3D')
);
#259212=(
GEOMETRIC_REPRESENTATION_CONTEXT(3)
GLOBAL_UNCERTAINTY_ASSIGNED_CONTEXT((#259190))
GLOBAL_UNIT_ASSIGNED_CONTEXT((#259225,#259227,#259228))
REPRESENTATION_CONTEXT('','3D')
);
#259213=(
GEOMETRIC_REPRESENTATION_CONTEXT(3)
GLOBAL_UNCERTAINTY_ASSIGNED_CONTEXT((#259191))
GLOBAL_UNIT_ASSIGNED_CONTEXT((#259225,#259227,#259228))
REPRESENTATION_CONTEXT('','3D')
);
#259214=(
GEOMETRIC_REPRESENTATION_CONTEXT(3)
GLOBAL_UNCERTAINTY_ASSIGNED_CONTEXT((#259192))
GLOBAL_UNIT_ASSIGNED_CONTEXT((#259225,#259227,#259228))
REPRESENTATION_CONTEXT('','3D')
);
#259215=(
GEOMETRIC_REPRESENTATION_CONTEXT(3)
GLOBAL_UNCERTAINTY_ASSIGNED_CONTEXT((#259193))
GLOBAL_UNIT_ASSIGNED_CONTEXT((#259225,#259227,#259228))
REPRESENTATION_CONTEXT('','3D')
);
#259216=(
GEOMETRIC_REPRESENTATION_CONTEXT(3)
GLOBAL_UNCERTAINTY_ASSIGNED_CONTEXT((#259194))
GLOBAL_UNIT_ASSIGNED_CONTEXT((#259225,#259227,#259228))
REPRESENTATION_CONTEXT('','3D')
);
#259217=(
GEOMETRIC_REPRESENTATION_CONTEXT(3)
GLOBAL_UNCERTAINTY_ASSIGNED_CONTEXT((#259195))
GLOBAL_UNIT_ASSIGNED_CONTEXT((#259225,#259227,#259228))
REPRESENTATION_CONTEXT('','3D')
);
#259218=(
GEOMETRIC_REPRESENTATION_CONTEXT(3)
GLOBAL_UNCERTAINTY_ASSIGNED_CONTEXT((#259196))
GLOBAL_UNIT_ASSIGNED_CONTEXT((#259225,#259227,#259228))
REPRESENTATION_CONTEXT('','3D')
);
#259219=(
GEOMETRIC_REPRESENTATION_CONTEXT(3)
GLOBAL_UNCERTAINTY_ASSIGNED_CONTEXT((#259197))
GLOBAL_UNIT_ASSIGNED_CONTEXT((#259225,#259227,#259228))
REPRESENTATION_CONTEXT('','3D')
);
#259220=(
GEOMETRIC_REPRESENTATION_CONTEXT(3)
GLOBAL_UNCERTAINTY_ASSIGNED_CONTEXT((#259198))
GLOBAL_UNIT_ASSIGNED_CONTEXT((#259225,#259227,#259228))
REPRESENTATION_CONTEXT('','3D')
);
#259221=(
GEOMETRIC_REPRESENTATION_CONTEXT(3)
GLOBAL_UNCERTAINTY_ASSIGNED_CONTEXT((#259199))
GLOBAL_UNIT_ASSIGNED_CONTEXT((#259225,#259227,#259228))
REPRESENTATION_CONTEXT('','3D')
);
#259222=(
GEOMETRIC_REPRESENTATION_CONTEXT(3)
GLOBAL_UNCERTAINTY_ASSIGNED_CONTEXT((#259200))
GLOBAL_UNIT_ASSIGNED_CONTEXT((#259225,#259227,#259228))
REPRESENTATION_CONTEXT('','3D')
);
#259223=(
GEOMETRIC_REPRESENTATION_CONTEXT(3)
GLOBAL_UNCERTAINTY_ASSIGNED_CONTEXT((#259201))
GLOBAL_UNIT_ASSIGNED_CONTEXT((#259225,#259227,#259228))
REPRESENTATION_CONTEXT('','3D')
);
#259224=(
GEOMETRIC_REPRESENTATION_CONTEXT(3)
GLOBAL_UNCERTAINTY_ASSIGNED_CONTEXT((#259202))
GLOBAL_UNIT_ASSIGNED_CONTEXT((#259225,#259227,#259228))
REPRESENTATION_CONTEXT('','3D')
);
#259225=(
LENGTH_UNIT()
NAMED_UNIT(*)
SI_UNIT(.MILLI.,.METRE.)
);
#259226=(
LENGTH_UNIT()
NAMED_UNIT(*)
SI_UNIT($,.METRE.)
);
#259227=(
NAMED_UNIT(*)
PLANE_ANGLE_UNIT()
SI_UNIT($,.RADIAN.)
);
#259228=(
NAMED_UNIT(*)
SI_UNIT($,.STERADIAN.)
SOLID_ANGLE_UNIT()
);
#259229=SHAPE_DEFINITION_REPRESENTATION(#259250,#259369);
#259230=SHAPE_DEFINITION_REPRESENTATION(#259251,#259370);
#259231=SHAPE_DEFINITION_REPRESENTATION(#259252,#259371);
#259232=SHAPE_DEFINITION_REPRESENTATION(#259253,#259372);
#259233=SHAPE_DEFINITION_REPRESENTATION(#259254,#259373);
#259234=SHAPE_DEFINITION_REPRESENTATION(#259255,#259374);
#259235=SHAPE_DEFINITION_REPRESENTATION(#259256,#259375);
#259236=SHAPE_DEFINITION_REPRESENTATION(#259257,#259376);
#259237=SHAPE_DEFINITION_REPRESENTATION(#259258,#259377);
#259238=SHAPE_DEFINITION_REPRESENTATION(#259259,#259378);
#259239=SHAPE_DEFINITION_REPRESENTATION(#259260,#259379);
#259240=SHAPE_DEFINITION_REPRESENTATION(#259261,#259380);
#259241=SHAPE_DEFINITION_REPRESENTATION(#259262,#259381);
#259242=SHAPE_DEFINITION_REPRESENTATION(#259263,#259382);
#259243=SHAPE_DEFINITION_REPRESENTATION(#259264,#259383);
#259244=SHAPE_DEFINITION_REPRESENTATION(#259265,#259384);
#259245=SHAPE_DEFINITION_REPRESENTATION(#259266,#259385);
#259246=SHAPE_DEFINITION_REPRESENTATION(#259267,#259386);
#259247=SHAPE_DEFINITION_REPRESENTATION(#259268,#259387);
#259248=SHAPE_DEFINITION_REPRESENTATION(#259269,#259388);
#259249=SHAPE_DEFINITION_REPRESENTATION(#259270,#259389);
#259250=PRODUCT_DEFINITION_SHAPE('',$,#259391);
#259251=PRODUCT_DEFINITION_SHAPE('',$,#259392);
#259252=PRODUCT_DEFINITION_SHAPE('',$,#259393);
#259253=PRODUCT_DEFINITION_SHAPE('',$,#259394);
#259254=PRODUCT_DEFINITION_SHAPE('',$,#259395);
#259255=PRODUCT_DEFINITION_SHAPE('',$,#259396);
#259256=PRODUCT_DEFINITION_SHAPE('',$,#259397);
#259257=PRODUCT_DEFINITION_SHAPE('',$,#259398);
#259258=PRODUCT_DEFINITION_SHAPE('',$,#259399);
#259259=PRODUCT_DEFINITION_SHAPE('',$,#259400);
#259260=PRODUCT_DEFINITION_SHAPE('',$,#259401);
#259261=PRODUCT_DEFINITION_SHAPE('',$,#259402);
#259262=PRODUCT_DEFINITION_SHAPE('',$,#259403);
#259263=PRODUCT_DEFINITION_SHAPE('',$,#259404);
#259264=PRODUCT_DEFINITION_SHAPE('',$,#259405);
#259265=PRODUCT_DEFINITION_SHAPE('',$,#259406);
#259266=PRODUCT_DEFINITION_SHAPE('',$,#259407);
#259267=PRODUCT_DEFINITION_SHAPE('',$,#259408);
#259268=PRODUCT_DEFINITION_SHAPE('',$,#259409);
#259269=PRODUCT_DEFINITION_SHAPE('',$,#259410);
#259270=PRODUCT_DEFINITION_SHAPE('',$,#259411);
#259271=PRODUCT_DEFINITION_SHAPE($,$,#305);
#259272=PRODUCT_DEFINITION_SHAPE($,$,#306);
#259273=PRODUCT_DEFINITION_SHAPE($,$,#307);
#259274=PRODUCT_DEFINITION_SHAPE($,$,#308);
#259275=PRODUCT_DEFINITION_SHAPE($,$,#309);
#259276=PRODUCT_DEFINITION_SHAPE($,$,#310);
#259277=PRODUCT_DEFINITION_SHAPE($,$,#311);
#259278=PRODUCT_DEFINITION_SHAPE($,$,#312);
#259279=PRODUCT_DEFINITION_SHAPE($,$,#313);
#259280=PRODUCT_DEFINITION_SHAPE($,$,#314);
#259281=PRODUCT_DEFINITION_SHAPE($,$,#315);
#259282=PRODUCT_DEFINITION_SHAPE($,$,#316);
#259283=PRODUCT_DEFINITION_SHAPE($,$,#317);
#259284=PRODUCT_DEFINITION_SHAPE($,$,#318);
#259285=PRODUCT_DEFINITION_SHAPE($,$,#319);
#259286=PRODUCT_DEFINITION_SHAPE($,$,#320);
#259287=PRODUCT_DEFINITION_SHAPE($,$,#321);
#259288=PRODUCT_DEFINITION_SHAPE($,$,#322);
#259289=PRODUCT_DEFINITION_SHAPE($,$,#323);
#259290=PRODUCT_DEFINITION_SHAPE($,$,#324);
#259291=PRODUCT_DEFINITION_SHAPE($,$,#325);
#259292=PRODUCT_DEFINITION_SHAPE($,$,#326);
#259293=PRODUCT_DEFINITION_SHAPE($,$,#327);
#259294=PRODUCT_DEFINITION_SHAPE($,$,#328);
#259295=PRODUCT_DEFINITION_SHAPE($,$,#329);
#259296=PRODUCT_DEFINITION_SHAPE($,$,#330);
#259297=PRODUCT_DEFINITION_SHAPE($,$,#331);
#259298=PRODUCT_DEFINITION_SHAPE($,$,#332);
#259299=PRODUCT_DEFINITION_SHAPE($,$,#333);
#259300=PRODUCT_DEFINITION_SHAPE($,$,#334);
#259301=PRODUCT_DEFINITION_SHAPE($,$,#335);
#259302=PRODUCT_DEFINITION_SHAPE($,$,#336);
#259303=PRODUCT_DEFINITION_SHAPE($,$,#337);
#259304=PRODUCT_DEFINITION_SHAPE($,$,#338);
#259305=PRODUCT_DEFINITION_SHAPE($,$,#339);
#259306=PRODUCT_DEFINITION_SHAPE($,$,#340);
#259307=PRODUCT_DEFINITION_SHAPE($,$,#341);
#259308=PRODUCT_DEFINITION_SHAPE($,$,#342);
#259309=PRODUCT_DEFINITION_SHAPE($,$,#343);
#259310=PRODUCT_DEFINITION_SHAPE($,$,#344);
#259311=PRODUCT_DEFINITION_SHAPE($,$,#345);
#259312=PRODUCT_DEFINITION_SHAPE($,$,#346);
#259313=PRODUCT_DEFINITION_SHAPE($,$,#347);
#259314=PRODUCT_DEFINITION_SHAPE($,$,#348);
#259315=PRODUCT_DEFINITION_SHAPE($,$,#349);
#259316=PRODUCT_DEFINITION_SHAPE($,$,#350);
#259317=PRODUCT_DEFINITION_SHAPE($,$,#351);
#259318=PRODUCT_DEFINITION_SHAPE($,$,#352);
#259319=PRODUCT_DEFINITION_SHAPE($,$,#353);
#259320=PRODUCT_DEFINITION_SHAPE($,$,#354);
#259321=PRODUCT_DEFINITION_SHAPE($,$,#355);
#259322=PRODUCT_DEFINITION_SHAPE($,$,#356);
#259323=PRODUCT_DEFINITION_SHAPE($,$,#357);
#259324=PRODUCT_DEFINITION_SHAPE($,$,#358);
#259325=PRODUCT_DEFINITION_SHAPE($,$,#359);
#259326=PRODUCT_DEFINITION_SHAPE($,$,#360);
#259327=PRODUCT_DEFINITION_SHAPE($,$,#361);
#259328=PRODUCT_DEFINITION_SHAPE($,$,#362);
#259329=PRODUCT_DEFINITION_SHAPE($,$,#363);
#259330=PRODUCT_DEFINITION_SHAPE($,$,#364);
#259331=PRODUCT_DEFINITION_SHAPE($,$,#365);
#259332=PRODUCT_DEFINITION_SHAPE($,$,#366);
#259333=PRODUCT_DEFINITION_SHAPE($,$,#367);
#259334=PRODUCT_DEFINITION_SHAPE($,$,#368);
#259335=PRODUCT_DEFINITION_SHAPE($,$,#369);
#259336=PRODUCT_DEFINITION_SHAPE($,$,#370);
#259337=PRODUCT_DEFINITION_SHAPE($,$,#371);
#259338=PRODUCT_DEFINITION_SHAPE($,$,#372);
#259339=PRODUCT_DEFINITION_SHAPE($,$,#373);
#259340=PRODUCT_DEFINITION_SHAPE($,$,#374);
#259341=PRODUCT_DEFINITION_SHAPE($,$,#375);
#259342=PRODUCT_DEFINITION_SHAPE($,$,#376);
#259343=PRODUCT_DEFINITION_SHAPE($,$,#377);
#259344=PRODUCT_DEFINITION_SHAPE($,$,#378);
#259345=PRODUCT_DEFINITION_SHAPE($,$,#379);
#259346=PRODUCT_DEFINITION_SHAPE($,$,#380);
#259347=PRODUCT_DEFINITION_SHAPE($,$,#381);
#259348=PRODUCT_DEFINITION_SHAPE($,$,#382);
#259349=PRODUCT_DEFINITION_SHAPE($,$,#383);
#259350=PRODUCT_DEFINITION_SHAPE($,$,#384);
#259351=PRODUCT_DEFINITION_SHAPE($,$,#385);
#259352=PRODUCT_DEFINITION_SHAPE($,$,#386);
#259353=PRODUCT_DEFINITION_SHAPE($,$,#387);
#259354=PRODUCT_DEFINITION_SHAPE($,$,#388);
#259355=PRODUCT_DEFINITION_SHAPE($,$,#389);
#259356=PRODUCT_DEFINITION_SHAPE($,$,#390);
#259357=PRODUCT_DEFINITION_SHAPE($,$,#391);
#259358=PRODUCT_DEFINITION_SHAPE($,$,#392);
#259359=PRODUCT_DEFINITION_SHAPE($,$,#393);
#259360=PRODUCT_DEFINITION_SHAPE($,$,#394);
#259361=PRODUCT_DEFINITION_SHAPE($,$,#395);
#259362=PRODUCT_DEFINITION_SHAPE($,$,#396);
#259363=PRODUCT_DEFINITION_SHAPE($,$,#397);
#259364=PRODUCT_DEFINITION_SHAPE($,$,#398);
#259365=PRODUCT_DEFINITION_SHAPE($,$,#399);
#259366=PRODUCT_DEFINITION_SHAPE($,$,#400);
#259367=PRODUCT_DEFINITION_SHAPE($,$,#401);
#259368=PRODUCT_DEFINITION_SHAPE($,$,#402);
#259369=SHAPE_REPRESENTATION('',(#25391,#27236,#27237,#27238,#27239,#27240,
#27241,#27242,#27243,#27244,#27245,#27246,#27247,#27248,#27249,#27250,#27251,
#27252,#27253,#27254,#27255,#27256,#27257,#27258,#27259,#27260,#27261,#27262,
#27263,#27264,#27265,#27266,#27267,#27268,#27269,#27270,#27271,#27272,#27273,
#27274,#27275,#27276,#27277,#27278,#27279,#27280,#27281,#27282,#27283,#27284,
#27285,#27286,#27287,#27288,#27289,#27290,#27291,#27292,#27293,#27294,#27295,
#27296,#27297,#27298,#27299,#27300,#27301,#27302,#27303,#27304,#27305,#27306,
#27307,#27308,#27309,#27310,#27311,#27312,#27313,#27314,#27315,#27316,#27317,
#27318,#27319,#27320,#27321,#27322,#27323,#27324,#27325,#27326,#27327,#27328,
#27329,#27330,#27331,#27332,#27333),#259203);
#259370=SHAPE_REPRESENTATION('',(#25392),#259204);
#259371=SHAPE_REPRESENTATION('',(#25757),#259205);
#259372=SHAPE_REPRESENTATION('',(#25778),#259206);
#259373=SHAPE_REPRESENTATION('',(#25811),#259207);
#259374=SHAPE_REPRESENTATION('',(#25864),#259208);
#259375=SHAPE_REPRESENTATION('',(#26314),#259209);
#259376=SHAPE_REPRESENTATION('',(#26659),#259210);
#259377=SHAPE_REPRESENTATION('',(#27001),#259211);
#259378=SHAPE_REPRESENTATION('',(#27010),#259212);
#259379=SHAPE_REPRESENTATION('',(#27076),#259213);
#259380=SHAPE_REPRESENTATION('',(#27083),#259214);
#259381=SHAPE_REPRESENTATION('',(#27092),#259215);
#259382=SHAPE_REPRESENTATION('',(#27110),#259216);
#259383=SHAPE_REPRESENTATION('',(#27121),#259217);
#259384=SHAPE_REPRESENTATION('',(#27130),#259218);
#259385=SHAPE_REPRESENTATION('',(#27139),#259219);
#259386=SHAPE_REPRESENTATION('',(#27148),#259220);
#259387=SHAPE_REPRESENTATION('',(#27159),#259221);
#259388=SHAPE_REPRESENTATION('',(#27170),#259222);
#259389=SHAPE_REPRESENTATION('',(#27176),#259223);
#259390=PRODUCT_DEFINITION_CONTEXT('part definition',#259455,'design');
#259391=PRODUCT_DEFINITION('MAS-355','MAS-355',#259412,#259390);
#259392=PRODUCT_DEFINITION('Casing','Casing',#259413,#259390);
#259393=PRODUCT_DEFINITION('Bearing partition','Bearing partition',#259414,
#259390);
#259394=PRODUCT_DEFINITION('End cover','End cover',#259415,#259390);
#259395=PRODUCT_DEFINITION('Input shaft','Input shaft',#259416,#259390);
#259396=PRODUCT_DEFINITION('Ring gear','Ring gear',#259417,#259390);
#259397=PRODUCT_DEFINITION('Sun gear','Sun gear',#259418,#259390);
#259398=PRODUCT_DEFINITION('Planet gear','Planet gear',#259419,#259390);
#259399=PRODUCT_DEFINITION('Journal bushing','Journal bushing',#259420,
#259390);
#259400=PRODUCT_DEFINITION('Carrier','Carrier',#259421,#259390);
#259401=PRODUCT_DEFINITION('Drive key','Drive key',#259422,#259390);
#259402=PRODUCT_DEFINITION('Planet bushing','Planet bushing',#259423,#259390);
#259403=PRODUCT_DEFINITION('Planet pin','Planet pin',#259424,#259390);
#259404=PRODUCT_DEFINITION('Pivot retaining ring',
'Pivot retaining ring',#259425,#259390);
#259405=PRODUCT_DEFINITION('Pivot washer','Pivot washer',#259426,#259390);
#259406=PRODUCT_DEFINITION('Sun thrust washer','Sun thrust washer',#259427,
#259390);
#259407=PRODUCT_DEFINITION('Journal thrust washer',
'Journal thrust washer',#259428,#259390);
#259408=PRODUCT_DEFINITION('Sun retaining ring','Sun retaining ring',#259429,
#259390);
#259409=PRODUCT_DEFINITION('Journal retaining ring',
'Journal retaining ring',#259430,#259390);
#259410=PRODUCT_DEFINITION('Locating dowel','Locating dowel',#259431,#259390);
#259411=PRODUCT_DEFINITION('Socket head cap screw M6x20',
'Socket head cap screw M6x20',#259432,#259390);
#259412=PRODUCT_DEFINITION_FORMATION('',$,#259457);
#259413=PRODUCT_DEFINITION_FORMATION('',$,#259458);
#259414=PRODUCT_DEFINITION_FORMATION('',$,#259459);
#259415=PRODUCT_DEFINITION_FORMATION('',$,#259460);
#259416=PRODUCT_DEFINITION_FORMATION('',$,#259461);
#259417=PRODUCT_DEFINITION_FORMATION('',$,#259462);
#259418=PRODUCT_DEFINITION_FORMATION('',$,#259463);
#259419=PRODUCT_DEFINITION_FORMATION('',$,#259464);
#259420=PRODUCT_DEFINITION_FORMATION('',$,#259465);
#259421=PRODUCT_DEFINITION_FORMATION('',$,#259466);
#259422=PRODUCT_DEFINITION_FORMATION('',$,#259467);
#259423=PRODUCT_DEFINITION_FORMATION('',$,#259468);
#259424=PRODUCT_DEFINITION_FORMATION('',$,#259469);
#259425=PRODUCT_DEFINITION_FORMATION('',$,#259470);
#259426=PRODUCT_DEFINITION_FORMATION('',$,#259471);
#259427=PRODUCT_DEFINITION_FORMATION('',$,#259472);
#259428=PRODUCT_DEFINITION_FORMATION('',$,#259473);
#259429=PRODUCT_DEFINITION_FORMATION('',$,#259474);
#259430=PRODUCT_DEFINITION_FORMATION('',$,#259475);
#259431=PRODUCT_DEFINITION_FORMATION('',$,#259476);
#259432=PRODUCT_DEFINITION_FORMATION('',$,#259477);
#259433=PRODUCT_RELATED_PRODUCT_CATEGORY('MAS-355','MAS-355',(#259457));
#259434=PRODUCT_RELATED_PRODUCT_CATEGORY('Casing','Casing',(#259458));
#259435=PRODUCT_RELATED_PRODUCT_CATEGORY('Bearing partition',
'Bearing partition',(#259459));
#259436=PRODUCT_RELATED_PRODUCT_CATEGORY('End cover','End cover',(#259460));
#259437=PRODUCT_RELATED_PRODUCT_CATEGORY('Input shaft','Input shaft',(#259461));
#259438=PRODUCT_RELATED_PRODUCT_CATEGORY('Ring gear','Ring gear',(#259462));
#259439=PRODUCT_RELATED_PRODUCT_CATEGORY('Sun gear','Sun gear',(#259463));
#259440=PRODUCT_RELATED_PRODUCT_CATEGORY('Planet gear','Planet gear',(#259464));
#259441=PRODUCT_RELATED_PRODUCT_CATEGORY('Journal bushing',
'Journal bushing',(#259465));
#259442=PRODUCT_RELATED_PRODUCT_CATEGORY('Carrier','Carrier',(#259466));
#259443=PRODUCT_RELATED_PRODUCT_CATEGORY('Drive key','Drive key',(#259467));
#259444=PRODUCT_RELATED_PRODUCT_CATEGORY('Planet bushing',
'Planet bushing',(#259468));
#259445=PRODUCT_RELATED_PRODUCT_CATEGORY('Planet pin','Planet pin',(#259469));
#259446=PRODUCT_RELATED_PRODUCT_CATEGORY('Pivot retaining ring',
'Pivot retaining ring',(#259470));
#259447=PRODUCT_RELATED_PRODUCT_CATEGORY('Pivot washer','Pivot washer',
(#259471));
#259448=PRODUCT_RELATED_PRODUCT_CATEGORY('Sun thrust washer',
'Sun thrust washer',(#259472));
#259449=PRODUCT_RELATED_PRODUCT_CATEGORY('Journal thrust washer',
'Journal thrust washer',(#259473));
#259450=PRODUCT_RELATED_PRODUCT_CATEGORY('Sun retaining ring',
'Sun retaining ring',(#259474));
#259451=PRODUCT_RELATED_PRODUCT_CATEGORY('Journal retaining ring',
'Journal retaining ring',(#259475));
#259452=PRODUCT_RELATED_PRODUCT_CATEGORY('Locating dowel',
'Locating dowel',(#259476));
#259453=PRODUCT_RELATED_PRODUCT_CATEGORY('Socket head cap screw M6x20',
'Socket head cap screw M6x20',(#259477));
#259454=APPLICATION_PROTOCOL_DEFINITION('international standard',
'automotive_design',2009,#259455);
#259455=APPLICATION_CONTEXT(
'Core Data for Automotive Mechanical Design Process');
#259456=PRODUCT_CONTEXT('part definition',#259455,'mechanical');
#259457=PRODUCT('MAS-355','MAS-355',
'Independent two-stage fixed-ring planetary gearbox,24/24/72 teeth,mod
ule2,20deg involutes,three planets per stage,4:1 x4:1=16:1. Native cut
-space/fillet/pattern tooth profiles derived from reusable gear blanks
; shared sun/planet/ring/carrier parts across both stages. Captured br
onze-journal input/carriers, headed retained planet pins, keyed inters
tage drive and modular keyed output interface. Native ideal gear links
; no torque, precision grade, production backlash/fits, lubrication, s
peed or life rating.',(#259456));
#259458=PRODUCT('Casing','Casing',$,(#259456));
#259459=PRODUCT('Bearing partition','Bearing partition',$,(#259456));
#259460=PRODUCT('End cover','End cover',$,(#259456));
#259461=PRODUCT('Input shaft','Input shaft','Input shaft',(#259456));
#259462=PRODUCT('Ring gear','Ring gear',
'{"standard_geometry": "Unshifted20degree involute", "teeth": 72, "mod
ule_mm": 2, "pitch_diameter_mm": 144.0, "root_diameter_mm": 149.0, "ti
p_diameter_mm": 140.0, "face_mm": 12, "per_gear_circular_tooth_thinnin
g_mm": 0.1, "derived_root_fillet_mm": 0.5, "involute_fit_points_per_fl
ank": 41, "internal": true, "source_stock": "Native reusable Gear blan
k; assembly-specific machining", "manufacturing_scope": "Standard prof
ile reference; grade, cutter/root transition validation, tolerances, b
acklash and load rating require production selection."}',(#259456));
#259463=PRODUCT('Sun gear','Sun gear',
'{"standard_geometry": "Unshifted20degree involute", "teeth": 24, "mod
ule_mm": 2, "pitch_diameter_mm": 48.0, "root_diameter_mm": 43.0, "tip_
diameter_mm": 52.0, "face_mm": 12, "per_gear_circular_tooth_thinning_m
m": 0.1, "derived_root_fillet_mm": 0.5, "involute_fit_points_per_flank
": 41, "internal": false, "source_stock": "Native reusable Gear blank;
 assembly-specific machining", "manufacturing_scope": "Standard profil
e reference; grade, cutter/root transition validation, tolerances, bac
klash and load rating require production selection."}',(#259456));
#259464=PRODUCT('Planet gear','Planet gear',
'{"standard_geometry": "Unshifted20degree involute", "teeth": 24, "mod
ule_mm": 2, "pitch_diameter_mm": 48.0, "root_diameter_mm": 43.0, "tip_
diameter_mm": 52.0, "face_mm": 12, "per_gear_circular_tooth_thinning_m
m": 0.1, "derived_root_fillet_mm": 0.5, "involute_fit_points_per_flank
": 41, "internal": false, "source_stock": "Native reusable Gear blank;
 assembly-specific machining", "manufacturing_scope": "Standard profil
e reference; grade, cutter/root transition validation, tolerances, bac
klash and load rating require production selection."}',(#259456));
#259465=PRODUCT('Journal bushing','Journal bushing',$,(#259456));
#259466=PRODUCT('Carrier','Carrier',$,(#259456));
#259467=PRODUCT('Drive key','Drive key',$,(#259456));
#259468=PRODUCT('Planet bushing','Planet bushing',$,(#259456));
#259469=PRODUCT('Planet pin','Planet pin',$,(#259456));
#259470=PRODUCT('Pivot retaining ring','Pivot retaining ring',$,(#259456));
#259471=PRODUCT('Pivot washer','Pivot washer',$,(#259456));
#259472=PRODUCT('Sun thrust washer','Sun thrust washer',$,(#259456));
#259473=PRODUCT('Journal thrust washer','Journal thrust washer',$,(#259456));
#259474=PRODUCT('Sun retaining ring','Sun retaining ring',$,(#259456));
#259475=PRODUCT('Journal retaining ring','Journal retaining ring',$,(#259456));
#259476=PRODUCT('Locating dowel','Locating dowel',$,(#259456));
#259477=PRODUCT('Socket head cap screw M6x20',
'Socket head cap screw M6x20',$,(#259456));
#259478=PRESENTATION_STYLE_ASSIGNMENT((#259493));
#259479=PRESENTATION_STYLE_ASSIGNMENT((#259494));
#259480=PRESENTATION_STYLE_ASSIGNMENT((#259495));
#259481=PRESENTATION_STYLE_ASSIGNMENT((#259496));
#259482=PRESENTATION_STYLE_ASSIGNMENT((#259497));
#259483=PRESENTATION_STYLE_ASSIGNMENT((#259498));
#259484=PRESENTATION_STYLE_ASSIGNMENT((#259499));
#259485=PRESENTATION_STYLE_ASSIGNMENT((#259500));
#259486=PRESENTATION_STYLE_ASSIGNMENT((#259501));
#259487=PRESENTATION_STYLE_ASSIGNMENT((#259502));
#259488=PRESENTATION_STYLE_ASSIGNMENT((#259503));
#259489=PRESENTATION_STYLE_ASSIGNMENT((#259504));
#259490=PRESENTATION_STYLE_ASSIGNMENT((#259505));
#259491=PRESENTATION_STYLE_ASSIGNMENT((#259506));
#259492=PRESENTATION_STYLE_ASSIGNMENT((#259507));
#259493=SURFACE_STYLE_USAGE(.BOTH.,#259508);
#259494=SURFACE_STYLE_USAGE(.BOTH.,#259509);
#259495=SURFACE_STYLE_USAGE(.BOTH.,#259510);
#259496=SURFACE_STYLE_USAGE(.BOTH.,#259511);
#259497=SURFACE_STYLE_USAGE(.BOTH.,#259512);
#259498=SURFACE_STYLE_USAGE(.BOTH.,#259513);
#259499=SURFACE_STYLE_USAGE(.BOTH.,#259514);
#259500=SURFACE_STYLE_USAGE(.BOTH.,#259515);
#259501=SURFACE_STYLE_USAGE(.BOTH.,#259516);
#259502=SURFACE_STYLE_USAGE(.BOTH.,#259517);
#259503=SURFACE_STYLE_USAGE(.BOTH.,#259518);
#259504=SURFACE_STYLE_USAGE(.BOTH.,#259519);
#259505=SURFACE_STYLE_USAGE(.BOTH.,#259520);
#259506=SURFACE_STYLE_USAGE(.BOTH.,#259521);
#259507=SURFACE_STYLE_USAGE(.BOTH.,#259522);
#259508=SURFACE_SIDE_STYLE('',(#259523));
#259509=SURFACE_SIDE_STYLE('',(#259524));
#259510=SURFACE_SIDE_STYLE('',(#259525));
#259511=SURFACE_SIDE_STYLE('',(#259526));
#259512=SURFACE_SIDE_STYLE('',(#259527));
#259513=SURFACE_SIDE_STYLE('',(#259528));
#259514=SURFACE_SIDE_STYLE('',(#259529));
#259515=SURFACE_SIDE_STYLE('',(#259530));
#259516=SURFACE_SIDE_STYLE('',(#259531));
#259517=SURFACE_SIDE_STYLE('',(#259532));
#259518=SURFACE_SIDE_STYLE('',(#259533));
#259519=SURFACE_SIDE_STYLE('',(#259534));
#259520=SURFACE_SIDE_STYLE('',(#259535));
#259521=SURFACE_SIDE_STYLE('',(#259536));
#259522=SURFACE_SIDE_STYLE('',(#259537));
#259523=SURFACE_STYLE_FILL_AREA(#259538);
#259524=SURFACE_STYLE_FILL_AREA(#259539);
#259525=SURFACE_STYLE_FILL_AREA(#259540);
#259526=SURFACE_STYLE_FILL_AREA(#259541);
#259527=SURFACE_STYLE_FILL_AREA(#259542);
#259528=SURFACE_STYLE_FILL_AREA(#259543);
#259529=SURFACE_STYLE_FILL_AREA(#259544);
#259530=SURFACE_STYLE_FILL_AREA(#259545);
#259531=SURFACE_STYLE_FILL_AREA(#259546);
#259532=SURFACE_STYLE_FILL_AREA(#259547);
#259533=SURFACE_STYLE_FILL_AREA(#259548);
#259534=SURFACE_STYLE_FILL_AREA(#259549);
#259535=SURFACE_STYLE_FILL_AREA(#259550);
#259536=SURFACE_STYLE_FILL_AREA(#259551);
#259537=SURFACE_STYLE_FILL_AREA(#259552);
#259538=FILL_AREA_STYLE('Steel - Satin',(#259553));
#259539=FILL_AREA_STYLE('Casing dark blue',(#259554));
#259540=FILL_AREA_STYLE('Partition gray',(#259555));
#259541=FILL_AREA_STYLE('Cover sky blue',(#259556));
#259542=FILL_AREA_STYLE('Shaft gray',(#259557));
#259543=FILL_AREA_STYLE('Ring dark blue',(#259558));
#259544=FILL_AREA_STYLE('Gear light blue',(#259559));
#259545=FILL_AREA_STYLE('Bearing light gray',(#259560));
#259546=FILL_AREA_STYLE('Carrier sky blue',(#259561));
#259547=FILL_AREA_STYLE('Key gray',(#259562));
#259548=FILL_AREA_STYLE('Pin gray',(#259563));
#259549=FILL_AREA_STYLE('Dark gray',(#259564));
#259550=FILL_AREA_STYLE('Washer light gray',(#259565));
#259551=FILL_AREA_STYLE('Dowel gray',(#259566));
#259552=FILL_AREA_STYLE('Fastener dark gray',(#259567));
#259553=FILL_AREA_STYLE_COLOUR('Steel - Satin',#259568);
#259554=FILL_AREA_STYLE_COLOUR('Casing dark blue',#259569);
#259555=FILL_AREA_STYLE_COLOUR('Partition gray',#259570);
#259556=FILL_AREA_STYLE_COLOUR('Cover sky blue',#259571);
#259557=FILL_AREA_STYLE_COLOUR('Shaft gray',#259572);
#259558=FILL_AREA_STYLE_COLOUR('Ring dark blue',#259573);
#259559=FILL_AREA_STYLE_COLOUR('Gear light blue',#259574);
#259560=FILL_AREA_STYLE_COLOUR('Bearing light gray',#259575);
#259561=FILL_AREA_STYLE_COLOUR('Carrier sky blue',#259576);
#259562=FILL_AREA_STYLE_COLOUR('Key gray',#259577);
#259563=FILL_AREA_STYLE_COLOUR('Pin gray',#259578);
#259564=FILL_AREA_STYLE_COLOUR('Dark gray',#259579);
#259565=FILL_AREA_STYLE_COLOUR('Washer light gray',#259580);
#259566=FILL_AREA_STYLE_COLOUR('Dowel gray',#259581);
#259567=FILL_AREA_STYLE_COLOUR('Fastener dark gray',#259582);
#259568=COLOUR_RGB('Steel - Satin',0.627450980392157,0.627450980392157,
0.627450980392157);
#259569=COLOUR_RGB('Casing dark blue',0.0901960784313725,0.270588235294118,
0.513725490196078);
#259570=COLOUR_RGB('Partition gray',0.407843137254902,0.447058823529412,
0.498039215686275);
#259571=COLOUR_RGB('Cover sky blue',0.317647058823529,0.686274509803922,
0.890196078431372);
#259572=COLOUR_RGB('Shaft gray',0.576470588235294,0.615686274509804,0.666666666666667);
#259573=COLOUR_RGB('Ring dark blue',0.0901960784313725,0.270588235294118,
0.513725490196078);
#259574=COLOUR_RGB('Gear light blue',0.662745098039216,0.831372549019608,
0.949019607843137);
#259575=COLOUR_RGB('Bearing light gray',0.725490196078431,0.752941176470588,
0.792156862745098);
#259576=COLOUR_RGB('Carrier sky blue',0.317647058823529,0.686274509803922,
0.890196078431372);
#259577=COLOUR_RGB('Key gray',0.576470588235294,0.615686274509804,0.666666666666667);
#259578=COLOUR_RGB('Pin gray',0.576470588235294,0.615686274509804,0.666666666666667);
#259579=COLOUR_RGB('Dark gray',0.250980392156863,0.282352941176471,0.32156862745098);
#259580=COLOUR_RGB('Washer light gray',0.725490196078431,0.752941176470588,
0.792156862745098);
#259581=COLOUR_RGB('Dowel gray',0.576470588235294,0.615686274509804,0.666666666666667);
#259582=COLOUR_RGB('Fastener dark gray',0.250980392156863,0.282352941176471,
0.32156862745098);
ENDSEC;
END-ISO-10303-21;
